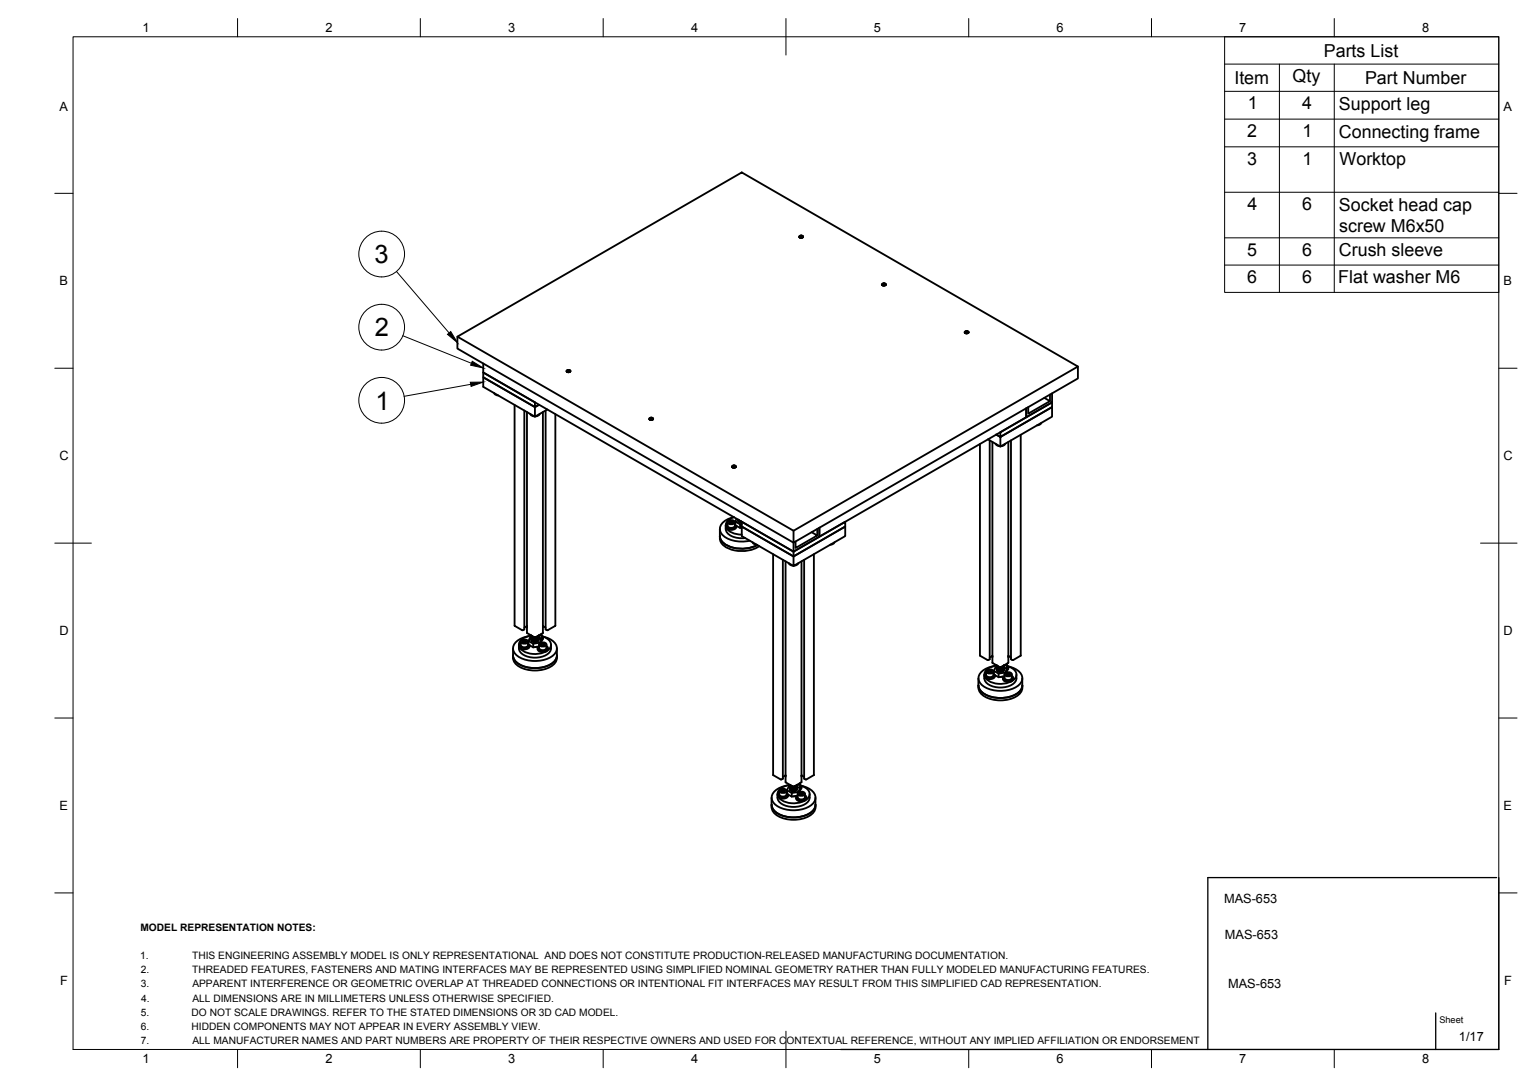
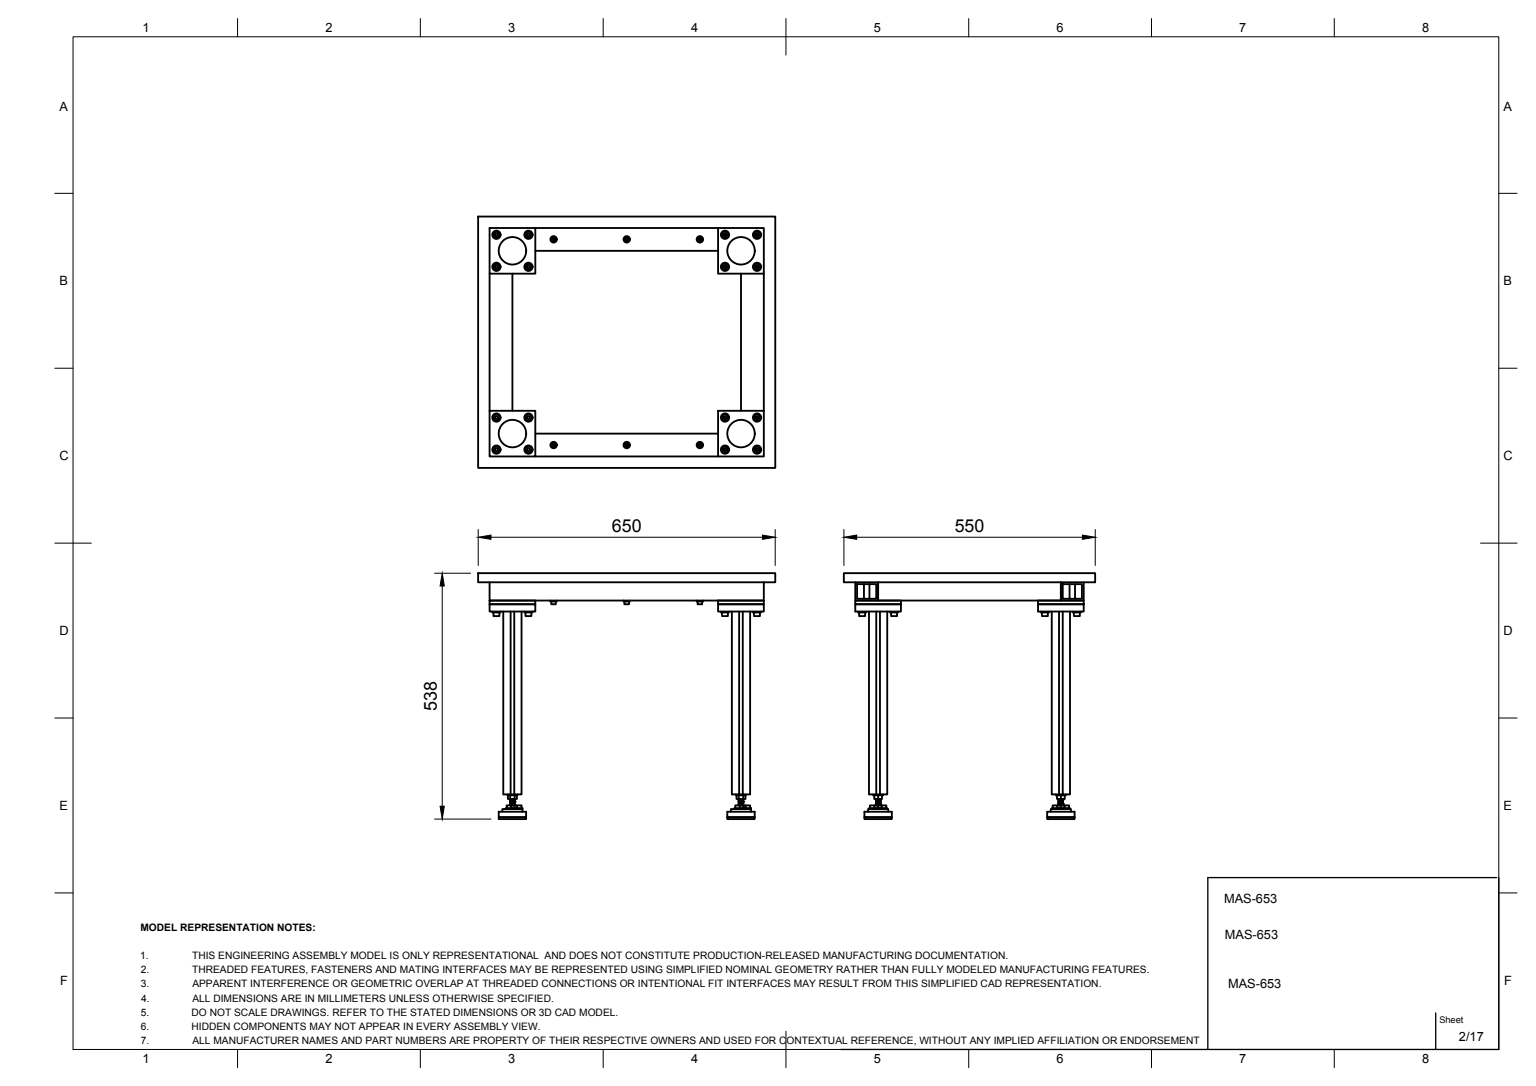
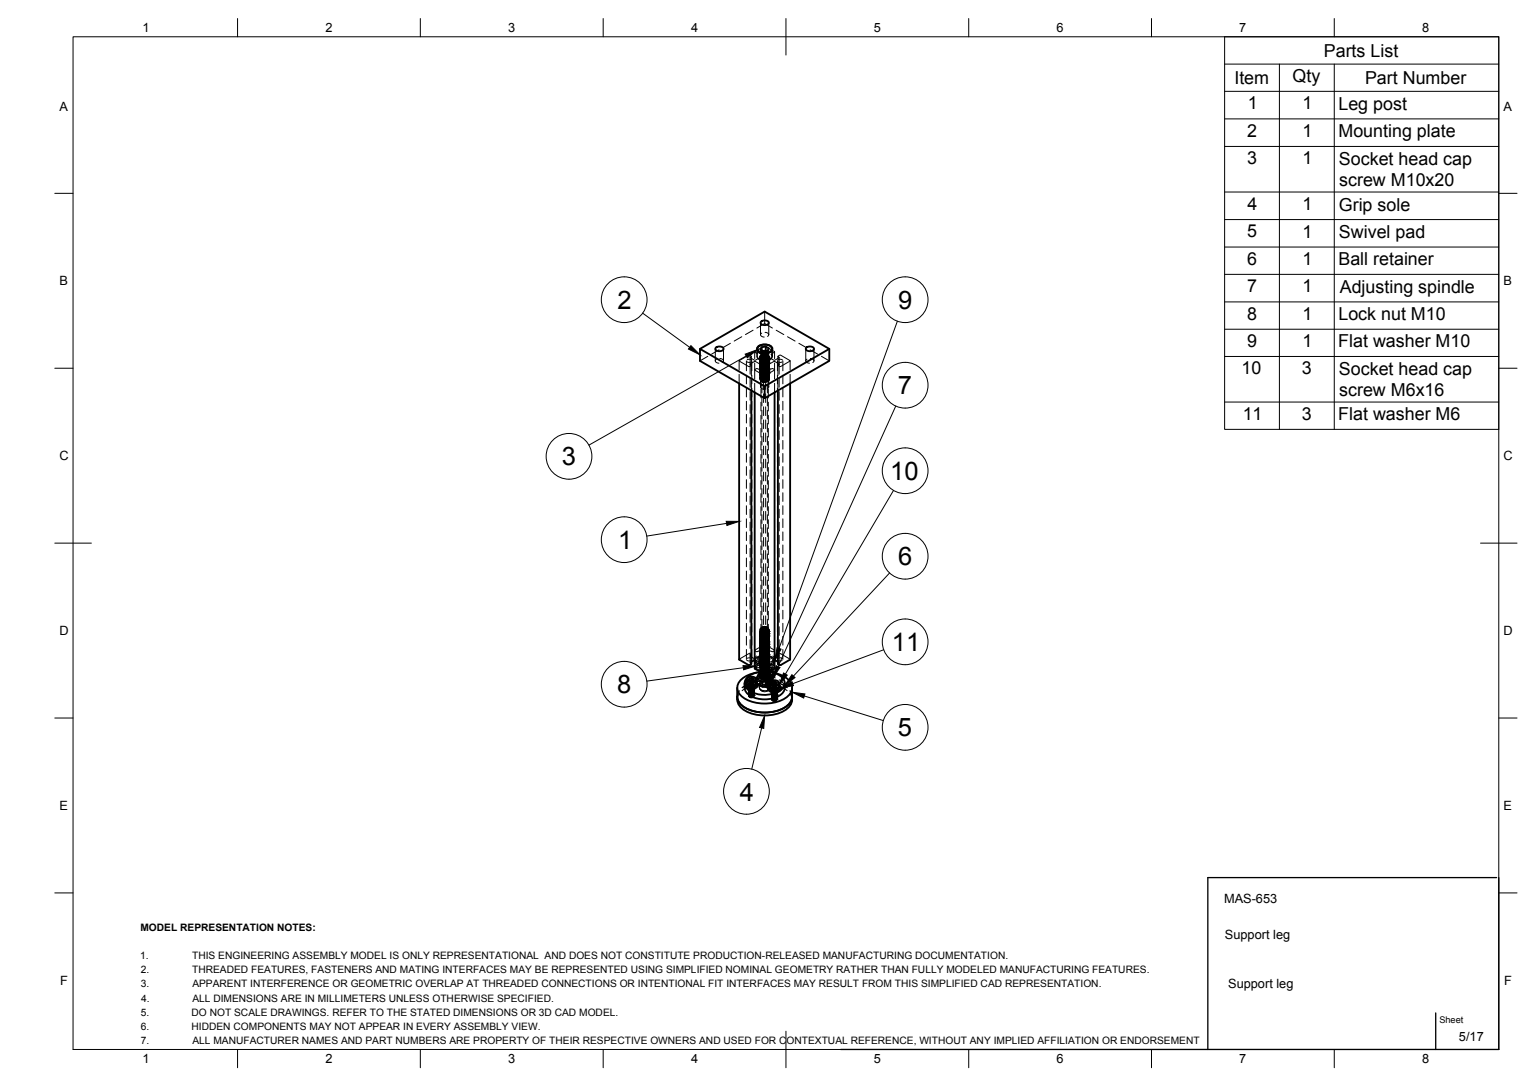
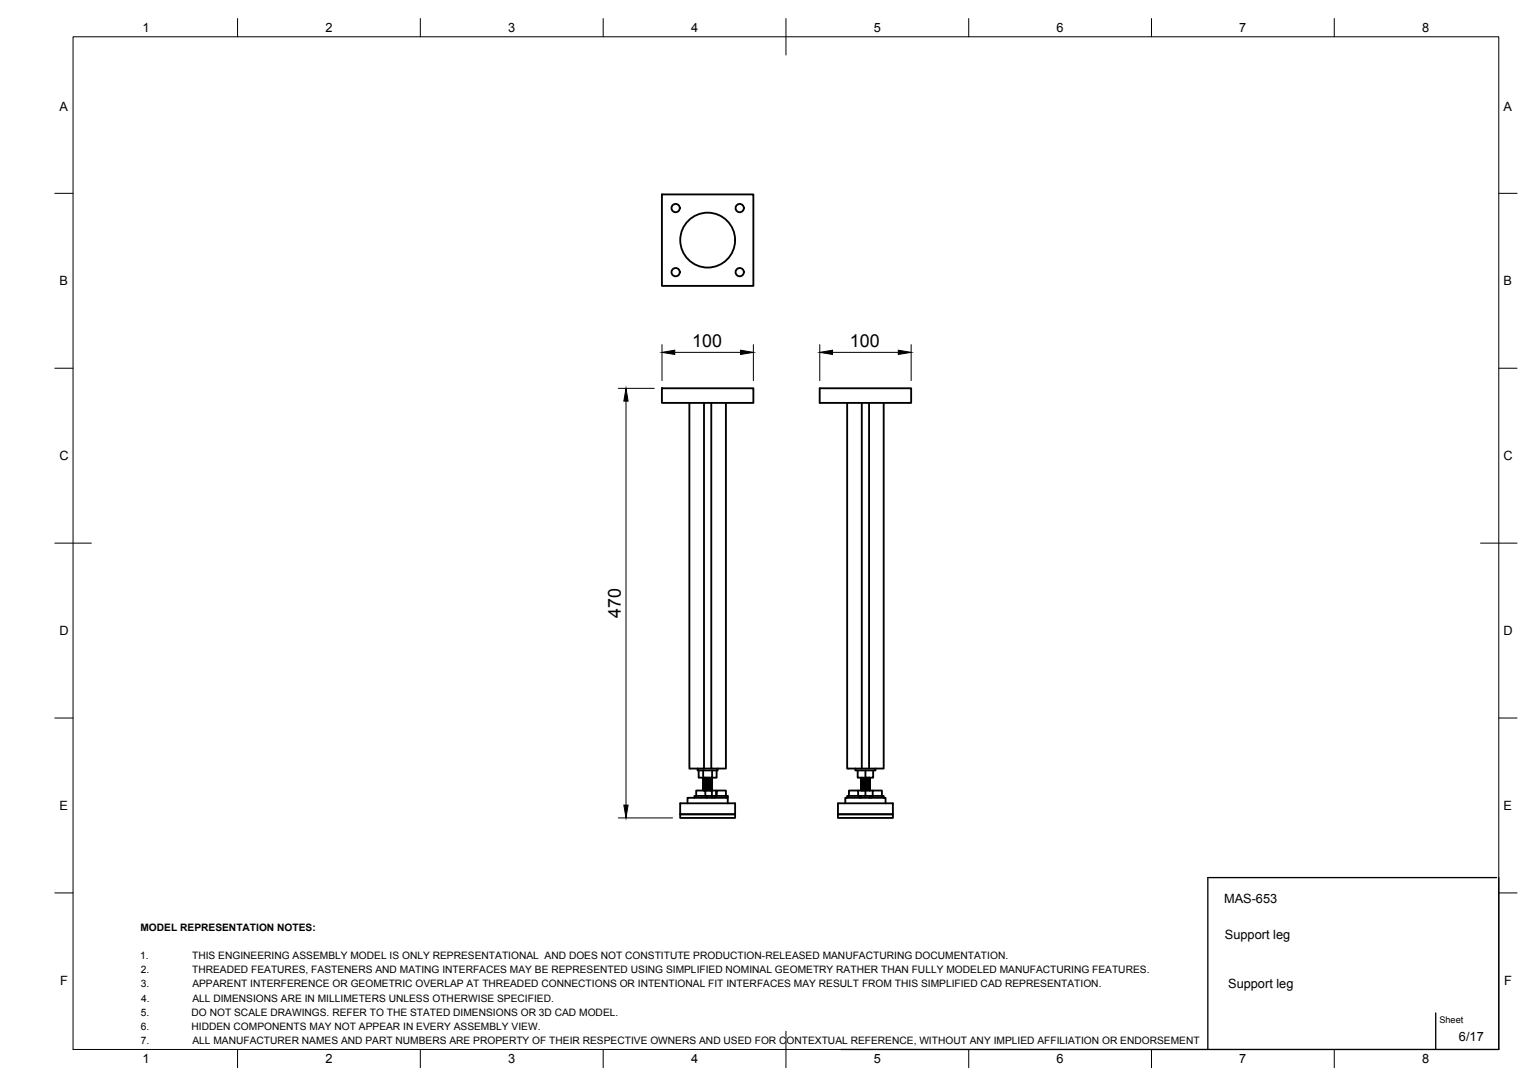
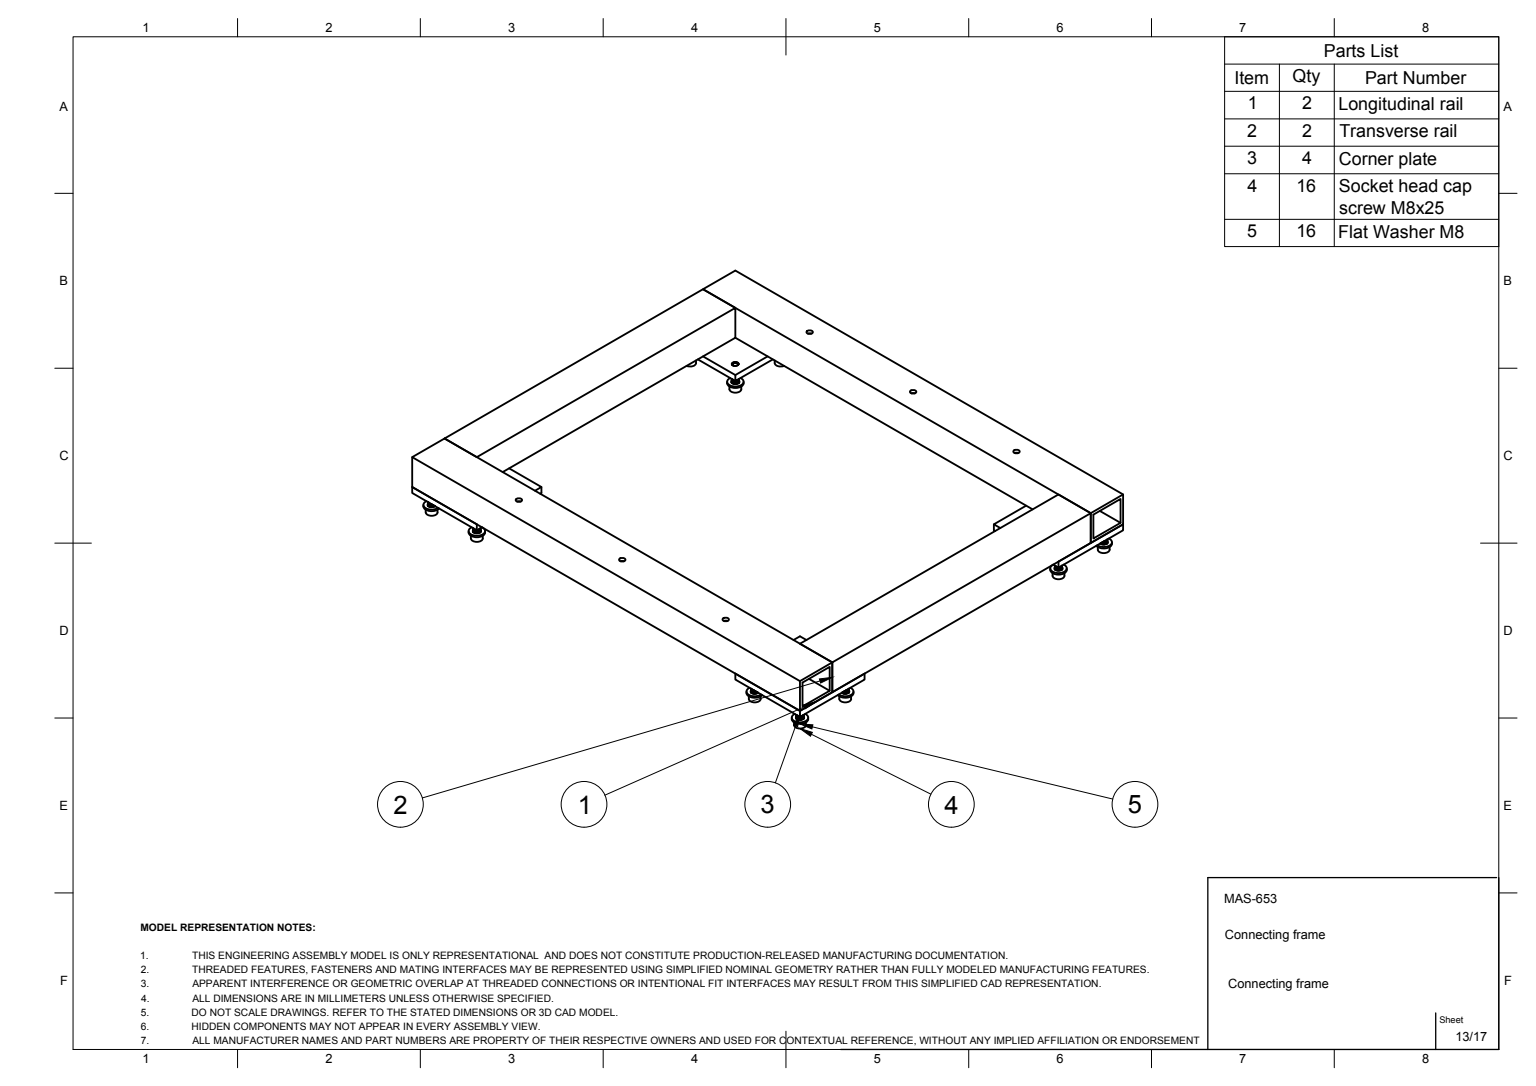
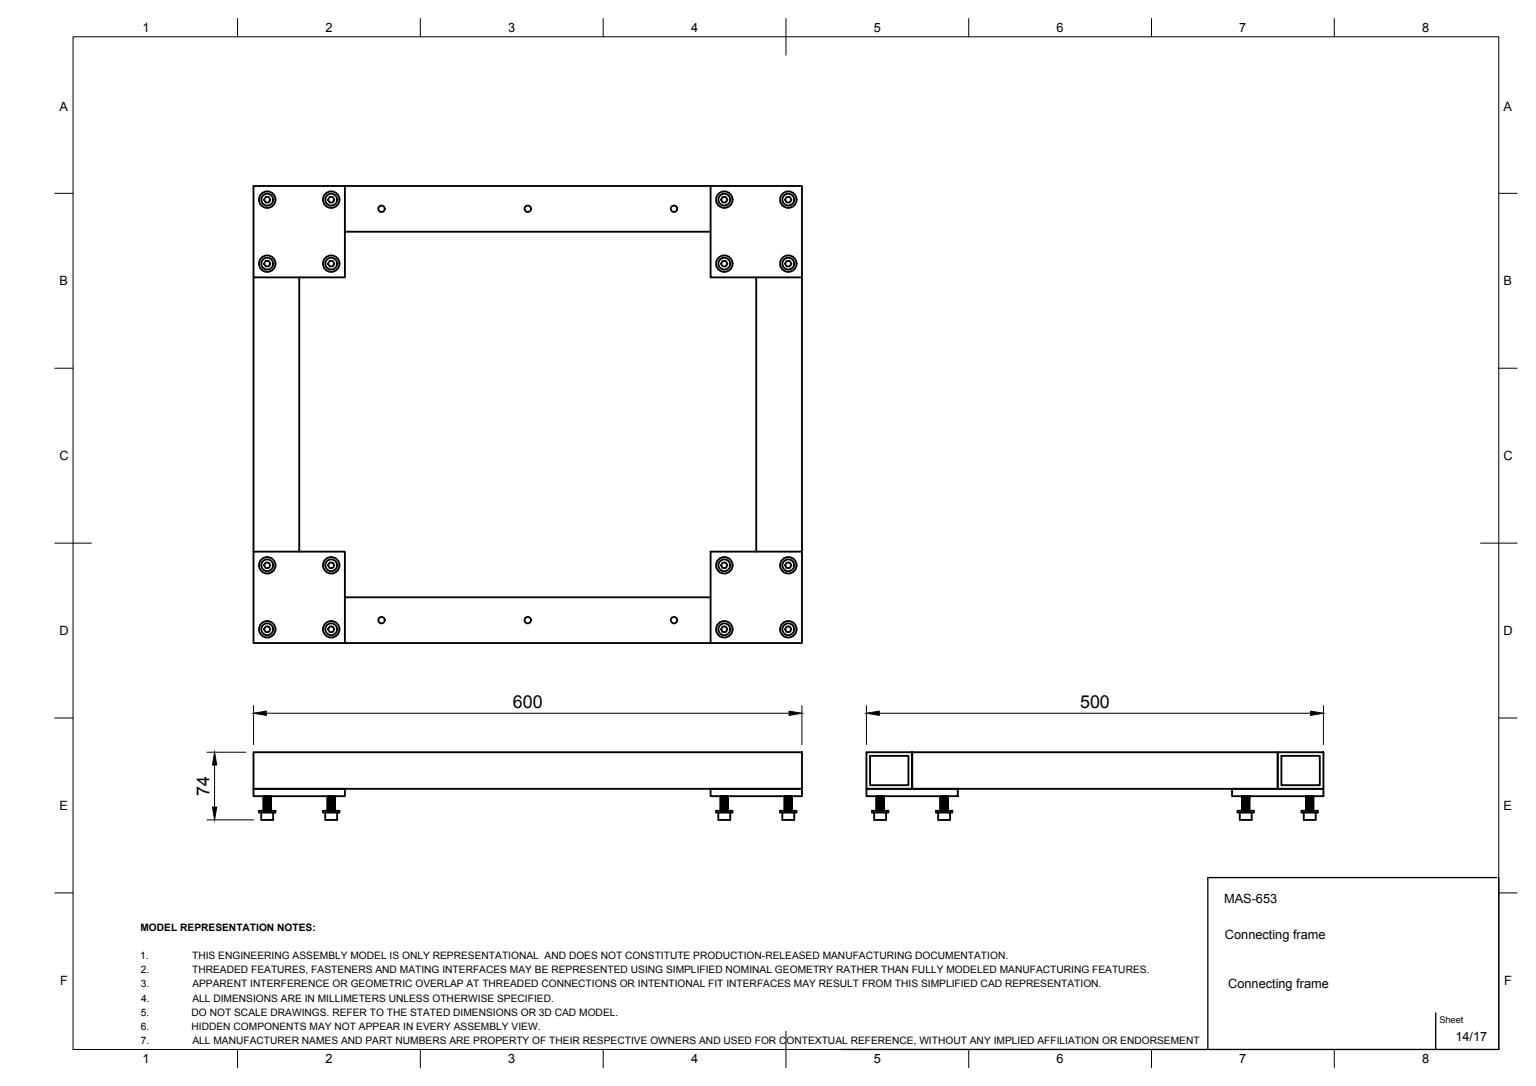
ISO-10303-21;
HEADER;
/* Generated by software containing ST-Developer
 * from STEP Tools, Inc. (www.steptools.com) 
 */

FILE_DESCRIPTION(
/* description */ ('Independent compact industrial fixture table, bolted aluminum worktop
 on connected adjustable support base. Whole-mm nominal dimensions. No
 load rating assigned.'),
/* implementation_level */ '2;1');

FILE_NAME(
/* name */ 'MAS-653.step',
/* time_stamp */ '2026-11-07T17:47:58-08:00',
/* author */ (''),
/* organization */ (''),
/* preprocessor_version */ 'ST-DEVELOPER v20.2',
/* originating_system */ 'Autodesk Translation Framework v15.17.0.0',
/* authorisation */ '');

FILE_SCHEMA (('AUTOMOTIVE_DESIGN { 1 0 10303 214 3 1 1 }'));
ENDSEC;

DATA;
#10=MECHANICAL_DESIGN_GEOMETRIC_PRESENTATION_REPRESENTATION('',(#2250,#2251,
#2252,#2253,#2254,#2255,#2256,#2257,#2258,#2259,#2260,#2261,#2262,#2263,
#2264,#2265,#2266,#2267,#2268),#97475);
#11=SPHERICAL_SURFACE('',#22780,6.);
#12=SPHERICAL_SURFACE('',#22798,6.);
#13=SPHERICAL_SURFACE('',#22948,6.);
#14=ITEM_DEFINED_TRANSFORMATION($,$,#22042,#22256);
#15=ITEM_DEFINED_TRANSFORMATION($,$,#22071,#22257);
#16=ITEM_DEFINED_TRANSFORMATION($,$,#22082,#22258);
#17=ITEM_DEFINED_TRANSFORMATION($,$,#22177,#22259);
#18=ITEM_DEFINED_TRANSFORMATION($,$,#22247,#22260);
#19=ITEM_DEFINED_TRANSFORMATION($,$,#22042,#22261);
#20=ITEM_DEFINED_TRANSFORMATION($,$,#22071,#22262);
#21=ITEM_DEFINED_TRANSFORMATION($,$,#22082,#22263);
#22=ITEM_DEFINED_TRANSFORMATION($,$,#22082,#22264);
#23=ITEM_DEFINED_TRANSFORMATION($,$,#22082,#22265);
#24=ITEM_DEFINED_TRANSFORMATION($,$,#22177,#22266);
#25=ITEM_DEFINED_TRANSFORMATION($,$,#22247,#22267);
#26=ITEM_DEFINED_TRANSFORMATION($,$,#22177,#22268);
#27=ITEM_DEFINED_TRANSFORMATION($,$,#22247,#22269);
#28=ITEM_DEFINED_TRANSFORMATION($,$,#22177,#22270);
#29=ITEM_DEFINED_TRANSFORMATION($,$,#22247,#22271);
#30=ITEM_DEFINED_TRANSFORMATION($,$,#22177,#22272);
#31=ITEM_DEFINED_TRANSFORMATION($,$,#22247,#22273);
#32=ITEM_DEFINED_TRANSFORMATION($,$,#22177,#22274);
#33=ITEM_DEFINED_TRANSFORMATION($,$,#22247,#22275);
#34=ITEM_DEFINED_TRANSFORMATION($,$,#22177,#22276);
#35=ITEM_DEFINED_TRANSFORMATION($,$,#22247,#22277);
#36=ITEM_DEFINED_TRANSFORMATION($,$,#22177,#22278);
#37=ITEM_DEFINED_TRANSFORMATION($,$,#22247,#22279);
#38=ITEM_DEFINED_TRANSFORMATION($,$,#22177,#22280);
#39=ITEM_DEFINED_TRANSFORMATION($,$,#22247,#22281);
#40=ITEM_DEFINED_TRANSFORMATION($,$,#22177,#22282);
#41=ITEM_DEFINED_TRANSFORMATION($,$,#22247,#22283);
#42=ITEM_DEFINED_TRANSFORMATION($,$,#22177,#22284);
#43=ITEM_DEFINED_TRANSFORMATION($,$,#22247,#22285);
#44=ITEM_DEFINED_TRANSFORMATION($,$,#22177,#22286);
#45=ITEM_DEFINED_TRANSFORMATION($,$,#22247,#22287);
#46=ITEM_DEFINED_TRANSFORMATION($,$,#22177,#22288);
#47=ITEM_DEFINED_TRANSFORMATION($,$,#22247,#22289);
#48=ITEM_DEFINED_TRANSFORMATION($,$,#22177,#22290);
#49=ITEM_DEFINED_TRANSFORMATION($,$,#22247,#22291);
#50=ITEM_DEFINED_TRANSFORMATION($,$,#22177,#22292);
#51=ITEM_DEFINED_TRANSFORMATION($,$,#22247,#22293);
#52=ITEM_DEFINED_TRANSFORMATION($,$,#22177,#22294);
#53=ITEM_DEFINED_TRANSFORMATION($,$,#22247,#22295);
#54=ITEM_DEFINED_TRANSFORMATION($,$,#22297,#23463);
#55=ITEM_DEFINED_TRANSFORMATION($,$,#22609,#23464);
#56=ITEM_DEFINED_TRANSFORMATION($,$,#22635,#23465);
#57=ITEM_DEFINED_TRANSFORMATION($,$,#22695,#23466);
#58=ITEM_DEFINED_TRANSFORMATION($,$,#22701,#23467);
#59=ITEM_DEFINED_TRANSFORMATION($,$,#22788,#23468);
#60=ITEM_DEFINED_TRANSFORMATION($,$,#22809,#23469);
#61=ITEM_DEFINED_TRANSFORMATION($,$,#22950,#23470);
#62=ITEM_DEFINED_TRANSFORMATION($,$,#22981,#23471);
#63=ITEM_DEFINED_TRANSFORMATION($,$,#22990,#23472);
#64=ITEM_DEFINED_TRANSFORMATION($,$,#23454,#23473);
#65=ITEM_DEFINED_TRANSFORMATION($,$,#22990,#23474);
#66=ITEM_DEFINED_TRANSFORMATION($,$,#23454,#23475);
#67=ITEM_DEFINED_TRANSFORMATION($,$,#22990,#23476);
#68=ITEM_DEFINED_TRANSFORMATION($,$,#23454,#23477);
#69=ITEM_DEFINED_TRANSFORMATION($,$,#22296,#23478);
#70=ITEM_DEFINED_TRANSFORMATION($,$,#22041,#23479);
#71=ITEM_DEFINED_TRANSFORMATION($,$,#22296,#23480);
#72=ITEM_DEFINED_TRANSFORMATION($,$,#22296,#23481);
#73=ITEM_DEFINED_TRANSFORMATION($,$,#22296,#23482);
#74=ITEM_DEFINED_TRANSFORMATION($,$,#23042,#23483);
#75=ITEM_DEFINED_TRANSFORMATION($,$,#23325,#23484);
#76=ITEM_DEFINED_TRANSFORMATION($,$,#23445,#23485);
#77=ITEM_DEFINED_TRANSFORMATION($,$,#23454,#23486);
#78=ITEM_DEFINED_TRANSFORMATION($,$,#23325,#23487);
#79=ITEM_DEFINED_TRANSFORMATION($,$,#23445,#23488);
#80=ITEM_DEFINED_TRANSFORMATION($,$,#23454,#23489);
#81=ITEM_DEFINED_TRANSFORMATION($,$,#23325,#23490);
#82=ITEM_DEFINED_TRANSFORMATION($,$,#23445,#23491);
#83=ITEM_DEFINED_TRANSFORMATION($,$,#23454,#23492);
#84=ITEM_DEFINED_TRANSFORMATION($,$,#23325,#23493);
#85=ITEM_DEFINED_TRANSFORMATION($,$,#23445,#23494);
#86=ITEM_DEFINED_TRANSFORMATION($,$,#23454,#23495);
#87=ITEM_DEFINED_TRANSFORMATION($,$,#23325,#23496);
#88=ITEM_DEFINED_TRANSFORMATION($,$,#23445,#23497);
#89=ITEM_DEFINED_TRANSFORMATION($,$,#23454,#23498);
#90=ITEM_DEFINED_TRANSFORMATION($,$,#23325,#23499);
#91=ITEM_DEFINED_TRANSFORMATION($,$,#23445,#23500);
#92=ITEM_DEFINED_TRANSFORMATION($,$,#23454,#23501);
#93=(
REPRESENTATION_RELATIONSHIP($,$,#97605,#97604)
REPRESENTATION_RELATIONSHIP_WITH_TRANSFORMATION(#14)
SHAPE_REPRESENTATION_RELATIONSHIP()
);
#94=(
REPRESENTATION_RELATIONSHIP($,$,#97606,#97604)
REPRESENTATION_RELATIONSHIP_WITH_TRANSFORMATION(#15)
SHAPE_REPRESENTATION_RELATIONSHIP()
);
#95=(
REPRESENTATION_RELATIONSHIP($,$,#97607,#97604)
REPRESENTATION_RELATIONSHIP_WITH_TRANSFORMATION(#16)
SHAPE_REPRESENTATION_RELATIONSHIP()
);
#96=(
REPRESENTATION_RELATIONSHIP($,$,#97608,#97604)
REPRESENTATION_RELATIONSHIP_WITH_TRANSFORMATION(#17)
SHAPE_REPRESENTATION_RELATIONSHIP()
);
#97=(
REPRESENTATION_RELATIONSHIP($,$,#97609,#97604)
REPRESENTATION_RELATIONSHIP_WITH_TRANSFORMATION(#18)
SHAPE_REPRESENTATION_RELATIONSHIP()
);
#98=(
REPRESENTATION_RELATIONSHIP($,$,#97605,#97604)
REPRESENTATION_RELATIONSHIP_WITH_TRANSFORMATION(#19)
SHAPE_REPRESENTATION_RELATIONSHIP()
);
#99=(
REPRESENTATION_RELATIONSHIP($,$,#97606,#97604)
REPRESENTATION_RELATIONSHIP_WITH_TRANSFORMATION(#20)
SHAPE_REPRESENTATION_RELATIONSHIP()
);
#100=(
REPRESENTATION_RELATIONSHIP($,$,#97607,#97604)
REPRESENTATION_RELATIONSHIP_WITH_TRANSFORMATION(#21)
SHAPE_REPRESENTATION_RELATIONSHIP()
);
#101=(
REPRESENTATION_RELATIONSHIP($,$,#97607,#97604)
REPRESENTATION_RELATIONSHIP_WITH_TRANSFORMATION(#22)
SHAPE_REPRESENTATION_RELATIONSHIP()
);
#102=(
REPRESENTATION_RELATIONSHIP($,$,#97607,#97604)
REPRESENTATION_RELATIONSHIP_WITH_TRANSFORMATION(#23)
SHAPE_REPRESENTATION_RELATIONSHIP()
);
#103=(
REPRESENTATION_RELATIONSHIP($,$,#97608,#97604)
REPRESENTATION_RELATIONSHIP_WITH_TRANSFORMATION(#24)
SHAPE_REPRESENTATION_RELATIONSHIP()
);
#104=(
REPRESENTATION_RELATIONSHIP($,$,#97609,#97604)
REPRESENTATION_RELATIONSHIP_WITH_TRANSFORMATION(#25)
SHAPE_REPRESENTATION_RELATIONSHIP()
);
#105=(
REPRESENTATION_RELATIONSHIP($,$,#97608,#97604)
REPRESENTATION_RELATIONSHIP_WITH_TRANSFORMATION(#26)
SHAPE_REPRESENTATION_RELATIONSHIP()
);
#106=(
REPRESENTATION_RELATIONSHIP($,$,#97609,#97604)
REPRESENTATION_RELATIONSHIP_WITH_TRANSFORMATION(#27)
SHAPE_REPRESENTATION_RELATIONSHIP()
);
#107=(
REPRESENTATION_RELATIONSHIP($,$,#97608,#97604)
REPRESENTATION_RELATIONSHIP_WITH_TRANSFORMATION(#28)
SHAPE_REPRESENTATION_RELATIONSHIP()
);
#108=(
REPRESENTATION_RELATIONSHIP($,$,#97609,#97604)
REPRESENTATION_RELATIONSHIP_WITH_TRANSFORMATION(#29)
SHAPE_REPRESENTATION_RELATIONSHIP()
);
#109=(
REPRESENTATION_RELATIONSHIP($,$,#97608,#97604)
REPRESENTATION_RELATIONSHIP_WITH_TRANSFORMATION(#30)
SHAPE_REPRESENTATION_RELATIONSHIP()
);
#110=(
REPRESENTATION_RELATIONSHIP($,$,#97609,#97604)
REPRESENTATION_RELATIONSHIP_WITH_TRANSFORMATION(#31)
SHAPE_REPRESENTATION_RELATIONSHIP()
);
#111=(
REPRESENTATION_RELATIONSHIP($,$,#97608,#97604)
REPRESENTATION_RELATIONSHIP_WITH_TRANSFORMATION(#32)
SHAPE_REPRESENTATION_RELATIONSHIP()
);
#112=(
REPRESENTATION_RELATIONSHIP($,$,#97609,#97604)
REPRESENTATION_RELATIONSHIP_WITH_TRANSFORMATION(#33)
SHAPE_REPRESENTATION_RELATIONSHIP()
);
#113=(
REPRESENTATION_RELATIONSHIP($,$,#97608,#97604)
REPRESENTATION_RELATIONSHIP_WITH_TRANSFORMATION(#34)
SHAPE_REPRESENTATION_RELATIONSHIP()
);
#114=(
REPRESENTATION_RELATIONSHIP($,$,#97609,#97604)
REPRESENTATION_RELATIONSHIP_WITH_TRANSFORMATION(#35)
SHAPE_REPRESENTATION_RELATIONSHIP()
);
#115=(
REPRESENTATION_RELATIONSHIP($,$,#97608,#97604)
REPRESENTATION_RELATIONSHIP_WITH_TRANSFORMATION(#36)
SHAPE_REPRESENTATION_RELATIONSHIP()
);
#116=(
REPRESENTATION_RELATIONSHIP($,$,#97609,#97604)
REPRESENTATION_RELATIONSHIP_WITH_TRANSFORMATION(#37)
SHAPE_REPRESENTATION_RELATIONSHIP()
);
#117=(
REPRESENTATION_RELATIONSHIP($,$,#97608,#97604)
REPRESENTATION_RELATIONSHIP_WITH_TRANSFORMATION(#38)
SHAPE_REPRESENTATION_RELATIONSHIP()
);
#118=(
REPRESENTATION_RELATIONSHIP($,$,#97609,#97604)
REPRESENTATION_RELATIONSHIP_WITH_TRANSFORMATION(#39)
SHAPE_REPRESENTATION_RELATIONSHIP()
);
#119=(
REPRESENTATION_RELATIONSHIP($,$,#97608,#97604)
REPRESENTATION_RELATIONSHIP_WITH_TRANSFORMATION(#40)
SHAPE_REPRESENTATION_RELATIONSHIP()
);
#120=(
REPRESENTATION_RELATIONSHIP($,$,#97609,#97604)
REPRESENTATION_RELATIONSHIP_WITH_TRANSFORMATION(#41)
SHAPE_REPRESENTATION_RELATIONSHIP()
);
#121=(
REPRESENTATION_RELATIONSHIP($,$,#97608,#97604)
REPRESENTATION_RELATIONSHIP_WITH_TRANSFORMATION(#42)
SHAPE_REPRESENTATION_RELATIONSHIP()
);
#122=(
REPRESENTATION_RELATIONSHIP($,$,#97609,#97604)
REPRESENTATION_RELATIONSHIP_WITH_TRANSFORMATION(#43)
SHAPE_REPRESENTATION_RELATIONSHIP()
);
#123=(
REPRESENTATION_RELATIONSHIP($,$,#97608,#97604)
REPRESENTATION_RELATIONSHIP_WITH_TRANSFORMATION(#44)
SHAPE_REPRESENTATION_RELATIONSHIP()
);
#124=(
REPRESENTATION_RELATIONSHIP($,$,#97609,#97604)
REPRESENTATION_RELATIONSHIP_WITH_TRANSFORMATION(#45)
SHAPE_REPRESENTATION_RELATIONSHIP()
);
#125=(
REPRESENTATION_RELATIONSHIP($,$,#97608,#97604)
REPRESENTATION_RELATIONSHIP_WITH_TRANSFORMATION(#46)
SHAPE_REPRESENTATION_RELATIONSHIP()
);
#126=(
REPRESENTATION_RELATIONSHIP($,$,#97609,#97604)
REPRESENTATION_RELATIONSHIP_WITH_TRANSFORMATION(#47)
SHAPE_REPRESENTATION_RELATIONSHIP()
);
#127=(
REPRESENTATION_RELATIONSHIP($,$,#97608,#97604)
REPRESENTATION_RELATIONSHIP_WITH_TRANSFORMATION(#48)
SHAPE_REPRESENTATION_RELATIONSHIP()
);
#128=(
REPRESENTATION_RELATIONSHIP($,$,#97609,#97604)
REPRESENTATION_RELATIONSHIP_WITH_TRANSFORMATION(#49)
SHAPE_REPRESENTATION_RELATIONSHIP()
);
#129=(
REPRESENTATION_RELATIONSHIP($,$,#97608,#97604)
REPRESENTATION_RELATIONSHIP_WITH_TRANSFORMATION(#50)
SHAPE_REPRESENTATION_RELATIONSHIP()
);
#130=(
REPRESENTATION_RELATIONSHIP($,$,#97609,#97604)
REPRESENTATION_RELATIONSHIP_WITH_TRANSFORMATION(#51)
SHAPE_REPRESENTATION_RELATIONSHIP()
);
#131=(
REPRESENTATION_RELATIONSHIP($,$,#97608,#97604)
REPRESENTATION_RELATIONSHIP_WITH_TRANSFORMATION(#52)
SHAPE_REPRESENTATION_RELATIONSHIP()
);
#132=(
REPRESENTATION_RELATIONSHIP($,$,#97609,#97604)
REPRESENTATION_RELATIONSHIP_WITH_TRANSFORMATION(#53)
SHAPE_REPRESENTATION_RELATIONSHIP()
);
#133=(
REPRESENTATION_RELATIONSHIP($,$,#97611,#97610)
REPRESENTATION_RELATIONSHIP_WITH_TRANSFORMATION(#54)
SHAPE_REPRESENTATION_RELATIONSHIP()
);
#134=(
REPRESENTATION_RELATIONSHIP($,$,#97612,#97610)
REPRESENTATION_RELATIONSHIP_WITH_TRANSFORMATION(#55)
SHAPE_REPRESENTATION_RELATIONSHIP()
);
#135=(
REPRESENTATION_RELATIONSHIP($,$,#97613,#97610)
REPRESENTATION_RELATIONSHIP_WITH_TRANSFORMATION(#56)
SHAPE_REPRESENTATION_RELATIONSHIP()
);
#136=(
REPRESENTATION_RELATIONSHIP($,$,#97614,#97610)
REPRESENTATION_RELATIONSHIP_WITH_TRANSFORMATION(#57)
SHAPE_REPRESENTATION_RELATIONSHIP()
);
#137=(
REPRESENTATION_RELATIONSHIP($,$,#97615,#97610)
REPRESENTATION_RELATIONSHIP_WITH_TRANSFORMATION(#58)
SHAPE_REPRESENTATION_RELATIONSHIP()
);
#138=(
REPRESENTATION_RELATIONSHIP($,$,#97616,#97610)
REPRESENTATION_RELATIONSHIP_WITH_TRANSFORMATION(#59)
SHAPE_REPRESENTATION_RELATIONSHIP()
);
#139=(
REPRESENTATION_RELATIONSHIP($,$,#97617,#97610)
REPRESENTATION_RELATIONSHIP_WITH_TRANSFORMATION(#60)
SHAPE_REPRESENTATION_RELATIONSHIP()
);
#140=(
REPRESENTATION_RELATIONSHIP($,$,#97618,#97610)
REPRESENTATION_RELATIONSHIP_WITH_TRANSFORMATION(#61)
SHAPE_REPRESENTATION_RELATIONSHIP()
);
#141=(
REPRESENTATION_RELATIONSHIP($,$,#97619,#97610)
REPRESENTATION_RELATIONSHIP_WITH_TRANSFORMATION(#62)
SHAPE_REPRESENTATION_RELATIONSHIP()
);
#142=(
REPRESENTATION_RELATIONSHIP($,$,#97620,#97610)
REPRESENTATION_RELATIONSHIP_WITH_TRANSFORMATION(#63)
SHAPE_REPRESENTATION_RELATIONSHIP()
);
#143=(
REPRESENTATION_RELATIONSHIP($,$,#97624,#97610)
REPRESENTATION_RELATIONSHIP_WITH_TRANSFORMATION(#64)
SHAPE_REPRESENTATION_RELATIONSHIP()
);
#144=(
REPRESENTATION_RELATIONSHIP($,$,#97620,#97610)
REPRESENTATION_RELATIONSHIP_WITH_TRANSFORMATION(#65)
SHAPE_REPRESENTATION_RELATIONSHIP()
);
#145=(
REPRESENTATION_RELATIONSHIP($,$,#97624,#97610)
REPRESENTATION_RELATIONSHIP_WITH_TRANSFORMATION(#66)
SHAPE_REPRESENTATION_RELATIONSHIP()
);
#146=(
REPRESENTATION_RELATIONSHIP($,$,#97620,#97610)
REPRESENTATION_RELATIONSHIP_WITH_TRANSFORMATION(#67)
SHAPE_REPRESENTATION_RELATIONSHIP()
);
#147=(
REPRESENTATION_RELATIONSHIP($,$,#97624,#97610)
REPRESENTATION_RELATIONSHIP_WITH_TRANSFORMATION(#68)
SHAPE_REPRESENTATION_RELATIONSHIP()
);
#148=(
REPRESENTATION_RELATIONSHIP($,$,#97610,#97603)
REPRESENTATION_RELATIONSHIP_WITH_TRANSFORMATION(#69)
SHAPE_REPRESENTATION_RELATIONSHIP()
);
#149=(
REPRESENTATION_RELATIONSHIP($,$,#97604,#97603)
REPRESENTATION_RELATIONSHIP_WITH_TRANSFORMATION(#70)
SHAPE_REPRESENTATION_RELATIONSHIP()
);
#150=(
REPRESENTATION_RELATIONSHIP($,$,#97610,#97603)
REPRESENTATION_RELATIONSHIP_WITH_TRANSFORMATION(#71)
SHAPE_REPRESENTATION_RELATIONSHIP()
);
#151=(
REPRESENTATION_RELATIONSHIP($,$,#97610,#97603)
REPRESENTATION_RELATIONSHIP_WITH_TRANSFORMATION(#72)
SHAPE_REPRESENTATION_RELATIONSHIP()
);
#152=(
REPRESENTATION_RELATIONSHIP($,$,#97610,#97603)
REPRESENTATION_RELATIONSHIP_WITH_TRANSFORMATION(#73)
SHAPE_REPRESENTATION_RELATIONSHIP()
);
#153=(
REPRESENTATION_RELATIONSHIP($,$,#97621,#97603)
REPRESENTATION_RELATIONSHIP_WITH_TRANSFORMATION(#74)
SHAPE_REPRESENTATION_RELATIONSHIP()
);
#154=(
REPRESENTATION_RELATIONSHIP($,$,#97622,#97603)
REPRESENTATION_RELATIONSHIP_WITH_TRANSFORMATION(#75)
SHAPE_REPRESENTATION_RELATIONSHIP()
);
#155=(
REPRESENTATION_RELATIONSHIP($,$,#97623,#97603)
REPRESENTATION_RELATIONSHIP_WITH_TRANSFORMATION(#76)
SHAPE_REPRESENTATION_RELATIONSHIP()
);
#156=(
REPRESENTATION_RELATIONSHIP($,$,#97624,#97603)
REPRESENTATION_RELATIONSHIP_WITH_TRANSFORMATION(#77)
SHAPE_REPRESENTATION_RELATIONSHIP()
);
#157=(
REPRESENTATION_RELATIONSHIP($,$,#97622,#97603)
REPRESENTATION_RELATIONSHIP_WITH_TRANSFORMATION(#78)
SHAPE_REPRESENTATION_RELATIONSHIP()
);
#158=(
REPRESENTATION_RELATIONSHIP($,$,#97623,#97603)
REPRESENTATION_RELATIONSHIP_WITH_TRANSFORMATION(#79)
SHAPE_REPRESENTATION_RELATIONSHIP()
);
#159=(
REPRESENTATION_RELATIONSHIP($,$,#97624,#97603)
REPRESENTATION_RELATIONSHIP_WITH_TRANSFORMATION(#80)
SHAPE_REPRESENTATION_RELATIONSHIP()
);
#160=(
REPRESENTATION_RELATIONSHIP($,$,#97622,#97603)
REPRESENTATION_RELATIONSHIP_WITH_TRANSFORMATION(#81)
SHAPE_REPRESENTATION_RELATIONSHIP()
);
#161=(
REPRESENTATION_RELATIONSHIP($,$,#97623,#97603)
REPRESENTATION_RELATIONSHIP_WITH_TRANSFORMATION(#82)
SHAPE_REPRESENTATION_RELATIONSHIP()
);
#162=(
REPRESENTATION_RELATIONSHIP($,$,#97624,#97603)
REPRESENTATION_RELATIONSHIP_WITH_TRANSFORMATION(#83)
SHAPE_REPRESENTATION_RELATIONSHIP()
);
#163=(
REPRESENTATION_RELATIONSHIP($,$,#97622,#97603)
REPRESENTATION_RELATIONSHIP_WITH_TRANSFORMATION(#84)
SHAPE_REPRESENTATION_RELATIONSHIP()
);
#164=(
REPRESENTATION_RELATIONSHIP($,$,#97623,#97603)
REPRESENTATION_RELATIONSHIP_WITH_TRANSFORMATION(#85)
SHAPE_REPRESENTATION_RELATIONSHIP()
);
#165=(
REPRESENTATION_RELATIONSHIP($,$,#97624,#97603)
REPRESENTATION_RELATIONSHIP_WITH_TRANSFORMATION(#86)
SHAPE_REPRESENTATION_RELATIONSHIP()
);
#166=(
REPRESENTATION_RELATIONSHIP($,$,#97622,#97603)
REPRESENTATION_RELATIONSHIP_WITH_TRANSFORMATION(#87)
SHAPE_REPRESENTATION_RELATIONSHIP()
);
#167=(
REPRESENTATION_RELATIONSHIP($,$,#97623,#97603)
REPRESENTATION_RELATIONSHIP_WITH_TRANSFORMATION(#88)
SHAPE_REPRESENTATION_RELATIONSHIP()
);
#168=(
REPRESENTATION_RELATIONSHIP($,$,#97624,#97603)
REPRESENTATION_RELATIONSHIP_WITH_TRANSFORMATION(#89)
SHAPE_REPRESENTATION_RELATIONSHIP()
);
#169=(
REPRESENTATION_RELATIONSHIP($,$,#97622,#97603)
REPRESENTATION_RELATIONSHIP_WITH_TRANSFORMATION(#90)
SHAPE_REPRESENTATION_RELATIONSHIP()
);
#170=(
REPRESENTATION_RELATIONSHIP($,$,#97623,#97603)
REPRESENTATION_RELATIONSHIP_WITH_TRANSFORMATION(#91)
SHAPE_REPRESENTATION_RELATIONSHIP()
);
#171=(
REPRESENTATION_RELATIONSHIP($,$,#97624,#97603)
REPRESENTATION_RELATIONSHIP_WITH_TRANSFORMATION(#92)
SHAPE_REPRESENTATION_RELATIONSHIP()
);
#172=CONTEXT_DEPENDENT_SHAPE_REPRESENTATION(#93,#97509);
#173=CONTEXT_DEPENDENT_SHAPE_REPRESENTATION(#94,#97510);
#174=CONTEXT_DEPENDENT_SHAPE_REPRESENTATION(#95,#97511);
#175=CONTEXT_DEPENDENT_SHAPE_REPRESENTATION(#96,#97512);
#176=CONTEXT_DEPENDENT_SHAPE_REPRESENTATION(#97,#97513);
#177=CONTEXT_DEPENDENT_SHAPE_REPRESENTATION(#98,#97514);
#178=CONTEXT_DEPENDENT_SHAPE_REPRESENTATION(#99,#97515);
#179=CONTEXT_DEPENDENT_SHAPE_REPRESENTATION(#100,#97516);
#180=CONTEXT_DEPENDENT_SHAPE_REPRESENTATION(#101,#97517);
#181=CONTEXT_DEPENDENT_SHAPE_REPRESENTATION(#102,#97518);
#182=CONTEXT_DEPENDENT_SHAPE_REPRESENTATION(#103,#97519);
#183=CONTEXT_DEPENDENT_SHAPE_REPRESENTATION(#104,#97520);
#184=CONTEXT_DEPENDENT_SHAPE_REPRESENTATION(#105,#97521);
#185=CONTEXT_DEPENDENT_SHAPE_REPRESENTATION(#106,#97522);
#186=CONTEXT_DEPENDENT_SHAPE_REPRESENTATION(#107,#97523);
#187=CONTEXT_DEPENDENT_SHAPE_REPRESENTATION(#108,#97524);
#188=CONTEXT_DEPENDENT_SHAPE_REPRESENTATION(#109,#97525);
#189=CONTEXT_DEPENDENT_SHAPE_REPRESENTATION(#110,#97526);
#190=CONTEXT_DEPENDENT_SHAPE_REPRESENTATION(#111,#97527);
#191=CONTEXT_DEPENDENT_SHAPE_REPRESENTATION(#112,#97528);
#192=CONTEXT_DEPENDENT_SHAPE_REPRESENTATION(#113,#97529);
#193=CONTEXT_DEPENDENT_SHAPE_REPRESENTATION(#114,#97530);
#194=CONTEXT_DEPENDENT_SHAPE_REPRESENTATION(#115,#97531);
#195=CONTEXT_DEPENDENT_SHAPE_REPRESENTATION(#116,#97532);
#196=CONTEXT_DEPENDENT_SHAPE_REPRESENTATION(#117,#97533);
#197=CONTEXT_DEPENDENT_SHAPE_REPRESENTATION(#118,#97534);
#198=CONTEXT_DEPENDENT_SHAPE_REPRESENTATION(#119,#97535);
#199=CONTEXT_DEPENDENT_SHAPE_REPRESENTATION(#120,#97536);
#200=CONTEXT_DEPENDENT_SHAPE_REPRESENTATION(#121,#97537);
#201=CONTEXT_DEPENDENT_SHAPE_REPRESENTATION(#122,#97538);
#202=CONTEXT_DEPENDENT_SHAPE_REPRESENTATION(#123,#97539);
#203=CONTEXT_DEPENDENT_SHAPE_REPRESENTATION(#124,#97540);
#204=CONTEXT_DEPENDENT_SHAPE_REPRESENTATION(#125,#97541);
#205=CONTEXT_DEPENDENT_SHAPE_REPRESENTATION(#126,#97542);
#206=CONTEXT_DEPENDENT_SHAPE_REPRESENTATION(#127,#97543);
#207=CONTEXT_DEPENDENT_SHAPE_REPRESENTATION(#128,#97544);
#208=CONTEXT_DEPENDENT_SHAPE_REPRESENTATION(#129,#97545);
#209=CONTEXT_DEPENDENT_SHAPE_REPRESENTATION(#130,#97546);
#210=CONTEXT_DEPENDENT_SHAPE_REPRESENTATION(#131,#97547);
#211=CONTEXT_DEPENDENT_SHAPE_REPRESENTATION(#132,#97548);
#212=CONTEXT_DEPENDENT_SHAPE_REPRESENTATION(#133,#97564);
#213=CONTEXT_DEPENDENT_SHAPE_REPRESENTATION(#134,#97565);
#214=CONTEXT_DEPENDENT_SHAPE_REPRESENTATION(#135,#97566);
#215=CONTEXT_DEPENDENT_SHAPE_REPRESENTATION(#136,#97567);
#216=CONTEXT_DEPENDENT_SHAPE_REPRESENTATION(#137,#97568);
#217=CONTEXT_DEPENDENT_SHAPE_REPRESENTATION(#138,#97569);
#218=CONTEXT_DEPENDENT_SHAPE_REPRESENTATION(#139,#97570);
#219=CONTEXT_DEPENDENT_SHAPE_REPRESENTATION(#140,#97571);
#220=CONTEXT_DEPENDENT_SHAPE_REPRESENTATION(#141,#97572);
#221=CONTEXT_DEPENDENT_SHAPE_REPRESENTATION(#142,#97573);
#222=CONTEXT_DEPENDENT_SHAPE_REPRESENTATION(#143,#97574);
#223=CONTEXT_DEPENDENT_SHAPE_REPRESENTATION(#144,#97575);
#224=CONTEXT_DEPENDENT_SHAPE_REPRESENTATION(#145,#97576);
#225=CONTEXT_DEPENDENT_SHAPE_REPRESENTATION(#146,#97577);
#226=CONTEXT_DEPENDENT_SHAPE_REPRESENTATION(#147,#97578);
#227=CONTEXT_DEPENDENT_SHAPE_REPRESENTATION(#148,#97579);
#228=CONTEXT_DEPENDENT_SHAPE_REPRESENTATION(#149,#97580);
#229=CONTEXT_DEPENDENT_SHAPE_REPRESENTATION(#150,#97581);
#230=CONTEXT_DEPENDENT_SHAPE_REPRESENTATION(#151,#97582);
#231=CONTEXT_DEPENDENT_SHAPE_REPRESENTATION(#152,#97583);
#232=CONTEXT_DEPENDENT_SHAPE_REPRESENTATION(#153,#97584);
#233=CONTEXT_DEPENDENT_SHAPE_REPRESENTATION(#154,#97585);
#234=CONTEXT_DEPENDENT_SHAPE_REPRESENTATION(#155,#97586);
#235=CONTEXT_DEPENDENT_SHAPE_REPRESENTATION(#156,#97587);
#236=CONTEXT_DEPENDENT_SHAPE_REPRESENTATION(#157,#97588);
#237=CONTEXT_DEPENDENT_SHAPE_REPRESENTATION(#158,#97589);
#238=CONTEXT_DEPENDENT_SHAPE_REPRESENTATION(#159,#97590);
#239=CONTEXT_DEPENDENT_SHAPE_REPRESENTATION(#160,#97591);
#240=CONTEXT_DEPENDENT_SHAPE_REPRESENTATION(#161,#97592);
#241=CONTEXT_DEPENDENT_SHAPE_REPRESENTATION(#162,#97593);
#242=CONTEXT_DEPENDENT_SHAPE_REPRESENTATION(#163,#97594);
#243=CONTEXT_DEPENDENT_SHAPE_REPRESENTATION(#164,#97595);
#244=CONTEXT_DEPENDENT_SHAPE_REPRESENTATION(#165,#97596);
#245=CONTEXT_DEPENDENT_SHAPE_REPRESENTATION(#166,#97597);
#246=CONTEXT_DEPENDENT_SHAPE_REPRESENTATION(#167,#97598);
#247=CONTEXT_DEPENDENT_SHAPE_REPRESENTATION(#168,#97599);
#248=CONTEXT_DEPENDENT_SHAPE_REPRESENTATION(#169,#97600);
#249=CONTEXT_DEPENDENT_SHAPE_REPRESENTATION(#170,#97601);
#250=CONTEXT_DEPENDENT_SHAPE_REPRESENTATION(#171,#97602);
#251=NEXT_ASSEMBLY_USAGE_OCCURRENCE('Longitudinal rail:1',
'Longitudinal rail:1','Longitudinal rail:1',#97627,#97628,
'Longitudinal rail:1');
#252=NEXT_ASSEMBLY_USAGE_OCCURRENCE('Transverse rail:1',
'Transverse rail:1','Transverse rail:1',#97627,#97629,
'Transverse rail:1');
#253=NEXT_ASSEMBLY_USAGE_OCCURRENCE('Corner plate:1','Corner plate:1',
'Corner plate:1',#97627,#97630,'Corner plate:1');
#254=NEXT_ASSEMBLY_USAGE_OCCURRENCE('Socket head cap screw M8x25:1',
'Socket head cap screw M8x25:1','Socket head cap screw M8x25:1',#97627,
#97631,'Socket head cap screw M8x25:1');
#255=NEXT_ASSEMBLY_USAGE_OCCURRENCE('Flat washer M8:1',
'Flat washer M8:1','Flat washer M8:1',#97627,#97632,'Flat washer M8:1');
#256=NEXT_ASSEMBLY_USAGE_OCCURRENCE('Longitudinal rail:2',
'Longitudinal rail:2','Longitudinal rail:2',#97627,#97628,
'Longitudinal rail:2');
#257=NEXT_ASSEMBLY_USAGE_OCCURRENCE('Transverse rail:2',
'Transverse rail:2','Transverse rail:2',#97627,#97629,
'Transverse rail:2');
#258=NEXT_ASSEMBLY_USAGE_OCCURRENCE('Corner plate:2','Corner plate:2',
'Corner plate:2',#97627,#97630,'Corner plate:2');
#259=NEXT_ASSEMBLY_USAGE_OCCURRENCE('Corner plate:3','Corner plate:3',
'Corner plate:3',#97627,#97630,'Corner plate:3');
#260=NEXT_ASSEMBLY_USAGE_OCCURRENCE('Corner plate:4','Corner plate:4',
'Corner plate:4',#97627,#97630,'Corner plate:4');
#261=NEXT_ASSEMBLY_USAGE_OCCURRENCE('Socket head cap screw M8x25:2',
'Socket head cap screw M8x25:2','Socket head cap screw M8x25:2',#97627,
#97631,'Socket head cap screw M8x25:2');
#262=NEXT_ASSEMBLY_USAGE_OCCURRENCE('Flat washer M8:2',
'Flat washer M8:2','Flat washer M8:2',#97627,#97632,'Flat washer M8:2');
#263=NEXT_ASSEMBLY_USAGE_OCCURRENCE('Socket head cap screw M8x25:3',
'Socket head cap screw M8x25:3','Socket head cap screw M8x25:3',#97627,
#97631,'Socket head cap screw M8x25:3');
#264=NEXT_ASSEMBLY_USAGE_OCCURRENCE('Flat washer M8:3',
'Flat washer M8:3','Flat washer M8:3',#97627,#97632,'Flat washer M8:3');
#265=NEXT_ASSEMBLY_USAGE_OCCURRENCE('Socket head cap screw M8x25:4',
'Socket head cap screw M8x25:4','Socket head cap screw M8x25:4',#97627,
#97631,'Socket head cap screw M8x25:4');
#266=NEXT_ASSEMBLY_USAGE_OCCURRENCE('Flat washer M8:4',
'Flat washer M8:4','Flat washer M8:4',#97627,#97632,'Flat washer M8:4');
#267=NEXT_ASSEMBLY_USAGE_OCCURRENCE('Socket head cap screw M8x25:5',
'Socket head cap screw M8x25:5','Socket head cap screw M8x25:5',#97627,
#97631,'Socket head cap screw M8x25:5');
#268=NEXT_ASSEMBLY_USAGE_OCCURRENCE('Flat washer M8:5',
'Flat washer M8:5','Flat washer M8:5',#97627,#97632,'Flat washer M8:5');
#269=NEXT_ASSEMBLY_USAGE_OCCURRENCE('Socket head cap screw M8x25:6',
'Socket head cap screw M8x25:6','Socket head cap screw M8x25:6',#97627,
#97631,'Socket head cap screw M8x25:6');
#270=NEXT_ASSEMBLY_USAGE_OCCURRENCE('Flat washer M8:6',
'Flat washer M8:6','Flat washer M8:6',#97627,#97632,'Flat washer M8:6');
#271=NEXT_ASSEMBLY_USAGE_OCCURRENCE('Socket head cap screw M8x25:7',
'Socket head cap screw M8x25:7','Socket head cap screw M8x25:7',#97627,
#97631,'Socket head cap screw M8x25:7');
#272=NEXT_ASSEMBLY_USAGE_OCCURRENCE('Flat washer M8:7',
'Flat washer M8:7','Flat washer M8:7',#97627,#97632,'Flat washer M8:7');
#273=NEXT_ASSEMBLY_USAGE_OCCURRENCE('Socket head cap screw M8x25:8',
'Socket head cap screw M8x25:8','Socket head cap screw M8x25:8',#97627,
#97631,'Socket head cap screw M8x25:8');
#274=NEXT_ASSEMBLY_USAGE_OCCURRENCE('Flat washer M8:8',
'Flat washer M8:8','Flat washer M8:8',#97627,#97632,'Flat washer M8:8');
#275=NEXT_ASSEMBLY_USAGE_OCCURRENCE('Socket head cap screw M8x25:9',
'Socket head cap screw M8x25:9','Socket head cap screw M8x25:9',#97627,
#97631,'Socket head cap screw M8x25:9');
#276=NEXT_ASSEMBLY_USAGE_OCCURRENCE('Flat washer M8:9',
'Flat washer M8:9','Flat washer M8:9',#97627,#97632,'Flat washer M8:9');
#277=NEXT_ASSEMBLY_USAGE_OCCURRENCE('Socket head cap screw M8x25:10',
'Socket head cap screw M8x25:10','Socket head cap screw M8x25:10',#97627,
#97631,'Socket head cap screw M8x25:10');
#278=NEXT_ASSEMBLY_USAGE_OCCURRENCE('Flat washer M8:10',
'Flat washer M8:10','Flat washer M8:10',#97627,#97632,
'Flat washer M8:10');
#279=NEXT_ASSEMBLY_USAGE_OCCURRENCE('Socket head cap screw M8x25:11',
'Socket head cap screw M8x25:11','Socket head cap screw M8x25:11',#97627,
#97631,'Socket head cap screw M8x25:11');
#280=NEXT_ASSEMBLY_USAGE_OCCURRENCE('Flat washer M8:11',
'Flat washer M8:11','Flat washer M8:11',#97627,#97632,
'Flat washer M8:11');
#281=NEXT_ASSEMBLY_USAGE_OCCURRENCE('Socket head cap screw M8x25:12',
'Socket head cap screw M8x25:12','Socket head cap screw M8x25:12',#97627,
#97631,'Socket head cap screw M8x25:12');
#282=NEXT_ASSEMBLY_USAGE_OCCURRENCE('Flat washer M8:12',
'Flat washer M8:12','Flat washer M8:12',#97627,#97632,
'Flat washer M8:12');
#283=NEXT_ASSEMBLY_USAGE_OCCURRENCE('Socket head cap screw M8x25:13',
'Socket head cap screw M8x25:13','Socket head cap screw M8x25:13',#97627,
#97631,'Socket head cap screw M8x25:13');
#284=NEXT_ASSEMBLY_USAGE_OCCURRENCE('Flat washer M8:13',
'Flat washer M8:13','Flat washer M8:13',#97627,#97632,
'Flat washer M8:13');
#285=NEXT_ASSEMBLY_USAGE_OCCURRENCE('Socket head cap screw M8x25:14',
'Socket head cap screw M8x25:14','Socket head cap screw M8x25:14',#97627,
#97631,'Socket head cap screw M8x25:14');
#286=NEXT_ASSEMBLY_USAGE_OCCURRENCE('Flat washer M8:14',
'Flat washer M8:14','Flat washer M8:14',#97627,#97632,
'Flat washer M8:14');
#287=NEXT_ASSEMBLY_USAGE_OCCURRENCE('Socket head cap screw M8x25:15',
'Socket head cap screw M8x25:15','Socket head cap screw M8x25:15',#97627,
#97631,'Socket head cap screw M8x25:15');
#288=NEXT_ASSEMBLY_USAGE_OCCURRENCE('Flat washer M8:15',
'Flat washer M8:15','Flat washer M8:15',#97627,#97632,
'Flat washer M8:15');
#289=NEXT_ASSEMBLY_USAGE_OCCURRENCE('Socket head cap screw M8x25:16',
'Socket head cap screw M8x25:16','Socket head cap screw M8x25:16',#97627,
#97631,'Socket head cap screw M8x25:16');
#290=NEXT_ASSEMBLY_USAGE_OCCURRENCE('Flat washer M8:16',
'Flat washer M8:16','Flat washer M8:16',#97627,#97632,
'Flat washer M8:16');
#291=NEXT_ASSEMBLY_USAGE_OCCURRENCE('Leg post:1','Leg post:1',
'Leg post:1',#97633,#97634,'Leg post:1');
#292=NEXT_ASSEMBLY_USAGE_OCCURRENCE('Mounting plate:1',
'Mounting plate:1','Mounting plate:1',#97633,#97635,'Mounting plate:1');
#293=NEXT_ASSEMBLY_USAGE_OCCURRENCE('Socket head cap screw M10x20:1',
'Socket head cap screw M10x20:1','Socket head cap screw M10x20:1',#97633,
#97636,'Socket head cap screw M10x20:1');
#294=NEXT_ASSEMBLY_USAGE_OCCURRENCE('Grip sole:1','Grip sole:1',
'Grip sole:1',#97633,#97637,'Grip sole:1');
#295=NEXT_ASSEMBLY_USAGE_OCCURRENCE('Swivel pad:1','Swivel pad:1',
'Swivel pad:1',#97633,#97638,'Swivel pad:1');
#296=NEXT_ASSEMBLY_USAGE_OCCURRENCE('Ball retainer:1','Ball retainer:1',
'Ball retainer:1',#97633,#97639,'Ball retainer:1');
#297=NEXT_ASSEMBLY_USAGE_OCCURRENCE('Adjusting spindle:1',
'Adjusting spindle:1','Adjusting spindle:1',#97633,#97640,
'Adjusting spindle:1');
#298=NEXT_ASSEMBLY_USAGE_OCCURRENCE('Lock nut M10:1','Lock nut M10:1',
'Lock nut M10:1',#97633,#97641,'Lock nut M10:1');
#299=NEXT_ASSEMBLY_USAGE_OCCURRENCE('Flat washer M10:1',
'Flat washer M10:1','Flat washer M10:1',#97633,#97642,
'Flat washer M10:1');
#300=NEXT_ASSEMBLY_USAGE_OCCURRENCE('Socket head cap screw M6x16:1',
'Socket head cap screw M6x16:1','Socket head cap screw M6x16:1',#97633,
#97643,'Socket head cap screw M6x16:1');
#301=NEXT_ASSEMBLY_USAGE_OCCURRENCE('Flat washer M6:1',
'Flat washer M6:1','Flat washer M6:1',#97633,#97647,'Flat washer M6:1');
#302=NEXT_ASSEMBLY_USAGE_OCCURRENCE('Socket head cap screw M6x16:2',
'Socket head cap screw M6x16:2','Socket head cap screw M6x16:2',#97633,
#97643,'Socket head cap screw M6x16:2');
#303=NEXT_ASSEMBLY_USAGE_OCCURRENCE('Flat washer M6:2',
'Flat washer M6:2','Flat washer M6:2',#97633,#97647,'Flat washer M6:2');
#304=NEXT_ASSEMBLY_USAGE_OCCURRENCE('Socket head cap screw M6x16:3',
'Socket head cap screw M6x16:3','Socket head cap screw M6x16:3',#97633,
#97643,'Socket head cap screw M6x16:3');
#305=NEXT_ASSEMBLY_USAGE_OCCURRENCE('Flat washer M6:3',
'Flat washer M6:3','Flat washer M6:3',#97633,#97647,'Flat washer M6:3');
#306=NEXT_ASSEMBLY_USAGE_OCCURRENCE('Support leg:1','Support leg:1',
'Support leg:1',#97626,#97633,'Support leg:1');
#307=NEXT_ASSEMBLY_USAGE_OCCURRENCE('Connecting frame:1',
'Connecting frame:1','Connecting frame:1',#97626,#97627,
'Connecting frame:1');
#308=NEXT_ASSEMBLY_USAGE_OCCURRENCE('Support leg:2','Support leg:2',
'Support leg:2',#97626,#97633,'Support leg:2');
#309=NEXT_ASSEMBLY_USAGE_OCCURRENCE('Support leg:3','Support leg:3',
'Support leg:3',#97626,#97633,'Support leg:3');
#310=NEXT_ASSEMBLY_USAGE_OCCURRENCE('Support leg:4','Support leg:4',
'Support leg:4',#97626,#97633,'Support leg:4');
#311=NEXT_ASSEMBLY_USAGE_OCCURRENCE('Worktop:1','Worktop:1','Worktop:1',
#97626,#97644,'Worktop:1');
#312=NEXT_ASSEMBLY_USAGE_OCCURRENCE('Socket head cap screw M6x50:1',
'Socket head cap screw M6x50:1','Socket head cap screw M6x50:1',#97626,
#97645,'Socket head cap screw M6x50:1');
#313=NEXT_ASSEMBLY_USAGE_OCCURRENCE('Crush sleeve:1','Crush sleeve:1',
'Crush sleeve:1',#97626,#97646,'Crush sleeve:1');
#314=NEXT_ASSEMBLY_USAGE_OCCURRENCE('Flat washer M6:4',
'Flat washer M6:4','Flat washer M6:4',#97626,#97647,'Flat washer M6:4');
#315=NEXT_ASSEMBLY_USAGE_OCCURRENCE('Socket head cap screw M6x50:2',
'Socket head cap screw M6x50:2','Socket head cap screw M6x50:2',#97626,
#97645,'Socket head cap screw M6x50:2');
#316=NEXT_ASSEMBLY_USAGE_OCCURRENCE('Crush sleeve:2','Crush sleeve:2',
'Crush sleeve:2',#97626,#97646,'Crush sleeve:2');
#317=NEXT_ASSEMBLY_USAGE_OCCURRENCE('Flat washer M6:5',
'Flat washer M6:5','Flat washer M6:5',#97626,#97647,'Flat washer M6:5');
#318=NEXT_ASSEMBLY_USAGE_OCCURRENCE('Socket head cap screw M6x50:3',
'Socket head cap screw M6x50:3','Socket head cap screw M6x50:3',#97626,
#97645,'Socket head cap screw M6x50:3');
#319=NEXT_ASSEMBLY_USAGE_OCCURRENCE('Crush sleeve:3','Crush sleeve:3',
'Crush sleeve:3',#97626,#97646,'Crush sleeve:3');
#320=NEXT_ASSEMBLY_USAGE_OCCURRENCE('Flat washer M6:6',
'Flat washer M6:6','Flat washer M6:6',#97626,#97647,'Flat washer M6:6');
#321=NEXT_ASSEMBLY_USAGE_OCCURRENCE('Socket head cap screw M6x50:4',
'Socket head cap screw M6x50:4','Socket head cap screw M6x50:4',#97626,
#97645,'Socket head cap screw M6x50:4');
#322=NEXT_ASSEMBLY_USAGE_OCCURRENCE('Crush sleeve:4','Crush sleeve:4',
'Crush sleeve:4',#97626,#97646,'Crush sleeve:4');
#323=NEXT_ASSEMBLY_USAGE_OCCURRENCE('Flat washer M6:7',
'Flat washer M6:7','Flat washer M6:7',#97626,#97647,'Flat washer M6:7');
#324=NEXT_ASSEMBLY_USAGE_OCCURRENCE('Socket head cap screw M6x50:5',
'Socket head cap screw M6x50:5','Socket head cap screw M6x50:5',#97626,
#97645,'Socket head cap screw M6x50:5');
#325=NEXT_ASSEMBLY_USAGE_OCCURRENCE('Crush sleeve:5','Crush sleeve:5',
'Crush sleeve:5',#97626,#97646,'Crush sleeve:5');
#326=NEXT_ASSEMBLY_USAGE_OCCURRENCE('Flat washer M6:8',
'Flat washer M6:8','Flat washer M6:8',#97626,#97647,'Flat washer M6:8');
#327=NEXT_ASSEMBLY_USAGE_OCCURRENCE('Socket head cap screw M6x50:6',
'Socket head cap screw M6x50:6','Socket head cap screw M6x50:6',#97626,
#97645,'Socket head cap screw M6x50:6');
#328=NEXT_ASSEMBLY_USAGE_OCCURRENCE('Crush sleeve:6','Crush sleeve:6',
'Crush sleeve:6',#97626,#97646,'Crush sleeve:6');
#329=NEXT_ASSEMBLY_USAGE_OCCURRENCE('Flat washer M6:9',
'Flat washer M6:9','Flat washer M6:9',#97626,#97647,'Flat washer M6:9');
#330=CONICAL_SURFACE('',#22228,3.5,0.785398163397448);
#331=CONICAL_SURFACE('',#22676,4.5,0.785398163397448);
#332=CONICAL_SURFACE('',#23023,2.5,0.785398163397448);
#333=CONICAL_SURFACE('',#23426,2.5,0.78539816339745);
#334=B_SPLINE_SURFACE_WITH_KNOTS('',3,3,((#29999,#30000,#30001,#30002,#30003,
#30004,#30005,#30006,#30007,#30008,#30009,#30010,#30011,#30012,#30013,#30014,
#30015,#30016,#30017,#30018,#30019,#30020,#30021,#30022,#30023,#30024,#30025,
#30026,#30027,#30028,#30029,#30030,#30031,#30032,#30033,#30034,#30035,#30036,
#30037,#30038,#30039,#30040,#30041,#30042,#30043,#30044,#30045,#30046,#30047,
#30048,#30049,#30050,#30051,#30052,#30053,#30054),(#30055,#30056,#30057,
#30058,#30059,#30060,#30061,#30062,#30063,#30064,#30065,#30066,#30067,#30068,
#30069,#30070,#30071,#30072,#30073,#30074,#30075,#30076,#30077,#30078,#30079,
#30080,#30081,#30082,#30083,#30084,#30085,#30086,#30087,#30088,#30089,#30090,
#30091,#30092,#30093,#30094,#30095,#30096,#30097,#30098,#30099,#30100,#30101,
#30102,#30103,#30104,#30105,#30106,#30107,#30108,#30109,#30110),(#30111,
#30112,#30113,#30114,#30115,#30116,#30117,#30118,#30119,#30120,#30121,#30122,
#30123,#30124,#30125,#30126,#30127,#30128,#30129,#30130,#30131,#30132,#30133,
#30134,#30135,#30136,#30137,#30138,#30139,#30140,#30141,#30142,#30143,#30144,
#30145,#30146,#30147,#30148,#30149,#30150,#30151,#30152,#30153,#30154,#30155,
#30156,#30157,#30158,#30159,#30160,#30161,#30162,#30163,#30164,#30165,#30166),
(#30167,#30168,#30169,#30170,#30171,#30172,#30173,#30174,#30175,#30176,
#30177,#30178,#30179,#30180,#30181,#30182,#30183,#30184,#30185,#30186,#30187,
#30188,#30189,#30190,#30191,#30192,#30193,#30194,#30195,#30196,#30197,#30198,
#30199,#30200,#30201,#30202,#30203,#30204,#30205,#30206,#30207,#30208,#30209,
#30210,#30211,#30212,#30213,#30214,#30215,#30216,#30217,#30218,#30219,#30220,
#30221,#30222)),.UNSPECIFIED.,.F.,.F.,.F.,(4,4),(4,1,1,1,1,1,1,1,1,1,1,
1,1,1,1,1,1,1,1,1,1,1,1,1,1,1,1,1,1,1,1,1,1,1,1,1,1,1,1,1,1,1,1,1,1,1,1,
1,1,1,1,1,1,4),(0.,0.0642013499338865),(11.8589888623078,12.8454497557128,
13.8319106491178,14.8183715425228,15.8048324359278,16.7912933293328,17.7777542227378,
18.7642151161428,19.7506760095478,20.7371369029528,21.7235977963578,22.7100586897628,
23.6965195831678,24.6829804765728,25.6694413699778,26.6559022633828,27.6423631567878,
28.6288240501928,29.6152849435978,30.6017458370028,31.5882067304078,32.5746676238129,
33.5611285172179,34.5475894106229,35.5340503040279,36.5205111974329,37.5069720908379,
38.4934329842429,39.4798938776479,40.4663547710529,41.4528156644579,42.4392765578629,
43.4257374512679,44.4121983446729,45.3986592380779,46.3851201314829,47.3715810248879,
48.3580419182929,49.3445028116979,50.3309637051029,51.3174245985079,52.3038854919129,
53.2903463853179,54.2768072787229,55.2632681721279,56.2497290655329,57.2361899589379,
58.2226508523429,59.2091117457479,60.1955726391529,61.1820335325579,62.1684944259629,
63.1549553193679,64.1414162127729),.UNSPECIFIED.);
#335=B_SPLINE_SURFACE_WITH_KNOTS('',3,3,((#30439,#30440,#30441,#30442,#30443,
#30444,#30445,#30446,#30447,#30448,#30449,#30450,#30451,#30452,#30453,#30454,
#30455,#30456,#30457,#30458,#30459,#30460,#30461,#30462,#30463,#30464,#30465,
#30466,#30467,#30468,#30469,#30470,#30471,#30472,#30473,#30474,#30475,#30476,
#30477,#30478,#30479,#30480,#30481,#30482,#30483,#30484,#30485,#30486,#30487,
#30488,#30489,#30490,#30491,#30492,#30493,#30494),(#30495,#30496,#30497,
#30498,#30499,#30500,#30501,#30502,#30503,#30504,#30505,#30506,#30507,#30508,
#30509,#30510,#30511,#30512,#30513,#30514,#30515,#30516,#30517,#30518,#30519,
#30520,#30521,#30522,#30523,#30524,#30525,#30526,#30527,#30528,#30529,#30530,
#30531,#30532,#30533,#30534,#30535,#30536,#30537,#30538,#30539,#30540,#30541,
#30542,#30543,#30544,#30545,#30546,#30547,#30548,#30549,#30550),(#30551,
#30552,#30553,#30554,#30555,#30556,#30557,#30558,#30559,#30560,#30561,#30562,
#30563,#30564,#30565,#30566,#30567,#30568,#30569,#30570,#30571,#30572,#30573,
#30574,#30575,#30576,#30577,#30578,#30579,#30580,#30581,#30582,#30583,#30584,
#30585,#30586,#30587,#30588,#30589,#30590,#30591,#30592,#30593,#30594,#30595,
#30596,#30597,#30598,#30599,#30600,#30601,#30602,#30603,#30604,#30605,#30606),
(#30607,#30608,#30609,#30610,#30611,#30612,#30613,#30614,#30615,#30616,
#30617,#30618,#30619,#30620,#30621,#30622,#30623,#30624,#30625,#30626,#30627,
#30628,#30629,#30630,#30631,#30632,#30633,#30634,#30635,#30636,#30637,#30638,
#30639,#30640,#30641,#30642,#30643,#30644,#30645,#30646,#30647,#30648,#30649,
#30650,#30651,#30652,#30653,#30654,#30655,#30656,#30657,#30658,#30659,#30660,
#30661,#30662)),.UNSPECIFIED.,.F.,.F.,.F.,(4,4),(4,1,1,1,1,1,1,1,1,1,1,
1,1,1,1,1,1,1,1,1,1,1,1,1,1,1,1,1,1,1,1,1,1,1,1,1,1,1,1,1,1,1,1,1,1,1,1,
1,1,1,1,1,1,4),(0.,0.0642013499338865),(14.3984001269718,15.3848610203768,
16.3713219137818,17.3577828071868,18.3442437005918,19.3307045939968,20.3171654874019,
21.3036263808069,22.2900872742119,23.2765481676169,24.2630090610219,25.2494699544269,
26.2359308478319,27.2223917412369,28.2088526346419,29.1953135280469,30.1817744214519,
31.1682353148569,32.1546962082619,33.1411571016669,34.1276179950719,35.1140788884769,
36.1005397818819,37.0870006752869,38.0734615686919,39.0599224620969,40.0463833555019,
41.0328442489069,42.0193051423119,43.0057660357169,43.9922269291219,44.9786878225269,
45.9651487159319,46.9516096093369,47.9380705027419,48.9245313961469,49.9109922895519,
50.8974531829569,51.8839140763619,52.8703749697669,53.856835863172,54.843296756577,
55.829757649982,56.816218543387,57.802679436792,58.789140330197,59.775601223602,
60.762062117007,61.748523010412,62.734983903817,63.721444797222,64.707905690627,
65.694366584032,66.680827477437),.UNSPECIFIED.);
#336=B_SPLINE_SURFACE_WITH_KNOTS('',3,3,((#31483,#31484,#31485,#31486,#31487,
#31488,#31489,#31490,#31491,#31492,#31493,#31494,#31495,#31496,#31497,#31498,
#31499,#31500,#31501,#31502,#31503,#31504,#31505,#31506,#31507,#31508,#31509,
#31510,#31511,#31512,#31513,#31514,#31515,#31516,#31517,#31518,#31519,#31520,
#31521,#31522,#31523,#31524,#31525,#31526,#31527,#31528,#31529,#31530,#31531,
#31532,#31533,#31534,#31535,#31536,#31537,#31538),(#31539,#31540,#31541,
#31542,#31543,#31544,#31545,#31546,#31547,#31548,#31549,#31550,#31551,#31552,
#31553,#31554,#31555,#31556,#31557,#31558,#31559,#31560,#31561,#31562,#31563,
#31564,#31565,#31566,#31567,#31568,#31569,#31570,#31571,#31572,#31573,#31574,
#31575,#31576,#31577,#31578,#31579,#31580,#31581,#31582,#31583,#31584,#31585,
#31586,#31587,#31588,#31589,#31590,#31591,#31592,#31593,#31594),(#31595,
#31596,#31597,#31598,#31599,#31600,#31601,#31602,#31603,#31604,#31605,#31606,
#31607,#31608,#31609,#31610,#31611,#31612,#31613,#31614,#31615,#31616,#31617,
#31618,#31619,#31620,#31621,#31622,#31623,#31624,#31625,#31626,#31627,#31628,
#31629,#31630,#31631,#31632,#31633,#31634,#31635,#31636,#31637,#31638,#31639,
#31640,#31641,#31642,#31643,#31644,#31645,#31646,#31647,#31648,#31649,#31650),
(#31651,#31652,#31653,#31654,#31655,#31656,#31657,#31658,#31659,#31660,
#31661,#31662,#31663,#31664,#31665,#31666,#31667,#31668,#31669,#31670,#31671,
#31672,#31673,#31674,#31675,#31676,#31677,#31678,#31679,#31680,#31681,#31682,
#31683,#31684,#31685,#31686,#31687,#31688,#31689,#31690,#31691,#31692,#31693,
#31694,#31695,#31696,#31697,#31698,#31699,#31700,#31701,#31702,#31703,#31704,
#31705,#31706)),.UNSPECIFIED.,.F.,.F.,.F.,(4,4),(4,1,1,1,1,1,1,1,1,1,1,
1,1,1,1,1,1,1,1,1,1,1,1,1,1,1,1,1,1,1,1,1,1,1,1,1,1,1,1,1,1,1,1,1,1,1,1,
1,1,1,1,1,1,4),(0.,0.0642013499338865),(11.8589888623078,12.8454497557128,
13.8319106491178,14.8183715425228,15.8048324359278,16.7912933293328,17.7777542227378,
18.7642151161428,19.7506760095478,20.7371369029528,21.7235977963578,22.7100586897628,
23.6965195831678,24.6829804765728,25.6694413699778,26.6559022633828,27.6423631567879,
28.6288240501929,29.6152849435979,30.6017458370029,31.5882067304079,32.5746676238129,
33.5611285172179,34.5475894106229,35.5340503040279,36.5205111974329,37.5069720908379,
38.4934329842429,39.4798938776479,40.4663547710529,41.4528156644579,42.4392765578629,
43.4257374512679,44.4121983446729,45.3986592380779,46.3851201314829,47.3715810248879,
48.3580419182929,49.3445028116979,50.3309637051029,51.3174245985079,52.3038854919129,
53.2903463853179,54.2768072787229,55.2632681721279,56.2497290655329,57.2361899589379,
58.2226508523429,59.2091117457479,60.1955726391529,61.1820335325579,62.1684944259629,
63.154955319368,64.141416212773),.UNSPECIFIED.);
#337=B_SPLINE_SURFACE_WITH_KNOTS('',3,3,((#31829,#31830,#31831,#31832,#31833,
#31834,#31835,#31836,#31837,#31838,#31839,#31840,#31841,#31842,#31843,#31844,
#31845,#31846,#31847,#31848,#31849,#31850,#31851,#31852,#31853,#31854,#31855,
#31856,#31857,#31858,#31859,#31860,#31861,#31862,#31863,#31864,#31865,#31866,
#31867,#31868,#31869,#31870,#31871,#31872,#31873,#31874,#31875,#31876,#31877,
#31878,#31879,#31880,#31881,#31882,#31883,#31884),(#31885,#31886,#31887,
#31888,#31889,#31890,#31891,#31892,#31893,#31894,#31895,#31896,#31897,#31898,
#31899,#31900,#31901,#31902,#31903,#31904,#31905,#31906,#31907,#31908,#31909,
#31910,#31911,#31912,#31913,#31914,#31915,#31916,#31917,#31918,#31919,#31920,
#31921,#31922,#31923,#31924,#31925,#31926,#31927,#31928,#31929,#31930,#31931,
#31932,#31933,#31934,#31935,#31936,#31937,#31938,#31939,#31940),(#31941,
#31942,#31943,#31944,#31945,#31946,#31947,#31948,#31949,#31950,#31951,#31952,
#31953,#31954,#31955,#31956,#31957,#31958,#31959,#31960,#31961,#31962,#31963,
#31964,#31965,#31966,#31967,#31968,#31969,#31970,#31971,#31972,#31973,#31974,
#31975,#31976,#31977,#31978,#31979,#31980,#31981,#31982,#31983,#31984,#31985,
#31986,#31987,#31988,#31989,#31990,#31991,#31992,#31993,#31994,#31995,#31996),
(#31997,#31998,#31999,#32000,#32001,#32002,#32003,#32004,#32005,#32006,
#32007,#32008,#32009,#32010,#32011,#32012,#32013,#32014,#32015,#32016,#32017,
#32018,#32019,#32020,#32021,#32022,#32023,#32024,#32025,#32026,#32027,#32028,
#32029,#32030,#32031,#32032,#32033,#32034,#32035,#32036,#32037,#32038,#32039,
#32040,#32041,#32042,#32043,#32044,#32045,#32046,#32047,#32048,#32049,#32050,
#32051,#32052)),.UNSPECIFIED.,.F.,.F.,.F.,(4,4),(4,1,1,1,1,1,1,1,1,1,1,
1,1,1,1,1,1,1,1,1,1,1,1,1,1,1,1,1,1,1,1,1,1,1,1,1,1,1,1,1,1,1,1,1,1,1,1,
1,1,1,1,1,1,4),(0.,0.0642013499338865),(14.3984001269718,15.3848610203768,
16.3713219137818,17.3577828071869,18.3442437005919,19.3307045939969,20.3171654874019,
21.3036263808069,22.2900872742119,23.2765481676169,24.2630090610219,25.2494699544269,
26.2359308478319,27.2223917412369,28.2088526346419,29.1953135280469,30.1817744214519,
31.1682353148569,32.1546962082619,33.1411571016669,34.1276179950719,35.1140788884769,
36.1005397818819,37.0870006752869,38.0734615686919,39.0599224620969,40.0463833555019,
41.0328442489069,42.0193051423119,43.0057660357169,43.9922269291219,44.9786878225269,
45.9651487159319,46.9516096093369,47.9380705027419,48.9245313961469,49.9109922895519,
50.8974531829569,51.8839140763619,52.8703749697669,53.856835863172,54.843296756577,
55.829757649982,56.816218543387,57.802679436792,58.789140330197,59.775601223602,
60.762062117007,61.748523010412,62.734983903817,63.721444797222,64.707905690627,
65.694366584032,66.680827477437),.UNSPECIFIED.);
#338=B_SPLINE_SURFACE_WITH_KNOTS('',3,3,((#32194,#32195,#32196,#32197,#32198,
#32199,#32200,#32201,#32202,#32203,#32204,#32205,#32206,#32207,#32208,#32209,
#32210,#32211,#32212,#32213,#32214,#32215,#32216,#32217,#32218,#32219,#32220,
#32221,#32222,#32223,#32224,#32225,#32226,#32227,#32228,#32229,#32230,#32231,
#32232,#32233,#32234,#32235,#32236,#32237,#32238,#32239,#32240,#32241,#32242,
#32243,#32244,#32245,#32246,#32247,#32248,#32249),(#32250,#32251,#32252,
#32253,#32254,#32255,#32256,#32257,#32258,#32259,#32260,#32261,#32262,#32263,
#32264,#32265,#32266,#32267,#32268,#32269,#32270,#32271,#32272,#32273,#32274,
#32275,#32276,#32277,#32278,#32279,#32280,#32281,#32282,#32283,#32284,#32285,
#32286,#32287,#32288,#32289,#32290,#32291,#32292,#32293,#32294,#32295,#32296,
#32297,#32298,#32299,#32300,#32301,#32302,#32303,#32304,#32305),(#32306,
#32307,#32308,#32309,#32310,#32311,#32312,#32313,#32314,#32315,#32316,#32317,
#32318,#32319,#32320,#32321,#32322,#32323,#32324,#32325,#32326,#32327,#32328,
#32329,#32330,#32331,#32332,#32333,#32334,#32335,#32336,#32337,#32338,#32339,
#32340,#32341,#32342,#32343,#32344,#32345,#32346,#32347,#32348,#32349,#32350,
#32351,#32352,#32353,#32354,#32355,#32356,#32357,#32358,#32359,#32360,#32361),
(#32362,#32363,#32364,#32365,#32366,#32367,#32368,#32369,#32370,#32371,
#32372,#32373,#32374,#32375,#32376,#32377,#32378,#32379,#32380,#32381,#32382,
#32383,#32384,#32385,#32386,#32387,#32388,#32389,#32390,#32391,#32392,#32393,
#32394,#32395,#32396,#32397,#32398,#32399,#32400,#32401,#32402,#32403,#32404,
#32405,#32406,#32407,#32408,#32409,#32410,#32411,#32412,#32413,#32414,#32415,
#32416,#32417)),.UNSPECIFIED.,.F.,.F.,.F.,(4,4),(4,1,1,1,1,1,1,1,1,1,1,
1,1,1,1,1,1,1,1,1,1,1,1,1,1,1,1,1,1,1,1,1,1,1,1,1,1,1,1,1,1,1,1,1,1,1,1,
1,1,1,1,1,1,4),(0.,0.0642013499338865),(11.8589888623078,12.8454497557128,
13.8319106491178,14.8183715425228,15.8048324359278,16.7912933293328,17.7777542227378,
18.7642151161428,19.7506760095478,20.7371369029528,21.7235977963578,22.7100586897628,
23.6965195831678,24.6829804765728,25.6694413699778,26.6559022633828,27.6423631567878,
28.6288240501928,29.6152849435978,30.6017458370028,31.5882067304078,32.5746676238129,
33.5611285172179,34.5475894106229,35.5340503040279,36.5205111974329,37.5069720908379,
38.4934329842429,39.4798938776479,40.4663547710529,41.4528156644579,42.4392765578629,
43.4257374512679,44.4121983446729,45.3986592380779,46.3851201314829,47.3715810248879,
48.3580419182929,49.3445028116979,50.3309637051029,51.3174245985079,52.3038854919129,
53.2903463853179,54.2768072787229,55.2632681721279,56.2497290655329,57.2361899589379,
58.2226508523429,59.2091117457479,60.1955726391529,61.1820335325579,62.1684944259629,
63.1549553193679,64.1414162127729),.UNSPECIFIED.);
#339=B_SPLINE_SURFACE_WITH_KNOTS('',3,3,((#32540,#32541,#32542,#32543,#32544,
#32545,#32546,#32547,#32548,#32549,#32550,#32551,#32552,#32553,#32554,#32555,
#32556,#32557,#32558,#32559,#32560,#32561,#32562,#32563,#32564,#32565,#32566,
#32567,#32568,#32569,#32570,#32571,#32572,#32573,#32574,#32575,#32576,#32577,
#32578,#32579,#32580,#32581,#32582,#32583,#32584,#32585,#32586,#32587,#32588,
#32589,#32590,#32591,#32592,#32593,#32594,#32595),(#32596,#32597,#32598,
#32599,#32600,#32601,#32602,#32603,#32604,#32605,#32606,#32607,#32608,#32609,
#32610,#32611,#32612,#32613,#32614,#32615,#32616,#32617,#32618,#32619,#32620,
#32621,#32622,#32623,#32624,#32625,#32626,#32627,#32628,#32629,#32630,#32631,
#32632,#32633,#32634,#32635,#32636,#32637,#32638,#32639,#32640,#32641,#32642,
#32643,#32644,#32645,#32646,#32647,#32648,#32649,#32650,#32651),(#32652,
#32653,#32654,#32655,#32656,#32657,#32658,#32659,#32660,#32661,#32662,#32663,
#32664,#32665,#32666,#32667,#32668,#32669,#32670,#32671,#32672,#32673,#32674,
#32675,#32676,#32677,#32678,#32679,#32680,#32681,#32682,#32683,#32684,#32685,
#32686,#32687,#32688,#32689,#32690,#32691,#32692,#32693,#32694,#32695,#32696,
#32697,#32698,#32699,#32700,#32701,#32702,#32703,#32704,#32705,#32706,#32707),
(#32708,#32709,#32710,#32711,#32712,#32713,#32714,#32715,#32716,#32717,
#32718,#32719,#32720,#32721,#32722,#32723,#32724,#32725,#32726,#32727,#32728,
#32729,#32730,#32731,#32732,#32733,#32734,#32735,#32736,#32737,#32738,#32739,
#32740,#32741,#32742,#32743,#32744,#32745,#32746,#32747,#32748,#32749,#32750,
#32751,#32752,#32753,#32754,#32755,#32756,#32757,#32758,#32759,#32760,#32761,
#32762,#32763)),.UNSPECIFIED.,.F.,.F.,.F.,(4,4),(4,1,1,1,1,1,1,1,1,1,1,
1,1,1,1,1,1,1,1,1,1,1,1,1,1,1,1,1,1,1,1,1,1,1,1,1,1,1,1,1,1,1,1,1,1,1,1,
1,1,1,1,1,1,4),(0.,0.0642013499338865),(14.3984001269718,15.3848610203768,
16.3713219137818,17.3577828071868,18.3442437005918,19.3307045939968,20.3171654874019,
21.3036263808069,22.2900872742119,23.2765481676169,24.2630090610219,25.2494699544269,
26.2359308478319,27.2223917412369,28.2088526346419,29.1953135280469,30.1817744214519,
31.1682353148569,32.1546962082619,33.1411571016669,34.1276179950719,35.1140788884769,
36.1005397818819,37.0870006752869,38.0734615686919,39.0599224620969,40.0463833555019,
41.0328442489069,42.0193051423119,43.0057660357169,43.9922269291219,44.9786878225269,
45.9651487159319,46.9516096093369,47.9380705027419,48.9245313961469,49.9109922895519,
50.8974531829569,51.8839140763619,52.8703749697669,53.856835863172,54.843296756577,
55.829757649982,56.816218543387,57.802679436792,58.789140330197,59.775601223602,
60.762062117007,61.748523010412,62.734983903817,63.721444797222,64.707905690627,
65.694366584032,66.680827477437),.UNSPECIFIED.);
#340=B_SPLINE_SURFACE_WITH_KNOTS('',3,3,((#32905,#32906,#32907,#32908,#32909,
#32910,#32911,#32912,#32913,#32914,#32915,#32916,#32917,#32918,#32919,#32920,
#32921,#32922,#32923,#32924,#32925,#32926,#32927,#32928,#32929,#32930,#32931,
#32932,#32933,#32934,#32935,#32936,#32937,#32938,#32939,#32940,#32941,#32942,
#32943,#32944,#32945,#32946,#32947,#32948,#32949,#32950,#32951,#32952,#32953,
#32954,#32955,#32956,#32957,#32958,#32959,#32960),(#32961,#32962,#32963,
#32964,#32965,#32966,#32967,#32968,#32969,#32970,#32971,#32972,#32973,#32974,
#32975,#32976,#32977,#32978,#32979,#32980,#32981,#32982,#32983,#32984,#32985,
#32986,#32987,#32988,#32989,#32990,#32991,#32992,#32993,#32994,#32995,#32996,
#32997,#32998,#32999,#33000,#33001,#33002,#33003,#33004,#33005,#33006,#33007,
#33008,#33009,#33010,#33011,#33012,#33013,#33014,#33015,#33016),(#33017,
#33018,#33019,#33020,#33021,#33022,#33023,#33024,#33025,#33026,#33027,#33028,
#33029,#33030,#33031,#33032,#33033,#33034,#33035,#33036,#33037,#33038,#33039,
#33040,#33041,#33042,#33043,#33044,#33045,#33046,#33047,#33048,#33049,#33050,
#33051,#33052,#33053,#33054,#33055,#33056,#33057,#33058,#33059,#33060,#33061,
#33062,#33063,#33064,#33065,#33066,#33067,#33068,#33069,#33070,#33071,#33072),
(#33073,#33074,#33075,#33076,#33077,#33078,#33079,#33080,#33081,#33082,
#33083,#33084,#33085,#33086,#33087,#33088,#33089,#33090,#33091,#33092,#33093,
#33094,#33095,#33096,#33097,#33098,#33099,#33100,#33101,#33102,#33103,#33104,
#33105,#33106,#33107,#33108,#33109,#33110,#33111,#33112,#33113,#33114,#33115,
#33116,#33117,#33118,#33119,#33120,#33121,#33122,#33123,#33124,#33125,#33126,
#33127,#33128)),.UNSPECIFIED.,.F.,.F.,.F.,(4,4),(4,1,1,1,1,1,1,1,1,1,1,
1,1,1,1,1,1,1,1,1,1,1,1,1,1,1,1,1,1,1,1,1,1,1,1,1,1,1,1,1,1,1,1,1,1,1,1,
1,1,1,1,1,1,4),(0.,0.0642013499338865),(11.8589888623078,12.8454497557128,
13.8319106491178,14.8183715425228,15.8048324359278,16.7912933293328,17.7777542227378,
18.7642151161428,19.7506760095478,20.7371369029528,21.7235977963578,22.7100586897628,
23.6965195831678,24.6829804765728,25.6694413699778,26.6559022633828,27.6423631567879,
28.6288240501929,29.6152849435979,30.6017458370029,31.5882067304079,32.5746676238129,
33.5611285172179,34.5475894106229,35.5340503040279,36.5205111974329,37.5069720908379,
38.4934329842429,39.4798938776479,40.4663547710529,41.4528156644579,42.4392765578629,
43.4257374512679,44.4121983446729,45.3986592380779,46.3851201314829,47.3715810248879,
48.3580419182929,49.3445028116979,50.3309637051029,51.3174245985079,52.3038854919129,
53.2903463853179,54.2768072787229,55.2632681721279,56.2497290655329,57.2361899589379,
58.2226508523429,59.2091117457479,60.1955726391529,61.1820335325579,62.1684944259629,
63.154955319368,64.141416212773),.UNSPECIFIED.);
#341=B_SPLINE_SURFACE_WITH_KNOTS('',3,3,((#33251,#33252,#33253,#33254,#33255,
#33256,#33257,#33258,#33259,#33260,#33261,#33262,#33263,#33264,#33265,#33266,
#33267,#33268,#33269,#33270,#33271,#33272,#33273,#33274,#33275,#33276,#33277,
#33278,#33279,#33280,#33281,#33282,#33283,#33284,#33285,#33286,#33287,#33288,
#33289,#33290,#33291,#33292,#33293,#33294,#33295,#33296,#33297,#33298,#33299,
#33300,#33301,#33302,#33303,#33304,#33305,#33306),(#33307,#33308,#33309,
#33310,#33311,#33312,#33313,#33314,#33315,#33316,#33317,#33318,#33319,#33320,
#33321,#33322,#33323,#33324,#33325,#33326,#33327,#33328,#33329,#33330,#33331,
#33332,#33333,#33334,#33335,#33336,#33337,#33338,#33339,#33340,#33341,#33342,
#33343,#33344,#33345,#33346,#33347,#33348,#33349,#33350,#33351,#33352,#33353,
#33354,#33355,#33356,#33357,#33358,#33359,#33360,#33361,#33362),(#33363,
#33364,#33365,#33366,#33367,#33368,#33369,#33370,#33371,#33372,#33373,#33374,
#33375,#33376,#33377,#33378,#33379,#33380,#33381,#33382,#33383,#33384,#33385,
#33386,#33387,#33388,#33389,#33390,#33391,#33392,#33393,#33394,#33395,#33396,
#33397,#33398,#33399,#33400,#33401,#33402,#33403,#33404,#33405,#33406,#33407,
#33408,#33409,#33410,#33411,#33412,#33413,#33414,#33415,#33416,#33417,#33418),
(#33419,#33420,#33421,#33422,#33423,#33424,#33425,#33426,#33427,#33428,
#33429,#33430,#33431,#33432,#33433,#33434,#33435,#33436,#33437,#33438,#33439,
#33440,#33441,#33442,#33443,#33444,#33445,#33446,#33447,#33448,#33449,#33450,
#33451,#33452,#33453,#33454,#33455,#33456,#33457,#33458,#33459,#33460,#33461,
#33462,#33463,#33464,#33465,#33466,#33467,#33468,#33469,#33470,#33471,#33472,
#33473,#33474)),.UNSPECIFIED.,.F.,.F.,.F.,(4,4),(4,1,1,1,1,1,1,1,1,1,1,
1,1,1,1,1,1,1,1,1,1,1,1,1,1,1,1,1,1,1,1,1,1,1,1,1,1,1,1,1,1,1,1,1,1,1,1,
1,1,1,1,1,1,4),(0.,0.0642013499338865),(14.3984001269718,15.3848610203768,
16.3713219137818,17.3577828071869,18.3442437005919,19.3307045939969,20.3171654874019,
21.3036263808069,22.2900872742119,23.2765481676169,24.2630090610219,25.2494699544269,
26.2359308478319,27.2223917412369,28.2088526346419,29.1953135280469,30.1817744214519,
31.1682353148569,32.1546962082619,33.1411571016669,34.1276179950719,35.1140788884769,
36.1005397818819,37.0870006752869,38.0734615686919,39.0599224620969,40.0463833555019,
41.0328442489069,42.0193051423119,43.0057660357169,43.9922269291219,44.9786878225269,
45.9651487159319,46.9516096093369,47.9380705027419,48.9245313961469,49.9109922895519,
50.8974531829569,51.8839140763619,52.8703749697669,53.856835863172,54.843296756577,
55.829757649982,56.816218543387,57.802679436792,58.789140330197,59.775601223602,
60.762062117007,61.748523010412,62.734983903817,63.721444797222,64.707905690627,
65.694366584032,66.680827477437),.UNSPECIFIED.);
#342=B_SPLINE_SURFACE_WITH_KNOTS('',3,3,((#35708,#35709,#35710,#35711,#35712,
#35713,#35714,#35715,#35716,#35717,#35718,#35719,#35720,#35721,#35722,#35723,
#35724,#35725,#35726,#35727,#35728,#35729,#35730,#35731,#35732,#35733,#35734,
#35735,#35736,#35737,#35738,#35739,#35740,#35741,#35742,#35743,#35744,#35745,
#35746,#35747,#35748,#35749,#35750,#35751,#35752,#35753,#35754,#35755,#35756,
#35757,#35758,#35759,#35760,#35761,#35762,#35763,#35764,#35765,#35766,#35767,
#35768,#35769,#35770,#35771,#35772,#35773,#35774,#35775,#35776,#35777,#35778,
#35779,#35780,#35781,#35782,#35783,#35784,#35785,#35786,#35787,#35788,#35789,
#35790,#35791,#35792,#35793,#35794,#35795,#35796,#35797,#35798,#35799,#35800,
#35801,#35802,#35803,#35804,#35805,#35806,#35807,#35808,#35809,#35810,#35811,
#35812,#35813,#35814,#35815,#35816,#35817,#35818,#35819,#35820,#35821,#35822,
#35823,#35824,#35825,#35826,#35827,#35828,#35829,#35830,#35831,#35832,#35833,
#35834,#35835,#35836,#35837,#35838,#35839,#35840,#35841,#35842,#35843,#35844,
#35845,#35846,#35847,#35848,#35849,#35850,#35851,#35852,#35853,#35854,#35855,
#35856,#35857,#35858,#35859,#35860,#35861,#35862,#35863,#35864,#35865),
(#35866,#35867,#35868,#35869,#35870,#35871,#35872,#35873,#35874,#35875,
#35876,#35877,#35878,#35879,#35880,#35881,#35882,#35883,#35884,#35885,#35886,
#35887,#35888,#35889,#35890,#35891,#35892,#35893,#35894,#35895,#35896,#35897,
#35898,#35899,#35900,#35901,#35902,#35903,#35904,#35905,#35906,#35907,#35908,
#35909,#35910,#35911,#35912,#35913,#35914,#35915,#35916,#35917,#35918,#35919,
#35920,#35921,#35922,#35923,#35924,#35925,#35926,#35927,#35928,#35929,#35930,
#35931,#35932,#35933,#35934,#35935,#35936,#35937,#35938,#35939,#35940,#35941,
#35942,#35943,#35944,#35945,#35946,#35947,#35948,#35949,#35950,#35951,#35952,
#35953,#35954,#35955,#35956,#35957,#35958,#35959,#35960,#35961,#35962,#35963,
#35964,#35965,#35966,#35967,#35968,#35969,#35970,#35971,#35972,#35973,#35974,
#35975,#35976,#35977,#35978,#35979,#35980,#35981,#35982,#35983,#35984,#35985,
#35986,#35987,#35988,#35989,#35990,#35991,#35992,#35993,#35994,#35995,#35996,
#35997,#35998,#35999,#36000,#36001,#36002,#36003,#36004,#36005,#36006,#36007,
#36008,#36009,#36010,#36011,#36012,#36013,#36014,#36015,#36016,#36017,#36018,
#36019,#36020,#36021,#36022,#36023),(#36024,#36025,#36026,#36027,#36028,
#36029,#36030,#36031,#36032,#36033,#36034,#36035,#36036,#36037,#36038,#36039,
#36040,#36041,#36042,#36043,#36044,#36045,#36046,#36047,#36048,#36049,#36050,
#36051,#36052,#36053,#36054,#36055,#36056,#36057,#36058,#36059,#36060,#36061,
#36062,#36063,#36064,#36065,#36066,#36067,#36068,#36069,#36070,#36071,#36072,
#36073,#36074,#36075,#36076,#36077,#36078,#36079,#36080,#36081,#36082,#36083,
#36084,#36085,#36086,#36087,#36088,#36089,#36090,#36091,#36092,#36093,#36094,
#36095,#36096,#36097,#36098,#36099,#36100,#36101,#36102,#36103,#36104,#36105,
#36106,#36107,#36108,#36109,#36110,#36111,#36112,#36113,#36114,#36115,#36116,
#36117,#36118,#36119,#36120,#36121,#36122,#36123,#36124,#36125,#36126,#36127,
#36128,#36129,#36130,#36131,#36132,#36133,#36134,#36135,#36136,#36137,#36138,
#36139,#36140,#36141,#36142,#36143,#36144,#36145,#36146,#36147,#36148,#36149,
#36150,#36151,#36152,#36153,#36154,#36155,#36156,#36157,#36158,#36159,#36160,
#36161,#36162,#36163,#36164,#36165,#36166,#36167,#36168,#36169,#36170,#36171,
#36172,#36173,#36174,#36175,#36176,#36177,#36178,#36179,#36180,#36181),
(#36182,#36183,#36184,#36185,#36186,#36187,#36188,#36189,#36190,#36191,
#36192,#36193,#36194,#36195,#36196,#36197,#36198,#36199,#36200,#36201,#36202,
#36203,#36204,#36205,#36206,#36207,#36208,#36209,#36210,#36211,#36212,#36213,
#36214,#36215,#36216,#36217,#36218,#36219,#36220,#36221,#36222,#36223,#36224,
#36225,#36226,#36227,#36228,#36229,#36230,#36231,#36232,#36233,#36234,#36235,
#36236,#36237,#36238,#36239,#36240,#36241,#36242,#36243,#36244,#36245,#36246,
#36247,#36248,#36249,#36250,#36251,#36252,#36253,#36254,#36255,#36256,#36257,
#36258,#36259,#36260,#36261,#36262,#36263,#36264,#36265,#36266,#36267,#36268,
#36269,#36270,#36271,#36272,#36273,#36274,#36275,#36276,#36277,#36278,#36279,
#36280,#36281,#36282,#36283,#36284,#36285,#36286,#36287,#36288,#36289,#36290,
#36291,#36292,#36293,#36294,#36295,#36296,#36297,#36298,#36299,#36300,#36301,
#36302,#36303,#36304,#36305,#36306,#36307,#36308,#36309,#36310,#36311,#36312,
#36313,#36314,#36315,#36316,#36317,#36318,#36319,#36320,#36321,#36322,#36323,
#36324,#36325,#36326,#36327,#36328,#36329,#36330,#36331,#36332,#36333,#36334,
#36335,#36336,#36337,#36338,#36339)),.UNSPECIFIED.,.F.,.F.,.F.,(4,4),(4,
1,1,1,1,1,1,1,1,1,1,1,1,1,1,1,1,1,1,1,1,1,1,1,1,1,1,1,1,1,1,1,1,1,1,1,1,
1,1,1,1,1,1,1,1,1,1,1,1,1,1,1,1,1,1,1,1,1,1,1,1,1,1,1,1,1,1,1,1,1,1,1,1,
1,1,1,1,1,1,1,1,1,1,1,1,1,1,1,1,1,1,1,1,1,1,1,1,1,1,1,1,1,1,1,1,1,1,1,1,
1,1,1,1,1,1,1,1,1,1,1,1,1,1,1,1,1,1,1,1,1,1,1,1,1,1,1,1,1,1,1,1,1,1,1,1,
1,1,1,1,1,1,1,1,1,1,4),(0.,0.0658467982010769),(11.6150328478184,12.61338032228,
13.6117277967416,14.6100752712031,15.6084227456647,16.6067702201263,17.6051176945879,
18.6034651690495,19.6018126435111,20.6001601179726,21.5985075924342,22.5968550668958,
23.5952025413574,24.593550015819,25.5918974902806,26.5902449647422,27.5885924392037,
28.5869399136653,29.5852873881269,30.5836348625885,31.5819823370501,32.5803298115117,
33.5786772859732,34.5770247604348,35.5753722348964,36.573719709358,37.5720671838196,
38.5704146582812,39.5687621327428,40.5671096072043,41.5654570816659,42.5638045561275,
43.5621520305891,44.5604995050507,45.5588469795123,46.5571944539738,47.5555419284354,
48.553889402897,49.5522368773586,50.5505843518202,51.5489318262818,52.5472793007434,
53.545626775205,54.5439742496665,55.5423217241281,56.5406691985897,57.5390166730513,
58.5373641475129,59.5357116219745,60.534059096436,61.5324065708976,62.5307540453592,
63.5291015198208,64.5274489942824,65.525796468744,66.5241439432056,67.5224914176671,
68.5208388921287,69.5191863665903,70.5175338410519,71.5158813155135,72.5142287899751,
73.5125762644366,74.5109237388982,75.5092712133598,76.5076186878214,77.505966162283,
78.5043136367446,79.5026611112062,80.5010085856677,81.4993560601293,82.4977035345909,
83.4960510090525,84.4943984835141,85.4927459579757,86.4910934324373,87.4894409068988,
88.4877883813604,89.486135855822,90.4844833302836,91.4828308047452,92.4811782792068,
93.4795257536684,94.4778732281299,95.4762207025915,96.4745681770531,97.4729156515147,
98.4712631259763,99.4696106004379,100.467958074899,101.466305549361,102.464653023823,
103.463000498284,104.461347972746,105.459695447207,106.458042921669,107.456390396131,
108.454737870592,109.453085345054,110.451432819515,111.449780293977,112.448127768438,
113.4464752429,114.444822717362,115.443170191823,116.441517666285,117.439865140746,
118.438212615208,119.43656008967,120.434907564131,121.433255038593,122.431602513054,
123.429949987516,124.428297461977,125.426644936439,126.424992410901,127.423339885362,
128.421687359824,129.420034834285,130.418382308747,131.416729783209,132.41507725767,
133.413424732132,134.411772206593,135.410119681055,136.408467155516,137.406814629978,
138.40516210444,139.403509578901,140.401857053363,141.400204527824,142.398552002286,
143.396899476748,144.395246951209,145.393594425671,146.391941900132,147.390289374594,
148.388636849056,149.386984323517,150.385331797979,151.38367927244,152.382026746902,
153.380374221363,154.378721695825,155.377069170287,156.375416644748,157.37376411921,
158.372111593671,159.370459068133,160.368806542595,161.367154017056,162.365501491518,
163.363848965979,164.362196440441,165.360543914902,166.358891389364),
 .UNSPECIFIED.);
#343=B_SPLINE_SURFACE_WITH_KNOTS('',3,3,((#36477,#36478,#36479,#36480,#36481,
#36482,#36483,#36484,#36485,#36486,#36487,#36488,#36489,#36490,#36491,#36492,
#36493,#36494,#36495,#36496,#36497,#36498,#36499,#36500,#36501,#36502,#36503,
#36504,#36505,#36506,#36507,#36508,#36509,#36510,#36511,#36512,#36513,#36514,
#36515,#36516,#36517,#36518,#36519,#36520,#36521,#36522,#36523,#36524,#36525,
#36526,#36527,#36528,#36529,#36530,#36531,#36532,#36533,#36534,#36535,#36536,
#36537,#36538,#36539,#36540,#36541,#36542,#36543,#36544,#36545,#36546,#36547,
#36548,#36549,#36550,#36551,#36552,#36553,#36554,#36555,#36556,#36557,#36558,
#36559,#36560,#36561,#36562,#36563,#36564,#36565,#36566,#36567,#36568,#36569,
#36570,#36571,#36572,#36573,#36574,#36575,#36576,#36577,#36578,#36579,#36580,
#36581,#36582,#36583,#36584,#36585,#36586,#36587,#36588,#36589,#36590,#36591,
#36592,#36593,#36594,#36595,#36596,#36597,#36598,#36599,#36600,#36601,#36602,
#36603,#36604,#36605,#36606,#36607,#36608,#36609,#36610,#36611,#36612,#36613,
#36614,#36615,#36616,#36617,#36618,#36619,#36620,#36621,#36622,#36623,#36624,
#36625,#36626,#36627,#36628,#36629,#36630,#36631,#36632,#36633,#36634,#36635,
#36636),(#36637,#36638,#36639,#36640,#36641,#36642,#36643,#36644,#36645,
#36646,#36647,#36648,#36649,#36650,#36651,#36652,#36653,#36654,#36655,#36656,
#36657,#36658,#36659,#36660,#36661,#36662,#36663,#36664,#36665,#36666,#36667,
#36668,#36669,#36670,#36671,#36672,#36673,#36674,#36675,#36676,#36677,#36678,
#36679,#36680,#36681,#36682,#36683,#36684,#36685,#36686,#36687,#36688,#36689,
#36690,#36691,#36692,#36693,#36694,#36695,#36696,#36697,#36698,#36699,#36700,
#36701,#36702,#36703,#36704,#36705,#36706,#36707,#36708,#36709,#36710,#36711,
#36712,#36713,#36714,#36715,#36716,#36717,#36718,#36719,#36720,#36721,#36722,
#36723,#36724,#36725,#36726,#36727,#36728,#36729,#36730,#36731,#36732,#36733,
#36734,#36735,#36736,#36737,#36738,#36739,#36740,#36741,#36742,#36743,#36744,
#36745,#36746,#36747,#36748,#36749,#36750,#36751,#36752,#36753,#36754,#36755,
#36756,#36757,#36758,#36759,#36760,#36761,#36762,#36763,#36764,#36765,#36766,
#36767,#36768,#36769,#36770,#36771,#36772,#36773,#36774,#36775,#36776,#36777,
#36778,#36779,#36780,#36781,#36782,#36783,#36784,#36785,#36786,#36787,#36788,
#36789,#36790,#36791,#36792,#36793,#36794,#36795,#36796),(#36797,#36798,
#36799,#36800,#36801,#36802,#36803,#36804,#36805,#36806,#36807,#36808,#36809,
#36810,#36811,#36812,#36813,#36814,#36815,#36816,#36817,#36818,#36819,#36820,
#36821,#36822,#36823,#36824,#36825,#36826,#36827,#36828,#36829,#36830,#36831,
#36832,#36833,#36834,#36835,#36836,#36837,#36838,#36839,#36840,#36841,#36842,
#36843,#36844,#36845,#36846,#36847,#36848,#36849,#36850,#36851,#36852,#36853,
#36854,#36855,#36856,#36857,#36858,#36859,#36860,#36861,#36862,#36863,#36864,
#36865,#36866,#36867,#36868,#36869,#36870,#36871,#36872,#36873,#36874,#36875,
#36876,#36877,#36878,#36879,#36880,#36881,#36882,#36883,#36884,#36885,#36886,
#36887,#36888,#36889,#36890,#36891,#36892,#36893,#36894,#36895,#36896,#36897,
#36898,#36899,#36900,#36901,#36902,#36903,#36904,#36905,#36906,#36907,#36908,
#36909,#36910,#36911,#36912,#36913,#36914,#36915,#36916,#36917,#36918,#36919,
#36920,#36921,#36922,#36923,#36924,#36925,#36926,#36927,#36928,#36929,#36930,
#36931,#36932,#36933,#36934,#36935,#36936,#36937,#36938,#36939,#36940,#36941,
#36942,#36943,#36944,#36945,#36946,#36947,#36948,#36949,#36950,#36951,#36952,
#36953,#36954,#36955,#36956),(#36957,#36958,#36959,#36960,#36961,#36962,
#36963,#36964,#36965,#36966,#36967,#36968,#36969,#36970,#36971,#36972,#36973,
#36974,#36975,#36976,#36977,#36978,#36979,#36980,#36981,#36982,#36983,#36984,
#36985,#36986,#36987,#36988,#36989,#36990,#36991,#36992,#36993,#36994,#36995,
#36996,#36997,#36998,#36999,#37000,#37001,#37002,#37003,#37004,#37005,#37006,
#37007,#37008,#37009,#37010,#37011,#37012,#37013,#37014,#37015,#37016,#37017,
#37018,#37019,#37020,#37021,#37022,#37023,#37024,#37025,#37026,#37027,#37028,
#37029,#37030,#37031,#37032,#37033,#37034,#37035,#37036,#37037,#37038,#37039,
#37040,#37041,#37042,#37043,#37044,#37045,#37046,#37047,#37048,#37049,#37050,
#37051,#37052,#37053,#37054,#37055,#37056,#37057,#37058,#37059,#37060,#37061,
#37062,#37063,#37064,#37065,#37066,#37067,#37068,#37069,#37070,#37071,#37072,
#37073,#37074,#37075,#37076,#37077,#37078,#37079,#37080,#37081,#37082,#37083,
#37084,#37085,#37086,#37087,#37088,#37089,#37090,#37091,#37092,#37093,#37094,
#37095,#37096,#37097,#37098,#37099,#37100,#37101,#37102,#37103,#37104,#37105,
#37106,#37107,#37108,#37109,#37110,#37111,#37112,#37113,#37114,#37115,#37116)),
 .UNSPECIFIED.,.F.,.F.,.F.,(4,4),(4,1,1,1,1,1,1,1,1,1,1,1,1,1,1,1,1,1,1,
1,1,1,1,1,1,1,1,1,1,1,1,1,1,1,1,1,1,1,1,1,1,1,1,1,1,1,1,1,1,1,1,1,1,1,1,
1,1,1,1,1,1,1,1,1,1,1,1,1,1,1,1,1,1,1,1,1,1,1,1,1,1,1,1,1,1,1,1,1,1,1,1,
1,1,1,1,1,1,1,1,1,1,1,1,1,1,1,1,1,1,1,1,1,1,1,1,1,1,1,1,1,1,1,1,1,1,1,1,
1,1,1,1,1,1,1,1,1,1,1,1,1,1,1,1,1,1,1,1,1,1,1,1,1,1,1,1,1,1,4),(0.,0.0658467982010769),
(8.30747755240114,9.30628326397092,10.3050889755407,11.3038946871105,12.3027003986802,
13.30150611025,14.3003118218198,15.2991175333896,16.2979232449593,17.2967289565291,
18.2955346680989,19.2943403796687,20.2931460912385,21.2919518028082,22.290757514378,
23.2895632259478,24.2883689375176,25.2871746490873,26.2859803606571,27.2847860722269,
28.2835917837967,29.2823974953664,30.2812032069362,31.280008918506,32.2788146300758,
33.2776203416455,34.2764260532153,35.2752317647851,36.2740374763549,37.2728431879246,
38.2716488994944,39.2704546110642,40.269260322634,41.2680660342037,42.2668717457735,
43.2656774573433,44.2644831689131,45.2632888804829,46.2620945920526,47.2609003036224,
48.2597060151922,49.258511726762,50.2573174383317,51.2561231499015,52.2549288614713,
53.2537345730411,54.2525402846108,55.2513459961806,56.2501517077504,57.2489574193202,
58.2477631308899,59.2465688424597,60.2453745540295,61.2441802655993,62.242985977169,
63.2417916887388,64.2405974003086,65.2394031118784,66.2382088234481,67.2370145350179,
68.2358202465877,69.2346259581575,70.2334316697272,71.232237381297,72.2310430928668,
73.2298488044366,74.2286545160063,75.2274602275761,76.2262659391459,77.2250716507157,
78.2238773622854,79.2226830738552,80.221488785425,81.2202944969948,82.2191002085646,
83.2179059201343,84.2167116317041,85.2155173432739,86.2143230548436,87.2131287664134,
88.2119344779832,89.210740189553,90.2095459011228,91.2083516126925,92.2071573242623,
93.2059630358321,94.2047687474019,95.2035744589716,96.2023801705414,97.2011858821112,
98.199991593681,99.1987973052507,100.197603016821,101.19640872839,102.19521443996,
103.19402015153,104.1928258631,105.191631574669,106.190437286239,107.189242997809,
108.188048709379,109.186854420948,110.185660132518,111.184465844088,112.183271555658,
113.182077267228,114.180882978797,115.179688690367,116.178494401937,117.177300113507,
118.176105825076,119.174911536646,120.173717248216,121.172522959786,122.171328671356,
123.170134382925,124.168940094495,125.167745806065,126.166551517635,127.165357229204,
128.164162940774,129.162968652344,130.161774363914,131.160580075484,132.159385787053,
133.158191498623,134.156997210193,135.155802921763,136.154608633332,137.153414344902,
138.152220056472,139.151025768042,140.149831479612,141.148637191181,142.147442902751,
143.146248614321,144.145054325891,145.14386003746,146.14266574903,147.1414714606,
148.14027717217,149.13908288374,150.137888595309,151.136694306879,152.135500018449,
153.134305730019,154.133111441588,155.131917153158,156.130722864728,157.129528576298,
158.128334287868,159.127139999437,160.125945711007,161.124751422577,162.123557134147,
163.122362845716,164.121168557286,165.119974268856),.UNSPECIFIED.);
#344=B_SPLINE_SURFACE_WITH_KNOTS('',3,3,((#45406,#45407,#45408,#45409,#45410,
#45411,#45412,#45413,#45414,#45415,#45416,#45417,#45418,#45419,#45420,#45421,
#45422,#45423,#45424,#45425,#45426,#45427,#45428,#45429,#45430,#45431,#45432,
#45433,#45434,#45435,#45436,#45437,#45438,#45439,#45440,#45441,#45442,#45443,
#45444,#45445,#45446,#45447,#45448,#45449,#45450,#45451,#45452,#45453,#45454,
#45455,#45456,#45457,#45458,#45459,#45460,#45461,#45462,#45463,#45464,#45465,
#45466,#45467,#45468,#45469,#45470,#45471,#45472,#45473,#45474,#45475,#45476,
#45477,#45478,#45479,#45480,#45481,#45482,#45483,#45484,#45485,#45486,#45487,
#45488,#45489,#45490,#45491,#45492,#45493,#45494,#45495,#45496,#45497,#45498,
#45499,#45500,#45501,#45502,#45503,#45504,#45505,#45506,#45507,#45508,#45509,
#45510,#45511,#45512,#45513,#45514,#45515,#45516,#45517,#45518,#45519,#45520,
#45521,#45522,#45523,#45524,#45525,#45526,#45527,#45528,#45529,#45530,#45531,
#45532,#45533,#45534,#45535,#45536,#45537,#45538,#45539,#45540,#45541,#45542,
#45543,#45544,#45545,#45546,#45547,#45548,#45549,#45550,#45551,#45552,#45553,
#45554,#45555,#45556,#45557,#45558,#45559,#45560,#45561,#45562,#45563,#45564,
#45565,#45566,#45567,#45568,#45569,#45570,#45571,#45572,#45573,#45574,#45575,
#45576,#45577,#45578,#45579,#45580,#45581,#45582,#45583,#45584,#45585,#45586,
#45587,#45588,#45589,#45590,#45591,#45592,#45593,#45594,#45595,#45596,#45597,
#45598,#45599,#45600,#45601,#45602,#45603,#45604,#45605,#45606,#45607,#45608,
#45609,#45610,#45611,#45612,#45613,#45614,#45615,#45616,#45617,#45618,#45619,
#45620,#45621,#45622,#45623,#45624,#45625,#45626,#45627,#45628,#45629,#45630,
#45631,#45632,#45633,#45634,#45635,#45636,#45637,#45638,#45639,#45640,#45641,
#45642,#45643,#45644,#45645,#45646,#45647,#45648,#45649,#45650,#45651,#45652,
#45653,#45654,#45655,#45656,#45657,#45658,#45659,#45660,#45661,#45662,#45663,
#45664,#45665,#45666,#45667,#45668,#45669,#45670,#45671,#45672,#45673,#45674,
#45675,#45676,#45677,#45678,#45679,#45680,#45681,#45682,#45683,#45684,#45685,
#45686,#45687,#45688,#45689,#45690,#45691,#45692,#45693,#45694,#45695,#45696,
#45697,#45698,#45699,#45700,#45701,#45702,#45703,#45704,#45705,#45706,#45707,
#45708,#45709,#45710,#45711,#45712,#45713,#45714,#45715,#45716,#45717,#45718,
#45719,#45720,#45721,#45722,#45723,#45724,#45725,#45726,#45727,#45728,#45729,
#45730,#45731,#45732,#45733,#45734,#45735,#45736,#45737,#45738,#45739,#45740,
#45741,#45742,#45743,#45744,#45745,#45746,#45747,#45748,#45749,#45750,#45751,
#45752,#45753,#45754,#45755,#45756,#45757,#45758,#45759,#45760,#45761,#45762,
#45763,#45764,#45765,#45766,#45767,#45768,#45769,#45770,#45771,#45772,#45773,
#45774,#45775,#45776,#45777,#45778,#45779,#45780,#45781,#45782,#45783,#45784,
#45785,#45786,#45787,#45788,#45789,#45790,#45791,#45792,#45793,#45794,#45795,
#45796,#45797,#45798,#45799,#45800,#45801,#45802,#45803,#45804,#45805,#45806,
#45807,#45808,#45809,#45810,#45811,#45812,#45813,#45814,#45815,#45816,#45817,
#45818,#45819,#45820,#45821,#45822,#45823,#45824,#45825,#45826,#45827,#45828,
#45829,#45830,#45831,#45832,#45833,#45834,#45835,#45836,#45837,#45838,#45839,
#45840,#45841,#45842,#45843,#45844,#45845,#45846,#45847,#45848,#45849,#45850,
#45851,#45852,#45853,#45854,#45855,#45856,#45857,#45858,#45859,#45860,#45861,
#45862,#45863,#45864,#45865,#45866,#45867,#45868,#45869,#45870,#45871,#45872,
#45873,#45874,#45875,#45876,#45877,#45878,#45879,#45880,#45881,#45882,#45883,
#45884,#45885,#45886,#45887,#45888,#45889,#45890,#45891,#45892,#45893,#45894,
#45895,#45896,#45897,#45898,#45899,#45900,#45901,#45902),(#45903,#45904,
#45905,#45906,#45907,#45908,#45909,#45910,#45911,#45912,#45913,#45914,#45915,
#45916,#45917,#45918,#45919,#45920,#45921,#45922,#45923,#45924,#45925,#45926,
#45927,#45928,#45929,#45930,#45931,#45932,#45933,#45934,#45935,#45936,#45937,
#45938,#45939,#45940,#45941,#45942,#45943,#45944,#45945,#45946,#45947,#45948,
#45949,#45950,#45951,#45952,#45953,#45954,#45955,#45956,#45957,#45958,#45959,
#45960,#45961,#45962,#45963,#45964,#45965,#45966,#45967,#45968,#45969,#45970,
#45971,#45972,#45973,#45974,#45975,#45976,#45977,#45978,#45979,#45980,#45981,
#45982,#45983,#45984,#45985,#45986,#45987,#45988,#45989,#45990,#45991,#45992,
#45993,#45994,#45995,#45996,#45997,#45998,#45999,#46000,#46001,#46002,#46003,
#46004,#46005,#46006,#46007,#46008,#46009,#46010,#46011,#46012,#46013,#46014,
#46015,#46016,#46017,#46018,#46019,#46020,#46021,#46022,#46023,#46024,#46025,
#46026,#46027,#46028,#46029,#46030,#46031,#46032,#46033,#46034,#46035,#46036,
#46037,#46038,#46039,#46040,#46041,#46042,#46043,#46044,#46045,#46046,#46047,
#46048,#46049,#46050,#46051,#46052,#46053,#46054,#46055,#46056,#46057,#46058,
#46059,#46060,#46061,#46062,#46063,#46064,#46065,#46066,#46067,#46068,#46069,
#46070,#46071,#46072,#46073,#46074,#46075,#46076,#46077,#46078,#46079,#46080,
#46081,#46082,#46083,#46084,#46085,#46086,#46087,#46088,#46089,#46090,#46091,
#46092,#46093,#46094,#46095,#46096,#46097,#46098,#46099,#46100,#46101,#46102,
#46103,#46104,#46105,#46106,#46107,#46108,#46109,#46110,#46111,#46112,#46113,
#46114,#46115,#46116,#46117,#46118,#46119,#46120,#46121,#46122,#46123,#46124,
#46125,#46126,#46127,#46128,#46129,#46130,#46131,#46132,#46133,#46134,#46135,
#46136,#46137,#46138,#46139,#46140,#46141,#46142,#46143,#46144,#46145,#46146,
#46147,#46148,#46149,#46150,#46151,#46152,#46153,#46154,#46155,#46156,#46157,
#46158,#46159,#46160,#46161,#46162,#46163,#46164,#46165,#46166,#46167,#46168,
#46169,#46170,#46171,#46172,#46173,#46174,#46175,#46176,#46177,#46178,#46179,
#46180,#46181,#46182,#46183,#46184,#46185,#46186,#46187,#46188,#46189,#46190,
#46191,#46192,#46193,#46194,#46195,#46196,#46197,#46198,#46199,#46200,#46201,
#46202,#46203,#46204,#46205,#46206,#46207,#46208,#46209,#46210,#46211,#46212,
#46213,#46214,#46215,#46216,#46217,#46218,#46219,#46220,#46221,#46222,#46223,
#46224,#46225,#46226,#46227,#46228,#46229,#46230,#46231,#46232,#46233,#46234,
#46235,#46236,#46237,#46238,#46239,#46240,#46241,#46242,#46243,#46244,#46245,
#46246,#46247,#46248,#46249,#46250,#46251,#46252,#46253,#46254,#46255,#46256,
#46257,#46258,#46259,#46260,#46261,#46262,#46263,#46264,#46265,#46266,#46267,
#46268,#46269,#46270,#46271,#46272,#46273,#46274,#46275,#46276,#46277,#46278,
#46279,#46280,#46281,#46282,#46283,#46284,#46285,#46286,#46287,#46288,#46289,
#46290,#46291,#46292,#46293,#46294,#46295,#46296,#46297,#46298,#46299,#46300,
#46301,#46302,#46303,#46304,#46305,#46306,#46307,#46308,#46309,#46310,#46311,
#46312,#46313,#46314,#46315,#46316,#46317,#46318,#46319,#46320,#46321,#46322,
#46323,#46324,#46325,#46326,#46327,#46328,#46329,#46330,#46331,#46332,#46333,
#46334,#46335,#46336,#46337,#46338,#46339,#46340,#46341,#46342,#46343,#46344,
#46345,#46346,#46347,#46348,#46349,#46350,#46351,#46352,#46353,#46354,#46355,
#46356,#46357,#46358,#46359,#46360,#46361,#46362,#46363,#46364,#46365,#46366,
#46367,#46368,#46369,#46370,#46371,#46372,#46373,#46374,#46375,#46376,#46377,
#46378,#46379,#46380,#46381,#46382,#46383,#46384,#46385,#46386,#46387,#46388,
#46389,#46390,#46391,#46392,#46393,#46394,#46395,#46396,#46397,#46398,#46399),
(#46400,#46401,#46402,#46403,#46404,#46405,#46406,#46407,#46408,#46409,
#46410,#46411,#46412,#46413,#46414,#46415,#46416,#46417,#46418,#46419,#46420,
#46421,#46422,#46423,#46424,#46425,#46426,#46427,#46428,#46429,#46430,#46431,
#46432,#46433,#46434,#46435,#46436,#46437,#46438,#46439,#46440,#46441,#46442,
#46443,#46444,#46445,#46446,#46447,#46448,#46449,#46450,#46451,#46452,#46453,
#46454,#46455,#46456,#46457,#46458,#46459,#46460,#46461,#46462,#46463,#46464,
#46465,#46466,#46467,#46468,#46469,#46470,#46471,#46472,#46473,#46474,#46475,
#46476,#46477,#46478,#46479,#46480,#46481,#46482,#46483,#46484,#46485,#46486,
#46487,#46488,#46489,#46490,#46491,#46492,#46493,#46494,#46495,#46496,#46497,
#46498,#46499,#46500,#46501,#46502,#46503,#46504,#46505,#46506,#46507,#46508,
#46509,#46510,#46511,#46512,#46513,#46514,#46515,#46516,#46517,#46518,#46519,
#46520,#46521,#46522,#46523,#46524,#46525,#46526,#46527,#46528,#46529,#46530,
#46531,#46532,#46533,#46534,#46535,#46536,#46537,#46538,#46539,#46540,#46541,
#46542,#46543,#46544,#46545,#46546,#46547,#46548,#46549,#46550,#46551,#46552,
#46553,#46554,#46555,#46556,#46557,#46558,#46559,#46560,#46561,#46562,#46563,
#46564,#46565,#46566,#46567,#46568,#46569,#46570,#46571,#46572,#46573,#46574,
#46575,#46576,#46577,#46578,#46579,#46580,#46581,#46582,#46583,#46584,#46585,
#46586,#46587,#46588,#46589,#46590,#46591,#46592,#46593,#46594,#46595,#46596,
#46597,#46598,#46599,#46600,#46601,#46602,#46603,#46604,#46605,#46606,#46607,
#46608,#46609,#46610,#46611,#46612,#46613,#46614,#46615,#46616,#46617,#46618,
#46619,#46620,#46621,#46622,#46623,#46624,#46625,#46626,#46627,#46628,#46629,
#46630,#46631,#46632,#46633,#46634,#46635,#46636,#46637,#46638,#46639,#46640,
#46641,#46642,#46643,#46644,#46645,#46646,#46647,#46648,#46649,#46650,#46651,
#46652,#46653,#46654,#46655,#46656,#46657,#46658,#46659,#46660,#46661,#46662,
#46663,#46664,#46665,#46666,#46667,#46668,#46669,#46670,#46671,#46672,#46673,
#46674,#46675,#46676,#46677,#46678,#46679,#46680,#46681,#46682,#46683,#46684,
#46685,#46686,#46687,#46688,#46689,#46690,#46691,#46692,#46693,#46694,#46695,
#46696,#46697,#46698,#46699,#46700,#46701,#46702,#46703,#46704,#46705,#46706,
#46707,#46708,#46709,#46710,#46711,#46712,#46713,#46714,#46715,#46716,#46717,
#46718,#46719,#46720,#46721,#46722,#46723,#46724,#46725,#46726,#46727,#46728,
#46729,#46730,#46731,#46732,#46733,#46734,#46735,#46736,#46737,#46738,#46739,
#46740,#46741,#46742,#46743,#46744,#46745,#46746,#46747,#46748,#46749,#46750,
#46751,#46752,#46753,#46754,#46755,#46756,#46757,#46758,#46759,#46760,#46761,
#46762,#46763,#46764,#46765,#46766,#46767,#46768,#46769,#46770,#46771,#46772,
#46773,#46774,#46775,#46776,#46777,#46778,#46779,#46780,#46781,#46782,#46783,
#46784,#46785,#46786,#46787,#46788,#46789,#46790,#46791,#46792,#46793,#46794,
#46795,#46796,#46797,#46798,#46799,#46800,#46801,#46802,#46803,#46804,#46805,
#46806,#46807,#46808,#46809,#46810,#46811,#46812,#46813,#46814,#46815,#46816,
#46817,#46818,#46819,#46820,#46821,#46822,#46823,#46824,#46825,#46826,#46827,
#46828,#46829,#46830,#46831,#46832,#46833,#46834,#46835,#46836,#46837,#46838,
#46839,#46840,#46841,#46842,#46843,#46844,#46845,#46846,#46847,#46848,#46849,
#46850,#46851,#46852,#46853,#46854,#46855,#46856,#46857,#46858,#46859,#46860,
#46861,#46862,#46863,#46864,#46865,#46866,#46867,#46868,#46869,#46870,#46871,
#46872,#46873,#46874,#46875,#46876,#46877,#46878,#46879,#46880,#46881,#46882,
#46883,#46884,#46885,#46886,#46887,#46888,#46889,#46890,#46891,#46892,#46893,
#46894,#46895,#46896),(#46897,#46898,#46899,#46900,#46901,#46902,#46903,
#46904,#46905,#46906,#46907,#46908,#46909,#46910,#46911,#46912,#46913,#46914,
#46915,#46916,#46917,#46918,#46919,#46920,#46921,#46922,#46923,#46924,#46925,
#46926,#46927,#46928,#46929,#46930,#46931,#46932,#46933,#46934,#46935,#46936,
#46937,#46938,#46939,#46940,#46941,#46942,#46943,#46944,#46945,#46946,#46947,
#46948,#46949,#46950,#46951,#46952,#46953,#46954,#46955,#46956,#46957,#46958,
#46959,#46960,#46961,#46962,#46963,#46964,#46965,#46966,#46967,#46968,#46969,
#46970,#46971,#46972,#46973,#46974,#46975,#46976,#46977,#46978,#46979,#46980,
#46981,#46982,#46983,#46984,#46985,#46986,#46987,#46988,#46989,#46990,#46991,
#46992,#46993,#46994,#46995,#46996,#46997,#46998,#46999,#47000,#47001,#47002,
#47003,#47004,#47005,#47006,#47007,#47008,#47009,#47010,#47011,#47012,#47013,
#47014,#47015,#47016,#47017,#47018,#47019,#47020,#47021,#47022,#47023,#47024,
#47025,#47026,#47027,#47028,#47029,#47030,#47031,#47032,#47033,#47034,#47035,
#47036,#47037,#47038,#47039,#47040,#47041,#47042,#47043,#47044,#47045,#47046,
#47047,#47048,#47049,#47050,#47051,#47052,#47053,#47054,#47055,#47056,#47057,
#47058,#47059,#47060,#47061,#47062,#47063,#47064,#47065,#47066,#47067,#47068,
#47069,#47070,#47071,#47072,#47073,#47074,#47075,#47076,#47077,#47078,#47079,
#47080,#47081,#47082,#47083,#47084,#47085,#47086,#47087,#47088,#47089,#47090,
#47091,#47092,#47093,#47094,#47095,#47096,#47097,#47098,#47099,#47100,#47101,
#47102,#47103,#47104,#47105,#47106,#47107,#47108,#47109,#47110,#47111,#47112,
#47113,#47114,#47115,#47116,#47117,#47118,#47119,#47120,#47121,#47122,#47123,
#47124,#47125,#47126,#47127,#47128,#47129,#47130,#47131,#47132,#47133,#47134,
#47135,#47136,#47137,#47138,#47139,#47140,#47141,#47142,#47143,#47144,#47145,
#47146,#47147,#47148,#47149,#47150,#47151,#47152,#47153,#47154,#47155,#47156,
#47157,#47158,#47159,#47160,#47161,#47162,#47163,#47164,#47165,#47166,#47167,
#47168,#47169,#47170,#47171,#47172,#47173,#47174,#47175,#47176,#47177,#47178,
#47179,#47180,#47181,#47182,#47183,#47184,#47185,#47186,#47187,#47188,#47189,
#47190,#47191,#47192,#47193,#47194,#47195,#47196,#47197,#47198,#47199,#47200,
#47201,#47202,#47203,#47204,#47205,#47206,#47207,#47208,#47209,#47210,#47211,
#47212,#47213,#47214,#47215,#47216,#47217,#47218,#47219,#47220,#47221,#47222,
#47223,#47224,#47225,#47226,#47227,#47228,#47229,#47230,#47231,#47232,#47233,
#47234,#47235,#47236,#47237,#47238,#47239,#47240,#47241,#47242,#47243,#47244,
#47245,#47246,#47247,#47248,#47249,#47250,#47251,#47252,#47253,#47254,#47255,
#47256,#47257,#47258,#47259,#47260,#47261,#47262,#47263,#47264,#47265,#47266,
#47267,#47268,#47269,#47270,#47271,#47272,#47273,#47274,#47275,#47276,#47277,
#47278,#47279,#47280,#47281,#47282,#47283,#47284,#47285,#47286,#47287,#47288,
#47289,#47290,#47291,#47292,#47293,#47294,#47295,#47296,#47297,#47298,#47299,
#47300,#47301,#47302,#47303,#47304,#47305,#47306,#47307,#47308,#47309,#47310,
#47311,#47312,#47313,#47314,#47315,#47316,#47317,#47318,#47319,#47320,#47321,
#47322,#47323,#47324,#47325,#47326,#47327,#47328,#47329,#47330,#47331,#47332,
#47333,#47334,#47335,#47336,#47337,#47338,#47339,#47340,#47341,#47342,#47343,
#47344,#47345,#47346,#47347,#47348,#47349,#47350,#47351,#47352,#47353,#47354,
#47355,#47356,#47357,#47358,#47359,#47360,#47361,#47362,#47363,#47364,#47365,
#47366,#47367,#47368,#47369,#47370,#47371,#47372,#47373,#47374,#47375,#47376,
#47377,#47378,#47379,#47380,#47381,#47382,#47383,#47384,#47385,#47386,#47387,
#47388,#47389,#47390,#47391,#47392,#47393)),.UNSPECIFIED.,.F.,.F.,.F.,(4,
4),(4,1,1,1,1,1,1,1,1,1,1,1,1,1,1,1,1,1,1,1,1,1,1,1,1,1,1,1,1,1,1,1,1,1,
1,1,1,1,1,1,1,1,1,1,1,1,1,1,1,1,1,1,1,1,1,1,1,1,1,1,1,1,1,1,1,1,1,1,1,1,
1,1,1,1,1,1,1,1,1,1,1,1,1,1,1,1,1,1,1,1,1,1,1,1,1,1,1,1,1,1,1,1,1,1,1,1,
1,1,1,1,1,1,1,1,1,1,1,1,1,1,1,1,1,1,1,1,1,1,1,1,1,1,1,1,1,1,1,1,1,1,1,1,
1,1,1,1,1,1,1,1,1,1,1,1,1,1,1,1,1,1,1,1,1,1,1,1,1,1,1,1,1,1,1,1,1,1,1,1,
1,1,1,1,1,1,1,1,1,1,1,1,1,1,1,1,1,1,1,1,1,1,1,1,1,1,1,1,1,1,1,1,1,1,1,1,
1,1,1,1,1,1,1,1,1,1,1,1,1,1,1,1,1,1,1,1,1,1,1,1,1,1,1,1,1,1,1,1,1,1,1,1,
1,1,1,1,1,1,1,1,1,1,1,1,1,1,1,1,1,1,1,1,1,1,1,1,1,1,1,1,1,1,1,1,1,1,1,1,
1,1,1,1,1,1,1,1,1,1,1,1,1,1,1,1,1,1,1,1,1,1,1,1,1,1,1,1,1,1,1,1,1,1,1,1,
1,1,1,1,1,1,1,1,1,1,1,1,1,1,1,1,1,1,1,1,1,1,1,1,1,1,1,1,1,1,1,1,1,1,1,1,
1,1,1,1,1,1,1,1,1,1,1,1,1,1,1,1,1,1,1,1,1,1,1,1,1,1,1,1,1,1,1,1,1,1,1,1,
1,1,1,1,1,1,1,1,1,1,1,1,1,1,1,1,1,1,1,1,1,1,1,1,1,1,1,1,1,1,1,1,1,1,1,1,
1,1,1,1,1,1,1,1,1,1,1,1,1,1,1,1,1,1,1,1,1,1,1,1,1,1,1,1,1,1,1,1,1,1,1,1,
1,1,1,1,1,1,1,1,1,1,1,1,1,1,1,1,1,1,1,1,1,1,1,1,1,1,1,1,4),(0.,0.0641840294258107),
(11.8589888623082,12.3576971556948,12.8564054490814,13.355113742468,13.8538220358547,
14.3525303292413,14.8512386226279,15.3499469160145,15.8486552094011,16.3473635027878,
16.8460717961744,17.344780089561,17.8434883829476,18.3421966763342,18.8409049697209,
19.3396132631075,19.8383215564941,20.3370298498807,20.8357381432673,21.334446436654,
21.8331547300406,22.3318630234272,22.8305713168138,23.3292796102004,23.8279879035871,
24.3266961969737,24.8254044903603,25.3241127837469,25.8228210771335,26.3215293705201,
26.8202376639068,27.3189459572934,27.81765425068,28.3163625440666,28.8150708374532,
29.3137791308399,29.8124874242265,30.3111957176131,30.8099040109997,31.3086123043863,
31.807320597773,32.3060288911596,32.8047371845462,33.3034454779328,33.8021537713194,
34.3008620647061,34.7995703580927,35.2982786514793,35.7969869448659,36.2956952382525,
36.7944035316392,37.2931118250258,37.7918201184124,38.290528411799,38.7892367051856,
39.2879449985723,39.7866532919589,40.2853615853455,40.7840698787321,41.2827781721187,
41.7814864655054,42.280194758892,42.7789030522786,43.2776113456652,43.7763196390518,
44.2750279324384,44.7737362258251,45.2724445192117,45.7711528125983,46.2698611059849,
46.7685693993716,47.2672776927582,47.7659859861448,48.2646942795314,48.763402572918,
49.2621108663046,49.7608191596913,50.2595274530779,50.7582357464645,51.2569440398511,
51.7556523332377,52.2543606266244,52.753068920011,53.2517772133976,53.7504855067842,
54.2491938001708,54.7479020935575,55.2466103869441,55.7453186803307,56.2440269737173,
56.7427352671039,57.2414435604906,57.7401518538772,58.2388601472638,58.7375684406504,
59.236276734037,59.7349850274237,60.2336933208103,60.7324016141969,61.2311099075835,
61.7298182009701,62.2285264943567,62.7272347877434,63.22594308113,63.7246513745166,
64.2233596679032,64.7220679612898,65.2207762546765,65.7194845480631,66.2181928414497,
66.7169011348363,67.2156094282229,67.7143177216096,68.2130260149962,68.7117343083828,
69.2104426017694,69.709150895156,70.2078591885427,70.7065674819293,71.2052757753159,
71.7039840687025,72.2026923620891,72.7014006554758,73.2001089488624,73.698817242249,
74.1975255356356,74.6962338290222,75.1949421224089,75.6936504157955,76.1923587091821,
76.6910670025687,77.1897752959553,77.6884835893419,78.1871918827286,78.6859001761152,
79.1846084695018,79.6833167628884,80.1820250562751,80.6807333496617,81.1794416430483,
81.6781499364349,82.1768582298215,82.6755665232081,83.1742748165948,83.6729831099814,
84.171691403368,84.6703996967546,85.1691079901412,85.6678162835279,86.1665245769145,
86.6652328703011,87.1639411636877,87.6626494570743,88.161357750461,88.6600660438476,
89.1587743372342,89.6574826306208,90.1561909240074,90.654899217394,91.1536075107807,
91.6523158041673,92.1510240975539,92.6497323909405,93.1484406843271,93.6471489777138,
94.1458572711004,94.644565564487,95.1432738578736,95.6419821512603,96.1406904446469,
96.6393987380335,97.1381070314201,97.6368153248067,98.1355236181933,98.63423191158,
99.1329402049666,99.6316484983532,100.13035679174,100.629065085126,101.127773378513,
101.6264816719,102.125189965286,102.623898258673,103.12260655206,103.621314845446,
104.120023138833,104.618731432219,105.117439725606,105.616148018993,106.114856312379,
106.613564605766,107.112272899152,107.610981192539,108.109689485926,108.608397779312,
109.107106072699,109.605814366086,110.104522659472,110.603230952859,111.101939246245,
111.600647539632,112.099355833019,112.598064126405,113.096772419792,113.595480713179,
114.094189006565,114.592897299952,115.091605593338,115.590313886725,116.089022180112,
116.587730473498,117.086438766885,117.585147060271,118.083855353658,118.582563647045,
119.081271940431,119.579980233818,120.078688527205,120.577396820591,121.076105113978,
121.574813407364,122.073521700751,122.572229994138,123.070938287524,123.569646580911,
124.068354874298,124.567063167684,125.065771461071,125.564479754457,126.063188047844,
126.561896341231,127.060604634617,127.559312928004,128.058021221391,128.556729514777,
129.055437808164,129.55414610155,130.052854394937,130.551562688324,131.05027098171,
131.548979275097,132.54639586187,133.543812448643,134.541229035417,135.53864562219,
136.536062208963,137.533478795736,138.53089538251,139.528311969283,140.525728556056,
141.523145142829,142.520561729602,143.517978316376,144.515394903149,145.512811489922,
146.011519783309,146.510228076695,147.008936370082,147.507644663469,148.006352956855,
148.505061250242,149.003769543629,149.502477837015,150.001186130402,150.499894423788,
150.998602717175,151.497311010562,151.996019303948,152.494727597335,152.993435890721,
153.492144184108,153.990852477495,154.489560770881,154.988269064268,155.486977357655,
155.985685651041,156.484393944428,156.983102237814,157.481810531201,157.980518824588,
158.479227117974,158.977935411361,159.476643704748,159.975351998134,160.474060291521,
160.972768584907,161.471476878294,161.970185171681,162.468893465067,162.967601758454,
163.466310051841,163.965018345227,164.463726638614,164.962434932,165.461143225387,
165.959851518774,166.45855981216,166.957268105547,167.455976398933,167.95468469232,
168.453392985707,168.952101279093,169.45080957248,169.949517865867,170.448226159253,
170.94693445264,171.445642746026,171.944351039413,172.4430593328,172.941767626186,
173.440475919573,173.93918421296,174.437892506346,174.936600799733,175.435309093119,
175.934017386506,176.432725679893,176.931433973279,177.430142266666,177.928850560052,
178.427558853439,178.926267146826,179.424975440212,179.923683733599,180.422392026986,
180.921100320372,181.419808613759,181.918516907145,182.417225200532,182.915933493919,
183.414641787305,183.913350080692,184.412058374079,184.910766667465,185.409474960852,
185.908183254238,186.406891547625,186.905599841012,187.404308134398,187.903016427785,
188.401724721171,188.900433014558,189.399141307945,189.897849601331,190.396557894718,
190.895266188105,191.393974481491,191.892682774878,192.391391068264,192.890099361651,
193.388807655038,193.887515948424,194.386224241811,194.884932535198,195.383640828584,
195.882349121971,196.381057415357,196.879765708744,197.378474002131,197.877182295517,
198.375890588904,198.87459888229,199.373307175677,199.872015469064,200.37072376245,
200.869432055837,201.368140349224,201.86684864261,202.365556935997,202.864265229383,
203.36297352277,203.861681816157,204.360390109543,204.85909840293,205.357806696317,
205.856514989703,206.35522328309,206.853931576476,207.352639869863,207.85134816325,
208.350056456636,208.848764750023,209.347473043409,209.846181336796,210.344889630183,
210.843597923569,211.342306216956,211.841014510343,212.339722803729,212.838431097116,
213.337139390502,213.835847683889,214.334555977276,214.833264270662,215.331972564049,
215.830680857436,216.329389150822,216.828097444209,217.326805737595,217.825514030982,
218.324222324369,218.822930617755,219.321638911142,219.820347204529,220.319055497915,
220.817763791302,221.316472084688,221.815180378075,222.313888671462,222.812596964848,
223.311305258235,223.810013551621,224.308721845008,224.807430138395,225.306138431781,
225.804846725168,226.303555018555,226.802263311941,227.300971605328,227.799679898714,
228.298388192101,228.797096485488,229.295804778874,229.794513072261,230.293221365647,
230.791929659034,231.290637952421,231.789346245807,232.288054539194,232.786762832581,
233.285471125967,233.784179419354,234.28288771274,234.781596006127,235.280304299514,
235.7790125929,236.277720886287,236.776429179674,237.27513747306,237.773845766447,
238.272554059833,238.77126235322,239.269970646607,239.768678939993,240.26738723338,
240.766095526767,241.264803820153,241.76351211354,242.262220406926,242.760928700313,
243.2596369937,243.758345287086,244.257053580473,244.755761873859,245.254470167246,
245.753178460633,246.251886754019,246.750595047406,247.249303340793,247.748011634179,
248.246719927566,248.745428220952,249.244136514339,249.742844807726,250.241553101112,
250.740261394499,251.238969687886,251.737677981272,252.236386274659,252.735094568045,
253.233802861432,253.732511154819,254.231219448205,254.729927741592,255.228636034978,
255.727344328365,256.226052621752,256.724760915138,257.223469208525,257.722177501912,
258.220885795298,258.719594088685,259.218302382071,259.717010675458,260.215718968845,
260.714427262231,261.213135555618,261.711843849004,262.210552142391,262.709260435778,
263.207968729164,263.706677022551,264.205385315938,264.704093609324,265.202801902711),
 .UNSPECIFIED.);
#345=B_SPLINE_SURFACE_WITH_KNOTS('',3,3,((#47543,#47544,#47545,#47546,#47547,
#47548,#47549,#47550,#47551,#47552,#47553,#47554,#47555,#47556,#47557,#47558,
#47559,#47560,#47561,#47562,#47563,#47564,#47565,#47566,#47567,#47568,#47569,
#47570,#47571,#47572,#47573,#47574,#47575,#47576,#47577,#47578,#47579,#47580,
#47581,#47582,#47583,#47584,#47585,#47586,#47587,#47588,#47589,#47590,#47591,
#47592,#47593,#47594,#47595,#47596,#47597,#47598,#47599,#47600,#47601,#47602,
#47603,#47604,#47605,#47606,#47607,#47608,#47609,#47610,#47611,#47612,#47613,
#47614,#47615,#47616,#47617,#47618,#47619,#47620,#47621,#47622,#47623,#47624,
#47625,#47626,#47627,#47628,#47629,#47630,#47631,#47632,#47633,#47634,#47635,
#47636,#47637,#47638,#47639,#47640,#47641,#47642,#47643,#47644,#47645,#47646,
#47647,#47648,#47649,#47650,#47651,#47652,#47653,#47654,#47655,#47656,#47657,
#47658,#47659,#47660,#47661,#47662,#47663,#47664,#47665,#47666,#47667,#47668,
#47669,#47670,#47671,#47672,#47673,#47674,#47675,#47676,#47677,#47678,#47679,
#47680,#47681,#47682,#47683,#47684,#47685,#47686,#47687,#47688,#47689,#47690,
#47691,#47692,#47693,#47694,#47695,#47696,#47697,#47698,#47699,#47700,#47701,
#47702,#47703,#47704,#47705,#47706,#47707,#47708,#47709,#47710,#47711,#47712,
#47713,#47714,#47715,#47716,#47717,#47718,#47719,#47720,#47721,#47722,#47723,
#47724,#47725,#47726,#47727,#47728,#47729,#47730,#47731,#47732,#47733,#47734,
#47735,#47736,#47737,#47738,#47739,#47740,#47741,#47742,#47743,#47744,#47745,
#47746,#47747,#47748,#47749,#47750,#47751,#47752,#47753,#47754,#47755,#47756,
#47757,#47758,#47759,#47760,#47761,#47762,#47763,#47764,#47765,#47766,#47767,
#47768,#47769,#47770,#47771,#47772,#47773,#47774,#47775,#47776,#47777,#47778,
#47779,#47780,#47781,#47782,#47783,#47784,#47785,#47786,#47787,#47788,#47789,
#47790,#47791,#47792,#47793,#47794,#47795,#47796,#47797,#47798,#47799,#47800,
#47801,#47802,#47803,#47804,#47805,#47806,#47807,#47808,#47809,#47810,#47811,
#47812,#47813,#47814,#47815,#47816,#47817,#47818,#47819,#47820,#47821,#47822,
#47823,#47824,#47825,#47826,#47827,#47828,#47829,#47830,#47831,#47832,#47833,
#47834,#47835,#47836,#47837,#47838,#47839,#47840,#47841,#47842,#47843,#47844,
#47845,#47846,#47847,#47848,#47849,#47850,#47851,#47852,#47853,#47854,#47855,
#47856,#47857,#47858,#47859,#47860,#47861,#47862,#47863,#47864,#47865,#47866,
#47867,#47868,#47869,#47870,#47871,#47872,#47873,#47874,#47875,#47876,#47877,
#47878,#47879,#47880,#47881,#47882,#47883,#47884,#47885,#47886,#47887,#47888,
#47889,#47890,#47891,#47892,#47893,#47894,#47895,#47896,#47897,#47898,#47899,
#47900,#47901,#47902,#47903,#47904,#47905,#47906,#47907,#47908,#47909,#47910,
#47911,#47912,#47913,#47914,#47915,#47916,#47917,#47918,#47919,#47920,#47921,
#47922,#47923,#47924,#47925,#47926,#47927,#47928,#47929,#47930,#47931,#47932,
#47933,#47934,#47935,#47936,#47937,#47938,#47939,#47940,#47941,#47942,#47943,
#47944,#47945,#47946,#47947,#47948,#47949,#47950,#47951,#47952,#47953,#47954,
#47955,#47956,#47957,#47958,#47959,#47960,#47961,#47962,#47963,#47964,#47965,
#47966,#47967,#47968,#47969,#47970,#47971,#47972,#47973,#47974,#47975,#47976,
#47977,#47978,#47979,#47980,#47981,#47982,#47983,#47984,#47985,#47986,#47987,
#47988,#47989,#47990,#47991,#47992,#47993,#47994,#47995,#47996,#47997,#47998,
#47999,#48000,#48001,#48002,#48003,#48004,#48005,#48006,#48007,#48008,#48009,
#48010,#48011,#48012,#48013,#48014,#48015,#48016,#48017,#48018,#48019,#48020,
#48021,#48022,#48023,#48024,#48025,#48026,#48027,#48028,#48029,#48030,#48031,
#48032,#48033,#48034,#48035,#48036,#48037,#48038,#48039),(#48040,#48041,
#48042,#48043,#48044,#48045,#48046,#48047,#48048,#48049,#48050,#48051,#48052,
#48053,#48054,#48055,#48056,#48057,#48058,#48059,#48060,#48061,#48062,#48063,
#48064,#48065,#48066,#48067,#48068,#48069,#48070,#48071,#48072,#48073,#48074,
#48075,#48076,#48077,#48078,#48079,#48080,#48081,#48082,#48083,#48084,#48085,
#48086,#48087,#48088,#48089,#48090,#48091,#48092,#48093,#48094,#48095,#48096,
#48097,#48098,#48099,#48100,#48101,#48102,#48103,#48104,#48105,#48106,#48107,
#48108,#48109,#48110,#48111,#48112,#48113,#48114,#48115,#48116,#48117,#48118,
#48119,#48120,#48121,#48122,#48123,#48124,#48125,#48126,#48127,#48128,#48129,
#48130,#48131,#48132,#48133,#48134,#48135,#48136,#48137,#48138,#48139,#48140,
#48141,#48142,#48143,#48144,#48145,#48146,#48147,#48148,#48149,#48150,#48151,
#48152,#48153,#48154,#48155,#48156,#48157,#48158,#48159,#48160,#48161,#48162,
#48163,#48164,#48165,#48166,#48167,#48168,#48169,#48170,#48171,#48172,#48173,
#48174,#48175,#48176,#48177,#48178,#48179,#48180,#48181,#48182,#48183,#48184,
#48185,#48186,#48187,#48188,#48189,#48190,#48191,#48192,#48193,#48194,#48195,
#48196,#48197,#48198,#48199,#48200,#48201,#48202,#48203,#48204,#48205,#48206,
#48207,#48208,#48209,#48210,#48211,#48212,#48213,#48214,#48215,#48216,#48217,
#48218,#48219,#48220,#48221,#48222,#48223,#48224,#48225,#48226,#48227,#48228,
#48229,#48230,#48231,#48232,#48233,#48234,#48235,#48236,#48237,#48238,#48239,
#48240,#48241,#48242,#48243,#48244,#48245,#48246,#48247,#48248,#48249,#48250,
#48251,#48252,#48253,#48254,#48255,#48256,#48257,#48258,#48259,#48260,#48261,
#48262,#48263,#48264,#48265,#48266,#48267,#48268,#48269,#48270,#48271,#48272,
#48273,#48274,#48275,#48276,#48277,#48278,#48279,#48280,#48281,#48282,#48283,
#48284,#48285,#48286,#48287,#48288,#48289,#48290,#48291,#48292,#48293,#48294,
#48295,#48296,#48297,#48298,#48299,#48300,#48301,#48302,#48303,#48304,#48305,
#48306,#48307,#48308,#48309,#48310,#48311,#48312,#48313,#48314,#48315,#48316,
#48317,#48318,#48319,#48320,#48321,#48322,#48323,#48324,#48325,#48326,#48327,
#48328,#48329,#48330,#48331,#48332,#48333,#48334,#48335,#48336,#48337,#48338,
#48339,#48340,#48341,#48342,#48343,#48344,#48345,#48346,#48347,#48348,#48349,
#48350,#48351,#48352,#48353,#48354,#48355,#48356,#48357,#48358,#48359,#48360,
#48361,#48362,#48363,#48364,#48365,#48366,#48367,#48368,#48369,#48370,#48371,
#48372,#48373,#48374,#48375,#48376,#48377,#48378,#48379,#48380,#48381,#48382,
#48383,#48384,#48385,#48386,#48387,#48388,#48389,#48390,#48391,#48392,#48393,
#48394,#48395,#48396,#48397,#48398,#48399,#48400,#48401,#48402,#48403,#48404,
#48405,#48406,#48407,#48408,#48409,#48410,#48411,#48412,#48413,#48414,#48415,
#48416,#48417,#48418,#48419,#48420,#48421,#48422,#48423,#48424,#48425,#48426,
#48427,#48428,#48429,#48430,#48431,#48432,#48433,#48434,#48435,#48436,#48437,
#48438,#48439,#48440,#48441,#48442,#48443,#48444,#48445,#48446,#48447,#48448,
#48449,#48450,#48451,#48452,#48453,#48454,#48455,#48456,#48457,#48458,#48459,
#48460,#48461,#48462,#48463,#48464,#48465,#48466,#48467,#48468,#48469,#48470,
#48471,#48472,#48473,#48474,#48475,#48476,#48477,#48478,#48479,#48480,#48481,
#48482,#48483,#48484,#48485,#48486,#48487,#48488,#48489,#48490,#48491,#48492,
#48493,#48494,#48495,#48496,#48497,#48498,#48499,#48500,#48501,#48502,#48503,
#48504,#48505,#48506,#48507,#48508,#48509,#48510,#48511,#48512,#48513,#48514,
#48515,#48516,#48517,#48518,#48519,#48520,#48521,#48522,#48523,#48524,#48525,
#48526,#48527,#48528,#48529,#48530,#48531,#48532,#48533,#48534,#48535,#48536),
(#48537,#48538,#48539,#48540,#48541,#48542,#48543,#48544,#48545,#48546,
#48547,#48548,#48549,#48550,#48551,#48552,#48553,#48554,#48555,#48556,#48557,
#48558,#48559,#48560,#48561,#48562,#48563,#48564,#48565,#48566,#48567,#48568,
#48569,#48570,#48571,#48572,#48573,#48574,#48575,#48576,#48577,#48578,#48579,
#48580,#48581,#48582,#48583,#48584,#48585,#48586,#48587,#48588,#48589,#48590,
#48591,#48592,#48593,#48594,#48595,#48596,#48597,#48598,#48599,#48600,#48601,
#48602,#48603,#48604,#48605,#48606,#48607,#48608,#48609,#48610,#48611,#48612,
#48613,#48614,#48615,#48616,#48617,#48618,#48619,#48620,#48621,#48622,#48623,
#48624,#48625,#48626,#48627,#48628,#48629,#48630,#48631,#48632,#48633,#48634,
#48635,#48636,#48637,#48638,#48639,#48640,#48641,#48642,#48643,#48644,#48645,
#48646,#48647,#48648,#48649,#48650,#48651,#48652,#48653,#48654,#48655,#48656,
#48657,#48658,#48659,#48660,#48661,#48662,#48663,#48664,#48665,#48666,#48667,
#48668,#48669,#48670,#48671,#48672,#48673,#48674,#48675,#48676,#48677,#48678,
#48679,#48680,#48681,#48682,#48683,#48684,#48685,#48686,#48687,#48688,#48689,
#48690,#48691,#48692,#48693,#48694,#48695,#48696,#48697,#48698,#48699,#48700,
#48701,#48702,#48703,#48704,#48705,#48706,#48707,#48708,#48709,#48710,#48711,
#48712,#48713,#48714,#48715,#48716,#48717,#48718,#48719,#48720,#48721,#48722,
#48723,#48724,#48725,#48726,#48727,#48728,#48729,#48730,#48731,#48732,#48733,
#48734,#48735,#48736,#48737,#48738,#48739,#48740,#48741,#48742,#48743,#48744,
#48745,#48746,#48747,#48748,#48749,#48750,#48751,#48752,#48753,#48754,#48755,
#48756,#48757,#48758,#48759,#48760,#48761,#48762,#48763,#48764,#48765,#48766,
#48767,#48768,#48769,#48770,#48771,#48772,#48773,#48774,#48775,#48776,#48777,
#48778,#48779,#48780,#48781,#48782,#48783,#48784,#48785,#48786,#48787,#48788,
#48789,#48790,#48791,#48792,#48793,#48794,#48795,#48796,#48797,#48798,#48799,
#48800,#48801,#48802,#48803,#48804,#48805,#48806,#48807,#48808,#48809,#48810,
#48811,#48812,#48813,#48814,#48815,#48816,#48817,#48818,#48819,#48820,#48821,
#48822,#48823,#48824,#48825,#48826,#48827,#48828,#48829,#48830,#48831,#48832,
#48833,#48834,#48835,#48836,#48837,#48838,#48839,#48840,#48841,#48842,#48843,
#48844,#48845,#48846,#48847,#48848,#48849,#48850,#48851,#48852,#48853,#48854,
#48855,#48856,#48857,#48858,#48859,#48860,#48861,#48862,#48863,#48864,#48865,
#48866,#48867,#48868,#48869,#48870,#48871,#48872,#48873,#48874,#48875,#48876,
#48877,#48878,#48879,#48880,#48881,#48882,#48883,#48884,#48885,#48886,#48887,
#48888,#48889,#48890,#48891,#48892,#48893,#48894,#48895,#48896,#48897,#48898,
#48899,#48900,#48901,#48902,#48903,#48904,#48905,#48906,#48907,#48908,#48909,
#48910,#48911,#48912,#48913,#48914,#48915,#48916,#48917,#48918,#48919,#48920,
#48921,#48922,#48923,#48924,#48925,#48926,#48927,#48928,#48929,#48930,#48931,
#48932,#48933,#48934,#48935,#48936,#48937,#48938,#48939,#48940,#48941,#48942,
#48943,#48944,#48945,#48946,#48947,#48948,#48949,#48950,#48951,#48952,#48953,
#48954,#48955,#48956,#48957,#48958,#48959,#48960,#48961,#48962,#48963,#48964,
#48965,#48966,#48967,#48968,#48969,#48970,#48971,#48972,#48973,#48974,#48975,
#48976,#48977,#48978,#48979,#48980,#48981,#48982,#48983,#48984,#48985,#48986,
#48987,#48988,#48989,#48990,#48991,#48992,#48993,#48994,#48995,#48996,#48997,
#48998,#48999,#49000,#49001,#49002,#49003,#49004,#49005,#49006,#49007,#49008,
#49009,#49010,#49011,#49012,#49013,#49014,#49015,#49016,#49017,#49018,#49019,
#49020,#49021,#49022,#49023,#49024,#49025,#49026,#49027,#49028,#49029,#49030,
#49031,#49032,#49033),(#49034,#49035,#49036,#49037,#49038,#49039,#49040,
#49041,#49042,#49043,#49044,#49045,#49046,#49047,#49048,#49049,#49050,#49051,
#49052,#49053,#49054,#49055,#49056,#49057,#49058,#49059,#49060,#49061,#49062,
#49063,#49064,#49065,#49066,#49067,#49068,#49069,#49070,#49071,#49072,#49073,
#49074,#49075,#49076,#49077,#49078,#49079,#49080,#49081,#49082,#49083,#49084,
#49085,#49086,#49087,#49088,#49089,#49090,#49091,#49092,#49093,#49094,#49095,
#49096,#49097,#49098,#49099,#49100,#49101,#49102,#49103,#49104,#49105,#49106,
#49107,#49108,#49109,#49110,#49111,#49112,#49113,#49114,#49115,#49116,#49117,
#49118,#49119,#49120,#49121,#49122,#49123,#49124,#49125,#49126,#49127,#49128,
#49129,#49130,#49131,#49132,#49133,#49134,#49135,#49136,#49137,#49138,#49139,
#49140,#49141,#49142,#49143,#49144,#49145,#49146,#49147,#49148,#49149,#49150,
#49151,#49152,#49153,#49154,#49155,#49156,#49157,#49158,#49159,#49160,#49161,
#49162,#49163,#49164,#49165,#49166,#49167,#49168,#49169,#49170,#49171,#49172,
#49173,#49174,#49175,#49176,#49177,#49178,#49179,#49180,#49181,#49182,#49183,
#49184,#49185,#49186,#49187,#49188,#49189,#49190,#49191,#49192,#49193,#49194,
#49195,#49196,#49197,#49198,#49199,#49200,#49201,#49202,#49203,#49204,#49205,
#49206,#49207,#49208,#49209,#49210,#49211,#49212,#49213,#49214,#49215,#49216,
#49217,#49218,#49219,#49220,#49221,#49222,#49223,#49224,#49225,#49226,#49227,
#49228,#49229,#49230,#49231,#49232,#49233,#49234,#49235,#49236,#49237,#49238,
#49239,#49240,#49241,#49242,#49243,#49244,#49245,#49246,#49247,#49248,#49249,
#49250,#49251,#49252,#49253,#49254,#49255,#49256,#49257,#49258,#49259,#49260,
#49261,#49262,#49263,#49264,#49265,#49266,#49267,#49268,#49269,#49270,#49271,
#49272,#49273,#49274,#49275,#49276,#49277,#49278,#49279,#49280,#49281,#49282,
#49283,#49284,#49285,#49286,#49287,#49288,#49289,#49290,#49291,#49292,#49293,
#49294,#49295,#49296,#49297,#49298,#49299,#49300,#49301,#49302,#49303,#49304,
#49305,#49306,#49307,#49308,#49309,#49310,#49311,#49312,#49313,#49314,#49315,
#49316,#49317,#49318,#49319,#49320,#49321,#49322,#49323,#49324,#49325,#49326,
#49327,#49328,#49329,#49330,#49331,#49332,#49333,#49334,#49335,#49336,#49337,
#49338,#49339,#49340,#49341,#49342,#49343,#49344,#49345,#49346,#49347,#49348,
#49349,#49350,#49351,#49352,#49353,#49354,#49355,#49356,#49357,#49358,#49359,
#49360,#49361,#49362,#49363,#49364,#49365,#49366,#49367,#49368,#49369,#49370,
#49371,#49372,#49373,#49374,#49375,#49376,#49377,#49378,#49379,#49380,#49381,
#49382,#49383,#49384,#49385,#49386,#49387,#49388,#49389,#49390,#49391,#49392,
#49393,#49394,#49395,#49396,#49397,#49398,#49399,#49400,#49401,#49402,#49403,
#49404,#49405,#49406,#49407,#49408,#49409,#49410,#49411,#49412,#49413,#49414,
#49415,#49416,#49417,#49418,#49419,#49420,#49421,#49422,#49423,#49424,#49425,
#49426,#49427,#49428,#49429,#49430,#49431,#49432,#49433,#49434,#49435,#49436,
#49437,#49438,#49439,#49440,#49441,#49442,#49443,#49444,#49445,#49446,#49447,
#49448,#49449,#49450,#49451,#49452,#49453,#49454,#49455,#49456,#49457,#49458,
#49459,#49460,#49461,#49462,#49463,#49464,#49465,#49466,#49467,#49468,#49469,
#49470,#49471,#49472,#49473,#49474,#49475,#49476,#49477,#49478,#49479,#49480,
#49481,#49482,#49483,#49484,#49485,#49486,#49487,#49488,#49489,#49490,#49491,
#49492,#49493,#49494,#49495,#49496,#49497,#49498,#49499,#49500,#49501,#49502,
#49503,#49504,#49505,#49506,#49507,#49508,#49509,#49510,#49511,#49512,#49513,
#49514,#49515,#49516,#49517,#49518,#49519,#49520,#49521,#49522,#49523,#49524,
#49525,#49526,#49527,#49528,#49529,#49530)),.UNSPECIFIED.,.F.,.F.,.F.,(4,
4),(4,1,1,1,1,1,1,1,1,1,1,1,1,1,1,1,1,1,1,1,1,1,1,1,1,1,1,1,1,1,1,1,1,1,
1,1,1,1,1,1,1,1,1,1,1,1,1,1,1,1,1,1,1,1,1,1,1,1,1,1,1,1,1,1,1,1,1,1,1,1,
1,1,1,1,1,1,1,1,1,1,1,1,1,1,1,1,1,1,1,1,1,1,1,1,1,1,1,1,1,1,1,1,1,1,1,1,
1,1,1,1,1,1,1,1,1,1,1,1,1,1,1,1,1,1,1,1,1,1,1,1,1,1,1,1,1,1,1,1,1,1,1,1,
1,1,1,1,1,1,1,1,1,1,1,1,1,1,1,1,1,1,1,1,1,1,1,1,1,1,1,1,1,1,1,1,1,1,1,1,
1,1,1,1,1,1,1,1,1,1,1,1,1,1,1,1,1,1,1,1,1,1,1,1,1,1,1,1,1,1,1,1,1,1,1,1,
1,1,1,1,1,1,1,1,1,1,1,1,1,1,1,1,1,1,1,1,1,1,1,1,1,1,1,1,1,1,1,1,1,1,1,1,
1,1,1,1,1,1,1,1,1,1,1,1,1,1,1,1,1,1,1,1,1,1,1,1,1,1,1,1,1,1,1,1,1,1,1,1,
1,1,1,1,1,1,1,1,1,1,1,1,1,1,1,1,1,1,1,1,1,1,1,1,1,1,1,1,1,1,1,1,1,1,1,1,
1,1,1,1,1,1,1,1,1,1,1,1,1,1,1,1,1,1,1,1,1,1,1,1,1,1,1,1,1,1,1,1,1,1,1,1,
1,1,1,1,1,1,1,1,1,1,1,1,1,1,1,1,1,1,1,1,1,1,1,1,1,1,1,1,1,1,1,1,1,1,1,1,
1,1,1,1,1,1,1,1,1,1,1,1,1,1,1,1,1,1,1,1,1,1,1,1,1,1,1,1,1,1,1,1,1,1,1,1,
1,1,1,1,1,1,1,1,1,1,1,1,1,1,1,1,1,1,1,1,1,1,1,1,1,1,1,1,1,1,1,1,1,1,1,1,
1,1,1,1,1,1,1,1,1,1,1,1,1,1,1,1,1,1,1,1,1,1,1,1,1,1,1,1,4),(0.,0.0641840294258107),
(14.3989442667815,14.8976525601681,15.3963608535547,15.8950691469414,16.393777440328,
16.8924857337146,17.3911940271012,17.8899023204878,18.3886106138744,18.8873189072611,
19.3860272006477,19.8847354940343,20.3834437874209,20.8821520808075,21.3808603741942,
21.8795686675808,22.3782769609674,22.876985254354,23.3756935477406,23.8744018411273,
24.3731101345139,24.8718184279005,25.3705267212871,25.8692350146737,26.3679433080604,
26.866651601447,27.3653598948336,27.8640681882202,28.3627764816068,28.8614847749935,
29.3601930683801,29.8589013617667,30.3576096551533,30.8563179485399,31.3550262419266,
31.8537345353132,32.3524428286998,32.8511511220864,33.349859415473,33.8485677088597,
34.3472760022463,34.8459842956329,35.3446925890195,35.8434008824061,36.3421091757927,
36.8408174691794,37.339525762566,37.8382340559526,38.3369423493392,38.8356506427259,
39.3343589361125,39.8330672294991,40.3317755228857,40.8304838162723,41.3291921096589,
41.8279004030456,42.3266086964322,42.8253169898188,43.3240252832054,43.822733576592,
44.3214418699787,44.8201501633653,45.3188584567519,45.8175667501385,46.3162750435251,
46.8149833369118,47.3136916302984,47.812399923685,48.3111082170716,48.8098165104582,
49.3085248038449,49.8072330972315,50.3059413906181,50.8046496840047,51.3033579773913,
51.802066270778,52.3007745641646,52.7994828575512,53.2981911509378,53.7968994443244,
54.2956077377111,54.7943160310977,55.2930243244843,55.7917326178709,56.2904409112575,
56.7891492046442,57.2878574980308,57.7865657914174,58.285274084804,58.7839823781906,
59.2826906715772,59.7813989649639,60.2801072583505,60.7788155517371,61.2775238451237,
61.7762321385104,62.274940431897,62.7736487252836,63.2723570186702,63.7710653120568,
64.2697736054434,64.7684818988301,65.2671901922167,65.7658984856033,66.2646067789899,
66.7633150723765,67.2620233657632,67.7607316591498,68.2594399525364,68.758148245923,
69.2568565393096,69.7555648326963,70.2542731260829,70.7529814194695,71.2516897128561,
71.7503980062427,72.2491062996294,72.747814593016,73.2465228864026,73.7452311797892,
74.2439394731758,74.7426477665625,75.2413560599491,75.7400643533357,76.2387726467223,
76.7374809401089,77.2361892334956,77.7348975268822,78.2336058202688,78.7323141136554,
79.231022407042,79.7297307004287,80.2284389938153,80.7271472872019,81.2258555805885,
81.7245638739751,82.2232721673618,82.7219804607484,83.220688754135,83.7193970475216,
84.2181053409082,84.7168136342949,85.2155219276815,85.7142302210681,86.2129385144547,
86.7116468078413,87.2103551012279,87.7090633946146,88.2077716880012,88.7064799813878,
89.2051882747744,89.703896568161,90.2026048615477,90.7013131549343,91.2000214483209,
91.6987297417075,92.1974380350942,92.6961463284808,93.1948546218674,93.693562915254,
94.1922712086406,94.6909795020272,95.1896877954139,95.6883960888005,96.1871043821871,
96.6858126755737,97.1845209689603,97.683229262347,98.1819375557336,98.6806458491202,
99.1793541425068,99.6780624358935,100.17677072928,100.675479022667,101.174187316053,
101.67289560944,102.171603902827,102.670312196213,103.1690204896,103.667728782986,
104.166437076373,104.66514536976,105.163853663146,105.662561956533,106.161270249919,
106.659978543306,107.158686836693,107.657395130079,108.156103423466,108.654811716853,
109.153520010239,109.652228303626,110.150936597012,110.649644890399,111.148353183786,
111.647061477172,112.145769770559,112.644478063946,113.143186357332,113.641894650719,
114.140602944105,114.639311237492,115.138019530879,115.636727824265,116.135436117652,
116.634144411039,117.132852704425,117.631560997812,118.130269291198,118.628977584585,
119.127685877972,119.626394171358,120.125102464745,120.623810758131,121.122519051518,
121.621227344905,122.119935638291,122.618643931678,123.117352225065,123.616060518451,
124.114768811838,124.613477105224,125.112185398611,125.610893691998,126.109601985384,
126.608310278771,127.107018572158,127.605726865544,128.104435158931,128.603143452317,
129.101851745704,129.600560039091,130.099268332477,130.597976625864,131.09668491925,
131.595393212637,132.094101506024,132.59280979941,133.091518092797,133.590226386184,
134.08893467957,135.086351266343,136.083767853117,137.08118443989,138.078601026663,
139.076017613436,140.07343420021,141.070850786983,142.068267373756,143.065683960529,
144.063100547303,145.060517134076,146.057933720849,147.055350307622,148.052766894396,
148.551475187782,149.050183481169,149.548891774555,150.047600067942,150.546308361329,
151.045016654715,151.543724948102,152.042433241488,152.541141534875,153.039849828262,
153.538558121648,154.037266415035,154.535974708422,155.034683001808,155.533391295195,
156.032099588581,156.530807881968,157.029516175355,157.528224468741,158.026932762128,
158.525641055515,159.024349348901,159.523057642288,160.021765935674,160.520474229061,
161.019182522448,161.517890815834,162.016599109221,162.515307402608,163.014015695994,
163.512723989381,164.011432282767,164.510140576154,165.008848869541,165.507557162927,
166.006265456314,166.5049737497,167.003682043087,167.502390336474,168.00109862986,
168.499806923247,168.998515216634,169.49722351002,169.995931803407,170.494640096793,
170.99334839018,171.492056683567,171.990764976953,172.48947327034,172.988181563726,
173.486889857113,173.9855981505,174.484306443886,174.983014737273,175.48172303066,
175.980431324046,176.479139617433,176.977847910819,177.476556204206,177.975264497593,
178.473972790979,178.972681084366,179.471389377753,179.970097671139,180.468805964526,
180.967514257912,181.466222551299,181.964930844686,182.463639138072,182.962347431459,
183.461055724845,183.959764018232,184.458472311619,184.957180605005,185.455888898392,
185.954597191779,186.453305485165,186.952013778552,187.450722071938,187.949430365325,
188.448138658712,188.946846952098,189.445555245485,189.944263538872,190.442971832258,
190.941680125645,191.440388419031,191.939096712418,192.437805005805,192.936513299191,
193.435221592578,193.933929885965,194.432638179351,194.931346472738,195.430054766124,
195.928763059511,196.427471352898,196.926179646284,197.424887939671,197.923596233057,
198.422304526444,198.921012819831,199.419721113217,199.918429406604,200.417137699991,
200.915845993377,201.414554286764,201.91326258015,202.411970873537,202.910679166924,
203.40938746031,203.908095753697,204.406804047084,204.90551234047,205.404220633857,
205.902928927243,206.40163722063,206.900345514017,207.399053807403,207.89776210079,
208.396470394177,208.895178687563,209.39388698095,209.892595274336,210.391303567723,
210.89001186111,211.388720154496,211.887428447883,212.386136741269,212.884845034656,
213.383553328043,213.882261621429,214.380969914816,214.879678208203,215.378386501589,
215.877094794976,216.375803088362,216.874511381749,217.373219675136,217.871927968522,
218.370636261909,218.869344555295,219.368052848682,219.866761142069,220.365469435455,
220.864177728842,221.362886022229,221.861594315615,222.360302609002,222.859010902388,
223.357719195775,223.856427489162,224.355135782548,224.853844075935,225.352552369322,
225.851260662708,226.349968956095,226.848677249481,227.347385542868,227.846093836255,
228.344802129641,228.843510423028,229.342218716414,229.840927009801,230.339635303188,
230.838343596574,231.337051889961,231.835760183348,232.334468476734,232.833176770121,
233.331885063507,233.830593356894,234.329301650281,234.828009943667,235.326718237054,
235.825426530441,236.324134823827,236.822843117214,237.3215514106,237.820259703987,
238.318967997374,238.81767629076,239.316384584147,239.815092877534,240.31380117092,
240.812509464307,241.311217757693,241.80992605108,242.308634344467,242.807342637853,
243.30605093124,243.804759224626,244.303467518013,244.8021758114,245.300884104786,
245.799592398173,246.29830069156,246.797008984946,247.295717278333,247.794425571719,
248.293133865106,248.791842158493,249.290550451879,249.789258745266,250.287967038653,
250.786675332039,251.285383625426,251.784091918812,252.282800212199,252.781508505586,
253.280216798972,253.778925092359,254.277633385745,254.776341679132,255.275049972519,
255.773758265905,256.272466559292,256.771174852679,257.269883146065,257.768591439452,
258.267299732838,258.766008026225,259.264716319612,259.763424612998,260.262132906385,
260.760841199772,261.259549493158,261.758257786545,262.256966079931,262.755674373318,
263.254382666705,263.753090960091,264.251799253478,264.750507546865,265.249215840251,
265.747924133638,266.246632427024,266.745340720411,267.244049013798,267.742757307184),
 .UNSPECIFIED.);
#346=B_SPLINE_SURFACE_WITH_KNOTS('',3,3,((#49923,#49924,#49925,#49926,#49927,
#49928,#49929,#49930,#49931,#49932,#49933,#49934,#49935,#49936,#49937,#49938,
#49939,#49940,#49941,#49942,#49943,#49944,#49945,#49946,#49947,#49948,#49949,
#49950,#49951,#49952,#49953,#49954,#49955,#49956,#49957,#49958,#49959,#49960,
#49961,#49962,#49963,#49964,#49965,#49966,#49967,#49968,#49969,#49970,#49971,
#49972,#49973,#49974,#49975,#49976,#49977,#49978,#49979,#49980,#49981,#49982,
#49983,#49984,#49985,#49986,#49987,#49988,#49989,#49990,#49991,#49992,#49993,
#49994,#49995,#49996,#49997,#49998,#49999,#50000,#50001,#50002,#50003,#50004,
#50005,#50006,#50007,#50008,#50009,#50010,#50011,#50012,#50013,#50014,#50015,
#50016,#50017,#50018,#50019,#50020,#50021,#50022,#50023,#50024,#50025,#50026,
#50027,#50028,#50029,#50030,#50031,#50032,#50033,#50034,#50035,#50036,#50037,
#50038,#50039,#50040,#50041,#50042,#50043,#50044,#50045,#50046,#50047,#50048,
#50049,#50050,#50051,#50052,#50053,#50054,#50055,#50056,#50057,#50058,#50059,
#50060,#50061,#50062,#50063,#50064,#50065,#50066,#50067,#50068,#50069,#50070,
#50071,#50072,#50073,#50074,#50075,#50076,#50077,#50078,#50079,#50080,#50081,
#50082,#50083,#50084,#50085,#50086,#50087,#50088,#50089,#50090,#50091,#50092,
#50093,#50094,#50095,#50096,#50097,#50098,#50099,#50100,#50101,#50102,#50103,
#50104,#50105,#50106,#50107,#50108,#50109,#50110,#50111,#50112,#50113,#50114,
#50115,#50116,#50117,#50118,#50119,#50120,#50121,#50122,#50123,#50124,#50125,
#50126,#50127,#50128,#50129,#50130,#50131,#50132,#50133,#50134,#50135,#50136,
#50137,#50138,#50139,#50140,#50141,#50142,#50143,#50144,#50145,#50146,#50147,
#50148,#50149,#50150,#50151,#50152,#50153,#50154,#50155,#50156,#50157,#50158,
#50159,#50160,#50161,#50162,#50163,#50164,#50165,#50166,#50167,#50168,#50169,
#50170,#50171,#50172,#50173,#50174,#50175,#50176,#50177,#50178,#50179,#50180,
#50181,#50182,#50183,#50184,#50185,#50186,#50187,#50188,#50189,#50190,#50191,
#50192,#50193,#50194,#50195,#50196,#50197,#50198,#50199,#50200,#50201,#50202,
#50203,#50204,#50205,#50206,#50207,#50208,#50209,#50210,#50211,#50212,#50213,
#50214,#50215,#50216,#50217,#50218,#50219,#50220,#50221,#50222,#50223,#50224,
#50225,#50226,#50227,#50228,#50229,#50230,#50231,#50232,#50233,#50234,#50235,
#50236,#50237,#50238,#50239,#50240,#50241,#50242,#50243,#50244,#50245),
(#50246,#50247,#50248,#50249,#50250,#50251,#50252,#50253,#50254,#50255,
#50256,#50257,#50258,#50259,#50260,#50261,#50262,#50263,#50264,#50265,#50266,
#50267,#50268,#50269,#50270,#50271,#50272,#50273,#50274,#50275,#50276,#50277,
#50278,#50279,#50280,#50281,#50282,#50283,#50284,#50285,#50286,#50287,#50288,
#50289,#50290,#50291,#50292,#50293,#50294,#50295,#50296,#50297,#50298,#50299,
#50300,#50301,#50302,#50303,#50304,#50305,#50306,#50307,#50308,#50309,#50310,
#50311,#50312,#50313,#50314,#50315,#50316,#50317,#50318,#50319,#50320,#50321,
#50322,#50323,#50324,#50325,#50326,#50327,#50328,#50329,#50330,#50331,#50332,
#50333,#50334,#50335,#50336,#50337,#50338,#50339,#50340,#50341,#50342,#50343,
#50344,#50345,#50346,#50347,#50348,#50349,#50350,#50351,#50352,#50353,#50354,
#50355,#50356,#50357,#50358,#50359,#50360,#50361,#50362,#50363,#50364,#50365,
#50366,#50367,#50368,#50369,#50370,#50371,#50372,#50373,#50374,#50375,#50376,
#50377,#50378,#50379,#50380,#50381,#50382,#50383,#50384,#50385,#50386,#50387,
#50388,#50389,#50390,#50391,#50392,#50393,#50394,#50395,#50396,#50397,#50398,
#50399,#50400,#50401,#50402,#50403,#50404,#50405,#50406,#50407,#50408,#50409,
#50410,#50411,#50412,#50413,#50414,#50415,#50416,#50417,#50418,#50419,#50420,
#50421,#50422,#50423,#50424,#50425,#50426,#50427,#50428,#50429,#50430,#50431,
#50432,#50433,#50434,#50435,#50436,#50437,#50438,#50439,#50440,#50441,#50442,
#50443,#50444,#50445,#50446,#50447,#50448,#50449,#50450,#50451,#50452,#50453,
#50454,#50455,#50456,#50457,#50458,#50459,#50460,#50461,#50462,#50463,#50464,
#50465,#50466,#50467,#50468,#50469,#50470,#50471,#50472,#50473,#50474,#50475,
#50476,#50477,#50478,#50479,#50480,#50481,#50482,#50483,#50484,#50485,#50486,
#50487,#50488,#50489,#50490,#50491,#50492,#50493,#50494,#50495,#50496,#50497,
#50498,#50499,#50500,#50501,#50502,#50503,#50504,#50505,#50506,#50507,#50508,
#50509,#50510,#50511,#50512,#50513,#50514,#50515,#50516,#50517,#50518,#50519,
#50520,#50521,#50522,#50523,#50524,#50525,#50526,#50527,#50528,#50529,#50530,
#50531,#50532,#50533,#50534,#50535,#50536,#50537,#50538,#50539,#50540,#50541,
#50542,#50543,#50544,#50545,#50546,#50547,#50548,#50549,#50550,#50551,#50552,
#50553,#50554,#50555,#50556,#50557,#50558,#50559,#50560,#50561,#50562,#50563,
#50564,#50565,#50566,#50567,#50568),(#50569,#50570,#50571,#50572,#50573,
#50574,#50575,#50576,#50577,#50578,#50579,#50580,#50581,#50582,#50583,#50584,
#50585,#50586,#50587,#50588,#50589,#50590,#50591,#50592,#50593,#50594,#50595,
#50596,#50597,#50598,#50599,#50600,#50601,#50602,#50603,#50604,#50605,#50606,
#50607,#50608,#50609,#50610,#50611,#50612,#50613,#50614,#50615,#50616,#50617,
#50618,#50619,#50620,#50621,#50622,#50623,#50624,#50625,#50626,#50627,#50628,
#50629,#50630,#50631,#50632,#50633,#50634,#50635,#50636,#50637,#50638,#50639,
#50640,#50641,#50642,#50643,#50644,#50645,#50646,#50647,#50648,#50649,#50650,
#50651,#50652,#50653,#50654,#50655,#50656,#50657,#50658,#50659,#50660,#50661,
#50662,#50663,#50664,#50665,#50666,#50667,#50668,#50669,#50670,#50671,#50672,
#50673,#50674,#50675,#50676,#50677,#50678,#50679,#50680,#50681,#50682,#50683,
#50684,#50685,#50686,#50687,#50688,#50689,#50690,#50691,#50692,#50693,#50694,
#50695,#50696,#50697,#50698,#50699,#50700,#50701,#50702,#50703,#50704,#50705,
#50706,#50707,#50708,#50709,#50710,#50711,#50712,#50713,#50714,#50715,#50716,
#50717,#50718,#50719,#50720,#50721,#50722,#50723,#50724,#50725,#50726,#50727,
#50728,#50729,#50730,#50731,#50732,#50733,#50734,#50735,#50736,#50737,#50738,
#50739,#50740,#50741,#50742,#50743,#50744,#50745,#50746,#50747,#50748,#50749,
#50750,#50751,#50752,#50753,#50754,#50755,#50756,#50757,#50758,#50759,#50760,
#50761,#50762,#50763,#50764,#50765,#50766,#50767,#50768,#50769,#50770,#50771,
#50772,#50773,#50774,#50775,#50776,#50777,#50778,#50779,#50780,#50781,#50782,
#50783,#50784,#50785,#50786,#50787,#50788,#50789,#50790,#50791,#50792,#50793,
#50794,#50795,#50796,#50797,#50798,#50799,#50800,#50801,#50802,#50803,#50804,
#50805,#50806,#50807,#50808,#50809,#50810,#50811,#50812,#50813,#50814,#50815,
#50816,#50817,#50818,#50819,#50820,#50821,#50822,#50823,#50824,#50825,#50826,
#50827,#50828,#50829,#50830,#50831,#50832,#50833,#50834,#50835,#50836,#50837,
#50838,#50839,#50840,#50841,#50842,#50843,#50844,#50845,#50846,#50847,#50848,
#50849,#50850,#50851,#50852,#50853,#50854,#50855,#50856,#50857,#50858,#50859,
#50860,#50861,#50862,#50863,#50864,#50865,#50866,#50867,#50868,#50869,#50870,
#50871,#50872,#50873,#50874,#50875,#50876,#50877,#50878,#50879,#50880,#50881,
#50882,#50883,#50884,#50885,#50886,#50887,#50888,#50889,#50890,#50891),
(#50892,#50893,#50894,#50895,#50896,#50897,#50898,#50899,#50900,#50901,
#50902,#50903,#50904,#50905,#50906,#50907,#50908,#50909,#50910,#50911,#50912,
#50913,#50914,#50915,#50916,#50917,#50918,#50919,#50920,#50921,#50922,#50923,
#50924,#50925,#50926,#50927,#50928,#50929,#50930,#50931,#50932,#50933,#50934,
#50935,#50936,#50937,#50938,#50939,#50940,#50941,#50942,#50943,#50944,#50945,
#50946,#50947,#50948,#50949,#50950,#50951,#50952,#50953,#50954,#50955,#50956,
#50957,#50958,#50959,#50960,#50961,#50962,#50963,#50964,#50965,#50966,#50967,
#50968,#50969,#50970,#50971,#50972,#50973,#50974,#50975,#50976,#50977,#50978,
#50979,#50980,#50981,#50982,#50983,#50984,#50985,#50986,#50987,#50988,#50989,
#50990,#50991,#50992,#50993,#50994,#50995,#50996,#50997,#50998,#50999,#51000,
#51001,#51002,#51003,#51004,#51005,#51006,#51007,#51008,#51009,#51010,#51011,
#51012,#51013,#51014,#51015,#51016,#51017,#51018,#51019,#51020,#51021,#51022,
#51023,#51024,#51025,#51026,#51027,#51028,#51029,#51030,#51031,#51032,#51033,
#51034,#51035,#51036,#51037,#51038,#51039,#51040,#51041,#51042,#51043,#51044,
#51045,#51046,#51047,#51048,#51049,#51050,#51051,#51052,#51053,#51054,#51055,
#51056,#51057,#51058,#51059,#51060,#51061,#51062,#51063,#51064,#51065,#51066,
#51067,#51068,#51069,#51070,#51071,#51072,#51073,#51074,#51075,#51076,#51077,
#51078,#51079,#51080,#51081,#51082,#51083,#51084,#51085,#51086,#51087,#51088,
#51089,#51090,#51091,#51092,#51093,#51094,#51095,#51096,#51097,#51098,#51099,
#51100,#51101,#51102,#51103,#51104,#51105,#51106,#51107,#51108,#51109,#51110,
#51111,#51112,#51113,#51114,#51115,#51116,#51117,#51118,#51119,#51120,#51121,
#51122,#51123,#51124,#51125,#51126,#51127,#51128,#51129,#51130,#51131,#51132,
#51133,#51134,#51135,#51136,#51137,#51138,#51139,#51140,#51141,#51142,#51143,
#51144,#51145,#51146,#51147,#51148,#51149,#51150,#51151,#51152,#51153,#51154,
#51155,#51156,#51157,#51158,#51159,#51160,#51161,#51162,#51163,#51164,#51165,
#51166,#51167,#51168,#51169,#51170,#51171,#51172,#51173,#51174,#51175,#51176,
#51177,#51178,#51179,#51180,#51181,#51182,#51183,#51184,#51185,#51186,#51187,
#51188,#51189,#51190,#51191,#51192,#51193,#51194,#51195,#51196,#51197,#51198,
#51199,#51200,#51201,#51202,#51203,#51204,#51205,#51206,#51207,#51208,#51209,
#51210,#51211,#51212,#51213,#51214)),.UNSPECIFIED.,.F.,.F.,.F.,(4,4),(4,
1,1,1,1,1,1,1,1,1,1,1,1,1,1,1,1,1,1,1,1,1,1,1,1,1,1,1,1,1,1,1,1,1,1,1,1,
1,1,1,1,1,1,1,1,1,1,1,1,1,1,1,1,1,1,1,1,1,1,1,1,1,1,1,1,1,1,1,1,1,1,1,1,
1,1,1,1,1,1,1,1,1,1,1,1,1,1,1,1,1,1,1,1,1,1,1,1,1,1,1,1,1,1,1,1,1,1,1,1,
1,1,1,1,1,1,1,1,1,1,1,1,1,1,1,1,1,1,1,1,1,1,1,1,1,1,1,1,1,1,1,1,1,1,1,1,
1,1,1,1,1,1,1,1,1,1,1,1,1,1,1,1,1,1,1,1,1,1,1,1,1,1,1,1,1,1,1,1,1,1,1,1,
1,1,1,1,1,1,1,1,1,1,1,1,1,1,1,1,1,1,1,1,1,1,1,1,1,1,1,1,1,1,1,1,1,1,1,1,
1,1,1,1,1,1,1,1,1,1,1,1,1,1,1,1,1,1,1,1,1,1,1,1,1,1,1,1,1,1,1,1,1,1,1,1,
1,1,1,1,1,1,1,1,1,1,1,1,1,1,1,1,1,1,1,1,1,1,1,1,1,1,1,1,1,1,1,1,1,1,1,1,
1,1,1,1,1,1,1,1,1,1,1,1,1,1,1,1,1,1,1,1,1,1,1,1,1,1,1,1,1,1,1,4),(0.,0.0641840294258124),
(11.8589888623079,12.3561639667852,12.8533390712624,13.3505141757396,13.8476892802168,
14.344864384694,14.8420394891712,15.3392145936484,15.8363896981257,16.3335648026029,
16.8307399070801,17.3279150115573,17.8250901160345,18.3222652205117,18.8194403249889,
19.3166154294662,19.8137905339434,20.3109656384206,20.8081407428978,21.305315847375,
21.8024909518522,22.2996660563294,22.7968411608067,23.2940162652839,23.7911913697611,
24.2883664742383,24.7855415787155,25.2827166831927,25.7798917876699,26.2770668921472,
26.7742419966244,27.2714171011016,27.7685922055788,28.265767310056,28.7629424145332,
29.2601175190104,29.7572926234877,30.2544677279649,30.7516428324421,31.2488179369193,
31.7459930413965,32.2431681458737,32.7403432503509,33.2375183548282,33.7346934593054,
34.2318685637826,34.7290436682598,35.226218772737,35.7233938772142,36.2205689816915,
36.7177440861687,37.2149191906459,37.7120942951231,38.2092693996003,38.7064445040775,
39.2036196085547,39.700794713032,40.1979698175092,40.6951449219864,41.1923200264636,
41.6894951309408,42.186670235418,42.6838453398952,43.1810204443725,43.6781955488497,
44.1753706533269,44.6725457578041,45.1697208622813,45.6668959667585,46.1640710712357,
46.661246175713,47.1584212801902,47.6555963846674,48.1527714891446,48.6499465936218,
49.147121698099,49.6442968025762,50.1414719070535,50.6386470115307,51.1358221160079,
51.6329972204851,52.1301723249623,52.6273474294395,53.1245225339167,53.621697638394,
54.1188727428712,54.6160478473484,55.1132229518256,55.6103980563028,56.10757316078,
56.6047482652572,57.1019233697345,57.5990984742117,58.0962735786889,58.5934486831661,
59.0906237876433,59.5877988921205,60.0849739965977,60.582149101075,61.0793242055522,
61.5764993100294,62.0736744145066,62.5708495189838,63.068024623461,63.5651997279382,
64.0623748324155,64.5595499368927,65.0567250413699,65.5539001458471,66.0510752503243,
66.5482503548015,67.0454254592788,67.542600563756,68.0397756682332,68.5369507727104,
69.0341258771876,69.5313009816648,70.028476086142,70.5256511906192,71.0228262950965,
71.5200013995737,72.0171765040509,72.5143516085281,73.0115267130053,73.5087018174825,
74.0058769219598,74.503052026437,75.0002271309142,75.4974022353914,75.9945773398686,
76.4917524443458,76.988927548823,77.4861026533003,77.9832777577775,78.4804528622547,
78.9776279667319,79.4748030712091,79.9719781756863,80.4691532801635,80.9663283846407,
81.463503489118,81.9606785935952,82.4578536980724,82.9550288025496,83.4522039070268,
83.949379011504,84.4465541159813,84.9437292204585,85.4409043249357,85.9380794294129,
86.4352545338901,86.9324296383673,87.4296047428445,87.9267798473217,88.423954951799,
88.9211300562762,89.4183051607534,89.9154802652306,90.4126553697078,90.909830474185,
91.4070055786623,91.9041806831395,92.4013557876167,92.8985308920939,93.3957059965711,
93.8928811010483,94.3900562055255,94.8872313100028,95.38440641448,95.8815815189572,
96.3787566234344,96.8759317279116,97.3731068323888,97.870281936866,98.3674570413433,
98.8646321458205,99.3618072502977,99.8589823547749,100.356157459252,100.853332563729,
101.350507668207,101.847682772684,102.344857877161,102.842032981638,103.339208086115,
103.836383190593,104.33355829507,104.830733399547,105.327908504024,105.825083608501,
106.322258712979,106.819433817456,107.316608921933,107.81378402641,108.310959130888,
108.808134235365,109.305309339842,109.802484444319,110.299659548796,110.796834653274,
111.294009757751,111.791184862228,112.288359966705,112.785535071182,113.28271017566,
113.779885280137,114.277060384614,114.774235489091,115.271410593569,115.768585698046,
116.265760802523,116.762935907,117.260111011477,117.757286115955,118.254461220432,
118.751636324909,119.248811429386,119.745986533863,120.243161638341,120.740336742818,
121.237511847295,121.734686951772,122.23186205625,122.729037160727,123.226212265204,
123.723387369681,124.220562474158,124.717737578636,125.214912683113,125.71208778759,
126.209262892067,126.706437996544,127.203613101022,127.700788205499,128.197963309976,
128.695138414453,129.192313518931,129.689488623408,130.186663727885,130.683838832362,
131.181013936839,131.678189041317,132.175364145794,132.672539250271,133.169714354748,
133.666889459226,134.164064563703,134.66123966818,135.158414772657,135.655589877134,
136.152764981612,136.649940086089,137.147115190566,137.644290295043,138.14146539952,
138.638640503998,139.135815608475,139.632990712952,140.130165817429,140.627340921906,
141.124516026384,141.621691130861,142.118866235338,142.616041339815,143.113216444293,
143.61039154877,144.107566653247,144.604741757724,145.101916862201,145.599091966679,
146.096267071156,146.593442175633,147.09061728011,147.587792384587,148.084967489065,
148.582142593542,149.079317698019,149.576492802496,150.073667906974,150.570843011451,
151.068018115928,151.565193220405,152.062368324882,152.55954342936,153.056718533837,
153.553893638314,154.051068742791,154.548243847269,155.045418951746,155.542594056223,
156.0397691607,156.536944265177,157.034119369655,157.531294474132,158.028469578609,
158.525644683086,159.022819787563,159.519994892041,160.017169996518,160.514345100995,
161.011520205472,161.508695309949,162.005870414427,162.503045518904,163.000220623381,
163.497395727858,163.994570832336,164.491745936813,164.98892104129,165.486096145767,
165.983271250244,166.480446354722,166.977621459199,167.474796563676,167.971971668153,
168.46914677263,168.966321877108,169.463496981585,169.960672086062,170.457847190539,
170.955022295017),.UNSPECIFIED.);
#347=B_SPLINE_SURFACE_WITH_KNOTS('',3,3,((#51364,#51365,#51366,#51367,#51368,
#51369,#51370,#51371,#51372,#51373,#51374,#51375,#51376,#51377,#51378,#51379,
#51380,#51381,#51382,#51383,#51384,#51385,#51386,#51387,#51388,#51389,#51390,
#51391,#51392,#51393,#51394,#51395,#51396,#51397,#51398,#51399,#51400,#51401,
#51402,#51403,#51404,#51405,#51406,#51407,#51408,#51409,#51410,#51411,#51412,
#51413,#51414,#51415,#51416,#51417,#51418,#51419,#51420,#51421,#51422,#51423,
#51424,#51425,#51426,#51427,#51428,#51429,#51430,#51431,#51432,#51433,#51434,
#51435,#51436,#51437,#51438,#51439,#51440,#51441,#51442,#51443,#51444,#51445,
#51446,#51447,#51448,#51449,#51450,#51451,#51452,#51453,#51454,#51455,#51456,
#51457,#51458,#51459,#51460,#51461,#51462,#51463,#51464,#51465,#51466,#51467,
#51468,#51469,#51470,#51471,#51472,#51473,#51474,#51475,#51476,#51477,#51478,
#51479,#51480,#51481,#51482,#51483,#51484,#51485,#51486,#51487,#51488,#51489,
#51490,#51491,#51492,#51493,#51494,#51495,#51496,#51497,#51498,#51499,#51500,
#51501,#51502,#51503,#51504,#51505,#51506,#51507,#51508,#51509,#51510,#51511,
#51512,#51513,#51514,#51515,#51516,#51517,#51518,#51519,#51520,#51521,#51522,
#51523,#51524,#51525,#51526,#51527,#51528,#51529,#51530,#51531,#51532,#51533,
#51534,#51535,#51536,#51537,#51538,#51539,#51540,#51541,#51542,#51543,#51544,
#51545,#51546,#51547,#51548,#51549,#51550,#51551,#51552,#51553,#51554,#51555,
#51556,#51557,#51558,#51559,#51560,#51561,#51562,#51563,#51564,#51565,#51566,
#51567,#51568,#51569,#51570,#51571,#51572,#51573,#51574,#51575,#51576,#51577,
#51578,#51579,#51580,#51581,#51582,#51583,#51584,#51585,#51586,#51587,#51588,
#51589,#51590,#51591,#51592,#51593,#51594,#51595,#51596,#51597,#51598,#51599,
#51600,#51601,#51602,#51603,#51604,#51605,#51606,#51607,#51608,#51609,#51610,
#51611,#51612,#51613,#51614,#51615,#51616,#51617,#51618,#51619,#51620,#51621,
#51622,#51623,#51624,#51625,#51626,#51627,#51628,#51629,#51630,#51631,#51632,
#51633,#51634,#51635,#51636,#51637,#51638,#51639,#51640,#51641,#51642,#51643,
#51644,#51645,#51646,#51647,#51648,#51649,#51650,#51651,#51652,#51653,#51654,
#51655,#51656,#51657,#51658,#51659,#51660,#51661,#51662,#51663,#51664,#51665,
#51666,#51667,#51668,#51669,#51670,#51671,#51672,#51673,#51674,#51675,#51676,
#51677,#51678,#51679,#51680,#51681,#51682,#51683,#51684,#51685,#51686),
(#51687,#51688,#51689,#51690,#51691,#51692,#51693,#51694,#51695,#51696,
#51697,#51698,#51699,#51700,#51701,#51702,#51703,#51704,#51705,#51706,#51707,
#51708,#51709,#51710,#51711,#51712,#51713,#51714,#51715,#51716,#51717,#51718,
#51719,#51720,#51721,#51722,#51723,#51724,#51725,#51726,#51727,#51728,#51729,
#51730,#51731,#51732,#51733,#51734,#51735,#51736,#51737,#51738,#51739,#51740,
#51741,#51742,#51743,#51744,#51745,#51746,#51747,#51748,#51749,#51750,#51751,
#51752,#51753,#51754,#51755,#51756,#51757,#51758,#51759,#51760,#51761,#51762,
#51763,#51764,#51765,#51766,#51767,#51768,#51769,#51770,#51771,#51772,#51773,
#51774,#51775,#51776,#51777,#51778,#51779,#51780,#51781,#51782,#51783,#51784,
#51785,#51786,#51787,#51788,#51789,#51790,#51791,#51792,#51793,#51794,#51795,
#51796,#51797,#51798,#51799,#51800,#51801,#51802,#51803,#51804,#51805,#51806,
#51807,#51808,#51809,#51810,#51811,#51812,#51813,#51814,#51815,#51816,#51817,
#51818,#51819,#51820,#51821,#51822,#51823,#51824,#51825,#51826,#51827,#51828,
#51829,#51830,#51831,#51832,#51833,#51834,#51835,#51836,#51837,#51838,#51839,
#51840,#51841,#51842,#51843,#51844,#51845,#51846,#51847,#51848,#51849,#51850,
#51851,#51852,#51853,#51854,#51855,#51856,#51857,#51858,#51859,#51860,#51861,
#51862,#51863,#51864,#51865,#51866,#51867,#51868,#51869,#51870,#51871,#51872,
#51873,#51874,#51875,#51876,#51877,#51878,#51879,#51880,#51881,#51882,#51883,
#51884,#51885,#51886,#51887,#51888,#51889,#51890,#51891,#51892,#51893,#51894,
#51895,#51896,#51897,#51898,#51899,#51900,#51901,#51902,#51903,#51904,#51905,
#51906,#51907,#51908,#51909,#51910,#51911,#51912,#51913,#51914,#51915,#51916,
#51917,#51918,#51919,#51920,#51921,#51922,#51923,#51924,#51925,#51926,#51927,
#51928,#51929,#51930,#51931,#51932,#51933,#51934,#51935,#51936,#51937,#51938,
#51939,#51940,#51941,#51942,#51943,#51944,#51945,#51946,#51947,#51948,#51949,
#51950,#51951,#51952,#51953,#51954,#51955,#51956,#51957,#51958,#51959,#51960,
#51961,#51962,#51963,#51964,#51965,#51966,#51967,#51968,#51969,#51970,#51971,
#51972,#51973,#51974,#51975,#51976,#51977,#51978,#51979,#51980,#51981,#51982,
#51983,#51984,#51985,#51986,#51987,#51988,#51989,#51990,#51991,#51992,#51993,
#51994,#51995,#51996,#51997,#51998,#51999,#52000,#52001,#52002,#52003,#52004,
#52005,#52006,#52007,#52008,#52009),(#52010,#52011,#52012,#52013,#52014,
#52015,#52016,#52017,#52018,#52019,#52020,#52021,#52022,#52023,#52024,#52025,
#52026,#52027,#52028,#52029,#52030,#52031,#52032,#52033,#52034,#52035,#52036,
#52037,#52038,#52039,#52040,#52041,#52042,#52043,#52044,#52045,#52046,#52047,
#52048,#52049,#52050,#52051,#52052,#52053,#52054,#52055,#52056,#52057,#52058,
#52059,#52060,#52061,#52062,#52063,#52064,#52065,#52066,#52067,#52068,#52069,
#52070,#52071,#52072,#52073,#52074,#52075,#52076,#52077,#52078,#52079,#52080,
#52081,#52082,#52083,#52084,#52085,#52086,#52087,#52088,#52089,#52090,#52091,
#52092,#52093,#52094,#52095,#52096,#52097,#52098,#52099,#52100,#52101,#52102,
#52103,#52104,#52105,#52106,#52107,#52108,#52109,#52110,#52111,#52112,#52113,
#52114,#52115,#52116,#52117,#52118,#52119,#52120,#52121,#52122,#52123,#52124,
#52125,#52126,#52127,#52128,#52129,#52130,#52131,#52132,#52133,#52134,#52135,
#52136,#52137,#52138,#52139,#52140,#52141,#52142,#52143,#52144,#52145,#52146,
#52147,#52148,#52149,#52150,#52151,#52152,#52153,#52154,#52155,#52156,#52157,
#52158,#52159,#52160,#52161,#52162,#52163,#52164,#52165,#52166,#52167,#52168,
#52169,#52170,#52171,#52172,#52173,#52174,#52175,#52176,#52177,#52178,#52179,
#52180,#52181,#52182,#52183,#52184,#52185,#52186,#52187,#52188,#52189,#52190,
#52191,#52192,#52193,#52194,#52195,#52196,#52197,#52198,#52199,#52200,#52201,
#52202,#52203,#52204,#52205,#52206,#52207,#52208,#52209,#52210,#52211,#52212,
#52213,#52214,#52215,#52216,#52217,#52218,#52219,#52220,#52221,#52222,#52223,
#52224,#52225,#52226,#52227,#52228,#52229,#52230,#52231,#52232,#52233,#52234,
#52235,#52236,#52237,#52238,#52239,#52240,#52241,#52242,#52243,#52244,#52245,
#52246,#52247,#52248,#52249,#52250,#52251,#52252,#52253,#52254,#52255,#52256,
#52257,#52258,#52259,#52260,#52261,#52262,#52263,#52264,#52265,#52266,#52267,
#52268,#52269,#52270,#52271,#52272,#52273,#52274,#52275,#52276,#52277,#52278,
#52279,#52280,#52281,#52282,#52283,#52284,#52285,#52286,#52287,#52288,#52289,
#52290,#52291,#52292,#52293,#52294,#52295,#52296,#52297,#52298,#52299,#52300,
#52301,#52302,#52303,#52304,#52305,#52306,#52307,#52308,#52309,#52310,#52311,
#52312,#52313,#52314,#52315,#52316,#52317,#52318,#52319,#52320,#52321,#52322,
#52323,#52324,#52325,#52326,#52327,#52328,#52329,#52330,#52331,#52332),
(#52333,#52334,#52335,#52336,#52337,#52338,#52339,#52340,#52341,#52342,
#52343,#52344,#52345,#52346,#52347,#52348,#52349,#52350,#52351,#52352,#52353,
#52354,#52355,#52356,#52357,#52358,#52359,#52360,#52361,#52362,#52363,#52364,
#52365,#52366,#52367,#52368,#52369,#52370,#52371,#52372,#52373,#52374,#52375,
#52376,#52377,#52378,#52379,#52380,#52381,#52382,#52383,#52384,#52385,#52386,
#52387,#52388,#52389,#52390,#52391,#52392,#52393,#52394,#52395,#52396,#52397,
#52398,#52399,#52400,#52401,#52402,#52403,#52404,#52405,#52406,#52407,#52408,
#52409,#52410,#52411,#52412,#52413,#52414,#52415,#52416,#52417,#52418,#52419,
#52420,#52421,#52422,#52423,#52424,#52425,#52426,#52427,#52428,#52429,#52430,
#52431,#52432,#52433,#52434,#52435,#52436,#52437,#52438,#52439,#52440,#52441,
#52442,#52443,#52444,#52445,#52446,#52447,#52448,#52449,#52450,#52451,#52452,
#52453,#52454,#52455,#52456,#52457,#52458,#52459,#52460,#52461,#52462,#52463,
#52464,#52465,#52466,#52467,#52468,#52469,#52470,#52471,#52472,#52473,#52474,
#52475,#52476,#52477,#52478,#52479,#52480,#52481,#52482,#52483,#52484,#52485,
#52486,#52487,#52488,#52489,#52490,#52491,#52492,#52493,#52494,#52495,#52496,
#52497,#52498,#52499,#52500,#52501,#52502,#52503,#52504,#52505,#52506,#52507,
#52508,#52509,#52510,#52511,#52512,#52513,#52514,#52515,#52516,#52517,#52518,
#52519,#52520,#52521,#52522,#52523,#52524,#52525,#52526,#52527,#52528,#52529,
#52530,#52531,#52532,#52533,#52534,#52535,#52536,#52537,#52538,#52539,#52540,
#52541,#52542,#52543,#52544,#52545,#52546,#52547,#52548,#52549,#52550,#52551,
#52552,#52553,#52554,#52555,#52556,#52557,#52558,#52559,#52560,#52561,#52562,
#52563,#52564,#52565,#52566,#52567,#52568,#52569,#52570,#52571,#52572,#52573,
#52574,#52575,#52576,#52577,#52578,#52579,#52580,#52581,#52582,#52583,#52584,
#52585,#52586,#52587,#52588,#52589,#52590,#52591,#52592,#52593,#52594,#52595,
#52596,#52597,#52598,#52599,#52600,#52601,#52602,#52603,#52604,#52605,#52606,
#52607,#52608,#52609,#52610,#52611,#52612,#52613,#52614,#52615,#52616,#52617,
#52618,#52619,#52620,#52621,#52622,#52623,#52624,#52625,#52626,#52627,#52628,
#52629,#52630,#52631,#52632,#52633,#52634,#52635,#52636,#52637,#52638,#52639,
#52640,#52641,#52642,#52643,#52644,#52645,#52646,#52647,#52648,#52649,#52650,
#52651,#52652,#52653,#52654,#52655)),.UNSPECIFIED.,.F.,.F.,.F.,(4,4),(4,
1,1,1,1,1,1,1,1,1,1,1,1,1,1,1,1,1,1,1,1,1,1,1,1,1,1,1,1,1,1,1,1,1,1,1,1,
1,1,1,1,1,1,1,1,1,1,1,1,1,1,1,1,1,1,1,1,1,1,1,1,1,1,1,1,1,1,1,1,1,1,1,1,
1,1,1,1,1,1,1,1,1,1,1,1,1,1,1,1,1,1,1,1,1,1,1,1,1,1,1,1,1,1,1,1,1,1,1,1,
1,1,1,1,1,1,1,1,1,1,1,1,1,1,1,1,1,1,1,1,1,1,1,1,1,1,1,1,1,1,1,1,1,1,1,1,
1,1,1,1,1,1,1,1,1,1,1,1,1,1,1,1,1,1,1,1,1,1,1,1,1,1,1,1,1,1,1,1,1,1,1,1,
1,1,1,1,1,1,1,1,1,1,1,1,1,1,1,1,1,1,1,1,1,1,1,1,1,1,1,1,1,1,1,1,1,1,1,1,
1,1,1,1,1,1,1,1,1,1,1,1,1,1,1,1,1,1,1,1,1,1,1,1,1,1,1,1,1,1,1,1,1,1,1,1,
1,1,1,1,1,1,1,1,1,1,1,1,1,1,1,1,1,1,1,1,1,1,1,1,1,1,1,1,1,1,1,1,1,1,1,1,
1,1,1,1,1,1,1,1,1,1,1,1,1,1,1,1,1,1,1,1,1,1,1,1,1,1,1,1,1,1,1,4),(0.,0.0641840294258124),
(14.398944266781,14.8961193712582,15.3932944757354,15.8904695802126,16.3876446846898,
16.884819789167,17.3819948936443,17.8791699981215,18.3763451025987,18.8735202070759,
19.3706953115531,19.8678704160303,20.3650455205075,20.8622206249848,21.359395729462,
21.8565708339392,22.3537459384164,22.8509210428936,23.3480961473708,23.845271251848,
24.3424463563253,24.8396214608025,25.3367965652797,25.8339716697569,26.3311467742341,
26.8283218787113,27.3254969831885,27.8226720876658,28.319847192143,28.8170222966202,
29.3141974010974,29.8113725055746,30.3085476100518,30.805722714529,31.3028978190063,
31.8000729234835,32.2972480279607,32.7944231324379,33.2915982369151,33.7887733413923,
34.2859484458695,34.7831235503468,35.280298654824,35.7774737593012,36.2746488637784,
36.7718239682556,37.2689990727328,37.76617417721,38.2633492816873,38.7605243861645,
39.2576994906417,39.7548745951189,40.2520496995961,40.7492248040733,41.2463999085505,
41.7435750130278,42.240750117505,42.7379252219822,43.2351003264594,43.7322754309366,
44.2294505354138,44.726625639891,45.2238007443683,45.7209758488455,46.2181509533227,
46.7153260577999,47.2125011622771,47.7096762667543,48.2068513712315,48.7040264757088,
49.201201580186,49.6983766846632,50.1955517891404,50.6927268936176,51.1899019980948,
51.687077102572,52.1842522070493,52.6814273115265,53.1786024160037,53.6757775204809,
54.1729526249581,54.6701277294353,55.1673028339125,55.6644779383898,56.161653042867,
56.6588281473442,57.1560032518214,57.6531783562986,58.1503534607758,58.647528565253,
59.1447036697303,59.6418787742075,60.1390538786847,60.6362289831619,61.1334040876391,
61.6305791921163,62.1277542965935,62.6249294010708,63.122104505548,63.6192796100252,
64.1164547145024,64.6136298189796,65.1108049234568,65.607980027934,66.1051551324113,
66.6023302368885,67.0995053413657,67.5966804458429,68.0938555503201,68.5910306547973,
69.0882057592745,69.5853808637518,70.082555968229,70.5797310727062,71.0769061771834,
71.5740812816606,72.0712563861378,72.568431490615,73.0656065950923,73.5627816995695,
74.0599568040467,74.5571319085239,75.0543070130011,75.5514821174783,76.0486572219556,
76.5458323264328,77.04300743091,77.5401825353872,78.0373576398644,78.5345327443416,
79.0317078488188,79.528882953296,80.0260580577733,80.5232331622505,81.0204082667277,
81.5175833712049,82.0147584756821,82.5119335801593,83.0091086846365,83.5062837891138,
84.003458893591,84.5006339980682,84.9978091025454,85.4949842070226,85.9921593114998,
86.4893344159771,86.9865095204543,87.4836846249315,87.9808597294087,88.4780348338859,
88.9752099383631,89.4723850428403,89.9695601473175,90.4667352517948,90.963910356272,
91.4610854607492,91.9582605652264,92.4554356697036,92.9526107741808,93.449785878658,
93.9469609831353,94.4441360876125,94.9413111920897,95.4384862965669,95.9356614010441,
96.4328365055213,96.9300116099986,97.4271867144758,97.924361818953,98.4215369234302,
98.9187120279074,99.4158871323846,99.9130622368618,100.410237341339,100.907412445816,
101.404587550293,101.901762654771,102.398937759248,102.896112863725,103.393287968202,
103.89046307268,104.387638177157,104.884813281634,105.381988386111,105.879163490588,
106.376338595066,106.873513699543,107.37068880402,107.867863908497,108.365039012974,
108.862214117452,109.359389221929,109.856564326406,110.353739430883,110.850914535361,
111.348089639838,111.845264744315,112.342439848792,112.839614953269,113.336790057747,
113.833965162224,114.331140266701,114.828315371178,115.325490475655,115.822665580133,
116.31984068461,116.817015789087,117.314190893564,117.811365998042,118.308541102519,
118.805716206996,119.302891311473,119.80006641595,120.297241520428,120.794416624905,
121.291591729382,121.788766833859,122.285941938336,122.783117042814,123.280292147291,
123.777467251768,124.274642356245,124.771817460723,125.2689925652,125.766167669677,
126.263342774154,126.760517878631,127.257692983109,127.754868087586,128.252043192063,
128.74921829654,129.246393401017,129.743568505495,130.240743609972,130.737918714449,
131.235093818926,131.732268923404,132.229444027881,132.726619132358,133.223794236835,
133.720969341312,134.21814444579,134.715319550267,135.212494654744,135.709669759221,
136.206844863698,136.704019968176,137.201195072653,137.69837017713,138.195545281607,
138.692720386085,139.189895490562,139.687070595039,140.184245699516,140.681420803993,
141.178595908471,141.675771012948,142.172946117425,142.670121221902,143.167296326379,
143.664471430857,144.161646535334,144.658821639811,145.155996744288,145.653171848766,
146.150346953243,146.64752205772,147.144697162197,147.641872266674,148.139047371152,
148.636222475629,149.133397580106,149.630572684583,150.12774778906,150.624922893538,
151.122097998015,151.619273102492,152.116448206969,152.613623311447,153.110798415924,
153.607973520401,154.105148624878,154.602323729355,155.099498833833,155.59667393831,
156.093849042787,156.591024147264,157.088199251742,157.585374356219,158.082549460696,
158.579724565173,159.07689966965,159.574074774128,160.071249878605,160.568424983082,
161.065600087559,161.562775192036,162.059950296514,162.557125400991,163.054300505468,
163.551475609945,164.048650714422,164.5458258189,165.043000923377,165.540176027854,
166.037351132331,166.534526236809,167.031701341286,167.528876445763,168.02605155024,
168.523226654717,169.020401759195,169.517576863672,170.014751968149,170.511927072626,
171.009102177104,171.506277281581,172.003452386058,172.500627490535,172.997802595012,
173.49497769949),.UNSPECIFIED.);
#348=B_SPLINE_SURFACE_WITH_KNOTS('',3,3,((#55084,#55085,#55086,#55087,#55088,
#55089,#55090,#55091,#55092,#55093,#55094,#55095,#55096,#55097,#55098,#55099,
#55100,#55101,#55102,#55103,#55104,#55105,#55106,#55107,#55108,#55109,#55110,
#55111,#55112,#55113,#55114,#55115,#55116,#55117,#55118,#55119,#55120,#55121,
#55122,#55123,#55124,#55125,#55126,#55127,#55128,#55129,#55130,#55131,#55132,
#55133,#55134,#55135,#55136,#55137,#55138,#55139,#55140,#55141,#55142,#55143,
#55144,#55145,#55146,#55147,#55148,#55149,#55150,#55151,#55152,#55153,#55154,
#55155,#55156,#55157,#55158,#55159,#55160,#55161,#55162,#55163,#55164,#55165,
#55166,#55167,#55168,#55169,#55170,#55171,#55172,#55173,#55174,#55175,#55176,
#55177,#55178,#55179,#55180,#55181,#55182,#55183,#55184,#55185,#55186,#55187,
#55188,#55189,#55190,#55191,#55192,#55193,#55194,#55195,#55196,#55197,#55198,
#55199,#55200,#55201,#55202,#55203,#55204,#55205,#55206,#55207,#55208,#55209,
#55210,#55211,#55212),(#55213,#55214,#55215,#55216,#55217,#55218,#55219,
#55220,#55221,#55222,#55223,#55224,#55225,#55226,#55227,#55228,#55229,#55230,
#55231,#55232,#55233,#55234,#55235,#55236,#55237,#55238,#55239,#55240,#55241,
#55242,#55243,#55244,#55245,#55246,#55247,#55248,#55249,#55250,#55251,#55252,
#55253,#55254,#55255,#55256,#55257,#55258,#55259,#55260,#55261,#55262,#55263,
#55264,#55265,#55266,#55267,#55268,#55269,#55270,#55271,#55272,#55273,#55274,
#55275,#55276,#55277,#55278,#55279,#55280,#55281,#55282,#55283,#55284,#55285,
#55286,#55287,#55288,#55289,#55290,#55291,#55292,#55293,#55294,#55295,#55296,
#55297,#55298,#55299,#55300,#55301,#55302,#55303,#55304,#55305,#55306,#55307,
#55308,#55309,#55310,#55311,#55312,#55313,#55314,#55315,#55316,#55317,#55318,
#55319,#55320,#55321,#55322,#55323,#55324,#55325,#55326,#55327,#55328,#55329,
#55330,#55331,#55332,#55333,#55334,#55335,#55336,#55337,#55338,#55339,#55340,
#55341),(#55342,#55343,#55344,#55345,#55346,#55347,#55348,#55349,#55350,
#55351,#55352,#55353,#55354,#55355,#55356,#55357,#55358,#55359,#55360,#55361,
#55362,#55363,#55364,#55365,#55366,#55367,#55368,#55369,#55370,#55371,#55372,
#55373,#55374,#55375,#55376,#55377,#55378,#55379,#55380,#55381,#55382,#55383,
#55384,#55385,#55386,#55387,#55388,#55389,#55390,#55391,#55392,#55393,#55394,
#55395,#55396,#55397,#55398,#55399,#55400,#55401,#55402,#55403,#55404,#55405,
#55406,#55407,#55408,#55409,#55410,#55411,#55412,#55413,#55414,#55415,#55416,
#55417,#55418,#55419,#55420,#55421,#55422,#55423,#55424,#55425,#55426,#55427,
#55428,#55429,#55430,#55431,#55432,#55433,#55434,#55435,#55436,#55437,#55438,
#55439,#55440,#55441,#55442,#55443,#55444,#55445,#55446,#55447,#55448,#55449,
#55450,#55451,#55452,#55453,#55454,#55455,#55456,#55457,#55458,#55459,#55460,
#55461,#55462,#55463,#55464,#55465,#55466,#55467,#55468,#55469,#55470),
(#55471,#55472,#55473,#55474,#55475,#55476,#55477,#55478,#55479,#55480,
#55481,#55482,#55483,#55484,#55485,#55486,#55487,#55488,#55489,#55490,#55491,
#55492,#55493,#55494,#55495,#55496,#55497,#55498,#55499,#55500,#55501,#55502,
#55503,#55504,#55505,#55506,#55507,#55508,#55509,#55510,#55511,#55512,#55513,
#55514,#55515,#55516,#55517,#55518,#55519,#55520,#55521,#55522,#55523,#55524,
#55525,#55526,#55527,#55528,#55529,#55530,#55531,#55532,#55533,#55534,#55535,
#55536,#55537,#55538,#55539,#55540,#55541,#55542,#55543,#55544,#55545,#55546,
#55547,#55548,#55549,#55550,#55551,#55552,#55553,#55554,#55555,#55556,#55557,
#55558,#55559,#55560,#55561,#55562,#55563,#55564,#55565,#55566,#55567,#55568,
#55569,#55570,#55571,#55572,#55573,#55574,#55575,#55576,#55577,#55578,#55579,
#55580,#55581,#55582,#55583,#55584,#55585,#55586,#55587,#55588,#55589,#55590,
#55591,#55592,#55593,#55594,#55595,#55596,#55597,#55598,#55599)),
 .UNSPECIFIED.,.F.,.F.,.F.,(4,4),(4,1,1,1,1,1,1,1,1,1,1,1,1,1,1,1,1,1,1,
1,1,1,1,1,1,1,1,1,1,1,1,1,1,1,1,1,1,1,1,1,1,1,1,1,1,1,1,1,1,1,1,1,1,1,1,
1,1,1,1,1,1,1,1,1,1,1,1,1,1,1,1,1,1,1,1,1,1,1,1,1,1,1,1,1,1,1,1,1,1,1,1,
1,1,1,1,1,1,1,1,1,1,1,1,1,1,1,1,1,1,1,1,1,1,1,1,1,1,1,1,1,1,1,1,1,1,1,4),
(0.,0.0658179306876173),(11.6150328478182,12.1123165623719,12.6096002769257,
13.6041677060331,14.5987351351405,15.5933025642479,16.5878699933554,17.5824374224628,
18.5770048515702,19.5715722806776,20.5661397097851,21.5607071388925,22.5552745679999,
23.5498419971074,24.5444094262148,25.5389768553222,26.5335442844296,27.5281117135371,
28.5226791426445,29.5172465717519,30.5118140008593,31.5063814299668,32.5009488590742,
33.4955162881816,34.490083717289,35.4846511463965,36.4792185755039,37.4737860046113,
38.4683534337187,39.4629208628262,40.4574882919336,41.452055721041,42.4466231501485,
43.4411905792559,44.4357580083633,45.4303254374707,46.4248928665782,47.4194602956856,
48.414027724793,49.4085951539004,50.4031625830079,51.3977300121153,52.3922974412227,
53.3868648703302,54.3814322994376,55.375999728545,56.3705671576524,57.3651345867599,
58.3597020158673,59.3542694449747,60.3488368740821,61.3434043031896,62.337971732297,
63.3325391614044,64.3271065905118,65.3216740196193,66.3162414487267,67.3108088778341,
68.3053763069416,69.299943736049,70.2945111651564,71.2890785942638,72.2836460233713,
73.2782134524787,74.2727808815861,75.2673483106935,76.261915739801,77.2564831689084,
78.2510505980158,79.2456180271232,80.2401854562307,81.2347528853381,82.2293203144455,
83.223887743553,84.2184551726604,85.2130226017678,86.2075900308752,87.2021574599827,
88.1967248890901,89.1912923181975,90.1858597473049,91.1804271764124,92.1749946055198,
93.1695620346272,94.1641294637347,95.1586968928421,96.1532643219495,97.1478317510569,
98.1423991801644,99.1369666092718,100.131534038379,101.126101467487,102.120668896594,
103.115236325701,104.109803754809,105.104371183916,106.098938613024,107.093506042131,
108.088073471239,109.082640900346,110.077208329453,111.071775758561,112.066343187668,
113.060910616776,114.055478045883,115.050045474991,116.044612904098,117.039180333205,
118.033747762313,119.02831519142,120.022882620528,121.017450049635,122.012017478743,
123.00658490785,124.001152336957,124.995719766065,125.990287195172,126.98485462428,
127.979422053387,128.973989482495,129.968556911602,130.963124340709,131.957691769817,
132.952259198924,133.946826628032,134.444110342585,134.941394057139),
 .UNSPECIFIED.);
#349=B_SPLINE_SURFACE_WITH_KNOTS('',3,3,((#55744,#55745,#55746,#55747,#55748,
#55749,#55750,#55751,#55752,#55753,#55754,#55755,#55756,#55757,#55758,#55759,
#55760,#55761,#55762,#55763,#55764,#55765,#55766,#55767,#55768,#55769,#55770,
#55771,#55772,#55773,#55774,#55775,#55776,#55777,#55778,#55779,#55780,#55781,
#55782,#55783,#55784,#55785,#55786,#55787,#55788,#55789,#55790,#55791,#55792,
#55793,#55794,#55795,#55796,#55797,#55798,#55799,#55800,#55801,#55802,#55803,
#55804,#55805,#55806,#55807,#55808,#55809,#55810,#55811,#55812,#55813,#55814,
#55815,#55816,#55817,#55818,#55819,#55820,#55821,#55822,#55823,#55824,#55825,
#55826,#55827,#55828,#55829,#55830,#55831,#55832,#55833,#55834,#55835,#55836,
#55837,#55838,#55839,#55840,#55841,#55842,#55843,#55844,#55845,#55846,#55847,
#55848,#55849,#55850,#55851,#55852,#55853,#55854,#55855,#55856,#55857,#55858,
#55859,#55860,#55861,#55862,#55863,#55864,#55865,#55866,#55867,#55868,#55869,
#55870,#55871,#55872,#55873,#55874),(#55875,#55876,#55877,#55878,#55879,
#55880,#55881,#55882,#55883,#55884,#55885,#55886,#55887,#55888,#55889,#55890,
#55891,#55892,#55893,#55894,#55895,#55896,#55897,#55898,#55899,#55900,#55901,
#55902,#55903,#55904,#55905,#55906,#55907,#55908,#55909,#55910,#55911,#55912,
#55913,#55914,#55915,#55916,#55917,#55918,#55919,#55920,#55921,#55922,#55923,
#55924,#55925,#55926,#55927,#55928,#55929,#55930,#55931,#55932,#55933,#55934,
#55935,#55936,#55937,#55938,#55939,#55940,#55941,#55942,#55943,#55944,#55945,
#55946,#55947,#55948,#55949,#55950,#55951,#55952,#55953,#55954,#55955,#55956,
#55957,#55958,#55959,#55960,#55961,#55962,#55963,#55964,#55965,#55966,#55967,
#55968,#55969,#55970,#55971,#55972,#55973,#55974,#55975,#55976,#55977,#55978,
#55979,#55980,#55981,#55982,#55983,#55984,#55985,#55986,#55987,#55988,#55989,
#55990,#55991,#55992,#55993,#55994,#55995,#55996,#55997,#55998,#55999,#56000,
#56001,#56002,#56003,#56004,#56005),(#56006,#56007,#56008,#56009,#56010,
#56011,#56012,#56013,#56014,#56015,#56016,#56017,#56018,#56019,#56020,#56021,
#56022,#56023,#56024,#56025,#56026,#56027,#56028,#56029,#56030,#56031,#56032,
#56033,#56034,#56035,#56036,#56037,#56038,#56039,#56040,#56041,#56042,#56043,
#56044,#56045,#56046,#56047,#56048,#56049,#56050,#56051,#56052,#56053,#56054,
#56055,#56056,#56057,#56058,#56059,#56060,#56061,#56062,#56063,#56064,#56065,
#56066,#56067,#56068,#56069,#56070,#56071,#56072,#56073,#56074,#56075,#56076,
#56077,#56078,#56079,#56080,#56081,#56082,#56083,#56084,#56085,#56086,#56087,
#56088,#56089,#56090,#56091,#56092,#56093,#56094,#56095,#56096,#56097,#56098,
#56099,#56100,#56101,#56102,#56103,#56104,#56105,#56106,#56107,#56108,#56109,
#56110,#56111,#56112,#56113,#56114,#56115,#56116,#56117,#56118,#56119,#56120,
#56121,#56122,#56123,#56124,#56125,#56126,#56127,#56128,#56129,#56130,#56131,
#56132,#56133,#56134,#56135,#56136),(#56137,#56138,#56139,#56140,#56141,
#56142,#56143,#56144,#56145,#56146,#56147,#56148,#56149,#56150,#56151,#56152,
#56153,#56154,#56155,#56156,#56157,#56158,#56159,#56160,#56161,#56162,#56163,
#56164,#56165,#56166,#56167,#56168,#56169,#56170,#56171,#56172,#56173,#56174,
#56175,#56176,#56177,#56178,#56179,#56180,#56181,#56182,#56183,#56184,#56185,
#56186,#56187,#56188,#56189,#56190,#56191,#56192,#56193,#56194,#56195,#56196,
#56197,#56198,#56199,#56200,#56201,#56202,#56203,#56204,#56205,#56206,#56207,
#56208,#56209,#56210,#56211,#56212,#56213,#56214,#56215,#56216,#56217,#56218,
#56219,#56220,#56221,#56222,#56223,#56224,#56225,#56226,#56227,#56228,#56229,
#56230,#56231,#56232,#56233,#56234,#56235,#56236,#56237,#56238,#56239,#56240,
#56241,#56242,#56243,#56244,#56245,#56246,#56247,#56248,#56249,#56250,#56251,
#56252,#56253,#56254,#56255,#56256,#56257,#56258,#56259,#56260,#56261,#56262,
#56263,#56264,#56265,#56266,#56267)),.UNSPECIFIED.,.F.,.F.,.F.,(4,4),(4,
1,1,1,1,1,1,1,1,1,1,1,1,1,1,1,1,1,1,1,1,1,1,1,1,1,1,1,1,1,1,1,1,1,1,1,1,
1,1,1,1,1,1,1,1,1,1,1,1,1,1,1,1,1,1,1,1,1,1,1,1,1,1,1,1,1,1,1,1,1,1,1,1,
1,1,1,1,1,1,1,1,1,1,1,1,1,1,1,1,1,1,1,1,1,1,1,1,1,1,1,1,1,1,1,1,1,1,1,1,
1,1,1,1,1,1,1,1,1,1,1,1,1,1,1,1,1,1,1,4),(0.,0.0658179306876173),(8.30838445208313,
8.80598005718054,9.30357566227795,10.2987668724728,11.2939580826676,12.2891492928624,
13.2843405030573,14.2795317132521,15.2747229234469,16.2699141336417,17.2651053438366,
18.2602965540314,19.2554877642262,20.250678974421,21.2458701846159,22.2410613948107,
23.2362526050055,24.2314438152003,25.2266350253952,26.22182623559,27.2170174457848,
28.2122086559796,29.2073998661744,30.2025910763693,31.1977822865641,32.1929734967589,
33.1881647069537,34.1833559171486,35.1785471273434,36.1737383375382,37.168929547733,
38.1641207579279,39.1593119681227,40.1545031783175,41.1496943885123,42.1448855987072,
43.140076808902,44.1352680190968,45.1304592292916,46.1256504394865,47.1208416496813,
48.1160328598761,49.1112240700709,50.1064152802658,51.1016064904606,52.0967977006554,
53.0919889108502,54.0871801210451,55.0823713312399,56.0775625414347,57.0727537516295,
58.0679449618244,59.0631361720192,60.058327382214,61.0535185924088,62.0487098026037,
63.0439010127985,64.0390922229933,65.0342834331881,66.029474643383,67.0246658535778,
68.0198570637726,69.0150482739674,70.0102394841623,71.0054306943571,72.0006219045519,
72.9958131147467,73.9910043249416,74.9861955351364,75.9813867453312,76.976577955526,
77.9717691657209,78.9669603759157,79.9621515861105,80.9573427963053,81.9525340065002,
82.947725216695,83.9429164268898,84.9381076370846,85.9332988472795,86.9284900574743,
87.9236812676691,88.9188724778639,89.9140636880588,90.9092548982536,91.9044461084484,
92.8996373186432,93.8948285288381,94.8900197390329,95.8852109492277,96.8804021594225,
97.8755933696174,98.8707845798122,99.865975790007,100.861167000202,101.856358210397,
102.851549420591,103.846740630786,104.841931840981,105.837123051176,106.832314261371,
107.827505471566,108.82269668176,109.817887891955,110.81307910215,111.808270312345,
112.80346152254,113.798652732735,114.793843942929,115.789035153124,116.784226363319,
117.779417573514,118.774608783709,119.769799993904,120.764991204098,121.760182414293,
122.755373624488,123.750564834683,124.745756044878,125.740947255072,126.736138465267,
127.731329675462,128.726520885657,129.721712095852,130.716903306047,131.712094516241,
132.707285726436,133.204881331534,133.702476936631),.UNSPECIFIED.);
#350=B_SPLINE_SURFACE_WITH_KNOTS('',3,3,((#58329,#58330,#58331,#58332,#58333,
#58334,#58335,#58336,#58337,#58338,#58339,#58340,#58341,#58342,#58343,#58344,
#58345,#58346,#58347,#58348,#58349,#58350,#58351,#58352,#58353,#58354,#58355,
#58356,#58357,#58358,#58359,#58360,#58361,#58362,#58363,#58364,#58365,#58366,
#58367,#58368,#58369,#58370,#58371,#58372,#58373,#58374,#58375,#58376,#58377,
#58378,#58379,#58380,#58381,#58382,#58383,#58384),(#58385,#58386,#58387,
#58388,#58389,#58390,#58391,#58392,#58393,#58394,#58395,#58396,#58397,#58398,
#58399,#58400,#58401,#58402,#58403,#58404,#58405,#58406,#58407,#58408,#58409,
#58410,#58411,#58412,#58413,#58414,#58415,#58416,#58417,#58418,#58419,#58420,
#58421,#58422,#58423,#58424,#58425,#58426,#58427,#58428,#58429,#58430,#58431,
#58432,#58433,#58434,#58435,#58436,#58437,#58438,#58439,#58440),(#58441,
#58442,#58443,#58444,#58445,#58446,#58447,#58448,#58449,#58450,#58451,#58452,
#58453,#58454,#58455,#58456,#58457,#58458,#58459,#58460,#58461,#58462,#58463,
#58464,#58465,#58466,#58467,#58468,#58469,#58470,#58471,#58472,#58473,#58474,
#58475,#58476,#58477,#58478,#58479,#58480,#58481,#58482,#58483,#58484,#58485,
#58486,#58487,#58488,#58489,#58490,#58491,#58492,#58493,#58494,#58495,#58496),
(#58497,#58498,#58499,#58500,#58501,#58502,#58503,#58504,#58505,#58506,
#58507,#58508,#58509,#58510,#58511,#58512,#58513,#58514,#58515,#58516,#58517,
#58518,#58519,#58520,#58521,#58522,#58523,#58524,#58525,#58526,#58527,#58528,
#58529,#58530,#58531,#58532,#58533,#58534,#58535,#58536,#58537,#58538,#58539,
#58540,#58541,#58542,#58543,#58544,#58545,#58546,#58547,#58548,#58549,#58550,
#58551,#58552)),.UNSPECIFIED.,.F.,.F.,.F.,(4,4),(4,1,1,1,1,1,1,1,1,1,1,
1,1,1,1,1,1,1,1,1,1,1,1,1,1,1,1,1,1,1,1,1,1,1,1,1,1,1,1,1,1,1,1,1,1,1,1,
1,1,1,1,1,1,4),(0.,0.0642013499338863),(11.8589888623078,12.8454497557128,
13.8319106491178,14.8183715425228,15.8048324359278,16.7912933293328,17.7777542227378,
18.7642151161429,19.7506760095479,20.7371369029529,21.7235977963579,22.7100586897629,
23.6965195831679,24.6829804765729,25.6694413699779,26.6559022633829,27.6423631567879,
28.6288240501929,29.6152849435979,30.6017458370029,31.5882067304079,32.5746676238129,
33.5611285172179,34.5475894106229,35.5340503040279,36.5205111974329,37.5069720908379,
38.4934329842429,39.4798938776479,40.4663547710529,41.4528156644579,42.4392765578629,
43.4257374512679,44.4121983446729,45.3986592380779,46.3851201314829,47.3715810248879,
48.3580419182929,49.3445028116979,50.3309637051029,51.3174245985079,52.3038854919129,
53.2903463853179,54.2768072787229,55.2632681721279,56.2497290655329,57.2361899589379,
58.222650852343,59.209111745748,60.195572639153,61.182033532558,62.168494425963,
63.154955319368,64.141416212773),.UNSPECIFIED.);
#351=B_SPLINE_SURFACE_WITH_KNOTS('',3,3,((#58669,#58670,#58671,#58672,#58673,
#58674,#58675,#58676,#58677,#58678,#58679,#58680,#58681,#58682,#58683,#58684,
#58685,#58686,#58687,#58688,#58689,#58690,#58691,#58692,#58693,#58694,#58695,
#58696,#58697,#58698,#58699,#58700,#58701,#58702,#58703,#58704,#58705,#58706,
#58707,#58708,#58709,#58710,#58711,#58712,#58713,#58714,#58715,#58716,#58717,
#58718,#58719,#58720,#58721,#58722,#58723,#58724),(#58725,#58726,#58727,
#58728,#58729,#58730,#58731,#58732,#58733,#58734,#58735,#58736,#58737,#58738,
#58739,#58740,#58741,#58742,#58743,#58744,#58745,#58746,#58747,#58748,#58749,
#58750,#58751,#58752,#58753,#58754,#58755,#58756,#58757,#58758,#58759,#58760,
#58761,#58762,#58763,#58764,#58765,#58766,#58767,#58768,#58769,#58770,#58771,
#58772,#58773,#58774,#58775,#58776,#58777,#58778,#58779,#58780),(#58781,
#58782,#58783,#58784,#58785,#58786,#58787,#58788,#58789,#58790,#58791,#58792,
#58793,#58794,#58795,#58796,#58797,#58798,#58799,#58800,#58801,#58802,#58803,
#58804,#58805,#58806,#58807,#58808,#58809,#58810,#58811,#58812,#58813,#58814,
#58815,#58816,#58817,#58818,#58819,#58820,#58821,#58822,#58823,#58824,#58825,
#58826,#58827,#58828,#58829,#58830,#58831,#58832,#58833,#58834,#58835,#58836),
(#58837,#58838,#58839,#58840,#58841,#58842,#58843,#58844,#58845,#58846,
#58847,#58848,#58849,#58850,#58851,#58852,#58853,#58854,#58855,#58856,#58857,
#58858,#58859,#58860,#58861,#58862,#58863,#58864,#58865,#58866,#58867,#58868,
#58869,#58870,#58871,#58872,#58873,#58874,#58875,#58876,#58877,#58878,#58879,
#58880,#58881,#58882,#58883,#58884,#58885,#58886,#58887,#58888,#58889,#58890,
#58891,#58892)),.UNSPECIFIED.,.F.,.F.,.F.,(4,4),(4,1,1,1,1,1,1,1,1,1,1,
1,1,1,1,1,1,1,1,1,1,1,1,1,1,1,1,1,1,1,1,1,1,1,1,1,1,1,1,1,1,1,1,1,1,1,1,
1,1,1,1,1,1,4),(0.,0.0642013499338863),(14.3984001269719,15.3848610203769,
16.3713219137819,17.3577828071869,18.3442437005919,19.3307045939969,20.3171654874019,
21.3036263808069,22.2900872742119,23.2765481676169,24.2630090610219,25.2494699544269,
26.2359308478319,27.2223917412369,28.2088526346419,29.1953135280469,30.1817744214519,
31.1682353148569,32.1546962082619,33.1411571016669,34.1276179950719,35.1140788884769,
36.1005397818819,37.0870006752869,38.0734615686919,39.0599224620969,40.0463833555019,
41.0328442489069,42.0193051423119,43.0057660357169,43.9922269291219,44.978687822527,
45.965148715932,46.951609609337,47.938070502742,48.924531396147,49.910992289552,
50.897453182957,51.883914076362,52.870374969767,53.856835863172,54.843296756577,
55.829757649982,56.816218543387,57.802679436792,58.789140330197,59.775601223602,
60.762062117007,61.748523010412,62.734983903817,63.721444797222,64.707905690627,
65.694366584032,66.680827477437),.UNSPECIFIED.);
#352=B_SPLINE_SURFACE_WITH_KNOTS('',3,3,((#59221,#59222,#59223,#59224,#59225,
#59226,#59227,#59228,#59229,#59230,#59231,#59232,#59233,#59234,#59235,#59236,
#59237,#59238,#59239,#59240,#59241,#59242,#59243,#59244,#59245,#59246,#59247,
#59248,#59249,#59250,#59251,#59252,#59253,#59254,#59255,#59256,#59257,#59258,
#59259,#59260,#59261,#59262,#59263,#59264,#59265,#59266,#59267,#59268,#59269,
#59270,#59271,#59272,#59273,#59274,#59275,#59276),(#59277,#59278,#59279,
#59280,#59281,#59282,#59283,#59284,#59285,#59286,#59287,#59288,#59289,#59290,
#59291,#59292,#59293,#59294,#59295,#59296,#59297,#59298,#59299,#59300,#59301,
#59302,#59303,#59304,#59305,#59306,#59307,#59308,#59309,#59310,#59311,#59312,
#59313,#59314,#59315,#59316,#59317,#59318,#59319,#59320,#59321,#59322,#59323,
#59324,#59325,#59326,#59327,#59328,#59329,#59330,#59331,#59332),(#59333,
#59334,#59335,#59336,#59337,#59338,#59339,#59340,#59341,#59342,#59343,#59344,
#59345,#59346,#59347,#59348,#59349,#59350,#59351,#59352,#59353,#59354,#59355,
#59356,#59357,#59358,#59359,#59360,#59361,#59362,#59363,#59364,#59365,#59366,
#59367,#59368,#59369,#59370,#59371,#59372,#59373,#59374,#59375,#59376,#59377,
#59378,#59379,#59380,#59381,#59382,#59383,#59384,#59385,#59386,#59387,#59388),
(#59389,#59390,#59391,#59392,#59393,#59394,#59395,#59396,#59397,#59398,
#59399,#59400,#59401,#59402,#59403,#59404,#59405,#59406,#59407,#59408,#59409,
#59410,#59411,#59412,#59413,#59414,#59415,#59416,#59417,#59418,#59419,#59420,
#59421,#59422,#59423,#59424,#59425,#59426,#59427,#59428,#59429,#59430,#59431,
#59432,#59433,#59434,#59435,#59436,#59437,#59438,#59439,#59440,#59441,#59442,
#59443,#59444)),.UNSPECIFIED.,.F.,.F.,.F.,(4,4),(4,1,1,1,1,1,1,1,1,1,1,
1,1,1,1,1,1,1,1,1,1,1,1,1,1,1,1,1,1,1,1,1,1,1,1,1,1,1,1,1,1,1,1,1,1,1,1,
1,1,1,1,1,1,4),(0.,0.0642013499338863),(11.8589888623078,12.8454497557128,
13.8319106491178,14.8183715425228,15.8048324359278,16.7912933293328,17.7777542227378,
18.7642151161428,19.7506760095478,20.7371369029528,21.7235977963578,22.7100586897628,
23.6965195831678,24.6829804765729,25.6694413699779,26.6559022633829,27.6423631567879,
28.6288240501929,29.6152849435979,30.6017458370029,31.5882067304079,32.5746676238129,
33.5611285172179,34.5475894106229,35.5340503040279,36.5205111974329,37.5069720908379,
38.4934329842429,39.4798938776479,40.4663547710529,41.4528156644579,42.4392765578629,
43.4257374512679,44.4121983446729,45.3986592380779,46.3851201314829,47.3715810248879,
48.3580419182929,49.3445028116979,50.3309637051029,51.3174245985079,52.3038854919129,
53.2903463853179,54.2768072787229,55.2632681721279,56.2497290655329,57.2361899589379,
58.2226508523429,59.2091117457479,60.1955726391529,61.1820335325579,62.1684944259629,
63.154955319368,64.141416212773),.UNSPECIFIED.);
#353=B_SPLINE_SURFACE_WITH_KNOTS('',3,3,((#59561,#59562,#59563,#59564,#59565,
#59566,#59567,#59568,#59569,#59570,#59571,#59572,#59573,#59574,#59575,#59576,
#59577,#59578,#59579,#59580,#59581,#59582,#59583,#59584,#59585,#59586,#59587,
#59588,#59589,#59590,#59591,#59592,#59593,#59594,#59595,#59596,#59597,#59598,
#59599,#59600,#59601,#59602,#59603,#59604,#59605,#59606,#59607,#59608,#59609,
#59610,#59611,#59612,#59613,#59614,#59615,#59616),(#59617,#59618,#59619,
#59620,#59621,#59622,#59623,#59624,#59625,#59626,#59627,#59628,#59629,#59630,
#59631,#59632,#59633,#59634,#59635,#59636,#59637,#59638,#59639,#59640,#59641,
#59642,#59643,#59644,#59645,#59646,#59647,#59648,#59649,#59650,#59651,#59652,
#59653,#59654,#59655,#59656,#59657,#59658,#59659,#59660,#59661,#59662,#59663,
#59664,#59665,#59666,#59667,#59668,#59669,#59670,#59671,#59672),(#59673,
#59674,#59675,#59676,#59677,#59678,#59679,#59680,#59681,#59682,#59683,#59684,
#59685,#59686,#59687,#59688,#59689,#59690,#59691,#59692,#59693,#59694,#59695,
#59696,#59697,#59698,#59699,#59700,#59701,#59702,#59703,#59704,#59705,#59706,
#59707,#59708,#59709,#59710,#59711,#59712,#59713,#59714,#59715,#59716,#59717,
#59718,#59719,#59720,#59721,#59722,#59723,#59724,#59725,#59726,#59727,#59728),
(#59729,#59730,#59731,#59732,#59733,#59734,#59735,#59736,#59737,#59738,
#59739,#59740,#59741,#59742,#59743,#59744,#59745,#59746,#59747,#59748,#59749,
#59750,#59751,#59752,#59753,#59754,#59755,#59756,#59757,#59758,#59759,#59760,
#59761,#59762,#59763,#59764,#59765,#59766,#59767,#59768,#59769,#59770,#59771,
#59772,#59773,#59774,#59775,#59776,#59777,#59778,#59779,#59780,#59781,#59782,
#59783,#59784)),.UNSPECIFIED.,.F.,.F.,.F.,(4,4),(4,1,1,1,1,1,1,1,1,1,1,
1,1,1,1,1,1,1,1,1,1,1,1,1,1,1,1,1,1,1,1,1,1,1,1,1,1,1,1,1,1,1,1,1,1,1,1,
1,1,1,1,1,1,4),(0.,0.0642013499338863),(14.3984001269719,15.3848610203769,
16.3713219137819,17.3577828071869,18.3442437005919,19.3307045939969,20.3171654874019,
21.3036263808069,22.2900872742119,23.2765481676169,24.2630090610219,25.2494699544269,
26.2359308478319,27.2223917412369,28.2088526346419,29.1953135280469,30.1817744214519,
31.1682353148569,32.1546962082619,33.1411571016669,34.1276179950719,35.1140788884769,
36.1005397818819,37.0870006752869,38.0734615686919,39.0599224620969,40.0463833555019,
41.0328442489069,42.0193051423119,43.0057660357169,43.9922269291219,44.9786878225269,
45.9651487159319,46.9516096093369,47.9380705027419,48.9245313961469,49.9109922895519,
50.897453182957,51.883914076362,52.870374969767,53.856835863172,54.843296756577,
55.829757649982,56.816218543387,57.802679436792,58.789140330197,59.775601223602,
60.762062117007,61.748523010412,62.734983903817,63.721444797222,64.707905690627,
65.694366584032,66.680827477437),.UNSPECIFIED.);
#354=B_SPLINE_SURFACE_WITH_KNOTS('',3,3,((#60113,#60114,#60115,#60116,#60117,
#60118,#60119,#60120,#60121,#60122,#60123,#60124,#60125,#60126,#60127,#60128,
#60129,#60130,#60131,#60132,#60133,#60134,#60135,#60136,#60137,#60138,#60139,
#60140,#60141,#60142,#60143,#60144,#60145,#60146,#60147,#60148,#60149,#60150,
#60151,#60152,#60153,#60154,#60155,#60156,#60157,#60158,#60159,#60160,#60161,
#60162,#60163,#60164,#60165,#60166,#60167,#60168),(#60169,#60170,#60171,
#60172,#60173,#60174,#60175,#60176,#60177,#60178,#60179,#60180,#60181,#60182,
#60183,#60184,#60185,#60186,#60187,#60188,#60189,#60190,#60191,#60192,#60193,
#60194,#60195,#60196,#60197,#60198,#60199,#60200,#60201,#60202,#60203,#60204,
#60205,#60206,#60207,#60208,#60209,#60210,#60211,#60212,#60213,#60214,#60215,
#60216,#60217,#60218,#60219,#60220,#60221,#60222,#60223,#60224),(#60225,
#60226,#60227,#60228,#60229,#60230,#60231,#60232,#60233,#60234,#60235,#60236,
#60237,#60238,#60239,#60240,#60241,#60242,#60243,#60244,#60245,#60246,#60247,
#60248,#60249,#60250,#60251,#60252,#60253,#60254,#60255,#60256,#60257,#60258,
#60259,#60260,#60261,#60262,#60263,#60264,#60265,#60266,#60267,#60268,#60269,
#60270,#60271,#60272,#60273,#60274,#60275,#60276,#60277,#60278,#60279,#60280),
(#60281,#60282,#60283,#60284,#60285,#60286,#60287,#60288,#60289,#60290,
#60291,#60292,#60293,#60294,#60295,#60296,#60297,#60298,#60299,#60300,#60301,
#60302,#60303,#60304,#60305,#60306,#60307,#60308,#60309,#60310,#60311,#60312,
#60313,#60314,#60315,#60316,#60317,#60318,#60319,#60320,#60321,#60322,#60323,
#60324,#60325,#60326,#60327,#60328,#60329,#60330,#60331,#60332,#60333,#60334,
#60335,#60336)),.UNSPECIFIED.,.F.,.F.,.F.,(4,4),(4,1,1,1,1,1,1,1,1,1,1,
1,1,1,1,1,1,1,1,1,1,1,1,1,1,1,1,1,1,1,1,1,1,1,1,1,1,1,1,1,1,1,1,1,1,1,1,
1,1,1,1,1,1,4),(0.,0.0642013499338865),(11.8589888623078,12.8454497557128,
13.8319106491178,14.8183715425228,15.8048324359278,16.7912933293328,17.7777542227378,
18.7642151161428,19.7506760095478,20.7371369029528,21.7235977963578,22.7100586897628,
23.6965195831678,24.6829804765729,25.6694413699779,26.6559022633829,27.6423631567879,
28.6288240501929,29.6152849435979,30.6017458370029,31.5882067304079,32.5746676238129,
33.5611285172179,34.5475894106229,35.5340503040279,36.5205111974329,37.5069720908379,
38.4934329842429,39.4798938776479,40.4663547710529,41.4528156644579,42.4392765578629,
43.4257374512679,44.4121983446729,45.3986592380779,46.3851201314829,47.3715810248879,
48.3580419182929,49.3445028116979,50.3309637051029,51.3174245985079,52.3038854919129,
53.2903463853179,54.2768072787229,55.2632681721279,56.2497290655329,57.2361899589379,
58.2226508523429,59.2091117457479,60.1955726391529,61.1820335325579,62.1684944259629,
63.154955319368,64.141416212773),.UNSPECIFIED.);
#355=B_SPLINE_SURFACE_WITH_KNOTS('',3,3,((#60453,#60454,#60455,#60456,#60457,
#60458,#60459,#60460,#60461,#60462,#60463,#60464,#60465,#60466,#60467,#60468,
#60469,#60470,#60471,#60472,#60473,#60474,#60475,#60476,#60477,#60478,#60479,
#60480,#60481,#60482,#60483,#60484,#60485,#60486,#60487,#60488,#60489,#60490,
#60491,#60492,#60493,#60494,#60495,#60496,#60497,#60498,#60499,#60500,#60501,
#60502,#60503,#60504,#60505,#60506,#60507,#60508),(#60509,#60510,#60511,
#60512,#60513,#60514,#60515,#60516,#60517,#60518,#60519,#60520,#60521,#60522,
#60523,#60524,#60525,#60526,#60527,#60528,#60529,#60530,#60531,#60532,#60533,
#60534,#60535,#60536,#60537,#60538,#60539,#60540,#60541,#60542,#60543,#60544,
#60545,#60546,#60547,#60548,#60549,#60550,#60551,#60552,#60553,#60554,#60555,
#60556,#60557,#60558,#60559,#60560,#60561,#60562,#60563,#60564),(#60565,
#60566,#60567,#60568,#60569,#60570,#60571,#60572,#60573,#60574,#60575,#60576,
#60577,#60578,#60579,#60580,#60581,#60582,#60583,#60584,#60585,#60586,#60587,
#60588,#60589,#60590,#60591,#60592,#60593,#60594,#60595,#60596,#60597,#60598,
#60599,#60600,#60601,#60602,#60603,#60604,#60605,#60606,#60607,#60608,#60609,
#60610,#60611,#60612,#60613,#60614,#60615,#60616,#60617,#60618,#60619,#60620),
(#60621,#60622,#60623,#60624,#60625,#60626,#60627,#60628,#60629,#60630,
#60631,#60632,#60633,#60634,#60635,#60636,#60637,#60638,#60639,#60640,#60641,
#60642,#60643,#60644,#60645,#60646,#60647,#60648,#60649,#60650,#60651,#60652,
#60653,#60654,#60655,#60656,#60657,#60658,#60659,#60660,#60661,#60662,#60663,
#60664,#60665,#60666,#60667,#60668,#60669,#60670,#60671,#60672,#60673,#60674,
#60675,#60676)),.UNSPECIFIED.,.F.,.F.,.F.,(4,4),(4,1,1,1,1,1,1,1,1,1,1,
1,1,1,1,1,1,1,1,1,1,1,1,1,1,1,1,1,1,1,1,1,1,1,1,1,1,1,1,1,1,1,1,1,1,1,1,
1,1,1,1,1,1,4),(0.,0.0642013499338865),(14.3984001269719,15.3848610203769,
16.3713219137819,17.3577828071869,18.3442437005919,19.3307045939969,20.3171654874019,
21.3036263808069,22.2900872742119,23.2765481676169,24.2630090610219,25.2494699544269,
26.2359308478319,27.2223917412369,28.2088526346419,29.1953135280469,30.1817744214519,
31.1682353148569,32.1546962082619,33.1411571016669,34.1276179950719,35.1140788884769,
36.1005397818819,37.0870006752869,38.0734615686919,39.0599224620969,40.0463833555019,
41.0328442489069,42.0193051423119,43.0057660357169,43.9922269291219,44.9786878225269,
45.9651487159319,46.9516096093369,47.9380705027419,48.9245313961469,49.9109922895519,
50.897453182957,51.883914076362,52.870374969767,53.856835863172,54.843296756577,
55.829757649982,56.816218543387,57.802679436792,58.789140330197,59.775601223602,
60.762062117007,61.748523010412,62.734983903817,63.721444797222,64.707905690627,
65.694366584032,66.680827477437),.UNSPECIFIED.);
#356=B_SPLINE_SURFACE_WITH_KNOTS('',3,3,((#65272,#65273,#65274,#65275,#65276,
#65277,#65278,#65279,#65280,#65281,#65282,#65283,#65284,#65285,#65286,#65287,
#65288,#65289,#65290,#65291,#65292,#65293,#65294,#65295,#65296,#65297,#65298,
#65299,#65300,#65301,#65302,#65303,#65304,#65305,#65306,#65307,#65308,#65309,
#65310,#65311,#65312,#65313,#65314,#65315,#65316,#65317,#65318,#65319,#65320,
#65321,#65322,#65323,#65324,#65325,#65326,#65327,#65328,#65329,#65330,#65331,
#65332,#65333,#65334,#65335,#65336,#65337,#65338,#65339,#65340,#65341,#65342,
#65343,#65344,#65345,#65346,#65347,#65348,#65349,#65350,#65351,#65352,#65353,
#65354,#65355,#65356,#65357,#65358,#65359,#65360,#65361,#65362,#65363,#65364,
#65365,#65366,#65367,#65368,#65369,#65370,#65371,#65372,#65373,#65374,#65375,
#65376,#65377,#65378,#65379,#65380,#65381,#65382,#65383,#65384,#65385,#65386,
#65387,#65388,#65389,#65390,#65391,#65392,#65393,#65394,#65395,#65396,#65397,
#65398,#65399,#65400,#65401,#65402,#65403,#65404,#65405,#65406,#65407,#65408,
#65409,#65410,#65411,#65412,#65413,#65414,#65415,#65416,#65417,#65418,#65419,
#65420,#65421,#65422,#65423,#65424,#65425,#65426,#65427,#65428,#65429,#65430,
#65431,#65432,#65433,#65434,#65435,#65436,#65437,#65438,#65439,#65440,#65441,
#65442,#65443,#65444,#65445,#65446,#65447,#65448,#65449,#65450,#65451,#65452,
#65453,#65454,#65455,#65456,#65457,#65458,#65459,#65460,#65461,#65462,#65463,
#65464,#65465,#65466,#65467,#65468,#65469,#65470,#65471,#65472,#65473,#65474,
#65475,#65476,#65477,#65478,#65479,#65480,#65481,#65482,#65483,#65484,#65485,
#65486,#65487,#65488,#65489,#65490,#65491,#65492,#65493,#65494,#65495,#65496,
#65497,#65498,#65499,#65500,#65501,#65502,#65503,#65504,#65505,#65506,#65507,
#65508,#65509,#65510,#65511,#65512,#65513,#65514,#65515,#65516,#65517,#65518,
#65519,#65520,#65521,#65522,#65523,#65524,#65525,#65526,#65527,#65528,#65529,
#65530,#65531,#65532,#65533,#65534,#65535,#65536,#65537,#65538,#65539,#65540,
#65541,#65542,#65543,#65544,#65545,#65546,#65547,#65548,#65549,#65550,#65551,
#65552,#65553,#65554,#65555,#65556,#65557,#65558,#65559,#65560,#65561,#65562,
#65563,#65564,#65565,#65566,#65567,#65568,#65569,#65570,#65571,#65572,#65573,
#65574,#65575,#65576,#65577,#65578,#65579,#65580,#65581,#65582,#65583,#65584,
#65585,#65586,#65587,#65588,#65589,#65590,#65591,#65592,#65593,#65594,#65595,
#65596,#65597,#65598,#65599,#65600,#65601,#65602,#65603,#65604,#65605,#65606,
#65607,#65608,#65609,#65610,#65611,#65612,#65613,#65614,#65615,#65616,#65617,
#65618,#65619,#65620,#65621,#65622,#65623,#65624,#65625,#65626,#65627,#65628,
#65629,#65630,#65631,#65632,#65633,#65634,#65635,#65636,#65637,#65638,#65639,
#65640,#65641,#65642,#65643,#65644,#65645,#65646,#65647,#65648,#65649,#65650,
#65651,#65652,#65653,#65654,#65655,#65656),(#65657,#65658,#65659,#65660,
#65661,#65662,#65663,#65664,#65665,#65666,#65667,#65668,#65669,#65670,#65671,
#65672,#65673,#65674,#65675,#65676,#65677,#65678,#65679,#65680,#65681,#65682,
#65683,#65684,#65685,#65686,#65687,#65688,#65689,#65690,#65691,#65692,#65693,
#65694,#65695,#65696,#65697,#65698,#65699,#65700,#65701,#65702,#65703,#65704,
#65705,#65706,#65707,#65708,#65709,#65710,#65711,#65712,#65713,#65714,#65715,
#65716,#65717,#65718,#65719,#65720,#65721,#65722,#65723,#65724,#65725,#65726,
#65727,#65728,#65729,#65730,#65731,#65732,#65733,#65734,#65735,#65736,#65737,
#65738,#65739,#65740,#65741,#65742,#65743,#65744,#65745,#65746,#65747,#65748,
#65749,#65750,#65751,#65752,#65753,#65754,#65755,#65756,#65757,#65758,#65759,
#65760,#65761,#65762,#65763,#65764,#65765,#65766,#65767,#65768,#65769,#65770,
#65771,#65772,#65773,#65774,#65775,#65776,#65777,#65778,#65779,#65780,#65781,
#65782,#65783,#65784,#65785,#65786,#65787,#65788,#65789,#65790,#65791,#65792,
#65793,#65794,#65795,#65796,#65797,#65798,#65799,#65800,#65801,#65802,#65803,
#65804,#65805,#65806,#65807,#65808,#65809,#65810,#65811,#65812,#65813,#65814,
#65815,#65816,#65817,#65818,#65819,#65820,#65821,#65822,#65823,#65824,#65825,
#65826,#65827,#65828,#65829,#65830,#65831,#65832,#65833,#65834,#65835,#65836,
#65837,#65838,#65839,#65840,#65841,#65842,#65843,#65844,#65845,#65846,#65847,
#65848,#65849,#65850,#65851,#65852,#65853,#65854,#65855,#65856,#65857,#65858,
#65859,#65860,#65861,#65862,#65863,#65864,#65865,#65866,#65867,#65868,#65869,
#65870,#65871,#65872,#65873,#65874,#65875,#65876,#65877,#65878,#65879,#65880,
#65881,#65882,#65883,#65884,#65885,#65886,#65887,#65888,#65889,#65890,#65891,
#65892,#65893,#65894,#65895,#65896,#65897,#65898,#65899,#65900,#65901,#65902,
#65903,#65904,#65905,#65906,#65907,#65908,#65909,#65910,#65911,#65912,#65913,
#65914,#65915,#65916,#65917,#65918,#65919,#65920,#65921,#65922,#65923,#65924,
#65925,#65926,#65927,#65928,#65929,#65930,#65931,#65932,#65933,#65934,#65935,
#65936,#65937,#65938,#65939,#65940,#65941,#65942,#65943,#65944,#65945,#65946,
#65947,#65948,#65949,#65950,#65951,#65952,#65953,#65954,#65955,#65956,#65957,
#65958,#65959,#65960,#65961,#65962,#65963,#65964,#65965,#65966,#65967,#65968,
#65969,#65970,#65971,#65972,#65973,#65974,#65975,#65976,#65977,#65978,#65979,
#65980,#65981,#65982,#65983,#65984,#65985,#65986,#65987,#65988,#65989,#65990,
#65991,#65992,#65993,#65994,#65995,#65996,#65997,#65998,#65999,#66000,#66001,
#66002,#66003,#66004,#66005,#66006,#66007,#66008,#66009,#66010,#66011,#66012,
#66013,#66014,#66015,#66016,#66017,#66018,#66019,#66020,#66021,#66022,#66023,
#66024,#66025,#66026,#66027,#66028,#66029,#66030,#66031,#66032,#66033,#66034,
#66035,#66036,#66037,#66038,#66039,#66040,#66041),(#66042,#66043,#66044,
#66045,#66046,#66047,#66048,#66049,#66050,#66051,#66052,#66053,#66054,#66055,
#66056,#66057,#66058,#66059,#66060,#66061,#66062,#66063,#66064,#66065,#66066,
#66067,#66068,#66069,#66070,#66071,#66072,#66073,#66074,#66075,#66076,#66077,
#66078,#66079,#66080,#66081,#66082,#66083,#66084,#66085,#66086,#66087,#66088,
#66089,#66090,#66091,#66092,#66093,#66094,#66095,#66096,#66097,#66098,#66099,
#66100,#66101,#66102,#66103,#66104,#66105,#66106,#66107,#66108,#66109,#66110,
#66111,#66112,#66113,#66114,#66115,#66116,#66117,#66118,#66119,#66120,#66121,
#66122,#66123,#66124,#66125,#66126,#66127,#66128,#66129,#66130,#66131,#66132,
#66133,#66134,#66135,#66136,#66137,#66138,#66139,#66140,#66141,#66142,#66143,
#66144,#66145,#66146,#66147,#66148,#66149,#66150,#66151,#66152,#66153,#66154,
#66155,#66156,#66157,#66158,#66159,#66160,#66161,#66162,#66163,#66164,#66165,
#66166,#66167,#66168,#66169,#66170,#66171,#66172,#66173,#66174,#66175,#66176,
#66177,#66178,#66179,#66180,#66181,#66182,#66183,#66184,#66185,#66186,#66187,
#66188,#66189,#66190,#66191,#66192,#66193,#66194,#66195,#66196,#66197,#66198,
#66199,#66200,#66201,#66202,#66203,#66204,#66205,#66206,#66207,#66208,#66209,
#66210,#66211,#66212,#66213,#66214,#66215,#66216,#66217,#66218,#66219,#66220,
#66221,#66222,#66223,#66224,#66225,#66226,#66227,#66228,#66229,#66230,#66231,
#66232,#66233,#66234,#66235,#66236,#66237,#66238,#66239,#66240,#66241,#66242,
#66243,#66244,#66245,#66246,#66247,#66248,#66249,#66250,#66251,#66252,#66253,
#66254,#66255,#66256,#66257,#66258,#66259,#66260,#66261,#66262,#66263,#66264,
#66265,#66266,#66267,#66268,#66269,#66270,#66271,#66272,#66273,#66274,#66275,
#66276,#66277,#66278,#66279,#66280,#66281,#66282,#66283,#66284,#66285,#66286,
#66287,#66288,#66289,#66290,#66291,#66292,#66293,#66294,#66295,#66296,#66297,
#66298,#66299,#66300,#66301,#66302,#66303,#66304,#66305,#66306,#66307,#66308,
#66309,#66310,#66311,#66312,#66313,#66314,#66315,#66316,#66317,#66318,#66319,
#66320,#66321,#66322,#66323,#66324,#66325,#66326,#66327,#66328,#66329,#66330,
#66331,#66332,#66333,#66334,#66335,#66336,#66337,#66338,#66339,#66340,#66341,
#66342,#66343,#66344,#66345,#66346,#66347,#66348,#66349,#66350,#66351,#66352,
#66353,#66354,#66355,#66356,#66357,#66358,#66359,#66360,#66361,#66362,#66363,
#66364,#66365,#66366,#66367,#66368,#66369,#66370,#66371,#66372,#66373,#66374,
#66375,#66376,#66377,#66378,#66379,#66380,#66381,#66382,#66383,#66384,#66385,
#66386,#66387,#66388,#66389,#66390,#66391,#66392,#66393,#66394,#66395,#66396,
#66397,#66398,#66399,#66400,#66401,#66402,#66403,#66404,#66405,#66406,#66407,
#66408,#66409,#66410,#66411,#66412,#66413,#66414,#66415,#66416,#66417,#66418,
#66419,#66420,#66421,#66422,#66423,#66424,#66425,#66426),(#66427,#66428,
#66429,#66430,#66431,#66432,#66433,#66434,#66435,#66436,#66437,#66438,#66439,
#66440,#66441,#66442,#66443,#66444,#66445,#66446,#66447,#66448,#66449,#66450,
#66451,#66452,#66453,#66454,#66455,#66456,#66457,#66458,#66459,#66460,#66461,
#66462,#66463,#66464,#66465,#66466,#66467,#66468,#66469,#66470,#66471,#66472,
#66473,#66474,#66475,#66476,#66477,#66478,#66479,#66480,#66481,#66482,#66483,
#66484,#66485,#66486,#66487,#66488,#66489,#66490,#66491,#66492,#66493,#66494,
#66495,#66496,#66497,#66498,#66499,#66500,#66501,#66502,#66503,#66504,#66505,
#66506,#66507,#66508,#66509,#66510,#66511,#66512,#66513,#66514,#66515,#66516,
#66517,#66518,#66519,#66520,#66521,#66522,#66523,#66524,#66525,#66526,#66527,
#66528,#66529,#66530,#66531,#66532,#66533,#66534,#66535,#66536,#66537,#66538,
#66539,#66540,#66541,#66542,#66543,#66544,#66545,#66546,#66547,#66548,#66549,
#66550,#66551,#66552,#66553,#66554,#66555,#66556,#66557,#66558,#66559,#66560,
#66561,#66562,#66563,#66564,#66565,#66566,#66567,#66568,#66569,#66570,#66571,
#66572,#66573,#66574,#66575,#66576,#66577,#66578,#66579,#66580,#66581,#66582,
#66583,#66584,#66585,#66586,#66587,#66588,#66589,#66590,#66591,#66592,#66593,
#66594,#66595,#66596,#66597,#66598,#66599,#66600,#66601,#66602,#66603,#66604,
#66605,#66606,#66607,#66608,#66609,#66610,#66611,#66612,#66613,#66614,#66615,
#66616,#66617,#66618,#66619,#66620,#66621,#66622,#66623,#66624,#66625,#66626,
#66627,#66628,#66629,#66630,#66631,#66632,#66633,#66634,#66635,#66636,#66637,
#66638,#66639,#66640,#66641,#66642,#66643,#66644,#66645,#66646,#66647,#66648,
#66649,#66650,#66651,#66652,#66653,#66654,#66655,#66656,#66657,#66658,#66659,
#66660,#66661,#66662,#66663,#66664,#66665,#66666,#66667,#66668,#66669,#66670,
#66671,#66672,#66673,#66674,#66675,#66676,#66677,#66678,#66679,#66680,#66681,
#66682,#66683,#66684,#66685,#66686,#66687,#66688,#66689,#66690,#66691,#66692,
#66693,#66694,#66695,#66696,#66697,#66698,#66699,#66700,#66701,#66702,#66703,
#66704,#66705,#66706,#66707,#66708,#66709,#66710,#66711,#66712,#66713,#66714,
#66715,#66716,#66717,#66718,#66719,#66720,#66721,#66722,#66723,#66724,#66725,
#66726,#66727,#66728,#66729,#66730,#66731,#66732,#66733,#66734,#66735,#66736,
#66737,#66738,#66739,#66740,#66741,#66742,#66743,#66744,#66745,#66746,#66747,
#66748,#66749,#66750,#66751,#66752,#66753,#66754,#66755,#66756,#66757,#66758,
#66759,#66760,#66761,#66762,#66763,#66764,#66765,#66766,#66767,#66768,#66769,
#66770,#66771,#66772,#66773,#66774,#66775,#66776,#66777,#66778,#66779,#66780,
#66781,#66782,#66783,#66784,#66785,#66786,#66787,#66788,#66789,#66790,#66791,
#66792,#66793,#66794,#66795,#66796,#66797,#66798,#66799,#66800,#66801,#66802,
#66803,#66804,#66805,#66806,#66807,#66808,#66809,#66810,#66811)),
 .UNSPECIFIED.,.F.,.F.,.F.,(4,4),(4,1,1,1,1,1,1,1,1,1,1,1,1,1,1,1,1,1,1,
1,1,1,1,1,1,1,1,1,1,1,1,1,1,1,1,1,1,1,1,1,1,1,1,1,1,1,1,1,1,1,1,1,1,1,1,
1,1,1,1,1,1,1,1,1,1,1,1,1,1,1,1,1,1,1,1,1,1,1,1,1,1,1,1,1,1,1,1,1,1,1,1,
1,1,1,1,1,1,1,1,1,1,1,1,1,1,1,1,1,1,1,1,1,1,1,1,1,1,1,1,1,1,1,1,1,1,1,1,
1,1,1,1,1,1,1,1,1,1,1,1,1,1,1,1,1,1,1,1,1,1,1,1,1,1,1,1,1,1,1,1,1,1,1,1,
1,1,1,1,1,1,1,1,1,1,1,1,1,1,1,1,1,1,1,1,1,1,1,1,1,1,1,1,1,1,1,1,1,1,1,1,
1,1,1,1,1,1,1,1,1,1,1,1,1,1,1,1,1,1,1,1,1,1,1,1,1,1,1,1,1,1,1,1,1,1,1,1,
1,1,1,1,1,1,1,1,1,1,1,1,1,1,1,1,1,1,1,1,1,1,1,1,1,1,1,1,1,1,1,1,1,1,1,1,
1,1,1,1,1,1,1,1,1,1,1,1,1,1,1,1,1,1,1,1,1,1,1,1,1,1,1,1,1,1,1,1,1,1,1,1,
1,1,1,1,1,1,1,1,1,1,1,1,1,1,1,1,1,1,1,1,1,1,1,1,1,1,1,1,1,1,1,1,1,1,1,1,
1,1,1,1,1,1,1,1,1,1,1,1,1,1,1,1,1,1,1,1,1,1,1,1,1,1,1,1,1,1,1,1,1,1,1,1,
1,1,1,4),(0.,0.0658179306876174),(8.30838445208392,8.80714609643392,9.30590774078392,
10.3034310294839,11.3009543181839,12.2984776068839,13.2960008955839,14.2935241842839,
15.291047472984,16.288570761684,17.286094050384,18.283617339084,19.281140627784,
20.278663916484,21.276187205184,22.273710493884,23.271233782584,24.268757071284,
25.266280359984,26.263803648684,27.261326937384,28.258850226084,29.256373514784,
30.253896803484,31.251420092184,32.2489433808841,33.2464666695841,34.2439899582841,
35.2415132469841,36.2390365356841,37.2365598243841,38.2340831130841,39.2316064017841,
40.2291296904841,41.2266529791841,42.2241762678841,43.2216995565841,44.2192228452841,
45.2167461339841,46.2142694226841,47.2117927113841,48.2093160000841,49.2068392887841,
50.2043625774841,51.2018858661842,52.1994091548842,53.1969324435842,54.1944557322842,
55.1919790209842,56.1895023096842,57.1870255983842,58.1845488870842,59.1820721757842,
60.1795954644842,61.1771187531842,62.1746420418842,63.1721653305842,64.1696886192842,
65.1672119079842,66.1647351966842,67.1622584853842,68.1597817740843,69.1573050627842,
70.1548283514843,71.1523516401843,72.1498749288843,73.1473982175843,74.1449215062843,
75.1424447949843,76.1399680836843,77.1374913723843,78.1350146610843,79.1325379497843,
80.1300612384843,81.1275845271843,82.1251078158843,83.1226311045843,84.1201543932843,
85.1176776819843,86.1152009706843,87.1127242593844,88.1102475480844,89.1077708367844,
90.1052941254844,91.1028174141844,92.1003407028844,93.0978639915844,94.0953872802844,
95.0929105689844,96.0904338576844,97.0879571463844,98.0854804350844,99.0830037237844,
100.080527012484,101.078050301184,102.075573589884,103.073096878584,104.070620167284,
105.068143455984,106.065666744684,107.063190033384,108.060713322084,109.058236610784,
110.055759899484,111.053283188184,112.050806476884,113.048329765584,114.045853054284,
115.043376342985,116.040899631685,117.038422920385,118.035946209085,119.033469497785,
120.030992786485,121.028516075185,122.026039363885,123.023562652585,124.021085941285,
125.018609229985,126.016132518685,127.013655807385,128.011179096085,129.008702384785,
130.006225673485,131.003748962185,132.001272250885,132.998795539585,133.996318828285,
134.993842116985,135.991365405685,136.988888694385,137.986411983085,138.983935271785,
139.981458560485,140.978981849185,141.976505137885,142.974028426585,143.971551715285,
144.969075003985,145.966598292685,146.964121581385,147.961644870085,148.959168158785,
149.956691447485,150.954214736185,151.951738024885,152.949261313585,153.946784602285,
154.944307890985,155.941831179685,156.939354468385,157.936877757085,158.934401045785,
159.931924334485,160.929447623185,161.926970911885,162.924494200585,163.922017489285,
164.919540777985,165.917064066685,166.914587355385,167.912110644085,168.909633932785,
169.907157221485,170.904680510185,171.902203798885,172.899727087585,173.897250376285,
174.894773664985,175.892296953685,176.889820242385,177.887343531085,178.884866819785,
179.882390108485,180.879913397185,181.877436685885,182.874959974585,183.872483263285,
184.870006551985,185.867529840685,186.865053129385,187.862576418085,188.860099706785,
189.857622995485,190.855146284185,191.852669572885,192.850192861585,193.847716150285,
194.845239438985,195.842762727685,196.840286016385,197.837809305085,198.835332593785,
199.832855882485,200.830379171185,201.827902459885,202.825425748585,203.822949037285,
204.820472325985,205.817995614685,206.815518903385,207.813042192085,208.810565480785,
209.808088769485,210.805612058185,211.803135346885,212.800658635585,213.798181924285,
214.795705212985,215.793228501685,216.790751790385,217.788275079085,218.785798367785,
219.783321656485,220.780844945185,221.778368233885,222.775891522585,223.773414811285,
224.770938099985,225.768461388685,226.765984677385,227.763507966085,228.761031254785,
229.758554543485,230.756077832185,231.753601120885,232.751124409585,233.748647698285,
234.746170986985,235.743694275685,236.741217564385,237.738740853085,238.736264141785,
239.733787430485,240.731310719185,241.728834007885,242.726357296585,243.723880585285,
244.721403873985,245.718927162685,246.716450451385,247.713973740085,248.711497028785,
249.709020317485,250.706543606185,251.704066894885,252.701590183585,253.699113472285,
254.696636760985,255.694160049685,256.691683338385,257.689206627085,258.686729915785,
259.684253204485,260.681776493185,261.679299781885,262.676823070585,263.674346359285,
264.671869647985,265.669392936685,266.666916225385,267.664439514085,268.661962802785,
269.659486091485,270.657009380185,271.654532668885,272.652055957585,273.649579246285,
274.647102534985,275.644625823685,276.642149112385,277.639672401085,278.637195689785,
279.634718978485,280.632242267185,281.629765555885,282.627288844585,283.624812133285,
284.622335421985,285.619858710685,286.617381999385,287.614905288085,288.612428576785,
289.609951865485,290.607475154186,291.604998442886,292.602521731586,293.600045020286,
294.597568308986,295.595091597686,296.592614886386,297.590138175086,298.587661463786,
299.585184752486,300.582708041186,301.580231329886,302.577754618586,303.575277907286,
304.572801195986,305.570324484686,306.567847773386,307.565371062086,308.562894350786,
309.560417639486,310.557940928186,311.555464216886,312.552987505586,313.550510794286,
314.548034082986,315.545557371686,316.543080660386,317.540603949086,318.538127237786,
319.535650526486,320.533173815186,321.530697103886,322.528220392586,323.525743681286,
324.523266969986,325.520790258686,326.518313547386,327.515836836086,328.513360124786,
329.510883413486,330.508406702186,331.505929990886,332.503453279586,333.500976568286,
334.498499856986,335.496023145686,336.493546434386,337.491069723086,338.488593011786,
339.486116300486,340.483639589186,341.481162877886,342.478686166586,343.476209455286,
344.473732743986,345.471256032686,346.468779321386,347.466302610086,348.463825898786,
349.461349187486,350.458872476186,351.456395764886,352.453919053586,353.451442342286,
354.448965630986,355.446488919686,356.444012208386,357.441535497086,358.439058785786,
359.436582074486,360.434105363186,361.431628651886,362.429151940586,363.426675229286,
364.424198517986,365.421721806686,366.419245095386,367.416768384086,368.414291672786,
369.411814961486,370.409338250186,371.406861538886,372.404384827586,373.401908116286,
374.399431404986,375.396954693686,376.394477982386,377.392001271086,378.389524559786,
379.387047848486,380.384571137186,381.382094425886,382.379617714586,383.377141003286,
384.374664291986,385.372187580686,386.369710869386,386.868472513736,387.367234158086),
 .UNSPECIFIED.);
#357=B_SPLINE_SURFACE_WITH_KNOTS('',3,3,((#67069,#67070,#67071,#67072,#67073,
#67074,#67075,#67076,#67077,#67078,#67079,#67080,#67081,#67082,#67083,#67084,
#67085,#67086,#67087,#67088,#67089,#67090,#67091,#67092,#67093,#67094,#67095,
#67096,#67097,#67098,#67099,#67100,#67101,#67102,#67103,#67104,#67105,#67106,
#67107,#67108,#67109,#67110,#67111,#67112,#67113,#67114,#67115,#67116,#67117,
#67118,#67119,#67120,#67121,#67122,#67123,#67124,#67125,#67126,#67127,#67128,
#67129,#67130,#67131,#67132,#67133,#67134,#67135,#67136,#67137,#67138,#67139,
#67140,#67141,#67142,#67143,#67144,#67145,#67146,#67147,#67148,#67149,#67150,
#67151,#67152,#67153,#67154,#67155,#67156,#67157,#67158,#67159,#67160,#67161,
#67162,#67163,#67164,#67165,#67166,#67167,#67168,#67169,#67170,#67171,#67172,
#67173,#67174,#67175,#67176,#67177,#67178,#67179,#67180,#67181,#67182,#67183,
#67184,#67185,#67186,#67187,#67188,#67189,#67190,#67191,#67192,#67193,#67194,
#67195,#67196,#67197,#67198,#67199,#67200,#67201,#67202,#67203,#67204,#67205,
#67206,#67207,#67208,#67209,#67210,#67211,#67212,#67213,#67214,#67215,#67216,
#67217,#67218,#67219,#67220,#67221,#67222,#67223,#67224,#67225,#67226,#67227,
#67228,#67229,#67230,#67231,#67232,#67233,#67234,#67235,#67236,#67237,#67238,
#67239,#67240,#67241,#67242,#67243,#67244,#67245,#67246,#67247,#67248,#67249,
#67250,#67251,#67252,#67253,#67254,#67255,#67256,#67257,#67258,#67259,#67260,
#67261,#67262,#67263,#67264,#67265,#67266,#67267,#67268,#67269,#67270,#67271,
#67272,#67273,#67274,#67275,#67276,#67277,#67278,#67279,#67280,#67281,#67282,
#67283,#67284,#67285,#67286,#67287,#67288,#67289,#67290,#67291,#67292,#67293,
#67294,#67295,#67296,#67297,#67298,#67299,#67300,#67301,#67302,#67303,#67304,
#67305,#67306,#67307,#67308,#67309,#67310,#67311,#67312,#67313,#67314,#67315,
#67316,#67317,#67318,#67319,#67320,#67321,#67322,#67323,#67324,#67325,#67326,
#67327,#67328,#67329,#67330,#67331,#67332,#67333,#67334,#67335,#67336,#67337,
#67338,#67339,#67340,#67341,#67342,#67343,#67344,#67345,#67346,#67347,#67348,
#67349,#67350,#67351,#67352,#67353,#67354,#67355,#67356,#67357,#67358,#67359,
#67360,#67361,#67362,#67363,#67364,#67365,#67366,#67367,#67368,#67369,#67370,
#67371,#67372,#67373,#67374,#67375,#67376,#67377,#67378,#67379,#67380,#67381,
#67382,#67383,#67384,#67385,#67386,#67387,#67388,#67389,#67390,#67391,#67392,
#67393,#67394,#67395,#67396,#67397,#67398,#67399,#67400,#67401,#67402,#67403,
#67404,#67405,#67406,#67407,#67408,#67409,#67410,#67411,#67412,#67413,#67414,
#67415,#67416,#67417,#67418,#67419,#67420,#67421,#67422,#67423,#67424,#67425,
#67426,#67427,#67428,#67429,#67430,#67431,#67432,#67433,#67434,#67435,#67436,
#67437,#67438,#67439,#67440,#67441,#67442,#67443,#67444,#67445,#67446,#67447,
#67448,#67449,#67450,#67451,#67452,#67453),(#67454,#67455,#67456,#67457,
#67458,#67459,#67460,#67461,#67462,#67463,#67464,#67465,#67466,#67467,#67468,
#67469,#67470,#67471,#67472,#67473,#67474,#67475,#67476,#67477,#67478,#67479,
#67480,#67481,#67482,#67483,#67484,#67485,#67486,#67487,#67488,#67489,#67490,
#67491,#67492,#67493,#67494,#67495,#67496,#67497,#67498,#67499,#67500,#67501,
#67502,#67503,#67504,#67505,#67506,#67507,#67508,#67509,#67510,#67511,#67512,
#67513,#67514,#67515,#67516,#67517,#67518,#67519,#67520,#67521,#67522,#67523,
#67524,#67525,#67526,#67527,#67528,#67529,#67530,#67531,#67532,#67533,#67534,
#67535,#67536,#67537,#67538,#67539,#67540,#67541,#67542,#67543,#67544,#67545,
#67546,#67547,#67548,#67549,#67550,#67551,#67552,#67553,#67554,#67555,#67556,
#67557,#67558,#67559,#67560,#67561,#67562,#67563,#67564,#67565,#67566,#67567,
#67568,#67569,#67570,#67571,#67572,#67573,#67574,#67575,#67576,#67577,#67578,
#67579,#67580,#67581,#67582,#67583,#67584,#67585,#67586,#67587,#67588,#67589,
#67590,#67591,#67592,#67593,#67594,#67595,#67596,#67597,#67598,#67599,#67600,
#67601,#67602,#67603,#67604,#67605,#67606,#67607,#67608,#67609,#67610,#67611,
#67612,#67613,#67614,#67615,#67616,#67617,#67618,#67619,#67620,#67621,#67622,
#67623,#67624,#67625,#67626,#67627,#67628,#67629,#67630,#67631,#67632,#67633,
#67634,#67635,#67636,#67637,#67638,#67639,#67640,#67641,#67642,#67643,#67644,
#67645,#67646,#67647,#67648,#67649,#67650,#67651,#67652,#67653,#67654,#67655,
#67656,#67657,#67658,#67659,#67660,#67661,#67662,#67663,#67664,#67665,#67666,
#67667,#67668,#67669,#67670,#67671,#67672,#67673,#67674,#67675,#67676,#67677,
#67678,#67679,#67680,#67681,#67682,#67683,#67684,#67685,#67686,#67687,#67688,
#67689,#67690,#67691,#67692,#67693,#67694,#67695,#67696,#67697,#67698,#67699,
#67700,#67701,#67702,#67703,#67704,#67705,#67706,#67707,#67708,#67709,#67710,
#67711,#67712,#67713,#67714,#67715,#67716,#67717,#67718,#67719,#67720,#67721,
#67722,#67723,#67724,#67725,#67726,#67727,#67728,#67729,#67730,#67731,#67732,
#67733,#67734,#67735,#67736,#67737,#67738,#67739,#67740,#67741,#67742,#67743,
#67744,#67745,#67746,#67747,#67748,#67749,#67750,#67751,#67752,#67753,#67754,
#67755,#67756,#67757,#67758,#67759,#67760,#67761,#67762,#67763,#67764,#67765,
#67766,#67767,#67768,#67769,#67770,#67771,#67772,#67773,#67774,#67775,#67776,
#67777,#67778,#67779,#67780,#67781,#67782,#67783,#67784,#67785,#67786,#67787,
#67788,#67789,#67790,#67791,#67792,#67793,#67794,#67795,#67796,#67797,#67798,
#67799,#67800,#67801,#67802,#67803,#67804,#67805,#67806,#67807,#67808,#67809,
#67810,#67811,#67812,#67813,#67814,#67815,#67816,#67817,#67818,#67819,#67820,
#67821,#67822,#67823,#67824,#67825,#67826,#67827,#67828,#67829,#67830,#67831,
#67832,#67833,#67834,#67835,#67836,#67837,#67838),(#67839,#67840,#67841,
#67842,#67843,#67844,#67845,#67846,#67847,#67848,#67849,#67850,#67851,#67852,
#67853,#67854,#67855,#67856,#67857,#67858,#67859,#67860,#67861,#67862,#67863,
#67864,#67865,#67866,#67867,#67868,#67869,#67870,#67871,#67872,#67873,#67874,
#67875,#67876,#67877,#67878,#67879,#67880,#67881,#67882,#67883,#67884,#67885,
#67886,#67887,#67888,#67889,#67890,#67891,#67892,#67893,#67894,#67895,#67896,
#67897,#67898,#67899,#67900,#67901,#67902,#67903,#67904,#67905,#67906,#67907,
#67908,#67909,#67910,#67911,#67912,#67913,#67914,#67915,#67916,#67917,#67918,
#67919,#67920,#67921,#67922,#67923,#67924,#67925,#67926,#67927,#67928,#67929,
#67930,#67931,#67932,#67933,#67934,#67935,#67936,#67937,#67938,#67939,#67940,
#67941,#67942,#67943,#67944,#67945,#67946,#67947,#67948,#67949,#67950,#67951,
#67952,#67953,#67954,#67955,#67956,#67957,#67958,#67959,#67960,#67961,#67962,
#67963,#67964,#67965,#67966,#67967,#67968,#67969,#67970,#67971,#67972,#67973,
#67974,#67975,#67976,#67977,#67978,#67979,#67980,#67981,#67982,#67983,#67984,
#67985,#67986,#67987,#67988,#67989,#67990,#67991,#67992,#67993,#67994,#67995,
#67996,#67997,#67998,#67999,#68000,#68001,#68002,#68003,#68004,#68005,#68006,
#68007,#68008,#68009,#68010,#68011,#68012,#68013,#68014,#68015,#68016,#68017,
#68018,#68019,#68020,#68021,#68022,#68023,#68024,#68025,#68026,#68027,#68028,
#68029,#68030,#68031,#68032,#68033,#68034,#68035,#68036,#68037,#68038,#68039,
#68040,#68041,#68042,#68043,#68044,#68045,#68046,#68047,#68048,#68049,#68050,
#68051,#68052,#68053,#68054,#68055,#68056,#68057,#68058,#68059,#68060,#68061,
#68062,#68063,#68064,#68065,#68066,#68067,#68068,#68069,#68070,#68071,#68072,
#68073,#68074,#68075,#68076,#68077,#68078,#68079,#68080,#68081,#68082,#68083,
#68084,#68085,#68086,#68087,#68088,#68089,#68090,#68091,#68092,#68093,#68094,
#68095,#68096,#68097,#68098,#68099,#68100,#68101,#68102,#68103,#68104,#68105,
#68106,#68107,#68108,#68109,#68110,#68111,#68112,#68113,#68114,#68115,#68116,
#68117,#68118,#68119,#68120,#68121,#68122,#68123,#68124,#68125,#68126,#68127,
#68128,#68129,#68130,#68131,#68132,#68133,#68134,#68135,#68136,#68137,#68138,
#68139,#68140,#68141,#68142,#68143,#68144,#68145,#68146,#68147,#68148,#68149,
#68150,#68151,#68152,#68153,#68154,#68155,#68156,#68157,#68158,#68159,#68160,
#68161,#68162,#68163,#68164,#68165,#68166,#68167,#68168,#68169,#68170,#68171,
#68172,#68173,#68174,#68175,#68176,#68177,#68178,#68179,#68180,#68181,#68182,
#68183,#68184,#68185,#68186,#68187,#68188,#68189,#68190,#68191,#68192,#68193,
#68194,#68195,#68196,#68197,#68198,#68199,#68200,#68201,#68202,#68203,#68204,
#68205,#68206,#68207,#68208,#68209,#68210,#68211,#68212,#68213,#68214,#68215,
#68216,#68217,#68218,#68219,#68220,#68221,#68222,#68223),(#68224,#68225,
#68226,#68227,#68228,#68229,#68230,#68231,#68232,#68233,#68234,#68235,#68236,
#68237,#68238,#68239,#68240,#68241,#68242,#68243,#68244,#68245,#68246,#68247,
#68248,#68249,#68250,#68251,#68252,#68253,#68254,#68255,#68256,#68257,#68258,
#68259,#68260,#68261,#68262,#68263,#68264,#68265,#68266,#68267,#68268,#68269,
#68270,#68271,#68272,#68273,#68274,#68275,#68276,#68277,#68278,#68279,#68280,
#68281,#68282,#68283,#68284,#68285,#68286,#68287,#68288,#68289,#68290,#68291,
#68292,#68293,#68294,#68295,#68296,#68297,#68298,#68299,#68300,#68301,#68302,
#68303,#68304,#68305,#68306,#68307,#68308,#68309,#68310,#68311,#68312,#68313,
#68314,#68315,#68316,#68317,#68318,#68319,#68320,#68321,#68322,#68323,#68324,
#68325,#68326,#68327,#68328,#68329,#68330,#68331,#68332,#68333,#68334,#68335,
#68336,#68337,#68338,#68339,#68340,#68341,#68342,#68343,#68344,#68345,#68346,
#68347,#68348,#68349,#68350,#68351,#68352,#68353,#68354,#68355,#68356,#68357,
#68358,#68359,#68360,#68361,#68362,#68363,#68364,#68365,#68366,#68367,#68368,
#68369,#68370,#68371,#68372,#68373,#68374,#68375,#68376,#68377,#68378,#68379,
#68380,#68381,#68382,#68383,#68384,#68385,#68386,#68387,#68388,#68389,#68390,
#68391,#68392,#68393,#68394,#68395,#68396,#68397,#68398,#68399,#68400,#68401,
#68402,#68403,#68404,#68405,#68406,#68407,#68408,#68409,#68410,#68411,#68412,
#68413,#68414,#68415,#68416,#68417,#68418,#68419,#68420,#68421,#68422,#68423,
#68424,#68425,#68426,#68427,#68428,#68429,#68430,#68431,#68432,#68433,#68434,
#68435,#68436,#68437,#68438,#68439,#68440,#68441,#68442,#68443,#68444,#68445,
#68446,#68447,#68448,#68449,#68450,#68451,#68452,#68453,#68454,#68455,#68456,
#68457,#68458,#68459,#68460,#68461,#68462,#68463,#68464,#68465,#68466,#68467,
#68468,#68469,#68470,#68471,#68472,#68473,#68474,#68475,#68476,#68477,#68478,
#68479,#68480,#68481,#68482,#68483,#68484,#68485,#68486,#68487,#68488,#68489,
#68490,#68491,#68492,#68493,#68494,#68495,#68496,#68497,#68498,#68499,#68500,
#68501,#68502,#68503,#68504,#68505,#68506,#68507,#68508,#68509,#68510,#68511,
#68512,#68513,#68514,#68515,#68516,#68517,#68518,#68519,#68520,#68521,#68522,
#68523,#68524,#68525,#68526,#68527,#68528,#68529,#68530,#68531,#68532,#68533,
#68534,#68535,#68536,#68537,#68538,#68539,#68540,#68541,#68542,#68543,#68544,
#68545,#68546,#68547,#68548,#68549,#68550,#68551,#68552,#68553,#68554,#68555,
#68556,#68557,#68558,#68559,#68560,#68561,#68562,#68563,#68564,#68565,#68566,
#68567,#68568,#68569,#68570,#68571,#68572,#68573,#68574,#68575,#68576,#68577,
#68578,#68579,#68580,#68581,#68582,#68583,#68584,#68585,#68586,#68587,#68588,
#68589,#68590,#68591,#68592,#68593,#68594,#68595,#68596,#68597,#68598,#68599,
#68600,#68601,#68602,#68603,#68604,#68605,#68606,#68607,#68608)),
 .UNSPECIFIED.,.F.,.F.,.F.,(4,4),(4,1,1,1,1,1,1,1,1,1,1,1,1,1,1,1,1,1,1,
1,1,1,1,1,1,1,1,1,1,1,1,1,1,1,1,1,1,1,1,1,1,1,1,1,1,1,1,1,1,1,1,1,1,1,1,
1,1,1,1,1,1,1,1,1,1,1,1,1,1,1,1,1,1,1,1,1,1,1,1,1,1,1,1,1,1,1,1,1,1,1,1,
1,1,1,1,1,1,1,1,1,1,1,1,1,1,1,1,1,1,1,1,1,1,1,1,1,1,1,1,1,1,1,1,1,1,1,1,
1,1,1,1,1,1,1,1,1,1,1,1,1,1,1,1,1,1,1,1,1,1,1,1,1,1,1,1,1,1,1,1,1,1,1,1,
1,1,1,1,1,1,1,1,1,1,1,1,1,1,1,1,1,1,1,1,1,1,1,1,1,1,1,1,1,1,1,1,1,1,1,1,
1,1,1,1,1,1,1,1,1,1,1,1,1,1,1,1,1,1,1,1,1,1,1,1,1,1,1,1,1,1,1,1,1,1,1,1,
1,1,1,1,1,1,1,1,1,1,1,1,1,1,1,1,1,1,1,1,1,1,1,1,1,1,1,1,1,1,1,1,1,1,1,1,
1,1,1,1,1,1,1,1,1,1,1,1,1,1,1,1,1,1,1,1,1,1,1,1,1,1,1,1,1,1,1,1,1,1,1,1,
1,1,1,1,1,1,1,1,1,1,1,1,1,1,1,1,1,1,1,1,1,1,1,1,1,1,1,1,1,1,1,1,1,1,1,1,
1,1,1,1,1,1,1,1,1,1,1,1,1,1,1,1,1,1,1,1,1,1,1,1,1,1,1,1,1,1,1,1,1,1,1,1,
1,1,1,4),(0.,0.0658179306876174),(11.6150328478191,12.1137944921691,12.6125561365191,
13.6100794252191,14.6076027139191,15.6051260026191,16.6026492913191,17.6001725800191,
18.5976958687191,19.5952191574192,20.5927424461192,21.5902657348192,22.5877890235192,
23.5853123122192,24.5828356009192,25.5803588896192,26.5778821783192,27.5754054670192,
28.5729287557192,29.5704520444192,30.5679753331192,31.5654986218192,32.5630219105192,
33.5605451992192,34.5580684879192,35.5555917766192,36.5531150653192,37.5506383540192,
38.5481616427193,39.5456849314193,40.5432082201193,41.5407315088193,42.5382547975193,
43.5357780862193,44.5333013749193,45.5308246636193,46.5283479523193,47.5258712410193,
48.5233945297193,49.5209178184193,50.5184411071193,51.5159643958193,52.5134876845193,
53.5110109732193,54.5085342619193,55.5060575506193,56.5035808393194,57.5011041280194,
58.4986274167194,59.4961507054194,60.4936739941194,61.4911972828194,62.4887205715194,
63.4862438602194,64.4837671489194,65.4812904376194,66.4788137263194,67.4763370150194,
68.4738603037194,69.4713835924194,70.4689068811194,71.4664301698194,72.4639534585194,
73.4614767472195,74.4590000359194,75.4565233246195,76.4540466133195,77.4515699020195,
78.4490931907195,79.4466164794195,80.4441397681195,81.4416630568195,82.4391863455195,
83.4367096342195,84.4342329229195,85.4317562116195,86.4292795003195,87.4268027890195,
88.4243260777195,89.4218493664195,90.4193726551195,91.4168959438195,92.4144192325195,
93.4119425212196,94.4094658099196,95.4069890986196,96.4045123873196,97.4020356760196,
98.3995589647196,99.3970822534196,100.39460554212,101.39212883082,102.38965211952,
103.38717540822,104.38469869692,105.38222198562,106.37974527432,107.37726856302,
108.37479185172,109.37231514042,110.36983842912,111.36736171782,112.36488500652,
113.36240829522,114.35993158392,115.35745487262,116.35497816132,117.35250145002,
118.35002473872,119.34754802742,120.34507131612,121.34259460482,122.34011789352,
123.33764118222,124.33516447092,125.33268775962,126.33021104832,127.32773433702,
128.32525762572,129.32278091442,130.32030420312,131.31782749182,132.31535078052,
133.31287406922,134.31039735792,135.30792064662,136.30544393532,137.30296722402,
138.30049051272,139.29801380142,140.29553709012,141.29306037882,142.29058366752,
143.28810695622,144.28563024492,145.28315353362,146.28067682232,147.27820011102,
148.27572339972,149.27324668842,150.27076997712,151.26829326582,152.26581655452,
153.26333984322,154.26086313192,155.25838642062,156.25590970932,157.25343299802,
158.25095628672,159.24847957542,160.24600286412,161.24352615282,162.24104944152,
163.23857273022,164.23609601892,165.23361930762,166.23114259632,167.22866588502,
168.22618917372,169.22371246242,170.22123575112,171.21875903982,172.21628232852,
173.21380561722,174.21132890592,175.20885219462,176.20637548332,177.20389877202,
178.20142206072,179.19894534942,180.19646863812,181.19399192682,182.19151521552,
183.18903850422,184.18656179292,185.18408508162,186.18160837032,187.17913165902,
188.17665494772,189.17417823642,190.17170152512,191.16922481382,192.16674810252,
193.16427139122,194.16179467992,195.15931796862,196.15684125732,197.15436454602,
198.15188783472,199.14941112342,200.14693441212,201.14445770082,202.14198098952,
203.13950427822,204.13702756692,205.13455085562,206.13207414432,207.12959743302,
208.12712072172,209.12464401042,210.12216729912,211.11969058782,212.11721387652,
213.11473716522,214.11226045392,215.10978374262,216.10730703132,217.10483032002,
218.10235360872,219.09987689742,220.09740018612,221.09492347482,222.09244676352,
223.08997005222,224.08749334092,225.08501662962,226.08253991832,227.08006320702,
228.07758649572,229.07510978442,230.07263307312,231.07015636182,232.06767965052,
233.06520293922,234.06272622792,235.06024951662,236.05777280532,237.05529609402,
238.05281938272,239.05034267142,240.04786596012,241.04538924882,242.04291253752,
243.04043582622,244.03795911492,245.03548240362,246.03300569232,247.03052898102,
248.02805226972,249.02557555842,250.02309884712,251.02062213582,252.01814542452,
253.01566871322,254.01319200192,255.01071529062,256.00823857932,257.00576186802,
258.00328515672,259.00080844542,259.99833173412,260.99585502282,261.99337831152,
262.99090160022,263.98842488892,264.98594817762,265.983471466321,266.980994755021,
267.97851804372,268.97604133242,269.973564621121,270.971087909821,271.968611198521,
272.966134487221,273.963657775921,274.961181064621,275.958704353321,276.956227642021,
277.953750930721,278.951274219421,279.948797508121,280.946320796821,281.943844085521,
282.941367374221,283.938890662921,284.936413951621,285.933937240321,286.931460529021,
287.928983817721,288.926507106421,289.924030395121,290.921553683821,291.919076972521,
292.916600261221,293.914123549921,294.911646838621,295.909170127321,296.906693416021,
297.904216704721,298.901739993421,299.899263282121,300.896786570821,301.894309859521,
302.891833148221,303.889356436921,304.886879725621,305.884403014321,306.881926303021,
307.879449591721,308.876972880421,309.874496169121,310.872019457821,311.869542746521,
312.867066035221,313.864589323921,314.862112612621,315.859635901321,316.857159190021,
317.854682478721,318.852205767421,319.849729056121,320.847252344821,321.844775633521,
322.842298922221,323.839822210921,324.837345499621,325.834868788321,326.832392077021,
327.829915365721,328.827438654421,329.824961943121,330.822485231821,331.820008520521,
332.817531809221,333.815055097921,334.812578386621,335.810101675321,336.807624964021,
337.805148252721,338.802671541421,339.800194830121,340.797718118821,341.795241407521,
342.792764696221,343.790287984921,344.787811273621,345.785334562321,346.782857851021,
347.780381139721,348.777904428421,349.775427717121,350.772951005821,351.770474294521,
352.767997583221,353.765520871921,354.763044160621,355.760567449321,356.758090738021,
357.755614026721,358.753137315421,359.750660604121,360.748183892821,361.745707181521,
362.743230470221,363.740753758921,364.738277047621,365.735800336321,366.733323625021,
367.730846913721,368.728370202421,369.725893491121,370.723416779821,371.720940068521,
372.718463357221,373.715986645921,374.713509934621,375.711033223321,376.708556512021,
377.706079800721,378.703603089421,379.701126378121,380.698649666821,381.696172955521,
382.693696244221,383.691219532921,384.688742821621,385.686266110321,386.683789399021,
387.681312687721,388.678835976421,389.676359265121,390.175120909471,390.673882553821),
 .UNSPECIFIED.);
#358=B_SPLINE_SURFACE_WITH_KNOTS('',3,3,((#69471,#69472,#69473,#69474,#69475,
#69476,#69477,#69478,#69479,#69480,#69481,#69482,#69483,#69484,#69485,#69486,
#69487,#69488,#69489,#69490,#69491,#69492,#69493,#69494,#69495,#69496,#69497,
#69498,#69499,#69500,#69501,#69502,#69503,#69504,#69505,#69506,#69507,#69508,
#69509,#69510,#69511,#69512,#69513,#69514,#69515,#69516,#69517,#69518,#69519,
#69520,#69521,#69522,#69523,#69524,#69525,#69526,#69527,#69528),(#69529,
#69530,#69531,#69532,#69533,#69534,#69535,#69536,#69537,#69538,#69539,#69540,
#69541,#69542,#69543,#69544,#69545,#69546,#69547,#69548,#69549,#69550,#69551,
#69552,#69553,#69554,#69555,#69556,#69557,#69558,#69559,#69560,#69561,#69562,
#69563,#69564,#69565,#69566,#69567,#69568,#69569,#69570,#69571,#69572,#69573,
#69574,#69575,#69576,#69577,#69578,#69579,#69580,#69581,#69582,#69583,#69584,
#69585,#69586),(#69587,#69588,#69589,#69590,#69591,#69592,#69593,#69594,
#69595,#69596,#69597,#69598,#69599,#69600,#69601,#69602,#69603,#69604,#69605,
#69606,#69607,#69608,#69609,#69610,#69611,#69612,#69613,#69614,#69615,#69616,
#69617,#69618,#69619,#69620,#69621,#69622,#69623,#69624,#69625,#69626,#69627,
#69628,#69629,#69630,#69631,#69632,#69633,#69634,#69635,#69636,#69637,#69638,
#69639,#69640,#69641,#69642,#69643,#69644),(#69645,#69646,#69647,#69648,
#69649,#69650,#69651,#69652,#69653,#69654,#69655,#69656,#69657,#69658,#69659,
#69660,#69661,#69662,#69663,#69664,#69665,#69666,#69667,#69668,#69669,#69670,
#69671,#69672,#69673,#69674,#69675,#69676,#69677,#69678,#69679,#69680,#69681,
#69682,#69683,#69684,#69685,#69686,#69687,#69688,#69689,#69690,#69691,#69692,
#69693,#69694,#69695,#69696,#69697,#69698,#69699,#69700,#69701,#69702)),
 .UNSPECIFIED.,.F.,.F.,.F.,(4,4),(4,1,1,1,1,1,1,1,1,1,1,1,1,1,1,1,1,1,1,
1,1,1,1,1,1,1,1,1,1,1,1,1,1,1,1,1,1,1,1,1,1,1,1,1,1,1,1,1,1,1,1,1,1,1,1,
4),(0.,0.0641840294258107),(11.8589888623078,12.3522141756159,12.8454394889239,
13.8318901155401,14.8183407421562,15.8047913687724,16.7912419953885,17.7776926220047,
18.7641432486208,19.750593875237,20.7370445018531,21.7234951284693,22.7099457550854,
23.6963963817016,24.6828470083177,25.6692976349339,26.65574826155,27.6421988881662,
28.6286495147823,29.6151001413985,30.6015507680146,31.5880013946308,32.5744520212469,
33.5609026478631,34.5473532744792,35.5338039010954,36.5202545277115,37.5067051543277,
38.4931557809438,39.47960640756,40.4660570341761,41.4525076607923,42.4389582874084,
43.4254089140245,44.4118595406407,45.3983101672568,46.384760793873,47.3712114204891,
48.3576620471053,49.3441126737214,50.3305633003376,51.3170139269537,52.3034645535699,
53.289915180186,54.2763658068022,55.2628164334183,56.2492670600345,57.2357176866506,
58.2221683132668,59.2086189398829,60.1950695664991,61.1815201931152,62.1679708197314,
63.1544214463475,63.6476467596556,64.1408720729637),.UNSPECIFIED.);
#359=B_SPLINE_SURFACE_WITH_KNOTS('',3,3,((#69937,#69938,#69939,#69940,#69941,
#69942,#69943,#69944,#69945,#69946,#69947,#69948,#69949,#69950,#69951,#69952,
#69953,#69954,#69955,#69956,#69957,#69958,#69959,#69960,#69961,#69962,#69963,
#69964,#69965,#69966,#69967,#69968,#69969,#69970,#69971,#69972,#69973,#69974,
#69975,#69976,#69977,#69978,#69979,#69980,#69981,#69982,#69983,#69984,#69985,
#69986,#69987,#69988,#69989,#69990,#69991,#69992,#69993,#69994),(#69995,
#69996,#69997,#69998,#69999,#70000,#70001,#70002,#70003,#70004,#70005,#70006,
#70007,#70008,#70009,#70010,#70011,#70012,#70013,#70014,#70015,#70016,#70017,
#70018,#70019,#70020,#70021,#70022,#70023,#70024,#70025,#70026,#70027,#70028,
#70029,#70030,#70031,#70032,#70033,#70034,#70035,#70036,#70037,#70038,#70039,
#70040,#70041,#70042,#70043,#70044,#70045,#70046,#70047,#70048,#70049,#70050,
#70051,#70052),(#70053,#70054,#70055,#70056,#70057,#70058,#70059,#70060,
#70061,#70062,#70063,#70064,#70065,#70066,#70067,#70068,#70069,#70070,#70071,
#70072,#70073,#70074,#70075,#70076,#70077,#70078,#70079,#70080,#70081,#70082,
#70083,#70084,#70085,#70086,#70087,#70088,#70089,#70090,#70091,#70092,#70093,
#70094,#70095,#70096,#70097,#70098,#70099,#70100,#70101,#70102,#70103,#70104,
#70105,#70106,#70107,#70108,#70109,#70110),(#70111,#70112,#70113,#70114,
#70115,#70116,#70117,#70118,#70119,#70120,#70121,#70122,#70123,#70124,#70125,
#70126,#70127,#70128,#70129,#70130,#70131,#70132,#70133,#70134,#70135,#70136,
#70137,#70138,#70139,#70140,#70141,#70142,#70143,#70144,#70145,#70146,#70147,
#70148,#70149,#70150,#70151,#70152,#70153,#70154,#70155,#70156,#70157,#70158,
#70159,#70160,#70161,#70162,#70163,#70164,#70165,#70166,#70167,#70168)),
 .UNSPECIFIED.,.F.,.F.,.F.,(4,4),(4,1,1,1,1,1,1,1,1,1,1,1,1,1,1,1,1,1,1,
1,1,1,1,1,1,1,1,1,1,1,1,1,1,1,1,1,1,1,1,1,1,1,1,1,1,1,1,1,1,1,1,1,1,1,1,
4),(0.,0.0641840294258107),(14.3989442667811,14.8921695800892,15.3853948933972,
16.3718455200134,17.3582961466295,18.3447467732457,19.3311973998618,20.317648026478,
21.3040986530941,22.2905492797103,23.2769999063264,24.2634505329426,25.2499011595587,
26.2363517861749,27.222802412791,28.2092530394072,29.1957036660233,30.1821542926395,
31.1686049192556,32.1550555458718,33.1415061724879,34.1279567991041,35.1144074257202,
36.1008580523364,37.0873086789525,38.0737593055687,39.0602099321848,40.046660558801,
41.0331111854171,42.0195618120333,43.0060124386494,43.9924630652656,44.9789136918817,
45.9653643184979,46.951814945114,47.9382655717301,48.9247161983463,49.9111668249625,
50.8976174515786,51.8840680781948,52.8705187048109,53.856969331427,54.8434199580432,
55.8298705846593,56.8163212112755,57.8027718378916,58.7892224645078,59.7756730911239,
60.7621237177401,61.7485743443562,62.7350249709724,63.7214755975885,64.7079262242047,
65.6943768508208,66.1876021641289,66.680827477437),.UNSPECIFIED.);
#360=B_SPLINE_SURFACE_WITH_KNOTS('',3,3,((#71871,#71872,#71873,#71874,#71875,
#71876,#71877,#71878,#71879,#71880,#71881,#71882,#71883,#71884,#71885,#71886,
#71887,#71888,#71889,#71890,#71891,#71892,#71893,#71894,#71895,#71896,#71897,
#71898,#71899,#71900,#71901,#71902,#71903,#71904,#71905,#71906,#71907,#71908,
#71909,#71910,#71911,#71912,#71913,#71914,#71915,#71916,#71917,#71918,#71919,
#71920,#71921,#71922,#71923,#71924,#71925,#71926,#71927,#71928,#71929,#71930,
#71931,#71932,#71933,#71934,#71935,#71936,#71937,#71938,#71939,#71940,#71941,
#71942,#71943,#71944,#71945,#71946,#71947,#71948,#71949,#71950,#71951,#71952,
#71953,#71954,#71955,#71956,#71957,#71958,#71959,#71960,#71961,#71962,#71963,
#71964,#71965,#71966,#71967,#71968,#71969,#71970,#71971,#71972),(#71973,
#71974,#71975,#71976,#71977,#71978,#71979,#71980,#71981,#71982,#71983,#71984,
#71985,#71986,#71987,#71988,#71989,#71990,#71991,#71992,#71993,#71994,#71995,
#71996,#71997,#71998,#71999,#72000,#72001,#72002,#72003,#72004,#72005,#72006,
#72007,#72008,#72009,#72010,#72011,#72012,#72013,#72014,#72015,#72016,#72017,
#72018,#72019,#72020,#72021,#72022,#72023,#72024,#72025,#72026,#72027,#72028,
#72029,#72030,#72031,#72032,#72033,#72034,#72035,#72036,#72037,#72038,#72039,
#72040,#72041,#72042,#72043,#72044,#72045,#72046,#72047,#72048,#72049,#72050,
#72051,#72052,#72053,#72054,#72055,#72056,#72057,#72058,#72059,#72060,#72061,
#72062,#72063,#72064,#72065,#72066,#72067,#72068,#72069,#72070,#72071,#72072,
#72073,#72074),(#72075,#72076,#72077,#72078,#72079,#72080,#72081,#72082,
#72083,#72084,#72085,#72086,#72087,#72088,#72089,#72090,#72091,#72092,#72093,
#72094,#72095,#72096,#72097,#72098,#72099,#72100,#72101,#72102,#72103,#72104,
#72105,#72106,#72107,#72108,#72109,#72110,#72111,#72112,#72113,#72114,#72115,
#72116,#72117,#72118,#72119,#72120,#72121,#72122,#72123,#72124,#72125,#72126,
#72127,#72128,#72129,#72130,#72131,#72132,#72133,#72134,#72135,#72136,#72137,
#72138,#72139,#72140,#72141,#72142,#72143,#72144,#72145,#72146,#72147,#72148,
#72149,#72150,#72151,#72152,#72153,#72154,#72155,#72156,#72157,#72158,#72159,
#72160,#72161,#72162,#72163,#72164,#72165,#72166,#72167,#72168,#72169,#72170,
#72171,#72172,#72173,#72174,#72175,#72176),(#72177,#72178,#72179,#72180,
#72181,#72182,#72183,#72184,#72185,#72186,#72187,#72188,#72189,#72190,#72191,
#72192,#72193,#72194,#72195,#72196,#72197,#72198,#72199,#72200,#72201,#72202,
#72203,#72204,#72205,#72206,#72207,#72208,#72209,#72210,#72211,#72212,#72213,
#72214,#72215,#72216,#72217,#72218,#72219,#72220,#72221,#72222,#72223,#72224,
#72225,#72226,#72227,#72228,#72229,#72230,#72231,#72232,#72233,#72234,#72235,
#72236,#72237,#72238,#72239,#72240,#72241,#72242,#72243,#72244,#72245,#72246,
#72247,#72248,#72249,#72250,#72251,#72252,#72253,#72254,#72255,#72256,#72257,
#72258,#72259,#72260,#72261,#72262,#72263,#72264,#72265,#72266,#72267,#72268,
#72269,#72270,#72271,#72272,#72273,#72274,#72275,#72276,#72277,#72278)),
 .UNSPECIFIED.,.F.,.F.,.F.,(4,4),(4,1,1,1,1,1,1,1,1,1,1,1,1,1,1,1,1,1,1,
1,1,1,1,1,1,1,1,1,1,1,1,1,1,1,1,1,1,1,1,1,1,1,1,1,1,1,1,1,1,1,1,1,1,1,1,
1,1,1,1,1,1,1,1,1,1,1,1,1,1,1,1,1,1,1,1,1,1,1,1,1,1,1,1,1,1,1,1,1,1,1,1,
1,1,1,1,1,1,1,1,4),(0.,0.0658467982010768),(11.6150328478182,12.6069034617266,
13.598774075635,14.5906446895433,15.5825153034517,16.5743859173601,17.5662565312685,
18.5581271451769,19.5499977590852,20.5418683729936,21.533738986902,22.5256096008104,
23.5174802147187,24.5093508286271,25.5012214425355,26.4930920564439,27.4849626703523,
28.4768332842606,29.468703898169,30.4605745120774,31.4524451259858,32.4443157398941,
33.4361863538025,34.4280569677109,35.4199275816193,36.4117981955277,37.403668809436,
38.3955394233444,39.3874100372528,40.3792806511612,41.3711512650695,42.3630218789779,
43.3548924928863,44.3467631067947,45.3386337207031,46.3305043346114,47.3223749485198,
48.3142455624282,49.3061161763366,50.2979867902449,51.2898574041533,52.2817280180617,
53.2735986319701,54.2654692458785,55.2573398597868,56.2492104736952,57.2410810876036,
58.232951701512,59.2248223154203,60.2166929293287,61.2085635432371,62.2004341571455,
63.1923047710539,64.1841753849622,65.1760459988706,66.167916612779,67.1597872266874,
68.1516578405957,69.1435284545041,70.1353990684125,71.1272696823209,72.1191402962293,
73.1110109101376,74.102881524046,75.0947521379544,76.0866227518628,77.0784933657711,
78.0703639796795,79.0622345935879,80.0541052074963,81.0459758214047,82.037846435313,
83.0297170492214,84.0215876631298,85.0134582770382,86.0053288909465,86.9971995048549,
87.9890701187633,88.9809407326717,89.9728113465801,90.9646819604884,91.9565525743968,
92.9484231883052,93.9402938022136,94.9321644161219,95.9240350300303,96.9159056439387,
97.9077762578471,98.8996468717555,99.8915174856638,100.883388099572,101.875258713481,
102.867129327389,103.858999941297,104.850870555206,105.842741169114,106.834611783022,
107.826482396931,108.818353010839,109.810223624748),.UNSPECIFIED.);
#361=B_SPLINE_SURFACE_WITH_KNOTS('',3,3,((#72407,#72408,#72409,#72410,#72411,
#72412,#72413,#72414,#72415,#72416,#72417,#72418,#72419,#72420,#72421,#72422,
#72423,#72424,#72425,#72426,#72427,#72428,#72429,#72430,#72431,#72432,#72433,
#72434,#72435,#72436,#72437,#72438,#72439,#72440,#72441,#72442,#72443,#72444,
#72445,#72446,#72447,#72448,#72449,#72450,#72451,#72452,#72453,#72454,#72455,
#72456,#72457,#72458,#72459,#72460,#72461,#72462,#72463,#72464,#72465,#72466,
#72467,#72468,#72469,#72470,#72471,#72472,#72473,#72474,#72475,#72476,#72477,
#72478,#72479,#72480,#72481,#72482,#72483,#72484,#72485,#72486,#72487,#72488,
#72489,#72490,#72491,#72492,#72493,#72494,#72495,#72496,#72497,#72498,#72499,
#72500,#72501,#72502,#72503,#72504,#72505,#72506,#72507,#72508,#72509,#72510),
(#72511,#72512,#72513,#72514,#72515,#72516,#72517,#72518,#72519,#72520,
#72521,#72522,#72523,#72524,#72525,#72526,#72527,#72528,#72529,#72530,#72531,
#72532,#72533,#72534,#72535,#72536,#72537,#72538,#72539,#72540,#72541,#72542,
#72543,#72544,#72545,#72546,#72547,#72548,#72549,#72550,#72551,#72552,#72553,
#72554,#72555,#72556,#72557,#72558,#72559,#72560,#72561,#72562,#72563,#72564,
#72565,#72566,#72567,#72568,#72569,#72570,#72571,#72572,#72573,#72574,#72575,
#72576,#72577,#72578,#72579,#72580,#72581,#72582,#72583,#72584,#72585,#72586,
#72587,#72588,#72589,#72590,#72591,#72592,#72593,#72594,#72595,#72596,#72597,
#72598,#72599,#72600,#72601,#72602,#72603,#72604,#72605,#72606,#72607,#72608,
#72609,#72610,#72611,#72612,#72613,#72614),(#72615,#72616,#72617,#72618,
#72619,#72620,#72621,#72622,#72623,#72624,#72625,#72626,#72627,#72628,#72629,
#72630,#72631,#72632,#72633,#72634,#72635,#72636,#72637,#72638,#72639,#72640,
#72641,#72642,#72643,#72644,#72645,#72646,#72647,#72648,#72649,#72650,#72651,
#72652,#72653,#72654,#72655,#72656,#72657,#72658,#72659,#72660,#72661,#72662,
#72663,#72664,#72665,#72666,#72667,#72668,#72669,#72670,#72671,#72672,#72673,
#72674,#72675,#72676,#72677,#72678,#72679,#72680,#72681,#72682,#72683,#72684,
#72685,#72686,#72687,#72688,#72689,#72690,#72691,#72692,#72693,#72694,#72695,
#72696,#72697,#72698,#72699,#72700,#72701,#72702,#72703,#72704,#72705,#72706,
#72707,#72708,#72709,#72710,#72711,#72712,#72713,#72714,#72715,#72716,#72717,
#72718),(#72719,#72720,#72721,#72722,#72723,#72724,#72725,#72726,#72727,
#72728,#72729,#72730,#72731,#72732,#72733,#72734,#72735,#72736,#72737,#72738,
#72739,#72740,#72741,#72742,#72743,#72744,#72745,#72746,#72747,#72748,#72749,
#72750,#72751,#72752,#72753,#72754,#72755,#72756,#72757,#72758,#72759,#72760,
#72761,#72762,#72763,#72764,#72765,#72766,#72767,#72768,#72769,#72770,#72771,
#72772,#72773,#72774,#72775,#72776,#72777,#72778,#72779,#72780,#72781,#72782,
#72783,#72784,#72785,#72786,#72787,#72788,#72789,#72790,#72791,#72792,#72793,
#72794,#72795,#72796,#72797,#72798,#72799,#72800,#72801,#72802,#72803,#72804,
#72805,#72806,#72807,#72808,#72809,#72810,#72811,#72812,#72813,#72814,#72815,
#72816,#72817,#72818,#72819,#72820,#72821,#72822)),.UNSPECIFIED.,.F.,.F.,
 .F.,(4,4),(4,1,1,1,1,1,1,1,1,1,1,1,1,1,1,1,1,1,1,1,1,1,1,1,1,1,1,1,1,1,
1,1,1,1,1,1,1,1,1,1,1,1,1,1,1,1,1,1,1,1,1,1,1,1,1,1,1,1,1,1,1,1,1,1,1,1,
1,1,1,1,1,1,1,1,1,1,1,1,1,1,1,1,1,1,1,1,1,1,1,1,1,1,1,1,1,1,1,1,1,1,1,4),
(0.,0.0658467982010768),(8.30747755240101,9.30018873014199,10.292899907883,
11.2856110856239,12.2783222633649,13.2710334411059,14.2637446188469,15.2564557965878,
16.2491669743288,17.2418781520698,18.2345893298108,19.2273005075518,20.2200116852927,
21.2127228630337,22.2054340407747,23.1981452185157,24.1908563962566,25.1835675739976,
26.1762787517386,27.1689899294796,28.1617011072206,29.1544122849615,30.1471234627025,
31.1398346404435,32.1325458181845,33.1252569959254,34.1179681736664,35.1106793514074,
36.1033905291484,37.0961017068893,38.0888128846303,39.0815240623713,40.0742352401123,
41.0669464178533,42.0596575955942,43.0523687733352,44.0450799510762,45.0377911288172,
46.0305023065581,47.0232134842991,48.0159246620401,49.0086358397811,50.001347017522,
50.994058195263,51.986769373004,52.979480550745,53.972191728486,54.9649029062269,
55.9576140839679,56.9503252617089,57.9430364394499,58.9357476171908,59.9284587949318,
60.9211699726728,61.9138811504138,62.9065923281547,63.8993035058957,64.8920146836367,
65.8847258613777,66.8774370391187,67.8701482168596,68.8628593946006,69.8555705723416,
70.8482817500825,71.8409929278235,72.8337041055645,73.8264152833055,74.8191264610465,
75.8118376387874,76.8045488165284,77.7972599942694,78.7899711720104,79.7826823497514,
80.7753935274923,81.7681047052333,82.7608158829743,83.7535270607153,84.7462382384562,
85.7389494161972,86.7316605939382,87.7243717716792,88.7170829494201,89.7097941271611,
90.7025053049021,91.6952164826431,92.687927660384,93.680638838125,94.673350015866,
95.666061193607,96.658772371348,97.6514835490889,98.6441947268299,99.6369059045709,
100.629617082312,101.622328260053,102.615039437794,103.607750615535,104.600461793276,
105.593172971017,106.585884148758,107.578595326499,108.57130650424),
 .UNSPECIFIED.);
#362=B_SPLINE_SURFACE_WITH_KNOTS('',3,3,((#81643,#81644,#81645,#81646,#81647,
#81648,#81649,#81650,#81651,#81652,#81653,#81654,#81655,#81656,#81657,#81658,
#81659,#81660,#81661,#81662,#81663,#81664,#81665,#81666,#81667,#81668,#81669,
#81670,#81671,#81672,#81673,#81674,#81675,#81676,#81677,#81678,#81679,#81680,
#81681,#81682,#81683,#81684,#81685,#81686,#81687,#81688,#81689,#81690,#81691,
#81692,#81693,#81694,#81695,#81696,#81697,#81698,#81699,#81700,#81701,#81702,
#81703,#81704,#81705,#81706,#81707,#81708,#81709,#81710,#81711,#81712,#81713,
#81714,#81715,#81716,#81717,#81718,#81719,#81720,#81721,#81722,#81723,#81724,
#81725,#81726,#81727,#81728,#81729,#81730,#81731,#81732,#81733,#81734,#81735,
#81736,#81737,#81738,#81739,#81740,#81741,#81742,#81743,#81744,#81745,#81746,
#81747,#81748,#81749,#81750,#81751,#81752,#81753,#81754,#81755,#81756,#81757,
#81758,#81759,#81760,#81761,#81762,#81763,#81764,#81765,#81766,#81767,#81768,
#81769,#81770,#81771,#81772,#81773),(#81774,#81775,#81776,#81777,#81778,
#81779,#81780,#81781,#81782,#81783,#81784,#81785,#81786,#81787,#81788,#81789,
#81790,#81791,#81792,#81793,#81794,#81795,#81796,#81797,#81798,#81799,#81800,
#81801,#81802,#81803,#81804,#81805,#81806,#81807,#81808,#81809,#81810,#81811,
#81812,#81813,#81814,#81815,#81816,#81817,#81818,#81819,#81820,#81821,#81822,
#81823,#81824,#81825,#81826,#81827,#81828,#81829,#81830,#81831,#81832,#81833,
#81834,#81835,#81836,#81837,#81838,#81839,#81840,#81841,#81842,#81843,#81844,
#81845,#81846,#81847,#81848,#81849,#81850,#81851,#81852,#81853,#81854,#81855,
#81856,#81857,#81858,#81859,#81860,#81861,#81862,#81863,#81864,#81865,#81866,
#81867,#81868,#81869,#81870,#81871,#81872,#81873,#81874,#81875,#81876,#81877,
#81878,#81879,#81880,#81881,#81882,#81883,#81884,#81885,#81886,#81887,#81888,
#81889,#81890,#81891,#81892,#81893,#81894,#81895,#81896,#81897,#81898,#81899,
#81900,#81901,#81902,#81903,#81904),(#81905,#81906,#81907,#81908,#81909,
#81910,#81911,#81912,#81913,#81914,#81915,#81916,#81917,#81918,#81919,#81920,
#81921,#81922,#81923,#81924,#81925,#81926,#81927,#81928,#81929,#81930,#81931,
#81932,#81933,#81934,#81935,#81936,#81937,#81938,#81939,#81940,#81941,#81942,
#81943,#81944,#81945,#81946,#81947,#81948,#81949,#81950,#81951,#81952,#81953,
#81954,#81955,#81956,#81957,#81958,#81959,#81960,#81961,#81962,#81963,#81964,
#81965,#81966,#81967,#81968,#81969,#81970,#81971,#81972,#81973,#81974,#81975,
#81976,#81977,#81978,#81979,#81980,#81981,#81982,#81983,#81984,#81985,#81986,
#81987,#81988,#81989,#81990,#81991,#81992,#81993,#81994,#81995,#81996,#81997,
#81998,#81999,#82000,#82001,#82002,#82003,#82004,#82005,#82006,#82007,#82008,
#82009,#82010,#82011,#82012,#82013,#82014,#82015,#82016,#82017,#82018,#82019,
#82020,#82021,#82022,#82023,#82024,#82025,#82026,#82027,#82028,#82029,#82030,
#82031,#82032,#82033,#82034,#82035),(#82036,#82037,#82038,#82039,#82040,
#82041,#82042,#82043,#82044,#82045,#82046,#82047,#82048,#82049,#82050,#82051,
#82052,#82053,#82054,#82055,#82056,#82057,#82058,#82059,#82060,#82061,#82062,
#82063,#82064,#82065,#82066,#82067,#82068,#82069,#82070,#82071,#82072,#82073,
#82074,#82075,#82076,#82077,#82078,#82079,#82080,#82081,#82082,#82083,#82084,
#82085,#82086,#82087,#82088,#82089,#82090,#82091,#82092,#82093,#82094,#82095,
#82096,#82097,#82098,#82099,#82100,#82101,#82102,#82103,#82104,#82105,#82106,
#82107,#82108,#82109,#82110,#82111,#82112,#82113,#82114,#82115,#82116,#82117,
#82118,#82119,#82120,#82121,#82122,#82123,#82124,#82125,#82126,#82127,#82128,
#82129,#82130,#82131,#82132,#82133,#82134,#82135,#82136,#82137,#82138,#82139,
#82140,#82141,#82142,#82143,#82144,#82145,#82146,#82147,#82148,#82149,#82150,
#82151,#82152,#82153,#82154,#82155,#82156,#82157,#82158,#82159,#82160,#82161,
#82162,#82163,#82164,#82165,#82166)),.UNSPECIFIED.,.F.,.F.,.F.,(4,4),(4,
1,1,1,1,1,1,1,1,1,1,1,1,1,1,1,1,1,1,1,1,1,1,1,1,1,1,1,1,1,1,1,1,1,1,1,1,
1,1,1,1,1,1,1,1,1,1,1,1,1,1,1,1,1,1,1,1,1,1,1,1,1,1,1,1,1,1,1,1,1,1,1,1,
1,1,1,1,1,1,1,1,1,1,1,1,1,1,1,1,1,1,1,1,1,1,1,1,1,1,1,1,1,1,1,1,1,1,1,1,
1,1,1,1,1,1,1,1,1,1,1,1,1,1,1,1,1,1,1,4),(0.,0.0642013499338863),(11.8589888623077,
12.8564939485313,13.8539990347549,14.8515041209785,15.8490092072021,16.8465142934257,
17.8440193796493,18.8415244658729,19.8390295520965,20.8365346383201,21.8340397245437,
22.8315448107673,23.8290498969909,24.8265549832145,25.8240600694381,26.8215651556617,
27.8190702418853,28.8165753281089,29.8140804143324,30.811585500556,31.8090905867796,
32.8065956730032,33.8041007592268,34.8016058454504,35.799110931674,36.7966160178976,
37.7941211041212,38.7916261903448,39.7891312765684,40.786636362792,41.7841414490156,
42.7816465352392,43.7791516214628,44.7766567076864,45.77416179391,46.7716668801336,
47.7691719663572,48.7666770525807,49.7641821388043,50.7616872250279,51.7591923112515,
52.7566973974751,53.7542024836987,54.7517075699223,55.7492126561459,56.7467177423695,
57.7442228285931,58.7417279148167,59.7392330010403,60.7367380872639,61.7342431734875,
62.7317482597111,63.7292533459347,64.7267584321583,65.7242635183819,66.7217686046055,
67.7192736908291,68.7167787770527,69.7142838632763,70.7117889494998,71.7092940357234,
72.706799121947,73.7043042081706,74.7018092943942,75.6993143806178,76.6968194668414,
77.694324553065,78.6918296392886,79.6893347255122,80.6868398117358,81.6843448979594,
82.681849984183,83.6793550704066,84.6768601566302,85.6743652428538,86.6718703290774,
87.669375415301,88.6668805015246,89.6643855877482,90.6618906739717,91.6593957601953,
92.6569008464189,93.6544059326425,94.6519110188661,95.6494161050897,96.6469211913133,
97.6444262775369,98.6419313637605,99.6394364499841,100.636941536208,101.634446622431,
102.631951708655,103.629456794878,104.626961881102,105.624466967326,106.621972053549,
107.619477139773,108.616982225996,109.61448731222,110.611992398444,111.609497484667,
112.607002570891,113.604507657114,114.602012743338,115.599517829562,116.597022915785,
117.594528002009,118.592033088232,119.589538174456,120.58704326068,121.584548346903,
122.582053433127,123.57955851935,124.577063605574,125.574568691798,126.572073778021,
127.569578864245,128.567083950468,129.564589036692,130.562094122916,131.559599209139,
132.557104295363,133.554609381586,134.55211446781,135.549619554034,136.547124640257,
137.544629726481,138.542134812704,139.539639898928),.UNSPECIFIED.);
#363=B_SPLINE_SURFACE_WITH_KNOTS('',3,3,((#82380,#82381,#82382,#82383,#82384,
#82385,#82386,#82387,#82388,#82389,#82390,#82391,#82392,#82393,#82394,#82395,
#82396,#82397,#82398,#82399,#82400,#82401,#82402,#82403,#82404,#82405,#82406,
#82407,#82408,#82409,#82410,#82411,#82412,#82413,#82414,#82415,#82416,#82417,
#82418,#82419,#82420,#82421,#82422,#82423,#82424,#82425,#82426,#82427,#82428,
#82429,#82430,#82431,#82432,#82433,#82434,#82435,#82436,#82437,#82438,#82439,
#82440,#82441,#82442,#82443,#82444,#82445,#82446,#82447,#82448,#82449,#82450,
#82451,#82452,#82453,#82454,#82455,#82456,#82457,#82458,#82459,#82460,#82461,
#82462,#82463,#82464,#82465,#82466,#82467,#82468,#82469,#82470,#82471,#82472,
#82473,#82474,#82475,#82476,#82477,#82478,#82479,#82480,#82481,#82482,#82483,
#82484,#82485,#82486,#82487,#82488,#82489,#82490,#82491,#82492,#82493,#82494,
#82495,#82496,#82497,#82498,#82499,#82500,#82501,#82502,#82503,#82504,#82505,
#82506,#82507,#82508,#82509,#82510),(#82511,#82512,#82513,#82514,#82515,
#82516,#82517,#82518,#82519,#82520,#82521,#82522,#82523,#82524,#82525,#82526,
#82527,#82528,#82529,#82530,#82531,#82532,#82533,#82534,#82535,#82536,#82537,
#82538,#82539,#82540,#82541,#82542,#82543,#82544,#82545,#82546,#82547,#82548,
#82549,#82550,#82551,#82552,#82553,#82554,#82555,#82556,#82557,#82558,#82559,
#82560,#82561,#82562,#82563,#82564,#82565,#82566,#82567,#82568,#82569,#82570,
#82571,#82572,#82573,#82574,#82575,#82576,#82577,#82578,#82579,#82580,#82581,
#82582,#82583,#82584,#82585,#82586,#82587,#82588,#82589,#82590,#82591,#82592,
#82593,#82594,#82595,#82596,#82597,#82598,#82599,#82600,#82601,#82602,#82603,
#82604,#82605,#82606,#82607,#82608,#82609,#82610,#82611,#82612,#82613,#82614,
#82615,#82616,#82617,#82618,#82619,#82620,#82621,#82622,#82623,#82624,#82625,
#82626,#82627,#82628,#82629,#82630,#82631,#82632,#82633,#82634,#82635,#82636,
#82637,#82638,#82639,#82640,#82641),(#82642,#82643,#82644,#82645,#82646,
#82647,#82648,#82649,#82650,#82651,#82652,#82653,#82654,#82655,#82656,#82657,
#82658,#82659,#82660,#82661,#82662,#82663,#82664,#82665,#82666,#82667,#82668,
#82669,#82670,#82671,#82672,#82673,#82674,#82675,#82676,#82677,#82678,#82679,
#82680,#82681,#82682,#82683,#82684,#82685,#82686,#82687,#82688,#82689,#82690,
#82691,#82692,#82693,#82694,#82695,#82696,#82697,#82698,#82699,#82700,#82701,
#82702,#82703,#82704,#82705,#82706,#82707,#82708,#82709,#82710,#82711,#82712,
#82713,#82714,#82715,#82716,#82717,#82718,#82719,#82720,#82721,#82722,#82723,
#82724,#82725,#82726,#82727,#82728,#82729,#82730,#82731,#82732,#82733,#82734,
#82735,#82736,#82737,#82738,#82739,#82740,#82741,#82742,#82743,#82744,#82745,
#82746,#82747,#82748,#82749,#82750,#82751,#82752,#82753,#82754,#82755,#82756,
#82757,#82758,#82759,#82760,#82761,#82762,#82763,#82764,#82765,#82766,#82767,
#82768,#82769,#82770,#82771,#82772),(#82773,#82774,#82775,#82776,#82777,
#82778,#82779,#82780,#82781,#82782,#82783,#82784,#82785,#82786,#82787,#82788,
#82789,#82790,#82791,#82792,#82793,#82794,#82795,#82796,#82797,#82798,#82799,
#82800,#82801,#82802,#82803,#82804,#82805,#82806,#82807,#82808,#82809,#82810,
#82811,#82812,#82813,#82814,#82815,#82816,#82817,#82818,#82819,#82820,#82821,
#82822,#82823,#82824,#82825,#82826,#82827,#82828,#82829,#82830,#82831,#82832,
#82833,#82834,#82835,#82836,#82837,#82838,#82839,#82840,#82841,#82842,#82843,
#82844,#82845,#82846,#82847,#82848,#82849,#82850,#82851,#82852,#82853,#82854,
#82855,#82856,#82857,#82858,#82859,#82860,#82861,#82862,#82863,#82864,#82865,
#82866,#82867,#82868,#82869,#82870,#82871,#82872,#82873,#82874,#82875,#82876,
#82877,#82878,#82879,#82880,#82881,#82882,#82883,#82884,#82885,#82886,#82887,
#82888,#82889,#82890,#82891,#82892,#82893,#82894,#82895,#82896,#82897,#82898,
#82899,#82900,#82901,#82902,#82903)),.UNSPECIFIED.,.F.,.F.,.F.,(4,4),(4,
1,1,1,1,1,1,1,1,1,1,1,1,1,1,1,1,1,1,1,1,1,1,1,1,1,1,1,1,1,1,1,1,1,1,1,1,
1,1,1,1,1,1,1,1,1,1,1,1,1,1,1,1,1,1,1,1,1,1,1,1,1,1,1,1,1,1,1,1,1,1,1,1,
1,1,1,1,1,1,1,1,1,1,1,1,1,1,1,1,1,1,1,1,1,1,1,1,1,1,1,1,1,1,1,1,1,1,1,1,
1,1,1,1,1,1,1,1,1,1,1,1,1,1,1,1,1,1,1,4),(0.,0.0642013499338863),(14.3984001269718,
15.3959052131954,16.393410299419,17.3909153856426,18.3884204718662,19.3859255580897,
20.3834306443133,21.3809357305369,22.3784408167605,23.3759459029841,24.3734509892077,
25.3709560754313,26.3684611616549,27.3659662478785,28.3634713341021,29.3609764203257,
30.3584815065493,31.3559865927729,32.3534916789965,33.3509967652201,34.3485018514437,
35.3460069376673,36.3435120238909,37.3410171101145,38.3385221963381,39.3360272825616,
40.3335323687852,41.3310374550088,42.3285425412324,43.326047627456,44.3235527136796,
45.3210577999032,46.3185628861268,47.3160679723504,48.313573058574,49.3110781447976,
50.3085832310212,51.3060883172448,52.3035934034684,53.301098489692,54.2986035759156,
55.2961086621392,56.2936137483628,57.2911188345864,58.28862392081,59.2861290070336,
60.2836340932571,61.2811391794807,62.2786442657043,63.2761493519279,64.2736544381515,
65.2711595243751,66.2686646105987,67.2661696968223,68.2636747830459,69.2611798692695,
70.2586849554931,71.2561900417167,72.2536951279403,73.2512002141639,74.2487053003875,
75.2462103866111,76.2437154728347,77.2412205590583,78.2387256452818,79.2362307315055,
80.233735817729,81.2312409039526,82.2287459901762,83.2262510763998,84.2237561626234,
85.221261248847,86.2187663350706,87.2162714212942,88.2137765075178,89.2112815937414,
90.208786679965,91.2062917661886,92.2037968524122,93.2013019386358,94.1988070248594,
95.196312111083,96.1938171973066,97.1913222835302,98.1888273697538,99.1863324559774,
100.183837542201,101.181342628425,102.178847714648,103.176352800872,104.173857887095,
105.171362973319,106.168868059543,107.166373145766,108.16387823199,109.161383318213,
110.158888404437,111.15639349066,112.153898576884,113.151403663108,114.148908749331,
115.146413835555,116.143918921778,117.141424008002,118.138929094226,119.136434180449,
120.133939266673,121.131444352896,122.12894943912,123.126454525344,124.123959611567,
125.121464697791,126.118969784014,127.116474870238,128.113979956462,129.111485042685,
130.108990128909,131.106495215132,132.104000301356,133.10150538758,134.099010473803,
135.096515560027,136.09402064625,137.091525732474,138.089030818698,139.086535904921,
140.084040991145,141.081546077368,142.079051163592),.UNSPECIFIED.);
#364=B_SPLINE_SURFACE_WITH_KNOTS('',3,3,((#84085,#84086,#84087,#84088,#84089,
#84090,#84091,#84092,#84093,#84094,#84095,#84096,#84097,#84098,#84099,#84100,
#84101,#84102,#84103,#84104,#84105,#84106,#84107,#84108,#84109,#84110,#84111,
#84112,#84113,#84114,#84115,#84116,#84117,#84118,#84119,#84120,#84121,#84122,
#84123,#84124,#84125,#84126,#84127,#84128,#84129,#84130,#84131,#84132,#84133,
#84134,#84135,#84136,#84137,#84138,#84139,#84140,#84141,#84142,#84143,#84144,
#84145,#84146,#84147,#84148,#84149,#84150,#84151,#84152,#84153,#84154,#84155,
#84156,#84157,#84158,#84159,#84160,#84161,#84162,#84163,#84164,#84165,#84166,
#84167,#84168,#84169,#84170,#84171,#84172,#84173,#84174,#84175,#84176,#84177,
#84178,#84179,#84180,#84181,#84182,#84183,#84184,#84185,#84186,#84187,#84188,
#84189,#84190,#84191,#84192,#84193,#84194,#84195,#84196,#84197,#84198,#84199,
#84200,#84201,#84202,#84203,#84204,#84205,#84206,#84207,#84208,#84209,#84210,
#84211,#84212,#84213,#84214,#84215),(#84216,#84217,#84218,#84219,#84220,
#84221,#84222,#84223,#84224,#84225,#84226,#84227,#84228,#84229,#84230,#84231,
#84232,#84233,#84234,#84235,#84236,#84237,#84238,#84239,#84240,#84241,#84242,
#84243,#84244,#84245,#84246,#84247,#84248,#84249,#84250,#84251,#84252,#84253,
#84254,#84255,#84256,#84257,#84258,#84259,#84260,#84261,#84262,#84263,#84264,
#84265,#84266,#84267,#84268,#84269,#84270,#84271,#84272,#84273,#84274,#84275,
#84276,#84277,#84278,#84279,#84280,#84281,#84282,#84283,#84284,#84285,#84286,
#84287,#84288,#84289,#84290,#84291,#84292,#84293,#84294,#84295,#84296,#84297,
#84298,#84299,#84300,#84301,#84302,#84303,#84304,#84305,#84306,#84307,#84308,
#84309,#84310,#84311,#84312,#84313,#84314,#84315,#84316,#84317,#84318,#84319,
#84320,#84321,#84322,#84323,#84324,#84325,#84326,#84327,#84328,#84329,#84330,
#84331,#84332,#84333,#84334,#84335,#84336,#84337,#84338,#84339,#84340,#84341,
#84342,#84343,#84344,#84345,#84346),(#84347,#84348,#84349,#84350,#84351,
#84352,#84353,#84354,#84355,#84356,#84357,#84358,#84359,#84360,#84361,#84362,
#84363,#84364,#84365,#84366,#84367,#84368,#84369,#84370,#84371,#84372,#84373,
#84374,#84375,#84376,#84377,#84378,#84379,#84380,#84381,#84382,#84383,#84384,
#84385,#84386,#84387,#84388,#84389,#84390,#84391,#84392,#84393,#84394,#84395,
#84396,#84397,#84398,#84399,#84400,#84401,#84402,#84403,#84404,#84405,#84406,
#84407,#84408,#84409,#84410,#84411,#84412,#84413,#84414,#84415,#84416,#84417,
#84418,#84419,#84420,#84421,#84422,#84423,#84424,#84425,#84426,#84427,#84428,
#84429,#84430,#84431,#84432,#84433,#84434,#84435,#84436,#84437,#84438,#84439,
#84440,#84441,#84442,#84443,#84444,#84445,#84446,#84447,#84448,#84449,#84450,
#84451,#84452,#84453,#84454,#84455,#84456,#84457,#84458,#84459,#84460,#84461,
#84462,#84463,#84464,#84465,#84466,#84467,#84468,#84469,#84470,#84471,#84472,
#84473,#84474,#84475,#84476,#84477),(#84478,#84479,#84480,#84481,#84482,
#84483,#84484,#84485,#84486,#84487,#84488,#84489,#84490,#84491,#84492,#84493,
#84494,#84495,#84496,#84497,#84498,#84499,#84500,#84501,#84502,#84503,#84504,
#84505,#84506,#84507,#84508,#84509,#84510,#84511,#84512,#84513,#84514,#84515,
#84516,#84517,#84518,#84519,#84520,#84521,#84522,#84523,#84524,#84525,#84526,
#84527,#84528,#84529,#84530,#84531,#84532,#84533,#84534,#84535,#84536,#84537,
#84538,#84539,#84540,#84541,#84542,#84543,#84544,#84545,#84546,#84547,#84548,
#84549,#84550,#84551,#84552,#84553,#84554,#84555,#84556,#84557,#84558,#84559,
#84560,#84561,#84562,#84563,#84564,#84565,#84566,#84567,#84568,#84569,#84570,
#84571,#84572,#84573,#84574,#84575,#84576,#84577,#84578,#84579,#84580,#84581,
#84582,#84583,#84584,#84585,#84586,#84587,#84588,#84589,#84590,#84591,#84592,
#84593,#84594,#84595,#84596,#84597,#84598,#84599,#84600,#84601,#84602,#84603,
#84604,#84605,#84606,#84607,#84608)),.UNSPECIFIED.,.F.,.F.,.F.,(4,4),(4,
1,1,1,1,1,1,1,1,1,1,1,1,1,1,1,1,1,1,1,1,1,1,1,1,1,1,1,1,1,1,1,1,1,1,1,1,
1,1,1,1,1,1,1,1,1,1,1,1,1,1,1,1,1,1,1,1,1,1,1,1,1,1,1,1,1,1,1,1,1,1,1,1,
1,1,1,1,1,1,1,1,1,1,1,1,1,1,1,1,1,1,1,1,1,1,1,1,1,1,1,1,1,1,1,1,1,1,1,1,
1,1,1,1,1,1,1,1,1,1,1,1,1,1,1,1,1,1,1,4),(0.,0.0642013499338864),(11.8589888623077,
12.8564939485313,13.8539990347549,14.8515041209785,15.8490092072021,16.8465142934257,
17.8440193796493,18.8415244658729,19.8390295520965,20.8365346383201,21.8340397245437,
22.8315448107673,23.8290498969909,24.8265549832144,25.824060069438,26.8215651556616,
27.8190702418852,28.8165753281088,29.8140804143324,30.811585500556,31.8090905867796,
32.8065956730032,33.8041007592268,34.8016058454504,35.799110931674,36.7966160178976,
37.7941211041212,38.7916261903448,39.7891312765684,40.786636362792,41.7841414490156,
42.7816465352392,43.7791516214628,44.7766567076863,45.7741617939099,46.7716668801335,
47.7691719663571,48.7666770525807,49.7641821388043,50.7616872250279,51.7591923112515,
52.7566973974751,53.7542024836987,54.7517075699223,55.7492126561459,56.7467177423695,
57.7442228285931,58.7417279148167,59.7392330010403,60.7367380872639,61.7342431734875,
62.7317482597111,63.7292533459347,64.7267584321582,65.7242635183818,66.7217686046054,
67.719273690829,68.7167787770526,69.7142838632762,70.7117889494998,71.7092940357234,
72.706799121947,73.7043042081706,74.7018092943942,75.6993143806178,76.6968194668414,
77.694324553065,78.6918296392886,79.6893347255122,80.6868398117358,81.6843448979594,
82.681849984183,83.6793550704066,84.6768601566301,85.6743652428537,86.6718703290773,
87.6693754153009,88.6668805015245,89.6643855877481,90.6618906739717,91.6593957601953,
92.6569008464189,93.6544059326425,94.6519110188661,95.6494161050897,96.6469211913133,
97.6444262775369,98.6419313637605,99.6394364499841,100.636941536208,101.634446622431,
102.631951708655,103.629456794878,104.626961881102,105.624466967326,106.621972053549,
107.619477139773,108.616982225996,109.61448731222,110.611992398444,111.609497484667,
112.607002570891,113.604507657114,114.602012743338,115.599517829562,116.597022915785,
117.594528002009,118.592033088232,119.589538174456,120.58704326068,121.584548346903,
122.582053433127,123.57955851935,124.577063605574,125.574568691798,126.572073778021,
127.569578864245,128.567083950468,129.564589036692,130.562094122916,131.559599209139,
132.557104295363,133.554609381586,134.55211446781,135.549619554033,136.547124640257,
137.544629726481,138.542134812704,139.539639898928),.UNSPECIFIED.);
#365=B_SPLINE_SURFACE_WITH_KNOTS('',3,3,((#84728,#84729,#84730,#84731,#84732,
#84733,#84734,#84735,#84736,#84737,#84738,#84739,#84740,#84741,#84742,#84743,
#84744,#84745,#84746,#84747,#84748,#84749,#84750,#84751,#84752,#84753,#84754,
#84755,#84756,#84757,#84758,#84759,#84760,#84761,#84762,#84763,#84764,#84765,
#84766,#84767,#84768,#84769,#84770,#84771,#84772,#84773,#84774,#84775,#84776,
#84777,#84778,#84779,#84780,#84781,#84782,#84783,#84784,#84785,#84786,#84787,
#84788,#84789,#84790,#84791,#84792,#84793,#84794,#84795,#84796,#84797,#84798,
#84799,#84800,#84801,#84802,#84803,#84804,#84805,#84806,#84807,#84808,#84809,
#84810,#84811,#84812,#84813,#84814,#84815,#84816,#84817,#84818,#84819,#84820,
#84821,#84822,#84823,#84824,#84825,#84826,#84827,#84828,#84829,#84830,#84831,
#84832,#84833,#84834,#84835,#84836,#84837,#84838,#84839,#84840,#84841,#84842,
#84843,#84844,#84845,#84846,#84847,#84848,#84849,#84850,#84851,#84852,#84853,
#84854,#84855,#84856,#84857,#84858),(#84859,#84860,#84861,#84862,#84863,
#84864,#84865,#84866,#84867,#84868,#84869,#84870,#84871,#84872,#84873,#84874,
#84875,#84876,#84877,#84878,#84879,#84880,#84881,#84882,#84883,#84884,#84885,
#84886,#84887,#84888,#84889,#84890,#84891,#84892,#84893,#84894,#84895,#84896,
#84897,#84898,#84899,#84900,#84901,#84902,#84903,#84904,#84905,#84906,#84907,
#84908,#84909,#84910,#84911,#84912,#84913,#84914,#84915,#84916,#84917,#84918,
#84919,#84920,#84921,#84922,#84923,#84924,#84925,#84926,#84927,#84928,#84929,
#84930,#84931,#84932,#84933,#84934,#84935,#84936,#84937,#84938,#84939,#84940,
#84941,#84942,#84943,#84944,#84945,#84946,#84947,#84948,#84949,#84950,#84951,
#84952,#84953,#84954,#84955,#84956,#84957,#84958,#84959,#84960,#84961,#84962,
#84963,#84964,#84965,#84966,#84967,#84968,#84969,#84970,#84971,#84972,#84973,
#84974,#84975,#84976,#84977,#84978,#84979,#84980,#84981,#84982,#84983,#84984,
#84985,#84986,#84987,#84988,#84989),(#84990,#84991,#84992,#84993,#84994,
#84995,#84996,#84997,#84998,#84999,#85000,#85001,#85002,#85003,#85004,#85005,
#85006,#85007,#85008,#85009,#85010,#85011,#85012,#85013,#85014,#85015,#85016,
#85017,#85018,#85019,#85020,#85021,#85022,#85023,#85024,#85025,#85026,#85027,
#85028,#85029,#85030,#85031,#85032,#85033,#85034,#85035,#85036,#85037,#85038,
#85039,#85040,#85041,#85042,#85043,#85044,#85045,#85046,#85047,#85048,#85049,
#85050,#85051,#85052,#85053,#85054,#85055,#85056,#85057,#85058,#85059,#85060,
#85061,#85062,#85063,#85064,#85065,#85066,#85067,#85068,#85069,#85070,#85071,
#85072,#85073,#85074,#85075,#85076,#85077,#85078,#85079,#85080,#85081,#85082,
#85083,#85084,#85085,#85086,#85087,#85088,#85089,#85090,#85091,#85092,#85093,
#85094,#85095,#85096,#85097,#85098,#85099,#85100,#85101,#85102,#85103,#85104,
#85105,#85106,#85107,#85108,#85109,#85110,#85111,#85112,#85113,#85114,#85115,
#85116,#85117,#85118,#85119,#85120),(#85121,#85122,#85123,#85124,#85125,
#85126,#85127,#85128,#85129,#85130,#85131,#85132,#85133,#85134,#85135,#85136,
#85137,#85138,#85139,#85140,#85141,#85142,#85143,#85144,#85145,#85146,#85147,
#85148,#85149,#85150,#85151,#85152,#85153,#85154,#85155,#85156,#85157,#85158,
#85159,#85160,#85161,#85162,#85163,#85164,#85165,#85166,#85167,#85168,#85169,
#85170,#85171,#85172,#85173,#85174,#85175,#85176,#85177,#85178,#85179,#85180,
#85181,#85182,#85183,#85184,#85185,#85186,#85187,#85188,#85189,#85190,#85191,
#85192,#85193,#85194,#85195,#85196,#85197,#85198,#85199,#85200,#85201,#85202,
#85203,#85204,#85205,#85206,#85207,#85208,#85209,#85210,#85211,#85212,#85213,
#85214,#85215,#85216,#85217,#85218,#85219,#85220,#85221,#85222,#85223,#85224,
#85225,#85226,#85227,#85228,#85229,#85230,#85231,#85232,#85233,#85234,#85235,
#85236,#85237,#85238,#85239,#85240,#85241,#85242,#85243,#85244,#85245,#85246,
#85247,#85248,#85249,#85250,#85251)),.UNSPECIFIED.,.F.,.F.,.F.,(4,4),(4,
1,1,1,1,1,1,1,1,1,1,1,1,1,1,1,1,1,1,1,1,1,1,1,1,1,1,1,1,1,1,1,1,1,1,1,1,
1,1,1,1,1,1,1,1,1,1,1,1,1,1,1,1,1,1,1,1,1,1,1,1,1,1,1,1,1,1,1,1,1,1,1,1,
1,1,1,1,1,1,1,1,1,1,1,1,1,1,1,1,1,1,1,1,1,1,1,1,1,1,1,1,1,1,1,1,1,1,1,1,
1,1,1,1,1,1,1,1,1,1,1,1,1,1,1,1,1,1,1,4),(0.,0.0642013499338864),(14.3984001269717,
15.3959052131953,16.3934102994189,17.3909153856425,18.3884204718661,19.3859255580897,
20.3834306443133,21.3809357305369,22.3784408167605,23.3759459029841,24.3734509892077,
25.3709560754313,26.3684611616549,27.3659662478785,28.3634713341021,29.3609764203257,
30.3584815065493,31.3559865927729,32.3534916789965,33.3509967652201,34.3485018514437,
35.3460069376672,36.3435120238908,37.3410171101144,38.338522196338,39.3360272825616,
40.3335323687852,41.3310374550088,42.3285425412324,43.326047627456,44.3235527136796,
45.3210577999032,46.3185628861268,47.3160679723504,48.313573058574,49.3110781447976,
50.3085832310212,51.3060883172448,52.3035934034684,53.301098489692,54.2986035759156,
55.2961086621392,56.2936137483628,57.2911188345863,58.2886239208099,59.2861290070335,
60.2836340932571,61.2811391794807,62.2786442657043,63.2761493519279,64.2736544381515,
65.2711595243751,66.2686646105987,67.2661696968223,68.2636747830459,69.2611798692695,
70.2586849554931,71.2561900417167,72.2536951279403,73.2512002141639,74.2487053003875,
75.2462103866111,76.2437154728347,77.2412205590582,78.2387256452818,79.2362307315054,
80.233735817729,81.2312409039526,82.2287459901762,83.2262510763998,84.2237561626234,
85.221261248847,86.2187663350706,87.2162714212942,88.2137765075178,89.2112815937414,
90.208786679965,91.2062917661886,92.2037968524122,93.2013019386358,94.1988070248594,
95.196312111083,96.1938171973066,97.1913222835302,98.1888273697538,99.1863324559773,
100.183837542201,101.181342628425,102.178847714648,103.176352800872,104.173857887095,
105.171362973319,106.168868059543,107.166373145766,108.16387823199,109.161383318213,
110.158888404437,111.15639349066,112.153898576884,113.151403663108,114.148908749331,
115.146413835555,116.143918921778,117.141424008002,118.138929094226,119.136434180449,
120.133939266673,121.131444352896,122.12894943912,123.126454525344,124.123959611567,
125.121464697791,126.118969784014,127.116474870238,128.113979956462,129.111485042685,
130.108990128909,131.106495215132,132.104000301356,133.10150538758,134.099010473803,
135.096515560027,136.09402064625,137.091525732474,138.089030818698,139.086535904921,
140.084040991145,141.081546077368,142.079051163592),.UNSPECIFIED.);
#366=B_SPLINE_SURFACE_WITH_KNOTS('',3,3,((#85390,#85391,#85392,#85393,#85394,
#85395,#85396,#85397,#85398,#85399,#85400,#85401,#85402,#85403,#85404,#85405,
#85406,#85407,#85408,#85409,#85410,#85411,#85412,#85413,#85414,#85415,#85416,
#85417,#85418,#85419,#85420,#85421,#85422,#85423,#85424,#85425,#85426,#85427,
#85428,#85429,#85430,#85431,#85432,#85433,#85434,#85435,#85436,#85437,#85438,
#85439,#85440,#85441,#85442,#85443,#85444,#85445,#85446,#85447,#85448,#85449,
#85450,#85451,#85452,#85453,#85454,#85455,#85456,#85457,#85458,#85459,#85460,
#85461,#85462,#85463,#85464,#85465,#85466,#85467,#85468,#85469,#85470,#85471,
#85472,#85473,#85474,#85475,#85476,#85477,#85478,#85479,#85480,#85481,#85482,
#85483,#85484,#85485,#85486,#85487,#85488,#85489,#85490,#85491,#85492,#85493,
#85494,#85495,#85496,#85497,#85498,#85499,#85500,#85501,#85502,#85503,#85504,
#85505,#85506,#85507,#85508,#85509,#85510,#85511,#85512,#85513,#85514,#85515,
#85516,#85517,#85518,#85519,#85520),(#85521,#85522,#85523,#85524,#85525,
#85526,#85527,#85528,#85529,#85530,#85531,#85532,#85533,#85534,#85535,#85536,
#85537,#85538,#85539,#85540,#85541,#85542,#85543,#85544,#85545,#85546,#85547,
#85548,#85549,#85550,#85551,#85552,#85553,#85554,#85555,#85556,#85557,#85558,
#85559,#85560,#85561,#85562,#85563,#85564,#85565,#85566,#85567,#85568,#85569,
#85570,#85571,#85572,#85573,#85574,#85575,#85576,#85577,#85578,#85579,#85580,
#85581,#85582,#85583,#85584,#85585,#85586,#85587,#85588,#85589,#85590,#85591,
#85592,#85593,#85594,#85595,#85596,#85597,#85598,#85599,#85600,#85601,#85602,
#85603,#85604,#85605,#85606,#85607,#85608,#85609,#85610,#85611,#85612,#85613,
#85614,#85615,#85616,#85617,#85618,#85619,#85620,#85621,#85622,#85623,#85624,
#85625,#85626,#85627,#85628,#85629,#85630,#85631,#85632,#85633,#85634,#85635,
#85636,#85637,#85638,#85639,#85640,#85641,#85642,#85643,#85644,#85645,#85646,
#85647,#85648,#85649,#85650,#85651),(#85652,#85653,#85654,#85655,#85656,
#85657,#85658,#85659,#85660,#85661,#85662,#85663,#85664,#85665,#85666,#85667,
#85668,#85669,#85670,#85671,#85672,#85673,#85674,#85675,#85676,#85677,#85678,
#85679,#85680,#85681,#85682,#85683,#85684,#85685,#85686,#85687,#85688,#85689,
#85690,#85691,#85692,#85693,#85694,#85695,#85696,#85697,#85698,#85699,#85700,
#85701,#85702,#85703,#85704,#85705,#85706,#85707,#85708,#85709,#85710,#85711,
#85712,#85713,#85714,#85715,#85716,#85717,#85718,#85719,#85720,#85721,#85722,
#85723,#85724,#85725,#85726,#85727,#85728,#85729,#85730,#85731,#85732,#85733,
#85734,#85735,#85736,#85737,#85738,#85739,#85740,#85741,#85742,#85743,#85744,
#85745,#85746,#85747,#85748,#85749,#85750,#85751,#85752,#85753,#85754,#85755,
#85756,#85757,#85758,#85759,#85760,#85761,#85762,#85763,#85764,#85765,#85766,
#85767,#85768,#85769,#85770,#85771,#85772,#85773,#85774,#85775,#85776,#85777,
#85778,#85779,#85780,#85781,#85782),(#85783,#85784,#85785,#85786,#85787,
#85788,#85789,#85790,#85791,#85792,#85793,#85794,#85795,#85796,#85797,#85798,
#85799,#85800,#85801,#85802,#85803,#85804,#85805,#85806,#85807,#85808,#85809,
#85810,#85811,#85812,#85813,#85814,#85815,#85816,#85817,#85818,#85819,#85820,
#85821,#85822,#85823,#85824,#85825,#85826,#85827,#85828,#85829,#85830,#85831,
#85832,#85833,#85834,#85835,#85836,#85837,#85838,#85839,#85840,#85841,#85842,
#85843,#85844,#85845,#85846,#85847,#85848,#85849,#85850,#85851,#85852,#85853,
#85854,#85855,#85856,#85857,#85858,#85859,#85860,#85861,#85862,#85863,#85864,
#85865,#85866,#85867,#85868,#85869,#85870,#85871,#85872,#85873,#85874,#85875,
#85876,#85877,#85878,#85879,#85880,#85881,#85882,#85883,#85884,#85885,#85886,
#85887,#85888,#85889,#85890,#85891,#85892,#85893,#85894,#85895,#85896,#85897,
#85898,#85899,#85900,#85901,#85902,#85903,#85904,#85905,#85906,#85907,#85908,
#85909,#85910,#85911,#85912,#85913)),.UNSPECIFIED.,.F.,.F.,.F.,(4,4),(4,
1,1,1,1,1,1,1,1,1,1,1,1,1,1,1,1,1,1,1,1,1,1,1,1,1,1,1,1,1,1,1,1,1,1,1,1,
1,1,1,1,1,1,1,1,1,1,1,1,1,1,1,1,1,1,1,1,1,1,1,1,1,1,1,1,1,1,1,1,1,1,1,1,
1,1,1,1,1,1,1,1,1,1,1,1,1,1,1,1,1,1,1,1,1,1,1,1,1,1,1,1,1,1,1,1,1,1,1,1,
1,1,1,1,1,1,1,1,1,1,1,1,1,1,1,1,1,1,1,4),(0.,0.0642013499338879),(11.8589888623077,
12.8564939485313,13.8539990347549,14.8515041209785,15.8490092072021,16.8465142934257,
17.8440193796493,18.8415244658729,19.8390295520965,20.8365346383201,21.8340397245437,
22.8315448107673,23.8290498969909,24.8265549832145,25.8240600694381,26.8215651556617,
27.8190702418853,28.8165753281089,29.8140804143324,30.811585500556,31.8090905867796,
32.8065956730032,33.8041007592268,34.8016058454504,35.799110931674,36.7966160178976,
37.7941211041212,38.7916261903448,39.7891312765684,40.786636362792,41.7841414490156,
42.7816465352392,43.7791516214628,44.7766567076864,45.77416179391,46.7716668801336,
47.7691719663572,48.7666770525808,49.7641821388044,50.7616872250279,51.7591923112515,
52.7566973974751,53.7542024836987,54.7517075699223,55.7492126561459,56.7467177423695,
57.7442228285931,58.7417279148167,59.7392330010403,60.7367380872639,61.7342431734875,
62.7317482597111,63.7292533459347,64.7267584321583,65.7242635183819,66.7217686046055,
67.7192736908291,68.7167787770527,69.7142838632763,70.7117889494998,71.7092940357234,
72.706799121947,73.7043042081706,74.7018092943942,75.6993143806178,76.6968194668414,
77.694324553065,78.6918296392886,79.6893347255122,80.6868398117358,81.6843448979594,
82.681849984183,83.6793550704066,84.6768601566302,85.6743652428538,86.6718703290774,
87.669375415301,88.6668805015246,89.6643855877482,90.6618906739718,91.6593957601954,
92.6569008464189,93.6544059326425,94.6519110188661,95.6494161050897,96.6469211913133,
97.6444262775369,98.6419313637605,99.6394364499841,100.636941536208,101.634446622431,
102.631951708655,103.629456794878,104.626961881102,105.624466967326,106.621972053549,
107.619477139773,108.616982225996,109.61448731222,110.611992398444,111.609497484667,
112.607002570891,113.604507657114,114.602012743338,115.599517829562,116.597022915785,
117.594528002009,118.592033088232,119.589538174456,120.58704326068,121.584548346903,
122.582053433127,123.57955851935,124.577063605574,125.574568691798,126.572073778021,
127.569578864245,128.567083950468,129.564589036692,130.562094122916,131.559599209139,
132.557104295363,133.554609381586,134.55211446781,135.549619554034,136.547124640257,
137.544629726481,138.542134812704,139.539639898928),.UNSPECIFIED.);
#367=B_SPLINE_SURFACE_WITH_KNOTS('',3,3,((#86033,#86034,#86035,#86036,#86037,
#86038,#86039,#86040,#86041,#86042,#86043,#86044,#86045,#86046,#86047,#86048,
#86049,#86050,#86051,#86052,#86053,#86054,#86055,#86056,#86057,#86058,#86059,
#86060,#86061,#86062,#86063,#86064,#86065,#86066,#86067,#86068,#86069,#86070,
#86071,#86072,#86073,#86074,#86075,#86076,#86077,#86078,#86079,#86080,#86081,
#86082,#86083,#86084,#86085,#86086,#86087,#86088,#86089,#86090,#86091,#86092,
#86093,#86094,#86095,#86096,#86097,#86098,#86099,#86100,#86101,#86102,#86103,
#86104,#86105,#86106,#86107,#86108,#86109,#86110,#86111,#86112,#86113,#86114,
#86115,#86116,#86117,#86118,#86119,#86120,#86121,#86122,#86123,#86124,#86125,
#86126,#86127,#86128,#86129,#86130,#86131,#86132,#86133,#86134,#86135,#86136,
#86137,#86138,#86139,#86140,#86141,#86142,#86143,#86144,#86145,#86146,#86147,
#86148,#86149,#86150,#86151,#86152,#86153,#86154,#86155,#86156,#86157,#86158,
#86159,#86160,#86161,#86162,#86163),(#86164,#86165,#86166,#86167,#86168,
#86169,#86170,#86171,#86172,#86173,#86174,#86175,#86176,#86177,#86178,#86179,
#86180,#86181,#86182,#86183,#86184,#86185,#86186,#86187,#86188,#86189,#86190,
#86191,#86192,#86193,#86194,#86195,#86196,#86197,#86198,#86199,#86200,#86201,
#86202,#86203,#86204,#86205,#86206,#86207,#86208,#86209,#86210,#86211,#86212,
#86213,#86214,#86215,#86216,#86217,#86218,#86219,#86220,#86221,#86222,#86223,
#86224,#86225,#86226,#86227,#86228,#86229,#86230,#86231,#86232,#86233,#86234,
#86235,#86236,#86237,#86238,#86239,#86240,#86241,#86242,#86243,#86244,#86245,
#86246,#86247,#86248,#86249,#86250,#86251,#86252,#86253,#86254,#86255,#86256,
#86257,#86258,#86259,#86260,#86261,#86262,#86263,#86264,#86265,#86266,#86267,
#86268,#86269,#86270,#86271,#86272,#86273,#86274,#86275,#86276,#86277,#86278,
#86279,#86280,#86281,#86282,#86283,#86284,#86285,#86286,#86287,#86288,#86289,
#86290,#86291,#86292,#86293,#86294),(#86295,#86296,#86297,#86298,#86299,
#86300,#86301,#86302,#86303,#86304,#86305,#86306,#86307,#86308,#86309,#86310,
#86311,#86312,#86313,#86314,#86315,#86316,#86317,#86318,#86319,#86320,#86321,
#86322,#86323,#86324,#86325,#86326,#86327,#86328,#86329,#86330,#86331,#86332,
#86333,#86334,#86335,#86336,#86337,#86338,#86339,#86340,#86341,#86342,#86343,
#86344,#86345,#86346,#86347,#86348,#86349,#86350,#86351,#86352,#86353,#86354,
#86355,#86356,#86357,#86358,#86359,#86360,#86361,#86362,#86363,#86364,#86365,
#86366,#86367,#86368,#86369,#86370,#86371,#86372,#86373,#86374,#86375,#86376,
#86377,#86378,#86379,#86380,#86381,#86382,#86383,#86384,#86385,#86386,#86387,
#86388,#86389,#86390,#86391,#86392,#86393,#86394,#86395,#86396,#86397,#86398,
#86399,#86400,#86401,#86402,#86403,#86404,#86405,#86406,#86407,#86408,#86409,
#86410,#86411,#86412,#86413,#86414,#86415,#86416,#86417,#86418,#86419,#86420,
#86421,#86422,#86423,#86424,#86425),(#86426,#86427,#86428,#86429,#86430,
#86431,#86432,#86433,#86434,#86435,#86436,#86437,#86438,#86439,#86440,#86441,
#86442,#86443,#86444,#86445,#86446,#86447,#86448,#86449,#86450,#86451,#86452,
#86453,#86454,#86455,#86456,#86457,#86458,#86459,#86460,#86461,#86462,#86463,
#86464,#86465,#86466,#86467,#86468,#86469,#86470,#86471,#86472,#86473,#86474,
#86475,#86476,#86477,#86478,#86479,#86480,#86481,#86482,#86483,#86484,#86485,
#86486,#86487,#86488,#86489,#86490,#86491,#86492,#86493,#86494,#86495,#86496,
#86497,#86498,#86499,#86500,#86501,#86502,#86503,#86504,#86505,#86506,#86507,
#86508,#86509,#86510,#86511,#86512,#86513,#86514,#86515,#86516,#86517,#86518,
#86519,#86520,#86521,#86522,#86523,#86524,#86525,#86526,#86527,#86528,#86529,
#86530,#86531,#86532,#86533,#86534,#86535,#86536,#86537,#86538,#86539,#86540,
#86541,#86542,#86543,#86544,#86545,#86546,#86547,#86548,#86549,#86550,#86551,
#86552,#86553,#86554,#86555,#86556)),.UNSPECIFIED.,.F.,.F.,.F.,(4,4),(4,
1,1,1,1,1,1,1,1,1,1,1,1,1,1,1,1,1,1,1,1,1,1,1,1,1,1,1,1,1,1,1,1,1,1,1,1,
1,1,1,1,1,1,1,1,1,1,1,1,1,1,1,1,1,1,1,1,1,1,1,1,1,1,1,1,1,1,1,1,1,1,1,1,
1,1,1,1,1,1,1,1,1,1,1,1,1,1,1,1,1,1,1,1,1,1,1,1,1,1,1,1,1,1,1,1,1,1,1,1,
1,1,1,1,1,1,1,1,1,1,1,1,1,1,1,1,1,1,1,4),(0.,0.0642013499338879),(14.3984001269718,
15.3959052131954,16.393410299419,17.3909153856426,18.3884204718662,19.3859255580897,
20.3834306443133,21.3809357305369,22.3784408167605,23.3759459029841,24.3734509892077,
25.3709560754313,26.3684611616549,27.3659662478785,28.3634713341021,29.3609764203257,
30.3584815065493,31.3559865927729,32.3534916789965,33.3509967652201,34.3485018514437,
35.3460069376673,36.3435120238909,37.3410171101145,38.3385221963381,39.3360272825617,
40.3335323687852,41.3310374550088,42.3285425412324,43.326047627456,44.3235527136796,
45.3210577999032,46.3185628861268,47.3160679723504,48.313573058574,49.3110781447976,
50.3085832310212,51.3060883172448,52.3035934034684,53.301098489692,54.2986035759156,
55.2961086621392,56.2936137483628,57.2911188345864,58.28862392081,59.2861290070336,
60.2836340932571,61.2811391794807,62.2786442657043,63.2761493519279,64.2736544381515,
65.2711595243751,66.2686646105987,67.2661696968223,68.2636747830459,69.2611798692695,
70.2586849554931,71.2561900417167,72.2536951279403,73.2512002141639,74.2487053003875,
75.2462103866111,76.2437154728347,77.2412205590583,78.2387256452819,79.2362307315055,
80.2337358177291,81.2312409039526,82.2287459901762,83.2262510763998,84.2237561626234,
85.221261248847,86.2187663350706,87.2162714212942,88.2137765075178,89.2112815937414,
90.208786679965,91.2062917661886,92.2037968524122,93.2013019386358,94.1988070248594,
95.196312111083,96.1938171973066,97.1913222835302,98.1888273697538,99.1863324559774,
100.183837542201,101.181342628425,102.178847714648,103.176352800872,104.173857887095,
105.171362973319,106.168868059543,107.166373145766,108.16387823199,109.161383318213,
110.158888404437,111.15639349066,112.153898576884,113.151403663108,114.148908749331,
115.146413835555,116.143918921778,117.141424008002,118.138929094226,119.136434180449,
120.133939266673,121.131444352896,122.12894943912,123.126454525344,124.123959611567,
125.121464697791,126.118969784014,127.116474870238,128.113979956462,129.111485042685,
130.108990128909,131.106495215132,132.104000301356,133.10150538758,134.099010473803,
135.096515560027,136.09402064625,137.091525732474,138.089030818698,139.086535904921,
140.084040991145,141.081546077368,142.079051163592),.UNSPECIFIED.);
#368=B_SPLINE_SURFACE_WITH_KNOTS('',3,3,((#86695,#86696,#86697,#86698,#86699,
#86700,#86701,#86702,#86703,#86704,#86705,#86706,#86707,#86708,#86709,#86710,
#86711,#86712,#86713,#86714,#86715,#86716,#86717,#86718,#86719,#86720,#86721,
#86722,#86723,#86724,#86725,#86726,#86727,#86728,#86729,#86730,#86731,#86732,
#86733,#86734,#86735,#86736,#86737,#86738,#86739,#86740,#86741,#86742,#86743,
#86744,#86745,#86746,#86747,#86748,#86749,#86750,#86751,#86752,#86753,#86754,
#86755,#86756,#86757,#86758,#86759,#86760,#86761,#86762,#86763,#86764,#86765,
#86766,#86767,#86768,#86769,#86770,#86771,#86772,#86773,#86774,#86775,#86776,
#86777,#86778,#86779,#86780,#86781,#86782,#86783,#86784,#86785,#86786,#86787,
#86788,#86789,#86790,#86791,#86792,#86793,#86794,#86795,#86796,#86797,#86798,
#86799,#86800,#86801,#86802,#86803,#86804,#86805,#86806,#86807,#86808,#86809,
#86810,#86811,#86812,#86813,#86814,#86815,#86816,#86817,#86818,#86819,#86820,
#86821,#86822,#86823,#86824,#86825),(#86826,#86827,#86828,#86829,#86830,
#86831,#86832,#86833,#86834,#86835,#86836,#86837,#86838,#86839,#86840,#86841,
#86842,#86843,#86844,#86845,#86846,#86847,#86848,#86849,#86850,#86851,#86852,
#86853,#86854,#86855,#86856,#86857,#86858,#86859,#86860,#86861,#86862,#86863,
#86864,#86865,#86866,#86867,#86868,#86869,#86870,#86871,#86872,#86873,#86874,
#86875,#86876,#86877,#86878,#86879,#86880,#86881,#86882,#86883,#86884,#86885,
#86886,#86887,#86888,#86889,#86890,#86891,#86892,#86893,#86894,#86895,#86896,
#86897,#86898,#86899,#86900,#86901,#86902,#86903,#86904,#86905,#86906,#86907,
#86908,#86909,#86910,#86911,#86912,#86913,#86914,#86915,#86916,#86917,#86918,
#86919,#86920,#86921,#86922,#86923,#86924,#86925,#86926,#86927,#86928,#86929,
#86930,#86931,#86932,#86933,#86934,#86935,#86936,#86937,#86938,#86939,#86940,
#86941,#86942,#86943,#86944,#86945,#86946,#86947,#86948,#86949,#86950,#86951,
#86952,#86953,#86954,#86955,#86956),(#86957,#86958,#86959,#86960,#86961,
#86962,#86963,#86964,#86965,#86966,#86967,#86968,#86969,#86970,#86971,#86972,
#86973,#86974,#86975,#86976,#86977,#86978,#86979,#86980,#86981,#86982,#86983,
#86984,#86985,#86986,#86987,#86988,#86989,#86990,#86991,#86992,#86993,#86994,
#86995,#86996,#86997,#86998,#86999,#87000,#87001,#87002,#87003,#87004,#87005,
#87006,#87007,#87008,#87009,#87010,#87011,#87012,#87013,#87014,#87015,#87016,
#87017,#87018,#87019,#87020,#87021,#87022,#87023,#87024,#87025,#87026,#87027,
#87028,#87029,#87030,#87031,#87032,#87033,#87034,#87035,#87036,#87037,#87038,
#87039,#87040,#87041,#87042,#87043,#87044,#87045,#87046,#87047,#87048,#87049,
#87050,#87051,#87052,#87053,#87054,#87055,#87056,#87057,#87058,#87059,#87060,
#87061,#87062,#87063,#87064,#87065,#87066,#87067,#87068,#87069,#87070,#87071,
#87072,#87073,#87074,#87075,#87076,#87077,#87078,#87079,#87080,#87081,#87082,
#87083,#87084,#87085,#87086,#87087),(#87088,#87089,#87090,#87091,#87092,
#87093,#87094,#87095,#87096,#87097,#87098,#87099,#87100,#87101,#87102,#87103,
#87104,#87105,#87106,#87107,#87108,#87109,#87110,#87111,#87112,#87113,#87114,
#87115,#87116,#87117,#87118,#87119,#87120,#87121,#87122,#87123,#87124,#87125,
#87126,#87127,#87128,#87129,#87130,#87131,#87132,#87133,#87134,#87135,#87136,
#87137,#87138,#87139,#87140,#87141,#87142,#87143,#87144,#87145,#87146,#87147,
#87148,#87149,#87150,#87151,#87152,#87153,#87154,#87155,#87156,#87157,#87158,
#87159,#87160,#87161,#87162,#87163,#87164,#87165,#87166,#87167,#87168,#87169,
#87170,#87171,#87172,#87173,#87174,#87175,#87176,#87177,#87178,#87179,#87180,
#87181,#87182,#87183,#87184,#87185,#87186,#87187,#87188,#87189,#87190,#87191,
#87192,#87193,#87194,#87195,#87196,#87197,#87198,#87199,#87200,#87201,#87202,
#87203,#87204,#87205,#87206,#87207,#87208,#87209,#87210,#87211,#87212,#87213,
#87214,#87215,#87216,#87217,#87218)),.UNSPECIFIED.,.F.,.F.,.F.,(4,4),(4,
1,1,1,1,1,1,1,1,1,1,1,1,1,1,1,1,1,1,1,1,1,1,1,1,1,1,1,1,1,1,1,1,1,1,1,1,
1,1,1,1,1,1,1,1,1,1,1,1,1,1,1,1,1,1,1,1,1,1,1,1,1,1,1,1,1,1,1,1,1,1,1,1,
1,1,1,1,1,1,1,1,1,1,1,1,1,1,1,1,1,1,1,1,1,1,1,1,1,1,1,1,1,1,1,1,1,1,1,1,
1,1,1,1,1,1,1,1,1,1,1,1,1,1,1,1,1,1,1,4),(0.,0.0642013499338879),(11.8589888623077,
12.8564939485313,13.8539990347549,14.8515041209785,15.8490092072021,16.8465142934257,
17.8440193796493,18.8415244658729,19.8390295520965,20.8365346383201,21.8340397245437,
22.8315448107673,23.8290498969909,24.8265549832145,25.8240600694381,26.8215651556617,
27.8190702418853,28.8165753281089,29.8140804143324,30.811585500556,31.8090905867796,
32.8065956730032,33.8041007592268,34.8016058454504,35.799110931674,36.7966160178976,
37.7941211041212,38.7916261903448,39.7891312765684,40.786636362792,41.7841414490156,
42.7816465352392,43.7791516214628,44.7766567076864,45.77416179391,46.7716668801336,
47.7691719663572,48.7666770525807,49.7641821388043,50.7616872250279,51.7591923112515,
52.7566973974751,53.7542024836987,54.7517075699223,55.7492126561459,56.7467177423695,
57.7442228285931,58.7417279148167,59.7392330010403,60.7367380872639,61.7342431734875,
62.7317482597111,63.7292533459347,64.7267584321583,65.7242635183819,66.7217686046055,
67.7192736908291,68.7167787770527,69.7142838632763,70.7117889494998,71.7092940357234,
72.706799121947,73.7043042081706,74.7018092943942,75.6993143806178,76.6968194668414,
77.694324553065,78.6918296392886,79.6893347255122,80.6868398117358,81.6843448979594,
82.681849984183,83.6793550704066,84.6768601566302,85.6743652428538,86.6718703290774,
87.669375415301,88.6668805015246,89.6643855877482,90.6618906739717,91.6593957601953,
92.6569008464189,93.6544059326425,94.6519110188661,95.6494161050897,96.6469211913133,
97.6444262775369,98.6419313637605,99.6394364499841,100.636941536208,101.634446622431,
102.631951708655,103.629456794878,104.626961881102,105.624466967326,106.621972053549,
107.619477139773,108.616982225996,109.61448731222,110.611992398444,111.609497484667,
112.607002570891,113.604507657114,114.602012743338,115.599517829562,116.597022915785,
117.594528002009,118.592033088232,119.589538174456,120.58704326068,121.584548346903,
122.582053433127,123.57955851935,124.577063605574,125.574568691798,126.572073778021,
127.569578864245,128.567083950468,129.564589036692,130.562094122916,131.559599209139,
132.557104295363,133.554609381586,134.55211446781,135.549619554034,136.547124640257,
137.544629726481,138.542134812704,139.539639898928),.UNSPECIFIED.);
#369=B_SPLINE_SURFACE_WITH_KNOTS('',3,3,((#87338,#87339,#87340,#87341,#87342,
#87343,#87344,#87345,#87346,#87347,#87348,#87349,#87350,#87351,#87352,#87353,
#87354,#87355,#87356,#87357,#87358,#87359,#87360,#87361,#87362,#87363,#87364,
#87365,#87366,#87367,#87368,#87369,#87370,#87371,#87372,#87373,#87374,#87375,
#87376,#87377,#87378,#87379,#87380,#87381,#87382,#87383,#87384,#87385,#87386,
#87387,#87388,#87389,#87390,#87391,#87392,#87393,#87394,#87395,#87396,#87397,
#87398,#87399,#87400,#87401,#87402,#87403,#87404,#87405,#87406,#87407,#87408,
#87409,#87410,#87411,#87412,#87413,#87414,#87415,#87416,#87417,#87418,#87419,
#87420,#87421,#87422,#87423,#87424,#87425,#87426,#87427,#87428,#87429,#87430,
#87431,#87432,#87433,#87434,#87435,#87436,#87437,#87438,#87439,#87440,#87441,
#87442,#87443,#87444,#87445,#87446,#87447,#87448,#87449,#87450,#87451,#87452,
#87453,#87454,#87455,#87456,#87457,#87458,#87459,#87460,#87461,#87462,#87463,
#87464,#87465,#87466,#87467,#87468),(#87469,#87470,#87471,#87472,#87473,
#87474,#87475,#87476,#87477,#87478,#87479,#87480,#87481,#87482,#87483,#87484,
#87485,#87486,#87487,#87488,#87489,#87490,#87491,#87492,#87493,#87494,#87495,
#87496,#87497,#87498,#87499,#87500,#87501,#87502,#87503,#87504,#87505,#87506,
#87507,#87508,#87509,#87510,#87511,#87512,#87513,#87514,#87515,#87516,#87517,
#87518,#87519,#87520,#87521,#87522,#87523,#87524,#87525,#87526,#87527,#87528,
#87529,#87530,#87531,#87532,#87533,#87534,#87535,#87536,#87537,#87538,#87539,
#87540,#87541,#87542,#87543,#87544,#87545,#87546,#87547,#87548,#87549,#87550,
#87551,#87552,#87553,#87554,#87555,#87556,#87557,#87558,#87559,#87560,#87561,
#87562,#87563,#87564,#87565,#87566,#87567,#87568,#87569,#87570,#87571,#87572,
#87573,#87574,#87575,#87576,#87577,#87578,#87579,#87580,#87581,#87582,#87583,
#87584,#87585,#87586,#87587,#87588,#87589,#87590,#87591,#87592,#87593,#87594,
#87595,#87596,#87597,#87598,#87599),(#87600,#87601,#87602,#87603,#87604,
#87605,#87606,#87607,#87608,#87609,#87610,#87611,#87612,#87613,#87614,#87615,
#87616,#87617,#87618,#87619,#87620,#87621,#87622,#87623,#87624,#87625,#87626,
#87627,#87628,#87629,#87630,#87631,#87632,#87633,#87634,#87635,#87636,#87637,
#87638,#87639,#87640,#87641,#87642,#87643,#87644,#87645,#87646,#87647,#87648,
#87649,#87650,#87651,#87652,#87653,#87654,#87655,#87656,#87657,#87658,#87659,
#87660,#87661,#87662,#87663,#87664,#87665,#87666,#87667,#87668,#87669,#87670,
#87671,#87672,#87673,#87674,#87675,#87676,#87677,#87678,#87679,#87680,#87681,
#87682,#87683,#87684,#87685,#87686,#87687,#87688,#87689,#87690,#87691,#87692,
#87693,#87694,#87695,#87696,#87697,#87698,#87699,#87700,#87701,#87702,#87703,
#87704,#87705,#87706,#87707,#87708,#87709,#87710,#87711,#87712,#87713,#87714,
#87715,#87716,#87717,#87718,#87719,#87720,#87721,#87722,#87723,#87724,#87725,
#87726,#87727,#87728,#87729,#87730),(#87731,#87732,#87733,#87734,#87735,
#87736,#87737,#87738,#87739,#87740,#87741,#87742,#87743,#87744,#87745,#87746,
#87747,#87748,#87749,#87750,#87751,#87752,#87753,#87754,#87755,#87756,#87757,
#87758,#87759,#87760,#87761,#87762,#87763,#87764,#87765,#87766,#87767,#87768,
#87769,#87770,#87771,#87772,#87773,#87774,#87775,#87776,#87777,#87778,#87779,
#87780,#87781,#87782,#87783,#87784,#87785,#87786,#87787,#87788,#87789,#87790,
#87791,#87792,#87793,#87794,#87795,#87796,#87797,#87798,#87799,#87800,#87801,
#87802,#87803,#87804,#87805,#87806,#87807,#87808,#87809,#87810,#87811,#87812,
#87813,#87814,#87815,#87816,#87817,#87818,#87819,#87820,#87821,#87822,#87823,
#87824,#87825,#87826,#87827,#87828,#87829,#87830,#87831,#87832,#87833,#87834,
#87835,#87836,#87837,#87838,#87839,#87840,#87841,#87842,#87843,#87844,#87845,
#87846,#87847,#87848,#87849,#87850,#87851,#87852,#87853,#87854,#87855,#87856,
#87857,#87858,#87859,#87860,#87861)),.UNSPECIFIED.,.F.,.F.,.F.,(4,4),(4,
1,1,1,1,1,1,1,1,1,1,1,1,1,1,1,1,1,1,1,1,1,1,1,1,1,1,1,1,1,1,1,1,1,1,1,1,
1,1,1,1,1,1,1,1,1,1,1,1,1,1,1,1,1,1,1,1,1,1,1,1,1,1,1,1,1,1,1,1,1,1,1,1,
1,1,1,1,1,1,1,1,1,1,1,1,1,1,1,1,1,1,1,1,1,1,1,1,1,1,1,1,1,1,1,1,1,1,1,1,
1,1,1,1,1,1,1,1,1,1,1,1,1,1,1,1,1,1,1,4),(0.,0.0642013499338879),(14.3984001269718,
15.3959052131954,16.393410299419,17.3909153856426,18.3884204718662,19.3859255580897,
20.3834306443133,21.3809357305369,22.3784408167605,23.3759459029841,24.3734509892077,
25.3709560754313,26.3684611616549,27.3659662478785,28.3634713341021,29.3609764203257,
30.3584815065493,31.3559865927729,32.3534916789965,33.3509967652201,34.3485018514437,
35.3460069376673,36.3435120238909,37.3410171101145,38.3385221963381,39.3360272825616,
40.3335323687852,41.3310374550088,42.3285425412324,43.326047627456,44.3235527136796,
45.3210577999032,46.3185628861268,47.3160679723504,48.313573058574,49.3110781447976,
50.3085832310212,51.3060883172448,52.3035934034684,53.301098489692,54.2986035759156,
55.2961086621392,56.2936137483628,57.2911188345864,58.28862392081,59.2861290070336,
60.2836340932571,61.2811391794807,62.2786442657043,63.2761493519279,64.2736544381515,
65.2711595243751,66.2686646105987,67.2661696968223,68.2636747830459,69.2611798692695,
70.2586849554931,71.2561900417167,72.2536951279403,73.2512002141639,74.2487053003875,
75.2462103866111,76.2437154728347,77.2412205590583,78.2387256452818,79.2362307315055,
80.233735817729,81.2312409039526,82.2287459901762,83.2262510763998,84.2237561626234,
85.221261248847,86.2187663350706,87.2162714212942,88.2137765075178,89.2112815937414,
90.208786679965,91.2062917661886,92.2037968524122,93.2013019386358,94.1988070248594,
95.196312111083,96.1938171973066,97.1913222835302,98.1888273697538,99.1863324559774,
100.183837542201,101.181342628425,102.178847714648,103.176352800872,104.173857887095,
105.171362973319,106.168868059543,107.166373145766,108.16387823199,109.161383318213,
110.158888404437,111.15639349066,112.153898576884,113.151403663108,114.148908749331,
115.146413835555,116.143918921778,117.141424008002,118.138929094226,119.136434180449,
120.133939266673,121.131444352896,122.12894943912,123.126454525344,124.123959611567,
125.121464697791,126.118969784014,127.116474870238,128.113979956462,129.111485042685,
130.108990128909,131.106495215132,132.104000301356,133.10150538758,134.099010473803,
135.096515560027,136.09402064625,137.091525732474,138.089030818698,139.086535904921,
140.084040991145,141.081546077368,142.079051163592),.UNSPECIFIED.);
#370=B_SPLINE_SURFACE_WITH_KNOTS('',3,3,((#88000,#88001,#88002,#88003,#88004,
#88005,#88006,#88007,#88008,#88009,#88010,#88011,#88012,#88013,#88014,#88015,
#88016,#88017,#88018,#88019,#88020,#88021,#88022,#88023,#88024,#88025,#88026,
#88027,#88028,#88029,#88030,#88031,#88032,#88033,#88034,#88035,#88036,#88037,
#88038,#88039,#88040,#88041,#88042,#88043,#88044,#88045,#88046,#88047,#88048,
#88049,#88050,#88051,#88052,#88053,#88054,#88055,#88056,#88057,#88058,#88059,
#88060,#88061,#88062,#88063,#88064,#88065,#88066,#88067,#88068,#88069,#88070,
#88071,#88072,#88073,#88074,#88075,#88076,#88077,#88078,#88079,#88080,#88081,
#88082,#88083,#88084,#88085,#88086,#88087,#88088,#88089,#88090,#88091,#88092,
#88093,#88094,#88095,#88096,#88097,#88098,#88099,#88100,#88101,#88102,#88103,
#88104,#88105,#88106,#88107,#88108,#88109,#88110,#88111,#88112,#88113,#88114,
#88115,#88116,#88117,#88118,#88119,#88120,#88121,#88122,#88123,#88124,#88125,
#88126,#88127,#88128,#88129,#88130),(#88131,#88132,#88133,#88134,#88135,
#88136,#88137,#88138,#88139,#88140,#88141,#88142,#88143,#88144,#88145,#88146,
#88147,#88148,#88149,#88150,#88151,#88152,#88153,#88154,#88155,#88156,#88157,
#88158,#88159,#88160,#88161,#88162,#88163,#88164,#88165,#88166,#88167,#88168,
#88169,#88170,#88171,#88172,#88173,#88174,#88175,#88176,#88177,#88178,#88179,
#88180,#88181,#88182,#88183,#88184,#88185,#88186,#88187,#88188,#88189,#88190,
#88191,#88192,#88193,#88194,#88195,#88196,#88197,#88198,#88199,#88200,#88201,
#88202,#88203,#88204,#88205,#88206,#88207,#88208,#88209,#88210,#88211,#88212,
#88213,#88214,#88215,#88216,#88217,#88218,#88219,#88220,#88221,#88222,#88223,
#88224,#88225,#88226,#88227,#88228,#88229,#88230,#88231,#88232,#88233,#88234,
#88235,#88236,#88237,#88238,#88239,#88240,#88241,#88242,#88243,#88244,#88245,
#88246,#88247,#88248,#88249,#88250,#88251,#88252,#88253,#88254,#88255,#88256,
#88257,#88258,#88259,#88260,#88261),(#88262,#88263,#88264,#88265,#88266,
#88267,#88268,#88269,#88270,#88271,#88272,#88273,#88274,#88275,#88276,#88277,
#88278,#88279,#88280,#88281,#88282,#88283,#88284,#88285,#88286,#88287,#88288,
#88289,#88290,#88291,#88292,#88293,#88294,#88295,#88296,#88297,#88298,#88299,
#88300,#88301,#88302,#88303,#88304,#88305,#88306,#88307,#88308,#88309,#88310,
#88311,#88312,#88313,#88314,#88315,#88316,#88317,#88318,#88319,#88320,#88321,
#88322,#88323,#88324,#88325,#88326,#88327,#88328,#88329,#88330,#88331,#88332,
#88333,#88334,#88335,#88336,#88337,#88338,#88339,#88340,#88341,#88342,#88343,
#88344,#88345,#88346,#88347,#88348,#88349,#88350,#88351,#88352,#88353,#88354,
#88355,#88356,#88357,#88358,#88359,#88360,#88361,#88362,#88363,#88364,#88365,
#88366,#88367,#88368,#88369,#88370,#88371,#88372,#88373,#88374,#88375,#88376,
#88377,#88378,#88379,#88380,#88381,#88382,#88383,#88384,#88385,#88386,#88387,
#88388,#88389,#88390,#88391,#88392),(#88393,#88394,#88395,#88396,#88397,
#88398,#88399,#88400,#88401,#88402,#88403,#88404,#88405,#88406,#88407,#88408,
#88409,#88410,#88411,#88412,#88413,#88414,#88415,#88416,#88417,#88418,#88419,
#88420,#88421,#88422,#88423,#88424,#88425,#88426,#88427,#88428,#88429,#88430,
#88431,#88432,#88433,#88434,#88435,#88436,#88437,#88438,#88439,#88440,#88441,
#88442,#88443,#88444,#88445,#88446,#88447,#88448,#88449,#88450,#88451,#88452,
#88453,#88454,#88455,#88456,#88457,#88458,#88459,#88460,#88461,#88462,#88463,
#88464,#88465,#88466,#88467,#88468,#88469,#88470,#88471,#88472,#88473,#88474,
#88475,#88476,#88477,#88478,#88479,#88480,#88481,#88482,#88483,#88484,#88485,
#88486,#88487,#88488,#88489,#88490,#88491,#88492,#88493,#88494,#88495,#88496,
#88497,#88498,#88499,#88500,#88501,#88502,#88503,#88504,#88505,#88506,#88507,
#88508,#88509,#88510,#88511,#88512,#88513,#88514,#88515,#88516,#88517,#88518,
#88519,#88520,#88521,#88522,#88523)),.UNSPECIFIED.,.F.,.F.,.F.,(4,4),(4,
1,1,1,1,1,1,1,1,1,1,1,1,1,1,1,1,1,1,1,1,1,1,1,1,1,1,1,1,1,1,1,1,1,1,1,1,
1,1,1,1,1,1,1,1,1,1,1,1,1,1,1,1,1,1,1,1,1,1,1,1,1,1,1,1,1,1,1,1,1,1,1,1,
1,1,1,1,1,1,1,1,1,1,1,1,1,1,1,1,1,1,1,1,1,1,1,1,1,1,1,1,1,1,1,1,1,1,1,1,
1,1,1,1,1,1,1,1,1,1,1,1,1,1,1,1,1,1,1,4),(0.,0.0642013499338864),(11.8589888623077,
12.8564939485313,13.8539990347549,14.8515041209785,15.8490092072021,16.8465142934256,
17.8440193796492,18.8415244658728,19.8390295520964,20.83653463832,21.8340397245436,
22.8315448107672,23.8290498969908,24.8265549832144,25.824060069438,26.8215651556616,
27.8190702418852,28.8165753281088,29.8140804143324,30.811585500556,31.8090905867796,
32.8065956730032,33.8041007592268,34.8016058454504,35.799110931674,36.7966160178976,
37.7941211041212,38.7916261903448,39.7891312765683,40.7866363627919,41.7841414490155,
42.7816465352391,43.7791516214627,44.7766567076863,45.7741617939099,46.7716668801335,
47.7691719663571,48.7666770525807,49.7641821388043,50.7616872250279,51.7591923112515,
52.7566973974751,53.7542024836987,54.7517075699223,55.7492126561459,56.7467177423695,
57.7442228285931,58.7417279148167,59.7392330010403,60.7367380872638,61.7342431734874,
62.731748259711,63.7292533459346,64.7267584321582,65.7242635183818,66.7217686046054,
67.719273690829,68.7167787770526,69.7142838632762,70.7117889494998,71.7092940357234,
72.706799121947,73.7043042081706,74.7018092943942,75.6993143806178,76.6968194668414,
77.694324553065,78.6918296392886,79.6893347255122,80.6868398117358,81.6843448979593,
82.6818499841829,83.6793550704065,84.6768601566301,85.6743652428537,86.6718703290773,
87.6693754153009,88.6668805015245,89.6643855877481,90.6618906739717,91.6593957601953,
92.6569008464189,93.6544059326425,94.6519110188661,95.6494161050897,96.6469211913133,
97.6444262775369,98.6419313637605,99.6394364499841,100.636941536208,101.634446622431,
102.631951708655,103.629456794878,104.626961881102,105.624466967326,106.621972053549,
107.619477139773,108.616982225996,109.61448731222,110.611992398444,111.609497484667,
112.607002570891,113.604507657114,114.602012743338,115.599517829562,116.597022915785,
117.594528002009,118.592033088232,119.589538174456,120.58704326068,121.584548346903,
122.582053433127,123.57955851935,124.577063605574,125.574568691798,126.572073778021,
127.569578864245,128.567083950468,129.564589036692,130.562094122916,131.559599209139,
132.557104295363,133.554609381586,134.55211446781,135.549619554034,136.547124640257,
137.544629726481,138.542134812704,139.539639898928),.UNSPECIFIED.);
#371=B_SPLINE_SURFACE_WITH_KNOTS('',3,3,((#88643,#88644,#88645,#88646,#88647,
#88648,#88649,#88650,#88651,#88652,#88653,#88654,#88655,#88656,#88657,#88658,
#88659,#88660,#88661,#88662,#88663,#88664,#88665,#88666,#88667,#88668,#88669,
#88670,#88671,#88672,#88673,#88674,#88675,#88676,#88677,#88678,#88679,#88680,
#88681,#88682,#88683,#88684,#88685,#88686,#88687,#88688,#88689,#88690,#88691,
#88692,#88693,#88694,#88695,#88696,#88697,#88698,#88699,#88700,#88701,#88702,
#88703,#88704,#88705,#88706,#88707,#88708,#88709,#88710,#88711,#88712,#88713,
#88714,#88715,#88716,#88717,#88718,#88719,#88720,#88721,#88722,#88723,#88724,
#88725,#88726,#88727,#88728,#88729,#88730,#88731,#88732,#88733,#88734,#88735,
#88736,#88737,#88738,#88739,#88740,#88741,#88742,#88743,#88744,#88745,#88746,
#88747,#88748,#88749,#88750,#88751,#88752,#88753,#88754,#88755,#88756,#88757,
#88758,#88759,#88760,#88761,#88762,#88763,#88764,#88765,#88766,#88767,#88768,
#88769,#88770,#88771,#88772,#88773),(#88774,#88775,#88776,#88777,#88778,
#88779,#88780,#88781,#88782,#88783,#88784,#88785,#88786,#88787,#88788,#88789,
#88790,#88791,#88792,#88793,#88794,#88795,#88796,#88797,#88798,#88799,#88800,
#88801,#88802,#88803,#88804,#88805,#88806,#88807,#88808,#88809,#88810,#88811,
#88812,#88813,#88814,#88815,#88816,#88817,#88818,#88819,#88820,#88821,#88822,
#88823,#88824,#88825,#88826,#88827,#88828,#88829,#88830,#88831,#88832,#88833,
#88834,#88835,#88836,#88837,#88838,#88839,#88840,#88841,#88842,#88843,#88844,
#88845,#88846,#88847,#88848,#88849,#88850,#88851,#88852,#88853,#88854,#88855,
#88856,#88857,#88858,#88859,#88860,#88861,#88862,#88863,#88864,#88865,#88866,
#88867,#88868,#88869,#88870,#88871,#88872,#88873,#88874,#88875,#88876,#88877,
#88878,#88879,#88880,#88881,#88882,#88883,#88884,#88885,#88886,#88887,#88888,
#88889,#88890,#88891,#88892,#88893,#88894,#88895,#88896,#88897,#88898,#88899,
#88900,#88901,#88902,#88903,#88904),(#88905,#88906,#88907,#88908,#88909,
#88910,#88911,#88912,#88913,#88914,#88915,#88916,#88917,#88918,#88919,#88920,
#88921,#88922,#88923,#88924,#88925,#88926,#88927,#88928,#88929,#88930,#88931,
#88932,#88933,#88934,#88935,#88936,#88937,#88938,#88939,#88940,#88941,#88942,
#88943,#88944,#88945,#88946,#88947,#88948,#88949,#88950,#88951,#88952,#88953,
#88954,#88955,#88956,#88957,#88958,#88959,#88960,#88961,#88962,#88963,#88964,
#88965,#88966,#88967,#88968,#88969,#88970,#88971,#88972,#88973,#88974,#88975,
#88976,#88977,#88978,#88979,#88980,#88981,#88982,#88983,#88984,#88985,#88986,
#88987,#88988,#88989,#88990,#88991,#88992,#88993,#88994,#88995,#88996,#88997,
#88998,#88999,#89000,#89001,#89002,#89003,#89004,#89005,#89006,#89007,#89008,
#89009,#89010,#89011,#89012,#89013,#89014,#89015,#89016,#89017,#89018,#89019,
#89020,#89021,#89022,#89023,#89024,#89025,#89026,#89027,#89028,#89029,#89030,
#89031,#89032,#89033,#89034,#89035),(#89036,#89037,#89038,#89039,#89040,
#89041,#89042,#89043,#89044,#89045,#89046,#89047,#89048,#89049,#89050,#89051,
#89052,#89053,#89054,#89055,#89056,#89057,#89058,#89059,#89060,#89061,#89062,
#89063,#89064,#89065,#89066,#89067,#89068,#89069,#89070,#89071,#89072,#89073,
#89074,#89075,#89076,#89077,#89078,#89079,#89080,#89081,#89082,#89083,#89084,
#89085,#89086,#89087,#89088,#89089,#89090,#89091,#89092,#89093,#89094,#89095,
#89096,#89097,#89098,#89099,#89100,#89101,#89102,#89103,#89104,#89105,#89106,
#89107,#89108,#89109,#89110,#89111,#89112,#89113,#89114,#89115,#89116,#89117,
#89118,#89119,#89120,#89121,#89122,#89123,#89124,#89125,#89126,#89127,#89128,
#89129,#89130,#89131,#89132,#89133,#89134,#89135,#89136,#89137,#89138,#89139,
#89140,#89141,#89142,#89143,#89144,#89145,#89146,#89147,#89148,#89149,#89150,
#89151,#89152,#89153,#89154,#89155,#89156,#89157,#89158,#89159,#89160,#89161,
#89162,#89163,#89164,#89165,#89166)),.UNSPECIFIED.,.F.,.F.,.F.,(4,4),(4,
1,1,1,1,1,1,1,1,1,1,1,1,1,1,1,1,1,1,1,1,1,1,1,1,1,1,1,1,1,1,1,1,1,1,1,1,
1,1,1,1,1,1,1,1,1,1,1,1,1,1,1,1,1,1,1,1,1,1,1,1,1,1,1,1,1,1,1,1,1,1,1,1,
1,1,1,1,1,1,1,1,1,1,1,1,1,1,1,1,1,1,1,1,1,1,1,1,1,1,1,1,1,1,1,1,1,1,1,1,
1,1,1,1,1,1,1,1,1,1,1,1,1,1,1,1,1,1,1,4),(0.,0.0642013499338864),(14.3984001269717,
15.3959052131953,16.3934102994189,17.3909153856425,18.3884204718661,19.3859255580897,
20.3834306443133,21.3809357305369,22.3784408167605,23.3759459029841,24.3734509892077,
25.3709560754313,26.3684611616549,27.3659662478785,28.363471334102,29.3609764203256,
30.3584815065492,31.3559865927728,32.3534916789964,33.35099676522,34.3485018514436,
35.3460069376672,36.3435120238908,37.3410171101144,38.338522196338,39.3360272825616,
40.3335323687852,41.3310374550088,42.3285425412324,43.326047627456,44.3235527136796,
45.3210577999032,46.3185628861268,47.3160679723504,48.3135730585739,49.3110781447975,
50.3085832310211,51.3060883172447,52.3035934034683,53.3010984896919,54.2986035759155,
55.2961086621391,56.2936137483627,57.2911188345863,58.2886239208099,59.2861290070335,
60.2836340932571,61.2811391794807,62.2786442657043,63.2761493519279,64.2736544381515,
65.2711595243751,66.2686646105986,67.2661696968223,68.2636747830458,69.2611798692694,
70.258684955493,71.2561900417166,72.2536951279402,73.2512002141638,74.2487053003874,
75.246210386611,76.2437154728346,77.2412205590582,78.2387256452818,79.2362307315054,
80.233735817729,81.2312409039526,82.2287459901762,83.2262510763998,84.2237561626234,
85.221261248847,86.2187663350706,87.2162714212942,88.2137765075177,89.2112815937413,
90.2087866799649,91.2062917661885,92.2037968524121,93.2013019386357,94.1988070248593,
95.1963121110829,96.1938171973065,97.1913222835301,98.1888273697537,99.1863324559773,
100.183837542201,101.181342628424,102.178847714648,103.176352800872,104.173857887095,
105.171362973319,106.168868059542,107.166373145766,108.16387823199,109.161383318213,
110.158888404437,111.15639349066,112.153898576884,113.151403663108,114.148908749331,
115.146413835555,116.143918921778,117.141424008002,118.138929094226,119.136434180449,
120.133939266673,121.131444352896,122.12894943912,123.126454525344,124.123959611567,
125.121464697791,126.118969784014,127.116474870238,128.113979956462,129.111485042685,
130.108990128909,131.106495215132,132.104000301356,133.10150538758,134.099010473803,
135.096515560027,136.09402064625,137.091525732474,138.089030818697,139.086535904921,
140.084040991145,141.081546077368,142.079051163592),.UNSPECIFIED.);
#372=B_SPLINE_SURFACE_WITH_KNOTS('',3,3,((#89305,#89306,#89307,#89308,#89309,
#89310,#89311,#89312,#89313,#89314,#89315,#89316,#89317,#89318,#89319,#89320,
#89321,#89322,#89323,#89324,#89325,#89326,#89327,#89328,#89329,#89330,#89331,
#89332,#89333,#89334,#89335,#89336,#89337,#89338,#89339,#89340,#89341,#89342,
#89343,#89344,#89345,#89346,#89347,#89348,#89349,#89350,#89351,#89352,#89353,
#89354,#89355,#89356,#89357,#89358,#89359,#89360,#89361,#89362,#89363,#89364,
#89365,#89366,#89367,#89368,#89369,#89370,#89371,#89372,#89373,#89374,#89375,
#89376,#89377,#89378,#89379,#89380,#89381,#89382,#89383,#89384,#89385,#89386,
#89387,#89388,#89389,#89390,#89391,#89392,#89393,#89394,#89395,#89396,#89397,
#89398,#89399,#89400,#89401,#89402,#89403,#89404,#89405,#89406,#89407,#89408,
#89409,#89410,#89411,#89412,#89413,#89414,#89415,#89416,#89417,#89418,#89419,
#89420,#89421,#89422,#89423,#89424,#89425,#89426,#89427,#89428,#89429,#89430,
#89431,#89432,#89433,#89434,#89435),(#89436,#89437,#89438,#89439,#89440,
#89441,#89442,#89443,#89444,#89445,#89446,#89447,#89448,#89449,#89450,#89451,
#89452,#89453,#89454,#89455,#89456,#89457,#89458,#89459,#89460,#89461,#89462,
#89463,#89464,#89465,#89466,#89467,#89468,#89469,#89470,#89471,#89472,#89473,
#89474,#89475,#89476,#89477,#89478,#89479,#89480,#89481,#89482,#89483,#89484,
#89485,#89486,#89487,#89488,#89489,#89490,#89491,#89492,#89493,#89494,#89495,
#89496,#89497,#89498,#89499,#89500,#89501,#89502,#89503,#89504,#89505,#89506,
#89507,#89508,#89509,#89510,#89511,#89512,#89513,#89514,#89515,#89516,#89517,
#89518,#89519,#89520,#89521,#89522,#89523,#89524,#89525,#89526,#89527,#89528,
#89529,#89530,#89531,#89532,#89533,#89534,#89535,#89536,#89537,#89538,#89539,
#89540,#89541,#89542,#89543,#89544,#89545,#89546,#89547,#89548,#89549,#89550,
#89551,#89552,#89553,#89554,#89555,#89556,#89557,#89558,#89559,#89560,#89561,
#89562,#89563,#89564,#89565,#89566),(#89567,#89568,#89569,#89570,#89571,
#89572,#89573,#89574,#89575,#89576,#89577,#89578,#89579,#89580,#89581,#89582,
#89583,#89584,#89585,#89586,#89587,#89588,#89589,#89590,#89591,#89592,#89593,
#89594,#89595,#89596,#89597,#89598,#89599,#89600,#89601,#89602,#89603,#89604,
#89605,#89606,#89607,#89608,#89609,#89610,#89611,#89612,#89613,#89614,#89615,
#89616,#89617,#89618,#89619,#89620,#89621,#89622,#89623,#89624,#89625,#89626,
#89627,#89628,#89629,#89630,#89631,#89632,#89633,#89634,#89635,#89636,#89637,
#89638,#89639,#89640,#89641,#89642,#89643,#89644,#89645,#89646,#89647,#89648,
#89649,#89650,#89651,#89652,#89653,#89654,#89655,#89656,#89657,#89658,#89659,
#89660,#89661,#89662,#89663,#89664,#89665,#89666,#89667,#89668,#89669,#89670,
#89671,#89672,#89673,#89674,#89675,#89676,#89677,#89678,#89679,#89680,#89681,
#89682,#89683,#89684,#89685,#89686,#89687,#89688,#89689,#89690,#89691,#89692,
#89693,#89694,#89695,#89696,#89697),(#89698,#89699,#89700,#89701,#89702,
#89703,#89704,#89705,#89706,#89707,#89708,#89709,#89710,#89711,#89712,#89713,
#89714,#89715,#89716,#89717,#89718,#89719,#89720,#89721,#89722,#89723,#89724,
#89725,#89726,#89727,#89728,#89729,#89730,#89731,#89732,#89733,#89734,#89735,
#89736,#89737,#89738,#89739,#89740,#89741,#89742,#89743,#89744,#89745,#89746,
#89747,#89748,#89749,#89750,#89751,#89752,#89753,#89754,#89755,#89756,#89757,
#89758,#89759,#89760,#89761,#89762,#89763,#89764,#89765,#89766,#89767,#89768,
#89769,#89770,#89771,#89772,#89773,#89774,#89775,#89776,#89777,#89778,#89779,
#89780,#89781,#89782,#89783,#89784,#89785,#89786,#89787,#89788,#89789,#89790,
#89791,#89792,#89793,#89794,#89795,#89796,#89797,#89798,#89799,#89800,#89801,
#89802,#89803,#89804,#89805,#89806,#89807,#89808,#89809,#89810,#89811,#89812,
#89813,#89814,#89815,#89816,#89817,#89818,#89819,#89820,#89821,#89822,#89823,
#89824,#89825,#89826,#89827,#89828)),.UNSPECIFIED.,.F.,.F.,.F.,(4,4),(4,
1,1,1,1,1,1,1,1,1,1,1,1,1,1,1,1,1,1,1,1,1,1,1,1,1,1,1,1,1,1,1,1,1,1,1,1,
1,1,1,1,1,1,1,1,1,1,1,1,1,1,1,1,1,1,1,1,1,1,1,1,1,1,1,1,1,1,1,1,1,1,1,1,
1,1,1,1,1,1,1,1,1,1,1,1,1,1,1,1,1,1,1,1,1,1,1,1,1,1,1,1,1,1,1,1,1,1,1,1,
1,1,1,1,1,1,1,1,1,1,1,1,1,1,1,1,1,1,1,4),(0.,0.0642013499338863),(11.8589888623077,
12.8564939485313,13.8539990347549,14.8515041209785,15.8490092072021,16.8465142934257,
17.8440193796493,18.8415244658729,19.8390295520965,20.8365346383201,21.8340397245437,
22.8315448107673,23.8290498969909,24.8265549832145,25.8240600694381,26.8215651556617,
27.8190702418853,28.8165753281089,29.8140804143324,30.811585500556,31.8090905867796,
32.8065956730032,33.8041007592268,34.8016058454504,35.799110931674,36.7966160178976,
37.7941211041212,38.7916261903448,39.7891312765684,40.786636362792,41.7841414490156,
42.7816465352392,43.7791516214628,44.7766567076864,45.77416179391,46.7716668801336,
47.7691719663572,48.7666770525807,49.7641821388043,50.7616872250279,51.7591923112515,
52.7566973974751,53.7542024836987,54.7517075699223,55.7492126561459,56.7467177423695,
57.7442228285931,58.7417279148167,59.7392330010403,60.7367380872639,61.7342431734875,
62.7317482597111,63.7292533459347,64.7267584321583,65.7242635183819,66.7217686046055,
67.7192736908291,68.7167787770527,69.7142838632763,70.7117889494998,71.7092940357234,
72.706799121947,73.7043042081706,74.7018092943942,75.6993143806178,76.6968194668414,
77.694324553065,78.6918296392886,79.6893347255122,80.6868398117358,81.6843448979594,
82.681849984183,83.6793550704066,84.6768601566302,85.6743652428538,86.6718703290774,
87.669375415301,88.6668805015246,89.6643855877482,90.6618906739717,91.6593957601953,
92.6569008464189,93.6544059326425,94.6519110188661,95.6494161050897,96.6469211913133,
97.6444262775369,98.6419313637605,99.6394364499841,100.636941536208,101.634446622431,
102.631951708655,103.629456794878,104.626961881102,105.624466967326,106.621972053549,
107.619477139773,108.616982225996,109.61448731222,110.611992398444,111.609497484667,
112.607002570891,113.604507657114,114.602012743338,115.599517829562,116.597022915785,
117.594528002009,118.592033088232,119.589538174456,120.58704326068,121.584548346903,
122.582053433127,123.57955851935,124.577063605574,125.574568691798,126.572073778021,
127.569578864245,128.567083950468,129.564589036692,130.562094122916,131.559599209139,
132.557104295363,133.554609381586,134.55211446781,135.549619554034,136.547124640257,
137.544629726481,138.542134812704,139.539639898928),.UNSPECIFIED.);
#373=B_SPLINE_SURFACE_WITH_KNOTS('',3,3,((#89948,#89949,#89950,#89951,#89952,
#89953,#89954,#89955,#89956,#89957,#89958,#89959,#89960,#89961,#89962,#89963,
#89964,#89965,#89966,#89967,#89968,#89969,#89970,#89971,#89972,#89973,#89974,
#89975,#89976,#89977,#89978,#89979,#89980,#89981,#89982,#89983,#89984,#89985,
#89986,#89987,#89988,#89989,#89990,#89991,#89992,#89993,#89994,#89995,#89996,
#89997,#89998,#89999,#90000,#90001,#90002,#90003,#90004,#90005,#90006,#90007,
#90008,#90009,#90010,#90011,#90012,#90013,#90014,#90015,#90016,#90017,#90018,
#90019,#90020,#90021,#90022,#90023,#90024,#90025,#90026,#90027,#90028,#90029,
#90030,#90031,#90032,#90033,#90034,#90035,#90036,#90037,#90038,#90039,#90040,
#90041,#90042,#90043,#90044,#90045,#90046,#90047,#90048,#90049,#90050,#90051,
#90052,#90053,#90054,#90055,#90056,#90057,#90058,#90059,#90060,#90061,#90062,
#90063,#90064,#90065,#90066,#90067,#90068,#90069,#90070,#90071,#90072,#90073,
#90074,#90075,#90076,#90077,#90078),(#90079,#90080,#90081,#90082,#90083,
#90084,#90085,#90086,#90087,#90088,#90089,#90090,#90091,#90092,#90093,#90094,
#90095,#90096,#90097,#90098,#90099,#90100,#90101,#90102,#90103,#90104,#90105,
#90106,#90107,#90108,#90109,#90110,#90111,#90112,#90113,#90114,#90115,#90116,
#90117,#90118,#90119,#90120,#90121,#90122,#90123,#90124,#90125,#90126,#90127,
#90128,#90129,#90130,#90131,#90132,#90133,#90134,#90135,#90136,#90137,#90138,
#90139,#90140,#90141,#90142,#90143,#90144,#90145,#90146,#90147,#90148,#90149,
#90150,#90151,#90152,#90153,#90154,#90155,#90156,#90157,#90158,#90159,#90160,
#90161,#90162,#90163,#90164,#90165,#90166,#90167,#90168,#90169,#90170,#90171,
#90172,#90173,#90174,#90175,#90176,#90177,#90178,#90179,#90180,#90181,#90182,
#90183,#90184,#90185,#90186,#90187,#90188,#90189,#90190,#90191,#90192,#90193,
#90194,#90195,#90196,#90197,#90198,#90199,#90200,#90201,#90202,#90203,#90204,
#90205,#90206,#90207,#90208,#90209),(#90210,#90211,#90212,#90213,#90214,
#90215,#90216,#90217,#90218,#90219,#90220,#90221,#90222,#90223,#90224,#90225,
#90226,#90227,#90228,#90229,#90230,#90231,#90232,#90233,#90234,#90235,#90236,
#90237,#90238,#90239,#90240,#90241,#90242,#90243,#90244,#90245,#90246,#90247,
#90248,#90249,#90250,#90251,#90252,#90253,#90254,#90255,#90256,#90257,#90258,
#90259,#90260,#90261,#90262,#90263,#90264,#90265,#90266,#90267,#90268,#90269,
#90270,#90271,#90272,#90273,#90274,#90275,#90276,#90277,#90278,#90279,#90280,
#90281,#90282,#90283,#90284,#90285,#90286,#90287,#90288,#90289,#90290,#90291,
#90292,#90293,#90294,#90295,#90296,#90297,#90298,#90299,#90300,#90301,#90302,
#90303,#90304,#90305,#90306,#90307,#90308,#90309,#90310,#90311,#90312,#90313,
#90314,#90315,#90316,#90317,#90318,#90319,#90320,#90321,#90322,#90323,#90324,
#90325,#90326,#90327,#90328,#90329,#90330,#90331,#90332,#90333,#90334,#90335,
#90336,#90337,#90338,#90339,#90340),(#90341,#90342,#90343,#90344,#90345,
#90346,#90347,#90348,#90349,#90350,#90351,#90352,#90353,#90354,#90355,#90356,
#90357,#90358,#90359,#90360,#90361,#90362,#90363,#90364,#90365,#90366,#90367,
#90368,#90369,#90370,#90371,#90372,#90373,#90374,#90375,#90376,#90377,#90378,
#90379,#90380,#90381,#90382,#90383,#90384,#90385,#90386,#90387,#90388,#90389,
#90390,#90391,#90392,#90393,#90394,#90395,#90396,#90397,#90398,#90399,#90400,
#90401,#90402,#90403,#90404,#90405,#90406,#90407,#90408,#90409,#90410,#90411,
#90412,#90413,#90414,#90415,#90416,#90417,#90418,#90419,#90420,#90421,#90422,
#90423,#90424,#90425,#90426,#90427,#90428,#90429,#90430,#90431,#90432,#90433,
#90434,#90435,#90436,#90437,#90438,#90439,#90440,#90441,#90442,#90443,#90444,
#90445,#90446,#90447,#90448,#90449,#90450,#90451,#90452,#90453,#90454,#90455,
#90456,#90457,#90458,#90459,#90460,#90461,#90462,#90463,#90464,#90465,#90466,
#90467,#90468,#90469,#90470,#90471)),.UNSPECIFIED.,.F.,.F.,.F.,(4,4),(4,
1,1,1,1,1,1,1,1,1,1,1,1,1,1,1,1,1,1,1,1,1,1,1,1,1,1,1,1,1,1,1,1,1,1,1,1,
1,1,1,1,1,1,1,1,1,1,1,1,1,1,1,1,1,1,1,1,1,1,1,1,1,1,1,1,1,1,1,1,1,1,1,1,
1,1,1,1,1,1,1,1,1,1,1,1,1,1,1,1,1,1,1,1,1,1,1,1,1,1,1,1,1,1,1,1,1,1,1,1,
1,1,1,1,1,1,1,1,1,1,1,1,1,1,1,1,1,1,1,4),(0.,0.0642013499338863),(14.3984001269718,
15.3959052131954,16.393410299419,17.3909153856426,18.3884204718662,19.3859255580897,
20.3834306443133,21.3809357305369,22.3784408167605,23.3759459029841,24.3734509892077,
25.3709560754313,26.3684611616549,27.3659662478785,28.3634713341021,29.3609764203257,
30.3584815065493,31.3559865927729,32.3534916789965,33.3509967652201,34.3485018514437,
35.3460069376673,36.3435120238909,37.3410171101145,38.3385221963381,39.3360272825617,
40.3335323687852,41.3310374550088,42.3285425412324,43.326047627456,44.3235527136796,
45.3210577999032,46.3185628861268,47.3160679723504,48.313573058574,49.3110781447976,
50.3085832310212,51.3060883172448,52.3035934034684,53.301098489692,54.2986035759156,
55.2961086621392,56.2936137483628,57.2911188345864,58.28862392081,59.2861290070336,
60.2836340932571,61.2811391794807,62.2786442657043,63.2761493519279,64.2736544381515,
65.2711595243751,66.2686646105987,67.2661696968223,68.2636747830459,69.2611798692695,
70.2586849554931,71.2561900417167,72.2536951279403,73.2512002141639,74.2487053003875,
75.2462103866111,76.2437154728347,77.2412205590583,78.2387256452819,79.2362307315055,
80.2337358177291,81.2312409039527,82.2287459901763,83.2262510763998,84.2237561626234,
85.221261248847,86.2187663350706,87.2162714212942,88.2137765075178,89.2112815937414,
90.208786679965,91.2062917661886,92.2037968524122,93.2013019386358,94.1988070248594,
95.196312111083,96.1938171973066,97.1913222835302,98.1888273697538,99.1863324559774,
100.183837542201,101.181342628425,102.178847714648,103.176352800872,104.173857887095,
105.171362973319,106.168868059543,107.166373145766,108.16387823199,109.161383318213,
110.158888404437,111.156393490661,112.153898576884,113.151403663108,114.148908749331,
115.146413835555,116.143918921778,117.141424008002,118.138929094226,119.136434180449,
120.133939266673,121.131444352896,122.12894943912,123.126454525344,124.123959611567,
125.121464697791,126.118969784014,127.116474870238,128.113979956462,129.111485042685,
130.108990128909,131.106495215132,132.104000301356,133.10150538758,134.099010473803,
135.096515560027,136.09402064625,137.091525732474,138.089030818698,139.086535904921,
140.084040991145,141.081546077368,142.079051163592),.UNSPECIFIED.);
#374=B_SPLINE_SURFACE_WITH_KNOTS('',3,3,((#94542,#94543,#94544,#94545,#94546,
#94547,#94548,#94549,#94550,#94551,#94552,#94553,#94554,#94555,#94556,#94557,
#94558,#94559,#94560,#94561,#94562,#94563,#94564,#94565,#94566,#94567,#94568,
#94569,#94570,#94571,#94572,#94573,#94574,#94575,#94576,#94577,#94578,#94579,
#94580,#94581,#94582,#94583,#94584,#94585,#94586,#94587,#94588,#94589,#94590,
#94591,#94592,#94593,#94594,#94595,#94596,#94597,#94598,#94599,#94600,#94601,
#94602,#94603,#94604,#94605,#94606,#94607,#94608,#94609,#94610,#94611,#94612,
#94613,#94614,#94615,#94616,#94617,#94618,#94619,#94620,#94621,#94622,#94623,
#94624,#94625,#94626,#94627,#94628,#94629,#94630,#94631,#94632,#94633,#94634,
#94635,#94636,#94637,#94638,#94639,#94640,#94641,#94642,#94643,#94644,#94645,
#94646,#94647,#94648,#94649,#94650,#94651,#94652,#94653,#94654,#94655,#94656,
#94657,#94658,#94659,#94660,#94661,#94662,#94663,#94664,#94665,#94666,#94667,
#94668,#94669,#94670,#94671,#94672,#94673,#94674,#94675,#94676,#94677,#94678,
#94679,#94680,#94681,#94682,#94683,#94684,#94685,#94686,#94687,#94688,#94689,
#94690,#94691,#94692,#94693,#94694,#94695,#94696,#94697,#94698,#94699,#94700,
#94701,#94702,#94703,#94704,#94705,#94706,#94707,#94708,#94709,#94710,#94711,
#94712,#94713,#94714,#94715,#94716,#94717,#94718,#94719,#94720,#94721,#94722,
#94723,#94724,#94725,#94726,#94727,#94728,#94729,#94730,#94731,#94732,#94733,
#94734,#94735,#94736,#94737,#94738,#94739,#94740,#94741,#94742,#94743,#94744,
#94745,#94746,#94747,#94748,#94749,#94750,#94751,#94752,#94753,#94754,#94755,
#94756,#94757,#94758,#94759,#94760,#94761,#94762,#94763,#94764,#94765,#94766,
#94767,#94768,#94769,#94770,#94771,#94772,#94773,#94774,#94775,#94776,#94777,
#94778,#94779,#94780,#94781,#94782,#94783,#94784,#94785,#94786,#94787,#94788,
#94789,#94790,#94791,#94792,#94793,#94794,#94795,#94796,#94797,#94798,#94799,
#94800,#94801,#94802,#94803,#94804,#94805,#94806,#94807,#94808,#94809,#94810,
#94811,#94812,#94813,#94814,#94815,#94816,#94817,#94818,#94819,#94820,#94821,
#94822,#94823,#94824,#94825,#94826,#94827,#94828,#94829,#94830,#94831,#94832,
#94833,#94834,#94835,#94836,#94837,#94838,#94839,#94840,#94841,#94842,#94843,
#94844,#94845,#94846,#94847,#94848,#94849,#94850,#94851,#94852,#94853,#94854,
#94855,#94856),(#94857,#94858,#94859,#94860,#94861,#94862,#94863,#94864,
#94865,#94866,#94867,#94868,#94869,#94870,#94871,#94872,#94873,#94874,#94875,
#94876,#94877,#94878,#94879,#94880,#94881,#94882,#94883,#94884,#94885,#94886,
#94887,#94888,#94889,#94890,#94891,#94892,#94893,#94894,#94895,#94896,#94897,
#94898,#94899,#94900,#94901,#94902,#94903,#94904,#94905,#94906,#94907,#94908,
#94909,#94910,#94911,#94912,#94913,#94914,#94915,#94916,#94917,#94918,#94919,
#94920,#94921,#94922,#94923,#94924,#94925,#94926,#94927,#94928,#94929,#94930,
#94931,#94932,#94933,#94934,#94935,#94936,#94937,#94938,#94939,#94940,#94941,
#94942,#94943,#94944,#94945,#94946,#94947,#94948,#94949,#94950,#94951,#94952,
#94953,#94954,#94955,#94956,#94957,#94958,#94959,#94960,#94961,#94962,#94963,
#94964,#94965,#94966,#94967,#94968,#94969,#94970,#94971,#94972,#94973,#94974,
#94975,#94976,#94977,#94978,#94979,#94980,#94981,#94982,#94983,#94984,#94985,
#94986,#94987,#94988,#94989,#94990,#94991,#94992,#94993,#94994,#94995,#94996,
#94997,#94998,#94999,#95000,#95001,#95002,#95003,#95004,#95005,#95006,#95007,
#95008,#95009,#95010,#95011,#95012,#95013,#95014,#95015,#95016,#95017,#95018,
#95019,#95020,#95021,#95022,#95023,#95024,#95025,#95026,#95027,#95028,#95029,
#95030,#95031,#95032,#95033,#95034,#95035,#95036,#95037,#95038,#95039,#95040,
#95041,#95042,#95043,#95044,#95045,#95046,#95047,#95048,#95049,#95050,#95051,
#95052,#95053,#95054,#95055,#95056,#95057,#95058,#95059,#95060,#95061,#95062,
#95063,#95064,#95065,#95066,#95067,#95068,#95069,#95070,#95071,#95072,#95073,
#95074,#95075,#95076,#95077,#95078,#95079,#95080,#95081,#95082,#95083,#95084,
#95085,#95086,#95087,#95088,#95089,#95090,#95091,#95092,#95093,#95094,#95095,
#95096,#95097,#95098,#95099,#95100,#95101,#95102,#95103,#95104,#95105,#95106,
#95107,#95108,#95109,#95110,#95111,#95112,#95113,#95114,#95115,#95116,#95117,
#95118,#95119,#95120,#95121,#95122,#95123,#95124,#95125,#95126,#95127,#95128,
#95129,#95130,#95131,#95132,#95133,#95134,#95135,#95136,#95137,#95138,#95139,
#95140,#95141,#95142,#95143,#95144,#95145,#95146,#95147,#95148,#95149,#95150,
#95151,#95152,#95153,#95154,#95155,#95156,#95157,#95158,#95159,#95160,#95161,
#95162,#95163,#95164,#95165,#95166,#95167,#95168,#95169,#95170,#95171),
(#95172,#95173,#95174,#95175,#95176,#95177,#95178,#95179,#95180,#95181,
#95182,#95183,#95184,#95185,#95186,#95187,#95188,#95189,#95190,#95191,#95192,
#95193,#95194,#95195,#95196,#95197,#95198,#95199,#95200,#95201,#95202,#95203,
#95204,#95205,#95206,#95207,#95208,#95209,#95210,#95211,#95212,#95213,#95214,
#95215,#95216,#95217,#95218,#95219,#95220,#95221,#95222,#95223,#95224,#95225,
#95226,#95227,#95228,#95229,#95230,#95231,#95232,#95233,#95234,#95235,#95236,
#95237,#95238,#95239,#95240,#95241,#95242,#95243,#95244,#95245,#95246,#95247,
#95248,#95249,#95250,#95251,#95252,#95253,#95254,#95255,#95256,#95257,#95258,
#95259,#95260,#95261,#95262,#95263,#95264,#95265,#95266,#95267,#95268,#95269,
#95270,#95271,#95272,#95273,#95274,#95275,#95276,#95277,#95278,#95279,#95280,
#95281,#95282,#95283,#95284,#95285,#95286,#95287,#95288,#95289,#95290,#95291,
#95292,#95293,#95294,#95295,#95296,#95297,#95298,#95299,#95300,#95301,#95302,
#95303,#95304,#95305,#95306,#95307,#95308,#95309,#95310,#95311,#95312,#95313,
#95314,#95315,#95316,#95317,#95318,#95319,#95320,#95321,#95322,#95323,#95324,
#95325,#95326,#95327,#95328,#95329,#95330,#95331,#95332,#95333,#95334,#95335,
#95336,#95337,#95338,#95339,#95340,#95341,#95342,#95343,#95344,#95345,#95346,
#95347,#95348,#95349,#95350,#95351,#95352,#95353,#95354,#95355,#95356,#95357,
#95358,#95359,#95360,#95361,#95362,#95363,#95364,#95365,#95366,#95367,#95368,
#95369,#95370,#95371,#95372,#95373,#95374,#95375,#95376,#95377,#95378,#95379,
#95380,#95381,#95382,#95383,#95384,#95385,#95386,#95387,#95388,#95389,#95390,
#95391,#95392,#95393,#95394,#95395,#95396,#95397,#95398,#95399,#95400,#95401,
#95402,#95403,#95404,#95405,#95406,#95407,#95408,#95409,#95410,#95411,#95412,
#95413,#95414,#95415,#95416,#95417,#95418,#95419,#95420,#95421,#95422,#95423,
#95424,#95425,#95426,#95427,#95428,#95429,#95430,#95431,#95432,#95433,#95434,
#95435,#95436,#95437,#95438,#95439,#95440,#95441,#95442,#95443,#95444,#95445,
#95446,#95447,#95448,#95449,#95450,#95451,#95452,#95453,#95454,#95455,#95456,
#95457,#95458,#95459,#95460,#95461,#95462,#95463,#95464,#95465,#95466,#95467,
#95468,#95469,#95470,#95471,#95472,#95473,#95474,#95475,#95476,#95477,#95478,
#95479,#95480,#95481,#95482,#95483,#95484,#95485,#95486),(#95487,#95488,
#95489,#95490,#95491,#95492,#95493,#95494,#95495,#95496,#95497,#95498,#95499,
#95500,#95501,#95502,#95503,#95504,#95505,#95506,#95507,#95508,#95509,#95510,
#95511,#95512,#95513,#95514,#95515,#95516,#95517,#95518,#95519,#95520,#95521,
#95522,#95523,#95524,#95525,#95526,#95527,#95528,#95529,#95530,#95531,#95532,
#95533,#95534,#95535,#95536,#95537,#95538,#95539,#95540,#95541,#95542,#95543,
#95544,#95545,#95546,#95547,#95548,#95549,#95550,#95551,#95552,#95553,#95554,
#95555,#95556,#95557,#95558,#95559,#95560,#95561,#95562,#95563,#95564,#95565,
#95566,#95567,#95568,#95569,#95570,#95571,#95572,#95573,#95574,#95575,#95576,
#95577,#95578,#95579,#95580,#95581,#95582,#95583,#95584,#95585,#95586,#95587,
#95588,#95589,#95590,#95591,#95592,#95593,#95594,#95595,#95596,#95597,#95598,
#95599,#95600,#95601,#95602,#95603,#95604,#95605,#95606,#95607,#95608,#95609,
#95610,#95611,#95612,#95613,#95614,#95615,#95616,#95617,#95618,#95619,#95620,
#95621,#95622,#95623,#95624,#95625,#95626,#95627,#95628,#95629,#95630,#95631,
#95632,#95633,#95634,#95635,#95636,#95637,#95638,#95639,#95640,#95641,#95642,
#95643,#95644,#95645,#95646,#95647,#95648,#95649,#95650,#95651,#95652,#95653,
#95654,#95655,#95656,#95657,#95658,#95659,#95660,#95661,#95662,#95663,#95664,
#95665,#95666,#95667,#95668,#95669,#95670,#95671,#95672,#95673,#95674,#95675,
#95676,#95677,#95678,#95679,#95680,#95681,#95682,#95683,#95684,#95685,#95686,
#95687,#95688,#95689,#95690,#95691,#95692,#95693,#95694,#95695,#95696,#95697,
#95698,#95699,#95700,#95701,#95702,#95703,#95704,#95705,#95706,#95707,#95708,
#95709,#95710,#95711,#95712,#95713,#95714,#95715,#95716,#95717,#95718,#95719,
#95720,#95721,#95722,#95723,#95724,#95725,#95726,#95727,#95728,#95729,#95730,
#95731,#95732,#95733,#95734,#95735,#95736,#95737,#95738,#95739,#95740,#95741,
#95742,#95743,#95744,#95745,#95746,#95747,#95748,#95749,#95750,#95751,#95752,
#95753,#95754,#95755,#95756,#95757,#95758,#95759,#95760,#95761,#95762,#95763,
#95764,#95765,#95766,#95767,#95768,#95769,#95770,#95771,#95772,#95773,#95774,
#95775,#95776,#95777,#95778,#95779,#95780,#95781,#95782,#95783,#95784,#95785,
#95786,#95787,#95788,#95789,#95790,#95791,#95792,#95793,#95794,#95795,#95796,
#95797,#95798,#95799,#95800,#95801)),.UNSPECIFIED.,.F.,.F.,.F.,(4,4),(4,
1,1,1,1,1,1,1,1,1,1,1,1,1,1,1,1,1,1,1,1,1,1,1,1,1,1,1,1,1,1,1,1,1,1,1,1,
1,1,1,1,1,1,1,1,1,1,1,1,1,1,1,1,1,1,1,1,1,1,1,1,1,1,1,1,1,1,1,1,1,1,1,1,
1,1,1,1,1,1,1,1,1,1,1,1,1,1,1,1,1,1,1,1,1,1,1,1,1,1,1,1,1,1,1,1,1,1,1,1,
1,1,1,1,1,1,1,1,1,1,1,1,1,1,1,1,1,1,1,1,1,1,1,1,1,1,1,1,1,1,1,1,1,1,1,1,
1,1,1,1,1,1,1,1,1,1,1,1,1,1,1,1,1,1,1,1,1,1,1,1,1,1,1,1,1,1,1,1,1,1,1,1,
1,1,1,1,1,1,1,1,1,1,1,1,1,1,1,1,1,1,1,1,1,1,1,1,1,1,1,1,1,1,1,1,1,1,1,1,
1,1,1,1,1,1,1,1,1,1,1,1,1,1,1,1,1,1,1,1,1,1,1,1,1,1,1,1,1,1,1,1,1,1,1,1,
1,1,1,1,1,1,1,1,1,1,1,1,1,1,1,1,1,1,1,1,1,1,1,1,1,1,1,1,1,1,1,1,1,1,1,1,
1,1,1,1,1,1,1,1,1,1,1,1,1,1,1,1,1,1,1,1,1,1,1,4),(0.,0.0658467982010768),
(11.6150328478189,12.614467114553,13.6139013812871,14.6133356480212,15.6127699147553,
16.6122041814894,17.6116384482234,18.6110727149575,19.6105069816916,20.6099412484257,
21.6093755151598,22.6088097818939,23.608244048628,24.6076783153621,25.6071125820962,
26.6065468488302,27.6059811155643,28.6054153822984,29.6048496490325,30.6042839157666,
31.6037181825007,32.6031524492348,33.6025867159689,34.6020209827029,35.601455249437,
36.6008895161711,37.6003237829052,38.5997580496393,39.5991923163734,40.5986265831075,
41.5980608498416,42.5974951165757,43.5969293833097,44.5963636500438,45.5957979167779,
46.595232183512,47.5946664502461,48.5941007169802,49.5935349837143,50.5929692504484,
51.5924035171824,52.5918377839165,53.5912720506506,54.5907063173847,55.5901405841188,
56.5895748508529,57.589009117587,58.5884433843211,59.5878776510552,60.5873119177892,
61.5867461845233,62.5861804512574,63.5856147179915,64.5850489847256,65.5844832514597,
66.5839175181938,67.5833517849279,68.582786051662,69.582220318396,70.5816545851301,
71.5810888518642,72.5805231185983,73.5799573853324,74.5793916520665,75.5788259188006,
76.5782601855347,77.5776944522688,78.5771287190028,79.5765629857369,80.575997252471,
81.5754315192051,82.5748657859392,83.5743000526733,84.5737343194074,85.5731685861415,
86.5726028528755,87.5720371196096,88.5714713863437,89.5709056530778,90.5703399198119,
91.569774186546,92.5692084532801,93.5686427200142,94.5680769867483,95.5675112534823,
96.5669455202164,97.5663797869505,98.5658140536846,99.5652483204187,100.564682587153,
101.564116853887,102.563551120621,103.562985387355,104.562419654089,105.561853920823,
106.561288187557,107.560722454291,108.560156721025,109.55959098776,110.559025254494,
111.558459521228,112.557893787962,113.557328054696,114.55676232143,115.556196588164,
116.555630854898,117.555065121632,118.554499388366,119.5539336551,120.553367921835,
121.552802188569,122.552236455303,123.551670722037,124.551104988771,125.550539255505,
126.549973522239,127.549407788973,128.548842055707,129.548276322441,130.547710589175,
131.54714485591,132.546579122644,133.546013389378,134.545447656112,135.544881922846,
136.54431618958,137.543750456314,138.543184723048,139.542618989782,140.542053256516,
141.54148752325,142.540921789984,143.540356056719,144.539790323453,145.539224590187,
146.538658856921,147.538093123655,148.537527390389,149.536961657123,150.536395923857,
151.535830190591,152.535264457325,153.534698724059,154.534132990794,155.533567257528,
156.533001524262,157.532435790996,158.53187005773,159.531304324464,160.530738591198,
161.530172857932,162.529607124666,163.5290413914,164.528475658134,165.527909924869,
166.527344191603,167.526778458337,168.526212725071,169.525646991805,170.525081258539,
171.524515525273,172.523949792007,173.523384058741,174.522818325475,175.522252592209,
176.521686858943,177.521121125678,178.520555392412,179.519989659146,180.51942392588,
181.518858192614,182.518292459348,183.517726726082,184.517160992816,185.51659525955,
186.516029526284,187.515463793018,188.514898059753,189.514332326487,190.513766593221,
191.513200859955,192.512635126689,193.512069393423,194.511503660157,195.510937926891,
196.510372193625,197.509806460359,198.509240727093,199.508674993828,200.508109260562,
201.507543527296,202.50697779403,203.506412060764,204.505846327498,205.505280594232,
206.504714860966,207.5041491277,208.503583394434,209.503017661168,210.502451927902,
211.501886194637,212.501320461371,213.500754728105,214.500188994839,215.499623261573,
216.499057528307,217.498491795041,218.497926061775,219.497360328509,220.496794595243,
221.496228861977,222.495663128712,223.495097395446,224.49453166218,225.493965928914,
226.493400195648,227.492834462382,228.492268729116,229.49170299585,230.491137262584,
231.490571529318,232.490005796052,233.489440062787,234.488874329521,235.488308596255,
236.487742862989,237.487177129723,238.486611396457,239.486045663191,240.485479929925,
241.484914196659,242.484348463393,243.483782730127,244.483216996862,245.482651263596,
246.48208553033,247.481519797064,248.480954063798,249.480388330532,250.479822597266,
251.479256864,252.478691130734,253.478125397468,254.477559664202,255.476993930936,
256.476428197671,257.475862464405,258.475296731139,259.474730997873,260.474165264607,
261.473599531341,262.473033798075,263.472468064809,264.471902331543,265.471336598277,
266.470770865011,267.470205131746,268.46963939848,269.469073665214,270.468507931948,
271.467942198682,272.467376465416,273.46681073215,274.466244998884,275.465679265618,
276.465113532352,277.464547799086,278.46398206582,279.463416332555,280.462850599289,
281.462284866023,282.461719132757,283.461153399491,284.460587666225,285.460021932959,
286.459456199693,287.458890466427,288.458324733161,289.457758999895,290.45719326663,
291.456627533364,292.456061800098,293.455496066832,294.454930333566,295.4543646003,
296.453798867034,297.453233133768,298.452667400502,299.452101667236,300.45153593397,
301.450970200704,302.450404467439,303.449838734173,304.449273000907,305.448707267641,
306.448141534375,307.447575801109,308.447010067843,309.446444334577,310.445878601311,
311.445312868045,312.444747134779,313.444181401514,314.443615668248,315.443049934982,
316.442484201716,317.44191846845,318.441352735184,319.440787001918,320.440221268652,
321.439655535386,322.43908980212,323.438524068854),.UNSPECIFIED.);
#375=B_SPLINE_SURFACE_WITH_KNOTS('',3,3,((#95936,#95937,#95938,#95939,#95940,
#95941,#95942,#95943,#95944,#95945,#95946,#95947,#95948,#95949,#95950,#95951,
#95952,#95953,#95954,#95955,#95956,#95957,#95958,#95959,#95960,#95961,#95962,
#95963,#95964,#95965,#95966,#95967,#95968,#95969,#95970,#95971,#95972,#95973,
#95974,#95975,#95976,#95977,#95978,#95979,#95980,#95981,#95982,#95983,#95984,
#95985,#95986,#95987,#95988,#95989,#95990,#95991,#95992,#95993,#95994,#95995,
#95996,#95997,#95998,#95999,#96000,#96001,#96002,#96003,#96004,#96005,#96006,
#96007,#96008,#96009,#96010,#96011,#96012,#96013,#96014,#96015,#96016,#96017,
#96018,#96019,#96020,#96021,#96022,#96023,#96024,#96025,#96026,#96027,#96028,
#96029,#96030,#96031,#96032,#96033,#96034,#96035,#96036,#96037,#96038,#96039,
#96040,#96041,#96042,#96043,#96044,#96045,#96046,#96047,#96048,#96049,#96050,
#96051,#96052,#96053,#96054,#96055,#96056,#96057,#96058,#96059,#96060,#96061,
#96062,#96063,#96064,#96065,#96066,#96067,#96068,#96069,#96070,#96071,#96072,
#96073,#96074,#96075,#96076,#96077,#96078,#96079,#96080,#96081,#96082,#96083,
#96084,#96085,#96086,#96087,#96088,#96089,#96090,#96091,#96092,#96093,#96094,
#96095,#96096,#96097,#96098,#96099,#96100,#96101,#96102,#96103,#96104,#96105,
#96106,#96107,#96108,#96109,#96110,#96111,#96112,#96113,#96114,#96115,#96116,
#96117,#96118,#96119,#96120,#96121,#96122,#96123,#96124,#96125,#96126,#96127,
#96128,#96129,#96130,#96131,#96132,#96133,#96134,#96135,#96136,#96137,#96138,
#96139,#96140,#96141,#96142,#96143,#96144,#96145,#96146,#96147,#96148,#96149,
#96150,#96151,#96152,#96153,#96154,#96155,#96156,#96157,#96158,#96159,#96160,
#96161,#96162,#96163,#96164,#96165,#96166,#96167,#96168,#96169,#96170,#96171,
#96172,#96173,#96174,#96175,#96176,#96177,#96178,#96179,#96180,#96181,#96182,
#96183,#96184,#96185,#96186,#96187,#96188,#96189,#96190,#96191,#96192,#96193,
#96194,#96195,#96196,#96197,#96198,#96199,#96200,#96201,#96202,#96203,#96204,
#96205,#96206,#96207,#96208,#96209,#96210,#96211,#96212,#96213,#96214,#96215,
#96216,#96217,#96218,#96219,#96220,#96221,#96222,#96223,#96224,#96225,#96226,
#96227,#96228,#96229,#96230,#96231,#96232,#96233,#96234,#96235,#96236,#96237,
#96238,#96239,#96240,#96241,#96242,#96243,#96244,#96245,#96246,#96247,#96248,
#96249,#96250,#96251,#96252),(#96253,#96254,#96255,#96256,#96257,#96258,
#96259,#96260,#96261,#96262,#96263,#96264,#96265,#96266,#96267,#96268,#96269,
#96270,#96271,#96272,#96273,#96274,#96275,#96276,#96277,#96278,#96279,#96280,
#96281,#96282,#96283,#96284,#96285,#96286,#96287,#96288,#96289,#96290,#96291,
#96292,#96293,#96294,#96295,#96296,#96297,#96298,#96299,#96300,#96301,#96302,
#96303,#96304,#96305,#96306,#96307,#96308,#96309,#96310,#96311,#96312,#96313,
#96314,#96315,#96316,#96317,#96318,#96319,#96320,#96321,#96322,#96323,#96324,
#96325,#96326,#96327,#96328,#96329,#96330,#96331,#96332,#96333,#96334,#96335,
#96336,#96337,#96338,#96339,#96340,#96341,#96342,#96343,#96344,#96345,#96346,
#96347,#96348,#96349,#96350,#96351,#96352,#96353,#96354,#96355,#96356,#96357,
#96358,#96359,#96360,#96361,#96362,#96363,#96364,#96365,#96366,#96367,#96368,
#96369,#96370,#96371,#96372,#96373,#96374,#96375,#96376,#96377,#96378,#96379,
#96380,#96381,#96382,#96383,#96384,#96385,#96386,#96387,#96388,#96389,#96390,
#96391,#96392,#96393,#96394,#96395,#96396,#96397,#96398,#96399,#96400,#96401,
#96402,#96403,#96404,#96405,#96406,#96407,#96408,#96409,#96410,#96411,#96412,
#96413,#96414,#96415,#96416,#96417,#96418,#96419,#96420,#96421,#96422,#96423,
#96424,#96425,#96426,#96427,#96428,#96429,#96430,#96431,#96432,#96433,#96434,
#96435,#96436,#96437,#96438,#96439,#96440,#96441,#96442,#96443,#96444,#96445,
#96446,#96447,#96448,#96449,#96450,#96451,#96452,#96453,#96454,#96455,#96456,
#96457,#96458,#96459,#96460,#96461,#96462,#96463,#96464,#96465,#96466,#96467,
#96468,#96469,#96470,#96471,#96472,#96473,#96474,#96475,#96476,#96477,#96478,
#96479,#96480,#96481,#96482,#96483,#96484,#96485,#96486,#96487,#96488,#96489,
#96490,#96491,#96492,#96493,#96494,#96495,#96496,#96497,#96498,#96499,#96500,
#96501,#96502,#96503,#96504,#96505,#96506,#96507,#96508,#96509,#96510,#96511,
#96512,#96513,#96514,#96515,#96516,#96517,#96518,#96519,#96520,#96521,#96522,
#96523,#96524,#96525,#96526,#96527,#96528,#96529,#96530,#96531,#96532,#96533,
#96534,#96535,#96536,#96537,#96538,#96539,#96540,#96541,#96542,#96543,#96544,
#96545,#96546,#96547,#96548,#96549,#96550,#96551,#96552,#96553,#96554,#96555,
#96556,#96557,#96558,#96559,#96560,#96561,#96562,#96563,#96564,#96565,#96566,
#96567,#96568,#96569),(#96570,#96571,#96572,#96573,#96574,#96575,#96576,
#96577,#96578,#96579,#96580,#96581,#96582,#96583,#96584,#96585,#96586,#96587,
#96588,#96589,#96590,#96591,#96592,#96593,#96594,#96595,#96596,#96597,#96598,
#96599,#96600,#96601,#96602,#96603,#96604,#96605,#96606,#96607,#96608,#96609,
#96610,#96611,#96612,#96613,#96614,#96615,#96616,#96617,#96618,#96619,#96620,
#96621,#96622,#96623,#96624,#96625,#96626,#96627,#96628,#96629,#96630,#96631,
#96632,#96633,#96634,#96635,#96636,#96637,#96638,#96639,#96640,#96641,#96642,
#96643,#96644,#96645,#96646,#96647,#96648,#96649,#96650,#96651,#96652,#96653,
#96654,#96655,#96656,#96657,#96658,#96659,#96660,#96661,#96662,#96663,#96664,
#96665,#96666,#96667,#96668,#96669,#96670,#96671,#96672,#96673,#96674,#96675,
#96676,#96677,#96678,#96679,#96680,#96681,#96682,#96683,#96684,#96685,#96686,
#96687,#96688,#96689,#96690,#96691,#96692,#96693,#96694,#96695,#96696,#96697,
#96698,#96699,#96700,#96701,#96702,#96703,#96704,#96705,#96706,#96707,#96708,
#96709,#96710,#96711,#96712,#96713,#96714,#96715,#96716,#96717,#96718,#96719,
#96720,#96721,#96722,#96723,#96724,#96725,#96726,#96727,#96728,#96729,#96730,
#96731,#96732,#96733,#96734,#96735,#96736,#96737,#96738,#96739,#96740,#96741,
#96742,#96743,#96744,#96745,#96746,#96747,#96748,#96749,#96750,#96751,#96752,
#96753,#96754,#96755,#96756,#96757,#96758,#96759,#96760,#96761,#96762,#96763,
#96764,#96765,#96766,#96767,#96768,#96769,#96770,#96771,#96772,#96773,#96774,
#96775,#96776,#96777,#96778,#96779,#96780,#96781,#96782,#96783,#96784,#96785,
#96786,#96787,#96788,#96789,#96790,#96791,#96792,#96793,#96794,#96795,#96796,
#96797,#96798,#96799,#96800,#96801,#96802,#96803,#96804,#96805,#96806,#96807,
#96808,#96809,#96810,#96811,#96812,#96813,#96814,#96815,#96816,#96817,#96818,
#96819,#96820,#96821,#96822,#96823,#96824,#96825,#96826,#96827,#96828,#96829,
#96830,#96831,#96832,#96833,#96834,#96835,#96836,#96837,#96838,#96839,#96840,
#96841,#96842,#96843,#96844,#96845,#96846,#96847,#96848,#96849,#96850,#96851,
#96852,#96853,#96854,#96855,#96856,#96857,#96858,#96859,#96860,#96861,#96862,
#96863,#96864,#96865,#96866,#96867,#96868,#96869,#96870,#96871,#96872,#96873,
#96874,#96875,#96876,#96877,#96878,#96879,#96880,#96881,#96882,#96883,#96884,
#96885,#96886),(#96887,#96888,#96889,#96890,#96891,#96892,#96893,#96894,
#96895,#96896,#96897,#96898,#96899,#96900,#96901,#96902,#96903,#96904,#96905,
#96906,#96907,#96908,#96909,#96910,#96911,#96912,#96913,#96914,#96915,#96916,
#96917,#96918,#96919,#96920,#96921,#96922,#96923,#96924,#96925,#96926,#96927,
#96928,#96929,#96930,#96931,#96932,#96933,#96934,#96935,#96936,#96937,#96938,
#96939,#96940,#96941,#96942,#96943,#96944,#96945,#96946,#96947,#96948,#96949,
#96950,#96951,#96952,#96953,#96954,#96955,#96956,#96957,#96958,#96959,#96960,
#96961,#96962,#96963,#96964,#96965,#96966,#96967,#96968,#96969,#96970,#96971,
#96972,#96973,#96974,#96975,#96976,#96977,#96978,#96979,#96980,#96981,#96982,
#96983,#96984,#96985,#96986,#96987,#96988,#96989,#96990,#96991,#96992,#96993,
#96994,#96995,#96996,#96997,#96998,#96999,#97000,#97001,#97002,#97003,#97004,
#97005,#97006,#97007,#97008,#97009,#97010,#97011,#97012,#97013,#97014,#97015,
#97016,#97017,#97018,#97019,#97020,#97021,#97022,#97023,#97024,#97025,#97026,
#97027,#97028,#97029,#97030,#97031,#97032,#97033,#97034,#97035,#97036,#97037,
#97038,#97039,#97040,#97041,#97042,#97043,#97044,#97045,#97046,#97047,#97048,
#97049,#97050,#97051,#97052,#97053,#97054,#97055,#97056,#97057,#97058,#97059,
#97060,#97061,#97062,#97063,#97064,#97065,#97066,#97067,#97068,#97069,#97070,
#97071,#97072,#97073,#97074,#97075,#97076,#97077,#97078,#97079,#97080,#97081,
#97082,#97083,#97084,#97085,#97086,#97087,#97088,#97089,#97090,#97091,#97092,
#97093,#97094,#97095,#97096,#97097,#97098,#97099,#97100,#97101,#97102,#97103,
#97104,#97105,#97106,#97107,#97108,#97109,#97110,#97111,#97112,#97113,#97114,
#97115,#97116,#97117,#97118,#97119,#97120,#97121,#97122,#97123,#97124,#97125,
#97126,#97127,#97128,#97129,#97130,#97131,#97132,#97133,#97134,#97135,#97136,
#97137,#97138,#97139,#97140,#97141,#97142,#97143,#97144,#97145,#97146,#97147,
#97148,#97149,#97150,#97151,#97152,#97153,#97154,#97155,#97156,#97157,#97158,
#97159,#97160,#97161,#97162,#97163,#97164,#97165,#97166,#97167,#97168,#97169,
#97170,#97171,#97172,#97173,#97174,#97175,#97176,#97177,#97178,#97179,#97180,
#97181,#97182,#97183,#97184,#97185,#97186,#97187,#97188,#97189,#97190,#97191,
#97192,#97193,#97194,#97195,#97196,#97197,#97198,#97199,#97200,#97201,#97202,
#97203)),.UNSPECIFIED.,.F.,.F.,.F.,(4,4),(4,1,1,1,1,1,1,1,1,1,1,1,1,1,1,
1,1,1,1,1,1,1,1,1,1,1,1,1,1,1,1,1,1,1,1,1,1,1,1,1,1,1,1,1,1,1,1,1,1,1,1,
1,1,1,1,1,1,1,1,1,1,1,1,1,1,1,1,1,1,1,1,1,1,1,1,1,1,1,1,1,1,1,1,1,1,1,1,
1,1,1,1,1,1,1,1,1,1,1,1,1,1,1,1,1,1,1,1,1,1,1,1,1,1,1,1,1,1,1,1,1,1,1,1,
1,1,1,1,1,1,1,1,1,1,1,1,1,1,1,1,1,1,1,1,1,1,1,1,1,1,1,1,1,1,1,1,1,1,1,1,
1,1,1,1,1,1,1,1,1,1,1,1,1,1,1,1,1,1,1,1,1,1,1,1,1,1,1,1,1,1,1,1,1,1,1,1,
1,1,1,1,1,1,1,1,1,1,1,1,1,1,1,1,1,1,1,1,1,1,1,1,1,1,1,1,1,1,1,1,1,1,1,1,
1,1,1,1,1,1,1,1,1,1,1,1,1,1,1,1,1,1,1,1,1,1,1,1,1,1,1,1,1,1,1,1,1,1,1,1,
1,1,1,1,1,1,1,1,1,1,1,1,1,1,1,1,1,1,1,1,1,1,1,1,1,1,1,1,1,1,1,1,1,1,1,1,
1,1,1,1,1,1,1,1,1,1,1,4),(0.,0.0658467982010768),(8.30747755240155,9.30713401544597,
10.3067904784904,11.3064469415348,12.3061034045792,13.3057598676236,14.305416330668,
15.3050727937124,16.3047292567569,17.3043857198013,18.3040421828457,19.3036986458901,
20.3033551089345,21.3030115719789,22.3026680350233,23.3023244980677,24.3019809611122,
25.3016374241566,26.301293887201,27.3009503502454,28.3006068132898,29.3002632763342,
30.2999197393786,31.299576202423,32.2992326654675,33.2988891285119,34.2985455915563,
35.2982020546007,36.2978585176451,37.2975149806895,38.2971714437339,39.2968279067783,
40.2964843698228,41.2961408328672,42.2957972959116,43.295453758956,44.2951102220004,
45.2947666850448,46.2944231480892,47.2940796111337,48.2937360741781,49.2933925372225,
50.2930490002669,51.2927054633113,52.2923619263557,53.2920183894001,54.2916748524445,
55.2913313154889,56.2909877785334,57.2906442415778,58.2903007046222,59.2899571676666,
60.289613630711,61.2892700937554,62.2889265567998,63.2885830198443,64.2882394828887,
65.2878959459331,66.2875524089775,67.2872088720219,68.2868653350663,69.2865217981107,
70.2861782611551,71.2858347241996,72.285491187244,73.2851476502884,74.2848041133328,
75.2844605763772,76.2841170394216,77.283773502466,78.2834299655104,79.2830864285549,
80.2827428915993,81.2823993546437,82.2820558176881,83.2817122807325,84.2813687437769,
85.2810252068213,86.2806816698657,87.2803381329102,88.2799945959546,89.279651058999,
90.2793075220434,91.2789639850878,92.2786204481322,93.2782769111766,94.277933374221,
95.2775898372655,96.2772463003099,97.2769027633543,98.2765592263987,99.2762156894431,
100.275872152488,101.275528615532,102.275185078576,103.274841541621,104.274498004665,
105.27415446771,106.273810930754,107.273467393798,108.273123856843,109.272780319887,
110.272436782932,111.272093245976,112.27174970902,113.271406172065,114.271062635109,
115.270719098154,116.270375561198,117.270032024243,118.269688487287,119.269344950331,
120.269001413376,121.26865787642,122.268314339465,123.267970802509,124.267627265553,
125.267283728598,126.266940191642,127.266596654687,128.266253117731,129.265909580775,
130.26556604382,131.265222506864,132.264878969909,133.264535432953,134.264191895998,
135.263848359042,136.263504822086,137.263161285131,138.262817748175,139.26247421122,
140.262130674264,141.261787137308,142.261443600353,143.261100063397,144.260756526442,
145.260412989486,146.260069452531,147.259725915575,148.259382378619,149.259038841664,
150.258695304708,151.258351767753,152.258008230797,153.257664693841,154.257321156886,
155.25697761993,156.256634082975,157.256290546019,158.255947009063,159.255603472108,
160.255259935152,161.254916398197,162.254572861241,163.254229324286,164.25388578733,
165.253542250374,166.253198713419,167.252855176463,168.252511639508,169.252168102552,
170.251824565596,171.251481028641,172.251137491685,173.25079395473,174.250450417774,
175.250106880818,176.249763343863,177.249419806907,178.249076269952,179.248732732996,
180.248389196041,181.248045659085,182.247702122129,183.247358585174,184.247015048218,
185.246671511263,186.246327974307,187.245984437351,188.245640900396,189.24529736344,
190.244953826485,191.244610289529,192.244266752574,193.243923215618,194.243579678662,
195.243236141707,196.242892604751,197.242549067796,198.24220553084,199.241861993884,
200.241518456929,201.241174919973,202.240831383018,203.240487846062,204.240144309106,
205.239800772151,206.239457235195,207.23911369824,208.238770161284,209.238426624329,
210.238083087373,211.237739550417,212.237396013462,213.237052476506,214.236708939551,
215.236365402595,216.236021865639,217.235678328684,218.235334791728,219.234991254773,
220.234647717817,221.234304180861,222.233960643906,223.23361710695,224.233273569995,
225.232930033039,226.232586496084,227.232242959128,228.231899422172,229.231555885217,
230.231212348261,231.230868811306,232.23052527435,233.230181737394,234.229838200439,
235.229494663483,236.229151126528,237.228807589572,238.228464052616,239.228120515661,
240.227776978705,241.22743344175,242.227089904794,243.226746367839,244.226402830883,
245.226059293927,246.225715756972,247.225372220016,248.225028683061,249.224685146105,
250.224341609149,251.223998072194,252.223654535238,253.223310998283,254.222967461327,
255.222623924372,256.222280387416,257.22193685046,258.221593313505,259.221249776549,
260.220906239594,261.220562702638,262.220219165682,263.219875628727,264.219532091771,
265.219188554816,266.21884501786,267.218501480904,268.218157943949,269.217814406993,
270.217470870038,271.217127333082,272.216783796126,273.216440259171,274.216096722215,
275.21575318526,276.215409648304,277.215066111349,278.214722574393,279.214379037437,
280.214035500482,281.213691963526,282.213348426571,283.213004889615,284.212661352659,
285.212317815704,286.211974278748,287.211630741793,288.211287204837,289.210943667882,
290.210600130926,291.21025659397,292.209913057015,293.209569520059,294.209225983104,
295.208882446148,296.208538909192,297.208195372237,298.207851835281,299.207508298326,
300.20716476137,301.206821224415,302.206477687459,303.206134150503,304.205790613548,
305.205447076592,306.205103539637,307.204760002681,308.204416465725,309.20407292877,
310.203729391814,311.203385854859,312.203042317903,313.202698780947,314.202355243992,
315.202011707036,316.201668170081,317.201324633125,318.200981096169,319.200637559214,
320.200294022258,321.199950485303,322.199606948347),.UNSPECIFIED.);
#376=B_SPLINE_CURVE_WITH_KNOTS('',3,(#27786,#27787,#27788,#27789),
 .UNSPECIFIED.,.F.,.F.,(4,4),(51.5750455984138,52.2824273504652),
 .UNSPECIFIED.);
#377=B_SPLINE_CURVE_WITH_KNOTS('',3,(#27792,#27793,#27794,#27795,#27796,
#27797,#27798,#27799,#27800,#27801),.UNSPECIFIED.,.F.,.F.,(4,3,3,4),(-50.2654824574367,
-49.3230446702501,-48.3365837768451,-47.8312715558983),.UNSPECIFIED.);
#378=B_SPLINE_CURVE_WITH_KNOTS('',3,(#27806,#27807,#27808,#27809,#27810,
#27811,#27812,#27813,#27814,#27815,#27816,#27817,#27818,#27819,#27820,#27821,
#27822,#27823,#27824,#27825,#27826,#27827,#27828,#27829,#27830),
 .UNSPECIFIED.,.F.,.F.,(4,3,3,3,3,3,3,3,4),(45.2918602912342,45.3772010966301,
46.3636619900351,47.3501228834401,48.3365837768452,49.3230446702501,50.3095055636552,
51.2959664570602,51.5750455984138),.UNSPECIFIED.);
#379=B_SPLINE_CURVE_WITH_KNOTS('',3,(#27831,#27832,#27833,#27834,#27835,
#27836,#27837,#27838,#27839,#27840,#27841,#27842,#27843,#27844,#27845,#27846,
#27847,#27848,#27849,#27850,#27851,#27852),.UNSPECIFIED.,.F.,.F.,(4,3,3,
3,3,3,3,4),(-47.8312715558983,-47.3501228834401,-46.3636619900351,-45.3772010966301,
-44.3907402032251,-43.4042793098201,-42.4178184164151,-41.5480862487187),
 .UNSPECIFIED.);
#380=B_SPLINE_CURVE_WITH_KNOTS('',3,(#27857,#27858,#27859,#27860,#27861,
#27862,#27863,#27864,#27865,#27866,#27867,#27868,#27869,#27870,#27871,#27872,
#27873,#27874,#27875,#27876,#27877,#27878),.UNSPECIFIED.,.F.,.F.,(4,3,3,
3,3,3,3,4),(39.0086749840546,39.4584357362001,40.4448966296051,41.4313575230101,
42.4178184164151,43.4042793098201,44.3907402032251,45.2918602912342),
 .UNSPECIFIED.);
#381=B_SPLINE_CURVE_WITH_KNOTS('',3,(#27879,#27880,#27881,#27882,#27883,
#27884,#27885,#27886,#27887,#27888,#27889,#27890,#27891,#27892,#27893,#27894,
#27895,#27896,#27897,#27898,#27899,#27900,#27901,#27902,#27903),
 .UNSPECIFIED.,.F.,.F.,(4,3,3,3,3,3,3,3,4),(-41.5480862487187,-41.4313575230101,
-40.4448966296051,-39.4584357362001,-38.4719748427951,-37.4855139493901,
-36.4990530559851,-35.5125921625801,-35.2649009415391),.UNSPECIFIED.);
#382=B_SPLINE_CURVE_WITH_KNOTS('',3,(#27908,#27909,#27910,#27911,#27912,
#27913,#27914,#27915,#27916,#27917,#27918,#27919,#27920,#27921,#27922,#27923,
#27924,#27925,#27926,#27927,#27928,#27929),.UNSPECIFIED.,.F.,.F.,(4,3,3,
3,3,3,3,4),(32.725489676875,33.5396703757701,34.5261312691751,35.5125921625801,
36.4990530559851,37.4855139493901,38.4719748427951,39.0086749840546),
 .UNSPECIFIED.);
#383=B_SPLINE_CURVE_WITH_KNOTS('',3,(#27930,#27931,#27932,#27933,#27934,
#27935,#27936,#27937,#27938,#27939,#27940,#27941,#27942,#27943,#27944,#27945,
#27946,#27947,#27948,#27949,#27950,#27951),.UNSPECIFIED.,.F.,.F.,(4,3,3,
3,3,3,3,4),(-35.2649009415391,-34.5261312691751,-33.5396703757701,-32.5532094823651,
-31.5667485889601,-30.5802876955551,-29.5938268021501,-28.9817156343595),
 .UNSPECIFIED.);
#384=B_SPLINE_CURVE_WITH_KNOTS('',3,(#27956,#27957,#27958,#27959,#27960,
#27961,#27962,#27963,#27964,#27965,#27966,#27967,#27968,#27969,#27970,#27971,
#27972,#27973,#27974,#27975,#27976,#27977,#27978,#27979,#27980),
 .UNSPECIFIED.,.F.,.F.,(4,3,3,3,3,3,3,3,4),(26.4423043696954,26.6344441219351,
27.6209050153401,28.6073659087451,29.5938268021501,30.5802876955551,31.5667485889601,
32.5532094823651,32.725489676875),.UNSPECIFIED.);
#385=B_SPLINE_CURVE_WITH_KNOTS('',3,(#27981,#27982,#27983,#27984,#27985,
#27986,#27987,#27988,#27989,#27990,#27991,#27992,#27993,#27994,#27995,#27996,
#27997,#27998,#27999,#28000,#28001,#28002),.UNSPECIFIED.,.F.,.F.,(4,3,3,
3,3,3,3,4),(-28.9817156343595,-28.6073659087451,-27.6209050153401,-26.6344441219351,
-25.6479832285301,-24.6615223351251,-23.6750614417201,-22.6985303271799),
 .UNSPECIFIED.);
#386=B_SPLINE_CURVE_WITH_KNOTS('',3,(#28007,#28008,#28009,#28010,#28011,
#28012,#28013,#28014,#28015,#28016,#28017,#28018,#28019,#28020,#28021,#28022,
#28023,#28024,#28025,#28026,#28027,#28028),.UNSPECIFIED.,.F.,.F.,(4,3,3,
3,3,3,3,4),(20.1591190625159,20.7156787615051,21.7021396549101,22.6886005483151,
23.6750614417201,24.6615223351251,25.6479832285301,26.4423043696954),
 .UNSPECIFIED.);
#387=B_SPLINE_CURVE_WITH_KNOTS('',3,(#28029,#28030,#28031,#28032,#28033,
#28034,#28035,#28036,#28037,#28038,#28039,#28040,#28041,#28042,#28043,#28044,
#28045,#28046,#28047,#28048,#28049,#28050,#28051,#28052,#28053),
 .UNSPECIFIED.,.F.,.F.,(4,3,3,3,3,3,3,3,4),(-22.6985303271799,-22.6886005483151,
-21.7021396549101,-20.7156787615051,-19.7292178681001,-18.7427569746951,
-17.7562960812901,-16.7698351878851,-16.4153450200003),.UNSPECIFIED.);
#388=B_SPLINE_CURVE_WITH_KNOTS('',3,(#28058,#28059,#28060,#28061,#28062,
#28063,#28064,#28065,#28066,#28067,#28068,#28069,#28070,#28071,#28072,#28073,
#28074,#28075,#28076,#28077,#28078,#28079),.UNSPECIFIED.,.F.,.F.,(4,3,3,
3,3,3,3,4),(13.8759337553363,14.7969134010751,15.78337429448,16.7698351878851,
17.75629608129,18.7427569746951,19.7292178681001,20.1591190625159),
 .UNSPECIFIED.);
#389=B_SPLINE_CURVE_WITH_KNOTS('',3,(#28080,#28081,#28082,#28083,#28084,
#28085,#28086,#28087,#28088,#28089,#28090,#28091,#28092,#28093,#28094,#28095,
#28096,#28097,#28098,#28099,#28100,#28101),.UNSPECIFIED.,.F.,.F.,(4,3,3,
3,3,3,3,4),(-16.4153450200003,-15.78337429448,-14.796913401075,-13.81045250767,
-12.823991614265,-11.83753072086,-10.851069827455,-10.1321597128207),
 .UNSPECIFIED.);
#390=B_SPLINE_CURVE_WITH_KNOTS('',3,(#28107,#28108,#28109,#28110,#28111,
#28112,#28113,#28114,#28115,#28116,#28117,#28118,#28119),.UNSPECIFIED.,
 .F.,.F.,(4,3,3,3,4),(-3.84897440564115,-2.95938268021501,-1.97292178681001,
-0.986460893405001,0.),.UNSPECIFIED.);
#391=B_SPLINE_CURVE_WITH_KNOTS('',3,(#28122,#28123,#28124,#28125,#28126,
#28127,#28128,#28129,#28130,#28131,#28132,#28133,#28134,#28135,#28136,#28137,
#28138,#28139,#28140),.UNSPECIFIED.,.F.,.F.,(4,3,3,3,3,3,4),(2.01694489302848,
2.95938268021501,3.94584357362001,4.93230446702502,5.91876536043002,6.90522625383502,
7.59274844815668),.UNSPECIFIED.);
#392=B_SPLINE_CURVE_WITH_KNOTS('',3,(#28146,#28147,#28148,#28149),
 .UNSPECIFIED.,.F.,.F.,(4,4),(51.5750455984138,52.2824273504652),
 .UNSPECIFIED.);
#393=B_SPLINE_CURVE_WITH_KNOTS('',3,(#28152,#28153,#28154,#28155,#28156,
#28157,#28158,#28159,#28160,#28161),.UNSPECIFIED.,.F.,.F.,(4,3,3,4),(-50.2654824574367,
-49.3230446702501,-48.3365837768451,-47.8312715558982),.UNSPECIFIED.);
#394=B_SPLINE_CURVE_WITH_KNOTS('',3,(#28166,#28167,#28168,#28169,#28170,
#28171,#28172,#28173,#28174,#28175,#28176,#28177,#28178,#28179,#28180,#28181,
#28182,#28183,#28184,#28185,#28186,#28187,#28188,#28189,#28190),
 .UNSPECIFIED.,.F.,.F.,(4,3,3,3,3,3,3,3,4),(45.2918602912342,45.3772010966301,
46.3636619900351,47.3501228834401,48.3365837768451,49.3230446702501,50.3095055636551,
51.2959664570602,51.5750455984138),.UNSPECIFIED.);
#395=B_SPLINE_CURVE_WITH_KNOTS('',3,(#28191,#28192,#28193,#28194,#28195,
#28196,#28197,#28198,#28199,#28200,#28201,#28202,#28203,#28204,#28205,#28206,
#28207,#28208,#28209,#28210,#28211,#28212),.UNSPECIFIED.,.F.,.F.,(4,3,3,
3,3,3,3,4),(-47.8312715558982,-47.3501228834401,-46.3636619900351,-45.3772010966301,
-44.3907402032251,-43.4042793098201,-42.4178184164151,-41.5480862487187),
 .UNSPECIFIED.);
#396=B_SPLINE_CURVE_WITH_KNOTS('',3,(#28217,#28218,#28219,#28220,#28221,
#28222,#28223,#28224,#28225,#28226,#28227,#28228,#28229,#28230,#28231,#28232,
#28233,#28234,#28235,#28236,#28237,#28238),.UNSPECIFIED.,.F.,.F.,(4,3,3,
3,3,3,3,4),(39.0086749840546,39.4584357362001,40.4448966296051,41.4313575230101,
42.4178184164151,43.4042793098201,44.3907402032251,45.2918602912342),
 .UNSPECIFIED.);
#397=B_SPLINE_CURVE_WITH_KNOTS('',3,(#28239,#28240,#28241,#28242,#28243,
#28244,#28245,#28246,#28247,#28248,#28249,#28250,#28251,#28252,#28253,#28254,
#28255,#28256,#28257,#28258,#28259,#28260,#28261,#28262,#28263),
 .UNSPECIFIED.,.F.,.F.,(4,3,3,3,3,3,3,3,4),(-41.5480862487187,-41.4313575230101,
-40.4448966296051,-39.4584357362001,-38.4719748427951,-37.4855139493901,
-36.4990530559851,-35.5125921625801,-35.2649009415391),.UNSPECIFIED.);
#398=B_SPLINE_CURVE_WITH_KNOTS('',3,(#28268,#28269,#28270,#28271,#28272,
#28273,#28274,#28275,#28276,#28277,#28278,#28279,#28280,#28281,#28282,#28283,
#28284,#28285,#28286,#28287,#28288,#28289),.UNSPECIFIED.,.F.,.F.,(4,3,3,
3,3,3,3,4),(32.725489676875,33.5396703757701,34.5261312691751,35.5125921625801,
36.4990530559851,37.4855139493901,38.4719748427951,39.0086749840546),
 .UNSPECIFIED.);
#399=B_SPLINE_CURVE_WITH_KNOTS('',3,(#28290,#28291,#28292,#28293,#28294,
#28295,#28296,#28297,#28298,#28299,#28300,#28301,#28302,#28303,#28304,#28305,
#28306,#28307,#28308,#28309,#28310,#28311),.UNSPECIFIED.,.F.,.F.,(4,3,3,
3,3,3,3,4),(-35.2649009415391,-34.5261312691751,-33.5396703757701,-32.5532094823651,
-31.5667485889601,-30.5802876955551,-29.5938268021501,-28.9817156343595),
 .UNSPECIFIED.);
#400=B_SPLINE_CURVE_WITH_KNOTS('',3,(#28316,#28317,#28318,#28319,#28320,
#28321,#28322,#28323,#28324,#28325,#28326,#28327,#28328,#28329,#28330,#28331,
#28332,#28333,#28334,#28335,#28336,#28337,#28338,#28339,#28340),
 .UNSPECIFIED.,.F.,.F.,(4,3,3,3,3,3,3,3,4),(26.4423043696954,26.6344441219351,
27.6209050153401,28.6073659087451,29.5938268021501,30.5802876955551,31.5667485889601,
32.5532094823651,32.725489676875),.UNSPECIFIED.);
#401=B_SPLINE_CURVE_WITH_KNOTS('',3,(#28341,#28342,#28343,#28344,#28345,
#28346,#28347,#28348,#28349,#28350,#28351,#28352,#28353,#28354,#28355,#28356,
#28357,#28358,#28359,#28360,#28361,#28362),.UNSPECIFIED.,.F.,.F.,(4,3,3,
3,3,3,3,4),(-28.9817156343595,-28.6073659087451,-27.6209050153401,-26.6344441219351,
-25.6479832285301,-24.6615223351251,-23.6750614417201,-22.6985303271799),
 .UNSPECIFIED.);
#402=B_SPLINE_CURVE_WITH_KNOTS('',3,(#28367,#28368,#28369,#28370,#28371,
#28372,#28373,#28374,#28375,#28376,#28377,#28378,#28379,#28380,#28381,#28382,
#28383,#28384,#28385,#28386,#28387,#28388),.UNSPECIFIED.,.F.,.F.,(4,3,3,
3,3,3,3,4),(20.1591190625158,20.7156787615051,21.7021396549101,22.6886005483151,
23.6750614417201,24.6615223351251,25.6479832285301,26.4423043696954),
 .UNSPECIFIED.);
#403=B_SPLINE_CURVE_WITH_KNOTS('',3,(#28389,#28390,#28391,#28392,#28393,
#28394,#28395,#28396,#28397,#28398,#28399,#28400,#28401,#28402,#28403,#28404,
#28405,#28406,#28407,#28408,#28409,#28410,#28411,#28412,#28413),
 .UNSPECIFIED.,.F.,.F.,(4,3,3,3,3,3,3,3,4),(-22.6985303271799,-22.6886005483151,
-21.7021396549101,-20.7156787615051,-19.7292178681001,-18.7427569746951,
-17.7562960812901,-16.7698351878851,-16.4153450200003),.UNSPECIFIED.);
#404=B_SPLINE_CURVE_WITH_KNOTS('',3,(#28418,#28419,#28420,#28421,#28422,
#28423,#28424,#28425,#28426,#28427,#28428,#28429,#28430,#28431,#28432,#28433,
#28434,#28435,#28436,#28437,#28438,#28439),.UNSPECIFIED.,.F.,.F.,(4,3,3,
3,3,3,3,4),(13.8759337553363,14.796913401075,15.78337429448,16.7698351878851,
17.7562960812901,18.7427569746951,19.7292178681001,20.1591190625158),
 .UNSPECIFIED.);
#405=B_SPLINE_CURVE_WITH_KNOTS('',3,(#28440,#28441,#28442,#28443,#28444,
#28445,#28446,#28447,#28448,#28449,#28450,#28451,#28452,#28453,#28454,#28455,
#28456,#28457,#28458,#28459,#28460,#28461),.UNSPECIFIED.,.F.,.F.,(4,3,3,
3,3,3,3,4),(-16.4153450200003,-15.7833742944801,-14.796913401075,-13.81045250767,
-12.823991614265,-11.83753072086,-10.851069827455,-10.1321597128207),
 .UNSPECIFIED.);
#406=B_SPLINE_CURVE_WITH_KNOTS('',3,(#28467,#28468,#28469,#28470,#28471,
#28472,#28473,#28474,#28475,#28476,#28477,#28478,#28479),.UNSPECIFIED.,
 .F.,.F.,(4,3,3,3,4),(-3.84897440564114,-2.95938268021501,-1.97292178681001,
-0.986460893405001,0.),.UNSPECIFIED.);
#407=B_SPLINE_CURVE_WITH_KNOTS('',3,(#28482,#28483,#28484,#28485,#28486,
#28487,#28488,#28489,#28490,#28491,#28492,#28493,#28494,#28495,#28496,#28497,
#28498,#28499,#28500),.UNSPECIFIED.,.F.,.F.,(4,3,3,3,3,3,4),(2.01694489302845,
2.95938268021501,3.94584357362001,4.93230446702501,5.91876536043001,6.90522625383501,
7.59274844815667),.UNSPECIFIED.);
#408=B_SPLINE_CURVE_WITH_KNOTS('',3,(#28506,#28507,#28508,#28509),
 .UNSPECIFIED.,.F.,.F.,(4,4),(51.5750455984138,52.2824273504652),
 .UNSPECIFIED.);
#409=B_SPLINE_CURVE_WITH_KNOTS('',3,(#28512,#28513,#28514,#28515,#28516,
#28517,#28518,#28519,#28520,#28521),.UNSPECIFIED.,.F.,.F.,(4,3,3,4),(-50.2654824574367,
-49.3230446702501,-48.3365837768451,-47.8312715558982),.UNSPECIFIED.);
#410=B_SPLINE_CURVE_WITH_KNOTS('',3,(#28526,#28527,#28528,#28529,#28530,
#28531,#28532,#28533,#28534,#28535,#28536,#28537,#28538,#28539,#28540,#28541,
#28542,#28543,#28544,#28545,#28546,#28547,#28548,#28549,#28550),
 .UNSPECIFIED.,.F.,.F.,(4,3,3,3,3,3,3,3,4),(45.2918602912342,45.3772010966301,
46.3636619900351,47.3501228834401,48.3365837768451,49.3230446702501,50.3095055636552,
51.2959664570602,51.5750455984138),.UNSPECIFIED.);
#411=B_SPLINE_CURVE_WITH_KNOTS('',3,(#28551,#28552,#28553,#28554,#28555,
#28556,#28557,#28558,#28559,#28560,#28561,#28562,#28563,#28564,#28565,#28566,
#28567,#28568,#28569,#28570,#28571,#28572),.UNSPECIFIED.,.F.,.F.,(4,3,3,
3,3,3,3,4),(-47.8312715558982,-47.3501228834401,-46.3636619900351,-45.3772010966301,
-44.3907402032251,-43.4042793098201,-42.4178184164151,-41.5480862487187),
 .UNSPECIFIED.);
#412=B_SPLINE_CURVE_WITH_KNOTS('',3,(#28577,#28578,#28579,#28580,#28581,
#28582,#28583,#28584,#28585,#28586,#28587,#28588,#28589,#28590,#28591,#28592,
#28593,#28594,#28595,#28596,#28597,#28598),.UNSPECIFIED.,.F.,.F.,(4,3,3,
3,3,3,3,4),(39.0086749840546,39.4584357362001,40.4448966296051,41.4313575230101,
42.4178184164151,43.4042793098201,44.3907402032251,45.2918602912342),
 .UNSPECIFIED.);
#413=B_SPLINE_CURVE_WITH_KNOTS('',3,(#28599,#28600,#28601,#28602,#28603,
#28604,#28605,#28606,#28607,#28608,#28609,#28610,#28611,#28612,#28613,#28614,
#28615,#28616,#28617,#28618,#28619,#28620,#28621,#28622,#28623),
 .UNSPECIFIED.,.F.,.F.,(4,3,3,3,3,3,3,3,4),(-41.5480862487187,-41.4313575230101,
-40.4448966296051,-39.4584357362001,-38.4719748427951,-37.4855139493901,
-36.4990530559851,-35.5125921625801,-35.2649009415391),.UNSPECIFIED.);
#414=B_SPLINE_CURVE_WITH_KNOTS('',3,(#28628,#28629,#28630,#28631,#28632,
#28633,#28634,#28635,#28636,#28637,#28638,#28639,#28640,#28641,#28642,#28643,
#28644,#28645,#28646,#28647,#28648,#28649),.UNSPECIFIED.,.F.,.F.,(4,3,3,
3,3,3,3,4),(32.725489676875,33.5396703757701,34.5261312691751,35.5125921625801,
36.4990530559851,37.4855139493901,38.4719748427951,39.0086749840546),
 .UNSPECIFIED.);
#415=B_SPLINE_CURVE_WITH_KNOTS('',3,(#28650,#28651,#28652,#28653,#28654,
#28655,#28656,#28657,#28658,#28659,#28660,#28661,#28662,#28663,#28664,#28665,
#28666,#28667,#28668,#28669,#28670,#28671),.UNSPECIFIED.,.F.,.F.,(4,3,3,
3,3,3,3,4),(-35.2649009415391,-34.5261312691751,-33.5396703757701,-32.5532094823651,
-31.5667485889601,-30.5802876955551,-29.5938268021501,-28.9817156343595),
 .UNSPECIFIED.);
#416=B_SPLINE_CURVE_WITH_KNOTS('',3,(#28676,#28677,#28678,#28679,#28680,
#28681,#28682,#28683,#28684,#28685,#28686,#28687,#28688,#28689,#28690,#28691,
#28692,#28693,#28694,#28695,#28696,#28697,#28698,#28699,#28700),
 .UNSPECIFIED.,.F.,.F.,(4,3,3,3,3,3,3,3,4),(26.4423043696954,26.6344441219351,
27.6209050153401,28.6073659087451,29.5938268021501,30.5802876955551,31.5667485889601,
32.5532094823651,32.725489676875),.UNSPECIFIED.);
#417=B_SPLINE_CURVE_WITH_KNOTS('',3,(#28701,#28702,#28703,#28704,#28705,
#28706,#28707,#28708,#28709,#28710,#28711,#28712,#28713,#28714,#28715,#28716,
#28717,#28718,#28719,#28720,#28721,#28722),.UNSPECIFIED.,.F.,.F.,(4,3,3,
3,3,3,3,4),(-28.9817156343595,-28.6073659087451,-27.6209050153401,-26.6344441219351,
-25.6479832285301,-24.6615223351251,-23.6750614417201,-22.6985303271799),
 .UNSPECIFIED.);
#418=B_SPLINE_CURVE_WITH_KNOTS('',3,(#28727,#28728,#28729,#28730,#28731,
#28732,#28733,#28734,#28735,#28736,#28737,#28738,#28739,#28740,#28741,#28742,
#28743,#28744,#28745,#28746,#28747,#28748),.UNSPECIFIED.,.F.,.F.,(4,3,3,
3,3,3,3,4),(20.1591190625158,20.7156787615051,21.7021396549101,22.6886005483151,
23.6750614417201,24.6615223351251,25.6479832285301,26.4423043696954),
 .UNSPECIFIED.);
#419=B_SPLINE_CURVE_WITH_KNOTS('',3,(#28749,#28750,#28751,#28752,#28753,
#28754,#28755,#28756,#28757,#28758,#28759,#28760,#28761,#28762,#28763,#28764,
#28765,#28766,#28767,#28768,#28769,#28770,#28771,#28772,#28773),
 .UNSPECIFIED.,.F.,.F.,(4,3,3,3,3,3,3,3,4),(-22.6985303271799,-22.6886005483151,
-21.7021396549101,-20.715678761505,-19.7292178681001,-18.742756974695,-17.75629608129,
-16.769835187885,-16.4153450200003),.UNSPECIFIED.);
#420=B_SPLINE_CURVE_WITH_KNOTS('',3,(#28778,#28779,#28780,#28781,#28782,
#28783,#28784,#28785,#28786,#28787,#28788,#28789,#28790,#28791,#28792,#28793,
#28794,#28795,#28796,#28797,#28798,#28799),.UNSPECIFIED.,.F.,.F.,(4,3,3,
3,3,3,3,4),(13.8759337553363,14.796913401075,15.78337429448,16.7698351878851,
17.7562960812901,18.7427569746951,19.7292178681001,20.1591190625158),
 .UNSPECIFIED.);
#421=B_SPLINE_CURVE_WITH_KNOTS('',3,(#28800,#28801,#28802,#28803,#28804,
#28805,#28806,#28807,#28808,#28809,#28810,#28811,#28812,#28813,#28814,#28815,
#28816,#28817,#28818,#28819,#28820,#28821),.UNSPECIFIED.,.F.,.F.,(4,3,3,
3,3,3,3,4),(-16.4153450200003,-15.78337429448,-14.796913401075,-13.81045250767,
-12.823991614265,-11.83753072086,-10.851069827455,-10.1321597128207),
 .UNSPECIFIED.);
#422=B_SPLINE_CURVE_WITH_KNOTS('',3,(#28827,#28828,#28829,#28830,#28831,
#28832,#28833,#28834,#28835,#28836,#28837,#28838,#28839),.UNSPECIFIED.,
 .F.,.F.,(4,3,3,3,4),(-3.84897440564114,-2.95938268021501,-1.97292178681001,
-0.986460893405004,0.),.UNSPECIFIED.);
#423=B_SPLINE_CURVE_WITH_KNOTS('',3,(#28842,#28843,#28844,#28845,#28846,
#28847,#28848,#28849,#28850,#28851,#28852,#28853,#28854,#28855,#28856,#28857,
#28858,#28859,#28860),.UNSPECIFIED.,.F.,.F.,(4,3,3,3,3,3,4),(2.01694489302844,
2.95938268021501,3.94584357362001,4.93230446702501,5.91876536043001,6.90522625383502,
7.59274844815667),.UNSPECIFIED.);
#424=B_SPLINE_CURVE_WITH_KNOTS('',3,(#28866,#28867,#28868,#28869),
 .UNSPECIFIED.,.F.,.F.,(4,4),(51.5750455984138,52.2824273504652),
 .UNSPECIFIED.);
#425=B_SPLINE_CURVE_WITH_KNOTS('',3,(#28872,#28873,#28874,#28875,#28876,
#28877,#28878,#28879,#28880,#28881),.UNSPECIFIED.,.F.,.F.,(4,3,3,4),(-50.2654824574367,
-49.3230446702501,-48.3365837768451,-47.8312715558983),.UNSPECIFIED.);
#426=B_SPLINE_CURVE_WITH_KNOTS('',3,(#28886,#28887,#28888,#28889,#28890,
#28891,#28892,#28893,#28894,#28895,#28896,#28897,#28898,#28899,#28900,#28901,
#28902,#28903,#28904,#28905,#28906,#28907,#28908,#28909,#28910),
 .UNSPECIFIED.,.F.,.F.,(4,3,3,3,3,3,3,3,4),(45.2918602912342,45.3772010966301,
46.3636619900351,47.3501228834401,48.3365837768452,49.3230446702501,50.3095055636552,
51.2959664570602,51.5750455984138),.UNSPECIFIED.);
#427=B_SPLINE_CURVE_WITH_KNOTS('',3,(#28911,#28912,#28913,#28914,#28915,
#28916,#28917,#28918,#28919,#28920,#28921,#28922,#28923,#28924,#28925,#28926,
#28927,#28928,#28929,#28930,#28931,#28932),.UNSPECIFIED.,.F.,.F.,(4,3,3,
3,3,3,3,4),(-47.8312715558983,-47.3501228834401,-46.3636619900351,-45.3772010966301,
-44.3907402032251,-43.4042793098201,-42.4178184164151,-41.5480862487187),
 .UNSPECIFIED.);
#428=B_SPLINE_CURVE_WITH_KNOTS('',3,(#28937,#28938,#28939,#28940,#28941,
#28942,#28943,#28944,#28945,#28946,#28947,#28948,#28949,#28950,#28951,#28952,
#28953,#28954,#28955,#28956,#28957,#28958),.UNSPECIFIED.,.F.,.F.,(4,3,3,
3,3,3,3,4),(39.0086749840546,39.4584357362001,40.4448966296051,41.4313575230101,
42.4178184164151,43.4042793098201,44.3907402032251,45.2918602912342),
 .UNSPECIFIED.);
#429=B_SPLINE_CURVE_WITH_KNOTS('',3,(#28959,#28960,#28961,#28962,#28963,
#28964,#28965,#28966,#28967,#28968,#28969,#28970,#28971,#28972,#28973,#28974,
#28975,#28976,#28977,#28978,#28979,#28980,#28981,#28982,#28983),
 .UNSPECIFIED.,.F.,.F.,(4,3,3,3,3,3,3,3,4),(-41.5480862487187,-41.4313575230101,
-40.4448966296051,-39.4584357362001,-38.4719748427951,-37.4855139493901,
-36.4990530559851,-35.5125921625801,-35.2649009415391),.UNSPECIFIED.);
#430=B_SPLINE_CURVE_WITH_KNOTS('',3,(#28988,#28989,#28990,#28991,#28992,
#28993,#28994,#28995,#28996,#28997,#28998,#28999,#29000,#29001,#29002,#29003,
#29004,#29005,#29006,#29007,#29008,#29009),.UNSPECIFIED.,.F.,.F.,(4,3,3,
3,3,3,3,4),(32.725489676875,33.5396703757701,34.5261312691751,35.5125921625801,
36.4990530559851,37.4855139493901,38.4719748427951,39.0086749840546),
 .UNSPECIFIED.);
#431=B_SPLINE_CURVE_WITH_KNOTS('',3,(#29010,#29011,#29012,#29013,#29014,
#29015,#29016,#29017,#29018,#29019,#29020,#29021,#29022,#29023,#29024,#29025,
#29026,#29027,#29028,#29029,#29030,#29031),.UNSPECIFIED.,.F.,.F.,(4,3,3,
3,3,3,3,4),(-35.2649009415391,-34.5261312691751,-33.5396703757701,-32.5532094823651,
-31.5667485889601,-30.5802876955551,-29.5938268021501,-28.9817156343595),
 .UNSPECIFIED.);
#432=B_SPLINE_CURVE_WITH_KNOTS('',3,(#29036,#29037,#29038,#29039,#29040,
#29041,#29042,#29043,#29044,#29045,#29046,#29047,#29048,#29049,#29050,#29051,
#29052,#29053,#29054,#29055,#29056,#29057,#29058,#29059,#29060),
 .UNSPECIFIED.,.F.,.F.,(4,3,3,3,3,3,3,3,4),(26.4423043696954,26.6344441219351,
27.6209050153401,28.6073659087451,29.5938268021501,30.5802876955551,31.5667485889601,
32.5532094823651,32.725489676875),.UNSPECIFIED.);
#433=B_SPLINE_CURVE_WITH_KNOTS('',3,(#29061,#29062,#29063,#29064,#29065,
#29066,#29067,#29068,#29069,#29070,#29071,#29072,#29073,#29074,#29075,#29076,
#29077,#29078,#29079,#29080,#29081,#29082),.UNSPECIFIED.,.F.,.F.,(4,3,3,
3,3,3,3,4),(-28.9817156343595,-28.6073659087451,-27.6209050153401,-26.6344441219351,
-25.6479832285301,-24.6615223351251,-23.6750614417201,-22.6985303271799),
 .UNSPECIFIED.);
#434=B_SPLINE_CURVE_WITH_KNOTS('',3,(#29087,#29088,#29089,#29090,#29091,
#29092,#29093,#29094,#29095,#29096,#29097,#29098,#29099,#29100,#29101,#29102,
#29103,#29104,#29105,#29106,#29107,#29108),.UNSPECIFIED.,.F.,.F.,(4,3,3,
3,3,3,3,4),(20.1591190625159,20.7156787615051,21.7021396549101,22.6886005483151,
23.6750614417201,24.6615223351251,25.6479832285301,26.4423043696954),
 .UNSPECIFIED.);
#435=B_SPLINE_CURVE_WITH_KNOTS('',3,(#29109,#29110,#29111,#29112,#29113,
#29114,#29115,#29116,#29117,#29118,#29119,#29120,#29121,#29122,#29123,#29124,
#29125,#29126,#29127,#29128,#29129,#29130,#29131,#29132,#29133),
 .UNSPECIFIED.,.F.,.F.,(4,3,3,3,3,3,3,3,4),(-22.6985303271799,-22.6886005483151,
-21.7021396549101,-20.7156787615051,-19.7292178681001,-18.7427569746951,
-17.7562960812901,-16.7698351878851,-16.4153450200003),.UNSPECIFIED.);
#436=B_SPLINE_CURVE_WITH_KNOTS('',3,(#29138,#29139,#29140,#29141,#29142,
#29143,#29144,#29145,#29146,#29147,#29148,#29149,#29150,#29151,#29152,#29153,
#29154,#29155,#29156,#29157,#29158,#29159),.UNSPECIFIED.,.F.,.F.,(4,3,3,
3,3,3,3,4),(13.8759337553363,14.7969134010751,15.78337429448,16.7698351878851,
17.75629608129,18.7427569746951,19.7292178681001,20.1591190625159),
 .UNSPECIFIED.);
#437=B_SPLINE_CURVE_WITH_KNOTS('',3,(#29160,#29161,#29162,#29163,#29164,
#29165,#29166,#29167,#29168,#29169,#29170,#29171,#29172,#29173,#29174,#29175,
#29176,#29177,#29178,#29179,#29180,#29181),.UNSPECIFIED.,.F.,.F.,(4,3,3,
3,3,3,3,4),(-16.4153450200003,-15.78337429448,-14.796913401075,-13.81045250767,
-12.823991614265,-11.83753072086,-10.851069827455,-10.1321597128207),
 .UNSPECIFIED.);
#438=B_SPLINE_CURVE_WITH_KNOTS('',3,(#29187,#29188,#29189,#29190,#29191,
#29192,#29193,#29194,#29195,#29196,#29197,#29198,#29199),.UNSPECIFIED.,
 .F.,.F.,(4,3,3,3,4),(-3.84897440564115,-2.95938268021501,-1.97292178681001,
-0.986460893405001,0.),.UNSPECIFIED.);
#439=B_SPLINE_CURVE_WITH_KNOTS('',3,(#29202,#29203,#29204,#29205,#29206,
#29207,#29208,#29209,#29210,#29211,#29212,#29213,#29214,#29215,#29216,#29217,
#29218,#29219,#29220),.UNSPECIFIED.,.F.,.F.,(4,3,3,3,3,3,4),(2.01694489302845,
2.95938268021501,3.94584357362001,4.93230446702501,5.91876536043001,6.90522625383502,
7.59274844815668),.UNSPECIFIED.);
#440=B_SPLINE_CURVE_WITH_KNOTS('',3,(#29226,#29227,#29228,#29229,#29230,
#29231,#29232,#29233),.UNSPECIFIED.,.F.,.F.,(4,1,1,1,1,4),(59.6902604182061,
60.1955726391529,61.1820335325579,62.1684944259629,63.154955319368,64.141416212773),
 .UNSPECIFIED.);
#441=B_SPLINE_CURVE_WITH_KNOTS('',3,(#29236,#29237,#29238,#29239,#29240,
#29241,#29242,#29243,#29244),.UNSPECIFIED.,.F.,.F.,(4,1,1,1,1,1,4),(59.6902604182061,
59.775601223602,60.762062117007,61.748523010412,62.734983903817,63.721444797222,
64.6638825844085),.UNSPECIFIED.);
#442=B_SPLINE_CURVE_WITH_KNOTS('',3,(#29249,#29250,#29251,#29252,#29253,
#29254,#29255,#29256,#29257,#29258),.UNSPECIFIED.,.F.,.F.,(4,1,1,1,1,1,
1,4),(53.4070751110265,54.2768072787229,55.2632681721279,56.2497290655329,
57.2361899589379,58.2226508523429,59.2091117457479,59.6902604182061),
 .UNSPECIFIED.);
#443=B_SPLINE_CURVE_WITH_KNOTS('',3,(#29259,#29260,#29261,#29262,#29263,
#29264,#29265,#29266,#29267,#29268),.UNSPECIFIED.,.F.,.F.,(4,1,1,1,1,1,
1,4),(53.4070751110265,53.856835863172,54.843296756577,55.829757649982,
56.816218543387,57.802679436792,58.789140330197,59.6902604182061),
 .UNSPECIFIED.);
#444=B_SPLINE_CURVE_WITH_KNOTS('',3,(#29273,#29274,#29275,#29276,#29277,
#29278,#29279,#29280,#29281,#29282,#29283),.UNSPECIFIED.,.F.,.F.,(4,1,1,
1,1,1,1,1,4),(47.1238898038469,47.3715810248879,48.3580419182929,49.3445028116979,
50.3309637051029,51.3174245985079,52.3038854919129,53.2903463853179,53.4070751110265),
 .UNSPECIFIED.);
#445=B_SPLINE_CURVE_WITH_KNOTS('',3,(#29284,#29285,#29286,#29287,#29288,
#29289,#29290,#29291,#29292,#29293),.UNSPECIFIED.,.F.,.F.,(4,1,1,1,1,1,
1,4),(47.1238898038469,47.9380705027419,48.9245313961469,49.9109922895519,
50.8974531829569,51.8839140763619,52.8703749697669,53.4070751110265),
 .UNSPECIFIED.);
#446=B_SPLINE_CURVE_WITH_KNOTS('',3,(#29298,#29299,#29300,#29301,#29302,
#29303,#29304,#29305,#29306,#29307),.UNSPECIFIED.,.F.,.F.,(4,1,1,1,1,1,
1,4),(40.8407044966673,41.4528156644579,42.4392765578629,43.4257374512679,
44.4121983446729,45.3986592380779,46.3851201314829,47.1238898038469),
 .UNSPECIFIED.);
#447=B_SPLINE_CURVE_WITH_KNOTS('',3,(#29308,#29309,#29310,#29311,#29312,
#29313,#29314,#29315,#29316,#29317,#29318),.UNSPECIFIED.,.F.,.F.,(4,1,1,
1,1,1,1,1,4),(40.8407044966673,41.0328442489069,42.0193051423119,43.0057660357169,
43.9922269291219,44.9786878225269,45.9651487159319,46.9516096093369,47.1238898038469),
 .UNSPECIFIED.);
#448=B_SPLINE_CURVE_WITH_KNOTS('',3,(#29323,#29324,#29325,#29326,#29327,
#29328,#29329,#29330,#29331,#29332),.UNSPECIFIED.,.F.,.F.,(4,1,1,1,1,1,
1,4),(34.5575191894877,35.5340503040279,36.5205111974329,37.5069720908379,
38.4934329842429,39.4798938776479,40.4663547710529,40.8407044966673),
 .UNSPECIFIED.);
#449=B_SPLINE_CURVE_WITH_KNOTS('',3,(#29333,#29334,#29335,#29336,#29337,
#29338,#29339,#29340,#29341,#29342),.UNSPECIFIED.,.F.,.F.,(4,1,1,1,1,1,
1,4),(34.5575191894877,35.1140788884769,36.1005397818819,37.0870006752869,
38.0734615686919,39.0599224620969,40.0463833555019,40.8407044966673),
 .UNSPECIFIED.);
#450=B_SPLINE_CURVE_WITH_KNOTS('',3,(#29347,#29348,#29349,#29350,#29351,
#29352,#29353,#29354,#29355,#29356,#29357),.UNSPECIFIED.,.F.,.F.,(4,1,1,
1,1,1,1,1,4),(28.2743338823081,28.6288240501929,29.6152849435979,30.6017458370029,
31.5882067304079,32.5746676238129,33.5611285172179,34.5475894106229,34.5575191894877),
 .UNSPECIFIED.);
#451=B_SPLINE_CURVE_WITH_KNOTS('',3,(#29358,#29359,#29360,#29361,#29362,
#29363,#29364,#29365,#29366,#29367),.UNSPECIFIED.,.F.,.F.,(4,1,1,1,1,1,
1,4),(28.2743338823081,29.1953135280469,30.1817744214519,31.1682353148569,
32.1546962082619,33.1411571016669,34.1276179950719,34.5575191894877),
 .UNSPECIFIED.);
#452=B_SPLINE_CURVE_WITH_KNOTS('',3,(#29372,#29373,#29374,#29375,#29376,
#29377,#29378,#29379,#29380,#29381),.UNSPECIFIED.,.F.,.F.,(4,1,1,1,1,1,
1,4),(21.9911485751285,22.7100586897628,23.6965195831678,24.6829804765728,
25.6694413699778,26.6559022633828,27.6423631567879,28.2743338823081),
 .UNSPECIFIED.);
#453=B_SPLINE_CURVE_WITH_KNOTS('',3,(#29382,#29383,#29384,#29385,#29386,
#29387,#29388,#29389,#29390,#29391,#29392),.UNSPECIFIED.,.F.,.F.,(4,1,1,
1,1,1,1,1,4),(21.9911485751285,22.2900872742119,23.2765481676169,24.2630090610219,
25.2494699544269,26.2359308478319,27.2223917412369,28.2088526346419,28.2743338823081),
 .UNSPECIFIED.);
#454=B_SPLINE_CURVE_WITH_KNOTS('',3,(#29398,#29399,#29400,#29401,#29402),
 .UNSPECIFIED.,.F.,.F.,(4,1,4),(14.3984001269718,15.3848610203768,15.7079632679489),
 .UNSPECIFIED.);
#455=B_SPLINE_CURVE_WITH_KNOTS('',3,(#29405,#29406,#29407,#29408,#29409),
 .UNSPECIFIED.,.F.,.F.,(4,1,4),(13.8759337553363,14.8183715425228,15.7079632679489),
 .UNSPECIFIED.);
#456=B_SPLINE_CURVE_WITH_KNOTS('',3,(#29415,#29416,#29417,#29418,#29419,
#29420,#29421,#29422),.UNSPECIFIED.,.F.,.F.,(4,1,1,1,1,4),(59.6902604182061,
60.1955726391529,61.1820335325579,62.1684944259629,63.1549553193679,64.1414162127729),
 .UNSPECIFIED.);
#457=B_SPLINE_CURVE_WITH_KNOTS('',3,(#29425,#29426,#29427,#29428,#29429,
#29430,#29431,#29432,#29433),.UNSPECIFIED.,.F.,.F.,(4,1,1,1,1,1,4),(59.6902604182061,
59.775601223602,60.762062117007,61.748523010412,62.734983903817,63.721444797222,
64.6638825844085),.UNSPECIFIED.);
#458=B_SPLINE_CURVE_WITH_KNOTS('',3,(#29438,#29439,#29440,#29441,#29442,
#29443,#29444,#29445,#29446,#29447),.UNSPECIFIED.,.F.,.F.,(4,1,1,1,1,1,
1,4),(53.4070751110265,54.2768072787229,55.2632681721279,56.2497290655329,
57.2361899589379,58.2226508523429,59.2091117457479,59.6902604182061),
 .UNSPECIFIED.);
#459=B_SPLINE_CURVE_WITH_KNOTS('',3,(#29448,#29449,#29450,#29451,#29452,
#29453,#29454,#29455,#29456,#29457),.UNSPECIFIED.,.F.,.F.,(4,1,1,1,1,1,
1,4),(53.4070751110265,53.856835863172,54.843296756577,55.829757649982,
56.816218543387,57.802679436792,58.789140330197,59.6902604182061),
 .UNSPECIFIED.);
#460=B_SPLINE_CURVE_WITH_KNOTS('',3,(#29462,#29463,#29464,#29465,#29466,
#29467,#29468,#29469,#29470,#29471,#29472),.UNSPECIFIED.,.F.,.F.,(4,1,1,
1,1,1,1,1,4),(47.1238898038469,47.3715810248879,48.3580419182929,49.3445028116979,
50.3309637051029,51.3174245985079,52.3038854919129,53.2903463853179,53.4070751110265),
 .UNSPECIFIED.);
#461=B_SPLINE_CURVE_WITH_KNOTS('',3,(#29473,#29474,#29475,#29476,#29477,
#29478,#29479,#29480,#29481,#29482),.UNSPECIFIED.,.F.,.F.,(4,1,1,1,1,1,
1,4),(47.1238898038469,47.9380705027419,48.9245313961469,49.9109922895519,
50.8974531829569,51.8839140763619,52.8703749697669,53.4070751110265),
 .UNSPECIFIED.);
#462=B_SPLINE_CURVE_WITH_KNOTS('',3,(#29487,#29488,#29489,#29490,#29491,
#29492,#29493,#29494,#29495,#29496),.UNSPECIFIED.,.F.,.F.,(4,1,1,1,1,1,
1,4),(40.8407044966673,41.4528156644579,42.4392765578629,43.4257374512679,
44.4121983446729,45.3986592380779,46.3851201314829,47.1238898038469),
 .UNSPECIFIED.);
#463=B_SPLINE_CURVE_WITH_KNOTS('',3,(#29497,#29498,#29499,#29500,#29501,
#29502,#29503,#29504,#29505,#29506,#29507),.UNSPECIFIED.,.F.,.F.,(4,1,1,
1,1,1,1,1,4),(40.8407044966673,41.0328442489069,42.0193051423119,43.0057660357169,
43.9922269291219,44.9786878225269,45.9651487159319,46.9516096093369,47.1238898038469),
 .UNSPECIFIED.);
#464=B_SPLINE_CURVE_WITH_KNOTS('',3,(#29512,#29513,#29514,#29515,#29516,
#29517,#29518,#29519,#29520,#29521),.UNSPECIFIED.,.F.,.F.,(4,1,1,1,1,1,
1,4),(34.5575191894877,35.5340503040279,36.5205111974329,37.5069720908379,
38.4934329842429,39.4798938776479,40.4663547710529,40.8407044966673),
 .UNSPECIFIED.);
#465=B_SPLINE_CURVE_WITH_KNOTS('',3,(#29522,#29523,#29524,#29525,#29526,
#29527,#29528,#29529,#29530,#29531),.UNSPECIFIED.,.F.,.F.,(4,1,1,1,1,1,
1,4),(34.5575191894877,35.1140788884769,36.1005397818819,37.0870006752869,
38.0734615686919,39.0599224620969,40.0463833555019,40.8407044966673),
 .UNSPECIFIED.);
#466=B_SPLINE_CURVE_WITH_KNOTS('',3,(#29536,#29537,#29538,#29539,#29540,
#29541,#29542,#29543,#29544,#29545,#29546),.UNSPECIFIED.,.F.,.F.,(4,1,1,
1,1,1,1,1,4),(28.2743338823081,28.6288240501928,29.6152849435978,30.6017458370028,
31.5882067304078,32.5746676238129,33.5611285172179,34.5475894106229,34.5575191894877),
 .UNSPECIFIED.);
#467=B_SPLINE_CURVE_WITH_KNOTS('',3,(#29547,#29548,#29549,#29550,#29551,
#29552,#29553,#29554,#29555,#29556),.UNSPECIFIED.,.F.,.F.,(4,1,1,1,1,1,
1,4),(28.2743338823081,29.1953135280469,30.1817744214519,31.1682353148569,
32.1546962082619,33.1411571016669,34.1276179950719,34.5575191894877),
 .UNSPECIFIED.);
#468=B_SPLINE_CURVE_WITH_KNOTS('',3,(#29561,#29562,#29563,#29564,#29565,
#29566,#29567,#29568,#29569,#29570),.UNSPECIFIED.,.F.,.F.,(4,1,1,1,1,1,
1,4),(21.9911485751285,22.7100586897628,23.6965195831678,24.6829804765728,
25.6694413699778,26.6559022633828,27.6423631567878,28.2743338823081),
 .UNSPECIFIED.);
#469=B_SPLINE_CURVE_WITH_KNOTS('',3,(#29571,#29572,#29573,#29574,#29575,
#29576,#29577,#29578,#29579,#29580,#29581),.UNSPECIFIED.,.F.,.F.,(4,1,1,
1,1,1,1,1,4),(21.9911485751285,22.2900872742119,23.2765481676169,24.2630090610219,
25.2494699544269,26.2359308478319,27.2223917412369,28.2088526346419,28.2743338823081),
 .UNSPECIFIED.);
#470=B_SPLINE_CURVE_WITH_KNOTS('',3,(#29587,#29588,#29589,#29590,#29591),
 .UNSPECIFIED.,.F.,.F.,(4,1,4),(14.3984001269718,15.3848610203768,15.7079632679489),
 .UNSPECIFIED.);
#471=B_SPLINE_CURVE_WITH_KNOTS('',3,(#29594,#29595,#29596,#29597,#29598),
 .UNSPECIFIED.,.F.,.F.,(4,1,4),(13.8759337553362,14.8183715425228,15.707963267949),
 .UNSPECIFIED.);
#472=B_SPLINE_CURVE_WITH_KNOTS('',3,(#29604,#29605,#29606,#29607,#29608,
#29609,#29610,#29611),.UNSPECIFIED.,.F.,.F.,(4,1,1,1,1,4),(59.6902604182061,
60.1955726391529,61.1820335325579,62.1684944259629,63.154955319368,64.141416212773),
 .UNSPECIFIED.);
#473=B_SPLINE_CURVE_WITH_KNOTS('',3,(#29614,#29615,#29616,#29617,#29618,
#29619,#29620,#29621,#29622),.UNSPECIFIED.,.F.,.F.,(4,1,1,1,1,1,4),(59.6902604182061,
59.775601223602,60.762062117007,61.748523010412,62.734983903817,63.721444797222,
64.6638825844085),.UNSPECIFIED.);
#474=B_SPLINE_CURVE_WITH_KNOTS('',3,(#29627,#29628,#29629,#29630,#29631,
#29632,#29633,#29634,#29635,#29636),.UNSPECIFIED.,.F.,.F.,(4,1,1,1,1,1,
1,4),(53.4070751110265,54.2768072787229,55.2632681721279,56.2497290655329,
57.2361899589379,58.2226508523429,59.2091117457479,59.6902604182061),
 .UNSPECIFIED.);
#475=B_SPLINE_CURVE_WITH_KNOTS('',3,(#29637,#29638,#29639,#29640,#29641,
#29642,#29643,#29644,#29645,#29646),.UNSPECIFIED.,.F.,.F.,(4,1,1,1,1,1,
1,4),(53.4070751110265,53.856835863172,54.843296756577,55.829757649982,
56.816218543387,57.802679436792,58.789140330197,59.6902604182061),
 .UNSPECIFIED.);
#476=B_SPLINE_CURVE_WITH_KNOTS('',3,(#29651,#29652,#29653,#29654,#29655,
#29656,#29657,#29658,#29659,#29660,#29661),.UNSPECIFIED.,.F.,.F.,(4,1,1,
1,1,1,1,1,4),(47.1238898038469,47.3715810248879,48.3580419182929,49.3445028116979,
50.3309637051029,51.3174245985079,52.3038854919129,53.2903463853179,53.4070751110265),
 .UNSPECIFIED.);
#477=B_SPLINE_CURVE_WITH_KNOTS('',3,(#29662,#29663,#29664,#29665,#29666,
#29667,#29668,#29669,#29670,#29671),.UNSPECIFIED.,.F.,.F.,(4,1,1,1,1,1,
1,4),(47.1238898038469,47.9380705027419,48.9245313961469,49.9109922895519,
50.8974531829569,51.8839140763619,52.8703749697669,53.4070751110265),
 .UNSPECIFIED.);
#478=B_SPLINE_CURVE_WITH_KNOTS('',3,(#29676,#29677,#29678,#29679,#29680,
#29681,#29682,#29683,#29684,#29685),.UNSPECIFIED.,.F.,.F.,(4,1,1,1,1,1,
1,4),(40.8407044966673,41.4528156644579,42.4392765578629,43.4257374512679,
44.4121983446729,45.3986592380779,46.3851201314829,47.1238898038469),
 .UNSPECIFIED.);
#479=B_SPLINE_CURVE_WITH_KNOTS('',3,(#29686,#29687,#29688,#29689,#29690,
#29691,#29692,#29693,#29694,#29695,#29696),.UNSPECIFIED.,.F.,.F.,(4,1,1,
1,1,1,1,1,4),(40.8407044966673,41.0328442489069,42.0193051423119,43.0057660357169,
43.9922269291219,44.9786878225269,45.9651487159319,46.9516096093369,47.1238898038469),
 .UNSPECIFIED.);
#480=B_SPLINE_CURVE_WITH_KNOTS('',3,(#29701,#29702,#29703,#29704,#29705,
#29706,#29707,#29708,#29709,#29710),.UNSPECIFIED.,.F.,.F.,(4,1,1,1,1,1,
1,4),(34.5575191894877,35.5340503040279,36.5205111974329,37.5069720908379,
38.4934329842429,39.4798938776479,40.4663547710529,40.8407044966673),
 .UNSPECIFIED.);
#481=B_SPLINE_CURVE_WITH_KNOTS('',3,(#29711,#29712,#29713,#29714,#29715,
#29716,#29717,#29718,#29719,#29720),.UNSPECIFIED.,.F.,.F.,(4,1,1,1,1,1,
1,4),(34.5575191894877,35.1140788884769,36.1005397818819,37.0870006752869,
38.0734615686919,39.0599224620969,40.0463833555019,40.8407044966673),
 .UNSPECIFIED.);
#482=B_SPLINE_CURVE_WITH_KNOTS('',3,(#29725,#29726,#29727,#29728,#29729,
#29730,#29731,#29732,#29733,#29734,#29735),.UNSPECIFIED.,.F.,.F.,(4,1,1,
1,1,1,1,1,4),(28.2743338823081,28.6288240501929,29.6152849435979,30.6017458370029,
31.5882067304079,32.5746676238129,33.5611285172179,34.5475894106229,34.5575191894877),
 .UNSPECIFIED.);
#483=B_SPLINE_CURVE_WITH_KNOTS('',3,(#29736,#29737,#29738,#29739,#29740,
#29741,#29742,#29743,#29744,#29745),.UNSPECIFIED.,.F.,.F.,(4,1,1,1,1,1,
1,4),(28.2743338823081,29.1953135280469,30.1817744214519,31.1682353148569,
32.1546962082619,33.1411571016669,34.1276179950719,34.5575191894877),
 .UNSPECIFIED.);
#484=B_SPLINE_CURVE_WITH_KNOTS('',3,(#29750,#29751,#29752,#29753,#29754,
#29755,#29756,#29757,#29758,#29759),.UNSPECIFIED.,.F.,.F.,(4,1,1,1,1,1,
1,4),(21.9911485751285,22.7100586897628,23.6965195831678,24.6829804765728,
25.6694413699778,26.6559022633828,27.6423631567879,28.2743338823081),
 .UNSPECIFIED.);
#485=B_SPLINE_CURVE_WITH_KNOTS('',3,(#29760,#29761,#29762,#29763,#29764,
#29765,#29766,#29767,#29768,#29769,#29770),.UNSPECIFIED.,.F.,.F.,(4,1,1,
1,1,1,1,1,4),(21.9911485751285,22.2900872742119,23.2765481676169,24.2630090610219,
25.2494699544269,26.2359308478319,27.2223917412369,28.2088526346419,28.2743338823081),
 .UNSPECIFIED.);
#486=B_SPLINE_CURVE_WITH_KNOTS('',3,(#29776,#29777,#29778,#29779,#29780),
 .UNSPECIFIED.,.F.,.F.,(4,1,4),(14.3984001269718,15.3848610203768,15.7079632679489),
 .UNSPECIFIED.);
#487=B_SPLINE_CURVE_WITH_KNOTS('',3,(#29783,#29784,#29785,#29786,#29787),
 .UNSPECIFIED.,.F.,.F.,(4,1,4),(13.8759337553363,14.8183715425228,15.707963267949),
 .UNSPECIFIED.);
#488=B_SPLINE_CURVE_WITH_KNOTS('',3,(#29793,#29794,#29795,#29796,#29797,
#29798,#29799,#29800),.UNSPECIFIED.,.F.,.F.,(4,1,1,1,1,4),(59.6902604182061,
60.1955726391529,61.1820335325579,62.1684944259629,63.1549553193679,64.1414162127729),
 .UNSPECIFIED.);
#489=B_SPLINE_CURVE_WITH_KNOTS('',3,(#29803,#29804,#29805,#29806,#29807,
#29808,#29809,#29810,#29811),.UNSPECIFIED.,.F.,.F.,(4,1,1,1,1,1,4),(59.6902604182061,
59.775601223602,60.762062117007,61.748523010412,62.734983903817,63.721444797222,
64.6638825844085),.UNSPECIFIED.);
#490=B_SPLINE_CURVE_WITH_KNOTS('',3,(#29816,#29817,#29818,#29819,#29820,
#29821,#29822,#29823,#29824,#29825),.UNSPECIFIED.,.F.,.F.,(4,1,1,1,1,1,
1,4),(53.4070751110265,54.2768072787229,55.2632681721279,56.2497290655329,
57.2361899589379,58.2226508523429,59.2091117457479,59.6902604182061),
 .UNSPECIFIED.);
#491=B_SPLINE_CURVE_WITH_KNOTS('',3,(#29826,#29827,#29828,#29829,#29830,
#29831,#29832,#29833,#29834,#29835),.UNSPECIFIED.,.F.,.F.,(4,1,1,1,1,1,
1,4),(53.4070751110265,53.856835863172,54.843296756577,55.829757649982,
56.816218543387,57.802679436792,58.789140330197,59.6902604182061),
 .UNSPECIFIED.);
#492=B_SPLINE_CURVE_WITH_KNOTS('',3,(#29840,#29841,#29842,#29843,#29844,
#29845,#29846,#29847,#29848,#29849,#29850),.UNSPECIFIED.,.F.,.F.,(4,1,1,
1,1,1,1,1,4),(47.1238898038469,47.3715810248879,48.3580419182929,49.3445028116979,
50.3309637051029,51.3174245985079,52.3038854919129,53.2903463853179,53.4070751110265),
 .UNSPECIFIED.);
#493=B_SPLINE_CURVE_WITH_KNOTS('',3,(#29851,#29852,#29853,#29854,#29855,
#29856,#29857,#29858,#29859,#29860),.UNSPECIFIED.,.F.,.F.,(4,1,1,1,1,1,
1,4),(47.1238898038469,47.9380705027419,48.9245313961469,49.9109922895519,
50.8974531829569,51.8839140763619,52.8703749697669,53.4070751110265),
 .UNSPECIFIED.);
#494=B_SPLINE_CURVE_WITH_KNOTS('',3,(#29865,#29866,#29867,#29868,#29869,
#29870,#29871,#29872,#29873,#29874),.UNSPECIFIED.,.F.,.F.,(4,1,1,1,1,1,
1,4),(40.8407044966673,41.4528156644579,42.4392765578629,43.4257374512679,
44.4121983446729,45.3986592380779,46.3851201314829,47.1238898038469),
 .UNSPECIFIED.);
#495=B_SPLINE_CURVE_WITH_KNOTS('',3,(#29875,#29876,#29877,#29878,#29879,
#29880,#29881,#29882,#29883,#29884,#29885),.UNSPECIFIED.,.F.,.F.,(4,1,1,
1,1,1,1,1,4),(40.8407044966673,41.0328442489069,42.0193051423119,43.0057660357169,
43.9922269291219,44.9786878225269,45.9651487159319,46.9516096093369,47.1238898038469),
 .UNSPECIFIED.);
#496=B_SPLINE_CURVE_WITH_KNOTS('',3,(#29890,#29891,#29892,#29893,#29894,
#29895,#29896,#29897,#29898,#29899),.UNSPECIFIED.,.F.,.F.,(4,1,1,1,1,1,
1,4),(34.5575191894877,35.5340503040279,36.5205111974329,37.5069720908379,
38.4934329842429,39.4798938776479,40.4663547710529,40.8407044966673),
 .UNSPECIFIED.);
#497=B_SPLINE_CURVE_WITH_KNOTS('',3,(#29900,#29901,#29902,#29903,#29904,
#29905,#29906,#29907,#29908,#29909),.UNSPECIFIED.,.F.,.F.,(4,1,1,1,1,1,
1,4),(34.5575191894877,35.1140788884769,36.1005397818819,37.0870006752869,
38.0734615686919,39.0599224620969,40.0463833555019,40.8407044966673),
 .UNSPECIFIED.);
#498=B_SPLINE_CURVE_WITH_KNOTS('',3,(#29914,#29915,#29916,#29917,#29918,
#29919,#29920,#29921,#29922,#29923,#29924),.UNSPECIFIED.,.F.,.F.,(4,1,1,
1,1,1,1,1,4),(28.2743338823081,28.6288240501928,29.6152849435978,30.6017458370028,
31.5882067304078,32.5746676238129,33.5611285172179,34.5475894106229,34.5575191894877),
 .UNSPECIFIED.);
#499=B_SPLINE_CURVE_WITH_KNOTS('',3,(#29925,#29926,#29927,#29928,#29929,
#29930,#29931,#29932,#29933,#29934),.UNSPECIFIED.,.F.,.F.,(4,1,1,1,1,1,
1,4),(28.2743338823081,29.1953135280469,30.1817744214519,31.1682353148569,
32.1546962082619,33.1411571016669,34.1276179950719,34.5575191894877),
 .UNSPECIFIED.);
#500=B_SPLINE_CURVE_WITH_KNOTS('',3,(#29939,#29940,#29941,#29942,#29943,
#29944,#29945,#29946,#29947,#29948),.UNSPECIFIED.,.F.,.F.,(4,1,1,1,1,1,
1,4),(21.9911485751285,22.7100586897628,23.6965195831678,24.6829804765728,
25.6694413699778,26.6559022633828,27.6423631567878,28.2743338823081),
 .UNSPECIFIED.);
#501=B_SPLINE_CURVE_WITH_KNOTS('',3,(#29949,#29950,#29951,#29952,#29953,
#29954,#29955,#29956,#29957,#29958,#29959),.UNSPECIFIED.,.F.,.F.,(4,1,1,
1,1,1,1,1,4),(21.9911485751285,22.2900872742119,23.2765481676169,24.2630090610219,
25.2494699544269,26.2359308478319,27.2223917412369,28.2088526346419,28.2743338823081),
 .UNSPECIFIED.);
#502=B_SPLINE_CURVE_WITH_KNOTS('',3,(#29965,#29966,#29967,#29968,#29969),
 .UNSPECIFIED.,.F.,.F.,(4,1,4),(14.3984001269718,15.3848610203768,15.7079632679489),
 .UNSPECIFIED.);
#503=B_SPLINE_CURVE_WITH_KNOTS('',3,(#29972,#29973,#29974,#29975,#29976),
 .UNSPECIFIED.,.F.,.F.,(4,1,4),(13.8759337553362,14.8183715425228,15.707963267949),
 .UNSPECIFIED.);
#504=B_SPLINE_CURVE_WITH_KNOTS('',3,(#29978,#29979,#29980,#29981,#29982,
#29983,#29984,#29985,#29986,#29987,#29988),.UNSPECIFIED.,.F.,.F.,(4,1,1,
1,1,1,1,1,4),(15.707963267949,15.8048324359278,16.7912933293328,17.7777542227378,
18.7642151161428,19.7506760095478,20.7371369029528,21.7235977963578,21.9911485751285),
 .UNSPECIFIED.);
#505=B_SPLINE_CURVE_WITH_KNOTS('',3,(#29989,#29990,#29991,#29992,#29993,
#29994,#29995,#29996,#29997,#29998),.UNSPECIFIED.,.F.,.F.,(4,1,1,1,1,1,
1,4),(15.7079632679489,16.3713219137818,17.3577828071868,18.3442437005918,
19.3307045939968,20.3171654874019,21.3036263808069,21.9911485751285),
 .UNSPECIFIED.);
#506=B_SPLINE_CURVE_WITH_KNOTS('',3,(#30223,#30224,#30225,#30226,#30227,
#30228,#30229,#30230,#30231,#30232,#30233,#30234,#30235,#30236,#30237,#30238,
#30239,#30240,#30241,#30242,#30243,#30244,#30245,#30246,#30247,#30248,#30249,
#30250,#30251,#30252,#30253,#30254,#30255,#30256,#30257,#30258,#30259,#30260,
#30261,#30262,#30263,#30264,#30265,#30266,#30267,#30268,#30269,#30270,#30271,
#30272,#30273,#30274,#30275,#30276,#30277,#30278,#30279,#30280,#30281,#30282,
#30283,#30284,#30285,#30286,#30287,#30288,#30289,#30290,#30291,#30292,#30293,
#30294,#30295,#30296,#30297,#30298,#30299,#30300,#30301,#30302,#30303,#30304,
#30305,#30306,#30307,#30308,#30309,#30310,#30311,#30312,#30313,#30314,#30315,
#30316,#30317,#30318,#30319),.UNSPECIFIED.,.F.,.F.,(4,3,3,3,3,3,3,3,3,3,
3,3,3,3,3,3,3,3,3,3,3,3,3,3,3,3,3,3,3,3,3,3,4),(0.,0.0368039558979425,0.074433304608195,
0.113993701727663,0.148609049207197,0.155428774052918,0.160415086629183,
0.19765208124705,0.234804500431717,0.271449068097489,0.301315921464101,
0.308903275242872,0.314301747825082,0.350380426672586,0.385744311753463,
0.390916481563936,0.427339708778546,0.447829010848363,0.457282933923372,
0.462717602197838,0.49927396966006,0.535072007005015,0.570520291726377,
0.593601322997532,0.601390754314479,0.606406537654944,0.641366377472567,
0.669816918578329,0.683592881655056,0.691680493901417,0.725189682307058,
0.755168541895614,0.770777738583641),.UNSPECIFIED.);
#507=B_SPLINE_CURVE_WITH_KNOTS('',3,(#30320,#30321,#30322,#30323,#30324,
#30325,#30326,#30327,#30328,#30329,#30330,#30331,#30332,#30333,#30334,#30335,
#30336,#30337,#30338,#30339,#30340,#30341,#30342,#30343,#30344,#30345,#30346,
#30347,#30348,#30349,#30350,#30351,#30352,#30353,#30354,#30355,#30356,#30357,
#30358,#30359,#30360,#30361,#30362,#30363,#30364,#30365,#30366,#30367,#30368,
#30369,#30370,#30371,#30372,#30373,#30374,#30375,#30376,#30377,#30378,#30379,
#30380,#30381,#30382,#30383,#30384,#30385,#30386,#30387,#30388,#30389,#30390,
#30391,#30392,#30393,#30394,#30395,#30396,#30397,#30398,#30399,#30400,#30401,
#30402,#30403,#30404,#30405,#30406,#30407,#30408,#30409,#30410,#30411,#30412,
#30413),.UNSPECIFIED.,.F.,.F.,(4,3,3,3,3,3,3,3,3,3,3,3,3,3,3,3,3,3,3,3,
3,3,3,3,3,3,3,3,3,3,3,4),(0.,0.0327224441775746,0.0662804107708102,0.100536831058394,
0.133256562666979,0.138568566128973,0.143645838996043,0.178633774293771,
0.214080648720454,0.251134157522108,0.278924289123348,0.285558989031475,
0.321777080052277,0.357762779229756,0.362294683927068,0.397656599693718,
0.419708620040541,0.427245869011975,0.432639317722629,0.468078758515067,
0.504737423019667,0.541741021670041,0.567834509616647,0.5794821004587,0.584482028048437,
0.622064205916635,0.6541703857482,0.668577115889702,0.678363311229139,0.716158211242659,
0.750488925242892,0.768398079192695),.UNSPECIFIED.);
#508=B_SPLINE_CURVE_WITH_KNOTS('',3,(#30414,#30415,#30416,#30417,#30418,
#30419,#30420,#30421,#30422,#30423,#30424,#30425,#30426,#30427,#30428,#30429,
#30430,#30431,#30432,#30433,#30434,#30435,#30436,#30437,#30438),
 .UNSPECIFIED.,.F.,.F.,(4,3,3,3,3,3,3,3,4),(-10.1321597128207,-9.86460893405003,
-8.87814804064502,-7.89168714724003,-6.90522625383502,-5.91876536043002,
-4.93230446702502,-3.94584357362001,-3.84897440564115),.UNSPECIFIED.);
#509=B_SPLINE_CURVE_WITH_KNOTS('',3,(#30663,#30664,#30665,#30666,#30667,
#30668,#30669,#30670,#30671,#30672,#30673,#30674,#30675,#30676,#30677,#30678,
#30679,#30680,#30681,#30682,#30683,#30684,#30685,#30686,#30687,#30688,#30689,
#30690,#30691,#30692,#30693,#30694,#30695,#30696,#30697,#30698,#30699,#30700,
#30701,#30702,#30703,#30704,#30705,#30706,#30707,#30708,#30709,#30710,#30711,
#30712,#30713,#30714,#30715,#30716,#30717,#30718,#30719,#30720,#30721,#30722,
#30723,#30724,#30725,#30726,#30727,#30728,#30729,#30730,#30731,#30732,#30733,
#30734,#30735,#30736,#30737,#30738,#30739,#30740,#30741,#30742,#30743,#30744,
#30745,#30746,#30747,#30748,#30749,#30750,#30751,#30752,#30753,#30754,#30755,
#30756),.UNSPECIFIED.,.F.,.F.,(4,3,3,3,3,3,3,3,3,3,3,3,3,3,3,3,3,3,3,3,
3,3,3,3,3,3,3,3,3,3,3,4),(0.,0.0327225492804934,0.0662806081929849,0.100537094180834,
0.133256792899112,0.138569651942616,0.143645965484312,0.178633966005382,
0.214080867277344,0.251134321439773,0.278924412061594,0.285558992744241,
0.321777089637378,0.35776275463403,0.362294683927058,0.397656555534726,
0.419708578641487,0.427246439006672,0.432639234997264,0.468078611004923,
0.504737248356826,0.541740841146129,0.567834351658225,0.579481449773753,
0.584481041781399,0.622063204762494,0.654169634882595,0.668576564062872,
0.678363413635591,0.716158311359956,0.750488925242897,0.768398079192707),
 .UNSPECIFIED.);
#510=B_SPLINE_CURVE_WITH_KNOTS('',3,(#30757,#30758,#30759,#30760,#30761,
#30762,#30763,#30764,#30765,#30766,#30767,#30768,#30769,#30770,#30771,#30772,
#30773,#30774,#30775,#30776,#30777,#30778,#30779,#30780,#30781),
 .UNSPECIFIED.,.F.,.F.,(4,3,3,3,3,3,3,3,4),(7.59274844815668,7.89168714724002,
8.87814804064503,9.86460893405003,10.851069827455,11.83753072086,12.823991614265,
13.81045250767,13.8759337553363),.UNSPECIFIED.);
#511=B_SPLINE_CURVE_WITH_KNOTS('',3,(#30782,#30783,#30784,#30785,#30786,
#30787,#30788,#30789,#30790,#30791,#30792,#30793,#30794,#30795,#30796,#30797,
#30798,#30799,#30800,#30801,#30802,#30803,#30804,#30805,#30806,#30807,#30808,
#30809,#30810,#30811,#30812,#30813,#30814,#30815,#30816,#30817,#30818,#30819,
#30820,#30821,#30822,#30823,#30824,#30825,#30826,#30827,#30828,#30829,#30830,
#30831,#30832,#30833,#30834,#30835,#30836,#30837,#30838,#30839,#30840,#30841,
#30842,#30843,#30844,#30845,#30846,#30847,#30848,#30849,#30850,#30851,#30852,
#30853,#30854,#30855,#30856,#30857,#30858,#30859,#30860,#30861,#30862,#30863,
#30864,#30865,#30866,#30867,#30868,#30869,#30870,#30871,#30872,#30873,#30874,
#30875,#30876,#30877,#30878),.UNSPECIFIED.,.F.,.F.,(4,3,3,3,3,3,3,3,3,3,
3,3,3,3,3,3,3,3,3,3,3,3,3,3,3,3,3,3,3,3,3,3,4),(0.,0.036804046830165,0.0744334499110545,
0.113993828867664,0.148609160454698,0.155429461366191,0.160415755364031,
0.197652761113477,0.234805154528782,0.271449678901402,0.301316379567035,
0.30890483519103,0.314302031357973,0.350380678677425,0.385744531292533,
0.390916481563933,0.427339707871941,0.447829009998422,0.457282914861488,
0.462717597114684,0.499273965212302,0.535072004716797,0.570520279377824,
0.59360131219255,0.601390713399489,0.606406454642536,0.641366288894707,
0.669816852144937,0.683592817141769,0.691680484574319,0.72518963603372,
0.75516854189563,0.77077773858366),.UNSPECIFIED.);
#512=B_SPLINE_CURVE_WITH_KNOTS('',3,(#30888,#30889,#30890,#30891,#30892,
#30893,#30894,#30895,#30896,#30897,#30898,#30899,#30900,#30901,#30902,#30903,
#30904,#30905,#30906,#30907,#30908,#30909,#30910,#30911,#30912,#30913,#30914,
#30915,#30916,#30917,#30918,#30919,#30920,#30921,#30922,#30923,#30924,#30925,
#30926,#30927,#30928,#30929,#30930,#30931,#30932,#30933,#30934,#30935,#30936,
#30937,#30938,#30939,#30940,#30941,#30942,#30943,#30944,#30945,#30946,#30947,
#30948,#30949,#30950,#30951,#30952,#30953,#30954,#30955,#30956,#30957,#30958,
#30959,#30960,#30961,#30962,#30963,#30964,#30965,#30966,#30967,#30968,#30969,
#30970,#30971,#30972,#30973,#30974,#30975,#30976,#30977,#30978,#30979,#30980,
#30981),.UNSPECIFIED.,.F.,.F.,(4,3,3,3,3,3,3,3,3,3,3,3,3,3,3,3,3,3,3,3,
3,3,3,3,3,3,3,3,3,3,3,4),(0.,0.032722467477059,0.0662804545367435,0.10053688939052,
0.133256613707586,0.138568806761047,0.143645866999149,0.178633816756561,
0.214080697136686,0.251134193834276,0.278924316357469,0.285558989874725,
0.321777082201843,0.35776277380543,0.362294683927046,0.397656589907163,
0.419708610865643,0.427245995316486,0.432639299360784,0.468078725795143,
0.504737384281388,0.54174098163239,0.567834474583697,0.579481956142016,
0.584481809181592,0.622063983748247,0.654170219121896,0.668576993434055,
0.678363333947687,0.716158233455664,0.750488925242844,0.768398079192646),
 .UNSPECIFIED.);
#513=B_SPLINE_CURVE_WITH_KNOTS('',3,(#30982,#30983,#30984,#30985,#30986,
#30987,#30988,#30989,#30990,#30991,#30992,#30993,#30994,#30995,#30996,#30997,
#30998,#30999,#31000,#31001,#31002,#31003,#31004,#31005,#31006,#31007,#31008,
#31009,#31010,#31011,#31012,#31013,#31014,#31015,#31016,#31017,#31018,#31019,
#31020,#31021,#31022,#31023,#31024,#31025,#31026,#31027,#31028,#31029,#31030,
#31031,#31032,#31033,#31034,#31035,#31036,#31037,#31038,#31039,#31040,#31041,
#31042,#31043,#31044,#31045,#31046,#31047,#31048,#31049,#31050,#31051,#31052,
#31053,#31054,#31055,#31056,#31057,#31058,#31059,#31060,#31061,#31062,#31063,
#31064,#31065,#31066,#31067,#31068,#31069,#31070,#31071,#31072,#31073,#31074,
#31075,#31076,#31077,#31078),.UNSPECIFIED.,.F.,.F.,(4,3,3,3,3,3,3,3,3,3,
3,3,3,3,3,3,3,3,3,3,3,3,3,3,3,3,3,3,3,3,3,3,4),(0.,0.0368040733914109,0.0744334923513577,
0.113993866002931,0.148609192948057,0.155429662167008,0.160415950914505,
0.197652959912295,0.23480534579311,0.271449857509325,0.301316513522979,
0.308905291482282,0.314302114409216,0.350380752512021,0.385744595636286,
0.390916481563942,0.427339707606562,0.447829009749629,0.457282909273663,
0.462717595625807,0.499273963909537,0.53507200404104,0.57052027575377,0.593601309021504,
0.60139070143526,0.60640643038342,0.641366263001721,0.669816832725203,0.683592798284754,
0.691680481858046,0.725189622506651,0.755168541895646,0.770777738583679),
 .UNSPECIFIED.);
#514=B_SPLINE_CURVE_WITH_KNOTS('',3,(#31079,#31080,#31081,#31082,#31083,
#31084,#31085,#31086,#31087,#31088,#31089,#31090,#31091,#31092,#31093,#31094,
#31095,#31096,#31097,#31098,#31099,#31100,#31101,#31102,#31103,#31104,#31105,
#31106,#31107,#31108,#31109,#31110,#31111,#31112,#31113,#31114,#31115,#31116,
#31117,#31118,#31119,#31120,#31121,#31122,#31123,#31124,#31125,#31126,#31127,
#31128,#31129,#31130,#31131,#31132,#31133,#31134,#31135,#31136,#31137,#31138,
#31139,#31140,#31141,#31142,#31143,#31144,#31145,#31146,#31147,#31148,#31149,
#31150,#31151,#31152,#31153,#31154,#31155,#31156,#31157,#31158,#31159,#31160,
#31161,#31162,#31163,#31164,#31165,#31166,#31167,#31168,#31169,#31170,#31171,
#31172),.UNSPECIFIED.,.F.,.F.,(4,3,3,3,3,3,3,3,3,3,3,3,3,3,3,3,3,3,3,3,
3,3,3,3,3,3,3,3,3,3,3,4),(0.,0.0327224959120641,0.0662805079475318,0.100536960576692,
0.133256675995489,0.138569100515552,0.143645901206212,0.1786338686101,0.214080756253453,
0.251134238171856,0.278924349610658,0.285558990870915,0.321777084786821,
0.35776276714434,0.362294683927063,0.39765657796237,0.419708599667403,0.427246149485785,
0.432639276975905,0.468078685886249,0.504737337027106,0.541740932792406,
0.567834431848717,0.579481780097231,0.584481542244862,0.622063712786212,
0.654170015900382,0.6685768440841,0.678363361689231,0.716158260579035,0.750488925242892,
0.768398079192696),.UNSPECIFIED.);
#515=B_SPLINE_CURVE_WITH_KNOTS('',3,(#31173,#31174,#31175,#31176,#31177,
#31178,#31179,#31180,#31181,#31182,#31183,#31184,#31185,#31186,#31187,#31188,
#31189,#31190,#31191,#31192,#31193,#31194,#31195,#31196,#31197,#31198,#31199,
#31200,#31201,#31202,#31203,#31204,#31205,#31206,#31207,#31208,#31209,#31210,
#31211,#31212,#31213,#31214,#31215,#31216,#31217,#31218,#31219,#31220,#31221,
#31222,#31223,#31224,#31225,#31226,#31227,#31228,#31229,#31230,#31231,#31232,
#31233,#31234,#31235,#31236,#31237,#31238,#31239,#31240,#31241,#31242,#31243,
#31244,#31245,#31246,#31247,#31248,#31249,#31250,#31251,#31252,#31253,#31254,
#31255,#31256,#31257,#31258,#31259,#31260,#31261,#31262,#31263,#31264,#31265,
#31266,#31267,#31268,#31269),.UNSPECIFIED.,.F.,.F.,(4,3,3,3,3,3,3,3,3,3,
3,3,3,3,3,3,3,3,3,3,3,3,3,3,3,3,3,3,3,3,3,3,4),(0.,0.0368039914157241,0.0744333613634087,
0.113993751388472,0.148609092660403,0.155429042492168,0.160415347695229,
0.197652346662473,0.234804755786334,0.271449306551343,0.301316100304487,
0.308903884150417,0.314301858425386,0.350380524963378,0.385744397367857,
0.390916481563918,0.427339708424226,0.447829010516186,0.457282926489124,
0.462717600214839,0.499273967924932,0.53507200611566,0.570520286913965,
0.593601318786667,0.601390738323114,0.606406505217338,0.64136634286951,
0.669816892626028,0.683592856456032,0.691680490247784,0.725189664234744,
0.75516854189558,0.770777738583609),.UNSPECIFIED.);
#516=B_SPLINE_CURVE_WITH_KNOTS('',3,(#31270,#31271,#31272,#31273,#31274,
#31275,#31276,#31277,#31278,#31279,#31280,#31281,#31282,#31283,#31284,#31285,
#31286,#31287,#31288,#31289,#31290,#31291,#31292,#31293,#31294,#31295,#31296,
#31297,#31298,#31299,#31300,#31301,#31302,#31303,#31304,#31305,#31306,#31307,
#31308,#31309,#31310,#31311,#31312,#31313,#31314,#31315,#31316,#31317,#31318,
#31319,#31320,#31321,#31322,#31323,#31324,#31325,#31326,#31327,#31328,#31329,
#31330,#31331,#31332,#31333,#31334,#31335,#31336,#31337,#31338,#31339,#31340,
#31341,#31342,#31343,#31344,#31345,#31346,#31347,#31348,#31349,#31350,#31351,
#31352,#31353,#31354,#31355,#31356,#31357,#31358,#31359,#31360,#31361,#31362,
#31363),.UNSPECIFIED.,.F.,.F.,(4,3,3,3,3,3,3,3,3,3,3,3,3,3,3,3,3,3,3,3,
3,3,3,3,3,3,3,3,3,3,3,4),(0.,0.0327225294770781,0.0662805709960721,0.100537044605592,
0.133256749520777,0.138569447222746,0.143645941610917,0.17863392984422,
0.214080826059521,0.251134290526409,0.278924388876575,0.285558992053491,
0.321777087844177,0.357762759284444,0.362294683927074,0.397656563857957,
0.419708586444518,0.427246331524387,0.432639250564409,0.468078638783316,
0.50473728125208,0.541740875145429,0.567834381407617,0.579481572313244,
0.584481227357561,0.622063393148413,0.654169776172043,0.668576667903374,
0.678363394448717,0.71615829260595,0.750488925242933,0.768398079192735),
 .UNSPECIFIED.);
#517=B_SPLINE_CURVE_WITH_KNOTS('',3,(#31364,#31365,#31366,#31367,#31368,
#31369,#31370,#31371,#31372,#31373,#31374,#31375,#31376,#31377,#31378,#31379,
#31380,#31381,#31382,#31383,#31384,#31385,#31386,#31387,#31388,#31389,#31390,
#31391,#31392,#31393,#31394,#31395,#31396,#31397,#31398,#31399,#31400,#31401,
#31402,#31403,#31404,#31405,#31406,#31407,#31408,#31409,#31410,#31411,#31412,
#31413,#31414,#31415,#31416,#31417,#31418,#31419,#31420,#31421,#31422,#31423,
#31424,#31425,#31426,#31427,#31428,#31429,#31430,#31431,#31432,#31433,#31434,
#31435,#31436,#31437,#31438,#31439,#31440,#31441,#31442,#31443,#31444,#31445,
#31446,#31447,#31448,#31449,#31450,#31451,#31452,#31453,#31454,#31455,#31456,
#31457,#31458,#31459,#31460),.UNSPECIFIED.,.F.,.F.,(4,3,3,3,3,3,3,3,3,3,
3,3,3,3,3,3,3,3,3,3,3,3,3,3,3,3,3,3,3,3,3,3,4),(0.,0.0368040169038835,0.0744334020924358,
0.11399378702637,0.148609123843563,0.155429235171562,0.160415535189551,
0.197652537277058,0.234804939176668,0.271449477805488,0.301316228745094,
0.308904321525207,0.31430193792665,0.350380595626898,0.385744458930709,
0.390916481563911,0.427339708170469,0.447829010278287,0.45728292112946,
0.462717598788197,0.499273966676618,0.535072005472898,0.570520283450759,
0.593601315756361,0.601390726866048,0.606406481970154,0.641366318060403,
0.669816874019195,0.683592838382448,0.691680487645043,0.725189651274617,
0.75516854189557,0.770777738583599),.UNSPECIFIED.);
#518=B_SPLINE_CURVE_WITH_KNOTS('',3,(#31462,#31463,#31464,#31465,#31466,
#31467,#31468,#31469,#31470,#31471,#31472),.UNSPECIFIED.,.F.,.F.,(4,1,1,
1,1,1,1,1,4),(15.707963267949,15.8048324359278,16.7912933293328,17.7777542227378,
18.7642151161428,19.7506760095478,20.7371369029528,21.7235977963578,21.9911485751285),
 .UNSPECIFIED.);
#519=B_SPLINE_CURVE_WITH_KNOTS('',3,(#31473,#31474,#31475,#31476,#31477,
#31478,#31479,#31480,#31481,#31482),.UNSPECIFIED.,.F.,.F.,(4,1,1,1,1,1,
1,4),(15.7079632679489,16.3713219137818,17.3577828071869,18.3442437005919,
19.3307045939969,20.3171654874019,21.3036263808069,21.9911485751285),
 .UNSPECIFIED.);
#520=B_SPLINE_CURVE_WITH_KNOTS('',3,(#31707,#31708,#31709,#31710,#31711,
#31712,#31713,#31714,#31715,#31716,#31717,#31718,#31719,#31720,#31721,#31722,
#31723,#31724,#31725,#31726,#31727,#31728,#31729,#31730,#31731,#31732,#31733,
#31734,#31735,#31736,#31737,#31738,#31739,#31740,#31741,#31742,#31743,#31744,
#31745,#31746,#31747,#31748,#31749,#31750,#31751,#31752,#31753,#31754,#31755,
#31756,#31757,#31758,#31759,#31760,#31761,#31762,#31763,#31764,#31765,#31766,
#31767,#31768,#31769,#31770,#31771,#31772,#31773,#31774,#31775,#31776,#31777,
#31778,#31779,#31780,#31781,#31782,#31783,#31784,#31785,#31786,#31787,#31788,
#31789,#31790,#31791,#31792,#31793,#31794,#31795,#31796,#31797,#31798,#31799,
#31800,#31801,#31802,#31803),.UNSPECIFIED.,.F.,.F.,(4,3,3,3,3,3,3,3,3,3,
3,3,3,3,3,3,3,3,3,3,3,3,3,3,3,3,3,3,3,3,3,3,4),(0.,0.0368040006584821,0.0744333761311954,
0.113993764310286,0.14860910396699,0.155429112383965,0.160415415803185,
0.19765241590165,0.234804822404722,0.27144936877189,0.301316146969897,0.308904043046986,
0.314301887301155,0.350380550636825,0.385744419741531,0.39091648156392,
0.427339708332513,0.447829010430206,0.45728292453119,0.462717599696291,
0.499273967471206,0.535072005882051,0.570520285658179,0.593601317687859,
0.601390734201157,0.60640649698701,0.641366334082055,0.669816886035445,
0.683592850009941,0.691680489272535,0.725189659504915,0.755168541895614,
0.770777738583643),.UNSPECIFIED.);
#521=B_SPLINE_CURVE_WITH_KNOTS('',3,(#31804,#31805,#31806,#31807,#31808,
#31809,#31810,#31811,#31812,#31813,#31814,#31815,#31816,#31817,#31818,#31819,
#31820,#31821,#31822,#31823,#31824,#31825,#31826,#31827,#31828),
 .UNSPECIFIED.,.F.,.F.,(4,3,3,3,3,3,3,3,4),(-10.1321597128207,-9.86460893405003,
-8.87814804064502,-7.89168714724002,-6.90522625383502,-5.91876536043002,
-4.93230446702501,-3.94584357362001,-3.84897440564114),.UNSPECIFIED.);
#522=B_SPLINE_CURVE_WITH_KNOTS('',3,(#32053,#32054,#32055,#32056,#32057,
#32058,#32059,#32060,#32061,#32062,#32063,#32064,#32065,#32066,#32067,#32068,
#32069,#32070,#32071,#32072,#32073,#32074,#32075,#32076,#32077,#32078,#32079,
#32080,#32081,#32082,#32083,#32084,#32085,#32086,#32087,#32088,#32089,#32090,
#32091,#32092,#32093,#32094,#32095,#32096,#32097,#32098,#32099,#32100,#32101,
#32102,#32103,#32104,#32105,#32106,#32107,#32108,#32109,#32110,#32111,#32112,
#32113,#32114,#32115,#32116,#32117,#32118,#32119,#32120,#32121,#32122,#32123,
#32124,#32125,#32126,#32127,#32128,#32129,#32130,#32131,#32132,#32133,#32134,
#32135,#32136,#32137,#32138,#32139,#32140,#32141,#32142,#32143,#32144,#32145,
#32146),.UNSPECIFIED.,.F.,.F.,(4,3,3,3,3,3,3,3,3,3,3,3,3,3,3,3,3,3,3,3,
3,3,3,3,3,3,3,3,3,3,3,4),(0.,0.0327224852298601,0.0662804878799529,0.100536933829056,
0.133256652591307,0.138568990289855,0.143645888367285,0.178633849142766,
0.214080734056413,0.251134221524075,0.278924337124821,0.285558990484342,
0.321777083808023,0.357762769641534,0.362294683927059,0.397656582449134,
0.419708603873742,0.427246091593913,0.432639285230977,0.468078700718258,
0.504737354615871,0.541740950976496,0.567834447759792,0.579481845655055,
0.584481641657808,0.62206381370368,0.654170091588477,0.668576899729838,
0.678363351333556,0.716158250454694,0.750488925242868,0.768398079192674),
 .UNSPECIFIED.);
#523=B_SPLINE_CURVE_WITH_KNOTS('',3,(#32147,#32148,#32149,#32150,#32151,
#32152,#32153,#32154,#32155,#32156,#32157,#32158,#32159,#32160,#32161,#32162,
#32163,#32164,#32165,#32166,#32167,#32168,#32169,#32170,#32171),
 .UNSPECIFIED.,.F.,.F.,(4,3,3,3,3,3,3,3,4),(7.59274844815667,7.89168714724002,
8.87814804064502,9.86460893405003,10.851069827455,11.83753072086,12.823991614265,
13.81045250767,13.8759337553363),.UNSPECIFIED.);
#524=B_SPLINE_CURVE_WITH_KNOTS('',3,(#32173,#32174,#32175,#32176,#32177,
#32178,#32179,#32180,#32181,#32182,#32183),.UNSPECIFIED.,.F.,.F.,(4,1,1,
1,1,1,1,1,4),(15.707963267949,15.8048324359278,16.7912933293328,17.7777542227378,
18.7642151161428,19.7506760095478,20.7371369029528,21.7235977963578,21.9911485751285),
 .UNSPECIFIED.);
#525=B_SPLINE_CURVE_WITH_KNOTS('',3,(#32184,#32185,#32186,#32187,#32188,
#32189,#32190,#32191,#32192,#32193),.UNSPECIFIED.,.F.,.F.,(4,1,1,1,1,1,
1,4),(15.7079632679489,16.3713219137818,17.3577828071868,18.3442437005918,
19.3307045939968,20.3171654874019,21.3036263808069,21.9911485751285),
 .UNSPECIFIED.);
#526=B_SPLINE_CURVE_WITH_KNOTS('',3,(#32418,#32419,#32420,#32421,#32422,
#32423,#32424,#32425,#32426,#32427,#32428,#32429,#32430,#32431,#32432,#32433,
#32434,#32435,#32436,#32437,#32438,#32439,#32440,#32441,#32442,#32443,#32444,
#32445,#32446,#32447,#32448,#32449,#32450,#32451,#32452,#32453,#32454,#32455,
#32456,#32457,#32458,#32459,#32460,#32461,#32462,#32463,#32464,#32465,#32466,
#32467,#32468,#32469,#32470,#32471,#32472,#32473,#32474,#32475,#32476,#32477,
#32478,#32479,#32480,#32481,#32482,#32483,#32484,#32485,#32486,#32487,#32488,
#32489,#32490,#32491,#32492,#32493,#32494,#32495,#32496,#32497,#32498,#32499,
#32500,#32501,#32502,#32503,#32504,#32505,#32506,#32507,#32508,#32509,#32510,
#32511,#32512,#32513,#32514),.UNSPECIFIED.,.F.,.F.,(4,3,3,3,3,3,3,3,3,3,
3,3,3,3,3,3,3,3,3,3,3,3,3,3,3,3,3,3,3,3,3,3,4),(0.,0.0368039760561726,0.0744333368184212,
0.113993729911609,0.148609073868149,0.155428926386467,0.160415234743925,
0.197652231831378,0.234804645306633,0.271449203389433,0.301316022933056,
0.308903620706599,0.314301810562592,0.350380482429235,0.385744360315095,
0.390916481563925,0.427339708572203,0.447829010654916,0.457282929707203,
0.462717601073039,0.49927396867586,0.535072006502099,0.570520288994985,
0.593601320607563,0.601390745293023,0.606406519246091,0.641366357839995,
0.669816903853899,0.683592867357584,0.691680491796103,0.725189672020684,
0.755168541895609,0.770777738583641),.UNSPECIFIED.);
#527=B_SPLINE_CURVE_WITH_KNOTS('',3,(#32515,#32516,#32517,#32518,#32519,
#32520,#32521,#32522,#32523,#32524,#32525,#32526,#32527,#32528,#32529,#32530,
#32531,#32532,#32533,#32534,#32535,#32536,#32537,#32538,#32539),
 .UNSPECIFIED.,.F.,.F.,(4,3,3,3,3,3,3,3,4),(-10.1321597128207,-9.86460893405003,
-8.87814804064502,-7.89168714724003,-6.90522625383502,-5.91876536043002,
-4.93230446702502,-3.94584357362001,-3.84897440564115),.UNSPECIFIED.);
#528=B_SPLINE_CURVE_WITH_KNOTS('',3,(#32764,#32765,#32766,#32767,#32768,
#32769,#32770,#32771,#32772,#32773,#32774,#32775,#32776,#32777,#32778,#32779,
#32780,#32781,#32782,#32783,#32784,#32785,#32786,#32787,#32788,#32789,#32790,
#32791,#32792,#32793,#32794,#32795,#32796,#32797,#32798,#32799,#32800,#32801,
#32802,#32803,#32804,#32805,#32806,#32807,#32808,#32809,#32810,#32811,#32812,
#32813,#32814,#32815,#32816,#32817,#32818,#32819,#32820,#32821,#32822,#32823,
#32824,#32825,#32826,#32827,#32828,#32829,#32830,#32831,#32832,#32833,#32834,
#32835,#32836,#32837,#32838,#32839,#32840,#32841,#32842,#32843,#32844,#32845,
#32846,#32847,#32848,#32849,#32850,#32851,#32852,#32853,#32854,#32855,#32856,
#32857),.UNSPECIFIED.,.F.,.F.,(4,3,3,3,3,3,3,3,3,3,3,3,3,3,3,3,3,3,3,3,
3,3,3,3,3,3,3,3,3,3,3,4),(0.,0.0327225799773267,0.0662806658545984,0.100537171029244,
0.133256860141472,0.138569969050608,0.143646002487887,0.178634022059388,
0.214080931165366,0.251134369355791,0.27892444799861,0.285558993885552,
0.321777092476967,0.357762747477908,0.362294683927068,0.397656542631737,
0.419708566544936,0.427246605750548,0.432639210952107,0.468078568034648,
0.504737197455354,0.541740788532467,0.567834305621274,0.579481260120421,
0.584480754431237,0.622062913075079,0.654169416117039,0.668576403279121,
0.678363443657298,0.716158340709877,0.750488925242921,0.768398079192729),
 .UNSPECIFIED.);
#529=B_SPLINE_CURVE_WITH_KNOTS('',3,(#32858,#32859,#32860,#32861,#32862,
#32863,#32864,#32865,#32866,#32867,#32868,#32869,#32870,#32871,#32872,#32873,
#32874,#32875,#32876,#32877,#32878,#32879,#32880,#32881,#32882),
 .UNSPECIFIED.,.F.,.F.,(4,3,3,3,3,3,3,3,4),(7.59274844815668,7.89168714724002,
8.87814804064503,9.86460893405003,10.851069827455,11.83753072086,12.823991614265,
13.81045250767,13.8759337553363),.UNSPECIFIED.);
#530=B_SPLINE_CURVE_WITH_KNOTS('',3,(#32884,#32885,#32886,#32887,#32888,
#32889,#32890,#32891,#32892,#32893,#32894),.UNSPECIFIED.,.F.,.F.,(4,1,1,
1,1,1,1,1,4),(15.7079632679489,15.8048324359278,16.7912933293328,17.7777542227378,
18.7642151161428,19.7506760095478,20.7371369029528,21.7235977963578,21.9911485751285),
 .UNSPECIFIED.);
#531=B_SPLINE_CURVE_WITH_KNOTS('',3,(#32895,#32896,#32897,#32898,#32899,
#32900,#32901,#32902,#32903,#32904),.UNSPECIFIED.,.F.,.F.,(4,1,1,1,1,1,
1,4),(15.7079632679489,16.3713219137818,17.3577828071869,18.3442437005919,
19.3307045939969,20.3171654874019,21.3036263808069,21.9911485751285),
 .UNSPECIFIED.);
#532=B_SPLINE_CURVE_WITH_KNOTS('',3,(#33129,#33130,#33131,#33132,#33133,
#33134,#33135,#33136,#33137,#33138,#33139,#33140,#33141,#33142,#33143,#33144,
#33145,#33146,#33147,#33148,#33149,#33150,#33151,#33152,#33153,#33154,#33155,
#33156,#33157,#33158,#33159,#33160,#33161,#33162,#33163,#33164,#33165,#33166,
#33167,#33168,#33169,#33170,#33171,#33172,#33173,#33174,#33175,#33176,#33177,
#33178,#33179,#33180,#33181,#33182,#33183,#33184,#33185,#33186,#33187,#33188,
#33189,#33190,#33191,#33192,#33193,#33194,#33195,#33196,#33197,#33198,#33199,
#33200,#33201,#33202,#33203,#33204,#33205,#33206,#33207,#33208,#33209,#33210,
#33211,#33212,#33213,#33214,#33215,#33216,#33217,#33218,#33219,#33220,#33221,
#33222,#33223,#33224,#33225),.UNSPECIFIED.,.F.,.F.,(4,3,3,3,3,3,3,3,3,3,
3,3,3,3,3,3,3,3,3,3,3,3,3,3,3,3,3,3,3,3,3,3,4),(0.,0.0368040296983295,0.0744334225357169,
0.113993804914242,0.148609139495452,0.155429331856321,0.160415629309949,
0.19765263296232,0.234805031233744,0.271449563770314,0.301316293218716,
0.308904541097941,0.314301977856807,0.350380631124549,0.385744489860858,
0.39091648156392,0.427339708037647,0.447829010153769,0.457282918385807,
0.462717598065727,0.499273966044462,0.535072005142963,0.570520281705417,
0.593601314229191,0.601390721049491,0.606406470197016,0.641366305496701,
0.669816864596427,0.6835928292529,0.691680486306265,0.725189644734797,0.755168541895606,
0.770777738583634),.UNSPECIFIED.);
#533=B_SPLINE_CURVE_WITH_KNOTS('',3,(#33226,#33227,#33228,#33229,#33230,
#33231,#33232,#33233,#33234,#33235,#33236,#33237,#33238,#33239,#33240,#33241,
#33242,#33243,#33244,#33245,#33246,#33247,#33248,#33249,#33250),
 .UNSPECIFIED.,.F.,.F.,(4,3,3,3,3,3,3,3,4),(-10.1321597128207,-9.86460893405003,
-8.87814804064502,-7.89168714724002,-6.90522625383502,-5.91876536043002,
-4.93230446702502,-3.94584357362001,-3.84897440564114),.UNSPECIFIED.);
#534=B_SPLINE_CURVE_WITH_KNOTS('',3,(#33475,#33476,#33477,#33478,#33479,
#33480,#33481,#33482,#33483,#33484,#33485,#33486,#33487,#33488,#33489,#33490,
#33491,#33492,#33493,#33494,#33495,#33496,#33497,#33498,#33499,#33500,#33501,
#33502,#33503,#33504,#33505,#33506,#33507,#33508,#33509,#33510,#33511,#33512,
#33513,#33514,#33515,#33516,#33517,#33518,#33519,#33520,#33521,#33522,#33523,
#33524,#33525,#33526,#33527,#33528,#33529,#33530,#33531,#33532,#33533,#33534,
#33535,#33536,#33537,#33538,#33539,#33540,#33541,#33542,#33543,#33544,#33545,
#33546,#33547,#33548,#33549,#33550,#33551,#33552,#33553,#33554,#33555,#33556,
#33557,#33558,#33559,#33560,#33561,#33562,#33563,#33564,#33565,#33566,#33567,
#33568),.UNSPECIFIED.,.F.,.F.,(4,3,3,3,3,3,3,3,3,3,3,3,3,3,3,3,3,3,3,3,
3,3,3,3,3,3,3,3,3,3,3,4),(0.,0.0327225146876364,0.0662805432171355,0.10053700758566,
0.133256717128334,0.138569294358745,0.143645923792125,0.178633902850418,
0.21408079528951,0.251134267448895,0.278924371568434,0.28555899152832,0.321777086502174,
0.357762762756158,0.36229468392705,0.397656570072467,0.419708592270616,
0.427246251204994,0.432639262274467,0.468078659615991,0.504737305906693,
0.541740900625277,0.567834403702473,0.579481664146009,0.584481366534682,
0.622063534445468,0.654169882144813,0.668576745773135,0.678363380045444,
0.716158278526066,0.750488925242846,0.768398079192654),.UNSPECIFIED.);
#535=B_SPLINE_CURVE_WITH_KNOTS('',3,(#33569,#33570,#33571,#33572,#33573,
#33574,#33575,#33576,#33577,#33578,#33579,#33580,#33581,#33582,#33583,#33584,
#33585,#33586,#33587,#33588,#33589,#33590,#33591,#33592,#33593),
 .UNSPECIFIED.,.F.,.F.,(4,3,3,3,3,3,3,3,4),(7.59274844815667,7.89168714724002,
8.87814804064502,9.86460893405002,10.851069827455,11.83753072086,12.823991614265,
13.81045250767,13.8759337553363),.UNSPECIFIED.);
#536=B_SPLINE_CURVE_WITH_KNOTS('',3,(#33621,#33622,#33623,#33624,#33625,
#33626,#33627,#33628,#33629,#33630),.UNSPECIFIED.,.F.,.F.,(4,3,3,4),(-4.09293042013064,
-3.99338989784634,-2.99504242338475,-2.06863817490912),.UNSPECIFIED.);
#537=B_SPLINE_CURVE_WITH_KNOTS('',3,(#33633,#33634,#33635,#33636,#33637,
#33638,#33639),.UNSPECIFIED.,.F.,.F.,(4,3,4),(0.,0.998805711569778,1.11730040836826),
 .UNSPECIFIED.);
#538=B_SPLINE_CURVE_WITH_KNOTS('',3,(#33644,#33645,#33646,#33647,#33648,
#33649,#33650,#33651,#33652,#33653,#33654,#33655,#33656,#33657,#33658,#33659,
#33660,#33661,#33662,#33663,#33664,#33665),.UNSPECIFIED.,.F.,.F.,(4,3,3,
3,3,3,3,4),(-10.3761157273102,-9.98347474461585,-8.98512727015427,-7.98677979569268,
-6.98843232123109,-5.99008484676951,-4.99173737230793,-4.09293042013064),
 .UNSPECIFIED.);
#539=B_SPLINE_CURVE_WITH_KNOTS('',3,(#33666,#33667,#33668,#33669,#33670,
#33671,#33672,#33673,#33674,#33675,#33676,#33677,#33678,#33679,#33680,#33681,
#33682,#33683,#33684,#33685,#33686,#33687),.UNSPECIFIED.,.F.,.F.,(4,3,3,
3,3,3,3,4),(1.11730040836826,1.99761142313956,2.99641713470934,3.99522284627912,
4.99402855784889,5.99283426941867,6.99163998098846,7.40048571554784),
 .UNSPECIFIED.);
#540=B_SPLINE_CURVE_WITH_KNOTS('',3,(#33692,#33693,#33694,#33695,#33696,
#33697,#33698,#33699,#33700,#33701,#33702,#33703,#33704,#33705,#33706,#33707,
#33708,#33709,#33710,#33711,#33712,#33713),.UNSPECIFIED.,.F.,.F.,(4,3,3,
3,3,3,3,4),(-16.6593010344898,-15.9735595913854,-14.9752121169238,-13.9768646424622,
-12.9785171680006,-11.980169693539,-10.9818222190774,-10.3761157273102),
 .UNSPECIFIED.);
#541=B_SPLINE_CURVE_WITH_KNOTS('',3,(#33714,#33715,#33716,#33717,#33718,
#33719,#33720,#33721,#33722,#33723,#33724,#33725,#33726,#33727,#33728,#33729,
#33730,#33731,#33732,#33733,#33734,#33735),.UNSPECIFIED.,.F.,.F.,(4,3,3,
3,3,3,3,4),(7.40048571554784,7.99044569255823,8.989251404128,9.98805711569777,
10.9868628272675,11.9856685388373,12.9844742504071,13.6836710227274),
 .UNSPECIFIED.);
#542=B_SPLINE_CURVE_WITH_KNOTS('',3,(#33740,#33741,#33742,#33743,#33744,
#33745,#33746,#33747,#33748,#33749,#33750,#33751,#33752,#33753,#33754,#33755,
#33756,#33757,#33758,#33759,#33760,#33761),.UNSPECIFIED.,.F.,.F.,(4,3,3,
3,3,3,3,4),(-22.9424863416694,-21.9636444381549,-20.9652969636933,-19.9669494892317,
-18.9686020147701,-17.9702545403085,-16.9719070658469,-16.6593010344898),
 .UNSPECIFIED.);
#543=B_SPLINE_CURVE_WITH_KNOTS('',3,(#33762,#33763,#33764,#33765,#33766,
#33767,#33768,#33769,#33770,#33771,#33772,#33773,#33774,#33775,#33776,#33777,
#33778,#33779,#33780,#33781,#33782,#33783),.UNSPECIFIED.,.F.,.F.,(4,3,3,
3,3,3,3,4),(13.6836710227274,13.9832799619769,14.9820856735466,15.9808913851164,
16.9796970966862,17.978502808256,18.9773085198257,19.966856329907),
 .UNSPECIFIED.);
#544=B_SPLINE_CURVE_WITH_KNOTS('',3,(#33788,#33789,#33790,#33791,#33792,
#33793,#33794,#33795,#33796,#33797,#33798,#33799,#33800,#33801,#33802,#33803,
#33804,#33805,#33806,#33807,#33808,#33809,#33810,#33811,#33812),
 .UNSPECIFIED.,.F.,.F.,(4,3,3,3,3,3,3,3,4),(-29.225671648849,-28.952076759386,
-27.9537292849244,-26.9553818104628,-25.9570343360012,-24.9586868615396,
-23.960339387078,-22.9619919126165,-22.9424863416694),.UNSPECIFIED.);
#545=B_SPLINE_CURVE_WITH_KNOTS('',3,(#33813,#33814,#33815,#33816,#33817,
#33818,#33819,#33820,#33821,#33822,#33823,#33824,#33825,#33826,#33827,#33828,
#33829,#33830,#33831,#33832,#33833,#33834,#33835,#33836,#33837),
 .UNSPECIFIED.,.F.,.F.,(4,3,3,3,3,3,3,3,4),(19.966856329907,19.9761142313955,
20.9749199429653,21.9737256545351,22.9725313661048,23.9713370776746,24.9701427892444,
25.9689485008142,26.2500416370866),.UNSPECIFIED.);
#546=B_SPLINE_CURVE_WITH_KNOTS('',3,(#33842,#33843,#33844,#33845,#33846,
#33847,#33848,#33849,#33850,#33851,#33852,#33853,#33854,#33855,#33856,#33857,
#33858,#33859,#33860,#33861,#33862,#33863),.UNSPECIFIED.,.F.,.F.,(4,3,3,
3,3,3,3,4),(-35.5088569560286,-34.9421616061555,-33.9438141316939,-32.9454666572323,
-31.9471191827707,-30.9487717083091,-29.9504242338475,-29.225671648849),
 .UNSPECIFIED.);
#547=B_SPLINE_CURVE_WITH_KNOTS('',3,(#33864,#33865,#33866,#33867,#33868,
#33869,#33870,#33871,#33872,#33873,#33874,#33875,#33876,#33877,#33878,#33879,
#33880,#33881,#33882,#33883,#33884,#33885),.UNSPECIFIED.,.F.,.F.,(4,3,3,
3,3,3,3,4),(26.2500416370866,26.9677542123839,27.9665599239537,28.9653656355235,
29.9641713470933,30.9629770586631,31.9617827702328,32.5332269442662),
 .UNSPECIFIED.);
#548=B_SPLINE_CURVE_WITH_KNOTS('',3,(#33890,#33891,#33892,#33893,#33894,
#33895,#33896,#33897,#33898,#33899,#33900,#33901,#33902,#33903,#33904,#33905,
#33906,#33907,#33908,#33909,#33910,#33911),.UNSPECIFIED.,.F.,.F.,(4,3,3,
3,3,3,3,4),(-41.7920422632082,-40.932246452925,-39.9338989784634,-38.9355515040018,
-37.9372040295402,-36.9388565550787,-35.9405090806171,-35.5088569560286),
 .UNSPECIFIED.);
#549=B_SPLINE_CURVE_WITH_KNOTS('',3,(#33912,#33913,#33914,#33915,#33916,
#33917,#33918,#33919,#33920,#33921,#33922,#33923,#33924,#33925,#33926,#33927,
#33928,#33929,#33930,#33931,#33932,#33933),.UNSPECIFIED.,.F.,.F.,(4,3,3,
3,3,3,3,4),(32.5332269442662,32.9605884818026,33.9593941933724,34.9581999049422,
35.9570056165119,36.9558113280817,37.9546170396515,38.8164122514458),
 .UNSPECIFIED.);
#550=B_SPLINE_CURVE_WITH_KNOTS('',3,(#33938,#33939,#33940,#33941,#33942,
#33943,#33944,#33945,#33946,#33947,#33948,#33949,#33950,#33951,#33952,#33953,
#33954,#33955,#33956,#33957,#33958,#33959,#33960,#33961,#33962),
 .UNSPECIFIED.,.F.,.F.,(4,3,3,3,3,3,3,3,4),(-48.0752275703878,-47.9206787741561,
-46.9223312996945,-45.9239838252329,-44.9256363507713,-43.9272888763097,
-42.9289414018482,-41.9305939273866,-41.7920422632082),.UNSPECIFIED.);
#551=B_SPLINE_CURVE_WITH_KNOTS('',3,(#33963,#33964,#33965,#33966,#33967,
#33968,#33969,#33970,#33971,#33972,#33973,#33974,#33975,#33976,#33977,#33978,
#33979,#33980,#33981,#33982,#33983,#33984,#33985,#33986,#33987),
 .UNSPECIFIED.,.F.,.F.,(4,3,3,3,3,3,3,3,4),(38.8164122514458,38.9534227512213,
39.952228462791,40.9510341743608,41.9498398859306,42.9486455975004,43.9474513090701,
44.9462570206399,45.0995975586254),.UNSPECIFIED.);
#552=B_SPLINE_CURVE_WITH_KNOTS('',3,(#33992,#33993,#33994,#33995,#33996,
#33997,#33998,#33999,#34000,#34001,#34002,#34003,#34004,#34005,#34006,#34007,
#34008,#34009,#34010,#34011,#34012,#34013),.UNSPECIFIED.,.F.,.F.,(4,3,3,
3,3,3,3,4),(-54.3584128775673,-53.9107636209256,-52.912416146464,-51.9140686720024,
-50.9157211975408,-49.9173737230793,-48.9190262486177,-48.0752275703878),
 .UNSPECIFIED.);
#553=B_SPLINE_CURVE_WITH_KNOTS('',3,(#34014,#34015,#34016,#34017,#34018,
#34019,#34020,#34021,#34022,#34023,#34024,#34025,#34026,#34027,#34028,#34029,
#34030,#34031,#34032,#34033,#34034,#34035),.UNSPECIFIED.,.F.,.F.,(4,3,3,
3,3,3,3,4),(45.0995975586254,45.9450627322097,46.9438684437795,47.9426741553493,
48.941479866919,49.9402855784888,50.9390912900586,51.382782865805),
 .UNSPECIFIED.);
#554=B_SPLINE_CURVE_WITH_KNOTS('',3,(#34040,#34041,#34042,#34043,#34044,
#34045,#34046,#34047,#34048,#34049,#34050,#34051,#34052,#34053,#34054,#34055,
#34056,#34057,#34058,#34059,#34060,#34061),.UNSPECIFIED.,.F.,.F.,(4,3,3,
3,3,3,3,4),(-60.6415981847469,-59.9008484676951,-58.9025009932335,-57.9041535187719,
-56.9058060443103,-55.9074585698488,-54.9091110953872,-54.3584128775673),
 .UNSPECIFIED.);
#555=B_SPLINE_CURVE_WITH_KNOTS('',3,(#34062,#34063,#34064,#34065,#34066,
#34067,#34068,#34069,#34070,#34071,#34072,#34073,#34074,#34075,#34076,#34077,
#34078,#34079,#34080,#34081,#34082,#34083),.UNSPECIFIED.,.F.,.F.,(4,3,3,
3,3,3,3,4),(51.382782865805,51.9378970016283,52.9367027131981,53.9355084247679,
54.9343141363377,55.9331198479074,56.9319255594772,57.6659681729846),
 .UNSPECIFIED.);
#556=B_SPLINE_CURVE_WITH_KNOTS('',3,(#34088,#34089,#34090,#34091,#34092,
#34093,#34094,#34095,#34096,#34097,#34098,#34099,#34100,#34101,#34102,#34103,
#34104,#34105,#34106,#34107,#34108,#34109,#34110,#34111,#34112),
 .UNSPECIFIED.,.F.,.F.,(4,3,3,3,3,3,3,3,4),(-66.9247834919265,-66.8892807889262,
-65.8909333144646,-64.892585840003,-63.8942383655414,-62.8958908910799,
-61.8975434166182,-60.8991959421567,-60.6415981847469),.UNSPECIFIED.);
#557=B_SPLINE_CURVE_WITH_KNOTS('',3,(#34113,#34114,#34115,#34116,#34117,
#34118,#34119,#34120,#34121,#34122,#34123,#34124,#34125,#34126,#34127,#34128,
#34129,#34130,#34131,#34132,#34133,#34134,#34135,#34136,#34137),
 .UNSPECIFIED.,.F.,.F.,(4,3,3,3,3,3,3,3,4),(57.6659681729846,57.930731271047,
58.9295369826168,59.9283426941866,60.9271484057563,61.9259541173261,62.9247598288959,
63.9235655404657,63.9491534801642),.UNSPECIFIED.);
#558=B_SPLINE_CURVE_WITH_KNOTS('',3,(#34142,#34143,#34144,#34145,#34146,
#34147,#34148,#34149,#34150,#34151,#34152,#34153,#34154,#34155,#34156,#34157,
#34158,#34159,#34160,#34161,#34162,#34163),.UNSPECIFIED.,.F.,.F.,(4,3,3,
3,3,3,3,4),(-73.2079687991061,-72.8793656356957,-71.8810181612341,-70.8826706867726,
-69.8843232123109,-68.8859757378494,-67.8876282633878,-66.9247834919265),
 .UNSPECIFIED.);
#559=B_SPLINE_CURVE_WITH_KNOTS('',3,(#34164,#34165,#34166,#34167,#34168,
#34169,#34170,#34171,#34172,#34173,#34174,#34175,#34176,#34177,#34178,#34179,
#34180,#34181,#34182,#34183,#34184,#34185),.UNSPECIFIED.,.F.,.F.,(4,3,3,
3,3,3,3,4),(63.9491534801642,64.9223712520354,65.9211769636052,66.919982675175,
67.9187883867447,68.9175940983145,69.9163998098843,70.2323387873437),
 .UNSPECIFIED.);
#560=B_SPLINE_CURVE_WITH_KNOTS('',3,(#34190,#34191,#34192,#34193,#34194,
#34195,#34196,#34197,#34198,#34199,#34200,#34201,#34202,#34203,#34204,#34205,
#34206,#34207,#34208,#34209,#34210,#34211),.UNSPECIFIED.,.F.,.F.,(4,3,3,
3,3,3,3,4),(-79.4911541062857,-78.8694504824652,-77.8711030080036,-76.8727555335421,
-75.8744080590805,-74.8760605846189,-73.8777131101573,-73.2079687991061),
 .UNSPECIFIED.);
#561=B_SPLINE_CURVE_WITH_KNOTS('',3,(#34212,#34213,#34214,#34215,#34216,
#34217,#34218,#34219,#34220,#34221,#34222,#34223,#34224,#34225,#34226,#34227,
#34228,#34229,#34230,#34231,#34232,#34233),.UNSPECIFIED.,.F.,.F.,(4,3,3,
3,3,3,3,4),(70.2323387873437,70.9152055214541,71.9140112330238,72.9128169445936,
73.9116226561634,74.9104283677332,75.909234079303,76.5155240945233),
 .UNSPECIFIED.);
#562=B_SPLINE_CURVE_WITH_KNOTS('',3,(#34238,#34239,#34240,#34241,#34242,
#34243,#34244,#34245,#34246,#34247,#34248,#34249,#34250,#34251,#34252,#34253,
#34254,#34255,#34256,#34257,#34258,#34259),.UNSPECIFIED.,.F.,.F.,(4,3,3,
3,3,3,3,4),(-85.7743394134653,-84.8595353292348,-83.8611878547731,-82.8628403803116,
-81.86449290585,-80.8661454313884,-79.8677979569268,-79.4911541062857),
 .UNSPECIFIED.);
#563=B_SPLINE_CURVE_WITH_KNOTS('',3,(#34260,#34261,#34262,#34263,#34264,
#34265,#34266,#34267,#34268,#34269,#34270,#34271,#34272,#34273,#34274,#34275,
#34276,#34277,#34278,#34279,#34280,#34281),.UNSPECIFIED.,.F.,.F.,(4,3,3,
3,3,3,3,4),(76.5155240945233,76.9080397908727,77.9068455024425,78.9056512140123,
79.9044569255821,80.9032626371518,81.9020683487216,82.7987094017029),
 .UNSPECIFIED.);
#564=B_SPLINE_CURVE_WITH_KNOTS('',3,(#34286,#34287,#34288,#34289,#34290,
#34291,#34292,#34293,#34294,#34295,#34296,#34297,#34298,#34299,#34300,#34301,
#34302,#34303,#34304,#34305,#34306,#34307,#34308,#34309,#34310),
 .UNSPECIFIED.,.F.,.F.,(4,3,3,3,3,3,3,3,4),(-92.0575247206449,-91.8479676504658,
-90.8496201760042,-89.8512727015427,-88.8529252270811,-87.8545777526195,
-86.8562302781579,-85.8578828036963,-85.7743394134653),.UNSPECIFIED.);
#565=B_SPLINE_CURVE_WITH_KNOTS('',3,(#34311,#34312,#34313,#34314,#34315,
#34316,#34317,#34318,#34319,#34320,#34321,#34322,#34323,#34324,#34325,#34326,
#34327,#34328,#34329,#34330,#34331,#34332,#34333,#34334,#34335),
 .UNSPECIFIED.,.F.,.F.,(4,3,3,3,3,3,3,3,4),(82.7987094017029,82.9008740602914,
83.8996797718612,84.8984854834309,85.8972911950007,86.8960969065705,87.8949026181403,
88.8937083297101,89.0818947088825),.UNSPECIFIED.);
#566=B_SPLINE_CURVE_WITH_KNOTS('',3,(#34340,#34341,#34342,#34343,#34344,
#34345,#34346,#34347,#34348,#34349,#34350,#34351,#34352,#34353,#34354,#34355,
#34356,#34357,#34358,#34359,#34360,#34361),.UNSPECIFIED.,.F.,.F.,(4,3,3,
3,3,3,3,4),(-98.3407100278245,-97.8380524972353,-96.8397050227737,-95.8413575483122,
-94.8430100738506,-93.844662599389,-92.8463151249274,-92.0575247206449),
 .UNSPECIFIED.);
#567=B_SPLINE_CURVE_WITH_KNOTS('',3,(#34362,#34363,#34364,#34365,#34366,
#34367,#34368,#34369,#34370,#34371,#34372,#34373,#34374,#34375,#34376,#34377,
#34378,#34379,#34380,#34381,#34382,#34383),.UNSPECIFIED.,.F.,.F.,(4,3,3,
3,3,3,3,4),(89.0818947088825,89.8925140412798,90.8913197528496,91.8901254644194,
92.8889311759891,93.8877368875589,94.8865425991287,95.3650800160621),
 .UNSPECIFIED.);
#568=B_SPLINE_CURVE_WITH_KNOTS('',3,(#34388,#34389,#34390,#34391,#34392,
#34393,#34394,#34395,#34396,#34397,#34398,#34399,#34400,#34401,#34402,#34403,
#34404,#34405,#34406,#34407,#34408,#34409),.UNSPECIFIED.,.F.,.F.,(4,3,3,
3,3,3,3,4),(-104.623895335004,-103.828137344005,-102.829789869543,-101.831442395082,
-100.83309492062,-99.8347474461585,-98.8363999716969,-98.3407100278245),
 .UNSPECIFIED.);
#569=B_SPLINE_CURVE_WITH_KNOTS('',3,(#34410,#34411,#34412,#34413,#34414,
#34415,#34416,#34417,#34418,#34419,#34420,#34421,#34422,#34423,#34424,#34425,
#34426,#34427,#34428,#34429,#34430,#34431),.UNSPECIFIED.,.F.,.F.,(4,3,3,
3,3,3,3,4),(95.3650800160621,95.8853483106984,96.8841540222682,97.882959733838,
98.8817654454078,99.8805711569776,100.879376868547,101.648265323242),
 .UNSPECIFIED.);
#570=B_SPLINE_CURVE_WITH_KNOTS('',3,(#34436,#34437,#34438,#34439,#34440,
#34441,#34442,#34443,#34444,#34445,#34446,#34447,#34448,#34449,#34450,#34451,
#34452,#34453,#34454,#34455,#34456,#34457,#34458,#34459,#34460),
 .UNSPECIFIED.,.F.,.F.,(4,3,3,3,3,3,3,3,4),(-110.907080642184,-110.816569665236,
-109.818222190774,-108.819874716313,-107.821527241851,-106.82317976739,
-105.824832292928,-104.826484818466,-104.623895335004),.UNSPECIFIED.);
#571=B_SPLINE_CURVE_WITH_KNOTS('',3,(#34461,#34462,#34463,#34464,#34465,
#34466,#34467,#34468,#34469,#34470,#34471,#34472,#34473,#34474,#34475,#34476,
#34477,#34478,#34479,#34480,#34481,#34482,#34483,#34484,#34485),
 .UNSPECIFIED.,.F.,.F.,(4,3,3,3,3,3,3,3,4),(101.648265323242,101.878182580117,
102.876988291687,103.875794003257,104.874599714826,105.873405426396,106.872211137966,
107.871016849536,107.931450630421),.UNSPECIFIED.);
#572=B_SPLINE_CURVE_WITH_KNOTS('',3,(#34490,#34491,#34492,#34493,#34494,
#34495,#34496,#34497,#34498,#34499,#34500,#34501,#34502,#34503,#34504,#34505,
#34506,#34507,#34508,#34509,#34510,#34511),.UNSPECIFIED.,.F.,.F.,(4,3,3,
3,3,3,3,4),(-117.190265949363,-116.806654512005,-115.808307037544,-114.809959563082,
-113.811612088621,-112.813264614159,-111.814917139698,-110.907080642184),
 .UNSPECIFIED.);
#573=B_SPLINE_CURVE_WITH_KNOTS('',3,(#34512,#34513,#34514,#34515,#34516,
#34517,#34518,#34519,#34520,#34521,#34522,#34523,#34524,#34525,#34526,#34527,
#34528,#34529,#34530,#34531,#34532,#34533),.UNSPECIFIED.,.F.,.F.,(4,3,3,
3,3,3,3,4),(107.931450630421,108.869822561106,109.868628272675,110.867433984245,
111.866239695815,112.865045407385,113.863851118954,114.214635937601),
 .UNSPECIFIED.);
#574=B_SPLINE_CURVE_WITH_KNOTS('',3,(#34538,#34539,#34540,#34541,#34542,
#34543,#34544,#34545,#34546,#34547,#34548,#34549,#34550,#34551,#34552,#34553,
#34554,#34555,#34556,#34557,#34558,#34559),.UNSPECIFIED.,.F.,.F.,(4,3,3,
3,3,3,3,4),(-123.473451256543,-122.796739358775,-121.798391884313,-120.800044409852,
-119.80169693539,-118.803349460929,-117.805001986467,-117.190265949363),
 .UNSPECIFIED.);
#575=B_SPLINE_CURVE_WITH_KNOTS('',3,(#34560,#34561,#34562,#34563,#34564,
#34565,#34566,#34567,#34568,#34569,#34570,#34571,#34572,#34573,#34574,#34575,
#34576,#34577,#34578,#34579,#34580,#34581),.UNSPECIFIED.,.F.,.F.,(4,3,3,
3,3,3,3,4),(114.214635937601,114.862656830524,115.861462542094,116.860268253664,
117.859073965234,118.857879676803,119.856685388373,120.49782124478),
 .UNSPECIFIED.);
#576=B_SPLINE_CURVE_WITH_KNOTS('',3,(#34586,#34587,#34588,#34589,#34590,
#34591,#34592,#34593,#34594,#34595,#34596,#34597,#34598,#34599,#34600,#34601,
#34602,#34603,#34604,#34605,#34606,#34607),.UNSPECIFIED.,.F.,.F.,(4,3,3,
3,3,3,3,4),(-129.756636563722,-128.786824205544,-127.788476731083,-126.790129256621,
-125.79178178216,-124.793434307698,-123.795086833237,-123.473451256543),
 .UNSPECIFIED.);
#577=B_SPLINE_CURVE_WITH_KNOTS('',3,(#34608,#34609,#34610,#34611,#34612,
#34613,#34614,#34615,#34616,#34617,#34618,#34619,#34620,#34621,#34622,#34623,
#34624,#34625,#34626,#34627,#34628,#34629),.UNSPECIFIED.,.F.,.F.,(4,3,3,
3,3,3,3,4),(120.49782124478,120.855491099943,121.854296811513,122.853102523082,
123.851908234652,124.850713946222,125.849519657792,126.78100655196),
 .UNSPECIFIED.);
#578=B_SPLINE_CURVE_WITH_KNOTS('',3,(#34634,#34635,#34636,#34637,#34638,
#34639,#34640,#34641,#34642,#34643,#34644,#34645,#34646,#34647,#34648,#34649,
#34650,#34651,#34652,#34653,#34654,#34655,#34656,#34657,#34658),
 .UNSPECIFIED.,.F.,.F.,(4,3,3,3,3,3,3,3,4),(-136.039821870902,-135.775256526776,
-134.776909052314,-133.778561577852,-132.780214103391,-131.781866628929,
-130.783519154468,-129.785171680006,-129.756636563722),.UNSPECIFIED.);
#579=B_SPLINE_CURVE_WITH_KNOTS('',3,(#34659,#34660,#34661,#34662,#34663,
#34664,#34665,#34666,#34667,#34668,#34669,#34670,#34671,#34672,#34673,#34674,
#34675,#34676,#34677,#34678,#34679,#34680,#34681,#34682,#34683),
 .UNSPECIFIED.,.F.,.F.,(4,3,3,3,3,3,3,3,4),(126.78100655196,126.848325369362,
127.847131080931,128.845936792501,129.844742504071,130.843548215641,131.84235392721,
132.84115963878,133.06419185914),.UNSPECIFIED.);
#580=B_SPLINE_CURVE_WITH_KNOTS('',3,(#34688,#34689,#34690,#34691,#34692,
#34693,#34694,#34695,#34696,#34697,#34698,#34699,#34700,#34701,#34702,#34703,
#34704,#34705,#34706,#34707,#34708,#34709),.UNSPECIFIED.,.F.,.F.,(4,3,3,
3,3,3,3,4),(-142.323007178082,-141.765341373545,-140.766993899083,-139.768646424622,
-138.77029895016,-137.771951475699,-136.773604001237,-136.039821870902),
 .UNSPECIFIED.);
#581=B_SPLINE_CURVE_WITH_KNOTS('',3,(#34710,#34711,#34712,#34713,#34714,
#34715,#34716,#34717,#34718,#34719,#34720,#34721,#34722,#34723,#34724,#34725,
#34726,#34727,#34728,#34729,#34730,#34731),.UNSPECIFIED.,.F.,.F.,(4,3,3,
3,3,3,3,4),(133.06419185914,133.83996535035,134.83877106192,135.83757677349,
136.836382485059,137.835188196629,138.833993908199,139.347377166319),
 .UNSPECIFIED.);
#582=B_SPLINE_CURVE_WITH_KNOTS('',3,(#34736,#34737,#34738,#34739,#34740,
#34741,#34742,#34743,#34744,#34745,#34746,#34747,#34748,#34749,#34750,#34751,
#34752,#34753,#34754,#34755,#34756,#34757),.UNSPECIFIED.,.F.,.F.,(4,3,3,
3,3,3,3,4),(-148.606192485261,-147.755426220315,-146.757078745853,-145.758731271391,
-144.76038379693,-143.762036322468,-142.763688848007,-142.323007178082),
 .UNSPECIFIED.);
#583=B_SPLINE_CURVE_WITH_KNOTS('',3,(#34758,#34759,#34760,#34761,#34762,
#34763,#34764,#34765,#34766,#34767,#34768,#34769,#34770,#34771,#34772,#34773,
#34774,#34775,#34776,#34777,#34778,#34779),.UNSPECIFIED.,.F.,.F.,(4,3,3,
3,3,3,3,4),(139.347377166319,139.832799619769,140.831605331338,141.830411042908,
142.829216754478,143.828022466048,144.826828177618,145.630562473499),
 .UNSPECIFIED.);
#584=B_SPLINE_CURVE_WITH_KNOTS('',3,(#34785,#34786,#34787,#34788,#34789,
#34790,#34791,#34792,#34793,#34794),.UNSPECIFIED.,.F.,.F.,(4,1,1,1,1,1,
1,4),(160.221225333079,160.368806542595,161.367154017056,162.365501491518,
163.363848965979,164.362196440441,165.360543914902,166.358891389364),
 .UNSPECIFIED.);
#585=B_SPLINE_CURVE_WITH_KNOTS('',3,(#34797,#34798,#34799,#34800,#34801,
#34802,#34803,#34804),.UNSPECIFIED.,.F.,.F.,(4,1,1,1,1,4),(160.221225333079,
161.124751422577,162.123557134147,163.122362845716,164.121168557286,165.119974268856),
 .UNSPECIFIED.);
#586=B_SPLINE_CURVE_WITH_KNOTS('',3,(#34809,#34810,#34811,#34812,#34813,
#34814,#34815,#34816,#34817,#34818),.UNSPECIFIED.,.F.,.F.,(4,1,1,1,1,1,
1,4),(153.9380400259,154.378721695825,155.377069170287,156.375416644748,
157.37376411921,158.372111593671,159.370459068133,160.221225333079),
 .UNSPECIFIED.);
#587=B_SPLINE_CURVE_WITH_KNOTS('',3,(#34819,#34820,#34821,#34822,#34823,
#34824,#34825,#34826,#34827,#34828,#34829),.UNSPECIFIED.,.F.,.F.,(4,1,1,
1,1,1,1,1,4),(153.9380400259,154.133111441588,155.131917153158,156.130722864728,
157.129528576298,158.128334287868,159.127139999437,160.125945711007,160.221225333079),
 .UNSPECIFIED.);
#588=B_SPLINE_CURVE_WITH_KNOTS('',3,(#34834,#34835,#34836,#34837,#34838,
#34839,#34840,#34841,#34842,#34843),.UNSPECIFIED.,.F.,.F.,(4,1,1,1,1,1,
1,4),(147.65485471872,148.388636849056,149.386984323517,150.385331797979,
151.38367927244,152.382026746902,153.380374221363,153.9380400259),
 .UNSPECIFIED.);
#589=B_SPLINE_CURVE_WITH_KNOTS('',3,(#34844,#34845,#34846,#34847,#34848,
#34849,#34850,#34851,#34852,#34853),.UNSPECIFIED.,.F.,.F.,(4,1,1,1,1,1,
1,4),(147.65485471872,148.14027717217,149.13908288374,150.137888595309,
151.136694306879,152.135500018449,153.134305730019,153.9380400259),
 .UNSPECIFIED.);
#590=B_SPLINE_CURVE_WITH_KNOTS('',3,(#34858,#34859,#34860,#34861,#34862,
#34863,#34864,#34865,#34866,#34867,#34868),.UNSPECIFIED.,.F.,.F.,(4,1,1,
1,1,1,1,1,4),(141.371669411541,141.400204527824,142.398552002286,143.396899476748,
144.395246951209,145.393594425671,146.391941900132,147.390289374594,147.65485471872),
 .UNSPECIFIED.);
#591=B_SPLINE_CURVE_WITH_KNOTS('',3,(#34869,#34870,#34871,#34872,#34873,
#34874,#34875,#34876,#34877,#34878),.UNSPECIFIED.,.F.,.F.,(4,1,1,1,1,1,
1,4),(141.371669411541,142.147442902751,143.146248614321,144.145054325891,
145.14386003746,146.14266574903,147.1414714606,147.65485471872),
 .UNSPECIFIED.);
#592=B_SPLINE_CURVE_WITH_KNOTS('',3,(#34883,#34884,#34885,#34886,#34887,
#34888,#34889,#34890,#34891,#34892),.UNSPECIFIED.,.F.,.F.,(4,1,1,1,1,1,
1,4),(135.088484104361,135.410119681055,136.408467155516,137.406814629978,
138.40516210444,139.403509578901,140.401857053363,141.371669411541),
 .UNSPECIFIED.);
#593=B_SPLINE_CURVE_WITH_KNOTS('',3,(#34893,#34894,#34895,#34896,#34897,
#34898,#34899,#34900,#34901,#34902,#34903),.UNSPECIFIED.,.F.,.F.,(4,1,1,
1,1,1,1,1,4),(135.088484104361,135.155802921763,136.154608633332,137.153414344902,
138.152220056472,139.151025768042,140.149831479612,141.148637191181,141.371669411541),
 .UNSPECIFIED.);
#594=B_SPLINE_CURVE_WITH_KNOTS('',3,(#34908,#34909,#34910,#34911,#34912,
#34913,#34914,#34915,#34916,#34917),.UNSPECIFIED.,.F.,.F.,(4,1,1,1,1,1,
1,4),(128.805298797182,129.420034834285,130.418382308747,131.416729783209,
132.41507725767,133.413424732132,134.411772206593,135.088484104361),
 .UNSPECIFIED.);
#595=B_SPLINE_CURVE_WITH_KNOTS('',3,(#34918,#34919,#34920,#34921,#34922,
#34923,#34924,#34925,#34926,#34927),.UNSPECIFIED.,.F.,.F.,(4,1,1,1,1,1,
1,4),(128.805298797182,129.162968652344,130.161774363914,131.160580075484,
132.159385787053,133.158191498623,134.156997210193,135.088484104361),
 .UNSPECIFIED.);
#596=B_SPLINE_CURVE_WITH_KNOTS('',3,(#34932,#34933,#34934,#34935,#34936,
#34937,#34938,#34939,#34940,#34941),.UNSPECIFIED.,.F.,.F.,(4,1,1,1,1,1,
1,4),(122.522113490002,123.429949987516,124.428297461977,125.426644936439,
126.424992410901,127.423339885362,128.421687359824,128.805298797182),
 .UNSPECIFIED.);
#597=B_SPLINE_CURVE_WITH_KNOTS('',3,(#34942,#34943,#34944,#34945,#34946,
#34947,#34948,#34949,#34950,#34951),.UNSPECIFIED.,.F.,.F.,(4,1,1,1,1,1,
1,4),(122.522113490002,123.170134382925,124.168940094495,125.167745806065,
126.166551517635,127.165357229204,128.164162940774,128.805298797182),
 .UNSPECIFIED.);
#598=B_SPLINE_CURVE_WITH_KNOTS('',3,(#34956,#34957,#34958,#34959,#34960,
#34961,#34962,#34963,#34964,#34965,#34966),.UNSPECIFIED.,.F.,.F.,(4,1,1,
1,1,1,1,1,4),(116.238928182822,116.441517666285,117.439865140746,118.438212615208,
119.43656008967,120.434907564131,121.433255038593,122.431602513054,122.522113490002),
 .UNSPECIFIED.);
#599=B_SPLINE_CURVE_WITH_KNOTS('',3,(#34967,#34968,#34969,#34970,#34971,
#34972,#34973,#34974,#34975,#34976),.UNSPECIFIED.,.F.,.F.,(4,1,1,1,1,1,
1,4),(116.238928182822,117.177300113507,118.176105825076,119.174911536646,
120.173717248216,121.172522959786,122.171328671356,122.522113490002),
 .UNSPECIFIED.);
#600=B_SPLINE_CURVE_WITH_KNOTS('',3,(#34981,#34982,#34983,#34984,#34985,
#34986,#34987,#34988,#34989,#34990),.UNSPECIFIED.,.F.,.F.,(4,1,1,1,1,1,
1,4),(109.955742875643,110.451432819515,111.449780293977,112.448127768438,
113.4464752429,114.444822717362,115.443170191823,116.238928182822),
 .UNSPECIFIED.);
#601=B_SPLINE_CURVE_WITH_KNOTS('',3,(#34991,#34992,#34993,#34994,#34995,
#34996,#34997,#34998,#34999,#35000,#35001),.UNSPECIFIED.,.F.,.F.,(4,1,1,
1,1,1,1,1,4),(109.955742875643,110.185660132518,111.184465844088,112.183271555658,
113.182077267228,114.180882978797,115.179688690367,116.178494401937,116.238928182822),
 .UNSPECIFIED.);
#602=B_SPLINE_CURVE_WITH_KNOTS('',3,(#35006,#35007,#35008,#35009,#35010,
#35011,#35012,#35013,#35014,#35015),.UNSPECIFIED.,.F.,.F.,(4,1,1,1,1,1,
1,4),(103.672557568463,104.461347972746,105.459695447207,106.458042921669,
107.456390396131,108.454737870592,109.453085345054,109.955742875643),
 .UNSPECIFIED.);
#603=B_SPLINE_CURVE_WITH_KNOTS('',3,(#35016,#35017,#35018,#35019,#35020,
#35021,#35022,#35023,#35024,#35025),.UNSPECIFIED.,.F.,.F.,(4,1,1,1,1,1,
1,4),(103.672557568463,104.1928258631,105.191631574669,106.190437286239,
107.189242997809,108.188048709379,109.186854420948,109.955742875643),
 .UNSPECIFIED.);
#604=B_SPLINE_CURVE_WITH_KNOTS('',3,(#35030,#35031,#35032,#35033,#35034,
#35035,#35036,#35037,#35038,#35039,#35040),.UNSPECIFIED.,.F.,.F.,(4,1,1,
1,1,1,1,1,4),(97.3893722612837,97.4729156515147,98.4712631259763,99.4696106004379,
100.467958074899,101.466305549361,102.464653023823,103.463000498284,103.672557568463),
 .UNSPECIFIED.);
#605=B_SPLINE_CURVE_WITH_KNOTS('',3,(#35041,#35042,#35043,#35044,#35045,
#35046,#35047,#35048,#35049,#35050),.UNSPECIFIED.,.F.,.F.,(4,1,1,1,1,1,
1,4),(97.3893722612837,98.199991593681,99.1987973052507,100.197603016821,
101.19640872839,102.19521443996,103.19402015153,103.672557568463),
 .UNSPECIFIED.);
#606=B_SPLINE_CURVE_WITH_KNOTS('',3,(#35055,#35056,#35057,#35058,#35059,
#35060,#35061,#35062,#35063,#35064),.UNSPECIFIED.,.F.,.F.,(4,1,1,1,1,1,
1,4),(91.1061869541041,91.4828308047452,92.4811782792068,93.4795257536684,
94.4778732281299,95.4762207025915,96.4745681770531,97.3893722612837),
 .UNSPECIFIED.);
#607=B_SPLINE_CURVE_WITH_KNOTS('',3,(#35065,#35066,#35067,#35068,#35069,
#35070,#35071,#35072,#35073,#35074,#35075),.UNSPECIFIED.,.F.,.F.,(4,1,1,
1,1,1,1,1,4),(91.1061869541041,91.2083516126925,92.2071573242623,93.2059630358321,
94.2047687474019,95.2035744589716,96.2023801705414,97.2011858821112,97.3893722612837),
 .UNSPECIFIED.);
#608=B_SPLINE_CURVE_WITH_KNOTS('',3,(#35080,#35081,#35082,#35083,#35084,
#35085,#35086,#35087,#35088,#35089),.UNSPECIFIED.,.F.,.F.,(4,1,1,1,1,1,
1,4),(84.8230016469245,85.4927459579757,86.4910934324373,87.4894409068988,
88.4877883813604,89.486135855822,90.4844833302836,91.1061869541041),
 .UNSPECIFIED.);
#609=B_SPLINE_CURVE_WITH_KNOTS('',3,(#35090,#35091,#35092,#35093,#35094,
#35095,#35096,#35097,#35098,#35099),.UNSPECIFIED.,.F.,.F.,(4,1,1,1,1,1,
1,4),(84.8230016469245,85.2155173432739,86.2143230548436,87.2131287664134,
88.2119344779832,89.210740189553,90.2095459011228,91.1061869541041),
 .UNSPECIFIED.);
#610=B_SPLINE_CURVE_WITH_KNOTS('',3,(#35104,#35105,#35106,#35107,#35108,
#35109,#35110,#35111,#35112,#35113),.UNSPECIFIED.,.F.,.F.,(4,1,1,1,1,1,
1,4),(78.5398163397449,79.5026611112062,80.5010085856677,81.4993560601293,
82.4977035345909,83.4960510090525,84.4943984835141,84.8230016469245),
 .UNSPECIFIED.);
#611=B_SPLINE_CURVE_WITH_KNOTS('',3,(#35114,#35115,#35116,#35117,#35118,
#35119,#35120,#35121,#35122,#35123),.UNSPECIFIED.,.F.,.F.,(4,1,1,1,1,1,
1,4),(78.5398163397449,79.2226830738552,80.221488785425,81.2202944969948,
82.2191002085646,83.2179059201343,84.2167116317041,84.8230016469245),
 .UNSPECIFIED.);
#612=B_SPLINE_CURVE_WITH_KNOTS('',3,(#35128,#35129,#35130,#35131,#35132,
#35133,#35134,#35135,#35136,#35137,#35138),.UNSPECIFIED.,.F.,.F.,(4,1,1,
1,1,1,1,1,4),(72.2566310325653,72.5142287899751,73.5125762644366,74.5109237388982,
75.5092712133598,76.5076186878214,77.505966162283,78.5043136367446,78.5398163397449),
 .UNSPECIFIED.);
#613=B_SPLINE_CURVE_WITH_KNOTS('',3,(#35139,#35140,#35141,#35142,#35143,
#35144,#35145,#35146,#35147,#35148),.UNSPECIFIED.,.F.,.F.,(4,1,1,1,1,1,
1,4),(72.2566310325653,73.2298488044366,74.2286545160063,75.2274602275761,
76.2262659391459,77.2250716507157,78.2238773622854,78.5398163397449),
 .UNSPECIFIED.);
#614=B_SPLINE_CURVE_WITH_KNOTS('',3,(#35153,#35154,#35155,#35156,#35157,
#35158,#35159,#35160,#35161,#35162),.UNSPECIFIED.,.F.,.F.,(4,1,1,1,1,1,
1,4),(65.9734457253857,66.5241439432056,67.5224914176671,68.5208388921287,
69.5191863665903,70.5175338410519,71.5158813155135,72.2566310325653),
 .UNSPECIFIED.);
#615=B_SPLINE_CURVE_WITH_KNOTS('',3,(#35163,#35164,#35165,#35166,#35167,
#35168,#35169,#35170,#35171,#35172,#35173),.UNSPECIFIED.,.F.,.F.,(4,1,1,
1,1,1,1,1,4),(65.9734457253857,66.2382088234481,67.2370145350179,68.2358202465877,
69.2346259581575,70.2334316697272,71.232237381297,72.2310430928668,72.2566310325653),
 .UNSPECIFIED.);
#616=B_SPLINE_CURVE_WITH_KNOTS('',3,(#35178,#35179,#35180,#35181,#35182,
#35183,#35184,#35185,#35186,#35187),.UNSPECIFIED.,.F.,.F.,(4,1,1,1,1,1,
1,4),(59.6902604182061,60.534059096436,61.5324065708976,62.5307540453592,
63.5291015198208,64.5274489942824,65.525796468744,65.9734457253857),
 .UNSPECIFIED.);
#617=B_SPLINE_CURVE_WITH_KNOTS('',3,(#35188,#35189,#35190,#35191,#35192,
#35193,#35194,#35195,#35196,#35197),.UNSPECIFIED.,.F.,.F.,(4,1,1,1,1,1,
1,4),(59.6902604182061,60.2453745540295,61.2441802655993,62.242985977169,
63.2417916887388,64.2405974003086,65.2394031118784,65.9734457253857),
 .UNSPECIFIED.);
#618=B_SPLINE_CURVE_WITH_KNOTS('',3,(#35202,#35203,#35204,#35205,#35206,
#35207,#35208,#35209,#35210,#35211,#35212),.UNSPECIFIED.,.F.,.F.,(4,1,1,
1,1,1,1,1,4),(53.4070751110265,53.545626775205,54.5439742496665,55.5423217241281,
56.5406691985897,57.5390166730513,58.5373641475129,59.5357116219745,59.6902604182061),
 .UNSPECIFIED.);
#619=B_SPLINE_CURVE_WITH_KNOTS('',3,(#35213,#35214,#35215,#35216,#35217,
#35218,#35219,#35220,#35221,#35222),.UNSPECIFIED.,.F.,.F.,(4,1,1,1,1,1,
1,4),(53.4070751110265,54.2525402846108,55.2513459961806,56.2501517077504,
57.2489574193202,58.2477631308899,59.2465688424597,59.6902604182061),
 .UNSPECIFIED.);
#620=B_SPLINE_CURVE_WITH_KNOTS('',3,(#35227,#35228,#35229,#35230,#35231,
#35232,#35233,#35234,#35235,#35236),.UNSPECIFIED.,.F.,.F.,(4,1,1,1,1,1,
1,4),(47.1238898038469,47.5555419284354,48.553889402897,49.5522368773586,
50.5505843518202,51.5489318262818,52.5472793007434,53.4070751110265),
 .UNSPECIFIED.);
#621=B_SPLINE_CURVE_WITH_KNOTS('',3,(#35237,#35238,#35239,#35240,#35241,
#35242,#35243,#35244,#35245,#35246,#35247),.UNSPECIFIED.,.F.,.F.,(4,1,1,
1,1,1,1,1,4),(47.1238898038469,47.2609003036224,48.2597060151922,49.258511726762,
50.2573174383317,51.2561231499015,52.2549288614713,53.2537345730411,53.4070751110265),
 .UNSPECIFIED.);
#622=B_SPLINE_CURVE_WITH_KNOTS('',3,(#35252,#35253,#35254,#35255,#35256,
#35257,#35258,#35259,#35260,#35261),.UNSPECIFIED.,.F.,.F.,(4,1,1,1,1,1,
1,4),(40.8407044966673,41.5654570816659,42.5638045561275,43.5621520305891,
44.5604995050507,45.5588469795123,46.5571944539738,47.1238898038469),
 .UNSPECIFIED.);
#623=B_SPLINE_CURVE_WITH_KNOTS('',3,(#35262,#35263,#35264,#35265,#35266,
#35267,#35268,#35269,#35270,#35271),.UNSPECIFIED.,.F.,.F.,(4,1,1,1,1,1,
1,4),(40.8407044966673,41.2680660342037,42.2668717457735,43.2656774573433,
44.2644831689131,45.2632888804829,46.2620945920526,47.1238898038469),
 .UNSPECIFIED.);
#624=B_SPLINE_CURVE_WITH_KNOTS('',3,(#35276,#35277,#35278,#35279,#35280,
#35281,#35282,#35283,#35284,#35285,#35286),.UNSPECIFIED.,.F.,.F.,(4,1,1,
1,1,1,1,1,4),(34.5575191894877,34.5770247604348,35.5753722348964,36.573719709358,
37.5720671838196,38.5704146582812,39.5687621327428,40.5671096072043,40.8407044966673),
 .UNSPECIFIED.);
#625=B_SPLINE_CURVE_WITH_KNOTS('',3,(#35287,#35288,#35289,#35290,#35291,
#35292,#35293,#35294,#35295,#35296),.UNSPECIFIED.,.F.,.F.,(4,1,1,1,1,1,
1,4),(34.5575191894877,35.2752317647851,36.2740374763549,37.2728431879246,
38.2716488994944,39.2704546110642,40.269260322634,40.8407044966673),
 .UNSPECIFIED.);
#626=B_SPLINE_CURVE_WITH_KNOTS('',3,(#35301,#35302,#35303,#35304,#35305,
#35306,#35307,#35308,#35309,#35310),.UNSPECIFIED.,.F.,.F.,(4,1,1,1,1,1,
1,4),(28.2743338823082,28.5869399136653,29.5852873881269,30.5836348625885,
31.5819823370501,32.5803298115117,33.5786772859732,34.5575191894877),
 .UNSPECIFIED.);
#627=B_SPLINE_CURVE_WITH_KNOTS('',3,(#35311,#35312,#35313,#35314,#35315,
#35316,#35317,#35318,#35319,#35320,#35321),.UNSPECIFIED.,.F.,.F.,(4,1,1,
1,1,1,1,1,4),(28.2743338823082,28.2835917837967,29.2823974953664,30.2812032069362,
31.280008918506,32.2788146300758,33.2776203416455,34.2764260532153,34.5575191894877),
 .UNSPECIFIED.);
#628=B_SPLINE_CURVE_WITH_KNOTS('',3,(#35326,#35327,#35328,#35329,#35330,
#35331,#35332,#35333,#35334,#35335),.UNSPECIFIED.,.F.,.F.,(4,1,1,1,1,1,
1,4),(21.9911485751286,22.5968550668958,23.5952025413574,24.593550015819,
25.5918974902806,26.5902449647422,27.5885924392037,28.2743338823082),
 .UNSPECIFIED.);
#629=B_SPLINE_CURVE_WITH_KNOTS('',3,(#35336,#35337,#35338,#35339,#35340,
#35341,#35342,#35343,#35344,#35345),.UNSPECIFIED.,.F.,.F.,(4,1,1,1,1,1,
1,4),(21.9911485751286,22.290757514378,23.2895632259478,24.2883689375176,
25.2871746490873,26.2859803606571,27.2847860722269,28.2743338823082),
 .UNSPECIFIED.);
#630=B_SPLINE_CURVE_WITH_KNOTS('',3,(#35350,#35351,#35352,#35353,#35354,
#35355,#35356,#35357,#35358,#35359),.UNSPECIFIED.,.F.,.F.,(4,1,1,1,1,1,
1,4),(15.707963267949,16.6067702201263,17.6051176945879,18.6034651690495,
19.6018126435111,20.6001601179726,21.5985075924342,21.9911485751286),
 .UNSPECIFIED.);
#631=B_SPLINE_CURVE_WITH_KNOTS('',3,(#35360,#35361,#35362,#35363,#35364,
#35365,#35366,#35367,#35368,#35369),.UNSPECIFIED.,.F.,.F.,(4,1,1,1,1,1,
1,4),(15.707963267949,16.2979232449593,17.2967289565291,18.2955346680989,
19.2943403796687,20.2931460912385,21.2919518028082,21.9911485751286),
 .UNSPECIFIED.);
#632=B_SPLINE_CURVE_WITH_KNOTS('',3,(#35372,#35373,#35374,#35375,#35376,
#35377,#35378,#35379,#35380,#35381,#35382,#35383,#35384,#35385,#35386,#35387,
#35388,#35389,#35390,#35391,#35392,#35393,#35394,#35395,#35396,#35397,#35398,
#35399,#35400,#35401,#35402,#35403,#35404,#35405,#35406,#35407,#35408,#35409,
#35410,#35411,#35412,#35413,#35414,#35415,#35416,#35417,#35418,#35419,#35420,
#35421,#35422,#35423,#35424,#35425,#35426,#35427,#35428,#35429,#35430,#35431,
#35432,#35433,#35434,#35435,#35436,#35437,#35438,#35439,#35440,#35441,#35442,
#35443,#35444,#35445,#35446,#35447,#35448,#35449,#35450,#35451,#35452,#35453,
#35454,#35455,#35456,#35457,#35458,#35459,#35460,#35461,#35462,#35463,#35464,
#35465,#35466,#35467,#35468,#35469,#35470,#35471,#35472,#35473,#35474,#35475,
#35476,#35477,#35478,#35479,#35480,#35481,#35482,#35483,#35484,#35485,#35486,
#35487,#35488,#35489,#35490,#35491,#35492,#35493,#35494,#35495,#35496,#35497,
#35498,#35499,#35500,#35501,#35502,#35503,#35504,#35505,#35506,#35507,#35508,
#35509,#35510,#35511,#35512,#35513,#35514,#35515,#35516,#35517,#35518,#35519,
#35520,#35521,#35522,#35523,#35524,#35525,#35526,#35527,#35528,#35529,#35530,
#35531,#35532,#35533,#35534,#35535,#35536,#35537,#35538,#35539,#35540,#35541,
#35542,#35543,#35544,#35545,#35546,#35547,#35548,#35549,#35550,#35551,#35552,
#35553,#35554,#35555,#35556,#35557,#35558,#35559,#35560,#35561,#35562,#35563,
#35564,#35565,#35566,#35567,#35568,#35569,#35570,#35571,#35572,#35573,#35574,
#35575,#35576,#35577,#35578,#35579,#35580,#35581,#35582,#35583,#35584,#35585,
#35586,#35587,#35588,#35589,#35590,#35591,#35592,#35593,#35594,#35595,#35596,
#35597,#35598,#35599,#35600,#35601,#35602,#35603),.UNSPECIFIED.,.F.,.F.,
(4,3,3,3,3,3,3,3,3,3,3,3,3,3,3,3,3,3,3,3,3,3,3,3,3,3,3,3,3,3,3,3,3,3,3,
3,3,3,3,3,3,3,3,3,3,3,3,3,3,3,3,3,3,3,3,3,3,3,3,3,3,3,3,3,3,3,3,3,3,3,3,
3,3,3,3,3,3,4),(-2.07787844821581,-2.04563640817454,-2.01260600406739,-1.99390262471517,
-1.97880815407869,-1.97343611688677,-1.93978265453417,-1.90587423526444,
-1.88438455677208,-1.87589993511254,-1.87071648916707,-1.83652656870669,
-1.80253536734925,-1.7682460873374,-1.75110144733148,-1.74333138277347,
-1.73705920337893,-1.73395680732556,-1.70122489773177,-1.66760788468754,
-1.63163034935991,-1.61589017765406,-1.60492981834386,-1.60020318232811,
-1.56577415958123,-1.53098947454713,-1.49635100238812,-1.4672101523077,
-1.46216466120046,-1.42716054566692,-1.39267814268788,-1.37978760206645,
-1.34531390132733,-1.33245646351828,-1.32592267957129,-1.32082668753048,
-1.28679878189102,-1.2516716099619,-1.21635641577775,-1.19129075085948,
-1.18499879133774,-1.18014246087519,-1.1446795062145,-1.10922024591651,
-1.07424600071327,-1.04503854857244,-1.03811338002803,-1.0158310964316,
-0.981392848951218,-0.946133107350497,-0.910369520876374,-0.899628872347486,
-0.89368994999567,-0.857962841308724,-0.82181130706931,-0.785718553763474,
-0.767732714465289,-0.754402261382112,-0.748013249342093,-0.711600160631613,
-0.675777877337977,-0.641831839377992,-0.620163722971144,-0.609175591942721,
-0.603763283335243,-0.56872451739821,-0.532416642828612,-0.495724942594248,
-0.470652071878519,-0.458093605572563,-0.451831603827856,-0.415093157349795,
-0.378123471546787,-0.341518871530435,-0.318330424199427,-0.308274893383926,
-0.301672805800084,-0.295141976868419),.UNSPECIFIED.);
#633=B_SPLINE_CURVE_WITH_KNOTS('',3,(#35605,#35606,#35607,#35608,#35609,
#35610,#35611,#35612,#35613,#35614,#35615,#35616,#35617,#35618,#35619,#35620,
#35621,#35622,#35623,#35624,#35625,#35626,#35627,#35628,#35629,#35630,#35631,
#35632,#35633,#35634,#35635,#35636,#35637,#35638,#35639,#35640,#35641,#35642,
#35643,#35644,#35645,#35646,#35647,#35648,#35649,#35650,#35651,#35652,#35653,
#35654,#35655,#35656,#35657,#35658,#35659,#35660,#35661,#35662,#35663,#35664,
#35665,#35666,#35667,#35668,#35669,#35670,#35671),.UNSPECIFIED.,.F.,.F.,
(4,3,3,3,3,3,3,3,3,3,3,3,3,3,3,3,3,3,3,3,3,3,4),(-0.560387248253829,-0.523489675423405,
-0.486909280826814,-0.451409765500931,-0.428581929912694,-0.422644096024468,
-0.417538776764712,-0.382486843658728,-0.360098423147984,-0.324342694600126,
-0.288456460870319,-0.277039646852259,-0.272658549855339,-0.23782854730266,
-0.202954723102529,-0.168490668078001,-0.147429334568251,-0.135539740506508,
-0.130645012249701,-0.0971180289394068,-0.0640503905793665,-0.0319885771286076,
0.),.UNSPECIFIED.);
#634=B_SPLINE_CURVE_WITH_KNOTS('',3,(#35674,#35675,#35676,#35677,#35678,
#35679,#35680,#35681,#35682,#35683,#35684,#35685,#35686,#35687,#35688,#35689,
#35690,#35691,#35692,#35693,#35694,#35695,#35696,#35697,#35698,#35699,#35700,
#35701,#35702,#35703,#35704),.UNSPECIFIED.,.F.,.F.,(4,3,3,3,3,3,3,3,3,3,
4),(-0.295141976868419,-0.258118008913044,-0.221832521729933,-0.184905796964689,
-0.161792572344103,-0.155196944416255,-0.149950158553442,-0.112462618915081,
-0.0749997768837546,-0.0374998884418773,0.),.UNSPECIFIED.);
#635=B_SPLINE_CURVE_WITH_KNOTS('',3,(#36341,#36342,#36343,#36344,#36345,
#36346,#36347,#36348),.UNSPECIFIED.,.F.,.F.,(4,1,1,1,1,4),(11.6150328478184,
12.61338032228,13.6117277967416,14.6100752712031,15.6084227456647,15.707963267949),
 .UNSPECIFIED.);
#636=B_SPLINE_CURVE_WITH_KNOTS('',3,(#36349,#36350,#36351,#36352,#36353,
#36354,#36355,#36356,#36357,#36358,#36359,#36360,#36361,#36362,#36363,#36364,
#36365,#36366,#36367,#36368,#36369,#36370,#36371,#36372,#36373,#36374,#36375,
#36376,#36377,#36378,#36379,#36380,#36381,#36382,#36383,#36384,#36385,#36386,
#36387,#36388,#36389,#36390,#36391,#36392,#36393,#36394,#36395,#36396,#36397,
#36398,#36399,#36400,#36401,#36402,#36403,#36404,#36405,#36406,#36407,#36408,
#36409,#36410,#36411,#36412,#36413,#36414,#36415,#36416,#36417,#36418,#36419,
#36420,#36421,#36422,#36423,#36424,#36425,#36426,#36427,#36428,#36429,#36430,
#36431,#36432,#36433,#36434,#36435,#36436,#36437,#36438,#36439,#36440,#36441,
#36442,#36443,#36444,#36445),.UNSPECIFIED.,.F.,.F.,(4,3,3,3,3,3,3,3,3,3,
3,3,3,3,3,3,3,3,3,3,3,3,3,3,3,3,3,3,3,3,3,3,4),(-0.75940314415766,-0.731099230044352,
-0.694405090916541,-0.673021753795954,-0.659792230351525,-0.653579099280099,
-0.615915673993481,-0.58296017686769,-0.568542146875157,-0.56016187063185,
-0.554528541316208,-0.518574457756444,-0.482794928028838,-0.44802285832865,
-0.424085067993276,-0.41225754927003,-0.407433722504049,-0.373002009397425,
-0.352271696987154,-0.317344582417244,-0.282174956583422,-0.274866834214802,
-0.269904808501567,-0.23562822660491,-0.201185303792214,-0.167047167238569,
-0.146166271333748,-0.135071182701311,-0.130169248221992,-0.0967451917617864,
-0.0637506042838665,-0.03178494031496,0.),.UNSPECIFIED.);
#637=B_SPLINE_CURVE_WITH_KNOTS('',3,(#36446,#36447,#36448,#36449,#36450,
#36451,#36452,#36453,#36454,#36455,#36456,#36457,#36458,#36459,#36460,#36461,
#36462,#36463,#36464),.UNSPECIFIED.,.F.,.F.,(4,3,3,3,3,3,4),(-153.229510295036,
-152.747163592623,-151.748816118161,-150.750468643699,-149.752121169238,
-148.753773694776,-148.606192485261),.UNSPECIFIED.);
#638=B_SPLINE_CURVE_WITH_KNOTS('',3,(#36467,#36468,#36469,#36470,#36471,
#36472,#36473,#36474,#36475),.UNSPECIFIED.,.F.,.F.,(4,1,1,1,1,1,4),(10.3761157273103,
11.3038946871105,12.3027003986802,13.30150611025,14.3003118218198,15.2991175333896,
15.707963267949),.UNSPECIFIED.);
#639=B_SPLINE_CURVE_WITH_KNOTS('',3,(#37117,#37118,#37119,#37120,#37121,
#37122,#37123,#37124,#37125,#37126,#37127,#37128,#37129,#37130,#37131,#37132,
#37133,#37134,#37135,#37136,#37137,#37138),.UNSPECIFIED.,.F.,.F.,(4,3,3,
3,3,3,3,4),(145.630562473499,145.825633889187,146.824439600757,147.823245312327,
148.822051023897,149.820856735466,150.819662447036,151.160872120127),
 .UNSPECIFIED.);
#640=B_SPLINE_CURVE_WITH_KNOTS('',3,(#37139,#37140,#37141,#37142,#37143,
#37144,#37145,#37146,#37147,#37148,#37149,#37150,#37151,#37152,#37153,#37154,
#37155,#37156,#37157,#37158,#37159,#37160,#37161,#37162,#37163,#37164,#37165,
#37166,#37167,#37168,#37169,#37170,#37171,#37172,#37173,#37174,#37175,#37176,
#37177,#37178,#37179,#37180,#37181,#37182,#37183,#37184,#37185,#37186,#37187,
#37188,#37189,#37190,#37191,#37192,#37193,#37194,#37195,#37196,#37197,#37198,
#37199,#37200,#37201,#37202,#37203,#37204,#37205,#37206,#37207,#37208,#37209,
#37210,#37211,#37212,#37213,#37214,#37215,#37216,#37217,#37218,#37219,#37220,
#37221,#37222,#37223,#37224,#37225,#37226,#37227,#37228,#37229,#37230,#37231,
#37232,#37233,#37234,#37235),.UNSPECIFIED.,.F.,.F.,(4,3,3,3,3,3,3,3,3,3,
3,3,3,3,3,3,3,3,3,3,3,3,3,3,3,3,3,3,3,3,3,3,4),(-0.761903739928579,-0.737714840814909,
-0.705408016786385,-0.685226614670373,-0.676627161339419,-0.668738660960247,
-0.635678094311993,-0.604031530389268,-0.590186158673076,-0.583843379993958,
-0.578312161070379,-0.543995147795815,-0.509206617715678,-0.474634013675463,
-0.451601905989146,-0.445054542245308,-0.439067220218037,-0.403526955466083,
-0.382505582930195,-0.348068670802762,-0.312989133154698,-0.301425205487243,
-0.296110141258073,-0.261171717718659,-0.225140081955213,-0.188826370911274,
-0.165223074547365,-0.15245028863213,-0.147771515823046,-0.110734161208511,
-0.0736990584503352,-0.0368495292251676,0.),.UNSPECIFIED.);
#641=B_SPLINE_CURVE_WITH_KNOTS('',3,(#37345,#37346,#37347,#37348,#37349,
#37350,#37351),.UNSPECIFIED.,.F.,.F.,(4,3,4),(158.388651680658,158.598858328231,
159.096033432709),.UNSPECIFIED.);
#642=B_SPLINE_CURVE_WITH_KNOTS('',3,(#37359,#37360,#37361,#37362,#37363,
#37364,#37365,#37366,#37367,#37368,#37369,#37370,#37371,#37372,#37373,#37374),
 .UNSPECIFIED.,.F.,.F.,(4,3,3,3,3,4),(-157.079632679489,-156.610157910323,
-156.112982805845,-155.615807701368,-155.118632596891,-154.645421777951),
 .UNSPECIFIED.);
#643=B_SPLINE_CURVE_WITH_KNOTS('',3,(#37379,#37380,#37381,#37382,#37383,
#37384,#37385,#37386,#37387,#37388,#37389,#37390,#37391,#37392,#37393,#37394,
#37395,#37396,#37397,#37398,#37399,#37400,#37401,#37402,#37403,#37404,#37405,
#37406,#37407,#37408,#37409,#37410,#37411,#37412,#37413,#37414,#37415,#37416,
#37417,#37418,#37419,#37420,#37421),.UNSPECIFIED.,.F.,.F.,(4,3,3,3,3,3,
3,3,3,3,3,3,3,3,4),(152.105466373478,152.135581970028,152.632757074505,
153.129932178982,153.627107283459,154.124282387936,154.621457492414,155.118632596891,
155.615807701368,156.112982805845,156.610157910323,157.1073330148,157.604508119277,
158.101683223754,158.388651680658),.UNSPECIFIED.);
#644=B_SPLINE_CURVE_WITH_KNOTS('',3,(#37422,#37423,#37424,#37425,#37426,
#37427,#37428,#37429,#37430,#37431,#37432,#37433,#37434,#37435,#37436,#37437,
#37438,#37439,#37440,#37441,#37442,#37443,#37444,#37445,#37446,#37447,#37448,
#37449,#37450,#37451,#37452,#37453,#37454,#37455,#37456,#37457,#37458,#37459,
#37460,#37461,#37462,#37463,#37464),.UNSPECIFIED.,.F.,.F.,(4,3,3,3,3,3,
3,3,3,3,3,3,3,3,4),(-154.645421777951,-154.621457492414,-154.124282387936,
-153.627107283459,-153.129932178982,-152.632757074505,-152.135581970028,
-151.63840686555,-151.141231761073,-150.644056656596,-150.146881552119,
-149.649706447642,-149.152531343164,-148.655356238687,-148.362236470772),
 .UNSPECIFIED.);
#645=B_SPLINE_CURVE_WITH_KNOTS('',3,(#37469,#37470,#37471,#37472,#37473,
#37474,#37475,#37476,#37477,#37478,#37479,#37480,#37481,#37482,#37483,#37484,
#37485,#37486,#37487,#37488,#37489,#37490,#37491,#37492,#37493,#37494,#37495,
#37496,#37497,#37498,#37499,#37500,#37501,#37502,#37503,#37504,#37505,#37506,
#37507,#37508),.UNSPECIFIED.,.F.,.F.,(4,3,3,3,3,3,3,3,3,3,3,3,3,4),(145.822281066299,
146.169480716301,146.666655820778,147.163830925255,147.661006029733,148.15818113421,
148.655356238687,149.152531343164,149.649706447642,150.146881552119,150.644056656596,
151.141231761073,151.63840686555,152.105466373478),.UNSPECIFIED.);
#646=B_SPLINE_CURVE_WITH_KNOTS('',3,(#37509,#37510,#37511,#37512,#37513,
#37514,#37515,#37516,#37517,#37518,#37519,#37520,#37521,#37522,#37523,#37524,
#37525,#37526,#37527,#37528,#37529,#37530,#37531,#37532,#37533,#37534,#37535,
#37536,#37537,#37538,#37539,#37540,#37541,#37542,#37543,#37544,#37545,#37546,
#37547,#37548,#37549,#37550,#37551),.UNSPECIFIED.,.F.,.F.,(4,3,3,3,3,3,
3,3,3,3,3,3,3,3,4),(-148.362236470772,-148.15818113421,-147.661006029733,
-147.163830925255,-146.666655820778,-146.169480716301,-145.672305611824,
-145.175130507347,-144.677955402869,-144.180780298392,-143.683605193915,
-143.186430089438,-142.689254984961,-142.192079880483,-142.079051163592),
 .UNSPECIFIED.);
#647=B_SPLINE_CURVE_WITH_KNOTS('',3,(#37556,#37557,#37558,#37559,#37560,
#37561,#37562,#37563,#37564,#37565,#37566,#37567,#37568,#37569,#37570,#37571,
#37572,#37573,#37574,#37575,#37576,#37577,#37578,#37579,#37580,#37581,#37582,
#37583,#37584,#37585,#37586,#37587,#37588,#37589,#37590,#37591,#37592,#37593,
#37594,#37595,#37596,#37597,#37598),.UNSPECIFIED.,.F.,.F.,(4,3,3,3,3,3,
3,3,3,3,3,3,3,3,4),(139.539095759119,139.706204358097,140.203379462574,
140.700554567052,141.197729671529,141.694904776006,142.192079880483,142.689254984961,
143.186430089438,143.683605193915,144.180780298392,144.677955402869,145.175130507347,
145.672305611824,145.822281066299),.UNSPECIFIED.);
#648=B_SPLINE_CURVE_WITH_KNOTS('',3,(#37599,#37600,#37601,#37602,#37603,
#37604,#37605,#37606,#37607,#37608,#37609,#37610,#37611,#37612,#37613,#37614,
#37615,#37616,#37617,#37618,#37619,#37620,#37621,#37622,#37623,#37624,#37625,
#37626,#37627,#37628,#37629,#37630,#37631,#37632,#37633,#37634,#37635,#37636,
#37637,#37638),.UNSPECIFIED.,.F.,.F.,(4,3,3,3,3,3,3,3,3,3,3,3,3,4),(-142.079051163592,
-141.694904776006,-141.197729671529,-140.700554567052,-140.203379462574,
-139.706204358097,-139.20902925362,-138.711854149143,-138.214679044666,
-137.717503940188,-137.220328835711,-136.723153731234,-136.225978626757,
-135.795865856412),.UNSPECIFIED.);
#649=B_SPLINE_CURVE_WITH_KNOTS('',3,(#37643,#37644,#37645,#37646,#37647,
#37648,#37649,#37650,#37651,#37652,#37653,#37654,#37655,#37656,#37657,#37658,
#37659,#37660,#37661,#37662,#37663,#37664,#37665,#37666,#37667,#37668,#37669,
#37670,#37671,#37672,#37673,#37674,#37675,#37676,#37677,#37678,#37679,#37680,
#37681,#37682),.UNSPECIFIED.,.F.,.F.,(4,3,3,3,3,3,3,3,3,3,3,3,3,4),(133.255910451939,
133.740103104371,134.237278208848,134.734453313325,135.231628417802,135.72880352228,
136.225978626757,136.723153731234,137.220328835711,137.717503940188,138.214679044666,
138.711854149143,139.20902925362,139.539095759119),.UNSPECIFIED.);
#650=B_SPLINE_CURVE_WITH_KNOTS('',3,(#37683,#37684,#37685,#37686,#37687,
#37688,#37689,#37690,#37691,#37692,#37693,#37694,#37695,#37696,#37697,#37698,
#37699,#37700,#37701,#37702,#37703,#37704,#37705,#37706,#37707,#37708,#37709,
#37710,#37711,#37712,#37713,#37714,#37715,#37716,#37717,#37718,#37719,#37720,
#37721,#37722,#37723,#37724,#37725),.UNSPECIFIED.,.F.,.F.,(4,3,3,3,3,3,
3,3,3,3,3,3,3,3,4),(-135.795865856412,-135.72880352228,-135.231628417802,
-134.734453313325,-134.237278208848,-133.740103104371,-133.242927999893,
-132.745752895416,-132.248577790939,-131.751402686462,-131.254227581985,
-130.757052477507,-130.25987737303,-129.762702268553,-129.512680549233),
 .UNSPECIFIED.);
#651=B_SPLINE_CURVE_WITH_KNOTS('',3,(#37730,#37731,#37732,#37733,#37734,
#37735,#37736,#37737,#37738,#37739,#37740,#37741,#37742,#37743,#37744,#37745,
#37746,#37747,#37748,#37749,#37750,#37751,#37752,#37753,#37754,#37755,#37756,
#37757,#37758,#37759,#37760,#37761,#37762,#37763,#37764,#37765,#37766,#37767,
#37768,#37769,#37770,#37771,#37772),.UNSPECIFIED.,.F.,.F.,(4,3,3,3,3,3,
3,3,3,3,3,3,3,3,4),(126.97272514476,127.276826746167,127.774001850644,128.271176955121,
128.768352059598,129.265527164076,129.762702268553,130.25987737303,130.757052477507,
131.254227581985,131.751402686462,132.248577790939,132.745752895416,133.242927999893,
133.255910451939),.UNSPECIFIED.);
#652=B_SPLINE_CURVE_WITH_KNOTS('',3,(#37773,#37774,#37775,#37776,#37777,
#37778,#37779,#37780,#37781,#37782,#37783,#37784,#37785,#37786,#37787,#37788,
#37789,#37790,#37791,#37792,#37793,#37794,#37795,#37796,#37797,#37798,#37799,
#37800,#37801,#37802,#37803,#37804,#37805,#37806,#37807,#37808,#37809,#37810,
#37811,#37812,#37813,#37814,#37815),.UNSPECIFIED.,.F.,.F.,(4,3,3,3,3,3,
3,3,3,3,3,3,3,3,4),(-129.512680549233,-129.265527164076,-128.768352059599,
-128.271176955121,-127.774001850644,-127.276826746167,-126.77965164169,
-126.282476537213,-125.785301432735,-125.288126328258,-124.790951223781,
-124.293776119304,-123.796601014826,-123.299425910349,-123.229495242054),
 .UNSPECIFIED.);
#653=B_SPLINE_CURVE_WITH_KNOTS('',3,(#37820,#37821,#37822,#37823,#37824,
#37825,#37826,#37827,#37828,#37829,#37830,#37831,#37832,#37833,#37834,#37835,
#37836,#37837,#37838,#37839,#37840,#37841,#37842,#37843,#37844,#37845,#37846,
#37847,#37848,#37849,#37850,#37851,#37852,#37853,#37854,#37855,#37856,#37857,
#37858,#37859,#37860,#37861,#37862),.UNSPECIFIED.,.F.,.F.,(4,3,3,3,3,3,
3,3,3,3,3,3,3,3,4),(120.68953983758,120.813550387963,121.31072549244,121.807900596918,
122.305075701395,122.802250805872,123.299425910349,123.796601014826,124.293776119304,
124.790951223781,125.288126328258,125.785301432735,126.282476537212,126.77965164169,
126.97272514476),.UNSPECIFIED.);
#654=B_SPLINE_CURVE_WITH_KNOTS('',3,(#37863,#37864,#37865,#37866,#37867,
#37868,#37869,#37870,#37871,#37872,#37873,#37874,#37875,#37876,#37877,#37878,
#37879,#37880,#37881,#37882,#37883,#37884,#37885,#37886,#37887,#37888,#37889,
#37890,#37891,#37892,#37893,#37894,#37895,#37896,#37897,#37898,#37899,#37900,
#37901,#37902),.UNSPECIFIED.,.F.,.F.,(4,3,3,3,3,3,3,3,3,3,3,3,3,4),(-123.229495242054,
-122.802250805872,-122.305075701395,-121.807900596918,-121.31072549244,
-120.813550387963,-120.316375283486,-119.819200179009,-119.322025074531,
-118.824849970054,-118.327674865577,-117.8304997611,-117.333324656623,-116.946309934874),
 .UNSPECIFIED.);
#655=B_SPLINE_CURVE_WITH_KNOTS('',3,(#37907,#37908,#37909,#37910,#37911,
#37912,#37913,#37914,#37915,#37916,#37917,#37918,#37919,#37920,#37921,#37922,
#37923,#37924,#37925,#37926,#37927,#37928,#37929,#37930,#37931,#37932,#37933,
#37934,#37935,#37936,#37937,#37938,#37939,#37940,#37941,#37942,#37943,#37944,
#37945,#37946),.UNSPECIFIED.,.F.,.F.,(4,3,3,3,3,3,3,3,3,3,3,3,3,4),(114.406354530401,
114.847449134237,115.344624238714,115.841799343191,116.338974447668,116.836149552145,
117.333324656623,117.8304997611,118.327674865577,118.824849970054,119.322025074531,
119.819200179009,120.316375283486,120.68953983758),.UNSPECIFIED.);
#656=B_SPLINE_CURVE_WITH_KNOTS('',3,(#37947,#37948,#37949,#37950,#37951,
#37952,#37953,#37954,#37955,#37956,#37957,#37958,#37959,#37960,#37961,#37962,
#37963,#37964,#37965,#37966,#37967,#37968,#37969,#37970,#37971,#37972,#37973,
#37974,#37975,#37976,#37977,#37978,#37979,#37980,#37981,#37982,#37983,#37984,
#37985,#37986,#37987,#37988,#37989),.UNSPECIFIED.,.F.,.F.,(4,3,3,3,3,3,
3,3,3,3,3,3,3,3,4),(-116.946309934874,-116.836149552145,-116.338974447668,
-115.841799343191,-115.344624238714,-114.847449134237,-114.350274029759,
-113.853098925282,-113.355923820805,-112.858748716328,-112.36157361185,
-111.864398507373,-111.367223402896,-110.870048298419,-110.663124627694),
 .UNSPECIFIED.);
#657=B_SPLINE_CURVE_WITH_KNOTS('',3,(#37994,#37995,#37996,#37997,#37998,
#37999,#38000,#38001,#38002,#38003,#38004,#38005,#38006,#38007,#38008,#38009,
#38010,#38011,#38012,#38013,#38014,#38015,#38016,#38017,#38018,#38019,#38020,
#38021,#38022,#38023,#38024,#38025,#38026,#38027,#38028,#38029,#38030,#38031,
#38032,#38033,#38034,#38035,#38036),.UNSPECIFIED.,.F.,.F.,(4,3,3,3,3,3,
3,3,3,3,3,3,3,3,4),(108.123169223221,108.384172776033,108.88134788051,109.378522984987,
109.875698089464,110.372873193942,110.870048298419,111.367223402896,111.864398507373,
112.36157361185,112.858748716328,113.355923820805,113.853098925282,114.350274029759,
114.406354530401),.UNSPECIFIED.);
#658=B_SPLINE_CURVE_WITH_KNOTS('',3,(#38037,#38038,#38039,#38040,#38041,
#38042,#38043,#38044,#38045,#38046,#38047,#38048,#38049,#38050,#38051,#38052,
#38053,#38054,#38055,#38056,#38057,#38058,#38059,#38060,#38061,#38062,#38063,
#38064,#38065,#38066,#38067,#38068,#38069,#38070,#38071,#38072,#38073,#38074,
#38075,#38076,#38077,#38078,#38079),.UNSPECIFIED.,.F.,.F.,(4,3,3,3,3,3,
3,3,3,3,3,3,3,3,4),(-110.663124627694,-110.372873193942,-109.875698089464,
-109.378522984987,-108.88134788051,-108.384172776033,-107.886997671556,
-107.389822567078,-106.892647462601,-106.395472358124,-105.898297253647,
-105.401122149169,-104.903947044692,-104.406771940215,-104.379939320514),
 .UNSPECIFIED.);
#659=B_SPLINE_CURVE_WITH_KNOTS('',3,(#38084,#38085,#38086,#38087,#38088,
#38089,#38090,#38091,#38092,#38093,#38094,#38095,#38096,#38097,#38098,#38099,
#38100,#38101,#38102,#38103,#38104,#38105,#38106,#38107,#38108,#38109,#38110,
#38111,#38112,#38113,#38114,#38115,#38116,#38117,#38118,#38119,#38120,#38121,
#38122,#38123,#38124,#38125,#38126),.UNSPECIFIED.,.F.,.F.,(4,3,3,3,3,3,
3,3,3,3,3,3,3,3,4),(101.839983916041,101.920896417829,102.418071522306,
102.915246626783,103.412421731261,103.909596835738,104.406771940215,104.903947044692,
105.401122149169,105.898297253647,106.395472358124,106.892647462601,107.389822567078,
107.886997671556,108.123169223221),.UNSPECIFIED.);
#660=B_SPLINE_CURVE_WITH_KNOTS('',3,(#38127,#38128,#38129,#38130,#38131,
#38132,#38133,#38134,#38135,#38136,#38137,#38138,#38139,#38140,#38141,#38142,
#38143,#38144,#38145,#38146,#38147,#38148,#38149,#38150,#38151,#38152,#38153,
#38154,#38155,#38156,#38157,#38158,#38159,#38160,#38161,#38162,#38163,#38164,
#38165,#38166),.UNSPECIFIED.,.F.,.F.,(4,3,3,3,3,3,3,3,3,3,3,3,3,4),(-104.379939320514,
-103.909596835738,-103.412421731261,-102.915246626783,-102.418071522306,
-101.920896417829,-101.423721313352,-100.926546208875,-100.429371104397,
-99.9321959999201,-99.4350208954429,-98.9378457909657,-98.4406706864885,
-98.0967540133348),.UNSPECIFIED.);
#661=B_SPLINE_CURVE_WITH_KNOTS('',3,(#38171,#38172,#38173,#38174,#38175,
#38176,#38177,#38178,#38179,#38180,#38181,#38182,#38183,#38184,#38185,#38186,
#38187,#38188,#38189,#38190,#38191,#38192,#38193,#38194,#38195,#38196,#38197,
#38198,#38199,#38200,#38201,#38202,#38203,#38204,#38205,#38206,#38207,#38208,
#38209,#38210),.UNSPECIFIED.,.F.,.F.,(4,3,3,3,3,3,3,3,3,3,3,3,3,4),(95.5567986088618,
95.9547951641024,96.4519702685796,96.9491453730568,97.446320477534,97.9434955820112,
98.4406706864884,98.9378457909657,99.4350208954429,99.9321959999201,100.429371104397,
100.926546208875,101.423721313352,101.839983916041),.UNSPECIFIED.);
#662=B_SPLINE_CURVE_WITH_KNOTS('',3,(#38211,#38212,#38213,#38214,#38215,
#38216,#38217,#38218,#38219,#38220,#38221,#38222,#38223,#38224,#38225,#38226,
#38227,#38228,#38229,#38230,#38231,#38232,#38233,#38234,#38235,#38236,#38237,
#38238,#38239,#38240,#38241,#38242,#38243,#38244,#38245,#38246,#38247,#38248,
#38249,#38250,#38251,#38252,#38253),.UNSPECIFIED.,.F.,.F.,(4,3,3,3,3,3,
3,3,3,3,3,3,3,3,4),(-98.0967540133348,-97.9434955820113,-97.446320477534,
-96.9491453730568,-96.4519702685796,-95.9547951641024,-95.4576200596252,
-94.960444955148,-94.4632698506707,-93.9660947461935,-93.4689196417163,
-92.9717445372391,-92.4745694327619,-91.9773943282847,-91.8135687061551),
 .UNSPECIFIED.);
#663=B_SPLINE_CURVE_WITH_KNOTS('',3,(#38258,#38259,#38260,#38261,#38262,
#38263,#38264,#38265,#38266,#38267,#38268,#38269,#38270,#38271,#38272,#38273,
#38274,#38275,#38276,#38277,#38278,#38279,#38280,#38281,#38282,#38283,#38284,
#38285,#38286,#38287,#38288,#38289,#38290,#38291,#38292,#38293,#38294,#38295,
#38296,#38297,#38298,#38299,#38300),.UNSPECIFIED.,.F.,.F.,(4,3,3,3,3,3,
3,3,3,3,3,3,3,3,4),(89.2736133016821,89.4915188058986,89.9886939103758,
90.485869014853,90.9830441193302,91.4802192238075,91.9773943282847,92.4745694327619,
92.9717445372391,93.4689196417163,93.9660947461935,94.4632698506707,94.9604449551479,
95.4576200596252,95.5567986088618),.UNSPECIFIED.);
#664=B_SPLINE_CURVE_WITH_KNOTS('',3,(#38301,#38302,#38303,#38304,#38305,
#38306,#38307,#38308,#38309,#38310,#38311,#38312,#38313,#38314,#38315,#38316,
#38317,#38318,#38319,#38320,#38321,#38322,#38323,#38324,#38325,#38326,#38327,
#38328,#38329,#38330,#38331,#38332,#38333,#38334,#38335,#38336,#38337,#38338,
#38339,#38340),.UNSPECIFIED.,.F.,.F.,(4,3,3,3,3,3,3,3,3,3,3,3,3,4),(-91.8135687061551,
-91.4802192238075,-90.9830441193302,-90.485869014853,-89.9886939103758,
-89.4915188058986,-88.9943437014214,-88.4971685969442,-87.9999934924669,
-87.5028183879897,-87.0056432835125,-86.5084681790353,-86.0112930745581,
-85.5303833989759),.UNSPECIFIED.);
#665=B_SPLINE_CURVE_WITH_KNOTS('',3,(#38345,#38346,#38347,#38348,#38349,
#38350,#38351,#38352,#38353,#38354,#38355,#38356,#38357,#38358,#38359,#38360,
#38361,#38362,#38363,#38364,#38365,#38366,#38367,#38368,#38369,#38370,#38371,
#38372,#38373,#38374,#38375,#38376,#38377,#38378,#38379,#38380,#38381,#38382,
#38383,#38384,#38385,#38386,#38387),.UNSPECIFIED.,.F.,.F.,(4,3,3,3,3,3,
3,3,3,3,3,3,3,3,4),(82.9904279945029,83.0282424476948,83.525417552172,84.0225926566493,
84.5197677611265,85.0169428656037,85.5141179700809,86.0112930745581,86.5084681790353,
87.0056432835125,87.5028183879897,87.9999934924669,88.4971685969441,88.9943437014214,
89.2736133016821),.UNSPECIFIED.);
#666=B_SPLINE_CURVE_WITH_KNOTS('',3,(#38388,#38389,#38390,#38391,#38392,
#38393,#38394,#38395,#38396,#38397,#38398,#38399,#38400,#38401,#38402,#38403,
#38404,#38405,#38406,#38407,#38408,#38409,#38410,#38411,#38412,#38413,#38414,
#38415,#38416,#38417,#38418,#38419,#38420,#38421,#38422,#38423,#38424,#38425,
#38426,#38427,#38428,#38429,#38430),.UNSPECIFIED.,.F.,.F.,(4,3,3,3,3,3,
3,3,3,3,3,3,3,3,4),(-85.5303833989759,-85.5141179700809,-85.0169428656037,
-84.5197677611264,-84.0225926566492,-83.525417552172,-83.0282424476948,
-82.5310673432176,-82.0338922387404,-81.5367171342632,-81.039542029786,
-80.5423669253087,-80.0451918208315,-79.5480167163543,-79.2471980917962),
 .UNSPECIFIED.);
#667=B_SPLINE_CURVE_WITH_KNOTS('',3,(#38435,#38436,#38437,#38438,#38439,
#38440,#38441,#38442,#38443,#38444,#38445,#38446,#38447,#38448,#38449,#38450,
#38451,#38452,#38453,#38454,#38455,#38456,#38457,#38458,#38459,#38460,#38461,
#38462,#38463,#38464,#38465,#38466,#38467,#38468,#38469,#38470,#38471,#38472,
#38473,#38474),.UNSPECIFIED.,.F.,.F.,(4,3,3,3,3,3,3,3,3,3,3,3,3,4),(76.7072426873232,
77.0621411939682,77.5593162984454,78.0564914029227,78.5536665073999,79.0508416118771,
79.5480167163543,80.0451918208315,80.5423669253087,81.0395420297859,81.5367171342632,
82.0338922387404,82.5310673432176,82.9904279945029),.UNSPECIFIED.);
#668=B_SPLINE_CURVE_WITH_KNOTS('',3,(#38475,#38476,#38477,#38478,#38479,
#38480,#38481,#38482,#38483,#38484,#38485,#38486,#38487,#38488,#38489,#38490,
#38491,#38492,#38493,#38494,#38495,#38496,#38497,#38498,#38499,#38500,#38501,
#38502,#38503,#38504,#38505,#38506,#38507,#38508,#38509,#38510,#38511,#38512,
#38513,#38514,#38515,#38516,#38517),.UNSPECIFIED.,.F.,.F.,(4,3,3,3,3,3,
3,3,3,3,3,3,3,3,4),(-79.2471980917962,-79.0508416118771,-78.5536665073999,
-78.0564914029227,-77.5593162984455,-77.0621411939683,-76.564966089491,
-76.0677909850138,-75.5706158805366,-75.0734407760594,-74.5762656715822,
-74.079090567105,-73.5819154626277,-73.0847403581505,-72.9640127846165),
 .UNSPECIFIED.);
#669=B_SPLINE_CURVE_WITH_KNOTS('',3,(#38522,#38523,#38524,#38525,#38526,
#38527,#38528,#38529,#38530,#38531,#38532,#38533,#38534,#38535,#38536,#38537,
#38538,#38539,#38540,#38541,#38542,#38543,#38544,#38545,#38546,#38547,#38548,
#38549,#38550,#38551,#38552,#38553,#38554,#38555,#38556,#38557,#38558,#38559,
#38560,#38561,#38562,#38563,#38564),.UNSPECIFIED.,.F.,.F.,(4,3,3,3,3,3,
3,3,3,3,3,3,3,3,4),(70.4240573801435,70.5988648357644,71.0960399402417,
71.5932150447189,72.0903901491961,72.5875652536733,73.0847403581505,73.5819154626277,
74.0790905671049,74.5762656715822,75.0734407760594,75.5706158805366,76.0677909850138,
76.564966089491,76.7072426873232),.UNSPECIFIED.);
#670=B_SPLINE_CURVE_WITH_KNOTS('',3,(#38565,#38566,#38567,#38568,#38569,
#38570,#38571,#38572,#38573,#38574,#38575,#38576,#38577,#38578,#38579,#38580,
#38581,#38582,#38583,#38584,#38585,#38586,#38587,#38588,#38589,#38590,#38591,
#38592,#38593,#38594,#38595,#38596,#38597,#38598,#38599,#38600,#38601,#38602,
#38603,#38604),.UNSPECIFIED.,.F.,.F.,(4,3,3,3,3,3,3,3,3,3,3,3,3,4),(-72.9640127846165,
-72.5875652536733,-72.0903901491961,-71.5932150447189,-71.0960399402417,
-70.5988648357645,-70.1016897312873,-69.60451462681,-69.1073395223328,-68.6101644178556,
-68.1129893133784,-67.6158142089012,-67.1186391044239,-66.6808274774369),
 .UNSPECIFIED.);
#671=B_SPLINE_CURVE_WITH_KNOTS('',3,(#38609,#38610,#38611,#38612,#38613,
#38614,#38615,#38616,#38617,#38618,#38619,#38620,#38621,#38622,#38623,#38624,
#38625,#38626,#38627,#38628,#38629,#38630,#38631,#38632,#38633,#38634,#38635,
#38636,#38637,#38638,#38639,#38640,#38641,#38642,#38643,#38644,#38645,#38646,
#38647,#38648),.UNSPECIFIED.,.F.,.F.,(4,3,3,3,3,3,3,3,3,3,3,3,3,4),(64.1408720729639,
64.6327635820379,65.1299386865151,65.6271137909923,66.1242888954695,66.6214639999467,
67.1186391044239,67.6158142089012,68.1129893133784,68.6101644178556,69.1073395223328,
69.60451462681,70.1016897312872,70.4240573801435),.UNSPECIFIED.);
#672=B_SPLINE_CURVE_WITH_KNOTS('',3,(#38649,#38650,#38651,#38652,#38653,
#38654,#38655,#38656,#38657,#38658,#38659,#38660,#38661,#38662,#38663,#38664,
#38665,#38666,#38667,#38668,#38669,#38670,#38671,#38672,#38673,#38674,#38675,
#38676,#38677,#38678,#38679,#38680,#38681,#38682,#38683,#38684,#38685,#38686,
#38687,#38688,#38689,#38690,#38691),.UNSPECIFIED.,.F.,.F.,(4,3,3,3,3,3,
3,3,3,3,3,3,3,3,4),(-66.6808274774369,-66.6214639999467,-66.1242888954695,
-65.6271137909923,-65.1299386865151,-64.6327635820379,-64.1355884775607,
-63.6384133730835,-63.1412382686062,-62.644063164129,-62.1468880596518,
-61.6497129551746,-61.1525378506974,-60.6553627462202,-60.3976421702572),
 .UNSPECIFIED.);
#673=B_SPLINE_CURVE_WITH_KNOTS('',3,(#38696,#38697,#38698,#38699,#38700,
#38701,#38702,#38703,#38704,#38705,#38706,#38707,#38708,#38709,#38710,#38711,
#38712,#38713,#38714,#38715,#38716,#38717,#38718,#38719,#38720,#38721,#38722,
#38723,#38724,#38725,#38726,#38727,#38728,#38729,#38730,#38731,#38732,#38733,
#38734,#38735,#38736,#38737,#38738),.UNSPECIFIED.,.F.,.F.,(4,3,3,3,3,3,
3,3,3,3,3,3,3,3,4),(57.8576867657842,58.1694872238341,58.6666623283113,
59.1638374327885,59.6610125372657,60.1581876417429,60.6553627462201,61.1525378506974,
61.6497129551746,62.1468880596518,62.644063164129,63.1412382686062,63.6384133730835,
64.1355884775607,64.1408720729639),.UNSPECIFIED.);
#674=B_SPLINE_CURVE_WITH_KNOTS('',3,(#38739,#38740,#38741,#38742,#38743,
#38744,#38745,#38746,#38747,#38748,#38749,#38750,#38751,#38752,#38753,#38754,
#38755,#38756,#38757,#38758,#38759,#38760,#38761,#38762,#38763,#38764,#38765,
#38766,#38767,#38768,#38769,#38770,#38771,#38772,#38773,#38774,#38775,#38776,
#38777,#38778,#38779,#38780,#38781),.UNSPECIFIED.,.F.,.F.,(4,3,3,3,3,3,
3,3,3,3,3,3,3,3,4),(-60.3976421702572,-60.158187641743,-59.6610125372657,
-59.1638374327885,-58.6666623283113,-58.1694872238341,-57.6723121193569,
-57.1751370148797,-56.6779619104025,-56.1807868059252,-55.683611701448,
-55.1864365969708,-54.6892614924936,-54.1920863880164,-54.114456863078),
 .UNSPECIFIED.);
#675=B_SPLINE_CURVE_WITH_KNOTS('',3,(#38786,#38787,#38788,#38789,#38790,
#38791,#38792,#38793,#38794,#38795,#38796,#38797,#38798,#38799,#38800,#38801,
#38802,#38803,#38804,#38805,#38806,#38807,#38808,#38809,#38810,#38811,#38812,
#38813,#38814,#38815,#38816,#38817,#38818,#38819,#38820,#38821,#38822,#38823,
#38824,#38825,#38826,#38827,#38828),.UNSPECIFIED.,.F.,.F.,(4,3,3,3,3,3,
3,3,3,3,3,3,3,3,4),(51.5745014586045,51.7062108656303,52.2033859701075,
52.7005610745847,53.1977361790619,53.6949112835391,54.1920863880164,54.6892614924936,
55.1864365969708,55.683611701448,56.1807868059252,56.6779619104024,57.1751370148797,
57.6723121193569,57.8576867657842),.UNSPECIFIED.);
#676=B_SPLINE_CURVE_WITH_KNOTS('',3,(#38829,#38830,#38831,#38832,#38833,
#38834,#38835,#38836,#38837,#38838,#38839,#38840,#38841,#38842,#38843,#38844,
#38845,#38846,#38847,#38848,#38849,#38850,#38851,#38852,#38853,#38854,#38855,
#38856,#38857,#38858,#38859,#38860,#38861,#38862,#38863,#38864,#38865,#38866,
#38867,#38868),.UNSPECIFIED.,.F.,.F.,(4,3,3,3,3,3,3,3,3,3,3,3,3,4),(-54.114456863078,
-53.6949112835392,-53.197736179062,-52.7005610745847,-52.2033859701075,
-51.7062108656303,-51.2090357611531,-50.7118606566759,-50.2146855521987,
-49.7175104477215,-49.2203353432442,-48.723160238767,-48.2259851342898,
-47.8312715558983),.UNSPECIFIED.);
#677=B_SPLINE_CURVE_WITH_KNOTS('',3,(#38873,#38874,#38875,#38876,#38877,
#38878,#38879,#38880,#38881,#38882,#38883,#38884,#38885,#38886,#38887,#38888,
#38889,#38890,#38891,#38892,#38893,#38894,#38895,#38896,#38897,#38898,#38899,
#38900,#38901,#38902,#38903,#38904,#38905,#38906,#38907,#38908,#38909,#38910,
#38911,#38912),.UNSPECIFIED.,.F.,.F.,(4,3,3,3,3,3,3,3,3,3,3,3,3,4),(45.2913161514253,
45.7401096119037,46.2372847163809,46.7344598208582,47.2316349253354,47.7288100298126,
48.2259851342898,48.723160238767,49.2203353432442,49.7175104477214,50.2146855521987,
50.7118606566759,51.2090357611531,51.5745014586045),.UNSPECIFIED.);
#678=B_SPLINE_CURVE_WITH_KNOTS('',3,(#38913,#38914,#38915,#38916,#38917,
#38918,#38919,#38920,#38921,#38922,#38923,#38924,#38925,#38926,#38927,#38928,
#38929,#38930,#38931,#38932,#38933,#38934,#38935,#38936,#38937,#38938,#38939,
#38940,#38941,#38942,#38943,#38944,#38945,#38946,#38947,#38948,#38949,#38950,
#38951,#38952,#38953,#38954,#38955),.UNSPECIFIED.,.F.,.F.,(4,3,3,3,3,3,
3,3,3,3,3,3,3,3,4),(-47.8312715558983,-47.7288100298126,-47.2316349253354,
-46.7344598208582,-46.2372847163809,-45.7401096119037,-45.2429345074265,
-44.7457594029493,-44.2485842984721,-43.7514091939949,-43.2542340895177,
-42.7570589850404,-42.2598838805632,-41.762708776086,-41.5480862487186),
 .UNSPECIFIED.);
#679=B_SPLINE_CURVE_WITH_KNOTS('',3,(#38960,#38961,#38962,#38963,#38964,
#38965,#38966,#38967,#38968,#38969,#38970,#38971,#38972,#38973,#38974,#38975,
#38976,#38977,#38978,#38979,#38980,#38981,#38982,#38983,#38984,#38985,#38986,
#38987,#38988,#38989,#38990,#38991,#38992,#38993,#38994,#38995,#38996,#38997,
#38998,#38999,#39000,#39001,#39002),.UNSPECIFIED.,.F.,.F.,(4,3,3,3,3,3,
3,3,3,3,3,3,3,3,4),(39.0081308442456,39.2768332536999,39.7740083581771,
40.2711834626544,40.7683585671316,41.2655336716088,41.762708776086,42.2598838805632,
42.7570589850404,43.2542340895177,43.7514091939949,44.2485842984721,44.7457594029493,
45.2429345074265,45.2913161514253),.UNSPECIFIED.);
#680=B_SPLINE_CURVE_WITH_KNOTS('',3,(#39003,#39004,#39005,#39006,#39007,
#39008,#39009,#39010,#39011,#39012,#39013,#39014,#39015,#39016,#39017,#39018,
#39019,#39020,#39021,#39022,#39023,#39024,#39025,#39026,#39027,#39028,#39029,
#39030,#39031,#39032,#39033,#39034,#39035,#39036,#39037,#39038,#39039,#39040,
#39041,#39042,#39043,#39044,#39045),.UNSPECIFIED.,.F.,.F.,(4,3,3,3,3,3,
3,3,3,3,3,3,3,3,4),(-41.5480862487186,-41.2655336716088,-40.7683585671316,
-40.2711834626544,-39.7740083581772,-39.2768332536999,-38.7796581492227,
-38.2824830447455,-37.7853079402683,-37.2881328357911,-36.7909577313139,
-36.2937826268367,-35.7966075223594,-35.2994324178822,-35.2649009415389),
 .UNSPECIFIED.);
#681=B_SPLINE_CURVE_WITH_KNOTS('',3,(#39050,#39051,#39052,#39053,#39054,
#39055,#39056,#39057,#39058,#39059,#39060,#39061,#39062,#39063,#39064,#39065,
#39066,#39067,#39068,#39069,#39070,#39071,#39072,#39073,#39074,#39075,#39076,
#39077,#39078,#39079,#39080,#39081,#39082,#39083,#39084,#39085,#39086,#39087,
#39088,#39089,#39090,#39091,#39092),.UNSPECIFIED.,.F.,.F.,(4,3,3,3,3,3,
3,3,3,3,3,3,3,3,4),(32.7249455370659,32.8135568954961,33.3107319999734,
33.8079071044506,34.3050822089278,34.802257313405,35.2994324178822,35.7966075223594,
36.2937826268367,36.7909577313139,37.2881328357911,37.7853079402683,38.2824830447455,
38.7796581492227,39.0081308442456),.UNSPECIFIED.);
#682=B_SPLINE_CURVE_WITH_KNOTS('',3,(#39093,#39094,#39095,#39096,#39097,
#39098,#39099,#39100,#39101,#39102,#39103,#39104,#39105,#39106,#39107,#39108,
#39109,#39110,#39111,#39112,#39113,#39114,#39115,#39116,#39117,#39118,#39119,
#39120,#39121,#39122,#39123,#39124,#39125,#39126,#39127,#39128,#39129,#39130,
#39131,#39132),.UNSPECIFIED.,.F.,.F.,(4,3,3,3,3,3,3,3,3,3,3,3,3,4),(-35.2649009415389,
-34.802257313405,-34.3050822089278,-33.8079071044506,-33.3107319999734,
-32.8135568954962,-32.3163817910189,-31.8192066865417,-31.3220315820645,
-30.8248564775873,-30.3276813731101,-29.8305062686329,-29.3333311641557,
-28.9817156343593),.UNSPECIFIED.);
#683=B_SPLINE_CURVE_WITH_KNOTS('',3,(#39137,#39138,#39139,#39140,#39141,
#39142,#39143,#39144,#39145,#39146,#39147,#39148,#39149,#39150,#39151,#39152,
#39153,#39154,#39155,#39156,#39157,#39158,#39159,#39160,#39161,#39162,#39163,
#39164,#39165,#39166,#39167,#39168,#39169,#39170,#39171,#39172,#39173,#39174,
#39175,#39176),.UNSPECIFIED.,.F.,.F.,(4,3,3,3,3,3,3,3,3,3,3,3,3,4),(26.4417602298863,
26.8474556417696,27.3446307462468,27.841805850724,28.3389809552012,28.8361560596784,
29.3333311641556,29.8305062686329,30.3276813731101,30.8248564775873,31.3220315820645,
31.8192066865417,32.3163817910189,32.7249455370659),.UNSPECIFIED.);
#684=B_SPLINE_CURVE_WITH_KNOTS('',3,(#39177,#39178,#39179,#39180,#39181,
#39182,#39183,#39184,#39185,#39186,#39187,#39188,#39189,#39190,#39191,#39192,
#39193,#39194,#39195,#39196,#39197,#39198,#39199,#39200,#39201,#39202,#39203,
#39204,#39205,#39206,#39207,#39208,#39209,#39210,#39211,#39212,#39213,#39214,
#39215,#39216,#39217,#39218,#39219),.UNSPECIFIED.,.F.,.F.,(4,3,3,3,3,3,
3,3,3,3,3,3,3,3,4),(-28.9817156343593,-28.8361560596784,-28.3389809552012,
-27.841805850724,-27.3446307462468,-26.8474556417696,-26.3502805372924,
-25.8531054328152,-25.3559303283379,-24.8587552238607,-24.3615801193835,
-23.8644050149063,-23.3672299104291,-22.8700548059519,-22.69853032718),
 .UNSPECIFIED.);
#685=B_SPLINE_CURVE_WITH_KNOTS('',3,(#39224,#39225,#39226,#39227,#39228,
#39229,#39230,#39231,#39232,#39233,#39234,#39235,#39236,#39237,#39238,#39239,
#39240,#39241,#39242,#39243,#39244,#39245,#39246,#39247,#39248,#39249,#39250,
#39251,#39252,#39253,#39254,#39255,#39256,#39257,#39258,#39259,#39260,#39261,
#39262,#39263,#39264,#39265,#39266),.UNSPECIFIED.,.F.,.F.,(4,3,3,3,3,3,
3,3,3,3,3,3,3,3,4),(20.1585749227066,20.3841792835658,20.881354388043,21.3785294925202,
21.8757045969974,22.3728797014746,22.8700548059519,23.3672299104291,23.8644050149063,
24.3615801193835,24.8587552238607,25.3559303283379,25.8531054328151,26.3502805372924,
26.4417602298863),.UNSPECIFIED.);
#686=B_SPLINE_CURVE_WITH_KNOTS('',3,(#39267,#39268,#39269,#39270,#39271,
#39272,#39273,#39274,#39275,#39276,#39277,#39278,#39279,#39280,#39281,#39282,
#39283,#39284,#39285,#39286,#39287,#39288,#39289,#39290,#39291,#39292,#39293,
#39294,#39295,#39296,#39297,#39298,#39299,#39300,#39301,#39302,#39303,#39304,
#39305,#39306),.UNSPECIFIED.,.F.,.F.,(4,3,3,3,3,3,3,3,3,3,3,3,3,4),(-22.69853032718,
-22.3728797014747,-21.8757045969974,-21.3785294925202,-20.881354388043,
-20.3841792835658,-19.8870041790886,-19.3898290746114,-18.8926539701342,
-18.3954788656569,-17.8983037611797,-17.4011286567025,-16.9039535522253,
-16.4153450200004),.UNSPECIFIED.);
#687=B_SPLINE_CURVE_WITH_KNOTS('',3,(#39311,#39312,#39313,#39314,#39315,
#39316,#39317,#39318,#39319,#39320,#39321,#39322,#39323,#39324,#39325,#39326,
#39327,#39328,#39329,#39330,#39331,#39332,#39333,#39334,#39335,#39336,#39337,
#39338,#39339,#39340,#39341,#39342,#39343,#39344,#39345,#39346,#39347,#39348,
#39349,#39350,#39351,#39352,#39353),.UNSPECIFIED.,.F.,.F.,(4,3,3,3,3,3,
3,3,3,3,3,3,3,3,4),(13.8753896155273,13.920902925362,14.4180780298392,14.9152531343164,
15.4124282387936,15.9096033432709,16.4067784477481,16.9039535522253,17.4011286567025,
17.8983037611797,18.3954788656569,18.8926539701341,19.3898290746114,19.8870041790886,
20.1585749227066),.UNSPECIFIED.);
#688=B_SPLINE_CURVE_WITH_KNOTS('',3,(#39354,#39355,#39356,#39357,#39358,
#39359,#39360,#39361,#39362,#39363,#39364,#39365,#39366,#39367,#39368,#39369,
#39370,#39371,#39372,#39373,#39374,#39375,#39376,#39377,#39378,#39379,#39380,
#39381,#39382,#39383,#39384,#39385,#39386,#39387,#39388,#39389,#39390,#39391,
#39392,#39393,#39394,#39395,#39396),.UNSPECIFIED.,.F.,.F.,(4,3,3,3,3,3,
3,3,3,3,3,3,3,3,4),(-16.4153450200004,-16.4067784477481,-15.9096033432709,
-15.4124282387936,-14.9152531343164,-14.4180780298392,-13.920902925362,
-13.4237278208848,-12.9265527164076,-12.4293776119304,-11.9322025074531,
-11.4350274029759,-10.9378522984987,-10.4406771940215,-10.1321597128207),
 .UNSPECIFIED.);
#689=B_SPLINE_CURVE_WITH_KNOTS('',3,(#39402,#39403,#39404,#39405,#39406,
#39407,#39408,#39409,#39410,#39411,#39412,#39413,#39414,#39415,#39416,#39417,
#39418,#39419,#39420,#39421,#39422,#39423,#39424,#39425,#39426),
 .UNSPECIFIED.,.F.,.F.,(4,3,3,3,3,3,3,3,4),(-3.848974405641,-3.4802257313405,
-2.98305062686329,-2.48587552238607,-1.98870041790886,-1.49152531343164,
-0.99435020895443,-0.497175104477215,0.),.UNSPECIFIED.);
#690=B_SPLINE_CURVE_WITH_KNOTS('',3,(#39429,#39430,#39431,#39432,#39433,
#39434,#39435,#39436,#39437,#39438,#39439,#39440,#39441,#39442,#39443,#39444,
#39445,#39446,#39447,#39448,#39449,#39450,#39451,#39452,#39453,#39454,#39455,
#39456,#39457,#39458,#39459,#39460,#39461,#39462,#39463,#39464,#39465),
 .UNSPECIFIED.,.F.,.F.,(4,3,3,3,3,3,3,3,3,3,3,3,4),(2.01640075321939,2.48587552238607,
2.98305062686328,3.4802257313405,3.97740083581771,4.47457594029493,4.97175104477214,
5.46892614924935,5.96610125372657,6.46327635820378,6.960451462681,7.45762656715821,
7.59220430834767),.UNSPECIFIED.);
#691=B_SPLINE_CURVE_WITH_KNOTS('',3,(#39471,#39472,#39473,#39474,#39475,
#39476,#39477,#39478,#39479,#39480,#39481,#39482),.UNSPECIFIED.,.F.,.F.,
(4,1,1,1,1,1,1,1,1,4),(166.504410640259,166.977621459199,167.474796563676,
167.971971668153,168.46914677263,168.966321877108,169.463496981585,169.960672086062,
170.457847190539,170.955022295017),.UNSPECIFIED.);
#692=B_SPLINE_CURVE_WITH_KNOTS('',3,(#39485,#39486,#39487,#39488,#39489,
#39490,#39491,#39492,#39493,#39494,#39495,#39496,#39497,#39498),
 .UNSPECIFIED.,.F.,.F.,(4,1,1,1,1,1,1,1,1,1,1,4),(166.504410640259,166.534526236809,
167.031701341286,167.528876445763,168.02605155024,168.523226654717,169.020401759195,
169.517576863672,170.014751968149,170.511927072626,171.009102177104,171.47857694627),
 .UNSPECIFIED.);
#693=B_SPLINE_CURVE_WITH_KNOTS('',3,(#39503,#39504,#39505,#39506,#39507,
#39508,#39509,#39510,#39511,#39512,#39513,#39514,#39515,#39516,#39517,#39518,
#39519),.UNSPECIFIED.,.F.,.F.,(4,1,1,1,1,1,1,1,1,1,1,1,1,1,4),(160.22122533308,
160.514345100995,161.011520205472,161.508695309949,162.005870414427,162.503045518904,
163.000220623381,163.497395727858,163.994570832336,164.491745936813,164.98892104129,
165.486096145767,165.983271250244,166.480446354722,166.504410640259),
 .UNSPECIFIED.);
#694=B_SPLINE_CURVE_WITH_KNOTS('',3,(#39520,#39521,#39522,#39523,#39524,
#39525,#39526,#39527,#39528,#39529,#39530,#39531,#39532,#39533,#39534,#39535),
 .UNSPECIFIED.,.F.,.F.,(4,1,1,1,1,1,1,1,1,1,1,1,1,4),(160.22122533308,160.568424983082,
161.065600087559,161.562775192036,162.059950296514,162.557125400991,163.054300505468,
163.551475609945,164.048650714422,164.5458258189,165.043000923377,165.540176027854,
166.037351132331,166.504410640259),.UNSPECIFIED.);
#695=B_SPLINE_CURVE_WITH_KNOTS('',3,(#39540,#39541,#39542,#39543,#39544,
#39545,#39546,#39547,#39548,#39549,#39550,#39551,#39552,#39553,#39554,#39555,
#39556),.UNSPECIFIED.,.F.,.F.,(4,1,1,1,1,1,1,1,1,1,1,1,1,1,4),(153.9380400259,
154.051068742791,154.548243847269,155.045418951746,155.542594056223,156.0397691607,
156.536944265177,157.034119369655,157.531294474132,158.028469578609,158.525644683086,
159.022819787563,159.519994892041,160.017169996518,160.22122533308),
 .UNSPECIFIED.);
#696=B_SPLINE_CURVE_WITH_KNOTS('',3,(#39557,#39558,#39559,#39560,#39561,
#39562,#39563,#39564,#39565,#39566,#39567,#39568,#39569,#39570,#39571,#39572,
#39573),.UNSPECIFIED.,.F.,.F.,(4,1,1,1,1,1,1,1,1,1,1,1,1,1,4),(153.9380400259,
154.105148624878,154.602323729355,155.099498833833,155.59667393831,156.093849042787,
156.591024147264,157.088199251742,157.585374356219,158.082549460696,158.579724565173,
159.07689966965,159.574074774128,160.071249878605,160.22122533308),
 .UNSPECIFIED.);
#697=B_SPLINE_CURVE_WITH_KNOTS('',3,(#39578,#39579,#39580,#39581,#39582,
#39583,#39584,#39585,#39586,#39587,#39588,#39589,#39590,#39591,#39592,#39593),
 .UNSPECIFIED.,.F.,.F.,(4,1,1,1,1,1,1,1,1,1,1,1,1,4),(147.65485471872,148.084967489065,
148.582142593542,149.079317698019,149.576492802496,150.073667906974,150.570843011451,
151.068018115928,151.565193220405,152.062368324882,152.55954342936,153.056718533837,
153.553893638314,153.9380400259),.UNSPECIFIED.);
#698=B_SPLINE_CURVE_WITH_KNOTS('',3,(#39594,#39595,#39596,#39597,#39598,
#39599,#39600,#39601,#39602,#39603,#39604,#39605,#39606,#39607,#39608,#39609),
 .UNSPECIFIED.,.F.,.F.,(4,1,1,1,1,1,1,1,1,1,1,1,1,4),(147.65485471872,148.139047371152,
148.636222475629,149.133397580106,149.630572684583,150.12774778906,150.624922893538,
151.122097998015,151.619273102492,152.116448206969,152.613623311447,153.110798415924,
153.607973520401,153.9380400259),.UNSPECIFIED.);
#699=B_SPLINE_CURVE_WITH_KNOTS('',3,(#39614,#39615,#39616,#39617,#39618,
#39619,#39620,#39621,#39622,#39623,#39624,#39625,#39626,#39627,#39628,#39629,
#39630),.UNSPECIFIED.,.F.,.F.,(4,1,1,1,1,1,1,1,1,1,1,1,1,1,4),(141.371669411541,
141.621691130861,142.118866235338,142.616041339815,143.113216444293,143.61039154877,
144.107566653247,144.604741757724,145.101916862201,145.599091966679,146.096267071156,
146.593442175633,147.09061728011,147.587792384587,147.65485471872),
 .UNSPECIFIED.);
#700=B_SPLINE_CURVE_WITH_KNOTS('',3,(#39631,#39632,#39633,#39634,#39635,
#39636,#39637,#39638,#39639,#39640,#39641,#39642,#39643,#39644,#39645,#39646,
#39647),.UNSPECIFIED.,.F.,.F.,(4,1,1,1,1,1,1,1,1,1,1,1,1,1,4),(141.371669411541,
141.675771012948,142.172946117425,142.670121221902,143.167296326379,143.664471430857,
144.161646535334,144.658821639811,145.155996744288,145.653171848766,146.150346953243,
146.64752205772,147.144697162197,147.641872266674,147.65485471872),
 .UNSPECIFIED.);
#701=B_SPLINE_CURVE_WITH_KNOTS('',3,(#39652,#39653,#39654,#39655,#39656,
#39657,#39658,#39659,#39660,#39661,#39662,#39663,#39664,#39665,#39666,#39667,
#39668),.UNSPECIFIED.,.F.,.F.,(4,1,1,1,1,1,1,1,1,1,1,1,1,1,4),(135.088484104361,
135.158414772657,135.655589877134,136.152764981612,136.649940086089,137.147115190566,
137.644290295043,138.14146539952,138.638640503998,139.135815608475,139.632990712952,
140.130165817429,140.627340921906,141.124516026384,141.371669411541),
 .UNSPECIFIED.);
#702=B_SPLINE_CURVE_WITH_KNOTS('',3,(#39669,#39670,#39671,#39672,#39673,
#39674,#39675,#39676,#39677,#39678,#39679,#39680,#39681,#39682,#39683,#39684,
#39685),.UNSPECIFIED.,.F.,.F.,(4,1,1,1,1,1,1,1,1,1,1,1,1,1,4),(135.088484104361,
135.212494654744,135.709669759221,136.206844863698,136.704019968176,137.201195072653,
137.69837017713,138.195545281607,138.692720386085,139.189895490562,139.687070595039,
140.184245699516,140.681420803993,141.178595908471,141.371669411541),
 .UNSPECIFIED.);
#703=B_SPLINE_CURVE_WITH_KNOTS('',3,(#39690,#39691,#39692,#39693,#39694,
#39695,#39696,#39697,#39698,#39699,#39700,#39701,#39702,#39703,#39704,#39705),
 .UNSPECIFIED.,.F.,.F.,(4,1,1,1,1,1,1,1,1,1,1,1,1,4),(128.805298797182,
129.192313518931,129.689488623408,130.186663727885,130.683838832362,131.181013936839,
131.678189041317,132.175364145794,132.672539250271,133.169714354748,133.666889459226,
134.164064563703,134.66123966818,135.088484104361),.UNSPECIFIED.);
#704=B_SPLINE_CURVE_WITH_KNOTS('',3,(#39706,#39707,#39708,#39709,#39710,
#39711,#39712,#39713,#39714,#39715,#39716,#39717,#39718,#39719,#39720,#39721),
 .UNSPECIFIED.,.F.,.F.,(4,1,1,1,1,1,1,1,1,1,1,1,1,4),(128.805298797182,
129.246393401017,129.743568505495,130.240743609972,130.737918714449,131.235093818926,
131.732268923404,132.229444027881,132.726619132358,133.223794236835,133.720969341312,
134.21814444579,134.715319550267,135.088484104361),.UNSPECIFIED.);
#705=B_SPLINE_CURVE_WITH_KNOTS('',3,(#39726,#39727,#39728,#39729,#39730,
#39731,#39732,#39733,#39734,#39735,#39736,#39737,#39738,#39739,#39740,#39741,
#39742),.UNSPECIFIED.,.F.,.F.,(4,1,1,1,1,1,1,1,1,1,1,1,1,1,4),(122.522113490002,
122.729037160727,123.226212265204,123.723387369681,124.220562474158,124.717737578636,
125.214912683113,125.71208778759,126.209262892067,126.706437996544,127.203613101022,
127.700788205499,128.197963309976,128.695138414453,128.805298797182),
 .UNSPECIFIED.);
#706=B_SPLINE_CURVE_WITH_KNOTS('',3,(#39743,#39744,#39745,#39746,#39747,
#39748,#39749,#39750,#39751,#39752,#39753,#39754,#39755,#39756,#39757,#39758,
#39759),.UNSPECIFIED.,.F.,.F.,(4,1,1,1,1,1,1,1,1,1,1,1,1,1,4),(122.522113490002,
122.783117042814,123.280292147291,123.777467251768,124.274642356245,124.771817460723,
125.2689925652,125.766167669677,126.263342774154,126.760517878631,127.257692983109,
127.754868087586,128.252043192063,128.74921829654,128.805298797182),
 .UNSPECIFIED.);
#707=B_SPLINE_CURVE_WITH_KNOTS('',3,(#39764,#39765,#39766,#39767,#39768,
#39769,#39770,#39771,#39772,#39773,#39774,#39775,#39776,#39777,#39778,#39779,
#39780),.UNSPECIFIED.,.F.,.F.,(4,1,1,1,1,1,1,1,1,1,1,1,1,1,4),(116.238928182822,
116.265760802523,116.762935907,117.260111011477,117.757286115955,118.254461220432,
118.751636324909,119.248811429386,119.745986533863,120.243161638341,120.740336742818,
121.237511847295,121.734686951772,122.23186205625,122.522113490002),
 .UNSPECIFIED.);
#708=B_SPLINE_CURVE_WITH_KNOTS('',3,(#39781,#39782,#39783,#39784,#39785,
#39786,#39787,#39788,#39789,#39790,#39791,#39792,#39793,#39794,#39795,#39796,
#39797),.UNSPECIFIED.,.F.,.F.,(4,1,1,1,1,1,1,1,1,1,1,1,1,1,4),(116.238928182822,
116.31984068461,116.817015789087,117.314190893564,117.811365998042,118.308541102519,
118.805716206996,119.302891311473,119.80006641595,120.297241520428,120.794416624905,
121.291591729382,121.788766833859,122.285941938336,122.522113490002),
 .UNSPECIFIED.);
#709=B_SPLINE_CURVE_WITH_KNOTS('',3,(#39802,#39803,#39804,#39805,#39806,
#39807,#39808,#39809,#39810,#39811,#39812,#39813,#39814,#39815,#39816,#39817),
 .UNSPECIFIED.,.F.,.F.,(4,1,1,1,1,1,1,1,1,1,1,1,1,4),(109.955742875643,
110.299659548796,110.796834653274,111.294009757751,111.791184862228,112.288359966705,
112.785535071182,113.28271017566,113.779885280137,114.277060384614,114.774235489091,
115.271410593569,115.768585698046,116.238928182822),.UNSPECIFIED.);
#710=B_SPLINE_CURVE_WITH_KNOTS('',3,(#39818,#39819,#39820,#39821,#39822,
#39823,#39824,#39825,#39826,#39827,#39828,#39829,#39830,#39831,#39832,#39833),
 .UNSPECIFIED.,.F.,.F.,(4,1,1,1,1,1,1,1,1,1,1,1,1,4),(109.955742875643,
110.353739430883,110.850914535361,111.348089639838,111.845264744315,112.342439848792,
112.839614953269,113.336790057747,113.833965162224,114.331140266701,114.828315371178,
115.325490475655,115.822665580133,116.238928182822),.UNSPECIFIED.);
#711=B_SPLINE_CURVE_WITH_KNOTS('',3,(#39838,#39839,#39840,#39841,#39842,
#39843,#39844,#39845,#39846,#39847,#39848,#39849,#39850,#39851,#39852,#39853,
#39854),.UNSPECIFIED.,.F.,.F.,(4,1,1,1,1,1,1,1,1,1,1,1,1,1,4),(103.672557568463,
103.836383190593,104.33355829507,104.830733399547,105.327908504024,105.825083608501,
106.322258712979,106.819433817456,107.316608921933,107.81378402641,108.310959130888,
108.808134235365,109.305309339842,109.802484444319,109.955742875643),
 .UNSPECIFIED.);
#712=B_SPLINE_CURVE_WITH_KNOTS('',3,(#39855,#39856,#39857,#39858,#39859,
#39860,#39861,#39862,#39863,#39864,#39865,#39866,#39867,#39868,#39869,#39870,
#39871),.UNSPECIFIED.,.F.,.F.,(4,1,1,1,1,1,1,1,1,1,1,1,1,1,4),(103.672557568463,
103.89046307268,104.387638177157,104.884813281634,105.381988386111,105.879163490588,
106.376338595066,106.873513699543,107.37068880402,107.867863908497,108.365039012974,
108.862214117452,109.359389221929,109.856564326406,109.955742875643),
 .UNSPECIFIED.);
#713=B_SPLINE_CURVE_WITH_KNOTS('',3,(#39876,#39877,#39878,#39879,#39880,
#39881,#39882,#39883,#39884,#39885,#39886,#39887,#39888,#39889,#39890,#39891),
 .UNSPECIFIED.,.F.,.F.,(4,1,1,1,1,1,1,1,1,1,1,1,1,4),(97.3893722612839,
97.870281936866,98.3674570413433,98.8646321458205,99.3618072502977,99.8589823547749,
100.356157459252,100.853332563729,101.350507668207,101.847682772684,102.344857877161,
102.842032981638,103.339208086115,103.672557568463),.UNSPECIFIED.);
#714=B_SPLINE_CURVE_WITH_KNOTS('',3,(#39892,#39893,#39894,#39895,#39896,
#39897,#39898,#39899,#39900,#39901,#39902,#39903,#39904,#39905,#39906,#39907,
#39908),.UNSPECIFIED.,.F.,.F.,(4,1,1,1,1,1,1,1,1,1,1,1,1,1,4),(97.3893722612839,
97.4271867144758,97.924361818953,98.4215369234302,98.9187120279074,99.4158871323846,
99.9130622368618,100.410237341339,100.907412445816,101.404587550293,101.901762654771,
102.398937759248,102.896112863725,103.393287968202,103.672557568463),
 .UNSPECIFIED.);
#715=B_SPLINE_CURVE_WITH_KNOTS('',3,(#39913,#39914,#39915,#39916,#39917,
#39918,#39919,#39920,#39921,#39922,#39923,#39924,#39925,#39926,#39927,#39928,
#39929),.UNSPECIFIED.,.F.,.F.,(4,1,1,1,1,1,1,1,1,1,1,1,1,1,4),(91.1061869541042,
91.4070055786623,91.9041806831395,92.4013557876167,92.8985308920939,93.3957059965711,
93.8928811010483,94.3900562055255,94.8872313100028,95.38440641448,95.8815815189572,
96.3787566234344,96.8759317279116,97.3731068323888,97.3893722612839),
 .UNSPECIFIED.);
#716=B_SPLINE_CURVE_WITH_KNOTS('',3,(#39930,#39931,#39932,#39933,#39934,
#39935,#39936,#39937,#39938,#39939,#39940,#39941,#39942,#39943,#39944,#39945),
 .UNSPECIFIED.,.F.,.F.,(4,1,1,1,1,1,1,1,1,1,1,1,1,4),(91.1061869541042,
91.4610854607492,91.9582605652264,92.4554356697036,92.9526107741808,93.449785878658,
93.9469609831353,94.4441360876125,94.9413111920897,95.4384862965669,95.9356614010441,
96.4328365055213,96.9300116099986,97.3893722612839),.UNSPECIFIED.);
#717=B_SPLINE_CURVE_WITH_KNOTS('',3,(#39950,#39951,#39952,#39953,#39954,
#39955,#39956,#39957,#39958,#39959,#39960,#39961,#39962,#39963,#39964,#39965,
#39966),.UNSPECIFIED.,.F.,.F.,(4,1,1,1,1,1,1,1,1,1,1,1,1,1,4),(84.8230016469245,
84.9437292204585,85.4409043249357,85.9380794294129,86.4352545338901,86.9324296383673,
87.4296047428445,87.9267798473217,88.423954951799,88.9211300562762,89.4183051607534,
89.9154802652306,90.4126553697078,90.909830474185,91.1061869541042),
 .UNSPECIFIED.);
#718=B_SPLINE_CURVE_WITH_KNOTS('',3,(#39967,#39968,#39969,#39970,#39971,
#39972,#39973,#39974,#39975,#39976,#39977,#39978,#39979,#39980,#39981,#39982,
#39983),.UNSPECIFIED.,.F.,.F.,(4,1,1,1,1,1,1,1,1,1,1,1,1,1,4),(84.8230016469245,
84.9978091025454,85.4949842070226,85.9921593114998,86.4893344159771,86.9865095204543,
87.4836846249315,87.9808597294087,88.4780348338859,88.9752099383631,89.4723850428403,
89.9695601473175,90.4667352517948,90.963910356272,91.1061869541042),
 .UNSPECIFIED.);
#719=B_SPLINE_CURVE_WITH_KNOTS('',3,(#39988,#39989,#39990,#39991,#39992,
#39993,#39994,#39995,#39996,#39997,#39998,#39999,#40000,#40001,#40002,#40003),
 .UNSPECIFIED.,.F.,.F.,(4,1,1,1,1,1,1,1,1,1,1,1,1,4),(78.5398163397448,
78.9776279667319,79.4748030712091,79.9719781756863,80.4691532801635,80.9663283846407,
81.463503489118,81.9606785935952,82.4578536980724,82.9550288025496,83.4522039070268,
83.949379011504,84.4465541159813,84.8230016469245),.UNSPECIFIED.);
#720=B_SPLINE_CURVE_WITH_KNOTS('',3,(#40004,#40005,#40006,#40007,#40008,
#40009,#40010,#40011,#40012,#40013,#40014,#40015,#40016,#40017,#40018,#40019),
 .UNSPECIFIED.,.F.,.F.,(4,1,1,1,1,1,1,1,1,1,1,1,1,4),(78.5398163397448,
79.0317078488188,79.528882953296,80.0260580577733,80.5232331622505,81.0204082667277,
81.5175833712049,82.0147584756821,82.5119335801593,83.0091086846365,83.5062837891138,
84.003458893591,84.5006339980682,84.8230016469245),.UNSPECIFIED.);
#721=B_SPLINE_CURVE_WITH_KNOTS('',3,(#40024,#40025,#40026,#40027,#40028,
#40029,#40030,#40031,#40032,#40033,#40034,#40035,#40036,#40037,#40038,#40039,
#40040),.UNSPECIFIED.,.F.,.F.,(4,1,1,1,1,1,1,1,1,1,1,1,1,1,4),(72.2566310325651,
72.5143516085281,73.0115267130053,73.5087018174825,74.0058769219598,74.503052026437,
75.0002271309142,75.4974022353914,75.9945773398686,76.4917524443458,76.988927548823,
77.4861026533003,77.9832777577775,78.4804528622547,78.5398163397448),
 .UNSPECIFIED.);
#722=B_SPLINE_CURVE_WITH_KNOTS('',3,(#40041,#40042,#40043,#40044,#40045,
#40046,#40047,#40048,#40049,#40050,#40051,#40052,#40053,#40054,#40055,#40056,
#40057),.UNSPECIFIED.,.F.,.F.,(4,1,1,1,1,1,1,1,1,1,1,1,1,1,4),(72.2566310325651,
72.568431490615,73.0656065950923,73.5627816995695,74.0599568040467,74.5571319085239,
75.0543070130011,75.5514821174783,76.0486572219556,76.5458323264328,77.04300743091,
77.5401825353872,78.0373576398644,78.5345327443416,78.5398163397448),
 .UNSPECIFIED.);
#723=B_SPLINE_CURVE_WITH_KNOTS('',3,(#40062,#40063,#40064,#40065,#40066,
#40067,#40068,#40069,#40070,#40071,#40072,#40073,#40074,#40075,#40076,#40077,
#40078),.UNSPECIFIED.,.F.,.F.,(4,1,1,1,1,1,1,1,1,1,1,1,1,1,4),(65.9734457253859,
66.0510752503243,66.5482503548015,67.0454254592788,67.542600563756,68.0397756682332,
68.5369507727104,69.0341258771876,69.5313009816648,70.028476086142,70.5256511906192,
71.0228262950965,71.5200013995737,72.0171765040509,72.2566310325651),
 .UNSPECIFIED.);
#724=B_SPLINE_CURVE_WITH_KNOTS('',3,(#40079,#40080,#40081,#40082,#40083,
#40084,#40085,#40086,#40087,#40088,#40089,#40090,#40091,#40092,#40093,#40094,
#40095),.UNSPECIFIED.,.F.,.F.,(4,1,1,1,1,1,1,1,1,1,1,1,1,1,4),(65.9734457253859,
66.1051551324113,66.6023302368885,67.0995053413657,67.5966804458429,68.0938555503201,
68.5910306547973,69.0882057592745,69.5853808637518,70.082555968229,70.5797310727062,
71.0769061771834,71.5740812816606,72.0712563861378,72.2566310325651),
 .UNSPECIFIED.);
#725=B_SPLINE_CURVE_WITH_KNOTS('',3,(#40100,#40101,#40102,#40103,#40104,
#40105,#40106,#40107,#40108,#40109,#40110,#40111,#40112,#40113,#40114,#40115),
 .UNSPECIFIED.,.F.,.F.,(4,1,1,1,1,1,1,1,1,1,1,1,1,4),(59.6902604182062,
60.0849739965977,60.582149101075,61.0793242055522,61.5764993100294,62.0736744145066,
62.5708495189838,63.068024623461,63.5651997279382,64.0623748324155,64.5595499368927,
65.0567250413699,65.5539001458471,65.9734457253859),.UNSPECIFIED.);
#726=B_SPLINE_CURVE_WITH_KNOTS('',3,(#40116,#40117,#40118,#40119,#40120,
#40121,#40122,#40123,#40124,#40125,#40126,#40127,#40128,#40129,#40130,#40131),
 .UNSPECIFIED.,.F.,.F.,(4,1,1,1,1,1,1,1,1,1,1,1,1,4),(59.6902604182062,
60.1390538786847,60.6362289831619,61.1334040876391,61.6305791921163,62.1277542965935,
62.6249294010708,63.122104505548,63.6192796100252,64.1164547145024,64.6136298189796,
65.1108049234568,65.607980027934,65.9734457253859),.UNSPECIFIED.);
#727=B_SPLINE_CURVE_WITH_KNOTS('',3,(#40136,#40137,#40138,#40139,#40140,
#40141,#40142,#40143,#40144,#40145,#40146,#40147,#40148,#40149,#40150,#40151,
#40152),.UNSPECIFIED.,.F.,.F.,(4,1,1,1,1,1,1,1,1,1,1,1,1,1,4),(53.4070751110266,
53.621697638394,54.1188727428712,54.6160478473484,55.1132229518256,55.6103980563028,
56.10757316078,56.6047482652572,57.1019233697345,57.5990984742117,58.0962735786889,
58.5934486831661,59.0906237876433,59.5877988921205,59.6902604182062),
 .UNSPECIFIED.);
#728=B_SPLINE_CURVE_WITH_KNOTS('',3,(#40153,#40154,#40155,#40156,#40157,
#40158,#40159,#40160,#40161,#40162,#40163,#40164,#40165,#40166,#40167,#40168,
#40169),.UNSPECIFIED.,.F.,.F.,(4,1,1,1,1,1,1,1,1,1,1,1,1,1,4),(53.4070751110266,
53.6757775204809,54.1729526249581,54.6701277294353,55.1673028339125,55.6644779383898,
56.161653042867,56.6588281473442,57.1560032518214,57.6531783562986,58.1503534607758,
58.647528565253,59.1447036697303,59.6418787742075,59.6902604182062),
 .UNSPECIFIED.);
#729=B_SPLINE_CURVE_WITH_KNOTS('',3,(#40174,#40175,#40176,#40177,#40178,
#40179,#40180,#40181,#40182,#40183,#40184,#40185,#40186,#40187,#40188,#40189,
#40190),.UNSPECIFIED.,.F.,.F.,(4,1,1,1,1,1,1,1,1,1,1,1,1,1,4),(47.1238898038469,
47.1584212801902,47.6555963846674,48.1527714891446,48.6499465936218,49.147121698099,
49.6442968025762,50.1414719070535,50.6386470115307,51.1358221160079,51.6329972204851,
52.1301723249623,52.6273474294395,53.1245225339167,53.4070751110266),
 .UNSPECIFIED.);
#730=B_SPLINE_CURVE_WITH_KNOTS('',3,(#40191,#40192,#40193,#40194,#40195,
#40196,#40197,#40198,#40199,#40200,#40201,#40202,#40203,#40204,#40205,#40206,
#40207),.UNSPECIFIED.,.F.,.F.,(4,1,1,1,1,1,1,1,1,1,1,1,1,1,4),(47.1238898038469,
47.2125011622771,47.7096762667543,48.2068513712315,48.7040264757088,49.201201580186,
49.6983766846632,50.1955517891404,50.6927268936176,51.1899019980948,51.687077102572,
52.1842522070493,52.6814273115265,53.1786024160037,53.4070751110266),
 .UNSPECIFIED.);
#731=B_SPLINE_CURVE_WITH_KNOTS('',3,(#40212,#40213,#40214,#40215,#40216,
#40217,#40218,#40219,#40220,#40221,#40222,#40223,#40224,#40225,#40226,#40227),
 .UNSPECIFIED.,.F.,.F.,(4,1,1,1,1,1,1,1,1,1,1,1,1,4),(40.8407044966672,
41.1923200264636,41.6894951309408,42.186670235418,42.6838453398952,43.1810204443725,
43.6781955488497,44.1753706533269,44.6725457578041,45.1697208622813,45.6668959667585,
46.1640710712357,46.661246175713,47.1238898038469),.UNSPECIFIED.);
#732=B_SPLINE_CURVE_WITH_KNOTS('',3,(#40228,#40229,#40230,#40231,#40232,
#40233,#40234,#40235,#40236,#40237,#40238,#40239,#40240,#40241,#40242,#40243),
 .UNSPECIFIED.,.F.,.F.,(4,1,1,1,1,1,1,1,1,1,1,1,1,4),(40.8407044966672,
41.2463999085505,41.7435750130278,42.240750117505,42.7379252219822,43.2351003264594,
43.7322754309366,44.2294505354138,44.726625639891,45.2238007443683,45.7209758488455,
46.2181509533227,46.7153260577999,47.1238898038469),.UNSPECIFIED.);
#733=B_SPLINE_CURVE_WITH_KNOTS('',3,(#40248,#40249,#40250,#40251,#40252,
#40253,#40254,#40255,#40256,#40257,#40258,#40259,#40260,#40261,#40262,#40263,
#40264),.UNSPECIFIED.,.F.,.F.,(4,1,1,1,1,1,1,1,1,1,1,1,1,1,4),(34.557519189488,
34.7290436682598,35.226218772737,35.7233938772142,36.2205689816915,36.7177440861687,
37.2149191906459,37.7120942951231,38.2092693996003,38.7064445040775,39.2036196085547,
39.700794713032,40.1979698175092,40.6951449219864,40.8407044966672),
 .UNSPECIFIED.);
#734=B_SPLINE_CURVE_WITH_KNOTS('',3,(#40265,#40266,#40267,#40268,#40269,
#40270,#40271,#40272,#40273,#40274,#40275,#40276,#40277,#40278,#40279,#40280,
#40281),.UNSPECIFIED.,.F.,.F.,(4,1,1,1,1,1,1,1,1,1,1,1,1,1,4),(34.557519189488,
34.7831235503468,35.280298654824,35.7774737593012,36.2746488637784,36.7718239682556,
37.2689990727328,37.76617417721,38.2633492816873,38.7605243861645,39.2576994906417,
39.7548745951189,40.2520496995961,40.7492248040733,40.8407044966672),
 .UNSPECIFIED.);
#735=B_SPLINE_CURVE_WITH_KNOTS('',3,(#40286,#40287,#40288,#40289,#40290,
#40291,#40292,#40293,#40294,#40295,#40296,#40297,#40298,#40299,#40300,#40301),
 .UNSPECIFIED.,.F.,.F.,(4,1,1,1,1,1,1,1,1,1,1,1,1,4),(28.2743338823083,
28.7629424145332,29.2601175190104,29.7572926234877,30.2544677279649,30.7516428324421,
31.2488179369193,31.7459930413965,32.2431681458737,32.7403432503509,33.2375183548282,
33.7346934593054,34.2318685637826,34.557519189488),.UNSPECIFIED.);
#736=B_SPLINE_CURVE_WITH_KNOTS('',3,(#40302,#40303,#40304,#40305,#40306,
#40307,#40308,#40309,#40310,#40311,#40312,#40313,#40314,#40315,#40316,#40317,
#40318),.UNSPECIFIED.,.F.,.F.,(4,1,1,1,1,1,1,1,1,1,1,1,1,1,4),(28.2743338823083,
28.319847192143,28.8170222966202,29.3141974010974,29.8113725055746,30.3085476100518,
30.805722714529,31.3028978190063,31.8000729234835,32.2972480279607,32.7944231324379,
33.2915982369151,33.7887733413923,34.2859484458695,34.557519189488),
 .UNSPECIFIED.);
#737=B_SPLINE_CURVE_WITH_KNOTS('',3,(#40323,#40324,#40325,#40326,#40327,
#40328,#40329,#40330,#40331,#40332,#40333,#40334,#40335,#40336,#40337,#40338,
#40339),.UNSPECIFIED.,.F.,.F.,(4,1,1,1,1,1,1,1,1,1,1,1,1,1,4),(21.9911485751286,
22.2996660563294,22.7968411608067,23.2940162652839,23.7911913697611,24.2883664742383,
24.7855415787155,25.2827166831927,25.7798917876699,26.2770668921472,26.7742419966244,
27.2714171011016,27.7685922055788,28.265767310056,28.2743338823083),
 .UNSPECIFIED.);
#738=B_SPLINE_CURVE_WITH_KNOTS('',3,(#40340,#40341,#40342,#40343,#40344,
#40345,#40346,#40347,#40348,#40349,#40350,#40351,#40352,#40353,#40354,#40355),
 .UNSPECIFIED.,.F.,.F.,(4,1,1,1,1,1,1,1,1,1,1,1,1,4),(21.9911485751286,
22.3537459384164,22.8509210428936,23.3480961473708,23.845271251848,24.3424463563253,
24.8396214608025,25.3367965652797,25.8339716697569,26.3311467742341,26.8283218787113,
27.3254969831885,27.8226720876658,28.2743338823083),.UNSPECIFIED.);
#739=B_SPLINE_CURVE_WITH_KNOTS('',3,(#40361,#40362,#40363,#40364,#40365,
#40366),.UNSPECIFIED.,.F.,.F.,(4,1,1,4),(14.398944266781,14.8961193712582,
15.3932944757354,15.707963267949),.UNSPECIFIED.);
#740=B_SPLINE_CURVE_WITH_KNOTS('',3,(#40369,#40370,#40371,#40372,#40373,
#40374,#40375),.UNSPECIFIED.,.F.,.F.,(4,1,1,1,4),(13.8753896155273,14.344864384694,
14.8420394891712,15.3392145936484,15.707963267949),.UNSPECIFIED.);
#741=B_SPLINE_CURVE_WITH_KNOTS('',3,(#40381,#40382,#40383,#40384,#40385,
#40386,#40387),.UNSPECIFIED.,.F.,.F.,(4,3,4),(252.636431288351,252.845104747016,
253.343813040403),.UNSPECIFIED.);
#742=B_SPLINE_CURVE_WITH_KNOTS('',3,(#40395,#40396,#40397,#40398,#40399,
#40400,#40401,#40402,#40403,#40404,#40405,#40406,#40407,#40408,#40409,#40410),
 .UNSPECIFIED.,.F.,.F.,(4,3,3,3,3,4),(-251.327412287183,-250.85027157347,
-250.351563280083,-249.852854986696,-249.35414669331,-248.893201385645),
 .UNSPECIFIED.);
#743=B_SPLINE_CURVE_WITH_KNOTS('',3,(#40415,#40416,#40417,#40418,#40419,
#40420,#40421,#40422,#40423,#40424,#40425,#40426,#40427,#40428,#40429,#40430,
#40431,#40432,#40433,#40434,#40435,#40436,#40437,#40438,#40439,#40440,#40441,
#40442,#40443,#40444,#40445,#40446,#40447,#40448,#40449,#40450,#40451,#40452,
#40453,#40454,#40455,#40456,#40457),.UNSPECIFIED.,.F.,.F.,(4,3,3,3,3,3,
3,3,3,3,3,3,3,3,4),(246.353245981172,246.36189693299,246.860605226377,247.359313519763,
247.85802181315,248.356730106537,248.855438399923,249.35414669331,249.852854986696,
250.351563280083,250.85027157347,251.348979866856,251.847688160243,252.346396453629,
252.636431288351),.UNSPECIFIED.);
#744=B_SPLINE_CURVE_WITH_KNOTS('',3,(#40458,#40459,#40460,#40461,#40462,
#40463,#40464,#40465,#40466,#40467,#40468,#40469,#40470,#40471,#40472,#40473,
#40474,#40475,#40476,#40477,#40478,#40479,#40480,#40481,#40482,#40483,#40484,
#40485,#40486,#40487,#40488,#40489,#40490,#40491,#40492,#40493,#40494,#40495,
#40496,#40497,#40498,#40499,#40500),.UNSPECIFIED.,.F.,.F.,(4,3,3,3,3,3,
3,3,3,3,3,3,3,3,4),(-248.893201385645,-248.855438399923,-248.356730106536,
-247.85802181315,-247.359313519763,-246.860605226377,-246.36189693299,-245.863188639603,
-245.364480346217,-244.86577205283,-244.367063759444,-243.868355466057,
-243.36964717267,-242.870938879284,-242.610016078465),.UNSPECIFIED.);
#745=B_SPLINE_CURVE_WITH_KNOTS('',3,(#40505,#40506,#40507,#40508,#40509,
#40510,#40511,#40512,#40513,#40514,#40515,#40516,#40517,#40518,#40519,#40520,
#40521,#40522,#40523,#40524,#40525,#40526,#40527,#40528,#40529,#40530,#40531,
#40532,#40533,#40534,#40535,#40536,#40537,#40538,#40539,#40540,#40541,#40542,
#40543,#40544),.UNSPECIFIED.,.F.,.F.,(4,3,3,3,3,3,3,3,3,3,3,3,3,4),(240.070060673992,
240.377397412351,240.876105705737,241.374813999124,241.873522292511,242.372230585897,
242.870938879284,243.36964717267,243.868355466057,244.367063759444,244.86577205283,
245.364480346217,245.863188639603,246.353245981172),.UNSPECIFIED.);
#746=B_SPLINE_CURVE_WITH_KNOTS('',3,(#40545,#40546,#40547,#40548,#40549,
#40550,#40551,#40552,#40553,#40554,#40555,#40556,#40557,#40558,#40559,#40560,
#40561,#40562,#40563,#40564,#40565,#40566,#40567,#40568,#40569,#40570,#40571,
#40572,#40573,#40574,#40575,#40576,#40577,#40578,#40579,#40580,#40581,#40582,
#40583,#40584,#40585,#40586,#40587),.UNSPECIFIED.,.F.,.F.,(4,3,3,3,3,3,
3,3,3,3,3,3,3,3,4),(-242.610016078465,-242.372230585897,-241.87352229251,
-241.374813999124,-240.876105705737,-240.377397412351,-239.878689118964,
-239.379980825577,-238.881272532191,-238.382564238804,-237.883855945417,
-237.385147652031,-236.886439358644,-236.387731065258,-236.326830771286),
 .UNSPECIFIED.);
#747=B_SPLINE_CURVE_WITH_KNOTS('',3,(#40592,#40593,#40594,#40595,#40596,
#40597,#40598,#40599,#40600,#40601,#40602,#40603,#40604,#40605,#40606,#40607,
#40608,#40609,#40610,#40611,#40612,#40613,#40614,#40615,#40616,#40617,#40618,
#40619,#40620,#40621,#40622,#40623,#40624,#40625,#40626,#40627,#40628,#40629,
#40630,#40631,#40632,#40633,#40634),.UNSPECIFIED.,.F.,.F.,(4,3,3,3,3,3,
3,3,3,3,3,3,3,3,4),(233.786875366813,233.894189598325,234.392897891711,
234.891606185098,235.390314478484,235.889022771871,236.387731065258,236.886439358644,
237.385147652031,237.883855945418,238.382564238804,238.881272532191,239.379980825577,
239.878689118964,240.070060673992),.UNSPECIFIED.);
#748=B_SPLINE_CURVE_WITH_KNOTS('',3,(#40635,#40636,#40637,#40638,#40639,
#40640,#40641,#40642,#40643,#40644,#40645,#40646,#40647,#40648,#40649,#40650,
#40651,#40652,#40653,#40654,#40655,#40656,#40657,#40658,#40659,#40660,#40661,
#40662,#40663,#40664,#40665,#40666,#40667,#40668,#40669,#40670,#40671,#40672,
#40673,#40674),.UNSPECIFIED.,.F.,.F.,(4,3,3,3,3,3,3,3,3,3,3,3,3,4),(-236.326830771286,
-235.889022771871,-235.390314478484,-234.891606185098,-234.392897891711,
-233.894189598325,-233.395481304938,-232.896773011551,-232.398064718165,
-231.899356424778,-231.400648131391,-230.901939838005,-230.403231544618,
-230.043645464106),.UNSPECIFIED.);
#749=B_SPLINE_CURVE_WITH_KNOTS('',3,(#40679,#40680,#40681,#40682,#40683,
#40684,#40685,#40686,#40687,#40688,#40689,#40690,#40691,#40692,#40693,#40694,
#40695,#40696,#40697,#40698,#40699,#40700,#40701,#40702,#40703,#40704,#40705,
#40706,#40707,#40708,#40709,#40710,#40711,#40712,#40713,#40714,#40715,#40716,
#40717,#40718),.UNSPECIFIED.,.F.,.F.,(4,3,3,3,3,3,3,3,3,3,3,3,3,4),(227.503690059633,
227.909690077685,228.408398371072,228.907106664458,229.405814957845,229.904523251232,
230.403231544618,230.901939838005,231.400648131391,231.899356424778,232.398064718165,
232.896773011551,233.395481304938,233.786875366813),.UNSPECIFIED.);
#750=B_SPLINE_CURVE_WITH_KNOTS('',3,(#40719,#40720,#40721,#40722,#40723,
#40724,#40725,#40726,#40727,#40728,#40729,#40730,#40731,#40732,#40733,#40734,
#40735,#40736,#40737,#40738,#40739,#40740,#40741,#40742,#40743,#40744,#40745,
#40746,#40747,#40748,#40749,#40750,#40751,#40752,#40753,#40754,#40755,#40756,
#40757,#40758,#40759,#40760,#40761),.UNSPECIFIED.,.F.,.F.,(4,3,3,3,3,3,
3,3,3,3,3,3,3,3,4),(-230.043645464106,-229.904523251232,-229.405814957845,
-228.907106664458,-228.408398371072,-227.909690077685,-227.410981784298,
-226.912273490912,-226.413565197525,-225.914856904139,-225.416148610752,
-224.917440317365,-224.418732023979,-223.920023730592,-223.760460156926),
 .UNSPECIFIED.);
#751=B_SPLINE_CURVE_WITH_KNOTS('',3,(#40766,#40767,#40768,#40769,#40770,
#40771,#40772,#40773,#40774,#40775,#40776,#40777,#40778,#40779,#40780,#40781,
#40782,#40783,#40784,#40785,#40786,#40787,#40788,#40789,#40790,#40791,#40792,
#40793,#40794,#40795,#40796,#40797,#40798,#40799,#40800,#40801,#40802,#40803,
#40804,#40805,#40806,#40807,#40808),.UNSPECIFIED.,.F.,.F.,(4,3,3,3,3,3,
3,3,3,3,3,3,3,3,4),(221.220504752453,221.426482263659,221.925190557046,
222.423898850432,222.922607143819,223.421315437206,223.920023730592,224.418732023979,
224.917440317365,225.416148610752,225.914856904139,226.413565197525,226.912273490912,
227.410981784299,227.503690059633),.UNSPECIFIED.);
#752=B_SPLINE_CURVE_WITH_KNOTS('',3,(#40809,#40810,#40811,#40812,#40813,
#40814,#40815,#40816,#40817,#40818,#40819,#40820,#40821,#40822,#40823,#40824,
#40825,#40826,#40827,#40828,#40829,#40830,#40831,#40832,#40833,#40834,#40835,
#40836,#40837,#40838,#40839,#40840,#40841,#40842,#40843,#40844,#40845,#40846,
#40847,#40848),.UNSPECIFIED.,.F.,.F.,(4,3,3,3,3,3,3,3,3,3,3,3,3,4),(-223.760460156926,
-223.421315437206,-222.922607143819,-222.423898850432,-221.925190557046,
-221.426482263659,-220.927773970272,-220.429065676886,-219.930357383499,
-219.431649090113,-218.932940796726,-218.434232503339,-217.935524209953,
-217.477274849747),.UNSPECIFIED.);
#753=B_SPLINE_CURVE_WITH_KNOTS('',3,(#40853,#40854,#40855,#40856,#40857,
#40858,#40859,#40860,#40861,#40862,#40863,#40864,#40865,#40866,#40867,#40868,
#40869,#40870,#40871,#40872,#40873,#40874,#40875,#40876,#40877,#40878,#40879,
#40880,#40881,#40882,#40883,#40884,#40885,#40886,#40887,#40888,#40889,#40890,
#40891,#40892,#40893,#40894,#40895),.UNSPECIFIED.,.F.,.F.,(4,3,3,3,3,3,
3,3,3,3,3,3,3,3,4),(214.937319445274,214.943274449633,215.44198274302,215.940691036406,
216.439399329793,216.93810762318,217.436815916566,217.935524209953,218.434232503339,
218.932940796726,219.431649090113,219.930357383499,220.429065676886,220.927773970272,
221.220504752453),.UNSPECIFIED.);
#754=B_SPLINE_CURVE_WITH_KNOTS('',3,(#40896,#40897,#40898,#40899,#40900,
#40901,#40902,#40903,#40904,#40905,#40906,#40907,#40908,#40909,#40910,#40911,
#40912,#40913,#40914,#40915,#40916,#40917,#40918,#40919,#40920,#40921,#40922,
#40923,#40924,#40925,#40926,#40927,#40928,#40929,#40930,#40931,#40932,#40933,
#40934,#40935,#40936,#40937,#40938),.UNSPECIFIED.,.F.,.F.,(4,3,3,3,3,3,
3,3,3,3,3,3,3,3,4),(-217.477274849747,-217.436815916566,-216.938107623179,
-216.439399329793,-215.940691036406,-215.44198274302,-214.943274449633,
-214.444566156246,-213.94585786286,-213.447149569473,-212.948441276087,
-212.4497329827,-211.951024689313,-211.452316395927,-211.194089542567),
 .UNSPECIFIED.);
#755=B_SPLINE_CURVE_WITH_KNOTS('',3,(#40943,#40944,#40945,#40946,#40947,
#40948,#40949,#40950,#40951,#40952,#40953,#40954,#40955,#40956,#40957,#40958,
#40959,#40960,#40961,#40962,#40963,#40964,#40965,#40966,#40967,#40968,#40969,
#40970,#40971,#40972,#40973,#40974,#40975,#40976,#40977,#40978,#40979,#40980,
#40981,#40982),.UNSPECIFIED.,.F.,.F.,(4,3,3,3,3,3,3,3,3,3,3,3,3,4),(208.654134138094,
208.958774928994,209.45748322238,209.956191515767,210.454899809153,210.95360810254,
211.452316395927,211.951024689313,212.4497329827,212.948441276087,213.447149569473,
213.94585786286,214.444566156246,214.937319445274),.UNSPECIFIED.);
#756=B_SPLINE_CURVE_WITH_KNOTS('',3,(#40983,#40984,#40985,#40986,#40987,
#40988,#40989,#40990,#40991,#40992,#40993,#40994,#40995,#40996,#40997,#40998,
#40999,#41000,#41001,#41002,#41003,#41004,#41005,#41006,#41007,#41008,#41009,
#41010,#41011,#41012,#41013,#41014,#41015,#41016,#41017,#41018,#41019,#41020,
#41021,#41022,#41023,#41024,#41025),.UNSPECIFIED.,.F.,.F.,(4,3,3,3,3,3,
3,3,3,3,3,3,3,3,4),(-211.194089542567,-210.95360810254,-210.454899809153,
-209.956191515767,-209.45748322238,-208.958774928994,-208.460066635607,
-207.96135834222,-207.462650048834,-206.963941755447,-206.46523346206,-205.966525168674,
-205.467816875287,-204.969108581901,-204.910904235388),.UNSPECIFIED.);
#757=B_SPLINE_CURVE_WITH_KNOTS('',3,(#41030,#41031,#41032,#41033,#41034,
#41035,#41036,#41037,#41038,#41039,#41040,#41041,#41042,#41043,#41044,#41045,
#41046,#41047,#41048,#41049,#41050,#41051,#41052,#41053,#41054,#41055,#41056,
#41057,#41058,#41059,#41060,#41061,#41062,#41063,#41064,#41065,#41066,#41067,
#41068,#41069,#41070,#41071,#41072),.UNSPECIFIED.,.F.,.F.,(4,3,3,3,3,3,
3,3,3,3,3,3,3,3,4),(202.370948830915,202.475567114968,202.974275408354,
203.472983701741,203.971691995127,204.470400288514,204.969108581901,205.467816875287,
205.966525168674,206.46523346206,206.963941755447,207.462650048834,207.96135834222,
208.460066635607,208.654134138094),.UNSPECIFIED.);
#758=B_SPLINE_CURVE_WITH_KNOTS('',3,(#41073,#41074,#41075,#41076,#41077,
#41078,#41079,#41080,#41081,#41082,#41083,#41084,#41085,#41086,#41087,#41088,
#41089,#41090,#41091,#41092,#41093,#41094,#41095,#41096,#41097,#41098,#41099,
#41100,#41101,#41102,#41103,#41104,#41105,#41106,#41107,#41108,#41109,#41110,
#41111,#41112),.UNSPECIFIED.,.F.,.F.,(4,3,3,3,3,3,3,3,3,3,3,3,3,4),(-204.910904235388,
-204.470400288514,-203.971691995127,-203.472983701741,-202.974275408354,
-202.475567114968,-201.976858821581,-201.478150528194,-200.979442234808,
-200.480733941421,-199.982025648034,-199.483317354648,-198.984609061261,
-198.627718928208),.UNSPECIFIED.);
#759=B_SPLINE_CURVE_WITH_KNOTS('',3,(#41117,#41118,#41119,#41120,#41121,
#41122,#41123,#41124,#41125,#41126,#41127,#41128,#41129,#41130,#41131,#41132,
#41133,#41134,#41135,#41136,#41137,#41138,#41139,#41140,#41141,#41142,#41143,
#41144,#41145,#41146,#41147,#41148,#41149,#41150,#41151,#41152,#41153,#41154,
#41155,#41156),.UNSPECIFIED.,.F.,.F.,(4,3,3,3,3,3,3,3,3,3,3,3,3,4),(196.087763523735,
196.491067594328,196.989775887715,197.488484181101,197.987192474488,198.485900767875,
198.984609061261,199.483317354648,199.982025648034,200.480733941421,200.979442234808,
201.478150528194,201.976858821581,202.370948830915),.UNSPECIFIED.);
#760=B_SPLINE_CURVE_WITH_KNOTS('',3,(#41157,#41158,#41159,#41160,#41161,
#41162,#41163,#41164,#41165,#41166,#41167,#41168,#41169,#41170,#41171,#41172,
#41173,#41174,#41175,#41176,#41177,#41178,#41179,#41180,#41181,#41182,#41183,
#41184,#41185,#41186,#41187,#41188,#41189,#41190,#41191,#41192,#41193,#41194,
#41195,#41196,#41197,#41198,#41199),.UNSPECIFIED.,.F.,.F.,(4,3,3,3,3,3,
3,3,3,3,3,3,3,3,4),(-198.627718928208,-198.485900767875,-197.987192474488,
-197.488484181101,-196.989775887715,-196.491067594328,-195.992359300941,
-195.493651007555,-194.994942714168,-194.496234420782,-193.997526127395,
-193.498817834008,-193.000109540622,-192.501401247235,-192.344533621029),
 .UNSPECIFIED.);
#761=B_SPLINE_CURVE_WITH_KNOTS('',3,(#41204,#41205,#41206,#41207,#41208,
#41209,#41210,#41211,#41212,#41213,#41214,#41215,#41216,#41217,#41218,#41219,
#41220,#41221,#41222,#41223,#41224,#41225,#41226,#41227,#41228,#41229,#41230,
#41231,#41232,#41233,#41234,#41235,#41236,#41237,#41238,#41239,#41240,#41241,
#41242,#41243,#41244,#41245,#41246),.UNSPECIFIED.,.F.,.F.,(4,3,3,3,3,3,
3,3,3,3,3,3,3,3,4),(189.804578216556,190.007859780302,190.506568073689,
191.005276367075,191.503984660462,192.002692953849,192.501401247235,193.000109540622,
193.498817834008,193.997526127395,194.496234420782,194.994942714168,195.493651007555,
195.992359300941,196.087763523735),.UNSPECIFIED.);
#762=B_SPLINE_CURVE_WITH_KNOTS('',3,(#41247,#41248,#41249,#41250,#41251,
#41252,#41253,#41254,#41255,#41256,#41257,#41258,#41259,#41260,#41261,#41262,
#41263,#41264,#41265,#41266,#41267,#41268,#41269,#41270,#41271,#41272,#41273,
#41274,#41275,#41276,#41277,#41278,#41279,#41280,#41281,#41282,#41283,#41284,
#41285,#41286),.UNSPECIFIED.,.F.,.F.,(4,3,3,3,3,3,3,3,3,3,3,3,3,4),(-192.344533621029,
-192.002692953848,-191.503984660462,-191.005276367075,-190.506568073689,
-190.007859780302,-189.509151486915,-189.010443193529,-188.511734900142,
-188.013026606756,-187.514318313369,-187.015610019982,-186.516901726596,
-186.061348313849),.UNSPECIFIED.);
#763=B_SPLINE_CURVE_WITH_KNOTS('',3,(#41291,#41292,#41293,#41294,#41295,
#41296,#41297,#41298,#41299,#41300,#41301,#41302,#41303,#41304,#41305,#41306,
#41307,#41308,#41309,#41310,#41311,#41312,#41313,#41314,#41315,#41316,#41317,
#41318,#41319,#41320,#41321,#41322,#41323,#41324,#41325,#41326,#41327,#41328,
#41329,#41330,#41331,#41332,#41333),.UNSPECIFIED.,.F.,.F.,(4,3,3,3,3,3,
3,3,3,3,3,3,3,3,4),(183.521392909376,183.524651966276,184.023360259663,
184.522068553049,185.020776846436,185.519485139823,186.018193433209,186.516901726596,
187.015610019982,187.514318313369,188.013026606756,188.511734900142,189.010443193529,
189.509151486915,189.804578216556),.UNSPECIFIED.);
#764=B_SPLINE_CURVE_WITH_KNOTS('',3,(#41334,#41335,#41336,#41337,#41338,
#41339,#41340,#41341,#41342,#41343,#41344,#41345,#41346,#41347,#41348,#41349,
#41350,#41351,#41352,#41353,#41354,#41355,#41356,#41357,#41358,#41359,#41360,
#41361,#41362,#41363,#41364,#41365,#41366,#41367,#41368,#41369,#41370,#41371,
#41372,#41373,#41374,#41375,#41376),.UNSPECIFIED.,.F.,.F.,(4,3,3,3,3,3,
3,3,3,3,3,3,3,3,4),(-186.061348313849,-186.018193433209,-185.519485139822,
-185.020776846436,-184.522068553049,-184.023360259663,-183.524651966276,
-183.025943672889,-182.527235379503,-182.028527086116,-181.529818792729,
-181.031110499343,-180.532402205956,-180.03369391257,-179.77816300667),
 .UNSPECIFIED.);
#765=B_SPLINE_CURVE_WITH_KNOTS('',3,(#41381,#41382,#41383,#41384,#41385,
#41386,#41387,#41388,#41389,#41390,#41391,#41392,#41393,#41394,#41395,#41396,
#41397,#41398,#41399,#41400,#41401,#41402,#41403,#41404,#41405,#41406,#41407,
#41408,#41409,#41410,#41411,#41412,#41413,#41414,#41415,#41416,#41417,#41418,
#41419,#41420),.UNSPECIFIED.,.F.,.F.,(4,3,3,3,3,3,3,3,3,3,3,3,3,4),(177.238207602196,
177.540152445637,178.038860739023,178.53756903241,179.036277325796,179.534985619183,
180.03369391257,180.532402205956,181.031110499343,181.52981879273,182.028527086116,
182.527235379503,183.025943672889,183.521392909376),.UNSPECIFIED.);
#766=B_SPLINE_CURVE_WITH_KNOTS('',3,(#41421,#41422,#41423,#41424,#41425,
#41426,#41427,#41428,#41429,#41430,#41431,#41432,#41433,#41434,#41435,#41436,
#41437,#41438,#41439,#41440,#41441,#41442,#41443,#41444,#41445,#41446,#41447,
#41448,#41449,#41450,#41451,#41452,#41453,#41454,#41455,#41456,#41457,#41458,
#41459,#41460,#41461,#41462,#41463),.UNSPECIFIED.,.F.,.F.,(4,3,3,3,3,3,
3,3,3,3,3,3,3,3,4),(-179.77816300667,-179.534985619183,-179.036277325796,
-178.53756903241,-178.038860739023,-177.540152445637,-177.04144415225,-176.542735858863,
-176.044027565477,-175.54531927209,-175.046610978703,-174.547902685317,
-174.04919439193,-173.550486098544,-173.49497769949),.UNSPECIFIED.);
#767=B_SPLINE_CURVE_WITH_KNOTS('',3,(#41468,#41469,#41470,#41471,#41472,
#41473,#41474,#41475,#41476,#41477,#41478,#41479,#41480,#41481,#41482,#41483,
#41484,#41485,#41486,#41487,#41488,#41489,#41490,#41491,#41492,#41493,#41494,
#41495,#41496,#41497,#41498,#41499,#41500,#41501,#41502,#41503,#41504,#41505,
#41506,#41507,#41508,#41509,#41510),.UNSPECIFIED.,.F.,.F.,(4,3,3,3,3,3,
3,3,3,3,3,3,3,3,4),(170.955022295017,171.056944631611,171.555652924997,
172.054361218384,172.55306951177,173.051777805157,173.550486098544,174.04919439193,
174.547902685317,175.046610978703,175.54531927209,176.044027565477,176.542735858863,
177.04144415225,177.238207602196),.UNSPECIFIED.);
#768=B_SPLINE_CURVE_WITH_KNOTS('',3,(#41511,#41512,#41513,#41514,#41515,
#41516,#41517,#41518,#41519,#41520,#41521,#41522,#41523,#41524,#41525,#41526,
#41527,#41528,#41529,#41530,#41531,#41532,#41533,#41534,#41535,#41536,#41537,
#41538,#41539,#41540,#41541,#41542,#41543,#41544,#41545,#41546,#41547,#41548,
#41549,#41550),.UNSPECIFIED.,.F.,.F.,(4,3,3,3,3,3,3,3,3,3,3,3,3,4),(-173.49497769949,
-173.051777805157,-172.55306951177,-172.054361218384,-171.555652924997,
-171.05694463161,-170.558236338224,-170.059528044837,-169.560819751451,
-169.062111458064,-168.563403164677,-168.064694871291,-167.565986577904,
-167.21179239231),.UNSPECIFIED.);
#769=B_SPLINE_CURVE_WITH_KNOTS('',3,(#41555,#41556,#41557,#41558,#41559,
#41560,#41561,#41562,#41563,#41564,#41565,#41566,#41567,#41568,#41569,#41570,
#41571,#41572,#41573,#41574,#41575,#41576,#41577,#41578,#41579,#41580,#41581,
#41582,#41583,#41584,#41585,#41586,#41587,#41588,#41589,#41590,#41591,#41592,
#41593,#41594),.UNSPECIFIED.,.F.,.F.,(4,3,3,3,3,3,3,3,3,3,3,3,3,4),(164.671836987837,
165.072445110971,165.571153404358,166.069861697744,166.568569991131,167.067278284518,
167.565986577904,168.064694871291,168.563403164677,169.062111458064,169.560819751451,
170.059528044837,170.558236338224,170.955022295017),.UNSPECIFIED.);
#770=B_SPLINE_CURVE_WITH_KNOTS('',3,(#41595,#41596,#41597,#41598,#41599,
#41600,#41601,#41602,#41603,#41604,#41605,#41606,#41607,#41608,#41609,#41610,
#41611,#41612,#41613,#41614,#41615,#41616,#41617,#41618,#41619,#41620,#41621,
#41622,#41623,#41624,#41625,#41626,#41627,#41628,#41629,#41630,#41631,#41632,
#41633,#41634,#41635,#41636,#41637),.UNSPECIFIED.,.F.,.F.,(4,3,3,3,3,3,
3,3,3,3,3,3,3,3,4),(-167.21179239231,-167.067278284517,-166.568569991131,
-166.069861697744,-165.571153404358,-165.072445110971,-164.573736817584,
-164.075028524198,-163.576320230811,-163.077611937425,-162.578903644038,
-162.080195350651,-161.581487057265,-161.082778763878,-160.928607085131),
 .UNSPECIFIED.);
#771=B_SPLINE_CURVE_WITH_KNOTS('',3,(#41642,#41643,#41644,#41645,#41646,
#41647,#41648,#41649,#41650,#41651,#41652,#41653,#41654,#41655,#41656,#41657,
#41658,#41659,#41660,#41661,#41662,#41663,#41664,#41665,#41666,#41667,#41668,
#41669,#41670,#41671,#41672,#41673,#41674,#41675,#41676,#41677,#41678,#41679,
#41680,#41681,#41682,#41683,#41684),.UNSPECIFIED.,.F.,.F.,(4,3,3,3,3,3,
3,3,3,3,3,3,3,3,4),(158.388651680658,158.589237296945,159.087945590332,
159.586653883718,160.085362177105,160.584070470491,161.082778763878,161.581487057265,
162.080195350651,162.578903644038,163.077611937425,163.576320230811,164.075028524198,
164.573736817584,164.671836987837),.UNSPECIFIED.);
#772=B_SPLINE_CURVE_WITH_KNOTS('',3,(#41685,#41686,#41687,#41688,#41689,
#41690,#41691,#41692,#41693,#41694,#41695,#41696,#41697,#41698,#41699,#41700,
#41701,#41702,#41703,#41704,#41705,#41706,#41707,#41708,#41709,#41710,#41711,
#41712,#41713,#41714,#41715,#41716,#41717,#41718,#41719,#41720,#41721,#41722,
#41723,#41724),.UNSPECIFIED.,.F.,.F.,(4,3,3,3,3,3,3,3,3,3,3,3,3,4),(-160.928607085131,
-160.584070470491,-160.085362177105,-159.586653883718,-159.087945590332,
-158.589237296945,-158.090529003558,-157.591820710172,-157.093112416785,
-156.594404123399,-156.095695830012,-155.596987536625,-155.098279243239,
-154.645421777951),.UNSPECIFIED.);
#773=B_SPLINE_CURVE_WITH_KNOTS('',3,(#41729,#41730,#41731,#41732,#41733,
#41734,#41735,#41736,#41737,#41738,#41739,#41740,#41741,#41742,#41743,#41744,
#41745,#41746,#41747,#41748,#41749,#41750,#41751,#41752,#41753,#41754,#41755,
#41756,#41757,#41758,#41759,#41760,#41761,#41762,#41763,#41764,#41765,#41766,
#41767,#41768),.UNSPECIFIED.,.F.,.F.,(4,3,3,3,3,3,3,3,3,3,3,3,3,4),(152.105466373478,
152.604737776306,153.103446069692,153.602154363079,154.100862656465,154.599570949852,
155.098279243239,155.596987536625,156.095695830012,156.594404123399,157.093112416785,
157.591820710172,158.090529003558,158.388651680658),.UNSPECIFIED.);
#774=B_SPLINE_CURVE_WITH_KNOTS('',3,(#41769,#41770,#41771,#41772,#41773,
#41774,#41775,#41776,#41777,#41778,#41779,#41780,#41781,#41782,#41783,#41784,
#41785,#41786,#41787,#41788,#41789,#41790,#41791,#41792,#41793,#41794,#41795,
#41796,#41797,#41798,#41799,#41800,#41801,#41802,#41803,#41804,#41805,#41806,
#41807,#41808,#41809,#41810,#41811),.UNSPECIFIED.,.F.,.F.,(4,3,3,3,3,3,
3,3,3,3,3,3,3,3,4),(-154.645421777951,-154.599570949852,-154.100862656465,
-153.602154363079,-153.103446069692,-152.604737776306,-152.106029482919,
-151.607321189532,-151.108612896146,-150.609904602759,-150.111196309372,
-149.612488015986,-149.113779722599,-148.615071429213,-148.362236470772),
 .UNSPECIFIED.);
#775=B_SPLINE_CURVE_WITH_KNOTS('',3,(#41816,#41817,#41818,#41819,#41820,
#41821,#41822,#41823,#41824,#41825,#41826,#41827,#41828,#41829,#41830,#41831,
#41832,#41833,#41834,#41835,#41836,#41837,#41838,#41839,#41840,#41841,#41842,
#41843,#41844,#41845,#41846,#41847,#41848,#41849,#41850,#41851,#41852,#41853,
#41854,#41855),.UNSPECIFIED.,.F.,.F.,(4,3,3,3,3,3,3,3,3,3,3,3,3,4),(145.822281066299,
146.121529962279,146.620238255666,147.118946549053,147.617654842439,148.116363135826,
148.615071429213,149.113779722599,149.612488015986,150.111196309372,150.609904602759,
151.108612896146,151.607321189532,152.105466373478),.UNSPECIFIED.);
#776=B_SPLINE_CURVE_WITH_KNOTS('',3,(#41856,#41857,#41858,#41859,#41860,
#41861,#41862,#41863,#41864,#41865,#41866,#41867,#41868,#41869,#41870,#41871,
#41872,#41873,#41874,#41875,#41876,#41877,#41878,#41879,#41880,#41881,#41882,
#41883,#41884,#41885,#41886,#41887,#41888,#41889,#41890,#41891,#41892,#41893,
#41894,#41895,#41896,#41897,#41898),.UNSPECIFIED.,.F.,.F.,(4,3,3,3,3,3,
3,3,3,3,3,3,3,3,4),(-148.362236470772,-148.116363135826,-147.617654842439,
-147.118946549053,-146.620238255666,-146.12152996228,-145.622821668893,
-145.124113375506,-144.62540508212,-144.126696788733,-143.627988495346,
-143.12928020196,-142.630571908573,-142.131863615187,-142.079051163592),
 .UNSPECIFIED.);
#777=B_SPLINE_CURVE_WITH_KNOTS('',3,(#41903,#41904,#41905,#41906,#41907,
#41908,#41909,#41910,#41911,#41912,#41913,#41914,#41915,#41916,#41917,#41918,
#41919,#41920,#41921,#41922,#41923,#41924,#41925,#41926,#41927,#41928,#41929,
#41930,#41931,#41932,#41933,#41934,#41935,#41936,#41937,#41938,#41939,#41940,
#41941,#41942,#41943,#41944,#41945),.UNSPECIFIED.,.F.,.F.,(4,3,3,3,3,3,
3,3,3,3,3,3,3,3,4),(139.539095759119,139.638322148253,140.13703044164,140.635738735027,
141.134447028413,141.6331553218,142.131863615187,142.630571908573,143.12928020196,
143.627988495346,144.126696788733,144.62540508212,145.124113375506,145.622821668893,
145.822281066299),.UNSPECIFIED.);
#778=B_SPLINE_CURVE_WITH_KNOTS('',3,(#41946,#41947,#41948,#41949,#41950,
#41951,#41952,#41953,#41954,#41955,#41956,#41957,#41958,#41959,#41960,#41961,
#41962,#41963,#41964,#41965,#41966,#41967,#41968,#41969,#41970,#41971,#41972,
#41973,#41974,#41975,#41976,#41977,#41978,#41979,#41980,#41981,#41982,#41983,
#41984,#41985),.UNSPECIFIED.,.F.,.F.,(4,3,3,3,3,3,3,3,3,3,3,3,3,4),(-142.079051163592,
-141.6331553218,-141.134447028413,-140.635738735027,-140.13703044164,-139.638322148253,
-139.139613854867,-138.64090556148,-138.142197268094,-137.643488974707,
-137.14478068132,-136.646072387934,-136.147364094547,-135.795865856413),
 .UNSPECIFIED.);
#779=B_SPLINE_CURVE_WITH_KNOTS('',3,(#41990,#41991,#41992,#41993,#41994,
#41995,#41996,#41997,#41998,#41999,#42000,#42001,#42002,#42003,#42004,#42005,
#42006,#42007,#42008,#42009,#42010,#42011,#42012,#42013,#42014,#42015,#42016,
#42017,#42018,#42019,#42020,#42021,#42022,#42023,#42024,#42025,#42026,#42027,
#42028,#42029),.UNSPECIFIED.,.F.,.F.,(4,3,3,3,3,3,3,3,3,3,3,3,3,4),(133.25591045194,
133.653822627614,134.152530921001,134.651239214387,135.149947507774,135.648655801161,
136.147364094547,136.646072387934,137.14478068132,137.643488974707,138.142197268094,
138.64090556148,139.139613854867,139.539095759119),.UNSPECIFIED.);
#780=B_SPLINE_CURVE_WITH_KNOTS('',3,(#42030,#42031,#42032,#42033,#42034,
#42035,#42036,#42037,#42038,#42039,#42040,#42041,#42042,#42043,#42044,#42045,
#42046,#42047,#42048,#42049,#42050,#42051,#42052,#42053,#42054,#42055,#42056,
#42057,#42058,#42059,#42060),.UNSPECIFIED.,.F.,.F.,(4,3,3,3,3,3,3,3,3,3,
4),(-135.795865856413,-135.648655801161,-135.149947507774,-134.651239214387,
-134.152530921001,-133.653822627614,-132.656406040841,-131.658989454068,
-130.661572867294,-129.664156280521,-129.512680549233),.UNSPECIFIED.);
#781=B_SPLINE_CURVE_WITH_KNOTS('',3,(#42065,#42066,#42067,#42068,#42069,
#42070,#42071,#42072,#42073,#42074,#42075,#42076,#42077,#42078,#42079,#42080,
#42081,#42082,#42083,#42084,#42085,#42086),.UNSPECIFIED.,.F.,.F.,(4,3,3,
3,3,3,3,4),(126.97272514476,127.669323106975,128.666739693748,129.664156280521,
130.661572867294,131.658989454068,132.656406040841,133.25591045194),
 .UNSPECIFIED.);
#782=B_SPLINE_CURVE_WITH_KNOTS('',3,(#42087,#42088,#42089,#42090,#42091,
#42092,#42093,#42094,#42095,#42096,#42097,#42098,#42099,#42100,#42101,#42102,
#42103,#42104,#42105,#42106,#42107,#42108),.UNSPECIFIED.,.F.,.F.,(4,3,3,
3,3,3,3,4),(-129.512680549233,-128.666739693748,-127.669323106975,-126.671906520201,
-125.674489933428,-124.677073346655,-123.679656759882,-123.229495242053),
 .UNSPECIFIED.);
#783=B_SPLINE_CURVE_WITH_KNOTS('',3,(#42113,#42114,#42115,#42116,#42117,
#42118,#42119,#42120,#42121,#42122,#42123,#42124,#42125,#42126,#42127,#42128,
#42129,#42130,#42131,#42132,#42133,#42134),.UNSPECIFIED.,.F.,.F.,(4,3,3,
3,3,3,3,4),(120.68953983758,121.684823586335,122.682240173108,123.679656759882,
124.677073346655,125.674489933428,126.671906520201,126.97272514476),
 .UNSPECIFIED.);
#784=B_SPLINE_CURVE_WITH_KNOTS('',3,(#42135,#42136,#42137,#42138,#42139,
#42140,#42141,#42142,#42143,#42144,#42145,#42146,#42147,#42148,#42149,#42150,
#42151,#42152,#42153,#42154,#42155,#42156,#42157,#42158,#42159,#42160,#42161,
#42162,#42163,#42164,#42165),.UNSPECIFIED.,.F.,.F.,(4,3,3,3,3,3,3,3,3,3,
4),(-123.229495242053,-122.682240173108,-121.684823586335,-120.687406999562,
-119.689990412789,-119.191282119402,-118.692573826015,-118.193865532629,
-117.695157239242,-117.196448945856,-116.946309934874),.UNSPECIFIED.);
#785=B_SPLINE_CURVE_WITH_KNOTS('',3,(#42170,#42171,#42172,#42173,#42174,
#42175,#42176,#42177,#42178,#42179,#42180,#42181,#42182,#42183,#42184,#42185,
#42186,#42187,#42188,#42189,#42190,#42191,#42192,#42193,#42194,#42195,#42196,
#42197,#42198,#42199,#42200,#42201,#42202,#42203,#42204,#42205,#42206,#42207,
#42208,#42209),.UNSPECIFIED.,.F.,.F.,(4,3,3,3,3,3,3,3,3,3,3,3,3,4),(114.406354530401,
114.702907478922,115.201615772309,115.700324065696,116.199032359082,116.697740652469,
117.196448945856,117.695157239242,118.193865532629,118.692573826015,119.191282119402,
119.689990412789,120.687406999562,120.68953983758),.UNSPECIFIED.);
#786=B_SPLINE_CURVE_WITH_KNOTS('',3,(#42210,#42211,#42212,#42213,#42214,
#42215,#42216,#42217,#42218,#42219,#42220,#42221,#42222,#42223,#42224,#42225,
#42226,#42227,#42228,#42229,#42230,#42231,#42232,#42233,#42234,#42235,#42236,
#42237,#42238,#42239,#42240,#42241,#42242,#42243,#42244,#42245,#42246,#42247,
#42248,#42249,#42250,#42251,#42252),.UNSPECIFIED.,.F.,.F.,(4,3,3,3,3,3,
3,3,3,3,3,3,3,3,4),(-116.946309934874,-116.697740652469,-116.199032359082,
-115.700324065696,-115.201615772309,-114.702907478922,-114.204199185536,
-113.705490892149,-113.206782598763,-112.708074305376,-112.209366011989,
-111.710657718603,-111.211949425216,-110.71324113183,-110.663124627694),
 .UNSPECIFIED.);
#787=B_SPLINE_CURVE_WITH_KNOTS('',3,(#42257,#42258,#42259,#42260,#42261,
#42262,#42263,#42264,#42265,#42266,#42267,#42268,#42269,#42270,#42271,#42272,
#42273,#42274,#42275,#42276,#42277,#42278,#42279,#42280,#42281,#42282,#42283,
#42284,#42285,#42286,#42287,#42288,#42289,#42290,#42291,#42292,#42293,#42294,
#42295,#42296,#42297,#42298,#42299),.UNSPECIFIED.,.F.,.F.,(4,3,3,3,3,3,
3,3,3,3,3,3,3,3,4),(108.123169223221,108.219699664896,108.718407958283,
109.21711625167,109.715824545056,110.214532838443,110.71324113183,111.211949425216,
111.710657718603,112.209366011989,112.708074305376,113.206782598763,113.705490892149,
114.204199185536,114.406354530401),.UNSPECIFIED.);
#788=B_SPLINE_CURVE_WITH_KNOTS('',3,(#42300,#42301,#42302,#42303,#42304,
#42305,#42306,#42307,#42308,#42309,#42310,#42311,#42312,#42313,#42314,#42315,
#42316,#42317,#42318,#42319,#42320,#42321,#42322,#42323,#42324,#42325,#42326,
#42327,#42328,#42329,#42330,#42331,#42332,#42333,#42334,#42335,#42336,#42337,
#42338,#42339),.UNSPECIFIED.,.F.,.F.,(4,3,3,3,3,3,3,3,3,3,3,3,3,4),(-110.663124627694,
-110.214532838443,-109.715824545056,-109.21711625167,-108.718407958283,
-108.219699664896,-107.72099137151,-107.222283078123,-106.723574784737,
-106.22486649135,-105.726158197963,-105.227449904577,-104.72874161119,-104.379939320515),
 .UNSPECIFIED.);
#789=B_SPLINE_CURVE_WITH_KNOTS('',3,(#42344,#42345,#42346,#42347,#42348,
#42349,#42350,#42351,#42352,#42353,#42354,#42355,#42356,#42357,#42358,#42359,
#42360,#42361,#42362,#42363,#42364,#42365,#42366,#42367,#42368,#42369,#42370,
#42371,#42372,#42373,#42374,#42375,#42376,#42377,#42378,#42379,#42380,#42381,
#42382,#42383),.UNSPECIFIED.,.F.,.F.,(4,3,3,3,3,3,3,3,3,3,3,3,3,4),(101.839983916042,
102.235200144257,102.733908437644,103.23261673103,103.731325024417,104.230033317804,
104.72874161119,105.227449904577,105.726158197963,106.22486649135,106.723574784737,
107.222283078123,107.72099137151,108.123169223221),.UNSPECIFIED.);
#790=B_SPLINE_CURVE_WITH_KNOTS('',3,(#42384,#42385,#42386,#42387,#42388,
#42389,#42390,#42391,#42392,#42393,#42394,#42395,#42396,#42397,#42398,#42399,
#42400,#42401,#42402,#42403,#42404,#42405,#42406,#42407,#42408,#42409,#42410,
#42411,#42412,#42413,#42414,#42415,#42416,#42417,#42418,#42419,#42420,#42421,
#42422,#42423,#42424,#42425,#42426),.UNSPECIFIED.,.F.,.F.,(4,3,3,3,3,3,
3,3,3,3,3,3,3,3,4),(-104.379939320515,-104.230033317803,-103.731325024417,
-103.23261673103,-102.733908437644,-102.235200144257,-101.73649185087,-101.237783557484,
-100.739075264097,-100.24036697071,-99.7416586773239,-99.2429503839373,
-98.7442420905506,-98.245533797164,-98.096754013335),.UNSPECIFIED.);
#791=B_SPLINE_CURVE_WITH_KNOTS('',3,(#42431,#42432,#42433,#42434,#42435,
#42436,#42437,#42438,#42439,#42440,#42441,#42442,#42443,#42444,#42445,#42446,
#42447,#42448,#42449,#42450,#42451,#42452,#42453,#42454,#42455,#42456,#42457,
#42458,#42459,#42460,#42461,#42462,#42463,#42464,#42465,#42466,#42467,#42468,
#42469,#42470,#42471,#42472,#42473),.UNSPECIFIED.,.F.,.F.,(4,3,3,3,3,3,
3,3,3,3,3,3,3,3,4),(95.556798608862,95.751992330231,96.2507006236176,96.7494089170042,
97.2481172103908,97.7468255037774,98.2455337971641,98.7442420905507,99.2429503839373,
99.7416586773239,100.240366970711,100.739075264097,101.237783557484,101.73649185087,
101.839983916042),.UNSPECIFIED.);
#792=B_SPLINE_CURVE_WITH_KNOTS('',3,(#42474,#42475,#42476,#42477,#42478,
#42479,#42480,#42481,#42482,#42483,#42484,#42485,#42486,#42487,#42488,#42489,
#42490,#42491,#42492,#42493,#42494,#42495,#42496,#42497,#42498,#42499,#42500,
#42501,#42502,#42503,#42504,#42505,#42506,#42507,#42508,#42509,#42510,#42511,
#42512,#42513),.UNSPECIFIED.,.F.,.F.,(4,3,3,3,3,3,3,3,3,3,3,3,3,4),(-98.096754013335,
-97.7468255037774,-97.2481172103908,-96.7494089170042,-96.2507006236176,
-95.7519923302309,-95.2532840368443,-94.7545757434577,-94.2558674500711,
-93.7571591566845,-93.2584508632978,-92.7597425699112,-92.2610342765246,
-91.8135687061554),.UNSPECIFIED.);
#793=B_SPLINE_CURVE_WITH_KNOTS('',3,(#42518,#42519,#42520,#42521,#42522,
#42523,#42524,#42525,#42526,#42527,#42528,#42529,#42530,#42531,#42532,#42533,
#42534,#42535,#42536,#42537,#42538,#42539,#42540,#42541,#42542,#42543,#42544,
#42545,#42546,#42547,#42548,#42549,#42550,#42551,#42552,#42553,#42554,#42555,
#42556,#42557),.UNSPECIFIED.,.F.,.F.,(4,3,3,3,3,3,3,3,3,3,3,3,3,4),(89.2736133016824,
89.7674928095915,90.2662011029781,90.7649093963648,91.2636176897514,91.762325983138,
92.2610342765246,92.7597425699113,93.2584508632979,93.7571591566845,94.2558674500711,
94.7545757434577,95.2532840368443,95.556798608862),.UNSPECIFIED.);
#794=B_SPLINE_CURVE_WITH_KNOTS('',3,(#42558,#42559,#42560,#42561,#42562,
#42563,#42564,#42565,#42566,#42567,#42568,#42569,#42570,#42571,#42572,#42573,
#42574,#42575,#42576,#42577,#42578,#42579,#42580,#42581,#42582,#42583,#42584,
#42585,#42586,#42587,#42588,#42589,#42590,#42591,#42592,#42593,#42594,#42595,
#42596,#42597,#42598,#42599,#42600),.UNSPECIFIED.,.F.,.F.,(4,3,3,3,3,3,
3,3,3,3,3,3,3,3,4),(-91.8135687061554,-91.762325983138,-91.2636176897513,
-90.7649093963647,-90.2662011029781,-89.7674928095915,-89.2687845162049,
-88.7700762228182,-88.2713679294316,-87.772659636045,-87.2739513426584,
-86.7752430492718,-86.2765347558852,-85.7778264624986,-85.5303833989758),
 .UNSPECIFIED.);
#795=B_SPLINE_CURVE_WITH_KNOTS('',3,(#42605,#42606,#42607,#42608,#42609,
#42610,#42611,#42612,#42613,#42614,#42615,#42616,#42617,#42618,#42619,#42620,
#42621,#42622,#42623,#42624,#42625,#42626,#42627,#42628,#42629,#42630,#42631,
#42632,#42633,#42634,#42635,#42636,#42637,#42638,#42639,#42640,#42641,#42642,
#42643,#42644,#42645,#42646,#42647),.UNSPECIFIED.,.F.,.F.,(4,3,3,3,3,3,
3,3,3,3,3,3,3,3,4),(82.9904279945028,83.2842849955655,83.7829932889521,
84.2817015823387,84.7804098757253,85.279118169112,85.7778264624986,86.2765347558852,
86.7752430492718,87.2739513426584,87.772659636045,88.2713679294317,88.7700762228183,
89.2687845162049,89.2736133016824),.UNSPECIFIED.);
#796=B_SPLINE_CURVE_WITH_KNOTS('',3,(#42648,#42649,#42650,#42651,#42652,
#42653,#42654,#42655,#42656,#42657,#42658,#42659,#42660,#42661,#42662,#42663,
#42664,#42665,#42666,#42667,#42668,#42669,#42670,#42671,#42672,#42673,#42674,
#42675,#42676,#42677,#42678,#42679,#42680,#42681,#42682,#42683,#42684,#42685,
#42686,#42687,#42688,#42689,#42690),.UNSPECIFIED.,.F.,.F.,(4,3,3,3,3,3,
3,3,3,3,3,3,3,3,4),(-85.5303833989758,-85.2791181691119,-84.7804098757253,
-84.2817015823387,-83.7829932889521,-83.2842849955654,-82.7855767021788,
-82.2868684087922,-81.7881601154056,-81.289451822019,-80.7907435286323,
-80.2920352352457,-79.7933269418591,-79.2946186484725,-79.2471980917962),
 .UNSPECIFIED.);
#797=B_SPLINE_CURVE_WITH_KNOTS('',3,(#42695,#42696,#42697,#42698,#42699,
#42700,#42701,#42702,#42703,#42704,#42705,#42706,#42707,#42708,#42709,#42710,
#42711,#42712,#42713,#42714,#42715,#42716,#42717,#42718,#42719,#42720,#42721,
#42722,#42723,#42724,#42725,#42726,#42727,#42728,#42729,#42730,#42731,#42732,
#42733,#42734,#42735,#42736,#42737),.UNSPECIFIED.,.F.,.F.,(4,3,3,3,3,3,
3,3,3,3,3,3,3,3,4),(76.7072426873232,76.8010771815394,77.299785474926,77.7984937683127,
78.2972020616993,78.7959103550859,79.2946186484725,79.7933269418591,80.2920352352457,
80.7907435286324,81.289451822019,81.7881601154056,82.2868684087922,82.7855767021789,
82.9904279945028),.UNSPECIFIED.);
#798=B_SPLINE_CURVE_WITH_KNOTS('',3,(#42738,#42739,#42740,#42741,#42742,
#42743,#42744,#42745,#42746,#42747,#42748,#42749,#42750,#42751,#42752,#42753,
#42754,#42755,#42756,#42757,#42758,#42759,#42760,#42761,#42762,#42763,#42764,
#42765,#42766,#42767,#42768,#42769,#42770,#42771,#42772,#42773,#42774,#42775,
#42776,#42777),.UNSPECIFIED.,.F.,.F.,(4,3,3,3,3,3,3,3,3,3,3,3,3,4),(-79.2471980917962,
-78.7959103550859,-78.2972020616993,-77.7984937683126,-77.299785474926,
-76.8010771815394,-76.3023688881528,-75.8036605947662,-75.3049523013795,
-74.8062440079929,-74.3075357146063,-73.8088274212197,-73.3101191278331,
-72.9640127846166),.UNSPECIFIED.);
#799=B_SPLINE_CURVE_WITH_KNOTS('',3,(#42782,#42783,#42784,#42785,#42786,
#42787,#42788,#42789,#42790,#42791,#42792,#42793,#42794,#42795,#42796,#42797,
#42798,#42799,#42800,#42801,#42802,#42803,#42804,#42805,#42806,#42807,#42808,
#42809,#42810,#42811,#42812,#42813,#42814,#42815,#42816,#42817,#42818,#42819,
#42820,#42821),.UNSPECIFIED.,.F.,.F.,(4,3,3,3,3,3,3,3,3,3,3,3,3,4),(70.4240573801436,
70.8165776609,71.3152859542866,71.8139942476732,72.3127025410598,72.8114108344465,
73.3101191278331,73.8088274212197,74.3075357146063,74.8062440079929,75.3049523013796,
75.8036605947662,76.3023688881528,76.7072426873232),.UNSPECIFIED.);
#800=B_SPLINE_CURVE_WITH_KNOTS('',3,(#42822,#42823,#42824,#42825,#42826,
#42827,#42828,#42829,#42830,#42831,#42832,#42833,#42834,#42835,#42836,#42837,
#42838,#42839,#42840,#42841,#42842,#42843,#42844,#42845,#42846,#42847,#42848,
#42849,#42850,#42851,#42852,#42853,#42854,#42855,#42856,#42857,#42858,#42859,
#42860,#42861,#42862,#42863,#42864),.UNSPECIFIED.,.F.,.F.,(4,3,3,3,3,3,
3,3,3,3,3,3,3,3,4),(-72.9640127846166,-72.8114108344464,-72.3127025410598,
-71.8139942476732,-71.3152859542866,-70.8165776609,-70.3178693675133,-69.8191610741267,
-69.3204527807401,-68.8217444873535,-68.3230361939669,-67.8243279005802,
-67.3256196071936,-66.826911313807,-66.680827477437),.UNSPECIFIED.);
#801=B_SPLINE_CURVE_WITH_KNOTS('',3,(#42869,#42870,#42871,#42872,#42873,
#42874,#42875,#42876,#42877,#42878,#42879,#42880,#42881,#42882,#42883,#42884,
#42885,#42886,#42887,#42888,#42889,#42890,#42891,#42892,#42893,#42894,#42895,
#42896,#42897,#42898,#42899,#42900,#42901,#42902,#42903,#42904,#42905,#42906,
#42907,#42908,#42909,#42910,#42911),.UNSPECIFIED.,.F.,.F.,(4,3,3,3,3,3,
3,3,3,3,3,3,3,3,4),(64.140872072964,64.3333698468739,64.8320781402605,65.3307864336472,
65.8294947270338,66.3282030204204,66.826911313807,67.3256196071937,67.8243279005803,
68.3230361939669,68.8217444873535,69.3204527807401,69.8191610741268,70.3178693675134,
70.4240573801436),.UNSPECIFIED.);
#802=B_SPLINE_CURVE_WITH_KNOTS('',3,(#42912,#42913,#42914,#42915,#42916,
#42917,#42918,#42919,#42920,#42921,#42922,#42923,#42924,#42925,#42926,#42927,
#42928,#42929,#42930,#42931,#42932,#42933,#42934,#42935,#42936,#42937,#42938,
#42939,#42940,#42941,#42942,#42943,#42944,#42945,#42946,#42947,#42948,#42949,
#42950,#42951),.UNSPECIFIED.,.F.,.F.,(4,3,3,3,3,3,3,3,3,3,3,3,3,4),(-66.680827477437,
-66.3282030204204,-65.8294947270337,-65.3307864336471,-64.8320781402605,
-64.3333698468739,-63.8346615534873,-63.3359532601007,-62.837244966714,
-62.3385366733274,-61.8398283799408,-61.3411200865542,-60.8424117931676,
-60.3976421702575),.UNSPECIFIED.);
#803=B_SPLINE_CURVE_WITH_KNOTS('',3,(#42956,#42957,#42958,#42959,#42960,
#42961,#42962,#42963,#42964,#42965,#42966,#42967,#42968,#42969,#42970,#42971,
#42972,#42973,#42974,#42975,#42976,#42977,#42978,#42979,#42980,#42981,#42982,
#42983,#42984,#42985,#42986,#42987,#42988,#42989,#42990,#42991,#42992,#42993,
#42994,#42995),.UNSPECIFIED.,.F.,.F.,(4,3,3,3,3,3,3,3,3,3,3,3,3,4),(57.8576867657844,
58.3488703262345,58.8475786196211,59.3462869130077,59.8449952063944,60.343703499781,
60.8424117931676,61.3411200865542,61.8398283799408,62.3385366733274,62.8372449667141,
63.3359532601007,63.8346615534873,64.140872072964),.UNSPECIFIED.);
#804=B_SPLINE_CURVE_WITH_KNOTS('',3,(#42996,#42997,#42998,#42999,#43000,
#43001,#43002,#43003,#43004,#43005,#43006,#43007,#43008,#43009,#43010,#43011,
#43012,#43013,#43014,#43015,#43016,#43017,#43018,#43019,#43020,#43021,#43022,
#43023,#43024,#43025,#43026,#43027,#43028,#43029,#43030,#43031,#43032,#43033,
#43034,#43035,#43036,#43037,#43038),.UNSPECIFIED.,.F.,.F.,(4,3,3,3,3,3,
3,3,3,3,3,3,3,3,4),(-60.3976421702575,-60.3437034997809,-59.8449952063943,
-59.3462869130077,-58.8475786196211,-58.3488703262345,-57.8501620328479,
-57.3514537394612,-56.8527454460746,-56.354037152688,-55.8553288593014,
-55.3566205659148,-54.8579122725281,-54.3592039791415,-54.1144568630779),
 .UNSPECIFIED.);
#805=B_SPLINE_CURVE_WITH_KNOTS('',3,(#43043,#43044,#43045,#43046,#43047,
#43048,#43049,#43050,#43051,#43052,#43053,#43054,#43055,#43056,#43057,#43058,
#43059,#43060,#43061,#43062,#43063,#43064,#43065,#43066,#43067,#43068,#43069,
#43070,#43071,#43072,#43073,#43074,#43075,#43076,#43077,#43078,#43079,#43080,
#43081,#43082,#43083,#43084,#43085),.UNSPECIFIED.,.F.,.F.,(4,3,3,3,3,3,
3,3,3,3,3,3,3,3,4),(51.5745014586048,51.8656625122084,52.3643708055951,
52.8630790989817,53.3617873923683,53.8604956857549,54.3592039791415,54.8579122725282,
55.3566205659148,55.8553288593014,56.354037152688,56.8527454460746,57.3514537394612,
57.8501620328479,57.8576867657844),.UNSPECIFIED.);
#806=B_SPLINE_CURVE_WITH_KNOTS('',3,(#43086,#43087,#43088,#43089,#43090,
#43091,#43092,#43093,#43094,#43095,#43096,#43097,#43098,#43099,#43100,#43101,
#43102,#43103,#43104,#43105,#43106,#43107,#43108,#43109,#43110,#43111,#43112,
#43113,#43114,#43115,#43116,#43117,#43118,#43119,#43120,#43121,#43122,#43123,
#43124,#43125,#43126,#43127,#43128),.UNSPECIFIED.,.F.,.F.,(4,3,3,3,3,3,
3,3,3,3,3,3,3,3,4),(-54.1144568630779,-53.8604956857549,-53.3617873923683,
-52.8630790989817,-52.3643708055951,-51.8656625122084,-51.3669542188218,
-50.8682459254352,-50.3695376320486,-49.8708293386619,-49.3721210452753,
-48.8734127518887,-48.3747044585021,-47.8759961651155,-47.8312715558983),
 .UNSPECIFIED.);
#807=B_SPLINE_CURVE_WITH_KNOTS('',3,(#43133,#43134,#43135,#43136,#43137,
#43138,#43139,#43140,#43141,#43142,#43143,#43144,#43145,#43146,#43147,#43148,
#43149,#43150,#43151,#43152,#43153,#43154,#43155,#43156,#43157,#43158,#43159,
#43160,#43161,#43162,#43163,#43164,#43165,#43166,#43167,#43168,#43169,#43170,
#43171,#43172,#43173,#43174,#43175),.UNSPECIFIED.,.F.,.F.,(4,3,3,3,3,3,
3,3,3,3,3,3,3,3,4),(45.2913161514252,45.3824546981824,45.881162991569,46.3798712849556,
46.8785795783422,47.3772878717289,47.8759961651155,48.3747044585021,48.8734127518887,
49.3721210452753,49.870829338662,50.3695376320486,50.8682459254352,51.3669542188218,
51.5745014586048),.UNSPECIFIED.);
#808=B_SPLINE_CURVE_WITH_KNOTS('',3,(#43176,#43177,#43178,#43179,#43180,
#43181,#43182,#43183,#43184,#43185,#43186,#43187,#43188,#43189,#43190,#43191,
#43192,#43193,#43194,#43195,#43196,#43197,#43198,#43199,#43200,#43201,#43202,
#43203,#43204,#43205,#43206,#43207,#43208,#43209,#43210,#43211,#43212,#43213,
#43214,#43215),.UNSPECIFIED.,.F.,.F.,(4,3,3,3,3,3,3,3,3,3,3,3,3,4),(-47.8312715558983,
-47.3772878717289,-46.8785795783422,-46.3798712849556,-45.881162991569,
-45.3824546981824,-44.8837464047958,-44.3850381114091,-43.8863298180225,
-43.3876215246359,-42.8889132312493,-42.3902049378627,-41.891496644476,
-41.5480862487187),.UNSPECIFIED.);
#809=B_SPLINE_CURVE_WITH_KNOTS('',3,(#43220,#43221,#43222,#43223,#43224,
#43225,#43226,#43227,#43228,#43229,#43230,#43231,#43232,#43233,#43234,#43235,
#43236,#43237,#43238,#43239,#43240,#43241,#43242,#43243,#43244,#43245,#43246,
#43247,#43248,#43249,#43250,#43251,#43252,#43253,#43254,#43255,#43256,#43257,
#43258,#43259),.UNSPECIFIED.,.F.,.F.,(4,3,3,3,3,3,3,3,3,3,3,3,3,4),(39.0081308442456,
39.3979551775429,39.8966634709296,40.3953717643162,40.8940800577028,41.3927883510894,
41.891496644476,42.3902049378627,42.8889132312493,43.3876215246359,43.8863298180225,
44.3850381114091,44.8837464047958,45.2913161514252),.UNSPECIFIED.);
#810=B_SPLINE_CURVE_WITH_KNOTS('',3,(#43260,#43261,#43262,#43263,#43264,
#43265,#43266,#43267,#43268,#43269,#43270,#43271,#43272,#43273,#43274,#43275,
#43276,#43277,#43278,#43279,#43280,#43281,#43282,#43283,#43284,#43285,#43286,
#43287,#43288,#43289,#43290,#43291,#43292,#43293,#43294,#43295,#43296,#43297,
#43298,#43299,#43300,#43301,#43302),.UNSPECIFIED.,.F.,.F.,(4,3,3,3,3,3,
3,3,3,3,3,3,3,3,4),(-41.5480862487187,-41.3927883510894,-40.8940800577028,
-40.3953717643162,-39.8966634709296,-39.3979551775429,-38.8992468841563,
-38.4005385907697,-37.9018302973831,-37.4031220039965,-36.9044137106098,
-36.4057054172232,-35.9069971238366,-35.40828883045,-35.2649009415391),
 .UNSPECIFIED.);
#811=B_SPLINE_CURVE_WITH_KNOTS('',3,(#43307,#43308,#43309,#43310,#43311,
#43312,#43313,#43314,#43315,#43316,#43317,#43318,#43319,#43320,#43321,#43322,
#43323,#43324,#43325,#43326,#43327,#43328,#43329,#43330,#43331,#43332,#43333,
#43334,#43335,#43336,#43337,#43338,#43339,#43340,#43341,#43342,#43343,#43344,
#43345,#43346,#43347,#43348,#43349),.UNSPECIFIED.,.F.,.F.,(4,3,3,3,3,3,
3,3,3,3,3,3,3,3,4),(32.7249455370661,32.9147473635169,33.4134556569035,
33.9121639502901,34.4108722436767,34.9095805370634,35.40828883045,35.9069971238366,
36.4057054172232,36.9044137106099,37.4031220039965,37.9018302973831,38.4005385907697,
38.8992468841563,39.0081308442456),.UNSPECIFIED.);
#812=B_SPLINE_CURVE_WITH_KNOTS('',3,(#43350,#43351,#43352,#43353,#43354,
#43355,#43356,#43357,#43358,#43359,#43360,#43361,#43362,#43363,#43364,#43365,
#43366,#43367,#43368,#43369,#43370,#43371,#43372,#43373,#43374,#43375,#43376,
#43377,#43378,#43379,#43380,#43381,#43382,#43383,#43384,#43385,#43386,#43387,
#43388,#43389),.UNSPECIFIED.,.F.,.F.,(4,3,3,3,3,3,3,3,3,3,3,3,3,4),(-35.2649009415391,
-34.9095805370634,-34.4108722436767,-33.9121639502901,-33.4134556569035,
-32.9147473635169,-32.4160390701303,-31.9173307767436,-31.418622483357,
-30.9199141899704,-30.4212058965838,-29.9224976031972,-29.4237893098105,
-28.9817156343595),.UNSPECIFIED.);
#813=B_SPLINE_CURVE_WITH_KNOTS('',3,(#43394,#43395,#43396,#43397,#43398,
#43399,#43400,#43401,#43402,#43403,#43404,#43405,#43406,#43407,#43408,#43409,
#43410,#43411,#43412,#43413,#43414,#43415,#43416,#43417,#43418,#43419,#43420,
#43421,#43422,#43423,#43424,#43425,#43426,#43427,#43428,#43429,#43430,#43431,
#43432,#43433),.UNSPECIFIED.,.F.,.F.,(4,3,3,3,3,3,3,3,3,3,3,3,3,4),(26.4417602298865,
26.9302478428775,27.4289561362641,27.9276644296507,28.4263727230373,28.9250810164239,
29.4237893098106,29.9224976031972,30.4212058965838,30.9199141899704,31.418622483357,
31.9173307767437,32.4160390701303,32.7249455370661),.UNSPECIFIED.);
#814=B_SPLINE_CURVE_WITH_KNOTS('',3,(#43434,#43435,#43436,#43437,#43438,
#43439,#43440,#43441,#43442,#43443,#43444,#43445,#43446,#43447,#43448,#43449,
#43450,#43451,#43452,#43453,#43454,#43455,#43456,#43457,#43458,#43459,#43460,
#43461,#43462,#43463,#43464,#43465,#43466,#43467,#43468,#43469,#43470,#43471,
#43472,#43473,#43474,#43475,#43476),.UNSPECIFIED.,.F.,.F.,(4,3,3,3,3,3,
3,3,3,3,3,3,3,3,4),(-28.9817156343595,-28.9250810164239,-28.4263727230373,
-27.9276644296507,-27.4289561362641,-26.9302478428774,-26.4315395494908,
-25.9328312561042,-25.4341229627176,-24.935414669331,-24.4367063759443,
-23.9379980825577,-23.4392897891711,-22.9405814957845,-22.6985303271799),
 .UNSPECIFIED.);
#815=B_SPLINE_CURVE_WITH_KNOTS('',3,(#43481,#43482,#43483,#43484,#43485,
#43486,#43487,#43488,#43489,#43490,#43491,#43492,#43493,#43494,#43495,#43496,
#43497,#43498,#43499,#43500,#43501,#43502,#43503,#43504,#43505,#43506,#43507,
#43508,#43509,#43510,#43511,#43512,#43513,#43514,#43515,#43516,#43517,#43518,
#43519,#43520,#43521,#43522,#43523),.UNSPECIFIED.,.F.,.F.,(4,3,3,3,3,3,
3,3,3,3,3,3,3,3,4),(20.1585749227069,20.4470400288514,20.945748322238,21.4444566156246,
21.9431649090113,22.4418732023979,22.9405814957845,23.4392897891711,23.9379980825577,
24.4367063759444,24.935414669331,25.4341229627176,25.9328312561042,26.4315395494908,
26.4417602298865),.UNSPECIFIED.);
#816=B_SPLINE_CURVE_WITH_KNOTS('',3,(#43524,#43525,#43526,#43527,#43528,
#43529,#43530,#43531,#43532,#43533,#43534,#43535,#43536,#43537,#43538,#43539,
#43540,#43541,#43542,#43543,#43544,#43545,#43546,#43547,#43548,#43549,#43550,
#43551,#43552,#43553,#43554,#43555,#43556,#43557,#43558,#43559,#43560,#43561,
#43562,#43563,#43564,#43565,#43566),.UNSPECIFIED.,.F.,.F.,(4,3,3,3,3,3,
3,3,3,3,3,3,3,3,4),(-22.6985303271799,-22.4418732023979,-21.9431649090112,
-21.4444566156246,-20.945748322238,-20.4470400288514,-19.9483317354648,
-19.4496234420782,-18.9509151486915,-18.4522068553049,-17.9534985619183,
-17.4547902685317,-16.9560819751451,-16.4573736817584,-16.4153450200003),
 .UNSPECIFIED.);
#817=B_SPLINE_CURVE_WITH_KNOTS('',3,(#43571,#43572,#43573,#43574,#43575,
#43576,#43577,#43578,#43579,#43580,#43581,#43582,#43583,#43584,#43585,#43586,
#43587,#43588,#43589,#43590,#43591,#43592,#43593,#43594,#43595,#43596,#43597,
#43598,#43599,#43600,#43601,#43602,#43603,#43604,#43605,#43606,#43607,#43608,
#43609,#43610,#43611,#43612,#43613),.UNSPECIFIED.,.F.,.F.,(4,3,3,3,3,3,
3,3,3,3,3,3,3,3,4),(13.8753896155273,13.9638322148253,14.462540508212,14.9612488015986,
15.4599570949852,15.9586653883718,16.4573736817584,16.9560819751451,17.4547902685317,
17.9534985619183,18.4522068553049,18.9509151486915,19.4496234420782,19.9483317354648,
20.1585749227069),.UNSPECIFIED.);
#818=B_SPLINE_CURVE_WITH_KNOTS('',3,(#43614,#43615,#43616,#43617,#43618,
#43619,#43620,#43621,#43622,#43623,#43624,#43625,#43626,#43627,#43628,#43629,
#43630,#43631,#43632,#43633,#43634,#43635,#43636,#43637,#43638,#43639,#43640,
#43641,#43642,#43643,#43644,#43645,#43646,#43647,#43648,#43649,#43650,#43651,
#43652,#43653),.UNSPECIFIED.,.F.,.F.,(4,3,3,3,3,3,3,3,3,3,3,3,3,4),(-16.4153450200003,
-15.9586653883718,-15.4599570949852,-14.9612488015986,-14.462540508212,
-13.9638322148253,-13.4651239214387,-12.9664156280521,-12.4677073346655,
-11.9689990412789,-11.4702907478922,-10.9715824545056,-10.472874161119,
-10.1321597128207),.UNSPECIFIED.);
#819=B_SPLINE_CURVE_WITH_KNOTS('',3,(#43659,#43660,#43661,#43662,#43663,
#43664,#43665,#43666,#43667,#43668,#43669,#43670,#43671,#43672,#43673,#43674,
#43675,#43676,#43677,#43678,#43679,#43680,#43681,#43682,#43683),
 .UNSPECIFIED.,.F.,.F.,(4,3,3,3,3,3,3,3,4),(-3.84897440564115,-3.49095805370634,
-2.99224976031972,-2.4935414669331,-1.99483317354648,-1.49612488015986,
-0.997416586773239,-0.49870829338662,0.),.UNSPECIFIED.);
#820=B_SPLINE_CURVE_WITH_KNOTS('',3,(#43686,#43687,#43688,#43689,#43690,
#43691,#43692,#43693,#43694,#43695,#43696,#43697,#43698,#43699,#43700,#43701,
#43702,#43703,#43704,#43705,#43706,#43707,#43708,#43709,#43710,#43711,#43712,
#43713,#43714,#43715,#43716,#43717,#43718,#43719,#43720,#43721,#43722),
 .UNSPECIFIED.,.F.,.F.,(4,3,3,3,3,3,3,3,3,3,3,3,4),(2.01640075321917,2.4935414669331,
2.99224976031972,3.49095805370634,3.98966634709296,4.48837464047958,4.9870829338662,
5.48579122725282,5.98449952063944,6.48320781402605,6.98191610741268,7.48062440079929,
7.59220430834772),.UNSPECIFIED.);
#821=B_SPLINE_CURVE_WITH_KNOTS('',3,(#43728,#43729,#43730,#43731,#43732,
#43733,#43734,#43735,#43736,#43737,#43738,#43739),.UNSPECIFIED.,.F.,.F.,
(4,1,1,1,1,1,1,1,1,4),(260.752190247953,261.213135555618,261.711843849004,
262.210552142391,262.709260435778,263.207968729164,263.706677022551,264.205385315938,
264.704093609324,265.202801902711),.UNSPECIFIED.);
#822=B_SPLINE_CURVE_WITH_KNOTS('',3,(#43742,#43743,#43744,#43745,#43746,
#43747,#43748,#43749,#43750,#43751,#43752,#43753,#43754,#43755),
 .UNSPECIFIED.,.F.,.F.,(4,1,1,1,1,1,1,1,1,1,1,4),(260.752190247953,260.760841199772,
261.259549493158,261.758257786545,262.256966079931,262.755674373318,263.254382666705,
263.753090960091,264.251799253478,264.750507546865,265.249215840251,265.726356553965),
 .UNSPECIFIED.);
#823=B_SPLINE_CURVE_WITH_KNOTS('',3,(#43760,#43761,#43762,#43763,#43764,
#43765,#43766,#43767,#43768,#43769,#43770,#43771,#43772,#43773,#43774,#43775,
#43776),.UNSPECIFIED.,.F.,.F.,(4,1,1,1,1,1,1,1,1,1,1,1,1,1,4),(254.469004940773,
254.729927741592,255.228636034978,255.727344328365,256.226052621752,256.724760915138,
257.223469208525,257.722177501912,258.220885795298,258.719594088685,259.218302382071,
259.717010675458,260.215718968845,260.714427262231,260.752190247953),
 .UNSPECIFIED.);
#824=B_SPLINE_CURVE_WITH_KNOTS('',3,(#43777,#43778,#43779,#43780,#43781,
#43782,#43783,#43784,#43785,#43786,#43787,#43788,#43789,#43790,#43791,#43792),
 .UNSPECIFIED.,.F.,.F.,(4,1,1,1,1,1,1,1,1,1,1,1,1,4),(254.469004940773,
254.776341679132,255.275049972519,255.773758265905,256.272466559292,256.771174852679,
257.269883146065,257.768591439452,258.267299732838,258.766008026225,259.264716319612,
259.763424612998,260.262132906385,260.752190247953),.UNSPECIFIED.);
#825=B_SPLINE_CURVE_WITH_KNOTS('',3,(#43797,#43798,#43799,#43800,#43801,
#43802,#43803,#43804,#43805,#43806,#43807,#43808,#43809,#43810,#43811,#43812,
#43813),.UNSPECIFIED.,.F.,.F.,(4,1,1,1,1,1,1,1,1,1,1,1,1,1,4),(248.185819633594,
248.246719927566,248.745428220952,249.244136514339,249.742844807726,250.241553101112,
250.740261394499,251.238969687886,251.737677981272,252.236386274659,252.735094568045,
253.233802861432,253.732511154819,254.231219448205,254.469004940773),
 .UNSPECIFIED.);
#826=B_SPLINE_CURVE_WITH_KNOTS('',3,(#43814,#43815,#43816,#43817,#43818,
#43819,#43820,#43821,#43822,#43823,#43824,#43825,#43826,#43827,#43828,#43829,
#43830),.UNSPECIFIED.,.F.,.F.,(4,1,1,1,1,1,1,1,1,1,1,1,1,1,4),(248.185819633594,
248.293133865106,248.791842158493,249.290550451879,249.789258745266,250.287967038653,
250.786675332039,251.285383625426,251.784091918812,252.282800212199,252.781508505586,
253.280216798972,253.778925092359,254.277633385745,254.469004940773),
 .UNSPECIFIED.);
#827=B_SPLINE_CURVE_WITH_KNOTS('',3,(#43835,#43836,#43837,#43838,#43839,
#43840,#43841,#43842,#43843,#43844,#43845,#43846,#43847,#43848,#43849,#43850),
 .UNSPECIFIED.,.F.,.F.,(4,1,1,1,1,1,1,1,1,1,1,1,1,4),(241.902634326414,
242.262220406926,242.760928700313,243.2596369937,243.758345287086,244.257053580473,
244.755761873859,245.254470167246,245.753178460633,246.251886754019,246.750595047406,
247.249303340793,247.748011634179,248.185819633594),.UNSPECIFIED.);
#828=B_SPLINE_CURVE_WITH_KNOTS('',3,(#43851,#43852,#43853,#43854,#43855,
#43856,#43857,#43858,#43859,#43860,#43861,#43862,#43863,#43864,#43865,#43866),
 .UNSPECIFIED.,.F.,.F.,(4,1,1,1,1,1,1,1,1,1,1,1,1,4),(241.902634326414,
242.308634344467,242.807342637853,243.30605093124,243.804759224626,244.303467518013,
244.8021758114,245.300884104786,245.799592398173,246.29830069156,246.797008984946,
247.295717278333,247.794425571719,248.185819633594),.UNSPECIFIED.);
#829=B_SPLINE_CURVE_WITH_KNOTS('',3,(#43871,#43872,#43873,#43874,#43875,
#43876,#43877,#43878,#43879,#43880,#43881,#43882,#43883,#43884,#43885,#43886,
#43887),.UNSPECIFIED.,.F.,.F.,(4,1,1,1,1,1,1,1,1,1,1,1,1,1,4),(235.619449019235,
235.7790125929,236.277720886287,236.776429179674,237.27513747306,237.773845766447,
238.272554059833,238.77126235322,239.269970646607,239.768678939993,240.26738723338,
240.766095526767,241.264803820153,241.76351211354,241.902634326414),
 .UNSPECIFIED.);
#830=B_SPLINE_CURVE_WITH_KNOTS('',3,(#43888,#43889,#43890,#43891,#43892,
#43893,#43894,#43895,#43896,#43897,#43898,#43899,#43900,#43901,#43902,#43903,
#43904),.UNSPECIFIED.,.F.,.F.,(4,1,1,1,1,1,1,1,1,1,1,1,1,1,4),(235.619449019235,
235.825426530441,236.324134823827,236.822843117214,237.3215514106,237.820259703987,
238.318967997374,238.81767629076,239.316384584147,239.815092877534,240.31380117092,
240.812509464307,241.311217757693,241.80992605108,241.902634326414),
 .UNSPECIFIED.);
#831=B_SPLINE_CURVE_WITH_KNOTS('',3,(#43909,#43910,#43911,#43912,#43913,
#43914,#43915,#43916,#43917,#43918,#43919,#43920,#43921,#43922,#43923,#43924),
 .UNSPECIFIED.,.F.,.F.,(4,1,1,1,1,1,1,1,1,1,1,1,1,4),(229.336263712055,
229.794513072261,230.293221365647,230.791929659034,231.290637952421,231.789346245807,
232.288054539194,232.786762832581,233.285471125967,233.784179419354,234.28288771274,
234.781596006127,235.280304299514,235.619449019235),.UNSPECIFIED.);
#832=B_SPLINE_CURVE_WITH_KNOTS('',3,(#43925,#43926,#43927,#43928,#43929,
#43930,#43931,#43932,#43933,#43934,#43935,#43936,#43937,#43938,#43939,#43940,
#43941),.UNSPECIFIED.,.F.,.F.,(4,1,1,1,1,1,1,1,1,1,1,1,1,1,4),(229.336263712055,
229.342218716414,229.840927009801,230.339635303188,230.838343596574,231.337051889961,
231.835760183348,232.334468476734,232.833176770121,233.331885063507,233.830593356894,
234.329301650281,234.828009943667,235.326718237054,235.619449019235),
 .UNSPECIFIED.);
#833=B_SPLINE_CURVE_WITH_KNOTS('',3,(#43946,#43947,#43948,#43949,#43950,
#43951,#43952,#43953,#43954,#43955,#43956,#43957,#43958,#43959,#43960,#43961,
#43962),.UNSPECIFIED.,.F.,.F.,(4,1,1,1,1,1,1,1,1,1,1,1,1,1,4),(223.053078404875,
223.311305258235,223.810013551621,224.308721845008,224.807430138395,225.306138431781,
225.804846725168,226.303555018555,226.802263311941,227.300971605328,227.799679898714,
228.298388192101,228.797096485488,229.295804778874,229.336263712055),
 .UNSPECIFIED.);
#834=B_SPLINE_CURVE_WITH_KNOTS('',3,(#43963,#43964,#43965,#43966,#43967,
#43968,#43969,#43970,#43971,#43972,#43973,#43974,#43975,#43976,#43977,#43978),
 .UNSPECIFIED.,.F.,.F.,(4,1,1,1,1,1,1,1,1,1,1,1,1,4),(223.053078404875,
223.357719195775,223.856427489162,224.355135782548,224.853844075935,225.352552369322,
225.851260662708,226.349968956095,226.848677249481,227.347385542868,227.846093836255,
228.344802129641,228.843510423028,229.336263712055),.UNSPECIFIED.);
#835=B_SPLINE_CURVE_WITH_KNOTS('',3,(#43983,#43984,#43985,#43986,#43987,
#43988,#43989,#43990,#43991,#43992,#43993,#43994,#43995,#43996,#43997,#43998,
#43999),.UNSPECIFIED.,.F.,.F.,(4,1,1,1,1,1,1,1,1,1,1,1,1,1,4),(216.769893097696,
216.828097444209,217.326805737595,217.825514030982,218.324222324369,218.822930617755,
219.321638911142,219.820347204529,220.319055497915,220.817763791302,221.316472084688,
221.815180378075,222.313888671462,222.812596964848,223.053078404875),
 .UNSPECIFIED.);
#836=B_SPLINE_CURVE_WITH_KNOTS('',3,(#44000,#44001,#44002,#44003,#44004,
#44005,#44006,#44007,#44008,#44009,#44010,#44011,#44012,#44013,#44014,#44015,
#44016),.UNSPECIFIED.,.F.,.F.,(4,1,1,1,1,1,1,1,1,1,1,1,1,1,4),(216.769893097696,
216.874511381749,217.373219675136,217.871927968522,218.370636261909,218.869344555295,
219.368052848682,219.866761142069,220.365469435455,220.864177728842,221.362886022229,
221.861594315615,222.360302609002,222.859010902388,223.053078404875),
 .UNSPECIFIED.);
#837=B_SPLINE_CURVE_WITH_KNOTS('',3,(#44021,#44022,#44023,#44024,#44025,
#44026,#44027,#44028,#44029,#44030,#44031,#44032,#44033,#44034,#44035,#44036),
 .UNSPECIFIED.,.F.,.F.,(4,1,1,1,1,1,1,1,1,1,1,1,1,4),(210.486707790516,
210.843597923569,211.342306216956,211.841014510343,212.339722803729,212.838431097116,
213.337139390502,213.835847683889,214.334555977276,214.833264270662,215.331972564049,
215.830680857436,216.329389150822,216.769893097696),.UNSPECIFIED.);
#838=B_SPLINE_CURVE_WITH_KNOTS('',3,(#44037,#44038,#44039,#44040,#44041,
#44042,#44043,#44044,#44045,#44046,#44047,#44048,#44049,#44050,#44051,#44052),
 .UNSPECIFIED.,.F.,.F.,(4,1,1,1,1,1,1,1,1,1,1,1,1,4),(210.486707790516,
210.89001186111,211.388720154496,211.887428447883,212.386136741269,212.884845034656,
213.383553328043,213.882261621429,214.380969914816,214.879678208203,215.378386501589,
215.877094794976,216.375803088362,216.769893097696),.UNSPECIFIED.);
#839=B_SPLINE_CURVE_WITH_KNOTS('',3,(#44057,#44058,#44059,#44060,#44061,
#44062,#44063,#44064,#44065,#44066,#44067,#44068,#44069,#44070,#44071,#44072,
#44073),.UNSPECIFIED.,.F.,.F.,(4,1,1,1,1,1,1,1,1,1,1,1,1,1,4),(204.203522483337,
204.360390109543,204.85909840293,205.357806696317,205.856514989703,206.35522328309,
206.853931576476,207.352639869863,207.85134816325,208.350056456636,208.848764750023,
209.347473043409,209.846181336796,210.344889630183,210.486707790516),
 .UNSPECIFIED.);
#840=B_SPLINE_CURVE_WITH_KNOTS('',3,(#44074,#44075,#44076,#44077,#44078,
#44079,#44080,#44081,#44082,#44083,#44084,#44085,#44086,#44087,#44088,#44089,
#44090),.UNSPECIFIED.,.F.,.F.,(4,1,1,1,1,1,1,1,1,1,1,1,1,1,4),(204.203522483337,
204.406804047084,204.90551234047,205.404220633857,205.902928927243,206.40163722063,
206.900345514017,207.399053807403,207.89776210079,208.396470394177,208.895178687563,
209.39388698095,209.892595274336,210.391303567723,210.486707790516),
 .UNSPECIFIED.);
#841=B_SPLINE_CURVE_WITH_KNOTS('',3,(#44095,#44096,#44097,#44098,#44099,
#44100,#44101,#44102,#44103,#44104,#44105,#44106,#44107,#44108,#44109,#44110),
 .UNSPECIFIED.,.F.,.F.,(4,1,1,1,1,1,1,1,1,1,1,1,1,4),(197.920337176157,
198.375890588904,198.87459888229,199.373307175677,199.872015469064,200.37072376245,
200.869432055837,201.368140349224,201.86684864261,202.365556935997,202.864265229383,
203.36297352277,203.861681816157,204.203522483337),.UNSPECIFIED.);
#842=B_SPLINE_CURVE_WITH_KNOTS('',3,(#44111,#44112,#44113,#44114,#44115,
#44116,#44117,#44118,#44119,#44120,#44121,#44122,#44123,#44124,#44125,#44126,
#44127),.UNSPECIFIED.,.F.,.F.,(4,1,1,1,1,1,1,1,1,1,1,1,1,1,4),(197.920337176157,
197.923596233057,198.422304526444,198.921012819831,199.419721113217,199.918429406604,
200.417137699991,200.915845993377,201.414554286764,201.91326258015,202.411970873537,
202.910679166924,203.40938746031,203.908095753697,204.203522483337),
 .UNSPECIFIED.);
#843=B_SPLINE_CURVE_WITH_KNOTS('',3,(#44132,#44133,#44134,#44135,#44136,
#44137,#44138,#44139,#44140,#44141,#44142,#44143,#44144,#44145,#44146,#44147,
#44148),.UNSPECIFIED.,.F.,.F.,(4,1,1,1,1,1,1,1,1,1,1,1,1,1,4),(191.637151868978,
191.892682774878,192.391391068264,192.890099361651,193.388807655038,193.887515948424,
194.386224241811,194.884932535198,195.383640828584,195.882349121971,196.381057415357,
196.879765708744,197.378474002131,197.877182295517,197.920337176157),
 .UNSPECIFIED.);
#844=B_SPLINE_CURVE_WITH_KNOTS('',3,(#44149,#44150,#44151,#44152,#44153,
#44154,#44155,#44156,#44157,#44158,#44159,#44160,#44161,#44162,#44163,#44164),
 .UNSPECIFIED.,.F.,.F.,(4,1,1,1,1,1,1,1,1,1,1,1,1,4),(191.637151868978,
191.939096712418,192.437805005805,192.936513299191,193.435221592578,193.933929885965,
194.432638179351,194.931346472738,195.430054766124,195.928763059511,196.427471352898,
196.926179646284,197.424887939671,197.920337176157),.UNSPECIFIED.);
#845=B_SPLINE_CURVE_WITH_KNOTS('',3,(#44169,#44170,#44171,#44172,#44173,
#44174,#44175,#44176,#44177,#44178,#44179,#44180,#44181,#44182,#44183,#44184,
#44185),.UNSPECIFIED.,.F.,.F.,(4,1,1,1,1,1,1,1,1,1,1,1,1,1,4),(185.353966561798,
185.409474960852,185.908183254238,186.406891547625,186.905599841012,187.404308134398,
187.903016427785,188.401724721171,188.900433014558,189.399141307945,189.897849601331,
190.396557894718,190.895266188105,191.393974481491,191.637151868978),
 .UNSPECIFIED.);
#846=B_SPLINE_CURVE_WITH_KNOTS('',3,(#44186,#44187,#44188,#44189,#44190,
#44191,#44192,#44193,#44194,#44195,#44196,#44197,#44198,#44199,#44200,#44201,
#44202),.UNSPECIFIED.,.F.,.F.,(4,1,1,1,1,1,1,1,1,1,1,1,1,1,4),(185.353966561798,
185.455888898392,185.954597191779,186.453305485165,186.952013778552,187.450722071938,
187.949430365325,188.448138658712,188.946846952098,189.445555245485,189.944263538872,
190.442971832258,190.941680125645,191.440388419031,191.637151868978),
 .UNSPECIFIED.);
#847=B_SPLINE_CURVE_WITH_KNOTS('',3,(#44207,#44208,#44209,#44210,#44211,
#44212,#44213,#44214,#44215,#44216,#44217,#44218,#44219,#44220,#44221,#44222),
 .UNSPECIFIED.,.F.,.F.,(4,1,1,1,1,1,1,1,1,1,1,1,1,4),(179.070781254618,
179.424975440212,179.923683733599,180.422392026986,180.921100320372,181.419808613759,
181.918516907145,182.417225200532,182.915933493919,183.414641787305,183.913350080692,
184.412058374079,184.910766667465,185.353966561798),.UNSPECIFIED.);
#848=B_SPLINE_CURVE_WITH_KNOTS('',3,(#44223,#44224,#44225,#44226,#44227,
#44228,#44229,#44230,#44231,#44232,#44233,#44234,#44235,#44236,#44237,#44238),
 .UNSPECIFIED.,.F.,.F.,(4,1,1,1,1,1,1,1,1,1,1,1,1,4),(179.070781254618,
179.471389377753,179.970097671139,180.468805964526,180.967514257912,181.466222551299,
181.964930844686,182.463639138072,182.962347431459,183.461055724845,183.959764018232,
184.458472311619,184.957180605005,185.353966561798),.UNSPECIFIED.);
#849=B_SPLINE_CURVE_WITH_KNOTS('',3,(#44243,#44244,#44245,#44246,#44247,
#44248,#44249,#44250,#44251,#44252,#44253,#44254,#44255,#44256,#44257,#44258,
#44259),.UNSPECIFIED.,.F.,.F.,(4,1,1,1,1,1,1,1,1,1,1,1,1,1,4),(172.787595947439,
172.941767626186,173.440475919573,173.93918421296,174.437892506346,174.936600799733,
175.435309093119,175.934017386506,176.432725679893,176.931433973279,177.430142266666,
177.928850560052,178.427558853439,178.926267146826,179.070781254618),
 .UNSPECIFIED.);
#850=B_SPLINE_CURVE_WITH_KNOTS('',3,(#44260,#44261,#44262,#44263,#44264,
#44265,#44266,#44267,#44268,#44269,#44270,#44271,#44272,#44273,#44274,#44275,
#44276),.UNSPECIFIED.,.F.,.F.,(4,1,1,1,1,1,1,1,1,1,1,1,1,1,4),(172.787595947439,
172.988181563726,173.486889857113,173.9855981505,174.484306443886,174.983014737273,
175.48172303066,175.980431324046,176.479139617433,176.977847910819,177.476556204206,
177.975264497593,178.473972790979,178.972681084366,179.070781254618),
 .UNSPECIFIED.);
#851=B_SPLINE_CURVE_WITH_KNOTS('',3,(#44281,#44282,#44283,#44284,#44285,
#44286,#44287,#44288,#44289,#44290,#44291,#44292,#44293,#44294,#44295,#44296),
 .UNSPECIFIED.,.F.,.F.,(4,1,1,1,1,1,1,1,1,1,1,1,1,4),(166.504410640259,
166.957268105547,167.455976398933,167.95468469232,168.453392985707,168.952101279093,
169.45080957248,169.949517865867,170.448226159253,170.94693445264,171.445642746026,
171.944351039413,172.4430593328,172.787595947439),.UNSPECIFIED.);
#852=B_SPLINE_CURVE_WITH_KNOTS('',3,(#44297,#44298,#44299,#44300,#44301,
#44302,#44303,#44304,#44305,#44306,#44307,#44308,#44309,#44310,#44311,#44312,
#44313),.UNSPECIFIED.,.F.,.F.,(4,1,1,1,1,1,1,1,1,1,1,1,1,1,4),(166.504410640259,
166.5049737497,167.003682043087,167.502390336474,168.00109862986,168.499806923247,
168.998515216634,169.49722351002,169.995931803407,170.494640096793,170.99334839018,
171.492056683567,171.990764976953,172.48947327034,172.787595947439),
 .UNSPECIFIED.);
#853=B_SPLINE_CURVE_WITH_KNOTS('',3,(#44318,#44319,#44320,#44321,#44322,
#44323,#44324,#44325,#44326,#44327,#44328,#44329,#44330,#44331,#44332,#44333,
#44334),.UNSPECIFIED.,.F.,.F.,(4,1,1,1,1,1,1,1,1,1,1,1,1,1,4),(160.22122533308,
160.474060291521,160.972768584907,161.471476878294,161.970185171681,162.468893465067,
162.967601758454,163.466310051841,163.965018345227,164.463726638614,164.962434932,
165.461143225387,165.959851518774,166.45855981216,166.504410640259),
 .UNSPECIFIED.);
#854=B_SPLINE_CURVE_WITH_KNOTS('',3,(#44335,#44336,#44337,#44338,#44339,
#44340,#44341,#44342,#44343,#44344,#44345,#44346,#44347,#44348,#44349,#44350),
 .UNSPECIFIED.,.F.,.F.,(4,1,1,1,1,1,1,1,1,1,1,1,1,4),(160.22122533308,160.520474229061,
161.019182522448,161.517890815834,162.016599109221,162.515307402608,163.014015695994,
163.512723989381,164.011432282767,164.510140576154,165.008848869541,165.507557162927,
166.006265456314,166.504410640259),.UNSPECIFIED.);
#855=B_SPLINE_CURVE_WITH_KNOTS('',3,(#44355,#44356,#44357,#44358,#44359,
#44360,#44361,#44362,#44363,#44364,#44365,#44366,#44367,#44368,#44369,#44370,
#44371),.UNSPECIFIED.,.F.,.F.,(4,1,1,1,1,1,1,1,1,1,1,1,1,1,4),(153.9380400259,
153.990852477495,154.489560770881,154.988269064268,155.486977357655,155.985685651041,
156.484393944428,156.983102237814,157.481810531201,157.980518824588,158.479227117974,
158.977935411361,159.476643704748,159.975351998134,160.22122533308),
 .UNSPECIFIED.);
#856=B_SPLINE_CURVE_WITH_KNOTS('',3,(#44372,#44373,#44374,#44375,#44376,
#44377,#44378,#44379,#44380,#44381,#44382,#44383,#44384,#44385,#44386,#44387,
#44388),.UNSPECIFIED.,.F.,.F.,(4,1,1,1,1,1,1,1,1,1,1,1,1,1,4),(153.9380400259,
154.037266415035,154.535974708422,155.034683001808,155.533391295195,156.032099588581,
156.530807881968,157.029516175355,157.528224468741,158.026932762128,158.525641055515,
159.024349348901,159.523057642288,160.021765935674,160.22122533308),
 .UNSPECIFIED.);
#857=B_SPLINE_CURVE_WITH_KNOTS('',3,(#44393,#44394,#44395,#44396,#44397,
#44398,#44399,#44400,#44401,#44402,#44403,#44404,#44405,#44406,#44407,#44408),
 .UNSPECIFIED.,.F.,.F.,(4,1,1,1,1,1,1,1,1,1,1,1,1,4),(147.654854718721,
148.006352956855,148.505061250242,149.003769543629,149.502477837015,150.001186130402,
150.499894423788,150.998602717175,151.497311010562,151.996019303948,152.494727597335,
152.993435890721,153.492144184108,153.9380400259),.UNSPECIFIED.);
#858=B_SPLINE_CURVE_WITH_KNOTS('',3,(#44409,#44410,#44411,#44412,#44413,
#44414,#44415,#44416,#44417,#44418,#44419,#44420,#44421,#44422,#44423,#44424),
 .UNSPECIFIED.,.F.,.F.,(4,1,1,1,1,1,1,1,1,1,1,1,1,4),(147.654854718721,
148.052766894396,148.551475187782,149.050183481169,149.548891774555,150.047600067942,
150.546308361329,151.045016654715,151.543724948102,152.042433241488,152.541141534875,
153.039849828262,153.538558121648,153.9380400259),.UNSPECIFIED.);
#859=B_SPLINE_CURVE_WITH_KNOTS('',3,(#44429,#44430,#44431,#44432,#44433,
#44434,#44435,#44436,#44437,#44438,#44439,#44440,#44441),.UNSPECIFIED.,
 .F.,.F.,(4,1,1,1,1,1,1,1,1,1,4),(141.371669411541,141.523145142829,142.520561729602,
143.517978316376,144.515394903149,145.512811489922,146.011519783309,146.510228076695,
147.008936370082,147.507644663469,147.654854718721),.UNSPECIFIED.);
#860=B_SPLINE_CURVE_WITH_KNOTS('',3,(#44442,#44443,#44444,#44445,#44446,
#44447,#44448,#44449,#44450,#44451),.UNSPECIFIED.,.F.,.F.,(4,1,1,1,1,1,
1,4),(141.371669411541,142.068267373756,143.065683960529,144.063100547303,
145.060517134076,146.057933720849,147.055350307622,147.654854718721),
 .UNSPECIFIED.);
#861=B_SPLINE_CURVE_WITH_KNOTS('',3,(#44456,#44457,#44458,#44459,#44460,
#44461,#44462,#44463,#44464,#44465),.UNSPECIFIED.,.F.,.F.,(4,1,1,1,1,1,
1,4),(135.088484104362,135.53864562219,136.536062208963,137.533478795736,
138.53089538251,139.528311969283,140.525728556056,141.371669411541),
 .UNSPECIFIED.);
#862=B_SPLINE_CURVE_WITH_KNOTS('',3,(#44466,#44467,#44468,#44469,#44470,
#44471,#44472,#44473,#44474,#44475),.UNSPECIFIED.,.F.,.F.,(4,1,1,1,1,1,
1,4),(135.088484104362,136.083767853117,137.08118443989,138.078601026663,
139.076017613436,140.07343420021,141.070850786983,141.371669411541),
 .UNSPECIFIED.);
#863=B_SPLINE_CURVE_WITH_KNOTS('',3,(#44480,#44481,#44482,#44483,#44484,
#44485,#44486,#44487,#44488,#44489,#44490,#44491,#44492),.UNSPECIFIED.,
 .F.,.F.,(4,1,1,1,1,1,1,1,1,1,4),(128.805298797182,129.055437808164,129.55414610155,
130.052854394937,130.551562688324,131.05027098171,131.548979275097,132.54639586187,
133.543812448643,134.541229035417,135.088484104362),.UNSPECIFIED.);
#864=B_SPLINE_CURVE_WITH_KNOTS('',3,(#44493,#44494,#44495,#44496,#44497,
#44498,#44499,#44500,#44501,#44502,#44503,#44504,#44505,#44506,#44507,#44508),
 .UNSPECIFIED.,.F.,.F.,(4,1,1,1,1,1,1,1,1,1,1,1,1,4),(128.805298797182,
129.101851745704,129.600560039091,130.099268332477,130.597976625864,131.09668491925,
131.595393212637,132.094101506024,132.59280979941,133.091518092797,133.590226386184,
134.08893467957,135.086351266343,135.088484104362),.UNSPECIFIED.);
#865=B_SPLINE_CURVE_WITH_KNOTS('',3,(#44513,#44514,#44515,#44516,#44517,
#44518,#44519,#44520,#44521,#44522,#44523,#44524,#44525,#44526,#44527,#44528,
#44529),.UNSPECIFIED.,.F.,.F.,(4,1,1,1,1,1,1,1,1,1,1,1,1,1,4),(122.522113490002,
122.572229994138,123.070938287524,123.569646580911,124.068354874298,124.567063167684,
125.065771461071,125.564479754457,126.063188047844,126.561896341231,127.060604634617,
127.559312928004,128.058021221391,128.556729514777,128.805298797182),
 .UNSPECIFIED.);
#866=B_SPLINE_CURVE_WITH_KNOTS('',3,(#44530,#44531,#44532,#44533,#44534,
#44535,#44536,#44537,#44538,#44539,#44540,#44541,#44542,#44543,#44544,#44545,
#44546),.UNSPECIFIED.,.F.,.F.,(4,1,1,1,1,1,1,1,1,1,1,1,1,1,4),(122.522113490002,
122.618643931678,123.117352225065,123.616060518451,124.114768811838,124.613477105224,
125.112185398611,125.610893691998,126.109601985384,126.608310278771,127.107018572158,
127.605726865544,128.104435158931,128.603143452317,128.805298797182),
 .UNSPECIFIED.);
#867=B_SPLINE_CURVE_WITH_KNOTS('',3,(#44551,#44552,#44553,#44554,#44555,
#44556,#44557,#44558,#44559,#44560,#44561,#44562,#44563,#44564,#44565,#44566),
 .UNSPECIFIED.,.F.,.F.,(4,1,1,1,1,1,1,1,1,1,1,1,1,4),(116.238928182823,
116.587730473498,117.086438766885,117.585147060271,118.083855353658,118.582563647045,
119.081271940431,119.579980233818,120.078688527205,120.577396820591,121.076105113978,
121.574813407364,122.073521700751,122.522113490002),.UNSPECIFIED.);
#868=B_SPLINE_CURVE_WITH_KNOTS('',3,(#44567,#44568,#44569,#44570,#44571,
#44572,#44573,#44574,#44575,#44576,#44577,#44578,#44579,#44580,#44581,#44582),
 .UNSPECIFIED.,.F.,.F.,(4,1,1,1,1,1,1,1,1,1,1,1,1,4),(116.238928182823,
116.634144411039,117.132852704425,117.631560997812,118.130269291198,118.628977584585,
119.127685877972,119.626394171358,120.125102464745,120.623810758131,121.122519051518,
121.621227344905,122.119935638291,122.522113490002),.UNSPECIFIED.);
#869=B_SPLINE_CURVE_WITH_KNOTS('',3,(#44587,#44588,#44589,#44590,#44591,
#44592,#44593,#44594,#44595,#44596,#44597,#44598,#44599,#44600,#44601,#44602,
#44603),.UNSPECIFIED.,.F.,.F.,(4,1,1,1,1,1,1,1,1,1,1,1,1,1,4),(109.955742875643,
110.104522659472,110.603230952859,111.101939246245,111.600647539632,112.099355833019,
112.598064126405,113.096772419792,113.595480713179,114.094189006565,114.592897299952,
115.091605593338,115.590313886725,116.089022180112,116.238928182823),
 .UNSPECIFIED.);
#870=B_SPLINE_CURVE_WITH_KNOTS('',3,(#44604,#44605,#44606,#44607,#44608,
#44609,#44610,#44611,#44612,#44613,#44614,#44615,#44616,#44617,#44618,#44619,
#44620),.UNSPECIFIED.,.F.,.F.,(4,1,1,1,1,1,1,1,1,1,1,1,1,1,4),(109.955742875643,
110.150936597012,110.649644890399,111.148353183786,111.647061477172,112.145769770559,
112.644478063946,113.143186357332,113.641894650719,114.140602944105,114.639311237492,
115.138019530879,115.636727824265,116.135436117652,116.238928182823),
 .UNSPECIFIED.);
#871=B_SPLINE_CURVE_WITH_KNOTS('',3,(#44625,#44626,#44627,#44628,#44629,
#44630,#44631,#44632,#44633,#44634,#44635,#44636,#44637,#44638,#44639,#44640),
 .UNSPECIFIED.,.F.,.F.,(4,1,1,1,1,1,1,1,1,1,1,1,1,4),(103.672557568464,
104.120023138833,104.618731432219,105.117439725606,105.616148018993,106.114856312379,
106.613564605766,107.112272899152,107.610981192539,108.109689485926,108.608397779312,
109.107106072699,109.605814366086,109.955742875643),.UNSPECIFIED.);
#872=B_SPLINE_CURVE_WITH_KNOTS('',3,(#44641,#44642,#44643,#44644,#44645,
#44646,#44647,#44648,#44649,#44650,#44651,#44652,#44653,#44654,#44655,#44656),
 .UNSPECIFIED.,.F.,.F.,(4,1,1,1,1,1,1,1,1,1,1,1,1,4),(103.672557568464,
104.166437076373,104.66514536976,105.163853663146,105.662561956533,106.161270249919,
106.659978543306,107.158686836693,107.657395130079,108.156103423466,108.654811716853,
109.153520010239,109.652228303626,109.955742875643),.UNSPECIFIED.);
#873=B_SPLINE_CURVE_WITH_KNOTS('',3,(#44661,#44662,#44663,#44664,#44665,
#44666,#44667,#44668,#44669,#44670,#44671,#44672,#44673,#44674,#44675,#44676,
#44677),.UNSPECIFIED.,.F.,.F.,(4,1,1,1,1,1,1,1,1,1,1,1,1,1,4),(97.389372261284,
97.6368153248067,98.1355236181933,98.63423191158,99.1329402049666,99.6316484983532,
100.13035679174,100.629065085126,101.127773378513,101.6264816719,102.125189965286,
102.623898258673,103.12260655206,103.621314845446,103.672557568464),
 .UNSPECIFIED.);
#874=B_SPLINE_CURVE_WITH_KNOTS('',3,(#44678,#44679,#44680,#44681,#44682,
#44683,#44684,#44685,#44686,#44687,#44688,#44689,#44690,#44691,#44692,#44693,
#44694),.UNSPECIFIED.,.F.,.F.,(4,1,1,1,1,1,1,1,1,1,1,1,1,1,4),(97.389372261284,
97.683229262347,98.1819375557336,98.6806458491202,99.1793541425068,99.6780624358935,
100.17677072928,100.675479022667,101.174187316053,101.67289560944,102.171603902827,
102.670312196213,103.1690204896,103.667728782986,103.672557568464),
 .UNSPECIFIED.);
#875=B_SPLINE_CURVE_WITH_KNOTS('',3,(#44699,#44700,#44701,#44702,#44703,
#44704,#44705,#44706,#44707,#44708,#44709,#44710,#44711,#44712,#44713,#44714,
#44715),.UNSPECIFIED.,.F.,.F.,(4,1,1,1,1,1,1,1,1,1,1,1,1,1,4),(91.1061869541044,
91.1536075107807,91.6523158041673,92.1510240975539,92.6497323909405,93.1484406843271,
93.6471489777138,94.1458572711004,94.644565564487,95.1432738578736,95.6419821512603,
96.1406904446469,96.6393987380335,97.1381070314201,97.389372261284),
 .UNSPECIFIED.);
#876=B_SPLINE_CURVE_WITH_KNOTS('',3,(#44716,#44717,#44718,#44719,#44720,
#44721,#44722,#44723,#44724,#44725,#44726,#44727,#44728,#44729,#44730,#44731,
#44732),.UNSPECIFIED.,.F.,.F.,(4,1,1,1,1,1,1,1,1,1,1,1,1,1,4),(91.1061869541044,
91.2000214483209,91.6987297417075,92.1974380350942,92.6961463284808,93.1948546218674,
93.693562915254,94.1922712086406,94.6909795020272,95.1896877954139,95.6883960888005,
96.1871043821871,96.6858126755737,97.1845209689603,97.389372261284),
 .UNSPECIFIED.);
#877=B_SPLINE_CURVE_WITH_KNOTS('',3,(#44737,#44738,#44739,#44740,#44741,
#44742,#44743,#44744,#44745,#44746,#44747,#44748,#44749,#44750,#44751,#44752),
 .UNSPECIFIED.,.F.,.F.,(4,1,1,1,1,1,1,1,1,1,1,1,1,4),(84.8230016469248,
85.1691079901412,85.6678162835279,86.1665245769145,86.6652328703011,87.1639411636877,
87.6626494570743,88.161357750461,88.6600660438476,89.1587743372342,89.6574826306208,
90.1561909240074,90.654899217394,91.1061869541044),.UNSPECIFIED.);
#878=B_SPLINE_CURVE_WITH_KNOTS('',3,(#44753,#44754,#44755,#44756,#44757,
#44758,#44759,#44760,#44761,#44762,#44763,#44764,#44765,#44766,#44767,#44768),
 .UNSPECIFIED.,.F.,.F.,(4,1,1,1,1,1,1,1,1,1,1,1,1,4),(84.8230016469248,
85.2155219276815,85.7142302210681,86.2129385144547,86.7116468078413,87.2103551012279,
87.7090633946146,88.2077716880012,88.7064799813878,89.2051882747744,89.703896568161,
90.2026048615477,90.7013131549343,91.1061869541044),.UNSPECIFIED.);
#879=B_SPLINE_CURVE_WITH_KNOTS('',3,(#44773,#44774,#44775,#44776,#44777,
#44778,#44779,#44780,#44781,#44782,#44783,#44784,#44785,#44786,#44787,#44788,
#44789),.UNSPECIFIED.,.F.,.F.,(4,1,1,1,1,1,1,1,1,1,1,1,1,1,4),(78.5398163397452,
78.6859001761152,79.1846084695018,79.6833167628884,80.1820250562751,80.6807333496617,
81.1794416430483,81.6781499364349,82.1768582298215,82.6755665232081,83.1742748165948,
83.6729831099814,84.171691403368,84.6703996967546,84.8230016469248),
 .UNSPECIFIED.);
#880=B_SPLINE_CURVE_WITH_KNOTS('',3,(#44790,#44791,#44792,#44793,#44794,
#44795,#44796,#44797,#44798,#44799,#44800,#44801,#44802,#44803,#44804,#44805,
#44806),.UNSPECIFIED.,.F.,.F.,(4,1,1,1,1,1,1,1,1,1,1,1,1,1,4),(78.5398163397452,
78.7323141136554,79.231022407042,79.7297307004287,80.2284389938153,80.7271472872019,
81.2258555805885,81.7245638739751,82.2232721673618,82.7219804607484,83.220688754135,
83.7193970475216,84.2181053409082,84.7168136342949,84.8230016469248),
 .UNSPECIFIED.);
#881=B_SPLINE_CURVE_WITH_KNOTS('',3,(#44811,#44812,#44813,#44814,#44815,
#44816,#44817,#44818,#44819,#44820,#44821,#44822,#44823,#44824,#44825,#44826),
 .UNSPECIFIED.,.F.,.F.,(4,1,1,1,1,1,1,1,1,1,1,1,1,4),(72.2566310325657,
72.7014006554758,73.2001089488624,73.698817242249,74.1975255356356,74.6962338290222,
75.1949421224089,75.6936504157955,76.1923587091821,76.6910670025687,77.1897752959553,
77.6884835893419,78.1871918827286,78.5398163397452),.UNSPECIFIED.);
#882=B_SPLINE_CURVE_WITH_KNOTS('',3,(#44827,#44828,#44829,#44830,#44831,
#44832,#44833,#44834,#44835,#44836,#44837,#44838,#44839,#44840,#44841,#44842),
 .UNSPECIFIED.,.F.,.F.,(4,1,1,1,1,1,1,1,1,1,1,1,1,4),(72.2566310325657,
72.747814593016,73.2465228864026,73.7452311797892,74.2439394731758,74.7426477665625,
75.2413560599491,75.7400643533357,76.2387726467223,76.7374809401089,77.2361892334956,
77.7348975268822,78.2336058202688,78.5398163397452),.UNSPECIFIED.);
#883=B_SPLINE_CURVE_WITH_KNOTS('',3,(#44847,#44848,#44849,#44850,#44851,
#44852,#44853,#44854,#44855,#44856,#44857,#44858,#44859,#44860,#44861,#44862,
#44863),.UNSPECIFIED.,.F.,.F.,(4,1,1,1,1,1,1,1,1,1,1,1,1,1,4),(65.973445725386,
66.2181928414497,66.7169011348363,67.2156094282229,67.7143177216096,68.2130260149962,
68.7117343083828,69.2104426017694,69.709150895156,70.2078591885427,70.7065674819293,
71.2052757753159,71.7039840687025,72.2026923620891,72.2566310325657),
 .UNSPECIFIED.);
#884=B_SPLINE_CURVE_WITH_KNOTS('',3,(#44864,#44865,#44866,#44867,#44868,
#44869,#44870,#44871,#44872,#44873,#44874,#44875,#44876,#44877,#44878,#44879,
#44880),.UNSPECIFIED.,.F.,.F.,(4,1,1,1,1,1,1,1,1,1,1,1,1,1,4),(65.973445725386,
66.2646067789899,66.7633150723765,67.2620233657632,67.7607316591498,68.2594399525364,
68.758148245923,69.2568565393096,69.7555648326963,70.2542731260829,70.7529814194695,
71.2516897128561,71.7503980062427,72.2491062996294,72.2566310325657),
 .UNSPECIFIED.);
#885=B_SPLINE_CURVE_WITH_KNOTS('',3,(#44885,#44886,#44887,#44888,#44889,
#44890,#44891,#44892,#44893,#44894,#44895,#44896,#44897,#44898,#44899,#44900,
#44901),.UNSPECIFIED.,.F.,.F.,(4,1,1,1,1,1,1,1,1,1,1,1,1,1,4),(59.6902604182065,
59.7349850274237,60.2336933208103,60.7324016141969,61.2311099075835,61.7298182009701,
62.2285264943567,62.7272347877434,63.22594308113,63.7246513745166,64.2233596679032,
64.7220679612898,65.2207762546765,65.7194845480631,65.973445725386),
 .UNSPECIFIED.);
#886=B_SPLINE_CURVE_WITH_KNOTS('',3,(#44902,#44903,#44904,#44905,#44906,
#44907,#44908,#44909,#44910,#44911,#44912,#44913,#44914,#44915,#44916,#44917,
#44918),.UNSPECIFIED.,.F.,.F.,(4,1,1,1,1,1,1,1,1,1,1,1,1,1,4),(59.6902604182065,
59.7813989649639,60.2801072583505,60.7788155517371,61.2775238451237,61.7762321385104,
62.274940431897,62.7736487252836,63.2723570186702,63.7710653120568,64.2697736054434,
64.7684818988301,65.2671901922167,65.7658984856033,65.973445725386),
 .UNSPECIFIED.);
#887=B_SPLINE_CURVE_WITH_KNOTS('',3,(#44923,#44924,#44925,#44926,#44927,
#44928,#44929,#44930,#44931,#44932,#44933,#44934,#44935,#44936,#44937,#44938),
 .UNSPECIFIED.,.F.,.F.,(4,1,1,1,1,1,1,1,1,1,1,1,1,4),(53.4070751110269,
53.7504855067842,54.2491938001708,54.7479020935575,55.2466103869441,55.7453186803307,
56.2440269737173,56.7427352671039,57.2414435604906,57.7401518538772,58.2388601472638,
58.7375684406504,59.236276734037,59.6902604182065),.UNSPECIFIED.);
#888=B_SPLINE_CURVE_WITH_KNOTS('',3,(#44939,#44940,#44941,#44942,#44943,
#44944,#44945,#44946,#44947,#44948,#44949,#44950,#44951,#44952,#44953,#44954),
 .UNSPECIFIED.,.F.,.F.,(4,1,1,1,1,1,1,1,1,1,1,1,1,4),(53.4070751110269,
53.7968994443244,54.2956077377111,54.7943160310977,55.2930243244843,55.7917326178709,
56.2904409112575,56.7891492046442,57.2878574980308,57.7865657914174,58.285274084804,
58.7839823781906,59.2826906715772,59.6902604182065),.UNSPECIFIED.);
#889=B_SPLINE_CURVE_WITH_KNOTS('',3,(#44959,#44960,#44961,#44962,#44963,
#44964,#44965,#44966,#44967,#44968,#44969,#44970,#44971,#44972,#44973,#44974,
#44975),.UNSPECIFIED.,.F.,.F.,(4,1,1,1,1,1,1,1,1,1,1,1,1,1,4),(47.1238898038473,
47.2672776927582,47.7659859861448,48.2646942795314,48.763402572918,49.2621108663046,
49.7608191596913,50.2595274530779,50.7582357464645,51.2569440398511,51.7556523332377,
52.2543606266244,52.753068920011,53.2517772133976,53.4070751110269),
 .UNSPECIFIED.);
#890=B_SPLINE_CURVE_WITH_KNOTS('',3,(#44976,#44977,#44978,#44979,#44980,
#44981,#44982,#44983,#44984,#44985,#44986,#44987,#44988,#44989,#44990,#44991,
#44992),.UNSPECIFIED.,.F.,.F.,(4,1,1,1,1,1,1,1,1,1,1,1,1,1,4),(47.1238898038473,
47.3136916302984,47.812399923685,48.3111082170716,48.8098165104582,49.3085248038449,
49.8072330972315,50.3059413906181,50.8046496840047,51.3033579773913,51.802066270778,
52.3007745641646,52.7994828575512,53.2981911509378,53.4070751110269),
 .UNSPECIFIED.);
#891=B_SPLINE_CURVE_WITH_KNOTS('',3,(#44997,#44998,#44999,#45000,#45001,
#45002,#45003,#45004,#45005,#45006,#45007,#45008,#45009,#45010,#45011,#45012),
 .UNSPECIFIED.,.F.,.F.,(4,1,1,1,1,1,1,1,1,1,1,1,1,4),(40.8407044966677,
41.2827781721187,41.7814864655054,42.280194758892,42.7789030522786,43.2776113456652,
43.7763196390518,44.2750279324384,44.7737362258251,45.2724445192117,45.7711528125983,
46.2698611059849,46.7685693993716,47.1238898038473),.UNSPECIFIED.);
#892=B_SPLINE_CURVE_WITH_KNOTS('',3,(#45013,#45014,#45015,#45016,#45017,
#45018,#45019,#45020,#45021,#45022,#45023,#45024,#45025,#45026,#45027,#45028),
 .UNSPECIFIED.,.F.,.F.,(4,1,1,1,1,1,1,1,1,1,1,1,1,4),(40.8407044966677,
41.3291921096589,41.8279004030456,42.3266086964322,42.8253169898188,43.3240252832054,
43.822733576592,44.3214418699787,44.8201501633653,45.3188584567519,45.8175667501385,
46.3162750435251,46.8149833369118,47.1238898038473),.UNSPECIFIED.);
#893=B_SPLINE_CURVE_WITH_KNOTS('',3,(#45033,#45034,#45035,#45036,#45037,
#45038,#45039,#45040,#45041,#45042,#45043,#45044,#45045,#45046,#45047,#45048,
#45049),.UNSPECIFIED.,.F.,.F.,(4,1,1,1,1,1,1,1,1,1,1,1,1,1,4),(34.5575191894881,
34.7995703580927,35.2982786514793,35.7969869448659,36.2956952382525,36.7944035316392,
37.2931118250258,37.7918201184124,38.290528411799,38.7892367051856,39.2879449985723,
39.7866532919589,40.2853615853455,40.7840698787321,40.8407044966677),
 .UNSPECIFIED.);
#894=B_SPLINE_CURVE_WITH_KNOTS('',3,(#45050,#45051,#45052,#45053,#45054,
#45055,#45056,#45057,#45058,#45059,#45060,#45061,#45062,#45063,#45064,#45065,
#45066),.UNSPECIFIED.,.F.,.F.,(4,1,1,1,1,1,1,1,1,1,1,1,1,1,4),(34.5575191894881,
34.8459842956329,35.3446925890195,35.8434008824061,36.3421091757927,36.8408174691794,
37.339525762566,37.8382340559526,38.3369423493392,38.8356506427259,39.3343589361125,
39.8330672294991,40.3317755228857,40.8304838162723,40.8407044966677),
 .UNSPECIFIED.);
#895=B_SPLINE_CURVE_WITH_KNOTS('',3,(#45071,#45072,#45073,#45074,#45075,
#45076,#45077,#45078,#45079,#45080,#45081,#45082,#45083,#45084,#45085,#45086,
#45087),.UNSPECIFIED.,.F.,.F.,(4,1,1,1,1,1,1,1,1,1,1,1,1,1,4),(28.2743338823085,
28.3163625440666,28.8150708374532,29.3137791308399,29.8124874242265,30.3111957176131,
30.8099040109997,31.3086123043863,31.807320597773,32.3060288911596,32.8047371845462,
33.3034454779328,33.8021537713194,34.3008620647061,34.5575191894881),
 .UNSPECIFIED.);
#896=B_SPLINE_CURVE_WITH_KNOTS('',3,(#45088,#45089,#45090,#45091,#45092,
#45093,#45094,#45095,#45096,#45097,#45098,#45099,#45100,#45101,#45102,#45103,
#45104),.UNSPECIFIED.,.F.,.F.,(4,1,1,1,1,1,1,1,1,1,1,1,1,1,4),(28.2743338823085,
28.3627764816068,28.8614847749935,29.3601930683801,29.8589013617667,30.3576096551533,
30.8563179485399,31.3550262419266,31.8537345353132,32.3524428286998,32.8511511220864,
33.349859415473,33.8485677088597,34.3472760022463,34.5575191894881),
 .UNSPECIFIED.);
#897=B_SPLINE_CURVE_WITH_KNOTS('',3,(#45109,#45110,#45111,#45112,#45113,
#45114,#45115,#45116,#45117,#45118,#45119,#45120,#45121,#45122,#45123,#45124),
 .UNSPECIFIED.,.F.,.F.,(4,1,1,1,1,1,1,1,1,1,1,1,1,4),(21.9911485751289,
22.3318630234272,22.8305713168138,23.3292796102004,23.8279879035871,24.3266961969737,
24.8254044903603,25.3241127837469,25.8228210771335,26.3215293705201,26.8202376639068,
27.3189459572934,27.81765425068,28.2743338823085),.UNSPECIFIED.);
#898=B_SPLINE_CURVE_WITH_KNOTS('',3,(#45125,#45126,#45127,#45128,#45129,
#45130,#45131,#45132,#45133,#45134,#45135,#45136,#45137,#45138,#45139,#45140),
 .UNSPECIFIED.,.F.,.F.,(4,1,1,1,1,1,1,1,1,1,1,1,1,4),(21.9911485751289,
22.3782769609674,22.876985254354,23.3756935477406,23.8744018411273,24.3731101345139,
24.8718184279005,25.3705267212871,25.8692350146737,26.3679433080604,26.866651601447,
27.3653598948336,27.8640681882202,28.2743338823085),.UNSPECIFIED.);
#899=B_SPLINE_CURVE_WITH_KNOTS('',3,(#45146,#45147,#45148,#45149,#45150,
#45151),.UNSPECIFIED.,.F.,.F.,(4,1,1,4),(14.3989442667815,14.8976525601681,
15.3963608535547,15.7079632679493),.UNSPECIFIED.);
#900=B_SPLINE_CURVE_WITH_KNOTS('',3,(#45154,#45155,#45156,#45157,#45158,
#45159,#45160),.UNSPECIFIED.,.F.,.F.,(4,1,1,1,4),(13.8753896155274,14.3525303292413,
14.8512386226279,15.3499469160145,15.7079632679493),.UNSPECIFIED.);
#901=B_SPLINE_CURVE_WITH_KNOTS('',3,(#45162,#45163,#45164,#45165,#45166,
#45167,#45168,#45169,#45170,#45171,#45172,#45173,#45174,#45175,#45176,#45177,
#45178,#45179,#45180,#45181,#45182,#45183,#45184,#45185,#45186,#45187,#45188,
#45189,#45190,#45191,#45192,#45193,#45194,#45195,#45196,#45197,#45198,#45199,
#45200,#45201,#45202,#45203,#45204,#45205,#45206,#45207,#45208,#45209,#45210,
#45211,#45212,#45213,#45214,#45215,#45216,#45217,#45218,#45219,#45220,#45221,
#45222,#45223,#45224,#45225,#45226,#45227,#45228,#45229,#45230,#45231,#45232,
#45233,#45234,#45235,#45236,#45237,#45238,#45239,#45240,#45241,#45242,#45243,
#45244,#45245,#45246,#45247,#45248,#45249,#45250,#45251,#45252,#45253,#45254,
#45255,#45256,#45257,#45258,#45259,#45260,#45261,#45262,#45263,#45264,#45265,
#45266,#45267),.UNSPECIFIED.,.F.,.F.,(4,3,3,3,3,3,3,3,3,3,3,3,3,3,3,3,3,
3,3,3,3,3,3,3,3,3,3,3,3,3,3,3,3,3,3,4),(-0.972375876542216,-0.931557379101648,
-0.890218542042487,-0.869392708916521,-0.861677237530619,-0.819813801882793,
-0.781167845425456,-0.769475619651221,-0.760546025724648,-0.754411794373795,
-0.74252188896812,-0.700976733031894,-0.65877791376378,-0.616292150528589,
-0.588572673703484,-0.579879678859757,-0.574332463387633,-0.531223905437004,
-0.505414243228169,-0.462559206201071,-0.419378313085458,-0.399643768345371,
-0.391565714980685,-0.383732909736738,-0.340135839018284,-0.296193649678293,
-0.261501955164762,-0.217668074296404,-0.204748702273309,-0.197210738162037,
-0.192140598791969,-0.1468449795757,-0.102253744983165,-0.0566059334550285,
-0.0109581219268922,0.),.UNSPECIFIED.);
#902=B_SPLINE_CURVE_WITH_KNOTS('',3,(#45268,#45269,#45270,#45271,#45272,
#45273,#45274,#45275,#45276,#45277,#45278,#45279,#45280,#45281,#45282,#45283,
#45284,#45285,#45286,#45287,#45288,#45289,#45290,#45291,#45292,#45293,#45294,
#45295,#45296,#45297,#45298,#45299,#45300,#45301,#45302,#45303,#45304,#45305,
#45306,#45307,#45308,#45309,#45310,#45311,#45312,#45313,#45314,#45315,#45316,
#45317,#45318,#45319,#45320,#45321,#45322,#45323,#45324,#45325,#45326,#45327,
#45328,#45329,#45330,#45331,#45332,#45333,#45334,#45335,#45336,#45337,#45338,
#45339,#45340,#45341,#45342,#45343,#45344,#45345,#45346,#45347,#45348,#45349,
#45350,#45351,#45352,#45353,#45354,#45355,#45356,#45357,#45358,#45359,#45360,
#45361,#45362,#45363,#45364,#45365,#45366,#45367,#45368,#45369,#45370),
 .UNSPECIFIED.,.F.,.F.,(4,3,3,3,3,3,3,3,3,3,3,3,3,3,3,3,3,3,3,3,3,3,3,3,
3,3,3,3,3,3,3,3,3,3,4),(-0.970006587573357,-0.925489021709122,-0.880831606117785,
-0.860106336836479,-0.852213503588024,-0.808023919462815,-0.764142093829507,
-0.741127929891385,-0.732995659095006,-0.720260268196198,-0.676886083169421,
-0.633189091074775,-0.58989356338977,-0.561603730397805,-0.548456029491321,
-0.542926374323804,-0.500045602531121,-0.476734231421911,-0.433752968122039,
-0.390893110149348,-0.372012672166435,-0.363955407652349,-0.356648068723258,
-0.314412819484753,-0.272458136815843,-0.239849606286048,-0.197688110523089,
-0.185715478561588,-0.179206252930902,-0.173732780061183,-0.132200928727762,
-0.0907046629355285,-0.0499294541163457,-0.00977294415302305,0.),
 .UNSPECIFIED.);
#903=B_SPLINE_CURVE_WITH_KNOTS('',3,(#45372,#45373,#45374,#45375,#45376,
#45377,#45378,#45379,#45380,#45381,#45382,#45383,#45384,#45385,#45386,#45387,
#45388),.UNSPECIFIED.,.F.,.F.,(4,1,1,1,1,1,1,1,1,1,1,1,1,1,4),(15.7079632679493,
15.8486552094011,16.3473635027878,16.8460717961744,17.344780089561,17.8434883829476,
18.3421966763342,18.8409049697209,19.3396132631075,19.8383215564941,20.3370298498807,
20.8357381432673,21.334446436654,21.8331547300406,21.9911485751289),
 .UNSPECIFIED.);
#904=B_SPLINE_CURVE_WITH_KNOTS('',3,(#45389,#45390,#45391,#45392,#45393,
#45394,#45395,#45396,#45397,#45398,#45399,#45400,#45401,#45402,#45403,#45404,
#45405),.UNSPECIFIED.,.F.,.F.,(4,1,1,1,1,1,1,1,1,1,1,1,1,1,4),(15.7079632679493,
15.8950691469414,16.393777440328,16.8924857337146,17.3911940271012,17.8899023204878,
18.3886106138744,18.8873189072611,19.3860272006477,19.8847354940343,20.3834437874209,
20.8821520808075,21.3808603741942,21.8795686675808,21.9911485751289),
 .UNSPECIFIED.);
#905=B_SPLINE_CURVE_WITH_KNOTS('',3,(#47394,#47395,#47396,#47397,#47398,
#47399,#47400,#47401,#47402,#47403,#47404,#47405,#47406,#47407,#47408,#47409,
#47410,#47411,#47412,#47413,#47414,#47415,#47416,#47417,#47418,#47419,#47420,
#47421,#47422,#47423,#47424,#47425,#47426,#47427,#47428,#47429,#47430,#47431,
#47432,#47433,#47434,#47435,#47436,#47437,#47438,#47439,#47440,#47441,#47442,
#47443,#47444,#47445,#47446,#47447,#47448,#47449,#47450,#47451,#47452,#47453,
#47454,#47455,#47456,#47457,#47458,#47459,#47460,#47461,#47462,#47463,#47464,
#47465,#47466,#47467,#47468,#47469,#47470,#47471,#47472,#47473,#47474,#47475,
#47476,#47477,#47478,#47479,#47480,#47481,#47482,#47483,#47484,#47485,#47486,
#47487,#47488,#47489,#47490,#47491,#47492,#47493,#47494,#47495,#47496,#47497,
#47498,#47499),.UNSPECIFIED.,.F.,.F.,(4,3,3,3,3,3,3,3,3,3,3,3,3,3,3,3,3,
3,3,3,3,3,3,3,3,3,3,3,3,3,3,3,3,3,3,4),(0.,0.040424976116911,0.081552621191953,
0.123116379418818,0.164484386952486,0.177258002125512,0.182429040513286,
0.224585211732574,0.229750939065668,0.271485437391992,0.313663426362065,
0.351832391899687,0.358992185792409,0.364434825962351,0.407093430609824,
0.45008484068709,0.466339288512555,0.509174339674324,0.534227886997736,
0.545013114142881,0.550666578456316,0.593964513128218,0.637614398405316,
0.68114810979745,0.709602718261623,0.725600523556765,0.736529828545389,
0.743509911151027,0.78723345430323,0.830193673824424,0.848440235266336,
0.858098500020291,0.902703209392534,0.947246712359152,0.959074332388006,
0.970006587573436),.UNSPECIFIED.);
#906=B_SPLINE_CURVE_WITH_KNOTS('',3,(#47500,#47501,#47502,#47503,#47504,
#47505,#47506,#47507,#47508,#47509,#47510,#47511,#47512,#47513,#47514,#47515,
#47516,#47517,#47518,#47519,#47520,#47521,#47522,#47523,#47524,#47525,#47526,
#47527,#47528,#47529,#47530,#47531,#47532,#47533,#47534,#47535,#47536,#47537,
#47538,#47539,#47540,#47541,#47542),.UNSPECIFIED.,.F.,.F.,(4,3,3,3,3,3,
3,3,3,3,3,3,3,3,4),(-10.1321597128207,-9.97416586773239,-9.47545757434577,
-8.97674928095915,-8.47804098757253,-7.97933269418591,-7.48062440079929,
-6.98191610741267,-6.48320781402605,-5.98449952063943,-5.48579122725281,
-4.98708293386619,-4.48837464047957,-3.98966634709295,-3.84897440564115),
 .UNSPECIFIED.);
#907=B_SPLINE_CURVE_WITH_KNOTS('',3,(#49531,#49532,#49533,#49534,#49535,
#49536,#49537,#49538,#49539,#49540,#49541,#49542,#49543,#49544,#49545,#49546,
#49547,#49548,#49549,#49550,#49551,#49552,#49553,#49554,#49555,#49556,#49557,
#49558,#49559,#49560,#49561,#49562,#49563,#49564,#49565,#49566,#49567,#49568,
#49569,#49570),.UNSPECIFIED.,.F.,.F.,(4,3,3,3,3,3,3,3,3,3,3,3,3,4),(7.59220430834772,
7.97933269418591,8.47804098757253,8.97674928095915,9.47545757434577,9.97416586773239,
10.472874161119,10.9715824545056,11.4702907478922,11.9689990412789,12.4677073346655,
12.9664156280521,13.4651239214387,13.8753896155273),.UNSPECIFIED.);
#908=B_SPLINE_CURVE_WITH_KNOTS('',3,(#49571,#49572,#49573,#49574,#49575,
#49576,#49577,#49578,#49579,#49580,#49581,#49582,#49583,#49584,#49585,#49586,
#49587,#49588,#49589,#49590,#49591,#49592,#49593,#49594,#49595,#49596,#49597,
#49598,#49599,#49600,#49601,#49602,#49603,#49604,#49605,#49606,#49607,#49608,
#49609,#49610,#49611,#49612,#49613,#49614,#49615,#49616,#49617,#49618,#49619,
#49620,#49621,#49622,#49623,#49624,#49625,#49626,#49627,#49628,#49629,#49630,
#49631,#49632,#49633,#49634,#49635,#49636,#49637,#49638,#49639,#49640,#49641,
#49642,#49643,#49644,#49645,#49646,#49647,#49648,#49649,#49650,#49651,#49652,
#49653,#49654,#49655,#49656,#49657,#49658,#49659,#49660,#49661,#49662,#49663,
#49664,#49665,#49666,#49667,#49668,#49669,#49670,#49671,#49672,#49673,#49674,
#49675,#49676),.UNSPECIFIED.,.F.,.F.,(4,3,3,3,3,3,3,3,3,3,3,3,3,3,3,3,3,
3,3,3,3,3,3,3,3,3,3,3,3,3,3,3,3,3,3,4),(0.,0.0441576970943254,0.088758491595093,
0.133154322886181,0.177017836347152,0.193697049021019,0.19965188566726,
0.243475277581627,0.250795014009384,0.294669452308725,0.338569619728244,
0.37767568962022,0.38721824859893,0.393275053464473,0.436458598855563,0.479377262352089,
0.494993899296151,0.538189921814499,0.562468636762688,0.572092716170009,
0.579226787127647,0.621711263641225,0.664154373258728,0.70594102510778,
0.732419641400012,0.748330061688134,0.757222465646011,0.763401818269173,
0.80529293424602,0.844615778238015,0.861173358979439,0.871344162504664,
0.912748133225373,0.953576775379504,0.962584310214001,0.972375876542313),
 .UNSPECIFIED.);
#909=B_SPLINE_CURVE_WITH_KNOTS('',3,(#49682,#49683,#49684,#49685,#49686,
#49687,#49688,#49689,#49690,#49691,#49692,#49693,#49694,#49695,#49696,#49697,
#49698,#49699,#49700,#49701,#49702,#49703,#49704,#49705,#49706,#49707,#49708,
#49709,#49710,#49711,#49712,#49713,#49714,#49715,#49716,#49717,#49718,#49719,
#49720,#49721,#49722,#49723,#49724,#49725,#49726,#49727,#49728,#49729,#49730,
#49731,#49732,#49733,#49734,#49735,#49736,#49737,#49738,#49739,#49740,#49741,
#49742,#49743,#49744,#49745,#49746,#49747,#49748,#49749,#49750,#49751,#49752,
#49753,#49754,#49755,#49756,#49757,#49758,#49759,#49760,#49761,#49762,#49763,
#49764,#49765,#49766,#49767,#49768,#49769,#49770,#49771,#49772,#49773,#49774,
#49775,#49776,#49777,#49778,#49779,#49780,#49781,#49782,#49783,#49784),
 .UNSPECIFIED.,.F.,.F.,(4,3,3,3,3,3,3,3,3,3,3,3,3,3,3,3,3,3,3,3,3,3,3,3,
3,3,3,3,3,3,3,3,3,3,4),(-0.972375876542414,-0.931565253728255,-0.890231005347033,
-0.869571408761885,-0.861266125665987,-0.819404433385386,-0.781321836236662,
-0.759040374121689,-0.752934683192443,-0.743239239087938,-0.701695078724687,
-0.659497058703992,-0.617009387497169,-0.589480672868744,-0.57644702705794,
-0.5714452780933,-0.528325351620324,-0.506894528983471,-0.464054318866617,
-0.420876860304666,-0.401240281040809,-0.388666227231065,-0.383537192824514,
-0.339939758883143,-0.295998103578765,-0.263784226193809,-0.219954566467475,
-0.204809517925579,-0.197308554950036,-0.192241015625869,-0.147699202975487,
-0.103111401264591,-0.0585925831444644,-0.0140737650243382,0.),
 .UNSPECIFIED.);
#910=B_SPLINE_CURVE_WITH_KNOTS('',3,(#49785,#49786,#49787,#49788,#49789,
#49790,#49791,#49792,#49793,#49794,#49795,#49796,#49797,#49798,#49799,#49800,
#49801,#49802,#49803,#49804,#49805,#49806,#49807,#49808,#49809,#49810,#49811,
#49812,#49813,#49814,#49815,#49816,#49817,#49818,#49819,#49820,#49821,#49822,
#49823,#49824,#49825,#49826,#49827,#49828,#49829,#49830,#49831,#49832,#49833,
#49834,#49835,#49836,#49837,#49838,#49839,#49840,#49841,#49842,#49843,#49844,
#49845,#49846,#49847,#49848,#49849,#49850,#49851,#49852,#49853,#49854,#49855,
#49856,#49857,#49858,#49859,#49860,#49861,#49862,#49863,#49864,#49865,#49866,
#49867,#49868,#49869,#49870,#49871,#49872,#49873,#49874,#49875,#49876,#49877,
#49878,#49879,#49880,#49881,#49882,#49883,#49884,#49885,#49886,#49887),
 .UNSPECIFIED.,.F.,.F.,(4,3,3,3,3,3,3,3,3,3,3,3,3,3,3,3,3,3,3,3,3,3,3,3,
3,3,3,3,3,3,3,3,3,3,4),(-0.97000658757332,-0.925493326456513,-0.880835987444213,
-0.86024842639854,-0.852333874766883,-0.808142692209155,-0.764580356539862,
-0.742334794451242,-0.733010188832428,-0.721018020870569,-0.677646574841948,
-0.633950360266973,-0.590648734368262,-0.562539792613221,-0.550153753024242,
-0.542978093928587,-0.50009796533363,-0.478212967348099,-0.435235450336473,
-0.392367497022972,-0.373572235159268,-0.361228651726056,-0.355614322341834,
-0.313378921971217,-0.271427075980555,-0.242005402113342,-0.199831951142943,
-0.186315085816715,-0.179649707786883,-0.174232916759018,-0.132703725702247,
-0.0912075908119877,-0.0504161836307489,-0.0125558726020182,0.),
 .UNSPECIFIED.);
#911=B_SPLINE_CURVE_WITH_KNOTS('',3,(#49889,#49890,#49891,#49892,#49893,
#49894,#49895,#49896,#49897,#49898,#49899,#49900,#49901,#49902,#49903,#49904,
#49905),.UNSPECIFIED.,.F.,.F.,(4,1,1,1,1,1,1,1,1,1,1,1,1,1,4),(15.707963267949,
15.8363896981257,16.3335648026029,16.8307399070801,17.3279150115573,17.8250901160345,
18.3222652205117,18.8194403249889,19.3166154294662,19.8137905339434,20.3109656384206,
20.8081407428978,21.305315847375,21.8024909518522,21.9911485751286),
 .UNSPECIFIED.);
#912=B_SPLINE_CURVE_WITH_KNOTS('',3,(#49906,#49907,#49908,#49909,#49910,
#49911,#49912,#49913,#49914,#49915,#49916,#49917,#49918,#49919,#49920,#49921,
#49922),.UNSPECIFIED.,.F.,.F.,(4,1,1,1,1,1,1,1,1,1,1,1,1,1,4),(15.707963267949,
15.8904695802126,16.3876446846898,16.884819789167,17.3819948936443,17.8791699981215,
18.3763451025987,18.8735202070759,19.3706953115531,19.8678704160303,20.3650455205075,
20.8622206249848,21.359395729462,21.8565708339392,21.9911485751286),
 .UNSPECIFIED.);
#913=B_SPLINE_CURVE_WITH_KNOTS('',3,(#51215,#51216,#51217,#51218,#51219,
#51220,#51221,#51222,#51223,#51224,#51225,#51226,#51227,#51228,#51229,#51230,
#51231,#51232,#51233,#51234,#51235,#51236,#51237,#51238,#51239,#51240,#51241,
#51242,#51243,#51244,#51245,#51246,#51247,#51248,#51249,#51250,#51251,#51252,
#51253,#51254,#51255,#51256,#51257,#51258,#51259,#51260,#51261,#51262,#51263,
#51264,#51265,#51266,#51267,#51268,#51269,#51270,#51271,#51272,#51273,#51274,
#51275,#51276,#51277,#51278,#51279,#51280,#51281,#51282,#51283,#51284,#51285,
#51286,#51287,#51288,#51289,#51290,#51291,#51292,#51293,#51294,#51295,#51296,
#51297,#51298,#51299,#51300,#51301,#51302,#51303,#51304,#51305,#51306,#51307,
#51308,#51309,#51310,#51311,#51312,#51313,#51314,#51315,#51316,#51317,#51318,
#51319,#51320),.UNSPECIFIED.,.F.,.F.,(4,3,3,3,3,3,3,3,3,3,3,3,3,3,3,3,3,
3,3,3,3,3,3,3,3,3,3,3,3,3,3,3,3,3,3,4),(0.,0.0404156030320338,0.0815364170314856,
0.123099442202208,0.164471164259153,0.177417333177223,0.182894508577368,
0.225046885757466,0.229033692090525,0.270767557602402,0.312945697761686,
0.350924838148176,0.357993918766748,0.363846074008531,0.406502560546029,
0.449493818503337,0.464862259307647,0.507689818261392,0.532644888553053,
0.54674918267878,0.552366866895522,0.595682545020243,0.639338821245014,
0.682868010841828,0.707330380594682,0.725816624679753,0.736955855775304,
0.74358314378864,0.787317407834192,0.829479796072424,0.846856648451819,
0.854114186312316,0.898699022066203,0.94326334774114,0.955966960787121,
0.97000658757331),.UNSPECIFIED.);
#914=B_SPLINE_CURVE_WITH_KNOTS('',3,(#51321,#51322,#51323,#51324,#51325,
#51326,#51327,#51328,#51329,#51330,#51331,#51332,#51333,#51334,#51335,#51336,
#51337,#51338,#51339,#51340,#51341,#51342,#51343,#51344,#51345,#51346,#51347,
#51348,#51349,#51350,#51351,#51352,#51353,#51354,#51355,#51356,#51357,#51358,
#51359,#51360,#51361,#51362,#51363),.UNSPECIFIED.,.F.,.F.,(4,3,3,3,3,3,
3,3,3,3,3,3,3,3,4),(-10.1321597128207,-9.94350208954429,-9.44632698506708,
-8.94915188058987,-8.45197677611265,-7.95480167163544,-7.45762656715822,
-6.96045146268101,-6.46327635820379,-5.96610125372657,-5.46892614924936,
-4.97175104477214,-4.47457594029493,-3.97740083581771,-3.848974405641),
 .UNSPECIFIED.);
#915=B_SPLINE_CURVE_WITH_KNOTS('',3,(#52656,#52657,#52658,#52659,#52660,
#52661,#52662,#52663,#52664,#52665,#52666,#52667,#52668,#52669,#52670,#52671,
#52672,#52673,#52674,#52675,#52676,#52677,#52678,#52679,#52680,#52681,#52682,
#52683,#52684,#52685,#52686,#52687,#52688,#52689,#52690,#52691,#52692,#52693,
#52694,#52695),.UNSPECIFIED.,.F.,.F.,(4,3,3,3,3,3,3,3,3,3,3,3,3,4),(7.59220430834767,
7.95480167163543,8.45197677611264,8.94915188058986,9.44632698506707,9.94350208954429,
10.4406771940215,10.9378522984987,11.4350274029759,11.9322025074531,12.4293776119304,
12.9265527164076,13.4237278208848,13.8753896155273),.UNSPECIFIED.);
#916=B_SPLINE_CURVE_WITH_KNOTS('',3,(#52696,#52697,#52698,#52699,#52700,
#52701,#52702,#52703,#52704,#52705,#52706,#52707,#52708,#52709,#52710,#52711,
#52712,#52713,#52714,#52715,#52716,#52717,#52718,#52719,#52720,#52721,#52722,
#52723,#52724,#52725,#52726,#52727,#52728,#52729,#52730,#52731,#52732,#52733,
#52734,#52735,#52736,#52737,#52738,#52739,#52740,#52741,#52742,#52743,#52744,
#52745,#52746,#52747,#52748,#52749,#52750,#52751,#52752,#52753,#52754,#52755,
#52756,#52757,#52758,#52759,#52760,#52761,#52762,#52763,#52764,#52765,#52766,
#52767,#52768,#52769,#52770,#52771,#52772,#52773,#52774,#52775,#52776,#52777,
#52778,#52779,#52780,#52781,#52782,#52783,#52784,#52785,#52786,#52787,#52788,
#52789,#52790,#52791,#52792,#52793,#52794,#52795,#52796,#52797,#52798,#52799,
#52800,#52801),.UNSPECIFIED.,.F.,.F.,(4,3,3,3,3,3,3,3,3,3,3,3,3,3,3,3,3,
3,3,3,3,3,3,3,3,3,3,3,3,3,3,3,3,3,3,4),(0.,0.044150773052086,0.0887487507111273,
0.133148741969068,0.177019043965151,0.193023436662248,0.199907412815446,
0.24373234733986,0.250033573379215,0.293906609053928,0.337808296166161,
0.376734021006827,0.385567082155686,0.391401994113249,0.434581851246655,
0.477513379513922,0.493511195528826,0.53671130462677,0.560905212030567,
0.574207000071321,0.579201605029167,0.62168463125547,0.664125603281933,
0.705919109414855,0.730262563857148,0.748325604460628,0.757394747707568,
0.762943677116111,0.804834492856293,0.843575066915537,0.859283154994003,
0.866889043776386,0.908311110283104,0.949189929713081,0.959796789093269,
0.972375876542504),.UNSPECIFIED.);
#917=B_SPLINE_CURVE_WITH_KNOTS('',3,(#53336,#53337,#53338,#53339,#53340,
#53341,#53342,#53343,#53344,#53345),.UNSPECIFIED.,.F.,.F.,(4,3,3,4),(-4.09293042013065,
-3.97826971642971,-2.98370228732228,-2.06773127522702),.UNSPECIFIED.);
#918=B_SPLINE_CURVE_WITH_KNOTS('',3,(#53348,#53349,#53350,#53351,#53352,
#53353,#53354,#53355,#53356,#53357),.UNSPECIFIED.,.F.,.F.,(4,3,3,4),(0.,
0.49759560509741,0.995191210194833,1.11639350868605),.UNSPECIFIED.);
#919=B_SPLINE_CURVE_WITH_KNOTS('',3,(#53362,#53363,#53364,#53365,#53366,
#53367,#53368,#53369,#53370,#53371,#53372,#53373,#53374,#53375,#53376,#53377,
#53378,#53379,#53380,#53381,#53382,#53383),.UNSPECIFIED.,.F.,.F.,(4,3,3,
3,3,3,3,4),(-10.3761157273102,-9.94567429107427,-8.95110686196684,-7.95653943285942,
-6.96197200375199,-5.96740457464456,-4.97283714553713,-4.09293042013065),
 .UNSPECIFIED.);
#920=B_SPLINE_CURVE_WITH_KNOTS('',3,(#53384,#53385,#53386,#53387,#53388,
#53389,#53390,#53391,#53392,#53393,#53394,#53395,#53396,#53397,#53398,#53399,
#53400,#53401,#53402,#53403,#53404,#53405),.UNSPECIFIED.,.F.,.F.,(4,3,3,
3,3,3,3,4),(1.11639350868605,1.99038242038966,2.98557363058448,3.9807648407793,
4.97595605097413,5.97114726116895,6.96633847136377,7.39957881586564),
 .UNSPECIFIED.);
#921=B_SPLINE_CURVE_WITH_KNOTS('',3,(#53410,#53411,#53412,#53413,#53414,
#53415,#53416,#53417,#53418,#53419,#53420,#53421,#53422,#53423,#53424,#53425,
#53426,#53427,#53428,#53429,#53430,#53431),.UNSPECIFIED.,.F.,.F.,(4,3,3,
3,3,3,3,4),(-16.6593010344898,-15.9130788657188,-14.9185114366114,-13.923944007504,
-12.9293765783965,-11.9348091492891,-10.9402417201817,-10.3761157273102),
 .UNSPECIFIED.);
#922=B_SPLINE_CURVE_WITH_KNOTS('',3,(#53432,#53433,#53434,#53435,#53436,
#53437,#53438,#53439,#53440,#53441,#53442,#53443,#53444,#53445,#53446,#53447,
#53448,#53449,#53450,#53451,#53452,#53453),.UNSPECIFIED.,.F.,.F.,(4,3,3,
3,3,3,3,4),(7.39957881586564,7.9615296815586,8.95672089175343,9.95191210194825,
10.9471033121431,11.9422945223379,12.9374857325327,13.6827641230452),
 .UNSPECIFIED.);
#923=B_SPLINE_CURVE_WITH_KNOTS('',3,(#53458,#53459,#53460,#53461,#53462,
#53463,#53464,#53465,#53466,#53467,#53468,#53469,#53470,#53471,#53472,#53473,
#53474,#53475,#53476,#53477,#53478,#53479,#53480,#53481,#53482),
 .UNSPECIFIED.,.F.,.F.,(4,3,3,3,3,3,3,3,4),(-22.9424863416694,-22.8750508694708,
-21.8804834403634,-20.885916011256,-19.8913485821485,-18.8967811530411,
-17.9022137239337,-16.9076462948263,-16.6593010344898),.UNSPECIFIED.);
#924=B_SPLINE_CURVE_WITH_KNOTS('',3,(#53483,#53484,#53485,#53486,#53487,
#53488,#53489,#53490,#53491,#53492,#53493,#53494,#53495,#53496,#53497,#53498,
#53499,#53500,#53501,#53502,#53503,#53504,#53505,#53506,#53507),
 .UNSPECIFIED.,.F.,.F.,(4,3,3,3,3,3,3,3,4),(13.6827641230452,13.9326769427276,
14.9278681529224,15.9230593631172,16.918250573312,17.9134417835069,18.9086329937017,
19.9038242038965,19.9659494302248),.UNSPECIFIED.);
#925=B_SPLINE_CURVE_WITH_KNOTS('',3,(#53512,#53513,#53514,#53515,#53516,
#53517,#53518,#53519,#53520,#53521,#53522,#53523,#53524,#53525,#53526,#53527,
#53528,#53529,#53530,#53531,#53532,#53533),.UNSPECIFIED.,.F.,.F.,(4,3,3,
3,3,3,3,4),(-29.225671648849,-28.8424554441154,-27.847888015008,-26.8533205859005,
-25.8587531567931,-24.8641857276857,-23.8696182985782,-22.9424863416694),
 .UNSPECIFIED.);
#926=B_SPLINE_CURVE_WITH_KNOTS('',3,(#53534,#53535,#53536,#53537,#53538,
#53539,#53540,#53541,#53542,#53543,#53544,#53545,#53546,#53547,#53548,#53549,
#53550,#53551,#53552,#53553,#53554,#53555),.UNSPECIFIED.,.F.,.F.,(4,3,3,
3,3,3,3,4),(19.9659494302248,20.8990154140913,21.8942066242861,22.889397834481,
23.8845890446758,24.8797802548706,25.8749714650654,26.2491347374044),
 .UNSPECIFIED.);
#927=B_SPLINE_CURVE_WITH_KNOTS('',3,(#53560,#53561,#53562,#53563,#53564,
#53565,#53566,#53567,#53568,#53569,#53570,#53571,#53572,#53573,#53574,#53575,
#53576,#53577,#53578,#53579,#53580,#53581),.UNSPECIFIED.,.F.,.F.,(4,3,3,
3,3,3,3,4),(-35.5088569560286,-34.8098600187599,-33.8152925896525,-32.8207251605451,
-31.8261577314377,-30.8315903023302,-29.8370228732228,-29.225671648849),
 .UNSPECIFIED.);
#928=B_SPLINE_CURVE_WITH_KNOTS('',3,(#53582,#53583,#53584,#53585,#53586,
#53587,#53588,#53589,#53590,#53591,#53592,#53593,#53594,#53595,#53596,#53597,
#53598,#53599,#53600,#53601,#53602,#53603),.UNSPECIFIED.,.F.,.F.,(4,3,3,
3,3,3,3,4),(26.2491347374044,26.8701626752603,27.8653538854551,28.8605450956499,
29.8557363058448,30.8509275160396,31.8461187262344,32.532320044584),
 .UNSPECIFIED.);
#929=B_SPLINE_CURVE_WITH_KNOTS('',3,(#53608,#53609,#53610,#53611,#53612,
#53613,#53614,#53615,#53616,#53617,#53618,#53619,#53620,#53621,#53622,#53623,
#53624,#53625,#53626,#53627,#53628,#53629,#53630,#53631,#53632),
 .UNSPECIFIED.,.F.,.F.,(4,3,3,3,3,3,3,3,4),(-41.7920422632082,-41.7718320225119,
-40.7772645934045,-39.7826971642971,-38.7881297351896,-37.7935623060822,
-36.7989948769748,-35.8044274478674,-35.5088569560286),.UNSPECIFIED.);
#930=B_SPLINE_CURVE_WITH_KNOTS('',3,(#53633,#53634,#53635,#53636,#53637,
#53638,#53639,#53640,#53641,#53642,#53643,#53644,#53645,#53646,#53647,#53648,
#53649,#53650,#53651,#53652,#53653,#53654,#53655,#53656,#53657),
 .UNSPECIFIED.,.F.,.F.,(4,3,3,3,3,3,3,3,4),(32.532320044584,32.8413099364292,
33.8365011466241,34.8316923568189,35.8268835670137,36.8220747772085,37.8172659874034,
38.8124571975982,38.8155053517636),.UNSPECIFIED.);
#931=B_SPLINE_CURVE_WITH_KNOTS('',3,(#53662,#53663,#53664,#53665,#53666,
#53667,#53668,#53669,#53670,#53671,#53672,#53673,#53674,#53675,#53676,#53677,
#53678,#53679,#53680,#53681,#53682,#53683),.UNSPECIFIED.,.F.,.F.,(4,3,3,
3,3,3,3,4),(-48.0752275703878,-47.7392365971565,-46.7446691680491,-45.7501017389416,
-44.7555343098342,-43.7609668807268,-42.7663994516193,-41.7920422632082),
 .UNSPECIFIED.);
#932=B_SPLINE_CURVE_WITH_KNOTS('',3,(#53684,#53685,#53686,#53687,#53688,
#53689,#53690,#53691,#53692,#53693,#53694,#53695,#53696,#53697,#53698,#53699,
#53700,#53701,#53702,#53703,#53704,#53705),.UNSPECIFIED.,.F.,.F.,(4,3,3,
3,3,3,3,4),(38.8155053517636,39.807648407793,40.8028396179878,41.7980308281826,
42.7932220383775,43.7884132485723,44.7836044587671,45.0986906589432),
 .UNSPECIFIED.);
#933=B_SPLINE_CURVE_WITH_KNOTS('',3,(#53710,#53711,#53712,#53713,#53714,
#53715,#53716,#53717,#53718,#53719,#53720,#53721,#53722,#53723,#53724,#53725,
#53726,#53727,#53728,#53729,#53730,#53731),.UNSPECIFIED.,.F.,.F.,(4,3,3,
3,3,3,3,4),(-54.3584128775674,-53.7066411718011,-52.7120737426936,-51.7175063135862,
-50.7229388844788,-49.7283714553713,-48.7338040262639,-48.0752275703878),
 .UNSPECIFIED.);
#934=B_SPLINE_CURVE_WITH_KNOTS('',3,(#53732,#53733,#53734,#53735,#53736,
#53737,#53738,#53739,#53740,#53741,#53742,#53743,#53744,#53745,#53746,#53747,
#53748,#53749,#53750,#53751,#53752,#53753),.UNSPECIFIED.,.F.,.F.,(4,3,3,
3,3,3,3,4),(45.0986906589432,45.7787956689619,46.7739868791568,47.7691780893516,
48.7643692995464,49.7595605097412,50.7547517199361,51.3818759661228),
 .UNSPECIFIED.);
#935=B_SPLINE_CURVE_WITH_KNOTS('',3,(#53758,#53759,#53760,#53761,#53762,
#53763,#53764,#53765,#53766,#53767,#53768,#53769,#53770,#53771,#53772,#53773,
#53774,#53775,#53776,#53777,#53778,#53779),.UNSPECIFIED.,.F.,.F.,(4,3,3,
3,3,3,3,4),(-60.641598184747,-59.6740457464456,-58.6794783173382,-57.6849108882308,
-56.6903434591233,-55.6957760300159,-54.7012086009085,-54.3584128775674),
 .UNSPECIFIED.);
#936=B_SPLINE_CURVE_WITH_KNOTS('',3,(#53780,#53781,#53782,#53783,#53784,
#53785,#53786,#53787,#53788,#53789,#53790,#53791,#53792,#53793,#53794,#53795,
#53796,#53797,#53798,#53799,#53800,#53801),.UNSPECIFIED.,.F.,.F.,(4,3,3,
3,3,3,3,4),(51.3818759661228,51.7499429301309,52.7451341403257,53.7403253505205,
54.7355165607154,55.7307077709102,56.725898981105,57.6650612733024),
 .UNSPECIFIED.);
#937=B_SPLINE_CURVE_WITH_KNOTS('',3,(#53806,#53807,#53808,#53809,#53810,
#53811,#53812,#53813,#53814,#53815,#53816,#53817,#53818,#53819,#53820,#53821,
#53822,#53823,#53824,#53825,#53826,#53827,#53828,#53829,#53830),
 .UNSPECIFIED.,.F.,.F.,(4,3,3,3,3,3,3,3,4),(-66.9247834919265,-66.6360177501976,
-65.6414503210902,-64.6468828919827,-63.6523154628753,-62.6577480337679,
-61.6631806046605,-60.668613175553,-60.641598184747),.UNSPECIFIED.);
#938=B_SPLINE_CURVE_WITH_KNOTS('',3,(#53831,#53832,#53833,#53834,#53835,
#53836,#53837,#53838,#53839,#53840,#53841,#53842,#53843,#53844,#53845,#53846,
#53847,#53848,#53849,#53850,#53851,#53852,#53853,#53854,#53855),
 .UNSPECIFIED.,.F.,.F.,(4,3,3,3,3,3,3,3,4),(57.6650612733024,57.7210901912998,
58.7162814014946,59.7114726116895,60.7066638218843,61.7018550320791,62.697046242274,
63.6922374524688,63.9482465804819),.UNSPECIFIED.);
#939=B_SPLINE_CURVE_WITH_KNOTS('',3,(#53860,#53861,#53862,#53863,#53864,
#53865,#53866,#53867,#53868,#53869,#53870,#53871,#53872,#53873,#53874,#53875,
#53876,#53877,#53878,#53879,#53880,#53881),.UNSPECIFIED.,.F.,.F.,(4,3,3,
3,3,3,3,4),(-73.2079687991061,-72.6034223248422,-71.6088548957347,-70.6142874666273,
-69.6197200375199,-68.6251526084124,-67.630585179305,-66.9247834919265),
 .UNSPECIFIED.);
#940=B_SPLINE_CURVE_WITH_KNOTS('',3,(#53882,#53883,#53884,#53885,#53886,
#53887,#53888,#53889,#53890,#53891,#53892,#53893,#53894,#53895,#53896,#53897,
#53898,#53899,#53900,#53901,#53902,#53903),.UNSPECIFIED.,.F.,.F.,(4,3,3,
3,3,3,3,4),(63.9482465804819,64.6874286626636,65.6826198728584,66.6778110830533,
67.6730022932481,68.6681935034429,69.6633847136378,70.2314318876615),
 .UNSPECIFIED.);
#941=B_SPLINE_CURVE_WITH_KNOTS('',3,(#53908,#53909,#53910,#53911,#53912,
#53913,#53914,#53915,#53916,#53917,#53918,#53919,#53920,#53921,#53922,#53923,
#53924,#53925,#53926,#53927,#53928,#53929),.UNSPECIFIED.,.F.,.F.,(4,3,3,
3,3,3,3,4),(-79.4911541062857,-78.5708268994867,-77.5762594703793,-76.5816920412719,
-75.5871246121644,-74.592557183057,-73.5979897539496,-73.2079687991061),
 .UNSPECIFIED.);
#942=B_SPLINE_CURVE_WITH_KNOTS('',3,(#53930,#53931,#53932,#53933,#53934,
#53935,#53936,#53937,#53938,#53939,#53940,#53941,#53942,#53943,#53944,#53945,
#53946,#53947,#53948,#53949,#53950,#53951),.UNSPECIFIED.,.F.,.F.,(4,3,3,
3,3,3,3,4),(70.2314318876615,70.6585759238326,71.6537671340274,72.6489583442222,
73.644149554417,74.6393407646119,75.6345319748067,76.5146171948411),
 .UNSPECIFIED.);
#943=B_SPLINE_CURVE_WITH_KNOTS('',3,(#53956,#53957,#53958,#53959,#53960,
#53961,#53962,#53963,#53964,#53965,#53966,#53967,#53968,#53969,#53970,#53971,
#53972,#53973,#53974,#53975,#53976,#53977,#53978,#53979,#53980),
 .UNSPECIFIED.,.F.,.F.,(4,3,3,3,3,3,3,3,4),(-85.7743394134653,-85.5327989032387,
-84.5382314741313,-83.5436640450238,-82.5490966159164,-81.554529186809,
-80.5599617577016,-79.5653943285942,-79.4911541062857),.UNSPECIFIED.);
#944=B_SPLINE_CURVE_WITH_KNOTS('',3,(#53981,#53982,#53983,#53984,#53985,
#53986,#53987,#53988,#53989,#53990,#53991,#53992,#53993,#53994,#53995,#53996,
#53997,#53998,#53999,#54000,#54001,#54002,#54003,#54004,#54005),
 .UNSPECIFIED.,.F.,.F.,(4,3,3,3,3,3,3,3,4),(76.5146171948411,76.6297231850015,
77.6249143951963,78.6201056053912,79.615296815586,80.6104880257808,81.6056792359756,
82.6008704461705,82.7978025020207),.UNSPECIFIED.);
#945=B_SPLINE_CURVE_WITH_KNOTS('',3,(#54010,#54011,#54012,#54013,#54014,
#54015,#54016,#54017,#54018,#54019,#54020,#54021,#54022,#54023,#54024,#54025,
#54026,#54027,#54028,#54029,#54030,#54031),.UNSPECIFIED.,.F.,.F.,(4,3,3,
3,3,3,3,4),(-92.0575247206449,-91.5002034778833,-90.5056360487758,-89.5110686196684,
-88.516501190561,-87.5219337614536,-86.5273663323461,-85.7743394134653),
 .UNSPECIFIED.);
#946=B_SPLINE_CURVE_WITH_KNOTS('',3,(#54032,#54033,#54034,#54035,#54036,
#54037,#54038,#54039,#54040,#54041,#54042,#54043,#54044,#54045,#54046,#54047,
#54048,#54049,#54050,#54051,#54052,#54053),.UNSPECIFIED.,.F.,.F.,(4,3,3,
3,3,3,3,4),(82.7978025020207,83.5960616563653,84.5912528665601,85.5864440767549,
86.5816352869498,87.5768264971446,88.5720177073394,89.0809878092003),
 .UNSPECIFIED.);
#947=B_SPLINE_CURVE_WITH_KNOTS('',3,(#54058,#54059,#54060,#54061,#54062,
#54063,#54064,#54065,#54066,#54067,#54068,#54069,#54070,#54071,#54072,#54073,
#54074,#54075,#54076,#54077,#54078,#54079),.UNSPECIFIED.,.F.,.F.,(4,3,3,
3,3,3,3,4),(-98.3407100278245,-97.4676080525278,-96.4730406234204,-95.478473194313,
-94.4839057652055,-93.4893383360981,-92.4947709069907,-92.0575247206449),
 .UNSPECIFIED.);
#948=B_SPLINE_CURVE_WITH_KNOTS('',3,(#54080,#54081,#54082,#54083,#54084,
#54085,#54086,#54087,#54088,#54089,#54090,#54091,#54092,#54093,#54094,#54095,
#54096,#54097,#54098,#54099,#54100,#54101),.UNSPECIFIED.,.F.,.F.,(4,3,3,
3,3,3,3,4),(89.0809878092003,89.5672089175342,90.5624001277291,91.5575913379239,
92.5527825481187,93.5479737583135,94.5431649685084,95.3641731163799),
 .UNSPECIFIED.);
#949=B_SPLINE_CURVE_WITH_KNOTS('',3,(#54106,#54107,#54108,#54109,#54110,
#54111,#54112,#54113,#54114,#54115,#54116,#54117,#54118,#54119,#54120,#54121,
#54122,#54123,#54124,#54125,#54126,#54127,#54128,#54129,#54130),
 .UNSPECIFIED.,.F.,.F.,(4,3,3,3,3,3,3,3,4),(-104.623895335004,-104.42958005628,
-103.435012627172,-102.440445198065,-101.445877768958,-100.45131033985,
-99.4567429107427,-98.4621754816353,-98.3407100278245),.UNSPECIFIED.);
#950=B_SPLINE_CURVE_WITH_KNOTS('',3,(#54131,#54132,#54133,#54134,#54135,
#54136,#54137,#54138,#54139,#54140,#54141,#54142,#54143,#54144,#54145,#54146,
#54147,#54148,#54149,#54150,#54151,#54152,#54153,#54154,#54155),
 .UNSPECIFIED.,.F.,.F.,(4,3,3,3,3,3,3,3,4),(95.3641731163799,95.5383561787032,
96.533547388898,97.5287385990929,98.5239298092877,99.5191210194825,100.514312229677,
101.509503439872,101.64735842356),.UNSPECIFIED.);
#951=B_SPLINE_CURVE_WITH_KNOTS('',3,(#54160,#54161,#54162,#54163,#54164,
#54165,#54166,#54167,#54168,#54169,#54170,#54171,#54172,#54173,#54174,#54175,
#54176,#54177,#54178,#54179,#54180,#54181),.UNSPECIFIED.,.F.,.F.,(4,3,3,
3,3,3,3,4),(-110.907080642184,-110.396984630924,-109.402417201817,-108.40784977271,
-107.413282343602,-106.418714914495,-105.424147485387,-104.623895335004),
 .UNSPECIFIED.);
#952=B_SPLINE_CURVE_WITH_KNOTS('',3,(#54182,#54183,#54184,#54185,#54186,
#54187,#54188,#54189,#54190,#54191,#54192,#54193,#54194,#54195,#54196,#54197,
#54198,#54199,#54200,#54201,#54202,#54203),.UNSPECIFIED.,.F.,.F.,(4,3,3,
3,3,3,3,4),(101.64735842356,102.504694650067,103.499885860262,104.495077070457,
105.490268280651,106.485459490846,107.480650701041,107.930543730739),
 .UNSPECIFIED.);
#953=B_SPLINE_CURVE_WITH_KNOTS('',3,(#54208,#54209,#54210,#54211,#54212,
#54213,#54214,#54215,#54216,#54217,#54218,#54219,#54220,#54221,#54222,#54223,
#54224,#54225,#54226,#54227,#54228,#54229),.UNSPECIFIED.,.F.,.F.,(4,3,3,
3,3,3,3,4),(-117.190265949363,-116.364389205569,-115.369821776462,-114.375254347354,
-113.380686918247,-112.386119489139,-111.391552060032,-110.907080642184),
 .UNSPECIFIED.);
#954=B_SPLINE_CURVE_WITH_KNOTS('',3,(#54230,#54231,#54232,#54233,#54234,
#54235,#54236,#54237,#54238,#54239,#54240,#54241,#54242,#54243,#54244,#54245,
#54246,#54247,#54248,#54249,#54250,#54251),.UNSPECIFIED.,.F.,.F.,(4,3,3,
3,3,3,3,4),(107.930543730739,108.475841911236,109.471033121431,110.466224331626,
111.46141554182,112.456606752015,113.45179796221,114.213729037919),
 .UNSPECIFIED.);
#955=B_SPLINE_CURVE_WITH_KNOTS('',3,(#54257,#54258,#54259,#54260,#54261,
#54262,#54263,#54264,#54265,#54266,#54267),.UNSPECIFIED.,.F.,.F.,(4,1,1,
1,1,1,1,1,4),(128.805298797182,128.973989482495,129.968556911602,130.963124340709,
131.957691769817,132.952259198924,133.946826628032,134.444110342585,134.941394057139),
 .UNSPECIFIED.);
#956=B_SPLINE_CURVE_WITH_KNOTS('',3,(#54270,#54271,#54272,#54273,#54274,
#54275,#54276,#54277,#54278),.UNSPECIFIED.,.F.,.F.,(4,1,1,1,1,1,4),(128.805298797182,
129.721712095852,130.716903306047,131.712094516241,132.707285726436,133.204881331534,
133.702476936631),.UNSPECIFIED.);
#957=B_SPLINE_CURVE_WITH_KNOTS('',3,(#54283,#54284,#54285,#54286,#54287,
#54288,#54289,#54290,#54291,#54292),.UNSPECIFIED.,.F.,.F.,(4,1,1,1,1,1,
1,4),(122.522113490002,123.00658490785,124.001152336957,124.995719766065,
125.990287195172,126.98485462428,127.979422053387,128.805298797182),
 .UNSPECIFIED.);
#958=B_SPLINE_CURVE_WITH_KNOTS('',3,(#54293,#54294,#54295,#54296,#54297,
#54298,#54299,#54300,#54301,#54302,#54303),.UNSPECIFIED.,.F.,.F.,(4,1,1,
1,1,1,1,1,4),(122.522113490002,122.755373624488,123.750564834683,124.745756044878,
125.740947255072,126.736138465267,127.731329675462,128.726520885657,128.805298797182),
 .UNSPECIFIED.);
#959=B_SPLINE_CURVE_WITH_KNOTS('',3,(#54308,#54309,#54310,#54311,#54312,
#54313,#54314,#54315,#54316,#54317),.UNSPECIFIED.,.F.,.F.,(4,1,1,1,1,1,
1,4),(116.238928182822,117.039180333205,118.033747762313,119.02831519142,
120.022882620528,121.017450049635,122.012017478743,122.522113490002),
 .UNSPECIFIED.);
#960=B_SPLINE_CURVE_WITH_KNOTS('',3,(#54318,#54319,#54320,#54321,#54322,
#54323,#54324,#54325,#54326,#54327),.UNSPECIFIED.,.F.,.F.,(4,1,1,1,1,1,
1,4),(116.238928182822,116.784226363319,117.779417573514,118.774608783709,
119.769799993904,120.764991204098,121.760182414293,122.522113490002),
 .UNSPECIFIED.);
#961=B_SPLINE_CURVE_WITH_KNOTS('',3,(#54332,#54333,#54334,#54335,#54336,
#54337,#54338,#54339,#54340,#54341,#54342),.UNSPECIFIED.,.F.,.F.,(4,1,1,
1,1,1,1,1,4),(109.955742875643,110.077208329453,111.071775758561,112.066343187668,
113.060910616776,114.055478045883,115.050045474991,116.044612904098,116.238928182822),
 .UNSPECIFIED.);
#962=B_SPLINE_CURVE_WITH_KNOTS('',3,(#54343,#54344,#54345,#54346,#54347,
#54348,#54349,#54350,#54351,#54352),.UNSPECIFIED.,.F.,.F.,(4,1,1,1,1,1,
1,4),(109.955742875643,110.81307910215,111.808270312345,112.80346152254,
113.798652732735,114.793843942929,115.789035153124,116.238928182822),
 .UNSPECIFIED.);
#963=B_SPLINE_CURVE_WITH_KNOTS('',3,(#54357,#54358,#54359,#54360,#54361,
#54362,#54363,#54364,#54365,#54366),.UNSPECIFIED.,.F.,.F.,(4,1,1,1,1,1,
1,4),(103.672557568463,104.109803754809,105.104371183916,106.098938613024,
107.093506042131,108.088073471239,109.082640900346,109.955742875643),
 .UNSPECIFIED.);
#964=B_SPLINE_CURVE_WITH_KNOTS('',3,(#54367,#54368,#54369,#54370,#54371,
#54372,#54373,#54374,#54375,#54376,#54377),.UNSPECIFIED.,.F.,.F.,(4,1,1,
1,1,1,1,1,4),(103.672557568463,103.846740630786,104.841931840981,105.837123051176,
106.832314261371,107.827505471566,108.82269668176,109.817887891955,109.955742875643),
 .UNSPECIFIED.);
#965=B_SPLINE_CURVE_WITH_KNOTS('',3,(#54382,#54383,#54384,#54385,#54386,
#54387,#54388,#54389,#54390,#54391),.UNSPECIFIED.,.F.,.F.,(4,1,1,1,1,1,
1,4),(97.3893722612836,98.1423991801644,99.1369666092718,100.131534038379,
101.126101467487,102.120668896594,103.115236325701,103.672557568463),
 .UNSPECIFIED.);
#966=B_SPLINE_CURVE_WITH_KNOTS('',3,(#54392,#54393,#54394,#54395,#54396,
#54397,#54398,#54399,#54400,#54401),.UNSPECIFIED.,.F.,.F.,(4,1,1,1,1,1,
1,4),(97.3893722612835,97.8755933696174,98.8707845798122,99.865975790007,
100.861167000202,101.856358210397,102.851549420591,103.672557568463),
 .UNSPECIFIED.);
#967=B_SPLINE_CURVE_WITH_KNOTS('',3,(#54406,#54407,#54408,#54409,#54410,
#54411,#54412,#54413,#54414,#54415,#54416),.UNSPECIFIED.,.F.,.F.,(4,1,1,
1,1,1,1,1,4),(91.106186954104,91.1804271764124,92.1749946055198,93.1695620346272,
94.1641294637347,95.1586968928421,96.1532643219495,97.1478317510569,97.3893722612836),
 .UNSPECIFIED.);
#968=B_SPLINE_CURVE_WITH_KNOTS('',3,(#54417,#54418,#54419,#54420,#54421,
#54422,#54423,#54424,#54425,#54426),.UNSPECIFIED.,.F.,.F.,(4,1,1,1,1,1,
1,4),(91.106186954104,91.9044461084484,92.8996373186432,93.8948285288381,
94.8900197390329,95.8852109492277,96.8804021594225,97.3893722612835),
 .UNSPECIFIED.);
#969=B_SPLINE_CURVE_WITH_KNOTS('',3,(#54431,#54432,#54433,#54434,#54435,
#54436,#54437,#54438,#54439,#54440),.UNSPECIFIED.,.F.,.F.,(4,1,1,1,1,1,
1,4),(84.8230016469244,85.2130226017678,86.2075900308752,87.2021574599827,
88.1967248890901,89.1912923181975,90.1858597473049,91.106186954104),
 .UNSPECIFIED.);
#970=B_SPLINE_CURVE_WITH_KNOTS('',3,(#54441,#54442,#54443,#54444,#54445,
#54446,#54447,#54448,#54449,#54450,#54451),.UNSPECIFIED.,.F.,.F.,(4,1,1,
1,1,1,1,1,4),(84.8230016469244,84.9381076370846,85.9332988472795,86.9284900574743,
87.9236812676691,88.9188724778639,89.9140636880588,90.9092548982536,91.106186954104),
 .UNSPECIFIED.);
#971=B_SPLINE_CURVE_WITH_KNOTS('',3,(#54456,#54457,#54458,#54459,#54460,
#54461,#54462,#54463,#54464,#54465),.UNSPECIFIED.,.F.,.F.,(4,1,1,1,1,1,
1,4),(78.5398163397448,79.2456180271232,80.2401854562307,81.2347528853381,
82.2293203144455,83.223887743553,84.2184551726604,84.8230016469244),
 .UNSPECIFIED.);
#972=B_SPLINE_CURVE_WITH_KNOTS('',3,(#54466,#54467,#54468,#54469,#54470,
#54471,#54472,#54473,#54474,#54475),.UNSPECIFIED.,.F.,.F.,(4,1,1,1,1,1,
1,4),(78.5398163397448,78.9669603759157,79.9621515861105,80.9573427963053,
81.9525340065002,82.947725216695,83.9429164268898,84.8230016469244),
 .UNSPECIFIED.);
#973=B_SPLINE_CURVE_WITH_KNOTS('',3,(#54480,#54481,#54482,#54483,#54484,
#54485,#54486,#54487,#54488,#54489,#54490),.UNSPECIFIED.,.F.,.F.,(4,1,1,
1,1,1,1,1,4),(72.2566310325652,72.2836460233713,73.2782134524787,74.2727808815861,
75.2673483106935,76.261915739801,77.2564831689084,78.2510505980158,78.5398163397448),
 .UNSPECIFIED.);
#974=B_SPLINE_CURVE_WITH_KNOTS('',3,(#54491,#54492,#54493,#54494,#54495,
#54496,#54497,#54498,#54499,#54500),.UNSPECIFIED.,.F.,.F.,(4,1,1,1,1,1,
1,4),(72.2566310325652,72.9958131147467,73.9910043249416,74.9861955351364,
75.9813867453312,76.976577955526,77.9717691657209,78.5398163397448),
 .UNSPECIFIED.);
#975=B_SPLINE_CURVE_WITH_KNOTS('',3,(#54505,#54506,#54507,#54508,#54509,
#54510,#54511,#54512,#54513,#54514),.UNSPECIFIED.,.F.,.F.,(4,1,1,1,1,1,
1,4),(65.9734457253856,66.3162414487267,67.3108088778341,68.3053763069416,
69.299943736049,70.2945111651564,71.2890785942638,72.2566310325652),
 .UNSPECIFIED.);
#976=B_SPLINE_CURVE_WITH_KNOTS('',3,(#54515,#54516,#54517,#54518,#54519,
#54520,#54521,#54522,#54523,#54524,#54525),.UNSPECIFIED.,.F.,.F.,(4,1,1,
1,1,1,1,1,4),(65.9734457253856,66.029474643383,67.0246658535778,68.0198570637726,
69.0150482739674,70.0102394841623,71.0054306943571,72.0006219045519,72.2566310325652),
 .UNSPECIFIED.);
#977=B_SPLINE_CURVE_WITH_KNOTS('',3,(#54530,#54531,#54532,#54533,#54534,
#54535,#54536,#54537,#54538,#54539),.UNSPECIFIED.,.F.,.F.,(4,1,1,1,1,1,
1,4),(59.690260418206,60.3488368740821,61.3434043031896,62.337971732297,
63.3325391614044,64.3271065905118,65.3216740196193,65.9734457253856),
 .UNSPECIFIED.);
#978=B_SPLINE_CURVE_WITH_KNOTS('',3,(#54540,#54541,#54542,#54543,#54544,
#54545,#54546,#54547,#54548,#54549),.UNSPECIFIED.,.F.,.F.,(4,1,1,1,1,1,
1,4),(59.690260418206,60.058327382214,61.0535185924088,62.0487098026037,
63.0439010127985,64.0390922229933,65.0342834331881,65.9734457253856),
 .UNSPECIFIED.);
#979=B_SPLINE_CURVE_WITH_KNOTS('',3,(#54554,#54555,#54556,#54557,#54558,
#54559,#54560,#54561,#54562,#54563),.UNSPECIFIED.,.F.,.F.,(4,1,1,1,1,1,
1,4),(53.4070751110264,54.3814322994376,55.375999728545,56.3705671576524,
57.3651345867599,58.3597020158673,59.3542694449747,59.690260418206),
 .UNSPECIFIED.);
#980=B_SPLINE_CURVE_WITH_KNOTS('',3,(#54564,#54565,#54566,#54567,#54568,
#54569,#54570,#54571,#54572,#54573),.UNSPECIFIED.,.F.,.F.,(4,1,1,1,1,1,
1,4),(53.4070751110264,54.0871801210451,55.0823713312399,56.0775625414347,
57.0727537516295,58.0679449618244,59.0631361720192,59.690260418206),
 .UNSPECIFIED.);
#981=B_SPLINE_CURVE_WITH_KNOTS('',3,(#54578,#54579,#54580,#54581,#54582,
#54583,#54584,#54585,#54586,#54587,#54588),.UNSPECIFIED.,.F.,.F.,(4,1,1,
1,1,1,1,1,4),(47.1238898038468,47.4194602956856,48.414027724793,49.4085951539004,
50.4031625830079,51.3977300121153,52.3922974412227,53.3868648703302,53.4070751110264),
 .UNSPECIFIED.);
#982=B_SPLINE_CURVE_WITH_KNOTS('',3,(#54589,#54590,#54591,#54592,#54593,
#54594,#54595,#54596,#54597,#54598),.UNSPECIFIED.,.F.,.F.,(4,1,1,1,1,1,
1,4),(47.1238898038468,48.1160328598761,49.1112240700709,50.1064152802658,
51.1016064904606,52.0967977006554,53.0919889108502,53.4070751110264),
 .UNSPECIFIED.);
#983=B_SPLINE_CURVE_WITH_KNOTS('',3,(#54603,#54604,#54605,#54606,#54607,
#54608,#54609,#54610,#54611,#54612),.UNSPECIFIED.,.F.,.F.,(4,1,1,1,1,1,
1,4),(40.8407044966672,41.452055721041,42.4466231501485,43.4411905792559,
44.4357580083633,45.4303254374707,46.4248928665782,47.1238898038468),
 .UNSPECIFIED.);
#984=B_SPLINE_CURVE_WITH_KNOTS('',3,(#54613,#54614,#54615,#54616,#54617,
#54618,#54619,#54620,#54621,#54622,#54623),.UNSPECIFIED.,.F.,.F.,(4,1,1,
1,1,1,1,1,4),(40.8407044966672,41.1496943885123,42.1448855987072,43.140076808902,
44.1352680190968,45.1304592292916,46.1256504394865,47.1208416496813,47.1238898038468),
 .UNSPECIFIED.);
#985=B_SPLINE_CURVE_WITH_KNOTS('',3,(#54628,#54629,#54630,#54631,#54632,
#54633,#54634,#54635,#54636,#54637),.UNSPECIFIED.,.F.,.F.,(4,1,1,1,1,1,
1,4),(34.5575191894876,35.4846511463965,36.4792185755039,37.4737860046113,
38.4683534337187,39.4629208628262,40.4574882919336,40.8407044966672),
 .UNSPECIFIED.);
#986=B_SPLINE_CURVE_WITH_KNOTS('',3,(#54638,#54639,#54640,#54641,#54642,
#54643,#54644,#54645,#54646,#54647),.UNSPECIFIED.,.F.,.F.,(4,1,1,1,1,1,
1,4),(34.5575191894876,35.1785471273434,36.1737383375382,37.168929547733,
38.1641207579279,39.1593119681227,40.1545031783175,40.8407044966672),
 .UNSPECIFIED.);
#987=B_SPLINE_CURVE_WITH_KNOTS('',3,(#54652,#54653,#54654,#54655,#54656,
#54657,#54658,#54659,#54660,#54661,#54662),.UNSPECIFIED.,.F.,.F.,(4,1,1,
1,1,1,1,1,4),(28.274333882308,28.5226791426445,29.5172465717519,30.5118140008593,
31.5063814299668,32.5009488590742,33.4955162881816,34.490083717289,34.5575191894876),
 .UNSPECIFIED.);
#988=B_SPLINE_CURVE_WITH_KNOTS('',3,(#54663,#54664,#54665,#54666,#54667,
#54668,#54669,#54670,#54671,#54672),.UNSPECIFIED.,.F.,.F.,(4,1,1,1,1,1,
1,4),(28.274333882308,29.2073998661744,30.2025910763693,31.1977822865641,
32.1929734967589,33.1881647069537,34.1833559171486,34.5575191894876),
 .UNSPECIFIED.);
#989=B_SPLINE_CURVE_WITH_KNOTS('',3,(#54677,#54678,#54679,#54680,#54681,
#54682,#54683,#54684,#54685,#54686),.UNSPECIFIED.,.F.,.F.,(4,1,1,1,1,1,
1,4),(21.9911485751285,22.5552745679999,23.5498419971074,24.5444094262148,
25.5389768553222,26.5335442844296,27.5281117135371,28.274333882308),
 .UNSPECIFIED.);
#990=B_SPLINE_CURVE_WITH_KNOTS('',3,(#54687,#54688,#54689,#54690,#54691,
#54692,#54693,#54694,#54695,#54696,#54697),.UNSPECIFIED.,.F.,.F.,(4,1,1,
1,1,1,1,1,4),(21.9911485751285,22.2410613948107,23.2362526050055,24.2314438152003,
25.2266350253952,26.22182623559,27.2170174457848,28.2122086559796,28.274333882308),
 .UNSPECIFIED.);
#991=B_SPLINE_CURVE_WITH_KNOTS('',3,(#54702,#54703,#54704,#54705,#54706,
#54707,#54708,#54709,#54710,#54711),.UNSPECIFIED.,.F.,.F.,(4,1,1,1,1,1,
1,4),(15.7079632679489,16.5878699933554,17.5824374224628,18.5770048515702,
19.5715722806776,20.5661397097851,21.5607071388925,21.9911485751285),
 .UNSPECIFIED.);
#992=B_SPLINE_CURVE_WITH_KNOTS('',3,(#54712,#54713,#54714,#54715,#54716,
#54717,#54718,#54719,#54720,#54721),.UNSPECIFIED.,.F.,.F.,(4,1,1,1,1,1,
1,4),(15.7079632679489,16.2699141336417,17.2651053438366,18.2602965540314,
19.2554877642262,20.250678974421,21.2458701846159,21.9911485751285),
 .UNSPECIFIED.);
#993=B_SPLINE_CURVE_WITH_KNOTS('',3,(#54724,#54725,#54726,#54727,#54728,
#54729,#54730,#54731,#54732,#54733,#54734,#54735,#54736,#54737,#54738,#54739,
#54740,#54741,#54742,#54743,#54744,#54745,#54746,#54747,#54748,#54749,#54750,
#54751,#54752,#54753,#54754,#54755,#54756,#54757,#54758,#54759,#54760,#54761,
#54762,#54763,#54764,#54765,#54766,#54767,#54768,#54769,#54770,#54771,#54772,
#54773,#54774,#54775,#54776,#54777,#54778,#54779,#54780,#54781,#54782,#54783,
#54784,#54785,#54786,#54787,#54788,#54789,#54790,#54791,#54792,#54793,#54794,
#54795,#54796,#54797,#54798,#54799,#54800,#54801,#54802,#54803,#54804,#54805,
#54806,#54807,#54808,#54809,#54810,#54811,#54812,#54813,#54814,#54815,#54816,
#54817,#54818,#54819,#54820,#54821,#54822,#54823,#54824,#54825,#54826,#54827,
#54828,#54829,#54830,#54831,#54832,#54833,#54834,#54835,#54836,#54837,#54838,
#54839,#54840,#54841,#54842,#54843,#54844,#54845,#54846,#54847,#54848,#54849,
#54850,#54851,#54852,#54853,#54854,#54855,#54856,#54857,#54858,#54859,#54860,
#54861,#54862,#54863,#54864,#54865,#54866,#54867,#54868,#54869,#54870,#54871,
#54872,#54873,#54874,#54875,#54876,#54877,#54878,#54879,#54880,#54881,#54882,
#54883,#54884,#54885,#54886,#54887,#54888,#54889,#54890,#54891,#54892,#54893,
#54894,#54895,#54896,#54897,#54898,#54899,#54900,#54901,#54902,#54903,#54904,
#54905,#54906,#54907,#54908,#54909,#54910,#54911,#54912,#54913,#54914,#54915,
#54916,#54917,#54918,#54919,#54920,#54921,#54922,#54923,#54924,#54925,#54926,
#54927,#54928,#54929,#54930,#54931,#54932,#54933,#54934,#54935,#54936,#54937,
#54938,#54939,#54940,#54941,#54942,#54943,#54944,#54945,#54946,#54947,#54948,
#54949,#54950,#54951,#54952,#54953,#54954,#54955,#54956,#54957,#54958,#54959,
#54960,#54961,#54962,#54963,#54964,#54965,#54966,#54967),.UNSPECIFIED.,
 .F.,.F.,(4,3,3,3,3,3,3,3,3,3,3,3,3,3,3,3,3,3,3,3,3,3,3,3,3,3,3,3,3,3,3,
3,3,3,3,3,3,3,3,3,3,3,3,3,3,3,3,3,3,3,3,3,3,3,3,3,3,3,3,3,3,3,3,3,3,3,3,
3,3,3,3,3,3,3,3,3,3,3,3,3,3,4),(-2.64334436896556,-2.60354403016607,-2.56319357704322,
-2.52826625024512,-2.51459318907079,-2.50781535649548,-2.46564981317316,
-2.42348426985084,-2.39566963603287,-2.38341570939638,-2.37761610684016,
-2.336849738158,-2.29583153162079,-2.25519438983726,-2.22808079457215,-2.2136427889914,
-2.20824896814423,-2.20096719930704,-2.16123852890373,-2.12054358173304,
-2.07915011465577,-2.03779648847865,-2.03243166702702,-1.99089005776529,
-1.94895701700167,-1.90713874879756,-1.86743433790788,-1.85926764668736,
-1.85203534200324,-1.80992713326301,-1.76842432689819,-1.74832110523882,
-1.70676763322338,-1.68046855645703,-1.67322668686903,-1.63229330306282,
-1.58900444080018,-1.54654889761395,-1.51397808603242,-1.5045713939363,
-1.49689579776549,-1.49148547399684,-1.44889513044297,-1.40637477884859,
-1.36441427917375,-1.32519834206773,-1.31745702219618,-1.31155026142285,
-1.28598240496172,-1.24479777214057,-1.20266268120784,-1.15989915790716,
-1.13825803467134,-1.13225377395059,-1.12622665290763,-1.08347961800304,
-1.04027268262164,-0.997123369249094,-0.954546729607404,-0.947141190072399,
-0.941377976925763,-0.897944447185484,-0.855190214624572,-0.813641186133967,
-0.785925562678236,-0.769826109785476,-0.761910560472749,-0.75632393840638,
-0.714342458530382,-0.67097419230323,-0.627232222714931,-0.595102096230848,
-0.581045165894062,-0.572765453161588,-0.566918945151293,-0.523130330920948,
-0.47917700856887,-0.435659870904986,-0.402925540873628,-0.383690774196495,
-0.377633521738216,-0.37019121084227),.UNSPECIFIED.);
#994=B_SPLINE_CURVE_WITH_KNOTS('',3,(#54969,#54970,#54971,#54972,#54973,
#54974,#54975,#54976,#54977,#54978,#54979,#54980,#54981,#54982,#54983,#54984,
#54985,#54986,#54987,#54988,#54989,#54990,#54991,#54992,#54993,#54994,#54995,
#54996,#54997,#54998,#54999,#55000,#55001,#55002,#55003,#55004,#55005,#55006,
#55007,#55008,#55009,#55010,#55011,#55012,#55013,#55014,#55015,#55016,#55017,
#55018,#55019,#55020,#55021,#55022,#55023,#55024,#55025,#55026,#55027,#55028,
#55029,#55030,#55031,#55032,#55033,#55034,#55035,#55036,#55037,#55038,#55039,
#55040,#55041),.UNSPECIFIED.,.F.,.F.,(4,3,3,3,3,3,3,3,3,3,3,3,3,3,3,3,3,
3,3,3,3,3,3,3,4),(-0.710745924398683,-0.666804013499017,-0.623090002091155,
-0.580490043399667,-0.549769720878275,-0.540030794848239,-0.533787755766615,
-0.491609440904295,-0.4576087533141,-0.414988201685294,-0.372400295436586,
-0.356121723662545,-0.350309819512417,-0.308708315030754,-0.266458526938774,
-0.224208738846794,-0.196182646490945,-0.183254318429312,-0.17525918271343,
-0.169900496948286,-0.127425372711214,-0.0868708094010787,-0.0467252344004481,
-0.00739903503843566,0.),.UNSPECIFIED.);
#995=B_SPLINE_CURVE_WITH_KNOTS('',3,(#55044,#55045,#55046,#55047,#55048,
#55049,#55050,#55051,#55052,#55053,#55054,#55055,#55056,#55057,#55058,#55059,
#55060,#55061,#55062,#55063,#55064,#55065,#55066,#55067,#55068,#55069,#55070,
#55071,#55072,#55073,#55074,#55075,#55076,#55077,#55078,#55079,#55080),
 .UNSPECIFIED.,.F.,.F.,(4,3,3,3,3,3,3,3,3,3,3,3,4),(-0.37019121084227,-0.331697325929431,
-0.288622232780515,-0.244797719637212,-0.21419800468256,-0.2008106293899,
-0.194172952745162,-0.188472403894731,-0.144967619206762,-0.100508059630889,
-0.0559598465844598,-0.0119678329618413,0.),.UNSPECIFIED.);
#996=B_SPLINE_CURVE_WITH_KNOTS('',3,(#55601,#55602,#55603,#55604,#55605,
#55606,#55607,#55608,#55609),.UNSPECIFIED.,.F.,.F.,(4,1,1,1,1,1,4),(11.6150328478182,
12.1123165623719,12.6096002769257,13.6041677060331,14.5987351351405,15.5933025642479,
15.7079632679489),.UNSPECIFIED.);
#997=B_SPLINE_CURVE_WITH_KNOTS('',3,(#55610,#55611,#55612,#55613,#55614,
#55615,#55616,#55617,#55618,#55619,#55620,#55621,#55622,#55623,#55624,#55625,
#55626,#55627,#55628,#55629,#55630,#55631,#55632,#55633,#55634,#55635,#55636,
#55637,#55638,#55639,#55640,#55641,#55642,#55643,#55644,#55645,#55646,#55647,
#55648,#55649,#55650,#55651,#55652,#55653,#55654,#55655,#55656,#55657,#55658,
#55659,#55660,#55661,#55662,#55663,#55664,#55665,#55666,#55667,#55668,#55669,
#55670,#55671,#55672,#55673,#55674,#55675,#55676,#55677,#55678,#55679,#55680,
#55681,#55682,#55683,#55684,#55685,#55686,#55687,#55688,#55689,#55690,#55691,
#55692,#55693,#55694,#55695,#55696,#55697,#55698,#55699,#55700,#55701,#55702,
#55703,#55704,#55705,#55706,#55707,#55708,#55709,#55710,#55711,#55712),
 .UNSPECIFIED.,.F.,.F.,(4,3,3,3,3,3,3,3,3,3,3,3,3,3,3,3,3,3,3,3,3,3,3,3,
3,3,3,3,3,3,3,3,3,3,4),(-0.965990216419481,-0.9272199902169,-0.883653696268922,
-0.856578499606751,-0.840281614965736,-0.83272424860471,-0.78942649842623,
-0.747054504832225,-0.728516757634848,-0.714850133126621,-0.708733859333935,
-0.665685633827477,-0.622719517527392,-0.579652275564091,-0.547351844091615,
-0.533932274491217,-0.525881927440116,-0.484249432147785,-0.450450549674188,
-0.408562082241703,-0.366597621077022,-0.351118396676314,-0.345479700399037,
-0.304353213451827,-0.263090931261655,-0.221828649071483,-0.194100067937547,
-0.181335497105944,-0.172973757166477,-0.167228677968348,-0.125421508476261,
-0.0849791978641806,-0.0449278087924871,-0.005690172937603,0.),
 .UNSPECIFIED.);
#998=B_SPLINE_CURVE_WITH_KNOTS('',3,(#55713,#55714,#55715,#55716,#55717,
#55718,#55719,#55720,#55721,#55722,#55723,#55724,#55725,#55726,#55727,#55728,
#55729,#55730,#55731),.UNSPECIFIED.,.F.,.F.,(4,3,3,3,3,3,4),(-121.812676859456,
-121.337226351106,-120.342658921999,-119.348091492891,-118.353524063784,
-117.358956634676,-117.190265949363),.UNSPECIFIED.);
#999=B_SPLINE_CURVE_WITH_KNOTS('',3,(#55734,#55735,#55736,#55737,#55738,
#55739,#55740,#55741,#55742),.UNSPECIFIED.,.F.,.F.,(4,1,1,1,1,1,4),(10.3761157273101,
11.2939580826676,12.2891492928624,13.2843405030573,14.2795317132521,15.2747229234469,
15.7079632679489),.UNSPECIFIED.);
#1000=B_SPLINE_CURVE_WITH_KNOTS('',3,(#56268,#56269,#56270,#56271,#56272,
#56273,#56274,#56275,#56276,#56277,#56278,#56279,#56280,#56281,#56282,#56283,
#56284,#56285,#56286,#56287,#56288,#56289),.UNSPECIFIED.,.F.,.F.,(4,3,3,
3,3,3,3,4),(114.213729037919,114.446989172405,115.4421803826,116.437371592795,
117.432562802989,118.427754013184,119.422945223379,119.744945584229),
 .UNSPECIFIED.);
#1001=B_SPLINE_CURVE_WITH_KNOTS('',3,(#56290,#56291,#56292,#56293,#56294,
#56295,#56296,#56297,#56298,#56299,#56300,#56301,#56302,#56303,#56304,#56305,
#56306,#56307,#56308,#56309,#56310,#56311,#56312,#56313,#56314,#56315,#56316,
#56317,#56318,#56319,#56320,#56321,#56322,#56323,#56324,#56325,#56326,#56327,
#56328,#56329,#56330,#56331,#56332,#56333,#56334,#56335,#56336,#56337,#56338,
#56339,#56340,#56341,#56342,#56343,#56344,#56345,#56346,#56347,#56348,#56349,
#56350,#56351,#56352,#56353,#56354,#56355,#56356,#56357,#56358,#56359,#56360,
#56361,#56362,#56363,#56364,#56365,#56366,#56367,#56368,#56369,#56370,#56371,
#56372,#56373,#56374,#56375,#56376,#56377,#56378,#56379,#56380,#56381,#56382,
#56383,#56384,#56385,#56386,#56387,#56388,#56389,#56390,#56391,#56392,#56393,
#56394,#56395),.UNSPECIFIED.,.F.,.F.,(4,3,3,3,3,3,3,3,3,3,3,3,3,3,3,3,3,
3,3,3,3,3,3,3,3,3,3,3,3,3,3,3,3,3,3,4),(-0.968477696161952,-0.934401878411372,
-0.894940908856935,-0.869057110968003,-0.857761995024893,-0.84957581141373,
-0.809420536841839,-0.768342987565862,-0.750371559757621,-0.741288256886726,
-0.734041921366352,-0.692568544969978,-0.650621991967233,-0.60816652963393,
-0.576324932883953,-0.562465720811907,-0.556565387998925,-0.513962262185476,
-0.480800142634022,-0.43927778705218,-0.397173024145668,-0.382659788254531,
-0.376822993230344,-0.334735665268914,-0.292008067784669,-0.248907378913767,
-0.243684959408641,-0.213224339482561,-0.199897818264901,-0.191569349313896,
-0.186008989480452,-0.142614739306227,-0.0987671132040068,-0.0550446346348842,
-0.0119839009752852,0.),.UNSPECIFIED.);
#1002=B_SPLINE_CURVE_WITH_KNOTS('',3,(#56458,#56459,#56460,#56461),
 .UNSPECIFIED.,.F.,.F.,(4,4),(51.5750455984138,52.2824273504651),
 .UNSPECIFIED.);
#1003=B_SPLINE_CURVE_WITH_KNOTS('',3,(#56469,#56470,#56471,#56472,#56473,
#56474,#56475,#56476,#56477,#56478),.UNSPECIFIED.,.F.,.F.,(4,3,3,4),(-50.2654824574367,
-49.3230446702501,-48.3365837768451,-47.8312715558982),.UNSPECIFIED.);
#1004=B_SPLINE_CURVE_WITH_KNOTS('',3,(#56483,#56484,#56485,#56486,#56487,
#56488,#56489,#56490,#56491,#56492,#56493,#56494,#56495,#56496,#56497,#56498,
#56499,#56500,#56501,#56502,#56503,#56504,#56505,#56506,#56507),
 .UNSPECIFIED.,.F.,.F.,(4,3,3,3,3,3,3,3,4),(45.2918602912342,45.3772010966301,
46.3636619900351,47.3501228834401,48.3365837768451,49.3230446702501,50.3095055636551,
51.2959664570601,51.5750455984138),.UNSPECIFIED.);
#1005=B_SPLINE_CURVE_WITH_KNOTS('',3,(#56508,#56509,#56510,#56511,#56512,
#56513,#56514,#56515,#56516,#56517,#56518,#56519,#56520,#56521,#56522,#56523,
#56524,#56525,#56526,#56527,#56528,#56529),.UNSPECIFIED.,.F.,.F.,(4,3,3,
3,3,3,3,4),(-47.8312715558982,-47.3501228834401,-46.3636619900351,-45.3772010966301,
-44.3907402032251,-43.4042793098201,-42.4178184164151,-41.5480862487186),
 .UNSPECIFIED.);
#1006=B_SPLINE_CURVE_WITH_KNOTS('',3,(#56534,#56535,#56536,#56537,#56538,
#56539,#56540,#56541,#56542,#56543,#56544,#56545,#56546,#56547,#56548,#56549,
#56550,#56551,#56552,#56553,#56554,#56555),.UNSPECIFIED.,.F.,.F.,(4,3,3,
3,3,3,3,4),(39.0086749840546,39.4584357362001,40.4448966296051,41.4313575230101,
42.4178184164151,43.4042793098201,44.3907402032251,45.2918602912342),
 .UNSPECIFIED.);
#1007=B_SPLINE_CURVE_WITH_KNOTS('',3,(#56556,#56557,#56558,#56559,#56560,
#56561,#56562,#56563,#56564,#56565,#56566,#56567,#56568,#56569,#56570,#56571,
#56572,#56573,#56574,#56575,#56576,#56577,#56578,#56579,#56580),
 .UNSPECIFIED.,.F.,.F.,(4,3,3,3,3,3,3,3,4),(-41.5480862487186,-41.4313575230101,
-40.4448966296051,-39.4584357362001,-38.4719748427951,-37.4855139493901,
-36.4990530559851,-35.5125921625801,-35.2649009415391),.UNSPECIFIED.);
#1008=B_SPLINE_CURVE_WITH_KNOTS('',3,(#56585,#56586,#56587,#56588,#56589,
#56590,#56591,#56592,#56593,#56594,#56595,#56596,#56597,#56598,#56599,#56600,
#56601,#56602,#56603,#56604,#56605,#56606),.UNSPECIFIED.,.F.,.F.,(4,3,3,
3,3,3,3,4),(32.725489676875,33.5396703757701,34.5261312691751,35.5125921625801,
36.4990530559851,37.4855139493901,38.4719748427951,39.0086749840546),
 .UNSPECIFIED.);
#1009=B_SPLINE_CURVE_WITH_KNOTS('',3,(#56607,#56608,#56609,#56610,#56611,
#56612,#56613,#56614,#56615,#56616,#56617,#56618,#56619,#56620,#56621,#56622,
#56623,#56624,#56625,#56626,#56627,#56628),.UNSPECIFIED.,.F.,.F.,(4,3,3,
3,3,3,3,4),(-35.2649009415391,-34.5261312691751,-33.5396703757701,-32.5532094823651,
-31.5667485889601,-30.5802876955551,-29.5938268021501,-28.9817156343595),
 .UNSPECIFIED.);
#1010=B_SPLINE_CURVE_WITH_KNOTS('',3,(#56633,#56634,#56635,#56636,#56637,
#56638,#56639,#56640,#56641,#56642,#56643,#56644,#56645,#56646,#56647,#56648,
#56649,#56650,#56651,#56652,#56653,#56654,#56655,#56656,#56657),
 .UNSPECIFIED.,.F.,.F.,(4,3,3,3,3,3,3,3,4),(26.4423043696954,26.6344441219351,
27.6209050153401,28.6073659087451,29.5938268021501,30.5802876955551,31.5667485889601,
32.5532094823651,32.725489676875),.UNSPECIFIED.);
#1011=B_SPLINE_CURVE_WITH_KNOTS('',3,(#56658,#56659,#56660,#56661,#56662,
#56663,#56664,#56665,#56666,#56667,#56668,#56669,#56670,#56671,#56672,#56673,
#56674,#56675,#56676,#56677,#56678,#56679),.UNSPECIFIED.,.F.,.F.,(4,3,3,
3,3,3,3,4),(-28.9817156343595,-28.6073659087451,-27.6209050153401,-26.6344441219351,
-25.6479832285301,-24.6615223351251,-23.6750614417201,-22.6985303271799),
 .UNSPECIFIED.);
#1012=B_SPLINE_CURVE_WITH_KNOTS('',3,(#56684,#56685,#56686,#56687,#56688,
#56689,#56690,#56691,#56692,#56693,#56694,#56695,#56696,#56697,#56698,#56699,
#56700,#56701,#56702,#56703,#56704,#56705),.UNSPECIFIED.,.F.,.F.,(4,3,3,
3,3,3,3,4),(20.1591190625158,20.7156787615051,21.7021396549101,22.6886005483151,
23.6750614417201,24.6615223351251,25.6479832285301,26.4423043696954),
 .UNSPECIFIED.);
#1013=B_SPLINE_CURVE_WITH_KNOTS('',3,(#56706,#56707,#56708,#56709,#56710,
#56711,#56712,#56713,#56714,#56715,#56716,#56717,#56718,#56719,#56720,#56721,
#56722,#56723,#56724,#56725,#56726,#56727,#56728,#56729,#56730),
 .UNSPECIFIED.,.F.,.F.,(4,3,3,3,3,3,3,3,4),(-22.6985303271799,-22.6886005483151,
-21.7021396549101,-20.7156787615051,-19.7292178681001,-18.742756974695,
-17.75629608129,-16.769835187885,-16.4153450200003),.UNSPECIFIED.);
#1014=B_SPLINE_CURVE_WITH_KNOTS('',3,(#56735,#56736,#56737,#56738,#56739,
#56740,#56741,#56742,#56743,#56744,#56745,#56746,#56747,#56748,#56749,#56750,
#56751,#56752,#56753,#56754,#56755,#56756),.UNSPECIFIED.,.F.,.F.,(4,3,3,
3,3,3,3,4),(13.8759337553362,14.796913401075,15.78337429448,16.769835187885,
17.75629608129,18.7427569746951,19.7292178681001,20.1591190625158),
 .UNSPECIFIED.);
#1015=B_SPLINE_CURVE_WITH_KNOTS('',3,(#56757,#56758,#56759,#56760,#56761,
#56762,#56763,#56764,#56765,#56766,#56767,#56768,#56769,#56770,#56771,#56772,
#56773,#56774,#56775,#56776,#56777,#56778),.UNSPECIFIED.,.F.,.F.,(4,3,3,
3,3,3,3,4),(-16.4153450200003,-15.78337429448,-14.796913401075,-13.81045250767,
-12.823991614265,-11.83753072086,-10.851069827455,-10.1321597128207),
 .UNSPECIFIED.);
#1016=B_SPLINE_CURVE_WITH_KNOTS('',3,(#56784,#56785,#56786,#56787,#56788,
#56789,#56790,#56791,#56792,#56793,#56794,#56795,#56796),.UNSPECIFIED.,
 .F.,.F.,(4,3,3,3,4),(-3.84897440564113,-2.95938268021501,-1.97292178681001,
-0.986460893405003,0.),.UNSPECIFIED.);
#1017=B_SPLINE_CURVE_WITH_KNOTS('',3,(#56799,#56800,#56801,#56802,#56803,
#56804,#56805,#56806,#56807,#56808,#56809,#56810,#56811,#56812,#56813,#56814,
#56815,#56816,#56817),.UNSPECIFIED.,.F.,.F.,(4,3,3,3,3,3,4),(2.01694489302845,
2.95938268021501,3.94584357362001,4.93230446702502,5.91876536043002,6.90522625383502,
7.59274844815666),.UNSPECIFIED.);
#1018=B_SPLINE_CURVE_WITH_KNOTS('',3,(#56823,#56824,#56825,#56826,#56827,
#56828,#56829,#56830),.UNSPECIFIED.,.F.,.F.,(4,1,1,1,1,4),(59.6902604182061,
60.1955726391529,61.1820335325579,62.1684944259629,63.154955319368,64.141416212773),
 .UNSPECIFIED.);
#1019=B_SPLINE_CURVE_WITH_KNOTS('',3,(#56833,#56834,#56835,#56836,#56837,
#56838,#56839,#56840,#56841),.UNSPECIFIED.,.F.,.F.,(4,1,1,1,1,1,4),(59.6902604182061,
59.775601223602,60.762062117007,61.748523010412,62.734983903817,63.721444797222,
64.6638825844085),.UNSPECIFIED.);
#1020=B_SPLINE_CURVE_WITH_KNOTS('',3,(#56846,#56847,#56848,#56849,#56850,
#56851,#56852,#56853,#56854,#56855),.UNSPECIFIED.,.F.,.F.,(4,1,1,1,1,1,
1,4),(53.4070751110265,54.2768072787229,55.2632681721279,56.2497290655329,
57.2361899589379,58.2226508523429,59.2091117457479,59.6902604182061),
 .UNSPECIFIED.);
#1021=B_SPLINE_CURVE_WITH_KNOTS('',3,(#56856,#56857,#56858,#56859,#56860,
#56861,#56862,#56863,#56864,#56865),.UNSPECIFIED.,.F.,.F.,(4,1,1,1,1,1,
1,4),(53.4070751110265,53.856835863172,54.843296756577,55.829757649982,
56.816218543387,57.802679436792,58.789140330197,59.6902604182061),
 .UNSPECIFIED.);
#1022=B_SPLINE_CURVE_WITH_KNOTS('',3,(#56870,#56871,#56872,#56873,#56874,
#56875,#56876,#56877,#56878,#56879,#56880),.UNSPECIFIED.,.F.,.F.,(4,1,1,
1,1,1,1,1,4),(47.1238898038469,47.3715810248879,48.3580419182929,49.3445028116979,
50.3309637051029,51.3174245985079,52.3038854919129,53.2903463853179,53.4070751110265),
 .UNSPECIFIED.);
#1023=B_SPLINE_CURVE_WITH_KNOTS('',3,(#56881,#56882,#56883,#56884,#56885,
#56886,#56887,#56888,#56889,#56890),.UNSPECIFIED.,.F.,.F.,(4,1,1,1,1,1,
1,4),(47.1238898038469,47.9380705027419,48.9245313961469,49.9109922895519,
50.897453182957,51.883914076362,52.870374969767,53.4070751110265),
 .UNSPECIFIED.);
#1024=B_SPLINE_CURVE_WITH_KNOTS('',3,(#56895,#56896,#56897,#56898,#56899,
#56900,#56901,#56902,#56903,#56904),.UNSPECIFIED.,.F.,.F.,(4,1,1,1,1,1,
1,4),(40.8407044966673,41.4528156644579,42.4392765578629,43.4257374512679,
44.4121983446729,45.3986592380779,46.3851201314829,47.1238898038469),
 .UNSPECIFIED.);
#1025=B_SPLINE_CURVE_WITH_KNOTS('',3,(#56905,#56906,#56907,#56908,#56909,
#56910,#56911,#56912,#56913,#56914,#56915),.UNSPECIFIED.,.F.,.F.,(4,1,1,
1,1,1,1,1,4),(40.8407044966673,41.0328442489069,42.0193051423119,43.0057660357169,
43.9922269291219,44.9786878225269,45.9651487159319,46.9516096093369,47.1238898038469),
 .UNSPECIFIED.);
#1026=B_SPLINE_CURVE_WITH_KNOTS('',3,(#56920,#56921,#56922,#56923,#56924,
#56925,#56926,#56927,#56928,#56929),.UNSPECIFIED.,.F.,.F.,(4,1,1,1,1,1,
1,4),(34.5575191894877,35.5340503040279,36.5205111974329,37.5069720908379,
38.4934329842429,39.4798938776479,40.4663547710529,40.8407044966673),
 .UNSPECIFIED.);
#1027=B_SPLINE_CURVE_WITH_KNOTS('',3,(#56930,#56931,#56932,#56933,#56934,
#56935,#56936,#56937,#56938,#56939),.UNSPECIFIED.,.F.,.F.,(4,1,1,1,1,1,
1,4),(34.5575191894877,35.1140788884769,36.1005397818819,37.0870006752869,
38.0734615686919,39.0599224620969,40.0463833555019,40.8407044966673),
 .UNSPECIFIED.);
#1028=B_SPLINE_CURVE_WITH_KNOTS('',3,(#56944,#56945,#56946,#56947,#56948,
#56949,#56950,#56951,#56952,#56953,#56954),.UNSPECIFIED.,.F.,.F.,(4,1,1,
1,1,1,1,1,4),(28.2743338823081,28.6288240501929,29.6152849435979,30.6017458370029,
31.5882067304079,32.5746676238129,33.5611285172179,34.5475894106229,34.5575191894877),
 .UNSPECIFIED.);
#1029=B_SPLINE_CURVE_WITH_KNOTS('',3,(#56955,#56956,#56957,#56958,#56959,
#56960,#56961,#56962,#56963,#56964),.UNSPECIFIED.,.F.,.F.,(4,1,1,1,1,1,
1,4),(28.2743338823081,29.1953135280469,30.1817744214519,31.1682353148569,
32.1546962082619,33.1411571016669,34.1276179950719,34.5575191894877),
 .UNSPECIFIED.);
#1030=B_SPLINE_CURVE_WITH_KNOTS('',3,(#56969,#56970,#56971,#56972,#56973,
#56974,#56975,#56976,#56977,#56978),.UNSPECIFIED.,.F.,.F.,(4,1,1,1,1,1,
1,4),(21.9911485751285,22.7100586897628,23.6965195831678,24.6829804765729,
25.6694413699779,26.6559022633829,27.6423631567879,28.2743338823081),
 .UNSPECIFIED.);
#1031=B_SPLINE_CURVE_WITH_KNOTS('',3,(#56979,#56980,#56981,#56982,#56983,
#56984,#56985,#56986,#56987,#56988,#56989),.UNSPECIFIED.,.F.,.F.,(4,1,1,
1,1,1,1,1,4),(21.9911485751285,22.2900872742119,23.2765481676169,24.2630090610219,
25.2494699544269,26.2359308478319,27.2223917412369,28.2088526346419,28.2743338823081),
 .UNSPECIFIED.);
#1032=B_SPLINE_CURVE_WITH_KNOTS('',3,(#56995,#56996,#56997,#56998,#56999),
 .UNSPECIFIED.,.F.,.F.,(4,1,4),(14.3984001269719,15.3848610203769,15.7079632679489),
 .UNSPECIFIED.);
#1033=B_SPLINE_CURVE_WITH_KNOTS('',3,(#57002,#57003,#57004,#57005,#57006),
 .UNSPECIFIED.,.F.,.F.,(4,1,4),(13.8759337553363,14.8183715425228,15.7079632679489),
 .UNSPECIFIED.);
#1034=B_SPLINE_CURVE_WITH_KNOTS('',3,(#57012,#57013,#57014,#57015),
 .UNSPECIFIED.,.F.,.F.,(4,4),(51.5750455984138,52.2824273504651),
 .UNSPECIFIED.);
#1035=B_SPLINE_CURVE_WITH_KNOTS('',3,(#57023,#57024,#57025,#57026,#57027,
#57028,#57029,#57030,#57031,#57032),.UNSPECIFIED.,.F.,.F.,(4,3,3,4),(-50.2654824574367,
-49.3230446702501,-48.3365837768451,-47.8312715558982),.UNSPECIFIED.);
#1036=B_SPLINE_CURVE_WITH_KNOTS('',3,(#57037,#57038,#57039,#57040,#57041,
#57042,#57043,#57044,#57045,#57046,#57047,#57048,#57049,#57050,#57051,#57052,
#57053,#57054,#57055,#57056,#57057,#57058,#57059,#57060,#57061),
 .UNSPECIFIED.,.F.,.F.,(4,3,3,3,3,3,3,3,4),(45.2918602912342,45.3772010966301,
46.3636619900351,47.3501228834401,48.3365837768451,49.3230446702501,50.3095055636551,
51.2959664570601,51.5750455984138),.UNSPECIFIED.);
#1037=B_SPLINE_CURVE_WITH_KNOTS('',3,(#57062,#57063,#57064,#57065,#57066,
#57067,#57068,#57069,#57070,#57071,#57072,#57073,#57074,#57075,#57076,#57077,
#57078,#57079,#57080,#57081,#57082,#57083),.UNSPECIFIED.,.F.,.F.,(4,3,3,
3,3,3,3,4),(-47.8312715558982,-47.3501228834401,-46.3636619900351,-45.3772010966301,
-44.3907402032251,-43.4042793098201,-42.4178184164151,-41.5480862487186),
 .UNSPECIFIED.);
#1038=B_SPLINE_CURVE_WITH_KNOTS('',3,(#57088,#57089,#57090,#57091,#57092,
#57093,#57094,#57095,#57096,#57097,#57098,#57099,#57100,#57101,#57102,#57103,
#57104,#57105,#57106,#57107,#57108,#57109),.UNSPECIFIED.,.F.,.F.,(4,3,3,
3,3,3,3,4),(39.0086749840546,39.4584357362001,40.4448966296051,41.4313575230101,
42.4178184164151,43.4042793098201,44.3907402032251,45.2918602912342),
 .UNSPECIFIED.);
#1039=B_SPLINE_CURVE_WITH_KNOTS('',3,(#57110,#57111,#57112,#57113,#57114,
#57115,#57116,#57117,#57118,#57119,#57120,#57121,#57122,#57123,#57124,#57125,
#57126,#57127,#57128,#57129,#57130,#57131,#57132,#57133,#57134),
 .UNSPECIFIED.,.F.,.F.,(4,3,3,3,3,3,3,3,4),(-41.5480862487186,-41.4313575230101,
-40.4448966296051,-39.4584357362001,-38.4719748427951,-37.4855139493901,
-36.4990530559851,-35.5125921625801,-35.2649009415391),.UNSPECIFIED.);
#1040=B_SPLINE_CURVE_WITH_KNOTS('',3,(#57139,#57140,#57141,#57142,#57143,
#57144,#57145,#57146,#57147,#57148,#57149,#57150,#57151,#57152,#57153,#57154,
#57155,#57156,#57157,#57158,#57159,#57160),.UNSPECIFIED.,.F.,.F.,(4,3,3,
3,3,3,3,4),(32.725489676875,33.5396703757701,34.5261312691751,35.5125921625801,
36.4990530559851,37.4855139493901,38.4719748427951,39.0086749840546),
 .UNSPECIFIED.);
#1041=B_SPLINE_CURVE_WITH_KNOTS('',3,(#57161,#57162,#57163,#57164,#57165,
#57166,#57167,#57168,#57169,#57170,#57171,#57172,#57173,#57174,#57175,#57176,
#57177,#57178,#57179,#57180,#57181,#57182),.UNSPECIFIED.,.F.,.F.,(4,3,3,
3,3,3,3,4),(-35.2649009415391,-34.5261312691751,-33.5396703757701,-32.5532094823651,
-31.5667485889601,-30.5802876955551,-29.5938268021501,-28.9817156343595),
 .UNSPECIFIED.);
#1042=B_SPLINE_CURVE_WITH_KNOTS('',3,(#57187,#57188,#57189,#57190,#57191,
#57192,#57193,#57194,#57195,#57196,#57197,#57198,#57199,#57200,#57201,#57202,
#57203,#57204,#57205,#57206,#57207,#57208,#57209,#57210,#57211),
 .UNSPECIFIED.,.F.,.F.,(4,3,3,3,3,3,3,3,4),(26.4423043696954,26.6344441219351,
27.6209050153401,28.6073659087451,29.5938268021501,30.5802876955551,31.5667485889601,
32.5532094823651,32.725489676875),.UNSPECIFIED.);
#1043=B_SPLINE_CURVE_WITH_KNOTS('',3,(#57212,#57213,#57214,#57215,#57216,
#57217,#57218,#57219,#57220,#57221,#57222,#57223,#57224,#57225,#57226,#57227,
#57228,#57229,#57230,#57231,#57232,#57233),.UNSPECIFIED.,.F.,.F.,(4,3,3,
3,3,3,3,4),(-28.9817156343595,-28.6073659087451,-27.6209050153401,-26.6344441219351,
-25.6479832285301,-24.6615223351251,-23.6750614417201,-22.6985303271799),
 .UNSPECIFIED.);
#1044=B_SPLINE_CURVE_WITH_KNOTS('',3,(#57238,#57239,#57240,#57241,#57242,
#57243,#57244,#57245,#57246,#57247,#57248,#57249,#57250,#57251,#57252,#57253,
#57254,#57255,#57256,#57257,#57258,#57259),.UNSPECIFIED.,.F.,.F.,(4,3,3,
3,3,3,3,4),(20.1591190625158,20.7156787615051,21.7021396549101,22.6886005483151,
23.6750614417201,24.6615223351251,25.6479832285301,26.4423043696954),
 .UNSPECIFIED.);
#1045=B_SPLINE_CURVE_WITH_KNOTS('',3,(#57260,#57261,#57262,#57263,#57264,
#57265,#57266,#57267,#57268,#57269,#57270,#57271,#57272,#57273,#57274,#57275,
#57276,#57277,#57278,#57279,#57280,#57281,#57282,#57283,#57284),
 .UNSPECIFIED.,.F.,.F.,(4,3,3,3,3,3,3,3,4),(-22.6985303271799,-22.6886005483151,
-21.70213965491,-20.715678761505,-19.7292178681,-18.742756974695,-17.75629608129,
-16.769835187885,-16.4153450200003),.UNSPECIFIED.);
#1046=B_SPLINE_CURVE_WITH_KNOTS('',3,(#57289,#57290,#57291,#57292,#57293,
#57294,#57295,#57296,#57297,#57298,#57299,#57300,#57301,#57302,#57303,#57304,
#57305,#57306,#57307,#57308,#57309,#57310),.UNSPECIFIED.,.F.,.F.,(4,3,3,
3,3,3,3,4),(13.8759337553362,14.796913401075,15.78337429448,16.769835187885,
17.7562960812901,18.7427569746951,19.7292178681001,20.1591190625158),
 .UNSPECIFIED.);
#1047=B_SPLINE_CURVE_WITH_KNOTS('',3,(#57311,#57312,#57313,#57314,#57315,
#57316,#57317,#57318,#57319,#57320,#57321,#57322,#57323,#57324,#57325,#57326,
#57327,#57328,#57329,#57330,#57331,#57332),.UNSPECIFIED.,.F.,.F.,(4,3,3,
3,3,3,3,4),(-16.4153450200003,-15.78337429448,-14.796913401075,-13.81045250767,
-12.823991614265,-11.83753072086,-10.851069827455,-10.1321597128207),
 .UNSPECIFIED.);
#1048=B_SPLINE_CURVE_WITH_KNOTS('',3,(#57338,#57339,#57340,#57341,#57342,
#57343,#57344,#57345,#57346,#57347,#57348,#57349,#57350),.UNSPECIFIED.,
 .F.,.F.,(4,3,3,3,4),(-3.84897440564113,-2.95938268021501,-1.97292178681,
-0.986460893405001,0.),.UNSPECIFIED.);
#1049=B_SPLINE_CURVE_WITH_KNOTS('',3,(#57353,#57354,#57355,#57356,#57357,
#57358,#57359,#57360,#57361,#57362,#57363,#57364,#57365,#57366,#57367,#57368,
#57369,#57370,#57371),.UNSPECIFIED.,.F.,.F.,(4,3,3,3,3,3,4),(2.01694489302845,
2.95938268021501,3.94584357362001,4.93230446702501,5.91876536043002,6.90522625383501,
7.59274844815666),.UNSPECIFIED.);
#1050=B_SPLINE_CURVE_WITH_KNOTS('',3,(#57377,#57378,#57379,#57380,#57381,
#57382,#57383,#57384),.UNSPECIFIED.,.F.,.F.,(4,1,1,1,1,4),(59.6902604182061,
60.1955726391529,61.1820335325579,62.1684944259629,63.154955319368,64.141416212773),
 .UNSPECIFIED.);
#1051=B_SPLINE_CURVE_WITH_KNOTS('',3,(#57387,#57388,#57389,#57390,#57391,
#57392,#57393,#57394,#57395),.UNSPECIFIED.,.F.,.F.,(4,1,1,1,1,1,4),(59.6902604182061,
59.775601223602,60.762062117007,61.748523010412,62.734983903817,63.721444797222,
64.6638825844085),.UNSPECIFIED.);
#1052=B_SPLINE_CURVE_WITH_KNOTS('',3,(#57400,#57401,#57402,#57403,#57404,
#57405,#57406,#57407,#57408,#57409),.UNSPECIFIED.,.F.,.F.,(4,1,1,1,1,1,
1,4),(53.4070751110265,54.2768072787229,55.2632681721279,56.2497290655329,
57.2361899589379,58.2226508523429,59.2091117457479,59.6902604182061),
 .UNSPECIFIED.);
#1053=B_SPLINE_CURVE_WITH_KNOTS('',3,(#57410,#57411,#57412,#57413,#57414,
#57415,#57416,#57417,#57418,#57419),.UNSPECIFIED.,.F.,.F.,(4,1,1,1,1,1,
1,4),(53.4070751110265,53.856835863172,54.843296756577,55.829757649982,
56.816218543387,57.802679436792,58.789140330197,59.6902604182061),
 .UNSPECIFIED.);
#1054=B_SPLINE_CURVE_WITH_KNOTS('',3,(#57424,#57425,#57426,#57427,#57428,
#57429,#57430,#57431,#57432,#57433,#57434),.UNSPECIFIED.,.F.,.F.,(4,1,1,
1,1,1,1,1,4),(47.1238898038469,47.3715810248879,48.3580419182929,49.3445028116979,
50.3309637051029,51.3174245985079,52.3038854919129,53.2903463853179,53.4070751110265),
 .UNSPECIFIED.);
#1055=B_SPLINE_CURVE_WITH_KNOTS('',3,(#57435,#57436,#57437,#57438,#57439,
#57440,#57441,#57442,#57443,#57444),.UNSPECIFIED.,.F.,.F.,(4,1,1,1,1,1,
1,4),(47.1238898038469,47.9380705027419,48.9245313961469,49.9109922895519,
50.897453182957,51.883914076362,52.870374969767,53.4070751110265),
 .UNSPECIFIED.);
#1056=B_SPLINE_CURVE_WITH_KNOTS('',3,(#57449,#57450,#57451,#57452,#57453,
#57454,#57455,#57456,#57457,#57458),.UNSPECIFIED.,.F.,.F.,(4,1,1,1,1,1,
1,4),(40.8407044966673,41.4528156644579,42.4392765578629,43.4257374512679,
44.4121983446729,45.3986592380779,46.3851201314829,47.1238898038469),
 .UNSPECIFIED.);
#1057=B_SPLINE_CURVE_WITH_KNOTS('',3,(#57459,#57460,#57461,#57462,#57463,
#57464,#57465,#57466,#57467,#57468,#57469),.UNSPECIFIED.,.F.,.F.,(4,1,1,
1,1,1,1,1,4),(40.8407044966673,41.0328442489069,42.0193051423119,43.0057660357169,
43.9922269291219,44.9786878225269,45.9651487159319,46.9516096093369,47.1238898038469),
 .UNSPECIFIED.);
#1058=B_SPLINE_CURVE_WITH_KNOTS('',3,(#57474,#57475,#57476,#57477,#57478,
#57479,#57480,#57481,#57482,#57483),.UNSPECIFIED.,.F.,.F.,(4,1,1,1,1,1,
1,4),(34.5575191894877,35.5340503040279,36.5205111974329,37.5069720908379,
38.4934329842429,39.4798938776479,40.4663547710529,40.8407044966673),
 .UNSPECIFIED.);
#1059=B_SPLINE_CURVE_WITH_KNOTS('',3,(#57484,#57485,#57486,#57487,#57488,
#57489,#57490,#57491,#57492,#57493),.UNSPECIFIED.,.F.,.F.,(4,1,1,1,1,1,
1,4),(34.5575191894877,35.1140788884769,36.1005397818819,37.0870006752869,
38.0734615686919,39.0599224620969,40.0463833555019,40.8407044966673),
 .UNSPECIFIED.);
#1060=B_SPLINE_CURVE_WITH_KNOTS('',3,(#57498,#57499,#57500,#57501,#57502,
#57503,#57504,#57505,#57506,#57507,#57508),.UNSPECIFIED.,.F.,.F.,(4,1,1,
1,1,1,1,1,4),(28.2743338823081,28.6288240501929,29.6152849435979,30.6017458370029,
31.5882067304079,32.5746676238129,33.5611285172179,34.5475894106229,34.5575191894877),
 .UNSPECIFIED.);
#1061=B_SPLINE_CURVE_WITH_KNOTS('',3,(#57509,#57510,#57511,#57512,#57513,
#57514,#57515,#57516,#57517,#57518),.UNSPECIFIED.,.F.,.F.,(4,1,1,1,1,1,
1,4),(28.2743338823081,29.1953135280469,30.1817744214519,31.1682353148569,
32.1546962082619,33.1411571016669,34.1276179950719,34.5575191894877),
 .UNSPECIFIED.);
#1062=B_SPLINE_CURVE_WITH_KNOTS('',3,(#57523,#57524,#57525,#57526,#57527,
#57528,#57529,#57530,#57531,#57532),.UNSPECIFIED.,.F.,.F.,(4,1,1,1,1,1,
1,4),(21.9911485751285,22.7100586897628,23.6965195831678,24.6829804765729,
25.6694413699779,26.6559022633829,27.6423631567879,28.2743338823081),
 .UNSPECIFIED.);
#1063=B_SPLINE_CURVE_WITH_KNOTS('',3,(#57533,#57534,#57535,#57536,#57537,
#57538,#57539,#57540,#57541,#57542,#57543),.UNSPECIFIED.,.F.,.F.,(4,1,1,
1,1,1,1,1,4),(21.9911485751285,22.2900872742119,23.2765481676169,24.2630090610219,
25.2494699544269,26.2359308478319,27.2223917412369,28.2088526346419,28.2743338823081),
 .UNSPECIFIED.);
#1064=B_SPLINE_CURVE_WITH_KNOTS('',3,(#57549,#57550,#57551,#57552,#57553),
 .UNSPECIFIED.,.F.,.F.,(4,1,4),(14.3984001269719,15.3848610203769,15.7079632679489),
 .UNSPECIFIED.);
#1065=B_SPLINE_CURVE_WITH_KNOTS('',3,(#57556,#57557,#57558,#57559,#57560),
 .UNSPECIFIED.,.F.,.F.,(4,1,4),(13.8759337553363,14.8183715425228,15.7079632679489),
 .UNSPECIFIED.);
#1066=B_SPLINE_CURVE_WITH_KNOTS('',3,(#57566,#57567,#57568,#57569),
 .UNSPECIFIED.,.F.,.F.,(4,4),(51.5750455984138,52.2824273504651),
 .UNSPECIFIED.);
#1067=B_SPLINE_CURVE_WITH_KNOTS('',3,(#57577,#57578,#57579,#57580,#57581,
#57582,#57583,#57584,#57585,#57586),.UNSPECIFIED.,.F.,.F.,(4,3,3,4),(-50.2654824574367,
-49.3230446702501,-48.3365837768451,-47.8312715558982),.UNSPECIFIED.);
#1068=B_SPLINE_CURVE_WITH_KNOTS('',3,(#57591,#57592,#57593,#57594,#57595,
#57596,#57597,#57598,#57599,#57600,#57601,#57602,#57603,#57604,#57605,#57606,
#57607,#57608,#57609,#57610,#57611,#57612,#57613,#57614,#57615),
 .UNSPECIFIED.,.F.,.F.,(4,3,3,3,3,3,3,3,4),(45.2918602912342,45.3772010966301,
46.3636619900351,47.3501228834401,48.3365837768451,49.3230446702501,50.3095055636551,
51.2959664570601,51.5750455984138),.UNSPECIFIED.);
#1069=B_SPLINE_CURVE_WITH_KNOTS('',3,(#57616,#57617,#57618,#57619,#57620,
#57621,#57622,#57623,#57624,#57625,#57626,#57627,#57628,#57629,#57630,#57631,
#57632,#57633,#57634,#57635,#57636,#57637),.UNSPECIFIED.,.F.,.F.,(4,3,3,
3,3,3,3,4),(-47.8312715558982,-47.3501228834401,-46.3636619900351,-45.3772010966301,
-44.3907402032251,-43.4042793098201,-42.4178184164151,-41.5480862487186),
 .UNSPECIFIED.);
#1070=B_SPLINE_CURVE_WITH_KNOTS('',3,(#57642,#57643,#57644,#57645,#57646,
#57647,#57648,#57649,#57650,#57651,#57652,#57653,#57654,#57655,#57656,#57657,
#57658,#57659,#57660,#57661,#57662,#57663),.UNSPECIFIED.,.F.,.F.,(4,3,3,
3,3,3,3,4),(39.0086749840546,39.4584357362001,40.4448966296051,41.4313575230101,
42.4178184164151,43.4042793098201,44.3907402032251,45.2918602912342),
 .UNSPECIFIED.);
#1071=B_SPLINE_CURVE_WITH_KNOTS('',3,(#57664,#57665,#57666,#57667,#57668,
#57669,#57670,#57671,#57672,#57673,#57674,#57675,#57676,#57677,#57678,#57679,
#57680,#57681,#57682,#57683,#57684,#57685,#57686,#57687,#57688),
 .UNSPECIFIED.,.F.,.F.,(4,3,3,3,3,3,3,3,4),(-41.5480862487186,-41.4313575230101,
-40.4448966296051,-39.4584357362001,-38.4719748427951,-37.4855139493901,
-36.4990530559851,-35.5125921625801,-35.264900941539),.UNSPECIFIED.);
#1072=B_SPLINE_CURVE_WITH_KNOTS('',3,(#57693,#57694,#57695,#57696,#57697,
#57698,#57699,#57700,#57701,#57702,#57703,#57704,#57705,#57706,#57707,#57708,
#57709,#57710,#57711,#57712,#57713,#57714),.UNSPECIFIED.,.F.,.F.,(4,3,3,
3,3,3,3,4),(32.725489676875,33.5396703757701,34.5261312691751,35.5125921625801,
36.4990530559851,37.4855139493901,38.4719748427951,39.0086749840546),
 .UNSPECIFIED.);
#1073=B_SPLINE_CURVE_WITH_KNOTS('',3,(#57715,#57716,#57717,#57718,#57719,
#57720,#57721,#57722,#57723,#57724,#57725,#57726,#57727,#57728,#57729,#57730,
#57731,#57732,#57733,#57734,#57735,#57736),.UNSPECIFIED.,.F.,.F.,(4,3,3,
3,3,3,3,4),(-35.264900941539,-34.5261312691751,-33.5396703757701,-32.5532094823651,
-31.5667485889601,-30.5802876955551,-29.5938268021501,-28.9817156343595),
 .UNSPECIFIED.);
#1074=B_SPLINE_CURVE_WITH_KNOTS('',3,(#57741,#57742,#57743,#57744,#57745,
#57746,#57747,#57748,#57749,#57750,#57751,#57752,#57753,#57754,#57755,#57756,
#57757,#57758,#57759,#57760,#57761,#57762,#57763,#57764,#57765),
 .UNSPECIFIED.,.F.,.F.,(4,3,3,3,3,3,3,3,4),(26.4423043696954,26.6344441219351,
27.6209050153401,28.6073659087451,29.5938268021501,30.5802876955551,31.5667485889601,
32.5532094823651,32.725489676875),.UNSPECIFIED.);
#1075=B_SPLINE_CURVE_WITH_KNOTS('',3,(#57766,#57767,#57768,#57769,#57770,
#57771,#57772,#57773,#57774,#57775,#57776,#57777,#57778,#57779,#57780,#57781,
#57782,#57783,#57784,#57785,#57786,#57787),.UNSPECIFIED.,.F.,.F.,(4,3,3,
3,3,3,3,4),(-28.9817156343595,-28.6073659087451,-27.6209050153401,-26.6344441219351,
-25.6479832285301,-24.6615223351251,-23.6750614417201,-22.6985303271799),
 .UNSPECIFIED.);
#1076=B_SPLINE_CURVE_WITH_KNOTS('',3,(#57792,#57793,#57794,#57795,#57796,
#57797,#57798,#57799,#57800,#57801,#57802,#57803,#57804,#57805,#57806,#57807,
#57808,#57809,#57810,#57811,#57812,#57813),.UNSPECIFIED.,.F.,.F.,(4,3,3,
3,3,3,3,4),(20.1591190625158,20.7156787615051,21.7021396549101,22.6886005483151,
23.6750614417201,24.6615223351251,25.6479832285301,26.4423043696954),
 .UNSPECIFIED.);
#1077=B_SPLINE_CURVE_WITH_KNOTS('',3,(#57814,#57815,#57816,#57817,#57818,
#57819,#57820,#57821,#57822,#57823,#57824,#57825,#57826,#57827,#57828,#57829,
#57830,#57831,#57832,#57833,#57834,#57835,#57836,#57837,#57838),
 .UNSPECIFIED.,.F.,.F.,(4,3,3,3,3,3,3,3,4),(-22.6985303271799,-22.6886005483151,
-21.7021396549101,-20.7156787615051,-19.7292178681001,-18.7427569746951,
-17.75629608129,-16.769835187885,-16.4153450200003),.UNSPECIFIED.);
#1078=B_SPLINE_CURVE_WITH_KNOTS('',3,(#57843,#57844,#57845,#57846,#57847,
#57848,#57849,#57850,#57851,#57852,#57853,#57854,#57855,#57856,#57857,#57858,
#57859,#57860,#57861,#57862,#57863,#57864),.UNSPECIFIED.,.F.,.F.,(4,3,3,
3,3,3,3,4),(13.8759337553362,14.796913401075,15.78337429448,16.769835187885,
17.75629608129,18.7427569746951,19.7292178681001,20.1591190625158),
 .UNSPECIFIED.);
#1079=B_SPLINE_CURVE_WITH_KNOTS('',3,(#57865,#57866,#57867,#57868,#57869,
#57870,#57871,#57872,#57873,#57874,#57875,#57876,#57877,#57878,#57879,#57880,
#57881,#57882,#57883,#57884,#57885,#57886),.UNSPECIFIED.,.F.,.F.,(4,3,3,
3,3,3,3,4),(-16.4153450200003,-15.78337429448,-14.796913401075,-13.81045250767,
-12.823991614265,-11.83753072086,-10.851069827455,-10.1321597128207),
 .UNSPECIFIED.);
#1080=B_SPLINE_CURVE_WITH_KNOTS('',3,(#57892,#57893,#57894,#57895,#57896,
#57897,#57898,#57899,#57900,#57901,#57902,#57903,#57904),.UNSPECIFIED.,
 .F.,.F.,(4,3,3,3,4),(-3.84897440564112,-2.95938268021501,-1.97292178681001,
-0.986460893405003,0.),.UNSPECIFIED.);
#1081=B_SPLINE_CURVE_WITH_KNOTS('',3,(#57907,#57908,#57909,#57910,#57911,
#57912,#57913,#57914,#57915,#57916,#57917,#57918,#57919,#57920,#57921,#57922,
#57923,#57924,#57925),.UNSPECIFIED.,.F.,.F.,(4,3,3,3,3,3,4),(2.01694489302844,
2.95938268021501,3.94584357362001,4.93230446702501,5.91876536043001,6.90522625383502,
7.59274844815664),.UNSPECIFIED.);
#1082=B_SPLINE_CURVE_WITH_KNOTS('',3,(#57931,#57932,#57933,#57934,#57935,
#57936,#57937,#57938),.UNSPECIFIED.,.F.,.F.,(4,1,1,1,1,4),(59.6902604182061,
60.195572639153,61.182033532558,62.168494425963,63.154955319368,64.141416212773),
 .UNSPECIFIED.);
#1083=B_SPLINE_CURVE_WITH_KNOTS('',3,(#57941,#57942,#57943,#57944,#57945,
#57946,#57947,#57948,#57949),.UNSPECIFIED.,.F.,.F.,(4,1,1,1,1,1,4),(59.6902604182061,
59.775601223602,60.762062117007,61.748523010412,62.734983903817,63.721444797222,
64.6638825844085),.UNSPECIFIED.);
#1084=B_SPLINE_CURVE_WITH_KNOTS('',3,(#57954,#57955,#57956,#57957,#57958,
#57959,#57960,#57961,#57962,#57963),.UNSPECIFIED.,.F.,.F.,(4,1,1,1,1,1,
1,4),(53.4070751110265,54.2768072787229,55.2632681721279,56.2497290655329,
57.2361899589379,58.222650852343,59.209111745748,59.6902604182061),
 .UNSPECIFIED.);
#1085=B_SPLINE_CURVE_WITH_KNOTS('',3,(#57964,#57965,#57966,#57967,#57968,
#57969,#57970,#57971,#57972,#57973),.UNSPECIFIED.,.F.,.F.,(4,1,1,1,1,1,
1,4),(53.4070751110265,53.856835863172,54.843296756577,55.829757649982,
56.816218543387,57.802679436792,58.789140330197,59.6902604182061),
 .UNSPECIFIED.);
#1086=B_SPLINE_CURVE_WITH_KNOTS('',3,(#57978,#57979,#57980,#57981,#57982,
#57983,#57984,#57985,#57986,#57987,#57988),.UNSPECIFIED.,.F.,.F.,(4,1,1,
1,1,1,1,1,4),(47.1238898038469,47.3715810248879,48.3580419182929,49.3445028116979,
50.3309637051029,51.3174245985079,52.3038854919129,53.2903463853179,53.4070751110265),
 .UNSPECIFIED.);
#1087=B_SPLINE_CURVE_WITH_KNOTS('',3,(#57989,#57990,#57991,#57992,#57993,
#57994,#57995,#57996,#57997,#57998),.UNSPECIFIED.,.F.,.F.,(4,1,1,1,1,1,
1,4),(47.1238898038469,47.938070502742,48.924531396147,49.910992289552,
50.897453182957,51.883914076362,52.870374969767,53.4070751110265),
 .UNSPECIFIED.);
#1088=B_SPLINE_CURVE_WITH_KNOTS('',3,(#58003,#58004,#58005,#58006,#58007,
#58008,#58009,#58010,#58011,#58012),.UNSPECIFIED.,.F.,.F.,(4,1,1,1,1,1,
1,4),(40.8407044966673,41.4528156644579,42.4392765578629,43.4257374512679,
44.4121983446729,45.3986592380779,46.3851201314829,47.1238898038469),
 .UNSPECIFIED.);
#1089=B_SPLINE_CURVE_WITH_KNOTS('',3,(#58013,#58014,#58015,#58016,#58017,
#58018,#58019,#58020,#58021,#58022,#58023),.UNSPECIFIED.,.F.,.F.,(4,1,1,
1,1,1,1,1,4),(40.8407044966673,41.0328442489069,42.0193051423119,43.0057660357169,
43.9922269291219,44.978687822527,45.965148715932,46.951609609337,47.1238898038469),
 .UNSPECIFIED.);
#1090=B_SPLINE_CURVE_WITH_KNOTS('',3,(#58028,#58029,#58030,#58031,#58032,
#58033,#58034,#58035,#58036,#58037),.UNSPECIFIED.,.F.,.F.,(4,1,1,1,1,1,
1,4),(34.5575191894877,35.5340503040279,36.5205111974329,37.5069720908379,
38.4934329842429,39.4798938776479,40.4663547710529,40.8407044966673),
 .UNSPECIFIED.);
#1091=B_SPLINE_CURVE_WITH_KNOTS('',3,(#58038,#58039,#58040,#58041,#58042,
#58043,#58044,#58045,#58046,#58047),.UNSPECIFIED.,.F.,.F.,(4,1,1,1,1,1,
1,4),(34.5575191894877,35.1140788884769,36.1005397818819,37.0870006752869,
38.0734615686919,39.0599224620969,40.0463833555019,40.8407044966673),
 .UNSPECIFIED.);
#1092=B_SPLINE_CURVE_WITH_KNOTS('',3,(#58052,#58053,#58054,#58055,#58056,
#58057,#58058,#58059,#58060,#58061,#58062),.UNSPECIFIED.,.F.,.F.,(4,1,1,
1,1,1,1,1,4),(28.2743338823081,28.6288240501929,29.6152849435979,30.6017458370029,
31.5882067304079,32.5746676238129,33.5611285172179,34.5475894106229,34.5575191894877),
 .UNSPECIFIED.);
#1093=B_SPLINE_CURVE_WITH_KNOTS('',3,(#58063,#58064,#58065,#58066,#58067,
#58068,#58069,#58070,#58071,#58072),.UNSPECIFIED.,.F.,.F.,(4,1,1,1,1,1,
1,4),(28.2743338823081,29.1953135280469,30.1817744214519,31.1682353148569,
32.1546962082619,33.1411571016669,34.1276179950719,34.5575191894877),
 .UNSPECIFIED.);
#1094=B_SPLINE_CURVE_WITH_KNOTS('',3,(#58077,#58078,#58079,#58080,#58081,
#58082,#58083,#58084,#58085,#58086),.UNSPECIFIED.,.F.,.F.,(4,1,1,1,1,1,
1,4),(21.9911485751285,22.7100586897629,23.6965195831679,24.6829804765729,
25.6694413699779,26.6559022633829,27.6423631567879,28.2743338823081),
 .UNSPECIFIED.);
#1095=B_SPLINE_CURVE_WITH_KNOTS('',3,(#58087,#58088,#58089,#58090,#58091,
#58092,#58093,#58094,#58095,#58096,#58097),.UNSPECIFIED.,.F.,.F.,(4,1,1,
1,1,1,1,1,4),(21.9911485751285,22.2900872742119,23.2765481676169,24.2630090610219,
25.2494699544269,26.2359308478319,27.2223917412369,28.2088526346419,28.2743338823081),
 .UNSPECIFIED.);
#1096=B_SPLINE_CURVE_WITH_KNOTS('',3,(#58103,#58104,#58105,#58106,#58107),
 .UNSPECIFIED.,.F.,.F.,(4,1,4),(14.3984001269719,15.3848610203769,15.7079632679489),
 .UNSPECIFIED.);
#1097=B_SPLINE_CURVE_WITH_KNOTS('',3,(#58110,#58111,#58112,#58113,#58114),
 .UNSPECIFIED.,.F.,.F.,(4,1,4),(13.8759337553363,14.8183715425228,15.7079632679489),
 .UNSPECIFIED.);
#1098=B_SPLINE_CURVE_WITH_KNOTS('',3,(#58116,#58117,#58118,#58119,#58120,
#58121,#58122,#58123,#58124,#58125,#58126,#58127,#58128,#58129,#58130,#58131,
#58132,#58133,#58134,#58135,#58136,#58137,#58138,#58139,#58140,#58141,#58142,
#58143,#58144,#58145,#58146,#58147,#58148,#58149,#58150,#58151,#58152,#58153,
#58154,#58155,#58156,#58157,#58158,#58159,#58160,#58161,#58162,#58163,#58164,
#58165,#58166,#58167,#58168,#58169,#58170,#58171,#58172,#58173,#58174,#58175,
#58176,#58177,#58178,#58179,#58180,#58181,#58182,#58183,#58184,#58185,#58186,
#58187,#58188,#58189,#58190,#58191,#58192,#58193,#58194,#58195,#58196,#58197,
#58198,#58199,#58200,#58201,#58202,#58203,#58204,#58205,#58206,#58207,#58208,
#58209),.UNSPECIFIED.,.F.,.F.,(4,3,3,3,3,3,3,3,3,3,3,3,3,3,3,3,3,3,3,3,
3,3,3,3,3,3,3,3,3,3,3,4),(-0.569248610399439,-0.54356321026788,-0.51725177755219,
-0.510354554433286,-0.504796969238609,-0.477731405971173,-0.456105549235436,
-0.448989007169752,-0.44252634525638,-0.41479354371395,-0.386635764628684,
-0.358697147124577,-0.345203998364752,-0.340863871144016,-0.336326749475397,
-0.307401033120815,-0.304724552085278,-0.27693747898326,-0.248513803621531,
-0.232656005969356,-0.228221175977861,-0.199230005786307,-0.169667310992576,
-0.139872005633123,-0.124084622535551,-0.117720237608985,-0.113355273030534,
-0.0828138353231538,-0.052246421283799,-0.0222710285652406,-0.0135729408525455,
0.),.UNSPECIFIED.);
#1099=B_SPLINE_CURVE_WITH_KNOTS('',3,(#58210,#58211,#58212,#58213,#58214,
#58215,#58216,#58217,#58218,#58219,#58220,#58221,#58222,#58223,#58224,#58225,
#58226,#58227,#58228,#58229,#58230,#58231,#58232,#58233,#58234,#58235,#58236,
#58237,#58238,#58239,#58240,#58241,#58242,#58243,#58244,#58245,#58246,#58247,
#58248,#58249,#58250,#58251,#58252,#58253,#58254,#58255,#58256,#58257,#58258,
#58259,#58260,#58261,#58262,#58263,#58264,#58265,#58266,#58267,#58268,#58269,
#58270,#58271,#58272,#58273,#58274,#58275,#58276,#58277,#58278,#58279,#58280,
#58281,#58282,#58283,#58284,#58285,#58286,#58287,#58288,#58289,#58290,#58291,
#58292,#58293,#58294,#58295,#58296,#58297,#58298,#58299,#58300,#58301,#58302,
#58303,#58304,#58305,#58306),.UNSPECIFIED.,.F.,.F.,(4,3,3,3,3,3,3,3,3,3,
3,3,3,3,3,3,3,3,3,3,3,3,3,3,3,3,3,3,3,3,3,3,4),(-0.566847306048084,-0.536659061903649,
-0.506054167513983,-0.49735931415594,-0.490469774907708,-0.46032717525434,
-0.437299554635119,-0.425273742105126,-0.42037664994689,-0.390957260822939,
-0.362078927205336,-0.333750616169337,-0.319339514702147,-0.312267662800037,
-0.308232039095118,-0.280241121737425,-0.276106210300576,-0.247648675773662,
-0.218090819684273,-0.209492296602851,-0.204738459070877,-0.200614645085577,
-0.172781389578512,-0.145026433045361,-0.117750656382618,-0.10443005271711,
-0.100025234036307,-0.0958388284225397,-0.0691738510173895,-0.0429555684736812,
-0.0175134533592336,-0.0111858270585534,0.),.UNSPECIFIED.);
#1100=B_SPLINE_CURVE_WITH_KNOTS('',3,(#58308,#58309,#58310,#58311,#58312,
#58313,#58314,#58315,#58316,#58317,#58318),.UNSPECIFIED.,.F.,.F.,(4,1,1,
1,1,1,1,1,4),(15.7079632679489,15.8048324359278,16.7912933293328,17.7777542227378,
18.7642151161429,19.7506760095479,20.7371369029529,21.7235977963579,21.9911485751285),
 .UNSPECIFIED.);
#1101=B_SPLINE_CURVE_WITH_KNOTS('',3,(#58319,#58320,#58321,#58322,#58323,
#58324,#58325,#58326,#58327,#58328),.UNSPECIFIED.,.F.,.F.,(4,1,1,1,1,1,
1,4),(15.7079632679489,16.3713219137819,17.3577828071869,18.3442437005919,
19.3307045939969,20.3171654874019,21.3036263808069,21.9911485751285),
 .UNSPECIFIED.);
#1102=B_SPLINE_CURVE_WITH_KNOTS('',3,(#58553,#58554,#58555,#58556,#58557,
#58558,#58559,#58560,#58561,#58562,#58563,#58564,#58565,#58566,#58567,#58568,
#58569,#58570,#58571,#58572,#58573,#58574,#58575,#58576,#58577,#58578,#58579,
#58580,#58581,#58582,#58583,#58584,#58585,#58586,#58587,#58588,#58589,#58590,
#58591,#58592,#58593,#58594,#58595,#58596,#58597,#58598,#58599,#58600,#58601,
#58602,#58603,#58604,#58605,#58606,#58607,#58608,#58609,#58610,#58611,#58612,
#58613,#58614,#58615,#58616,#58617,#58618,#58619,#58620,#58621,#58622,#58623,
#58624,#58625,#58626,#58627,#58628,#58629,#58630,#58631,#58632,#58633,#58634,
#58635,#58636,#58637,#58638,#58639,#58640,#58641,#58642,#58643),
 .UNSPECIFIED.,.F.,.F.,(4,3,3,3,3,3,3,3,3,3,3,3,3,3,3,3,3,3,3,3,3,3,3,3,
3,3,3,3,3,3,4),(0.,0.0253749761808373,0.0514202453857712,0.0779566483534038,
0.0899762183904566,0.0968038784409555,0.102648429733812,0.129953030321501,
0.157704740391969,0.184206422575685,0.195897654370316,0.20134852299372,
0.206600979641336,0.235231099301492,0.263711469126832,0.291580654157613,
0.307940063613124,0.312151264914525,0.340175958120619,0.369258857874792,
0.398694885878799,0.418024425824675,0.423205607838508,0.428149011920458,
0.459444560301794,0.482916221587795,0.491343691753009,0.498388187388185,
0.528903379110968,0.553331205445801,0.566847306048077),.UNSPECIFIED.);
#1103=B_SPLINE_CURVE_WITH_KNOTS('',3,(#58644,#58645,#58646,#58647,#58648,
#58649,#58650,#58651,#58652,#58653,#58654,#58655,#58656,#58657,#58658,#58659,
#58660,#58661,#58662,#58663,#58664,#58665,#58666,#58667,#58668),
 .UNSPECIFIED.,.F.,.F.,(4,3,3,3,3,3,3,3,4),(-10.1321597128207,-9.86460893405003,
-8.87814804064503,-7.89168714724002,-6.90522625383502,-5.91876536043002,
-4.93230446702501,-3.94584357362001,-3.84897440564112),.UNSPECIFIED.);
#1104=B_SPLINE_CURVE_WITH_KNOTS('',3,(#58893,#58894,#58895,#58896,#58897,
#58898,#58899,#58900,#58901,#58902,#58903,#58904,#58905,#58906,#58907,#58908,
#58909,#58910,#58911,#58912,#58913,#58914,#58915,#58916,#58917),
 .UNSPECIFIED.,.F.,.F.,(4,3,3,3,3,3,3,3,4),(7.59274844815664,7.89168714724002,
8.87814804064502,9.86460893405003,10.851069827455,11.83753072086,12.823991614265,
13.81045250767,13.8759337553362),.UNSPECIFIED.);
#1105=B_SPLINE_CURVE_WITH_KNOTS('',3,(#58918,#58919,#58920,#58921,#58922,
#58923,#58924,#58925,#58926,#58927,#58928,#58929,#58930,#58931,#58932,#58933,
#58934,#58935,#58936,#58937,#58938,#58939,#58940,#58941,#58942,#58943,#58944,
#58945,#58946,#58947,#58948,#58949,#58950,#58951,#58952,#58953,#58954,#58955,
#58956,#58957,#58958,#58959,#58960,#58961,#58962,#58963,#58964,#58965,#58966,
#58967,#58968,#58969,#58970,#58971,#58972,#58973,#58974,#58975,#58976,#58977,
#58978,#58979,#58980,#58981,#58982,#58983,#58984,#58985,#58986,#58987,#58988,
#58989,#58990,#58991,#58992,#58993,#58994,#58995,#58996,#58997,#58998,#58999,
#59000,#59001,#59002,#59003,#59004,#59005),.UNSPECIFIED.,.F.,.F.,(4,3,3,
3,3,3,3,3,3,3,3,3,3,3,3,3,3,3,3,3,3,3,3,3,3,3,3,3,3,4),(0.,0.0297343552567438,
0.0601207256243431,0.0891402780188099,0.114532386363968,0.120626668225237,
0.150381699187288,0.179970351010139,0.208047049452624,0.230390915983779,
0.234467415790057,0.263372280285067,0.292277144780078,0.321216399233671,
0.336017014192979,0.340284510578769,0.344592048040137,0.372696731227283,
0.400818676768978,0.428516493390579,0.439577089903316,0.445404908685826,
0.450327814198675,0.477288785913009,0.497473149080406,0.505236433644848,
0.511959475796908,0.537908351627998,0.558026238582596,0.569248610399449),
 .UNSPECIFIED.);
#1106=B_SPLINE_CURVE_WITH_KNOTS('',3,(#59008,#59009,#59010,#59011,#59012,
#59013,#59014,#59015,#59016,#59017,#59018,#59019,#59020,#59021,#59022,#59023,
#59024,#59025,#59026,#59027,#59028,#59029,#59030,#59031,#59032,#59033,#59034,
#59035,#59036,#59037,#59038,#59039,#59040,#59041,#59042,#59043,#59044,#59045,
#59046,#59047,#59048,#59049,#59050,#59051,#59052,#59053,#59054,#59055,#59056,
#59057,#59058,#59059,#59060,#59061,#59062,#59063,#59064,#59065,#59066,#59067,
#59068,#59069,#59070,#59071,#59072,#59073,#59074,#59075,#59076,#59077,#59078,
#59079,#59080,#59081,#59082,#59083,#59084,#59085,#59086,#59087,#59088,#59089,
#59090,#59091,#59092,#59093,#59094,#59095,#59096,#59097,#59098,#59099,#59100,
#59101),.UNSPECIFIED.,.F.,.F.,(4,3,3,3,3,3,3,3,3,3,3,3,3,3,3,3,3,3,3,3,
3,3,3,3,3,3,3,3,3,3,3,4),(-0.569248610399449,-0.543563182261633,-0.517251726319563,
-0.510354426439678,-0.50479695498386,-0.477731372271303,-0.456105519748053,
-0.448988869091777,-0.442526350881559,-0.414793531524841,-0.386635753667763,
-0.358697146614525,-0.34520399798222,-0.340863870845798,-0.33632674866549,
-0.307401034118885,-0.304724552085303,-0.276937498904782,-0.248513836066906,
-0.232656079580101,-0.228221193819419,-0.199230039362694,-0.1696673522492,
-0.139872047864531,-0.124084659488033,-0.117720027272243,-0.113355233265148,
-0.0828137979174933,-0.0522463837565239,-0.0222709947806455,-0.0135729408525504,
0.),.UNSPECIFIED.);
#1107=B_SPLINE_CURVE_WITH_KNOTS('',3,(#59102,#59103,#59104,#59105,#59106,
#59107,#59108,#59109,#59110,#59111,#59112,#59113,#59114,#59115,#59116,#59117,
#59118,#59119,#59120,#59121,#59122,#59123,#59124,#59125,#59126,#59127,#59128,
#59129,#59130,#59131,#59132,#59133,#59134,#59135,#59136,#59137,#59138,#59139,
#59140,#59141,#59142,#59143,#59144,#59145,#59146,#59147,#59148,#59149,#59150,
#59151,#59152,#59153,#59154,#59155,#59156,#59157,#59158,#59159,#59160,#59161,
#59162,#59163,#59164,#59165,#59166,#59167,#59168,#59169,#59170,#59171,#59172,
#59173,#59174,#59175,#59176,#59177,#59178,#59179,#59180,#59181,#59182,#59183,
#59184,#59185,#59186,#59187,#59188,#59189,#59190,#59191,#59192,#59193,#59194,
#59195,#59196,#59197,#59198),.UNSPECIFIED.,.F.,.F.,(4,3,3,3,3,3,3,3,3,3,
3,3,3,3,3,3,3,3,3,3,3,3,3,3,3,3,3,3,3,3,3,3,4),(-0.566847306048093,-0.536659041927388,
-0.506054142756331,-0.497359284644658,-0.490469768799004,-0.460327170439997,
-0.43729955042257,-0.425273732599625,-0.420376646332479,-0.390957260247852,
-0.362078935948881,-0.333750632250775,-0.319339526763226,-0.312267682102884,
-0.308232073167884,-0.280241164390834,-0.276106210300581,-0.247648676940529,
-0.218090820705282,-0.209492305755956,-0.204738428044034,-0.200614618605046,
-0.172781361973988,-0.145026407762726,-0.11775064123255,-0.1044300394608,
-0.100025210256123,-0.0958388268874492,-0.0691738559200647,-0.0429555864020897,
-0.0175134923892686,-0.011185827058555,0.),.UNSPECIFIED.);
#1108=B_SPLINE_CURVE_WITH_KNOTS('',3,(#59200,#59201,#59202,#59203,#59204,
#59205,#59206,#59207,#59208,#59209,#59210),.UNSPECIFIED.,.F.,.F.,(4,1,1,
1,1,1,1,1,4),(15.7079632679489,15.8048324359278,16.7912933293328,17.7777542227378,
18.7642151161428,19.7506760095478,20.7371369029528,21.7235977963578,21.9911485751285),
 .UNSPECIFIED.);
#1109=B_SPLINE_CURVE_WITH_KNOTS('',3,(#59211,#59212,#59213,#59214,#59215,
#59216,#59217,#59218,#59219,#59220),.UNSPECIFIED.,.F.,.F.,(4,1,1,1,1,1,
1,4),(15.7079632679489,16.3713219137819,17.3577828071869,18.3442437005919,
19.3307045939969,20.3171654874019,21.3036263808069,21.9911485751285),
 .UNSPECIFIED.);
#1110=B_SPLINE_CURVE_WITH_KNOTS('',3,(#59445,#59446,#59447,#59448,#59449,
#59450,#59451,#59452,#59453,#59454,#59455,#59456,#59457,#59458,#59459,#59460,
#59461,#59462,#59463,#59464,#59465,#59466,#59467,#59468,#59469,#59470,#59471,
#59472,#59473,#59474,#59475,#59476,#59477,#59478,#59479,#59480,#59481,#59482,
#59483,#59484,#59485,#59486,#59487,#59488,#59489,#59490,#59491,#59492,#59493,
#59494,#59495,#59496,#59497,#59498,#59499,#59500,#59501,#59502,#59503,#59504,
#59505,#59506,#59507,#59508,#59509,#59510,#59511,#59512,#59513,#59514,#59515,
#59516,#59517,#59518,#59519,#59520,#59521,#59522,#59523,#59524,#59525,#59526,
#59527,#59528,#59529,#59530,#59531,#59532,#59533,#59534,#59535),
 .UNSPECIFIED.,.F.,.F.,(4,3,3,3,3,3,3,3,3,3,3,3,3,3,3,3,3,3,3,3,3,3,3,3,
3,3,3,3,3,3,4),(0.,0.0253750087516075,0.0514203072172438,0.0779567024559424,
0.0899762332180016,0.0968038780381036,0.10264843024679,0.129953053284425,
0.157704773943122,0.18420644773905,0.195897666391424,0.201348497446843,
0.206600974226724,0.235231090538335,0.263711469126833,0.291580637154729,
0.307940047672921,0.312151253621455,0.340175922185425,0.369258810210864,
0.398694834915773,0.418024381232026,0.42320553295956,0.428148997028943,
0.459444549133158,0.482916213211318,0.491343671374895,0.498388182075807,
0.528903373982295,0.5533312054458,0.566847306048075),.UNSPECIFIED.);
#1111=B_SPLINE_CURVE_WITH_KNOTS('',3,(#59536,#59537,#59538,#59539,#59540,
#59541,#59542,#59543,#59544,#59545,#59546,#59547,#59548,#59549,#59550,#59551,
#59552,#59553,#59554,#59555,#59556,#59557,#59558,#59559,#59560),
 .UNSPECIFIED.,.F.,.F.,(4,3,3,3,3,3,3,3,4),(-10.1321597128207,-9.86460893405002,
-8.87814804064502,-7.89168714724002,-6.90522625383502,-5.91876536043002,
-4.93230446702501,-3.94584357362001,-3.84897440564113),.UNSPECIFIED.);
#1112=B_SPLINE_CURVE_WITH_KNOTS('',3,(#59785,#59786,#59787,#59788,#59789,
#59790,#59791,#59792,#59793,#59794,#59795,#59796,#59797,#59798,#59799,#59800,
#59801,#59802,#59803,#59804,#59805,#59806,#59807,#59808,#59809),
 .UNSPECIFIED.,.F.,.F.,(4,3,3,3,3,3,3,3,4),(7.59274844815666,7.89168714724002,
8.87814804064502,9.86460893405003,10.851069827455,11.83753072086,12.823991614265,
13.81045250767,13.8759337553362),.UNSPECIFIED.);
#1113=B_SPLINE_CURVE_WITH_KNOTS('',3,(#59810,#59811,#59812,#59813,#59814,
#59815,#59816,#59817,#59818,#59819,#59820,#59821,#59822,#59823,#59824,#59825,
#59826,#59827,#59828,#59829,#59830,#59831,#59832,#59833,#59834,#59835,#59836,
#59837,#59838,#59839,#59840,#59841,#59842,#59843,#59844,#59845,#59846,#59847,
#59848,#59849,#59850,#59851,#59852,#59853,#59854,#59855,#59856,#59857,#59858,
#59859,#59860,#59861,#59862,#59863,#59864,#59865,#59866,#59867,#59868,#59869,
#59870,#59871,#59872,#59873,#59874,#59875,#59876,#59877,#59878,#59879,#59880,
#59881,#59882,#59883,#59884,#59885,#59886,#59887,#59888,#59889,#59890,#59891,
#59892,#59893,#59894,#59895,#59896,#59897),.UNSPECIFIED.,.F.,.F.,(4,3,3,
3,3,3,3,3,3,3,3,3,3,3,3,3,3,3,3,3,3,3,3,3,3,3,3,3,3,4),(0.,0.0297343797035864,
0.060120761877283,0.0891403097401323,0.114532414120125,0.120626668186271,
0.150381698992516,0.17997034368319,0.208047043957412,0.230390900373193,
0.234467387186734,0.263372265983406,0.292277144780078,0.32121640004702,
0.336017014955494,0.340284508571086,0.34459204647613,0.372696730262498,
0.400818675119593,0.428516484798209,0.439577058767134,0.445404835481582,
0.450327801888399,0.477288765031749,0.497473133419461,0.505236404100872,
0.511959471749983,0.53790833305976,0.558026238582597,0.56924861039945),
 .UNSPECIFIED.);
#1114=B_SPLINE_CURVE_WITH_KNOTS('',3,(#59900,#59901,#59902,#59903,#59904,
#59905,#59906,#59907,#59908,#59909,#59910,#59911,#59912,#59913,#59914,#59915,
#59916,#59917,#59918,#59919,#59920,#59921,#59922,#59923,#59924,#59925,#59926,
#59927,#59928,#59929,#59930,#59931,#59932,#59933,#59934,#59935,#59936,#59937,
#59938,#59939,#59940,#59941,#59942,#59943,#59944,#59945,#59946,#59947,#59948,
#59949,#59950,#59951,#59952,#59953,#59954,#59955,#59956,#59957,#59958,#59959,
#59960,#59961,#59962,#59963,#59964,#59965,#59966,#59967,#59968,#59969,#59970,
#59971,#59972,#59973,#59974,#59975,#59976,#59977,#59978,#59979,#59980,#59981,
#59982,#59983,#59984,#59985,#59986,#59987,#59988,#59989,#59990,#59991,#59992,
#59993),.UNSPECIFIED.,.F.,.F.,(4,3,3,3,3,3,3,3,3,3,3,3,3,3,3,3,3,3,3,3,
3,3,3,3,3,3,3,3,3,3,3,4),(-0.569248610399453,-0.543562558043411,-0.517250584660783,
-0.510351573265488,-0.504796629765234,-0.477730613871864,-0.456104856148543,
-0.448985761186696,-0.442526474182097,-0.414793258161359,-0.386635508597981,
-0.358697135593994,-0.34520398971682,-0.340863862860947,-0.336326730527656,
-0.307401056922635,-0.304724552085299,-0.276937944371136,-0.248514561286397,
-0.23265772508323,-0.228221590562879,-0.199230787763733,-0.169668272024871,
-0.139872989252767,-0.12408548320274,-0.117715318700335,-0.113354339820942,
-0.0828129568830819,-0.0522455401301121,-0.022270235741096,-0.0135729408525504,
0.),.UNSPECIFIED.);
#1115=B_SPLINE_CURVE_WITH_KNOTS('',3,(#59994,#59995,#59996,#59997,#59998,
#59999,#60000,#60001,#60002,#60003,#60004,#60005,#60006,#60007,#60008,#60009,
#60010,#60011,#60012,#60013,#60014,#60015,#60016,#60017,#60018,#60019,#60020,
#60021,#60022,#60023,#60024,#60025,#60026,#60027,#60028,#60029,#60030,#60031,
#60032,#60033,#60034,#60035,#60036,#60037,#60038,#60039,#60040,#60041,#60042,
#60043,#60044,#60045,#60046,#60047,#60048,#60049,#60050,#60051,#60052,#60053,
#60054,#60055,#60056,#60057,#60058,#60059,#60060,#60061,#60062,#60063,#60064,
#60065,#60066,#60067,#60068,#60069,#60070,#60071,#60072,#60073,#60074,#60075,
#60076,#60077,#60078,#60079,#60080,#60081,#60082,#60083,#60084,#60085,#60086,
#60087,#60088,#60089,#60090),.UNSPECIFIED.,.F.,.F.,(4,3,3,3,3,3,3,3,3,3,
3,3,3,3,3,3,3,3,3,3,3,3,3,3,3,3,3,3,3,3,3,3,4),(-0.566847306048093,-0.536658716403432,
-0.50605373953314,-0.497358803993733,-0.490469668716376,-0.460327091817824,
-0.43729948162817,-0.425273577512184,-0.420376587364543,-0.390957251202536,
-0.362079079161669,-0.333750895422636,-0.319339724142124,-0.312267998605923,
-0.308232630749578,-0.280241862158672,-0.276106210300586,-0.247648696044962,
-0.218090837421661,-0.209492455589693,-0.204737921056362,-0.200614185310069,
-0.172780910553805,-0.145025994944757,-0.117750394973387,-0.104429823984033,
-0.100024823328952,-0.0958388020470428,-0.0691739371857627,-0.0429558817167698,
-0.017514133983365,-0.0111858270585532,0.),.UNSPECIFIED.);
#1116=B_SPLINE_CURVE_WITH_KNOTS('',3,(#60092,#60093,#60094,#60095,#60096,
#60097,#60098,#60099,#60100,#60101,#60102),.UNSPECIFIED.,.F.,.F.,(4,1,1,
1,1,1,1,1,4),(15.7079632679489,15.8048324359278,16.7912933293328,17.7777542227378,
18.7642151161428,19.7506760095478,20.7371369029528,21.7235977963578,21.9911485751285),
 .UNSPECIFIED.);
#1117=B_SPLINE_CURVE_WITH_KNOTS('',3,(#60103,#60104,#60105,#60106,#60107,
#60108,#60109,#60110,#60111,#60112),.UNSPECIFIED.,.F.,.F.,(4,1,1,1,1,1,
1,4),(15.7079632679489,16.3713219137819,17.3577828071869,18.3442437005919,
19.3307045939969,20.3171654874019,21.3036263808069,21.9911485751285),
 .UNSPECIFIED.);
#1118=B_SPLINE_CURVE_WITH_KNOTS('',3,(#60337,#60338,#60339,#60340,#60341,
#60342,#60343,#60344,#60345,#60346,#60347,#60348,#60349,#60350,#60351,#60352,
#60353,#60354,#60355,#60356,#60357,#60358,#60359,#60360,#60361,#60362,#60363,
#60364,#60365,#60366,#60367,#60368,#60369,#60370,#60371,#60372,#60373,#60374,
#60375,#60376,#60377,#60378,#60379,#60380,#60381,#60382,#60383,#60384,#60385,
#60386,#60387,#60388,#60389,#60390,#60391,#60392,#60393,#60394,#60395,#60396,
#60397,#60398,#60399,#60400,#60401,#60402,#60403,#60404,#60405,#60406,#60407,
#60408,#60409,#60410,#60411,#60412,#60413,#60414,#60415,#60416,#60417,#60418,
#60419,#60420,#60421,#60422,#60423,#60424,#60425,#60426,#60427),
 .UNSPECIFIED.,.F.,.F.,(4,3,3,3,3,3,3,3,3,3,3,3,3,3,3,3,3,3,3,3,3,3,3,3,
3,3,3,3,3,3,4),(0.,0.0253755398454445,0.0514213153132464,0.077957584539944,
0.0899764747654525,0.096803871475702,0.102648438541228,0.129953427359202,
0.157705320199216,0.184206857431119,0.195897861719558,0.201348082731475,
0.206600886453667,0.235230947526492,0.263711469126827,0.291580359310597,
0.307939787194046,0.312151069047901,0.340175334720984,0.369258031218753,
0.398694002185391,0.41802365259294,0.423204309536776,0.428148753834381,
0.459444366737233,0.482916076414372,0.491343338637999,0.498388095452059,
0.528903290158942,0.553331205445788,0.566847306048063),.UNSPECIFIED.);
#1119=B_SPLINE_CURVE_WITH_KNOTS('',3,(#60428,#60429,#60430,#60431,#60432,
#60433,#60434,#60435,#60436,#60437,#60438,#60439,#60440,#60441,#60442,#60443,
#60444,#60445,#60446,#60447,#60448,#60449,#60450,#60451,#60452),
 .UNSPECIFIED.,.F.,.F.,(4,3,3,3,3,3,3,3,4),(-10.1321597128207,-9.86460893405002,
-8.87814804064502,-7.89168714724002,-6.90522625383502,-5.91876536043002,
-4.93230446702501,-3.94584357362001,-3.84897440564113),.UNSPECIFIED.);
#1120=B_SPLINE_CURVE_WITH_KNOTS('',3,(#60677,#60678,#60679,#60680,#60681,
#60682,#60683,#60684,#60685,#60686,#60687,#60688,#60689,#60690,#60691,#60692,
#60693,#60694,#60695,#60696,#60697,#60698,#60699,#60700,#60701),
 .UNSPECIFIED.,.F.,.F.,(4,3,3,3,3,3,3,3,4),(7.59274844815666,7.89168714724002,
8.87814804064503,9.86460893405003,10.851069827455,11.83753072086,12.823991614265,
13.81045250767,13.8759337553362),.UNSPECIFIED.);
#1121=B_SPLINE_CURVE_WITH_KNOTS('',3,(#60702,#60703,#60704,#60705,#60706,
#60707,#60708,#60709,#60710,#60711,#60712,#60713,#60714,#60715,#60716,#60717,
#60718,#60719,#60720,#60721,#60722,#60723,#60724,#60725,#60726,#60727,#60728,
#60729,#60730,#60731,#60732,#60733,#60734,#60735,#60736,#60737,#60738,#60739,
#60740,#60741,#60742,#60743,#60744,#60745,#60746,#60747,#60748,#60749,#60750,
#60751,#60752,#60753,#60754,#60755,#60756,#60757,#60758,#60759,#60760,#60761,
#60762,#60763,#60764,#60765,#60766,#60767,#60768,#60769,#60770,#60771,#60772,
#60773,#60774,#60775,#60776,#60777,#60778,#60779,#60780,#60781,#60782,#60783,
#60784,#60785,#60786,#60787,#60788,#60789),.UNSPECIFIED.,.F.,.F.,(4,3,3,
3,3,3,3,3,3,3,3,3,3,3,3,3,3,3,3,3,3,3,3,3,3,3,3,3,3,4),(0.,0.0297349244535721,
0.060121569348429,0.0891410162773849,0.114533032340221,0.120626667476319,
0.15038169425931,0.17997017941563,0.208046920756741,0.230390549968388,0.234466744960236,
0.263371944870156,0.292277144780076,0.321216417936983,0.336017031727334,
0.340284462229876,0.344592011030409,0.372696707961539,0.400818636707195,
0.428516289762568,0.439576354164994,0.44540318305,0.450327524863458,0.477288294894219,
0.497472780816313,0.505235740104314,0.511959381000542,0.537907915849272,
0.558026238582596,0.569248610399449),.UNSPECIFIED.);
#1122=B_SPLINE_CURVE_WITH_KNOTS('',3,(#60850,#60851,#60852,#60853,#60854,
#60855,#60856,#60857,#60858,#60859),.UNSPECIFIED.,.F.,.F.,(4,3,3,4),(-4.09293042013064,
-3.99009315480002,-2.99256986610002,-2.06773127522702),.UNSPECIFIED.);
#1123=B_SPLINE_CURVE_WITH_KNOTS('',3,(#60862,#60863,#60864,#60865,#60866,
#60867,#60868,#60869,#60870,#60871),.UNSPECIFIED.,.F.,.F.,(4,3,3,4),(0.,
0.49876164434999,0.997523288699981,1.11639350868703),.UNSPECIFIED.);
#1124=B_SPLINE_CURVE_WITH_KNOTS('',3,(#60876,#60877,#60878,#60879,#60880,
#60881,#60882,#60883,#60884,#60885,#60886,#60887,#60888,#60889,#60890,#60891,
#60892,#60893,#60894,#60895,#60896,#60897),.UNSPECIFIED.,.F.,.F.,(4,3,3,
3,3,3,3,4),(-10.3761157273102,-9.97523288700005,-8.97770959830005,-7.98018630960004,
-6.98266302090004,-5.98513973220003,-4.98761644350003,-4.09293042013064),
 .UNSPECIFIED.);
#1125=B_SPLINE_CURVE_WITH_KNOTS('',3,(#60898,#60899,#60900,#60901,#60902,
#60903,#60904,#60905,#60906,#60907,#60908,#60909,#60910,#60911,#60912,#60913,
#60914,#60915,#60916,#60917,#60918,#60919),.UNSPECIFIED.,.F.,.F.,(4,3,3,
3,3,3,3,4),(1.11639350868703,1.99504657739999,2.9925698661,3.9900931548,
4.98761644350001,5.98513973220002,6.98266302090003,7.39957881586659),
 .UNSPECIFIED.);
#1126=B_SPLINE_CURVE_WITH_KNOTS('',3,(#60924,#60925,#60926,#60927,#60928,
#60929,#60930,#60931,#60932,#60933,#60934,#60935,#60936,#60937,#60938,#60939,
#60940,#60941,#60942,#60943,#60944,#60945),.UNSPECIFIED.,.F.,.F.,(4,3,3,
3,3,3,3,4),(-16.6593010344898,-15.9603726192001,-14.9628493305001,-13.9653260418001,
-12.9678027531001,-11.9702794644001,-10.9727561757001,-10.3761157273102),
 .UNSPECIFIED.);
#1127=B_SPLINE_CURVE_WITH_KNOTS('',3,(#60946,#60947,#60948,#60949,#60950,
#60951,#60952,#60953,#60954,#60955,#60956,#60957,#60958,#60959,#60960,#60961,
#60962,#60963,#60964,#60965,#60966,#60967),.UNSPECIFIED.,.F.,.F.,(4,3,3,
3,3,3,3,4),(7.39957881586659,7.98018630960004,8.97770959830006,9.97523288700007,
10.9727561757001,11.9702794644001,12.9678027531001,13.6827641230462),
 .UNSPECIFIED.);
#1128=B_SPLINE_CURVE_WITH_KNOTS('',3,(#60972,#60973,#60974,#60975,#60976,
#60977,#60978,#60979,#60980,#60981,#60982,#60983,#60984,#60985,#60986,#60987,
#60988,#60989,#60990,#60991,#60992,#60993),.UNSPECIFIED.,.F.,.F.,(4,3,3,
3,3,3,3,4),(-22.9424863416694,-21.9455123514001,-20.9479890627001,-19.9504657740001,
-18.9529424853001,-17.9554191966001,-16.9578959079001,-16.6593010344898),
 .UNSPECIFIED.);
#1129=B_SPLINE_CURVE_WITH_KNOTS('',3,(#60994,#60995,#60996,#60997,#60998,
#60999,#61000,#61001,#61002,#61003,#61004,#61005,#61006,#61007,#61008,#61009,
#61010,#61011,#61012,#61013,#61014,#61015,#61016,#61017,#61018),
 .UNSPECIFIED.,.F.,.F.,(4,3,3,3,3,3,3,3,4),(13.6827641230462,13.9653260418001,
14.9628493305001,15.9603726192001,16.9578959079001,17.9554191966001,18.9529424853001,
19.9504657740001,19.9659494302258),.UNSPECIFIED.);
#1130=B_SPLINE_CURVE_WITH_KNOTS('',3,(#61023,#61024,#61025,#61026,#61027,
#61028,#61029,#61030,#61031,#61032,#61033,#61034,#61035,#61036,#61037,#61038,
#61039,#61040,#61041,#61042,#61043,#61044),.UNSPECIFIED.,.F.,.F.,(4,3,3,
3,3,3,3,4),(-29.225671648849,-28.9281753723002,-27.9306520836002,-26.9331287949001,
-25.9356055062001,-24.9380822175001,-23.9405589288001,-22.9424863416694),
 .UNSPECIFIED.);
#1131=B_SPLINE_CURVE_WITH_KNOTS('',3,(#61045,#61046,#61047,#61048,#61049,
#61050,#61051,#61052,#61053,#61054,#61055,#61056,#61057,#61058,#61059,#61060,
#61061,#61062,#61063,#61064,#61065,#61066),.UNSPECIFIED.,.F.,.F.,(4,3,3,
3,3,3,3,4),(19.9659494302258,20.9479890627001,21.9455123514001,22.9430356401001,
23.9405589288002,24.9380822175002,25.9356055062002,26.2491347374054),
 .UNSPECIFIED.);
#1132=B_SPLINE_CURVE_WITH_KNOTS('',3,(#61071,#61072,#61073,#61074,#61075,
#61076,#61077,#61078,#61079,#61080,#61081,#61082,#61083,#61084,#61085,#61086,
#61087,#61088,#61089,#61090,#61091,#61092),.UNSPECIFIED.,.F.,.F.,(4,3,3,
3,3,3,3,4),(-35.5088569560286,-34.9133151045002,-33.9157918158002,-32.9182685271002,
-31.9207452384002,-30.9232219497002,-29.9256986610002,-29.225671648849),
 .UNSPECIFIED.);
#1133=B_SPLINE_CURVE_WITH_KNOTS('',3,(#61093,#61094,#61095,#61096,#61097,
#61098,#61099,#61100,#61101,#61102,#61103,#61104,#61105,#61106,#61107,#61108,
#61109,#61110,#61111,#61112,#61113,#61114),.UNSPECIFIED.,.F.,.F.,(4,3,3,
3,3,3,3,4),(26.2491347374054,26.9331287949002,27.9306520836002,28.9281753723002,
29.9256986610002,30.9232219497002,31.9207452384002,32.532320044585),
 .UNSPECIFIED.);
#1134=B_SPLINE_CURVE_WITH_KNOTS('',3,(#61119,#61120,#61121,#61122,#61123,
#61124,#61125,#61126,#61127,#61128,#61129,#61130,#61131,#61132,#61133,#61134,
#61135,#61136,#61137,#61138,#61139,#61140),.UNSPECIFIED.,.F.,.F.,(4,3,3,
3,3,3,3,4),(-41.7920422632082,-40.8984548367002,-39.9009315480002,-38.9034082593002,
-37.9058849706002,-36.9083616819002,-35.9108383932002,-35.5088569560286),
 .UNSPECIFIED.);
#1135=B_SPLINE_CURVE_WITH_KNOTS('',3,(#61141,#61142,#61143,#61144,#61145,
#61146,#61147,#61148,#61149,#61150,#61151,#61152,#61153,#61154,#61155,#61156,
#61157,#61158,#61159,#61160,#61161,#61162),.UNSPECIFIED.,.F.,.F.,(4,3,3,
3,3,3,3,4),(32.532320044585,32.9182685271002,33.9157918158002,34.9133151045002,
35.9108383932002,36.9083616819002,37.9058849706002,38.8155053517645),
 .UNSPECIFIED.);
#1136=B_SPLINE_CURVE_WITH_KNOTS('',3,(#61167,#61168,#61169,#61170,#61171,
#61172,#61173,#61174,#61175,#61176,#61177,#61178,#61179,#61180,#61181,#61182,
#61183,#61184,#61185,#61186,#61187,#61188,#61189,#61190,#61191),
 .UNSPECIFIED.,.F.,.F.,(4,3,3,3,3,3,3,3,4),(-48.0752275703878,-47.8811178576003,
-46.8835945689003,-45.8860712802002,-44.8885479915002,-43.8910247028002,
-42.8935014141002,-41.8959781254002,-41.7920422632082),.UNSPECIFIED.);
#1137=B_SPLINE_CURVE_WITH_KNOTS('',3,(#61192,#61193,#61194,#61195,#61196,
#61197,#61198,#61199,#61200,#61201,#61202,#61203,#61204,#61205,#61206,#61207,
#61208,#61209,#61210,#61211,#61212,#61213,#61214,#61215,#61216),
 .UNSPECIFIED.,.F.,.F.,(4,3,3,3,3,3,3,3,4),(38.8155053517645,38.9034082593002,
39.9009315480002,40.8984548367002,41.8959781254002,42.8935014141002,43.8910247028003,
44.8885479915003,45.0986906589441),.UNSPECIFIED.);
#1138=B_SPLINE_CURVE_WITH_KNOTS('',3,(#61221,#61222,#61223,#61224,#61225,
#61226,#61227,#61228,#61229,#61230,#61231,#61232,#61233,#61234,#61235,#61236,
#61237,#61238,#61239,#61240,#61241,#61242),.UNSPECIFIED.,.F.,.F.,(4,3,3,
3,3,3,3,4),(-54.3584128775673,-53.8662575898003,-52.8687343011003,-51.8712110124003,
-50.8736877237003,-49.8761644350003,-48.8786411463003,-48.0752275703878),
 .UNSPECIFIED.);
#1139=B_SPLINE_CURVE_WITH_KNOTS('',3,(#61243,#61244,#61245,#61246,#61247,
#61248,#61249,#61250,#61251,#61252,#61253,#61254,#61255,#61256,#61257,#61258,
#61259,#61260,#61261,#61262,#61263,#61264),.UNSPECIFIED.,.F.,.F.,(4,3,3,
3,3,3,3,4),(45.0986906589441,45.8860712802003,46.8835945689003,47.8811178576003,
48.8786411463002,49.8761644350002,50.8736877237002,51.3818759661237),
 .UNSPECIFIED.);
#1140=B_SPLINE_CURVE_WITH_KNOTS('',3,(#61269,#61270,#61271,#61272,#61273,
#61274,#61275,#61276,#61277,#61278,#61279,#61280,#61281,#61282,#61283,#61284,
#61285,#61286,#61287,#61288,#61289,#61290),.UNSPECIFIED.,.F.,.F.,(4,3,3,
3,3,3,3,4),(-60.6415981847469,-59.8513973220003,-58.8538740333003,-57.8563507446003,
-56.8588274559003,-55.8613041672003,-54.8637808785003,-54.3584128775673),
 .UNSPECIFIED.);
#1141=B_SPLINE_CURVE_WITH_KNOTS('',3,(#61291,#61292,#61293,#61294,#61295,
#61296,#61297,#61298,#61299,#61300,#61301,#61302,#61303,#61304,#61305,#61306,
#61307,#61308,#61309,#61310,#61311,#61312),.UNSPECIFIED.,.F.,.F.,(4,3,3,
3,3,3,3,4),(51.3818759661237,51.8712110124002,52.8687343011003,53.8662575898003,
54.8637808785003,55.8613041672003,56.8588274559003,57.6650612733033),
 .UNSPECIFIED.);
#1142=B_SPLINE_CURVE_WITH_KNOTS('',3,(#61317,#61318,#61319,#61320,#61321,
#61322,#61323,#61324,#61325,#61326,#61327,#61328,#61329,#61330,#61331,#61332,
#61333,#61334,#61335,#61336,#61337,#61338,#61339,#61340,#61341),
 .UNSPECIFIED.,.F.,.F.,(4,3,3,3,3,3,3,3,4),(-66.9247834919265,-66.8340603429004,
-65.8365370542004,-64.8390137655004,-63.8414904768003,-62.8439671881003,
-61.8464438994003,-60.8489206107003,-60.6415981847469),.UNSPECIFIED.);
#1143=B_SPLINE_CURVE_WITH_KNOTS('',3,(#61342,#61343,#61344,#61345,#61346,
#61347,#61348,#61349,#61350,#61351,#61352,#61353,#61354,#61355,#61356,#61357,
#61358,#61359,#61360,#61361,#61362,#61363,#61364,#61365,#61366),
 .UNSPECIFIED.,.F.,.F.,(4,3,3,3,3,3,3,3,4),(57.6650612733033,57.8563507446003,
58.8538740333003,59.8513973220003,60.8489206107003,61.8464438994003,62.8439671881003,
63.8414904768003,63.9482465804829),.UNSPECIFIED.);
#1144=B_SPLINE_CURVE_WITH_KNOTS('',3,(#61371,#61372,#61373,#61374,#61375,
#61376,#61377,#61378,#61379,#61380,#61381,#61382,#61383,#61384,#61385,#61386,
#61387,#61388,#61389,#61390,#61391,#61392),.UNSPECIFIED.,.F.,.F.,(4,3,3,
3,3,3,3,4),(-73.2079687991061,-72.8192000751004,-71.8216767864004,-70.8241534977004,
-69.8266302090004,-68.8291069203004,-67.8315836316004,-66.9247834919265),
 .UNSPECIFIED.);
#1145=B_SPLINE_CURVE_WITH_KNOTS('',3,(#61393,#61394,#61395,#61396,#61397,
#61398,#61399,#61400,#61401,#61402,#61403,#61404,#61405,#61406,#61407,#61408,
#61409,#61410,#61411,#61412,#61413,#61414),.UNSPECIFIED.,.F.,.F.,(4,3,3,
3,3,3,3,4),(63.9482465804829,64.8390137655003,65.8365370542003,66.8340603429004,
67.8315836316004,68.8291069203004,69.8266302090004,70.2314318876625),
 .UNSPECIFIED.);
#1146=B_SPLINE_CURVE_WITH_KNOTS('',3,(#61419,#61420,#61421,#61422,#61423,
#61424,#61425,#61426,#61427,#61428,#61429,#61430,#61431,#61432,#61433,#61434,
#61435,#61436,#61437,#61438,#61439,#61440),.UNSPECIFIED.,.F.,.F.,(4,3,3,
3,3,3,3,4),(-79.4911541062857,-78.8043398073004,-77.8068165186004,-76.8092932299004,
-75.8117699412004,-74.8142466525004,-73.8167233638004,-73.2079687991061),
 .UNSPECIFIED.);
#1147=B_SPLINE_CURVE_WITH_KNOTS('',3,(#61441,#61442,#61443,#61444,#61445,
#61446,#61447,#61448,#61449,#61450,#61451,#61452,#61453,#61454,#61455,#61456,
#61457,#61458,#61459,#61460,#61461,#61462),.UNSPECIFIED.,.F.,.F.,(4,3,3,
3,3,3,3,4),(70.2314318876625,70.8241534977004,71.8216767864004,72.8192000751004,
73.8167233638004,74.8142466525004,75.8117699412004,76.5146171948421),
 .UNSPECIFIED.);
#1148=B_SPLINE_CURVE_WITH_KNOTS('',3,(#61467,#61468,#61469,#61470,#61471,
#61472,#61473,#61474,#61475,#61476,#61477,#61478,#61479,#61480,#61481,#61482,
#61483,#61484,#61485,#61486,#61487,#61488),.UNSPECIFIED.,.F.,.F.,(4,3,3,
3,3,3,3,4),(-85.7743394134653,-84.7894795395005,-83.7919562508005,-82.7944329621005,
-81.7969096734005,-80.7993863847005,-79.8018630960004,-79.4911541062857),
 .UNSPECIFIED.);
#1149=B_SPLINE_CURVE_WITH_KNOTS('',3,(#61489,#61490,#61491,#61492,#61493,
#61494,#61495,#61496,#61497,#61498,#61499,#61500,#61501,#61502,#61503,#61504,
#61505,#61506,#61507,#61508,#61509,#61510,#61511,#61512,#61513),
 .UNSPECIFIED.,.F.,.F.,(4,3,3,3,3,3,3,3,4),(76.5146171948421,76.8092932299004,
77.8068165186004,78.8043398073004,79.8018630960004,80.7993863847004,81.7969096734004,
82.7944329621005,82.7978025020217),.UNSPECIFIED.);
#1150=B_SPLINE_CURVE_WITH_KNOTS('',3,(#61518,#61519,#61520,#61521,#61522,
#61523,#61524,#61525,#61526,#61527,#61528,#61529,#61530,#61531,#61532,#61533,
#61534,#61535,#61536,#61537,#61538,#61539,#61540,#61541,#61542),
 .UNSPECIFIED.,.F.,.F.,(4,3,3,3,3,3,3,3,4),(-92.0575247206449,-91.7721425604005,
-90.7746192717005,-89.7770959830005,-88.7795726943005,-87.7820494056005,
-86.7845261169005,-85.7870028282005,-85.7743394134653),.UNSPECIFIED.);
#1151=B_SPLINE_CURVE_WITH_KNOTS('',3,(#61543,#61544,#61545,#61546,#61547,
#61548,#61549,#61550,#61551,#61552,#61553,#61554,#61555,#61556,#61557,#61558,
#61559,#61560,#61561,#61562,#61563,#61564),.UNSPECIFIED.,.F.,.F.,(4,3,3,
3,3,3,3,4),(82.7978025020217,83.7919562508005,84.7894795395004,85.7870028282005,
86.7845261169005,87.7820494056005,88.7795726943005,89.0809878092013),
 .UNSPECIFIED.);
#1152=B_SPLINE_CURVE_WITH_KNOTS('',3,(#61569,#61570,#61571,#61572,#61573,
#61574,#61575,#61576,#61577,#61578,#61579,#61580,#61581,#61582,#61583,#61584,
#61585,#61586,#61587,#61588,#61589,#61590),.UNSPECIFIED.,.F.,.F.,(4,3,3,
3,3,3,3,4),(-98.3407100278245,-97.7572822926005,-96.7597590039005,-95.7622357152005,
-94.7647124265005,-93.7671891378005,-92.7696658491005,-92.0575247206449),
 .UNSPECIFIED.);
#1153=B_SPLINE_CURVE_WITH_KNOTS('',3,(#61591,#61592,#61593,#61594,#61595,
#61596,#61597,#61598,#61599,#61600,#61601,#61602,#61603,#61604,#61605,#61606,
#61607,#61608,#61609,#61610,#61611,#61612),.UNSPECIFIED.,.F.,.F.,(4,3,3,
3,3,3,3,4),(89.0809878092013,89.7770959830005,90.7746192717005,91.7721425604005,
92.7696658491005,93.7671891378005,94.7647124265005,95.3641731163809),
 .UNSPECIFIED.);
#1154=B_SPLINE_CURVE_WITH_KNOTS('',3,(#61617,#61618,#61619,#61620,#61621,
#61622,#61623,#61624,#61625,#61626,#61627,#61628,#61629,#61630,#61631,#61632,
#61633,#61634,#61635,#61636,#61637,#61638),.UNSPECIFIED.,.F.,.F.,(4,3,3,
3,3,3,3,4),(-104.623895335004,-103.742422024801,-102.744898736101,-101.747375447401,
-100.749852158701,-99.7523288700005,-98.7548055813005,-98.3407100278245),
 .UNSPECIFIED.);
#1155=B_SPLINE_CURVE_WITH_KNOTS('',3,(#61639,#61640,#61641,#61642,#61643,
#61644,#61645,#61646,#61647,#61648,#61649,#61650,#61651,#61652,#61653,#61654,
#61655,#61656,#61657,#61658,#61659,#61660),.UNSPECIFIED.,.F.,.F.,(4,3,3,
3,3,3,3,4),(95.3641731163809,95.7622357152005,96.7597590039006,97.7572822926005,
98.7548055813005,99.7523288700006,100.749852158701,101.647358423561),
 .UNSPECIFIED.);
#1156=B_SPLINE_CURVE_WITH_KNOTS('',3,(#61665,#61666,#61667,#61668,#61669,
#61670,#61671,#61672,#61673,#61674,#61675,#61676,#61677,#61678,#61679,#61680,
#61681,#61682,#61683,#61684,#61685,#61686,#61687,#61688,#61689),
 .UNSPECIFIED.,.F.,.F.,(4,3,3,3,3,3,3,3,4),(-110.907080642184,-110.725085045701,
-109.727561757001,-108.730038468301,-107.732515179601,-106.734991890901,
-105.737468602201,-104.739945313501,-104.623895335004),.UNSPECIFIED.);
#1157=B_SPLINE_CURVE_WITH_KNOTS('',3,(#61690,#61691,#61692,#61693,#61694,
#61695,#61696,#61697,#61698,#61699,#61700,#61701,#61702,#61703,#61704,#61705,
#61706,#61707,#61708,#61709,#61710,#61711,#61712,#61713,#61714),
 .UNSPECIFIED.,.F.,.F.,(4,3,3,3,3,3,3,3,4),(101.647358423561,101.747375447401,
102.744898736101,103.742422024801,104.739945313501,105.737468602201,106.734991890901,
107.732515179601,107.93054373074),.UNSPECIFIED.);
#1158=B_SPLINE_CURVE_WITH_KNOTS('',3,(#61719,#61720,#61721,#61722,#61723,
#61724,#61725,#61726,#61727,#61728,#61729,#61730,#61731,#61732,#61733,#61734,
#61735,#61736,#61737,#61738,#61739,#61740),.UNSPECIFIED.,.F.,.F.,(4,3,3,
3,3,3,3,4),(-117.190265949363,-116.710224777901,-115.712701489201,-114.715178200501,
-113.717654911801,-112.720131623101,-111.722608334401,-110.907080642184),
 .UNSPECIFIED.);
#1159=B_SPLINE_CURVE_WITH_KNOTS('',3,(#61741,#61742,#61743,#61744,#61745,
#61746,#61747,#61748,#61749,#61750,#61751,#61752,#61753,#61754,#61755,#61756,
#61757,#61758,#61759,#61760,#61761,#61762),.UNSPECIFIED.,.F.,.F.,(4,3,3,
3,3,3,3,4),(107.93054373074,108.730038468301,109.727561757001,110.725085045701,
111.722608334401,112.720131623101,113.717654911801,114.21372903792),
 .UNSPECIFIED.);
#1160=B_SPLINE_CURVE_WITH_KNOTS('',3,(#61767,#61768,#61769,#61770,#61771,
#61772,#61773,#61774,#61775,#61776,#61777,#61778,#61779,#61780,#61781,#61782,
#61783,#61784,#61785,#61786,#61787,#61788),.UNSPECIFIED.,.F.,.F.,(4,3,3,
3,3,3,3,4),(-123.473451256543,-122.695364510101,-121.697841221401,-120.700317932701,
-119.702794644001,-118.705271355301,-117.707748066601,-117.190265949363),
 .UNSPECIFIED.);
#1161=B_SPLINE_CURVE_WITH_KNOTS('',3,(#61789,#61790,#61791,#61792,#61793,
#61794,#61795,#61796,#61797,#61798,#61799,#61800,#61801,#61802,#61803,#61804,
#61805,#61806,#61807,#61808,#61809,#61810),.UNSPECIFIED.,.F.,.F.,(4,3,3,
3,3,3,3,4),(114.21372903792,114.715178200501,115.712701489201,116.710224777901,
117.707748066601,118.705271355301,119.702794644001,120.496914345099),
 .UNSPECIFIED.);
#1162=B_SPLINE_CURVE_WITH_KNOTS('',3,(#61815,#61816,#61817,#61818,#61819,
#61820,#61821,#61822,#61823,#61824,#61825,#61826,#61827,#61828,#61829,#61830,
#61831,#61832,#61833,#61834,#61835,#61836,#61837,#61838,#61839),
 .UNSPECIFIED.,.F.,.F.,(4,3,3,3,3,3,3,3,4),(-129.756636563722,-129.678027531001,
-128.680504242301,-127.682980953601,-126.685457664901,-125.687934376201,
-124.690411087501,-123.692887798801,-123.473451256543),.UNSPECIFIED.);
#1163=B_SPLINE_CURVE_WITH_KNOTS('',3,(#61840,#61841,#61842,#61843,#61844,
#61845,#61846,#61847,#61848,#61849,#61850,#61851,#61852,#61853,#61854,#61855,
#61856,#61857,#61858,#61859,#61860,#61861,#61862,#61863,#61864),
 .UNSPECIFIED.,.F.,.F.,(4,3,3,3,3,3,3,3,4),(120.496914345099,120.700317932701,
121.697841221401,122.695364510101,123.692887798801,124.690411087501,125.687934376201,
126.685457664901,126.780099652279),.UNSPECIFIED.);
#1164=B_SPLINE_CURVE_WITH_KNOTS('',3,(#61869,#61870,#61871,#61872,#61873,
#61874,#61875,#61876,#61877,#61878,#61879,#61880,#61881,#61882,#61883,#61884,
#61885,#61886,#61887,#61888,#61889,#61890),.UNSPECIFIED.,.F.,.F.,(4,3,3,
3,3,3,3,4),(-136.039821870902,-135.663167263201,-134.665643974501,-133.668120685801,
-132.670597397101,-131.673074108401,-130.675550819701,-129.756636563722),
 .UNSPECIFIED.);
#1165=B_SPLINE_CURVE_WITH_KNOTS('',3,(#61891,#61892,#61893,#61894,#61895,
#61896,#61897,#61898,#61899,#61900,#61901,#61902,#61903,#61904,#61905,#61906,
#61907,#61908,#61909,#61910,#61911,#61912),.UNSPECIFIED.,.F.,.F.,(4,3,3,
3,3,3,3,4),(126.780099652279,127.682980953601,128.680504242301,129.678027531001,
130.675550819701,131.673074108401,132.670597397101,133.063284959458),
 .UNSPECIFIED.);
#1166=B_SPLINE_CURVE_WITH_KNOTS('',3,(#61917,#61918,#61919,#61920,#61921,
#61922,#61923,#61924,#61925,#61926,#61927,#61928,#61929,#61930,#61931,#61932,
#61933,#61934,#61935,#61936,#61937,#61938),.UNSPECIFIED.,.F.,.F.,(4,3,3,
3,3,3,3,4),(-142.323007178082,-141.648306995401,-140.650783706701,-139.653260418001,
-138.655737129301,-137.658213840601,-136.660690551901,-136.039821870902),
 .UNSPECIFIED.);
#1167=B_SPLINE_CURVE_WITH_KNOTS('',3,(#61939,#61940,#61941,#61942,#61943,
#61944,#61945,#61946,#61947,#61948,#61949,#61950,#61951,#61952,#61953,#61954,
#61955,#61956,#61957,#61958,#61959,#61960),.UNSPECIFIED.,.F.,.F.,(4,3,3,
3,3,3,3,4),(133.063284959458,133.668120685801,134.665643974501,135.663167263201,
136.660690551901,137.658213840601,138.655737129301,139.346470266638),
 .UNSPECIFIED.);
#1168=B_SPLINE_CURVE_WITH_KNOTS('',3,(#61965,#61966,#61967,#61968,#61969,
#61970,#61971,#61972,#61973,#61974,#61975,#61976,#61977,#61978,#61979,#61980,
#61981,#61982,#61983,#61984,#61985,#61986),.UNSPECIFIED.,.F.,.F.,(4,3,3,
3,3,3,3,4),(-148.606192485261,-147.633446727601,-146.635923438901,-145.638400150201,
-144.640876861501,-143.643353572801,-142.645830284101,-142.323007178082),
 .UNSPECIFIED.);
#1169=B_SPLINE_CURVE_WITH_KNOTS('',3,(#61987,#61988,#61989,#61990,#61991,
#61992,#61993,#61994,#61995,#61996,#61997,#61998,#61999,#62000,#62001,#62002,
#62003,#62004,#62005,#62006,#62007,#62008),.UNSPECIFIED.,.F.,.F.,(4,3,3,
3,3,3,3,4),(139.346470266638,139.653260418001,140.650783706701,141.648306995401,
142.645830284101,143.643353572801,144.640876861501,145.629655573818),
 .UNSPECIFIED.);
#1170=B_SPLINE_CURVE_WITH_KNOTS('',3,(#62013,#62014,#62015,#62016,#62017,
#62018,#62019,#62020,#62021,#62022,#62023,#62024,#62025,#62026,#62027,#62028,
#62029,#62030,#62031,#62032,#62033,#62034,#62035,#62036,#62037),
 .UNSPECIFIED.,.F.,.F.,(4,3,3,3,3,3,3,3,4),(-154.889377792441,-154.616109748501,
-153.618586459801,-152.621063171101,-151.623539882401,-150.626016593701,
-149.628493305001,-148.630970016301,-148.606192485261),.UNSPECIFIED.);
#1171=B_SPLINE_CURVE_WITH_KNOTS('',3,(#62038,#62039,#62040,#62041,#62042,
#62043,#62044,#62045,#62046,#62047,#62048,#62049,#62050,#62051,#62052,#62053,
#62054,#62055,#62056,#62057,#62058,#62059,#62060,#62061,#62062),
 .UNSPECIFIED.,.F.,.F.,(4,3,3,3,3,3,3,3,4),(145.629655573818,145.638400150201,
146.635923438901,147.633446727601,148.630970016301,149.628493305001,150.626016593701,
151.623539882401,151.912840880997),.UNSPECIFIED.);
#1172=B_SPLINE_CURVE_WITH_KNOTS('',3,(#62067,#62068,#62069,#62070,#62071,
#62072,#62073,#62074,#62075,#62076,#62077,#62078,#62079,#62080,#62081,#62082,
#62083,#62084,#62085,#62086,#62087,#62088),.UNSPECIFIED.,.F.,.F.,(4,3,3,
3,3,3,3,4),(-161.17256309962,-160.601249480701,-159.603726192001,-158.606202903301,
-157.608679614601,-156.611156325901,-155.613633037201,-154.889377792441),
 .UNSPECIFIED.);
#1173=B_SPLINE_CURVE_WITH_KNOTS('',3,(#62089,#62090,#62091,#62092,#62093,
#62094,#62095,#62096,#62097,#62098,#62099,#62100,#62101,#62102,#62103,#62104,
#62105,#62106,#62107,#62108,#62109,#62110),.UNSPECIFIED.,.F.,.F.,(4,3,3,
3,3,3,3,4),(151.912840880997,152.621063171101,153.618586459801,154.616109748501,
155.613633037201,156.611156325901,157.608679614601,158.196026188177),
 .UNSPECIFIED.);
#1174=B_SPLINE_CURVE_WITH_KNOTS('',3,(#62115,#62116,#62117,#62118,#62119,
#62120,#62121,#62122,#62123,#62124,#62125,#62126,#62127,#62128,#62129,#62130,
#62131,#62132,#62133,#62134,#62135,#62136),.UNSPECIFIED.,.F.,.F.,(4,3,3,
3,3,3,3,4),(-167.4557484068,-166.586389212901,-165.588865924201,-164.591342635501,
-163.593819346801,-162.596296058101,-161.598772769401,-161.17256309962),
 .UNSPECIFIED.);
#1175=B_SPLINE_CURVE_WITH_KNOTS('',3,(#62137,#62138,#62139,#62140,#62141,
#62142,#62143,#62144,#62145,#62146,#62147,#62148,#62149,#62150,#62151,#62152,
#62153,#62154,#62155,#62156,#62157,#62158),.UNSPECIFIED.,.F.,.F.,(4,3,3,
3,3,3,3,4),(158.196026188177,158.606202903301,159.603726192001,160.601249480701,
161.598772769401,162.596296058101,163.593819346801,164.479211495356),
 .UNSPECIFIED.);
#1176=B_SPLINE_CURVE_WITH_KNOTS('',3,(#62163,#62164,#62165,#62166,#62167,
#62168,#62169,#62170,#62171,#62172,#62173,#62174,#62175,#62176,#62177,#62178,
#62179,#62180,#62181,#62182,#62183,#62184,#62185,#62186,#62187),
 .UNSPECIFIED.,.F.,.F.,(4,3,3,3,3,3,3,3,4),(-173.738933713979,-173.569052233801,
-172.571528945101,-171.574005656401,-170.576482367701,-169.578959079001,
-168.581435790301,-167.583912501601,-167.4557484068),.UNSPECIFIED.);
#1177=B_SPLINE_CURVE_WITH_KNOTS('',3,(#62188,#62189,#62190,#62191,#62192,
#62193,#62194,#62195,#62196,#62197,#62198,#62199,#62200,#62201,#62202,#62203,
#62204,#62205,#62206,#62207,#62208,#62209,#62210,#62211,#62212),
 .UNSPECIFIED.,.F.,.F.,(4,3,3,3,3,3,3,3,4),(164.479211495356,164.591342635501,
165.588865924201,166.586389212901,167.583912501601,168.581435790301,169.578959079001,
170.576482367701,170.762396802536),.UNSPECIFIED.);
#1178=B_SPLINE_CURVE_WITH_KNOTS('',3,(#62217,#62218,#62219,#62220,#62221,
#62222,#62223,#62224,#62225,#62226,#62227,#62228,#62229,#62230,#62231,#62232,
#62233,#62234,#62235,#62236,#62237,#62238),.UNSPECIFIED.,.F.,.F.,(4,3,3,
3,3,3,3,4),(-180.022119021159,-179.554191966001,-178.556668677301,-177.559145388601,
-176.561622099901,-175.564098811201,-174.566575522501,-173.738933713979),
 .UNSPECIFIED.);
#1179=B_SPLINE_CURVE_WITH_KNOTS('',3,(#62239,#62240,#62241,#62242,#62243,
#62244,#62245,#62246,#62247,#62248,#62249,#62250,#62251,#62252,#62253,#62254,
#62255,#62256,#62257,#62258,#62259,#62260),.UNSPECIFIED.,.F.,.F.,(4,3,3,
3,3,3,3,4),(170.762396802536,171.574005656401,172.571528945101,173.569052233801,
174.566575522501,175.564098811201,176.561622099901,177.045582109715),
 .UNSPECIFIED.);
#1180=B_SPLINE_CURVE_WITH_KNOTS('',3,(#62265,#62266,#62267,#62268,#62269,
#62270,#62271,#62272,#62273,#62274,#62275,#62276,#62277,#62278,#62279,#62280,
#62281,#62282,#62283,#62284,#62285,#62286),.UNSPECIFIED.,.F.,.F.,(4,3,3,
3,3,3,3,4),(-186.305304328338,-185.539331698201,-184.541808409501,-183.544285120801,
-182.546761832101,-181.549238543401,-180.551715254701,-180.022119021159),
 .UNSPECIFIED.);
#1181=B_SPLINE_CURVE_WITH_KNOTS('',3,(#62287,#62288,#62289,#62290,#62291,
#62292,#62293,#62294,#62295,#62296,#62297,#62298,#62299,#62300,#62301,#62302,
#62303,#62304,#62305,#62306,#62307,#62308),.UNSPECIFIED.,.F.,.F.,(4,3,3,
3,3,3,3,4),(177.045582109715,177.559145388601,178.556668677301,179.554191966001,
180.551715254701,181.549238543401,182.546761832101,183.328767416895),
 .UNSPECIFIED.);
#1182=B_SPLINE_CURVE_WITH_KNOTS('',3,(#62313,#62314,#62315,#62316,#62317,
#62318,#62319,#62320,#62321,#62322,#62323,#62324,#62325,#62326,#62327,#62328,
#62329,#62330,#62331,#62332,#62333,#62334,#62335,#62336,#62337),
 .UNSPECIFIED.,.F.,.F.,(4,3,3,3,3,3,3,3,4),(-192.588489635518,-192.521994719101,
-191.524471430401,-190.526948141701,-189.529424853001,-188.531901564301,
-187.534378275601,-186.536854986901,-186.305304328338),.UNSPECIFIED.);
#1183=B_SPLINE_CURVE_WITH_KNOTS('',3,(#62338,#62339,#62340,#62341,#62342,
#62343,#62344,#62345,#62346,#62347,#62348,#62349,#62350,#62351,#62352,#62353,
#62354,#62355,#62356,#62357,#62358,#62359,#62360,#62361,#62362),
 .UNSPECIFIED.,.F.,.F.,(4,3,3,3,3,3,3,3,4),(183.328767416895,183.544285120801,
184.541808409501,185.539331698201,186.536854986901,187.534378275601,188.531901564301,
189.529424853001,189.611952724075),.UNSPECIFIED.);
#1184=B_SPLINE_CURVE_WITH_KNOTS('',3,(#62367,#62368,#62369,#62370,#62371,
#62372,#62373,#62374,#62375,#62376,#62377,#62378,#62379,#62380,#62381,#62382,
#62383,#62384,#62385,#62386,#62387,#62388),.UNSPECIFIED.,.F.,.F.,(4,3,3,
3,3,3,3,4),(-198.871674942698,-198.507134451301,-197.509611162601,-196.512087873901,
-195.514564585201,-194.517041296501,-193.519518007801,-192.588489635518),
 .UNSPECIFIED.);
#1185=B_SPLINE_CURVE_WITH_KNOTS('',3,(#62389,#62390,#62391,#62392,#62393,
#62394,#62395,#62396,#62397,#62398,#62399,#62400,#62401,#62402,#62403,#62404,
#62405,#62406,#62407,#62408,#62409,#62410),.UNSPECIFIED.,.F.,.F.,(4,3,3,
3,3,3,3,4),(189.611952724075,190.526948141701,191.524471430401,192.521994719101,
193.519518007801,194.517041296501,195.514564585201,195.895138031254),
 .UNSPECIFIED.);
#1186=B_SPLINE_CURVE_WITH_KNOTS('',3,(#62415,#62416,#62417,#62418,#62419,
#62420,#62421,#62422,#62423,#62424,#62425,#62426,#62427,#62428,#62429,#62430,
#62431,#62432,#62433,#62434,#62435,#62436),.UNSPECIFIED.,.F.,.F.,(4,3,3,
3,3,3,3,4),(-205.154860249877,-204.492274183501,-203.494750894801,-202.497227606101,
-201.499704317401,-200.502181028701,-199.504657740001,-198.871674942698),
 .UNSPECIFIED.);
#1187=B_SPLINE_CURVE_WITH_KNOTS('',3,(#62437,#62438,#62439,#62440,#62441,
#62442,#62443,#62444,#62445,#62446,#62447,#62448,#62449,#62450,#62451,#62452,
#62453,#62454,#62455,#62456,#62457,#62458),.UNSPECIFIED.,.F.,.F.,(4,3,3,
3,3,3,3,4),(195.895138031254,196.512087873901,197.509611162601,198.507134451301,
199.504657740001,200.502181028701,201.499704317401,202.178323338434),
 .UNSPECIFIED.);
#1188=B_SPLINE_CURVE_WITH_KNOTS('',3,(#62463,#62464,#62465,#62466,#62467,
#62468,#62469,#62470,#62471,#62472,#62473,#62474,#62475,#62476,#62477,#62478,
#62479,#62480,#62481,#62482,#62483,#62484),.UNSPECIFIED.,.F.,.F.,(4,3,3,
3,3,3,3,4),(-211.438045557057,-210.477413915701,-209.479890627001,-208.482367338301,
-207.484844049601,-206.487320760901,-205.489797472201,-205.154860249877),
 .UNSPECIFIED.);
#1189=B_SPLINE_CURVE_WITH_KNOTS('',3,(#62485,#62486,#62487,#62488,#62489,
#62490,#62491,#62492,#62493,#62494,#62495,#62496,#62497,#62498,#62499,#62500,
#62501,#62502,#62503,#62504,#62505,#62506),.UNSPECIFIED.,.F.,.F.,(4,3,3,
3,3,3,3,4),(202.178323338434,202.497227606101,203.494750894801,204.492274183501,
205.489797472201,206.487320760901,207.484844049601,208.461508645613),
 .UNSPECIFIED.);
#1190=B_SPLINE_CURVE_WITH_KNOTS('',3,(#62511,#62512,#62513,#62514,#62515,
#62516,#62517,#62518,#62519,#62520,#62521,#62522,#62523,#62524,#62525,#62526,
#62527,#62528,#62529,#62530,#62531,#62532,#62533,#62534,#62535),
 .UNSPECIFIED.,.F.,.F.,(4,3,3,3,3,3,3,3,4),(-217.721230864236,-217.460076936601,
-216.462553647901,-215.465030359201,-214.467507070501,-213.469983781801,
-212.472460493101,-211.474937204401,-211.438045557057),.UNSPECIFIED.);
#1191=B_SPLINE_CURVE_WITH_KNOTS('',3,(#62536,#62537,#62538,#62539,#62540,
#62541,#62542,#62543,#62544,#62545,#62546,#62547,#62548,#62549,#62550,#62551,
#62552,#62553,#62554,#62555,#62556,#62557,#62558,#62559,#62560),
 .UNSPECIFIED.,.F.,.F.,(4,3,3,3,3,3,3,3,4),(208.461508645613,208.482367338301,
209.479890627001,210.477413915701,211.474937204401,212.472460493101,213.469983781801,
214.467507070501,214.744693952793),.UNSPECIFIED.);
#1192=B_SPLINE_CURVE_WITH_KNOTS('',3,(#62565,#62566,#62567,#62568,#62569,
#62570,#62571,#62572,#62573,#62574,#62575,#62576,#62577,#62578,#62579,#62580,
#62581,#62582,#62583,#62584,#62585,#62586),.UNSPECIFIED.,.F.,.F.,(4,3,3,
3,3,3,3,4),(-224.004416171416,-223.445216668801,-222.447693380101,-221.450170091401,
-220.452646802701,-219.455123514001,-218.457600225301,-217.721230864236),
 .UNSPECIFIED.);
#1193=B_SPLINE_CURVE_WITH_KNOTS('',3,(#62587,#62588,#62589,#62590,#62591,
#62592,#62593,#62594,#62595,#62596,#62597,#62598,#62599,#62600,#62601,#62602,
#62603,#62604,#62605,#62606,#62607,#62608),.UNSPECIFIED.,.F.,.F.,(4,3,3,
3,3,3,3,4),(214.744693952793,215.465030359201,216.462553647901,217.460076936601,
218.457600225301,219.455123514001,220.452646802701,221.027879259972),
 .UNSPECIFIED.);
#1194=B_SPLINE_CURVE_WITH_KNOTS('',3,(#62613,#62614,#62615,#62616,#62617,
#62618,#62619,#62620,#62621,#62622,#62623,#62624,#62625,#62626,#62627,#62628,
#62629,#62630,#62631,#62632,#62633,#62634),.UNSPECIFIED.,.F.,.F.,(4,3,3,
3,3,3,3,4),(-230.287601478595,-229.430356401001,-228.432833112301,-227.435309823601,
-226.437786534901,-225.440263246201,-224.442739957501,-224.004416171416),
 .UNSPECIFIED.);
#1195=B_SPLINE_CURVE_WITH_KNOTS('',3,(#62635,#62636,#62637,#62638,#62639,
#62640,#62641,#62642,#62643,#62644,#62645,#62646,#62647,#62648,#62649,#62650,
#62651,#62652,#62653,#62654,#62655,#62656),.UNSPECIFIED.,.F.,.F.,(4,3,3,
3,3,3,3,4),(221.027879259972,221.450170091401,222.447693380101,223.445216668801,
224.442739957501,225.440263246201,226.437786534901,227.311064567152),
 .UNSPECIFIED.);
#1196=B_SPLINE_CURVE_WITH_KNOTS('',3,(#62661,#62662,#62663,#62664,#62665,
#62666,#62667,#62668,#62669,#62670,#62671,#62672,#62673,#62674,#62675,#62676,
#62677,#62678,#62679,#62680,#62681,#62682,#62683,#62684,#62685),
 .UNSPECIFIED.,.F.,.F.,(4,3,3,3,3,3,3,3,4),(-236.570786785775,-236.413019421901,
-235.415496133201,-234.417972844501,-233.420449555801,-232.422926267101,
-231.425402978401,-230.427879689701,-230.287601478595),.UNSPECIFIED.);
#1197=B_SPLINE_CURVE_WITH_KNOTS('',3,(#62686,#62687,#62688,#62689,#62690,
#62691,#62692,#62693,#62694,#62695,#62696,#62697,#62698,#62699,#62700,#62701,
#62702,#62703,#62704,#62705,#62706,#62707,#62708,#62709,#62710),
 .UNSPECIFIED.,.F.,.F.,(4,3,3,3,3,3,3,3,4),(227.311064567152,227.435309823601,
228.432833112301,229.430356401001,230.427879689701,231.425402978401,232.422926267101,
233.420449555801,233.594249874331),.UNSPECIFIED.);
#1198=B_SPLINE_CURVE_WITH_KNOTS('',3,(#62715,#62716,#62717,#62718,#62719,
#62720,#62721,#62722,#62723,#62724,#62725,#62726,#62727,#62728,#62729,#62730,
#62731,#62732,#62733,#62734,#62735,#62736),.UNSPECIFIED.,.F.,.F.,(4,3,3,
3,3,3,3,4),(-242.853972092955,-242.398159154101,-241.400635865401,-240.403112576701,
-239.405589288001,-238.408065999301,-237.410542710601,-236.570786785775),
 .UNSPECIFIED.);
#1199=B_SPLINE_CURVE_WITH_KNOTS('',3,(#62737,#62738,#62739,#62740,#62741,
#62742,#62743,#62744,#62745,#62746,#62747,#62748,#62749,#62750,#62751,#62752,
#62753,#62754,#62755,#62756,#62757,#62758),.UNSPECIFIED.,.F.,.F.,(4,3,3,
3,3,3,3,4),(233.594249874331,234.417972844501,235.415496133201,236.413019421901,
237.410542710601,238.408065999301,239.405589288001,239.877435181511),
 .UNSPECIFIED.);
#1200=B_SPLINE_CURVE_WITH_KNOTS('',3,(#62763,#62764,#62765,#62766,#62767,
#62768,#62769,#62770,#62771,#62772,#62773,#62774,#62775,#62776,#62777,#62778,
#62779,#62780,#62781,#62782,#62783,#62784),.UNSPECIFIED.,.F.,.F.,(4,3,3,
3,3,3,3,4),(-249.137157400134,-248.383298886301,-247.385775597601,-246.388252308901,
-245.390729020201,-244.393205731501,-243.395682442801,-242.853972092955),
 .UNSPECIFIED.);
#1201=B_SPLINE_CURVE_WITH_KNOTS('',3,(#62785,#62786,#62787,#62788,#62789,
#62790,#62791,#62792,#62793,#62794,#62795,#62796,#62797,#62798,#62799,#62800,
#62801,#62802,#62803,#62804,#62805,#62806),.UNSPECIFIED.,.F.,.F.,(4,3,3,
3,3,3,3,4),(239.877435181511,240.403112576701,241.400635865401,242.398159154101,
243.395682442801,244.393205731501,245.390729020201,246.160620488691),
 .UNSPECIFIED.);
#1202=B_SPLINE_CURVE_WITH_KNOTS('',3,(#62811,#62812,#62813,#62814,#62815,
#62816,#62817,#62818,#62819,#62820,#62821,#62822,#62823,#62824,#62825,#62826,
#62827,#62828,#62829,#62830,#62831,#62832,#62833,#62834,#62835),
 .UNSPECIFIED.,.F.,.F.,(4,3,3,3,3,3,3,3,4),(-255.420342707314,-255.365961907201,
-254.368438618501,-253.370915329801,-252.373392041101,-251.375868752401,
-250.378345463701,-249.380822175001,-249.137157400134),.UNSPECIFIED.);
#1203=B_SPLINE_CURVE_WITH_KNOTS('',3,(#62836,#62837,#62838,#62839,#62840,
#62841,#62842,#62843,#62844,#62845,#62846,#62847,#62848,#62849,#62850,#62851,
#62852,#62853,#62854,#62855,#62856,#62857,#62858,#62859,#62860),
 .UNSPECIFIED.,.F.,.F.,(4,3,3,3,3,3,3,3,4),(246.160620488691,246.388252308901,
247.385775597601,248.383298886301,249.380822175001,250.378345463701,251.375868752401,
252.373392041101,252.44380579587),.UNSPECIFIED.);
#1204=B_SPLINE_CURVE_WITH_KNOTS('',3,(#62865,#62866,#62867,#62868,#62869,
#62870,#62871,#62872,#62873,#62874,#62875,#62876,#62877,#62878,#62879,#62880,
#62881,#62882,#62883,#62884,#62885,#62886),.UNSPECIFIED.,.F.,.F.,(4,3,3,
3,3,3,3,4),(-261.703528014493,-261.351101639401,-260.353578350701,-259.356055062001,
-258.358531773301,-257.361008484601,-256.363485195901,-255.420342707314),
 .UNSPECIFIED.);
#1205=B_SPLINE_CURVE_WITH_KNOTS('',3,(#62887,#62888,#62889,#62890,#62891,
#62892,#62893,#62894,#62895,#62896,#62897,#62898,#62899,#62900,#62901,#62902,
#62903,#62904,#62905,#62906,#62907,#62908),.UNSPECIFIED.,.F.,.F.,(4,3,3,
3,3,3,3,4),(252.44380579587,253.370915329801,254.368438618501,255.365961907201,
256.363485195901,257.361008484601,258.358531773301,258.72699110305),
 .UNSPECIFIED.);
#1206=B_SPLINE_CURVE_WITH_KNOTS('',3,(#62913,#62914,#62915,#62916,#62917,
#62918,#62919,#62920,#62921,#62922,#62923,#62924,#62925,#62926,#62927,#62928,
#62929,#62930,#62931,#62932,#62933,#62934),.UNSPECIFIED.,.F.,.F.,(4,3,3,
3,3,3,3,4),(-267.986713321673,-267.336241371601,-266.338718082901,-265.341194794201,
-264.343671505501,-263.346148216802,-262.348624928101,-261.703528014493),
 .UNSPECIFIED.);
#1207=B_SPLINE_CURVE_WITH_KNOTS('',3,(#62935,#62936,#62937,#62938,#62939,
#62940,#62941,#62942,#62943,#62944,#62945,#62946,#62947,#62948,#62949,#62950,
#62951,#62952,#62953,#62954,#62955,#62956),.UNSPECIFIED.,.F.,.F.,(4,3,3,
3,3,3,3,4),(258.72699110305,259.356055062001,260.353578350701,261.351101639402,
262.348624928102,263.346148216802,264.343671505502,265.010176410229),
 .UNSPECIFIED.);
#1208=B_SPLINE_CURVE_WITH_KNOTS('',3,(#62961,#62962,#62963,#62964,#62965,
#62966,#62967,#62968,#62969,#62970,#62971,#62972,#62973,#62974,#62975,#62976,
#62977,#62978,#62979,#62980,#62981,#62982),.UNSPECIFIED.,.F.,.F.,(4,3,3,
3,3,3,3,4),(-274.269898628852,-273.321381103802,-272.323857815102,-271.326334526402,
-270.328811237701,-269.331287949001,-268.333764660301,-267.986713321673),
 .UNSPECIFIED.);
#1209=B_SPLINE_CURVE_WITH_KNOTS('',3,(#62983,#62984,#62985,#62986,#62987,
#62988,#62989,#62990,#62991,#62992,#62993,#62994,#62995,#62996,#62997,#62998,
#62999,#63000,#63001,#63002,#63003,#63004),.UNSPECIFIED.,.F.,.F.,(4,3,3,
3,3,3,3,4),(265.010176410229,265.341194794201,266.338718082902,267.336241371602,
268.333764660302,269.331287949002,270.328811237702,271.293361717409),
 .UNSPECIFIED.);
#1210=B_SPLINE_CURVE_WITH_KNOTS('',3,(#63009,#63010,#63011,#63012,#63013,
#63014,#63015,#63016,#63017,#63018,#63019,#63020,#63021,#63022,#63023,#63024,
#63025,#63026,#63027,#63028,#63029,#63030,#63031,#63032,#63033),
 .UNSPECIFIED.,.F.,.F.,(4,3,3,3,3,3,3,3,4),(-280.553083936032,-280.304044124702,
-279.306520836001,-278.308997547301,-277.311474258601,-276.313950969901,
-275.316427681202,-274.318904392502,-274.269898628852),.UNSPECIFIED.);
#1211=B_SPLINE_CURVE_WITH_KNOTS('',3,(#63034,#63035,#63036,#63037,#63038,
#63039,#63040,#63041,#63042,#63043,#63044,#63045,#63046,#63047,#63048,#63049,
#63050,#63051,#63052,#63053,#63054,#63055,#63056,#63057,#63058),
 .UNSPECIFIED.,.F.,.F.,(4,3,3,3,3,3,3,3,4),(271.293361717409,271.326334526402,
272.323857815102,273.321381103802,274.318904392502,275.316427681202,276.313950969902,
277.311474258602,277.576547024588),.UNSPECIFIED.);
#1212=B_SPLINE_CURVE_WITH_KNOTS('',3,(#63063,#63064,#63065,#63066,#63067,
#63068,#63069,#63070,#63071,#63072,#63073,#63074,#63075,#63076,#63077,#63078,
#63079,#63080,#63081,#63082,#63083,#63084),.UNSPECIFIED.,.F.,.F.,(4,3,3,
3,3,3,3,4),(-286.836269243212,-286.289183856902,-285.291660568202,-284.294137279502,
-283.296613990802,-282.299090702102,-281.301567413402,-280.553083936032),
 .UNSPECIFIED.);
#1213=B_SPLINE_CURVE_WITH_KNOTS('',3,(#63085,#63086,#63087,#63088,#63089,
#63090,#63091,#63092,#63093,#63094,#63095,#63096,#63097,#63098,#63099,#63100,
#63101,#63102,#63103,#63104,#63105,#63106),.UNSPECIFIED.,.F.,.F.,(4,3,3,
3,3,3,3,4),(277.576547024588,278.308997547302,279.306520836002,280.304044124702,
281.301567413402,282.299090702102,283.296613990802,283.859732331768),
 .UNSPECIFIED.);
#1214=B_SPLINE_CURVE_WITH_KNOTS('',3,(#63111,#63112,#63113,#63114,#63115,
#63116,#63117,#63118,#63119,#63120,#63121,#63122,#63123,#63124,#63125,#63126,
#63127,#63128,#63129,#63130,#63131,#63132),.UNSPECIFIED.,.F.,.F.,(4,3,3,
3,3,3,3,4),(-293.119454550391,-292.274323589102,-291.276800300402,-290.279277011702,
-289.281753723002,-288.284230434302,-287.286707145602,-286.836269243212),
 .UNSPECIFIED.);
#1215=B_SPLINE_CURVE_WITH_KNOTS('',3,(#63133,#63134,#63135,#63136,#63137,
#63138,#63139,#63140,#63141,#63142,#63143,#63144,#63145,#63146,#63147,#63148,
#63149,#63150,#63151,#63152,#63153,#63154),.UNSPECIFIED.,.F.,.F.,(4,3,3,
3,3,3,3,4),(283.859732331768,284.294137279502,285.291660568202,286.289183856902,
287.286707145602,288.284230434302,289.281753723002,290.142917638947),
 .UNSPECIFIED.);
#1216=B_SPLINE_CURVE_WITH_KNOTS('',3,(#63159,#63160,#63161,#63162,#63163,
#63164,#63165,#63166,#63167,#63168,#63169,#63170,#63171,#63172,#63173,#63174,
#63175,#63176,#63177,#63178,#63179,#63180,#63181,#63182,#63183),
 .UNSPECIFIED.,.F.,.F.,(4,3,3,3,3,3,3,3,4),(-299.402639857571,-299.256986610002,
-298.259463321302,-297.261940032602,-296.264416743902,-295.266893455202,
-294.269370166502,-293.271846877802,-293.119454550391),.UNSPECIFIED.);
#1217=B_SPLINE_CURVE_WITH_KNOTS('',3,(#63184,#63185,#63186,#63187,#63188,
#63189,#63190,#63191,#63192,#63193,#63194,#63195,#63196,#63197,#63198,#63199,
#63200,#63201,#63202,#63203,#63204,#63205,#63206,#63207,#63208),
 .UNSPECIFIED.,.F.,.F.,(4,3,3,3,3,3,3,3,4),(290.142917638947,290.279277011702,
291.276800300402,292.274323589102,293.271846877802,294.269370166502,295.266893455202,
296.264416743902,296.426102946127),.UNSPECIFIED.);
#1218=B_SPLINE_CURVE_WITH_KNOTS('',3,(#63213,#63214,#63215,#63216,#63217,
#63218,#63219,#63220,#63221,#63222,#63223,#63224,#63225,#63226,#63227,#63228,
#63229,#63230,#63231,#63232,#63233,#63234),.UNSPECIFIED.,.F.,.F.,(4,3,3,
3,3,3,3,4),(-305.68582516475,-305.242126342202,-304.244603053502,-303.247079764802,
-302.249556476102,-301.252033187402,-300.254509898702,-299.402639857571),
 .UNSPECIFIED.);
#1219=B_SPLINE_CURVE_WITH_KNOTS('',3,(#63235,#63236,#63237,#63238,#63239,
#63240,#63241,#63242,#63243,#63244,#63245,#63246,#63247,#63248,#63249,#63250,
#63251,#63252,#63253,#63254,#63255,#63256),.UNSPECIFIED.,.F.,.F.,(4,3,3,
3,3,3,3,4),(296.426102946127,297.261940032602,298.259463321302,299.256986610002,
300.254509898702,301.252033187402,302.249556476102,302.709288253307),
 .UNSPECIFIED.);
#1220=B_SPLINE_CURVE_WITH_KNOTS('',3,(#63261,#63262,#63263,#63264,#63265,
#63266,#63267,#63268,#63269,#63270,#63271,#63272,#63273,#63274,#63275,#63276,
#63277,#63278,#63279,#63280,#63281,#63282),.UNSPECIFIED.,.F.,.F.,(4,3,3,
3,3,3,3,4),(-311.96901047193,-311.227266074402,-310.229742785702,-309.232219497002,
-308.234696208302,-307.237172919602,-306.239649630902,-305.68582516475),
 .UNSPECIFIED.);
#1221=B_SPLINE_CURVE_WITH_KNOTS('',3,(#63283,#63284,#63285,#63286,#63287,
#63288,#63289,#63290,#63291,#63292,#63293,#63294,#63295,#63296,#63297,#63298,
#63299,#63300,#63301,#63302,#63303,#63304),.UNSPECIFIED.,.F.,.F.,(4,3,3,
3,3,3,3,4),(302.709288253307,303.247079764802,304.244603053502,305.242126342202,
306.239649630902,307.237172919602,308.234696208302,308.992473560486),
 .UNSPECIFIED.);
#1222=B_SPLINE_CURVE_WITH_KNOTS('',3,(#63309,#63310,#63311,#63312,#63313,
#63314,#63315,#63316,#63317,#63318,#63319,#63320,#63321,#63322,#63323,#63324,
#63325,#63326,#63327,#63328,#63329,#63330,#63331,#63332,#63333),
 .UNSPECIFIED.,.F.,.F.,(4,3,3,3,3,3,3,3,4),(-318.252195779109,-318.209929095302,
-317.212405806602,-316.214882517902,-315.217359229202,-314.219835940502,
-313.222312651802,-312.224789363102,-311.96901047193),.UNSPECIFIED.);
#1223=B_SPLINE_CURVE_WITH_KNOTS('',3,(#63334,#63335,#63336,#63337,#63338,
#63339,#63340,#63341,#63342,#63343,#63344,#63345,#63346,#63347,#63348,#63349,
#63350,#63351,#63352,#63353,#63354,#63355,#63356,#63357,#63358),
 .UNSPECIFIED.,.F.,.F.,(4,3,3,3,3,3,3,3,4),(308.992473560486,309.232219497002,
310.229742785702,311.227266074402,312.224789363102,313.222312651802,314.219835940502,
315.217359229202,315.275658867666),.UNSPECIFIED.);
#1224=B_SPLINE_CURVE_WITH_KNOTS('',3,(#63363,#63364,#63365,#63366,#63367,
#63368,#63369,#63370,#63371,#63372,#63373,#63374,#63375,#63376,#63377,#63378,
#63379,#63380,#63381,#63382,#63383,#63384),.UNSPECIFIED.,.F.,.F.,(4,3,3,
3,3,3,3,4),(-324.535381086289,-324.195068827502,-323.197545538802,-322.200022250102,
-321.202498961402,-320.204975672702,-319.207452384002,-318.252195779109),
 .UNSPECIFIED.);
#1225=B_SPLINE_CURVE_WITH_KNOTS('',3,(#63385,#63386,#63387,#63388,#63389,
#63390,#63391,#63392,#63393,#63394,#63395,#63396,#63397,#63398,#63399,#63400,
#63401,#63402,#63403,#63404,#63405,#63406),.UNSPECIFIED.,.F.,.F.,(4,3,3,
3,3,3,3,4),(315.275658867666,316.214882517902,317.212405806602,318.209929095302,
319.207452384002,320.204975672702,321.202498961402,321.558844174845),
 .UNSPECIFIED.);
#1226=B_SPLINE_CURVE_WITH_KNOTS('',3,(#63411,#63412,#63413,#63414,#63415,
#63416,#63417,#63418,#63419,#63420,#63421,#63422,#63423,#63424,#63425,#63426,
#63427,#63428,#63429,#63430,#63431,#63432),.UNSPECIFIED.,.F.,.F.,(4,3,3,
3,3,3,3,4),(-330.818566393468,-330.180208559702,-329.182685271002,-328.185161982302,
-327.187638693602,-326.190115404902,-325.192592116202,-324.535381086289),
 .UNSPECIFIED.);
#1227=B_SPLINE_CURVE_WITH_KNOTS('',3,(#63433,#63434,#63435,#63436,#63437,
#63438,#63439,#63440,#63441,#63442,#63443,#63444,#63445,#63446,#63447,#63448,
#63449,#63450,#63451,#63452,#63453,#63454),.UNSPECIFIED.,.F.,.F.,(4,3,3,
3,3,3,3,4),(321.558844174845,322.200022250102,323.197545538802,324.195068827502,
325.192592116202,326.190115404902,327.187638693602,327.842029482025),
 .UNSPECIFIED.);
#1228=B_SPLINE_CURVE_WITH_KNOTS('',3,(#63459,#63460,#63461,#63462,#63463,
#63464,#63465,#63466,#63467,#63468,#63469,#63470,#63471,#63472,#63473,#63474,
#63475,#63476,#63477,#63478,#63479,#63480),.UNSPECIFIED.,.F.,.F.,(4,3,3,
3,3,3,3,4),(-337.101751700648,-336.165348291902,-335.167825003202,-334.170301714502,
-333.172778425802,-332.175255137102,-331.177731848402,-330.818566393468),
 .UNSPECIFIED.);
#1229=B_SPLINE_CURVE_WITH_KNOTS('',3,(#63481,#63482,#63483,#63484,#63485,
#63486,#63487,#63488,#63489,#63490,#63491,#63492,#63493,#63494,#63495,#63496,
#63497,#63498,#63499,#63500,#63501,#63502),.UNSPECIFIED.,.F.,.F.,(4,3,3,
3,3,3,3,4),(327.842029482025,328.185161982302,329.182685271002,330.180208559702,
331.177731848402,332.175255137102,333.172778425802,334.125214789205),
 .UNSPECIFIED.);
#1230=B_SPLINE_CURVE_WITH_KNOTS('',3,(#63507,#63508,#63509,#63510,#63511,
#63512,#63513,#63514,#63515,#63516,#63517,#63518,#63519,#63520,#63521,#63522,
#63523,#63524,#63525,#63526,#63527,#63528,#63529,#63530,#63531),
 .UNSPECIFIED.,.F.,.F.,(4,3,3,3,3,3,3,3,4),(-343.384937007828,-343.148011312802,
-342.150488024102,-341.152964735402,-340.155441446702,-339.157918158002,
-338.160394869302,-337.162871580602,-337.101751700648),.UNSPECIFIED.);
#1231=B_SPLINE_CURVE_WITH_KNOTS('',3,(#63532,#63533,#63534,#63535,#63536,
#63537,#63538,#63539,#63540,#63541,#63542,#63543,#63544,#63545,#63546,#63547,
#63548,#63549,#63550,#63551,#63552,#63553,#63554,#63555,#63556),
 .UNSPECIFIED.,.F.,.F.,(4,3,3,3,3,3,3,3,4),(334.125214789205,334.170301714502,
335.167825003202,336.165348291902,337.162871580602,338.160394869302,339.157918158002,
340.155441446702,340.408400096384),.UNSPECIFIED.);
#1232=B_SPLINE_CURVE_WITH_KNOTS('',3,(#63561,#63562,#63563,#63564,#63565,
#63566,#63567,#63568,#63569,#63570,#63571,#63572,#63573,#63574,#63575,#63576,
#63577,#63578,#63579,#63580,#63581,#63582),.UNSPECIFIED.,.F.,.F.,(4,3,3,
3,3,3,3,4),(-349.668122315007,-349.133151045002,-348.135627756302,-347.138104467602,
-346.140581178902,-345.143057890202,-344.145534601502,-343.384937007828),
 .UNSPECIFIED.);
#1233=B_SPLINE_CURVE_WITH_KNOTS('',3,(#63583,#63584,#63585,#63586,#63587,
#63588,#63589,#63590,#63591,#63592,#63593,#63594,#63595,#63596,#63597,#63598,
#63599,#63600,#63601,#63602,#63603,#63604),.UNSPECIFIED.,.F.,.F.,(4,3,3,
3,3,3,3,4),(340.408400096384,341.152964735402,342.150488024102,343.148011312802,
344.145534601502,345.143057890202,346.140581178902,346.691585403564),
 .UNSPECIFIED.);
#1234=B_SPLINE_CURVE_WITH_KNOTS('',3,(#63609,#63610,#63611,#63612,#63613,
#63614,#63615,#63616,#63617,#63618,#63619,#63620,#63621,#63622,#63623,#63624,
#63625,#63626,#63627,#63628,#63629,#63630),.UNSPECIFIED.,.F.,.F.,(4,3,3,
3,3,3,3,4),(-355.951307622187,-355.118290777202,-354.120767488502,-353.123244199802,
-352.125720911102,-351.128197622402,-350.130674333702,-349.668122315007),
 .UNSPECIFIED.);
#1235=B_SPLINE_CURVE_WITH_KNOTS('',3,(#63631,#63632,#63633,#63634,#63635,
#63636,#63637,#63638,#63639,#63640,#63641,#63642,#63643,#63644,#63645,#63646,
#63647,#63648,#63649,#63650,#63651,#63652),.UNSPECIFIED.,.F.,.F.,(4,3,3,
3,3,3,3,4),(346.691585403564,347.138104467602,348.135627756302,349.133151045002,
350.130674333702,351.128197622402,352.125720911102,352.974770710743),
 .UNSPECIFIED.);
#1236=B_SPLINE_CURVE_WITH_KNOTS('',3,(#63657,#63658,#63659,#63660,#63661,
#63662,#63663,#63664,#63665,#63666,#63667,#63668,#63669,#63670,#63671,#63672,
#63673,#63674,#63675,#63676,#63677,#63678,#63679,#63680,#63681),
 .UNSPECIFIED.,.F.,.F.,(4,3,3,3,3,3,3,3,4),(-362.234492929366,-362.100953798102,
-361.103430509402,-360.105907220702,-359.108383932002,-358.110860643302,
-357.113337354602,-356.115814065902,-355.951307622187),.UNSPECIFIED.);
#1237=B_SPLINE_CURVE_WITH_KNOTS('',3,(#63682,#63683,#63684,#63685,#63686,
#63687,#63688,#63689,#63690,#63691,#63692,#63693,#63694,#63695,#63696,#63697,
#63698,#63699,#63700,#63701,#63702,#63703,#63704,#63705,#63706),
 .UNSPECIFIED.,.F.,.F.,(4,3,3,3,3,3,3,3,4),(352.974770710743,353.123244199802,
354.120767488502,355.118290777202,356.115814065902,357.113337354602,358.110860643302,
359.108383932002,359.257956017923),.UNSPECIFIED.);
#1238=B_SPLINE_CURVE_WITH_KNOTS('',3,(#63711,#63712,#63713,#63714,#63715,
#63716,#63717,#63718,#63719,#63720,#63721,#63722,#63723,#63724,#63725,#63726,
#63727,#63728,#63729,#63730,#63731,#63732),.UNSPECIFIED.,.F.,.F.,(4,3,3,
3,3,3,3,4),(-368.517678236546,-368.086093530302,-367.088570241602,-366.091046952902,
-365.093523664202,-364.096000375502,-363.098477086802,-362.234492929366),
 .UNSPECIFIED.);
#1239=B_SPLINE_CURVE_WITH_KNOTS('',3,(#63733,#63734,#63735,#63736,#63737,
#63738,#63739,#63740,#63741,#63742,#63743,#63744,#63745,#63746,#63747,#63748,
#63749,#63750,#63751,#63752,#63753,#63754),.UNSPECIFIED.,.F.,.F.,(4,3,3,
3,3,3,3,4),(359.257956017923,360.105907220702,361.103430509402,362.100953798102,
363.098477086802,364.096000375502,365.093523664202,365.541141325102),
 .UNSPECIFIED.);
#1240=B_SPLINE_CURVE_WITH_KNOTS('',3,(#63759,#63760,#63761,#63762,#63763,
#63764,#63765,#63766,#63767,#63768,#63769,#63770,#63771,#63772,#63773,#63774,
#63775,#63776,#63777,#63778,#63779,#63780),.UNSPECIFIED.,.F.,.F.,(4,3,3,
3,3,3,3,4),(-374.800863543725,-374.071233262502,-373.073709973802,-372.076186685102,
-371.078663396402,-370.081140107702,-369.083616819002,-368.517678236546),
 .UNSPECIFIED.);
#1241=B_SPLINE_CURVE_WITH_KNOTS('',3,(#63781,#63782,#63783,#63784,#63785,
#63786,#63787,#63788,#63789,#63790,#63791,#63792,#63793,#63794,#63795,#63796,
#63797,#63798,#63799,#63800,#63801,#63802),.UNSPECIFIED.,.F.,.F.,(4,3,3,
3,3,3,3,4),(365.541141325102,366.091046952902,367.088570241602,368.086093530302,
369.083616819002,370.081140107702,371.078663396402,371.824326632282),
 .UNSPECIFIED.);
#1242=B_SPLINE_CURVE_WITH_KNOTS('',3,(#63808,#63809,#63810,#63811,#63812,
#63813),.UNSPECIFIED.,.F.,.F.,(4,1,1,4),(386.415896391544,386.683789399021,
387.681312687721,388.606151278594),.UNSPECIFIED.);
#1243=B_SPLINE_CURVE_WITH_KNOTS('',3,(#63816,#63817,#63818,#63819,#63820),
 .UNSPECIFIED.,.F.,.F.,(4,1,4),(386.415896391544,386.868472513736,387.367234158086),
 .UNSPECIFIED.);
#1244=B_SPLINE_CURVE_WITH_KNOTS('',3,(#63825,#63826,#63827,#63828,#63829,
#63830,#63831,#63832,#63833,#63834),.UNSPECIFIED.,.F.,.F.,(4,1,1,1,1,1,
1,4),(380.132711084365,380.698649666821,381.696172955521,382.693696244221,
383.691219532921,384.688742821621,385.686266110321,386.415896391544),
 .UNSPECIFIED.);
#1245=B_SPLINE_CURVE_WITH_KNOTS('',3,(#63835,#63836,#63837,#63838,#63839,
#63840,#63841,#63842,#63843,#63844,#63845),.UNSPECIFIED.,.F.,.F.,(4,1,1,
1,1,1,1,1,4),(380.132711084365,380.384571137186,381.382094425886,382.379617714586,
383.377141003286,384.374664291986,385.372187580686,386.369710869386,386.415896391544),
 .UNSPECIFIED.);
#1246=B_SPLINE_CURVE_WITH_KNOTS('',3,(#63850,#63851,#63852,#63853,#63854,
#63855,#63856,#63857,#63858,#63859),.UNSPECIFIED.,.F.,.F.,(4,1,1,1,1,1,
1,4),(373.849525777185,374.713509934621,375.711033223321,376.708556512021,
377.706079800721,378.703603089421,379.701126378121,380.132711084365),
 .UNSPECIFIED.);
#1247=B_SPLINE_CURVE_WITH_KNOTS('',3,(#63860,#63861,#63862,#63863,#63864,
#63865,#63866,#63867,#63868,#63869),.UNSPECIFIED.,.F.,.F.,(4,1,1,1,1,1,
1,4),(373.849525777185,374.399431404986,375.396954693686,376.394477982386,
377.392001271086,378.389524559786,379.387047848486,380.132711084365),
 .UNSPECIFIED.);
#1248=B_SPLINE_CURVE_WITH_KNOTS('',3,(#63874,#63875,#63876,#63877,#63878,
#63879,#63880,#63881,#63882,#63883,#63884),.UNSPECIFIED.,.F.,.F.,(4,1,1,
1,1,1,1,1,4),(367.566340470006,367.730846913721,368.728370202421,369.725893491121,
370.723416779821,371.720940068521,372.718463357221,373.715986645921,373.849525777185),
 .UNSPECIFIED.);
#1249=B_SPLINE_CURVE_WITH_KNOTS('',3,(#63885,#63886,#63887,#63888,#63889,
#63890,#63891,#63892,#63893,#63894),.UNSPECIFIED.,.F.,.F.,(4,1,1,1,1,1,
1,4),(367.566340470006,368.414291672786,369.411814961486,370.409338250186,
371.406861538886,372.404384827586,373.401908116286,373.849525777185),
 .UNSPECIFIED.);
#1250=B_SPLINE_CURVE_WITH_KNOTS('',3,(#63899,#63900,#63901,#63902,#63903,
#63904,#63905,#63906,#63907,#63908),.UNSPECIFIED.,.F.,.F.,(4,1,1,1,1,1,
1,4),(361.283155162826,361.745707181521,362.743230470221,363.740753758921,
364.738277047621,365.735800336321,366.733323625021,367.566340470006),
 .UNSPECIFIED.);
#1251=B_SPLINE_CURVE_WITH_KNOTS('',3,(#63909,#63910,#63911,#63912,#63913,
#63914,#63915,#63916,#63917,#63918,#63919),.UNSPECIFIED.,.F.,.F.,(4,1,1,
1,1,1,1,1,4),(361.283155162826,361.431628651886,362.429151940586,363.426675229286,
364.424198517986,365.421721806686,366.419245095386,367.416768384086,367.566340470006),
 .UNSPECIFIED.);
#1252=B_SPLINE_CURVE_WITH_KNOTS('',3,(#63924,#63925,#63926,#63927,#63928,
#63929,#63930,#63931,#63932,#63933),.UNSPECIFIED.,.F.,.F.,(4,1,1,1,1,1,
1,4),(354.999969855647,355.760567449321,356.758090738021,357.755614026721,
358.753137315421,359.750660604121,360.748183892821,361.283155162826),
 .UNSPECIFIED.);
#1253=B_SPLINE_CURVE_WITH_KNOTS('',3,(#63934,#63935,#63936,#63937,#63938,
#63939,#63940,#63941,#63942,#63943),.UNSPECIFIED.,.F.,.F.,(4,1,1,1,1,1,
1,4),(354.999969855647,355.446488919686,356.444012208386,357.441535497086,
358.439058785786,359.436582074486,360.434105363186,361.283155162826),
 .UNSPECIFIED.);
#1254=B_SPLINE_CURVE_WITH_KNOTS('',3,(#63948,#63949,#63950,#63951,#63952,
#63953,#63954,#63955,#63956,#63957,#63958),.UNSPECIFIED.,.F.,.F.,(4,1,1,
1,1,1,1,1,4),(348.716784548467,348.777904428421,349.775427717121,350.772951005821,
351.770474294521,352.767997583221,353.765520871921,354.763044160621,354.999969855647),
 .UNSPECIFIED.);
#1255=B_SPLINE_CURVE_WITH_KNOTS('',3,(#63959,#63960,#63961,#63962,#63963,
#63964,#63965,#63966,#63967,#63968),.UNSPECIFIED.,.F.,.F.,(4,1,1,1,1,1,
1,4),(348.716784548467,349.461349187486,350.458872476186,351.456395764886,
352.453919053586,353.451442342286,354.448965630986,354.999969855647),
 .UNSPECIFIED.);
#1256=B_SPLINE_CURVE_WITH_KNOTS('',3,(#63973,#63974,#63975,#63976,#63977,
#63978,#63979,#63980,#63981,#63982),.UNSPECIFIED.,.F.,.F.,(4,1,1,1,1,1,
1,4),(342.433599241287,342.792764696221,343.790287984921,344.787811273621,
345.785334562321,346.782857851021,347.780381139721,348.716784548467),
 .UNSPECIFIED.);
#1257=B_SPLINE_CURVE_WITH_KNOTS('',3,(#63983,#63984,#63985,#63986,#63987,
#63988,#63989,#63990,#63991,#63992,#63993),.UNSPECIFIED.,.F.,.F.,(4,1,1,
1,1,1,1,1,4),(342.433599241287,342.478686166586,343.476209455286,344.473732743986,
345.471256032686,346.468779321386,347.466302610086,348.463825898786,348.716784548467),
 .UNSPECIFIED.);
#1258=B_SPLINE_CURVE_WITH_KNOTS('',3,(#63998,#63999,#64000,#64001,#64002,
#64003,#64004,#64005,#64006,#64007),.UNSPECIFIED.,.F.,.F.,(4,1,1,1,1,1,
1,4),(336.150413934108,336.807624964021,337.805148252721,338.802671541421,
339.800194830121,340.797718118821,341.795241407521,342.433599241287),
 .UNSPECIFIED.);
#1259=B_SPLINE_CURVE_WITH_KNOTS('',3,(#64008,#64009,#64010,#64011,#64012,
#64013,#64014,#64015,#64016,#64017),.UNSPECIFIED.,.F.,.F.,(4,1,1,1,1,1,
1,4),(336.150413934108,336.493546434386,337.491069723086,338.488593011786,
339.486116300486,340.483639589186,341.481162877886,342.433599241287),
 .UNSPECIFIED.);
#1260=B_SPLINE_CURVE_WITH_KNOTS('',3,(#64022,#64023,#64024,#64025,#64026,
#64027,#64028,#64029,#64030,#64031),.UNSPECIFIED.,.F.,.F.,(4,1,1,1,1,1,
1,4),(329.867228626928,330.822485231821,331.820008520521,332.817531809221,
333.815055097921,334.812578386621,335.810101675321,336.150413934108),
 .UNSPECIFIED.);
#1261=B_SPLINE_CURVE_WITH_KNOTS('',3,(#64032,#64033,#64034,#64035,#64036,
#64037,#64038,#64039,#64040,#64041),.UNSPECIFIED.,.F.,.F.,(4,1,1,1,1,1,
1,4),(329.867228626928,330.508406702186,331.505929990886,332.503453279586,
333.500976568286,334.498499856986,335.496023145686,336.150413934108),
 .UNSPECIFIED.);
#1262=B_SPLINE_CURVE_WITH_KNOTS('',3,(#64046,#64047,#64048,#64049,#64050,
#64051,#64052,#64053,#64054,#64055,#64056),.UNSPECIFIED.,.F.,.F.,(4,1,1,
1,1,1,1,1,4),(323.584043319749,323.839822210921,324.837345499621,325.834868788321,
326.832392077021,327.829915365721,328.827438654421,329.824961943121,329.867228626928),
 .UNSPECIFIED.);
#1263=B_SPLINE_CURVE_WITH_KNOTS('',3,(#64057,#64058,#64059,#64060,#64061,
#64062,#64063,#64064,#64065,#64066),.UNSPECIFIED.,.F.,.F.,(4,1,1,1,1,1,
1,4),(323.584043319749,324.523266969986,325.520790258686,326.518313547386,
327.515836836086,328.513360124786,329.510883413486,329.867228626928),
 .UNSPECIFIED.);
#1264=B_SPLINE_CURVE_WITH_KNOTS('',3,(#64071,#64072,#64073,#64074,#64075,
#64076,#64077,#64078,#64079,#64080),.UNSPECIFIED.,.F.,.F.,(4,1,1,1,1,1,
1,4),(317.300858012569,317.854682478721,318.852205767421,319.849729056121,
320.847252344821,321.844775633521,322.842298922221,323.584043319749),
 .UNSPECIFIED.);
#1265=B_SPLINE_CURVE_WITH_KNOTS('',3,(#64081,#64082,#64083,#64084,#64085,
#64086,#64087,#64088,#64089,#64090,#64091),.UNSPECIFIED.,.F.,.F.,(4,1,1,
1,1,1,1,1,4),(317.300858012569,317.540603949086,318.538127237786,319.535650526486,
320.533173815186,321.530697103886,322.528220392586,323.525743681286,323.584043319749),
 .UNSPECIFIED.);
#1266=B_SPLINE_CURVE_WITH_KNOTS('',3,(#64096,#64097,#64098,#64099,#64100,
#64101,#64102,#64103,#64104,#64105),.UNSPECIFIED.,.F.,.F.,(4,1,1,1,1,1,
1,4),(311.01767270539,311.869542746521,312.867066035221,313.864589323921,
314.862112612621,315.859635901321,316.857159190021,317.300858012569),
 .UNSPECIFIED.);
#1267=B_SPLINE_CURVE_WITH_KNOTS('',3,(#64106,#64107,#64108,#64109,#64110,
#64111,#64112,#64113,#64114,#64115),.UNSPECIFIED.,.F.,.F.,(4,1,1,1,1,1,
1,4),(311.01767270539,311.555464216886,312.552987505586,313.550510794286,
314.548034082986,315.545557371686,316.543080660386,317.300858012569),
 .UNSPECIFIED.);
#1268=B_SPLINE_CURVE_WITH_KNOTS('',3,(#64120,#64121,#64122,#64123,#64124,
#64125,#64126,#64127,#64128,#64129,#64130),.UNSPECIFIED.,.F.,.F.,(4,1,1,
1,1,1,1,1,4),(304.73448739821,304.886879725621,305.884403014321,306.881926303021,
307.879449591721,308.876972880421,309.874496169121,310.872019457821,311.01767270539),
 .UNSPECIFIED.);
#1269=B_SPLINE_CURVE_WITH_KNOTS('',3,(#64131,#64132,#64133,#64134,#64135,
#64136,#64137,#64138,#64139,#64140),.UNSPECIFIED.,.F.,.F.,(4,1,1,1,1,1,
1,4),(304.73448739821,305.570324484686,306.567847773386,307.565371062086,
308.562894350786,309.560417639486,310.557940928186,311.01767270539),
 .UNSPECIFIED.);
#1270=B_SPLINE_CURVE_WITH_KNOTS('',3,(#64145,#64146,#64147,#64148,#64149,
#64150,#64151,#64152,#64153,#64154),.UNSPECIFIED.,.F.,.F.,(4,1,1,1,1,1,
1,4),(298.451302091031,298.901739993421,299.899263282121,300.896786570821,
301.894309859521,302.891833148221,303.889356436921,304.73448739821),
 .UNSPECIFIED.);
#1271=B_SPLINE_CURVE_WITH_KNOTS('',3,(#64155,#64156,#64157,#64158,#64159,
#64160,#64161,#64162,#64163,#64164,#64165),.UNSPECIFIED.,.F.,.F.,(4,1,1,
1,1,1,1,1,4),(298.451302091031,298.587661463786,299.585184752486,300.582708041186,
301.580231329886,302.577754618586,303.575277907286,304.572801195986,304.73448739821),
 .UNSPECIFIED.);
#1272=B_SPLINE_CURVE_WITH_KNOTS('',3,(#64170,#64171,#64172,#64173,#64174,
#64175,#64176,#64177,#64178,#64179),.UNSPECIFIED.,.F.,.F.,(4,1,1,1,1,1,
1,4),(292.168116783851,292.916600261221,293.914123549921,294.911646838621,
295.909170127321,296.906693416021,297.904216704721,298.451302091031),
 .UNSPECIFIED.);
#1273=B_SPLINE_CURVE_WITH_KNOTS('',3,(#64180,#64181,#64182,#64183,#64184,
#64185,#64186,#64187,#64188,#64189),.UNSPECIFIED.,.F.,.F.,(4,1,1,1,1,1,
1,4),(292.168116783851,292.602521731586,293.600045020286,294.597568308986,
295.595091597686,296.592614886386,297.590138175086,298.451302091031),
 .UNSPECIFIED.);
#1274=B_SPLINE_CURVE_WITH_KNOTS('',3,(#64194,#64195,#64196,#64197,#64198,
#64199,#64200,#64201,#64202,#64203,#64204),.UNSPECIFIED.,.F.,.F.,(4,1,1,
1,1,1,1,1,4),(285.884931476671,285.933937240321,286.931460529021,287.928983817721,
288.926507106421,289.924030395121,290.921553683821,291.919076972521,292.168116783851),
 .UNSPECIFIED.);
#1275=B_SPLINE_CURVE_WITH_KNOTS('',3,(#64205,#64206,#64207,#64208,#64209,
#64210,#64211,#64212,#64213,#64214),.UNSPECIFIED.,.F.,.F.,(4,1,1,1,1,1,
1,4),(285.884931476671,286.617381999385,287.614905288085,288.612428576785,
289.609951865485,290.607475154186,291.604998442886,292.168116783851),
 .UNSPECIFIED.);
#1276=B_SPLINE_CURVE_WITH_KNOTS('',3,(#64219,#64220,#64221,#64222,#64223,
#64224,#64225,#64226,#64227,#64228),.UNSPECIFIED.,.F.,.F.,(4,1,1,1,1,1,
1,4),(279.601746169492,279.948797508121,280.946320796821,281.943844085521,
282.941367374221,283.938890662921,284.936413951621,285.884931476671),
 .UNSPECIFIED.);
#1277=B_SPLINE_CURVE_WITH_KNOTS('',3,(#64229,#64230,#64231,#64232,#64233,
#64234,#64235,#64236,#64237,#64238,#64239),.UNSPECIFIED.,.F.,.F.,(4,1,1,
1,1,1,1,1,4),(279.601746169492,279.634718978485,280.632242267185,281.629765555885,
282.627288844585,283.624812133285,284.622335421985,285.619858710685,285.884931476671),
 .UNSPECIFIED.);
#1278=B_SPLINE_CURVE_WITH_KNOTS('',3,(#64244,#64245,#64246,#64247,#64248,
#64249,#64250,#64251,#64252,#64253),.UNSPECIFIED.,.F.,.F.,(4,1,1,1,1,1,
1,4),(273.318560862312,273.963657775921,274.961181064621,275.958704353321,
276.956227642021,277.953750930721,278.951274219421,279.601746169492),
 .UNSPECIFIED.);
#1279=B_SPLINE_CURVE_WITH_KNOTS('',3,(#64254,#64255,#64256,#64257,#64258,
#64259,#64260,#64261,#64262,#64263),.UNSPECIFIED.,.F.,.F.,(4,1,1,1,1,1,
1,4),(273.318560862312,273.649579246285,274.647102534985,275.644625823685,
276.642149112385,277.639672401085,278.637195689785,279.601746169492),
 .UNSPECIFIED.);
#1280=B_SPLINE_CURVE_WITH_KNOTS('',3,(#64268,#64269,#64270,#64271,#64272,
#64273,#64274,#64275,#64276,#64277),.UNSPECIFIED.,.F.,.F.,(4,1,1,1,1,1,
1,4),(267.035375555133,267.97851804372,268.97604133242,269.973564621121,
270.971087909821,271.968611198521,272.966134487221,273.318560862312),
 .UNSPECIFIED.);
#1281=B_SPLINE_CURVE_WITH_KNOTS('',3,(#64278,#64279,#64280,#64281,#64282,
#64283,#64284,#64285,#64286,#64287),.UNSPECIFIED.,.F.,.F.,(4,1,1,1,1,1,
1,4),(267.035375555133,267.664439514085,268.661962802785,269.659486091485,
270.657009380185,271.654532668885,272.652055957585,273.318560862312),
 .UNSPECIFIED.);
#1282=B_SPLINE_CURVE_WITH_KNOTS('',3,(#64292,#64293,#64294,#64295,#64296,
#64297,#64298,#64299,#64300,#64301,#64302),.UNSPECIFIED.,.F.,.F.,(4,1,1,
1,1,1,1,1,4),(260.752190247953,260.99585502282,261.99337831152,262.99090160022,
263.98842488892,264.98594817762,265.983471466321,266.980994755021,267.035375555133),
 .UNSPECIFIED.);
#1283=B_SPLINE_CURVE_WITH_KNOTS('',3,(#64303,#64304,#64305,#64306,#64307,
#64308,#64309,#64310,#64311,#64312),.UNSPECIFIED.,.F.,.F.,(4,1,1,1,1,1,
1,4),(260.752190247953,261.679299781885,262.676823070585,263.674346359285,
264.671869647985,265.669392936685,266.666916225385,267.035375555133),
 .UNSPECIFIED.);
#1284=B_SPLINE_CURVE_WITH_KNOTS('',3,(#64317,#64318,#64319,#64320,#64321,
#64322,#64323,#64324,#64325,#64326),.UNSPECIFIED.,.F.,.F.,(4,1,1,1,1,1,
1,4),(254.469004940774,255.01071529062,256.00823857932,257.00576186802,
258.00328515672,259.00080844542,259.99833173412,260.752190247953),
 .UNSPECIFIED.);
#1285=B_SPLINE_CURVE_WITH_KNOTS('',3,(#64327,#64328,#64329,#64330,#64331,
#64332,#64333,#64334,#64335,#64336,#64337),.UNSPECIFIED.,.F.,.F.,(4,1,1,
1,1,1,1,1,4),(254.469004940774,254.696636760985,255.694160049685,256.691683338385,
257.689206627085,258.686729915785,259.684253204485,260.681776493185,260.752190247953),
 .UNSPECIFIED.);
#1286=B_SPLINE_CURVE_WITH_KNOTS('',3,(#64342,#64343,#64344,#64345,#64346,
#64347,#64348,#64349,#64350,#64351),.UNSPECIFIED.,.F.,.F.,(4,1,1,1,1,1,
1,4),(248.185819633594,249.02557555842,250.02309884712,251.02062213582,
252.01814542452,253.01566871322,254.01319200192,254.469004940774),
 .UNSPECIFIED.);
#1287=B_SPLINE_CURVE_WITH_KNOTS('',3,(#64352,#64353,#64354,#64355,#64356,
#64357,#64358,#64359,#64360,#64361),.UNSPECIFIED.,.F.,.F.,(4,1,1,1,1,1,
1,4),(248.185819633594,248.711497028785,249.709020317485,250.706543606185,
251.704066894885,252.701590183585,253.699113472285,254.469004940774),
 .UNSPECIFIED.);
#1288=B_SPLINE_CURVE_WITH_KNOTS('',3,(#64366,#64367,#64368,#64369,#64370,
#64371,#64372,#64373,#64374,#64375,#64376),.UNSPECIFIED.,.F.,.F.,(4,1,1,
1,1,1,1,1,4),(241.902634326414,242.04291253752,243.04043582622,244.03795911492,
245.03548240362,246.03300569232,247.03052898102,248.02805226972,248.185819633594),
 .UNSPECIFIED.);
#1289=B_SPLINE_CURVE_WITH_KNOTS('',3,(#64377,#64378,#64379,#64380,#64381,
#64382,#64383,#64384,#64385,#64386),.UNSPECIFIED.,.F.,.F.,(4,1,1,1,1,1,
1,4),(241.902634326414,242.726357296585,243.723880585285,244.721403873985,
245.718927162685,246.716450451385,247.713973740085,248.185819633594),
 .UNSPECIFIED.);
#1290=B_SPLINE_CURVE_WITH_KNOTS('',3,(#64391,#64392,#64393,#64394,#64395,
#64396,#64397,#64398,#64399,#64400),.UNSPECIFIED.,.F.,.F.,(4,1,1,1,1,1,
1,4),(235.619449019235,236.05777280532,237.05529609402,238.05281938272,
239.05034267142,240.04786596012,241.04538924882,241.902634326414),
 .UNSPECIFIED.);
#1291=B_SPLINE_CURVE_WITH_KNOTS('',3,(#64401,#64402,#64403,#64404,#64405,
#64406,#64407,#64408,#64409,#64410,#64411),.UNSPECIFIED.,.F.,.F.,(4,1,1,
1,1,1,1,1,4),(235.619449019235,235.743694275685,236.741217564385,237.738740853085,
238.736264141785,239.733787430485,240.731310719185,241.728834007885,241.902634326414),
 .UNSPECIFIED.);
#1292=B_SPLINE_CURVE_WITH_KNOTS('',3,(#64416,#64417,#64418,#64419,#64420,
#64421,#64422,#64423,#64424,#64425),.UNSPECIFIED.,.F.,.F.,(4,1,1,1,1,1,
1,4),(229.336263712055,230.07263307312,231.07015636182,232.06767965052,
233.06520293922,234.06272622792,235.06024951662,235.619449019235),
 .UNSPECIFIED.);
#1293=B_SPLINE_CURVE_WITH_KNOTS('',3,(#64426,#64427,#64428,#64429,#64430,
#64431,#64432,#64433,#64434,#64435),.UNSPECIFIED.,.F.,.F.,(4,1,1,1,1,1,
1,4),(229.336263712055,229.758554543485,230.756077832185,231.753601120885,
232.751124409585,233.748647698285,234.746170986985,235.619449019235),
 .UNSPECIFIED.);
#1294=B_SPLINE_CURVE_WITH_KNOTS('',3,(#64440,#64441,#64442,#64443,#64444,
#64445,#64446,#64447,#64448,#64449,#64450),.UNSPECIFIED.,.F.,.F.,(4,1,1,
1,1,1,1,1,4),(223.053078404876,223.08997005222,224.08749334092,225.08501662962,
226.08253991832,227.08006320702,228.07758649572,229.07510978442,229.336263712055),
 .UNSPECIFIED.);
#1295=B_SPLINE_CURVE_WITH_KNOTS('',3,(#64451,#64452,#64453,#64454,#64455,
#64456,#64457,#64458,#64459,#64460),.UNSPECIFIED.,.F.,.F.,(4,1,1,1,1,1,
1,4),(223.053078404876,223.773414811285,224.770938099985,225.768461388685,
226.765984677385,227.763507966085,228.761031254785,229.336263712055),
 .UNSPECIFIED.);
#1296=B_SPLINE_CURVE_WITH_KNOTS('',3,(#64465,#64466,#64467,#64468,#64469,
#64470,#64471,#64472,#64473,#64474),.UNSPECIFIED.,.F.,.F.,(4,1,1,1,1,1,
1,4),(216.769893097696,217.10483032002,218.10235360872,219.09987689742,
220.09740018612,221.09492347482,222.09244676352,223.053078404876),
 .UNSPECIFIED.);
#1297=B_SPLINE_CURVE_WITH_KNOTS('',3,(#64475,#64476,#64477,#64478,#64479,
#64480,#64481,#64482,#64483,#64484,#64485),.UNSPECIFIED.,.F.,.F.,(4,1,1,
1,1,1,1,1,4),(216.769893097696,216.790751790385,217.788275079085,218.785798367785,
219.783321656485,220.780844945185,221.778368233885,222.775891522585,223.053078404876),
 .UNSPECIFIED.);
#1298=B_SPLINE_CURVE_WITH_KNOTS('',3,(#64490,#64491,#64492,#64493,#64494,
#64495,#64496,#64497,#64498,#64499),.UNSPECIFIED.,.F.,.F.,(4,1,1,1,1,1,
1,4),(210.486707790517,211.11969058782,212.11721387652,213.11473716522,
214.11226045392,215.10978374262,216.10730703132,216.769893097696),
 .UNSPECIFIED.);
#1299=B_SPLINE_CURVE_WITH_KNOTS('',3,(#64500,#64501,#64502,#64503,#64504,
#64505,#64506,#64507,#64508,#64509),.UNSPECIFIED.,.F.,.F.,(4,1,1,1,1,1,
1,4),(210.486707790517,210.805612058185,211.803135346885,212.800658635585,
213.798181924285,214.795705212985,215.793228501685,216.769893097696),
 .UNSPECIFIED.);
#1300=B_SPLINE_CURVE_WITH_KNOTS('',3,(#64514,#64515,#64516,#64517,#64518,
#64519,#64520,#64521,#64522,#64523),.UNSPECIFIED.,.F.,.F.,(4,1,1,1,1,1,
1,4),(204.203522483337,205.13455085562,206.13207414432,207.12959743302,
208.12712072172,209.12464401042,210.12216729912,210.486707790517),
 .UNSPECIFIED.);
#1301=B_SPLINE_CURVE_WITH_KNOTS('',3,(#64524,#64525,#64526,#64527,#64528,
#64529,#64530,#64531,#64532,#64533),.UNSPECIFIED.,.F.,.F.,(4,1,1,1,1,1,
1,4),(204.203522483337,204.820472325985,205.817995614685,206.815518903385,
207.813042192085,208.810565480785,209.808088769485,210.486707790517),
 .UNSPECIFIED.);
#1302=B_SPLINE_CURVE_WITH_KNOTS('',3,(#64538,#64539,#64540,#64541,#64542,
#64543,#64544,#64545,#64546,#64547,#64548),.UNSPECIFIED.,.F.,.F.,(4,1,1,
1,1,1,1,1,4),(197.920337176158,198.15188783472,199.14941112342,200.14693441212,
201.14445770082,202.14198098952,203.13950427822,204.13702756692,204.203522483337),
 .UNSPECIFIED.);
#1303=B_SPLINE_CURVE_WITH_KNOTS('',3,(#64549,#64550,#64551,#64552,#64553,
#64554,#64555,#64556,#64557,#64558),.UNSPECIFIED.,.F.,.F.,(4,1,1,1,1,1,
1,4),(197.920337176158,198.835332593785,199.832855882485,200.830379171185,
201.827902459885,202.825425748585,203.822949037285,204.203522483337),
 .UNSPECIFIED.);
#1304=B_SPLINE_CURVE_WITH_KNOTS('',3,(#64563,#64564,#64565,#64566,#64567,
#64568,#64569,#64570,#64571,#64572),.UNSPECIFIED.,.F.,.F.,(4,1,1,1,1,1,
1,4),(191.637151868978,192.16674810252,193.16427139122,194.16179467992,
195.15931796862,196.15684125732,197.15436454602,197.920337176158),
 .UNSPECIFIED.);
#1305=B_SPLINE_CURVE_WITH_KNOTS('',3,(#64573,#64574,#64575,#64576,#64577,
#64578,#64579,#64580,#64581,#64582,#64583),.UNSPECIFIED.,.F.,.F.,(4,1,1,
1,1,1,1,1,4),(191.637151868978,191.852669572885,192.850192861585,193.847716150285,
194.845239438985,195.842762727685,196.840286016385,197.837809305085,197.920337176158),
 .UNSPECIFIED.);
#1306=B_SPLINE_CURVE_WITH_KNOTS('',3,(#64588,#64589,#64590,#64591,#64592,
#64593,#64594,#64595,#64596,#64597),.UNSPECIFIED.,.F.,.F.,(4,1,1,1,1,1,
1,4),(185.353966561798,186.18160837032,187.17913165902,188.17665494772,
189.17417823642,190.17170152512,191.16922481382,191.637151868978),
 .UNSPECIFIED.);
#1307=B_SPLINE_CURVE_WITH_KNOTS('',3,(#64598,#64599,#64600,#64601,#64602,
#64603,#64604,#64605,#64606,#64607),.UNSPECIFIED.,.F.,.F.,(4,1,1,1,1,1,
1,4),(185.353966561798,185.867529840685,186.865053129385,187.862576418085,
188.860099706785,189.857622995485,190.855146284185,191.637151868978),
 .UNSPECIFIED.);
#1308=B_SPLINE_CURVE_WITH_KNOTS('',3,(#64612,#64613,#64614,#64615,#64616,
#64617,#64618,#64619,#64620,#64621,#64622),.UNSPECIFIED.,.F.,.F.,(4,1,1,
1,1,1,1,1,4),(179.070781254619,179.19894534942,180.19646863812,181.19399192682,
182.19151521552,183.18903850422,184.18656179292,185.18408508162,185.353966561798),
 .UNSPECIFIED.);
#1309=B_SPLINE_CURVE_WITH_KNOTS('',3,(#64623,#64624,#64625,#64626,#64627,
#64628,#64629,#64630,#64631,#64632),.UNSPECIFIED.,.F.,.F.,(4,1,1,1,1,1,
1,4),(179.070781254619,179.882390108485,180.879913397185,181.877436685885,
182.874959974585,183.872483263285,184.870006551985,185.353966561798),
 .UNSPECIFIED.);
#1310=B_SPLINE_CURVE_WITH_KNOTS('',3,(#64637,#64638,#64639,#64640,#64641,
#64642,#64643,#64644,#64645,#64646),.UNSPECIFIED.,.F.,.F.,(4,1,1,1,1,1,
1,4),(172.787595947439,173.21380561722,174.21132890592,175.20885219462,
176.20637548332,177.20389877202,178.20142206072,179.070781254619),
 .UNSPECIFIED.);
#1311=B_SPLINE_CURVE_WITH_KNOTS('',3,(#64647,#64648,#64649,#64650,#64651,
#64652,#64653,#64654,#64655,#64656,#64657),.UNSPECIFIED.,.F.,.F.,(4,1,1,
1,1,1,1,1,4),(172.787595947439,172.899727087585,173.897250376285,174.894773664985,
175.892296953685,176.889820242385,177.887343531085,178.884866819785,179.070781254619),
 .UNSPECIFIED.);
#1312=B_SPLINE_CURVE_WITH_KNOTS('',3,(#64662,#64663,#64664,#64665,#64666,
#64667,#64668,#64669,#64670,#64671),.UNSPECIFIED.,.F.,.F.,(4,1,1,1,1,1,
1,4),(166.50441064026,167.22866588502,168.22618917372,169.22371246242,170.22123575112,
171.21875903982,172.21628232852,172.787595947439),.UNSPECIFIED.);
#1313=B_SPLINE_CURVE_WITH_KNOTS('',3,(#64672,#64673,#64674,#64675,#64676,
#64677,#64678,#64679,#64680,#64681),.UNSPECIFIED.,.F.,.F.,(4,1,1,1,1,1,
1,4),(166.50441064026,166.914587355385,167.912110644085,168.909633932785,
169.907157221485,170.904680510185,171.902203798885,172.787595947439),
 .UNSPECIFIED.);
#1314=B_SPLINE_CURVE_WITH_KNOTS('',3,(#64686,#64687,#64688,#64689,#64690,
#64691,#64692,#64693,#64694,#64695,#64696),.UNSPECIFIED.,.F.,.F.,(4,1,1,
1,1,1,1,1,4),(160.22122533308,160.24600286412,161.24352615282,162.24104944152,
163.23857273022,164.23609601892,165.23361930762,166.23114259632,166.50441064026),
 .UNSPECIFIED.);
#1315=B_SPLINE_CURVE_WITH_KNOTS('',3,(#64697,#64698,#64699,#64700,#64701,
#64702,#64703,#64704,#64705,#64706),.UNSPECIFIED.,.F.,.F.,(4,1,1,1,1,1,
1,4),(160.22122533308,160.929447623185,161.926970911885,162.924494200585,
163.922017489285,164.919540777985,165.917064066685,166.50441064026),
 .UNSPECIFIED.);
#1316=B_SPLINE_CURVE_WITH_KNOTS('',3,(#64711,#64712,#64713,#64714,#64715,
#64716,#64717,#64718,#64719,#64720),.UNSPECIFIED.,.F.,.F.,(4,1,1,1,1,1,
1,4),(153.938040025901,154.26086313192,155.25838642062,156.25590970932,
157.25343299802,158.25095628672,159.24847957542,160.22122533308),
 .UNSPECIFIED.);
#1317=B_SPLINE_CURVE_WITH_KNOTS('',3,(#64721,#64722,#64723,#64724,#64725,
#64726,#64727,#64728,#64729,#64730,#64731),.UNSPECIFIED.,.F.,.F.,(4,1,1,
1,1,1,1,1,4),(153.938040025901,153.946784602285,154.944307890985,155.941831179685,
156.939354468385,157.936877757085,158.934401045785,159.931924334485,160.22122533308),
 .UNSPECIFIED.);
#1318=B_SPLINE_CURVE_WITH_KNOTS('',3,(#64736,#64737,#64738,#64739,#64740,
#64741,#64742,#64743,#64744,#64745),.UNSPECIFIED.,.F.,.F.,(4,1,1,1,1,1,
1,4),(147.654854718721,148.27572339972,149.27324668842,150.27076997712,
151.26829326582,152.26581655452,153.26333984322,153.938040025901),
 .UNSPECIFIED.);
#1319=B_SPLINE_CURVE_WITH_KNOTS('',3,(#64746,#64747,#64748,#64749,#64750,
#64751,#64752,#64753,#64754,#64755),.UNSPECIFIED.,.F.,.F.,(4,1,1,1,1,1,
1,4),(147.654854718721,147.961644870085,148.959168158785,149.956691447485,
150.954214736185,151.951738024885,152.949261313585,153.938040025901),
 .UNSPECIFIED.);
#1320=B_SPLINE_CURVE_WITH_KNOTS('',3,(#64760,#64761,#64762,#64763,#64764,
#64765,#64766,#64767,#64768,#64769),.UNSPECIFIED.,.F.,.F.,(4,1,1,1,1,1,
1,4),(141.371669411541,142.29058366752,143.28810695622,144.28563024492,
145.28315353362,146.28067682232,147.27820011102,147.654854718721),
 .UNSPECIFIED.);
#1321=B_SPLINE_CURVE_WITH_KNOTS('',3,(#64770,#64771,#64772,#64773,#64774,
#64775,#64776,#64777,#64778,#64779),.UNSPECIFIED.,.F.,.F.,(4,1,1,1,1,1,
1,4),(141.371669411541,141.976505137885,142.974028426585,143.971551715285,
144.969075003985,145.966598292685,146.964121581385,147.654854718721),
 .UNSPECIFIED.);
#1322=B_SPLINE_CURVE_WITH_KNOTS('',3,(#64784,#64785,#64786,#64787,#64788,
#64789,#64790,#64791,#64792,#64793,#64794),.UNSPECIFIED.,.F.,.F.,(4,1,1,
1,1,1,1,1,4),(135.088484104362,135.30792064662,136.30544393532,137.30296722402,
138.30049051272,139.29801380142,140.29553709012,141.29306037882,141.371669411541),
 .UNSPECIFIED.);
#1323=B_SPLINE_CURVE_WITH_KNOTS('',3,(#64795,#64796,#64797,#64798,#64799,
#64800,#64801,#64802,#64803,#64804),.UNSPECIFIED.,.F.,.F.,(4,1,1,1,1,1,
1,4),(135.088484104362,135.991365405685,136.988888694385,137.986411983085,
138.983935271785,139.981458560485,140.978981849185,141.371669411541),
 .UNSPECIFIED.);
#1324=B_SPLINE_CURVE_WITH_KNOTS('',3,(#64809,#64810,#64811,#64812,#64813,
#64814,#64815,#64816,#64817,#64818),.UNSPECIFIED.,.F.,.F.,(4,1,1,1,1,1,
1,4),(128.805298797182,129.32278091442,130.32030420312,131.31782749182,
132.31535078052,133.31287406922,134.31039735792,135.088484104362),
 .UNSPECIFIED.);
#1325=B_SPLINE_CURVE_WITH_KNOTS('',3,(#64819,#64820,#64821,#64822,#64823,
#64824,#64825,#64826,#64827,#64828,#64829),.UNSPECIFIED.,.F.,.F.,(4,1,1,
1,1,1,1,1,4),(128.805298797182,129.008702384785,130.006225673485,131.003748962185,
132.001272250885,132.998795539585,133.996318828285,134.993842116985,135.088484104362),
 .UNSPECIFIED.);
#1326=B_SPLINE_CURVE_WITH_KNOTS('',3,(#64834,#64835,#64836,#64837,#64838,
#64839,#64840,#64841,#64842,#64843),.UNSPECIFIED.,.F.,.F.,(4,1,1,1,1,1,
1,4),(122.522113490003,123.33764118222,124.33516447092,125.33268775962,
126.33021104832,127.32773433702,128.32525762572,128.805298797182),
 .UNSPECIFIED.);
#1327=B_SPLINE_CURVE_WITH_KNOTS('',3,(#64844,#64845,#64846,#64847,#64848,
#64849,#64850,#64851,#64852,#64853),.UNSPECIFIED.,.F.,.F.,(4,1,1,1,1,1,
1,4),(122.522113490003,123.023562652585,124.021085941285,125.018609229985,
126.016132518685,127.013655807385,128.011179096085,128.805298797182),
 .UNSPECIFIED.);
#1328=B_SPLINE_CURVE_WITH_KNOTS('',3,(#64858,#64859,#64860,#64861,#64862,
#64863,#64864,#64865,#64866,#64867,#64868),.UNSPECIFIED.,.F.,.F.,(4,1,1,
1,1,1,1,1,4),(116.238928182823,116.35497816132,117.35250145002,118.35002473872,
119.34754802742,120.34507131612,121.34259460482,122.34011789352,122.522113490003),
 .UNSPECIFIED.);
#1329=B_SPLINE_CURVE_WITH_KNOTS('',3,(#64869,#64870,#64871,#64872,#64873,
#64874,#64875,#64876,#64877,#64878),.UNSPECIFIED.,.F.,.F.,(4,1,1,1,1,1,
1,4),(116.238928182823,117.038422920385,118.035946209085,119.033469497785,
120.030992786485,121.028516075185,122.026039363885,122.522113490003),
 .UNSPECIFIED.);
#1330=B_SPLINE_CURVE_WITH_KNOTS('',3,(#64883,#64884,#64885,#64886,#64887,
#64888,#64889,#64890,#64891,#64892),.UNSPECIFIED.,.F.,.F.,(4,1,1,1,1,1,
1,4),(109.955742875644,110.36983842912,111.36736171782,112.36488500652,
113.36240829522,114.35993158392,115.35745487262,116.238928182823),
 .UNSPECIFIED.);
#1331=B_SPLINE_CURVE_WITH_KNOTS('',3,(#64893,#64894,#64895,#64896,#64897,
#64898,#64899,#64900,#64901,#64902,#64903),.UNSPECIFIED.,.F.,.F.,(4,1,1,
1,1,1,1,1,4),(109.955742875644,110.055759899484,111.053283188184,112.050806476884,
113.048329765584,114.045853054284,115.043376342985,116.040899631685,116.238928182823),
 .UNSPECIFIED.);
#1332=B_SPLINE_CURVE_WITH_KNOTS('',3,(#64908,#64909,#64910,#64911,#64912,
#64913,#64914,#64915,#64916,#64917),.UNSPECIFIED.,.F.,.F.,(4,1,1,1,1,1,
1,4),(103.672557568464,104.38469869692,105.38222198562,106.37974527432,
107.37726856302,108.37479185172,109.37231514042,109.955742875644),
 .UNSPECIFIED.);
#1333=B_SPLINE_CURVE_WITH_KNOTS('',3,(#64918,#64919,#64920,#64921,#64922,
#64923,#64924,#64925,#64926,#64927),.UNSPECIFIED.,.F.,.F.,(4,1,1,1,1,1,
1,4),(103.672557568464,104.070620167284,105.068143455984,106.065666744684,
107.063190033384,108.060713322084,109.058236610784,109.955742875644),
 .UNSPECIFIED.);
#1334=B_SPLINE_CURVE_WITH_KNOTS('',3,(#64932,#64933,#64934,#64935,#64936,
#64937,#64938,#64939,#64940,#64941,#64942),.UNSPECIFIED.,.F.,.F.,(4,1,1,
1,1,1,1,1,4),(97.3893722612843,97.4020356760196,98.3995589647196,99.3970822534196,
100.39460554212,101.39212883082,102.38965211952,103.38717540822,103.672557568464),
 .UNSPECIFIED.);
#1335=B_SPLINE_CURVE_WITH_KNOTS('',3,(#64943,#64944,#64945,#64946,#64947,
#64948,#64949,#64950,#64951,#64952),.UNSPECIFIED.,.F.,.F.,(4,1,1,1,1,1,
1,4),(97.3893722612844,98.0854804350844,99.0830037237844,100.080527012484,
101.078050301184,102.075573589884,103.073096878584,103.672557568464),
 .UNSPECIFIED.);
#1336=B_SPLINE_CURVE_WITH_KNOTS('',3,(#64957,#64958,#64959,#64960,#64961,
#64962,#64963,#64964,#64965,#64966),.UNSPECIFIED.,.F.,.F.,(4,1,1,1,1,1,
1,4),(91.1061869541047,91.4168959438195,92.4144192325195,93.4119425212196,
94.4094658099196,95.4069890986196,96.4045123873196,97.3893722612843),
 .UNSPECIFIED.);
#1337=B_SPLINE_CURVE_WITH_KNOTS('',3,(#64967,#64968,#64969,#64970,#64971,
#64972,#64973,#64974,#64975,#64976),.UNSPECIFIED.,.F.,.F.,(4,1,1,1,1,1,
1,4),(91.1061869541048,92.1003407028844,93.0978639915844,94.0953872802844,
95.0929105689844,96.0904338576844,97.0879571463844,97.3893722612844),
 .UNSPECIFIED.);
#1338=B_SPLINE_CURVE_WITH_KNOTS('',3,(#64981,#64982,#64983,#64984,#64985,
#64986,#64987,#64988,#64989,#64990),.UNSPECIFIED.,.F.,.F.,(4,1,1,1,1,1,
1,4),(84.8230016469251,85.4317562116195,86.4292795003195,87.4268027890195,
88.4243260777195,89.4218493664195,90.4193726551195,91.1061869541047),
 .UNSPECIFIED.);
#1339=B_SPLINE_CURVE_WITH_KNOTS('',3,(#64991,#64992,#64993,#64994,#64995,
#64996,#64997,#64998,#64999,#65000,#65001),.UNSPECIFIED.,.F.,.F.,(4,1,1,
1,1,1,1,1,4),(84.8230016469252,85.1176776819843,86.1152009706843,87.1127242593844,
88.1102475480844,89.1077708367844,90.1052941254844,91.1028174141844,91.1061869541048),
 .UNSPECIFIED.);
#1340=B_SPLINE_CURVE_WITH_KNOTS('',3,(#65006,#65007,#65008,#65009,#65010,
#65011,#65012,#65013,#65014,#65015),.UNSPECIFIED.,.F.,.F.,(4,1,1,1,1,1,
1,4),(78.5398163397455,79.4466164794195,80.4441397681195,81.4416630568195,
82.4391863455195,83.4367096342195,84.4342329229195,84.8230016469251),
 .UNSPECIFIED.);
#1341=B_SPLINE_CURVE_WITH_KNOTS('',3,(#65016,#65017,#65018,#65019,#65020,
#65021,#65022,#65023,#65024,#65025),.UNSPECIFIED.,.F.,.F.,(4,1,1,1,1,1,
1,4),(78.5398163397456,79.1325379497843,80.1300612384843,81.1275845271843,
82.1251078158843,83.1226311045843,84.1201543932843,84.8230016469252),
 .UNSPECIFIED.);
#1342=B_SPLINE_CURVE_WITH_KNOTS('',3,(#65030,#65031,#65032,#65033,#65034,
#65035,#65036,#65037,#65038,#65039,#65040),.UNSPECIFIED.,.F.,.F.,(4,1,1,
1,1,1,1,1,4),(72.2566310325659,72.4639534585194,73.4614767472195,74.4590000359194,
75.4565233246195,76.4540466133195,77.4515699020195,78.4490931907195,78.5398163397455),
 .UNSPECIFIED.);
#1343=B_SPLINE_CURVE_WITH_KNOTS('',3,(#65041,#65042,#65043,#65044,#65045,
#65046,#65047,#65048,#65049,#65050),.UNSPECIFIED.,.F.,.F.,(4,1,1,1,1,1,
1,4),(72.256631032566,73.1473982175843,74.1449215062843,75.1424447949843,
76.1399680836843,77.1374913723843,78.1350146610843,78.5398163397456),
 .UNSPECIFIED.);
#1344=B_SPLINE_CURVE_WITH_KNOTS('',3,(#65055,#65056,#65057,#65058,#65059,
#65060,#65061,#65062,#65063,#65064),.UNSPECIFIED.,.F.,.F.,(4,1,1,1,1,1,
1,4),(65.9734457253863,66.4788137263194,67.4763370150194,68.4738603037194,
69.4713835924194,70.4689068811194,71.4664301698194,72.2566310325659),
 .UNSPECIFIED.);
#1345=B_SPLINE_CURVE_WITH_KNOTS('',3,(#65065,#65066,#65067,#65068,#65069,
#65070,#65071,#65072,#65073,#65074,#65075),.UNSPECIFIED.,.F.,.F.,(4,1,1,
1,1,1,1,1,4),(65.9734457253864,66.1647351966842,67.1622584853842,68.1597817740843,
69.1573050627842,70.1548283514843,71.1523516401843,72.1498749288843,72.256631032566),
 .UNSPECIFIED.);
#1346=B_SPLINE_CURVE_WITH_KNOTS('',3,(#65080,#65081,#65082,#65083,#65084,
#65085,#65086,#65087,#65088,#65089),.UNSPECIFIED.,.F.,.F.,(4,1,1,1,1,1,
1,4),(59.6902604182067,60.4936739941194,61.4911972828194,62.4887205715194,
63.4862438602194,64.4837671489194,65.4812904376194,65.9734457253863),
 .UNSPECIFIED.);
#1347=B_SPLINE_CURVE_WITH_KNOTS('',3,(#65090,#65091,#65092,#65093,#65094,
#65095,#65096,#65097,#65098,#65099),.UNSPECIFIED.,.F.,.F.,(4,1,1,1,1,1,
1,4),(59.6902604182069,60.1795954644842,61.1771187531842,62.1746420418842,
63.1721653305842,64.1696886192842,65.1672119079842,65.9734457253864),
 .UNSPECIFIED.);
#1348=B_SPLINE_CURVE_WITH_KNOTS('',3,(#65104,#65105,#65106,#65107,#65108,
#65109,#65110,#65111,#65112,#65113,#65114),.UNSPECIFIED.,.F.,.F.,(4,1,1,
1,1,1,1,1,4),(53.4070751110272,53.5110109732193,54.5085342619193,55.5060575506193,
56.5035808393194,57.5011041280194,58.4986274167194,59.4961507054194,59.6902604182067),
 .UNSPECIFIED.);
#1349=B_SPLINE_CURVE_WITH_KNOTS('',3,(#65115,#65116,#65117,#65118,#65119,
#65120,#65121,#65122,#65123,#65124),.UNSPECIFIED.,.F.,.F.,(4,1,1,1,1,1,
1,4),(53.4070751110273,54.1944557322842,55.1919790209842,56.1895023096842,
57.1870255983842,58.1845488870842,59.1820721757842,59.6902604182069),
 .UNSPECIFIED.);
#1350=B_SPLINE_CURVE_WITH_KNOTS('',3,(#65129,#65130,#65131,#65132,#65133,
#65134,#65135,#65136,#65137,#65138),.UNSPECIFIED.,.F.,.F.,(4,1,1,1,1,1,
1,4),(47.1238898038476,47.5258712410193,48.5233945297193,49.5209178184193,
50.5184411071193,51.5159643958193,52.5134876845193,53.4070751110272),
 .UNSPECIFIED.);
#1351=B_SPLINE_CURVE_WITH_KNOTS('',3,(#65139,#65140,#65141,#65142,#65143,
#65144,#65145,#65146,#65147,#65148,#65149),.UNSPECIFIED.,.F.,.F.,(4,1,1,
1,1,1,1,1,4),(47.1238898038477,47.2117927113841,48.2093160000841,49.2068392887841,
50.2043625774841,51.2018858661842,52.1994091548842,53.1969324435842,53.4070751110273),
 .UNSPECIFIED.);
#1352=B_SPLINE_CURVE_WITH_KNOTS('',3,(#65154,#65155,#65156,#65157,#65158,
#65159,#65160,#65161,#65162,#65163),.UNSPECIFIED.,.F.,.F.,(4,1,1,1,1,1,
1,4),(40.840704496668,41.5407315088193,42.5382547975193,43.5357780862193,
44.5333013749193,45.5308246636193,46.5283479523193,47.1238898038476),
 .UNSPECIFIED.);
#1353=B_SPLINE_CURVE_WITH_KNOTS('',3,(#65164,#65165,#65166,#65167,#65168,
#65169,#65170,#65171,#65172,#65173),.UNSPECIFIED.,.F.,.F.,(4,1,1,1,1,1,
1,4),(40.8407044966681,41.2266529791841,42.2241762678841,43.2216995565841,
44.2192228452841,45.2167461339841,46.2142694226841,47.1238898038477),
 .UNSPECIFIED.);
#1354=B_SPLINE_CURVE_WITH_KNOTS('',3,(#65178,#65179,#65180,#65181,#65182,
#65183,#65184,#65185,#65186,#65187,#65188),.UNSPECIFIED.,.F.,.F.,(4,1,1,
1,1,1,1,1,4),(34.5575191894884,34.5580684879192,35.5555917766192,36.5531150653192,
37.5506383540192,38.5481616427193,39.5456849314193,40.5432082201193,40.840704496668),
 .UNSPECIFIED.);
#1355=B_SPLINE_CURVE_WITH_KNOTS('',3,(#65189,#65190,#65191,#65192,#65193,
#65194,#65195,#65196,#65197,#65198),.UNSPECIFIED.,.F.,.F.,(4,1,1,1,1,1,
1,4),(34.5575191894885,35.2415132469841,36.2390365356841,37.2365598243841,
38.2340831130841,39.2316064017841,40.2291296904841,40.8407044966681),
 .UNSPECIFIED.);
#1356=B_SPLINE_CURVE_WITH_KNOTS('',3,(#65203,#65204,#65205,#65206,#65207,
#65208,#65209,#65210,#65211,#65212),.UNSPECIFIED.,.F.,.F.,(4,1,1,1,1,1,
1,4),(28.2743338823088,28.5729287557192,29.5704520444192,30.5679753331192,
31.5654986218192,32.5630219105192,33.5605451992192,34.5575191894884),
 .UNSPECIFIED.);
#1357=B_SPLINE_CURVE_WITH_KNOTS('',3,(#65213,#65214,#65215,#65216,#65217,
#65218,#65219,#65220,#65221,#65222),.UNSPECIFIED.,.F.,.F.,(4,1,1,1,1,1,
1,4),(28.2743338823089,29.256373514784,30.253896803484,31.251420092184,
32.2489433808841,33.2464666695841,34.2439899582841,34.5575191894885),
 .UNSPECIFIED.);
#1358=B_SPLINE_CURVE_WITH_KNOTS('',3,(#65227,#65228,#65229,#65230,#65231,
#65232,#65233,#65234,#65235,#65236),.UNSPECIFIED.,.F.,.F.,(4,1,1,1,1,1,
1,4),(21.9911485751292,22.5877890235192,23.5853123122192,24.5828356009192,
25.5803588896192,26.5778821783192,27.5754054670192,28.2743338823088),
 .UNSPECIFIED.);
#1359=B_SPLINE_CURVE_WITH_KNOTS('',3,(#65237,#65238,#65239,#65240,#65241,
#65242,#65243,#65244,#65245,#65246,#65247),.UNSPECIFIED.,.F.,.F.,(4,1,1,
1,1,1,1,1,4),(21.9911485751293,22.273710493884,23.271233782584,24.268757071284,
25.266280359984,26.263803648684,27.261326937384,28.258850226084,28.2743338823089),
 .UNSPECIFIED.);
#1360=B_SPLINE_CURVE_WITH_KNOTS('',3,(#65252,#65253,#65254,#65255,#65256,
#65257,#65258,#65259,#65260,#65261),.UNSPECIFIED.,.F.,.F.,(4,1,1,1,1,1,
1,4),(15.7079632679496,16.6026492913191,17.6001725800191,18.5976958687191,
19.5952191574192,20.5927424461192,21.5902657348192,21.9911485751292),
 .UNSPECIFIED.);
#1361=B_SPLINE_CURVE_WITH_KNOTS('',3,(#65262,#65263,#65264,#65265,#65266,
#65267,#65268,#65269,#65270,#65271),.UNSPECIFIED.,.F.,.F.,(4,1,1,1,1,1,
1,4),(15.7079632679497,16.288570761684,17.286094050384,18.283617339084,
19.281140627784,20.278663916484,21.276187205184,21.9911485751293),
 .UNSPECIFIED.);
#1362=B_SPLINE_CURVE_WITH_KNOTS('',3,(#66813,#66814,#66815,#66816,#66817,
#66818,#66819,#66820,#66821,#66822,#66823,#66824,#66825,#66826,#66827,#66828,
#66829,#66830,#66831,#66832,#66833,#66834,#66835,#66836,#66837,#66838,#66839,
#66840,#66841,#66842,#66843,#66844,#66845,#66846,#66847,#66848,#66849,#66850,
#66851,#66852,#66853,#66854,#66855,#66856,#66857,#66858,#66859,#66860,#66861,
#66862,#66863,#66864,#66865,#66866,#66867,#66868,#66869,#66870,#66871,#66872,
#66873,#66874,#66875,#66876,#66877,#66878,#66879,#66880,#66881,#66882,#66883,
#66884,#66885,#66886,#66887,#66888,#66889,#66890,#66891,#66892,#66893,#66894,
#66895,#66896,#66897,#66898,#66899,#66900,#66901,#66902,#66903,#66904,#66905,
#66906,#66907,#66908,#66909,#66910,#66911,#66912,#66913,#66914,#66915,#66916,
#66917,#66918,#66919,#66920,#66921),.UNSPECIFIED.,.F.,.F.,(4,3,3,3,3,3,
3,3,3,3,3,3,3,3,3,3,3,3,3,3,3,3,3,3,3,3,3,3,3,3,3,3,3,3,3,3,4),(0.,0.0359628151845056,
0.0790640675124802,0.122944974172411,0.167078080679047,0.180430545026742,
0.19037773183983,0.196180338284082,0.239492682886256,0.282925566791464,
0.325969530232972,0.368238370501489,0.375078460706215,0.381042467863404,
0.42346125387141,0.465393907031249,0.506323913773678,0.51599109870151,0.544714566753401,
0.554178082246963,0.559723896450525,0.565364051500323,0.606359797650403,
0.648015429264718,0.689524423166306,0.717651633141474,0.732581126571207,
0.739096451862393,0.745778843116641,0.786822056096576,0.827804944486442,
0.845389038445888,0.853674880949773,0.860823772315063,0.901249933519242,
0.94103892518765,0.96847769616201),.UNSPECIFIED.);
#1363=B_SPLINE_CURVE_WITH_KNOTS('',3,(#66922,#66923,#66924,#66925,#66926,
#66927,#66928,#66929,#66930,#66931,#66932,#66933,#66934,#66935,#66936,#66937,
#66938,#66939,#66940),.UNSPECIFIED.,.F.,.F.,(4,3,3,3,3,3,4),(371.824326632282,
372.076186685102,373.073709973802,374.071233262502,375.068756551202,376.066279839902,
376.991118430775),.UNSPECIFIED.);
#1364=B_SPLINE_CURVE_WITH_KNOTS('',3,(#66942,#66943,#66944,#66945,#66946,
#66947,#66948,#66949,#66950,#66951,#66952,#66953,#66954,#66955,#66956,#66957,
#66958,#66959,#66960,#66961,#66962,#66963,#66964,#66965,#66966,#66967,#66968,
#66969,#66970,#66971,#66972,#66973,#66974,#66975,#66976,#66977,#66978,#66979,
#66980,#66981,#66982,#66983,#66984,#66985,#66986,#66987,#66988,#66989,#66990,
#66991,#66992,#66993,#66994,#66995,#66996,#66997,#66998,#66999,#67000,#67001,
#67002,#67003,#67004,#67005,#67006,#67007,#67008,#67009,#67010,#67011,#67012,
#67013,#67014,#67015,#67016,#67017,#67018,#67019,#67020,#67021,#67022,#67023,
#67024,#67025,#67026,#67027,#67028,#67029,#67030,#67031,#67032,#67033,#67034,
#67035,#67036,#67037,#67038,#67039,#67040,#67041,#67042,#67043,#67044,#67045,
#67046,#67047),.UNSPECIFIED.,.F.,.F.,(4,3,3,3,3,3,3,3,3,3,3,3,3,3,3,3,3,
3,3,3,3,3,3,3,3,3,3,3,3,3,3,3,3,3,3,4),(-0.968477696161913,-0.936462781732006,
-0.897034237282827,-0.871088158002514,-0.855755616551603,-0.849836345176422,
-0.809673382933614,-0.76870133116664,-0.750776058518589,-0.741856737530979,
-0.7341371378361,-0.692655598295136,-0.650704137993651,-0.608502345694694,
-0.576851001470477,-0.56347054188062,-0.556078670388381,-0.513475355214464,
-0.481896968797825,-0.440388916382611,-0.398291621794682,-0.386095361159993,
-0.379050278062876,-0.373539380612515,-0.331389873213074,-0.287819274607371,
-0.244248676001668,-0.213717591501459,-0.200360242032618,-0.19269654176718,
-0.1869673316623,-0.143586522253231,-0.0997397595963603,-0.0560111116848197,
-0.0129407155146067,0.),.UNSPECIFIED.);
#1365=B_SPLINE_CURVE_WITH_KNOTS('',3,(#67048,#67049,#67050,#67051,#67052,
#67053,#67054,#67055,#67056),.UNSPECIFIED.,.F.,.F.,(4,1,1,1,1,1,4),(10.3761157273111,
11.3009543181839,12.2984776068839,13.2960008955839,14.2935241842839,15.291047472984,
15.7079632679497),.UNSPECIFIED.);
#1366=B_SPLINE_CURVE_WITH_KNOTS('',3,(#67060,#67061,#67062,#67063,#67064,
#67065,#67066,#67067,#67068),.UNSPECIFIED.,.F.,.F.,(4,1,1,1,1,1,4),(11.6150328478191,
12.1137944921691,12.6125561365191,13.6100794252191,14.6076027139191,15.6051260026191,
15.7079632679496),.UNSPECIFIED.);
#1367=B_SPLINE_CURVE_WITH_KNOTS('',3,(#68610,#68611,#68612,#68613,#68614,
#68615,#68616,#68617,#68618,#68619,#68620,#68621,#68622,#68623,#68624,#68625,
#68626,#68627,#68628,#68629,#68630,#68631,#68632,#68633,#68634,#68635,#68636,
#68637,#68638,#68639,#68640,#68641,#68642,#68643,#68644,#68645,#68646,#68647,
#68648,#68649,#68650,#68651,#68652,#68653,#68654,#68655,#68656,#68657,#68658,
#68659,#68660,#68661,#68662,#68663,#68664,#68665,#68666,#68667,#68668,#68669,
#68670,#68671,#68672,#68673,#68674,#68675,#68676,#68677,#68678,#68679,#68680,
#68681,#68682,#68683,#68684,#68685,#68686,#68687,#68688,#68689,#68690,#68691,
#68692,#68693,#68694,#68695,#68696,#68697,#68698,#68699,#68700,#68701,#68702,
#68703,#68704,#68705,#68706,#68707,#68708,#68709,#68710,#68711,#68712,#68713,
#68714,#68715,#68716,#68717,#68718),.UNSPECIFIED.,.F.,.F.,(4,3,3,3,3,3,
3,3,3,3,3,3,3,3,3,3,3,3,3,3,3,3,3,3,3,3,3,3,3,3,3,3,3,3,3,3,4),(0.,0.0319610084124964,
0.0709970802367925,0.110918019903594,0.151489267836741,0.166268550959158,
0.172136820332691,0.17773227169752,0.218621519728627,0.260105203172031,
0.301749535598996,0.343042584632714,0.348577800050639,0.354310610465885,
0.396643769367683,0.438881645932778,0.480394489143215,0.485838103022159,
0.515447494563868,0.527322668925359,0.533096841618444,0.574119197999633,
0.616402831080215,0.659075854182062,0.69089454476895,0.706803890062393,
0.714443723340302,0.720575125052056,0.722713235355837,0.765747942600601,
0.80908641486819,0.828699390062085,0.838036583520388,0.844245630783005,
0.888067982944121,0.931632292905962,0.965990216419354),.UNSPECIFIED.);
#1368=B_SPLINE_CURVE_WITH_KNOTS('',3,(#68719,#68720,#68721,#68722,#68723,
#68724,#68725,#68726,#68727,#68728,#68729,#68730,#68731,#68732,#68733,#68734,
#68735,#68736,#68737,#68738,#68739,#68740,#68741,#68742,#68743,#68744,#68745,
#68746,#68747,#68748,#68749,#68750,#68751,#68752,#68753,#68754,#68755,#68756,
#68757,#68758,#68759,#68760,#68761,#68762,#68763,#68764,#68765,#68766,#68767,
#68768,#68769,#68770,#68771,#68772,#68773,#68774,#68775,#68776,#68777,#68778,
#68779,#68780,#68781,#68782,#68783,#68784,#68785,#68786,#68787,#68788,#68789,
#68790,#68791,#68792,#68793,#68794,#68795,#68796,#68797,#68798,#68799,#68800,
#68801,#68802,#68803,#68804,#68805,#68806,#68807,#68808,#68809,#68810,#68811,
#68812,#68813,#68814,#68815,#68816,#68817,#68818,#68819,#68820,#68821),
 .UNSPECIFIED.,.F.,.F.,(4,3,3,3,3,3,3,3,3,3,3,3,3,3,3,3,3,3,3,3,3,3,3,3,
3,3,3,3,3,3,3,3,3,3,4),(-0.965990216419533,-0.930132396483882,-0.886600314752691,
-0.859427241407658,-0.844575649172136,-0.83450269382505,-0.791217440053876,
-0.748794152701163,-0.730233964484351,-0.71490535117285,-0.708744621568391,
-0.665691199232105,-0.622727628938354,-0.580003507011809,-0.5479604155669,
-0.535021607402038,-0.529041072836267,-0.487381790675506,-0.451831141232172,
-0.409951411560376,-0.367982065107459,-0.353448430125576,-0.345247061313217,
-0.304116472475951,-0.262917042414806,-0.222498465588061,-0.194686157389553,
-0.181409937644946,-0.17316340151046,-0.167260443835079,-0.125445332876309,
-0.0850027204681986,-0.0449509623998064,-0.00571310113625183,0.),
 .UNSPECIFIED.);
#1369=B_SPLINE_CURVE_WITH_KNOTS('',3,(#68822,#68823,#68824,#68825,#68826,
#68827,#68828,#68829,#68830,#68831,#68832,#68833,#68834,#68835,#68836,#68837,
#68838,#68839,#68840),.UNSPECIFIED.,.F.,.F.,(4,3,3,3,3,3,4),(-379.058849706002,
-378.560088061652,-378.061326417302,-377.063803128602,-376.066279839902,
-375.068756551202,-374.800863543725),.UNSPECIFIED.);
#1370=B_SPLINE_CURVE_WITH_KNOTS('',3,(#68897,#68898,#68899,#68900,#68901,
#68902,#68903),.UNSPECIFIED.,.F.,.F.,(4,3,4),(51.5745014586045,51.7886578973478,
52.2818832106559),.UNSPECIFIED.);
#1371=B_SPLINE_CURVE_WITH_KNOTS('',3,(#68906,#68907,#68908,#68909,#68910,
#68911,#68912,#68913,#68914,#68915),.UNSPECIFIED.,.F.,.F.,(4,3,3,4),(-50.2654824574367,
-49.3225313308074,-48.3360807041913,-47.8312715558983),.UNSPECIFIED.);
#1372=B_SPLINE_CURVE_WITH_KNOTS('',3,(#68920,#68921,#68922,#68923,#68924,
#68925,#68926,#68927,#68928,#68929,#68930,#68931,#68932,#68933,#68934,#68935,
#68936,#68937,#68938,#68939,#68940,#68941,#68942,#68943,#68944),
 .UNSPECIFIED.,.F.,.F.,(4,3,3,3,3,3,3,3,4),(45.291316151425,45.3767288243428,
46.363179450959,47.3496300775751,48.3360807041913,49.3225313308074,50.3089819574236,
51.2954325840397,51.5745014586045),.UNSPECIFIED.);
#1373=B_SPLINE_CURVE_WITH_KNOTS('',3,(#68945,#68946,#68947,#68948,#68949,
#68950,#68951,#68952,#68953,#68954,#68955,#68956,#68957,#68958,#68959,#68960,
#68961,#68962,#68963,#68964,#68965,#68966),.UNSPECIFIED.,.F.,.F.,(4,3,3,
3,3,3,3,4),(-47.8312715558983,-47.3496300775751,-46.363179450959,-45.3767288243428,
-44.3902781977267,-43.4038275711106,-42.4173769444944,-41.5480862487187),
 .UNSPECIFIED.);
#1374=B_SPLINE_CURVE_WITH_KNOTS('',3,(#68971,#68972,#68973,#68974,#68975,
#68976,#68977,#68978,#68979,#68980,#68981,#68982,#68983,#68984,#68985,#68986,
#68987,#68988,#68989,#68990,#68991,#68992),.UNSPECIFIED.,.F.,.F.,(4,3,3,
3,3,3,3,4),(39.0081308442454,39.458025064646,40.4444756912621,41.4309263178782,
42.4173769444944,43.4038275711105,44.3902781977267,45.291316151425),
 .UNSPECIFIED.);
#1375=B_SPLINE_CURVE_WITH_KNOTS('',3,(#68993,#68994,#68995,#68996,#68997,
#68998,#68999,#69000,#69001,#69002,#69003,#69004,#69005,#69006,#69007,#69008,
#69009,#69010,#69011,#69012,#69013,#69014,#69015,#69016,#69017),
 .UNSPECIFIED.,.F.,.F.,(4,3,3,3,3,3,3,3,4),(-41.5480862487187,-41.4309263178783,
-40.4444756912621,-39.458025064646,-38.4715744380298,-37.4851238114137,
-36.4986731847975,-35.5122225581814,-35.2649009415391),.UNSPECIFIED.);
#1376=B_SPLINE_CURVE_WITH_KNOTS('',3,(#69022,#69023,#69024,#69025,#69026,
#69027,#69028,#69029,#69030,#69031,#69032,#69033,#69034,#69035,#69036,#69037,
#69038,#69039,#69040,#69041,#69042,#69043),.UNSPECIFIED.,.F.,.F.,(4,3,3,
3,3,3,3,4),(32.7249455370658,33.5393213049491,34.5257719315652,35.5122225581814,
36.4986731847975,37.4851238114137,38.4715744380298,39.0081308442454),
 .UNSPECIFIED.);
#1377=B_SPLINE_CURVE_WITH_KNOTS('',3,(#69044,#69045,#69046,#69047,#69048,
#69049,#69050,#69051,#69052,#69053,#69054,#69055,#69056,#69057,#69058,#69059,
#69060,#69061,#69062,#69063,#69064,#69065),.UNSPECIFIED.,.F.,.F.,(4,3,3,
3,3,3,3,4),(-35.2649009415391,-34.5257719315652,-33.5393213049491,-32.5528706783329,
-31.5664200517168,-30.5799694251006,-29.5935187984845,-28.9817156343595),
 .UNSPECIFIED.);
#1378=B_SPLINE_CURVE_WITH_KNOTS('',3,(#69070,#69071,#69072,#69073,#69074,
#69075,#69076,#69077,#69078,#69079,#69080,#69081,#69082,#69083,#69084,#69085,
#69086,#69087,#69088,#69089,#69090,#69091,#69092,#69093,#69094),
 .UNSPECIFIED.,.F.,.F.,(4,3,3,3,3,3,3,3,4),(26.4417602298862,26.634166918636,
27.6206175452522,28.6070681718683,29.5935187984845,30.5799694251006,31.5664200517168,
32.5528706783329,32.7249455370658),.UNSPECIFIED.);
#1379=B_SPLINE_CURVE_WITH_KNOTS('',3,(#69095,#69096,#69097,#69098,#69099,
#69100,#69101,#69102,#69103,#69104,#69105,#69106,#69107,#69108,#69109,#69110,
#69111,#69112,#69113,#69114,#69115,#69116),.UNSPECIFIED.,.F.,.F.,(4,3,3,
3,3,3,3,4),(-28.9817156343595,-28.6070681718683,-27.6206175452522,-26.634166918636,
-25.6477162920199,-24.6612656654037,-23.6748150387876,-22.6985303271799),
 .UNSPECIFIED.);
#1380=B_SPLINE_CURVE_WITH_KNOTS('',3,(#69121,#69122,#69123,#69124,#69125,
#69126,#69127,#69128,#69129,#69130,#69131,#69132,#69133,#69134,#69135,#69136,
#69137,#69138,#69139,#69140,#69141,#69142),.UNSPECIFIED.,.F.,.F.,(4,3,3,
3,3,3,3,4),(20.1585749227066,20.7154631589391,21.7019137855553,22.6883644121714,
23.6748150387876,24.6612656654037,25.6477162920199,26.4417602298862),
 .UNSPECIFIED.);
#1381=B_SPLINE_CURVE_WITH_KNOTS('',3,(#69143,#69144,#69145,#69146,#69147,
#69148,#69149,#69150,#69151,#69152,#69153,#69154,#69155,#69156,#69157,#69158,
#69159,#69160,#69161,#69162,#69163,#69164,#69165,#69166,#69167),
 .UNSPECIFIED.,.F.,.F.,(4,3,3,3,3,3,3,3,4),(-22.6985303271799,-22.6883644121714,
-21.7019137855553,-20.7154631589391,-19.729012532323,-18.7425619057068,
-17.7561112790907,-16.7696606524745,-16.4153450200003),.UNSPECIFIED.);
#1382=B_SPLINE_CURVE_WITH_KNOTS('',3,(#69172,#69173,#69174,#69175,#69176,
#69177,#69178,#69179,#69180,#69181,#69182,#69183,#69184,#69185,#69186,#69187,
#69188,#69189,#69190,#69191,#69192,#69193),.UNSPECIFIED.,.F.,.F.,(4,3,3,
3,3,3,3,4),(13.875389615527,14.7967593992422,15.7832100258584,16.7696606524745,
17.7561112790907,18.7425619057068,19.729012532323,20.1585749227066),
 .UNSPECIFIED.);
#1383=B_SPLINE_CURVE_WITH_KNOTS('',3,(#69194,#69195,#69196,#69197,#69198,
#69199,#69200,#69201,#69202,#69203,#69204,#69205,#69206,#69207,#69208,#69209,
#69210,#69211,#69212,#69213,#69214,#69215),.UNSPECIFIED.,.F.,.F.,(4,3,3,
3,3,3,3,4),(-16.4153450200003,-15.7832100258584,-14.7967593992422,-13.8103087726261,
-12.8238581460099,-11.8374075193938,-10.8509568927776,-10.1321597128207),
 .UNSPECIFIED.);
#1384=B_SPLINE_CURVE_WITH_KNOTS('',3,(#69221,#69222,#69223,#69224,#69225,
#69226,#69227,#69228,#69229,#69230,#69231,#69232,#69233,#69234,#69235,#69236),
 .UNSPECIFIED.,.F.,.F.,(4,3,3,3,3,4),(-3.84897440564117,-2.95935187984845,
-1.9729012532323,-0.986450626616147,-0.493225313308074,0.),
 .UNSPECIFIED.);
#1385=B_SPLINE_CURVE_WITH_KNOTS('',3,(#69239,#69240,#69241,#69242,#69243,
#69244,#69245,#69246,#69247,#69248,#69249,#69250,#69251,#69252,#69253,#69254,
#69255,#69256,#69257),.UNSPECIFIED.,.F.,.F.,(4,3,3,3,3,3,4),(2.01640075321919,
2.95935187984845,3.9458025064646,4.93225313308074,5.9187037596969,6.90515438631305,
7.59220430834742),.UNSPECIFIED.);
#1386=B_SPLINE_CURVE_WITH_KNOTS('',3,(#69263,#69264,#69265,#69266,#69267,
#69268,#69269,#69270,#69271),.UNSPECIFIED.,.F.,.F.,(4,1,1,1,1,1,4),(59.6902604182061,
60.1950695664991,61.1815201931152,62.1679708197314,63.1544214463475,63.6476467596556,
64.1408720729637),.UNSPECIFIED.);
#1387=B_SPLINE_CURVE_WITH_KNOTS('',3,(#69274,#69275,#69276,#69277,#69278,
#69279,#69280,#69281,#69282),.UNSPECIFIED.,.F.,.F.,(4,1,1,1,1,1,4),(59.6902604182061,
59.7756730911239,60.7621237177401,61.7485743443562,62.7350249709724,63.7214755975885,
64.6644267242178),.UNSPECIFIED.);
#1388=B_SPLINE_CURVE_WITH_KNOTS('',3,(#69287,#69288,#69289,#69290,#69291,
#69292,#69293,#69294,#69295,#69296),.UNSPECIFIED.,.F.,.F.,(4,1,1,1,1,1,
1,4),(53.4070751110265,54.2763658068022,55.2628164334183,56.2492670600345,
57.2357176866506,58.2221683132668,59.2086189398829,59.6902604182061),
 .UNSPECIFIED.);
#1389=B_SPLINE_CURVE_WITH_KNOTS('',3,(#69297,#69298,#69299,#69300,#69301,
#69302,#69303,#69304,#69305,#69306),.UNSPECIFIED.,.F.,.F.,(4,1,1,1,1,1,
1,4),(53.4070751110265,53.856969331427,54.8434199580432,55.8298705846593,
56.8163212112755,57.8027718378916,58.7892224645078,59.6902604182061),
 .UNSPECIFIED.);
#1390=B_SPLINE_CURVE_WITH_KNOTS('',3,(#69311,#69312,#69313,#69314,#69315,
#69316,#69317,#69318,#69319,#69320,#69321),.UNSPECIFIED.,.F.,.F.,(4,1,1,
1,1,1,1,1,4),(47.1238898038469,47.3712114204891,48.3576620471053,49.3441126737214,
50.3305633003376,51.3170139269537,52.3034645535699,53.289915180186,53.4070751110265),
 .UNSPECIFIED.);
#1391=B_SPLINE_CURVE_WITH_KNOTS('',3,(#69322,#69323,#69324,#69325,#69326,
#69327,#69328,#69329,#69330,#69331),.UNSPECIFIED.,.F.,.F.,(4,1,1,1,1,1,
1,4),(47.1238898038469,47.9382655717301,48.9247161983463,49.9111668249625,
50.8976174515786,51.8840680781948,52.8705187048109,53.4070751110265),
 .UNSPECIFIED.);
#1392=B_SPLINE_CURVE_WITH_KNOTS('',3,(#69336,#69337,#69338,#69339,#69340,
#69341,#69342,#69343,#69344,#69345),.UNSPECIFIED.,.F.,.F.,(4,1,1,1,1,1,
1,4),(40.8407044966673,41.4525076607923,42.4389582874084,43.4254089140245,
44.4118595406407,45.3983101672568,46.384760793873,47.1238898038469),
 .UNSPECIFIED.);
#1393=B_SPLINE_CURVE_WITH_KNOTS('',3,(#69346,#69347,#69348,#69349,#69350,
#69351,#69352,#69353,#69354,#69355,#69356),.UNSPECIFIED.,.F.,.F.,(4,1,1,
1,1,1,1,1,4),(40.8407044966673,41.0331111854171,42.0195618120333,43.0060124386494,
43.9924630652656,44.9789136918817,45.9653643184979,46.951814945114,47.1238898038469),
 .UNSPECIFIED.);
#1394=B_SPLINE_CURVE_WITH_KNOTS('',3,(#69361,#69362,#69363,#69364,#69365,
#69366,#69367,#69368,#69369,#69370),.UNSPECIFIED.,.F.,.F.,(4,1,1,1,1,1,
1,4),(34.5575191894877,35.5338039010954,36.5202545277115,37.5067051543277,
38.4931557809438,39.47960640756,40.4660570341761,40.8407044966673),
 .UNSPECIFIED.);
#1395=B_SPLINE_CURVE_WITH_KNOTS('',3,(#69371,#69372,#69373,#69374,#69375,
#69376,#69377,#69378,#69379,#69380),.UNSPECIFIED.,.F.,.F.,(4,1,1,1,1,1,
1,4),(34.5575191894877,35.1144074257202,36.1008580523364,37.0873086789525,
38.0737593055687,39.0602099321848,40.046660558801,40.8407044966673),
 .UNSPECIFIED.);
#1396=B_SPLINE_CURVE_WITH_KNOTS('',3,(#69385,#69386,#69387,#69388,#69389,
#69390,#69391,#69392,#69393,#69394,#69395),.UNSPECIFIED.,.F.,.F.,(4,1,1,
1,1,1,1,1,4),(28.2743338823081,28.6286495147823,29.6151001413985,30.6015507680146,
31.5880013946308,32.5744520212469,33.5609026478631,34.5473532744792,34.5575191894877),
 .UNSPECIFIED.);
#1397=B_SPLINE_CURVE_WITH_KNOTS('',3,(#69396,#69397,#69398,#69399,#69400,
#69401,#69402,#69403,#69404,#69405),.UNSPECIFIED.,.F.,.F.,(4,1,1,1,1,1,
1,4),(28.2743338823081,29.1957036660233,30.1821542926395,31.1686049192556,
32.1550555458718,33.1415061724879,34.1279567991041,34.5575191894877),
 .UNSPECIFIED.);
#1398=B_SPLINE_CURVE_WITH_KNOTS('',3,(#69410,#69411,#69412,#69413,#69414,
#69415,#69416,#69417,#69418,#69419),.UNSPECIFIED.,.F.,.F.,(4,1,1,1,1,1,
1,4),(21.9911485751285,22.7099457550854,23.6963963817016,24.6828470083177,
25.6692976349339,26.65574826155,27.6421988881662,28.2743338823081),
 .UNSPECIFIED.);
#1399=B_SPLINE_CURVE_WITH_KNOTS('',3,(#69420,#69421,#69422,#69423,#69424,
#69425,#69426,#69427,#69428,#69429,#69430),.UNSPECIFIED.,.F.,.F.,(4,1,1,
1,1,1,1,1,4),(21.9911485751285,22.2905492797103,23.2769999063264,24.2634505329426,
25.2499011595587,26.2363517861749,27.222802412791,28.2092530394072,28.2743338823081),
 .UNSPECIFIED.);
#1400=B_SPLINE_CURVE_WITH_KNOTS('',3,(#69436,#69437,#69438,#69439,#69440,
#69441),.UNSPECIFIED.,.F.,.F.,(4,1,1,4),(14.3989442667811,14.8921695800892,
15.3853948933972,15.7079632679489),.UNSPECIFIED.);
#1401=B_SPLINE_CURVE_WITH_KNOTS('',3,(#69444,#69445,#69446,#69447,#69448),
 .UNSPECIFIED.,.F.,.F.,(4,1,4),(13.875389615527,14.8183407421562,15.7079632679489),
 .UNSPECIFIED.);
#1402=B_SPLINE_CURVE_WITH_KNOTS('',3,(#69450,#69451,#69452,#69453,#69454,
#69455,#69456,#69457,#69458,#69459,#69460),.UNSPECIFIED.,.F.,.F.,(4,1,1,
1,1,1,1,1,4),(15.7079632679489,15.8047913687724,16.7912419953885,17.7776926220047,
18.7641432486208,19.750593875237,20.7370445018531,21.7234951284693,21.9911485751285),
 .UNSPECIFIED.);
#1403=B_SPLINE_CURVE_WITH_KNOTS('',3,(#69461,#69462,#69463,#69464,#69465,
#69466,#69467,#69468,#69469,#69470),.UNSPECIFIED.,.F.,.F.,(4,1,1,1,1,1,
1,4),(15.7079632679489,16.3718455200134,17.3582961466295,18.3447467732457,
19.3311973998618,20.317648026478,21.3040986530941,21.9911485751285),
 .UNSPECIFIED.);
#1404=B_SPLINE_CURVE_WITH_KNOTS('',3,(#69703,#69704,#69705,#69706,#69707,
#69708,#69709,#69710,#69711,#69712,#69713,#69714,#69715,#69716,#69717,#69718,
#69719,#69720,#69721,#69722,#69723,#69724,#69725,#69726,#69727,#69728,#69729,
#69730,#69731,#69732,#69733,#69734,#69735,#69736,#69737,#69738,#69739,#69740,
#69741,#69742,#69743,#69744,#69745,#69746,#69747,#69748,#69749,#69750,#69751,
#69752,#69753,#69754,#69755,#69756,#69757,#69758,#69759,#69760,#69761,#69762,
#69763,#69764,#69765,#69766,#69767,#69768,#69769,#69770,#69771,#69772,#69773,
#69774,#69775,#69776,#69777,#69778,#69779,#69780,#69781,#69782,#69783,#69784,
#69785,#69786,#69787,#69788,#69789,#69790,#69791,#69792,#69793,#69794,#69795,
#69796,#69797,#69798,#69799,#69800,#69801,#69802,#69803,#69804,#69805,#69806,
#69807,#69808),.UNSPECIFIED.,.F.,.F.,(4,3,3,3,3,3,3,3,3,3,3,3,3,3,3,3,3,
3,3,3,3,3,3,3,3,3,3,3,3,3,3,3,3,3,3,4),(0.,0.0439873495596682,0.088535234885729,
0.133203648537345,0.177539443303643,0.193269018030229,0.199971189808446,
0.243934275067846,0.248071778815114,0.292055723719706,0.335717872507241,
0.374210944067843,0.384315712222397,0.391619070879034,0.434698852730331,
0.47712046629841,0.48969015874965,0.533088907914198,0.559308924386188,0.574291000021554,
0.57984588764462,0.62205897872085,0.66496509314549,0.707636118884185,0.738257750456918,
0.752576412624451,0.758605909671541,0.765028679465915,0.807111218921827,
0.843485707057882,0.85917048475052,0.866049641644265,0.873236607794053,
0.913787166992983,0.952609171466047,0.972375876542335),.UNSPECIFIED.);
#1405=B_SPLINE_CURVE_WITH_KNOTS('',3,(#69809,#69810,#69811,#69812,#69813,
#69814,#69815,#69816,#69817,#69818,#69819,#69820,#69821,#69822,#69823,#69824,
#69825,#69826,#69827,#69828,#69829,#69830,#69831,#69832,#69833,#69834,#69835,
#69836,#69837,#69838,#69839,#69840,#69841,#69842,#69843,#69844,#69845,#69846,
#69847,#69848,#69849,#69850,#69851,#69852,#69853,#69854,#69855,#69856,#69857,
#69858,#69859,#69860,#69861,#69862,#69863,#69864,#69865,#69866,#69867,#69868,
#69869,#69870,#69871,#69872,#69873,#69874,#69875,#69876,#69877,#69878,#69879,
#69880,#69881,#69882,#69883,#69884,#69885,#69886,#69887,#69888,#69889,#69890,
#69891,#69892,#69893,#69894,#69895,#69896,#69897,#69898,#69899,#69900,#69901,
#69902,#69903,#69904,#69905,#69906,#69907,#69908,#69909,#69910,#69911),
 .UNSPECIFIED.,.F.,.F.,(4,3,3,3,3,3,3,3,3,3,3,3,3,3,3,3,3,3,3,3,3,3,3,3,
3,3,3,3,3,3,3,3,3,3,4),(0.,0.0403422905180338,0.0813682734786595,0.122949980351713,
0.16449095941097,0.178014361827899,0.183409369411602,0.227186329885339,
0.269229509469957,0.311535350955759,0.348916065443153,0.357705618004978,
0.364415764229672,0.407315005273426,0.450191512111689,0.461058208905336,
0.503507289353387,0.531285871131442,0.541027225498738,0.546474827271459,
0.552442453195144,0.594916660917874,0.639047653028424,0.683117962531696,
0.716223791940519,0.731747366121405,0.738184546707727,0.782779716156374,
0.824075936567849,0.84301368069624,0.852796512264844,0.860145827789084,
0.904729831180339,0.947964597802275,0.97000658757344),.UNSPECIFIED.);
#1406=B_SPLINE_CURVE_WITH_KNOTS('',3,(#69912,#69913,#69914,#69915,#69916,
#69917,#69918,#69919,#69920,#69921,#69922,#69923,#69924,#69925,#69926,#69927,
#69928,#69929,#69930,#69931,#69932,#69933,#69934,#69935,#69936),
 .UNSPECIFIED.,.F.,.F.,(4,3,3,3,3,3,3,3,4),(-10.1321597128207,-9.86450626616149,
-8.87805563954534,-7.89160501292919,-6.90515438631305,-5.91870375969689,
-4.93225313308075,-3.94580250646459,-3.84897440564117),.UNSPECIFIED.);
#1407=B_SPLINE_CURVE_WITH_KNOTS('',3,(#70169,#70170,#70171,#70172,#70173,
#70174,#70175,#70176,#70177,#70178,#70179,#70180,#70181,#70182,#70183,#70184,
#70185,#70186,#70187,#70188,#70189,#70190,#70191,#70192,#70193,#70194,#70195,
#70196,#70197,#70198,#70199,#70200,#70201,#70202,#70203,#70204,#70205,#70206,
#70207,#70208,#70209,#70210,#70211,#70212,#70213,#70214,#70215,#70216,#70217,
#70218,#70219,#70220,#70221,#70222,#70223,#70224,#70225,#70226,#70227,#70228,
#70229,#70230,#70231,#70232,#70233,#70234,#70235,#70236,#70237,#70238,#70239,
#70240,#70241,#70242,#70243,#70244,#70245,#70246,#70247,#70248,#70249,#70250,
#70251,#70252,#70253,#70254,#70255,#70256,#70257,#70258,#70259,#70260,#70261,
#70262,#70263,#70264,#70265,#70266,#70267,#70268,#70269,#70270,#70271),
 .UNSPECIFIED.,.F.,.F.,(4,3,3,3,3,3,3,3,3,3,3,3,3,3,3,3,3,3,3,3,3,3,3,3,
3,3,3,3,3,3,3,3,3,3,4),(0.,0.0403420728543006,0.0813678367855401,0.122949539928715,
0.164490759249614,0.178014431809021,0.183409385478703,0.227186329885338,
0.269229949539637,0.311536068831159,0.348916603849705,0.357706091108837,
0.364415856383174,0.407315466341614,0.450192046682075,0.461058208905346,
0.5035070595844,0.531285655723017,0.541026743529684,0.54647402973548,0.552442268108838,
0.59491621056702,0.639047258971427,0.683117463220518,0.716223355043237,
0.731746708435023,0.738183753475272,0.782778798969233,0.824075248677492,
0.843013807341498,0.852796973522259,0.860145921094186,0.904729940902664,
0.947964597802271,0.970006587573432),.UNSPECIFIED.);
#1408=B_SPLINE_CURVE_WITH_KNOTS('',3,(#70272,#70273,#70274,#70275,#70276,
#70277,#70278,#70279,#70280,#70281,#70282,#70283,#70284,#70285,#70286,#70287,
#70288,#70289,#70290,#70291,#70292,#70293,#70294,#70295,#70296),
 .UNSPECIFIED.,.F.,.F.,(4,3,3,3,3,3,3,3,4),(7.59220430834742,7.89160501292919,
8.87805563954534,9.86450626616149,10.8509568927776,11.8374075193938,12.8238581460099,
13.8103087726261,13.875389615527),.UNSPECIFIED.);
#1409=B_SPLINE_CURVE_WITH_KNOTS('',3,(#70297,#70298,#70299,#70300,#70301,
#70302,#70303,#70304,#70305,#70306,#70307,#70308,#70309,#70310,#70311,#70312,
#70313,#70314,#70315,#70316,#70317,#70318,#70319,#70320,#70321,#70322,#70323,
#70324,#70325,#70326,#70327,#70328,#70329,#70330,#70331,#70332,#70333,#70334,
#70335,#70336,#70337,#70338,#70339,#70340,#70341,#70342,#70343,#70344,#70345,
#70346,#70347,#70348,#70349,#70350,#70351,#70352,#70353,#70354,#70355,#70356,
#70357,#70358,#70359,#70360,#70361,#70362,#70363,#70364,#70365,#70366,#70367,
#70368,#70369,#70370,#70371,#70372,#70373,#70374,#70375,#70376,#70377,#70378,
#70379,#70380,#70381,#70382,#70383,#70384,#70385,#70386,#70387,#70388,#70389,
#70390,#70391,#70392,#70393,#70394,#70395,#70396,#70397,#70398,#70399,#70400,
#70401,#70402),.UNSPECIFIED.,.F.,.F.,(4,3,3,3,3,3,3,3,3,3,3,3,3,3,3,3,3,
3,3,3,3,3,3,3,3,3,3,3,3,3,3,3,3,3,3,4),(0.,0.0439870213484189,0.0885347768590274,
0.133203573182163,0.177540067473735,0.193271868519026,0.199972102087808,
0.24393536506854,0.248071778815114,0.29205601261511,0.335718137618304,0.374211142901135,
0.3843154671772,0.391619008898289,0.434698890696845,0.477120259746675,0.489690158749629,
0.533088750991939,0.55930877727157,0.574290713387234,0.579845401630218,
0.622058272372198,0.664964305291723,0.707635330968564,0.738257061030748,
0.752575428668685,0.758604644157454,0.765028377494937,0.80711091192384,
0.843485476809388,0.85917031769407,0.86604942682694,0.87323655891021,0.913787164180478,
0.95260917146603,0.972375876542318),.UNSPECIFIED.);
#1410=B_SPLINE_CURVE_WITH_KNOTS('',3,(#70463,#70464,#70465,#70466,#70467,
#70468,#70469,#70470,#70471,#70472),.UNSPECIFIED.,.F.,.F.,(4,3,3,4),(-4.09293042013066,
-3.96748245563351,-2.97561184172513,-2.06863817490915),.UNSPECIFIED.);
#1411=B_SPLINE_CURVE_WITH_KNOTS('',3,(#70475,#70476,#70477,#70478,#70479,
#70480,#70481),.UNSPECIFIED.,.F.,.F.,(4,3,4),(0.,0.992711177740983,1.1173004083682),
 .UNSPECIFIED.);
#1412=B_SPLINE_CURVE_WITH_KNOTS('',3,(#70486,#70487,#70488,#70489,#70490,
#70491,#70492,#70493,#70494,#70495,#70496,#70497,#70498,#70499,#70500,#70501,
#70502,#70503,#70504,#70505,#70506,#70507),.UNSPECIFIED.,.F.,.F.,(4,3,3,
3,3,3,3,4),(-10.3761157273102,-9.91870613908378,-8.9268355251754,-7.93496491126702,
-6.94309429735864,-5.95122368345026,-4.95935306954189,-4.09293042013066),
 .UNSPECIFIED.);
#1413=B_SPLINE_CURVE_WITH_KNOTS('',3,(#70508,#70509,#70510,#70511,#70512,
#70513,#70514,#70515,#70516,#70517,#70518,#70519,#70520,#70521,#70522,#70523,
#70524,#70525,#70526,#70527,#70528,#70529),.UNSPECIFIED.,.F.,.F.,(4,3,3,
3,3,3,3,4),(1.1173004083682,1.98542235548196,2.97813353322293,3.97084471096391,
4.96355588870488,5.95626706644586,6.94897824418683,7.40048571554779),
 .UNSPECIFIED.);
#1414=B_SPLINE_CURVE_WITH_KNOTS('',3,(#70534,#70535,#70536,#70537,#70538,
#70539,#70540,#70541,#70542,#70543,#70544,#70545,#70546,#70547,#70548,#70549,
#70550,#70551,#70552,#70553,#70554,#70555),.UNSPECIFIED.,.F.,.F.,(4,3,3,
3,3,3,3,4),(-16.6593010344898,-15.869929822534,-14.8780592086257,-13.8861885947173,
-12.8943179808089,-11.9024473669005,-10.9105767529922,-10.3761157273102),
 .UNSPECIFIED.);
#1415=B_SPLINE_CURVE_WITH_KNOTS('',3,(#70556,#70557,#70558,#70559,#70560,
#70561,#70562,#70563,#70564,#70565,#70566,#70567,#70568,#70569,#70570,#70571,
#70572,#70573,#70574,#70575,#70576,#70577),.UNSPECIFIED.,.F.,.F.,(4,3,3,
3,3,3,3,4),(7.40048571554779,7.94168942192781,8.93440059966879,9.92711177740977,
10.9198229551507,11.9125341328917,12.9052453106327,13.6836710227274),
 .UNSPECIFIED.);
#1416=B_SPLINE_CURVE_WITH_KNOTS('',3,(#70582,#70583,#70584,#70585,#70586,
#70587,#70588,#70589,#70590,#70591,#70592,#70593,#70594,#70595,#70596,#70597,
#70598,#70599,#70600,#70601,#70602,#70603,#70604,#70605,#70606),
 .UNSPECIFIED.,.F.,.F.,(4,3,3,3,3,3,3,3,4),(-22.9424863416694,-22.8130241198927,
-21.8211535059843,-20.8292828920759,-19.8374122781676,-18.8455416642592,
-17.8536710503508,-16.8618004364424,-16.6593010344898),.UNSPECIFIED.);
#1417=B_SPLINE_CURVE_WITH_KNOTS('',3,(#70607,#70608,#70609,#70610,#70611,
#70612,#70613,#70614,#70615,#70616,#70617,#70618,#70619,#70620,#70621,#70622,
#70623,#70624,#70625,#70626,#70627,#70628,#70629,#70630,#70631),
 .UNSPECIFIED.,.F.,.F.,(4,3,3,3,3,3,3,3,4),(13.6836710227274,13.8979564883737,
14.8906676661147,15.8833788438556,16.8760900215966,17.8688011993376,18.8615123770786,
19.8542235548195,19.966856329907),.UNSPECIFIED.);
#1418=B_SPLINE_CURVE_WITH_KNOTS('',3,(#70636,#70637,#70638,#70639,#70640,
#70641,#70642,#70643,#70644,#70645,#70646,#70647,#70648,#70649,#70650,#70651,
#70652,#70653,#70654,#70655,#70656,#70657),.UNSPECIFIED.,.F.,.F.,(4,3,3,
3,3,3,3,4),(-29.225671648849,-28.764247803343,-27.7723771894346,-26.7805065755262,
-25.7886359616178,-24.7967653477094,-23.8048947338011,-22.9424863416694),
 .UNSPECIFIED.);
#1419=B_SPLINE_CURVE_WITH_KNOTS('',3,(#70658,#70659,#70660,#70661,#70662,
#70663,#70664,#70665,#70666,#70667,#70668,#70669,#70670,#70671,#70672,#70673,
#70674,#70675,#70676,#70677,#70678,#70679),.UNSPECIFIED.,.F.,.F.,(4,3,3,
3,3,3,3,4),(19.966856329907,20.8469347325605,21.8396459103015,22.8323570880425,
23.8250682657834,24.8177794435244,25.8104906212654,26.2500416370865),
 .UNSPECIFIED.);
#1420=B_SPLINE_CURVE_WITH_KNOTS('',3,(#70684,#70685,#70686,#70687,#70688,
#70689,#70690,#70691,#70692,#70693,#70694,#70695,#70696,#70697,#70698,#70699,
#70700,#70701,#70702,#70703,#70704,#70705),.UNSPECIFIED.,.F.,.F.,(4,3,3,
3,3,3,3,4),(-35.5088569560286,-34.7154714867932,-33.7236008728848,-32.7317302589765,
-31.7398596450681,-30.7479890311597,-29.7561184172513,-29.225671648849),
 .UNSPECIFIED.);
#1421=B_SPLINE_CURVE_WITH_KNOTS('',3,(#70706,#70707,#70708,#70709,#70710,
#70711,#70712,#70713,#70714,#70715,#70716,#70717,#70718,#70719,#70720,#70721,
#70722,#70723,#70724,#70725,#70726,#70727),.UNSPECIFIED.,.F.,.F.,(4,3,3,
3,3,3,3,4),(26.2500416370865,26.8032017990064,27.7959129767474,28.7886241544883,
29.7813353322293,30.7740465099703,31.7667576877113,32.5332269442661),
 .UNSPECIFIED.);
#1422=B_SPLINE_CURVE_WITH_KNOTS('',3,(#70732,#70733,#70734,#70735,#70736,
#70737,#70738,#70739,#70740,#70741,#70742,#70743,#70744,#70745,#70746,#70747,
#70748,#70749,#70750,#70751,#70752,#70753,#70754,#70755,#70756),
 .UNSPECIFIED.,.F.,.F.,(4,3,3,3,3,3,3,3,4),(-41.7920422632082,-41.6585657841519,
-40.6666951702435,-39.6748245563351,-38.6829539424267,-37.6910833285184,
-36.69921271461,-35.7073421007016,-35.5088569560286),.UNSPECIFIED.);
#1423=B_SPLINE_CURVE_WITH_KNOTS('',3,(#70757,#70758,#70759,#70760,#70761,
#70762,#70763,#70764,#70765,#70766,#70767,#70768,#70769,#70770,#70771,#70772,
#70773,#70774,#70775,#70776,#70777,#70778,#70779,#70780,#70781),
 .UNSPECIFIED.,.F.,.F.,(4,3,3,3,3,3,3,3,4),(32.5332269442661,32.7594688654522,
33.7521800431932,34.7448912209342,35.7376023986752,36.7303135764161,37.7230247541571,
38.7157359318981,38.8164122514457),.UNSPECIFIED.);
#1424=B_SPLINE_CURVE_WITH_KNOTS('',3,(#70786,#70787,#70788,#70789,#70790,
#70791,#70792,#70793,#70794,#70795,#70796,#70797,#70798,#70799,#70800,#70801,
#70802,#70803,#70804,#70805,#70806,#70807),.UNSPECIFIED.,.F.,.F.,(4,3,3,
3,3,3,3,4),(-48.0752275703878,-47.6097894676021,-46.6179188536938,-45.6260482397854,
-44.634177625877,-43.6423070119686,-42.6504363980602,-41.7920422632082),
 .UNSPECIFIED.);
#1425=B_SPLINE_CURVE_WITH_KNOTS('',3,(#70808,#70809,#70810,#70811,#70812,
#70813,#70814,#70815,#70816,#70817,#70818,#70819,#70820,#70821,#70822,#70823,
#70824,#70825,#70826,#70827,#70828,#70829),.UNSPECIFIED.,.F.,.F.,(4,3,3,
3,3,3,3,4),(38.8164122514457,39.7084471096391,40.7011582873801,41.693869465121,
42.686580642862,43.679291820603,44.672002998344,45.0995975586253),
 .UNSPECIFIED.);
#1426=B_SPLINE_CURVE_WITH_KNOTS('',3,(#70834,#70835,#70836,#70837,#70838,
#70839,#70840,#70841,#70842,#70843,#70844,#70845,#70846,#70847,#70848,#70849,
#70850,#70851,#70852,#70853,#70854,#70855),.UNSPECIFIED.,.F.,.F.,(4,3,3,
3,3,3,3,4),(-54.3584128775674,-53.5610131510524,-52.569142537144,-51.5772719232356,
-50.5854013093273,-49.5935306954189,-48.6016600815105,-48.0752275703878),
 .UNSPECIFIED.);
#1427=B_SPLINE_CURVE_WITH_KNOTS('',3,(#70856,#70857,#70858,#70859,#70860,
#70861,#70862,#70863,#70864,#70865,#70866,#70867,#70868,#70869,#70870,#70871,
#70872,#70873,#70874,#70875,#70876,#70877),.UNSPECIFIED.,.F.,.F.,(4,3,3,
3,3,3,3,4),(45.0995975586253,45.6647141760849,46.6574253538259,47.6501365315669,
48.6428477093079,49.6355588870488,50.6282700647898,51.3827828658049),
 .UNSPECIFIED.);
#1428=B_SPLINE_CURVE_WITH_KNOTS('',3,(#70882,#70883,#70884,#70885,#70886,
#70887,#70888,#70889,#70890,#70891,#70892,#70893,#70894,#70895,#70896,#70897,
#70898,#70899,#70900,#70901,#70902,#70903,#70904,#70905,#70906),
 .UNSPECIFIED.,.F.,.F.,(4,3,3,3,3,3,3,3,4),(-60.641598184747,-60.5041074484111,
-59.5122368345027,-58.5203662205943,-57.5284956066859,-56.5366249927775,
-55.5447543788692,-54.5528837649608,-54.3584128775674),.UNSPECIFIED.);
#1429=B_SPLINE_CURVE_WITH_KNOTS('',3,(#70907,#70908,#70909,#70910,#70911,
#70912,#70913,#70914,#70915,#70916,#70917,#70918,#70919,#70920,#70921,#70922,
#70923,#70924,#70925,#70926,#70927,#70928,#70929,#70930,#70931),
 .UNSPECIFIED.,.F.,.F.,(4,3,3,3,3,3,3,3,4),(51.3827828658049,51.6209812425308,
52.6136924202718,53.6064035980127,54.5991147757537,55.5918259534947,56.5845371312357,
57.5772483089767,57.6659681729845),.UNSPECIFIED.);
#1430=B_SPLINE_CURVE_WITH_KNOTS('',3,(#70936,#70937,#70938,#70939,#70940,
#70941,#70942,#70943,#70944,#70945,#70946,#70947,#70948,#70949,#70950,#70951,
#70952,#70953,#70954,#70955,#70956,#70957),.UNSPECIFIED.,.F.,.F.,(4,3,3,
3,3,3,3,4),(-66.9247834919266,-66.4553311318613,-65.4634605179529,-64.4715899040445,
-63.4797192901362,-62.4878486762278,-61.4959780623194,-60.641598184747),
 .UNSPECIFIED.);
#1431=B_SPLINE_CURVE_WITH_KNOTS('',3,(#70958,#70959,#70960,#70961,#70962,
#70963,#70964,#70965,#70966,#70967,#70968,#70969,#70970,#70971,#70972,#70973,
#70974,#70975,#70976,#70977,#70978,#70979),.UNSPECIFIED.,.F.,.F.,(4,3,3,
3,3,3,3,4),(57.6659681729845,58.5699594867177,59.5626706644586,60.5553818421996,
61.5480930199406,62.5408041976816,63.5335153754225,63.9491534801641),
 .UNSPECIFIED.);
#1432=B_SPLINE_CURVE_WITH_KNOTS('',3,(#70984,#70985,#70986,#70987,#70988,
#70989,#70990,#70991,#70992,#70993,#70994,#70995,#70996,#70997,#70998,#70999,
#71000,#71001,#71002,#71003,#71004,#71005),.UNSPECIFIED.,.F.,.F.,(4,3,3,
3,3,3,3,4),(-73.2079687991062,-72.4065548153116,-71.4146842014032,-70.4228135874948,
-69.4309429735864,-68.4390723596781,-67.4472017457697,-66.9247834919266),
 .UNSPECIFIED.);
#1433=B_SPLINE_CURVE_WITH_KNOTS('',3,(#71006,#71007,#71008,#71009,#71010,
#71011,#71012,#71013,#71014,#71015,#71016,#71017,#71018,#71019,#71020,#71021,
#71022,#71023,#71024,#71025,#71026,#71027),.UNSPECIFIED.,.F.,.F.,(4,3,3,
3,3,3,3,4),(63.9491534801641,64.5262265531635,65.5189377309045,66.5116489086455,
67.5043600863864,68.4970712641274,69.4897824418684,70.2323387873437),
 .UNSPECIFIED.);
#1434=B_SPLINE_CURVE_WITH_KNOTS('',3,(#71032,#71033,#71034,#71035,#71036,
#71037,#71038,#71039,#71040,#71041,#71042,#71043,#71044,#71045,#71046,#71047,
#71048,#71049,#71050,#71051,#71052,#71053,#71054,#71055,#71056),
 .UNSPECIFIED.,.F.,.F.,(4,3,3,3,3,3,3,3,4),(-79.4911541062857,-79.3496491126702,
-78.3577784987618,-77.3659078848535,-76.3740372709451,-75.3821666570367,
-74.3902960431283,-73.3984254292199,-73.2079687991062),.UNSPECIFIED.);
#1435=B_SPLINE_CURVE_WITH_KNOTS('',3,(#71057,#71058,#71059,#71060,#71061,
#71062,#71063,#71064,#71065,#71066,#71067,#71068,#71069,#71070,#71071,#71072,
#71073,#71074,#71075,#71076,#71077,#71078,#71079,#71080,#71081),
 .UNSPECIFIED.,.F.,.F.,(4,3,3,3,3,3,3,3,4),(70.2323387873437,70.4824936196094,
71.4752047973503,72.4679159750913,73.4606271528323,74.4533383305733,75.4460495083142,
76.4387606860552,76.5155240945233),.UNSPECIFIED.);
#1436=B_SPLINE_CURVE_WITH_KNOTS('',3,(#71086,#71087,#71088,#71089,#71090,
#71091,#71092,#71093,#71094,#71095,#71096,#71097,#71098,#71099,#71100,#71101,
#71102,#71103,#71104,#71105,#71106,#71107),.UNSPECIFIED.,.F.,.F.,(4,3,3,
3,3,3,3,4),(-85.7743394134653,-85.3008727961205,-84.3090021822121,-83.3171315683037,
-82.3252609543953,-81.333390340487,-80.3415197265786,-79.4911541062857),
 .UNSPECIFIED.);
#1437=B_SPLINE_CURVE_WITH_KNOTS('',3,(#71108,#71109,#71110,#71111,#71112,
#71113,#71114,#71115,#71116,#71117,#71118,#71119,#71120,#71121,#71122,#71123,
#71124,#71125,#71126,#71127,#71128,#71129),.UNSPECIFIED.,.F.,.F.,(4,3,3,
3,3,3,3,4),(76.5155240945233,77.4314718637962,78.4241830415372,79.4168942192782,
80.4096053970191,81.4023165747601,82.3950277525011,82.7987094017029),
 .UNSPECIFIED.);
#1438=B_SPLINE_CURVE_WITH_KNOTS('',3,(#71134,#71135,#71136,#71137,#71138,
#71139,#71140,#71141,#71142,#71143,#71144,#71145,#71146,#71147,#71148,#71149,
#71150,#71151,#71152,#71153,#71154,#71155),.UNSPECIFIED.,.F.,.F.,(4,3,3,
3,3,3,3,4),(-92.0575247206449,-91.2520964795708,-90.2602258656624,-89.268355251754,
-88.2764846378456,-87.2846140239373,-86.2927434100289,-85.7743394134653),
 .UNSPECIFIED.);
#1439=B_SPLINE_CURVE_WITH_KNOTS('',3,(#71156,#71157,#71158,#71159,#71160,
#71161,#71162,#71163,#71164,#71165,#71166,#71167,#71168,#71169,#71170,#71171,
#71172,#71173,#71174,#71175,#71176,#71177),.UNSPECIFIED.,.F.,.F.,(4,3,3,
3,3,3,3,4),(82.7987094017029,83.3877389302421,84.380450107983,85.373161285724,
86.365872463465,87.358583641206,88.351294818947,89.0818947088825),
 .UNSPECIFIED.);
#1440=B_SPLINE_CURVE_WITH_KNOTS('',3,(#71183,#71184,#71185,#71186,#71187,
#71188,#71189,#71190,#71191,#71192),.UNSPECIFIED.,.F.,.F.,(4,1,1,1,1,1,
1,4),(103.672557568463,103.858999941297,104.850870555206,105.842741169114,
106.834611783022,107.826482396931,108.818353010839,109.810223624748),
 .UNSPECIFIED.);
#1441=B_SPLINE_CURVE_WITH_KNOTS('',3,(#71195,#71196,#71197,#71198,#71199,
#71200,#71201,#71202),.UNSPECIFIED.,.F.,.F.,(4,1,1,1,1,4),(103.672557568463,
104.600461793276,105.593172971017,106.585884148758,107.578595326499,108.57130650424),
 .UNSPECIFIED.);
#1442=B_SPLINE_CURVE_WITH_KNOTS('',3,(#71207,#71208,#71209,#71210,#71211,
#71212,#71213,#71214,#71215,#71216),.UNSPECIFIED.,.F.,.F.,(4,1,1,1,1,1,
1,4),(97.3893722612836,97.9077762578471,98.8996468717555,99.8915174856638,
100.883388099572,101.875258713481,102.867129327389,103.672557568463),
 .UNSPECIFIED.);
#1443=B_SPLINE_CURVE_WITH_KNOTS('',3,(#71217,#71218,#71219,#71220,#71221,
#71222,#71223,#71224,#71225,#71226,#71227),.UNSPECIFIED.,.F.,.F.,(4,1,1,
1,1,1,1,1,4),(97.3893722612836,97.6514835490889,98.6441947268299,99.6369059045709,
100.629617082312,101.622328260053,102.615039437794,103.607750615535,103.672557568463),
 .UNSPECIFIED.);
#1444=B_SPLINE_CURVE_WITH_KNOTS('',3,(#71232,#71233,#71234,#71235,#71236,
#71237,#71238,#71239,#71240,#71241),.UNSPECIFIED.,.F.,.F.,(4,1,1,1,1,1,
1,4),(91.106186954104,91.9565525743968,92.9484231883052,93.9402938022136,
94.9321644161219,95.9240350300303,96.9159056439387,97.3893722612836),
 .UNSPECIFIED.);
#1445=B_SPLINE_CURVE_WITH_KNOTS('',3,(#71242,#71243,#71244,#71245,#71246,
#71247,#71248,#71249,#71250,#71251),.UNSPECIFIED.,.F.,.F.,(4,1,1,1,1,1,
1,4),(91.106186954104,91.6952164826431,92.687927660384,93.680638838125,
94.673350015866,95.666061193607,96.658772371348,97.3893722612836),
 .UNSPECIFIED.);
#1446=B_SPLINE_CURVE_WITH_KNOTS('',3,(#71256,#71257,#71258,#71259,#71260,
#71261,#71262,#71263,#71264,#71265,#71266),.UNSPECIFIED.,.F.,.F.,(4,1,1,
1,1,1,1,1,4),(84.8230016469244,85.0134582770382,86.0053288909465,86.9971995048549,
87.9890701187633,88.9809407326717,89.9728113465801,90.9646819604884,91.106186954104),
 .UNSPECIFIED.);
#1447=B_SPLINE_CURVE_WITH_KNOTS('',3,(#71267,#71268,#71269,#71270,#71271,
#71272,#71273,#71274,#71275,#71276),.UNSPECIFIED.,.F.,.F.,(4,1,1,1,1,1,
1,4),(84.8230016469244,85.7389494161972,86.7316605939382,87.7243717716792,
88.7170829494201,89.7097941271611,90.7025053049021,91.106186954104),
 .UNSPECIFIED.);
#1448=B_SPLINE_CURVE_WITH_KNOTS('',3,(#71281,#71282,#71283,#71284,#71285,
#71286,#71287,#71288,#71289,#71290),.UNSPECIFIED.,.F.,.F.,(4,1,1,1,1,1,
1,4),(78.5398163397448,79.0622345935879,80.0541052074963,81.0459758214047,
82.037846435313,83.0297170492214,84.0215876631298,84.8230016469244),
 .UNSPECIFIED.);
#1449=B_SPLINE_CURVE_WITH_KNOTS('',3,(#71291,#71292,#71293,#71294,#71295,
#71296,#71297,#71298,#71299,#71300,#71301),.UNSPECIFIED.,.F.,.F.,(4,1,1,
1,1,1,1,1,4),(78.5398163397448,78.7899711720104,79.7826823497514,80.7753935274923,
81.7681047052333,82.7608158829743,83.7535270607153,84.7462382384562,84.8230016469244),
 .UNSPECIFIED.);
#1450=B_SPLINE_CURVE_WITH_KNOTS('',3,(#71306,#71307,#71308,#71309,#71310,
#71311,#71312,#71313,#71314,#71315),.UNSPECIFIED.,.F.,.F.,(4,1,1,1,1,1,
1,4),(72.2566310325652,73.1110109101376,74.102881524046,75.0947521379544,
76.0866227518628,77.0784933657711,78.0703639796795,78.5398163397448),
 .UNSPECIFIED.);
#1451=B_SPLINE_CURVE_WITH_KNOTS('',3,(#71316,#71317,#71318,#71319,#71320,
#71321,#71322,#71323,#71324,#71325),.UNSPECIFIED.,.F.,.F.,(4,1,1,1,1,1,
1,4),(72.2566310325652,72.8337041055645,73.8264152833055,74.8191264610465,
75.8118376387874,76.8045488165284,77.7972599942694,78.5398163397448),
 .UNSPECIFIED.);
#1452=B_SPLINE_CURVE_WITH_KNOTS('',3,(#71330,#71331,#71332,#71333,#71334,
#71335,#71336,#71337,#71338,#71339,#71340),.UNSPECIFIED.,.F.,.F.,(4,1,1,
1,1,1,1,1,4),(65.9734457253856,66.167916612779,67.1597872266874,68.1516578405957,
69.1435284545041,70.1353990684125,71.1272696823209,72.1191402962293,72.2566310325652),
 .UNSPECIFIED.);
#1453=B_SPLINE_CURVE_WITH_KNOTS('',3,(#71341,#71342,#71343,#71344,#71345,
#71346,#71347,#71348,#71349,#71350),.UNSPECIFIED.,.F.,.F.,(4,1,1,1,1,1,
1,4),(65.9734457253856,66.8774370391187,67.8701482168596,68.8628593946006,
69.8555705723416,70.8482817500825,71.8409929278235,72.2566310325652),
 .UNSPECIFIED.);
#1454=B_SPLINE_CURVE_WITH_KNOTS('',3,(#71355,#71356,#71357,#71358,#71359,
#71360,#71361,#71362,#71363,#71364),.UNSPECIFIED.,.F.,.F.,(4,1,1,1,1,1,
1,4),(59.6902604182061,60.2166929293287,61.2085635432371,62.2004341571455,
63.1923047710539,64.1841753849622,65.1760459988706,65.9734457253856),
 .UNSPECIFIED.);
#1455=B_SPLINE_CURVE_WITH_KNOTS('',3,(#71365,#71366,#71367,#71368,#71369,
#71370,#71371,#71372,#71373,#71374,#71375),.UNSPECIFIED.,.F.,.F.,(4,1,1,
1,1,1,1,1,4),(59.690260418206,59.9284587949318,60.9211699726728,61.9138811504138,
62.9065923281547,63.8993035058957,64.8920146836367,65.8847258613777,65.9734457253856),
 .UNSPECIFIED.);
#1456=B_SPLINE_CURVE_WITH_KNOTS('',3,(#71380,#71381,#71382,#71383,#71384,
#71385,#71386,#71387,#71388,#71389),.UNSPECIFIED.,.F.,.F.,(4,1,1,1,1,1,
1,4),(53.4070751110265,54.2654692458785,55.2573398597868,56.2492104736952,
57.2410810876036,58.232951701512,59.2248223154203,59.6902604182061),
 .UNSPECIFIED.);
#1457=B_SPLINE_CURVE_WITH_KNOTS('',3,(#71390,#71391,#71392,#71393,#71394,
#71395,#71396,#71397,#71398,#71399),.UNSPECIFIED.,.F.,.F.,(4,1,1,1,1,1,
1,4),(53.4070751110264,53.972191728486,54.9649029062269,55.9576140839679,
56.9503252617089,57.9430364394499,58.9357476171908,59.690260418206),
 .UNSPECIFIED.);
#1458=B_SPLINE_CURVE_WITH_KNOTS('',3,(#71404,#71405,#71406,#71407,#71408,
#71409,#71410,#71411,#71412,#71413,#71414),.UNSPECIFIED.,.F.,.F.,(4,1,1,
1,1,1,1,1,4),(47.1238898038469,47.3223749485198,48.3142455624282,49.3061161763366,
50.2979867902449,51.2898574041533,52.2817280180617,53.2735986319701,53.4070751110265),
 .UNSPECIFIED.);
#1459=B_SPLINE_CURVE_WITH_KNOTS('',3,(#71415,#71416,#71417,#71418,#71419,
#71420,#71421,#71422,#71423,#71424),.UNSPECIFIED.,.F.,.F.,(4,1,1,1,1,1,
1,4),(47.1238898038468,48.0159246620401,49.0086358397811,50.001347017522,
50.994058195263,51.986769373004,52.979480550745,53.4070751110264),
 .UNSPECIFIED.);
#1460=B_SPLINE_CURVE_WITH_KNOTS('',3,(#71429,#71430,#71431,#71432,#71433,
#71434,#71435,#71436,#71437,#71438),.UNSPECIFIED.,.F.,.F.,(4,1,1,1,1,1,
1,4),(40.8407044966673,41.3711512650695,42.3630218789779,43.3548924928863,
44.3467631067947,45.3386337207031,46.3305043346114,47.1238898038469),
 .UNSPECIFIED.);
#1461=B_SPLINE_CURVE_WITH_KNOTS('',3,(#71439,#71440,#71441,#71442,#71443,
#71444,#71445,#71446,#71447,#71448,#71449),.UNSPECIFIED.,.F.,.F.,(4,1,1,
1,1,1,1,1,4),(40.8407044966672,41.0669464178533,42.0596575955942,43.0523687733352,
44.0450799510762,45.0377911288172,46.0305023065581,47.0232134842991,47.1238898038468),
 .UNSPECIFIED.);
#1462=B_SPLINE_CURVE_WITH_KNOTS('',3,(#71454,#71455,#71456,#71457,#71458,
#71459,#71460,#71461,#71462,#71463),.UNSPECIFIED.,.F.,.F.,(4,1,1,1,1,1,
1,4),(34.5575191894877,35.4199275816193,36.4117981955277,37.403668809436,
38.3955394233444,39.3874100372528,40.3792806511612,40.8407044966673),
 .UNSPECIFIED.);
#1463=B_SPLINE_CURVE_WITH_KNOTS('',3,(#71464,#71465,#71466,#71467,#71468,
#71469,#71470,#71471,#71472,#71473),.UNSPECIFIED.,.F.,.F.,(4,1,1,1,1,1,
1,4),(34.5575191894876,35.1106793514074,36.1033905291484,37.0961017068893,
38.0888128846303,39.0815240623713,40.0742352401123,40.8407044966672),
 .UNSPECIFIED.);
#1464=B_SPLINE_CURVE_WITH_KNOTS('',3,(#71478,#71479,#71480,#71481,#71482,
#71483,#71484,#71485,#71486,#71487,#71488),.UNSPECIFIED.,.F.,.F.,(4,1,1,
1,1,1,1,1,4),(28.2743338823081,28.4768332842606,29.468703898169,30.4605745120774,
31.4524451259858,32.4443157398941,33.4361863538025,34.4280569677109,34.5575191894877),
 .UNSPECIFIED.);
#1465=B_SPLINE_CURVE_WITH_KNOTS('',3,(#71489,#71490,#71491,#71492,#71493,
#71494,#71495,#71496,#71497,#71498),.UNSPECIFIED.,.F.,.F.,(4,1,1,1,1,1,
1,4),(28.2743338823081,29.1544122849615,30.1471234627025,31.1398346404435,
32.1325458181845,33.1252569959254,34.1179681736664,34.5575191894876),
 .UNSPECIFIED.);
#1466=B_SPLINE_CURVE_WITH_KNOTS('',3,(#71503,#71504,#71505,#71506,#71507,
#71508,#71509,#71510,#71511,#71512),.UNSPECIFIED.,.F.,.F.,(4,1,1,1,1,1,
1,4),(21.9911485751285,22.5256096008104,23.5174802147187,24.5093508286271,
25.5012214425355,26.4930920564439,27.4849626703523,28.2743338823081),
 .UNSPECIFIED.);
#1467=B_SPLINE_CURVE_WITH_KNOTS('',3,(#71513,#71514,#71515,#71516,#71517,
#71518,#71519,#71520,#71521,#71522,#71523),.UNSPECIFIED.,.F.,.F.,(4,1,1,
1,1,1,1,1,4),(21.9911485751285,22.2054340407747,23.1981452185157,24.1908563962566,
25.1835675739976,26.1762787517386,27.1689899294796,28.1617011072206,28.2743338823081),
 .UNSPECIFIED.);
#1468=B_SPLINE_CURVE_WITH_KNOTS('',3,(#71528,#71529,#71530,#71531,#71532,
#71533,#71534,#71535,#71536,#71537),.UNSPECIFIED.,.F.,.F.,(4,1,1,1,1,1,
1,4),(15.7079632679489,16.5743859173601,17.5662565312685,18.5581271451769,
19.5499977590852,20.5418683729936,21.533738986902,21.9911485751285),
 .UNSPECIFIED.);
#1469=B_SPLINE_CURVE_WITH_KNOTS('',3,(#71538,#71539,#71540,#71541,#71542,
#71543,#71544,#71545,#71546,#71547),.UNSPECIFIED.,.F.,.F.,(4,1,1,1,1,1,
1,4),(15.7079632679489,16.2491669743288,17.2418781520698,18.2345893298108,
19.2273005075518,20.2200116852927,21.2127228630337,21.9911485751285),
 .UNSPECIFIED.);
#1470=B_SPLINE_CURVE_WITH_KNOTS('',3,(#71550,#71551,#71552,#71553,#71554,
#71555,#71556,#71557,#71558,#71559,#71560,#71561,#71562,#71563,#71564,#71565,
#71566,#71567,#71568,#71569,#71570,#71571,#71572,#71573,#71574,#71575,#71576,
#71577,#71578,#71579,#71580,#71581,#71582,#71583,#71584,#71585,#71586,#71587,
#71588,#71589,#71590,#71591,#71592,#71593,#71594,#71595,#71596,#71597,#71598,
#71599,#71600,#71601,#71602,#71603,#71604,#71605,#71606,#71607,#71608,#71609,
#71610,#71611,#71612,#71613,#71614,#71615,#71616,#71617,#71618,#71619,#71620,
#71621,#71622,#71623,#71624,#71625,#71626,#71627,#71628,#71629,#71630,#71631,
#71632,#71633,#71634,#71635,#71636,#71637,#71638,#71639,#71640,#71641,#71642,
#71643,#71644,#71645,#71646,#71647,#71648,#71649,#71650,#71651,#71652,#71653,
#71654,#71655,#71656,#71657,#71658,#71659,#71660,#71661,#71662,#71663,#71664,
#71665,#71666,#71667,#71668,#71669,#71670,#71671,#71672,#71673,#71674,#71675,
#71676,#71677,#71678,#71679,#71680,#71681,#71682,#71683,#71684,#71685,#71686,
#71687,#71688,#71689,#71690,#71691,#71692,#71693,#71694,#71695,#71696,#71697,
#71698,#71699,#71700,#71701,#71702,#71703,#71704,#71705,#71706,#71707,#71708,
#71709,#71710,#71711,#71712,#71713,#71714,#71715,#71716,#71717,#71718,#71719,
#71720,#71721,#71722,#71723,#71724,#71725,#71726,#71727,#71728,#71729,#71730,
#71731,#71732,#71733,#71734,#71735,#71736,#71737,#71738,#71739,#71740,#71741,
#71742,#71743,#71744,#71745,#71746,#71747,#71748,#71749,#71750,#71751,#71752,
#71753,#71754,#71755,#71756,#71757,#71758,#71759,#71760,#71761,#71762,#71763,
#71764,#71765,#71766,#71767,#71768,#71769),.UNSPECIFIED.,.F.,.F.,(4,3,3,
3,3,3,3,3,3,3,3,3,3,3,3,3,3,3,3,3,3,3,3,3,3,3,3,3,3,3,3,3,3,3,3,3,3,3,3,
3,3,3,3,3,3,3,3,3,3,3,3,3,3,3,3,3,3,3,3,3,3,3,3,3,3,3,3,3,3,3,3,3,3,4),
(-1.5115530493723,-1.48679433039677,-1.46137997144481,-1.44936627203976,
-1.44203978844916,-1.43723948275662,-1.41130482704604,-1.3851425648951,
-1.36907979899106,-1.36528335260342,-1.33883417182409,-1.31251413265359,
-1.29083745680875,-1.27999911888633,-1.27252822943752,-1.26916078096391,
-1.2438409010096,-1.21777622976252,-1.19264806966918,-1.18165449962834,
-1.17500808302858,-1.17140113753098,-1.14461626345551,-1.11752388424601,
-1.09233065043846,-1.08197947093734,-1.07663416157974,-1.07221334700158,
-1.04448214800868,-1.01675094901579,-0.989899829038698,-0.980534050538336,
-0.975142748268706,-0.971473262423844,-0.944367339171939,-0.916829945945447,
-0.889160172398661,-0.878253059899969,-0.87283587922991,-0.869128423226553,
-0.840502786522066,-0.812629809126308,-0.785184824902654,-0.776260550181423,
-0.769615191493828,-0.76539079696697,-0.754625876408607,-0.727617533495154,
-0.699889836956671,-0.672733437279935,-0.663027286995113,-0.658922109894078,
-0.630659562625353,-0.602060824740566,-0.57220527844112,-0.560770556686858,
-0.556383058918736,-0.552005977862112,-0.523133364911618,-0.494697204184849,
-0.482638639542781,-0.454174910522506,-0.448377858002803,-0.443883394073885,
-0.415482165359649,-0.386508614853008,-0.357316612716015,-0.340170191390177,
-0.335377465438287,-0.305918315871394,-0.27645436453335,-0.247645675491356,
-0.226999958751525,-0.219677966288016),.UNSPECIFIED.);
#1471=B_SPLINE_CURVE_WITH_KNOTS('',3,(#71771,#71772,#71773,#71774,#71775,
#71776,#71777,#71778,#71779,#71780,#71781,#71782,#71783,#71784,#71785,#71786,
#71787,#71788,#71789,#71790,#71791,#71792,#71793,#71794,#71795,#71796,#71797,
#71798,#71799,#71800,#71801,#71802,#71803,#71804,#71805,#71806,#71807,#71808,
#71809,#71810,#71811,#71812,#71813,#71814,#71815,#71816,#71817,#71818,#71819,
#71820,#71821,#71822,#71823,#71824,#71825,#71826,#71827,#71828,#71829,#71830,
#71831,#71832,#71833,#71834),.UNSPECIFIED.,.F.,.F.,(4,3,3,3,3,3,3,3,3,3,
3,3,3,3,3,3,3,3,3,3,3,4),(-0.410648750433038,-0.381296088292737,-0.350882391849445,
-0.328072119516976,-0.310964415267624,-0.305842993500878,-0.301661871504881,
-0.274116258800685,-0.259641302519569,-0.231392457082299,-0.202468399947011,
-0.198019208917011,-0.170841895434807,-0.143725312403613,-0.117042212888725,
-0.102411936277635,-0.097195049751494,-0.0935363835720784,-0.0677899334604712,
-0.0424347820407558,-0.0178142542830924,0.),.UNSPECIFIED.);
#1472=B_SPLINE_CURVE_WITH_KNOTS('',3,(#71837,#71838,#71839,#71840,#71841,
#71842,#71843,#71844,#71845,#71846,#71847,#71848,#71849,#71850,#71851,#71852,
#71853,#71854,#71855,#71856,#71857,#71858,#71859,#71860,#71861,#71862,#71863,
#71864,#71865,#71866,#71867),.UNSPECIFIED.,.F.,.F.,(4,3,3,3,3,3,3,3,3,3,
4),(-0.219677966288016,-0.201006229477425,-0.172158028090248,-0.142713390739092,
-0.124874216896705,-0.114789665948937,-0.110082687886506,-0.0803547102951982,
-0.0502957032480209,-0.0203907630638487,0.),.UNSPECIFIED.);
#1473=B_SPLINE_CURVE_WITH_KNOTS('',3,(#72280,#72281,#72282,#72283,#72284,
#72285,#72286,#72287),.UNSPECIFIED.,.F.,.F.,(4,1,1,1,1,4),(11.6150328478182,
12.6069034617266,13.598774075635,14.5906446895433,15.5825153034517,15.7079632679489),
 .UNSPECIFIED.);
#1474=B_SPLINE_CURVE_WITH_KNOTS('',3,(#72288,#72289,#72290,#72291,#72292,
#72293,#72294,#72295,#72296,#72297,#72298,#72299,#72300,#72301,#72302,#72303,
#72304,#72305,#72306,#72307,#72308,#72309,#72310,#72311,#72312,#72313,#72314,
#72315,#72316,#72317,#72318,#72319,#72320,#72321,#72322,#72323,#72324,#72325,
#72326,#72327,#72328,#72329,#72330,#72331,#72332,#72333,#72334,#72335,#72336,
#72337,#72338,#72339,#72340,#72341,#72342,#72343,#72344,#72345,#72346,#72347,
#72348,#72349,#72350,#72351,#72352,#72353,#72354,#72355,#72356,#72357,#72358,
#72359,#72360,#72361,#72362,#72363,#72364,#72365,#72366,#72367,#72368,#72369,
#72370,#72371,#72372,#72373,#72374,#72375),.UNSPECIFIED.,.F.,.F.,(4,3,3,
3,3,3,3,3,3,3,3,3,3,3,3,3,3,3,3,3,3,3,3,3,3,3,3,3,3,4),(-0.552745378375041,
-0.527830263536694,-0.498419933292456,-0.482944277728704,-0.477004703287069,
-0.471889411648522,-0.442842142020847,-0.418838054802294,-0.408336266644177,
-0.40199148464016,-0.397446251891128,-0.369139848009071,-0.341087780585202,
-0.313931322984348,-0.298150853306366,-0.293754274173184,-0.266922432864957,
-0.250809444272419,-0.223433348051691,-0.19550417954523,-0.19139998392206,
-0.164790719651446,-0.138164593558308,-0.11192170155777,-0.0979314888630491,
-0.0936568444848153,-0.0680692021908508,-0.0428602319276656,-0.0184469101431373,
0.),.UNSPECIFIED.);
#1475=B_SPLINE_CURVE_WITH_KNOTS('',3,(#72376,#72377,#72378,#72379,#72380,
#72381,#72382,#72383,#72384,#72385,#72386,#72387,#72388,#72389,#72390,#72391,
#72392,#72393,#72394),.UNSPECIFIED.,.F.,.F.,(4,3,3,3,3,3,4),(-96.6808425304193,
-96.2114495491126,-95.2195789352043,-94.2277083212959,-93.2358377073875,
-92.2439670934791,-92.0575247206449),.UNSPECIFIED.);
#1476=B_SPLINE_CURVE_WITH_KNOTS('',3,(#72397,#72398,#72399,#72400,#72401,
#72402,#72403,#72404,#72405),.UNSPECIFIED.,.F.,.F.,(4,1,1,1,1,1,4),(10.3761157273101,
11.2856110856239,12.2783222633649,13.2710334411059,14.2637446188469,15.2564557965878,
15.7079632679489),.UNSPECIFIED.);
#1477=B_SPLINE_CURVE_WITH_KNOTS('',3,(#72823,#72824,#72825,#72826,#72827,
#72828,#72829,#72830,#72831,#72832,#72833,#72834,#72835,#72836,#72837,#72838,
#72839,#72840,#72841,#72842,#72843,#72844),.UNSPECIFIED.,.F.,.F.,(4,3,3,
3,3,3,3,4),(89.0818947088825,89.3440059966879,90.3367171744289,91.3294283521699,
92.3221395299109,93.3148507076518,94.3075618853928,94.6122043555102),
 .UNSPECIFIED.);
#1478=B_SPLINE_CURVE_WITH_KNOTS('',3,(#72845,#72846,#72847,#72848,#72849,
#72850,#72851,#72852,#72853,#72854,#72855,#72856,#72857,#72858,#72859,#72860,
#72861,#72862,#72863,#72864,#72865,#72866,#72867,#72868,#72869,#72870,#72871,
#72872,#72873,#72874,#72875,#72876,#72877,#72878,#72879,#72880,#72881,#72882,
#72883,#72884,#72885,#72886,#72887,#72888,#72889,#72890,#72891,#72892,#72893,
#72894,#72895,#72896,#72897,#72898,#72899,#72900,#72901,#72902,#72903,#72904,
#72905,#72906,#72907,#72908,#72909,#72910,#72911,#72912,#72913,#72914,#72915,
#72916,#72917,#72918,#72919,#72920,#72921,#72922,#72923,#72924,#72925,#72926,
#72927,#72928,#72929,#72930,#72931,#72932),.UNSPECIFIED.,.F.,.F.,(4,3,3,
3,3,3,3,3,3,3,3,3,3,3,3,3,3,3,3,3,3,3,3,3,3,3,3,3,3,4),(-0.555272788399392,
-0.535208229286056,-0.51046000550438,-0.495927663091087,-0.490771565699598,
-0.464551573131573,-0.44160907963455,-0.431518091480653,-0.425427657470475,
-0.420791193383041,-0.394188077983384,-0.365893964776387,-0.344673379871139,
-0.328757941192203,-0.324434111993057,-0.296521822210165,-0.281011625155395,
-0.254049889550291,-0.226554106924644,-0.220947145848259,-0.216688100237889,
-0.188737539857684,-0.160250957640402,-0.131525362881473,-0.114279480489655,
-0.109581292141837,-0.0801117384511396,-0.0505679692714886,-0.0215915474943119,
0.),.UNSPECIFIED.);
#1479=B_SPLINE_CURVE_WITH_KNOTS('',3,(#72986,#72987,#72988,#72989),
 .UNSPECIFIED.,.F.,.F.,(4,4),(126.973269284569,127.68065103662),
 .UNSPECIFIED.);
#1480=B_SPLINE_CURVE_WITH_KNOTS('',3,(#72992,#72993,#72994,#72995,#72996,
#72997,#72998,#72999,#73000,#73001),.UNSPECIFIED.,.F.,.F.,(4,3,3,4),(-125.663706143592,
-124.688135777949,-123.690630691726,-123.229495242053),.UNSPECIFIED.);
#1481=B_SPLINE_CURVE_WITH_KNOTS('',3,(#73006,#73007,#73008,#73009,#73010,
#73011,#73012,#73013,#73014,#73015,#73016,#73017,#73018,#73019,#73020,#73021,
#73022,#73023,#73024,#73025,#73026,#73027,#73028,#73029,#73030),
 .UNSPECIFIED.,.F.,.F.,(4,3,3,3,3,3,3,3,4),(120.690083977389,120.698115433055,
121.695620519279,122.693125605502,123.690630691726,124.688135777949,125.685640864173,
126.683145950397,126.973269284569),.UNSPECIFIED.);
#1482=B_SPLINE_CURVE_WITH_KNOTS('',3,(#73031,#73032,#73033,#73034,#73035,
#73036,#73037,#73038,#73039,#73040,#73041,#73042,#73043,#73044,#73045,#73046,
#73047,#73048,#73049,#73050,#73051,#73052),.UNSPECIFIED.,.F.,.F.,(4,3,3,
3,3,3,3,4),(-123.229495242053,-122.693125605502,-121.695620519279,-120.698115433055,
-119.700610346831,-118.703105260608,-117.705600174384,-116.946309934874),
 .UNSPECIFIED.);
#1483=B_SPLINE_CURVE_WITH_KNOTS('',3,(#73057,#73058,#73059,#73060,#73061,
#73062,#73063,#73064,#73065,#73066,#73067,#73068,#73069,#73070,#73071,#73072,
#73073,#73074,#73075,#73076,#73077,#73078),.UNSPECIFIED.,.F.,.F.,(4,3,3,
3,3,3,3,4),(114.40689867021,114.713084915713,115.710590001937,116.708095088161,
117.705600174384,118.703105260608,119.700610346831,120.690083977389),
 .UNSPECIFIED.);
#1484=B_SPLINE_CURVE_WITH_KNOTS('',3,(#73079,#73080,#73081,#73082,#73083,
#73084,#73085,#73086,#73087,#73088,#73089,#73090,#73091,#73092,#73093,#73094,
#73095,#73096,#73097,#73098,#73099,#73100,#73101,#73102,#73103),
 .UNSPECIFIED.,.F.,.F.,(4,3,3,3,3,3,3,3,4),(-116.946309934874,-116.708095088161,
-115.710590001937,-114.713084915713,-113.71557982949,-112.718074743266,
-111.720569657043,-110.723064570819,-110.663124627694),.UNSPECIFIED.);
#1485=B_SPLINE_CURVE_WITH_KNOTS('',3,(#73108,#73109,#73110,#73111,#73112,
#73113,#73114,#73115,#73116,#73117,#73118,#73119,#73120,#73121,#73122,#73123,
#73124,#73125,#73126,#73127,#73128,#73129),.UNSPECIFIED.,.F.,.F.,(4,3,3,
3,3,3,3,4),(108.12371336303,108.728054398372,109.725559484595,110.723064570819,
111.720569657043,112.718074743266,113.71557982949,114.40689867021),
 .UNSPECIFIED.);
#1486=B_SPLINE_CURVE_WITH_KNOTS('',3,(#73130,#73131,#73132,#73133,#73134,
#73135,#73136,#73137,#73138,#73139,#73140,#73141,#73142,#73143,#73144,#73145,
#73146,#73147,#73148,#73149,#73150,#73151),.UNSPECIFIED.,.F.,.F.,(4,3,3,
3,3,3,3,4),(-110.663124627694,-109.725559484595,-108.728054398372,-107.730549312148,
-106.733044225925,-105.735539139701,-104.738034053478,-104.379939320515),
 .UNSPECIFIED.);
#1487=B_SPLINE_CURVE_WITH_KNOTS('',3,(#73156,#73157,#73158,#73159,#73160,
#73161,#73162,#73163,#73164,#73165,#73166,#73167,#73168,#73169,#73170,#73171,
#73172,#73173,#73174,#73175,#73176,#73177),.UNSPECIFIED.,.F.,.F.,(4,3,3,
3,3,3,3,4),(101.840528055851,102.74302388103,103.740528967254,104.738034053477,
105.735539139701,106.733044225925,107.730549312148,108.12371336303),
 .UNSPECIFIED.);
#1488=B_SPLINE_CURVE_WITH_KNOTS('',3,(#73178,#73179,#73180,#73181,#73182,
#73183,#73184,#73185,#73186,#73187,#73188,#73189,#73190,#73191,#73192,#73193,
#73194,#73195,#73196,#73197,#73198,#73199),.UNSPECIFIED.,.F.,.F.,(4,3,3,
3,3,3,3,4),(-104.379939320515,-103.740528967254,-102.74302388103,-101.745518794807,
-100.748013708583,-99.7505086223595,-98.7530035361359,-98.0967540133351),
 .UNSPECIFIED.);
#1489=B_SPLINE_CURVE_WITH_KNOTS('',3,(#73204,#73205,#73206,#73207,#73208,
#73209,#73210,#73211,#73212,#73213,#73214,#73215,#73216,#73217,#73218,#73219,
#73220,#73221,#73222,#73223,#73224,#73225,#73226,#73227,#73228),
 .UNSPECIFIED.,.F.,.F.,(4,3,3,3,3,3,3,3,4),(95.5573427486709,95.7604882774651,
96.7579933636887,97.7554984499123,98.7530035361359,99.7505086223595,100.748013708583,
101.745518794807,101.840528055851),.UNSPECIFIED.);
#1490=B_SPLINE_CURVE_WITH_KNOTS('',3,(#73229,#73230,#73231,#73232,#73233,
#73234,#73235,#73236,#73237,#73238,#73239,#73240,#73241,#73242,#73243,#73244,
#73245,#73246,#73247,#73248,#73249,#73250),.UNSPECIFIED.,.F.,.F.,(4,3,3,
3,3,3,3,4),(-98.0967540133351,-97.7554984499123,-96.7579933636887,-95.7604882774651,
-94.7629831912415,-93.7654781050179,-92.7679730187944,-91.8135687061555),
 .UNSPECIFIED.);
#1491=B_SPLINE_CURVE_WITH_KNOTS('',3,(#73255,#73256,#73257,#73258,#73259,
#73260,#73261,#73262,#73263,#73264,#73265,#73266,#73267,#73268,#73269,#73270,
#73271,#73272,#73273,#73274,#73275,#73276),.UNSPECIFIED.,.F.,.F.,(4,3,3,
3,3,3,3,4),(89.2741574414913,89.7754577601236,90.7729628463471,91.7704679325708,
92.7679730187943,93.7654781050179,94.7629831912415,95.5573427486709),
 .UNSPECIFIED.);
#1492=B_SPLINE_CURVE_WITH_KNOTS('',3,(#73277,#73278,#73279,#73280,#73281,
#73282,#73283,#73284,#73285,#73286,#73287,#73288,#73289,#73290,#73291,#73292,
#73293,#73294,#73295,#73296,#73297,#73298,#73299,#73300,#73301),
 .UNSPECIFIED.,.F.,.F.,(4,3,3,3,3,3,3,3,4),(-91.8135687061555,-91.7704679325708,
-90.7729628463472,-89.7754577601236,-88.7779526739,-87.7804475876764,-86.7829425014528,
-85.7854374152292,-85.5303833989759),.UNSPECIFIED.);
#1493=B_SPLINE_CURVE_WITH_KNOTS('',3,(#73306,#73307,#73308,#73309,#73310,
#73311,#73312,#73313,#73314,#73315,#73316,#73317,#73318,#73319,#73320,#73321,
#73322,#73323,#73324,#73325,#73326,#73327),.UNSPECIFIED.,.F.,.F.,(4,3,3,
3,3,3,3,4),(82.9909721343117,83.790427242782,84.7879323290056,85.7854374152292,
86.7829425014528,87.7804475876764,88.7779526739,89.2741574414913),
 .UNSPECIFIED.);
#1494=B_SPLINE_CURVE_WITH_KNOTS('',3,(#73328,#73329,#73330,#73331,#73332,
#73333,#73334,#73335,#73336,#73337,#73338,#73339,#73340,#73341,#73342,#73343,
#73344,#73345,#73346,#73347,#73348,#73349),.UNSPECIFIED.,.F.,.F.,(4,3,3,
3,3,3,3,4),(-85.5303833989759,-84.7879323290056,-83.790427242782,-82.7929221565584,
-81.7954170703348,-80.7979119841112,-79.8004068978876,-79.2471980917963),
 .UNSPECIFIED.);
#1495=B_SPLINE_CURVE_WITH_KNOTS('',3,(#73354,#73355,#73356,#73357,#73358,
#73359,#73360,#73361,#73362,#73363,#73364,#73365,#73366,#73367,#73368,#73369,
#73370,#73371,#73372,#73373,#73374,#73375,#73376,#73377,#73378),
 .UNSPECIFIED.,.F.,.F.,(4,3,3,3,3,3,3,3,4),(76.7077868271321,76.8078916392168,
77.8053967254404,78.802901811664,79.8004068978876,80.7979119841112,81.7954170703348,
82.7929221565584,82.9909721343117),.UNSPECIFIED.);
#1496=B_SPLINE_CURVE_WITH_KNOTS('',3,(#73379,#73380,#73381,#73382,#73383,
#73384,#73385,#73386,#73387,#73388,#73389,#73390,#73391,#73392,#73393,#73394,
#73395,#73396,#73397,#73398,#73399,#73400),.UNSPECIFIED.,.F.,.F.,(4,3,3,
3,3,3,3,4),(-79.2471980917963,-78.802901811664,-77.8053967254404,-76.8078916392168,
-75.8103865529932,-74.8128814667696,-73.815376380546,-72.9640127846167),
 .UNSPECIFIED.);
#1497=B_SPLINE_CURVE_WITH_KNOTS('',3,(#73405,#73406,#73407,#73408,#73409,
#73410,#73411,#73412,#73413,#73414,#73415,#73416,#73417,#73418,#73419,#73420,
#73421,#73422,#73423,#73424,#73425,#73426),.UNSPECIFIED.,.F.,.F.,(4,3,3,
3,3,3,3,4),(70.4246015199526,70.8228611218752,71.8203662080989,72.8178712943224,
73.815376380546,74.8128814667696,75.8103865529932,76.7077868271321),
 .UNSPECIFIED.);
#1498=B_SPLINE_CURVE_WITH_KNOTS('',3,(#73427,#73428,#73429,#73430,#73431,
#73432,#73433,#73434,#73435,#73436,#73437,#73438,#73439,#73440,#73441,#73442,
#73443,#73444,#73445,#73446,#73447,#73448,#73449,#73450,#73451),
 .UNSPECIFIED.,.F.,.F.,(4,3,3,3,3,3,3,3,4),(-72.9640127846167,-72.8178712943224,
-71.8203662080988,-70.8228611218752,-69.8253560356517,-68.8278509494281,
-67.8303458632045,-66.8328407769809,-66.6808274774371),.UNSPECIFIED.);
#1499=B_SPLINE_CURVE_WITH_KNOTS('',3,(#73456,#73457,#73458,#73459,#73460,
#73461,#73462,#73463,#73464,#73465,#73466,#73467,#73468,#73469,#73470,#73471,
#73472,#73473,#73474,#73475,#73476,#73477),.UNSPECIFIED.,.F.,.F.,(4,3,3,
3,3,3,3,4),(64.141416212773,64.8378306045337,65.8353356907573,66.8328407769809,
67.8303458632045,68.8278509494281,69.8253560356517,70.4246015199526),
 .UNSPECIFIED.);
#1500=B_SPLINE_CURVE_WITH_KNOTS('',3,(#73478,#73479,#73480,#73481,#73482,
#73483,#73484,#73485,#73486,#73487,#73488,#73489,#73490,#73491,#73492,#73493,
#73494,#73495,#73496,#73497,#73498,#73499),.UNSPECIFIED.,.F.,.F.,(4,3,3,
3,3,3,3,4),(-66.6808274774371,-65.8353356907573,-64.8378306045337,-63.8403255183101,
-62.8428204320865,-61.8453153458629,-60.8478102596393,-60.3976421702575),
 .UNSPECIFIED.);
#1501=B_SPLINE_CURVE_WITH_KNOTS('',3,(#73504,#73505,#73506,#73507,#73508,
#73509,#73510,#73511,#73512,#73513,#73514,#73515,#73516,#73517,#73518,#73519,
#73520,#73521,#73522,#73523,#73524,#73525),.UNSPECIFIED.,.F.,.F.,(4,3,3,
3,3,3,3,4),(57.8582309055934,58.8528000871921,59.8503051734157,60.8478102596393,
61.8453153458629,62.8428204320865,63.8403255183101,64.141416212773),
 .UNSPECIFIED.);
#1502=B_SPLINE_CURVE_WITH_KNOTS('',3,(#73526,#73527,#73528,#73529,#73530,
#73531,#73532,#73533,#73534,#73535,#73536,#73537,#73538,#73539,#73540,#73541,
#73542,#73543,#73544,#73545,#73546,#73547),.UNSPECIFIED.,.F.,.F.,(4,3,3,
3,3,3,3,4),(-60.3976421702575,-59.8503051734157,-58.8528000871921,-57.8552950009685,
-56.8577899147449,-55.8602848285214,-54.8627797422977,-54.1144568630779),
 .UNSPECIFIED.);
#1503=B_SPLINE_CURVE_WITH_KNOTS('',3,(#73552,#73553,#73554,#73555,#73556,
#73557,#73558,#73559,#73560,#73561,#73562,#73563,#73564,#73565,#73566,#73567,
#73568,#73569,#73570,#73571,#73572,#73573,#73574,#73575,#73576),
 .UNSPECIFIED.,.F.,.F.,(4,3,3,3,3,3,3,3,4),(51.5750455984138,51.8702644836269,
52.8677695698506,53.8652746560741,54.8627797422977,55.8602848285213,56.8577899147449,
57.8552950009686,57.8582309055934),.UNSPECIFIED.);
#1504=B_SPLINE_CURVE_WITH_KNOTS('',3,(#73577,#73578,#73579,#73580,#73581,
#73582,#73583,#73584,#73585,#73586,#73587,#73588,#73589,#73590,#73591,#73592,
#73593,#73594,#73595,#73596,#73597,#73598,#73599,#73600,#73601),
 .UNSPECIFIED.,.F.,.F.,(4,3,3,3,3,3,3,3,4),(-54.1144568630779,-53.8652746560741,
-52.8677695698505,-51.870264483627,-50.8727593974034,-49.8752543111798,
-48.8777492249562,-47.8802441387326,-47.8312715558983),.UNSPECIFIED.);
#1505=B_SPLINE_CURVE_WITH_KNOTS('',3,(#73606,#73607,#73608,#73609,#73610,
#73611,#73612,#73613,#73614,#73615,#73616,#73617,#73618,#73619,#73620,#73621,
#73622,#73623,#73624,#73625,#73626,#73627),.UNSPECIFIED.,.F.,.F.,(4,3,3,
3,3,3,3,4),(45.2918602912342,45.8852339662854,46.882739052509,47.8802441387326,
48.8777492249562,49.8752543111798,50.8727593974034,51.5750455984138),
 .UNSPECIFIED.);
#1506=B_SPLINE_CURVE_WITH_KNOTS('',3,(#73628,#73629,#73630,#73631,#73632,
#73633,#73634,#73635,#73636,#73637,#73638,#73639,#73640,#73641,#73642,#73643,
#73644,#73645,#73646,#73647,#73648,#73649),.UNSPECIFIED.,.F.,.F.,(4,3,3,
3,3,3,3,4),(-47.8312715558983,-46.882739052509,-45.8852339662854,-44.8877288800618,
-43.8902237938382,-42.8927187076146,-41.895213621391,-41.5480862487187),
 .UNSPECIFIED.);
#1507=B_SPLINE_CURVE_WITH_KNOTS('',3,(#73654,#73655,#73656,#73657,#73658,
#73659,#73660,#73661,#73662,#73663,#73664,#73665,#73666,#73667,#73668,#73669,
#73670,#73671,#73672,#73673,#73674,#73675),.UNSPECIFIED.,.F.,.F.,(4,3,3,
3,3,3,3,4),(39.0086749840546,39.9002034489438,40.8977085351674,41.895213621391,
42.8927187076146,43.8902237938382,44.8877288800618,45.2918602912342),
 .UNSPECIFIED.);
#1508=B_SPLINE_CURVE_WITH_KNOTS('',3,(#73676,#73677,#73678,#73679,#73680,
#73681,#73682,#73683,#73684,#73685,#73686,#73687,#73688,#73689,#73690,#73691,
#73692,#73693,#73694,#73695,#73696,#73697),.UNSPECIFIED.,.F.,.F.,(4,3,3,
3,3,3,3,4),(-41.5480862487187,-40.8977085351674,-39.9002034489438,-38.9026983627202,
-37.9051932764966,-36.907688190273,-35.9101831040494,-35.2649009415391),
 .UNSPECIFIED.);
#1509=B_SPLINE_CURVE_WITH_KNOTS('',3,(#73702,#73703,#73704,#73705,#73706,
#73707,#73708,#73709,#73710,#73711,#73712,#73713,#73714,#73715,#73716,#73717,
#73718,#73719,#73720,#73721,#73722,#73723,#73724,#73725,#73726),
 .UNSPECIFIED.,.F.,.F.,(4,3,3,3,3,3,3,3,4),(32.725489676875,32.9176678453786,
33.9151729316022,34.9126780178258,35.9101831040494,36.907688190273,37.9051932764966,
38.9026983627202,39.0086749840546),.UNSPECIFIED.);
#1510=B_SPLINE_CURVE_WITH_KNOTS('',3,(#73727,#73728,#73729,#73730,#73731,
#73732,#73733,#73734,#73735,#73736,#73737,#73738,#73739,#73740,#73741,#73742,
#73743,#73744,#73745,#73746,#73747,#73748),.UNSPECIFIED.,.F.,.F.,(4,3,3,
3,3,3,3,4),(-35.2649009415391,-34.9126780178258,-33.9151729316022,-32.9176678453786,
-31.920162759155,-30.9226576729315,-29.9251525867079,-28.9817156343596),
 .UNSPECIFIED.);
#1511=B_SPLINE_CURVE_WITH_KNOTS('',3,(#73753,#73754,#73755,#73756,#73757,
#73758,#73759,#73760,#73761,#73762,#73763,#73764,#73765,#73766,#73767,#73768,
#73769,#73770,#73771,#73772,#73773,#73774),.UNSPECIFIED.,.F.,.F.,(4,3,3,
3,3,3,3,4),(26.4423043696954,26.9326373280371,27.9301424142607,28.9276475004843,
29.9251525867079,30.9226576729315,31.920162759155,32.725489676875),
 .UNSPECIFIED.);
#1512=B_SPLINE_CURVE_WITH_KNOTS('',3,(#73775,#73776,#73777,#73778,#73779,
#73780,#73781,#73782,#73783,#73784,#73785,#73786,#73787,#73788,#73789,#73790,
#73791,#73792,#73793,#73794,#73795,#73796,#73797,#73798,#73799),
 .UNSPECIFIED.,.F.,.F.,(4,3,3,3,3,3,3,3,4),(-28.9817156343596,-28.9276475004843,
-27.9301424142607,-26.9326373280371,-25.9351322418135,-24.9376271555899,
-23.9401220693663,-22.9426169831427,-22.69853032718),.UNSPECIFIED.);
#1513=B_SPLINE_CURVE_WITH_KNOTS('',3,(#73804,#73805,#73806,#73807,#73808,
#73809,#73810,#73811,#73812,#73813,#73814,#73815,#73816,#73817,#73818,#73819,
#73820,#73821,#73822,#73823,#73824,#73825),.UNSPECIFIED.,.F.,.F.,(4,3,3,
3,3,3,3,4),(20.1591190625158,20.9476068106955,21.9451118969191,22.9426169831427,
23.9401220693663,24.9376271555899,25.9351322418135,26.4423043696954),
 .UNSPECIFIED.);
#1514=B_SPLINE_CURVE_WITH_KNOTS('',3,(#73826,#73827,#73828,#73829,#73830,
#73831,#73832,#73833,#73834,#73835,#73836,#73837,#73838,#73839,#73840,#73841,
#73842,#73843,#73844,#73845,#73846,#73847),.UNSPECIFIED.,.F.,.F.,(4,3,3,
3,3,3,3,4),(-22.69853032718,-21.9451118969191,-20.9476068106955,-19.9501017244719,
-18.9525966382483,-17.9550915520247,-16.9575864658011,-16.4153450200004),
 .UNSPECIFIED.);
#1515=B_SPLINE_CURVE_WITH_KNOTS('',3,(#73852,#73853,#73854,#73855,#73856,
#73857,#73858,#73859,#73860,#73861,#73862,#73863,#73864,#73865,#73866,#73867,
#73868,#73869,#73870,#73871,#73872,#73873,#73874,#73875,#73876),
 .UNSPECIFIED.,.F.,.F.,(4,3,3,3,3,3,3,3,4),(13.8759337553362,13.9650712071303,
14.9625762933539,15.9600813795775,16.9575864658011,17.9550915520247,18.9525966382483,
19.9501017244719,20.1591190625158),.UNSPECIFIED.);
#1516=B_SPLINE_CURVE_WITH_KNOTS('',3,(#73877,#73878,#73879,#73880,#73881,
#73882,#73883,#73884,#73885,#73886,#73887,#73888,#73889,#73890,#73891,#73892,
#73893,#73894,#73895,#73896,#73897,#73898),.UNSPECIFIED.,.F.,.F.,(4,3,3,
3,3,3,3,4),(-16.4153450200004,-15.9600813795775,-14.9625762933539,-13.9650712071303,
-12.9675661209067,-11.9700610346831,-10.9725559484595,-10.1321597128208),
 .UNSPECIFIED.);
#1517=B_SPLINE_CURVE_WITH_KNOTS('',3,(#73904,#73905,#73906,#73907,#73908,
#73909,#73910,#73911,#73912,#73913,#73914,#73915,#73916),.UNSPECIFIED.,
 .F.,.F.,(4,3,3,3,4),(-3.8489744056412,-2.99251525867078,-1.99501017244719,
-0.997505086223591,0.),.UNSPECIFIED.);
#1518=B_SPLINE_CURVE_WITH_KNOTS('',3,(#73919,#73920,#73921,#73922,#73923,
#73924,#73925,#73926,#73927,#73928,#73929,#73930,#73931,#73932,#73933,#73934,
#73935,#73936,#73937),.UNSPECIFIED.,.F.,.F.,(4,3,3,3,3,3,4),(2.01694489302841,
2.99251525867078,3.99002034489438,4.98752543111797,5.98503051734157,6.98253560356516,
7.59274844815666),.UNSPECIFIED.);
#1519=B_SPLINE_CURVE_WITH_KNOTS('',3,(#73943,#73944,#73945,#73946),
 .UNSPECIFIED.,.F.,.F.,(4,4),(126.973269284569,127.68065103662),
 .UNSPECIFIED.);
#1520=B_SPLINE_CURVE_WITH_KNOTS('',3,(#73949,#73950,#73951,#73952,#73953,
#73954,#73955,#73956,#73957,#73958),.UNSPECIFIED.,.F.,.F.,(4,3,3,4),(-125.663706143592,
-124.688135777949,-123.690630691726,-123.229495242053),.UNSPECIFIED.);
#1521=B_SPLINE_CURVE_WITH_KNOTS('',3,(#73963,#73964,#73965,#73966,#73967,
#73968,#73969,#73970,#73971,#73972,#73973,#73974,#73975,#73976,#73977,#73978,
#73979,#73980,#73981,#73982,#73983,#73984,#73985,#73986,#73987),
 .UNSPECIFIED.,.F.,.F.,(4,3,3,3,3,3,3,3,4),(120.690083977389,120.698115433055,
121.695620519279,122.693125605502,123.690630691726,124.688135777949,125.685640864173,
126.683145950397,126.973269284569),.UNSPECIFIED.);
#1522=B_SPLINE_CURVE_WITH_KNOTS('',3,(#73988,#73989,#73990,#73991,#73992,
#73993,#73994,#73995,#73996,#73997,#73998,#73999,#74000,#74001,#74002,#74003,
#74004,#74005,#74006,#74007,#74008,#74009),.UNSPECIFIED.,.F.,.F.,(4,3,3,
3,3,3,3,4),(-123.229495242053,-122.693125605502,-121.695620519279,-120.698115433055,
-119.700610346831,-118.703105260608,-117.705600174384,-116.946309934874),
 .UNSPECIFIED.);
#1523=B_SPLINE_CURVE_WITH_KNOTS('',3,(#74014,#74015,#74016,#74017,#74018,
#74019,#74020,#74021,#74022,#74023,#74024,#74025,#74026,#74027,#74028,#74029,
#74030,#74031,#74032,#74033,#74034,#74035),.UNSPECIFIED.,.F.,.F.,(4,3,3,
3,3,3,3,4),(114.40689867021,114.713084915713,115.710590001937,116.708095088161,
117.705600174384,118.703105260608,119.700610346831,120.690083977389),
 .UNSPECIFIED.);
#1524=B_SPLINE_CURVE_WITH_KNOTS('',3,(#74036,#74037,#74038,#74039,#74040,
#74041,#74042,#74043,#74044,#74045,#74046,#74047,#74048,#74049,#74050,#74051,
#74052,#74053,#74054,#74055,#74056,#74057,#74058,#74059,#74060),
 .UNSPECIFIED.,.F.,.F.,(4,3,3,3,3,3,3,3,4),(-116.946309934874,-116.708095088161,
-115.710590001937,-114.713084915713,-113.71557982949,-112.718074743266,
-111.720569657043,-110.723064570819,-110.663124627694),.UNSPECIFIED.);
#1525=B_SPLINE_CURVE_WITH_KNOTS('',3,(#74065,#74066,#74067,#74068,#74069,
#74070,#74071,#74072,#74073,#74074,#74075,#74076,#74077,#74078,#74079,#74080,
#74081,#74082,#74083,#74084,#74085,#74086),.UNSPECIFIED.,.F.,.F.,(4,3,3,
3,3,3,3,4),(108.12371336303,108.728054398372,109.725559484595,110.723064570819,
111.720569657043,112.718074743266,113.71557982949,114.40689867021),
 .UNSPECIFIED.);
#1526=B_SPLINE_CURVE_WITH_KNOTS('',3,(#74087,#74088,#74089,#74090,#74091,
#74092,#74093,#74094,#74095,#74096,#74097,#74098,#74099,#74100,#74101,#74102,
#74103,#74104,#74105,#74106,#74107,#74108),.UNSPECIFIED.,.F.,.F.,(4,3,3,
3,3,3,3,4),(-110.663124627694,-109.725559484595,-108.728054398372,-107.730549312148,
-106.733044225925,-105.735539139701,-104.738034053477,-104.379939320515),
 .UNSPECIFIED.);
#1527=B_SPLINE_CURVE_WITH_KNOTS('',3,(#74113,#74114,#74115,#74116,#74117,
#74118,#74119,#74120,#74121,#74122,#74123,#74124,#74125,#74126,#74127,#74128,
#74129,#74130,#74131,#74132,#74133,#74134),.UNSPECIFIED.,.F.,.F.,(4,3,3,
3,3,3,3,4),(101.84052805585,102.74302388103,103.740528967254,104.738034053477,
105.735539139701,106.733044225925,107.730549312148,108.12371336303),
 .UNSPECIFIED.);
#1528=B_SPLINE_CURVE_WITH_KNOTS('',3,(#74135,#74136,#74137,#74138,#74139,
#74140,#74141,#74142,#74143,#74144,#74145,#74146,#74147,#74148,#74149,#74150,
#74151,#74152,#74153,#74154,#74155,#74156),.UNSPECIFIED.,.F.,.F.,(4,3,3,
3,3,3,3,4),(-104.379939320515,-103.740528967254,-102.74302388103,-101.745518794807,
-100.748013708583,-99.7505086223595,-98.7530035361359,-98.096754013335),
 .UNSPECIFIED.);
#1529=B_SPLINE_CURVE_WITH_KNOTS('',3,(#74161,#74162,#74163,#74164,#74165,
#74166,#74167,#74168,#74169,#74170,#74171,#74172,#74173,#74174,#74175,#74176,
#74177,#74178,#74179,#74180,#74181,#74182,#74183,#74184,#74185),
 .UNSPECIFIED.,.F.,.F.,(4,3,3,3,3,3,3,3,4),(95.5573427486709,95.7604882774651,
96.7579933636887,97.7554984499123,98.7530035361359,99.7505086223595,100.748013708583,
101.745518794807,101.84052805585),.UNSPECIFIED.);
#1530=B_SPLINE_CURVE_WITH_KNOTS('',3,(#74186,#74187,#74188,#74189,#74190,
#74191,#74192,#74193,#74194,#74195,#74196,#74197,#74198,#74199,#74200,#74201,
#74202,#74203,#74204,#74205,#74206,#74207),.UNSPECIFIED.,.F.,.F.,(4,3,3,
3,3,3,3,4),(-98.096754013335,-97.7554984499123,-96.7579933636887,-95.7604882774651,
-94.7629831912415,-93.7654781050179,-92.7679730187943,-91.8135687061554),
 .UNSPECIFIED.);
#1531=B_SPLINE_CURVE_WITH_KNOTS('',3,(#74212,#74213,#74214,#74215,#74216,
#74217,#74218,#74219,#74220,#74221,#74222,#74223,#74224,#74225,#74226,#74227,
#74228,#74229,#74230,#74231,#74232,#74233),.UNSPECIFIED.,.F.,.F.,(4,3,3,
3,3,3,3,4),(89.2741574414913,89.7754577601235,90.7729628463471,91.7704679325707,
92.7679730187943,93.7654781050179,94.7629831912415,95.5573427486709),
 .UNSPECIFIED.);
#1532=B_SPLINE_CURVE_WITH_KNOTS('',3,(#74234,#74235,#74236,#74237,#74238,
#74239,#74240,#74241,#74242,#74243,#74244,#74245,#74246,#74247,#74248,#74249,
#74250,#74251,#74252,#74253,#74254,#74255,#74256,#74257,#74258),
 .UNSPECIFIED.,.F.,.F.,(4,3,3,3,3,3,3,3,4),(-91.8135687061554,-91.7704679325708,
-90.7729628463471,-89.7754577601236,-88.7779526739,-87.7804475876764,-86.7829425014528,
-85.7854374152292,-85.5303833989758),.UNSPECIFIED.);
#1533=B_SPLINE_CURVE_WITH_KNOTS('',3,(#74263,#74264,#74265,#74266,#74267,
#74268,#74269,#74270,#74271,#74272,#74273,#74274,#74275,#74276,#74277,#74278,
#74279,#74280,#74281,#74282,#74283,#74284),.UNSPECIFIED.,.F.,.F.,(4,3,3,
3,3,3,3,4),(82.9909721343117,83.790427242782,84.7879323290056,85.7854374152292,
86.7829425014528,87.7804475876763,88.7779526739,89.2741574414913),
 .UNSPECIFIED.);
#1534=B_SPLINE_CURVE_WITH_KNOTS('',3,(#74285,#74286,#74287,#74288,#74289,
#74290,#74291,#74292,#74293,#74294,#74295,#74296,#74297,#74298,#74299,#74300,
#74301,#74302,#74303,#74304,#74305,#74306),.UNSPECIFIED.,.F.,.F.,(4,3,3,
3,3,3,3,4),(-85.5303833989758,-84.7879323290056,-83.790427242782,-82.7929221565584,
-81.7954170703348,-80.7979119841112,-79.8004068978876,-79.2471980917962),
 .UNSPECIFIED.);
#1535=B_SPLINE_CURVE_WITH_KNOTS('',3,(#74311,#74312,#74313,#74314,#74315,
#74316,#74317,#74318,#74319,#74320,#74321,#74322,#74323,#74324,#74325,#74326,
#74327,#74328,#74329,#74330,#74331,#74332,#74333,#74334,#74335),
 .UNSPECIFIED.,.F.,.F.,(4,3,3,3,3,3,3,3,4),(76.7077868271321,76.8078916392168,
77.8053967254404,78.802901811664,79.8004068978876,80.7979119841112,81.7954170703348,
82.7929221565584,82.9909721343117),.UNSPECIFIED.);
#1536=B_SPLINE_CURVE_WITH_KNOTS('',3,(#74336,#74337,#74338,#74339,#74340,
#74341,#74342,#74343,#74344,#74345,#74346,#74347,#74348,#74349,#74350,#74351,
#74352,#74353,#74354,#74355,#74356,#74357),.UNSPECIFIED.,.F.,.F.,(4,3,3,
3,3,3,3,4),(-79.2471980917962,-78.802901811664,-77.8053967254404,-76.8078916392168,
-75.8103865529932,-74.8128814667696,-73.815376380546,-72.9640127846167),
 .UNSPECIFIED.);
#1537=B_SPLINE_CURVE_WITH_KNOTS('',3,(#74362,#74363,#74364,#74365,#74366,
#74367,#74368,#74369,#74370,#74371,#74372,#74373,#74374,#74375,#74376,#74377,
#74378,#74379,#74380,#74381,#74382,#74383),.UNSPECIFIED.,.F.,.F.,(4,3,3,
3,3,3,3,4),(70.4246015199525,70.8228611218752,71.8203662080988,72.8178712943224,
73.815376380546,74.8128814667696,75.8103865529932,76.7077868271321),
 .UNSPECIFIED.);
#1538=B_SPLINE_CURVE_WITH_KNOTS('',3,(#74384,#74385,#74386,#74387,#74388,
#74389,#74390,#74391,#74392,#74393,#74394,#74395,#74396,#74397,#74398,#74399,
#74400,#74401,#74402,#74403,#74404,#74405,#74406,#74407,#74408),
 .UNSPECIFIED.,.F.,.F.,(4,3,3,3,3,3,3,3,4),(-72.9640127846167,-72.8178712943224,
-71.8203662080988,-70.8228611218752,-69.8253560356517,-68.827850949428,
-67.8303458632045,-66.8328407769809,-66.680827477437),.UNSPECIFIED.);
#1539=B_SPLINE_CURVE_WITH_KNOTS('',3,(#74413,#74414,#74415,#74416,#74417,
#74418,#74419,#74420,#74421,#74422,#74423,#74424,#74425,#74426,#74427,#74428,
#74429,#74430,#74431,#74432,#74433,#74434),.UNSPECIFIED.,.F.,.F.,(4,3,3,
3,3,3,3,4),(64.1414162127729,64.8378306045337,65.8353356907573,66.8328407769808,
67.8303458632045,68.827850949428,69.8253560356517,70.4246015199525),
 .UNSPECIFIED.);
#1540=B_SPLINE_CURVE_WITH_KNOTS('',3,(#74435,#74436,#74437,#74438,#74439,
#74440,#74441,#74442,#74443,#74444,#74445,#74446,#74447,#74448,#74449,#74450,
#74451,#74452,#74453,#74454,#74455,#74456),.UNSPECIFIED.,.F.,.F.,(4,3,3,
3,3,3,3,4),(-66.680827477437,-65.8353356907573,-64.8378306045337,-63.8403255183101,
-62.8428204320865,-61.8453153458629,-60.8478102596393,-60.3976421702575),
 .UNSPECIFIED.);
#1541=B_SPLINE_CURVE_WITH_KNOTS('',3,(#74461,#74462,#74463,#74464,#74465,
#74466,#74467,#74468,#74469,#74470,#74471,#74472,#74473,#74474,#74475,#74476,
#74477,#74478,#74479,#74480,#74481,#74482),.UNSPECIFIED.,.F.,.F.,(4,3,3,
3,3,3,3,4),(57.8582309055933,58.8528000871921,59.8503051734157,60.8478102596393,
61.8453153458629,62.8428204320865,63.8403255183101,64.1414162127729),
 .UNSPECIFIED.);
#1542=B_SPLINE_CURVE_WITH_KNOTS('',3,(#74483,#74484,#74485,#74486,#74487,
#74488,#74489,#74490,#74491,#74492,#74493,#74494,#74495,#74496,#74497,#74498,
#74499,#74500,#74501,#74502,#74503,#74504),.UNSPECIFIED.,.F.,.F.,(4,3,3,
3,3,3,3,4),(-60.3976421702575,-59.8503051734157,-58.8528000871921,-57.8552950009685,
-56.8577899147449,-55.8602848285213,-54.8627797422977,-54.1144568630779),
 .UNSPECIFIED.);
#1543=B_SPLINE_CURVE_WITH_KNOTS('',3,(#74509,#74510,#74511,#74512,#74513,
#74514,#74515,#74516,#74517,#74518,#74519,#74520,#74521,#74522,#74523,#74524,
#74525,#74526,#74527,#74528,#74529,#74530,#74531,#74532,#74533),
 .UNSPECIFIED.,.F.,.F.,(4,3,3,3,3,3,3,3,4),(51.5750455984137,51.8702644836269,
52.8677695698505,53.8652746560741,54.8627797422977,55.8602848285213,56.8577899147449,
57.8552950009685,57.8582309055933),.UNSPECIFIED.);
#1544=B_SPLINE_CURVE_WITH_KNOTS('',3,(#74534,#74535,#74536,#74537,#74538,
#74539,#74540,#74541,#74542,#74543,#74544,#74545,#74546,#74547,#74548,#74549,
#74550,#74551,#74552,#74553,#74554,#74555,#74556,#74557,#74558),
 .UNSPECIFIED.,.F.,.F.,(4,3,3,3,3,3,3,3,4),(-54.1144568630779,-53.8652746560741,
-52.8677695698505,-51.8702644836269,-50.8727593974033,-49.8752543111797,
-48.8777492249561,-47.8802441387326,-47.8312715558983),.UNSPECIFIED.);
#1545=B_SPLINE_CURVE_WITH_KNOTS('',3,(#74563,#74564,#74565,#74566,#74567,
#74568,#74569,#74570,#74571,#74572,#74573,#74574,#74575,#74576,#74577,#74578,
#74579,#74580,#74581,#74582,#74583,#74584),.UNSPECIFIED.,.F.,.F.,(4,3,3,
3,3,3,3,4),(45.2918602912341,45.8852339662854,46.882739052509,47.8802441387326,
48.8777492249562,49.8752543111798,50.8727593974033,51.5750455984137),
 .UNSPECIFIED.);
#1546=B_SPLINE_CURVE_WITH_KNOTS('',3,(#74585,#74586,#74587,#74588,#74589,
#74590,#74591,#74592,#74593,#74594,#74595,#74596,#74597,#74598,#74599,#74600,
#74601,#74602,#74603,#74604,#74605,#74606),.UNSPECIFIED.,.F.,.F.,(4,3,3,
3,3,3,3,4),(-47.8312715558983,-46.882739052509,-45.8852339662854,-44.8877288800618,
-43.8902237938382,-42.8927187076146,-41.895213621391,-41.5480862487187),
 .UNSPECIFIED.);
#1547=B_SPLINE_CURVE_WITH_KNOTS('',3,(#74611,#74612,#74613,#74614,#74615,
#74616,#74617,#74618,#74619,#74620,#74621,#74622,#74623,#74624,#74625,#74626,
#74627,#74628,#74629,#74630,#74631,#74632),.UNSPECIFIED.,.F.,.F.,(4,3,3,
3,3,3,3,4),(39.0086749840545,39.9002034489438,40.8977085351674,41.895213621391,
42.8927187076146,43.8902237938382,44.8877288800618,45.2918602912341),
 .UNSPECIFIED.);
#1548=B_SPLINE_CURVE_WITH_KNOTS('',3,(#74633,#74634,#74635,#74636,#74637,
#74638,#74639,#74640,#74641,#74642,#74643,#74644,#74645,#74646,#74647,#74648,
#74649,#74650,#74651,#74652,#74653,#74654),.UNSPECIFIED.,.F.,.F.,(4,3,3,
3,3,3,3,4),(-41.5480862487187,-40.8977085351674,-39.9002034489438,-38.9026983627202,
-37.9051932764966,-36.907688190273,-35.9101831040494,-35.2649009415391),
 .UNSPECIFIED.);
#1549=B_SPLINE_CURVE_WITH_KNOTS('',3,(#74659,#74660,#74661,#74662,#74663,
#74664,#74665,#74666,#74667,#74668,#74669,#74670,#74671,#74672,#74673,#74674,
#74675,#74676,#74677,#74678,#74679,#74680,#74681,#74682,#74683),
 .UNSPECIFIED.,.F.,.F.,(4,3,3,3,3,3,3,3,4),(32.725489676875,32.9176678453786,
33.9151729316022,34.9126780178258,35.9101831040494,36.907688190273,37.9051932764966,
38.9026983627202,39.0086749840545),.UNSPECIFIED.);
#1550=B_SPLINE_CURVE_WITH_KNOTS('',3,(#74684,#74685,#74686,#74687,#74688,
#74689,#74690,#74691,#74692,#74693,#74694,#74695,#74696,#74697,#74698,#74699,
#74700,#74701,#74702,#74703,#74704,#74705),.UNSPECIFIED.,.F.,.F.,(4,3,3,
3,3,3,3,4),(-35.2649009415391,-34.9126780178258,-33.9151729316022,-32.9176678453786,
-31.920162759155,-30.9226576729314,-29.9251525867078,-28.9817156343595),
 .UNSPECIFIED.);
#1551=B_SPLINE_CURVE_WITH_KNOTS('',3,(#74710,#74711,#74712,#74713,#74714,
#74715,#74716,#74717,#74718,#74719,#74720,#74721,#74722,#74723,#74724,#74725,
#74726,#74727,#74728,#74729,#74730,#74731),.UNSPECIFIED.,.F.,.F.,(4,3,3,
3,3,3,3,4),(26.4423043696954,26.9326373280371,27.9301424142607,28.9276475004843,
29.9251525867078,30.9226576729314,31.920162759155,32.725489676875),
 .UNSPECIFIED.);
#1552=B_SPLINE_CURVE_WITH_KNOTS('',3,(#74732,#74733,#74734,#74735,#74736,
#74737,#74738,#74739,#74740,#74741,#74742,#74743,#74744,#74745,#74746,#74747,
#74748,#74749,#74750,#74751,#74752,#74753,#74754,#74755,#74756),
 .UNSPECIFIED.,.F.,.F.,(4,3,3,3,3,3,3,3,4),(-28.9817156343595,-28.9276475004842,
-27.9301424142607,-26.9326373280371,-25.9351322418135,-24.9376271555899,
-23.9401220693663,-22.9426169831427,-22.6985303271799),.UNSPECIFIED.);
#1553=B_SPLINE_CURVE_WITH_KNOTS('',3,(#74761,#74762,#74763,#74764,#74765,
#74766,#74767,#74768,#74769,#74770,#74771,#74772,#74773,#74774,#74775,#74776,
#74777,#74778,#74779,#74780,#74781,#74782),.UNSPECIFIED.,.F.,.F.,(4,3,3,
3,3,3,3,4),(20.1591190625158,20.9476068106955,21.9451118969191,22.9426169831427,
23.9401220693663,24.9376271555899,25.9351322418135,26.4423043696954),
 .UNSPECIFIED.);
#1554=B_SPLINE_CURVE_WITH_KNOTS('',3,(#74783,#74784,#74785,#74786,#74787,
#74788,#74789,#74790,#74791,#74792,#74793,#74794,#74795,#74796,#74797,#74798,
#74799,#74800,#74801,#74802,#74803,#74804),.UNSPECIFIED.,.F.,.F.,(4,3,3,
3,3,3,3,4),(-22.6985303271799,-21.9451118969191,-20.9476068106955,-19.9501017244719,
-18.9525966382483,-17.9550915520247,-16.9575864658011,-16.4153450200003),
 .UNSPECIFIED.);
#1555=B_SPLINE_CURVE_WITH_KNOTS('',3,(#74809,#74810,#74811,#74812,#74813,
#74814,#74815,#74816,#74817,#74818,#74819,#74820,#74821,#74822,#74823,#74824,
#74825,#74826,#74827,#74828,#74829,#74830,#74831,#74832,#74833),
 .UNSPECIFIED.,.F.,.F.,(4,3,3,3,3,3,3,3,4),(13.8759337553362,13.9650712071303,
14.9625762933539,15.9600813795775,16.9575864658011,17.9550915520247,18.9525966382483,
19.9501017244719,20.1591190625158),.UNSPECIFIED.);
#1556=B_SPLINE_CURVE_WITH_KNOTS('',3,(#74834,#74835,#74836,#74837,#74838,
#74839,#74840,#74841,#74842,#74843,#74844,#74845,#74846,#74847,#74848,#74849,
#74850,#74851,#74852,#74853,#74854,#74855),.UNSPECIFIED.,.F.,.F.,(4,3,3,
3,3,3,3,4),(-16.4153450200003,-15.9600813795775,-14.9625762933539,-13.9650712071303,
-12.9675661209067,-11.9700610346831,-10.9725559484595,-10.1321597128207),
 .UNSPECIFIED.);
#1557=B_SPLINE_CURVE_WITH_KNOTS('',3,(#74861,#74862,#74863,#74864,#74865,
#74866,#74867,#74868,#74869,#74870,#74871,#74872,#74873),.UNSPECIFIED.,
 .F.,.F.,(4,3,3,3,4),(-3.84897440564117,-2.99251525867078,-1.99501017244719,
-0.997505086223592,0.),.UNSPECIFIED.);
#1558=B_SPLINE_CURVE_WITH_KNOTS('',3,(#74876,#74877,#74878,#74879,#74880,
#74881,#74882,#74883,#74884,#74885,#74886,#74887,#74888,#74889,#74890,#74891,
#74892,#74893,#74894),.UNSPECIFIED.,.F.,.F.,(4,3,3,3,3,3,4),(2.01694489302822,
2.99251525867079,3.99002034489439,4.98752543111798,5.98503051734158,6.98253560356517,
7.59274844815661),.UNSPECIFIED.);
#1559=B_SPLINE_CURVE_WITH_KNOTS('',3,(#74900,#74901,#74902,#74903),
 .UNSPECIFIED.,.F.,.F.,(4,4),(126.973269284569,127.68065103662),
 .UNSPECIFIED.);
#1560=B_SPLINE_CURVE_WITH_KNOTS('',3,(#74906,#74907,#74908,#74909,#74910,
#74911,#74912,#74913,#74914,#74915),.UNSPECIFIED.,.F.,.F.,(4,3,3,4),(-125.663706143592,
-124.688135777949,-123.690630691726,-123.229495242053),.UNSPECIFIED.);
#1561=B_SPLINE_CURVE_WITH_KNOTS('',3,(#74920,#74921,#74922,#74923,#74924,
#74925,#74926,#74927,#74928,#74929,#74930,#74931,#74932,#74933,#74934,#74935,
#74936,#74937,#74938,#74939,#74940,#74941,#74942,#74943,#74944),
 .UNSPECIFIED.,.F.,.F.,(4,3,3,3,3,3,3,3,4),(120.690083977389,120.698115433055,
121.695620519279,122.693125605502,123.690630691726,124.688135777949,125.685640864173,
126.683145950397,126.973269284569),.UNSPECIFIED.);
#1562=B_SPLINE_CURVE_WITH_KNOTS('',3,(#74945,#74946,#74947,#74948,#74949,
#74950,#74951,#74952,#74953,#74954,#74955,#74956,#74957,#74958,#74959,#74960,
#74961,#74962,#74963,#74964,#74965,#74966),.UNSPECIFIED.,.F.,.F.,(4,3,3,
3,3,3,3,4),(-123.229495242053,-122.693125605502,-121.695620519279,-120.698115433055,
-119.700610346831,-118.703105260608,-117.705600174384,-116.946309934874),
 .UNSPECIFIED.);
#1563=B_SPLINE_CURVE_WITH_KNOTS('',3,(#74971,#74972,#74973,#74974,#74975,
#74976,#74977,#74978,#74979,#74980,#74981,#74982,#74983,#74984,#74985,#74986,
#74987,#74988,#74989,#74990,#74991,#74992),.UNSPECIFIED.,.F.,.F.,(4,3,3,
3,3,3,3,4),(114.40689867021,114.713084915713,115.710590001937,116.708095088161,
117.705600174384,118.703105260608,119.700610346831,120.690083977389),
 .UNSPECIFIED.);
#1564=B_SPLINE_CURVE_WITH_KNOTS('',3,(#74993,#74994,#74995,#74996,#74997,
#74998,#74999,#75000,#75001,#75002,#75003,#75004,#75005,#75006,#75007,#75008,
#75009,#75010,#75011,#75012,#75013,#75014,#75015,#75016,#75017),
 .UNSPECIFIED.,.F.,.F.,(4,3,3,3,3,3,3,3,4),(-116.946309934874,-116.708095088161,
-115.710590001937,-114.713084915713,-113.71557982949,-112.718074743266,
-111.720569657043,-110.723064570819,-110.663124627694),.UNSPECIFIED.);
#1565=B_SPLINE_CURVE_WITH_KNOTS('',3,(#75022,#75023,#75024,#75025,#75026,
#75027,#75028,#75029,#75030,#75031,#75032,#75033,#75034,#75035,#75036,#75037,
#75038,#75039,#75040,#75041,#75042,#75043),.UNSPECIFIED.,.F.,.F.,(4,3,3,
3,3,3,3,4),(108.12371336303,108.728054398372,109.725559484595,110.723064570819,
111.720569657043,112.718074743266,113.71557982949,114.40689867021),
 .UNSPECIFIED.);
#1566=B_SPLINE_CURVE_WITH_KNOTS('',3,(#75044,#75045,#75046,#75047,#75048,
#75049,#75050,#75051,#75052,#75053,#75054,#75055,#75056,#75057,#75058,#75059,
#75060,#75061,#75062,#75063,#75064,#75065),.UNSPECIFIED.,.F.,.F.,(4,3,3,
3,3,3,3,4),(-110.663124627694,-109.725559484595,-108.728054398372,-107.730549312148,
-106.733044225925,-105.735539139701,-104.738034053477,-104.379939320515),
 .UNSPECIFIED.);
#1567=B_SPLINE_CURVE_WITH_KNOTS('',3,(#75070,#75071,#75072,#75073,#75074,
#75075,#75076,#75077,#75078,#75079,#75080,#75081,#75082,#75083,#75084,#75085,
#75086,#75087,#75088,#75089,#75090,#75091),.UNSPECIFIED.,.F.,.F.,(4,3,3,
3,3,3,3,4),(101.84052805585,102.74302388103,103.740528967254,104.738034053477,
105.735539139701,106.733044225925,107.730549312148,108.12371336303),
 .UNSPECIFIED.);
#1568=B_SPLINE_CURVE_WITH_KNOTS('',3,(#75092,#75093,#75094,#75095,#75096,
#75097,#75098,#75099,#75100,#75101,#75102,#75103,#75104,#75105,#75106,#75107,
#75108,#75109,#75110,#75111,#75112,#75113),.UNSPECIFIED.,.F.,.F.,(4,3,3,
3,3,3,3,4),(-104.379939320515,-103.740528967254,-102.74302388103,-101.745518794807,
-100.748013708583,-99.7505086223595,-98.7530035361359,-98.096754013335),
 .UNSPECIFIED.);
#1569=B_SPLINE_CURVE_WITH_KNOTS('',3,(#75118,#75119,#75120,#75121,#75122,
#75123,#75124,#75125,#75126,#75127,#75128,#75129,#75130,#75131,#75132,#75133,
#75134,#75135,#75136,#75137,#75138,#75139,#75140,#75141,#75142),
 .UNSPECIFIED.,.F.,.F.,(4,3,3,3,3,3,3,3,4),(95.5573427486709,95.7604882774651,
96.7579933636887,97.7554984499123,98.7530035361359,99.7505086223595,100.748013708583,
101.745518794807,101.84052805585),.UNSPECIFIED.);
#1570=B_SPLINE_CURVE_WITH_KNOTS('',3,(#75143,#75144,#75145,#75146,#75147,
#75148,#75149,#75150,#75151,#75152,#75153,#75154,#75155,#75156,#75157,#75158,
#75159,#75160,#75161,#75162,#75163,#75164),.UNSPECIFIED.,.F.,.F.,(4,3,3,
3,3,3,3,4),(-98.096754013335,-97.7554984499123,-96.7579933636887,-95.7604882774651,
-94.7629831912415,-93.7654781050179,-92.7679730187943,-91.8135687061554),
 .UNSPECIFIED.);
#1571=B_SPLINE_CURVE_WITH_KNOTS('',3,(#75169,#75170,#75171,#75172,#75173,
#75174,#75175,#75176,#75177,#75178,#75179,#75180,#75181,#75182,#75183,#75184,
#75185,#75186,#75187,#75188,#75189,#75190),.UNSPECIFIED.,.F.,.F.,(4,3,3,
3,3,3,3,4),(89.2741574414913,89.7754577601236,90.7729628463471,91.7704679325707,
92.7679730187943,93.7654781050179,94.7629831912415,95.5573427486709),
 .UNSPECIFIED.);
#1572=B_SPLINE_CURVE_WITH_KNOTS('',3,(#75191,#75192,#75193,#75194,#75195,
#75196,#75197,#75198,#75199,#75200,#75201,#75202,#75203,#75204,#75205,#75206,
#75207,#75208,#75209,#75210,#75211,#75212,#75213,#75214,#75215),
 .UNSPECIFIED.,.F.,.F.,(4,3,3,3,3,3,3,3,4),(-91.8135687061554,-91.7704679325708,
-90.7729628463472,-89.7754577601236,-88.7779526739,-87.7804475876764,-86.7829425014528,
-85.7854374152292,-85.5303833989758),.UNSPECIFIED.);
#1573=B_SPLINE_CURVE_WITH_KNOTS('',3,(#75220,#75221,#75222,#75223,#75224,
#75225,#75226,#75227,#75228,#75229,#75230,#75231,#75232,#75233,#75234,#75235,
#75236,#75237,#75238,#75239,#75240,#75241),.UNSPECIFIED.,.F.,.F.,(4,3,3,
3,3,3,3,4),(82.9909721343117,83.790427242782,84.7879323290056,85.7854374152292,
86.7829425014528,87.7804475876764,88.7779526739,89.2741574414913),
 .UNSPECIFIED.);
#1574=B_SPLINE_CURVE_WITH_KNOTS('',3,(#75242,#75243,#75244,#75245,#75246,
#75247,#75248,#75249,#75250,#75251,#75252,#75253,#75254,#75255,#75256,#75257,
#75258,#75259,#75260,#75261,#75262,#75263),.UNSPECIFIED.,.F.,.F.,(4,3,3,
3,3,3,3,4),(-85.5303833989758,-84.7879323290056,-83.790427242782,-82.7929221565584,
-81.7954170703348,-80.7979119841112,-79.8004068978876,-79.2471980917962),
 .UNSPECIFIED.);
#1575=B_SPLINE_CURVE_WITH_KNOTS('',3,(#75268,#75269,#75270,#75271,#75272,
#75273,#75274,#75275,#75276,#75277,#75278,#75279,#75280,#75281,#75282,#75283,
#75284,#75285,#75286,#75287,#75288,#75289,#75290,#75291,#75292),
 .UNSPECIFIED.,.F.,.F.,(4,3,3,3,3,3,3,3,4),(76.7077868271321,76.8078916392168,
77.8053967254404,78.802901811664,79.8004068978876,80.7979119841112,81.7954170703348,
82.7929221565584,82.9909721343117),.UNSPECIFIED.);
#1576=B_SPLINE_CURVE_WITH_KNOTS('',3,(#75293,#75294,#75295,#75296,#75297,
#75298,#75299,#75300,#75301,#75302,#75303,#75304,#75305,#75306,#75307,#75308,
#75309,#75310,#75311,#75312,#75313,#75314),.UNSPECIFIED.,.F.,.F.,(4,3,3,
3,3,3,3,4),(-79.2471980917962,-78.802901811664,-77.8053967254404,-76.8078916392168,
-75.8103865529932,-74.8128814667696,-73.815376380546,-72.9640127846166),
 .UNSPECIFIED.);
#1577=B_SPLINE_CURVE_WITH_KNOTS('',3,(#75319,#75320,#75321,#75322,#75323,
#75324,#75325,#75326,#75327,#75328,#75329,#75330,#75331,#75332,#75333,#75334,
#75335,#75336,#75337,#75338,#75339,#75340),.UNSPECIFIED.,.F.,.F.,(4,3,3,
3,3,3,3,4),(70.4246015199525,70.8228611218752,71.8203662080988,72.8178712943224,
73.815376380546,74.8128814667696,75.8103865529932,76.7077868271321),
 .UNSPECIFIED.);
#1578=B_SPLINE_CURVE_WITH_KNOTS('',3,(#75341,#75342,#75343,#75344,#75345,
#75346,#75347,#75348,#75349,#75350,#75351,#75352,#75353,#75354,#75355,#75356,
#75357,#75358,#75359,#75360,#75361,#75362,#75363,#75364,#75365),
 .UNSPECIFIED.,.F.,.F.,(4,3,3,3,3,3,3,3,4),(-72.9640127846166,-72.8178712943224,
-71.8203662080988,-70.8228611218752,-69.8253560356517,-68.827850949428,
-67.8303458632045,-66.8328407769809,-66.680827477437),.UNSPECIFIED.);
#1579=B_SPLINE_CURVE_WITH_KNOTS('',3,(#75370,#75371,#75372,#75373,#75374,
#75375,#75376,#75377,#75378,#75379,#75380,#75381,#75382,#75383,#75384,#75385,
#75386,#75387,#75388,#75389,#75390,#75391),.UNSPECIFIED.,.F.,.F.,(4,3,3,
3,3,3,3,4),(64.1414162127729,64.8378306045337,65.8353356907573,66.8328407769809,
67.8303458632045,68.827850949428,69.8253560356517,70.4246015199525),
 .UNSPECIFIED.);
#1580=B_SPLINE_CURVE_WITH_KNOTS('',3,(#75392,#75393,#75394,#75395,#75396,
#75397,#75398,#75399,#75400,#75401,#75402,#75403,#75404,#75405,#75406,#75407,
#75408,#75409,#75410,#75411,#75412,#75413),.UNSPECIFIED.,.F.,.F.,(4,3,3,
3,3,3,3,4),(-66.680827477437,-65.8353356907573,-64.8378306045337,-63.8403255183101,
-62.8428204320865,-61.8453153458629,-60.8478102596393,-60.3976421702574),
 .UNSPECIFIED.);
#1581=B_SPLINE_CURVE_WITH_KNOTS('',3,(#75418,#75419,#75420,#75421,#75422,
#75423,#75424,#75425,#75426,#75427,#75428,#75429,#75430,#75431,#75432,#75433,
#75434,#75435,#75436,#75437,#75438,#75439),.UNSPECIFIED.,.F.,.F.,(4,3,3,
3,3,3,3,4),(57.8582309055933,58.8528000871921,59.8503051734157,60.8478102596393,
61.8453153458629,62.8428204320865,63.8403255183101,64.1414162127729),
 .UNSPECIFIED.);
#1582=B_SPLINE_CURVE_WITH_KNOTS('',3,(#75440,#75441,#75442,#75443,#75444,
#75445,#75446,#75447,#75448,#75449,#75450,#75451,#75452,#75453,#75454,#75455,
#75456,#75457,#75458,#75459,#75460,#75461),.UNSPECIFIED.,.F.,.F.,(4,3,3,
3,3,3,3,4),(-60.3976421702574,-59.8503051734157,-58.8528000871921,-57.8552950009685,
-56.8577899147449,-55.8602848285213,-54.8627797422977,-54.1144568630778),
 .UNSPECIFIED.);
#1583=B_SPLINE_CURVE_WITH_KNOTS('',3,(#75466,#75467,#75468,#75469,#75470,
#75471,#75472,#75473,#75474,#75475,#75476,#75477,#75478,#75479,#75480,#75481,
#75482,#75483,#75484,#75485,#75486,#75487,#75488,#75489,#75490),
 .UNSPECIFIED.,.F.,.F.,(4,3,3,3,3,3,3,3,4),(51.5750455984137,51.8702644836269,
52.8677695698506,53.8652746560741,54.8627797422977,55.8602848285213,56.8577899147449,
57.8552950009685,57.8582309055933),.UNSPECIFIED.);
#1584=B_SPLINE_CURVE_WITH_KNOTS('',3,(#75491,#75492,#75493,#75494,#75495,
#75496,#75497,#75498,#75499,#75500,#75501,#75502,#75503,#75504,#75505,#75506,
#75507,#75508,#75509,#75510,#75511,#75512,#75513,#75514,#75515),
 .UNSPECIFIED.,.F.,.F.,(4,3,3,3,3,3,3,3,4),(-54.1144568630778,-53.8652746560741,
-52.8677695698505,-51.8702644836269,-50.8727593974033,-49.8752543111797,
-48.8777492249561,-47.8802441387326,-47.8312715558983),.UNSPECIFIED.);
#1585=B_SPLINE_CURVE_WITH_KNOTS('',3,(#75520,#75521,#75522,#75523,#75524,
#75525,#75526,#75527,#75528,#75529,#75530,#75531,#75532,#75533,#75534,#75535,
#75536,#75537,#75538,#75539,#75540,#75541),.UNSPECIFIED.,.F.,.F.,(4,3,3,
3,3,3,3,4),(45.2918602912341,45.8852339662854,46.882739052509,47.8802441387326,
48.8777492249562,49.8752543111798,50.8727593974034,51.5750455984137),
 .UNSPECIFIED.);
#1586=B_SPLINE_CURVE_WITH_KNOTS('',3,(#75542,#75543,#75544,#75545,#75546,
#75547,#75548,#75549,#75550,#75551,#75552,#75553,#75554,#75555,#75556,#75557,
#75558,#75559,#75560,#75561,#75562,#75563),.UNSPECIFIED.,.F.,.F.,(4,3,3,
3,3,3,3,4),(-47.8312715558983,-46.882739052509,-45.8852339662854,-44.8877288800618,
-43.8902237938382,-42.8927187076146,-41.895213621391,-41.5480862487187),
 .UNSPECIFIED.);
#1587=B_SPLINE_CURVE_WITH_KNOTS('',3,(#75568,#75569,#75570,#75571,#75572,
#75573,#75574,#75575,#75576,#75577,#75578,#75579,#75580,#75581,#75582,#75583,
#75584,#75585,#75586,#75587,#75588,#75589),.UNSPECIFIED.,.F.,.F.,(4,3,3,
3,3,3,3,4),(39.0086749840545,39.9002034489438,40.8977085351674,41.895213621391,
42.8927187076146,43.8902237938382,44.8877288800618,45.2918602912341),
 .UNSPECIFIED.);
#1588=B_SPLINE_CURVE_WITH_KNOTS('',3,(#75590,#75591,#75592,#75593,#75594,
#75595,#75596,#75597,#75598,#75599,#75600,#75601,#75602,#75603,#75604,#75605,
#75606,#75607,#75608,#75609,#75610,#75611),.UNSPECIFIED.,.F.,.F.,(4,3,3,
3,3,3,3,4),(-41.5480862487187,-40.8977085351674,-39.9002034489438,-38.9026983627202,
-37.9051932764966,-36.907688190273,-35.9101831040494,-35.2649009415391),
 .UNSPECIFIED.);
#1589=B_SPLINE_CURVE_WITH_KNOTS('',3,(#75616,#75617,#75618,#75619,#75620,
#75621,#75622,#75623,#75624,#75625,#75626,#75627,#75628,#75629,#75630,#75631,
#75632,#75633,#75634,#75635,#75636,#75637,#75638,#75639,#75640),
 .UNSPECIFIED.,.F.,.F.,(4,3,3,3,3,3,3,3,4),(32.7254896768749,32.9176678453786,
33.9151729316022,34.9126780178258,35.9101831040494,36.907688190273,37.9051932764966,
38.9026983627202,39.0086749840545),.UNSPECIFIED.);
#1590=B_SPLINE_CURVE_WITH_KNOTS('',3,(#75641,#75642,#75643,#75644,#75645,
#75646,#75647,#75648,#75649,#75650,#75651,#75652,#75653,#75654,#75655,#75656,
#75657,#75658,#75659,#75660,#75661,#75662),.UNSPECIFIED.,.F.,.F.,(4,3,3,
3,3,3,3,4),(-35.2649009415391,-34.9126780178258,-33.9151729316022,-32.9176678453786,
-31.920162759155,-30.9226576729314,-29.9251525867078,-28.9817156343595),
 .UNSPECIFIED.);
#1591=B_SPLINE_CURVE_WITH_KNOTS('',3,(#75667,#75668,#75669,#75670,#75671,
#75672,#75673,#75674,#75675,#75676,#75677,#75678,#75679,#75680,#75681,#75682,
#75683,#75684,#75685,#75686,#75687,#75688),.UNSPECIFIED.,.F.,.F.,(4,3,3,
3,3,3,3,4),(26.4423043696953,26.9326373280371,27.9301424142607,28.9276475004843,
29.9251525867078,30.9226576729314,31.920162759155,32.7254896768749),
 .UNSPECIFIED.);
#1592=B_SPLINE_CURVE_WITH_KNOTS('',3,(#75689,#75690,#75691,#75692,#75693,
#75694,#75695,#75696,#75697,#75698,#75699,#75700,#75701,#75702,#75703,#75704,
#75705,#75706,#75707,#75708,#75709,#75710,#75711,#75712,#75713),
 .UNSPECIFIED.,.F.,.F.,(4,3,3,3,3,3,3,3,4),(-28.9817156343595,-28.9276475004843,
-27.9301424142607,-26.9326373280371,-25.9351322418135,-24.9376271555899,
-23.9401220693663,-22.9426169831427,-22.6985303271799),.UNSPECIFIED.);
#1593=B_SPLINE_CURVE_WITH_KNOTS('',3,(#75718,#75719,#75720,#75721,#75722,
#75723,#75724,#75725,#75726,#75727,#75728,#75729,#75730,#75731,#75732,#75733,
#75734,#75735,#75736,#75737,#75738,#75739),.UNSPECIFIED.,.F.,.F.,(4,3,3,
3,3,3,3,4),(20.1591190625158,20.9476068106955,21.9451118969191,22.9426169831427,
23.9401220693663,24.9376271555899,25.9351322418135,26.4423043696953),
 .UNSPECIFIED.);
#1594=B_SPLINE_CURVE_WITH_KNOTS('',3,(#75740,#75741,#75742,#75743,#75744,
#75745,#75746,#75747,#75748,#75749,#75750,#75751,#75752,#75753,#75754,#75755,
#75756,#75757,#75758,#75759,#75760,#75761),.UNSPECIFIED.,.F.,.F.,(4,3,3,
3,3,3,3,4),(-22.6985303271799,-21.9451118969191,-20.9476068106955,-19.9501017244719,
-18.9525966382483,-17.9550915520247,-16.9575864658011,-16.4153450200003),
 .UNSPECIFIED.);
#1595=B_SPLINE_CURVE_WITH_KNOTS('',3,(#75766,#75767,#75768,#75769,#75770,
#75771,#75772,#75773,#75774,#75775,#75776,#75777,#75778,#75779,#75780,#75781,
#75782,#75783,#75784,#75785,#75786,#75787,#75788,#75789,#75790),
 .UNSPECIFIED.,.F.,.F.,(4,3,3,3,3,3,3,3,4),(13.8759337553362,13.9650712071303,
14.9625762933539,15.9600813795775,16.9575864658011,17.9550915520247,18.9525966382483,
19.9501017244719,20.1591190625158),.UNSPECIFIED.);
#1596=B_SPLINE_CURVE_WITH_KNOTS('',3,(#75791,#75792,#75793,#75794,#75795,
#75796,#75797,#75798,#75799,#75800,#75801,#75802,#75803,#75804,#75805,#75806,
#75807,#75808,#75809,#75810,#75811,#75812),.UNSPECIFIED.,.F.,.F.,(4,3,3,
3,3,3,3,4),(-16.4153450200003,-15.9600813795775,-14.9625762933539,-13.9650712071303,
-12.9675661209067,-11.9700610346831,-10.9725559484596,-10.1321597128207),
 .UNSPECIFIED.);
#1597=B_SPLINE_CURVE_WITH_KNOTS('',3,(#75818,#75819,#75820,#75821,#75822,
#75823,#75824,#75825,#75826,#75827,#75828,#75829,#75830),.UNSPECIFIED.,
 .F.,.F.,(4,3,3,3,4),(-3.84897440564113,-2.99251525867078,-1.99501017244719,
-0.997505086223595,0.),.UNSPECIFIED.);
#1598=B_SPLINE_CURVE_WITH_KNOTS('',3,(#75833,#75834,#75835,#75836,#75837,
#75838,#75839,#75840,#75841,#75842,#75843,#75844,#75845,#75846,#75847,#75848,
#75849,#75850,#75851),.UNSPECIFIED.,.F.,.F.,(4,3,3,3,3,3,4),(2.01694489302847,
2.99251525867078,3.99002034489437,4.98752543111797,5.98503051734157,6.98253560356516,
7.59274844815659),.UNSPECIFIED.);
#1599=B_SPLINE_CURVE_WITH_KNOTS('',3,(#75857,#75858,#75859,#75860),
 .UNSPECIFIED.,.F.,.F.,(4,4),(126.973269284569,127.68065103662),
 .UNSPECIFIED.);
#1600=B_SPLINE_CURVE_WITH_KNOTS('',3,(#75863,#75864,#75865,#75866,#75867,
#75868,#75869,#75870,#75871,#75872),.UNSPECIFIED.,.F.,.F.,(4,3,3,4),(-125.663706143592,
-124.688135777949,-123.690630691726,-123.229495242053),.UNSPECIFIED.);
#1601=B_SPLINE_CURVE_WITH_KNOTS('',3,(#75877,#75878,#75879,#75880,#75881,
#75882,#75883,#75884,#75885,#75886,#75887,#75888,#75889,#75890,#75891,#75892,
#75893,#75894,#75895,#75896,#75897,#75898,#75899,#75900,#75901),
 .UNSPECIFIED.,.F.,.F.,(4,3,3,3,3,3,3,3,4),(120.690083977389,120.698115433055,
121.695620519279,122.693125605502,123.690630691726,124.688135777949,125.685640864173,
126.683145950397,126.973269284569),.UNSPECIFIED.);
#1602=B_SPLINE_CURVE_WITH_KNOTS('',3,(#75902,#75903,#75904,#75905,#75906,
#75907,#75908,#75909,#75910,#75911,#75912,#75913,#75914,#75915,#75916,#75917,
#75918,#75919,#75920,#75921,#75922,#75923),.UNSPECIFIED.,.F.,.F.,(4,3,3,
3,3,3,3,4),(-123.229495242053,-122.693125605502,-121.695620519279,-120.698115433055,
-119.700610346831,-118.703105260608,-117.705600174384,-116.946309934874),
 .UNSPECIFIED.);
#1603=B_SPLINE_CURVE_WITH_KNOTS('',3,(#75928,#75929,#75930,#75931,#75932,
#75933,#75934,#75935,#75936,#75937,#75938,#75939,#75940,#75941,#75942,#75943,
#75944,#75945,#75946,#75947,#75948,#75949),.UNSPECIFIED.,.F.,.F.,(4,3,3,
3,3,3,3,4),(114.40689867021,114.713084915713,115.710590001937,116.708095088161,
117.705600174384,118.703105260608,119.700610346831,120.690083977389),
 .UNSPECIFIED.);
#1604=B_SPLINE_CURVE_WITH_KNOTS('',3,(#75950,#75951,#75952,#75953,#75954,
#75955,#75956,#75957,#75958,#75959,#75960,#75961,#75962,#75963,#75964,#75965,
#75966,#75967,#75968,#75969,#75970,#75971,#75972,#75973,#75974),
 .UNSPECIFIED.,.F.,.F.,(4,3,3,3,3,3,3,3,4),(-116.946309934874,-116.708095088161,
-115.710590001937,-114.713084915713,-113.71557982949,-112.718074743266,
-111.720569657043,-110.723064570819,-110.663124627694),.UNSPECIFIED.);
#1605=B_SPLINE_CURVE_WITH_KNOTS('',3,(#75979,#75980,#75981,#75982,#75983,
#75984,#75985,#75986,#75987,#75988,#75989,#75990,#75991,#75992,#75993,#75994,
#75995,#75996,#75997,#75998,#75999,#76000),.UNSPECIFIED.,.F.,.F.,(4,3,3,
3,3,3,3,4),(108.12371336303,108.728054398372,109.725559484595,110.723064570819,
111.720569657043,112.718074743266,113.71557982949,114.40689867021),
 .UNSPECIFIED.);
#1606=B_SPLINE_CURVE_WITH_KNOTS('',3,(#76001,#76002,#76003,#76004,#76005,
#76006,#76007,#76008,#76009,#76010,#76011,#76012,#76013,#76014,#76015,#76016,
#76017,#76018,#76019,#76020,#76021,#76022),.UNSPECIFIED.,.F.,.F.,(4,3,3,
3,3,3,3,4),(-110.663124627694,-109.725559484596,-108.728054398372,-107.730549312148,
-106.733044225925,-105.735539139701,-104.738034053478,-104.379939320515),
 .UNSPECIFIED.);
#1607=B_SPLINE_CURVE_WITH_KNOTS('',3,(#76027,#76028,#76029,#76030,#76031,
#76032,#76033,#76034,#76035,#76036,#76037,#76038,#76039,#76040,#76041,#76042,
#76043,#76044,#76045,#76046,#76047,#76048),.UNSPECIFIED.,.F.,.F.,(4,3,3,
3,3,3,3,4),(101.84052805585,102.74302388103,103.740528967254,104.738034053478,
105.735539139701,106.733044225925,107.730549312148,108.12371336303),
 .UNSPECIFIED.);
#1608=B_SPLINE_CURVE_WITH_KNOTS('',3,(#76049,#76050,#76051,#76052,#76053,
#76054,#76055,#76056,#76057,#76058,#76059,#76060,#76061,#76062,#76063,#76064,
#76065,#76066,#76067,#76068,#76069,#76070),.UNSPECIFIED.,.F.,.F.,(4,3,3,
3,3,3,3,4),(-104.379939320515,-103.740528967254,-102.74302388103,-101.745518794807,
-100.748013708583,-99.7505086223595,-98.7530035361359,-98.096754013335),
 .UNSPECIFIED.);
#1609=B_SPLINE_CURVE_WITH_KNOTS('',3,(#76075,#76076,#76077,#76078,#76079,
#76080,#76081,#76082,#76083,#76084,#76085,#76086,#76087,#76088,#76089,#76090,
#76091,#76092,#76093,#76094,#76095,#76096,#76097,#76098,#76099),
 .UNSPECIFIED.,.F.,.F.,(4,3,3,3,3,3,3,3,4),(95.5573427486709,95.7604882774652,
96.7579933636887,97.7554984499123,98.7530035361359,99.7505086223595,100.748013708583,
101.745518794807,101.84052805585),.UNSPECIFIED.);
#1610=B_SPLINE_CURVE_WITH_KNOTS('',3,(#76100,#76101,#76102,#76103,#76104,
#76105,#76106,#76107,#76108,#76109,#76110,#76111,#76112,#76113,#76114,#76115,
#76116,#76117,#76118,#76119,#76120,#76121),.UNSPECIFIED.,.F.,.F.,(4,3,3,
3,3,3,3,4),(-98.096754013335,-97.7554984499123,-96.7579933636887,-95.7604882774651,
-94.7629831912416,-93.7654781050179,-92.7679730187944,-91.8135687061554),
 .UNSPECIFIED.);
#1611=B_SPLINE_CURVE_WITH_KNOTS('',3,(#76126,#76127,#76128,#76129,#76130,
#76131,#76132,#76133,#76134,#76135,#76136,#76137,#76138,#76139,#76140,#76141,
#76142,#76143,#76144,#76145,#76146,#76147),.UNSPECIFIED.,.F.,.F.,(4,3,3,
3,3,3,3,4),(89.2741574414913,89.7754577601236,90.7729628463472,91.7704679325708,
92.7679730187944,93.765478105018,94.7629831912415,95.5573427486709),
 .UNSPECIFIED.);
#1612=B_SPLINE_CURVE_WITH_KNOTS('',3,(#76148,#76149,#76150,#76151,#76152,
#76153,#76154,#76155,#76156,#76157,#76158,#76159,#76160,#76161,#76162,#76163,
#76164,#76165,#76166,#76167,#76168,#76169,#76170,#76171,#76172),
 .UNSPECIFIED.,.F.,.F.,(4,3,3,3,3,3,3,3,4),(-91.8135687061554,-91.7704679325708,
-90.7729628463472,-89.7754577601236,-88.7779526739,-87.7804475876764,-86.7829425014528,
-85.7854374152292,-85.5303833989758),.UNSPECIFIED.);
#1613=B_SPLINE_CURVE_WITH_KNOTS('',3,(#76177,#76178,#76179,#76180,#76181,
#76182,#76183,#76184,#76185,#76186,#76187,#76188,#76189,#76190,#76191,#76192,
#76193,#76194,#76195,#76196,#76197,#76198),.UNSPECIFIED.,.F.,.F.,(4,3,3,
3,3,3,3,4),(82.9909721343117,83.790427242782,84.7879323290056,85.7854374152292,
86.7829425014528,87.7804475876764,88.7779526739,89.2741574414913),
 .UNSPECIFIED.);
#1614=B_SPLINE_CURVE_WITH_KNOTS('',3,(#76199,#76200,#76201,#76202,#76203,
#76204,#76205,#76206,#76207,#76208,#76209,#76210,#76211,#76212,#76213,#76214,
#76215,#76216,#76217,#76218,#76219,#76220),.UNSPECIFIED.,.F.,.F.,(4,3,3,
3,3,3,3,4),(-85.5303833989758,-84.7879323290056,-83.790427242782,-82.7929221565584,
-81.7954170703348,-80.7979119841112,-79.8004068978876,-79.2471980917962),
 .UNSPECIFIED.);
#1615=B_SPLINE_CURVE_WITH_KNOTS('',3,(#76225,#76226,#76227,#76228,#76229,
#76230,#76231,#76232,#76233,#76234,#76235,#76236,#76237,#76238,#76239,#76240,
#76241,#76242,#76243,#76244,#76245,#76246,#76247,#76248,#76249),
 .UNSPECIFIED.,.F.,.F.,(4,3,3,3,3,3,3,3,4),(76.7077868271321,76.8078916392168,
77.8053967254404,78.802901811664,79.8004068978876,80.7979119841112,81.7954170703348,
82.7929221565584,82.9909721343117),.UNSPECIFIED.);
#1616=B_SPLINE_CURVE_WITH_KNOTS('',3,(#76250,#76251,#76252,#76253,#76254,
#76255,#76256,#76257,#76258,#76259,#76260,#76261,#76262,#76263,#76264,#76265,
#76266,#76267,#76268,#76269,#76270,#76271),.UNSPECIFIED.,.F.,.F.,(4,3,3,
3,3,3,3,4),(-79.2471980917962,-78.802901811664,-77.8053967254404,-76.8078916392168,
-75.8103865529932,-74.8128814667696,-73.815376380546,-72.9640127846166),
 .UNSPECIFIED.);
#1617=B_SPLINE_CURVE_WITH_KNOTS('',3,(#76276,#76277,#76278,#76279,#76280,
#76281,#76282,#76283,#76284,#76285,#76286,#76287,#76288,#76289,#76290,#76291,
#76292,#76293,#76294,#76295,#76296,#76297),.UNSPECIFIED.,.F.,.F.,(4,3,3,
3,3,3,3,4),(70.4246015199525,70.8228611218753,71.8203662080989,72.8178712943224,
73.815376380546,74.8128814667696,75.8103865529932,76.7077868271321),
 .UNSPECIFIED.);
#1618=B_SPLINE_CURVE_WITH_KNOTS('',3,(#76298,#76299,#76300,#76301,#76302,
#76303,#76304,#76305,#76306,#76307,#76308,#76309,#76310,#76311,#76312,#76313,
#76314,#76315,#76316,#76317,#76318,#76319,#76320,#76321,#76322),
 .UNSPECIFIED.,.F.,.F.,(4,3,3,3,3,3,3,3,4),(-72.9640127846166,-72.8178712943224,
-71.8203662080988,-70.8228611218752,-69.8253560356517,-68.8278509494281,
-67.8303458632045,-66.8328407769809,-66.680827477437),.UNSPECIFIED.);
#1619=B_SPLINE_CURVE_WITH_KNOTS('',3,(#76327,#76328,#76329,#76330,#76331,
#76332,#76333,#76334,#76335,#76336,#76337,#76338,#76339,#76340,#76341,#76342,
#76343,#76344,#76345,#76346,#76347,#76348),.UNSPECIFIED.,.F.,.F.,(4,3,3,
3,3,3,3,4),(64.1414162127729,64.8378306045337,65.8353356907573,66.8328407769809,
67.8303458632045,68.8278509494281,69.8253560356517,70.4246015199525),
 .UNSPECIFIED.);
#1620=B_SPLINE_CURVE_WITH_KNOTS('',3,(#76349,#76350,#76351,#76352,#76353,
#76354,#76355,#76356,#76357,#76358,#76359,#76360,#76361,#76362,#76363,#76364,
#76365,#76366,#76367,#76368,#76369,#76370),.UNSPECIFIED.,.F.,.F.,(4,3,3,
3,3,3,3,4),(-66.680827477437,-65.8353356907573,-64.8378306045337,-63.8403255183101,
-62.8428204320865,-61.8453153458629,-60.8478102596393,-60.3976421702575),
 .UNSPECIFIED.);
#1621=B_SPLINE_CURVE_WITH_KNOTS('',3,(#76375,#76376,#76377,#76378,#76379,
#76380,#76381,#76382,#76383,#76384,#76385,#76386,#76387,#76388,#76389,#76390,
#76391,#76392,#76393,#76394,#76395,#76396),.UNSPECIFIED.,.F.,.F.,(4,3,3,
3,3,3,3,4),(57.8582309055933,58.8528000871921,59.8503051734157,60.8478102596393,
61.8453153458629,62.8428204320865,63.8403255183101,64.1414162127729),
 .UNSPECIFIED.);
#1622=B_SPLINE_CURVE_WITH_KNOTS('',3,(#76397,#76398,#76399,#76400,#76401,
#76402,#76403,#76404,#76405,#76406,#76407,#76408,#76409,#76410,#76411,#76412,
#76413,#76414,#76415,#76416,#76417,#76418),.UNSPECIFIED.,.F.,.F.,(4,3,3,
3,3,3,3,4),(-60.3976421702575,-59.8503051734157,-58.8528000871921,-57.8552950009685,
-56.8577899147449,-55.8602848285213,-54.8627797422977,-54.1144568630778),
 .UNSPECIFIED.);
#1623=B_SPLINE_CURVE_WITH_KNOTS('',3,(#76423,#76424,#76425,#76426,#76427,
#76428,#76429,#76430,#76431,#76432,#76433,#76434,#76435,#76436,#76437,#76438,
#76439,#76440,#76441,#76442,#76443,#76444,#76445,#76446,#76447),
 .UNSPECIFIED.,.F.,.F.,(4,3,3,3,3,3,3,3,4),(51.5750455984137,51.870264483627,
52.8677695698506,53.8652746560741,54.8627797422977,55.8602848285213,56.8577899147449,
57.8552950009685,57.8582309055933),.UNSPECIFIED.);
#1624=B_SPLINE_CURVE_WITH_KNOTS('',3,(#76448,#76449,#76450,#76451,#76452,
#76453,#76454,#76455,#76456,#76457,#76458,#76459,#76460,#76461,#76462,#76463,
#76464,#76465,#76466,#76467,#76468,#76469,#76470,#76471,#76472),
 .UNSPECIFIED.,.F.,.F.,(4,3,3,3,3,3,3,3,4),(-54.1144568630778,-53.8652746560741,
-52.8677695698505,-51.870264483627,-50.8727593974034,-49.8752543111798,
-48.8777492249562,-47.8802441387326,-47.8312715558983),.UNSPECIFIED.);
#1625=B_SPLINE_CURVE_WITH_KNOTS('',3,(#76477,#76478,#76479,#76480,#76481,
#76482,#76483,#76484,#76485,#76486,#76487,#76488,#76489,#76490,#76491,#76492,
#76493,#76494,#76495,#76496,#76497,#76498),.UNSPECIFIED.,.F.,.F.,(4,3,3,
3,3,3,3,4),(45.2918602912341,45.8852339662854,46.882739052509,47.8802441387326,
48.8777492249562,49.8752543111798,50.8727593974034,51.5750455984137),
 .UNSPECIFIED.);
#1626=B_SPLINE_CURVE_WITH_KNOTS('',3,(#76499,#76500,#76501,#76502,#76503,
#76504,#76505,#76506,#76507,#76508,#76509,#76510,#76511,#76512,#76513,#76514,
#76515,#76516,#76517,#76518,#76519,#76520),.UNSPECIFIED.,.F.,.F.,(4,3,3,
3,3,3,3,4),(-47.8312715558983,-46.882739052509,-45.8852339662854,-44.8877288800618,
-43.8902237938382,-42.8927187076146,-41.895213621391,-41.5480862487187),
 .UNSPECIFIED.);
#1627=B_SPLINE_CURVE_WITH_KNOTS('',3,(#76525,#76526,#76527,#76528,#76529,
#76530,#76531,#76532,#76533,#76534,#76535,#76536,#76537,#76538,#76539,#76540,
#76541,#76542,#76543,#76544,#76545,#76546),.UNSPECIFIED.,.F.,.F.,(4,3,3,
3,3,3,3,4),(39.0086749840545,39.9002034489438,40.8977085351674,41.895213621391,
42.8927187076146,43.8902237938382,44.8877288800618,45.2918602912341),
 .UNSPECIFIED.);
#1628=B_SPLINE_CURVE_WITH_KNOTS('',3,(#76547,#76548,#76549,#76550,#76551,
#76552,#76553,#76554,#76555,#76556,#76557,#76558,#76559,#76560,#76561,#76562,
#76563,#76564,#76565,#76566,#76567,#76568),.UNSPECIFIED.,.F.,.F.,(4,3,3,
3,3,3,3,4),(-41.5480862487187,-40.8977085351674,-39.9002034489438,-38.9026983627202,
-37.9051932764966,-36.907688190273,-35.9101831040494,-35.2649009415391),
 .UNSPECIFIED.);
#1629=B_SPLINE_CURVE_WITH_KNOTS('',3,(#76573,#76574,#76575,#76576,#76577,
#76578,#76579,#76580,#76581,#76582,#76583,#76584,#76585,#76586,#76587,#76588,
#76589,#76590,#76591,#76592,#76593,#76594,#76595,#76596,#76597),
 .UNSPECIFIED.,.F.,.F.,(4,3,3,3,3,3,3,3,4),(32.725489676875,32.9176678453786,
33.9151729316022,34.9126780178258,35.9101831040494,36.907688190273,37.9051932764966,
38.9026983627202,39.0086749840545),.UNSPECIFIED.);
#1630=B_SPLINE_CURVE_WITH_KNOTS('',3,(#76598,#76599,#76600,#76601,#76602,
#76603,#76604,#76605,#76606,#76607,#76608,#76609,#76610,#76611,#76612,#76613,
#76614,#76615,#76616,#76617,#76618,#76619),.UNSPECIFIED.,.F.,.F.,(4,3,3,
3,3,3,3,4),(-35.2649009415391,-34.9126780178258,-33.9151729316022,-32.9176678453786,
-31.920162759155,-30.9226576729315,-29.9251525867079,-28.9817156343595),
 .UNSPECIFIED.);
#1631=B_SPLINE_CURVE_WITH_KNOTS('',3,(#76624,#76625,#76626,#76627,#76628,
#76629,#76630,#76631,#76632,#76633,#76634,#76635,#76636,#76637,#76638,#76639,
#76640,#76641,#76642,#76643,#76644,#76645),.UNSPECIFIED.,.F.,.F.,(4,3,3,
3,3,3,3,4),(26.4423043696954,26.9326373280371,27.9301424142607,28.9276475004843,
29.9251525867079,30.9226576729315,31.920162759155,32.725489676875),
 .UNSPECIFIED.);
#1632=B_SPLINE_CURVE_WITH_KNOTS('',3,(#76646,#76647,#76648,#76649,#76650,
#76651,#76652,#76653,#76654,#76655,#76656,#76657,#76658,#76659,#76660,#76661,
#76662,#76663,#76664,#76665,#76666,#76667,#76668,#76669,#76670),
 .UNSPECIFIED.,.F.,.F.,(4,3,3,3,3,3,3,3,4),(-28.9817156343595,-28.9276475004843,
-27.9301424142607,-26.9326373280371,-25.9351322418135,-24.9376271555899,
-23.9401220693663,-22.9426169831427,-22.6985303271799),.UNSPECIFIED.);
#1633=B_SPLINE_CURVE_WITH_KNOTS('',3,(#76675,#76676,#76677,#76678,#76679,
#76680,#76681,#76682,#76683,#76684,#76685,#76686,#76687,#76688,#76689,#76690,
#76691,#76692,#76693,#76694,#76695,#76696),.UNSPECIFIED.,.F.,.F.,(4,3,3,
3,3,3,3,4),(20.1591190625158,20.9476068106955,21.9451118969191,22.9426169831427,
23.9401220693663,24.9376271555899,25.9351322418135,26.4423043696954),
 .UNSPECIFIED.);
#1634=B_SPLINE_CURVE_WITH_KNOTS('',3,(#76697,#76698,#76699,#76700,#76701,
#76702,#76703,#76704,#76705,#76706,#76707,#76708,#76709,#76710,#76711,#76712,
#76713,#76714,#76715,#76716,#76717,#76718),.UNSPECIFIED.,.F.,.F.,(4,3,3,
3,3,3,3,4),(-22.6985303271799,-21.9451118969191,-20.9476068106955,-19.9501017244719,
-18.9525966382483,-17.9550915520247,-16.9575864658011,-16.4153450200003),
 .UNSPECIFIED.);
#1635=B_SPLINE_CURVE_WITH_KNOTS('',3,(#76723,#76724,#76725,#76726,#76727,
#76728,#76729,#76730,#76731,#76732,#76733,#76734,#76735,#76736,#76737,#76738,
#76739,#76740,#76741,#76742,#76743,#76744,#76745,#76746,#76747),
 .UNSPECIFIED.,.F.,.F.,(4,3,3,3,3,3,3,3,4),(13.8759337553362,13.9650712071303,
14.9625762933539,15.9600813795775,16.9575864658011,17.9550915520247,18.9525966382483,
19.9501017244719,20.1591190625158),.UNSPECIFIED.);
#1636=B_SPLINE_CURVE_WITH_KNOTS('',3,(#76748,#76749,#76750,#76751,#76752,
#76753,#76754,#76755,#76756,#76757,#76758,#76759,#76760,#76761,#76762,#76763,
#76764,#76765,#76766,#76767,#76768,#76769),.UNSPECIFIED.,.F.,.F.,(4,3,3,
3,3,3,3,4),(-16.4153450200003,-15.9600813795775,-14.9625762933539,-13.9650712071303,
-12.9675661209067,-11.9700610346831,-10.9725559484596,-10.1321597128207),
 .UNSPECIFIED.);
#1637=B_SPLINE_CURVE_WITH_KNOTS('',3,(#76775,#76776,#76777,#76778,#76779,
#76780,#76781,#76782,#76783,#76784,#76785,#76786,#76787),.UNSPECIFIED.,
 .F.,.F.,(4,3,3,3,4),(-3.84897440564114,-2.99251525867078,-1.99501017244719,
-0.997505086223593,0.),.UNSPECIFIED.);
#1638=B_SPLINE_CURVE_WITH_KNOTS('',3,(#76790,#76791,#76792,#76793,#76794,
#76795,#76796,#76797,#76798,#76799,#76800,#76801,#76802,#76803,#76804,#76805,
#76806,#76807,#76808),.UNSPECIFIED.,.F.,.F.,(4,3,3,3,3,3,4),(2.01694489302824,
2.99251525867079,3.99002034489439,4.98752543111799,5.98503051734158,6.98253560356518,
7.5927484481566),.UNSPECIFIED.);
#1639=B_SPLINE_CURVE_WITH_KNOTS('',3,(#76814,#76815,#76816,#76817),
 .UNSPECIFIED.,.F.,.F.,(4,4),(126.973269284569,127.68065103662),
 .UNSPECIFIED.);
#1640=B_SPLINE_CURVE_WITH_KNOTS('',3,(#76820,#76821,#76822,#76823,#76824,
#76825,#76826,#76827,#76828,#76829),.UNSPECIFIED.,.F.,.F.,(4,3,3,4),(-125.663706143592,
-124.688135777949,-123.690630691726,-123.229495242053),.UNSPECIFIED.);
#1641=B_SPLINE_CURVE_WITH_KNOTS('',3,(#76834,#76835,#76836,#76837,#76838,
#76839,#76840,#76841,#76842,#76843,#76844,#76845,#76846,#76847,#76848,#76849,
#76850,#76851,#76852,#76853,#76854,#76855,#76856,#76857,#76858),
 .UNSPECIFIED.,.F.,.F.,(4,3,3,3,3,3,3,3,4),(120.690083977389,120.698115433055,
121.695620519279,122.693125605502,123.690630691726,124.688135777949,125.685640864173,
126.683145950397,126.973269284569),.UNSPECIFIED.);
#1642=B_SPLINE_CURVE_WITH_KNOTS('',3,(#76859,#76860,#76861,#76862,#76863,
#76864,#76865,#76866,#76867,#76868,#76869,#76870,#76871,#76872,#76873,#76874,
#76875,#76876,#76877,#76878,#76879,#76880),.UNSPECIFIED.,.F.,.F.,(4,3,3,
3,3,3,3,4),(-123.229495242053,-122.693125605502,-121.695620519279,-120.698115433055,
-119.700610346831,-118.703105260608,-117.705600174384,-116.946309934874),
 .UNSPECIFIED.);
#1643=B_SPLINE_CURVE_WITH_KNOTS('',3,(#76885,#76886,#76887,#76888,#76889,
#76890,#76891,#76892,#76893,#76894,#76895,#76896,#76897,#76898,#76899,#76900,
#76901,#76902,#76903,#76904,#76905,#76906),.UNSPECIFIED.,.F.,.F.,(4,3,3,
3,3,3,3,4),(114.40689867021,114.713084915713,115.710590001937,116.708095088161,
117.705600174384,118.703105260608,119.700610346831,120.690083977389),
 .UNSPECIFIED.);
#1644=B_SPLINE_CURVE_WITH_KNOTS('',3,(#76907,#76908,#76909,#76910,#76911,
#76912,#76913,#76914,#76915,#76916,#76917,#76918,#76919,#76920,#76921,#76922,
#76923,#76924,#76925,#76926,#76927,#76928,#76929,#76930,#76931),
 .UNSPECIFIED.,.F.,.F.,(4,3,3,3,3,3,3,3,4),(-116.946309934874,-116.708095088161,
-115.710590001937,-114.713084915713,-113.71557982949,-112.718074743266,
-111.720569657043,-110.723064570819,-110.663124627694),.UNSPECIFIED.);
#1645=B_SPLINE_CURVE_WITH_KNOTS('',3,(#76936,#76937,#76938,#76939,#76940,
#76941,#76942,#76943,#76944,#76945,#76946,#76947,#76948,#76949,#76950,#76951,
#76952,#76953,#76954,#76955,#76956,#76957),.UNSPECIFIED.,.F.,.F.,(4,3,3,
3,3,3,3,4),(108.12371336303,108.728054398372,109.725559484595,110.723064570819,
111.720569657043,112.718074743266,113.71557982949,114.40689867021),
 .UNSPECIFIED.);
#1646=B_SPLINE_CURVE_WITH_KNOTS('',3,(#76958,#76959,#76960,#76961,#76962,
#76963,#76964,#76965,#76966,#76967,#76968,#76969,#76970,#76971,#76972,#76973,
#76974,#76975,#76976,#76977,#76978,#76979),.UNSPECIFIED.,.F.,.F.,(4,3,3,
3,3,3,3,4),(-110.663124627694,-109.725559484595,-108.728054398372,-107.730549312148,
-106.733044225925,-105.735539139701,-104.738034053477,-104.379939320515),
 .UNSPECIFIED.);
#1647=B_SPLINE_CURVE_WITH_KNOTS('',3,(#76984,#76985,#76986,#76987,#76988,
#76989,#76990,#76991,#76992,#76993,#76994,#76995,#76996,#76997,#76998,#76999,
#77000,#77001,#77002,#77003,#77004,#77005),.UNSPECIFIED.,.F.,.F.,(4,3,3,
3,3,3,3,4),(101.84052805585,102.74302388103,103.740528967254,104.738034053478,
105.735539139701,106.733044225925,107.730549312148,108.12371336303),
 .UNSPECIFIED.);
#1648=B_SPLINE_CURVE_WITH_KNOTS('',3,(#77006,#77007,#77008,#77009,#77010,
#77011,#77012,#77013,#77014,#77015,#77016,#77017,#77018,#77019,#77020,#77021,
#77022,#77023,#77024,#77025,#77026,#77027),.UNSPECIFIED.,.F.,.F.,(4,3,3,
3,3,3,3,4),(-104.379939320515,-103.740528967254,-102.74302388103,-101.745518794807,
-100.748013708583,-99.7505086223595,-98.7530035361359,-98.096754013335),
 .UNSPECIFIED.);
#1649=B_SPLINE_CURVE_WITH_KNOTS('',3,(#77032,#77033,#77034,#77035,#77036,
#77037,#77038,#77039,#77040,#77041,#77042,#77043,#77044,#77045,#77046,#77047,
#77048,#77049,#77050,#77051,#77052,#77053,#77054,#77055,#77056),
 .UNSPECIFIED.,.F.,.F.,(4,3,3,3,3,3,3,3,4),(95.5573427486709,95.7604882774652,
96.7579933636888,97.7554984499123,98.7530035361359,99.7505086223595,100.748013708583,
101.745518794807,101.84052805585),.UNSPECIFIED.);
#1650=B_SPLINE_CURVE_WITH_KNOTS('',3,(#77057,#77058,#77059,#77060,#77061,
#77062,#77063,#77064,#77065,#77066,#77067,#77068,#77069,#77070,#77071,#77072,
#77073,#77074,#77075,#77076,#77077,#77078),.UNSPECIFIED.,.F.,.F.,(4,3,3,
3,3,3,3,4),(-98.096754013335,-97.7554984499123,-96.7579933636887,-95.7604882774651,
-94.7629831912415,-93.7654781050179,-92.7679730187943,-91.8135687061554),
 .UNSPECIFIED.);
#1651=B_SPLINE_CURVE_WITH_KNOTS('',3,(#77083,#77084,#77085,#77086,#77087,
#77088,#77089,#77090,#77091,#77092,#77093,#77094,#77095,#77096,#77097,#77098,
#77099,#77100,#77101,#77102,#77103,#77104),.UNSPECIFIED.,.F.,.F.,(4,3,3,
3,3,3,3,4),(89.2741574414913,89.7754577601236,90.7729628463472,91.7704679325708,
92.7679730187944,93.765478105018,94.7629831912416,95.5573427486709),
 .UNSPECIFIED.);
#1652=B_SPLINE_CURVE_WITH_KNOTS('',3,(#77105,#77106,#77107,#77108,#77109,
#77110,#77111,#77112,#77113,#77114,#77115,#77116,#77117,#77118,#77119,#77120,
#77121,#77122,#77123,#77124,#77125,#77126,#77127,#77128,#77129),
 .UNSPECIFIED.,.F.,.F.,(4,3,3,3,3,3,3,3,4),(-91.8135687061554,-91.7704679325707,
-90.7729628463472,-89.7754577601236,-88.7779526739,-87.7804475876764,-86.7829425014528,
-85.7854374152292,-85.5303833989758),.UNSPECIFIED.);
#1653=B_SPLINE_CURVE_WITH_KNOTS('',3,(#77134,#77135,#77136,#77137,#77138,
#77139,#77140,#77141,#77142,#77143,#77144,#77145,#77146,#77147,#77148,#77149,
#77150,#77151,#77152,#77153,#77154,#77155),.UNSPECIFIED.,.F.,.F.,(4,3,3,
3,3,3,3,4),(82.9909721343117,83.790427242782,84.7879323290056,85.7854374152292,
86.7829425014528,87.7804475876764,88.7779526739,89.2741574414913),
 .UNSPECIFIED.);
#1654=B_SPLINE_CURVE_WITH_KNOTS('',3,(#77156,#77157,#77158,#77159,#77160,
#77161,#77162,#77163,#77164,#77165,#77166,#77167,#77168,#77169,#77170,#77171,
#77172,#77173,#77174,#77175,#77176,#77177),.UNSPECIFIED.,.F.,.F.,(4,3,3,
3,3,3,3,4),(-85.5303833989758,-84.7879323290056,-83.790427242782,-82.7929221565584,
-81.7954170703348,-80.7979119841112,-79.8004068978876,-79.2471980917962),
 .UNSPECIFIED.);
#1655=B_SPLINE_CURVE_WITH_KNOTS('',3,(#77182,#77183,#77184,#77185,#77186,
#77187,#77188,#77189,#77190,#77191,#77192,#77193,#77194,#77195,#77196,#77197,
#77198,#77199,#77200,#77201,#77202,#77203,#77204,#77205,#77206),
 .UNSPECIFIED.,.F.,.F.,(4,3,3,3,3,3,3,3,4),(76.7077868271321,76.8078916392168,
77.8053967254404,78.802901811664,79.8004068978876,80.7979119841112,81.7954170703348,
82.7929221565584,82.9909721343117),.UNSPECIFIED.);
#1656=B_SPLINE_CURVE_WITH_KNOTS('',3,(#77207,#77208,#77209,#77210,#77211,
#77212,#77213,#77214,#77215,#77216,#77217,#77218,#77219,#77220,#77221,#77222,
#77223,#77224,#77225,#77226,#77227,#77228),.UNSPECIFIED.,.F.,.F.,(4,3,3,
3,3,3,3,4),(-79.2471980917962,-78.802901811664,-77.8053967254404,-76.8078916392168,
-75.8103865529932,-74.8128814667696,-73.815376380546,-72.9640127846166),
 .UNSPECIFIED.);
#1657=B_SPLINE_CURVE_WITH_KNOTS('',3,(#77233,#77234,#77235,#77236,#77237,
#77238,#77239,#77240,#77241,#77242,#77243,#77244,#77245,#77246,#77247,#77248,
#77249,#77250,#77251,#77252,#77253,#77254),.UNSPECIFIED.,.F.,.F.,(4,3,3,
3,3,3,3,4),(70.4246015199525,70.8228611218753,71.8203662080989,72.8178712943225,
73.8153763805461,74.8128814667697,75.8103865529933,76.7077868271321),
 .UNSPECIFIED.);
#1658=B_SPLINE_CURVE_WITH_KNOTS('',3,(#77255,#77256,#77257,#77258,#77259,
#77260,#77261,#77262,#77263,#77264,#77265,#77266,#77267,#77268,#77269,#77270,
#77271,#77272,#77273,#77274,#77275,#77276,#77277,#77278,#77279),
 .UNSPECIFIED.,.F.,.F.,(4,3,3,3,3,3,3,3,4),(-72.9640127846166,-72.8178712943224,
-71.8203662080988,-70.8228611218753,-69.8253560356517,-68.8278509494281,
-67.8303458632045,-66.8328407769809,-66.680827477437),.UNSPECIFIED.);
#1659=B_SPLINE_CURVE_WITH_KNOTS('',3,(#77284,#77285,#77286,#77287,#77288,
#77289,#77290,#77291,#77292,#77293,#77294,#77295,#77296,#77297,#77298,#77299,
#77300,#77301,#77302,#77303,#77304,#77305),.UNSPECIFIED.,.F.,.F.,(4,3,3,
3,3,3,3,4),(64.1414162127729,64.8378306045337,65.8353356907573,66.8328407769809,
67.8303458632045,68.8278509494281,69.8253560356517,70.4246015199525),
 .UNSPECIFIED.);
#1660=B_SPLINE_CURVE_WITH_KNOTS('',3,(#77306,#77307,#77308,#77309,#77310,
#77311,#77312,#77313,#77314,#77315,#77316,#77317,#77318,#77319,#77320,#77321,
#77322,#77323,#77324,#77325,#77326,#77327),.UNSPECIFIED.,.F.,.F.,(4,3,3,
3,3,3,3,4),(-66.680827477437,-65.8353356907573,-64.8378306045337,-63.8403255183101,
-62.8428204320865,-61.8453153458629,-60.8478102596393,-60.3976421702575),
 .UNSPECIFIED.);
#1661=B_SPLINE_CURVE_WITH_KNOTS('',3,(#77332,#77333,#77334,#77335,#77336,
#77337,#77338,#77339,#77340,#77341,#77342,#77343,#77344,#77345,#77346,#77347,
#77348,#77349,#77350,#77351,#77352,#77353),.UNSPECIFIED.,.F.,.F.,(4,3,3,
3,3,3,3,4),(57.8582309055933,58.8528000871921,59.8503051734157,60.8478102596393,
61.8453153458629,62.8428204320865,63.8403255183101,64.1414162127729),
 .UNSPECIFIED.);
#1662=B_SPLINE_CURVE_WITH_KNOTS('',3,(#77354,#77355,#77356,#77357,#77358,
#77359,#77360,#77361,#77362,#77363,#77364,#77365,#77366,#77367,#77368,#77369,
#77370,#77371,#77372,#77373,#77374,#77375),.UNSPECIFIED.,.F.,.F.,(4,3,3,
3,3,3,3,4),(-60.3976421702575,-59.8503051734157,-58.8528000871921,-57.8552950009685,
-56.8577899147449,-55.8602848285213,-54.8627797422977,-54.1144568630778),
 .UNSPECIFIED.);
#1663=B_SPLINE_CURVE_WITH_KNOTS('',3,(#77380,#77381,#77382,#77383,#77384,
#77385,#77386,#77387,#77388,#77389,#77390,#77391,#77392,#77393,#77394,#77395,
#77396,#77397,#77398,#77399,#77400,#77401,#77402,#77403,#77404),
 .UNSPECIFIED.,.F.,.F.,(4,3,3,3,3,3,3,3,4),(51.5750455984137,51.870264483627,
52.8677695698506,53.8652746560742,54.8627797422978,55.8602848285214,56.857789914745,
57.8552950009686,57.8582309055933),.UNSPECIFIED.);
#1664=B_SPLINE_CURVE_WITH_KNOTS('',3,(#77405,#77406,#77407,#77408,#77409,
#77410,#77411,#77412,#77413,#77414,#77415,#77416,#77417,#77418,#77419,#77420,
#77421,#77422,#77423,#77424,#77425,#77426,#77427,#77428,#77429),
 .UNSPECIFIED.,.F.,.F.,(4,3,3,3,3,3,3,3,4),(-54.1144568630778,-53.8652746560741,
-52.8677695698505,-51.8702644836269,-50.8727593974033,-49.8752543111798,
-48.8777492249562,-47.8802441387326,-47.8312715558983),.UNSPECIFIED.);
#1665=B_SPLINE_CURVE_WITH_KNOTS('',3,(#77434,#77435,#77436,#77437,#77438,
#77439,#77440,#77441,#77442,#77443,#77444,#77445,#77446,#77447,#77448,#77449,
#77450,#77451,#77452,#77453,#77454,#77455),.UNSPECIFIED.,.F.,.F.,(4,3,3,
3,3,3,3,4),(45.2918602912341,45.8852339662854,46.882739052509,47.8802441387326,
48.8777492249562,49.8752543111798,50.8727593974034,51.5750455984137),
 .UNSPECIFIED.);
#1666=B_SPLINE_CURVE_WITH_KNOTS('',3,(#77456,#77457,#77458,#77459,#77460,
#77461,#77462,#77463,#77464,#77465,#77466,#77467,#77468,#77469,#77470,#77471,
#77472,#77473,#77474,#77475,#77476,#77477),.UNSPECIFIED.,.F.,.F.,(4,3,3,
3,3,3,3,4),(-47.8312715558983,-46.882739052509,-45.8852339662854,-44.8877288800618,
-43.8902237938382,-42.8927187076146,-41.895213621391,-41.5480862487187),
 .UNSPECIFIED.);
#1667=B_SPLINE_CURVE_WITH_KNOTS('',3,(#77482,#77483,#77484,#77485,#77486,
#77487,#77488,#77489,#77490,#77491,#77492,#77493,#77494,#77495,#77496,#77497,
#77498,#77499,#77500,#77501,#77502,#77503),.UNSPECIFIED.,.F.,.F.,(4,3,3,
3,3,3,3,4),(39.0086749840545,39.9002034489438,40.8977085351674,41.895213621391,
42.8927187076146,43.8902237938382,44.8877288800618,45.2918602912341),
 .UNSPECIFIED.);
#1668=B_SPLINE_CURVE_WITH_KNOTS('',3,(#77504,#77505,#77506,#77507,#77508,
#77509,#77510,#77511,#77512,#77513,#77514,#77515,#77516,#77517,#77518,#77519,
#77520,#77521,#77522,#77523,#77524,#77525),.UNSPECIFIED.,.F.,.F.,(4,3,3,
3,3,3,3,4),(-41.5480862487187,-40.8977085351674,-39.9002034489438,-38.9026983627202,
-37.9051932764966,-36.907688190273,-35.9101831040494,-35.2649009415391),
 .UNSPECIFIED.);
#1669=B_SPLINE_CURVE_WITH_KNOTS('',3,(#77530,#77531,#77532,#77533,#77534,
#77535,#77536,#77537,#77538,#77539,#77540,#77541,#77542,#77543,#77544,#77545,
#77546,#77547,#77548,#77549,#77550,#77551,#77552,#77553,#77554),
 .UNSPECIFIED.,.F.,.F.,(4,3,3,3,3,3,3,3,4),(32.725489676875,32.9176678453786,
33.9151729316022,34.9126780178258,35.9101831040494,36.907688190273,37.9051932764966,
38.9026983627202,39.0086749840545),.UNSPECIFIED.);
#1670=B_SPLINE_CURVE_WITH_KNOTS('',3,(#77555,#77556,#77557,#77558,#77559,
#77560,#77561,#77562,#77563,#77564,#77565,#77566,#77567,#77568,#77569,#77570,
#77571,#77572,#77573,#77574,#77575,#77576),.UNSPECIFIED.,.F.,.F.,(4,3,3,
3,3,3,3,4),(-35.2649009415391,-34.9126780178258,-33.9151729316022,-32.9176678453786,
-31.920162759155,-30.9226576729314,-29.9251525867079,-28.9817156343595),
 .UNSPECIFIED.);
#1671=B_SPLINE_CURVE_WITH_KNOTS('',3,(#77581,#77582,#77583,#77584,#77585,
#77586,#77587,#77588,#77589,#77590,#77591,#77592,#77593,#77594,#77595,#77596,
#77597,#77598,#77599,#77600,#77601,#77602),.UNSPECIFIED.,.F.,.F.,(4,3,3,
3,3,3,3,4),(26.4423043696954,26.9326373280371,27.9301424142607,28.9276475004843,
29.9251525867079,30.9226576729315,31.920162759155,32.725489676875),
 .UNSPECIFIED.);
#1672=B_SPLINE_CURVE_WITH_KNOTS('',3,(#77603,#77604,#77605,#77606,#77607,
#77608,#77609,#77610,#77611,#77612,#77613,#77614,#77615,#77616,#77617,#77618,
#77619,#77620,#77621,#77622,#77623,#77624,#77625,#77626,#77627),
 .UNSPECIFIED.,.F.,.F.,(4,3,3,3,3,3,3,3,4),(-28.9817156343595,-28.9276475004843,
-27.9301424142607,-26.9326373280371,-25.9351322418135,-24.9376271555899,
-23.9401220693663,-22.9426169831427,-22.6985303271799),.UNSPECIFIED.);
#1673=B_SPLINE_CURVE_WITH_KNOTS('',3,(#77632,#77633,#77634,#77635,#77636,
#77637,#77638,#77639,#77640,#77641,#77642,#77643,#77644,#77645,#77646,#77647,
#77648,#77649,#77650,#77651,#77652,#77653),.UNSPECIFIED.,.F.,.F.,(4,3,3,
3,3,3,3,4),(20.1591190625158,20.9476068106955,21.9451118969191,22.9426169831427,
23.9401220693663,24.9376271555899,25.9351322418135,26.4423043696954),
 .UNSPECIFIED.);
#1674=B_SPLINE_CURVE_WITH_KNOTS('',3,(#77654,#77655,#77656,#77657,#77658,
#77659,#77660,#77661,#77662,#77663,#77664,#77665,#77666,#77667,#77668,#77669,
#77670,#77671,#77672,#77673,#77674,#77675),.UNSPECIFIED.,.F.,.F.,(4,3,3,
3,3,3,3,4),(-22.6985303271799,-21.9451118969191,-20.9476068106955,-19.9501017244719,
-18.9525966382483,-17.9550915520247,-16.9575864658011,-16.4153450200003),
 .UNSPECIFIED.);
#1675=B_SPLINE_CURVE_WITH_KNOTS('',3,(#77680,#77681,#77682,#77683,#77684,
#77685,#77686,#77687,#77688,#77689,#77690,#77691,#77692,#77693,#77694,#77695,
#77696,#77697,#77698,#77699,#77700,#77701,#77702,#77703,#77704),
 .UNSPECIFIED.,.F.,.F.,(4,3,3,3,3,3,3,3,4),(13.8759337553362,13.9650712071303,
14.9625762933539,15.9600813795775,16.9575864658011,17.9550915520247,18.9525966382483,
19.9501017244719,20.1591190625158),.UNSPECIFIED.);
#1676=B_SPLINE_CURVE_WITH_KNOTS('',3,(#77705,#77706,#77707,#77708,#77709,
#77710,#77711,#77712,#77713,#77714,#77715,#77716,#77717,#77718,#77719,#77720,
#77721,#77722,#77723,#77724,#77725,#77726),.UNSPECIFIED.,.F.,.F.,(4,3,3,
3,3,3,3,4),(-16.4153450200003,-15.9600813795775,-14.9625762933539,-13.9650712071303,
-12.9675661209067,-11.9700610346831,-10.9725559484595,-10.1321597128207),
 .UNSPECIFIED.);
#1677=B_SPLINE_CURVE_WITH_KNOTS('',3,(#77732,#77733,#77734,#77735,#77736,
#77737,#77738,#77739,#77740,#77741,#77742,#77743,#77744),.UNSPECIFIED.,
 .F.,.F.,(4,3,3,3,4),(-3.84897440564114,-2.99251525867079,-1.99501017244719,
-0.997505086223596,0.),.UNSPECIFIED.);
#1678=B_SPLINE_CURVE_WITH_KNOTS('',3,(#77747,#77748,#77749,#77750,#77751,
#77752,#77753,#77754,#77755,#77756,#77757,#77758,#77759,#77760,#77761,#77762,
#77763,#77764,#77765),.UNSPECIFIED.,.F.,.F.,(4,3,3,3,3,3,4),(2.01694489302841,
2.99251525867079,3.99002034489439,4.98752543111798,5.98503051734158,6.98253560356517,
7.5927484481566),.UNSPECIFIED.);
#1679=B_SPLINE_CURVE_WITH_KNOTS('',3,(#77771,#77772,#77773,#77774),
 .UNSPECIFIED.,.F.,.F.,(4,4),(126.973269284569,127.68065103662),
 .UNSPECIFIED.);
#1680=B_SPLINE_CURVE_WITH_KNOTS('',3,(#77777,#77778,#77779,#77780,#77781,
#77782,#77783,#77784,#77785,#77786),.UNSPECIFIED.,.F.,.F.,(4,3,3,4),(-125.663706143592,
-124.688135777949,-123.690630691726,-123.229495242053),.UNSPECIFIED.);
#1681=B_SPLINE_CURVE_WITH_KNOTS('',3,(#77791,#77792,#77793,#77794,#77795,
#77796,#77797,#77798,#77799,#77800,#77801,#77802,#77803,#77804,#77805,#77806,
#77807,#77808,#77809,#77810,#77811,#77812,#77813,#77814,#77815),
 .UNSPECIFIED.,.F.,.F.,(4,3,3,3,3,3,3,3,4),(120.690083977389,120.698115433055,
121.695620519279,122.693125605502,123.690630691726,124.688135777949,125.685640864173,
126.683145950397,126.973269284569),.UNSPECIFIED.);
#1682=B_SPLINE_CURVE_WITH_KNOTS('',3,(#77816,#77817,#77818,#77819,#77820,
#77821,#77822,#77823,#77824,#77825,#77826,#77827,#77828,#77829,#77830,#77831,
#77832,#77833,#77834,#77835,#77836,#77837),.UNSPECIFIED.,.F.,.F.,(4,3,3,
3,3,3,3,4),(-123.229495242053,-122.693125605502,-121.695620519279,-120.698115433055,
-119.700610346831,-118.703105260608,-117.705600174384,-116.946309934874),
 .UNSPECIFIED.);
#1683=B_SPLINE_CURVE_WITH_KNOTS('',3,(#77842,#77843,#77844,#77845,#77846,
#77847,#77848,#77849,#77850,#77851,#77852,#77853,#77854,#77855,#77856,#77857,
#77858,#77859,#77860,#77861,#77862,#77863),.UNSPECIFIED.,.F.,.F.,(4,3,3,
3,3,3,3,4),(114.40689867021,114.713084915713,115.710590001937,116.708095088161,
117.705600174384,118.703105260608,119.700610346831,120.690083977389),
 .UNSPECIFIED.);
#1684=B_SPLINE_CURVE_WITH_KNOTS('',3,(#77864,#77865,#77866,#77867,#77868,
#77869,#77870,#77871,#77872,#77873,#77874,#77875,#77876,#77877,#77878,#77879,
#77880,#77881,#77882,#77883,#77884,#77885,#77886,#77887,#77888),
 .UNSPECIFIED.,.F.,.F.,(4,3,3,3,3,3,3,3,4),(-116.946309934874,-116.708095088161,
-115.710590001937,-114.713084915713,-113.71557982949,-112.718074743266,
-111.720569657043,-110.723064570819,-110.663124627694),.UNSPECIFIED.);
#1685=B_SPLINE_CURVE_WITH_KNOTS('',3,(#77893,#77894,#77895,#77896,#77897,
#77898,#77899,#77900,#77901,#77902,#77903,#77904,#77905,#77906,#77907,#77908,
#77909,#77910,#77911,#77912,#77913,#77914),.UNSPECIFIED.,.F.,.F.,(4,3,3,
3,3,3,3,4),(108.12371336303,108.728054398372,109.725559484595,110.723064570819,
111.720569657043,112.718074743266,113.71557982949,114.40689867021),
 .UNSPECIFIED.);
#1686=B_SPLINE_CURVE_WITH_KNOTS('',3,(#77915,#77916,#77917,#77918,#77919,
#77920,#77921,#77922,#77923,#77924,#77925,#77926,#77927,#77928,#77929,#77930,
#77931,#77932,#77933,#77934,#77935,#77936),.UNSPECIFIED.,.F.,.F.,(4,3,3,
3,3,3,3,4),(-110.663124627694,-109.725559484595,-108.728054398372,-107.730549312148,
-106.733044225925,-105.735539139701,-104.738034053477,-104.379939320515),
 .UNSPECIFIED.);
#1687=B_SPLINE_CURVE_WITH_KNOTS('',3,(#77941,#77942,#77943,#77944,#77945,
#77946,#77947,#77948,#77949,#77950,#77951,#77952,#77953,#77954,#77955,#77956,
#77957,#77958,#77959,#77960,#77961,#77962),.UNSPECIFIED.,.F.,.F.,(4,3,3,
3,3,3,3,4),(101.84052805585,102.74302388103,103.740528967254,104.738034053478,
105.735539139701,106.733044225925,107.730549312148,108.12371336303),
 .UNSPECIFIED.);
#1688=B_SPLINE_CURVE_WITH_KNOTS('',3,(#77963,#77964,#77965,#77966,#77967,
#77968,#77969,#77970,#77971,#77972,#77973,#77974,#77975,#77976,#77977,#77978,
#77979,#77980,#77981,#77982,#77983,#77984),.UNSPECIFIED.,.F.,.F.,(4,3,3,
3,3,3,3,4),(-104.379939320515,-103.740528967254,-102.74302388103,-101.745518794807,
-100.748013708583,-99.7505086223595,-98.7530035361359,-98.096754013335),
 .UNSPECIFIED.);
#1689=B_SPLINE_CURVE_WITH_KNOTS('',3,(#77989,#77990,#77991,#77992,#77993,
#77994,#77995,#77996,#77997,#77998,#77999,#78000,#78001,#78002,#78003,#78004,
#78005,#78006,#78007,#78008,#78009,#78010,#78011,#78012,#78013),
 .UNSPECIFIED.,.F.,.F.,(4,3,3,3,3,3,3,3,4),(95.5573427486709,95.7604882774652,
96.7579933636888,97.7554984499123,98.7530035361359,99.7505086223595,100.748013708583,
101.745518794807,101.84052805585),.UNSPECIFIED.);
#1690=B_SPLINE_CURVE_WITH_KNOTS('',3,(#78014,#78015,#78016,#78017,#78018,
#78019,#78020,#78021,#78022,#78023,#78024,#78025,#78026,#78027,#78028,#78029,
#78030,#78031,#78032,#78033,#78034,#78035),.UNSPECIFIED.,.F.,.F.,(4,3,3,
3,3,3,3,4),(-98.096754013335,-97.7554984499123,-96.7579933636887,-95.7604882774651,
-94.7629831912415,-93.7654781050179,-92.7679730187943,-91.8135687061554),
 .UNSPECIFIED.);
#1691=B_SPLINE_CURVE_WITH_KNOTS('',3,(#78040,#78041,#78042,#78043,#78044,
#78045,#78046,#78047,#78048,#78049,#78050,#78051,#78052,#78053,#78054,#78055,
#78056,#78057,#78058,#78059,#78060,#78061),.UNSPECIFIED.,.F.,.F.,(4,3,3,
3,3,3,3,4),(89.2741574414913,89.7754577601236,90.7729628463472,91.7704679325708,
92.7679730187944,93.765478105018,94.7629831912416,95.5573427486709),
 .UNSPECIFIED.);
#1692=B_SPLINE_CURVE_WITH_KNOTS('',3,(#78062,#78063,#78064,#78065,#78066,
#78067,#78068,#78069,#78070,#78071,#78072,#78073,#78074,#78075,#78076,#78077,
#78078,#78079,#78080,#78081,#78082,#78083,#78084,#78085,#78086),
 .UNSPECIFIED.,.F.,.F.,(4,3,3,3,3,3,3,3,4),(-91.8135687061554,-91.7704679325708,
-90.7729628463472,-89.7754577601236,-88.7779526739,-87.7804475876764,-86.7829425014528,
-85.7854374152292,-85.5303833989758),.UNSPECIFIED.);
#1693=B_SPLINE_CURVE_WITH_KNOTS('',3,(#78091,#78092,#78093,#78094,#78095,
#78096,#78097,#78098,#78099,#78100,#78101,#78102,#78103,#78104,#78105,#78106,
#78107,#78108,#78109,#78110,#78111,#78112),.UNSPECIFIED.,.F.,.F.,(4,3,3,
3,3,3,3,4),(82.9909721343117,83.790427242782,84.7879323290056,85.7854374152292,
86.7829425014528,87.7804475876764,88.7779526739,89.2741574414913),
 .UNSPECIFIED.);
#1694=B_SPLINE_CURVE_WITH_KNOTS('',3,(#78113,#78114,#78115,#78116,#78117,
#78118,#78119,#78120,#78121,#78122,#78123,#78124,#78125,#78126,#78127,#78128,
#78129,#78130,#78131,#78132,#78133,#78134),.UNSPECIFIED.,.F.,.F.,(4,3,3,
3,3,3,3,4),(-85.5303833989758,-84.7879323290056,-83.790427242782,-82.7929221565584,
-81.7954170703348,-80.7979119841112,-79.8004068978876,-79.2471980917962),
 .UNSPECIFIED.);
#1695=B_SPLINE_CURVE_WITH_KNOTS('',3,(#78139,#78140,#78141,#78142,#78143,
#78144,#78145,#78146,#78147,#78148,#78149,#78150,#78151,#78152,#78153,#78154,
#78155,#78156,#78157,#78158,#78159,#78160,#78161,#78162,#78163),
 .UNSPECIFIED.,.F.,.F.,(4,3,3,3,3,3,3,3,4),(76.7077868271321,76.8078916392168,
77.8053967254404,78.802901811664,79.8004068978876,80.7979119841112,81.7954170703348,
82.7929221565584,82.9909721343117),.UNSPECIFIED.);
#1696=B_SPLINE_CURVE_WITH_KNOTS('',3,(#78164,#78165,#78166,#78167,#78168,
#78169,#78170,#78171,#78172,#78173,#78174,#78175,#78176,#78177,#78178,#78179,
#78180,#78181,#78182,#78183,#78184,#78185),.UNSPECIFIED.,.F.,.F.,(4,3,3,
3,3,3,3,4),(-79.2471980917962,-78.802901811664,-77.8053967254404,-76.8078916392168,
-75.8103865529932,-74.8128814667696,-73.815376380546,-72.9640127846166),
 .UNSPECIFIED.);
#1697=B_SPLINE_CURVE_WITH_KNOTS('',3,(#78190,#78191,#78192,#78193,#78194,
#78195,#78196,#78197,#78198,#78199,#78200,#78201,#78202,#78203,#78204,#78205,
#78206,#78207,#78208,#78209,#78210,#78211),.UNSPECIFIED.,.F.,.F.,(4,3,3,
3,3,3,3,4),(70.4246015199525,70.8228611218753,71.8203662080989,72.8178712943224,
73.8153763805461,74.8128814667696,75.8103865529933,76.7077868271321),
 .UNSPECIFIED.);
#1698=B_SPLINE_CURVE_WITH_KNOTS('',3,(#78212,#78213,#78214,#78215,#78216,
#78217,#78218,#78219,#78220,#78221,#78222,#78223,#78224,#78225,#78226,#78227,
#78228,#78229,#78230,#78231,#78232,#78233,#78234,#78235,#78236),
 .UNSPECIFIED.,.F.,.F.,(4,3,3,3,3,3,3,3,4),(-72.9640127846166,-72.8178712943224,
-71.8203662080988,-70.8228611218752,-69.8253560356517,-68.827850949428,
-67.8303458632045,-66.8328407769809,-66.680827477437),.UNSPECIFIED.);
#1699=B_SPLINE_CURVE_WITH_KNOTS('',3,(#78241,#78242,#78243,#78244,#78245,
#78246,#78247,#78248,#78249,#78250,#78251,#78252,#78253,#78254,#78255,#78256,
#78257,#78258,#78259,#78260,#78261,#78262),.UNSPECIFIED.,.F.,.F.,(4,3,3,
3,3,3,3,4),(64.1414162127729,64.8378306045337,65.8353356907573,66.8328407769809,
67.8303458632045,68.8278509494281,69.8253560356517,70.4246015199525),
 .UNSPECIFIED.);
#1700=B_SPLINE_CURVE_WITH_KNOTS('',3,(#78263,#78264,#78265,#78266,#78267,
#78268,#78269,#78270,#78271,#78272,#78273,#78274,#78275,#78276,#78277,#78278,
#78279,#78280,#78281,#78282,#78283,#78284),.UNSPECIFIED.,.F.,.F.,(4,3,3,
3,3,3,3,4),(-66.680827477437,-65.8353356907573,-64.8378306045337,-63.8403255183101,
-62.8428204320865,-61.8453153458629,-60.8478102596393,-60.3976421702574),
 .UNSPECIFIED.);
#1701=B_SPLINE_CURVE_WITH_KNOTS('',3,(#78289,#78290,#78291,#78292,#78293,
#78294,#78295,#78296,#78297,#78298,#78299,#78300,#78301,#78302,#78303,#78304,
#78305,#78306,#78307,#78308,#78309,#78310),.UNSPECIFIED.,.F.,.F.,(4,3,3,
3,3,3,3,4),(57.8582309055933,58.8528000871921,59.8503051734157,60.8478102596393,
61.8453153458629,62.8428204320865,63.8403255183101,64.1414162127729),
 .UNSPECIFIED.);
#1702=B_SPLINE_CURVE_WITH_KNOTS('',3,(#78311,#78312,#78313,#78314,#78315,
#78316,#78317,#78318,#78319,#78320,#78321,#78322,#78323,#78324,#78325,#78326,
#78327,#78328,#78329,#78330,#78331,#78332),.UNSPECIFIED.,.F.,.F.,(4,3,3,
3,3,3,3,4),(-60.3976421702574,-59.8503051734157,-58.8528000871921,-57.8552950009685,
-56.8577899147449,-55.8602848285213,-54.8627797422977,-54.1144568630778),
 .UNSPECIFIED.);
#1703=B_SPLINE_CURVE_WITH_KNOTS('',3,(#78337,#78338,#78339,#78340,#78341,
#78342,#78343,#78344,#78345,#78346,#78347,#78348,#78349,#78350,#78351,#78352,
#78353,#78354,#78355,#78356,#78357,#78358,#78359,#78360,#78361),
 .UNSPECIFIED.,.F.,.F.,(4,3,3,3,3,3,3,3,4),(51.5750455984137,51.870264483627,
52.8677695698506,53.8652746560742,54.8627797422977,55.8602848285214,56.8577899147449,
57.8552950009685,57.8582309055933),.UNSPECIFIED.);
#1704=B_SPLINE_CURVE_WITH_KNOTS('',3,(#78362,#78363,#78364,#78365,#78366,
#78367,#78368,#78369,#78370,#78371,#78372,#78373,#78374,#78375,#78376,#78377,
#78378,#78379,#78380,#78381,#78382,#78383,#78384,#78385,#78386),
 .UNSPECIFIED.,.F.,.F.,(4,3,3,3,3,3,3,3,4),(-54.1144568630778,-53.8652746560741,
-52.8677695698505,-51.8702644836269,-50.8727593974033,-49.8752543111797,
-48.8777492249561,-47.8802441387326,-47.8312715558983),.UNSPECIFIED.);
#1705=B_SPLINE_CURVE_WITH_KNOTS('',3,(#78391,#78392,#78393,#78394,#78395,
#78396,#78397,#78398,#78399,#78400,#78401,#78402,#78403,#78404,#78405,#78406,
#78407,#78408,#78409,#78410,#78411,#78412),.UNSPECIFIED.,.F.,.F.,(4,3,3,
3,3,3,3,4),(45.2918602912341,45.8852339662854,46.882739052509,47.8802441387326,
48.8777492249562,49.8752543111798,50.8727593974034,51.5750455984137),
 .UNSPECIFIED.);
#1706=B_SPLINE_CURVE_WITH_KNOTS('',3,(#78413,#78414,#78415,#78416,#78417,
#78418,#78419,#78420,#78421,#78422,#78423,#78424,#78425,#78426,#78427,#78428,
#78429,#78430,#78431,#78432,#78433,#78434),.UNSPECIFIED.,.F.,.F.,(4,3,3,
3,3,3,3,4),(-47.8312715558983,-46.882739052509,-45.8852339662854,-44.8877288800618,
-43.8902237938382,-42.8927187076146,-41.895213621391,-41.5480862487187),
 .UNSPECIFIED.);
#1707=B_SPLINE_CURVE_WITH_KNOTS('',3,(#78439,#78440,#78441,#78442,#78443,
#78444,#78445,#78446,#78447,#78448,#78449,#78450,#78451,#78452,#78453,#78454,
#78455,#78456,#78457,#78458,#78459,#78460),.UNSPECIFIED.,.F.,.F.,(4,3,3,
3,3,3,3,4),(39.0086749840545,39.9002034489438,40.8977085351674,41.895213621391,
42.8927187076146,43.8902237938382,44.8877288800618,45.2918602912341),
 .UNSPECIFIED.);
#1708=B_SPLINE_CURVE_WITH_KNOTS('',3,(#78461,#78462,#78463,#78464,#78465,
#78466,#78467,#78468,#78469,#78470,#78471,#78472,#78473,#78474,#78475,#78476,
#78477,#78478,#78479,#78480,#78481,#78482),.UNSPECIFIED.,.F.,.F.,(4,3,3,
3,3,3,3,4),(-41.5480862487187,-40.8977085351674,-39.9002034489438,-38.9026983627202,
-37.9051932764966,-36.907688190273,-35.9101831040494,-35.2649009415391),
 .UNSPECIFIED.);
#1709=B_SPLINE_CURVE_WITH_KNOTS('',3,(#78487,#78488,#78489,#78490,#78491,
#78492,#78493,#78494,#78495,#78496,#78497,#78498,#78499,#78500,#78501,#78502,
#78503,#78504,#78505,#78506,#78507,#78508,#78509,#78510,#78511),
 .UNSPECIFIED.,.F.,.F.,(4,3,3,3,3,3,3,3,4),(32.7254896768749,32.9176678453786,
33.9151729316022,34.9126780178258,35.9101831040494,36.907688190273,37.9051932764966,
38.9026983627202,39.0086749840545),.UNSPECIFIED.);
#1710=B_SPLINE_CURVE_WITH_KNOTS('',3,(#78512,#78513,#78514,#78515,#78516,
#78517,#78518,#78519,#78520,#78521,#78522,#78523,#78524,#78525,#78526,#78527,
#78528,#78529,#78530,#78531,#78532,#78533),.UNSPECIFIED.,.F.,.F.,(4,3,3,
3,3,3,3,4),(-35.2649009415391,-34.9126780178258,-33.9151729316022,-32.9176678453786,
-31.920162759155,-30.9226576729314,-29.9251525867078,-28.9817156343595),
 .UNSPECIFIED.);
#1711=B_SPLINE_CURVE_WITH_KNOTS('',3,(#78538,#78539,#78540,#78541,#78542,
#78543,#78544,#78545,#78546,#78547,#78548,#78549,#78550,#78551,#78552,#78553,
#78554,#78555,#78556,#78557,#78558,#78559),.UNSPECIFIED.,.F.,.F.,(4,3,3,
3,3,3,3,4),(26.4423043696953,26.9326373280371,27.9301424142607,28.9276475004843,
29.9251525867079,30.9226576729315,31.920162759155,32.7254896768749),
 .UNSPECIFIED.);
#1712=B_SPLINE_CURVE_WITH_KNOTS('',3,(#78560,#78561,#78562,#78563,#78564,
#78565,#78566,#78567,#78568,#78569,#78570,#78571,#78572,#78573,#78574,#78575,
#78576,#78577,#78578,#78579,#78580,#78581,#78582,#78583,#78584),
 .UNSPECIFIED.,.F.,.F.,(4,3,3,3,3,3,3,3,4),(-28.9817156343595,-28.9276475004843,
-27.9301424142607,-26.9326373280371,-25.9351322418135,-24.9376271555899,
-23.9401220693663,-22.9426169831427,-22.6985303271799),.UNSPECIFIED.);
#1713=B_SPLINE_CURVE_WITH_KNOTS('',3,(#78589,#78590,#78591,#78592,#78593,
#78594,#78595,#78596,#78597,#78598,#78599,#78600,#78601,#78602,#78603,#78604,
#78605,#78606,#78607,#78608,#78609,#78610),.UNSPECIFIED.,.F.,.F.,(4,3,3,
3,3,3,3,4),(20.1591190625158,20.9476068106955,21.9451118969191,22.9426169831427,
23.9401220693663,24.9376271555899,25.9351322418135,26.4423043696953),
 .UNSPECIFIED.);
#1714=B_SPLINE_CURVE_WITH_KNOTS('',3,(#78611,#78612,#78613,#78614,#78615,
#78616,#78617,#78618,#78619,#78620,#78621,#78622,#78623,#78624,#78625,#78626,
#78627,#78628,#78629,#78630,#78631,#78632),.UNSPECIFIED.,.F.,.F.,(4,3,3,
3,3,3,3,4),(-22.6985303271799,-21.9451118969191,-20.9476068106955,-19.9501017244719,
-18.9525966382483,-17.9550915520247,-16.9575864658011,-16.4153450200003),
 .UNSPECIFIED.);
#1715=B_SPLINE_CURVE_WITH_KNOTS('',3,(#78637,#78638,#78639,#78640,#78641,
#78642,#78643,#78644,#78645,#78646,#78647,#78648,#78649,#78650,#78651,#78652,
#78653,#78654,#78655,#78656,#78657,#78658,#78659,#78660,#78661),
 .UNSPECIFIED.,.F.,.F.,(4,3,3,3,3,3,3,3,4),(13.8759337553362,13.9650712071303,
14.9625762933539,15.9600813795775,16.9575864658011,17.9550915520247,18.9525966382483,
19.9501017244719,20.1591190625158),.UNSPECIFIED.);
#1716=B_SPLINE_CURVE_WITH_KNOTS('',3,(#78662,#78663,#78664,#78665,#78666,
#78667,#78668,#78669,#78670,#78671,#78672,#78673,#78674,#78675,#78676,#78677,
#78678,#78679,#78680,#78681,#78682,#78683),.UNSPECIFIED.,.F.,.F.,(4,3,3,
3,3,3,3,4),(-16.4153450200003,-15.9600813795775,-14.9625762933539,-13.9650712071303,
-12.9675661209067,-11.9700610346831,-10.9725559484596,-10.1321597128207),
 .UNSPECIFIED.);
#1717=B_SPLINE_CURVE_WITH_KNOTS('',3,(#78689,#78690,#78691,#78692,#78693,
#78694,#78695,#78696,#78697,#78698,#78699,#78700,#78701),.UNSPECIFIED.,
 .F.,.F.,(4,3,3,3,4),(-3.84897440564113,-2.99251525867078,-1.99501017244719,
-0.997505086223595,0.),.UNSPECIFIED.);
#1718=B_SPLINE_CURVE_WITH_KNOTS('',3,(#78704,#78705,#78706,#78707,#78708,
#78709,#78710,#78711,#78712,#78713,#78714,#78715,#78716,#78717,#78718,#78719,
#78720,#78721,#78722),.UNSPECIFIED.,.F.,.F.,(4,3,3,3,3,3,4),(2.01694489302833,
2.99251525867079,3.99002034489438,4.98752543111798,5.98503051734158,6.98253560356517,
7.59274844815659),.UNSPECIFIED.);
#1719=B_SPLINE_CURVE_WITH_KNOTS('',3,(#78728,#78729,#78730,#78731,#78732,
#78733,#78734,#78735),.UNSPECIFIED.,.F.,.F.,(4,1,1,1,1,4),(135.088484104361,
135.549619554034,136.547124640257,137.544629726481,138.542134812704,139.539639898928),
 .UNSPECIFIED.);
#1720=B_SPLINE_CURVE_WITH_KNOTS('',3,(#78738,#78739,#78740,#78741,#78742,
#78743,#78744,#78745,#78746),.UNSPECIFIED.,.F.,.F.,(4,1,1,1,1,1,4),(135.088484104361,
135.096515560027,136.09402064625,137.091525732474,138.089030818698,139.086535904921,
140.062106270563),.UNSPECIFIED.);
#1721=B_SPLINE_CURVE_WITH_KNOTS('',3,(#78751,#78752,#78753,#78754,#78755,
#78756,#78757,#78758,#78759,#78760),.UNSPECIFIED.,.F.,.F.,(4,1,1,1,1,1,
1,4),(128.805298797182,129.564589036692,130.562094122916,131.559599209139,
132.557104295363,133.554609381586,134.55211446781,135.088484104361),
 .UNSPECIFIED.);
#1722=B_SPLINE_CURVE_WITH_KNOTS('',3,(#78761,#78762,#78763,#78764,#78765,
#78766,#78767,#78768,#78769,#78770),.UNSPECIFIED.,.F.,.F.,(4,1,1,1,1,1,
1,4),(128.805298797182,129.111485042685,130.108990128909,131.106495215132,
132.104000301356,133.10150538758,134.099010473803,135.088484104361),
 .UNSPECIFIED.);
#1723=B_SPLINE_CURVE_WITH_KNOTS('',3,(#78775,#78776,#78777,#78778,#78779,
#78780,#78781,#78782,#78783,#78784,#78785),.UNSPECIFIED.,.F.,.F.,(4,1,1,
1,1,1,1,1,4),(122.522113490002,122.582053433127,123.57955851935,124.577063605574,
125.574568691798,126.572073778021,127.569578864245,128.567083950468,128.805298797182),
 .UNSPECIFIED.);
#1724=B_SPLINE_CURVE_WITH_KNOTS('',3,(#78786,#78787,#78788,#78789,#78790,
#78791,#78792,#78793,#78794,#78795),.UNSPECIFIED.,.F.,.F.,(4,1,1,1,1,1,
1,4),(122.522113490002,123.126454525344,124.123959611567,125.121464697791,
126.118969784014,127.116474870238,128.113979956462,128.805298797182),
 .UNSPECIFIED.);
#1725=B_SPLINE_CURVE_WITH_KNOTS('',3,(#78800,#78801,#78802,#78803,#78804,
#78805,#78806,#78807,#78808,#78809),.UNSPECIFIED.,.F.,.F.,(4,1,1,1,1,1,
1,4),(116.238928182822,116.597022915785,117.594528002009,118.592033088232,
119.589538174456,120.58704326068,121.584548346903,122.522113490002),
 .UNSPECIFIED.);
#1726=B_SPLINE_CURVE_WITH_KNOTS('',3,(#78810,#78811,#78812,#78813,#78814,
#78815,#78816,#78817,#78818,#78819),.UNSPECIFIED.,.F.,.F.,(4,1,1,1,1,1,
1,4),(116.238928182822,117.141424008002,118.138929094226,119.136434180449,
120.133939266673,121.131444352896,122.12894943912,122.522113490002),
 .UNSPECIFIED.);
#1727=B_SPLINE_CURVE_WITH_KNOTS('',3,(#78824,#78825,#78826,#78827,#78828,
#78829,#78830,#78831,#78832,#78833),.UNSPECIFIED.,.F.,.F.,(4,1,1,1,1,1,
1,4),(109.955742875643,110.611992398444,111.609497484667,112.607002570891,
113.604507657114,114.602012743338,115.599517829562,116.238928182822),
 .UNSPECIFIED.);
#1728=B_SPLINE_CURVE_WITH_KNOTS('',3,(#78834,#78835,#78836,#78837,#78838,
#78839,#78840,#78841,#78842,#78843,#78844),.UNSPECIFIED.,.F.,.F.,(4,1,1,
1,1,1,1,1,4),(109.955742875643,110.158888404437,111.156393490661,112.153898576884,
113.151403663108,114.148908749331,115.146413835555,116.143918921778,116.238928182822),
 .UNSPECIFIED.);
#1729=B_SPLINE_CURVE_WITH_KNOTS('',3,(#78849,#78850,#78851,#78852,#78853,
#78854,#78855,#78856,#78857,#78858),.UNSPECIFIED.,.F.,.F.,(4,1,1,1,1,1,
1,4),(103.672557568463,104.626961881102,105.624466967326,106.621972053549,
107.619477139773,108.616982225996,109.61448731222,109.955742875643),
 .UNSPECIFIED.);
#1730=B_SPLINE_CURVE_WITH_KNOTS('',3,(#78859,#78860,#78861,#78862,#78863,
#78864,#78865,#78866,#78867,#78868),.UNSPECIFIED.,.F.,.F.,(4,1,1,1,1,1,
1,4),(103.672557568463,104.173857887095,105.171362973319,106.168868059543,
107.166373145766,108.16387823199,109.161383318213,109.955742875643),
 .UNSPECIFIED.);
#1731=B_SPLINE_CURVE_WITH_KNOTS('',3,(#78873,#78874,#78875,#78876,#78877,
#78878,#78879,#78880,#78881,#78882,#78883),.UNSPECIFIED.,.F.,.F.,(4,1,1,
1,1,1,1,1,4),(97.3893722612835,97.6444262775369,98.6419313637605,99.6394364499841,
100.636941536208,101.634446622431,102.631951708655,103.629456794878,103.672557568463),
 .UNSPECIFIED.);
#1732=B_SPLINE_CURVE_WITH_KNOTS('',3,(#78884,#78885,#78886,#78887,#78888,
#78889,#78890,#78891,#78892,#78893),.UNSPECIFIED.,.F.,.F.,(4,1,1,1,1,1,
1,4),(97.3893722612836,98.1888273697538,99.1863324559774,100.183837542201,
101.181342628425,102.178847714648,103.176352800872,103.672557568463),
 .UNSPECIFIED.);
#1733=B_SPLINE_CURVE_WITH_KNOTS('',3,(#78898,#78899,#78900,#78901,#78902,
#78903,#78904,#78905,#78906,#78907),.UNSPECIFIED.,.F.,.F.,(4,1,1,1,1,1,
1,4),(91.106186954104,91.6593957601953,92.6569008464189,93.6544059326425,
94.6519110188661,95.6494161050897,96.6469211913133,97.3893722612835),
 .UNSPECIFIED.);
#1734=B_SPLINE_CURVE_WITH_KNOTS('',3,(#78908,#78909,#78910,#78911,#78912,
#78913,#78914,#78915,#78916,#78917,#78918),.UNSPECIFIED.,.F.,.F.,(4,1,1,
1,1,1,1,1,4),(91.106186954104,91.2062917661886,92.2037968524122,93.2013019386358,
94.1988070248594,95.196312111083,96.1938171973066,97.1913222835302,97.3893722612836),
 .UNSPECIFIED.);
#1735=B_SPLINE_CURVE_WITH_KNOTS('',3,(#78923,#78924,#78925,#78926,#78927,
#78928,#78929,#78930,#78931,#78932),.UNSPECIFIED.,.F.,.F.,(4,1,1,1,1,1,
1,4),(84.8230016469244,85.6743652428538,86.6718703290774,87.669375415301,
88.6668805015246,89.6643855877482,90.6618906739717,91.106186954104),
 .UNSPECIFIED.);
#1736=B_SPLINE_CURVE_WITH_KNOTS('',3,(#78933,#78934,#78935,#78936,#78937,
#78938,#78939,#78940,#78941,#78942),.UNSPECIFIED.,.F.,.F.,(4,1,1,1,1,1,
1,4),(84.8230016469244,85.221261248847,86.2187663350706,87.2162714212942,
88.2137765075178,89.2112815937414,90.208786679965,91.106186954104),
 .UNSPECIFIED.);
#1737=B_SPLINE_CURVE_WITH_KNOTS('',3,(#78947,#78948,#78949,#78950,#78951,
#78952,#78953,#78954,#78955,#78956,#78957),.UNSPECIFIED.,.F.,.F.,(4,1,1,
1,1,1,1,1,4),(78.5398163397448,78.6918296392886,79.6893347255122,80.6868398117358,
81.6843448979594,82.681849984183,83.6793550704066,84.6768601566302,84.8230016469244),
 .UNSPECIFIED.);
#1738=B_SPLINE_CURVE_WITH_KNOTS('',3,(#78958,#78959,#78960,#78961,#78962,
#78963,#78964,#78965,#78966,#78967),.UNSPECIFIED.,.F.,.F.,(4,1,1,1,1,1,
1,4),(78.5398163397448,79.2362307315055,80.2337358177291,81.2312409039527,
82.2287459901763,83.2262510763998,84.2237561626234,84.8230016469244),
 .UNSPECIFIED.);
#1739=B_SPLINE_CURVE_WITH_KNOTS('',3,(#78972,#78973,#78974,#78975,#78976,
#78977,#78978,#78979,#78980,#78981),.UNSPECIFIED.,.F.,.F.,(4,1,1,1,1,1,
1,4),(72.2566310325652,72.706799121947,73.7043042081706,74.7018092943942,
75.6993143806178,76.6968194668414,77.694324553065,78.5398163397448),
 .UNSPECIFIED.);
#1740=B_SPLINE_CURVE_WITH_KNOTS('',3,(#78982,#78983,#78984,#78985,#78986,
#78987,#78988,#78989,#78990,#78991),.UNSPECIFIED.,.F.,.F.,(4,1,1,1,1,1,
1,4),(72.2566310325652,73.2512002141639,74.2487053003875,75.2462103866111,
76.2437154728347,77.2412205590583,78.2387256452819,78.5398163397448),
 .UNSPECIFIED.);
#1741=B_SPLINE_CURVE_WITH_KNOTS('',3,(#78996,#78997,#78998,#78999,#79000,
#79001,#79002,#79003,#79004,#79005),.UNSPECIFIED.,.F.,.F.,(4,1,1,1,1,1,
1,4),(65.9734457253856,66.7217686046055,67.7192736908291,68.7167787770527,
69.7142838632763,70.7117889494998,71.7092940357234,72.2566310325652),
 .UNSPECIFIED.);
#1742=B_SPLINE_CURVE_WITH_KNOTS('',3,(#79006,#79007,#79008,#79009,#79010,
#79011,#79012,#79013,#79014,#79015,#79016),.UNSPECIFIED.,.F.,.F.,(4,1,1,
1,1,1,1,1,4),(65.9734457253856,66.2686646105987,67.2661696968223,68.2636747830459,
69.2611798692695,70.2586849554931,71.2561900417167,72.2536951279403,72.2566310325652),
 .UNSPECIFIED.);
#1743=B_SPLINE_CURVE_WITH_KNOTS('',3,(#79021,#79022,#79023,#79024,#79025,
#79026,#79027,#79028,#79029,#79030,#79031),.UNSPECIFIED.,.F.,.F.,(4,1,1,
1,1,1,1,1,4),(59.690260418206,59.7392330010403,60.7367380872639,61.7342431734875,
62.7317482597111,63.7292533459347,64.7267584321583,65.7242635183819,65.9734457253856),
 .UNSPECIFIED.);
#1744=B_SPLINE_CURVE_WITH_KNOTS('',3,(#79032,#79033,#79034,#79035,#79036,
#79037,#79038,#79039,#79040,#79041),.UNSPECIFIED.,.F.,.F.,(4,1,1,1,1,1,
1,4),(59.690260418206,60.2836340932571,61.2811391794807,62.2786442657043,
63.2761493519279,64.2736544381515,65.2711595243751,65.9734457253856),
 .UNSPECIFIED.);
#1745=B_SPLINE_CURVE_WITH_KNOTS('',3,(#79046,#79047,#79048,#79049,#79050,
#79051,#79052,#79053,#79054,#79055),.UNSPECIFIED.,.F.,.F.,(4,1,1,1,1,1,
1,4),(53.4070751110264,53.7542024836987,54.7517075699223,55.7492126561459,
56.7467177423695,57.7442228285931,58.7417279148167,59.690260418206),
 .UNSPECIFIED.);
#1746=B_SPLINE_CURVE_WITH_KNOTS('',3,(#79056,#79057,#79058,#79059,#79060,
#79061,#79062,#79063,#79064,#79065),.UNSPECIFIED.,.F.,.F.,(4,1,1,1,1,1,
1,4),(53.4070751110264,54.2986035759156,55.2961086621392,56.2936137483628,
57.2911188345864,58.28862392081,59.2861290070336,59.690260418206),
 .UNSPECIFIED.);
#1747=B_SPLINE_CURVE_WITH_KNOTS('',3,(#79070,#79071,#79072,#79073,#79074,
#79075,#79076,#79077,#79078,#79079),.UNSPECIFIED.,.F.,.F.,(4,1,1,1,1,1,
1,4),(47.1238898038468,47.7691719663572,48.7666770525807,49.7641821388043,
50.7616872250279,51.7591923112515,52.7566973974751,53.4070751110264),
 .UNSPECIFIED.);
#1748=B_SPLINE_CURVE_WITH_KNOTS('',3,(#79080,#79081,#79082,#79083,#79084,
#79085,#79086,#79087,#79088,#79089,#79090),.UNSPECIFIED.,.F.,.F.,(4,1,1,
1,1,1,1,1,4),(47.1238898038468,47.3160679723504,48.313573058574,49.3110781447976,
50.3085832310212,51.3060883172448,52.3035934034684,53.301098489692,53.4070751110264),
 .UNSPECIFIED.);
#1749=B_SPLINE_CURVE_WITH_KNOTS('',3,(#79095,#79096,#79097,#79098,#79099,
#79100,#79101,#79102,#79103,#79104),.UNSPECIFIED.,.F.,.F.,(4,1,1,1,1,1,
1,4),(40.8407044966672,41.7841414490156,42.7816465352392,43.7791516214628,
44.7766567076864,45.77416179391,46.7716668801336,47.1238898038468),
 .UNSPECIFIED.);
#1750=B_SPLINE_CURVE_WITH_KNOTS('',3,(#79105,#79106,#79107,#79108,#79109,
#79110,#79111,#79112,#79113,#79114),.UNSPECIFIED.,.F.,.F.,(4,1,1,1,1,1,
1,4),(40.8407044966673,41.3310374550088,42.3285425412324,43.326047627456,
44.3235527136796,45.3210577999032,46.3185628861268,47.1238898038468),
 .UNSPECIFIED.);
#1751=B_SPLINE_CURVE_WITH_KNOTS('',3,(#79119,#79120,#79121,#79122,#79123,
#79124,#79125,#79126,#79127,#79128,#79129),.UNSPECIFIED.,.F.,.F.,(4,1,1,
1,1,1,1,1,4),(34.5575191894876,34.8016058454504,35.799110931674,36.7966160178976,
37.7941211041212,38.7916261903448,39.7891312765684,40.786636362792,40.8407044966672),
 .UNSPECIFIED.);
#1752=B_SPLINE_CURVE_WITH_KNOTS('',3,(#79130,#79131,#79132,#79133,#79134,
#79135,#79136,#79137,#79138,#79139),.UNSPECIFIED.,.F.,.F.,(4,1,1,1,1,1,
1,4),(34.5575191894877,35.3460069376673,36.3435120238909,37.3410171101145,
38.3385221963381,39.3360272825617,40.3335323687852,40.8407044966673),
 .UNSPECIFIED.);
#1753=B_SPLINE_CURVE_WITH_KNOTS('',3,(#79144,#79145,#79146,#79147,#79148,
#79149,#79150,#79151,#79152,#79153),.UNSPECIFIED.,.F.,.F.,(4,1,1,1,1,1,
1,4),(28.274333882308,28.8165753281089,29.8140804143324,30.811585500556,
31.8090905867796,32.8065956730032,33.8041007592268,34.5575191894876),
 .UNSPECIFIED.);
#1754=B_SPLINE_CURVE_WITH_KNOTS('',3,(#79154,#79155,#79156,#79157,#79158,
#79159,#79160,#79161,#79162,#79163,#79164),.UNSPECIFIED.,.F.,.F.,(4,1,1,
1,1,1,1,1,4),(28.2743338823081,28.3634713341021,29.3609764203257,30.3584815065493,
31.3559865927729,32.3534916789965,33.3509967652201,34.3485018514437,34.5575191894877),
 .UNSPECIFIED.);
#1755=B_SPLINE_CURVE_WITH_KNOTS('',3,(#79169,#79170,#79171,#79172,#79173,
#79174,#79175,#79176,#79177,#79178),.UNSPECIFIED.,.F.,.F.,(4,1,1,1,1,1,
1,4),(21.9911485751285,22.8315448107673,23.8290498969909,24.8265549832145,
25.8240600694381,26.8215651556617,27.8190702418853,28.274333882308),
 .UNSPECIFIED.);
#1756=B_SPLINE_CURVE_WITH_KNOTS('',3,(#79179,#79180,#79181,#79182,#79183,
#79184,#79185,#79186,#79187,#79188),.UNSPECIFIED.,.F.,.F.,(4,1,1,1,1,1,
1,4),(21.9911485751285,22.3784408167605,23.3759459029841,24.3734509892077,
25.3709560754313,26.3684611616549,27.3659662478785,28.2743338823081),
 .UNSPECIFIED.);
#1757=B_SPLINE_CURVE_WITH_KNOTS('',3,(#79194,#79195,#79196,#79197,#79198),
 .UNSPECIFIED.,.F.,.F.,(4,1,4),(14.3984001269718,15.3959052131954,15.7079632679489),
 .UNSPECIFIED.);
#1758=B_SPLINE_CURVE_WITH_KNOTS('',3,(#79201,#79202,#79203,#79204,#79205),
 .UNSPECIFIED.,.F.,.F.,(4,1,4),(13.8759337553362,14.8515041209785,15.7079632679489),
 .UNSPECIFIED.);
#1759=B_SPLINE_CURVE_WITH_KNOTS('',3,(#79211,#79212,#79213,#79214,#79215,
#79216,#79217,#79218),.UNSPECIFIED.,.F.,.F.,(4,1,1,1,1,4),(135.088484104361,
135.549619554034,136.547124640257,137.544629726481,138.542134812704,139.539639898928),
 .UNSPECIFIED.);
#1760=B_SPLINE_CURVE_WITH_KNOTS('',3,(#79221,#79222,#79223,#79224,#79225,
#79226,#79227,#79228,#79229),.UNSPECIFIED.,.F.,.F.,(4,1,1,1,1,1,4),(135.088484104361,
135.096515560027,136.09402064625,137.091525732474,138.089030818697,139.086535904921,
140.062106270563),.UNSPECIFIED.);
#1761=B_SPLINE_CURVE_WITH_KNOTS('',3,(#79234,#79235,#79236,#79237,#79238,
#79239,#79240,#79241,#79242,#79243),.UNSPECIFIED.,.F.,.F.,(4,1,1,1,1,1,
1,4),(128.805298797182,129.564589036692,130.562094122916,131.559599209139,
132.557104295363,133.554609381586,134.55211446781,135.088484104361),
 .UNSPECIFIED.);
#1762=B_SPLINE_CURVE_WITH_KNOTS('',3,(#79244,#79245,#79246,#79247,#79248,
#79249,#79250,#79251,#79252,#79253),.UNSPECIFIED.,.F.,.F.,(4,1,1,1,1,1,
1,4),(128.805298797182,129.111485042685,130.108990128909,131.106495215132,
132.104000301356,133.10150538758,134.099010473803,135.088484104361),
 .UNSPECIFIED.);
#1763=B_SPLINE_CURVE_WITH_KNOTS('',3,(#79258,#79259,#79260,#79261,#79262,
#79263,#79264,#79265,#79266,#79267,#79268),.UNSPECIFIED.,.F.,.F.,(4,1,1,
1,1,1,1,1,4),(122.522113490002,122.582053433127,123.57955851935,124.577063605574,
125.574568691798,126.572073778021,127.569578864245,128.567083950468,128.805298797182),
 .UNSPECIFIED.);
#1764=B_SPLINE_CURVE_WITH_KNOTS('',3,(#79269,#79270,#79271,#79272,#79273,
#79274,#79275,#79276,#79277,#79278),.UNSPECIFIED.,.F.,.F.,(4,1,1,1,1,1,
1,4),(122.522113490002,123.126454525344,124.123959611567,125.121464697791,
126.118969784014,127.116474870238,128.113979956462,128.805298797182),
 .UNSPECIFIED.);
#1765=B_SPLINE_CURVE_WITH_KNOTS('',3,(#79283,#79284,#79285,#79286,#79287,
#79288,#79289,#79290,#79291,#79292),.UNSPECIFIED.,.F.,.F.,(4,1,1,1,1,1,
1,4),(116.238928182822,116.597022915785,117.594528002009,118.592033088232,
119.589538174456,120.58704326068,121.584548346903,122.522113490002),
 .UNSPECIFIED.);
#1766=B_SPLINE_CURVE_WITH_KNOTS('',3,(#79293,#79294,#79295,#79296,#79297,
#79298,#79299,#79300,#79301,#79302),.UNSPECIFIED.,.F.,.F.,(4,1,1,1,1,1,
1,4),(116.238928182822,117.141424008002,118.138929094226,119.136434180449,
120.133939266673,121.131444352896,122.12894943912,122.522113490002),
 .UNSPECIFIED.);
#1767=B_SPLINE_CURVE_WITH_KNOTS('',3,(#79307,#79308,#79309,#79310,#79311,
#79312,#79313,#79314,#79315,#79316),.UNSPECIFIED.,.F.,.F.,(4,1,1,1,1,1,
1,4),(109.955742875643,110.611992398444,111.609497484667,112.607002570891,
113.604507657114,114.602012743338,115.599517829562,116.238928182822),
 .UNSPECIFIED.);
#1768=B_SPLINE_CURVE_WITH_KNOTS('',3,(#79317,#79318,#79319,#79320,#79321,
#79322,#79323,#79324,#79325,#79326,#79327),.UNSPECIFIED.,.F.,.F.,(4,1,1,
1,1,1,1,1,4),(109.955742875643,110.158888404437,111.15639349066,112.153898576884,
113.151403663108,114.148908749331,115.146413835555,116.143918921778,116.238928182822),
 .UNSPECIFIED.);
#1769=B_SPLINE_CURVE_WITH_KNOTS('',3,(#79332,#79333,#79334,#79335,#79336,
#79337,#79338,#79339,#79340,#79341),.UNSPECIFIED.,.F.,.F.,(4,1,1,1,1,1,
1,4),(103.672557568463,104.626961881102,105.624466967326,106.621972053549,
107.619477139773,108.616982225996,109.61448731222,109.955742875643),
 .UNSPECIFIED.);
#1770=B_SPLINE_CURVE_WITH_KNOTS('',3,(#79342,#79343,#79344,#79345,#79346,
#79347,#79348,#79349,#79350,#79351),.UNSPECIFIED.,.F.,.F.,(4,1,1,1,1,1,
1,4),(103.672557568463,104.173857887095,105.171362973319,106.168868059542,
107.166373145766,108.16387823199,109.161383318213,109.955742875643),
 .UNSPECIFIED.);
#1771=B_SPLINE_CURVE_WITH_KNOTS('',3,(#79356,#79357,#79358,#79359,#79360,
#79361,#79362,#79363,#79364,#79365,#79366),.UNSPECIFIED.,.F.,.F.,(4,1,1,
1,1,1,1,1,4),(97.3893722612835,97.6444262775369,98.6419313637605,99.6394364499841,
100.636941536208,101.634446622431,102.631951708655,103.629456794878,103.672557568463),
 .UNSPECIFIED.);
#1772=B_SPLINE_CURVE_WITH_KNOTS('',3,(#79367,#79368,#79369,#79370,#79371,
#79372,#79373,#79374,#79375,#79376),.UNSPECIFIED.,.F.,.F.,(4,1,1,1,1,1,
1,4),(97.3893722612836,98.1888273697537,99.1863324559773,100.183837542201,
101.181342628424,102.178847714648,103.176352800872,103.672557568463),
 .UNSPECIFIED.);
#1773=B_SPLINE_CURVE_WITH_KNOTS('',3,(#79381,#79382,#79383,#79384,#79385,
#79386,#79387,#79388,#79389,#79390),.UNSPECIFIED.,.F.,.F.,(4,1,1,1,1,1,
1,4),(91.106186954104,91.6593957601953,92.6569008464189,93.6544059326425,
94.6519110188661,95.6494161050897,96.6469211913133,97.3893722612835),
 .UNSPECIFIED.);
#1774=B_SPLINE_CURVE_WITH_KNOTS('',3,(#79391,#79392,#79393,#79394,#79395,
#79396,#79397,#79398,#79399,#79400,#79401),.UNSPECIFIED.,.F.,.F.,(4,1,1,
1,1,1,1,1,4),(91.106186954104,91.2062917661885,92.2037968524121,93.2013019386357,
94.1988070248593,95.1963121110829,96.1938171973065,97.1913222835301,97.3893722612836),
 .UNSPECIFIED.);
#1775=B_SPLINE_CURVE_WITH_KNOTS('',3,(#79406,#79407,#79408,#79409,#79410,
#79411,#79412,#79413,#79414,#79415),.UNSPECIFIED.,.F.,.F.,(4,1,1,1,1,1,
1,4),(84.8230016469244,85.6743652428537,86.6718703290773,87.6693754153009,
88.6668805015245,89.6643855877481,90.6618906739717,91.106186954104),
 .UNSPECIFIED.);
#1776=B_SPLINE_CURVE_WITH_KNOTS('',3,(#79416,#79417,#79418,#79419,#79420,
#79421,#79422,#79423,#79424,#79425),.UNSPECIFIED.,.F.,.F.,(4,1,1,1,1,1,
1,4),(84.8230016469244,85.221261248847,86.2187663350706,87.2162714212942,
88.2137765075177,89.2112815937413,90.2087866799649,91.106186954104),
 .UNSPECIFIED.);
#1777=B_SPLINE_CURVE_WITH_KNOTS('',3,(#79430,#79431,#79432,#79433,#79434,
#79435,#79436,#79437,#79438,#79439,#79440),.UNSPECIFIED.,.F.,.F.,(4,1,1,
1,1,1,1,1,4),(78.5398163397448,78.6918296392886,79.6893347255122,80.6868398117358,
81.6843448979593,82.6818499841829,83.6793550704065,84.6768601566301,84.8230016469244),
 .UNSPECIFIED.);
#1778=B_SPLINE_CURVE_WITH_KNOTS('',3,(#79441,#79442,#79443,#79444,#79445,
#79446,#79447,#79448,#79449,#79450),.UNSPECIFIED.,.F.,.F.,(4,1,1,1,1,1,
1,4),(78.5398163397448,79.2362307315054,80.233735817729,81.2312409039526,
82.2287459901762,83.2262510763998,84.2237561626234,84.8230016469244),
 .UNSPECIFIED.);
#1779=B_SPLINE_CURVE_WITH_KNOTS('',3,(#79455,#79456,#79457,#79458,#79459,
#79460,#79461,#79462,#79463,#79464),.UNSPECIFIED.,.F.,.F.,(4,1,1,1,1,1,
1,4),(72.2566310325652,72.706799121947,73.7043042081706,74.7018092943942,
75.6993143806178,76.6968194668414,77.694324553065,78.5398163397448),
 .UNSPECIFIED.);
#1780=B_SPLINE_CURVE_WITH_KNOTS('',3,(#79465,#79466,#79467,#79468,#79469,
#79470,#79471,#79472,#79473,#79474),.UNSPECIFIED.,.F.,.F.,(4,1,1,1,1,1,
1,4),(72.2566310325652,73.2512002141638,74.2487053003874,75.246210386611,
76.2437154728346,77.2412205590582,78.2387256452818,78.5398163397448),
 .UNSPECIFIED.);
#1781=B_SPLINE_CURVE_WITH_KNOTS('',3,(#79479,#79480,#79481,#79482,#79483,
#79484,#79485,#79486,#79487,#79488),.UNSPECIFIED.,.F.,.F.,(4,1,1,1,1,1,
1,4),(65.9734457253856,66.7217686046054,67.719273690829,68.7167787770526,
69.7142838632762,70.7117889494998,71.7092940357234,72.2566310325652),
 .UNSPECIFIED.);
#1782=B_SPLINE_CURVE_WITH_KNOTS('',3,(#79489,#79490,#79491,#79492,#79493,
#79494,#79495,#79496,#79497,#79498,#79499),.UNSPECIFIED.,.F.,.F.,(4,1,1,
1,1,1,1,1,4),(65.9734457253856,66.2686646105986,67.2661696968223,68.2636747830458,
69.2611798692694,70.258684955493,71.2561900417166,72.2536951279402,72.2566310325652),
 .UNSPECIFIED.);
#1783=B_SPLINE_CURVE_WITH_KNOTS('',3,(#79504,#79505,#79506,#79507,#79508,
#79509,#79510,#79511,#79512,#79513,#79514),.UNSPECIFIED.,.F.,.F.,(4,1,1,
1,1,1,1,1,4),(59.690260418206,59.7392330010403,60.7367380872638,61.7342431734874,
62.731748259711,63.7292533459346,64.7267584321582,65.7242635183818,65.9734457253856),
 .UNSPECIFIED.);
#1784=B_SPLINE_CURVE_WITH_KNOTS('',3,(#79515,#79516,#79517,#79518,#79519,
#79520,#79521,#79522,#79523,#79524),.UNSPECIFIED.,.F.,.F.,(4,1,1,1,1,1,
1,4),(59.690260418206,60.2836340932571,61.2811391794807,62.2786442657043,
63.2761493519279,64.2736544381515,65.2711595243751,65.9734457253856),
 .UNSPECIFIED.);
#1785=B_SPLINE_CURVE_WITH_KNOTS('',3,(#79529,#79530,#79531,#79532,#79533,
#79534,#79535,#79536,#79537,#79538),.UNSPECIFIED.,.F.,.F.,(4,1,1,1,1,1,
1,4),(53.4070751110264,53.7542024836987,54.7517075699223,55.7492126561459,
56.7467177423695,57.7442228285931,58.7417279148167,59.690260418206),
 .UNSPECIFIED.);
#1786=B_SPLINE_CURVE_WITH_KNOTS('',3,(#79539,#79540,#79541,#79542,#79543,
#79544,#79545,#79546,#79547,#79548),.UNSPECIFIED.,.F.,.F.,(4,1,1,1,1,1,
1,4),(53.4070751110264,54.2986035759155,55.2961086621391,56.2936137483627,
57.2911188345863,58.2886239208099,59.2861290070335,59.690260418206),
 .UNSPECIFIED.);
#1787=B_SPLINE_CURVE_WITH_KNOTS('',3,(#79553,#79554,#79555,#79556,#79557,
#79558,#79559,#79560,#79561,#79562),.UNSPECIFIED.,.F.,.F.,(4,1,1,1,1,1,
1,4),(47.1238898038468,47.7691719663571,48.7666770525807,49.7641821388043,
50.7616872250279,51.7591923112515,52.7566973974751,53.4070751110264),
 .UNSPECIFIED.);
#1788=B_SPLINE_CURVE_WITH_KNOTS('',3,(#79563,#79564,#79565,#79566,#79567,
#79568,#79569,#79570,#79571,#79572,#79573),.UNSPECIFIED.,.F.,.F.,(4,1,1,
1,1,1,1,1,4),(47.1238898038468,47.3160679723504,48.3135730585739,49.3110781447975,
50.3085832310211,51.3060883172447,52.3035934034683,53.3010984896919,53.4070751110264),
 .UNSPECIFIED.);
#1789=B_SPLINE_CURVE_WITH_KNOTS('',3,(#79578,#79579,#79580,#79581,#79582,
#79583,#79584,#79585,#79586,#79587),.UNSPECIFIED.,.F.,.F.,(4,1,1,1,1,1,
1,4),(40.8407044966672,41.7841414490155,42.7816465352391,43.7791516214627,
44.7766567076863,45.7741617939099,46.7716668801335,47.1238898038468),
 .UNSPECIFIED.);
#1790=B_SPLINE_CURVE_WITH_KNOTS('',3,(#79588,#79589,#79590,#79591,#79592,
#79593,#79594,#79595,#79596,#79597),.UNSPECIFIED.,.F.,.F.,(4,1,1,1,1,1,
1,4),(40.8407044966673,41.3310374550088,42.3285425412324,43.326047627456,
44.3235527136796,45.3210577999032,46.3185628861268,47.1238898038468),
 .UNSPECIFIED.);
#1791=B_SPLINE_CURVE_WITH_KNOTS('',3,(#79602,#79603,#79604,#79605,#79606,
#79607,#79608,#79609,#79610,#79611,#79612),.UNSPECIFIED.,.F.,.F.,(4,1,1,
1,1,1,1,1,4),(34.5575191894876,34.8016058454504,35.799110931674,36.7966160178976,
37.7941211041212,38.7916261903448,39.7891312765683,40.7866363627919,40.8407044966672),
 .UNSPECIFIED.);
#1792=B_SPLINE_CURVE_WITH_KNOTS('',3,(#79613,#79614,#79615,#79616,#79617,
#79618,#79619,#79620,#79621,#79622),.UNSPECIFIED.,.F.,.F.,(4,1,1,1,1,1,
1,4),(34.5575191894877,35.3460069376672,36.3435120238908,37.3410171101144,
38.338522196338,39.3360272825616,40.3335323687852,40.8407044966673),
 .UNSPECIFIED.);
#1793=B_SPLINE_CURVE_WITH_KNOTS('',3,(#79627,#79628,#79629,#79630,#79631,
#79632,#79633,#79634,#79635,#79636),.UNSPECIFIED.,.F.,.F.,(4,1,1,1,1,1,
1,4),(28.2743338823081,28.8165753281088,29.8140804143324,30.811585500556,
31.8090905867796,32.8065956730032,33.8041007592268,34.5575191894876),
 .UNSPECIFIED.);
#1794=B_SPLINE_CURVE_WITH_KNOTS('',3,(#79637,#79638,#79639,#79640,#79641,
#79642,#79643,#79644,#79645,#79646,#79647),.UNSPECIFIED.,.F.,.F.,(4,1,1,
1,1,1,1,1,4),(28.2743338823081,28.363471334102,29.3609764203256,30.3584815065492,
31.3559865927728,32.3534916789964,33.35099676522,34.3485018514436,34.5575191894877),
 .UNSPECIFIED.);
#1795=B_SPLINE_CURVE_WITH_KNOTS('',3,(#79652,#79653,#79654,#79655,#79656,
#79657,#79658,#79659,#79660,#79661),.UNSPECIFIED.,.F.,.F.,(4,1,1,1,1,1,
1,4),(21.9911485751285,22.8315448107672,23.8290498969908,24.8265549832144,
25.824060069438,26.8215651556616,27.8190702418852,28.2743338823081),
 .UNSPECIFIED.);
#1796=B_SPLINE_CURVE_WITH_KNOTS('',3,(#79662,#79663,#79664,#79665,#79666,
#79667,#79668,#79669,#79670,#79671),.UNSPECIFIED.,.F.,.F.,(4,1,1,1,1,1,
1,4),(21.9911485751285,22.3784408167605,23.3759459029841,24.3734509892077,
25.3709560754313,26.3684611616549,27.3659662478785,28.2743338823081),
 .UNSPECIFIED.);
#1797=B_SPLINE_CURVE_WITH_KNOTS('',3,(#79677,#79678,#79679,#79680,#79681),
 .UNSPECIFIED.,.F.,.F.,(4,1,4),(14.3984001269717,15.3959052131953,15.7079632679489),
 .UNSPECIFIED.);
#1798=B_SPLINE_CURVE_WITH_KNOTS('',3,(#79684,#79685,#79686,#79687,#79688),
 .UNSPECIFIED.,.F.,.F.,(4,1,4),(13.8759337553361,14.8515041209785,15.7079632679489),
 .UNSPECIFIED.);
#1799=B_SPLINE_CURVE_WITH_KNOTS('',3,(#79694,#79695,#79696,#79697,#79698,
#79699,#79700,#79701),.UNSPECIFIED.,.F.,.F.,(4,1,1,1,1,4),(135.088484104361,
135.549619554034,136.547124640257,137.544629726481,138.542134812704,139.539639898928),
 .UNSPECIFIED.);
#1800=B_SPLINE_CURVE_WITH_KNOTS('',3,(#79704,#79705,#79706,#79707,#79708,
#79709,#79710,#79711,#79712),.UNSPECIFIED.,.F.,.F.,(4,1,1,1,1,1,4),(135.088484104361,
135.096515560027,136.09402064625,137.091525732474,138.089030818698,139.086535904921,
140.062106270563),.UNSPECIFIED.);
#1801=B_SPLINE_CURVE_WITH_KNOTS('',3,(#79717,#79718,#79719,#79720,#79721,
#79722,#79723,#79724,#79725,#79726),.UNSPECIFIED.,.F.,.F.,(4,1,1,1,1,1,
1,4),(128.805298797182,129.564589036692,130.562094122916,131.559599209139,
132.557104295363,133.554609381586,134.55211446781,135.088484104361),
 .UNSPECIFIED.);
#1802=B_SPLINE_CURVE_WITH_KNOTS('',3,(#79727,#79728,#79729,#79730,#79731,
#79732,#79733,#79734,#79735,#79736),.UNSPECIFIED.,.F.,.F.,(4,1,1,1,1,1,
1,4),(128.805298797182,129.111485042685,130.108990128909,131.106495215132,
132.104000301356,133.10150538758,134.099010473803,135.088484104361),
 .UNSPECIFIED.);
#1803=B_SPLINE_CURVE_WITH_KNOTS('',3,(#79741,#79742,#79743,#79744,#79745,
#79746,#79747,#79748,#79749,#79750,#79751),.UNSPECIFIED.,.F.,.F.,(4,1,1,
1,1,1,1,1,4),(122.522113490002,122.582053433127,123.57955851935,124.577063605574,
125.574568691798,126.572073778021,127.569578864245,128.567083950468,128.805298797182),
 .UNSPECIFIED.);
#1804=B_SPLINE_CURVE_WITH_KNOTS('',3,(#79752,#79753,#79754,#79755,#79756,
#79757,#79758,#79759,#79760,#79761),.UNSPECIFIED.,.F.,.F.,(4,1,1,1,1,1,
1,4),(122.522113490002,123.126454525344,124.123959611567,125.121464697791,
126.118969784014,127.116474870238,128.113979956462,128.805298797182),
 .UNSPECIFIED.);
#1805=B_SPLINE_CURVE_WITH_KNOTS('',3,(#79766,#79767,#79768,#79769,#79770,
#79771,#79772,#79773,#79774,#79775),.UNSPECIFIED.,.F.,.F.,(4,1,1,1,1,1,
1,4),(116.238928182822,116.597022915785,117.594528002009,118.592033088232,
119.589538174456,120.58704326068,121.584548346903,122.522113490002),
 .UNSPECIFIED.);
#1806=B_SPLINE_CURVE_WITH_KNOTS('',3,(#79776,#79777,#79778,#79779,#79780,
#79781,#79782,#79783,#79784,#79785),.UNSPECIFIED.,.F.,.F.,(4,1,1,1,1,1,
1,4),(116.238928182822,117.141424008002,118.138929094226,119.136434180449,
120.133939266673,121.131444352896,122.12894943912,122.522113490002),
 .UNSPECIFIED.);
#1807=B_SPLINE_CURVE_WITH_KNOTS('',3,(#79790,#79791,#79792,#79793,#79794,
#79795,#79796,#79797,#79798,#79799),.UNSPECIFIED.,.F.,.F.,(4,1,1,1,1,1,
1,4),(109.955742875643,110.611992398444,111.609497484667,112.607002570891,
113.604507657114,114.602012743338,115.599517829562,116.238928182822),
 .UNSPECIFIED.);
#1808=B_SPLINE_CURVE_WITH_KNOTS('',3,(#79800,#79801,#79802,#79803,#79804,
#79805,#79806,#79807,#79808,#79809,#79810),.UNSPECIFIED.,.F.,.F.,(4,1,1,
1,1,1,1,1,4),(109.955742875643,110.158888404437,111.15639349066,112.153898576884,
113.151403663108,114.148908749331,115.146413835555,116.143918921778,116.238928182822),
 .UNSPECIFIED.);
#1809=B_SPLINE_CURVE_WITH_KNOTS('',3,(#79815,#79816,#79817,#79818,#79819,
#79820,#79821,#79822,#79823,#79824),.UNSPECIFIED.,.F.,.F.,(4,1,1,1,1,1,
1,4),(103.672557568463,104.626961881102,105.624466967326,106.621972053549,
107.619477139773,108.616982225996,109.61448731222,109.955742875643),
 .UNSPECIFIED.);
#1810=B_SPLINE_CURVE_WITH_KNOTS('',3,(#79825,#79826,#79827,#79828,#79829,
#79830,#79831,#79832,#79833,#79834),.UNSPECIFIED.,.F.,.F.,(4,1,1,1,1,1,
1,4),(103.672557568463,104.173857887095,105.171362973319,106.168868059543,
107.166373145766,108.16387823199,109.161383318213,109.955742875643),
 .UNSPECIFIED.);
#1811=B_SPLINE_CURVE_WITH_KNOTS('',3,(#79839,#79840,#79841,#79842,#79843,
#79844,#79845,#79846,#79847,#79848,#79849),.UNSPECIFIED.,.F.,.F.,(4,1,1,
1,1,1,1,1,4),(97.3893722612836,97.6444262775369,98.6419313637605,99.6394364499841,
100.636941536208,101.634446622431,102.631951708655,103.629456794878,103.672557568463),
 .UNSPECIFIED.);
#1812=B_SPLINE_CURVE_WITH_KNOTS('',3,(#79850,#79851,#79852,#79853,#79854,
#79855,#79856,#79857,#79858,#79859),.UNSPECIFIED.,.F.,.F.,(4,1,1,1,1,1,
1,4),(97.3893722612836,98.1888273697538,99.1863324559774,100.183837542201,
101.181342628425,102.178847714648,103.176352800872,103.672557568463),
 .UNSPECIFIED.);
#1813=B_SPLINE_CURVE_WITH_KNOTS('',3,(#79864,#79865,#79866,#79867,#79868,
#79869,#79870,#79871,#79872,#79873),.UNSPECIFIED.,.F.,.F.,(4,1,1,1,1,1,
1,4),(91.106186954104,91.6593957601953,92.6569008464189,93.6544059326425,
94.6519110188661,95.6494161050897,96.6469211913133,97.3893722612836),
 .UNSPECIFIED.);
#1814=B_SPLINE_CURVE_WITH_KNOTS('',3,(#79874,#79875,#79876,#79877,#79878,
#79879,#79880,#79881,#79882,#79883,#79884),.UNSPECIFIED.,.F.,.F.,(4,1,1,
1,1,1,1,1,4),(91.106186954104,91.2062917661886,92.2037968524122,93.2013019386358,
94.1988070248594,95.196312111083,96.1938171973066,97.1913222835302,97.3893722612836),
 .UNSPECIFIED.);
#1815=B_SPLINE_CURVE_WITH_KNOTS('',3,(#79889,#79890,#79891,#79892,#79893,
#79894,#79895,#79896,#79897,#79898),.UNSPECIFIED.,.F.,.F.,(4,1,1,1,1,1,
1,4),(84.8230016469244,85.6743652428538,86.6718703290774,87.669375415301,
88.6668805015246,89.6643855877482,90.6618906739717,91.106186954104),
 .UNSPECIFIED.);
#1816=B_SPLINE_CURVE_WITH_KNOTS('',3,(#79899,#79900,#79901,#79902,#79903,
#79904,#79905,#79906,#79907,#79908),.UNSPECIFIED.,.F.,.F.,(4,1,1,1,1,1,
1,4),(84.8230016469244,85.221261248847,86.2187663350706,87.2162714212942,
88.2137765075178,89.2112815937414,90.208786679965,91.106186954104),
 .UNSPECIFIED.);
#1817=B_SPLINE_CURVE_WITH_KNOTS('',3,(#79913,#79914,#79915,#79916,#79917,
#79918,#79919,#79920,#79921,#79922,#79923),.UNSPECIFIED.,.F.,.F.,(4,1,1,
1,1,1,1,1,4),(78.5398163397448,78.6918296392886,79.6893347255122,80.6868398117358,
81.6843448979594,82.681849984183,83.6793550704066,84.6768601566302,84.8230016469244),
 .UNSPECIFIED.);
#1818=B_SPLINE_CURVE_WITH_KNOTS('',3,(#79924,#79925,#79926,#79927,#79928,
#79929,#79930,#79931,#79932,#79933),.UNSPECIFIED.,.F.,.F.,(4,1,1,1,1,1,
1,4),(78.5398163397448,79.2362307315055,80.233735817729,81.2312409039526,
82.2287459901762,83.2262510763998,84.2237561626234,84.8230016469244),
 .UNSPECIFIED.);
#1819=B_SPLINE_CURVE_WITH_KNOTS('',3,(#79938,#79939,#79940,#79941,#79942,
#79943,#79944,#79945,#79946,#79947),.UNSPECIFIED.,.F.,.F.,(4,1,1,1,1,1,
1,4),(72.2566310325652,72.706799121947,73.7043042081706,74.7018092943942,
75.6993143806178,76.6968194668414,77.694324553065,78.5398163397448),
 .UNSPECIFIED.);
#1820=B_SPLINE_CURVE_WITH_KNOTS('',3,(#79948,#79949,#79950,#79951,#79952,
#79953,#79954,#79955,#79956,#79957),.UNSPECIFIED.,.F.,.F.,(4,1,1,1,1,1,
1,4),(72.2566310325652,73.2512002141639,74.2487053003875,75.2462103866111,
76.2437154728347,77.2412205590583,78.2387256452818,78.5398163397448),
 .UNSPECIFIED.);
#1821=B_SPLINE_CURVE_WITH_KNOTS('',3,(#79962,#79963,#79964,#79965,#79966,
#79967,#79968,#79969,#79970,#79971),.UNSPECIFIED.,.F.,.F.,(4,1,1,1,1,1,
1,4),(65.9734457253856,66.7217686046055,67.7192736908291,68.7167787770527,
69.7142838632763,70.7117889494998,71.7092940357234,72.2566310325652),
 .UNSPECIFIED.);
#1822=B_SPLINE_CURVE_WITH_KNOTS('',3,(#79972,#79973,#79974,#79975,#79976,
#79977,#79978,#79979,#79980,#79981,#79982),.UNSPECIFIED.,.F.,.F.,(4,1,1,
1,1,1,1,1,4),(65.9734457253856,66.2686646105987,67.2661696968223,68.2636747830459,
69.2611798692695,70.2586849554931,71.2561900417167,72.2536951279403,72.2566310325652),
 .UNSPECIFIED.);
#1823=B_SPLINE_CURVE_WITH_KNOTS('',3,(#79987,#79988,#79989,#79990,#79991,
#79992,#79993,#79994,#79995,#79996,#79997),.UNSPECIFIED.,.F.,.F.,(4,1,1,
1,1,1,1,1,4),(59.690260418206,59.7392330010403,60.7367380872639,61.7342431734875,
62.7317482597111,63.7292533459347,64.7267584321583,65.7242635183819,65.9734457253856),
 .UNSPECIFIED.);
#1824=B_SPLINE_CURVE_WITH_KNOTS('',3,(#79998,#79999,#80000,#80001,#80002,
#80003,#80004,#80005,#80006,#80007),.UNSPECIFIED.,.F.,.F.,(4,1,1,1,1,1,
1,4),(59.690260418206,60.2836340932571,61.2811391794807,62.2786442657043,
63.2761493519279,64.2736544381515,65.2711595243751,65.9734457253856),
 .UNSPECIFIED.);
#1825=B_SPLINE_CURVE_WITH_KNOTS('',3,(#80012,#80013,#80014,#80015,#80016,
#80017,#80018,#80019,#80020,#80021),.UNSPECIFIED.,.F.,.F.,(4,1,1,1,1,1,
1,4),(53.4070751110264,53.7542024836987,54.7517075699223,55.7492126561459,
56.7467177423695,57.7442228285931,58.7417279148167,59.690260418206),
 .UNSPECIFIED.);
#1826=B_SPLINE_CURVE_WITH_KNOTS('',3,(#80022,#80023,#80024,#80025,#80026,
#80027,#80028,#80029,#80030,#80031),.UNSPECIFIED.,.F.,.F.,(4,1,1,1,1,1,
1,4),(53.4070751110264,54.2986035759156,55.2961086621392,56.2936137483628,
57.2911188345864,58.28862392081,59.2861290070336,59.690260418206),
 .UNSPECIFIED.);
#1827=B_SPLINE_CURVE_WITH_KNOTS('',3,(#80036,#80037,#80038,#80039,#80040,
#80041,#80042,#80043,#80044,#80045),.UNSPECIFIED.,.F.,.F.,(4,1,1,1,1,1,
1,4),(47.1238898038468,47.7691719663572,48.7666770525807,49.7641821388043,
50.7616872250279,51.7591923112515,52.7566973974751,53.4070751110264),
 .UNSPECIFIED.);
#1828=B_SPLINE_CURVE_WITH_KNOTS('',3,(#80046,#80047,#80048,#80049,#80050,
#80051,#80052,#80053,#80054,#80055,#80056),.UNSPECIFIED.,.F.,.F.,(4,1,1,
1,1,1,1,1,4),(47.1238898038468,47.3160679723504,48.313573058574,49.3110781447976,
50.3085832310212,51.3060883172448,52.3035934034684,53.301098489692,53.4070751110264),
 .UNSPECIFIED.);
#1829=B_SPLINE_CURVE_WITH_KNOTS('',3,(#80061,#80062,#80063,#80064,#80065,
#80066,#80067,#80068,#80069,#80070),.UNSPECIFIED.,.F.,.F.,(4,1,1,1,1,1,
1,4),(40.8407044966673,41.7841414490156,42.7816465352392,43.7791516214628,
44.7766567076864,45.77416179391,46.7716668801336,47.1238898038468),
 .UNSPECIFIED.);
#1830=B_SPLINE_CURVE_WITH_KNOTS('',3,(#80071,#80072,#80073,#80074,#80075,
#80076,#80077,#80078,#80079,#80080),.UNSPECIFIED.,.F.,.F.,(4,1,1,1,1,1,
1,4),(40.8407044966673,41.3310374550088,42.3285425412324,43.326047627456,
44.3235527136796,45.3210577999032,46.3185628861268,47.1238898038468),
 .UNSPECIFIED.);
#1831=B_SPLINE_CURVE_WITH_KNOTS('',3,(#80085,#80086,#80087,#80088,#80089,
#80090,#80091,#80092,#80093,#80094,#80095),.UNSPECIFIED.,.F.,.F.,(4,1,1,
1,1,1,1,1,4),(34.5575191894877,34.8016058454504,35.799110931674,36.7966160178976,
37.7941211041212,38.7916261903448,39.7891312765684,40.786636362792,40.8407044966673),
 .UNSPECIFIED.);
#1832=B_SPLINE_CURVE_WITH_KNOTS('',3,(#80096,#80097,#80098,#80099,#80100,
#80101,#80102,#80103,#80104,#80105),.UNSPECIFIED.,.F.,.F.,(4,1,1,1,1,1,
1,4),(34.5575191894877,35.3460069376673,36.3435120238909,37.3410171101145,
38.3385221963381,39.3360272825616,40.3335323687852,40.8407044966673),
 .UNSPECIFIED.);
#1833=B_SPLINE_CURVE_WITH_KNOTS('',3,(#80110,#80111,#80112,#80113,#80114,
#80115,#80116,#80117,#80118,#80119),.UNSPECIFIED.,.F.,.F.,(4,1,1,1,1,1,
1,4),(28.2743338823081,28.8165753281089,29.8140804143324,30.811585500556,
31.8090905867796,32.8065956730032,33.8041007592268,34.5575191894877),
 .UNSPECIFIED.);
#1834=B_SPLINE_CURVE_WITH_KNOTS('',3,(#80120,#80121,#80122,#80123,#80124,
#80125,#80126,#80127,#80128,#80129,#80130),.UNSPECIFIED.,.F.,.F.,(4,1,1,
1,1,1,1,1,4),(28.2743338823081,28.3634713341021,29.3609764203257,30.3584815065493,
31.3559865927729,32.3534916789965,33.3509967652201,34.3485018514437,34.5575191894877),
 .UNSPECIFIED.);
#1835=B_SPLINE_CURVE_WITH_KNOTS('',3,(#80135,#80136,#80137,#80138,#80139,
#80140,#80141,#80142,#80143,#80144),.UNSPECIFIED.,.F.,.F.,(4,1,1,1,1,1,
1,4),(21.9911485751285,22.8315448107673,23.8290498969909,24.8265549832145,
25.8240600694381,26.8215651556617,27.8190702418853,28.2743338823081),
 .UNSPECIFIED.);
#1836=B_SPLINE_CURVE_WITH_KNOTS('',3,(#80145,#80146,#80147,#80148,#80149,
#80150,#80151,#80152,#80153,#80154),.UNSPECIFIED.,.F.,.F.,(4,1,1,1,1,1,
1,4),(21.9911485751285,22.3784408167605,23.3759459029841,24.3734509892077,
25.3709560754313,26.3684611616549,27.3659662478785,28.2743338823081),
 .UNSPECIFIED.);
#1837=B_SPLINE_CURVE_WITH_KNOTS('',3,(#80160,#80161,#80162,#80163,#80164),
 .UNSPECIFIED.,.F.,.F.,(4,1,4),(14.3984001269718,15.3959052131954,15.7079632679489),
 .UNSPECIFIED.);
#1838=B_SPLINE_CURVE_WITH_KNOTS('',3,(#80167,#80168,#80169,#80170,#80171),
 .UNSPECIFIED.,.F.,.F.,(4,1,4),(13.8759337553362,14.8515041209785,15.7079632679489),
 .UNSPECIFIED.);
#1839=B_SPLINE_CURVE_WITH_KNOTS('',3,(#80177,#80178,#80179,#80180,#80181,
#80182,#80183,#80184),.UNSPECIFIED.,.F.,.F.,(4,1,1,1,1,4),(135.088484104361,
135.549619554034,136.547124640257,137.544629726481,138.542134812704,139.539639898928),
 .UNSPECIFIED.);
#1840=B_SPLINE_CURVE_WITH_KNOTS('',3,(#80187,#80188,#80189,#80190,#80191,
#80192,#80193,#80194,#80195),.UNSPECIFIED.,.F.,.F.,(4,1,1,1,1,1,4),(135.088484104361,
135.096515560027,136.09402064625,137.091525732474,138.089030818698,139.086535904921,
140.062106270563),.UNSPECIFIED.);
#1841=B_SPLINE_CURVE_WITH_KNOTS('',3,(#80200,#80201,#80202,#80203,#80204,
#80205,#80206,#80207,#80208,#80209),.UNSPECIFIED.,.F.,.F.,(4,1,1,1,1,1,
1,4),(128.805298797182,129.564589036692,130.562094122916,131.559599209139,
132.557104295363,133.554609381586,134.55211446781,135.088484104361),
 .UNSPECIFIED.);
#1842=B_SPLINE_CURVE_WITH_KNOTS('',3,(#80210,#80211,#80212,#80213,#80214,
#80215,#80216,#80217,#80218,#80219),.UNSPECIFIED.,.F.,.F.,(4,1,1,1,1,1,
1,4),(128.805298797182,129.111485042685,130.108990128909,131.106495215132,
132.104000301356,133.10150538758,134.099010473803,135.088484104361),
 .UNSPECIFIED.);
#1843=B_SPLINE_CURVE_WITH_KNOTS('',3,(#80224,#80225,#80226,#80227,#80228,
#80229,#80230,#80231,#80232,#80233,#80234),.UNSPECIFIED.,.F.,.F.,(4,1,1,
1,1,1,1,1,4),(122.522113490002,122.582053433127,123.57955851935,124.577063605574,
125.574568691798,126.572073778021,127.569578864245,128.567083950468,128.805298797182),
 .UNSPECIFIED.);
#1844=B_SPLINE_CURVE_WITH_KNOTS('',3,(#80235,#80236,#80237,#80238,#80239,
#80240,#80241,#80242,#80243,#80244),.UNSPECIFIED.,.F.,.F.,(4,1,1,1,1,1,
1,4),(122.522113490002,123.126454525344,124.123959611567,125.121464697791,
126.118969784014,127.116474870238,128.113979956462,128.805298797182),
 .UNSPECIFIED.);
#1845=B_SPLINE_CURVE_WITH_KNOTS('',3,(#80249,#80250,#80251,#80252,#80253,
#80254,#80255,#80256,#80257,#80258),.UNSPECIFIED.,.F.,.F.,(4,1,1,1,1,1,
1,4),(116.238928182822,116.597022915785,117.594528002009,118.592033088232,
119.589538174456,120.58704326068,121.584548346903,122.522113490002),
 .UNSPECIFIED.);
#1846=B_SPLINE_CURVE_WITH_KNOTS('',3,(#80259,#80260,#80261,#80262,#80263,
#80264,#80265,#80266,#80267,#80268),.UNSPECIFIED.,.F.,.F.,(4,1,1,1,1,1,
1,4),(116.238928182822,117.141424008002,118.138929094226,119.136434180449,
120.133939266673,121.131444352896,122.12894943912,122.522113490002),
 .UNSPECIFIED.);
#1847=B_SPLINE_CURVE_WITH_KNOTS('',3,(#80273,#80274,#80275,#80276,#80277,
#80278,#80279,#80280,#80281,#80282),.UNSPECIFIED.,.F.,.F.,(4,1,1,1,1,1,
1,4),(109.955742875643,110.611992398444,111.609497484667,112.607002570891,
113.604507657114,114.602012743338,115.599517829562,116.238928182822),
 .UNSPECIFIED.);
#1848=B_SPLINE_CURVE_WITH_KNOTS('',3,(#80283,#80284,#80285,#80286,#80287,
#80288,#80289,#80290,#80291,#80292,#80293),.UNSPECIFIED.,.F.,.F.,(4,1,1,
1,1,1,1,1,4),(109.955742875643,110.158888404437,111.15639349066,112.153898576884,
113.151403663108,114.148908749331,115.146413835555,116.143918921778,116.238928182822),
 .UNSPECIFIED.);
#1849=B_SPLINE_CURVE_WITH_KNOTS('',3,(#80298,#80299,#80300,#80301,#80302,
#80303,#80304,#80305,#80306,#80307),.UNSPECIFIED.,.F.,.F.,(4,1,1,1,1,1,
1,4),(103.672557568463,104.626961881102,105.624466967326,106.621972053549,
107.619477139773,108.616982225996,109.61448731222,109.955742875643),
 .UNSPECIFIED.);
#1850=B_SPLINE_CURVE_WITH_KNOTS('',3,(#80308,#80309,#80310,#80311,#80312,
#80313,#80314,#80315,#80316,#80317),.UNSPECIFIED.,.F.,.F.,(4,1,1,1,1,1,
1,4),(103.672557568463,104.173857887095,105.171362973319,106.168868059543,
107.166373145766,108.16387823199,109.161383318213,109.955742875643),
 .UNSPECIFIED.);
#1851=B_SPLINE_CURVE_WITH_KNOTS('',3,(#80322,#80323,#80324,#80325,#80326,
#80327,#80328,#80329,#80330,#80331,#80332),.UNSPECIFIED.,.F.,.F.,(4,1,1,
1,1,1,1,1,4),(97.3893722612835,97.6444262775369,98.6419313637605,99.6394364499841,
100.636941536208,101.634446622431,102.631951708655,103.629456794878,103.672557568463),
 .UNSPECIFIED.);
#1852=B_SPLINE_CURVE_WITH_KNOTS('',3,(#80333,#80334,#80335,#80336,#80337,
#80338,#80339,#80340,#80341,#80342),.UNSPECIFIED.,.F.,.F.,(4,1,1,1,1,1,
1,4),(97.3893722612836,98.1888273697538,99.1863324559774,100.183837542201,
101.181342628425,102.178847714648,103.176352800872,103.672557568463),
 .UNSPECIFIED.);
#1853=B_SPLINE_CURVE_WITH_KNOTS('',3,(#80347,#80348,#80349,#80350,#80351,
#80352,#80353,#80354,#80355,#80356),.UNSPECIFIED.,.F.,.F.,(4,1,1,1,1,1,
1,4),(91.106186954104,91.6593957601954,92.6569008464189,93.6544059326425,
94.6519110188661,95.6494161050897,96.6469211913133,97.3893722612835),
 .UNSPECIFIED.);
#1854=B_SPLINE_CURVE_WITH_KNOTS('',3,(#80357,#80358,#80359,#80360,#80361,
#80362,#80363,#80364,#80365,#80366,#80367),.UNSPECIFIED.,.F.,.F.,(4,1,1,
1,1,1,1,1,4),(91.106186954104,91.2062917661886,92.2037968524122,93.2013019386358,
94.1988070248594,95.196312111083,96.1938171973066,97.1913222835302,97.3893722612836),
 .UNSPECIFIED.);
#1855=B_SPLINE_CURVE_WITH_KNOTS('',3,(#80372,#80373,#80374,#80375,#80376,
#80377,#80378,#80379,#80380,#80381),.UNSPECIFIED.,.F.,.F.,(4,1,1,1,1,1,
1,4),(84.8230016469244,85.6743652428538,86.6718703290774,87.669375415301,
88.6668805015246,89.6643855877482,90.6618906739718,91.106186954104),
 .UNSPECIFIED.);
#1856=B_SPLINE_CURVE_WITH_KNOTS('',3,(#80382,#80383,#80384,#80385,#80386,
#80387,#80388,#80389,#80390,#80391),.UNSPECIFIED.,.F.,.F.,(4,1,1,1,1,1,
1,4),(84.8230016469244,85.221261248847,86.2187663350706,87.2162714212942,
88.2137765075178,89.2112815937414,90.208786679965,91.106186954104),
 .UNSPECIFIED.);
#1857=B_SPLINE_CURVE_WITH_KNOTS('',3,(#80396,#80397,#80398,#80399,#80400,
#80401,#80402,#80403,#80404,#80405,#80406),.UNSPECIFIED.,.F.,.F.,(4,1,1,
1,1,1,1,1,4),(78.5398163397448,78.6918296392886,79.6893347255122,80.6868398117358,
81.6843448979594,82.681849984183,83.6793550704066,84.6768601566302,84.8230016469244),
 .UNSPECIFIED.);
#1858=B_SPLINE_CURVE_WITH_KNOTS('',3,(#80407,#80408,#80409,#80410,#80411,
#80412,#80413,#80414,#80415,#80416),.UNSPECIFIED.,.F.,.F.,(4,1,1,1,1,1,
1,4),(78.5398163397448,79.2362307315055,80.2337358177291,81.2312409039526,
82.2287459901762,83.2262510763998,84.2237561626234,84.8230016469244),
 .UNSPECIFIED.);
#1859=B_SPLINE_CURVE_WITH_KNOTS('',3,(#80421,#80422,#80423,#80424,#80425,
#80426,#80427,#80428,#80429,#80430),.UNSPECIFIED.,.F.,.F.,(4,1,1,1,1,1,
1,4),(72.2566310325652,72.706799121947,73.7043042081706,74.7018092943942,
75.6993143806178,76.6968194668414,77.694324553065,78.5398163397448),
 .UNSPECIFIED.);
#1860=B_SPLINE_CURVE_WITH_KNOTS('',3,(#80431,#80432,#80433,#80434,#80435,
#80436,#80437,#80438,#80439,#80440),.UNSPECIFIED.,.F.,.F.,(4,1,1,1,1,1,
1,4),(72.2566310325652,73.2512002141639,74.2487053003875,75.2462103866111,
76.2437154728347,77.2412205590583,78.2387256452819,78.5398163397448),
 .UNSPECIFIED.);
#1861=B_SPLINE_CURVE_WITH_KNOTS('',3,(#80445,#80446,#80447,#80448,#80449,
#80450,#80451,#80452,#80453,#80454),.UNSPECIFIED.,.F.,.F.,(4,1,1,1,1,1,
1,4),(65.9734457253856,66.7217686046055,67.7192736908291,68.7167787770527,
69.7142838632763,70.7117889494998,71.7092940357234,72.2566310325652),
 .UNSPECIFIED.);
#1862=B_SPLINE_CURVE_WITH_KNOTS('',3,(#80455,#80456,#80457,#80458,#80459,
#80460,#80461,#80462,#80463,#80464,#80465),.UNSPECIFIED.,.F.,.F.,(4,1,1,
1,1,1,1,1,4),(65.9734457253856,66.2686646105987,67.2661696968223,68.2636747830459,
69.2611798692695,70.2586849554931,71.2561900417167,72.2536951279403,72.2566310325652),
 .UNSPECIFIED.);
#1863=B_SPLINE_CURVE_WITH_KNOTS('',3,(#80470,#80471,#80472,#80473,#80474,
#80475,#80476,#80477,#80478,#80479,#80480),.UNSPECIFIED.,.F.,.F.,(4,1,1,
1,1,1,1,1,4),(59.690260418206,59.7392330010403,60.7367380872639,61.7342431734875,
62.7317482597111,63.7292533459347,64.7267584321583,65.7242635183819,65.9734457253856),
 .UNSPECIFIED.);
#1864=B_SPLINE_CURVE_WITH_KNOTS('',3,(#80481,#80482,#80483,#80484,#80485,
#80486,#80487,#80488,#80489,#80490),.UNSPECIFIED.,.F.,.F.,(4,1,1,1,1,1,
1,4),(59.690260418206,60.2836340932571,61.2811391794807,62.2786442657043,
63.2761493519279,64.2736544381515,65.2711595243751,65.9734457253856),
 .UNSPECIFIED.);
#1865=B_SPLINE_CURVE_WITH_KNOTS('',3,(#80495,#80496,#80497,#80498,#80499,
#80500,#80501,#80502,#80503,#80504),.UNSPECIFIED.,.F.,.F.,(4,1,1,1,1,1,
1,4),(53.4070751110264,53.7542024836987,54.7517075699223,55.7492126561459,
56.7467177423695,57.7442228285931,58.7417279148167,59.690260418206),
 .UNSPECIFIED.);
#1866=B_SPLINE_CURVE_WITH_KNOTS('',3,(#80505,#80506,#80507,#80508,#80509,
#80510,#80511,#80512,#80513,#80514),.UNSPECIFIED.,.F.,.F.,(4,1,1,1,1,1,
1,4),(53.4070751110264,54.2986035759156,55.2961086621392,56.2936137483628,
57.2911188345864,58.28862392081,59.2861290070336,59.690260418206),
 .UNSPECIFIED.);
#1867=B_SPLINE_CURVE_WITH_KNOTS('',3,(#80519,#80520,#80521,#80522,#80523,
#80524,#80525,#80526,#80527,#80528),.UNSPECIFIED.,.F.,.F.,(4,1,1,1,1,1,
1,4),(47.1238898038468,47.7691719663572,48.7666770525808,49.7641821388044,
50.7616872250279,51.7591923112515,52.7566973974751,53.4070751110264),
 .UNSPECIFIED.);
#1868=B_SPLINE_CURVE_WITH_KNOTS('',3,(#80529,#80530,#80531,#80532,#80533,
#80534,#80535,#80536,#80537,#80538,#80539),.UNSPECIFIED.,.F.,.F.,(4,1,1,
1,1,1,1,1,4),(47.1238898038468,47.3160679723504,48.313573058574,49.3110781447976,
50.3085832310212,51.3060883172448,52.3035934034684,53.301098489692,53.4070751110264),
 .UNSPECIFIED.);
#1869=B_SPLINE_CURVE_WITH_KNOTS('',3,(#80544,#80545,#80546,#80547,#80548,
#80549,#80550,#80551,#80552,#80553),.UNSPECIFIED.,.F.,.F.,(4,1,1,1,1,1,
1,4),(40.8407044966672,41.7841414490156,42.7816465352392,43.7791516214628,
44.7766567076864,45.77416179391,46.7716668801336,47.1238898038468),
 .UNSPECIFIED.);
#1870=B_SPLINE_CURVE_WITH_KNOTS('',3,(#80554,#80555,#80556,#80557,#80558,
#80559,#80560,#80561,#80562,#80563),.UNSPECIFIED.,.F.,.F.,(4,1,1,1,1,1,
1,4),(40.8407044966673,41.3310374550088,42.3285425412324,43.326047627456,
44.3235527136796,45.3210577999032,46.3185628861268,47.1238898038468),
 .UNSPECIFIED.);
#1871=B_SPLINE_CURVE_WITH_KNOTS('',3,(#80568,#80569,#80570,#80571,#80572,
#80573,#80574,#80575,#80576,#80577,#80578),.UNSPECIFIED.,.F.,.F.,(4,1,1,
1,1,1,1,1,4),(34.5575191894876,34.8016058454504,35.799110931674,36.7966160178976,
37.7941211041212,38.7916261903448,39.7891312765684,40.786636362792,40.8407044966672),
 .UNSPECIFIED.);
#1872=B_SPLINE_CURVE_WITH_KNOTS('',3,(#80579,#80580,#80581,#80582,#80583,
#80584,#80585,#80586,#80587,#80588),.UNSPECIFIED.,.F.,.F.,(4,1,1,1,1,1,
1,4),(34.5575191894877,35.3460069376673,36.3435120238909,37.3410171101145,
38.3385221963381,39.3360272825617,40.3335323687852,40.8407044966673),
 .UNSPECIFIED.);
#1873=B_SPLINE_CURVE_WITH_KNOTS('',3,(#80593,#80594,#80595,#80596,#80597,
#80598,#80599,#80600,#80601,#80602),.UNSPECIFIED.,.F.,.F.,(4,1,1,1,1,1,
1,4),(28.2743338823081,28.8165753281089,29.8140804143324,30.811585500556,
31.8090905867796,32.8065956730032,33.8041007592268,34.5575191894876),
 .UNSPECIFIED.);
#1874=B_SPLINE_CURVE_WITH_KNOTS('',3,(#80603,#80604,#80605,#80606,#80607,
#80608,#80609,#80610,#80611,#80612,#80613),.UNSPECIFIED.,.F.,.F.,(4,1,1,
1,1,1,1,1,4),(28.2743338823081,28.3634713341021,29.3609764203257,30.3584815065493,
31.3559865927729,32.3534916789965,33.3509967652201,34.3485018514437,34.5575191894877),
 .UNSPECIFIED.);
#1875=B_SPLINE_CURVE_WITH_KNOTS('',3,(#80618,#80619,#80620,#80621,#80622,
#80623,#80624,#80625,#80626,#80627),.UNSPECIFIED.,.F.,.F.,(4,1,1,1,1,1,
1,4),(21.9911485751285,22.8315448107673,23.8290498969909,24.8265549832145,
25.8240600694381,26.8215651556617,27.8190702418853,28.2743338823081),
 .UNSPECIFIED.);
#1876=B_SPLINE_CURVE_WITH_KNOTS('',3,(#80628,#80629,#80630,#80631,#80632,
#80633,#80634,#80635,#80636,#80637),.UNSPECIFIED.,.F.,.F.,(4,1,1,1,1,1,
1,4),(21.9911485751285,22.3784408167605,23.3759459029841,24.3734509892077,
25.3709560754313,26.3684611616549,27.3659662478785,28.2743338823081),
 .UNSPECIFIED.);
#1877=B_SPLINE_CURVE_WITH_KNOTS('',3,(#80643,#80644,#80645,#80646,#80647),
 .UNSPECIFIED.,.F.,.F.,(4,1,4),(14.3984001269718,15.3959052131954,15.7079632679489),
 .UNSPECIFIED.);
#1878=B_SPLINE_CURVE_WITH_KNOTS('',3,(#80650,#80651,#80652,#80653,#80654),
 .UNSPECIFIED.,.F.,.F.,(4,1,4),(13.8759337553362,14.8515041209785,15.7079632679489),
 .UNSPECIFIED.);
#1879=B_SPLINE_CURVE_WITH_KNOTS('',3,(#80660,#80661,#80662,#80663,#80664,
#80665,#80666,#80667),.UNSPECIFIED.,.F.,.F.,(4,1,1,1,1,4),(135.088484104361,
135.549619554033,136.547124640257,137.544629726481,138.542134812704,139.539639898928),
 .UNSPECIFIED.);
#1880=B_SPLINE_CURVE_WITH_KNOTS('',3,(#80670,#80671,#80672,#80673,#80674,
#80675,#80676,#80677,#80678),.UNSPECIFIED.,.F.,.F.,(4,1,1,1,1,1,4),(135.088484104361,
135.096515560027,136.09402064625,137.091525732474,138.089030818698,139.086535904921,
140.062106270563),.UNSPECIFIED.);
#1881=B_SPLINE_CURVE_WITH_KNOTS('',3,(#80683,#80684,#80685,#80686,#80687,
#80688,#80689,#80690,#80691,#80692),.UNSPECIFIED.,.F.,.F.,(4,1,1,1,1,1,
1,4),(128.805298797182,129.564589036692,130.562094122916,131.559599209139,
132.557104295363,133.554609381586,134.55211446781,135.088484104361),
 .UNSPECIFIED.);
#1882=B_SPLINE_CURVE_WITH_KNOTS('',3,(#80693,#80694,#80695,#80696,#80697,
#80698,#80699,#80700,#80701,#80702),.UNSPECIFIED.,.F.,.F.,(4,1,1,1,1,1,
1,4),(128.805298797182,129.111485042685,130.108990128909,131.106495215132,
132.104000301356,133.10150538758,134.099010473803,135.088484104361),
 .UNSPECIFIED.);
#1883=B_SPLINE_CURVE_WITH_KNOTS('',3,(#80707,#80708,#80709,#80710,#80711,
#80712,#80713,#80714,#80715,#80716,#80717),.UNSPECIFIED.,.F.,.F.,(4,1,1,
1,1,1,1,1,4),(122.522113490002,122.582053433127,123.57955851935,124.577063605574,
125.574568691798,126.572073778021,127.569578864245,128.567083950468,128.805298797182),
 .UNSPECIFIED.);
#1884=B_SPLINE_CURVE_WITH_KNOTS('',3,(#80718,#80719,#80720,#80721,#80722,
#80723,#80724,#80725,#80726,#80727),.UNSPECIFIED.,.F.,.F.,(4,1,1,1,1,1,
1,4),(122.522113490002,123.126454525344,124.123959611567,125.121464697791,
126.118969784014,127.116474870238,128.113979956462,128.805298797182),
 .UNSPECIFIED.);
#1885=B_SPLINE_CURVE_WITH_KNOTS('',3,(#80732,#80733,#80734,#80735,#80736,
#80737,#80738,#80739,#80740,#80741),.UNSPECIFIED.,.F.,.F.,(4,1,1,1,1,1,
1,4),(116.238928182822,116.597022915785,117.594528002009,118.592033088232,
119.589538174456,120.58704326068,121.584548346903,122.522113490002),
 .UNSPECIFIED.);
#1886=B_SPLINE_CURVE_WITH_KNOTS('',3,(#80742,#80743,#80744,#80745,#80746,
#80747,#80748,#80749,#80750,#80751),.UNSPECIFIED.,.F.,.F.,(4,1,1,1,1,1,
1,4),(116.238928182822,117.141424008002,118.138929094226,119.136434180449,
120.133939266673,121.131444352896,122.12894943912,122.522113490002),
 .UNSPECIFIED.);
#1887=B_SPLINE_CURVE_WITH_KNOTS('',3,(#80756,#80757,#80758,#80759,#80760,
#80761,#80762,#80763,#80764,#80765),.UNSPECIFIED.,.F.,.F.,(4,1,1,1,1,1,
1,4),(109.955742875643,110.611992398444,111.609497484667,112.607002570891,
113.604507657114,114.602012743338,115.599517829562,116.238928182822),
 .UNSPECIFIED.);
#1888=B_SPLINE_CURVE_WITH_KNOTS('',3,(#80766,#80767,#80768,#80769,#80770,
#80771,#80772,#80773,#80774,#80775,#80776),.UNSPECIFIED.,.F.,.F.,(4,1,1,
1,1,1,1,1,4),(109.955742875643,110.158888404437,111.15639349066,112.153898576884,
113.151403663108,114.148908749331,115.146413835555,116.143918921778,116.238928182822),
 .UNSPECIFIED.);
#1889=B_SPLINE_CURVE_WITH_KNOTS('',3,(#80781,#80782,#80783,#80784,#80785,
#80786,#80787,#80788,#80789,#80790),.UNSPECIFIED.,.F.,.F.,(4,1,1,1,1,1,
1,4),(103.672557568463,104.626961881102,105.624466967326,106.621972053549,
107.619477139773,108.616982225996,109.61448731222,109.955742875643),
 .UNSPECIFIED.);
#1890=B_SPLINE_CURVE_WITH_KNOTS('',3,(#80791,#80792,#80793,#80794,#80795,
#80796,#80797,#80798,#80799,#80800),.UNSPECIFIED.,.F.,.F.,(4,1,1,1,1,1,
1,4),(103.672557568463,104.173857887095,105.171362973319,106.168868059543,
107.166373145766,108.16387823199,109.161383318213,109.955742875643),
 .UNSPECIFIED.);
#1891=B_SPLINE_CURVE_WITH_KNOTS('',3,(#80805,#80806,#80807,#80808,#80809,
#80810,#80811,#80812,#80813,#80814,#80815),.UNSPECIFIED.,.F.,.F.,(4,1,1,
1,1,1,1,1,4),(97.3893722612835,97.6444262775369,98.6419313637605,99.6394364499841,
100.636941536208,101.634446622431,102.631951708655,103.629456794878,103.672557568463),
 .UNSPECIFIED.);
#1892=B_SPLINE_CURVE_WITH_KNOTS('',3,(#80816,#80817,#80818,#80819,#80820,
#80821,#80822,#80823,#80824,#80825),.UNSPECIFIED.,.F.,.F.,(4,1,1,1,1,1,
1,4),(97.3893722612836,98.1888273697538,99.1863324559773,100.183837542201,
101.181342628425,102.178847714648,103.176352800872,103.672557568463),
 .UNSPECIFIED.);
#1893=B_SPLINE_CURVE_WITH_KNOTS('',3,(#80830,#80831,#80832,#80833,#80834,
#80835,#80836,#80837,#80838,#80839),.UNSPECIFIED.,.F.,.F.,(4,1,1,1,1,1,
1,4),(91.106186954104,91.6593957601953,92.6569008464189,93.6544059326425,
94.6519110188661,95.6494161050897,96.6469211913133,97.3893722612835),
 .UNSPECIFIED.);
#1894=B_SPLINE_CURVE_WITH_KNOTS('',3,(#80840,#80841,#80842,#80843,#80844,
#80845,#80846,#80847,#80848,#80849,#80850),.UNSPECIFIED.,.F.,.F.,(4,1,1,
1,1,1,1,1,4),(91.106186954104,91.2062917661886,92.2037968524122,93.2013019386358,
94.1988070248594,95.196312111083,96.1938171973066,97.1913222835302,97.3893722612836),
 .UNSPECIFIED.);
#1895=B_SPLINE_CURVE_WITH_KNOTS('',3,(#80855,#80856,#80857,#80858,#80859,
#80860,#80861,#80862,#80863,#80864),.UNSPECIFIED.,.F.,.F.,(4,1,1,1,1,1,
1,4),(84.8230016469244,85.6743652428537,86.6718703290773,87.6693754153009,
88.6668805015245,89.6643855877481,90.6618906739717,91.106186954104),
 .UNSPECIFIED.);
#1896=B_SPLINE_CURVE_WITH_KNOTS('',3,(#80865,#80866,#80867,#80868,#80869,
#80870,#80871,#80872,#80873,#80874),.UNSPECIFIED.,.F.,.F.,(4,1,1,1,1,1,
1,4),(84.8230016469244,85.221261248847,86.2187663350706,87.2162714212942,
88.2137765075178,89.2112815937414,90.208786679965,91.106186954104),
 .UNSPECIFIED.);
#1897=B_SPLINE_CURVE_WITH_KNOTS('',3,(#80879,#80880,#80881,#80882,#80883,
#80884,#80885,#80886,#80887,#80888,#80889),.UNSPECIFIED.,.F.,.F.,(4,1,1,
1,1,1,1,1,4),(78.5398163397448,78.6918296392886,79.6893347255122,80.6868398117358,
81.6843448979594,82.681849984183,83.6793550704066,84.6768601566301,84.8230016469244),
 .UNSPECIFIED.);
#1898=B_SPLINE_CURVE_WITH_KNOTS('',3,(#80890,#80891,#80892,#80893,#80894,
#80895,#80896,#80897,#80898,#80899),.UNSPECIFIED.,.F.,.F.,(4,1,1,1,1,1,
1,4),(78.5398163397448,79.2362307315054,80.233735817729,81.2312409039526,
82.2287459901762,83.2262510763998,84.2237561626234,84.8230016469244),
 .UNSPECIFIED.);
#1899=B_SPLINE_CURVE_WITH_KNOTS('',3,(#80904,#80905,#80906,#80907,#80908,
#80909,#80910,#80911,#80912,#80913),.UNSPECIFIED.,.F.,.F.,(4,1,1,1,1,1,
1,4),(72.2566310325652,72.706799121947,73.7043042081706,74.7018092943942,
75.6993143806178,76.6968194668414,77.694324553065,78.5398163397448),
 .UNSPECIFIED.);
#1900=B_SPLINE_CURVE_WITH_KNOTS('',3,(#80914,#80915,#80916,#80917,#80918,
#80919,#80920,#80921,#80922,#80923),.UNSPECIFIED.,.F.,.F.,(4,1,1,1,1,1,
1,4),(72.2566310325652,73.2512002141639,74.2487053003875,75.2462103866111,
76.2437154728347,77.2412205590582,78.2387256452818,78.5398163397448),
 .UNSPECIFIED.);
#1901=B_SPLINE_CURVE_WITH_KNOTS('',3,(#80928,#80929,#80930,#80931,#80932,
#80933,#80934,#80935,#80936,#80937),.UNSPECIFIED.,.F.,.F.,(4,1,1,1,1,1,
1,4),(65.9734457253856,66.7217686046054,67.719273690829,68.7167787770526,
69.7142838632762,70.7117889494998,71.7092940357234,72.2566310325652),
 .UNSPECIFIED.);
#1902=B_SPLINE_CURVE_WITH_KNOTS('',3,(#80938,#80939,#80940,#80941,#80942,
#80943,#80944,#80945,#80946,#80947,#80948),.UNSPECIFIED.,.F.,.F.,(4,1,1,
1,1,1,1,1,4),(65.9734457253856,66.2686646105987,67.2661696968223,68.2636747830459,
69.2611798692695,70.2586849554931,71.2561900417167,72.2536951279403,72.2566310325652),
 .UNSPECIFIED.);
#1903=B_SPLINE_CURVE_WITH_KNOTS('',3,(#80953,#80954,#80955,#80956,#80957,
#80958,#80959,#80960,#80961,#80962,#80963),.UNSPECIFIED.,.F.,.F.,(4,1,1,
1,1,1,1,1,4),(59.690260418206,59.7392330010403,60.7367380872639,61.7342431734875,
62.7317482597111,63.7292533459347,64.7267584321582,65.7242635183818,65.9734457253856),
 .UNSPECIFIED.);
#1904=B_SPLINE_CURVE_WITH_KNOTS('',3,(#80964,#80965,#80966,#80967,#80968,
#80969,#80970,#80971,#80972,#80973),.UNSPECIFIED.,.F.,.F.,(4,1,1,1,1,1,
1,4),(59.690260418206,60.2836340932571,61.2811391794807,62.2786442657043,
63.2761493519279,64.2736544381515,65.2711595243751,65.9734457253856),
 .UNSPECIFIED.);
#1905=B_SPLINE_CURVE_WITH_KNOTS('',3,(#80978,#80979,#80980,#80981,#80982,
#80983,#80984,#80985,#80986,#80987),.UNSPECIFIED.,.F.,.F.,(4,1,1,1,1,1,
1,4),(53.4070751110264,53.7542024836987,54.7517075699223,55.7492126561459,
56.7467177423695,57.7442228285931,58.7417279148167,59.690260418206),
 .UNSPECIFIED.);
#1906=B_SPLINE_CURVE_WITH_KNOTS('',3,(#80988,#80989,#80990,#80991,#80992,
#80993,#80994,#80995,#80996,#80997),.UNSPECIFIED.,.F.,.F.,(4,1,1,1,1,1,
1,4),(53.4070751110264,54.2986035759156,55.2961086621392,56.2936137483628,
57.2911188345863,58.2886239208099,59.2861290070335,59.690260418206),
 .UNSPECIFIED.);
#1907=B_SPLINE_CURVE_WITH_KNOTS('',3,(#81002,#81003,#81004,#81005,#81006,
#81007,#81008,#81009,#81010,#81011),.UNSPECIFIED.,.F.,.F.,(4,1,1,1,1,1,
1,4),(47.1238898038468,47.7691719663571,48.7666770525807,49.7641821388043,
50.7616872250279,51.7591923112515,52.7566973974751,53.4070751110264),
 .UNSPECIFIED.);
#1908=B_SPLINE_CURVE_WITH_KNOTS('',3,(#81012,#81013,#81014,#81015,#81016,
#81017,#81018,#81019,#81020,#81021,#81022),.UNSPECIFIED.,.F.,.F.,(4,1,1,
1,1,1,1,1,4),(47.1238898038468,47.3160679723504,48.313573058574,49.3110781447976,
50.3085832310212,51.3060883172448,52.3035934034684,53.301098489692,53.4070751110264),
 .UNSPECIFIED.);
#1909=B_SPLINE_CURVE_WITH_KNOTS('',3,(#81027,#81028,#81029,#81030,#81031,
#81032,#81033,#81034,#81035,#81036),.UNSPECIFIED.,.F.,.F.,(4,1,1,1,1,1,
1,4),(40.8407044966672,41.7841414490156,42.7816465352392,43.7791516214628,
44.7766567076863,45.7741617939099,46.7716668801335,47.1238898038468),
 .UNSPECIFIED.);
#1910=B_SPLINE_CURVE_WITH_KNOTS('',3,(#81037,#81038,#81039,#81040,#81041,
#81042,#81043,#81044,#81045,#81046),.UNSPECIFIED.,.F.,.F.,(4,1,1,1,1,1,
1,4),(40.8407044966673,41.3310374550088,42.3285425412324,43.326047627456,
44.3235527136796,45.3210577999032,46.3185628861268,47.1238898038468),
 .UNSPECIFIED.);
#1911=B_SPLINE_CURVE_WITH_KNOTS('',3,(#81051,#81052,#81053,#81054,#81055,
#81056,#81057,#81058,#81059,#81060,#81061),.UNSPECIFIED.,.F.,.F.,(4,1,1,
1,1,1,1,1,4),(34.5575191894876,34.8016058454504,35.799110931674,36.7966160178976,
37.7941211041212,38.7916261903448,39.7891312765684,40.786636362792,40.8407044966672),
 .UNSPECIFIED.);
#1912=B_SPLINE_CURVE_WITH_KNOTS('',3,(#81062,#81063,#81064,#81065,#81066,
#81067,#81068,#81069,#81070,#81071),.UNSPECIFIED.,.F.,.F.,(4,1,1,1,1,1,
1,4),(34.5575191894877,35.3460069376672,36.3435120238908,37.3410171101144,
38.338522196338,39.3360272825616,40.3335323687852,40.8407044966673),
 .UNSPECIFIED.);
#1913=B_SPLINE_CURVE_WITH_KNOTS('',3,(#81076,#81077,#81078,#81079,#81080,
#81081,#81082,#81083,#81084,#81085),.UNSPECIFIED.,.F.,.F.,(4,1,1,1,1,1,
1,4),(28.2743338823081,28.8165753281088,29.8140804143324,30.811585500556,
31.8090905867796,32.8065956730032,33.8041007592268,34.5575191894876),
 .UNSPECIFIED.);
#1914=B_SPLINE_CURVE_WITH_KNOTS('',3,(#81086,#81087,#81088,#81089,#81090,
#81091,#81092,#81093,#81094,#81095,#81096),.UNSPECIFIED.,.F.,.F.,(4,1,1,
1,1,1,1,1,4),(28.2743338823081,28.3634713341021,29.3609764203257,30.3584815065493,
31.3559865927729,32.3534916789965,33.3509967652201,34.3485018514437,34.5575191894877),
 .UNSPECIFIED.);
#1915=B_SPLINE_CURVE_WITH_KNOTS('',3,(#81101,#81102,#81103,#81104,#81105,
#81106,#81107,#81108,#81109,#81110),.UNSPECIFIED.,.F.,.F.,(4,1,1,1,1,1,
1,4),(21.9911485751285,22.8315448107673,23.8290498969909,24.8265549832144,
25.824060069438,26.8215651556616,27.8190702418852,28.2743338823081),
 .UNSPECIFIED.);
#1916=B_SPLINE_CURVE_WITH_KNOTS('',3,(#81111,#81112,#81113,#81114,#81115,
#81116,#81117,#81118,#81119,#81120),.UNSPECIFIED.,.F.,.F.,(4,1,1,1,1,1,
1,4),(21.9911485751285,22.3784408167605,23.3759459029841,24.3734509892077,
25.3709560754313,26.3684611616549,27.3659662478785,28.2743338823081),
 .UNSPECIFIED.);
#1917=B_SPLINE_CURVE_WITH_KNOTS('',3,(#81126,#81127,#81128,#81129,#81130),
 .UNSPECIFIED.,.F.,.F.,(4,1,4),(14.3984001269717,15.3959052131953,15.7079632679489),
 .UNSPECIFIED.);
#1918=B_SPLINE_CURVE_WITH_KNOTS('',3,(#81133,#81134,#81135,#81136,#81137),
 .UNSPECIFIED.,.F.,.F.,(4,1,4),(13.8759337553361,14.8515041209785,15.7079632679489),
 .UNSPECIFIED.);
#1919=B_SPLINE_CURVE_WITH_KNOTS('',3,(#81143,#81144,#81145,#81146,#81147,
#81148,#81149,#81150),.UNSPECIFIED.,.F.,.F.,(4,1,1,1,1,4),(135.088484104361,
135.549619554034,136.547124640257,137.544629726481,138.542134812704,139.539639898928),
 .UNSPECIFIED.);
#1920=B_SPLINE_CURVE_WITH_KNOTS('',3,(#81153,#81154,#81155,#81156,#81157,
#81158,#81159,#81160,#81161),.UNSPECIFIED.,.F.,.F.,(4,1,1,1,1,1,4),(135.088484104361,
135.096515560027,136.09402064625,137.091525732474,138.089030818698,139.086535904921,
140.062106270563),.UNSPECIFIED.);
#1921=B_SPLINE_CURVE_WITH_KNOTS('',3,(#81166,#81167,#81168,#81169,#81170,
#81171,#81172,#81173,#81174,#81175),.UNSPECIFIED.,.F.,.F.,(4,1,1,1,1,1,
1,4),(128.805298797182,129.564589036692,130.562094122916,131.559599209139,
132.557104295363,133.554609381586,134.55211446781,135.088484104361),
 .UNSPECIFIED.);
#1922=B_SPLINE_CURVE_WITH_KNOTS('',3,(#81176,#81177,#81178,#81179,#81180,
#81181,#81182,#81183,#81184,#81185),.UNSPECIFIED.,.F.,.F.,(4,1,1,1,1,1,
1,4),(128.805298797182,129.111485042685,130.108990128909,131.106495215132,
132.104000301356,133.10150538758,134.099010473803,135.088484104361),
 .UNSPECIFIED.);
#1923=B_SPLINE_CURVE_WITH_KNOTS('',3,(#81190,#81191,#81192,#81193,#81194,
#81195,#81196,#81197,#81198,#81199,#81200),.UNSPECIFIED.,.F.,.F.,(4,1,1,
1,1,1,1,1,4),(122.522113490002,122.582053433127,123.57955851935,124.577063605574,
125.574568691798,126.572073778021,127.569578864245,128.567083950468,128.805298797182),
 .UNSPECIFIED.);
#1924=B_SPLINE_CURVE_WITH_KNOTS('',3,(#81201,#81202,#81203,#81204,#81205,
#81206,#81207,#81208,#81209,#81210),.UNSPECIFIED.,.F.,.F.,(4,1,1,1,1,1,
1,4),(122.522113490002,123.126454525344,124.123959611567,125.121464697791,
126.118969784014,127.116474870238,128.113979956462,128.805298797182),
 .UNSPECIFIED.);
#1925=B_SPLINE_CURVE_WITH_KNOTS('',3,(#81215,#81216,#81217,#81218,#81219,
#81220,#81221,#81222,#81223,#81224),.UNSPECIFIED.,.F.,.F.,(4,1,1,1,1,1,
1,4),(116.238928182822,116.597022915785,117.594528002009,118.592033088232,
119.589538174456,120.58704326068,121.584548346903,122.522113490002),
 .UNSPECIFIED.);
#1926=B_SPLINE_CURVE_WITH_KNOTS('',3,(#81225,#81226,#81227,#81228,#81229,
#81230,#81231,#81232,#81233,#81234),.UNSPECIFIED.,.F.,.F.,(4,1,1,1,1,1,
1,4),(116.238928182822,117.141424008002,118.138929094226,119.136434180449,
120.133939266673,121.131444352896,122.12894943912,122.522113490002),
 .UNSPECIFIED.);
#1927=B_SPLINE_CURVE_WITH_KNOTS('',3,(#81239,#81240,#81241,#81242,#81243,
#81244,#81245,#81246,#81247,#81248),.UNSPECIFIED.,.F.,.F.,(4,1,1,1,1,1,
1,4),(109.955742875643,110.611992398444,111.609497484667,112.607002570891,
113.604507657114,114.602012743338,115.599517829562,116.238928182822),
 .UNSPECIFIED.);
#1928=B_SPLINE_CURVE_WITH_KNOTS('',3,(#81249,#81250,#81251,#81252,#81253,
#81254,#81255,#81256,#81257,#81258,#81259),.UNSPECIFIED.,.F.,.F.,(4,1,1,
1,1,1,1,1,4),(109.955742875643,110.158888404437,111.15639349066,112.153898576884,
113.151403663108,114.148908749331,115.146413835555,116.143918921778,116.238928182822),
 .UNSPECIFIED.);
#1929=B_SPLINE_CURVE_WITH_KNOTS('',3,(#81264,#81265,#81266,#81267,#81268,
#81269,#81270,#81271,#81272,#81273),.UNSPECIFIED.,.F.,.F.,(4,1,1,1,1,1,
1,4),(103.672557568463,104.626961881102,105.624466967326,106.621972053549,
107.619477139773,108.616982225996,109.61448731222,109.955742875643),
 .UNSPECIFIED.);
#1930=B_SPLINE_CURVE_WITH_KNOTS('',3,(#81274,#81275,#81276,#81277,#81278,
#81279,#81280,#81281,#81282,#81283),.UNSPECIFIED.,.F.,.F.,(4,1,1,1,1,1,
1,4),(103.672557568463,104.173857887095,105.171362973319,106.168868059543,
107.166373145766,108.16387823199,109.161383318213,109.955742875643),
 .UNSPECIFIED.);
#1931=B_SPLINE_CURVE_WITH_KNOTS('',3,(#81288,#81289,#81290,#81291,#81292,
#81293,#81294,#81295,#81296,#81297,#81298),.UNSPECIFIED.,.F.,.F.,(4,1,1,
1,1,1,1,1,4),(97.3893722612835,97.6444262775369,98.6419313637605,99.6394364499841,
100.636941536208,101.634446622431,102.631951708655,103.629456794878,103.672557568463),
 .UNSPECIFIED.);
#1932=B_SPLINE_CURVE_WITH_KNOTS('',3,(#81299,#81300,#81301,#81302,#81303,
#81304,#81305,#81306,#81307,#81308),.UNSPECIFIED.,.F.,.F.,(4,1,1,1,1,1,
1,4),(97.3893722612836,98.1888273697538,99.1863324559774,100.183837542201,
101.181342628425,102.178847714648,103.176352800872,103.672557568463),
 .UNSPECIFIED.);
#1933=B_SPLINE_CURVE_WITH_KNOTS('',3,(#81313,#81314,#81315,#81316,#81317,
#81318,#81319,#81320,#81321,#81322),.UNSPECIFIED.,.F.,.F.,(4,1,1,1,1,1,
1,4),(91.106186954104,91.6593957601953,92.6569008464189,93.6544059326425,
94.6519110188661,95.6494161050897,96.6469211913133,97.3893722612835),
 .UNSPECIFIED.);
#1934=B_SPLINE_CURVE_WITH_KNOTS('',3,(#81323,#81324,#81325,#81326,#81327,
#81328,#81329,#81330,#81331,#81332,#81333),.UNSPECIFIED.,.F.,.F.,(4,1,1,
1,1,1,1,1,4),(91.106186954104,91.2062917661886,92.2037968524122,93.2013019386358,
94.1988070248594,95.196312111083,96.1938171973066,97.1913222835302,97.3893722612836),
 .UNSPECIFIED.);
#1935=B_SPLINE_CURVE_WITH_KNOTS('',3,(#81338,#81339,#81340,#81341,#81342,
#81343,#81344,#81345,#81346,#81347),.UNSPECIFIED.,.F.,.F.,(4,1,1,1,1,1,
1,4),(84.8230016469244,85.6743652428538,86.6718703290774,87.669375415301,
88.6668805015246,89.6643855877482,90.6618906739717,91.106186954104),
 .UNSPECIFIED.);
#1936=B_SPLINE_CURVE_WITH_KNOTS('',3,(#81348,#81349,#81350,#81351,#81352,
#81353,#81354,#81355,#81356,#81357),.UNSPECIFIED.,.F.,.F.,(4,1,1,1,1,1,
1,4),(84.8230016469244,85.221261248847,86.2187663350706,87.2162714212942,
88.2137765075178,89.2112815937414,90.208786679965,91.106186954104),
 .UNSPECIFIED.);
#1937=B_SPLINE_CURVE_WITH_KNOTS('',3,(#81362,#81363,#81364,#81365,#81366,
#81367,#81368,#81369,#81370,#81371,#81372),.UNSPECIFIED.,.F.,.F.,(4,1,1,
1,1,1,1,1,4),(78.5398163397448,78.6918296392886,79.6893347255122,80.6868398117358,
81.6843448979594,82.681849984183,83.6793550704066,84.6768601566302,84.8230016469244),
 .UNSPECIFIED.);
#1938=B_SPLINE_CURVE_WITH_KNOTS('',3,(#81373,#81374,#81375,#81376,#81377,
#81378,#81379,#81380,#81381,#81382),.UNSPECIFIED.,.F.,.F.,(4,1,1,1,1,1,
1,4),(78.5398163397448,79.2362307315055,80.233735817729,81.2312409039526,
82.2287459901762,83.2262510763998,84.2237561626234,84.8230016469244),
 .UNSPECIFIED.);
#1939=B_SPLINE_CURVE_WITH_KNOTS('',3,(#81387,#81388,#81389,#81390,#81391,
#81392,#81393,#81394,#81395,#81396),.UNSPECIFIED.,.F.,.F.,(4,1,1,1,1,1,
1,4),(72.2566310325652,72.706799121947,73.7043042081706,74.7018092943942,
75.6993143806178,76.6968194668414,77.694324553065,78.5398163397448),
 .UNSPECIFIED.);
#1940=B_SPLINE_CURVE_WITH_KNOTS('',3,(#81397,#81398,#81399,#81400,#81401,
#81402,#81403,#81404,#81405,#81406),.UNSPECIFIED.,.F.,.F.,(4,1,1,1,1,1,
1,4),(72.2566310325652,73.2512002141639,74.2487053003875,75.2462103866111,
76.2437154728347,77.2412205590583,78.2387256452818,78.5398163397448),
 .UNSPECIFIED.);
#1941=B_SPLINE_CURVE_WITH_KNOTS('',3,(#81411,#81412,#81413,#81414,#81415,
#81416,#81417,#81418,#81419,#81420),.UNSPECIFIED.,.F.,.F.,(4,1,1,1,1,1,
1,4),(65.9734457253856,66.7217686046055,67.7192736908291,68.7167787770527,
69.7142838632763,70.7117889494998,71.7092940357234,72.2566310325652),
 .UNSPECIFIED.);
#1942=B_SPLINE_CURVE_WITH_KNOTS('',3,(#81421,#81422,#81423,#81424,#81425,
#81426,#81427,#81428,#81429,#81430,#81431),.UNSPECIFIED.,.F.,.F.,(4,1,1,
1,1,1,1,1,4),(65.9734457253856,66.2686646105987,67.2661696968223,68.2636747830459,
69.2611798692695,70.2586849554931,71.2561900417167,72.2536951279403,72.2566310325652),
 .UNSPECIFIED.);
#1943=B_SPLINE_CURVE_WITH_KNOTS('',3,(#81436,#81437,#81438,#81439,#81440,
#81441,#81442,#81443,#81444,#81445,#81446),.UNSPECIFIED.,.F.,.F.,(4,1,1,
1,1,1,1,1,4),(59.690260418206,59.7392330010403,60.7367380872639,61.7342431734875,
62.7317482597111,63.7292533459347,64.7267584321583,65.7242635183819,65.9734457253856),
 .UNSPECIFIED.);
#1944=B_SPLINE_CURVE_WITH_KNOTS('',3,(#81447,#81448,#81449,#81450,#81451,
#81452,#81453,#81454,#81455,#81456),.UNSPECIFIED.,.F.,.F.,(4,1,1,1,1,1,
1,4),(59.690260418206,60.2836340932571,61.2811391794807,62.2786442657043,
63.2761493519279,64.2736544381515,65.2711595243751,65.9734457253856),
 .UNSPECIFIED.);
#1945=B_SPLINE_CURVE_WITH_KNOTS('',3,(#81461,#81462,#81463,#81464,#81465,
#81466,#81467,#81468,#81469,#81470),.UNSPECIFIED.,.F.,.F.,(4,1,1,1,1,1,
1,4),(53.4070751110264,53.7542024836987,54.7517075699223,55.7492126561459,
56.7467177423695,57.7442228285931,58.7417279148167,59.690260418206),
 .UNSPECIFIED.);
#1946=B_SPLINE_CURVE_WITH_KNOTS('',3,(#81471,#81472,#81473,#81474,#81475,
#81476,#81477,#81478,#81479,#81480),.UNSPECIFIED.,.F.,.F.,(4,1,1,1,1,1,
1,4),(53.4070751110264,54.2986035759156,55.2961086621392,56.2936137483628,
57.2911188345864,58.28862392081,59.2861290070336,59.690260418206),
 .UNSPECIFIED.);
#1947=B_SPLINE_CURVE_WITH_KNOTS('',3,(#81485,#81486,#81487,#81488,#81489,
#81490,#81491,#81492,#81493,#81494),.UNSPECIFIED.,.F.,.F.,(4,1,1,1,1,1,
1,4),(47.1238898038468,47.7691719663572,48.7666770525807,49.7641821388043,
50.7616872250279,51.7591923112515,52.7566973974751,53.4070751110264),
 .UNSPECIFIED.);
#1948=B_SPLINE_CURVE_WITH_KNOTS('',3,(#81495,#81496,#81497,#81498,#81499,
#81500,#81501,#81502,#81503,#81504,#81505),.UNSPECIFIED.,.F.,.F.,(4,1,1,
1,1,1,1,1,4),(47.1238898038468,47.3160679723504,48.313573058574,49.3110781447976,
50.3085832310212,51.3060883172448,52.3035934034684,53.301098489692,53.4070751110264),
 .UNSPECIFIED.);
#1949=B_SPLINE_CURVE_WITH_KNOTS('',3,(#81510,#81511,#81512,#81513,#81514,
#81515,#81516,#81517,#81518,#81519),.UNSPECIFIED.,.F.,.F.,(4,1,1,1,1,1,
1,4),(40.8407044966672,41.7841414490156,42.7816465352392,43.7791516214628,
44.7766567076864,45.77416179391,46.7716668801336,47.1238898038468),
 .UNSPECIFIED.);
#1950=B_SPLINE_CURVE_WITH_KNOTS('',3,(#81520,#81521,#81522,#81523,#81524,
#81525,#81526,#81527,#81528,#81529),.UNSPECIFIED.,.F.,.F.,(4,1,1,1,1,1,
1,4),(40.8407044966673,41.3310374550088,42.3285425412324,43.326047627456,
44.3235527136796,45.3210577999032,46.3185628861268,47.1238898038468),
 .UNSPECIFIED.);
#1951=B_SPLINE_CURVE_WITH_KNOTS('',3,(#81534,#81535,#81536,#81537,#81538,
#81539,#81540,#81541,#81542,#81543,#81544),.UNSPECIFIED.,.F.,.F.,(4,1,1,
1,1,1,1,1,4),(34.5575191894876,34.8016058454504,35.799110931674,36.7966160178976,
37.7941211041212,38.7916261903448,39.7891312765684,40.786636362792,40.8407044966672),
 .UNSPECIFIED.);
#1952=B_SPLINE_CURVE_WITH_KNOTS('',3,(#81545,#81546,#81547,#81548,#81549,
#81550,#81551,#81552,#81553,#81554),.UNSPECIFIED.,.F.,.F.,(4,1,1,1,1,1,
1,4),(34.5575191894877,35.3460069376673,36.3435120238909,37.3410171101145,
38.3385221963381,39.3360272825616,40.3335323687852,40.8407044966673),
 .UNSPECIFIED.);
#1953=B_SPLINE_CURVE_WITH_KNOTS('',3,(#81559,#81560,#81561,#81562,#81563,
#81564,#81565,#81566,#81567,#81568),.UNSPECIFIED.,.F.,.F.,(4,1,1,1,1,1,
1,4),(28.274333882308,28.8165753281089,29.8140804143324,30.811585500556,
31.8090905867796,32.8065956730032,33.8041007592268,34.5575191894876),
 .UNSPECIFIED.);
#1954=B_SPLINE_CURVE_WITH_KNOTS('',3,(#81569,#81570,#81571,#81572,#81573,
#81574,#81575,#81576,#81577,#81578,#81579),.UNSPECIFIED.,.F.,.F.,(4,1,1,
1,1,1,1,1,4),(28.2743338823081,28.3634713341021,29.3609764203257,30.3584815065493,
31.3559865927729,32.3534916789965,33.3509967652201,34.3485018514437,34.5575191894877),
 .UNSPECIFIED.);
#1955=B_SPLINE_CURVE_WITH_KNOTS('',3,(#81584,#81585,#81586,#81587,#81588,
#81589,#81590,#81591,#81592,#81593),.UNSPECIFIED.,.F.,.F.,(4,1,1,1,1,1,
1,4),(21.9911485751285,22.8315448107673,23.8290498969909,24.8265549832145,
25.8240600694381,26.8215651556617,27.8190702418853,28.274333882308),
 .UNSPECIFIED.);
#1956=B_SPLINE_CURVE_WITH_KNOTS('',3,(#81594,#81595,#81596,#81597,#81598,
#81599,#81600,#81601,#81602,#81603),.UNSPECIFIED.,.F.,.F.,(4,1,1,1,1,1,
1,4),(21.9911485751285,22.3784408167605,23.3759459029841,24.3734509892077,
25.3709560754313,26.3684611616549,27.3659662478785,28.2743338823081),
 .UNSPECIFIED.);
#1957=B_SPLINE_CURVE_WITH_KNOTS('',3,(#81609,#81610,#81611,#81612,#81613),
 .UNSPECIFIED.,.F.,.F.,(4,1,4),(14.3984001269718,15.3959052131954,15.7079632679489),
 .UNSPECIFIED.);
#1958=B_SPLINE_CURVE_WITH_KNOTS('',3,(#81616,#81617,#81618,#81619,#81620),
 .UNSPECIFIED.,.F.,.F.,(4,1,4),(13.8759337553362,14.8515041209785,15.7079632679489),
 .UNSPECIFIED.);
#1959=B_SPLINE_CURVE_WITH_KNOTS('',3,(#81622,#81623,#81624,#81625,#81626,
#81627,#81628,#81629,#81630,#81631,#81632),.UNSPECIFIED.,.F.,.F.,(4,1,1,
1,1,1,1,1,4),(15.7079632679489,15.8490092072021,16.8465142934257,17.8440193796493,
18.8415244658729,19.8390295520965,20.8365346383201,21.8340397245437,21.9911485751285),
 .UNSPECIFIED.);
#1960=B_SPLINE_CURVE_WITH_KNOTS('',3,(#81633,#81634,#81635,#81636,#81637,
#81638,#81639,#81640,#81641,#81642),.UNSPECIFIED.,.F.,.F.,(4,1,1,1,1,1,
1,4),(15.7079632679489,16.393410299419,17.3909153856426,18.3884204718662,
19.3859255580897,20.3834306443133,21.3809357305369,21.9911485751285),
 .UNSPECIFIED.);
#1961=B_SPLINE_CURVE_WITH_KNOTS('',3,(#82167,#82168,#82169,#82170,#82171,
#82172,#82173,#82174,#82175,#82176,#82177,#82178,#82179,#82180,#82181,#82182,
#82183,#82184,#82185,#82186,#82187,#82188,#82189,#82190,#82191,#82192,#82193,
#82194,#82195,#82196,#82197,#82198,#82199,#82200,#82201,#82202,#82203,#82204,
#82205,#82206,#82207,#82208,#82209,#82210,#82211,#82212,#82213,#82214,#82215,
#82216,#82217,#82218,#82219,#82220,#82221,#82222,#82223,#82224,#82225,#82226,
#82227,#82228,#82229,#82230,#82231,#82232,#82233,#82234,#82235,#82236,#82237,
#82238,#82239,#82240,#82241,#82242,#82243,#82244,#82245,#82246,#82247,#82248,
#82249,#82250,#82251,#82252,#82253,#82254,#82255,#82256,#82257,#82258,#82259,
#82260),.UNSPECIFIED.,.F.,.F.,(4,3,3,3,3,3,3,3,3,3,3,3,3,3,3,3,3,3,3,3,
3,3,3,3,3,3,3,3,3,3,3,4),(0.,0.0297230920696365,0.060107320285424,0.0895195747239277,
0.115255297357618,0.120660678709402,0.150423453169379,0.180022111707072,
0.208867922728668,0.221306013693075,0.229868731119957,0.234141593208093,
0.262685293208723,0.290598240531792,0.295405355793454,0.324357010294601,
0.334002571891444,0.339561520558749,0.343329583411178,0.371420199829295,
0.399566425708994,0.427315118725961,0.438104957742258,0.444429055894153,
0.449092671597708,0.477735779253812,0.499218109995891,0.505823880640041,
0.512084154674993,0.538002247703493,0.563665102222126,0.569248610399162),
 .UNSPECIFIED.);
#1962=B_SPLINE_CURVE_WITH_KNOTS('',3,(#82261,#82262,#82263,#82264,#82265,
#82266,#82267,#82268,#82269,#82270,#82271,#82272,#82273,#82274,#82275,#82276,
#82277,#82278,#82279,#82280,#82281,#82282,#82283,#82284,#82285,#82286,#82287,
#82288,#82289,#82290,#82291,#82292,#82293,#82294,#82295,#82296,#82297,#82298,
#82299,#82300,#82301,#82302,#82303,#82304,#82305,#82306,#82307,#82308,#82309,
#82310,#82311,#82312,#82313,#82314,#82315,#82316,#82317,#82318,#82319,#82320,
#82321,#82322,#82323,#82324,#82325,#82326,#82327,#82328,#82329,#82330,#82331,
#82332,#82333,#82334,#82335,#82336,#82337,#82338,#82339,#82340,#82341,#82342,
#82343,#82344,#82345,#82346,#82347,#82348,#82349,#82350,#82351,#82352,#82353,
#82354),.UNSPECIFIED.,.F.,.F.,(4,3,3,3,3,3,3,3,3,3,3,3,3,3,3,3,3,3,3,3,
3,3,3,3,3,3,3,3,3,3,3,4),(0.,0.0253621307813173,0.0513960159531074,0.0783235863046206,
0.0901043983334076,0.0965513395257098,0.102699668506175,0.130003032742825,
0.157757927018835,0.185022589955429,0.195825015771935,0.202226748487186,
0.206464577520137,0.235066962137,0.263572732749935,0.266816578765213,0.29472472571341,
0.305720896315937,0.310511082927085,0.314321197018662,0.342377239119157,
0.371487374222168,0.40093453850437,0.42163088746293,0.426693903714044,0.456743080020748,
0.482584342224751,0.492084926665187,0.49816865914989,0.529138393993325,
0.560108128836759,0.566847306048098),.UNSPECIFIED.);
#1963=B_SPLINE_CURVE_WITH_KNOTS('',3,(#82355,#82356,#82357,#82358,#82359,
#82360,#82361,#82362,#82363,#82364,#82365,#82366,#82367,#82368,#82369,#82370,
#82371,#82372,#82373,#82374,#82375,#82376,#82377,#82378,#82379),
 .UNSPECIFIED.,.F.,.F.,(4,3,3,3,3,3,3,3,4),(-10.1321597128207,-9.97505086223596,
-8.97754577601236,-7.98004068978877,-6.98253560356517,-5.98503051734157,
-4.98752543111798,-3.99002034489438,-3.84897440564113),.UNSPECIFIED.);
#1964=B_SPLINE_CURVE_WITH_KNOTS('',3,(#82904,#82905,#82906,#82907,#82908,
#82909,#82910,#82911,#82912,#82913,#82914,#82915,#82916,#82917,#82918,#82919,
#82920,#82921,#82922,#82923,#82924,#82925,#82926,#82927,#82928,#82929,#82930,
#82931,#82932,#82933,#82934,#82935,#82936,#82937,#82938,#82939,#82940,#82941,
#82942,#82943,#82944,#82945,#82946,#82947,#82948,#82949,#82950,#82951,#82952,
#82953,#82954,#82955,#82956,#82957,#82958,#82959,#82960,#82961,#82962,#82963,
#82964,#82965,#82966,#82967,#82968,#82969,#82970,#82971,#82972,#82973,#82974,
#82975,#82976,#82977,#82978,#82979,#82980,#82981,#82982,#82983,#82984,#82985,
#82986,#82987,#82988,#82989,#82990,#82991,#82992,#82993,#82994,#82995,#82996,
#82997),.UNSPECIFIED.,.F.,.F.,(4,3,3,3,3,3,3,3,3,3,3,3,3,3,3,3,3,3,3,3,
3,3,3,3,3,3,3,3,3,3,3,4),(0.,0.0253621358123242,0.0513960255360089,0.0783235946896633,
0.0901044061943871,0.096551342870137,0.102699667472934,0.130003035212993,
0.157757931226256,0.185022593111003,0.195825016620202,0.202226749482005,
0.206464578172652,0.23506696366167,0.263572732773266,0.266816578765244,
0.294724723356824,0.305720891161005,0.310511051384319,0.314321165540805,
0.342377203317934,0.371487336243674,0.400934499931709,0.421630800975239,
0.426693905360061,0.456743080929668,0.482584342906447,0.492084927719568,
0.498168658941421,0.529138393889102,0.560108128836783,0.56684730604811),
 .UNSPECIFIED.);
#1965=B_SPLINE_CURVE_WITH_KNOTS('',3,(#82998,#82999,#83000,#83001,#83002,
#83003,#83004,#83005,#83006,#83007,#83008,#83009,#83010,#83011,#83012,#83013,
#83014,#83015,#83016,#83017,#83018,#83019),.UNSPECIFIED.,.F.,.F.,(4,3,3,
3,3,3,3,4),(7.59274844815659,7.98004068978876,8.97754577601235,9.97505086223595,
10.9725559484595,11.9700610346831,12.9675661209067,13.8759337553362),
 .UNSPECIFIED.);
#1966=B_SPLINE_CURVE_WITH_KNOTS('',3,(#83020,#83021,#83022,#83023,#83024,
#83025,#83026,#83027,#83028,#83029,#83030,#83031,#83032,#83033,#83034,#83035,
#83036,#83037,#83038,#83039,#83040,#83041,#83042,#83043,#83044,#83045,#83046,
#83047,#83048,#83049,#83050,#83051,#83052,#83053,#83054,#83055,#83056,#83057,
#83058,#83059,#83060,#83061,#83062,#83063,#83064,#83065,#83066,#83067,#83068,
#83069,#83070,#83071,#83072,#83073,#83074,#83075,#83076,#83077,#83078,#83079,
#83080,#83081,#83082,#83083,#83084,#83085,#83086,#83087,#83088,#83089,#83090,
#83091,#83092,#83093,#83094,#83095,#83096,#83097,#83098,#83099,#83100,#83101,
#83102,#83103,#83104,#83105,#83106,#83107,#83108,#83109,#83110,#83111,#83112,
#83113),.UNSPECIFIED.,.F.,.F.,(4,3,3,3,3,3,3,3,3,3,3,3,3,3,3,3,3,3,3,3,
3,3,3,3,3,3,3,3,3,3,3,4),(0.,0.0297230962841146,0.0601073265980457,0.0895195802474777,
0.115255302190731,0.120660679792265,0.150423454314909,0.180022111713584,
0.208867922733564,0.221306013172714,0.229868724984429,0.234141588316278,
0.262685287083846,0.290598233431208,0.295405355793502,0.324357010515701,
0.334002571531716,0.339561519177542,0.343329581677685,0.371420198215134,
0.399566424158773,0.427315116346681,0.438104952273844,0.444429615489231,
0.449093069854903,0.477736077946735,0.499218334015609,0.505825295727651,
0.512084636520009,0.538002720680382,0.56366510222223,0.569248610399263),
 .UNSPECIFIED.);
#1967=B_SPLINE_CURVE_WITH_KNOTS('',3,(#83123,#83124,#83125,#83126,#83127,
#83128,#83129,#83130,#83131,#83132,#83133,#83134,#83135,#83136,#83137,#83138,
#83139,#83140,#83141,#83142,#83143,#83144,#83145,#83146,#83147,#83148,#83149,
#83150,#83151,#83152,#83153,#83154,#83155,#83156,#83157,#83158,#83159,#83160,
#83161,#83162,#83163,#83164,#83165,#83166,#83167,#83168,#83169,#83170,#83171,
#83172,#83173,#83174,#83175,#83176,#83177,#83178,#83179,#83180,#83181,#83182,
#83183,#83184,#83185,#83186,#83187,#83188,#83189,#83190,#83191,#83192,#83193,
#83194,#83195,#83196,#83197,#83198,#83199,#83200,#83201,#83202,#83203,#83204,
#83205,#83206,#83207,#83208,#83209,#83210,#83211,#83212,#83213,#83214,#83215,
#83216),.UNSPECIFIED.,.F.,.F.,(4,3,3,3,3,3,3,3,3,3,3,3,3,3,3,3,3,3,3,3,
3,3,3,3,3,3,3,3,3,3,3,4),(0.,0.0253579125993778,0.0513879730614739,0.078316548774439,
0.0900978006488612,0.096548549645776,0.10270053274012,0.130000942709176,
0.157754349497768,0.185019906814624,0.195824290931949,0.202225875665695,
0.206464010191211,0.235065614019142,0.263572590767915,0.266816578765194,
0.294726657909301,0.305725121816185,0.310537053618177,0.314348115889946,
0.342407723431573,0.37151966691571,0.400967327702673,0.42170458042185,0.426696514650315,
0.456746347586265,0.48258679289888,0.492091395740311,0.498168674804682,
0.529138401820704,0.560108128836725,0.566847306048067),.UNSPECIFIED.);
#1968=B_SPLINE_CURVE_WITH_KNOTS('',3,(#83217,#83218,#83219,#83220,#83221,
#83222,#83223,#83224,#83225,#83226,#83227,#83228,#83229,#83230,#83231,#83232,
#83233,#83234,#83235,#83236,#83237,#83238,#83239,#83240,#83241,#83242,#83243,
#83244,#83245,#83246,#83247,#83248,#83249,#83250,#83251,#83252,#83253,#83254,
#83255,#83256,#83257,#83258,#83259,#83260,#83261,#83262,#83263,#83264,#83265,
#83266,#83267,#83268,#83269,#83270,#83271,#83272,#83273,#83274,#83275,#83276,
#83277,#83278,#83279,#83280,#83281,#83282,#83283,#83284,#83285,#83286,#83287,
#83288,#83289,#83290,#83291,#83292,#83293,#83294,#83295,#83296,#83297,#83298,
#83299,#83300,#83301,#83302,#83303,#83304,#83305,#83306,#83307,#83308,#83309,
#83310),.UNSPECIFIED.,.F.,.F.,(4,3,3,3,3,3,3,3,3,3,3,3,3,3,3,3,3,3,3,3,
3,3,3,3,3,3,3,3,3,3,3,4),(0.,0.0297195669091192,0.0601020231284386,0.0895149397115918,
0.115251241721851,0.120659860690465,0.150422557383199,0.180022130955462,
0.208867937165012,0.221306452872675,0.229873833252823,0.234145682630168,
0.262690377679548,0.290604115247869,0.295405355793664,0.324356811547779,
0.334002824582243,0.339562575308007,0.343331007503921,0.371421512409186,
0.399567651381716,0.427316966374198,0.438109225720769,0.444058097014762,
0.44893104271735,0.47761455759364,0.499127193750858,0.50770469889405,0.513577910280885,
0.539477043608626,0.56366510222251,0.569248610399544),.UNSPECIFIED.);
#1969=B_SPLINE_CURVE_WITH_KNOTS('',3,(#83311,#83312,#83313,#83314,#83315,
#83316,#83317,#83318,#83319,#83320,#83321,#83322,#83323,#83324,#83325,#83326,
#83327,#83328,#83329,#83330,#83331,#83332,#83333,#83334,#83335,#83336,#83337,
#83338,#83339,#83340,#83341,#83342,#83343,#83344,#83345,#83346,#83347,#83348,
#83349,#83350,#83351,#83352,#83353,#83354,#83355,#83356,#83357,#83358,#83359,
#83360,#83361,#83362,#83363,#83364,#83365,#83366,#83367,#83368,#83369,#83370,
#83371,#83372,#83373,#83374,#83375,#83376,#83377,#83378,#83379,#83380,#83381,
#83382,#83383,#83384,#83385,#83386,#83387,#83388,#83389,#83390,#83391,#83392,
#83393,#83394,#83395,#83396,#83397,#83398,#83399,#83400,#83401,#83402,#83403,
#83404),.UNSPECIFIED.,.F.,.F.,(4,3,3,3,3,3,3,3,3,3,3,3,3,3,3,3,3,3,3,3,
3,3,3,3,3,3,3,3,3,3,3,4),(0.,0.0253579295510885,0.0513880054150265,0.0783165770837972,
0.0900978271888843,0.0965485607956795,0.102700529268948,0.13000095118214,
0.157754364082486,0.185019917753162,0.195824293899418,0.202225879318517,
0.206464012585979,0.235065619713782,0.263572591829656,0.266816578765192,
0.294726650343867,0.305725105274476,0.31053695159628,0.314348006525504,
0.342407600038078,0.371519536354756,0.400967195164478,0.421704281841331,
0.426696487776643,0.45674631791978,0.482586770649004,0.492091339583941,
0.498168675460501,0.529138402148588,0.560108128836676,0.566847306048011),
 .UNSPECIFIED.);
#1970=B_SPLINE_CURVE_WITH_KNOTS('',3,(#83405,#83406,#83407,#83408,#83409,
#83410,#83411,#83412,#83413,#83414,#83415,#83416,#83417,#83418,#83419,#83420,
#83421,#83422,#83423,#83424,#83425,#83426,#83427,#83428,#83429,#83430,#83431,
#83432,#83433,#83434,#83435,#83436,#83437,#83438,#83439,#83440,#83441,#83442,
#83443,#83444,#83445,#83446,#83447,#83448,#83449,#83450,#83451,#83452,#83453,
#83454,#83455,#83456,#83457,#83458,#83459,#83460,#83461,#83462,#83463,#83464,
#83465,#83466,#83467,#83468,#83469,#83470,#83471,#83472,#83473,#83474,#83475,
#83476,#83477,#83478,#83479,#83480,#83481,#83482,#83483,#83484,#83485,#83486,
#83487,#83488,#83489,#83490,#83491,#83492,#83493,#83494,#83495,#83496,#83497,
#83498),.UNSPECIFIED.,.F.,.F.,(4,3,3,3,3,3,3,3,3,3,3,3,3,3,3,3,3,3,3,3,
3,3,3,3,3,3,3,3,3,3,3,4),(0.,0.0297195615165264,0.0601020150014339,0.0895149326004449,
0.115251235499579,0.120659859449144,0.150422555982469,0.180022130905293,
0.20886793712735,0.221306453444634,0.229873839859354,0.2341456879374,0.26269038447235,
0.290604123217553,0.295405355793521,0.324356811216375,0.334002824878165,
0.339562576600837,0.343331009278728,0.371421513989523,0.399567652778866,
0.427316968616493,0.43810923101463,0.444057706366695,0.448930977598555,
0.47761450875452,0.499127157121493,0.507704470575279,0.513577860048999,
0.53947699656382,0.563665102222413,0.569248610399444),.UNSPECIFIED.);
#1971=B_SPLINE_CURVE_WITH_KNOTS('',3,(#83499,#83500,#83501,#83502,#83503,
#83504,#83505,#83506,#83507,#83508,#83509,#83510,#83511,#83512,#83513,#83514,
#83515,#83516,#83517,#83518,#83519,#83520,#83521,#83522,#83523,#83524,#83525,
#83526,#83527,#83528,#83529,#83530,#83531,#83532,#83533,#83534,#83535,#83536,
#83537,#83538,#83539,#83540,#83541,#83542,#83543,#83544,#83545,#83546,#83547,
#83548,#83549,#83550,#83551,#83552,#83553,#83554,#83555,#83556,#83557,#83558,
#83559,#83560,#83561,#83562,#83563,#83564,#83565,#83566,#83567,#83568,#83569,
#83570,#83571,#83572,#83573,#83574,#83575,#83576,#83577,#83578,#83579,#83580,
#83581,#83582,#83583,#83584,#83585,#83586,#83587,#83588,#83589,#83590,#83591,
#83592),.UNSPECIFIED.,.F.,.F.,(4,3,3,3,3,3,3,3,3,3,3,3,3,3,3,3,3,3,3,3,
3,3,3,3,3,3,3,3,3,3,3,4),(0.,0.0253579233504778,0.0513879935816182,0.078316566729565,
0.0900978174817918,0.0965485567174404,0.102700530547917,0.130000948093196,
0.157754358758536,0.1850199137602,0.195824292816032,0.202225877982008,0.206464011702015,
0.235065617622659,0.263572591433621,0.266816578765193,0.294726653110754,
0.305725111324118,0.310536988839073,0.314348046434504,0.342407645075261,
0.371519584011882,0.400967243544213,0.421704390831952,0.426696497574283,
0.456746328737469,0.482586778762282,0.492091360063141,0.498168675247584,
0.529138402042152,0.560108128836719,0.56684730604806),.UNSPECIFIED.);
#1972=B_SPLINE_CURVE_WITH_KNOTS('',3,(#83593,#83594,#83595,#83596,#83597,
#83598,#83599,#83600,#83601,#83602,#83603,#83604,#83605,#83606,#83607,#83608,
#83609,#83610,#83611,#83612,#83613,#83614,#83615,#83616,#83617,#83618,#83619,
#83620,#83621,#83622,#83623,#83624,#83625,#83626,#83627,#83628,#83629,#83630,
#83631,#83632,#83633,#83634,#83635,#83636,#83637,#83638,#83639,#83640,#83641,
#83642,#83643,#83644,#83645,#83646,#83647,#83648,#83649,#83650,#83651,#83652,
#83653,#83654,#83655,#83656,#83657,#83658,#83659,#83660,#83661,#83662,#83663,
#83664,#83665,#83666,#83667,#83668,#83669,#83670,#83671,#83672,#83673,#83674,
#83675,#83676,#83677,#83678,#83679,#83680,#83681,#83682,#83683,#83684,#83685,
#83686),.UNSPECIFIED.,.F.,.F.,(4,3,3,3,3,3,3,3,3,3,3,3,3,3,3,3,3,3,3,3,
3,3,3,3,3,3,3,3,3,3,3,4),(0.,0.02971955658432,0.0601020075682883,0.0895149260964493,
0.11525122980859,0.120659858309036,0.150422554696353,0.180022130854125,
0.208867937088988,0.221306453963038,0.229873845849775,0.234145692673294,
0.262690390567024,0.290604130388979,0.295405355793577,0.324356810915373,
0.334002825153036,0.339562577828411,0.343331010981896,0.371421515515497,
0.39956765413632,0.427316970744013,0.438109236017469,0.444057339059148,
0.448930916434902,0.47761446288177,0.49912712271692,0.507704256104763,0.513577812862897,
0.53947695230609,0.563665102222372,0.569248610399409),.UNSPECIFIED.);
#1973=B_SPLINE_CURVE_WITH_KNOTS('',3,(#83687,#83688,#83689,#83690,#83691,
#83692,#83693,#83694,#83695,#83696,#83697,#83698,#83699,#83700,#83701,#83702,
#83703,#83704,#83705,#83706,#83707,#83708,#83709,#83710,#83711,#83712,#83713,
#83714,#83715,#83716,#83717,#83718,#83719,#83720,#83721,#83722,#83723,#83724,
#83725,#83726,#83727,#83728,#83729,#83730,#83731,#83732,#83733,#83734,#83735,
#83736,#83737,#83738,#83739,#83740,#83741,#83742,#83743,#83744,#83745,#83746,
#83747,#83748,#83749,#83750,#83751,#83752,#83753,#83754,#83755,#83756,#83757,
#83758,#83759,#83760,#83761,#83762,#83763,#83764,#83765,#83766,#83767,#83768,
#83769,#83770,#83771,#83772,#83773,#83774,#83775,#83776,#83777,#83778,#83779,
#83780),.UNSPECIFIED.,.F.,.F.,(4,3,3,3,3,3,3,3,3,3,3,3,3,3,3,3,3,3,3,3,
3,3,3,3,3,3,3,3,3,3,3,4),(0.,0.0253579177000947,0.0513879827971935,0.0783165572931898,
0.0900978086351882,0.096548553000782,0.10270053169639,0.130000945260459,
0.15775435388846,0.185019910107636,0.195824291825238,0.202225876764932,
0.206464010941052,0.235065615761965,0.263572591116789,0.266816578765164,
0.294726655632965,0.305725116839123,0.310537022942245,0.314348082986944,
0.342407686307513,0.371519627634975,0.400967287826622,0.421704490588119,
0.42669650652894,0.456746338622913,0.482586786176388,0.492091378775912,
0.49816867504133,0.529138401939073,0.560108128836816,0.566847306048155),
 .UNSPECIFIED.);
#1974=B_SPLINE_CURVE_WITH_KNOTS('',3,(#83781,#83782,#83783,#83784,#83785,
#83786,#83787,#83788,#83789,#83790,#83791,#83792,#83793,#83794,#83795,#83796,
#83797,#83798,#83799,#83800,#83801,#83802,#83803,#83804,#83805,#83806,#83807,
#83808,#83809,#83810,#83811,#83812,#83813,#83814,#83815,#83816,#83817,#83818,
#83819,#83820,#83821,#83822,#83823,#83824,#83825,#83826,#83827,#83828,#83829,
#83830,#83831,#83832,#83833,#83834,#83835,#83836,#83837,#83838,#83839,#83840,
#83841,#83842,#83843,#83844,#83845,#83846,#83847,#83848,#83849,#83850,#83851,
#83852,#83853,#83854,#83855,#83856,#83857,#83858,#83859,#83860,#83861,#83862,
#83863,#83864,#83865,#83866,#83867,#83868,#83869,#83870,#83871,#83872,#83873,
#83874),.UNSPECIFIED.,.F.,.F.,(4,3,3,3,3,3,3,3,3,3,3,3,3,3,3,3,3,3,3,3,
3,3,3,3,3,3,3,3,3,3,3,4),(0.,0.0297195727594163,0.0601020319440672,0.0895149474252613,
0.115251248471306,0.120659862032104,0.150422558897904,0.180022131005185,
0.208867937202294,0.221306452247928,0.229873826038458,0.234145676897509,
0.262690370335612,0.290604106627827,0.29540535579362,0.32435681190214,0.334002824250451,
0.339562573810048,0.343331005503615,0.371421510618914,0.399567649790246,
0.427316963867809,0.43810921982249,0.444058531569151,0.448931115602164,
0.477614612257223,0.499127234748518,0.507704954507689,0.513577966546108,
0.539477096392581,0.563665102222402,0.569248610399436),.UNSPECIFIED.);
#1975=B_SPLINE_CURVE_WITH_KNOTS('',3,(#83875,#83876,#83877,#83878,#83879,
#83880,#83881,#83882,#83883,#83884,#83885,#83886,#83887,#83888,#83889,#83890,
#83891,#83892,#83893,#83894,#83895,#83896,#83897,#83898,#83899,#83900,#83901,
#83902,#83903,#83904,#83905,#83906,#83907,#83908,#83909,#83910,#83911,#83912,
#83913,#83914,#83915,#83916,#83917,#83918,#83919,#83920,#83921,#83922,#83923,
#83924,#83925,#83926,#83927,#83928,#83929,#83930,#83931,#83932,#83933,#83934,
#83935,#83936,#83937,#83938,#83939,#83940,#83941,#83942,#83943,#83944,#83945,
#83946,#83947,#83948,#83949,#83950,#83951,#83952,#83953,#83954,#83955,#83956,
#83957,#83958,#83959,#83960,#83961,#83962,#83963,#83964,#83965,#83966,#83967,
#83968),.UNSPECIFIED.,.F.,.F.,(4,3,3,3,3,3,3,3,3,3,3,3,3,3,3,3,3,3,3,3,
3,3,3,3,3,3,3,3,3,3,3,4),(0.,0.0253621238738449,0.051396002794732,0.078323574791042,
0.0901043875394277,0.0965513349313581,0.102699669924291,0.130003029352741,
0.157757921246207,0.185022585625959,0.195825014607035,0.202226747115019,
0.206464576640171,0.235066960042815,0.263572732714624,0.266816578765213,
0.294724728954443,0.305720903404729,0.310511126288789,0.314321240463125,
0.34237728851459,0.371487426613087,0.400934591712638,0.421631006765666,
0.426693901339546,0.456743078656559,0.482584341201609,0.492084925019561,
0.498168659606258,0.529138394221508,0.560108128836759,0.566847306048098),
 .UNSPECIFIED.);
#1976=B_SPLINE_CURVE_WITH_KNOTS('',3,(#83969,#83970,#83971,#83972,#83973,
#83974,#83975,#83976,#83977,#83978,#83979,#83980,#83981,#83982,#83983,#83984,
#83985,#83986,#83987,#83988,#83989,#83990,#83991,#83992,#83993,#83994,#83995,
#83996,#83997,#83998,#83999,#84000,#84001,#84002,#84003,#84004,#84005,#84006,
#84007,#84008,#84009,#84010,#84011,#84012,#84013,#84014,#84015,#84016,#84017,
#84018,#84019,#84020,#84021,#84022,#84023,#84024,#84025,#84026,#84027,#84028,
#84029,#84030,#84031,#84032,#84033,#84034,#84035,#84036,#84037,#84038,#84039,
#84040,#84041,#84042,#84043,#84044,#84045,#84046,#84047,#84048,#84049,#84050,
#84051,#84052,#84053,#84054,#84055,#84056,#84057,#84058,#84059,#84060,#84061,
#84062),.UNSPECIFIED.,.F.,.F.,(4,3,3,3,3,3,3,3,3,3,3,3,3,3,3,3,3,3,3,3,
3,3,3,3,3,3,3,3,3,3,3,4),(0.,0.0297231029452647,0.0601073365800704,0.0895195889817508,
0.115255309833221,0.120660681336277,0.15042345595793,0.18002211156947,0.208867922625481,
0.221306012212383,0.22986871379436,0.23414157933724,0.262685276183272,0.290598221000729,
0.295405355793514,0.324357010860702,0.334002570950606,0.339561516830048,
0.34332957848535,0.371420195205431,0.399566421251306,0.427315112131658,
0.438104942680454,0.444430605284565,0.449093775635353,0.477736607282077,
0.49921873101712,0.505827805964956,0.512085493792728,0.538003562612052,
0.56366510222225,0.569248610399281),.UNSPECIFIED.);
#1977=B_SPLINE_CURVE_WITH_KNOTS('',3,(#84064,#84065,#84066,#84067,#84068,
#84069,#84070,#84071,#84072,#84073,#84074),.UNSPECIFIED.,.F.,.F.,(4,1,1,
1,1,1,1,1,4),(15.7079632679489,15.8490092072021,16.8465142934257,17.8440193796493,
18.8415244658729,19.8390295520965,20.8365346383201,21.8340397245437,21.9911485751285),
 .UNSPECIFIED.);
#1978=B_SPLINE_CURVE_WITH_KNOTS('',3,(#84075,#84076,#84077,#84078,#84079,
#84080,#84081,#84082,#84083,#84084),.UNSPECIFIED.,.F.,.F.,(4,1,1,1,1,1,
1,4),(15.7079632679489,16.3934102994189,17.3909153856425,18.3884204718661,
19.3859255580897,20.3834306443133,21.3809357305369,21.9911485751285),
 .UNSPECIFIED.);
#1979=B_SPLINE_CURVE_WITH_KNOTS('',3,(#84609,#84610,#84611,#84612,#84613,
#84614,#84615,#84616,#84617,#84618,#84619,#84620,#84621,#84622,#84623,#84624,
#84625,#84626,#84627,#84628,#84629,#84630,#84631,#84632,#84633,#84634,#84635,
#84636,#84637,#84638,#84639,#84640,#84641,#84642,#84643,#84644,#84645,#84646,
#84647,#84648,#84649,#84650,#84651,#84652,#84653,#84654,#84655,#84656,#84657,
#84658,#84659,#84660,#84661,#84662,#84663,#84664,#84665,#84666,#84667,#84668,
#84669,#84670,#84671,#84672,#84673,#84674,#84675,#84676,#84677,#84678,#84679,
#84680,#84681,#84682,#84683,#84684,#84685,#84686,#84687,#84688,#84689,#84690,
#84691,#84692,#84693,#84694,#84695,#84696,#84697,#84698,#84699,#84700,#84701,
#84702),.UNSPECIFIED.,.F.,.F.,(4,3,3,3,3,3,3,3,3,3,3,3,3,3,3,3,3,3,3,3,
3,3,3,3,3,3,3,3,3,3,3,4),(0.,0.029719553462866,0.0601020028625436,0.0895149219789189,
0.115251226205747,0.120659857597101,0.150422553890565,0.180022130829953,
0.208867937070851,0.221306454298592,0.229873849718833,0.234145695936532,
0.262690394687643,0.290604135187481,0.295405355793546,0.324356810724873,
0.334002825327806,0.339562578752343,0.343331012311981,0.37142151673717,
0.39956765525167,0.427316972340056,0.438109239708711,0.44405706477218,0.448930870596609,
0.477614428503011,0.499127096932812,0.507704095272053,0.513577777440086,
0.539476918814607,0.563665102222215,0.569248610399244),.UNSPECIFIED.);
#1980=B_SPLINE_CURVE_WITH_KNOTS('',3,(#84703,#84704,#84705,#84706,#84707,
#84708,#84709,#84710,#84711,#84712,#84713,#84714,#84715,#84716,#84717,#84718,
#84719,#84720,#84721,#84722,#84723,#84724,#84725,#84726,#84727),
 .UNSPECIFIED.,.F.,.F.,(4,3,3,3,3,3,3,3,4),(-10.1321597128207,-9.97505086223594,
-8.97754577601236,-7.98004068978876,-6.98253560356516,-5.98503051734157,
-4.98752543111798,-3.99002034489438,-3.84897440564114),.UNSPECIFIED.);
#1981=B_SPLINE_CURVE_WITH_KNOTS('',3,(#85252,#85253,#85254,#85255,#85256,
#85257,#85258,#85259,#85260,#85261,#85262,#85263,#85264,#85265,#85266,#85267,
#85268,#85269,#85270,#85271,#85272,#85273,#85274,#85275,#85276,#85277,#85278,
#85279,#85280,#85281,#85282,#85283,#85284,#85285,#85286,#85287,#85288,#85289,
#85290,#85291,#85292,#85293,#85294,#85295,#85296,#85297,#85298,#85299,#85300,
#85301,#85302,#85303,#85304,#85305,#85306,#85307,#85308,#85309,#85310,#85311,
#85312,#85313,#85314,#85315,#85316,#85317,#85318,#85319,#85320,#85321,#85322,
#85323,#85324,#85325,#85326,#85327,#85328,#85329,#85330,#85331,#85332,#85333,
#85334,#85335,#85336,#85337,#85338,#85339,#85340,#85341,#85342,#85343,#85344,
#85345),.UNSPECIFIED.,.F.,.F.,(4,3,3,3,3,3,3,3,3,3,3,3,3,3,3,3,3,3,3,3,
3,3,3,3,3,3,3,3,3,3,3,4),(0.,0.0253579406450752,0.0513880265848102,0.0783165956073515,
0.0900978445547133,0.0965485680929113,0.102700527035756,0.130000956771981,
0.157754373672949,0.185019924945997,0.19582429585153,0.202225881705843,
0.206464013995299,0.235065623259909,0.26357259234097,0.26681657876514,0.294726645398039,
0.305725094458983,0.31053688482791,0.314347935050642,0.342407519392621,
0.371519451018736,0.400967108531887,0.42170408668503,0.426696470332184,
0.456746298642485,0.48258675619102,0.492091303088876,0.498168676068964,
0.529138402452796,0.560108128836627,0.566847306047961),.UNSPECIFIED.);
#1982=B_SPLINE_CURVE_WITH_KNOTS('',3,(#85346,#85347,#85348,#85349,#85350,
#85351,#85352,#85353,#85354,#85355,#85356,#85357,#85358,#85359,#85360,#85361,
#85362,#85363,#85364,#85365,#85366,#85367),.UNSPECIFIED.,.F.,.F.,(4,3,3,
3,3,3,3,4),(7.5927484481566,7.98004068978877,8.97754577601236,9.97505086223596,
10.9725559484596,11.9700610346831,12.9675661209067,13.8759337553362),
 .UNSPECIFIED.);
#1983=B_SPLINE_CURVE_WITH_KNOTS('',3,(#85369,#85370,#85371,#85372,#85373,
#85374,#85375,#85376,#85377,#85378,#85379),.UNSPECIFIED.,.F.,.F.,(4,1,1,
1,1,1,1,1,4),(15.7079632679489,15.8490092072021,16.8465142934257,17.8440193796493,
18.8415244658729,19.8390295520965,20.8365346383201,21.8340397245437,21.9911485751285),
 .UNSPECIFIED.);
#1984=B_SPLINE_CURVE_WITH_KNOTS('',3,(#85380,#85381,#85382,#85383,#85384,
#85385,#85386,#85387,#85388,#85389),.UNSPECIFIED.,.F.,.F.,(4,1,1,1,1,1,
1,4),(15.7079632679489,16.393410299419,17.3909153856426,18.3884204718662,
19.3859255580897,20.3834306443133,21.3809357305369,21.9911485751285),
 .UNSPECIFIED.);
#1985=B_SPLINE_CURVE_WITH_KNOTS('',3,(#85914,#85915,#85916,#85917,#85918,
#85919,#85920,#85921,#85922,#85923,#85924,#85925,#85926,#85927,#85928,#85929,
#85930,#85931,#85932,#85933,#85934,#85935,#85936,#85937,#85938,#85939,#85940,
#85941,#85942,#85943,#85944,#85945,#85946,#85947,#85948,#85949,#85950,#85951,
#85952,#85953,#85954,#85955,#85956,#85957,#85958,#85959,#85960,#85961,#85962,
#85963,#85964,#85965,#85966,#85967,#85968,#85969,#85970,#85971,#85972,#85973,
#85974,#85975,#85976,#85977,#85978,#85979,#85980,#85981,#85982,#85983,#85984,
#85985,#85986,#85987,#85988,#85989,#85990,#85991,#85992,#85993,#85994,#85995,
#85996,#85997,#85998,#85999,#86000,#86001,#86002,#86003,#86004,#86005,#86006,
#86007),.UNSPECIFIED.,.F.,.F.,(4,3,3,3,3,3,3,3,3,3,3,3,3,3,3,3,3,3,3,3,
3,3,3,3,3,3,3,3,3,3,3,4),(0.,0.0297195582152991,0.0601020100219757,0.0895149282434353,
0.115251231687213,0.120659858671462,0.150422555105996,0.180022130855786,
0.208867937090253,0.221306453778133,0.229873843701529,0.234145691059075,
0.262690388500622,0.290604127966643,0.295405355793653,0.324356811014206,
0.334002825060996,0.33956257734427,0.343331010204372,0.371421514794185,
0.399567653472246,0.427316969833453,0.43810923392799,0.444057492748723,
0.448930941962885,0.477614482027788,0.499127137076466,0.50770434571683,
0.51357783260646,0.539476971024577,0.563665102222498,0.569248610399526),
 .UNSPECIFIED.);
#1986=B_SPLINE_CURVE_WITH_KNOTS('',3,(#86008,#86009,#86010,#86011,#86012,
#86013,#86014,#86015,#86016,#86017,#86018,#86019,#86020,#86021,#86022,#86023,
#86024,#86025,#86026,#86027,#86028,#86029,#86030,#86031,#86032),
 .UNSPECIFIED.,.F.,.F.,(4,3,3,3,3,3,3,3,4),(-10.1321597128207,-9.97505086223596,
-8.97754577601236,-7.98004068978876,-6.98253560356516,-5.98503051734157,
-4.98752543111797,-3.99002034489438,-3.84897440564114),.UNSPECIFIED.);
#1987=B_SPLINE_CURVE_WITH_KNOTS('',3,(#86557,#86558,#86559,#86560,#86561,
#86562,#86563,#86564,#86565,#86566,#86567,#86568,#86569,#86570,#86571,#86572,
#86573,#86574,#86575,#86576,#86577,#86578,#86579,#86580,#86581,#86582,#86583,
#86584,#86585,#86586,#86587,#86588,#86589,#86590,#86591,#86592,#86593,#86594,
#86595,#86596,#86597,#86598,#86599,#86600,#86601,#86602,#86603,#86604,#86605,
#86606,#86607,#86608,#86609,#86610,#86611,#86612,#86613,#86614,#86615,#86616,
#86617,#86618,#86619,#86620,#86621,#86622,#86623,#86624,#86625,#86626,#86627,
#86628,#86629,#86630,#86631,#86632,#86633,#86634,#86635,#86636,#86637,#86638,
#86639,#86640,#86641,#86642,#86643,#86644,#86645,#86646,#86647,#86648,#86649,
#86650),.UNSPECIFIED.,.F.,.F.,(4,3,3,3,3,3,3,3,3,3,3,3,3,3,3,3,3,3,3,3,
3,3,3,3,3,3,3,3,3,3,3,4),(0.,0.0253579214134435,0.0513879898823703,0.0783165634927302,
0.0900978144472627,0.0965485554423931,0.10270053085291,0.130000947031645,
0.157754356995756,0.18501991243813,0.19582429245781,0.202225877564684,0.206464011401675,
0.235065616933209,0.263572591275628,0.26681657876525,0.294726653975806,
0.305725113216564,0.310537000090899,0.314348058459022,0.342407658669726,
0.371519598417381,0.400967258172793,0.421704423796584,0.42669650037878,
0.456746331848251,0.482586781095382,0.492091365967282,0.498168675056121,
0.529138401946449,0.560108128836777,0.56684730604809),.UNSPECIFIED.);
#1988=B_SPLINE_CURVE_WITH_KNOTS('',3,(#86651,#86652,#86653,#86654,#86655,
#86656,#86657,#86658,#86659,#86660,#86661,#86662,#86663,#86664,#86665,#86666,
#86667,#86668,#86669,#86670,#86671,#86672),.UNSPECIFIED.,.F.,.F.,(4,3,3,
3,3,3,3,4),(7.5927484481566,7.98004068978878,8.97754577601237,9.97505086223597,
10.9725559484596,11.9700610346831,12.9675661209067,13.8759337553362),
 .UNSPECIFIED.);
#1989=B_SPLINE_CURVE_WITH_KNOTS('',3,(#86674,#86675,#86676,#86677,#86678,
#86679,#86680,#86681,#86682,#86683,#86684),.UNSPECIFIED.,.F.,.F.,(4,1,1,
1,1,1,1,1,4),(15.7079632679489,15.8490092072021,16.8465142934257,17.8440193796493,
18.8415244658729,19.8390295520965,20.8365346383201,21.8340397245437,21.9911485751285),
 .UNSPECIFIED.);
#1990=B_SPLINE_CURVE_WITH_KNOTS('',3,(#86685,#86686,#86687,#86688,#86689,
#86690,#86691,#86692,#86693,#86694),.UNSPECIFIED.,.F.,.F.,(4,1,1,1,1,1,
1,4),(15.7079632679489,16.393410299419,17.3909153856426,18.3884204718662,
19.3859255580897,20.3834306443133,21.3809357305369,21.9911485751285),
 .UNSPECIFIED.);
#1991=B_SPLINE_CURVE_WITH_KNOTS('',3,(#87219,#87220,#87221,#87222,#87223,
#87224,#87225,#87226,#87227,#87228,#87229,#87230,#87231,#87232,#87233,#87234,
#87235,#87236,#87237,#87238,#87239,#87240,#87241,#87242,#87243,#87244,#87245,
#87246,#87247,#87248,#87249,#87250,#87251,#87252,#87253,#87254,#87255,#87256,
#87257,#87258,#87259,#87260,#87261,#87262,#87263,#87264,#87265,#87266,#87267,
#87268,#87269,#87270,#87271,#87272,#87273,#87274,#87275,#87276,#87277,#87278,
#87279,#87280,#87281,#87282,#87283,#87284,#87285,#87286,#87287,#87288,#87289,
#87290,#87291,#87292,#87293,#87294,#87295,#87296,#87297,#87298,#87299,#87300,
#87301,#87302,#87303,#87304,#87305,#87306,#87307,#87308,#87309,#87310,#87311,
#87312),.UNSPECIFIED.,.F.,.F.,(4,3,3,3,3,3,3,3,3,3,3,3,3,3,3,3,3,3,3,3,
3,3,3,3,3,3,3,3,3,3,3,4),(0.,0.0297195634297971,0.0601020178864358,0.089514935124822,
0.11525123770841,0.120659859971453,0.150422556566061,0.180022131006724,
0.208867937203424,0.221306453316953,0.229873838332913,0.234145686845126,
0.262690382844274,0.290604121164851,0.295405355793526,0.324356811328018,
0.334002824758734,0.33956257605137,0.343331008699606,0.371421513479927,
0.399567652332435,0.427316967866253,0.438109229229592,0.444057835021416,
0.448930999083887,0.477614524868509,0.499127169206975,0.507704545860101,
0.513577876601892,0.539477012001364,0.563665102222374,0.569248610399403),
 .UNSPECIFIED.);
#1992=B_SPLINE_CURVE_WITH_KNOTS('',3,(#87313,#87314,#87315,#87316,#87317,
#87318,#87319,#87320,#87321,#87322,#87323,#87324,#87325,#87326,#87327,#87328,
#87329,#87330,#87331,#87332,#87333,#87334,#87335,#87336,#87337),
 .UNSPECIFIED.,.F.,.F.,(4,3,3,3,3,3,3,3,4),(-10.1321597128207,-9.97505086223594,
-8.97754577601235,-7.98004068978876,-6.98253560356516,-5.98503051734157,
-4.98752543111797,-3.99002034489438,-3.84897440564117),.UNSPECIFIED.);
#1993=B_SPLINE_CURVE_WITH_KNOTS('',3,(#87862,#87863,#87864,#87865,#87866,
#87867,#87868,#87869,#87870,#87871,#87872,#87873,#87874,#87875,#87876,#87877,
#87878,#87879,#87880,#87881,#87882,#87883,#87884,#87885,#87886,#87887,#87888,
#87889,#87890,#87891,#87892,#87893,#87894,#87895,#87896,#87897,#87898,#87899,
#87900,#87901,#87902,#87903,#87904,#87905,#87906,#87907,#87908,#87909,#87910,
#87911,#87912,#87913,#87914,#87915,#87916,#87917,#87918,#87919,#87920,#87921,
#87922,#87923,#87924,#87925,#87926,#87927,#87928,#87929,#87930,#87931,#87932,
#87933,#87934,#87935,#87936,#87937,#87938,#87939,#87940,#87941,#87942,#87943,
#87944,#87945,#87946,#87947,#87948,#87949,#87950,#87951,#87952,#87953,#87954,
#87955),.UNSPECIFIED.,.F.,.F.,(4,3,3,3,3,3,3,3,3,3,3,3,3,3,3,3,3,3,3,3,
3,3,3,3,3,3,3,3,3,3,3,4),(0.,0.025357927272923,0.0513880010661254,0.0783165732785213,
0.0900978236214444,0.0965485592962299,0.10270052975136,0.130000950059032,
0.157754362139206,0.185019916295728,0.195824293504795,0.202225878835774,
0.206464012200268,0.235065618877475,0.263572591616992,0.266816578765292,
0.294726651357313,0.305725107490194,0.310536965130431,0.31434802098446,
0.342407616366947,0.371519553641245,0.400967212719098,0.421704321387406,
0.426696491317579,0.456746321829517,0.482586773581365,0.492091346987436,
0.498168675113734,0.52913840197532,0.560108128836907,0.566847306048237),
 .UNSPECIFIED.);
#1994=B_SPLINE_CURVE_WITH_KNOTS('',3,(#87956,#87957,#87958,#87959,#87960,
#87961,#87962,#87963,#87964,#87965,#87966,#87967,#87968,#87969,#87970,#87971,
#87972,#87973,#87974,#87975,#87976,#87977),.UNSPECIFIED.,.F.,.F.,(4,3,3,
3,3,3,3,4),(7.59274844815661,7.98004068978877,8.97754577601236,9.97505086223595,
10.9725559484595,11.9700610346831,12.9675661209067,13.8759337553362),
 .UNSPECIFIED.);
#1995=B_SPLINE_CURVE_WITH_KNOTS('',3,(#87979,#87980,#87981,#87982,#87983,
#87984,#87985,#87986,#87987,#87988,#87989),.UNSPECIFIED.,.F.,.F.,(4,1,1,
1,1,1,1,1,4),(15.7079632679489,15.8490092072021,16.8465142934256,17.8440193796492,
18.8415244658728,19.8390295520964,20.83653463832,21.8340397245436,21.9911485751285),
 .UNSPECIFIED.);
#1996=B_SPLINE_CURVE_WITH_KNOTS('',3,(#87990,#87991,#87992,#87993,#87994,
#87995,#87996,#87997,#87998,#87999),.UNSPECIFIED.,.F.,.F.,(4,1,1,1,1,1,
1,4),(15.7079632679489,16.3934102994189,17.3909153856425,18.3884204718661,
19.3859255580897,20.3834306443133,21.3809357305369,21.9911485751285),
 .UNSPECIFIED.);
#1997=B_SPLINE_CURVE_WITH_KNOTS('',3,(#88524,#88525,#88526,#88527,#88528,
#88529,#88530,#88531,#88532,#88533,#88534,#88535,#88536,#88537,#88538,#88539,
#88540,#88541,#88542,#88543,#88544,#88545,#88546,#88547,#88548,#88549,#88550,
#88551,#88552,#88553,#88554,#88555,#88556,#88557,#88558,#88559,#88560,#88561,
#88562,#88563,#88564,#88565,#88566,#88567,#88568,#88569,#88570,#88571,#88572,
#88573,#88574,#88575,#88576,#88577,#88578,#88579,#88580,#88581,#88582,#88583,
#88584,#88585,#88586,#88587,#88588,#88589,#88590,#88591,#88592,#88593,#88594,
#88595,#88596,#88597,#88598,#88599,#88600,#88601,#88602,#88603,#88604,#88605,
#88606,#88607,#88608,#88609,#88610,#88611,#88612,#88613,#88614,#88615,#88616,
#88617),.UNSPECIFIED.,.F.,.F.,(4,3,3,3,3,3,3,3,3,3,3,3,3,3,3,3,3,3,3,3,
3,3,3,3,3,3,3,3,3,3,3,4),(0.,0.0297195491700754,0.0601019963903511,0.0895149163157588,
0.11525122125049,0.120659856525908,0.150422552697531,0.180022130709648,
0.208867936980639,0.221306454680905,0.229873854178296,0.234145699383138,
0.262690399330253,0.290604140778558,0.295405355793612,0.324356810461168,
0.334002825560677,0.339562579599788,0.343331013402581,0.371421517667901,
0.399567656038419,0.427316973809471,0.438109243258802,0.444056806999033,
0.448930828212018,0.477614396714627,0.499127073091584,0.507703946830402,
0.513577744863538,0.539476888668399,0.563665102222456,0.569248610399499),
 .UNSPECIFIED.);
#1998=B_SPLINE_CURVE_WITH_KNOTS('',3,(#88618,#88619,#88620,#88621,#88622,
#88623,#88624,#88625,#88626,#88627,#88628,#88629,#88630,#88631,#88632,#88633,
#88634,#88635,#88636,#88637,#88638,#88639,#88640,#88641,#88642),
 .UNSPECIFIED.,.F.,.F.,(4,3,3,3,3,3,3,3,4),(-10.1321597128208,-9.97505086223595,
-8.97754577601236,-7.98004068978876,-6.98253560356516,-5.98503051734157,
-4.98752543111797,-3.99002034489437,-3.8489744056412),.UNSPECIFIED.);
#1999=B_SPLINE_CURVE_WITH_KNOTS('',3,(#89167,#89168,#89169,#89170,#89171,
#89172,#89173,#89174,#89175,#89176,#89177,#89178,#89179,#89180,#89181,#89182,
#89183,#89184,#89185,#89186,#89187,#89188,#89189,#89190,#89191,#89192,#89193,
#89194,#89195,#89196,#89197,#89198,#89199,#89200,#89201,#89202,#89203,#89204,
#89205,#89206,#89207,#89208,#89209,#89210,#89211,#89212,#89213,#89214,#89215,
#89216,#89217,#89218,#89219,#89220,#89221,#89222,#89223,#89224,#89225,#89226,
#89227,#89228,#89229,#89230,#89231,#89232,#89233,#89234,#89235,#89236,#89237,
#89238,#89239,#89240,#89241,#89242,#89243,#89244,#89245,#89246,#89247,#89248,
#89249,#89250,#89251,#89252,#89253,#89254,#89255,#89256,#89257,#89258,#89259,
#89260),.UNSPECIFIED.,.F.,.F.,(4,3,3,3,3,3,3,3,3,3,3,3,3,3,3,3,3,3,3,3,
3,3,3,3,3,3,3,3,3,3,3,4),(0.,0.0253579336883674,0.0513880133105813,0.0783165839924162,
0.0900978336657191,0.0965485635161028,0.102700528459906,0.130000953296085,
0.157754367684311,0.185019920454548,0.195824294631711,0.202225880214181,
0.206464013245021,0.235065621182224,0.263572592161767,0.266816578765261,
0.294726648497761,0.305725101238404,0.310536926466407,0.314347979466994,
0.342407569538569,0.371519504099032,0.400967162424359,0.421704208089393,
0.426696481095096,0.456746310536251,0.482586765111401,0.492091325612755,
0.498168675511062,0.529138402173956,0.56010812883685,0.566847306048169),
 .UNSPECIFIED.);
#2000=B_SPLINE_CURVE_WITH_KNOTS('',3,(#89261,#89262,#89263,#89264,#89265,
#89266,#89267,#89268,#89269,#89270,#89271,#89272,#89273,#89274,#89275,#89276,
#89277,#89278,#89279,#89280,#89281,#89282),.UNSPECIFIED.,.F.,.F.,(4,3,3,
3,3,3,3,4),(7.59274844815666,7.98004068978876,8.97754577601236,9.97505086223596,
10.9725559484595,11.9700610346831,12.9675661209067,13.8759337553362),
 .UNSPECIFIED.);
#2001=B_SPLINE_CURVE_WITH_KNOTS('',3,(#89284,#89285,#89286,#89287,#89288,
#89289,#89290,#89291,#89292,#89293,#89294),.UNSPECIFIED.,.F.,.F.,(4,1,1,
1,1,1,1,1,4),(15.7079632679489,15.8490092072021,16.8465142934257,17.8440193796493,
18.8415244658729,19.8390295520965,20.8365346383201,21.8340397245437,21.9911485751285),
 .UNSPECIFIED.);
#2002=B_SPLINE_CURVE_WITH_KNOTS('',3,(#89295,#89296,#89297,#89298,#89299,
#89300,#89301,#89302,#89303,#89304),.UNSPECIFIED.,.F.,.F.,(4,1,1,1,1,1,
1,4),(15.7079632679489,16.393410299419,17.3909153856426,18.3884204718662,
19.3859255580897,20.3834306443133,21.3809357305369,21.9911485751285),
 .UNSPECIFIED.);
#2003=B_SPLINE_CURVE_WITH_KNOTS('',3,(#89829,#89830,#89831,#89832,#89833,
#89834,#89835,#89836,#89837,#89838,#89839,#89840,#89841,#89842,#89843,#89844,
#89845,#89846,#89847,#89848,#89849,#89850,#89851,#89852,#89853,#89854,#89855,
#89856,#89857,#89858,#89859,#89860,#89861,#89862,#89863,#89864,#89865,#89866,
#89867,#89868,#89869,#89870,#89871,#89872,#89873,#89874,#89875,#89876,#89877,
#89878,#89879,#89880,#89881,#89882,#89883,#89884,#89885,#89886,#89887,#89888,
#89889,#89890,#89891,#89892,#89893,#89894,#89895,#89896,#89897,#89898,#89899,
#89900,#89901,#89902,#89903,#89904,#89905,#89906,#89907,#89908,#89909,#89910,
#89911,#89912,#89913,#89914,#89915,#89916,#89917,#89918,#89919,#89920,#89921,
#89922),.UNSPECIFIED.,.F.,.F.,(4,3,3,3,3,3,3,3,3,3,3,3,3,3,3,3,3,3,3,3,
3,3,3,3,3,3,3,3,3,3,3,4),(0.,0.0297230862766818,0.0601073115992879,0.0895195671235586,
0.115255290707296,0.120660677481967,0.150423451858438,0.180022111936673,
0.208867922900868,0.22130601462086,0.229868741866763,0.23414160178478,0.262685303441991,
0.290598252086167,0.295405355793454,0.324357009993761,0.334002572396988,
0.339561522550512,0.343329586354325,0.371420202614893,0.399566428404089,
0.42731512255639,0.438104966431693,0.444428160156713,0.4490920349478,0.477735301766382,
0.499217751880318,0.505821620193661,0.512083386782307,0.538001493461072,
0.563665102222126,0.569248610399162),.UNSPECIFIED.);
#2004=B_SPLINE_CURVE_WITH_KNOTS('',3,(#89923,#89924,#89925,#89926,#89927,
#89928,#89929,#89930,#89931,#89932,#89933,#89934,#89935,#89936,#89937,#89938,
#89939,#89940,#89941,#89942,#89943,#89944,#89945,#89946,#89947),
 .UNSPECIFIED.,.F.,.F.,(4,3,3,3,3,3,3,3,4),(-10.1321597128207,-9.97505086223596,
-8.97754577601236,-7.98004068978877,-6.98253560356517,-5.98503051734157,
-4.98752543111798,-3.99002034489438,-3.84897440564113),.UNSPECIFIED.);
#2005=B_SPLINE_CURVE_WITH_KNOTS('',3,(#90472,#90473,#90474,#90475,#90476,
#90477,#90478,#90479,#90480,#90481,#90482,#90483,#90484,#90485,#90486,#90487,
#90488,#90489,#90490,#90491,#90492,#90493,#90494,#90495,#90496,#90497,#90498,
#90499,#90500,#90501,#90502,#90503,#90504,#90505,#90506,#90507,#90508,#90509,
#90510,#90511,#90512,#90513,#90514,#90515,#90516,#90517,#90518,#90519,#90520,
#90521,#90522,#90523,#90524,#90525,#90526,#90527,#90528,#90529,#90530,#90531,
#90532,#90533,#90534,#90535,#90536,#90537,#90538,#90539,#90540,#90541,#90542,
#90543,#90544,#90545,#90546,#90547,#90548,#90549,#90550,#90551,#90552,#90553,
#90554,#90555,#90556,#90557,#90558,#90559,#90560,#90561,#90562,#90563,#90564,
#90565),.UNSPECIFIED.,.F.,.F.,(4,3,3,3,3,3,3,3,3,3,3,3,3,3,3,3,3,3,3,3,
3,3,3,3,3,3,3,3,3,3,3,4),(0.,0.0253621437511135,0.051396040655139,0.0783236079188992,
0.0901044185967943,0.096551348149287,0.102699665837524,0.130003039099533,
0.157757937849826,0.185022598078675,0.195825017956751,0.202226751064942,
0.206464579201341,0.235066966115335,0.263572732855357,0.266816578765221,
0.294724719624713,0.30572088299975,0.310511001289213,0.31432111535445,0.342377146267348,
0.371487275744893,0.400934438497277,0.421630663231168,0.426693908186306,
0.45674308258997,0.482584344151671,0.492084929769549,0.498168658059089,
0.529138393447932,0.560108128836774,0.566847306048129),.UNSPECIFIED.);
#2006=B_SPLINE_CURVE_WITH_KNOTS('',3,(#90566,#90567,#90568,#90569,#90570,
#90571,#90572,#90573,#90574,#90575,#90576,#90577,#90578,#90579,#90580,#90581,
#90582,#90583,#90584,#90585,#90586,#90587),.UNSPECIFIED.,.F.,.F.,(4,3,3,
3,3,3,3,4),(7.59274844815659,7.98004068978877,8.97754577601236,9.97505086223596,
10.9725559484595,11.9700610346831,12.9675661209067,13.8759337553362),
 .UNSPECIFIED.);
#2007=B_SPLINE_CURVE_WITH_KNOTS('',3,(#90617,#90618,#90619,#90620,#90621,
#90622,#90623,#90624,#90625,#90626),.UNSPECIFIED.,.F.,.F.,(4,3,3,4),(-4.09293042013064,
-3.99773706693635,-2.99830280020227,-2.06863817490912),.UNSPECIFIED.);
#2008=B_SPLINE_CURVE_WITH_KNOTS('',3,(#90629,#90630,#90631,#90632,#90633,
#90634,#90635),.UNSPECIFIED.,.F.,.F.,(4,3,4),(0.,0.999656463044431,1.11730040836905),
 .UNSPECIFIED.);
#2009=B_SPLINE_CURVE_WITH_KNOTS('',3,(#90640,#90641,#90642,#90643,#90644,
#90645,#90646,#90647,#90648,#90649,#90650,#90651,#90652,#90653,#90654,#90655,
#90656,#90657,#90658,#90659,#90660,#90661),.UNSPECIFIED.,.F.,.F.,(4,3,3,
3,3,3,3,4),(-10.3761157273102,-9.99434266734088,-8.99490840060679,-7.99547413387271,
-6.99603986713862,-5.99660560040453,-4.99717133367044,-4.09293042013064),
 .UNSPECIFIED.);
#2010=B_SPLINE_CURVE_WITH_KNOTS('',3,(#90662,#90663,#90664,#90665,#90666,
#90667,#90668,#90669,#90670,#90671,#90672,#90673,#90674,#90675,#90676,#90677,
#90678,#90679,#90680,#90681,#90682,#90683),.UNSPECIFIED.,.F.,.F.,(4,3,3,
3,3,3,3,4),(1.11730040836905,1.99931292608883,2.99896938913324,3.99862585217764,
4.99828231522204,5.99793877826645,6.99759524131085,7.40048571554864),
 .UNSPECIFIED.);
#2011=B_SPLINE_CURVE_WITH_KNOTS('',3,(#90688,#90689,#90690,#90691,#90692,
#90693,#90694,#90695,#90696,#90697,#90698,#90699,#90700,#90701,#90702,#90703,
#90704,#90705,#90706,#90707,#90708,#90709),.UNSPECIFIED.,.F.,.F.,(4,3,3,
3,3,3,3,4),(-16.6593010344898,-15.9909482677454,-14.9915140010113,-13.9920797342772,
-12.9926454675431,-11.9932112008091,-10.993776934075,-10.3761157273102),
 .UNSPECIFIED.);
#2012=B_SPLINE_CURVE_WITH_KNOTS('',3,(#90710,#90711,#90712,#90713,#90714,
#90715,#90716,#90717,#90718,#90719,#90720,#90721,#90722,#90723,#90724,#90725,
#90726,#90727,#90728,#90729,#90730,#90731),.UNSPECIFIED.,.F.,.F.,(4,3,3,
3,3,3,3,4),(7.40048571554864,7.99725170435527,8.99690816739968,9.99656463044411,
10.9962210934885,11.9958775565329,12.9955340195774,13.6836710227282),
 .UNSPECIFIED.);
#2013=B_SPLINE_CURVE_WITH_KNOTS('',3,(#90736,#90737,#90738,#90739,#90740,
#90741,#90742,#90743,#90744,#90745,#90746,#90747,#90748,#90749,#90750,#90751,
#90752,#90753,#90754,#90755,#90756,#90757),.UNSPECIFIED.,.F.,.F.,(4,3,3,
3,3,3,3,4),(-22.9424863416694,-21.9875538681499,-20.9881196014159,-19.9886853346818,
-18.9892510679477,-17.9898168012136,-16.9903825344795,-16.6593010344898),
 .UNSPECIFIED.);
#2014=B_SPLINE_CURVE_WITH_KNOTS('',3,(#90758,#90759,#90760,#90761,#90762,
#90763,#90764,#90765,#90766,#90767,#90768,#90769,#90770,#90771,#90772,#90773,
#90774,#90775,#90776,#90777,#90778,#90779),.UNSPECIFIED.,.F.,.F.,(4,3,3,
3,3,3,3,4),(13.6836710227282,13.9951904826218,14.9948469456662,15.9945034087106,
16.994159871755,17.9938163347994,18.9934727978439,19.9668563299078),
 .UNSPECIFIED.);
#2015=B_SPLINE_CURVE_WITH_KNOTS('',3,(#90784,#90785,#90786,#90787,#90788,
#90789,#90790,#90791,#90792,#90793,#90794,#90795,#90796,#90797,#90798,#90799,
#90800,#90801,#90802,#90803,#90804,#90805,#90806,#90807,#90808),
 .UNSPECIFIED.,.F.,.F.,(4,3,3,3,3,3,3,3,4),(-29.225671648849,-28.9835937352886,
-27.9841594685545,-26.9847252018204,-25.9852909350863,-24.9858566683522,
-23.9864224016181,-22.986988134884,-22.9424863416694),.UNSPECIFIED.);
#2016=B_SPLINE_CURVE_WITH_KNOTS('',3,(#90809,#90810,#90811,#90812,#90813,
#90814,#90815,#90816,#90817,#90818,#90819,#90820,#90821,#90822,#90823,#90824,
#90825,#90826,#90827,#90828,#90829,#90830,#90831,#90832,#90833),
 .UNSPECIFIED.,.F.,.F.,(4,3,3,3,3,3,3,3,4),(19.9668563299078,19.9931292608883,
20.9927857239327,21.9924421869771,22.9920986500215,23.9917551130659,24.9914115761103,
25.9910680391547,26.2500416370874),.UNSPECIFIED.);
#2017=B_SPLINE_CURVE_WITH_KNOTS('',3,(#90838,#90839,#90840,#90841,#90842,
#90843,#90844,#90845,#90846,#90847,#90848,#90849,#90850,#90851,#90852,#90853,
#90854,#90855,#90856,#90857,#90858,#90859),.UNSPECIFIED.,.F.,.F.,(4,3,3,
3,3,3,3,4),(-35.5088569560286,-34.9801993356931,-33.980765068959,-32.9813308022249,
-31.9818965354908,-30.9824622687567,-29.9830280020227,-29.225671648849),
 .UNSPECIFIED.);
#2018=B_SPLINE_CURVE_WITH_KNOTS('',3,(#90860,#90861,#90862,#90863,#90864,
#90865,#90866,#90867,#90868,#90869,#90870,#90871,#90872,#90873,#90874,#90875,
#90876,#90877,#90878,#90879,#90880,#90881),.UNSPECIFIED.,.F.,.F.,(4,3,3,
3,3,3,3,4),(26.2500416370874,26.9907245021991,27.9903809652435,28.990037428288,
29.9896938913324,30.9893503543768,31.9890068174212,32.533226944267),
 .UNSPECIFIED.);
#2019=B_SPLINE_CURVE_WITH_KNOTS('',3,(#90886,#90887,#90888,#90889,#90890,
#90891,#90892,#90893,#90894,#90895,#90896,#90897,#90898,#90899,#90900,#90901,
#90902,#90903,#90904,#90905,#90906,#90907),.UNSPECIFIED.,.F.,.F.,(4,3,3,
3,3,3,3,4),(-41.7920422632082,-40.9768049360976,-39.9773706693635,-38.9779364026294,
-37.9785021358954,-36.9790678691613,-35.9796336024272,-35.5088569560286),
 .UNSPECIFIED.);
#2020=B_SPLINE_CURVE_WITH_KNOTS('',3,(#90908,#90909,#90910,#90911,#90912,
#90913,#90914,#90915,#90916,#90917,#90918,#90919,#90920,#90921,#90922,#90923,
#90924,#90925,#90926,#90927,#90928,#90929),.UNSPECIFIED.,.F.,.F.,(4,3,3,
3,3,3,3,4),(32.533226944267,32.9886632804656,33.98831974351,34.9879762065544,
35.9876326695989,36.9872891326432,37.9869455956877,38.8164122514466),
 .UNSPECIFIED.);
#2021=B_SPLINE_CURVE_WITH_KNOTS('',3,(#90934,#90935,#90936,#90937,#90938,
#90939,#90940,#90941,#90942,#90943,#90944,#90945,#90946,#90947,#90948,#90949,
#90950,#90951,#90952,#90953,#90954,#90955,#90956,#90957,#90958),
 .UNSPECIFIED.,.F.,.F.,(4,3,3,3,3,3,3,3,4),(-48.0752275703878,-47.9728448032362,
-46.9734105365022,-45.9739762697681,-44.974542003034,-43.9751077362999,
-42.9756734695658,-41.9762392028317,-41.7920422632082),.UNSPECIFIED.);
#2022=B_SPLINE_CURVE_WITH_KNOTS('',3,(#90959,#90960,#90961,#90962,#90963,
#90964,#90965,#90966,#90967,#90968,#90969,#90970,#90971,#90972,#90973,#90974,
#90975,#90976,#90977,#90978,#90979,#90980,#90981,#90982,#90983),
 .UNSPECIFIED.,.F.,.F.,(4,3,3,3,3,3,3,3,4),(38.8164122514466,38.9866020587321,
39.9862585217765,40.9859149848209,41.9855714478653,42.9852279109097,43.9848843739542,
44.9845408369986,45.0995975586262),.UNSPECIFIED.);
#2023=B_SPLINE_CURVE_WITH_KNOTS('',3,(#90988,#90989,#90990,#90991,#90992,
#90993,#90994,#90995,#90996,#90997,#90998,#90999,#91000,#91001,#91002,#91003,
#91004,#91005,#91006,#91007,#91008,#91009),.UNSPECIFIED.,.F.,.F.,(4,3,3,
3,3,3,3,4),(-54.3584128775674,-53.9694504036408,-52.9700161369067,-51.9705818701726,
-50.9711476034385,-49.9717133367044,-48.9722790699703,-48.0752275703878),
 .UNSPECIFIED.);
#2024=B_SPLINE_CURVE_WITH_KNOTS('',3,(#91010,#91011,#91012,#91013,#91014,
#91015,#91016,#91017,#91018,#91019,#91020,#91021,#91022,#91023,#91024,#91025,
#91026,#91027,#91028,#91029,#91030,#91031),.UNSPECIFIED.,.F.,.F.,(4,3,3,
3,3,3,3,4),(45.0995975586262,45.984197300043,46.9838537630874,47.9835102261318,
48.9831666891762,49.9828231522206,50.982479615265,51.3827828658058),
 .UNSPECIFIED.);
#2025=B_SPLINE_CURVE_WITH_KNOTS('',3,(#91036,#91037,#91038,#91039,#91040,
#91041,#91042,#91043,#91044,#91045,#91046,#91047,#91048,#91049,#91050,#91051,
#91052,#91053,#91054,#91055,#91056,#91057),.UNSPECIFIED.,.F.,.F.,(4,3,3,
3,3,3,3,4),(-60.641598184747,-59.9660560040453,-58.9666217373112,-57.9671874705771,
-56.967753203843,-55.968318937109,-54.9688846703749,-54.3584128775674),
 .UNSPECIFIED.);
#2026=B_SPLINE_CURVE_WITH_KNOTS('',3,(#91058,#91059,#91060,#91061,#91062,
#91063,#91064,#91065,#91066,#91067,#91068,#91069,#91070,#91071,#91072,#91073,
#91074,#91075,#91076,#91077,#91078,#91079),.UNSPECIFIED.,.F.,.F.,(4,3,3,
3,3,3,3,4),(51.3827828658058,51.9821360783094,52.9817925413539,53.9814490043983,
54.9811054674427,55.9807619304871,56.9804183935315,57.6659681729854),
 .UNSPECIFIED.);
#2027=B_SPLINE_CURVE_WITH_KNOTS('',3,(#91084,#91085,#91086,#91087,#91088,
#91089,#91090,#91091,#91092,#91093,#91094,#91095,#91096,#91097,#91098,#91099,
#91100,#91101,#91102,#91103,#91104,#91105),.UNSPECIFIED.,.F.,.F.,(4,3,3,
3,3,3,3,4),(-66.9247834919265,-65.9626616044498,-64.9632273377157,-63.9637930709817,
-62.9643588042476,-61.9649245375135,-60.9654902707794,-60.641598184747),
 .UNSPECIFIED.);
#2028=B_SPLINE_CURVE_WITH_KNOTS('',3,(#91106,#91107,#91108,#91109,#91110,
#91111,#91112,#91113,#91114,#91115,#91116,#91117,#91118,#91119,#91120,#91121,
#91122,#91123,#91124,#91125,#91126,#91127),.UNSPECIFIED.,.F.,.F.,(4,3,3,
3,3,3,3,4),(57.6659681729854,57.980074856576,58.9797313196204,59.9793877826648,
60.9790442457092,61.9787007087536,62.978357171798,63.949153480165),
 .UNSPECIFIED.);
#2029=B_SPLINE_CURVE_WITH_KNOTS('',3,(#91132,#91133,#91134,#91135,#91136,
#91137,#91138,#91139,#91140,#91141,#91142,#91143,#91144,#91145,#91146,#91147,
#91148,#91149,#91150,#91151,#91152,#91153,#91154,#91155,#91156),
 .UNSPECIFIED.,.F.,.F.,(4,3,3,3,3,3,3,3,4),(-73.2079687991061,-72.9587014715884,
-71.9592672048544,-70.9598329381203,-69.9603986713862,-68.9609644046521,
-67.961530137918,-66.9620958711839,-66.9247834919265),.UNSPECIFIED.);
#2030=B_SPLINE_CURVE_WITH_KNOTS('',3,(#91157,#91158,#91159,#91160,#91161,
#91162,#91163,#91164,#91165,#91166,#91167,#91168,#91169,#91170,#91171,#91172,
#91173,#91174,#91175,#91176,#91177,#91178,#91179,#91180,#91181),
 .UNSPECIFIED.,.F.,.F.,(4,3,3,3,3,3,3,3,4),(63.949153480165,63.9780136348424,
64.9776700978868,65.9773265609312,66.9769830239756,67.9766394870201,68.9762959500645,
69.9759524131089,70.2323387873446),.UNSPECIFIED.);
#2031=B_SPLINE_CURVE_WITH_KNOTS('',3,(#91186,#91187,#91188,#91189,#91190,
#91191,#91192,#91193,#91194,#91195,#91196,#91197,#91198,#91199,#91200,#91201,
#91202,#91203,#91204,#91205,#91206,#91207),.UNSPECIFIED.,.F.,.F.,(4,3,3,
3,3,3,3,4),(-79.4911541062857,-78.955307071993,-77.9558728052589,-76.9564385385248,
-75.9570042717907,-74.9575700050566,-73.9581357383226,-73.2079687991061),
 .UNSPECIFIED.);
#2032=B_SPLINE_CURVE_WITH_KNOTS('',3,(#91208,#91209,#91210,#91211,#91212,
#91213,#91214,#91215,#91216,#91217,#91218,#91219,#91220,#91221,#91222,#91223,
#91224,#91225,#91226,#91227,#91228,#91229),.UNSPECIFIED.,.F.,.F.,(4,3,3,
3,3,3,3,4),(70.2323387873446,70.9756088761533,71.9752653391977,72.9749218022421,
73.9745782652865,74.9742347283309,75.9738911913753,76.5155240945241),
 .UNSPECIFIED.);
#2033=B_SPLINE_CURVE_WITH_KNOTS('',3,(#91234,#91235,#91236,#91237,#91238,
#91239,#91240,#91241,#91242,#91243,#91244,#91245,#91246,#91247,#91248,#91249,
#91250,#91251,#91252,#91253,#91254,#91255),.UNSPECIFIED.,.F.,.F.,(4,3,3,
3,3,3,3,4),(-85.7743394134653,-84.9519126723975,-83.9524784056634,-82.9530441389293,
-81.9536098721953,-80.9541756054612,-79.9547413387271,-79.4911541062857),
 .UNSPECIFIED.);
#2034=B_SPLINE_CURVE_WITH_KNOTS('',3,(#91256,#91257,#91258,#91259,#91260,
#91261,#91262,#91263,#91264,#91265,#91266,#91267,#91268,#91269,#91270,#91271,
#91272,#91273,#91274,#91275,#91276,#91277),.UNSPECIFIED.,.F.,.F.,(4,3,3,
3,3,3,3,4),(76.5155240945241,76.9735476544198,77.9732041174642,78.9728605805086,
79.972517043553,80.9721735065974,81.9718299696419,82.7987094017037),
 .UNSPECIFIED.);
#2035=B_SPLINE_CURVE_WITH_KNOTS('',3,(#91282,#91283,#91284,#91285,#91286,
#91287,#91288,#91289,#91290,#91291,#91292,#91293,#91294,#91295,#91296,#91297,
#91298,#91299,#91300,#91301,#91302,#91303,#91304,#91305,#91306),
 .UNSPECIFIED.,.F.,.F.,(4,3,3,3,3,3,3,3,4),(-92.0575247206449,-91.9479525395361,
-90.948518272802,-89.9490840060679,-88.9496497393339,-87.9502154725998,
-86.9507812058657,-85.9513469391316,-85.7743394134653),.UNSPECIFIED.);
#2036=B_SPLINE_CURVE_WITH_KNOTS('',3,(#91307,#91308,#91309,#91310,#91311,
#91312,#91313,#91314,#91315,#91316,#91317,#91318,#91319,#91320,#91321,#91322,
#91323,#91324,#91325,#91326,#91327,#91328,#91329,#91330,#91331),
 .UNSPECIFIED.,.F.,.F.,(4,3,3,3,3,3,3,3,4),(82.7987094017037,82.9714864326863,
83.9711428957307,84.9707993587751,85.9704558218195,86.9701122848639,87.9697687479083,
88.9694252109527,89.0818947088833),.UNSPECIFIED.);
#2037=B_SPLINE_CURVE_WITH_KNOTS('',3,(#91336,#91337,#91338,#91339,#91340,
#91341,#91342,#91343,#91344,#91345,#91346,#91347,#91348,#91349,#91350,#91351,
#91352,#91353,#91354,#91355,#91356,#91357),.UNSPECIFIED.,.F.,.F.,(4,3,3,
3,3,3,3,4),(-98.3407100278245,-97.9445581399407,-96.9451238732066,-95.9456896064725,
-94.9462553397384,-93.9468210730043,-92.9473868062702,-92.0575247206449),
 .UNSPECIFIED.);
#2038=B_SPLINE_CURVE_WITH_KNOTS('',3,(#91358,#91359,#91360,#91361,#91362,
#91363,#91364,#91365,#91366,#91367,#91368,#91369,#91370,#91371,#91372,#91373,
#91374,#91375,#91376,#91377,#91378,#91379),.UNSPECIFIED.,.F.,.F.,(4,3,3,
3,3,3,3,4),(89.0818947088833,89.9690816739971,90.9687381370416,91.968394600086,
92.9680510631304,93.9677075261748,94.9673639892192,95.3650800160629),
 .UNSPECIFIED.);
#2039=B_SPLINE_CURVE_WITH_KNOTS('',3,(#91384,#91385,#91386,#91387,#91388,
#91389,#91390,#91391,#91392,#91393,#91394,#91395,#91396,#91397,#91398,#91399,
#91400,#91401,#91402,#91403,#91404,#91405),.UNSPECIFIED.,.F.,.F.,(4,3,3,
3,3,3,3,4),(-104.623895335004,-103.941163740345,-102.941729473611,-101.942295206877,
-100.942860940143,-99.9434266734089,-98.9439924066748,-98.3407100278245),
 .UNSPECIFIED.);
#2040=B_SPLINE_CURVE_WITH_KNOTS('',3,(#91406,#91407,#91408,#91409,#91410,
#91411,#91412,#91413,#91414,#91415,#91416,#91417,#91418,#91419,#91420,#91421,
#91422,#91423,#91424,#91425,#91426,#91427),.UNSPECIFIED.,.F.,.F.,(4,3,3,
3,3,3,3,4),(95.3650800160629,95.9670204522636,96.966676915308,97.9663333783524,
98.9659898413969,99.9656463044413,100.965302767486,101.648265323242),
 .UNSPECIFIED.);
#2041=B_SPLINE_CURVE_WITH_KNOTS('',3,(#91432,#91433,#91434,#91435,#91436,
#91437,#91438,#91439,#91440,#91441,#91442,#91443,#91444,#91445,#91446,#91447,
#91448,#91449,#91450,#91451,#91452,#91453),.UNSPECIFIED.,.F.,.F.,(4,3,3,
3,3,3,3,4),(-110.907080642184,-109.93776934075,-108.938335074016,-107.938900807282,
-106.939466540547,-105.940032273813,-104.940598007079,-104.623895335004),
 .UNSPECIFIED.);
#2042=B_SPLINE_CURVE_WITH_KNOTS('',3,(#91454,#91455,#91456,#91457,#91458,
#91459,#91460,#91461,#91462,#91463,#91464,#91465,#91466,#91467,#91468,#91469,
#91470,#91471,#91472,#91473,#91474,#91475),.UNSPECIFIED.,.F.,.F.,(4,3,3,
3,3,3,3,4),(101.648265323242,101.96495923053,102.964615693575,103.964272156619,
104.963928619663,105.963585082708,106.963241545752,107.931450630422),
 .UNSPECIFIED.);
#2043=B_SPLINE_CURVE_WITH_KNOTS('',3,(#91480,#91481,#91482,#91483,#91484,
#91485,#91486,#91487,#91488,#91489,#91490,#91491,#91492,#91493,#91494,#91495,
#91496,#91497,#91498,#91499,#91500,#91501,#91502,#91503,#91504),
 .UNSPECIFIED.,.F.,.F.,(4,3,3,3,3,3,3,3,4),(-117.190265949363,-116.933809207888,
-115.934374941154,-114.93494067442,-113.935506407686,-112.936072140952,
-111.936637874218,-110.937203607484,-110.907080642184),.UNSPECIFIED.);
#2044=B_SPLINE_CURVE_WITH_KNOTS('',3,(#91505,#91506,#91507,#91508,#91509,
#91510,#91511,#91512,#91513,#91514,#91515,#91516,#91517,#91518,#91519,#91520,
#91521,#91522,#91523,#91524,#91525,#91526,#91527,#91528,#91529),
 .UNSPECIFIED.,.F.,.F.,(4,3,3,3,3,3,3,3,4),(107.931450630422,107.962898008797,
108.962554471841,109.962210934885,110.96186739793,111.961523860974,112.961180324019,
113.960836787063,114.214635937602),.UNSPECIFIED.);
#2045=B_SPLINE_CURVE_WITH_KNOTS('',3,(#91534,#91535,#91536,#91537,#91538,
#91539,#91540,#91541,#91542,#91543,#91544,#91545,#91546,#91547,#91548,#91549,
#91550,#91551,#91552,#91553,#91554,#91555),.UNSPECIFIED.,.F.,.F.,(4,3,3,
3,3,3,3,4),(-123.473451256543,-122.930414808293,-121.930980541559,-120.931546274825,
-119.932112008091,-118.932677741357,-117.933243474622,-117.190265949363),
 .UNSPECIFIED.);
#2046=B_SPLINE_CURVE_WITH_KNOTS('',3,(#91556,#91557,#91558,#91559,#91560,
#91561,#91562,#91563,#91564,#91565,#91566,#91567,#91568,#91569,#91570,#91571,
#91572,#91573,#91574,#91575,#91576,#91577),.UNSPECIFIED.,.F.,.F.,(4,3,3,
3,3,3,3,4),(114.214635937602,114.960493250107,115.960149713152,116.959806176196,
117.959462639241,118.959119102285,119.95877556533,120.497821244781),
 .UNSPECIFIED.);
#2047=B_SPLINE_CURVE_WITH_KNOTS('',3,(#91582,#91583,#91584,#91585,#91586,
#91587,#91588,#91589,#91590,#91591,#91592,#91593,#91594,#91595,#91596,#91597,
#91598,#91599,#91600,#91601,#91602,#91603),.UNSPECIFIED.,.F.,.F.,(4,3,3,
3,3,3,3,4),(-129.756636563722,-128.927020408697,-127.927586141963,-126.928151875229,
-125.928717608495,-124.929283341761,-123.929849075027,-123.473451256543),
 .UNSPECIFIED.);
#2048=B_SPLINE_CURVE_WITH_KNOTS('',3,(#91604,#91605,#91606,#91607,#91608,
#91609,#91610,#91611,#91612,#91613,#91614,#91615,#91616,#91617,#91618,#91619,
#91620,#91621,#91622,#91623,#91624,#91625),.UNSPECIFIED.,.F.,.F.,(4,3,3,
3,3,3,3,4),(120.497821244781,120.958432028374,121.958088491418,122.957744954463,
123.957401417507,124.957057880552,125.956714343596,126.781006551961),
 .UNSPECIFIED.);
#2049=B_SPLINE_CURVE_WITH_KNOTS('',3,(#91630,#91631,#91632,#91633,#91634,
#91635,#91636,#91637,#91638,#91639,#91640,#91641,#91642,#91643,#91644,#91645,
#91646,#91647,#91648,#91649,#91650,#91651,#91652,#91653,#91654),
 .UNSPECIFIED.,.F.,.F.,(4,3,3,3,3,3,3,3,4),(-136.039821870902,-135.923060275836,
-134.923626009102,-133.924191742368,-132.924757475634,-131.9253232089,-130.925888942166,
-129.926454675432,-129.756636563722),.UNSPECIFIED.);
#2050=B_SPLINE_CURVE_WITH_KNOTS('',3,(#91655,#91656,#91657,#91658,#91659,
#91660,#91661,#91662,#91663,#91664,#91665,#91666,#91667,#91668,#91669,#91670,
#91671,#91672,#91673,#91674,#91675,#91676,#91677,#91678,#91679),
 .UNSPECIFIED.,.F.,.F.,(4,3,3,3,3,3,3,3,4),(126.781006551961,126.95637080664,
127.956027269685,128.955683732729,129.955340195774,130.954996658818,131.954653121862,
132.954309584907,133.06419185914),.UNSPECIFIED.);
#2051=B_SPLINE_CURVE_WITH_KNOTS('',3,(#91684,#91685,#91686,#91687,#91688,
#91689,#91690,#91691,#91692,#91693,#91694,#91695,#91696,#91697,#91698,#91699,
#91700,#91701,#91702,#91703,#91704,#91705),.UNSPECIFIED.,.F.,.F.,(4,3,3,
3,3,3,3,4),(-142.323007178082,-141.919665876241,-140.920231609506,-139.920797342772,
-138.921363076038,-137.921928809304,-136.92249454257,-136.039821870902),
 .UNSPECIFIED.);
#2052=B_SPLINE_CURVE_WITH_KNOTS('',3,(#91706,#91707,#91708,#91709,#91710,
#91711,#91712,#91713,#91714,#91715,#91716,#91717,#91718,#91719,#91720,#91721,
#91722,#91723,#91724,#91725,#91726,#91727),.UNSPECIFIED.,.F.,.F.,(4,3,3,
3,3,3,3,4),(133.06419185914,133.953966047951,134.953622510996,135.95327897404,
136.952935437085,137.952591900129,138.952248363173,139.34737716632),
 .UNSPECIFIED.);
#2053=B_SPLINE_CURVE_WITH_KNOTS('',3,(#91732,#91733,#91734,#91735,#91736,
#91737,#91738,#91739,#91740,#91741,#91742,#91743,#91744,#91745,#91746,#91747,
#91748,#91749,#91750,#91751,#91752,#91753),.UNSPECIFIED.,.F.,.F.,(4,3,3,
3,3,3,3,4),(-148.606192485261,-147.916271476645,-146.916837209911,-145.917402943177,
-144.917968676443,-143.918534409709,-142.919100142975,-142.323007178082),
 .UNSPECIFIED.);
#2054=B_SPLINE_CURVE_WITH_KNOTS('',3,(#91754,#91755,#91756,#91757,#91758,
#91759,#91760,#91761,#91762,#91763,#91764,#91765,#91766,#91767,#91768,#91769,
#91770,#91771,#91772,#91773,#91774,#91775),.UNSPECIFIED.,.F.,.F.,(4,3,3,
3,3,3,3,4),(139.34737716632,139.951904826218,140.951561289262,141.951217752307,
142.950874215351,143.950530678395,144.95018714144,145.6305624735),
 .UNSPECIFIED.);
#2055=B_SPLINE_CURVE_WITH_KNOTS('',3,(#91780,#91781,#91782,#91783,#91784,
#91785,#91786,#91787,#91788,#91789,#91790,#91791,#91792,#91793,#91794,#91795,
#91796,#91797,#91798,#91799,#91800,#91801),.UNSPECIFIED.,.F.,.F.,(4,3,3,
3,3,3,3,4),(-154.889377792441,-153.91287707705,-152.913442810316,-151.914008543581,
-150.914574276847,-149.915140010113,-148.915705743379,-148.606192485261),
 .UNSPECIFIED.);
#2056=B_SPLINE_CURVE_WITH_KNOTS('',3,(#91802,#91803,#91804,#91805,#91806,
#91807,#91808,#91809,#91810,#91811,#91812,#91813,#91814,#91815,#91816,#91817,
#91818,#91819,#91820,#91821,#91822,#91823),.UNSPECIFIED.,.F.,.F.,(4,3,3,
3,3,3,3,4),(145.6305624735,145.949843604484,146.949500067529,147.949156530573,
148.948812993617,149.948469456662,150.948125919706,151.913747780679),
 .UNSPECIFIED.);
#2057=B_SPLINE_CURVE_WITH_KNOTS('',3,(#91828,#91829,#91830,#91831,#91832,
#91833,#91834,#91835,#91836,#91837,#91838,#91839,#91840,#91841,#91842,#91843,
#91844,#91845,#91846,#91847,#91848,#91849,#91850,#91851,#91852),
 .UNSPECIFIED.,.F.,.F.,(4,3,3,3,3,3,3,3,4),(-161.17256309962,-160.908916944188,
-159.909482677454,-158.91004841072,-157.910614143986,-156.911179877252,
-155.911745610518,-154.912311343784,-154.889377792441),.UNSPECIFIED.);
#2058=B_SPLINE_CURVE_WITH_KNOTS('',3,(#91853,#91854,#91855,#91856,#91857,
#91858,#91859,#91860,#91861,#91862,#91863,#91864,#91865,#91866,#91867,#91868,
#91869,#91870,#91871,#91872,#91873,#91874,#91875,#91876,#91877),
 .UNSPECIFIED.,.F.,.F.,(4,3,3,3,3,3,3,3,4),(151.913747780679,151.947782382751,
152.947438845795,153.94709530884,154.946751771884,155.946408234928,156.946064697973,
157.945721161017,158.196933087859),.UNSPECIFIED.);
#2059=B_SPLINE_CURVE_WITH_KNOTS('',3,(#91882,#91883,#91884,#91885,#91886,
#91887,#91888,#91889,#91890,#91891,#91892,#91893,#91894,#91895,#91896,#91897,
#91898,#91899,#91900,#91901,#91902,#91903),.UNSPECIFIED.,.F.,.F.,(4,3,3,
3,3,3,3,4),(-167.4557484068,-166.905522544593,-165.906088277859,-164.906654011125,
-163.90721974439,-162.907785477656,-161.908351210922,-161.17256309962),
 .UNSPECIFIED.);
#2060=B_SPLINE_CURVE_WITH_KNOTS('',3,(#91904,#91905,#91906,#91907,#91908,
#91909,#91910,#91911,#91912,#91913,#91914,#91915,#91916,#91917,#91918,#91919,
#91920,#91921,#91922,#91923,#91924,#91925),.UNSPECIFIED.,.F.,.F.,(4,3,3,
3,3,3,3,4),(158.196933087859,158.945377624062,159.945034087106,160.944690550151,
161.944347013195,162.944003476239,163.943659939284,164.480118395038),
 .UNSPECIFIED.);
#2061=B_SPLINE_CURVE_WITH_KNOTS('',3,(#91930,#91931,#91932,#91933,#91934,
#91935,#91936,#91937,#91938,#91939,#91940,#91941,#91942,#91943,#91944,#91945,
#91946,#91947,#91948,#91949,#91950,#91951),.UNSPECIFIED.,.F.,.F.,(4,3,3,
3,3,3,3,4),(-173.738933713979,-172.902128144997,-171.902693878263,-170.903259611529,
-169.903825344795,-168.904391078061,-167.904956811327,-167.4557484068),
 .UNSPECIFIED.);
#2062=B_SPLINE_CURVE_WITH_KNOTS('',3,(#91952,#91953,#91954,#91955,#91956,
#91957,#91958,#91959,#91960,#91961,#91962,#91963,#91964,#91965,#91966,#91967,
#91968,#91969,#91970,#91971,#91972,#91973),.UNSPECIFIED.,.F.,.F.,(4,3,3,
3,3,3,3,4),(164.480118395038,164.943316402328,165.942972865373,166.942629328417,
167.942285791461,168.941942254506,169.94159871755,170.763303702218),
 .UNSPECIFIED.);
#2063=B_SPLINE_CURVE_WITH_KNOTS('',3,(#91978,#91979,#91980,#91981,#91982,
#91983,#91984,#91985,#91986,#91987,#91988,#91989,#91990,#91991,#91992,#91993,
#91994,#91995,#91996,#91997,#91998,#91999,#92000,#92001,#92002),
 .UNSPECIFIED.,.F.,.F.,(4,3,3,3,3,3,3,3,4),(-180.022119021159,-179.898168012136,
-178.898733745402,-177.899299478668,-176.899865211934,-175.9004309452,-174.900996678466,
-173.901562411731,-173.738933713979),.UNSPECIFIED.);
#2064=B_SPLINE_CURVE_WITH_KNOTS('',3,(#92003,#92004,#92005,#92006,#92007,
#92008,#92009,#92010,#92011,#92012,#92013,#92014,#92015,#92016,#92017,#92018,
#92019,#92020,#92021,#92022,#92023,#92024,#92025,#92026,#92027),
 .UNSPECIFIED.,.F.,.F.,(4,3,3,3,3,3,3,3,4),(170.763303702218,170.941255180595,
171.940911643639,172.940568106683,173.940224569728,174.939881032772,175.939537495817,
176.939193958861,177.046489009397),.UNSPECIFIED.);
#2065=B_SPLINE_CURVE_WITH_KNOTS('',3,(#92032,#92033,#92034,#92035,#92036,
#92037,#92038,#92039,#92040,#92041,#92042,#92043,#92044,#92045,#92046,#92047,
#92048,#92049,#92050,#92051,#92052,#92053),.UNSPECIFIED.,.F.,.F.,(4,3,3,
3,3,3,3,4),(-186.305304328339,-185.89477361254,-184.895339345806,-183.895905079072,
-182.896470812338,-181.897036545604,-180.89760227887,-180.022119021159),
 .UNSPECIFIED.);
#2066=B_SPLINE_CURVE_WITH_KNOTS('',3,(#92054,#92055,#92056,#92057,#92058,
#92059,#92060,#92061,#92062,#92063,#92064,#92065,#92066,#92067,#92068,#92069,
#92070,#92071,#92072,#92073,#92074,#92075),.UNSPECIFIED.,.F.,.F.,(4,3,3,
3,3,3,3,4),(177.046489009397,177.938850421905,178.93850688495,179.938163347994,
180.937819811039,181.937476274083,182.937132737128,183.329674316577),
 .UNSPECIFIED.);
#2067=B_SPLINE_CURVE_WITH_KNOTS('',3,(#92080,#92081,#92082,#92083,#92084,
#92085,#92086,#92087,#92088,#92089,#92090,#92091,#92092,#92093,#92094,#92095,
#92096,#92097,#92098,#92099,#92100,#92101),.UNSPECIFIED.,.F.,.F.,(4,3,3,
3,3,3,3,4),(-192.588489635518,-191.891379212945,-190.891944946211,-189.892510679477,
-188.893076412743,-187.893642146009,-186.894207879275,-186.305304328339),
 .UNSPECIFIED.);
#2068=B_SPLINE_CURVE_WITH_KNOTS('',3,(#92102,#92103,#92104,#92105,#92106,
#92107,#92108,#92109,#92110,#92111,#92112,#92113,#92114,#92115,#92116,#92117,
#92118,#92119,#92120,#92121,#92122,#92123),.UNSPECIFIED.,.F.,.F.,(4,3,3,
3,3,3,3,4),(183.329674316577,183.936789200172,184.936445663216,185.936102126261,
186.935758589305,187.93541505235,188.935071515394,189.612859623757),
 .UNSPECIFIED.);
#2069=B_SPLINE_CURVE_WITH_KNOTS('',3,(#92128,#92129,#92130,#92131,#92132,
#92133,#92134,#92135,#92136,#92137,#92138,#92139,#92140,#92141,#92142,#92143,
#92144,#92145,#92146,#92147,#92148,#92149),.UNSPECIFIED.,.F.,.F.,(4,3,3,
3,3,3,3,4),(-198.871674942698,-197.887984813349,-196.888550546615,-195.889116279881,
-194.889682013147,-193.890247746413,-192.890813479679,-192.588489635518),
 .UNSPECIFIED.);
#2070=B_SPLINE_CURVE_WITH_KNOTS('',3,(#92150,#92151,#92152,#92153,#92154,
#92155,#92156,#92157,#92158,#92159,#92160,#92161,#92162,#92163,#92164,#92165,
#92166,#92167,#92168,#92169,#92170,#92171),.UNSPECIFIED.,.F.,.F.,(4,3,3,
3,3,3,3,4),(189.612859623757,189.934727978438,190.934384441483,191.934040904527,
192.933697367572,193.933353830616,194.93301029366,195.896044930936),
 .UNSPECIFIED.);
#2071=B_SPLINE_CURVE_WITH_KNOTS('',3,(#92176,#92177,#92178,#92179,#92180,
#92181,#92182,#92183,#92184,#92185,#92186,#92187,#92188,#92189,#92190,#92191,
#92192,#92193,#92194,#92195,#92196,#92197,#92198,#92199,#92200),
 .UNSPECIFIED.,.F.,.F.,(4,3,3,3,3,3,3,3,4),(-205.154860249877,-204.884024680488,
-203.884590413754,-202.88515614702,-201.885721880286,-200.886287613552,
-199.886853346818,-198.887419080084,-198.871674942698),.UNSPECIFIED.);
#2072=B_SPLINE_CURVE_WITH_KNOTS('',3,(#92201,#92202,#92203,#92204,#92205,
#92206,#92207,#92208,#92209,#92210,#92211,#92212,#92213,#92214,#92215,#92216,
#92217,#92218,#92219,#92220,#92221,#92222,#92223,#92224,#92225),
 .UNSPECIFIED.,.F.,.F.,(4,3,3,3,3,3,3,3,4),(195.896044930936,195.932666756705,
196.932323219749,197.931979682794,198.931636145838,199.931292608883,200.930949071927,
201.930605534971,202.179230238116),.UNSPECIFIED.);
#2073=B_SPLINE_CURVE_WITH_KNOTS('',3,(#92230,#92231,#92232,#92233,#92234,
#92235,#92236,#92237,#92238,#92239,#92240,#92241,#92242,#92243,#92244,#92245,
#92246,#92247,#92248,#92249,#92250,#92251),.UNSPECIFIED.,.F.,.F.,(4,3,3,
3,3,3,3,4),(-211.438045557057,-210.880630280893,-209.881196014159,-208.881761747424,
-207.88232748069,-206.882893213956,-205.883458947222,-205.154860249877),
 .UNSPECIFIED.);
#2074=B_SPLINE_CURVE_WITH_KNOTS('',3,(#92252,#92253,#92254,#92255,#92256,
#92257,#92258,#92259,#92260,#92261,#92262,#92263,#92264,#92265,#92266,#92267,
#92268,#92269,#92270,#92271,#92272,#92273),.UNSPECIFIED.,.F.,.F.,(4,3,3,
3,3,3,3,4),(202.179230238116,202.930261998016,203.92991846106,204.929574924105,
205.929231387149,206.928887850193,207.928544313238,208.462415545295),
 .UNSPECIFIED.);
#2075=B_SPLINE_CURVE_WITH_KNOTS('',3,(#92278,#92279,#92280,#92281,#92282,
#92283,#92284,#92285,#92286,#92287,#92288,#92289,#92290,#92291,#92292,#92293,
#92294,#92295,#92296,#92297,#92298,#92299),.UNSPECIFIED.,.F.,.F.,(4,3,3,
3,3,3,3,4),(-217.721230864236,-216.877235881297,-215.877801614563,-214.878367347829,
-213.878933081095,-212.879498814361,-211.880064547627,-211.438045557057),
 .UNSPECIFIED.);
#2076=B_SPLINE_CURVE_WITH_KNOTS('',3,(#92300,#92301,#92302,#92303,#92304,
#92305,#92306,#92307,#92308,#92309,#92310,#92311,#92312,#92313,#92314,#92315,
#92316,#92317,#92318,#92319,#92320,#92321),.UNSPECIFIED.,.F.,.F.,(4,3,3,
3,3,3,3,4),(208.462415545295,208.928200776282,209.927857239327,210.927513702371,
211.927170165416,212.92682662846,213.926483091504,214.745600852475),
 .UNSPECIFIED.);
#2077=B_SPLINE_CURVE_WITH_KNOTS('',3,(#92326,#92327,#92328,#92329,#92330,
#92331,#92332,#92333,#92334,#92335,#92336,#92337,#92338,#92339,#92340,#92341,
#92342,#92343,#92344,#92345,#92346,#92347,#92348,#92349,#92350),
 .UNSPECIFIED.,.F.,.F.,(4,3,3,3,3,3,3,3,4),(-224.004416171416,-223.873275748436,
-222.873841481702,-221.874407214968,-220.874972948234,-219.875538681499,
-218.876104414765,-217.876670148031,-217.721230864236),.UNSPECIFIED.);
#2078=B_SPLINE_CURVE_WITH_KNOTS('',3,(#92351,#92352,#92353,#92354,#92355,
#92356,#92357,#92358,#92359,#92360,#92361,#92362,#92363,#92364,#92365,#92366,
#92367,#92368,#92369,#92370,#92371,#92372,#92373,#92374,#92375),
 .UNSPECIFIED.,.F.,.F.,(4,3,3,3,3,3,3,3,4),(214.745600852475,214.926139554549,
215.925796017593,216.925452480638,217.925108943682,218.924765406726,219.924421869771,
220.924078332815,221.028786159654),.UNSPECIFIED.);
#2079=B_SPLINE_CURVE_WITH_KNOTS('',3,(#92380,#92381,#92382,#92383,#92384,
#92385,#92386,#92387,#92388,#92389,#92390,#92391,#92392,#92393,#92394,#92395,
#92396,#92397,#92398,#92399,#92400,#92401),.UNSPECIFIED.,.F.,.F.,(4,3,3,
3,3,3,3,4),(-230.287601478596,-229.86988134884,-228.870447082106,-227.871012815372,
-226.871578548638,-225.872144281904,-224.87271001517,-224.004416171416),
 .UNSPECIFIED.);
#2080=B_SPLINE_CURVE_WITH_KNOTS('',3,(#92402,#92403,#92404,#92405,#92406,
#92407,#92408,#92409,#92410,#92411,#92412,#92413,#92414,#92415,#92416,#92417,
#92418,#92419,#92420,#92421,#92422,#92423),.UNSPECIFIED.,.F.,.F.,(4,3,3,
3,3,3,3,4),(221.028786159654,221.92373479586,222.923391258904,223.923047721948,
224.922704184993,225.922360648037,226.922017111082,227.311971466834),
 .UNSPECIFIED.);
#2081=B_SPLINE_CURVE_WITH_KNOTS('',3,(#92428,#92429,#92430,#92431,#92432,
#92433,#92434,#92435,#92436,#92437,#92438,#92439,#92440,#92441,#92442,#92443,
#92444,#92445,#92446,#92447,#92448,#92449),.UNSPECIFIED.,.F.,.F.,(4,3,3,
3,3,3,3,4),(-236.570786785775,-235.866486949245,-234.867052682511,-233.867618415777,
-232.868184149043,-231.868749882309,-230.869315615574,-230.287601478596),
 .UNSPECIFIED.);
#2082=B_SPLINE_CURVE_WITH_KNOTS('',3,(#92450,#92451,#92452,#92453,#92454,
#92455,#92456,#92457,#92458,#92459,#92460,#92461,#92462,#92463,#92464,#92465,
#92466,#92467,#92468,#92469,#92470,#92471),.UNSPECIFIED.,.F.,.F.,(4,3,3,
3,3,3,3,4),(227.311971466834,227.921673574126,228.921330037171,229.920986500215,
230.920642963259,231.920299426304,232.919955889348,233.595156774013),
 .UNSPECIFIED.);
#2083=B_SPLINE_CURVE_WITH_KNOTS('',3,(#92476,#92477,#92478,#92479,#92480,
#92481,#92482,#92483,#92484,#92485,#92486,#92487,#92488,#92489,#92490,#92491,
#92492,#92493,#92494,#92495,#92496,#92497),.UNSPECIFIED.,.F.,.F.,(4,3,3,
3,3,3,3,4),(-242.853972092955,-241.863092549649,-240.863658282915,-239.864224016181,
-238.864789749447,-237.865355482713,-236.865921215979,-236.570786785775),
 .UNSPECIFIED.);
#2084=B_SPLINE_CURVE_WITH_KNOTS('',3,(#92498,#92499,#92500,#92501,#92502,
#92503,#92504,#92505,#92506,#92507,#92508,#92509,#92510,#92511,#92512,#92513,
#92514,#92515,#92516,#92517,#92518,#92519),.UNSPECIFIED.,.F.,.F.,(4,3,3,
3,3,3,3,4),(233.595156774013,233.919612352393,234.919268815437,235.918925278481,
236.918581741526,237.91823820457,238.917894667615,239.878342081193),
 .UNSPECIFIED.);
#2085=B_SPLINE_CURVE_WITH_KNOTS('',3,(#92524,#92525,#92526,#92527,#92528,
#92529,#92530,#92531,#92532,#92533,#92534,#92535,#92536,#92537,#92538,#92539,
#92540,#92541,#92542,#92543,#92544,#92545,#92546,#92547,#92548),
 .UNSPECIFIED.,.F.,.F.,(4,3,3,3,3,3,3,3,4),(-249.137157400134,-248.859132416788,
-247.859698150054,-246.86026388332,-245.860829616586,-244.861395349852,
-243.861961083118,-242.862526816383,-242.853972092955),.UNSPECIFIED.);
#2086=B_SPLINE_CURVE_WITH_KNOTS('',3,(#92549,#92550,#92551,#92552,#92553,
#92554,#92555,#92556,#92557,#92558,#92559,#92560,#92561,#92562,#92563,#92564,
#92565,#92566,#92567,#92568,#92569,#92570,#92571,#92572,#92573),
 .UNSPECIFIED.,.F.,.F.,(4,3,3,3,3,3,3,3,4),(239.878342081193,239.917551130659,
240.917207593703,241.916864056748,242.916520519792,243.916176982837,244.915833445881,
245.915489908926,246.161527388373),.UNSPECIFIED.);
#2087=B_SPLINE_CURVE_WITH_KNOTS('',3,(#92578,#92579,#92580,#92581,#92582,
#92583,#92584,#92585,#92586,#92587,#92588,#92589,#92590,#92591,#92592,#92593,
#92594,#92595,#92596,#92597,#92598,#92599),.UNSPECIFIED.,.F.,.F.,(4,3,3,
3,3,3,3,4),(-255.420342707314,-254.855738017193,-253.856303750458,-252.856869483724,
-251.85743521699,-250.858000950256,-249.858566683522,-249.137157400134),
 .UNSPECIFIED.);
#2088=B_SPLINE_CURVE_WITH_KNOTS('',3,(#92600,#92601,#92602,#92603,#92604,
#92605,#92606,#92607,#92608,#92609,#92610,#92611,#92612,#92613,#92614,#92615,
#92616,#92617,#92618,#92619,#92620,#92621),.UNSPECIFIED.,.F.,.F.,(4,3,3,
3,3,3,3,4),(246.161527388373,246.91514637197,247.914802835014,248.914459298059,
249.914115761103,250.913772224148,251.913428687192,252.444712695552),
 .UNSPECIFIED.);
#2089=B_SPLINE_CURVE_WITH_KNOTS('',3,(#92626,#92627,#92628,#92629,#92630,
#92631,#92632,#92633,#92634,#92635,#92636,#92637,#92638,#92639,#92640,#92641,
#92642,#92643,#92644,#92645,#92646,#92647),.UNSPECIFIED.,.F.,.F.,(4,3,3,
3,3,3,3,4),(-261.703528014493,-260.852343617597,-259.852909350863,-258.853475084129,
-257.854040817395,-256.854606550661,-255.855172283927,-255.420342707314),
 .UNSPECIFIED.);
#2090=B_SPLINE_CURVE_WITH_KNOTS('',3,(#92648,#92649,#92650,#92651,#92652,
#92653,#92654,#92655,#92656,#92657,#92658,#92659,#92660,#92661,#92662,#92663,
#92664,#92665,#92666,#92667,#92668,#92669),.UNSPECIFIED.,.F.,.F.,(4,3,3,
3,3,3,3,4),(252.444712695552,252.913085150236,253.912741613281,254.912398076325,
255.91205453937,256.911711002414,257.911367465458,258.727898002732),
 .UNSPECIFIED.);
#2091=B_SPLINE_CURVE_WITH_KNOTS('',3,(#92674,#92675,#92676,#92677,#92678,
#92679,#92680,#92681,#92682,#92683,#92684,#92685,#92686,#92687,#92688,#92689,
#92690,#92691,#92692,#92693,#92694,#92695,#92696,#92697,#92698),
 .UNSPECIFIED.,.F.,.F.,(4,3,3,3,3,3,3,3,4),(-267.986713321673,-267.848383484736,
-266.848949218002,-265.849514951268,-264.850080684533,-263.850646417799,
-262.851212151065,-261.851777884331,-261.703528014493),.UNSPECIFIED.);
#2092=B_SPLINE_CURVE_WITH_KNOTS('',3,(#92699,#92700,#92701,#92702,#92703,
#92704,#92705,#92706,#92707,#92708,#92709,#92710,#92711,#92712,#92713,#92714,
#92715,#92716,#92717,#92718,#92719,#92720,#92721,#92722,#92723),
 .UNSPECIFIED.,.F.,.F.,(4,3,3,3,3,3,3,3,4),(258.727898002732,258.911023928503,
259.910680391547,260.910336854592,261.909993317636,262.909649780681,263.909306243725,
264.908962706769,265.011083309911),.UNSPECIFIED.);
#2093=B_SPLINE_CURVE_WITH_KNOTS('',3,(#92728,#92729,#92730,#92731,#92732,
#92733,#92734,#92735,#92736,#92737,#92738,#92739,#92740,#92741,#92742,#92743,
#92744,#92745,#92746,#92747,#92748,#92749),.UNSPECIFIED.,.F.,.F.,(4,3,3,
3,3,3,3,4),(-274.269898628852,-273.84498908514,-272.845554818406,-271.846120551672,
-270.846686284938,-269.847252018204,-268.84781775147,-267.986713321673),
 .UNSPECIFIED.);
#2094=B_SPLINE_CURVE_WITH_KNOTS('',3,(#92750,#92751,#92752,#92753,#92754,
#92755,#92756,#92757,#92758,#92759,#92760,#92761,#92762,#92763,#92764,#92765,
#92766,#92767,#92768,#92769,#92770,#92771),.UNSPECIFIED.,.F.,.F.,(4,3,3,
3,3,3,3,4),(265.011083309911,265.908619169814,266.908275632858,267.907932095903,
268.907588558947,269.907245021991,270.906901485036,271.294268617091),
 .UNSPECIFIED.);
#2095=B_SPLINE_CURVE_WITH_KNOTS('',3,(#92776,#92777,#92778,#92779,#92780,
#92781,#92782,#92783,#92784,#92785,#92786,#92787,#92788,#92789,#92790,#92791,
#92792,#92793,#92794,#92795,#92796,#92797),.UNSPECIFIED.,.F.,.F.,(4,3,3,
3,3,3,3,4),(-280.553083936032,-279.841594685545,-278.842160418811,-277.842726152076,
-276.843291885342,-275.843857618608,-274.844423351874,-274.269898628852),
 .UNSPECIFIED.);
#2096=B_SPLINE_CURVE_WITH_KNOTS('',3,(#92798,#92799,#92800,#92801,#92802,
#92803,#92804,#92805,#92806,#92807,#92808,#92809,#92810,#92811,#92812,#92813,
#92814,#92815,#92816,#92817,#92818,#92819),.UNSPECIFIED.,.F.,.F.,(4,3,3,
3,3,3,3,4),(271.294268617091,271.90655794808,272.906214411125,273.905870874169,
274.905527337214,275.905183800258,276.904840263302,277.57745392427),
 .UNSPECIFIED.);
#2097=B_SPLINE_CURVE_WITH_KNOTS('',3,(#92824,#92825,#92826,#92827,#92828,
#92829,#92830,#92831,#92832,#92833,#92834,#92835,#92836,#92837,#92838,#92839,
#92840,#92841,#92842,#92843,#92844,#92845),.UNSPECIFIED.,.F.,.F.,(4,3,3,
3,3,3,3,4),(-286.836269243212,-285.838200285949,-284.838766019215,-283.839331752481,
-282.839897485747,-281.840463219013,-280.841028952279,-280.553083936032),
 .UNSPECIFIED.);
#2098=B_SPLINE_CURVE_WITH_KNOTS('',3,(#92846,#92847,#92848,#92849,#92850,
#92851,#92852,#92853,#92854,#92855,#92856,#92857,#92858,#92859,#92860,#92861,
#92862,#92863,#92864,#92865,#92866,#92867),.UNSPECIFIED.,.F.,.F.,(4,3,3,
3,3,3,3,4),(277.57745392427,277.904496726347,278.904153189391,279.903809652436,
280.90346611548,281.903122578524,282.902779041569,283.86063923145),
 .UNSPECIFIED.);
#2099=B_SPLINE_CURVE_WITH_KNOTS('',3,(#92872,#92873,#92874,#92875,#92876,
#92877,#92878,#92879,#92880,#92881,#92882,#92883,#92884,#92885,#92886,#92887,
#92888,#92889,#92890,#92891,#92892,#92893),.UNSPECIFIED.,.F.,.F.,(4,3,3,
3,3,3,3,4),(-293.119454550391,-292.834240153088,-291.834805886354,-290.83537161962,
-289.835937352886,-288.836503086152,-287.837068819417,-286.836269243212),
 .UNSPECIFIED.);
#2100=B_SPLINE_CURVE_WITH_KNOTS('',3,(#92894,#92895,#92896,#92897,#92898,
#92899,#92900,#92901,#92902,#92903,#92904,#92905,#92906,#92907,#92908,#92909,
#92910,#92911,#92912,#92913,#92914,#92915,#92916,#92917,#92918),
 .UNSPECIFIED.,.F.,.F.,(4,3,3,3,3,3,3,3,4),(283.86063923145,283.902435504613,
284.902091967658,285.901748430702,286.901404893746,287.901061356791,288.900717819835,
289.90037428288,290.14382453863),.UNSPECIFIED.);
#2101=B_SPLINE_CURVE_WITH_KNOTS('',3,(#92923,#92924,#92925,#92926,#92927,
#92928,#92929,#92930,#92931,#92932,#92933,#92934,#92935,#92936,#92937,#92938,
#92939,#92940,#92941,#92942,#92943,#92944),.UNSPECIFIED.,.F.,.F.,(4,3,3,
3,3,3,3,4),(-299.402639857571,-298.830845753492,-297.831411486758,-296.831977220024,
-295.83254295329,-294.833108686556,-293.833674419822,-293.119454550391),
 .UNSPECIFIED.);
#2102=B_SPLINE_CURVE_WITH_KNOTS('',3,(#92945,#92946,#92947,#92948,#92949,
#92950,#92951,#92952,#92953,#92954,#92955,#92956,#92957,#92958,#92959,#92960,
#92961,#92962,#92963,#92964,#92965,#92966),.UNSPECIFIED.,.F.,.F.,(4,3,3,
3,3,3,3,4),(290.14382453863,290.900030745924,291.899687208968,292.899343672013,
293.899000135057,294.898656598102,295.898313061146,296.427009845809),
 .UNSPECIFIED.);
#2103=B_SPLINE_CURVE_WITH_KNOTS('',3,(#92971,#92972,#92973,#92974,#92975,
#92976,#92977,#92978,#92979,#92980,#92981,#92982,#92983,#92984,#92985,#92986,
#92987,#92988,#92989,#92990,#92991,#92992),.UNSPECIFIED.,.F.,.F.,(4,3,3,
3,3,3,3,4),(-305.68582516475,-304.827451353897,-303.828017087163,-302.828582820429,
-301.829148553695,-300.829714286961,-299.830280020226,-299.402639857571),
 .UNSPECIFIED.);
#2104=B_SPLINE_CURVE_WITH_KNOTS('',3,(#92993,#92994,#92995,#92996,#92997,
#92998,#92999,#93000,#93001,#93002,#93003,#93004,#93005,#93006,#93007,#93008,
#93009,#93010,#93011,#93012,#93013,#93014),.UNSPECIFIED.,.F.,.F.,(4,3,3,
3,3,3,3,4),(296.427009845809,296.897969524191,297.897625987235,298.897282450279,
299.896938913324,300.896595376368,301.896251839413,302.710195152989),
 .UNSPECIFIED.);
#2105=B_SPLINE_CURVE_WITH_KNOTS('',3,(#93020,#93021,#93022,#93023,#93024,
#93025,#93026,#93027,#93028,#93029),.UNSPECIFIED.,.F.,.F.,(4,1,1,1,1,1,
1,4),(317.300858012569,317.44191846845,318.441352735184,319.440787001918,
320.440221268652,321.439655535386,322.43908980212,323.438524068854),
 .UNSPECIFIED.);
#2106=B_SPLINE_CURVE_WITH_KNOTS('',3,(#93032,#93033,#93034,#93035,#93036,
#93037,#93038,#93039),.UNSPECIFIED.,.F.,.F.,(4,1,1,1,1,4),(317.300858012569,
318.200981096169,319.200637559214,320.200294022258,321.199950485303,322.199606948347),
 .UNSPECIFIED.);
#2107=B_SPLINE_CURVE_WITH_KNOTS('',3,(#93044,#93045,#93046,#93047,#93048,
#93049,#93050,#93051,#93052,#93053),.UNSPECIFIED.,.F.,.F.,(4,1,1,1,1,1,
1,4),(311.017672705389,311.445312868045,312.444747134779,313.444181401514,
314.443615668248,315.443049934982,316.442484201716,317.300858012569),
 .UNSPECIFIED.);
#2108=B_SPLINE_CURVE_WITH_KNOTS('',3,(#93054,#93055,#93056,#93057,#93058,
#93059,#93060,#93061,#93062,#93063,#93064),.UNSPECIFIED.,.F.,.F.,(4,1,1,
1,1,1,1,1,4),(311.017672705389,311.203385854859,312.203042317903,313.202698780947,
314.202355243992,315.202011707036,316.201668170081,317.201324633125,317.300858012569),
 .UNSPECIFIED.);
#2109=B_SPLINE_CURVE_WITH_KNOTS('',3,(#93069,#93070,#93071,#93072,#93073,
#93074,#93075,#93076,#93077,#93078),.UNSPECIFIED.,.F.,.F.,(4,1,1,1,1,1,
1,4),(304.73448739821,305.448707267641,306.448141534375,307.447575801109,
308.447010067843,309.446444334577,310.445878601311,311.017672705389),
 .UNSPECIFIED.);
#2110=B_SPLINE_CURVE_WITH_KNOTS('',3,(#93079,#93080,#93081,#93082,#93083,
#93084,#93085,#93086,#93087,#93088),.UNSPECIFIED.,.F.,.F.,(4,1,1,1,1,1,
1,4),(304.73448739821,305.205447076592,306.205103539637,307.204760002681,
308.204416465725,309.20407292877,310.203729391814,311.017672705389),
 .UNSPECIFIED.);
#2111=B_SPLINE_CURVE_WITH_KNOTS('',3,(#93093,#93094,#93095,#93096,#93097,
#93098,#93099,#93100,#93101,#93102,#93103),.UNSPECIFIED.,.F.,.F.,(4,1,1,
1,1,1,1,1,4),(298.45130209103,298.452667400502,299.452101667236,300.45153593397,
301.450970200704,302.450404467439,303.449838734173,304.449273000907,304.73448739821),
 .UNSPECIFIED.);
#2112=B_SPLINE_CURVE_WITH_KNOTS('',3,(#93104,#93105,#93106,#93107,#93108,
#93109,#93110,#93111,#93112,#93113),.UNSPECIFIED.,.F.,.F.,(4,1,1,1,1,1,
1,4),(298.45130209103,299.207508298326,300.20716476137,301.206821224415,
302.206477687459,303.206134150503,304.205790613548,304.73448739821),
 .UNSPECIFIED.);
#2113=B_SPLINE_CURVE_WITH_KNOTS('',3,(#93118,#93119,#93120,#93121,#93122,
#93123,#93124,#93125,#93126,#93127),.UNSPECIFIED.,.F.,.F.,(4,1,1,1,1,1,
1,4),(292.168116783851,292.456061800098,293.455496066832,294.454930333566,
295.4543646003,296.453798867034,297.453233133768,298.45130209103),
 .UNSPECIFIED.);
#2114=B_SPLINE_CURVE_WITH_KNOTS('',3,(#93128,#93129,#93130,#93131,#93132,
#93133,#93134,#93135,#93136,#93137,#93138),.UNSPECIFIED.,.F.,.F.,(4,1,1,
1,1,1,1,1,4),(292.168116783851,292.209913057015,293.209569520059,294.209225983104,
295.208882446148,296.208538909192,297.208195372237,298.207851835281,298.45130209103),
 .UNSPECIFIED.);
#2115=B_SPLINE_CURVE_WITH_KNOTS('',3,(#93143,#93144,#93145,#93146,#93147,
#93148,#93149,#93150,#93151,#93152),.UNSPECIFIED.,.F.,.F.,(4,1,1,1,1,1,
1,4),(285.884931476671,286.459456199693,287.458890466427,288.458324733161,
289.457758999895,290.45719326663,291.456627533364,292.168116783851),
 .UNSPECIFIED.);
#2116=B_SPLINE_CURVE_WITH_KNOTS('',3,(#93153,#93154,#93155,#93156,#93157,
#93158,#93159,#93160,#93161,#93162),.UNSPECIFIED.,.F.,.F.,(4,1,1,1,1,1,
1,4),(285.884931476671,286.211974278748,287.211630741793,288.211287204837,
289.210943667882,290.210600130926,291.21025659397,292.168116783851),
 .UNSPECIFIED.);
#2117=B_SPLINE_CURVE_WITH_KNOTS('',3,(#93167,#93168,#93169,#93170,#93171,
#93172,#93173,#93174,#93175,#93176),.UNSPECIFIED.,.F.,.F.,(4,1,1,1,1,1,
1,4),(279.601746169491,280.462850599289,281.462284866023,282.461719132757,
283.461153399491,284.460587666225,285.460021932959,285.884931476671),
 .UNSPECIFIED.);
#2118=B_SPLINE_CURVE_WITH_KNOTS('',3,(#93177,#93178,#93179,#93180,#93181,
#93182,#93183,#93184,#93185,#93186),.UNSPECIFIED.,.F.,.F.,(4,1,1,1,1,1,
1,4),(279.601746169492,280.214035500482,281.213691963526,282.213348426571,
283.213004889615,284.212661352659,285.212317815704,285.884931476671),
 .UNSPECIFIED.);
#2119=B_SPLINE_CURVE_WITH_KNOTS('',3,(#93191,#93192,#93193,#93194,#93195,
#93196,#93197,#93198,#93199,#93200,#93201),.UNSPECIFIED.,.F.,.F.,(4,1,1,
1,1,1,1,1,4),(273.318560862312,273.46681073215,274.466244998884,275.465679265618,
276.465113532352,277.464547799086,278.46398206582,279.463416332555,279.601746169491),
 .UNSPECIFIED.);
#2120=B_SPLINE_CURVE_WITH_KNOTS('',3,(#93202,#93203,#93204,#93205,#93206,
#93207,#93208,#93209,#93210,#93211),.UNSPECIFIED.,.F.,.F.,(4,1,1,1,1,1,
1,4),(273.318560862312,274.216096722215,275.21575318526,276.215409648304,
277.215066111349,278.214722574393,279.214379037437,279.601746169492),
 .UNSPECIFIED.);
#2121=B_SPLINE_CURVE_WITH_KNOTS('',3,(#93216,#93217,#93218,#93219,#93220,
#93221,#93222,#93223,#93224,#93225),.UNSPECIFIED.,.F.,.F.,(4,1,1,1,1,1,
1,4),(267.035375555132,267.470205131746,268.46963939848,269.469073665214,
270.468507931948,271.467942198682,272.467376465416,273.318560862312),
 .UNSPECIFIED.);
#2122=B_SPLINE_CURVE_WITH_KNOTS('',3,(#93226,#93227,#93228,#93229,#93230,
#93231,#93232,#93233,#93234,#93235,#93236),.UNSPECIFIED.,.F.,.F.,(4,1,1,
1,1,1,1,1,4),(267.035375555133,267.218501480904,268.218157943949,269.217814406993,
270.217470870038,271.217127333082,272.216783796126,273.216440259171,273.318560862312),
 .UNSPECIFIED.);
#2123=B_SPLINE_CURVE_WITH_KNOTS('',3,(#93241,#93242,#93243,#93244,#93245,
#93246,#93247,#93248,#93249,#93250),.UNSPECIFIED.,.F.,.F.,(4,1,1,1,1,1,
1,4),(260.752190247953,261.473599531341,262.473033798075,263.472468064809,
264.471902331543,265.471336598277,266.470770865011,267.035375555132),
 .UNSPECIFIED.);
#2124=B_SPLINE_CURVE_WITH_KNOTS('',3,(#93251,#93252,#93253,#93254,#93255,
#93256,#93257,#93258,#93259,#93260),.UNSPECIFIED.,.F.,.F.,(4,1,1,1,1,1,
1,4),(260.752190247953,261.220562702638,262.220219165682,263.219875628727,
264.219532091771,265.219188554816,266.21884501786,267.035375555133),
 .UNSPECIFIED.);
#2125=B_SPLINE_CURVE_WITH_KNOTS('',3,(#93265,#93266,#93267,#93268,#93269,
#93270,#93271,#93272,#93273,#93274,#93275),.UNSPECIFIED.,.F.,.F.,(4,1,1,
1,1,1,1,1,4),(254.469004940773,254.477559664202,255.476993930936,256.476428197671,
257.475862464405,258.475296731139,259.474730997873,260.474165264607,260.752190247953),
 .UNSPECIFIED.);
#2126=B_SPLINE_CURVE_WITH_KNOTS('',3,(#93276,#93277,#93278,#93279,#93280,
#93281,#93282,#93283,#93284,#93285),.UNSPECIFIED.,.F.,.F.,(4,1,1,1,1,1,
1,4),(254.469004940773,255.222623924372,256.222280387416,257.22193685046,
258.221593313505,259.221249776549,260.220906239594,260.752190247953),
 .UNSPECIFIED.);
#2127=B_SPLINE_CURVE_WITH_KNOTS('',3,(#93290,#93291,#93292,#93293,#93294,
#93295,#93296,#93297,#93298,#93299),.UNSPECIFIED.,.F.,.F.,(4,1,1,1,1,1,
1,4),(248.185819633594,248.480954063798,249.480388330532,250.479822597266,
251.479256864,252.478691130734,253.478125397468,254.469004940773),
 .UNSPECIFIED.);
#2128=B_SPLINE_CURVE_WITH_KNOTS('',3,(#93300,#93301,#93302,#93303,#93304,
#93305,#93306,#93307,#93308,#93309,#93310),.UNSPECIFIED.,.F.,.F.,(4,1,1,
1,1,1,1,1,4),(248.185819633594,248.225028683061,249.224685146105,250.224341609149,
251.223998072194,252.223654535238,253.223310998283,254.222967461327,254.469004940773),
 .UNSPECIFIED.);
#2129=B_SPLINE_CURVE_WITH_KNOTS('',3,(#93315,#93316,#93317,#93318,#93319,
#93320,#93321,#93322,#93323,#93324),.UNSPECIFIED.,.F.,.F.,(4,1,1,1,1,1,
1,4),(241.902634326414,242.484348463393,243.483782730127,244.483216996862,
245.482651263596,246.48208553033,247.481519797064,248.185819633594),
 .UNSPECIFIED.);
#2130=B_SPLINE_CURVE_WITH_KNOTS('',3,(#93325,#93326,#93327,#93328,#93329,
#93330,#93331,#93332,#93333,#93334),.UNSPECIFIED.,.F.,.F.,(4,1,1,1,1,1,
1,4),(241.902634326414,242.227089904794,243.226746367839,244.226402830883,
245.226059293927,246.225715756972,247.225372220016,248.185819633594),
 .UNSPECIFIED.);
#2131=B_SPLINE_CURVE_WITH_KNOTS('',3,(#93339,#93340,#93341,#93342,#93343,
#93344,#93345,#93346,#93347,#93348),.UNSPECIFIED.,.F.,.F.,(4,1,1,1,1,1,
1,4),(235.619449019235,236.487742862989,237.487177129723,238.486611396457,
239.486045663191,240.485479929925,241.484914196659,241.902634326414),
 .UNSPECIFIED.);
#2132=B_SPLINE_CURVE_WITH_KNOTS('',3,(#93349,#93350,#93351,#93352,#93353,
#93354,#93355,#93356,#93357,#93358),.UNSPECIFIED.,.F.,.F.,(4,1,1,1,1,1,
1,4),(235.619449019235,236.229151126528,237.228807589572,238.228464052616,
239.228120515661,240.227776978705,241.22743344175,241.902634326414),
 .UNSPECIFIED.);
#2133=B_SPLINE_CURVE_WITH_KNOTS('',3,(#93363,#93364,#93365,#93366,#93367,
#93368,#93369,#93370,#93371,#93372,#93373),.UNSPECIFIED.,.F.,.F.,(4,1,1,
1,1,1,1,1,4),(229.336263712055,229.49170299585,230.491137262584,231.490571529318,
232.490005796052,233.489440062787,234.488874329521,235.488308596255,235.619449019235),
 .UNSPECIFIED.);
#2134=B_SPLINE_CURVE_WITH_KNOTS('',3,(#93374,#93375,#93376,#93377,#93378,
#93379,#93380,#93381,#93382,#93383),.UNSPECIFIED.,.F.,.F.,(4,1,1,1,1,1,
1,4),(229.336263712055,230.231212348261,231.230868811306,232.23052527435,
233.230181737394,234.229838200439,235.229494663483,235.619449019235),
 .UNSPECIFIED.);
#2135=B_SPLINE_CURVE_WITH_KNOTS('',3,(#93388,#93389,#93390,#93391,#93392,
#93393,#93394,#93395,#93396,#93397),.UNSPECIFIED.,.F.,.F.,(4,1,1,1,1,1,
1,4),(223.053078404875,223.495097395446,224.49453166218,225.493965928914,
226.493400195648,227.492834462382,228.492268729116,229.336263712055),
 .UNSPECIFIED.);
#2136=B_SPLINE_CURVE_WITH_KNOTS('',3,(#93398,#93399,#93400,#93401,#93402,
#93403,#93404,#93405,#93406,#93407,#93408),.UNSPECIFIED.,.F.,.F.,(4,1,1,
1,1,1,1,1,4),(223.053078404876,223.23361710695,224.233273569995,225.232930033039,
226.232586496084,227.232242959128,228.231899422172,229.231555885217,229.336263712055),
 .UNSPECIFIED.);
#2137=B_SPLINE_CURVE_WITH_KNOTS('',3,(#93413,#93414,#93415,#93416,#93417,
#93418,#93419,#93420,#93421,#93422),.UNSPECIFIED.,.F.,.F.,(4,1,1,1,1,1,
1,4),(216.769893097696,217.498491795041,218.497926061775,219.497360328509,
220.496794595243,221.496228861977,222.495663128712,223.053078404875),
 .UNSPECIFIED.);
#2138=B_SPLINE_CURVE_WITH_KNOTS('',3,(#93423,#93424,#93425,#93426,#93427,
#93428,#93429,#93430,#93431,#93432),.UNSPECIFIED.,.F.,.F.,(4,1,1,1,1,1,
1,4),(216.769893097696,217.235678328684,218.235334791728,219.234991254773,
220.234647717817,221.234304180861,222.233960643906,223.053078404876),
 .UNSPECIFIED.);
#2139=B_SPLINE_CURVE_WITH_KNOTS('',3,(#93437,#93438,#93439,#93440,#93441,
#93442,#93443,#93444,#93445,#93446,#93447),.UNSPECIFIED.,.F.,.F.,(4,1,1,
1,1,1,1,1,4),(210.486707790516,210.502451927902,211.501886194637,212.501320461371,
213.500754728105,214.500188994839,215.499623261573,216.499057528307,216.769893097696),
 .UNSPECIFIED.);
#2140=B_SPLINE_CURVE_WITH_KNOTS('',3,(#93448,#93449,#93450,#93451,#93452,
#93453,#93454,#93455,#93456,#93457),.UNSPECIFIED.,.F.,.F.,(4,1,1,1,1,1,
1,4),(210.486707790517,211.237739550417,212.237396013462,213.237052476506,
214.236708939551,215.236365402595,216.236021865639,216.769893097696),
 .UNSPECIFIED.);
#2141=B_SPLINE_CURVE_WITH_KNOTS('',3,(#93462,#93463,#93464,#93465,#93466,
#93467,#93468,#93469,#93470,#93471),.UNSPECIFIED.,.F.,.F.,(4,1,1,1,1,1,
1,4),(204.203522483337,204.505846327498,205.505280594232,206.504714860966,
207.5041491277,208.503583394434,209.503017661168,210.486707790516),
 .UNSPECIFIED.);
#2142=B_SPLINE_CURVE_WITH_KNOTS('',3,(#93472,#93473,#93474,#93475,#93476,
#93477,#93478,#93479,#93480,#93481,#93482),.UNSPECIFIED.,.F.,.F.,(4,1,1,
1,1,1,1,1,4),(204.203522483337,204.240144309106,205.239800772151,206.239457235195,
207.23911369824,208.238770161284,209.238426624329,210.238083087373,210.486707790517),
 .UNSPECIFIED.);
#2143=B_SPLINE_CURVE_WITH_KNOTS('',3,(#93487,#93488,#93489,#93490,#93491,
#93492,#93493,#93494,#93495,#93496),.UNSPECIFIED.,.F.,.F.,(4,1,1,1,1,1,
1,4),(197.920337176157,198.509240727093,199.508674993828,200.508109260562,
201.507543527296,202.50697779403,203.506412060764,204.203522483337),
 .UNSPECIFIED.);
#2144=B_SPLINE_CURVE_WITH_KNOTS('',3,(#93497,#93498,#93499,#93500,#93501,
#93502,#93503,#93504,#93505,#93506),.UNSPECIFIED.,.F.,.F.,(4,1,1,1,1,1,
1,4),(197.920337176157,198.24220553084,199.241861993884,200.241518456929,
201.241174919973,202.240831383018,203.240487846062,204.203522483337),
 .UNSPECIFIED.);
#2145=B_SPLINE_CURVE_WITH_KNOTS('',3,(#93511,#93512,#93513,#93514,#93515,
#93516,#93517,#93518,#93519,#93520),.UNSPECIFIED.,.F.,.F.,(4,1,1,1,1,1,
1,4),(191.637151868978,192.512635126689,193.512069393423,194.511503660157,
195.510937926891,196.510372193625,197.509806460359,197.920337176157),
 .UNSPECIFIED.);
#2146=B_SPLINE_CURVE_WITH_KNOTS('',3,(#93521,#93522,#93523,#93524,#93525,
#93526,#93527,#93528,#93529,#93530),.UNSPECIFIED.,.F.,.F.,(4,1,1,1,1,1,
1,4),(191.637151868978,192.244266752574,193.243923215618,194.243579678662,
195.243236141707,196.242892604751,197.242549067796,197.920337176157),
 .UNSPECIFIED.);
#2147=B_SPLINE_CURVE_WITH_KNOTS('',3,(#93535,#93536,#93537,#93538,#93539,
#93540,#93541,#93542,#93543,#93544,#93545),.UNSPECIFIED.,.F.,.F.,(4,1,1,
1,1,1,1,1,4),(185.353966561798,185.51659525955,186.516029526284,187.515463793018,
188.514898059753,189.514332326487,190.513766593221,191.513200859955,191.637151868978),
 .UNSPECIFIED.);
#2148=B_SPLINE_CURVE_WITH_KNOTS('',3,(#93546,#93547,#93548,#93549,#93550,
#93551,#93552,#93553,#93554,#93555),.UNSPECIFIED.,.F.,.F.,(4,1,1,1,1,1,
1,4),(185.353966561798,186.246327974307,187.245984437351,188.245640900396,
189.24529736344,190.244953826485,191.244610289529,191.637151868978),
 .UNSPECIFIED.);
#2149=B_SPLINE_CURVE_WITH_KNOTS('',3,(#93560,#93561,#93562,#93563,#93564,
#93565,#93566,#93567,#93568,#93569),.UNSPECIFIED.,.F.,.F.,(4,1,1,1,1,1,
1,4),(179.070781254618,179.519989659146,180.51942392588,181.518858192614,
182.518292459348,183.517726726082,184.517160992816,185.353966561798),
 .UNSPECIFIED.);
#2150=B_SPLINE_CURVE_WITH_KNOTS('',3,(#93570,#93571,#93572,#93573,#93574,
#93575,#93576,#93577,#93578,#93579,#93580),.UNSPECIFIED.,.F.,.F.,(4,1,1,
1,1,1,1,1,4),(179.070781254619,179.248732732996,180.248389196041,181.248045659085,
182.247702122129,183.247358585174,184.247015048218,185.246671511263,185.353966561798),
 .UNSPECIFIED.);
#2151=B_SPLINE_CURVE_WITH_KNOTS('',3,(#93585,#93586,#93587,#93588,#93589,
#93590,#93591,#93592,#93593,#93594),.UNSPECIFIED.,.F.,.F.,(4,1,1,1,1,1,
1,4),(172.787595947439,173.523384058741,174.522818325475,175.522252592209,
176.521686858943,177.521121125678,178.520555392412,179.070781254618),
 .UNSPECIFIED.);
#2152=B_SPLINE_CURVE_WITH_KNOTS('',3,(#93595,#93596,#93597,#93598,#93599,
#93600,#93601,#93602,#93603,#93604),.UNSPECIFIED.,.F.,.F.,(4,1,1,1,1,1,
1,4),(172.787595947439,173.25079395473,174.250450417774,175.250106880818,
176.249763343863,177.249419806907,178.249076269952,179.070781254619),
 .UNSPECIFIED.);
#2153=B_SPLINE_CURVE_WITH_KNOTS('',3,(#93609,#93610,#93611,#93612,#93613,
#93614,#93615,#93616,#93617,#93618,#93619),.UNSPECIFIED.,.F.,.F.,(4,1,1,
1,1,1,1,1,4),(166.504410640259,166.527344191603,167.526778458337,168.526212725071,
169.525646991805,170.525081258539,171.524515525273,172.523949792007,172.787595947439),
 .UNSPECIFIED.);
#2154=B_SPLINE_CURVE_WITH_KNOTS('',3,(#93620,#93621,#93622,#93623,#93624,
#93625,#93626,#93627,#93628,#93629),.UNSPECIFIED.,.F.,.F.,(4,1,1,1,1,1,
1,4),(166.50441064026,167.252855176463,168.252511639508,169.252168102552,
170.251824565596,171.251481028641,172.251137491685,172.787595947439),
 .UNSPECIFIED.);
#2155=B_SPLINE_CURVE_WITH_KNOTS('',3,(#93634,#93635,#93636,#93637,#93638,
#93639,#93640,#93641,#93642,#93643),.UNSPECIFIED.,.F.,.F.,(4,1,1,1,1,1,
1,4),(160.22122533308,160.530738591198,161.530172857932,162.529607124666,
163.5290413914,164.528475658134,165.527909924869,166.504410640259),
 .UNSPECIFIED.);
#2156=B_SPLINE_CURVE_WITH_KNOTS('',3,(#93644,#93645,#93646,#93647,#93648,
#93649,#93650,#93651,#93652,#93653,#93654),.UNSPECIFIED.,.F.,.F.,(4,1,1,
1,1,1,1,1,4),(160.22122533308,160.255259935152,161.254916398197,162.254572861241,
163.254229324286,164.25388578733,165.253542250374,166.253198713419,166.50441064026),
 .UNSPECIFIED.);
#2157=B_SPLINE_CURVE_WITH_KNOTS('',3,(#93659,#93660,#93661,#93662,#93663,
#93664,#93665,#93666,#93667,#93668),.UNSPECIFIED.,.F.,.F.,(4,1,1,1,1,1,
1,4),(153.9380400259,154.534132990794,155.533567257528,156.533001524262,
157.532435790996,158.53187005773,159.531304324464,160.22122533308),
 .UNSPECIFIED.);
#2158=B_SPLINE_CURVE_WITH_KNOTS('',3,(#93669,#93670,#93671,#93672,#93673,
#93674,#93675,#93676,#93677,#93678),.UNSPECIFIED.,.F.,.F.,(4,1,1,1,1,1,
1,4),(153.9380400259,154.257321156886,155.25697761993,156.256634082975,
157.256290546019,158.255947009063,159.255603472108,160.22122533308),
 .UNSPECIFIED.);
#2159=B_SPLINE_CURVE_WITH_KNOTS('',3,(#93683,#93684,#93685,#93686,#93687,
#93688,#93689,#93690,#93691,#93692),.UNSPECIFIED.,.F.,.F.,(4,1,1,1,1,1,
1,4),(147.654854718721,148.537527390389,149.536961657123,150.536395923857,
151.535830190591,152.535264457325,153.534698724059,153.9380400259),
 .UNSPECIFIED.);
#2160=B_SPLINE_CURVE_WITH_KNOTS('',3,(#93693,#93694,#93695,#93696,#93697,
#93698,#93699,#93700,#93701,#93702),.UNSPECIFIED.,.F.,.F.,(4,1,1,1,1,1,
1,4),(147.654854718721,148.259382378619,149.259038841664,150.258695304708,
151.258351767753,152.258008230797,153.257664693841,153.9380400259),
 .UNSPECIFIED.);
#2161=B_SPLINE_CURVE_WITH_KNOTS('',3,(#93707,#93708,#93709,#93710,#93711,
#93712,#93713,#93714,#93715,#93716,#93717),.UNSPECIFIED.,.F.,.F.,(4,1,1,
1,1,1,1,1,4),(141.371669411541,141.54148752325,142.540921789984,143.540356056719,
144.539790323453,145.539224590187,146.538658856921,147.538093123655,147.654854718721),
 .UNSPECIFIED.);
#2162=B_SPLINE_CURVE_WITH_KNOTS('',3,(#93718,#93719,#93720,#93721,#93722,
#93723,#93724,#93725,#93726,#93727),.UNSPECIFIED.,.F.,.F.,(4,1,1,1,1,1,
1,4),(141.371669411541,142.261443600353,143.261100063397,144.260756526442,
145.260412989486,146.260069452531,147.259725915575,147.654854718721),
 .UNSPECIFIED.);
#2163=B_SPLINE_CURVE_WITH_KNOTS('',3,(#93732,#93733,#93734,#93735,#93736,
#93737,#93738,#93739,#93740,#93741),.UNSPECIFIED.,.F.,.F.,(4,1,1,1,1,1,
1,4),(135.088484104362,135.544881922846,136.54431618958,137.543750456314,
138.543184723048,139.542618989782,140.542053256516,141.371669411541),
 .UNSPECIFIED.);
#2164=B_SPLINE_CURVE_WITH_KNOTS('',3,(#93742,#93743,#93744,#93745,#93746,
#93747,#93748,#93749,#93750,#93751,#93752),.UNSPECIFIED.,.F.,.F.,(4,1,1,
1,1,1,1,1,4),(135.088484104362,135.263848359042,136.263504822086,137.263161285131,
138.262817748175,139.26247421122,140.262130674264,141.261787137308,141.371669411541),
 .UNSPECIFIED.);
#2165=B_SPLINE_CURVE_WITH_KNOTS('',3,(#93757,#93758,#93759,#93760,#93761,
#93762,#93763,#93764,#93765,#93766),.UNSPECIFIED.,.F.,.F.,(4,1,1,1,1,1,
1,4),(128.805298797182,129.548276322441,130.547710589175,131.54714485591,
132.546579122644,133.546013389378,134.545447656112,135.088484104362),
 .UNSPECIFIED.);
#2166=B_SPLINE_CURVE_WITH_KNOTS('',3,(#93767,#93768,#93769,#93770,#93771,
#93772,#93773,#93774,#93775,#93776),.UNSPECIFIED.,.F.,.F.,(4,1,1,1,1,1,
1,4),(128.805298797182,129.265909580775,130.26556604382,131.265222506864,
132.264878969909,133.264535432953,134.264191895998,135.088484104362),
 .UNSPECIFIED.);
#2167=B_SPLINE_CURVE_WITH_KNOTS('',3,(#93781,#93782,#93783,#93784,#93785,
#93786,#93787,#93788,#93789,#93790,#93791),.UNSPECIFIED.,.F.,.F.,(4,1,1,
1,1,1,1,1,4),(122.522113490002,122.552236455303,123.551670722037,124.551104988771,
125.550539255505,126.549973522239,127.549407788973,128.548842055707,128.805298797182),
 .UNSPECIFIED.);
#2168=B_SPLINE_CURVE_WITH_KNOTS('',3,(#93792,#93793,#93794,#93795,#93796,
#93797,#93798,#93799,#93800,#93801),.UNSPECIFIED.,.F.,.F.,(4,1,1,1,1,1,
1,4),(122.522113490003,123.267970802509,124.267627265553,125.267283728598,
126.266940191642,127.266596654687,128.266253117731,128.805298797182),
 .UNSPECIFIED.);
#2169=B_SPLINE_CURVE_WITH_KNOTS('',3,(#93806,#93807,#93808,#93809,#93810,
#93811,#93812,#93813,#93814,#93815),.UNSPECIFIED.,.F.,.F.,(4,1,1,1,1,1,
1,4),(116.238928182823,116.555630854898,117.555065121632,118.554499388366,
119.5539336551,120.553367921835,121.552802188569,122.522113490002),
 .UNSPECIFIED.);
#2170=B_SPLINE_CURVE_WITH_KNOTS('',3,(#93816,#93817,#93818,#93819,#93820,
#93821,#93822,#93823,#93824,#93825,#93826),.UNSPECIFIED.,.F.,.F.,(4,1,1,
1,1,1,1,1,4),(116.238928182823,116.270375561198,117.270032024243,118.269688487287,
119.269344950331,120.269001413376,121.26865787642,122.268314339465,122.522113490003),
 .UNSPECIFIED.);
#2171=B_SPLINE_CURVE_WITH_KNOTS('',3,(#93831,#93832,#93833,#93834,#93835,
#93836,#93837,#93838,#93839,#93840),.UNSPECIFIED.,.F.,.F.,(4,1,1,1,1,1,
1,4),(109.955742875643,110.559025254494,111.558459521228,112.557893787962,
113.557328054696,114.55676232143,115.556196588164,116.238928182823),
 .UNSPECIFIED.);
#2172=B_SPLINE_CURVE_WITH_KNOTS('',3,(#93841,#93842,#93843,#93844,#93845,
#93846,#93847,#93848,#93849,#93850),.UNSPECIFIED.,.F.,.F.,(4,1,1,1,1,1,
1,4),(109.955742875643,110.272436782932,111.272093245976,112.27174970902,
113.271406172065,114.271062635109,115.270719098154,116.238928182823),
 .UNSPECIFIED.);
#2173=B_SPLINE_CURVE_WITH_KNOTS('',3,(#93855,#93856,#93857,#93858,#93859,
#93860,#93861,#93862,#93863,#93864),.UNSPECIFIED.,.F.,.F.,(4,1,1,1,1,1,
1,4),(103.672557568464,104.562419654089,105.561853920823,106.561288187557,
107.560722454291,108.560156721025,109.55959098776,109.955742875643),
 .UNSPECIFIED.);
#2174=B_SPLINE_CURVE_WITH_KNOTS('',3,(#93865,#93866,#93867,#93868,#93869,
#93870,#93871,#93872,#93873,#93874),.UNSPECIFIED.,.F.,.F.,(4,1,1,1,1,1,
1,4),(103.672557568464,104.274498004665,105.27415446771,106.273810930754,
107.273467393798,108.273123856843,109.272780319887,109.955742875643),
 .UNSPECIFIED.);
#2175=B_SPLINE_CURVE_WITH_KNOTS('',3,(#93879,#93880,#93881,#93882,#93883,
#93884,#93885,#93886,#93887,#93888,#93889),.UNSPECIFIED.,.F.,.F.,(4,1,1,
1,1,1,1,1,4),(97.389372261284,97.5663797869505,98.5658140536846,99.5652483204187,
100.564682587153,101.564116853887,102.563551120621,103.562985387355,103.672557568464),
 .UNSPECIFIED.);
#2176=B_SPLINE_CURVE_WITH_KNOTS('',3,(#93890,#93891,#93892,#93893,#93894,
#93895,#93896,#93897,#93898,#93899),.UNSPECIFIED.,.F.,.F.,(4,1,1,1,1,1,
1,4),(97.3893722612842,98.2765592263987,99.2762156894431,100.275872152488,
101.275528615532,102.275185078576,103.274841541621,103.672557568464),
 .UNSPECIFIED.);
#2177=B_SPLINE_CURVE_WITH_KNOTS('',3,(#93904,#93905,#93906,#93907,#93908,
#93909,#93910,#93911,#93912,#93913),.UNSPECIFIED.,.F.,.F.,(4,1,1,1,1,1,
1,4),(91.1061869541044,91.569774186546,92.5692084532801,93.5686427200142,
94.5680769867483,95.5675112534823,96.5669455202164,97.389372261284),
 .UNSPECIFIED.);
#2178=B_SPLINE_CURVE_WITH_KNOTS('',3,(#93914,#93915,#93916,#93917,#93918,
#93919,#93920,#93921,#93922,#93923,#93924),.UNSPECIFIED.,.F.,.F.,(4,1,1,
1,1,1,1,1,4),(91.1061869541046,91.2789639850878,92.2786204481322,93.2782769111766,
94.277933374221,95.2775898372655,96.2772463003099,97.2769027633543,97.3893722612842),
 .UNSPECIFIED.);
#2179=B_SPLINE_CURVE_WITH_KNOTS('',3,(#93929,#93930,#93931,#93932,#93933,
#93934,#93935,#93936,#93937,#93938),.UNSPECIFIED.,.F.,.F.,(4,1,1,1,1,1,
1,4),(84.8230016469248,85.5731685861415,86.5726028528755,87.5720371196096,
88.5714713863437,89.5709056530778,90.5703399198119,91.1061869541044),
 .UNSPECIFIED.);
#2180=B_SPLINE_CURVE_WITH_KNOTS('',3,(#93939,#93940,#93941,#93942,#93943,
#93944,#93945,#93946,#93947,#93948),.UNSPECIFIED.,.F.,.F.,(4,1,1,1,1,1,
1,4),(84.823001646925,85.2810252068213,86.2806816698657,87.2803381329102,
88.2799945959546,89.279651058999,90.2793075220434,91.1061869541046),
 .UNSPECIFIED.);
#2181=B_SPLINE_CURVE_WITH_KNOTS('',3,(#93953,#93954,#93955,#93956,#93957,
#93958,#93959,#93960,#93961,#93962,#93963),.UNSPECIFIED.,.F.,.F.,(4,1,1,
1,1,1,1,1,4),(78.5398163397452,78.5771287190028,79.5765629857369,80.575997252471,
81.5754315192051,82.5748657859392,83.5743000526733,84.5737343194074,84.8230016469248),
 .UNSPECIFIED.);
#2182=B_SPLINE_CURVE_WITH_KNOTS('',3,(#93964,#93965,#93966,#93967,#93968,
#93969,#93970,#93971,#93972,#93973),.UNSPECIFIED.,.F.,.F.,(4,1,1,1,1,1,
1,4),(78.5398163397454,79.2830864285549,80.2827428915993,81.2823993546437,
82.2820558176881,83.2817122807325,84.2813687437769,84.823001646925),
 .UNSPECIFIED.);
#2183=B_SPLINE_CURVE_WITH_KNOTS('',3,(#93978,#93979,#93980,#93981,#93982,
#93983,#93984,#93985,#93986,#93987),.UNSPECIFIED.,.F.,.F.,(4,1,1,1,1,1,
1,4),(72.2566310325657,72.5805231185983,73.5799573853324,74.5793916520665,
75.5788259188006,76.5782601855347,77.5776944522688,78.5398163397452),
 .UNSPECIFIED.);
#2184=B_SPLINE_CURVE_WITH_KNOTS('',3,(#93988,#93989,#93990,#93991,#93992,
#93993,#93994,#93995,#93996,#93997,#93998),.UNSPECIFIED.,.F.,.F.,(4,1,1,
1,1,1,1,1,4),(72.2566310325658,72.285491187244,73.2851476502884,74.2848041133328,
75.2844605763772,76.2841170394216,77.283773502466,78.2834299655104,78.5398163397454),
 .UNSPECIFIED.);
#2185=B_SPLINE_CURVE_WITH_KNOTS('',3,(#94003,#94004,#94005,#94006,#94007,
#94008,#94009,#94010,#94011,#94012),.UNSPECIFIED.,.F.,.F.,(4,1,1,1,1,1,
1,4),(65.973445725386,66.5839175181938,67.5833517849279,68.582786051662,
69.582220318396,70.5816545851301,71.5810888518642,72.2566310325657),
 .UNSPECIFIED.);
#2186=B_SPLINE_CURVE_WITH_KNOTS('',3,(#94013,#94014,#94015,#94016,#94017,
#94018,#94019,#94020,#94021,#94022),.UNSPECIFIED.,.F.,.F.,(4,1,1,1,1,1,
1,4),(65.9734457253862,66.2875524089775,67.2872088720219,68.2868653350663,
69.2865217981107,70.2861782611551,71.2858347241996,72.2566310325658),
 .UNSPECIFIED.);
#2187=B_SPLINE_CURVE_WITH_KNOTS('',3,(#94027,#94028,#94029,#94030,#94031,
#94032,#94033,#94034,#94035,#94036),.UNSPECIFIED.,.F.,.F.,(4,1,1,1,1,1,
1,4),(59.6902604182065,60.5873119177892,61.5867461845233,62.5861804512574,
63.5856147179915,64.5850489847256,65.5844832514597,65.973445725386),
 .UNSPECIFIED.);
#2188=B_SPLINE_CURVE_WITH_KNOTS('',3,(#94037,#94038,#94039,#94040,#94041,
#94042,#94043,#94044,#94045,#94046),.UNSPECIFIED.,.F.,.F.,(4,1,1,1,1,1,
1,4),(59.6902604182066,60.289613630711,61.2892700937554,62.2889265567998,
63.2885830198443,64.2882394828887,65.2878959459331,65.9734457253862),
 .UNSPECIFIED.);
#2189=B_SPLINE_CURVE_WITH_KNOTS('',3,(#94051,#94052,#94053,#94054,#94055,
#94056,#94057,#94058,#94059,#94060,#94061),.UNSPECIFIED.,.F.,.F.,(4,1,1,
1,1,1,1,1,4),(53.4070751110269,53.5912720506506,54.5907063173847,55.5901405841188,
56.5895748508529,57.589009117587,58.5884433843211,59.5878776510552,59.6902604182065),
 .UNSPECIFIED.);
#2190=B_SPLINE_CURVE_WITH_KNOTS('',3,(#94062,#94063,#94064,#94065,#94066,
#94067,#94068,#94069,#94070,#94071),.UNSPECIFIED.,.F.,.F.,(4,1,1,1,1,1,
1,4),(53.407075111027,54.2916748524445,55.2913313154889,56.2909877785334,
57.2906442415778,58.2903007046222,59.2899571676666,59.6902604182066),
 .UNSPECIFIED.);
#2191=B_SPLINE_CURVE_WITH_KNOTS('',3,(#94076,#94077,#94078,#94079,#94080,
#94081,#94082,#94083,#94084,#94085),.UNSPECIFIED.,.F.,.F.,(4,1,1,1,1,1,
1,4),(47.1238898038473,47.5946664502461,48.5941007169802,49.5935349837143,
50.5929692504484,51.5924035171824,52.5918377839165,53.4070751110269),
 .UNSPECIFIED.);
#2192=B_SPLINE_CURVE_WITH_KNOTS('',3,(#94086,#94087,#94088,#94089,#94090,
#94091,#94092,#94093,#94094,#94095,#94096),.UNSPECIFIED.,.F.,.F.,(4,1,1,
1,1,1,1,1,4),(47.1238898038474,47.2940796111337,48.2937360741781,49.2933925372225,
50.2930490002669,51.2927054633113,52.2923619263557,53.2920183894001,53.407075111027),
 .UNSPECIFIED.);
#2193=B_SPLINE_CURVE_WITH_KNOTS('',3,(#94101,#94102,#94103,#94104,#94105,
#94106,#94107,#94108,#94109,#94110),.UNSPECIFIED.,.F.,.F.,(4,1,1,1,1,1,
1,4),(40.8407044966677,41.5980608498416,42.5974951165757,43.5969293833097,
44.5963636500438,45.5957979167779,46.595232183512,47.1238898038473),
 .UNSPECIFIED.);
#2194=B_SPLINE_CURVE_WITH_KNOTS('',3,(#94111,#94112,#94113,#94114,#94115,
#94116,#94117,#94118,#94119,#94120),.UNSPECIFIED.,.F.,.F.,(4,1,1,1,1,1,
1,4),(40.8407044966679,41.2961408328672,42.2957972959116,43.295453758956,
44.2951102220004,45.2947666850448,46.2944231480892,47.1238898038474),
 .UNSPECIFIED.);
#2195=B_SPLINE_CURVE_WITH_KNOTS('',3,(#94125,#94126,#94127,#94128,#94129,
#94130,#94131,#94132,#94133,#94134,#94135),.UNSPECIFIED.,.F.,.F.,(4,1,1,
1,1,1,1,1,4),(34.5575191894881,34.6020209827029,35.601455249437,36.6008895161711,
37.6003237829052,38.5997580496393,39.5991923163734,40.5986265831075,40.8407044966677),
 .UNSPECIFIED.);
#2196=B_SPLINE_CURVE_WITH_KNOTS('',3,(#94136,#94137,#94138,#94139,#94140,
#94141,#94142,#94143,#94144,#94145),.UNSPECIFIED.,.F.,.F.,(4,1,1,1,1,1,
1,4),(34.5575191894883,35.2982020546007,36.2978585176451,37.2975149806895,
38.2971714437339,39.2968279067783,40.2964843698228,40.8407044966679),
 .UNSPECIFIED.);
#2197=B_SPLINE_CURVE_WITH_KNOTS('',3,(#94150,#94151,#94152,#94153,#94154,
#94155,#94156,#94157,#94158,#94159),.UNSPECIFIED.,.F.,.F.,(4,1,1,1,1,1,
1,4),(28.2743338823085,28.6054153822984,29.6048496490325,30.6042839157666,
31.6037181825007,32.6031524492348,33.6025867159689,34.5575191894881),
 .UNSPECIFIED.);
#2198=B_SPLINE_CURVE_WITH_KNOTS('',3,(#94160,#94161,#94162,#94163,#94164,
#94165,#94166,#94167,#94168,#94169,#94170),.UNSPECIFIED.,.F.,.F.,(4,1,1,
1,1,1,1,1,4),(28.2743338823087,28.3006068132898,29.3002632763342,30.2999197393786,
31.299576202423,32.2992326654675,33.2988891285119,34.2985455915563,34.5575191894883),
 .UNSPECIFIED.);
#2199=B_SPLINE_CURVE_WITH_KNOTS('',3,(#94175,#94176,#94177,#94178,#94179,
#94180,#94181,#94182,#94183,#94184),.UNSPECIFIED.,.F.,.F.,(4,1,1,1,1,1,
1,4),(21.9911485751289,22.6088097818939,23.608244048628,24.6076783153621,
25.6071125820962,26.6065468488302,27.6059811155643,28.2743338823085),
 .UNSPECIFIED.);
#2200=B_SPLINE_CURVE_WITH_KNOTS('',3,(#94185,#94186,#94187,#94188,#94189,
#94190,#94191,#94192,#94193,#94194),.UNSPECIFIED.,.F.,.F.,(4,1,1,1,1,1,
1,4),(21.9911485751291,22.3026680350233,23.3023244980677,24.3019809611122,
25.3016374241566,26.301293887201,27.3009503502454,28.2743338823087),
 .UNSPECIFIED.);
#2201=B_SPLINE_CURVE_WITH_KNOTS('',3,(#94199,#94200,#94201,#94202,#94203,
#94204,#94205,#94206,#94207,#94208),.UNSPECIFIED.,.F.,.F.,(4,1,1,1,1,1,
1,4),(15.7079632679493,16.6122041814894,17.6116384482234,18.6110727149575,
19.6105069816916,20.6099412484257,21.6093755151598,21.9911485751289),
 .UNSPECIFIED.);
#2202=B_SPLINE_CURVE_WITH_KNOTS('',3,(#94209,#94210,#94211,#94212,#94213,
#94214,#94215,#94216,#94217,#94218),.UNSPECIFIED.,.F.,.F.,(4,1,1,1,1,1,
1,4),(15.7079632679495,16.3047292567569,17.3043857198013,18.3040421828457,
19.3036986458901,20.3033551089345,21.3030115719789,21.9911485751291),
 .UNSPECIFIED.);
#2203=B_SPLINE_CURVE_WITH_KNOTS('',3,(#94221,#94222,#94223,#94224,#94225,
#94226,#94227,#94228,#94229,#94230,#94231,#94232,#94233,#94234,#94235,#94236,
#94237,#94238,#94239,#94240,#94241,#94242,#94243,#94244,#94245,#94246,#94247,
#94248,#94249,#94250,#94251,#94252,#94253,#94254,#94255,#94256,#94257,#94258,
#94259,#94260,#94261,#94262,#94263,#94264,#94265,#94266,#94267,#94268,#94269,
#94270,#94271,#94272,#94273,#94274,#94275,#94276,#94277,#94278,#94279,#94280,
#94281,#94282,#94283,#94284,#94285,#94286,#94287,#94288,#94289,#94290,#94291,
#94292,#94293,#94294,#94295,#94296,#94297,#94298,#94299,#94300,#94301,#94302,
#94303,#94304,#94305,#94306,#94307,#94308,#94309,#94310,#94311,#94312,#94313,
#94314,#94315,#94316,#94317,#94318,#94319,#94320,#94321,#94322,#94323,#94324,
#94325,#94326,#94327,#94328,#94329,#94330,#94331,#94332,#94333,#94334,#94335,
#94336,#94337,#94338,#94339,#94340,#94341,#94342,#94343,#94344,#94345,#94346,
#94347,#94348,#94349,#94350,#94351,#94352,#94353,#94354,#94355,#94356,#94357,
#94358,#94359,#94360,#94361,#94362,#94363,#94364,#94365,#94366,#94367,#94368,
#94369,#94370,#94371,#94372,#94373,#94374,#94375,#94376,#94377,#94378,#94379,
#94380,#94381,#94382,#94383,#94384,#94385,#94386,#94387,#94388,#94389,#94390,
#94391,#94392,#94393,#94394,#94395,#94396,#94397,#94398,#94399,#94400,#94401,
#94402,#94403,#94404,#94405,#94406,#94407,#94408,#94409,#94410,#94411,#94412,
#94413,#94414,#94415,#94416,#94417,#94418,#94419,#94420,#94421,#94422,#94423,
#94424,#94425,#94426,#94427,#94428,#94429,#94430,#94431,#94432,#94433,#94434,
#94435,#94436,#94437,#94438,#94439,#94440),.UNSPECIFIED.,.F.,.F.,(4,3,3,
3,3,3,3,3,3,3,3,3,3,3,3,3,3,3,3,3,3,3,3,3,3,3,3,3,3,3,3,3,3,3,3,3,3,3,3,
3,3,3,3,3,3,3,3,3,3,3,3,3,3,3,3,3,3,3,3,3,3,3,3,3,3,3,3,3,3,3,3,3,3,4),
(-1.51155304937021,-1.4867986341959,-1.46138663739248,-1.44926455530148,
-1.44198566695448,-1.43723139879395,-1.41129478811863,-1.38512863143085,
-1.36856346812421,-1.36399889752397,-1.33754355936836,-1.3112352326583,
-1.28933427829745,-1.27838380111703,-1.27269882676012,-1.26908809076141,
-1.2674333239366,-1.24208236385033,-1.21599084244255,-1.19063509328497,
-1.17954195302853,-1.17503012203446,-1.17142816095389,-1.1446505933564,
-1.11755538034957,-1.09145274755766,-1.08166426026069,-1.07535319071695,
-1.07096221841427,-1.04359919185664,-1.0166438108283,-1.01314484918191,
-0.98625222361255,-0.977200099492379,-0.971299394604424,-0.943514789093585,
-0.91597930726476,-0.888306650336328,-0.877800787937313,-0.872097086036976,
-0.867897812831546,-0.840032330792451,-0.812153981120299,-0.784705375823936,
-0.774482071494278,-0.768979249185249,-0.764756614985413,-0.749022550517709,
-0.721911653675323,-0.694106265473056,-0.66670330991581,-0.66275818307286,
-0.63460112991406,-0.606031897351057,-0.577483417867562,-0.564658318261003,
-0.558122567947299,-0.553679410026387,-0.524793660942482,-0.496363213790454,
-0.474882621015088,-0.459389954623598,-0.450074377816351,-0.44490829563357,
-0.416625100495465,-0.387728608299678,-0.358542858111977,-0.342099995691886,
-0.337681523304568,-0.308264569892219,-0.278761910588203,-0.24982670716456,
-0.226999958751254,-0.219677966287731),.UNSPECIFIED.);
#2204=B_SPLINE_CURVE_WITH_KNOTS('',3,(#94442,#94443,#94444,#94445,#94446,
#94447,#94448,#94449,#94450,#94451,#94452,#94453,#94454,#94455,#94456,#94457,
#94458,#94459,#94460,#94461,#94462,#94463,#94464,#94465,#94466,#94467,#94468,
#94469,#94470,#94471,#94472,#94473,#94474,#94475,#94476,#94477,#94478,#94479,
#94480,#94481,#94482,#94483,#94484,#94485,#94486,#94487,#94488,#94489,#94490,
#94491,#94492,#94493,#94494,#94495,#94496,#94497,#94498,#94499,#94500,#94501,
#94502,#94503,#94504,#94505),.UNSPECIFIED.,.F.,.F.,(4,3,3,3,3,3,3,3,3,3,
3,3,3,3,3,3,3,3,3,3,3,4),(-0.410648750431908,-0.381299054024905,-0.351414515897952,
-0.323345095993572,-0.314306783515406,-0.307608364286677,-0.302981488408948,
-0.275425436471569,-0.261760901517091,-0.233519805708424,-0.204329829994871,
-0.19862199232604,-0.194416727168087,-0.167215385011146,-0.140139152408172,
-0.113537500932685,-0.0982440424338316,-0.093782918547421,-0.0680367361001279,
-0.0426830224365629,-0.0180658198696843,0.),.UNSPECIFIED.);
#2205=B_SPLINE_CURVE_WITH_KNOTS('',3,(#94508,#94509,#94510,#94511,#94512,
#94513,#94514,#94515,#94516,#94517,#94518,#94519,#94520,#94521,#94522,#94523,
#94524,#94525,#94526,#94527,#94528,#94529,#94530,#94531,#94532,#94533,#94534,
#94535,#94536,#94537,#94538),.UNSPECIFIED.,.F.,.F.,(4,3,3,3,3,3,3,3,3,3,
4),(-0.219677966287731,-0.190969587719715,-0.161999262949595,-0.132480874583944,
-0.12283591709848,-0.116345167945464,-0.111098549044977,-0.0814759057122038,
-0.0514613231781522,-0.0214845368738984,0.),.UNSPECIFIED.);
#2206=B_SPLINE_CURVE_WITH_KNOTS('',3,(#95803,#95804,#95805,#95806,#95807,
#95808,#95809,#95810),.UNSPECIFIED.,.F.,.F.,(4,1,1,1,1,4),(11.6150328478189,
12.614467114553,13.6139013812871,14.6133356480212,15.6127699147553,15.7079632679493),
 .UNSPECIFIED.);
#2207=B_SPLINE_CURVE_WITH_KNOTS('',3,(#95811,#95812,#95813,#95814,#95815,
#95816,#95817,#95818,#95819,#95820,#95821,#95822,#95823,#95824,#95825,#95826,
#95827,#95828,#95829,#95830,#95831,#95832,#95833,#95834,#95835,#95836,#95837,
#95838,#95839,#95840,#95841,#95842,#95843,#95844,#95845,#95846,#95847,#95848,
#95849,#95850,#95851,#95852,#95853,#95854,#95855,#95856,#95857,#95858,#95859,
#95860,#95861,#95862,#95863,#95864,#95865,#95866,#95867,#95868,#95869,#95870,
#95871,#95872,#95873,#95874,#95875,#95876,#95877,#95878,#95879,#95880,#95881,
#95882,#95883,#95884,#95885,#95886,#95887,#95888,#95889,#95890,#95891,#95892,
#95893,#95894,#95895,#95896,#95897,#95898,#95899,#95900,#95901,#95902,#95903,
#95904),.UNSPECIFIED.,.F.,.F.,(4,3,3,3,3,3,3,3,3,3,3,3,3,3,3,3,3,3,3,3,
3,3,3,3,3,3,3,3,3,3,3,4),(-0.552745378375083,-0.532258650239557,-0.502894553245675,
-0.487265296433606,-0.479829702030211,-0.472037404847164,-0.442982148603388,
-0.419212685559536,-0.408392313611654,-0.401996182412567,-0.397451439969464,
-0.369143868093339,-0.340064512133147,-0.312946502615706,-0.297653419419827,
-0.291369319786409,-0.264567360030501,-0.252826444252568,-0.225465117340262,
-0.197281977672729,-0.192689798637887,-0.188527732452548,-0.16188748095911,
-0.135285222784929,-0.109106515899472,-0.100476530872862,-0.0940367162764452,
-0.0901450819999103,-0.0646019269342215,-0.0394615527910846,-0.015105273416719,
0.),.UNSPECIFIED.);
#2208=B_SPLINE_CURVE_WITH_KNOTS('',3,(#95905,#95906,#95907,#95908,#95909,
#95910,#95911,#95912,#95913,#95914,#95915,#95916,#95917,#95918,#95919,#95920,
#95921,#95922,#95923),.UNSPECIFIED.,.F.,.F.,(4,3,3,3,3,3,4),(-310.309142974525,
-309.824622687567,-308.825188420833,-307.825754154099,-306.826319887365,
-305.826885620631,-305.68582516475),.UNSPECIFIED.);
#2209=B_SPLINE_CURVE_WITH_KNOTS('',3,(#95926,#95927,#95928,#95929,#95930,
#95931,#95932,#95933,#95934),.UNSPECIFIED.,.F.,.F.,(4,1,1,1,1,1,4),(10.3761157273108,
11.3064469415348,12.3061034045792,13.3057598676236,14.305416330668,15.3050727937124,
15.7079632679495),.UNSPECIFIED.);
#2210=B_SPLINE_CURVE_WITH_KNOTS('',3,(#97204,#97205,#97206,#97207,#97208,
#97209,#97210,#97211,#97212,#97213,#97214,#97215,#97216,#97217,#97218,#97219,
#97220,#97221,#97222,#97223,#97224,#97225),.UNSPECIFIED.,.F.,.F.,(4,3,3,
3,3,3,3,4),(302.710195152989,302.895908302457,303.895564765501,304.895221228546,
305.89487769159,306.894534154635,307.894190617679,308.240504799617),
 .UNSPECIFIED.);
#2211=B_SPLINE_CURVE_WITH_KNOTS('',3,(#97226,#97227,#97228,#97229,#97230,
#97231,#97232,#97233,#97234,#97235,#97236,#97237,#97238,#97239,#97240,#97241,
#97242,#97243,#97244,#97245,#97246,#97247,#97248,#97249,#97250,#97251,#97252,
#97253,#97254,#97255,#97256,#97257,#97258,#97259,#97260,#97261,#97262,#97263,
#97264,#97265,#97266,#97267,#97268,#97269,#97270,#97271,#97272,#97273,#97274,
#97275,#97276,#97277,#97278,#97279,#97280,#97281,#97282,#97283,#97284,#97285,
#97286,#97287,#97288,#97289,#97290,#97291,#97292,#97293,#97294,#97295,#97296,
#97297,#97298,#97299,#97300,#97301,#97302,#97303,#97304,#97305,#97306,#97307,
#97308,#97309,#97310,#97311,#97312,#97313),.UNSPECIFIED.,.F.,.F.,(4,3,3,
3,3,3,3,3,3,3,3,3,3,3,3,3,3,3,3,3,3,3,3,3,3,3,3,3,3,4),(-0.555272788399347,
-0.538572946039236,-0.513888794201686,-0.499451161420365,-0.49303522077673,
-0.487943566425205,-0.462157372443835,-0.439748534600925,-0.429096047695605,
-0.424937757521379,-0.398410712364184,-0.371397275485531,-0.34441519227878,
-0.329033061634225,-0.324656870658717,-0.296742049498124,-0.282886669700559,
-0.255957572647936,-0.228482562489743,-0.22261183304744,-0.217969609570416,
-0.190037432453959,-0.161560762906833,-0.132831919803823,-0.116227929828345,
-0.111827184570658,-0.082369349120359,-0.0528160418819264,-0.0238157996808501,
0.),.UNSPECIFIED.);
#2212=SHAPE_REPRESENTATION_RELATIONSHIP('SRR','None',#97605,#2231);
#2213=SHAPE_REPRESENTATION_RELATIONSHIP('SRR','None',#97606,#2232);
#2214=SHAPE_REPRESENTATION_RELATIONSHIP('SRR','None',#97607,#2233);
#2215=SHAPE_REPRESENTATION_RELATIONSHIP('SRR','None',#97608,#2234);
#2216=SHAPE_REPRESENTATION_RELATIONSHIP('SRR','None',#97609,#2235);
#2217=SHAPE_REPRESENTATION_RELATIONSHIP('SRR','None',#97611,#2236);
#2218=SHAPE_REPRESENTATION_RELATIONSHIP('SRR','None',#97612,#2237);
#2219=SHAPE_REPRESENTATION_RELATIONSHIP('SRR','None',#97613,#2238);
#2220=SHAPE_REPRESENTATION_RELATIONSHIP('SRR','None',#97614,#2239);
#2221=SHAPE_REPRESENTATION_RELATIONSHIP('SRR','None',#97615,#2240);
#2222=SHAPE_REPRESENTATION_RELATIONSHIP('SRR','None',#97616,#2241);
#2223=SHAPE_REPRESENTATION_RELATIONSHIP('SRR','None',#97617,#2242);
#2224=SHAPE_REPRESENTATION_RELATIONSHIP('SRR','None',#97618,#2243);
#2225=SHAPE_REPRESENTATION_RELATIONSHIP('SRR','None',#97619,#2244);
#2226=SHAPE_REPRESENTATION_RELATIONSHIP('SRR','None',#97620,#2245);
#2227=SHAPE_REPRESENTATION_RELATIONSHIP('SRR','None',#97621,#2246);
#2228=SHAPE_REPRESENTATION_RELATIONSHIP('SRR','None',#97622,#2247);
#2229=SHAPE_REPRESENTATION_RELATIONSHIP('SRR','None',#97623,#2248);
#2230=SHAPE_REPRESENTATION_RELATIONSHIP('SRR','None',#97624,#2249);
#2231=ADVANCED_BREP_SHAPE_REPRESENTATION('',(#2269),#97455);
#2232=ADVANCED_BREP_SHAPE_REPRESENTATION('',(#2270),#97456);
#2233=ADVANCED_BREP_SHAPE_REPRESENTATION('',(#2271),#97457);
#2234=ADVANCED_BREP_SHAPE_REPRESENTATION('',(#2272),#97458);
#2235=ADVANCED_BREP_SHAPE_REPRESENTATION('',(#2273),#97459);
#2236=ADVANCED_BREP_SHAPE_REPRESENTATION('',(#2274),#97461);
#2237=ADVANCED_BREP_SHAPE_REPRESENTATION('',(#2275),#97462);
#2238=ADVANCED_BREP_SHAPE_REPRESENTATION('',(#2276),#97463);
#2239=ADVANCED_BREP_SHAPE_REPRESENTATION('',(#2277),#97464);
#2240=ADVANCED_BREP_SHAPE_REPRESENTATION('',(#2278),#97465);
#2241=ADVANCED_BREP_SHAPE_REPRESENTATION('',(#2279),#97466);
#2242=ADVANCED_BREP_SHAPE_REPRESENTATION('',(#2280),#97467);
#2243=ADVANCED_BREP_SHAPE_REPRESENTATION('',(#2281),#97468);
#2244=ADVANCED_BREP_SHAPE_REPRESENTATION('',(#2282),#97469);
#2245=ADVANCED_BREP_SHAPE_REPRESENTATION('',(#2283),#97470);
#2246=ADVANCED_BREP_SHAPE_REPRESENTATION('',(#2284),#97471);
#2247=ADVANCED_BREP_SHAPE_REPRESENTATION('',(#2285),#97472);
#2248=ADVANCED_BREP_SHAPE_REPRESENTATION('',(#2286),#97473);
#2249=ADVANCED_BREP_SHAPE_REPRESENTATION('',(#2287),#97474);
#2250=STYLED_ITEM('',(#97718),#2269);
#2251=STYLED_ITEM('',(#97718),#2270);
#2252=STYLED_ITEM('',(#97719),#2271);
#2253=STYLED_ITEM('',(#97720),#2272);
#2254=STYLED_ITEM('',(#97721),#2273);
#2255=STYLED_ITEM('',(#97718),#2274);
#2256=STYLED_ITEM('',(#97722),#2275);
#2257=STYLED_ITEM('',(#97720),#2276);
#2258=STYLED_ITEM('',(#97720),#2277);
#2259=STYLED_ITEM('',(#97722),#2278);
#2260=STYLED_ITEM('',(#97719),#2279);
#2261=STYLED_ITEM('',(#97723),#2280);
#2262=STYLED_ITEM('',(#97722),#2281);
#2263=STYLED_ITEM('',(#97721),#2282);
#2264=STYLED_ITEM('',(#97720),#2283);
#2265=STYLED_ITEM('',(#97721),#2284);
#2266=STYLED_ITEM('',(#97720),#2285);
#2267=STYLED_ITEM('',(#97722),#2286);
#2268=STYLED_ITEM('',(#97721),#2287);
#2269=MANIFOLD_SOLID_BREP('Body1',#21811);
#2270=MANIFOLD_SOLID_BREP('Body1',#21812);
#2271=MANIFOLD_SOLID_BREP('Body1',#21813);
#2272=MANIFOLD_SOLID_BREP('Body1',#21814);
#2273=MANIFOLD_SOLID_BREP('Body1',#21815);
#2274=MANIFOLD_SOLID_BREP('Aluminum slotted profile',#21816);
#2275=MANIFOLD_SOLID_BREP('Body1',#21817);
#2276=MANIFOLD_SOLID_BREP('Body1',#21818);
#2277=MANIFOLD_SOLID_BREP('Body1',#21819);
#2278=MANIFOLD_SOLID_BREP('Body1',#21820);
#2279=MANIFOLD_SOLID_BREP('Body1',#21821);
#2280=MANIFOLD_SOLID_BREP('Body1',#21822);
#2281=MANIFOLD_SOLID_BREP('Body1',#21823);
#2282=MANIFOLD_SOLID_BREP('Body1',#21824);
#2283=MANIFOLD_SOLID_BREP('Body1',#21825);
#2284=MANIFOLD_SOLID_BREP('Body1',#21826);
#2285=MANIFOLD_SOLID_BREP('Body1',#21827);
#2286=MANIFOLD_SOLID_BREP('Body1',#21828);
#2287=MANIFOLD_SOLID_BREP('Body1',#21829);
#2288=FACE_BOUND('',#3699,.T.);
#2289=FACE_BOUND('',#3700,.T.);
#2290=FACE_BOUND('',#3701,.T.);
#2291=FACE_BOUND('',#3704,.T.);
#2292=FACE_BOUND('',#3705,.T.);
#2293=FACE_BOUND('',#3706,.T.);
#2294=FACE_BOUND('',#3709,.T.);
#2295=FACE_BOUND('',#3710,.T.);
#2296=FACE_BOUND('',#3711,.T.);
#2297=FACE_BOUND('',#3714,.T.);
#2298=FACE_BOUND('',#3715,.T.);
#2299=FACE_BOUND('',#3716,.T.);
#2300=FACE_BOUND('',#3718,.T.);
#2301=FACE_BOUND('',#3720,.T.);
#2302=FACE_BOUND('',#3730,.T.);
#2303=FACE_BOUND('',#3732,.T.);
#2304=FACE_BOUND('',#3801,.T.);
#2305=FACE_BOUND('',#3802,.T.);
#2306=FACE_BOUND('',#3803,.T.);
#2307=FACE_BOUND('',#3804,.T.);
#2308=FACE_BOUND('',#3823,.T.);
#2309=FACE_BOUND('',#3824,.T.);
#2310=FACE_BOUND('',#3825,.T.);
#2311=FACE_BOUND('',#3826,.T.);
#2312=FACE_BOUND('',#3888,.T.);
#2313=FACE_BOUND('',#3891,.T.);
#2314=FACE_BOUND('',#3896,.T.);
#2315=FACE_BOUND('',#3898,.T.);
#2316=FACE_BOUND('',#4035,.T.);
#2317=FACE_BOUND('',#4042,.T.);
#2318=FACE_BOUND('',#4046,.T.);
#2319=FACE_BOUND('',#4047,.T.);
#2320=FACE_BOUND('',#4048,.T.);
#2321=FACE_BOUND('',#4049,.T.);
#2322=FACE_BOUND('',#4050,.T.);
#2323=FACE_BOUND('',#4127,.T.);
#2324=FACE_BOUND('',#4128,.T.);
#2325=FACE_BOUND('',#4129,.T.);
#2326=FACE_BOUND('',#4130,.T.);
#2327=FACE_BOUND('',#4131,.T.);
#2328=FACE_BOUND('',#4133,.T.);
#2329=FACE_BOUND('',#4145,.T.);
#2330=FACE_BOUND('',#4146,.T.);
#2331=FACE_BOUND('',#4147,.T.);
#2332=FACE_BOUND('',#4148,.T.);
#2333=FACE_BOUND('',#4149,.T.);
#2334=FACE_BOUND('',#4151,.T.);
#2335=FACE_BOUND('',#4152,.T.);
#2336=FACE_BOUND('',#4153,.T.);
#2337=FACE_BOUND('',#4154,.T.);
#2338=FACE_BOUND('',#4155,.T.);
#2339=FACE_BOUND('',#4207,.T.);
#2340=FACE_BOUND('',#4210,.T.);
#2341=FACE_BOUND('',#4284,.T.);
#2342=FACE_BOUND('',#4285,.T.);
#2343=FACE_BOUND('',#4286,.T.);
#2344=FACE_BOUND('',#4287,.T.);
#2345=FACE_BOUND('',#4296,.T.);
#2346=FACE_BOUND('',#4297,.T.);
#2347=FACE_BOUND('',#4298,.T.);
#2348=FACE_BOUND('',#4299,.T.);
#2349=FACE_BOUND('',#4301,.T.);
#2350=FACE_BOUND('',#4302,.T.);
#2351=FACE_BOUND('',#4303,.T.);
#2352=FACE_BOUND('',#4304,.T.);
#2353=FACE_BOUND('',#4430,.T.);
#2354=FACE_BOUND('',#4432,.T.);
#2355=FACE_BOUND('',#4462,.T.);
#2356=FACE_BOUND('',#4471,.T.);
#2357=FACE_BOUND('',#4475,.T.);
#2358=FACE_BOUND('',#4477,.T.);
#2359=FACE_BOUND('',#4521,.T.);
#2360=FACE_BOUND('',#4524,.T.);
#2361=FACE_BOUND('',#4770,.T.);
#2362=FACE_BOUND('',#4771,.T.);
#2363=FACE_BOUND('',#4772,.T.);
#2364=FACE_BOUND('',#4773,.T.);
#2365=FACE_BOUND('',#4774,.T.);
#2366=FACE_BOUND('',#4775,.T.);
#2367=FACE_BOUND('',#4802,.T.);
#2368=FACE_BOUND('',#4803,.T.);
#2369=FACE_BOUND('',#4804,.T.);
#2370=FACE_BOUND('',#4805,.T.);
#2371=FACE_BOUND('',#4806,.T.);
#2372=FACE_BOUND('',#4807,.T.);
#2373=FACE_BOUND('',#4919,.T.);
#2374=FACE_BOUND('',#4922,.T.);
#2375=FACE_BOUND('',#4927,.T.);
#2376=FACE_BOUND('',#4929,.T.);
#2377=FACE_BOUND('',#4933,.T.);
#2378=FACE_BOUND('',#4935,.T.);
#2379=PLANE('',#22061);
#2380=PLANE('',#22062);
#2381=PLANE('',#22063);
#2382=PLANE('',#22064);
#2383=PLANE('',#22065);
#2384=PLANE('',#22066);
#2385=PLANE('',#22067);
#2386=PLANE('',#22068);
#2387=PLANE('',#22069);
#2388=PLANE('',#22070);
#2389=PLANE('',#22072);
#2390=PLANE('',#22073);
#2391=PLANE('',#22074);
#2392=PLANE('',#22075);
#2393=PLANE('',#22076);
#2394=PLANE('',#22077);
#2395=PLANE('',#22078);
#2396=PLANE('',#22079);
#2397=PLANE('',#22080);
#2398=PLANE('',#22081);
#2399=PLANE('',#22164);
#2400=PLANE('',#22172);
#2401=PLANE('',#22173);
#2402=PLANE('',#22174);
#2403=PLANE('',#22175);
#2404=PLANE('',#22176);
#2405=PLANE('',#22234);
#2406=PLANE('',#22235);
#2407=PLANE('',#22236);
#2408=PLANE('',#22237);
#2409=PLANE('',#22238);
#2410=PLANE('',#22239);
#2411=PLANE('',#22240);
#2412=PLANE('',#22241);
#2413=PLANE('',#22245);
#2414=PLANE('',#22246);
#2415=PLANE('',#22254);
#2416=PLANE('',#22255);
#2417=PLANE('',#22440);
#2418=PLANE('',#22443);
#2419=PLANE('',#22445);
#2420=PLANE('',#22448);
#2421=PLANE('',#22453);
#2422=PLANE('',#22454);
#2423=PLANE('',#22496);
#2424=PLANE('',#22499);
#2425=PLANE('',#22502);
#2426=PLANE('',#22505);
#2427=PLANE('',#22510);
#2428=PLANE('',#22515);
#2429=PLANE('',#22520);
#2430=PLANE('',#22523);
#2431=PLANE('',#22526);
#2432=PLANE('',#22529);
#2433=PLANE('',#22534);
#2434=PLANE('',#22539);
#2435=PLANE('',#22544);
#2436=PLANE('',#22547);
#2437=PLANE('',#22550);
#2438=PLANE('',#22553);
#2439=PLANE('',#22558);
#2440=PLANE('',#22563);
#2441=PLANE('',#22568);
#2442=PLANE('',#22571);
#2443=PLANE('',#22574);
#2444=PLANE('',#22577);
#2445=PLANE('',#22582);
#2446=PLANE('',#22596);
#2447=PLANE('',#22597);
#2448=PLANE('',#22598);
#2449=PLANE('',#22599);
#2450=PLANE('',#22600);
#2451=PLANE('',#22601);
#2452=PLANE('',#22602);
#2453=PLANE('',#22603);
#2454=PLANE('',#22604);
#2455=PLANE('',#22605);
#2456=PLANE('',#22606);
#2457=PLANE('',#22607);
#2458=PLANE('',#22608);
#2459=PLANE('',#22610);
#2460=PLANE('',#22629);
#2461=PLANE('',#22630);
#2462=PLANE('',#22631);
#2463=PLANE('',#22632);
#2464=PLANE('',#22633);
#2465=PLANE('',#22634);
#2466=PLANE('',#22682);
#2467=PLANE('',#22683);
#2468=PLANE('',#22684);
#2469=PLANE('',#22685);
#2470=PLANE('',#22686);
#2471=PLANE('',#22687);
#2472=PLANE('',#22688);
#2473=PLANE('',#22689);
#2474=PLANE('',#22693);
#2475=PLANE('',#22694);
#2476=PLANE('',#22699);
#2477=PLANE('',#22700);
#2478=PLANE('',#22768);
#2479=PLANE('',#22771);
#2480=PLANE('',#22774);
#2481=PLANE('',#22777);
#2482=PLANE('',#22778);
#2483=PLANE('',#22779);
#2484=PLANE('',#22786);
#2485=PLANE('',#22787);
#2486=PLANE('',#22807);
#2487=PLANE('',#22808);
#2488=PLANE('',#22936);
#2489=PLANE('',#22937);
#2490=PLANE('',#22939);
#2491=PLANE('',#22940);
#2492=PLANE('',#22941);
#2493=PLANE('',#22942);
#2494=PLANE('',#22943);
#2495=PLANE('',#22944);
#2496=PLANE('',#22947);
#2497=PLANE('',#22972);
#2498=PLANE('',#22974);
#2499=PLANE('',#22975);
#2500=PLANE('',#22976);
#2501=PLANE('',#22977);
#2502=PLANE('',#22978);
#2503=PLANE('',#22979);
#2504=PLANE('',#22980);
#2505=PLANE('',#22988);
#2506=PLANE('',#22989);
#2507=PLANE('',#23029);
#2508=PLANE('',#23030);
#2509=PLANE('',#23031);
#2510=PLANE('',#23032);
#2511=PLANE('',#23033);
#2512=PLANE('',#23034);
#2513=PLANE('',#23035);
#2514=PLANE('',#23036);
#2515=PLANE('',#23040);
#2516=PLANE('',#23041);
#2517=PLANE('',#23308);
#2518=PLANE('',#23320);
#2519=PLANE('',#23321);
#2520=PLANE('',#23322);
#2521=PLANE('',#23323);
#2522=PLANE('',#23324);
#2523=PLANE('',#23432);
#2524=PLANE('',#23433);
#2525=PLANE('',#23434);
#2526=PLANE('',#23435);
#2527=PLANE('',#23436);
#2528=PLANE('',#23437);
#2529=PLANE('',#23438);
#2530=PLANE('',#23439);
#2531=PLANE('',#23443);
#2532=PLANE('',#23444);
#2533=PLANE('',#23452);
#2534=PLANE('',#23453);
#2535=PLANE('',#23461);
#2536=PLANE('',#23462);
#2537=FACE_OUTER_BOUND('',#3691,.T.);
#2538=FACE_OUTER_BOUND('',#3692,.T.);
#2539=FACE_OUTER_BOUND('',#3693,.T.);
#2540=FACE_OUTER_BOUND('',#3694,.T.);
#2541=FACE_OUTER_BOUND('',#3695,.T.);
#2542=FACE_OUTER_BOUND('',#3696,.T.);
#2543=FACE_OUTER_BOUND('',#3697,.T.);
#2544=FACE_OUTER_BOUND('',#3698,.T.);
#2545=FACE_OUTER_BOUND('',#3702,.T.);
#2546=FACE_OUTER_BOUND('',#3703,.T.);
#2547=FACE_OUTER_BOUND('',#3707,.T.);
#2548=FACE_OUTER_BOUND('',#3708,.T.);
#2549=FACE_OUTER_BOUND('',#3712,.T.);
#2550=FACE_OUTER_BOUND('',#3713,.T.);
#2551=FACE_OUTER_BOUND('',#3717,.T.);
#2552=FACE_OUTER_BOUND('',#3719,.T.);
#2553=FACE_OUTER_BOUND('',#3721,.T.);
#2554=FACE_OUTER_BOUND('',#3722,.T.);
#2555=FACE_OUTER_BOUND('',#3723,.T.);
#2556=FACE_OUTER_BOUND('',#3724,.T.);
#2557=FACE_OUTER_BOUND('',#3725,.T.);
#2558=FACE_OUTER_BOUND('',#3726,.T.);
#2559=FACE_OUTER_BOUND('',#3727,.T.);
#2560=FACE_OUTER_BOUND('',#3728,.T.);
#2561=FACE_OUTER_BOUND('',#3729,.T.);
#2562=FACE_OUTER_BOUND('',#3731,.T.);
#2563=FACE_OUTER_BOUND('',#3733,.T.);
#2564=FACE_OUTER_BOUND('',#3734,.T.);
#2565=FACE_OUTER_BOUND('',#3735,.T.);
#2566=FACE_OUTER_BOUND('',#3736,.T.);
#2567=FACE_OUTER_BOUND('',#3737,.T.);
#2568=FACE_OUTER_BOUND('',#3738,.T.);
#2569=FACE_OUTER_BOUND('',#3739,.T.);
#2570=FACE_OUTER_BOUND('',#3740,.T.);
#2571=FACE_OUTER_BOUND('',#3741,.T.);
#2572=FACE_OUTER_BOUND('',#3742,.T.);
#2573=FACE_OUTER_BOUND('',#3743,.T.);
#2574=FACE_OUTER_BOUND('',#3744,.T.);
#2575=FACE_OUTER_BOUND('',#3745,.T.);
#2576=FACE_OUTER_BOUND('',#3746,.T.);
#2577=FACE_OUTER_BOUND('',#3747,.T.);
#2578=FACE_OUTER_BOUND('',#3748,.T.);
#2579=FACE_OUTER_BOUND('',#3749,.T.);
#2580=FACE_OUTER_BOUND('',#3750,.T.);
#2581=FACE_OUTER_BOUND('',#3751,.T.);
#2582=FACE_OUTER_BOUND('',#3752,.T.);
#2583=FACE_OUTER_BOUND('',#3753,.T.);
#2584=FACE_OUTER_BOUND('',#3754,.T.);
#2585=FACE_OUTER_BOUND('',#3755,.T.);
#2586=FACE_OUTER_BOUND('',#3756,.T.);
#2587=FACE_OUTER_BOUND('',#3757,.T.);
#2588=FACE_OUTER_BOUND('',#3758,.T.);
#2589=FACE_OUTER_BOUND('',#3759,.T.);
#2590=FACE_OUTER_BOUND('',#3760,.T.);
#2591=FACE_OUTER_BOUND('',#3761,.T.);
#2592=FACE_OUTER_BOUND('',#3762,.T.);
#2593=FACE_OUTER_BOUND('',#3763,.T.);
#2594=FACE_OUTER_BOUND('',#3764,.T.);
#2595=FACE_OUTER_BOUND('',#3765,.T.);
#2596=FACE_OUTER_BOUND('',#3766,.T.);
#2597=FACE_OUTER_BOUND('',#3767,.T.);
#2598=FACE_OUTER_BOUND('',#3768,.T.);
#2599=FACE_OUTER_BOUND('',#3769,.T.);
#2600=FACE_OUTER_BOUND('',#3770,.T.);
#2601=FACE_OUTER_BOUND('',#3771,.T.);
#2602=FACE_OUTER_BOUND('',#3772,.T.);
#2603=FACE_OUTER_BOUND('',#3773,.T.);
#2604=FACE_OUTER_BOUND('',#3774,.T.);
#2605=FACE_OUTER_BOUND('',#3775,.T.);
#2606=FACE_OUTER_BOUND('',#3776,.T.);
#2607=FACE_OUTER_BOUND('',#3777,.T.);
#2608=FACE_OUTER_BOUND('',#3778,.T.);
#2609=FACE_OUTER_BOUND('',#3779,.T.);
#2610=FACE_OUTER_BOUND('',#3780,.T.);
#2611=FACE_OUTER_BOUND('',#3781,.T.);
#2612=FACE_OUTER_BOUND('',#3782,.T.);
#2613=FACE_OUTER_BOUND('',#3783,.T.);
#2614=FACE_OUTER_BOUND('',#3784,.T.);
#2615=FACE_OUTER_BOUND('',#3785,.T.);
#2616=FACE_OUTER_BOUND('',#3786,.T.);
#2617=FACE_OUTER_BOUND('',#3787,.T.);
#2618=FACE_OUTER_BOUND('',#3788,.T.);
#2619=FACE_OUTER_BOUND('',#3789,.T.);
#2620=FACE_OUTER_BOUND('',#3790,.T.);
#2621=FACE_OUTER_BOUND('',#3791,.T.);
#2622=FACE_OUTER_BOUND('',#3792,.T.);
#2623=FACE_OUTER_BOUND('',#3793,.T.);
#2624=FACE_OUTER_BOUND('',#3794,.T.);
#2625=FACE_OUTER_BOUND('',#3795,.T.);
#2626=FACE_OUTER_BOUND('',#3796,.T.);
#2627=FACE_OUTER_BOUND('',#3797,.T.);
#2628=FACE_OUTER_BOUND('',#3798,.T.);
#2629=FACE_OUTER_BOUND('',#3799,.T.);
#2630=FACE_OUTER_BOUND('',#3800,.T.);
#2631=FACE_OUTER_BOUND('',#3805,.T.);
#2632=FACE_OUTER_BOUND('',#3806,.T.);
#2633=FACE_OUTER_BOUND('',#3807,.T.);
#2634=FACE_OUTER_BOUND('',#3808,.T.);
#2635=FACE_OUTER_BOUND('',#3809,.T.);
#2636=FACE_OUTER_BOUND('',#3810,.T.);
#2637=FACE_OUTER_BOUND('',#3811,.T.);
#2638=FACE_OUTER_BOUND('',#3812,.T.);
#2639=FACE_OUTER_BOUND('',#3813,.T.);
#2640=FACE_OUTER_BOUND('',#3814,.T.);
#2641=FACE_OUTER_BOUND('',#3815,.T.);
#2642=FACE_OUTER_BOUND('',#3816,.T.);
#2643=FACE_OUTER_BOUND('',#3817,.T.);
#2644=FACE_OUTER_BOUND('',#3818,.T.);
#2645=FACE_OUTER_BOUND('',#3819,.T.);
#2646=FACE_OUTER_BOUND('',#3820,.T.);
#2647=FACE_OUTER_BOUND('',#3821,.T.);
#2648=FACE_OUTER_BOUND('',#3822,.T.);
#2649=FACE_OUTER_BOUND('',#3827,.T.);
#2650=FACE_OUTER_BOUND('',#3828,.T.);
#2651=FACE_OUTER_BOUND('',#3829,.T.);
#2652=FACE_OUTER_BOUND('',#3830,.T.);
#2653=FACE_OUTER_BOUND('',#3831,.T.);
#2654=FACE_OUTER_BOUND('',#3832,.T.);
#2655=FACE_OUTER_BOUND('',#3833,.T.);
#2656=FACE_OUTER_BOUND('',#3834,.T.);
#2657=FACE_OUTER_BOUND('',#3835,.T.);
#2658=FACE_OUTER_BOUND('',#3836,.T.);
#2659=FACE_OUTER_BOUND('',#3837,.T.);
#2660=FACE_OUTER_BOUND('',#3838,.T.);
#2661=FACE_OUTER_BOUND('',#3839,.T.);
#2662=FACE_OUTER_BOUND('',#3840,.T.);
#2663=FACE_OUTER_BOUND('',#3841,.T.);
#2664=FACE_OUTER_BOUND('',#3842,.T.);
#2665=FACE_OUTER_BOUND('',#3843,.T.);
#2666=FACE_OUTER_BOUND('',#3844,.T.);
#2667=FACE_OUTER_BOUND('',#3845,.T.);
#2668=FACE_OUTER_BOUND('',#3846,.T.);
#2669=FACE_OUTER_BOUND('',#3847,.T.);
#2670=FACE_OUTER_BOUND('',#3848,.T.);
#2671=FACE_OUTER_BOUND('',#3849,.T.);
#2672=FACE_OUTER_BOUND('',#3850,.T.);
#2673=FACE_OUTER_BOUND('',#3851,.T.);
#2674=FACE_OUTER_BOUND('',#3852,.T.);
#2675=FACE_OUTER_BOUND('',#3853,.T.);
#2676=FACE_OUTER_BOUND('',#3854,.T.);
#2677=FACE_OUTER_BOUND('',#3855,.T.);
#2678=FACE_OUTER_BOUND('',#3856,.T.);
#2679=FACE_OUTER_BOUND('',#3857,.T.);
#2680=FACE_OUTER_BOUND('',#3858,.T.);
#2681=FACE_OUTER_BOUND('',#3859,.T.);
#2682=FACE_OUTER_BOUND('',#3860,.T.);
#2683=FACE_OUTER_BOUND('',#3861,.T.);
#2684=FACE_OUTER_BOUND('',#3862,.T.);
#2685=FACE_OUTER_BOUND('',#3863,.T.);
#2686=FACE_OUTER_BOUND('',#3864,.T.);
#2687=FACE_OUTER_BOUND('',#3865,.T.);
#2688=FACE_OUTER_BOUND('',#3866,.T.);
#2689=FACE_OUTER_BOUND('',#3867,.T.);
#2690=FACE_OUTER_BOUND('',#3868,.T.);
#2691=FACE_OUTER_BOUND('',#3869,.T.);
#2692=FACE_OUTER_BOUND('',#3870,.T.);
#2693=FACE_OUTER_BOUND('',#3871,.T.);
#2694=FACE_OUTER_BOUND('',#3872,.T.);
#2695=FACE_OUTER_BOUND('',#3873,.T.);
#2696=FACE_OUTER_BOUND('',#3874,.T.);
#2697=FACE_OUTER_BOUND('',#3875,.T.);
#2698=FACE_OUTER_BOUND('',#3876,.T.);
#2699=FACE_OUTER_BOUND('',#3877,.T.);
#2700=FACE_OUTER_BOUND('',#3878,.T.);
#2701=FACE_OUTER_BOUND('',#3879,.T.);
#2702=FACE_OUTER_BOUND('',#3880,.T.);
#2703=FACE_OUTER_BOUND('',#3881,.T.);
#2704=FACE_OUTER_BOUND('',#3882,.T.);
#2705=FACE_OUTER_BOUND('',#3883,.T.);
#2706=FACE_OUTER_BOUND('',#3884,.T.);
#2707=FACE_OUTER_BOUND('',#3885,.T.);
#2708=FACE_OUTER_BOUND('',#3886,.T.);
#2709=FACE_OUTER_BOUND('',#3887,.T.);
#2710=FACE_OUTER_BOUND('',#3889,.T.);
#2711=FACE_OUTER_BOUND('',#3890,.T.);
#2712=FACE_OUTER_BOUND('',#3892,.T.);
#2713=FACE_OUTER_BOUND('',#3893,.T.);
#2714=FACE_OUTER_BOUND('',#3894,.T.);
#2715=FACE_OUTER_BOUND('',#3895,.T.);
#2716=FACE_OUTER_BOUND('',#3897,.T.);
#2717=FACE_OUTER_BOUND('',#3899,.T.);
#2718=FACE_OUTER_BOUND('',#3900,.T.);
#2719=FACE_OUTER_BOUND('',#3901,.T.);
#2720=FACE_OUTER_BOUND('',#3902,.T.);
#2721=FACE_OUTER_BOUND('',#3903,.T.);
#2722=FACE_OUTER_BOUND('',#3904,.T.);
#2723=FACE_OUTER_BOUND('',#3905,.T.);
#2724=FACE_OUTER_BOUND('',#3906,.T.);
#2725=FACE_OUTER_BOUND('',#3907,.T.);
#2726=FACE_OUTER_BOUND('',#3908,.T.);
#2727=FACE_OUTER_BOUND('',#3909,.T.);
#2728=FACE_OUTER_BOUND('',#3910,.T.);
#2729=FACE_OUTER_BOUND('',#3911,.T.);
#2730=FACE_OUTER_BOUND('',#3912,.T.);
#2731=FACE_OUTER_BOUND('',#3913,.T.);
#2732=FACE_OUTER_BOUND('',#3914,.T.);
#2733=FACE_OUTER_BOUND('',#3915,.T.);
#2734=FACE_OUTER_BOUND('',#3916,.T.);
#2735=FACE_OUTER_BOUND('',#3917,.T.);
#2736=FACE_OUTER_BOUND('',#3918,.T.);
#2737=FACE_OUTER_BOUND('',#3919,.T.);
#2738=FACE_OUTER_BOUND('',#3920,.T.);
#2739=FACE_OUTER_BOUND('',#3921,.T.);
#2740=FACE_OUTER_BOUND('',#3922,.T.);
#2741=FACE_OUTER_BOUND('',#3923,.T.);
#2742=FACE_OUTER_BOUND('',#3924,.T.);
#2743=FACE_OUTER_BOUND('',#3925,.T.);
#2744=FACE_OUTER_BOUND('',#3926,.T.);
#2745=FACE_OUTER_BOUND('',#3927,.T.);
#2746=FACE_OUTER_BOUND('',#3928,.T.);
#2747=FACE_OUTER_BOUND('',#3929,.T.);
#2748=FACE_OUTER_BOUND('',#3930,.T.);
#2749=FACE_OUTER_BOUND('',#3931,.T.);
#2750=FACE_OUTER_BOUND('',#3932,.T.);
#2751=FACE_OUTER_BOUND('',#3933,.T.);
#2752=FACE_OUTER_BOUND('',#3934,.T.);
#2753=FACE_OUTER_BOUND('',#3935,.T.);
#2754=FACE_OUTER_BOUND('',#3936,.T.);
#2755=FACE_OUTER_BOUND('',#3937,.T.);
#2756=FACE_OUTER_BOUND('',#3938,.T.);
#2757=FACE_OUTER_BOUND('',#3939,.T.);
#2758=FACE_OUTER_BOUND('',#3940,.T.);
#2759=FACE_OUTER_BOUND('',#3941,.T.);
#2760=FACE_OUTER_BOUND('',#3942,.T.);
#2761=FACE_OUTER_BOUND('',#3943,.T.);
#2762=FACE_OUTER_BOUND('',#3944,.T.);
#2763=FACE_OUTER_BOUND('',#3945,.T.);
#2764=FACE_OUTER_BOUND('',#3946,.T.);
#2765=FACE_OUTER_BOUND('',#3947,.T.);
#2766=FACE_OUTER_BOUND('',#3948,.T.);
#2767=FACE_OUTER_BOUND('',#3949,.T.);
#2768=FACE_OUTER_BOUND('',#3950,.T.);
#2769=FACE_OUTER_BOUND('',#3951,.T.);
#2770=FACE_OUTER_BOUND('',#3952,.T.);
#2771=FACE_OUTER_BOUND('',#3953,.T.);
#2772=FACE_OUTER_BOUND('',#3954,.T.);
#2773=FACE_OUTER_BOUND('',#3955,.T.);
#2774=FACE_OUTER_BOUND('',#3956,.T.);
#2775=FACE_OUTER_BOUND('',#3957,.T.);
#2776=FACE_OUTER_BOUND('',#3958,.T.);
#2777=FACE_OUTER_BOUND('',#3959,.T.);
#2778=FACE_OUTER_BOUND('',#3960,.T.);
#2779=FACE_OUTER_BOUND('',#3961,.T.);
#2780=FACE_OUTER_BOUND('',#3962,.T.);
#2781=FACE_OUTER_BOUND('',#3963,.T.);
#2782=FACE_OUTER_BOUND('',#3964,.T.);
#2783=FACE_OUTER_BOUND('',#3965,.T.);
#2784=FACE_OUTER_BOUND('',#3966,.T.);
#2785=FACE_OUTER_BOUND('',#3967,.T.);
#2786=FACE_OUTER_BOUND('',#3968,.T.);
#2787=FACE_OUTER_BOUND('',#3969,.T.);
#2788=FACE_OUTER_BOUND('',#3970,.T.);
#2789=FACE_OUTER_BOUND('',#3971,.T.);
#2790=FACE_OUTER_BOUND('',#3972,.T.);
#2791=FACE_OUTER_BOUND('',#3973,.T.);
#2792=FACE_OUTER_BOUND('',#3974,.T.);
#2793=FACE_OUTER_BOUND('',#3975,.T.);
#2794=FACE_OUTER_BOUND('',#3976,.T.);
#2795=FACE_OUTER_BOUND('',#3977,.T.);
#2796=FACE_OUTER_BOUND('',#3978,.T.);
#2797=FACE_OUTER_BOUND('',#3979,.T.);
#2798=FACE_OUTER_BOUND('',#3980,.T.);
#2799=FACE_OUTER_BOUND('',#3981,.T.);
#2800=FACE_OUTER_BOUND('',#3982,.T.);
#2801=FACE_OUTER_BOUND('',#3983,.T.);
#2802=FACE_OUTER_BOUND('',#3984,.T.);
#2803=FACE_OUTER_BOUND('',#3985,.T.);
#2804=FACE_OUTER_BOUND('',#3986,.T.);
#2805=FACE_OUTER_BOUND('',#3987,.T.);
#2806=FACE_OUTER_BOUND('',#3988,.T.);
#2807=FACE_OUTER_BOUND('',#3989,.T.);
#2808=FACE_OUTER_BOUND('',#3990,.T.);
#2809=FACE_OUTER_BOUND('',#3991,.T.);
#2810=FACE_OUTER_BOUND('',#3992,.T.);
#2811=FACE_OUTER_BOUND('',#3993,.T.);
#2812=FACE_OUTER_BOUND('',#3994,.T.);
#2813=FACE_OUTER_BOUND('',#3995,.T.);
#2814=FACE_OUTER_BOUND('',#3996,.T.);
#2815=FACE_OUTER_BOUND('',#3997,.T.);
#2816=FACE_OUTER_BOUND('',#3998,.T.);
#2817=FACE_OUTER_BOUND('',#3999,.T.);
#2818=FACE_OUTER_BOUND('',#4000,.T.);
#2819=FACE_OUTER_BOUND('',#4001,.T.);
#2820=FACE_OUTER_BOUND('',#4002,.T.);
#2821=FACE_OUTER_BOUND('',#4003,.T.);
#2822=FACE_OUTER_BOUND('',#4004,.T.);
#2823=FACE_OUTER_BOUND('',#4005,.T.);
#2824=FACE_OUTER_BOUND('',#4006,.T.);
#2825=FACE_OUTER_BOUND('',#4007,.T.);
#2826=FACE_OUTER_BOUND('',#4008,.T.);
#2827=FACE_OUTER_BOUND('',#4009,.T.);
#2828=FACE_OUTER_BOUND('',#4010,.T.);
#2829=FACE_OUTER_BOUND('',#4011,.T.);
#2830=FACE_OUTER_BOUND('',#4012,.T.);
#2831=FACE_OUTER_BOUND('',#4013,.T.);
#2832=FACE_OUTER_BOUND('',#4014,.T.);
#2833=FACE_OUTER_BOUND('',#4015,.T.);
#2834=FACE_OUTER_BOUND('',#4016,.T.);
#2835=FACE_OUTER_BOUND('',#4017,.T.);
#2836=FACE_OUTER_BOUND('',#4018,.T.);
#2837=FACE_OUTER_BOUND('',#4019,.T.);
#2838=FACE_OUTER_BOUND('',#4020,.T.);
#2839=FACE_OUTER_BOUND('',#4021,.T.);
#2840=FACE_OUTER_BOUND('',#4022,.T.);
#2841=FACE_OUTER_BOUND('',#4023,.T.);
#2842=FACE_OUTER_BOUND('',#4024,.T.);
#2843=FACE_OUTER_BOUND('',#4025,.T.);
#2844=FACE_OUTER_BOUND('',#4026,.T.);
#2845=FACE_OUTER_BOUND('',#4027,.T.);
#2846=FACE_OUTER_BOUND('',#4028,.T.);
#2847=FACE_OUTER_BOUND('',#4029,.T.);
#2848=FACE_OUTER_BOUND('',#4030,.T.);
#2849=FACE_OUTER_BOUND('',#4031,.T.);
#2850=FACE_OUTER_BOUND('',#4032,.T.);
#2851=FACE_OUTER_BOUND('',#4033,.T.);
#2852=FACE_OUTER_BOUND('',#4034,.T.);
#2853=FACE_OUTER_BOUND('',#4036,.T.);
#2854=FACE_OUTER_BOUND('',#4037,.T.);
#2855=FACE_OUTER_BOUND('',#4038,.T.);
#2856=FACE_OUTER_BOUND('',#4039,.T.);
#2857=FACE_OUTER_BOUND('',#4040,.T.);
#2858=FACE_OUTER_BOUND('',#4041,.T.);
#2859=FACE_OUTER_BOUND('',#4043,.T.);
#2860=FACE_OUTER_BOUND('',#4044,.T.);
#2861=FACE_OUTER_BOUND('',#4045,.T.);
#2862=FACE_OUTER_BOUND('',#4051,.T.);
#2863=FACE_OUTER_BOUND('',#4052,.T.);
#2864=FACE_OUTER_BOUND('',#4053,.T.);
#2865=FACE_OUTER_BOUND('',#4054,.T.);
#2866=FACE_OUTER_BOUND('',#4055,.T.);
#2867=FACE_OUTER_BOUND('',#4056,.T.);
#2868=FACE_OUTER_BOUND('',#4057,.T.);
#2869=FACE_OUTER_BOUND('',#4058,.T.);
#2870=FACE_OUTER_BOUND('',#4059,.T.);
#2871=FACE_OUTER_BOUND('',#4060,.T.);
#2872=FACE_OUTER_BOUND('',#4061,.T.);
#2873=FACE_OUTER_BOUND('',#4062,.T.);
#2874=FACE_OUTER_BOUND('',#4063,.T.);
#2875=FACE_OUTER_BOUND('',#4064,.T.);
#2876=FACE_OUTER_BOUND('',#4065,.T.);
#2877=FACE_OUTER_BOUND('',#4066,.T.);
#2878=FACE_OUTER_BOUND('',#4067,.T.);
#2879=FACE_OUTER_BOUND('',#4068,.T.);
#2880=FACE_OUTER_BOUND('',#4069,.T.);
#2881=FACE_OUTER_BOUND('',#4070,.T.);
#2882=FACE_OUTER_BOUND('',#4071,.T.);
#2883=FACE_OUTER_BOUND('',#4072,.T.);
#2884=FACE_OUTER_BOUND('',#4073,.T.);
#2885=FACE_OUTER_BOUND('',#4074,.T.);
#2886=FACE_OUTER_BOUND('',#4075,.T.);
#2887=FACE_OUTER_BOUND('',#4076,.T.);
#2888=FACE_OUTER_BOUND('',#4077,.T.);
#2889=FACE_OUTER_BOUND('',#4078,.T.);
#2890=FACE_OUTER_BOUND('',#4079,.T.);
#2891=FACE_OUTER_BOUND('',#4080,.T.);
#2892=FACE_OUTER_BOUND('',#4081,.T.);
#2893=FACE_OUTER_BOUND('',#4082,.T.);
#2894=FACE_OUTER_BOUND('',#4083,.T.);
#2895=FACE_OUTER_BOUND('',#4084,.T.);
#2896=FACE_OUTER_BOUND('',#4085,.T.);
#2897=FACE_OUTER_BOUND('',#4086,.T.);
#2898=FACE_OUTER_BOUND('',#4087,.T.);
#2899=FACE_OUTER_BOUND('',#4088,.T.);
#2900=FACE_OUTER_BOUND('',#4089,.T.);
#2901=FACE_OUTER_BOUND('',#4090,.T.);
#2902=FACE_OUTER_BOUND('',#4091,.T.);
#2903=FACE_OUTER_BOUND('',#4092,.T.);
#2904=FACE_OUTER_BOUND('',#4093,.T.);
#2905=FACE_OUTER_BOUND('',#4094,.T.);
#2906=FACE_OUTER_BOUND('',#4095,.T.);
#2907=FACE_OUTER_BOUND('',#4096,.T.);
#2908=FACE_OUTER_BOUND('',#4097,.T.);
#2909=FACE_OUTER_BOUND('',#4098,.T.);
#2910=FACE_OUTER_BOUND('',#4099,.T.);
#2911=FACE_OUTER_BOUND('',#4100,.T.);
#2912=FACE_OUTER_BOUND('',#4101,.T.);
#2913=FACE_OUTER_BOUND('',#4102,.T.);
#2914=FACE_OUTER_BOUND('',#4103,.T.);
#2915=FACE_OUTER_BOUND('',#4104,.T.);
#2916=FACE_OUTER_BOUND('',#4105,.T.);
#2917=FACE_OUTER_BOUND('',#4106,.T.);
#2918=FACE_OUTER_BOUND('',#4107,.T.);
#2919=FACE_OUTER_BOUND('',#4108,.T.);
#2920=FACE_OUTER_BOUND('',#4109,.T.);
#2921=FACE_OUTER_BOUND('',#4110,.T.);
#2922=FACE_OUTER_BOUND('',#4111,.T.);
#2923=FACE_OUTER_BOUND('',#4112,.T.);
#2924=FACE_OUTER_BOUND('',#4113,.T.);
#2925=FACE_OUTER_BOUND('',#4114,.T.);
#2926=FACE_OUTER_BOUND('',#4115,.T.);
#2927=FACE_OUTER_BOUND('',#4116,.T.);
#2928=FACE_OUTER_BOUND('',#4117,.T.);
#2929=FACE_OUTER_BOUND('',#4118,.T.);
#2930=FACE_OUTER_BOUND('',#4119,.T.);
#2931=FACE_OUTER_BOUND('',#4120,.T.);
#2932=FACE_OUTER_BOUND('',#4121,.T.);
#2933=FACE_OUTER_BOUND('',#4122,.T.);
#2934=FACE_OUTER_BOUND('',#4123,.T.);
#2935=FACE_OUTER_BOUND('',#4124,.T.);
#2936=FACE_OUTER_BOUND('',#4125,.T.);
#2937=FACE_OUTER_BOUND('',#4126,.T.);
#2938=FACE_OUTER_BOUND('',#4132,.T.);
#2939=FACE_OUTER_BOUND('',#4134,.T.);
#2940=FACE_OUTER_BOUND('',#4135,.T.);
#2941=FACE_OUTER_BOUND('',#4136,.T.);
#2942=FACE_OUTER_BOUND('',#4137,.T.);
#2943=FACE_OUTER_BOUND('',#4138,.T.);
#2944=FACE_OUTER_BOUND('',#4139,.T.);
#2945=FACE_OUTER_BOUND('',#4140,.T.);
#2946=FACE_OUTER_BOUND('',#4141,.T.);
#2947=FACE_OUTER_BOUND('',#4142,.T.);
#2948=FACE_OUTER_BOUND('',#4143,.T.);
#2949=FACE_OUTER_BOUND('',#4144,.T.);
#2950=FACE_OUTER_BOUND('',#4150,.T.);
#2951=FACE_OUTER_BOUND('',#4156,.T.);
#2952=FACE_OUTER_BOUND('',#4157,.T.);
#2953=FACE_OUTER_BOUND('',#4158,.T.);
#2954=FACE_OUTER_BOUND('',#4159,.T.);
#2955=FACE_OUTER_BOUND('',#4160,.T.);
#2956=FACE_OUTER_BOUND('',#4161,.T.);
#2957=FACE_OUTER_BOUND('',#4162,.T.);
#2958=FACE_OUTER_BOUND('',#4163,.T.);
#2959=FACE_OUTER_BOUND('',#4164,.T.);
#2960=FACE_OUTER_BOUND('',#4165,.T.);
#2961=FACE_OUTER_BOUND('',#4166,.T.);
#2962=FACE_OUTER_BOUND('',#4167,.T.);
#2963=FACE_OUTER_BOUND('',#4168,.T.);
#2964=FACE_OUTER_BOUND('',#4169,.T.);
#2965=FACE_OUTER_BOUND('',#4170,.T.);
#2966=FACE_OUTER_BOUND('',#4171,.T.);
#2967=FACE_OUTER_BOUND('',#4172,.T.);
#2968=FACE_OUTER_BOUND('',#4173,.T.);
#2969=FACE_OUTER_BOUND('',#4174,.T.);
#2970=FACE_OUTER_BOUND('',#4175,.T.);
#2971=FACE_OUTER_BOUND('',#4176,.T.);
#2972=FACE_OUTER_BOUND('',#4177,.T.);
#2973=FACE_OUTER_BOUND('',#4178,.T.);
#2974=FACE_OUTER_BOUND('',#4179,.T.);
#2975=FACE_OUTER_BOUND('',#4180,.T.);
#2976=FACE_OUTER_BOUND('',#4181,.T.);
#2977=FACE_OUTER_BOUND('',#4182,.T.);
#2978=FACE_OUTER_BOUND('',#4183,.T.);
#2979=FACE_OUTER_BOUND('',#4184,.T.);
#2980=FACE_OUTER_BOUND('',#4185,.T.);
#2981=FACE_OUTER_BOUND('',#4186,.T.);
#2982=FACE_OUTER_BOUND('',#4187,.T.);
#2983=FACE_OUTER_BOUND('',#4188,.T.);
#2984=FACE_OUTER_BOUND('',#4189,.T.);
#2985=FACE_OUTER_BOUND('',#4190,.T.);
#2986=FACE_OUTER_BOUND('',#4191,.T.);
#2987=FACE_OUTER_BOUND('',#4192,.T.);
#2988=FACE_OUTER_BOUND('',#4193,.T.);
#2989=FACE_OUTER_BOUND('',#4194,.T.);
#2990=FACE_OUTER_BOUND('',#4195,.T.);
#2991=FACE_OUTER_BOUND('',#4196,.T.);
#2992=FACE_OUTER_BOUND('',#4197,.T.);
#2993=FACE_OUTER_BOUND('',#4198,.T.);
#2994=FACE_OUTER_BOUND('',#4199,.T.);
#2995=FACE_OUTER_BOUND('',#4200,.T.);
#2996=FACE_OUTER_BOUND('',#4201,.T.);
#2997=FACE_OUTER_BOUND('',#4202,.T.);
#2998=FACE_OUTER_BOUND('',#4203,.T.);
#2999=FACE_OUTER_BOUND('',#4204,.T.);
#3000=FACE_OUTER_BOUND('',#4205,.T.);
#3001=FACE_OUTER_BOUND('',#4206,.T.);
#3002=FACE_OUTER_BOUND('',#4208,.T.);
#3003=FACE_OUTER_BOUND('',#4209,.T.);
#3004=FACE_OUTER_BOUND('',#4211,.T.);
#3005=FACE_OUTER_BOUND('',#4212,.T.);
#3006=FACE_OUTER_BOUND('',#4213,.T.);
#3007=FACE_OUTER_BOUND('',#4214,.T.);
#3008=FACE_OUTER_BOUND('',#4215,.T.);
#3009=FACE_OUTER_BOUND('',#4216,.T.);
#3010=FACE_OUTER_BOUND('',#4217,.T.);
#3011=FACE_OUTER_BOUND('',#4218,.T.);
#3012=FACE_OUTER_BOUND('',#4219,.T.);
#3013=FACE_OUTER_BOUND('',#4220,.T.);
#3014=FACE_OUTER_BOUND('',#4221,.T.);
#3015=FACE_OUTER_BOUND('',#4222,.T.);
#3016=FACE_OUTER_BOUND('',#4223,.T.);
#3017=FACE_OUTER_BOUND('',#4224,.T.);
#3018=FACE_OUTER_BOUND('',#4225,.T.);
#3019=FACE_OUTER_BOUND('',#4226,.T.);
#3020=FACE_OUTER_BOUND('',#4227,.T.);
#3021=FACE_OUTER_BOUND('',#4228,.T.);
#3022=FACE_OUTER_BOUND('',#4229,.T.);
#3023=FACE_OUTER_BOUND('',#4230,.T.);
#3024=FACE_OUTER_BOUND('',#4231,.T.);
#3025=FACE_OUTER_BOUND('',#4232,.T.);
#3026=FACE_OUTER_BOUND('',#4233,.T.);
#3027=FACE_OUTER_BOUND('',#4234,.T.);
#3028=FACE_OUTER_BOUND('',#4235,.T.);
#3029=FACE_OUTER_BOUND('',#4236,.T.);
#3030=FACE_OUTER_BOUND('',#4237,.T.);
#3031=FACE_OUTER_BOUND('',#4238,.T.);
#3032=FACE_OUTER_BOUND('',#4239,.T.);
#3033=FACE_OUTER_BOUND('',#4240,.T.);
#3034=FACE_OUTER_BOUND('',#4241,.T.);
#3035=FACE_OUTER_BOUND('',#4242,.T.);
#3036=FACE_OUTER_BOUND('',#4243,.T.);
#3037=FACE_OUTER_BOUND('',#4244,.T.);
#3038=FACE_OUTER_BOUND('',#4245,.T.);
#3039=FACE_OUTER_BOUND('',#4246,.T.);
#3040=FACE_OUTER_BOUND('',#4247,.T.);
#3041=FACE_OUTER_BOUND('',#4248,.T.);
#3042=FACE_OUTER_BOUND('',#4249,.T.);
#3043=FACE_OUTER_BOUND('',#4250,.T.);
#3044=FACE_OUTER_BOUND('',#4251,.T.);
#3045=FACE_OUTER_BOUND('',#4252,.T.);
#3046=FACE_OUTER_BOUND('',#4253,.T.);
#3047=FACE_OUTER_BOUND('',#4254,.T.);
#3048=FACE_OUTER_BOUND('',#4255,.T.);
#3049=FACE_OUTER_BOUND('',#4256,.T.);
#3050=FACE_OUTER_BOUND('',#4257,.T.);
#3051=FACE_OUTER_BOUND('',#4258,.T.);
#3052=FACE_OUTER_BOUND('',#4259,.T.);
#3053=FACE_OUTER_BOUND('',#4260,.T.);
#3054=FACE_OUTER_BOUND('',#4261,.T.);
#3055=FACE_OUTER_BOUND('',#4262,.T.);
#3056=FACE_OUTER_BOUND('',#4263,.T.);
#3057=FACE_OUTER_BOUND('',#4264,.T.);
#3058=FACE_OUTER_BOUND('',#4265,.T.);
#3059=FACE_OUTER_BOUND('',#4266,.T.);
#3060=FACE_OUTER_BOUND('',#4267,.T.);
#3061=FACE_OUTER_BOUND('',#4268,.T.);
#3062=FACE_OUTER_BOUND('',#4269,.T.);
#3063=FACE_OUTER_BOUND('',#4270,.T.);
#3064=FACE_OUTER_BOUND('',#4271,.T.);
#3065=FACE_OUTER_BOUND('',#4272,.T.);
#3066=FACE_OUTER_BOUND('',#4273,.T.);
#3067=FACE_OUTER_BOUND('',#4274,.T.);
#3068=FACE_OUTER_BOUND('',#4275,.T.);
#3069=FACE_OUTER_BOUND('',#4276,.T.);
#3070=FACE_OUTER_BOUND('',#4277,.T.);
#3071=FACE_OUTER_BOUND('',#4278,.T.);
#3072=FACE_OUTER_BOUND('',#4279,.T.);
#3073=FACE_OUTER_BOUND('',#4280,.T.);
#3074=FACE_OUTER_BOUND('',#4281,.T.);
#3075=FACE_OUTER_BOUND('',#4282,.T.);
#3076=FACE_OUTER_BOUND('',#4283,.T.);
#3077=FACE_OUTER_BOUND('',#4288,.T.);
#3078=FACE_OUTER_BOUND('',#4289,.T.);
#3079=FACE_OUTER_BOUND('',#4290,.T.);
#3080=FACE_OUTER_BOUND('',#4291,.T.);
#3081=FACE_OUTER_BOUND('',#4292,.T.);
#3082=FACE_OUTER_BOUND('',#4293,.T.);
#3083=FACE_OUTER_BOUND('',#4294,.T.);
#3084=FACE_OUTER_BOUND('',#4295,.T.);
#3085=FACE_OUTER_BOUND('',#4300,.T.);
#3086=FACE_OUTER_BOUND('',#4305,.T.);
#3087=FACE_OUTER_BOUND('',#4306,.T.);
#3088=FACE_OUTER_BOUND('',#4307,.T.);
#3089=FACE_OUTER_BOUND('',#4308,.T.);
#3090=FACE_OUTER_BOUND('',#4309,.T.);
#3091=FACE_OUTER_BOUND('',#4310,.T.);
#3092=FACE_OUTER_BOUND('',#4311,.T.);
#3093=FACE_OUTER_BOUND('',#4312,.T.);
#3094=FACE_OUTER_BOUND('',#4313,.T.);
#3095=FACE_OUTER_BOUND('',#4314,.T.);
#3096=FACE_OUTER_BOUND('',#4315,.T.);
#3097=FACE_OUTER_BOUND('',#4316,.T.);
#3098=FACE_OUTER_BOUND('',#4317,.T.);
#3099=FACE_OUTER_BOUND('',#4318,.T.);
#3100=FACE_OUTER_BOUND('',#4319,.T.);
#3101=FACE_OUTER_BOUND('',#4320,.T.);
#3102=FACE_OUTER_BOUND('',#4321,.T.);
#3103=FACE_OUTER_BOUND('',#4322,.T.);
#3104=FACE_OUTER_BOUND('',#4323,.T.);
#3105=FACE_OUTER_BOUND('',#4324,.T.);
#3106=FACE_OUTER_BOUND('',#4325,.T.);
#3107=FACE_OUTER_BOUND('',#4326,.T.);
#3108=FACE_OUTER_BOUND('',#4327,.T.);
#3109=FACE_OUTER_BOUND('',#4328,.T.);
#3110=FACE_OUTER_BOUND('',#4329,.T.);
#3111=FACE_OUTER_BOUND('',#4330,.T.);
#3112=FACE_OUTER_BOUND('',#4331,.T.);
#3113=FACE_OUTER_BOUND('',#4332,.T.);
#3114=FACE_OUTER_BOUND('',#4333,.T.);
#3115=FACE_OUTER_BOUND('',#4334,.T.);
#3116=FACE_OUTER_BOUND('',#4335,.T.);
#3117=FACE_OUTER_BOUND('',#4336,.T.);
#3118=FACE_OUTER_BOUND('',#4337,.T.);
#3119=FACE_OUTER_BOUND('',#4338,.T.);
#3120=FACE_OUTER_BOUND('',#4339,.T.);
#3121=FACE_OUTER_BOUND('',#4340,.T.);
#3122=FACE_OUTER_BOUND('',#4341,.T.);
#3123=FACE_OUTER_BOUND('',#4342,.T.);
#3124=FACE_OUTER_BOUND('',#4343,.T.);
#3125=FACE_OUTER_BOUND('',#4344,.T.);
#3126=FACE_OUTER_BOUND('',#4345,.T.);
#3127=FACE_OUTER_BOUND('',#4346,.T.);
#3128=FACE_OUTER_BOUND('',#4347,.T.);
#3129=FACE_OUTER_BOUND('',#4348,.T.);
#3130=FACE_OUTER_BOUND('',#4349,.T.);
#3131=FACE_OUTER_BOUND('',#4350,.T.);
#3132=FACE_OUTER_BOUND('',#4351,.T.);
#3133=FACE_OUTER_BOUND('',#4352,.T.);
#3134=FACE_OUTER_BOUND('',#4353,.T.);
#3135=FACE_OUTER_BOUND('',#4354,.T.);
#3136=FACE_OUTER_BOUND('',#4355,.T.);
#3137=FACE_OUTER_BOUND('',#4356,.T.);
#3138=FACE_OUTER_BOUND('',#4357,.T.);
#3139=FACE_OUTER_BOUND('',#4358,.T.);
#3140=FACE_OUTER_BOUND('',#4359,.T.);
#3141=FACE_OUTER_BOUND('',#4360,.T.);
#3142=FACE_OUTER_BOUND('',#4361,.T.);
#3143=FACE_OUTER_BOUND('',#4362,.T.);
#3144=FACE_OUTER_BOUND('',#4363,.T.);
#3145=FACE_OUTER_BOUND('',#4364,.T.);
#3146=FACE_OUTER_BOUND('',#4365,.T.);
#3147=FACE_OUTER_BOUND('',#4366,.T.);
#3148=FACE_OUTER_BOUND('',#4367,.T.);
#3149=FACE_OUTER_BOUND('',#4368,.T.);
#3150=FACE_OUTER_BOUND('',#4369,.T.);
#3151=FACE_OUTER_BOUND('',#4370,.T.);
#3152=FACE_OUTER_BOUND('',#4371,.T.);
#3153=FACE_OUTER_BOUND('',#4372,.T.);
#3154=FACE_OUTER_BOUND('',#4373,.T.);
#3155=FACE_OUTER_BOUND('',#4374,.T.);
#3156=FACE_OUTER_BOUND('',#4375,.T.);
#3157=FACE_OUTER_BOUND('',#4376,.T.);
#3158=FACE_OUTER_BOUND('',#4377,.T.);
#3159=FACE_OUTER_BOUND('',#4378,.T.);
#3160=FACE_OUTER_BOUND('',#4379,.T.);
#3161=FACE_OUTER_BOUND('',#4380,.T.);
#3162=FACE_OUTER_BOUND('',#4381,.T.);
#3163=FACE_OUTER_BOUND('',#4382,.T.);
#3164=FACE_OUTER_BOUND('',#4383,.T.);
#3165=FACE_OUTER_BOUND('',#4384,.T.);
#3166=FACE_OUTER_BOUND('',#4385,.T.);
#3167=FACE_OUTER_BOUND('',#4386,.T.);
#3168=FACE_OUTER_BOUND('',#4387,.T.);
#3169=FACE_OUTER_BOUND('',#4388,.T.);
#3170=FACE_OUTER_BOUND('',#4389,.T.);
#3171=FACE_OUTER_BOUND('',#4390,.T.);
#3172=FACE_OUTER_BOUND('',#4391,.T.);
#3173=FACE_OUTER_BOUND('',#4392,.T.);
#3174=FACE_OUTER_BOUND('',#4393,.T.);
#3175=FACE_OUTER_BOUND('',#4394,.T.);
#3176=FACE_OUTER_BOUND('',#4395,.T.);
#3177=FACE_OUTER_BOUND('',#4396,.T.);
#3178=FACE_OUTER_BOUND('',#4397,.T.);
#3179=FACE_OUTER_BOUND('',#4398,.T.);
#3180=FACE_OUTER_BOUND('',#4399,.T.);
#3181=FACE_OUTER_BOUND('',#4400,.T.);
#3182=FACE_OUTER_BOUND('',#4401,.T.);
#3183=FACE_OUTER_BOUND('',#4402,.T.);
#3184=FACE_OUTER_BOUND('',#4403,.T.);
#3185=FACE_OUTER_BOUND('',#4404,.T.);
#3186=FACE_OUTER_BOUND('',#4405,.T.);
#3187=FACE_OUTER_BOUND('',#4406,.T.);
#3188=FACE_OUTER_BOUND('',#4407,.T.);
#3189=FACE_OUTER_BOUND('',#4408,.T.);
#3190=FACE_OUTER_BOUND('',#4409,.T.);
#3191=FACE_OUTER_BOUND('',#4410,.T.);
#3192=FACE_OUTER_BOUND('',#4411,.T.);
#3193=FACE_OUTER_BOUND('',#4412,.T.);
#3194=FACE_OUTER_BOUND('',#4413,.T.);
#3195=FACE_OUTER_BOUND('',#4414,.T.);
#3196=FACE_OUTER_BOUND('',#4415,.T.);
#3197=FACE_OUTER_BOUND('',#4416,.T.);
#3198=FACE_OUTER_BOUND('',#4417,.T.);
#3199=FACE_OUTER_BOUND('',#4418,.T.);
#3200=FACE_OUTER_BOUND('',#4419,.T.);
#3201=FACE_OUTER_BOUND('',#4420,.T.);
#3202=FACE_OUTER_BOUND('',#4421,.T.);
#3203=FACE_OUTER_BOUND('',#4422,.T.);
#3204=FACE_OUTER_BOUND('',#4423,.T.);
#3205=FACE_OUTER_BOUND('',#4424,.T.);
#3206=FACE_OUTER_BOUND('',#4425,.T.);
#3207=FACE_OUTER_BOUND('',#4426,.T.);
#3208=FACE_OUTER_BOUND('',#4427,.T.);
#3209=FACE_OUTER_BOUND('',#4428,.T.);
#3210=FACE_OUTER_BOUND('',#4429,.T.);
#3211=FACE_OUTER_BOUND('',#4431,.T.);
#3212=FACE_OUTER_BOUND('',#4433,.T.);
#3213=FACE_OUTER_BOUND('',#4434,.T.);
#3214=FACE_OUTER_BOUND('',#4435,.T.);
#3215=FACE_OUTER_BOUND('',#4436,.T.);
#3216=FACE_OUTER_BOUND('',#4437,.T.);
#3217=FACE_OUTER_BOUND('',#4438,.T.);
#3218=FACE_OUTER_BOUND('',#4439,.T.);
#3219=FACE_OUTER_BOUND('',#4440,.T.);
#3220=FACE_OUTER_BOUND('',#4441,.T.);
#3221=FACE_OUTER_BOUND('',#4442,.T.);
#3222=FACE_OUTER_BOUND('',#4443,.T.);
#3223=FACE_OUTER_BOUND('',#4444,.T.);
#3224=FACE_OUTER_BOUND('',#4445,.T.);
#3225=FACE_OUTER_BOUND('',#4446,.T.);
#3226=FACE_OUTER_BOUND('',#4447,.T.);
#3227=FACE_OUTER_BOUND('',#4448,.T.);
#3228=FACE_OUTER_BOUND('',#4449,.T.);
#3229=FACE_OUTER_BOUND('',#4450,.T.);
#3230=FACE_OUTER_BOUND('',#4451,.T.);
#3231=FACE_OUTER_BOUND('',#4452,.T.);
#3232=FACE_OUTER_BOUND('',#4453,.T.);
#3233=FACE_OUTER_BOUND('',#4454,.T.);
#3234=FACE_OUTER_BOUND('',#4455,.T.);
#3235=FACE_OUTER_BOUND('',#4456,.T.);
#3236=FACE_OUTER_BOUND('',#4457,.T.);
#3237=FACE_OUTER_BOUND('',#4458,.T.);
#3238=FACE_OUTER_BOUND('',#4459,.T.);
#3239=FACE_OUTER_BOUND('',#4460,.T.);
#3240=FACE_OUTER_BOUND('',#4461,.T.);
#3241=FACE_OUTER_BOUND('',#4463,.T.);
#3242=FACE_OUTER_BOUND('',#4464,.T.);
#3243=FACE_OUTER_BOUND('',#4465,.T.);
#3244=FACE_OUTER_BOUND('',#4466,.T.);
#3245=FACE_OUTER_BOUND('',#4467,.T.);
#3246=FACE_OUTER_BOUND('',#4468,.T.);
#3247=FACE_OUTER_BOUND('',#4469,.T.);
#3248=FACE_OUTER_BOUND('',#4470,.T.);
#3249=FACE_OUTER_BOUND('',#4472,.T.);
#3250=FACE_OUTER_BOUND('',#4473,.T.);
#3251=FACE_OUTER_BOUND('',#4474,.T.);
#3252=FACE_OUTER_BOUND('',#4476,.T.);
#3253=FACE_OUTER_BOUND('',#4478,.T.);
#3254=FACE_OUTER_BOUND('',#4479,.T.);
#3255=FACE_OUTER_BOUND('',#4480,.T.);
#3256=FACE_OUTER_BOUND('',#4481,.T.);
#3257=FACE_OUTER_BOUND('',#4482,.T.);
#3258=FACE_OUTER_BOUND('',#4483,.T.);
#3259=FACE_OUTER_BOUND('',#4484,.T.);
#3260=FACE_OUTER_BOUND('',#4485,.T.);
#3261=FACE_OUTER_BOUND('',#4486,.T.);
#3262=FACE_OUTER_BOUND('',#4487,.T.);
#3263=FACE_OUTER_BOUND('',#4488,.T.);
#3264=FACE_OUTER_BOUND('',#4489,.T.);
#3265=FACE_OUTER_BOUND('',#4490,.T.);
#3266=FACE_OUTER_BOUND('',#4491,.T.);
#3267=FACE_OUTER_BOUND('',#4492,.T.);
#3268=FACE_OUTER_BOUND('',#4493,.T.);
#3269=FACE_OUTER_BOUND('',#4494,.T.);
#3270=FACE_OUTER_BOUND('',#4495,.T.);
#3271=FACE_OUTER_BOUND('',#4496,.T.);
#3272=FACE_OUTER_BOUND('',#4497,.T.);
#3273=FACE_OUTER_BOUND('',#4498,.T.);
#3274=FACE_OUTER_BOUND('',#4499,.T.);
#3275=FACE_OUTER_BOUND('',#4500,.T.);
#3276=FACE_OUTER_BOUND('',#4501,.T.);
#3277=FACE_OUTER_BOUND('',#4502,.T.);
#3278=FACE_OUTER_BOUND('',#4503,.T.);
#3279=FACE_OUTER_BOUND('',#4504,.T.);
#3280=FACE_OUTER_BOUND('',#4505,.T.);
#3281=FACE_OUTER_BOUND('',#4506,.T.);
#3282=FACE_OUTER_BOUND('',#4507,.T.);
#3283=FACE_OUTER_BOUND('',#4508,.T.);
#3284=FACE_OUTER_BOUND('',#4509,.T.);
#3285=FACE_OUTER_BOUND('',#4510,.T.);
#3286=FACE_OUTER_BOUND('',#4511,.T.);
#3287=FACE_OUTER_BOUND('',#4512,.T.);
#3288=FACE_OUTER_BOUND('',#4513,.T.);
#3289=FACE_OUTER_BOUND('',#4514,.T.);
#3290=FACE_OUTER_BOUND('',#4515,.T.);
#3291=FACE_OUTER_BOUND('',#4516,.T.);
#3292=FACE_OUTER_BOUND('',#4517,.T.);
#3293=FACE_OUTER_BOUND('',#4518,.T.);
#3294=FACE_OUTER_BOUND('',#4519,.T.);
#3295=FACE_OUTER_BOUND('',#4520,.T.);
#3296=FACE_OUTER_BOUND('',#4522,.T.);
#3297=FACE_OUTER_BOUND('',#4523,.T.);
#3298=FACE_OUTER_BOUND('',#4525,.T.);
#3299=FACE_OUTER_BOUND('',#4526,.T.);
#3300=FACE_OUTER_BOUND('',#4527,.T.);
#3301=FACE_OUTER_BOUND('',#4528,.T.);
#3302=FACE_OUTER_BOUND('',#4529,.T.);
#3303=FACE_OUTER_BOUND('',#4530,.T.);
#3304=FACE_OUTER_BOUND('',#4531,.T.);
#3305=FACE_OUTER_BOUND('',#4532,.T.);
#3306=FACE_OUTER_BOUND('',#4533,.T.);
#3307=FACE_OUTER_BOUND('',#4534,.T.);
#3308=FACE_OUTER_BOUND('',#4535,.T.);
#3309=FACE_OUTER_BOUND('',#4536,.T.);
#3310=FACE_OUTER_BOUND('',#4537,.T.);
#3311=FACE_OUTER_BOUND('',#4538,.T.);
#3312=FACE_OUTER_BOUND('',#4539,.T.);
#3313=FACE_OUTER_BOUND('',#4540,.T.);
#3314=FACE_OUTER_BOUND('',#4541,.T.);
#3315=FACE_OUTER_BOUND('',#4542,.T.);
#3316=FACE_OUTER_BOUND('',#4543,.T.);
#3317=FACE_OUTER_BOUND('',#4544,.T.);
#3318=FACE_OUTER_BOUND('',#4545,.T.);
#3319=FACE_OUTER_BOUND('',#4546,.T.);
#3320=FACE_OUTER_BOUND('',#4547,.T.);
#3321=FACE_OUTER_BOUND('',#4548,.T.);
#3322=FACE_OUTER_BOUND('',#4549,.T.);
#3323=FACE_OUTER_BOUND('',#4550,.T.);
#3324=FACE_OUTER_BOUND('',#4551,.T.);
#3325=FACE_OUTER_BOUND('',#4552,.T.);
#3326=FACE_OUTER_BOUND('',#4553,.T.);
#3327=FACE_OUTER_BOUND('',#4554,.T.);
#3328=FACE_OUTER_BOUND('',#4555,.T.);
#3329=FACE_OUTER_BOUND('',#4556,.T.);
#3330=FACE_OUTER_BOUND('',#4557,.T.);
#3331=FACE_OUTER_BOUND('',#4558,.T.);
#3332=FACE_OUTER_BOUND('',#4559,.T.);
#3333=FACE_OUTER_BOUND('',#4560,.T.);
#3334=FACE_OUTER_BOUND('',#4561,.T.);
#3335=FACE_OUTER_BOUND('',#4562,.T.);
#3336=FACE_OUTER_BOUND('',#4563,.T.);
#3337=FACE_OUTER_BOUND('',#4564,.T.);
#3338=FACE_OUTER_BOUND('',#4565,.T.);
#3339=FACE_OUTER_BOUND('',#4566,.T.);
#3340=FACE_OUTER_BOUND('',#4567,.T.);
#3341=FACE_OUTER_BOUND('',#4568,.T.);
#3342=FACE_OUTER_BOUND('',#4569,.T.);
#3343=FACE_OUTER_BOUND('',#4570,.T.);
#3344=FACE_OUTER_BOUND('',#4571,.T.);
#3345=FACE_OUTER_BOUND('',#4572,.T.);
#3346=FACE_OUTER_BOUND('',#4573,.T.);
#3347=FACE_OUTER_BOUND('',#4574,.T.);
#3348=FACE_OUTER_BOUND('',#4575,.T.);
#3349=FACE_OUTER_BOUND('',#4576,.T.);
#3350=FACE_OUTER_BOUND('',#4577,.T.);
#3351=FACE_OUTER_BOUND('',#4578,.T.);
#3352=FACE_OUTER_BOUND('',#4579,.T.);
#3353=FACE_OUTER_BOUND('',#4580,.T.);
#3354=FACE_OUTER_BOUND('',#4581,.T.);
#3355=FACE_OUTER_BOUND('',#4582,.T.);
#3356=FACE_OUTER_BOUND('',#4583,.T.);
#3357=FACE_OUTER_BOUND('',#4584,.T.);
#3358=FACE_OUTER_BOUND('',#4585,.T.);
#3359=FACE_OUTER_BOUND('',#4586,.T.);
#3360=FACE_OUTER_BOUND('',#4587,.T.);
#3361=FACE_OUTER_BOUND('',#4588,.T.);
#3362=FACE_OUTER_BOUND('',#4589,.T.);
#3363=FACE_OUTER_BOUND('',#4590,.T.);
#3364=FACE_OUTER_BOUND('',#4591,.T.);
#3365=FACE_OUTER_BOUND('',#4592,.T.);
#3366=FACE_OUTER_BOUND('',#4593,.T.);
#3367=FACE_OUTER_BOUND('',#4594,.T.);
#3368=FACE_OUTER_BOUND('',#4595,.T.);
#3369=FACE_OUTER_BOUND('',#4596,.T.);
#3370=FACE_OUTER_BOUND('',#4597,.T.);
#3371=FACE_OUTER_BOUND('',#4598,.T.);
#3372=FACE_OUTER_BOUND('',#4599,.T.);
#3373=FACE_OUTER_BOUND('',#4600,.T.);
#3374=FACE_OUTER_BOUND('',#4601,.T.);
#3375=FACE_OUTER_BOUND('',#4602,.T.);
#3376=FACE_OUTER_BOUND('',#4603,.T.);
#3377=FACE_OUTER_BOUND('',#4604,.T.);
#3378=FACE_OUTER_BOUND('',#4605,.T.);
#3379=FACE_OUTER_BOUND('',#4606,.T.);
#3380=FACE_OUTER_BOUND('',#4607,.T.);
#3381=FACE_OUTER_BOUND('',#4608,.T.);
#3382=FACE_OUTER_BOUND('',#4609,.T.);
#3383=FACE_OUTER_BOUND('',#4610,.T.);
#3384=FACE_OUTER_BOUND('',#4611,.T.);
#3385=FACE_OUTER_BOUND('',#4612,.T.);
#3386=FACE_OUTER_BOUND('',#4613,.T.);
#3387=FACE_OUTER_BOUND('',#4614,.T.);
#3388=FACE_OUTER_BOUND('',#4615,.T.);
#3389=FACE_OUTER_BOUND('',#4616,.T.);
#3390=FACE_OUTER_BOUND('',#4617,.T.);
#3391=FACE_OUTER_BOUND('',#4618,.T.);
#3392=FACE_OUTER_BOUND('',#4619,.T.);
#3393=FACE_OUTER_BOUND('',#4620,.T.);
#3394=FACE_OUTER_BOUND('',#4621,.T.);
#3395=FACE_OUTER_BOUND('',#4622,.T.);
#3396=FACE_OUTER_BOUND('',#4623,.T.);
#3397=FACE_OUTER_BOUND('',#4624,.T.);
#3398=FACE_OUTER_BOUND('',#4625,.T.);
#3399=FACE_OUTER_BOUND('',#4626,.T.);
#3400=FACE_OUTER_BOUND('',#4627,.T.);
#3401=FACE_OUTER_BOUND('',#4628,.T.);
#3402=FACE_OUTER_BOUND('',#4629,.T.);
#3403=FACE_OUTER_BOUND('',#4630,.T.);
#3404=FACE_OUTER_BOUND('',#4631,.T.);
#3405=FACE_OUTER_BOUND('',#4632,.T.);
#3406=FACE_OUTER_BOUND('',#4633,.T.);
#3407=FACE_OUTER_BOUND('',#4634,.T.);
#3408=FACE_OUTER_BOUND('',#4635,.T.);
#3409=FACE_OUTER_BOUND('',#4636,.T.);
#3410=FACE_OUTER_BOUND('',#4637,.T.);
#3411=FACE_OUTER_BOUND('',#4638,.T.);
#3412=FACE_OUTER_BOUND('',#4639,.T.);
#3413=FACE_OUTER_BOUND('',#4640,.T.);
#3414=FACE_OUTER_BOUND('',#4641,.T.);
#3415=FACE_OUTER_BOUND('',#4642,.T.);
#3416=FACE_OUTER_BOUND('',#4643,.T.);
#3417=FACE_OUTER_BOUND('',#4644,.T.);
#3418=FACE_OUTER_BOUND('',#4645,.T.);
#3419=FACE_OUTER_BOUND('',#4646,.T.);
#3420=FACE_OUTER_BOUND('',#4647,.T.);
#3421=FACE_OUTER_BOUND('',#4648,.T.);
#3422=FACE_OUTER_BOUND('',#4649,.T.);
#3423=FACE_OUTER_BOUND('',#4650,.T.);
#3424=FACE_OUTER_BOUND('',#4651,.T.);
#3425=FACE_OUTER_BOUND('',#4652,.T.);
#3426=FACE_OUTER_BOUND('',#4653,.T.);
#3427=FACE_OUTER_BOUND('',#4654,.T.);
#3428=FACE_OUTER_BOUND('',#4655,.T.);
#3429=FACE_OUTER_BOUND('',#4656,.T.);
#3430=FACE_OUTER_BOUND('',#4657,.T.);
#3431=FACE_OUTER_BOUND('',#4658,.T.);
#3432=FACE_OUTER_BOUND('',#4659,.T.);
#3433=FACE_OUTER_BOUND('',#4660,.T.);
#3434=FACE_OUTER_BOUND('',#4661,.T.);
#3435=FACE_OUTER_BOUND('',#4662,.T.);
#3436=FACE_OUTER_BOUND('',#4663,.T.);
#3437=FACE_OUTER_BOUND('',#4664,.T.);
#3438=FACE_OUTER_BOUND('',#4665,.T.);
#3439=FACE_OUTER_BOUND('',#4666,.T.);
#3440=FACE_OUTER_BOUND('',#4667,.T.);
#3441=FACE_OUTER_BOUND('',#4668,.T.);
#3442=FACE_OUTER_BOUND('',#4669,.T.);
#3443=FACE_OUTER_BOUND('',#4670,.T.);
#3444=FACE_OUTER_BOUND('',#4671,.T.);
#3445=FACE_OUTER_BOUND('',#4672,.T.);
#3446=FACE_OUTER_BOUND('',#4673,.T.);
#3447=FACE_OUTER_BOUND('',#4674,.T.);
#3448=FACE_OUTER_BOUND('',#4675,.T.);
#3449=FACE_OUTER_BOUND('',#4676,.T.);
#3450=FACE_OUTER_BOUND('',#4677,.T.);
#3451=FACE_OUTER_BOUND('',#4678,.T.);
#3452=FACE_OUTER_BOUND('',#4679,.T.);
#3453=FACE_OUTER_BOUND('',#4680,.T.);
#3454=FACE_OUTER_BOUND('',#4681,.T.);
#3455=FACE_OUTER_BOUND('',#4682,.T.);
#3456=FACE_OUTER_BOUND('',#4683,.T.);
#3457=FACE_OUTER_BOUND('',#4684,.T.);
#3458=FACE_OUTER_BOUND('',#4685,.T.);
#3459=FACE_OUTER_BOUND('',#4686,.T.);
#3460=FACE_OUTER_BOUND('',#4687,.T.);
#3461=FACE_OUTER_BOUND('',#4688,.T.);
#3462=FACE_OUTER_BOUND('',#4689,.T.);
#3463=FACE_OUTER_BOUND('',#4690,.T.);
#3464=FACE_OUTER_BOUND('',#4691,.T.);
#3465=FACE_OUTER_BOUND('',#4692,.T.);
#3466=FACE_OUTER_BOUND('',#4693,.T.);
#3467=FACE_OUTER_BOUND('',#4694,.T.);
#3468=FACE_OUTER_BOUND('',#4695,.T.);
#3469=FACE_OUTER_BOUND('',#4696,.T.);
#3470=FACE_OUTER_BOUND('',#4697,.T.);
#3471=FACE_OUTER_BOUND('',#4698,.T.);
#3472=FACE_OUTER_BOUND('',#4699,.T.);
#3473=FACE_OUTER_BOUND('',#4700,.T.);
#3474=FACE_OUTER_BOUND('',#4701,.T.);
#3475=FACE_OUTER_BOUND('',#4702,.T.);
#3476=FACE_OUTER_BOUND('',#4703,.T.);
#3477=FACE_OUTER_BOUND('',#4704,.T.);
#3478=FACE_OUTER_BOUND('',#4705,.T.);
#3479=FACE_OUTER_BOUND('',#4706,.T.);
#3480=FACE_OUTER_BOUND('',#4707,.T.);
#3481=FACE_OUTER_BOUND('',#4708,.T.);
#3482=FACE_OUTER_BOUND('',#4709,.T.);
#3483=FACE_OUTER_BOUND('',#4710,.T.);
#3484=FACE_OUTER_BOUND('',#4711,.T.);
#3485=FACE_OUTER_BOUND('',#4712,.T.);
#3486=FACE_OUTER_BOUND('',#4713,.T.);
#3487=FACE_OUTER_BOUND('',#4714,.T.);
#3488=FACE_OUTER_BOUND('',#4715,.T.);
#3489=FACE_OUTER_BOUND('',#4716,.T.);
#3490=FACE_OUTER_BOUND('',#4717,.T.);
#3491=FACE_OUTER_BOUND('',#4718,.T.);
#3492=FACE_OUTER_BOUND('',#4719,.T.);
#3493=FACE_OUTER_BOUND('',#4720,.T.);
#3494=FACE_OUTER_BOUND('',#4721,.T.);
#3495=FACE_OUTER_BOUND('',#4722,.T.);
#3496=FACE_OUTER_BOUND('',#4723,.T.);
#3497=FACE_OUTER_BOUND('',#4724,.T.);
#3498=FACE_OUTER_BOUND('',#4725,.T.);
#3499=FACE_OUTER_BOUND('',#4726,.T.);
#3500=FACE_OUTER_BOUND('',#4727,.T.);
#3501=FACE_OUTER_BOUND('',#4728,.T.);
#3502=FACE_OUTER_BOUND('',#4729,.T.);
#3503=FACE_OUTER_BOUND('',#4730,.T.);
#3504=FACE_OUTER_BOUND('',#4731,.T.);
#3505=FACE_OUTER_BOUND('',#4732,.T.);
#3506=FACE_OUTER_BOUND('',#4733,.T.);
#3507=FACE_OUTER_BOUND('',#4734,.T.);
#3508=FACE_OUTER_BOUND('',#4735,.T.);
#3509=FACE_OUTER_BOUND('',#4736,.T.);
#3510=FACE_OUTER_BOUND('',#4737,.T.);
#3511=FACE_OUTER_BOUND('',#4738,.T.);
#3512=FACE_OUTER_BOUND('',#4739,.T.);
#3513=FACE_OUTER_BOUND('',#4740,.T.);
#3514=FACE_OUTER_BOUND('',#4741,.T.);
#3515=FACE_OUTER_BOUND('',#4742,.T.);
#3516=FACE_OUTER_BOUND('',#4743,.T.);
#3517=FACE_OUTER_BOUND('',#4744,.T.);
#3518=FACE_OUTER_BOUND('',#4745,.T.);
#3519=FACE_OUTER_BOUND('',#4746,.T.);
#3520=FACE_OUTER_BOUND('',#4747,.T.);
#3521=FACE_OUTER_BOUND('',#4748,.T.);
#3522=FACE_OUTER_BOUND('',#4749,.T.);
#3523=FACE_OUTER_BOUND('',#4750,.T.);
#3524=FACE_OUTER_BOUND('',#4751,.T.);
#3525=FACE_OUTER_BOUND('',#4752,.T.);
#3526=FACE_OUTER_BOUND('',#4753,.T.);
#3527=FACE_OUTER_BOUND('',#4754,.T.);
#3528=FACE_OUTER_BOUND('',#4755,.T.);
#3529=FACE_OUTER_BOUND('',#4756,.T.);
#3530=FACE_OUTER_BOUND('',#4757,.T.);
#3531=FACE_OUTER_BOUND('',#4758,.T.);
#3532=FACE_OUTER_BOUND('',#4759,.T.);
#3533=FACE_OUTER_BOUND('',#4760,.T.);
#3534=FACE_OUTER_BOUND('',#4761,.T.);
#3535=FACE_OUTER_BOUND('',#4762,.T.);
#3536=FACE_OUTER_BOUND('',#4763,.T.);
#3537=FACE_OUTER_BOUND('',#4764,.T.);
#3538=FACE_OUTER_BOUND('',#4765,.T.);
#3539=FACE_OUTER_BOUND('',#4766,.T.);
#3540=FACE_OUTER_BOUND('',#4767,.T.);
#3541=FACE_OUTER_BOUND('',#4768,.T.);
#3542=FACE_OUTER_BOUND('',#4769,.T.);
#3543=FACE_OUTER_BOUND('',#4776,.T.);
#3544=FACE_OUTER_BOUND('',#4777,.T.);
#3545=FACE_OUTER_BOUND('',#4778,.T.);
#3546=FACE_OUTER_BOUND('',#4779,.T.);
#3547=FACE_OUTER_BOUND('',#4780,.T.);
#3548=FACE_OUTER_BOUND('',#4781,.T.);
#3549=FACE_OUTER_BOUND('',#4782,.T.);
#3550=FACE_OUTER_BOUND('',#4783,.T.);
#3551=FACE_OUTER_BOUND('',#4784,.T.);
#3552=FACE_OUTER_BOUND('',#4785,.T.);
#3553=FACE_OUTER_BOUND('',#4786,.T.);
#3554=FACE_OUTER_BOUND('',#4787,.T.);
#3555=FACE_OUTER_BOUND('',#4788,.T.);
#3556=FACE_OUTER_BOUND('',#4789,.T.);
#3557=FACE_OUTER_BOUND('',#4790,.T.);
#3558=FACE_OUTER_BOUND('',#4791,.T.);
#3559=FACE_OUTER_BOUND('',#4792,.T.);
#3560=FACE_OUTER_BOUND('',#4793,.T.);
#3561=FACE_OUTER_BOUND('',#4794,.T.);
#3562=FACE_OUTER_BOUND('',#4795,.T.);
#3563=FACE_OUTER_BOUND('',#4796,.T.);
#3564=FACE_OUTER_BOUND('',#4797,.T.);
#3565=FACE_OUTER_BOUND('',#4798,.T.);
#3566=FACE_OUTER_BOUND('',#4799,.T.);
#3567=FACE_OUTER_BOUND('',#4800,.T.);
#3568=FACE_OUTER_BOUND('',#4801,.T.);
#3569=FACE_OUTER_BOUND('',#4808,.T.);
#3570=FACE_OUTER_BOUND('',#4809,.T.);
#3571=FACE_OUTER_BOUND('',#4810,.T.);
#3572=FACE_OUTER_BOUND('',#4811,.T.);
#3573=FACE_OUTER_BOUND('',#4812,.T.);
#3574=FACE_OUTER_BOUND('',#4813,.T.);
#3575=FACE_OUTER_BOUND('',#4814,.T.);
#3576=FACE_OUTER_BOUND('',#4815,.T.);
#3577=FACE_OUTER_BOUND('',#4816,.T.);
#3578=FACE_OUTER_BOUND('',#4817,.T.);
#3579=FACE_OUTER_BOUND('',#4818,.T.);
#3580=FACE_OUTER_BOUND('',#4819,.T.);
#3581=FACE_OUTER_BOUND('',#4820,.T.);
#3582=FACE_OUTER_BOUND('',#4821,.T.);
#3583=FACE_OUTER_BOUND('',#4822,.T.);
#3584=FACE_OUTER_BOUND('',#4823,.T.);
#3585=FACE_OUTER_BOUND('',#4824,.T.);
#3586=FACE_OUTER_BOUND('',#4825,.T.);
#3587=FACE_OUTER_BOUND('',#4826,.T.);
#3588=FACE_OUTER_BOUND('',#4827,.T.);
#3589=FACE_OUTER_BOUND('',#4828,.T.);
#3590=FACE_OUTER_BOUND('',#4829,.T.);
#3591=FACE_OUTER_BOUND('',#4830,.T.);
#3592=FACE_OUTER_BOUND('',#4831,.T.);
#3593=FACE_OUTER_BOUND('',#4832,.T.);
#3594=FACE_OUTER_BOUND('',#4833,.T.);
#3595=FACE_OUTER_BOUND('',#4834,.T.);
#3596=FACE_OUTER_BOUND('',#4835,.T.);
#3597=FACE_OUTER_BOUND('',#4836,.T.);
#3598=FACE_OUTER_BOUND('',#4837,.T.);
#3599=FACE_OUTER_BOUND('',#4838,.T.);
#3600=FACE_OUTER_BOUND('',#4839,.T.);
#3601=FACE_OUTER_BOUND('',#4840,.T.);
#3602=FACE_OUTER_BOUND('',#4841,.T.);
#3603=FACE_OUTER_BOUND('',#4842,.T.);
#3604=FACE_OUTER_BOUND('',#4843,.T.);
#3605=FACE_OUTER_BOUND('',#4844,.T.);
#3606=FACE_OUTER_BOUND('',#4845,.T.);
#3607=FACE_OUTER_BOUND('',#4846,.T.);
#3608=FACE_OUTER_BOUND('',#4847,.T.);
#3609=FACE_OUTER_BOUND('',#4848,.T.);
#3610=FACE_OUTER_BOUND('',#4849,.T.);
#3611=FACE_OUTER_BOUND('',#4850,.T.);
#3612=FACE_OUTER_BOUND('',#4851,.T.);
#3613=FACE_OUTER_BOUND('',#4852,.T.);
#3614=FACE_OUTER_BOUND('',#4853,.T.);
#3615=FACE_OUTER_BOUND('',#4854,.T.);
#3616=FACE_OUTER_BOUND('',#4855,.T.);
#3617=FACE_OUTER_BOUND('',#4856,.T.);
#3618=FACE_OUTER_BOUND('',#4857,.T.);
#3619=FACE_OUTER_BOUND('',#4858,.T.);
#3620=FACE_OUTER_BOUND('',#4859,.T.);
#3621=FACE_OUTER_BOUND('',#4860,.T.);
#3622=FACE_OUTER_BOUND('',#4861,.T.);
#3623=FACE_OUTER_BOUND('',#4862,.T.);
#3624=FACE_OUTER_BOUND('',#4863,.T.);
#3625=FACE_OUTER_BOUND('',#4864,.T.);
#3626=FACE_OUTER_BOUND('',#4865,.T.);
#3627=FACE_OUTER_BOUND('',#4866,.T.);
#3628=FACE_OUTER_BOUND('',#4867,.T.);
#3629=FACE_OUTER_BOUND('',#4868,.T.);
#3630=FACE_OUTER_BOUND('',#4869,.T.);
#3631=FACE_OUTER_BOUND('',#4870,.T.);
#3632=FACE_OUTER_BOUND('',#4871,.T.);
#3633=FACE_OUTER_BOUND('',#4872,.T.);
#3634=FACE_OUTER_BOUND('',#4873,.T.);
#3635=FACE_OUTER_BOUND('',#4874,.T.);
#3636=FACE_OUTER_BOUND('',#4875,.T.);
#3637=FACE_OUTER_BOUND('',#4876,.T.);
#3638=FACE_OUTER_BOUND('',#4877,.T.);
#3639=FACE_OUTER_BOUND('',#4878,.T.);
#3640=FACE_OUTER_BOUND('',#4879,.T.);
#3641=FACE_OUTER_BOUND('',#4880,.T.);
#3642=FACE_OUTER_BOUND('',#4881,.T.);
#3643=FACE_OUTER_BOUND('',#4882,.T.);
#3644=FACE_OUTER_BOUND('',#4883,.T.);
#3645=FACE_OUTER_BOUND('',#4884,.T.);
#3646=FACE_OUTER_BOUND('',#4885,.T.);
#3647=FACE_OUTER_BOUND('',#4886,.T.);
#3648=FACE_OUTER_BOUND('',#4887,.T.);
#3649=FACE_OUTER_BOUND('',#4888,.T.);
#3650=FACE_OUTER_BOUND('',#4889,.T.);
#3651=FACE_OUTER_BOUND('',#4890,.T.);
#3652=FACE_OUTER_BOUND('',#4891,.T.);
#3653=FACE_OUTER_BOUND('',#4892,.T.);
#3654=FACE_OUTER_BOUND('',#4893,.T.);
#3655=FACE_OUTER_BOUND('',#4894,.T.);
#3656=FACE_OUTER_BOUND('',#4895,.T.);
#3657=FACE_OUTER_BOUND('',#4896,.T.);
#3658=FACE_OUTER_BOUND('',#4897,.T.);
#3659=FACE_OUTER_BOUND('',#4898,.T.);
#3660=FACE_OUTER_BOUND('',#4899,.T.);
#3661=FACE_OUTER_BOUND('',#4900,.T.);
#3662=FACE_OUTER_BOUND('',#4901,.T.);
#3663=FACE_OUTER_BOUND('',#4902,.T.);
#3664=FACE_OUTER_BOUND('',#4903,.T.);
#3665=FACE_OUTER_BOUND('',#4904,.T.);
#3666=FACE_OUTER_BOUND('',#4905,.T.);
#3667=FACE_OUTER_BOUND('',#4906,.T.);
#3668=FACE_OUTER_BOUND('',#4907,.T.);
#3669=FACE_OUTER_BOUND('',#4908,.T.);
#3670=FACE_OUTER_BOUND('',#4909,.T.);
#3671=FACE_OUTER_BOUND('',#4910,.T.);
#3672=FACE_OUTER_BOUND('',#4911,.T.);
#3673=FACE_OUTER_BOUND('',#4912,.T.);
#3674=FACE_OUTER_BOUND('',#4913,.T.);
#3675=FACE_OUTER_BOUND('',#4914,.T.);
#3676=FACE_OUTER_BOUND('',#4915,.T.);
#3677=FACE_OUTER_BOUND('',#4916,.T.);
#3678=FACE_OUTER_BOUND('',#4917,.T.);
#3679=FACE_OUTER_BOUND('',#4918,.T.);
#3680=FACE_OUTER_BOUND('',#4920,.T.);
#3681=FACE_OUTER_BOUND('',#4921,.T.);
#3682=FACE_OUTER_BOUND('',#4923,.T.);
#3683=FACE_OUTER_BOUND('',#4924,.T.);
#3684=FACE_OUTER_BOUND('',#4925,.T.);
#3685=FACE_OUTER_BOUND('',#4926,.T.);
#3686=FACE_OUTER_BOUND('',#4928,.T.);
#3687=FACE_OUTER_BOUND('',#4930,.T.);
#3688=FACE_OUTER_BOUND('',#4931,.T.);
#3689=FACE_OUTER_BOUND('',#4932,.T.);
#3690=FACE_OUTER_BOUND('',#4934,.T.);
#3691=EDGE_LOOP('',(#13112,#13113,#13114,#13115));
#3692=EDGE_LOOP('',(#13116,#13117,#13118,#13119));
#3693=EDGE_LOOP('',(#13120,#13121,#13122,#13123));
#3694=EDGE_LOOP('',(#13124,#13125,#13126,#13127));
#3695=EDGE_LOOP('',(#13128,#13129,#13130,#13131));
#3696=EDGE_LOOP('',(#13132,#13133,#13134,#13135));
#3697=EDGE_LOOP('',(#13136,#13137,#13138,#13139));
#3698=EDGE_LOOP('',(#13140,#13141,#13142,#13143));
#3699=EDGE_LOOP('',(#13144));
#3700=EDGE_LOOP('',(#13145));
#3701=EDGE_LOOP('',(#13146));
#3702=EDGE_LOOP('',(#13147,#13148,#13149,#13150));
#3703=EDGE_LOOP('',(#13151,#13152,#13153,#13154));
#3704=EDGE_LOOP('',(#13155));
#3705=EDGE_LOOP('',(#13156));
#3706=EDGE_LOOP('',(#13157));
#3707=EDGE_LOOP('',(#13158,#13159,#13160,#13161));
#3708=EDGE_LOOP('',(#13162,#13163,#13164,#13165));
#3709=EDGE_LOOP('',(#13166));
#3710=EDGE_LOOP('',(#13167));
#3711=EDGE_LOOP('',(#13168));
#3712=EDGE_LOOP('',(#13169,#13170,#13171,#13172));
#3713=EDGE_LOOP('',(#13173,#13174,#13175,#13176));
#3714=EDGE_LOOP('',(#13177));
#3715=EDGE_LOOP('',(#13178));
#3716=EDGE_LOOP('',(#13179));
#3717=EDGE_LOOP('',(#13180,#13181,#13182,#13183));
#3718=EDGE_LOOP('',(#13184,#13185,#13186,#13187));
#3719=EDGE_LOOP('',(#13188,#13189,#13190,#13191));
#3720=EDGE_LOOP('',(#13192,#13193,#13194,#13195));
#3721=EDGE_LOOP('',(#13196,#13197,#13198,#13199));
#3722=EDGE_LOOP('',(#13200,#13201,#13202,#13203));
#3723=EDGE_LOOP('',(#13204,#13205,#13206,#13207));
#3724=EDGE_LOOP('',(#13208,#13209,#13210,#13211));
#3725=EDGE_LOOP('',(#13212,#13213,#13214,#13215));
#3726=EDGE_LOOP('',(#13216,#13217,#13218,#13219));
#3727=EDGE_LOOP('',(#13220,#13221,#13222,#13223));
#3728=EDGE_LOOP('',(#13224,#13225,#13226,#13227));
#3729=EDGE_LOOP('',(#13228,#13229,#13230,#13231));
#3730=EDGE_LOOP('',(#13232,#13233,#13234,#13235));
#3731=EDGE_LOOP('',(#13236,#13237,#13238,#13239));
#3732=EDGE_LOOP('',(#13240,#13241,#13242,#13243));
#3733=EDGE_LOOP('',(#13244,#13245,#13246,#13247));
#3734=EDGE_LOOP('',(#13248,#13249,#13250,#13251));
#3735=EDGE_LOOP('',(#13252,#13253,#13254,#13255));
#3736=EDGE_LOOP('',(#13256,#13257,#13258,#13259));
#3737=EDGE_LOOP('',(#13260,#13261,#13262,#13263));
#3738=EDGE_LOOP('',(#13264,#13265,#13266,#13267));
#3739=EDGE_LOOP('',(#13268,#13269,#13270,#13271));
#3740=EDGE_LOOP('',(#13272,#13273,#13274,#13275));
#3741=EDGE_LOOP('',(#13276,#13277,#13278,#13279));
#3742=EDGE_LOOP('',(#13280,#13281,#13282,#13283));
#3743=EDGE_LOOP('',(#13284,#13285,#13286,#13287));
#3744=EDGE_LOOP('',(#13288,#13289,#13290,#13291));
#3745=EDGE_LOOP('',(#13292,#13293,#13294,#13295));
#3746=EDGE_LOOP('',(#13296,#13297,#13298,#13299));
#3747=EDGE_LOOP('',(#13300,#13301,#13302,#13303));
#3748=EDGE_LOOP('',(#13304,#13305,#13306,#13307));
#3749=EDGE_LOOP('',(#13308,#13309,#13310,#13311));
#3750=EDGE_LOOP('',(#13312,#13313,#13314,#13315));
#3751=EDGE_LOOP('',(#13316,#13317,#13318,#13319));
#3752=EDGE_LOOP('',(#13320,#13321,#13322,#13323));
#3753=EDGE_LOOP('',(#13324,#13325,#13326,#13327));
#3754=EDGE_LOOP('',(#13328,#13329,#13330,#13331));
#3755=EDGE_LOOP('',(#13332,#13333,#13334,#13335));
#3756=EDGE_LOOP('',(#13336,#13337,#13338,#13339));
#3757=EDGE_LOOP('',(#13340,#13341,#13342,#13343));
#3758=EDGE_LOOP('',(#13344,#13345,#13346,#13347));
#3759=EDGE_LOOP('',(#13348,#13349,#13350,#13351));
#3760=EDGE_LOOP('',(#13352,#13353,#13354,#13355));
#3761=EDGE_LOOP('',(#13356,#13357,#13358,#13359));
#3762=EDGE_LOOP('',(#13360,#13361,#13362,#13363));
#3763=EDGE_LOOP('',(#13364,#13365,#13366,#13367));
#3764=EDGE_LOOP('',(#13368,#13369,#13370,#13371));
#3765=EDGE_LOOP('',(#13372,#13373,#13374,#13375));
#3766=EDGE_LOOP('',(#13376,#13377,#13378,#13379));
#3767=EDGE_LOOP('',(#13380,#13381,#13382,#13383));
#3768=EDGE_LOOP('',(#13384,#13385,#13386,#13387));
#3769=EDGE_LOOP('',(#13388,#13389,#13390,#13391));
#3770=EDGE_LOOP('',(#13392,#13393,#13394,#13395));
#3771=EDGE_LOOP('',(#13396,#13397,#13398,#13399));
#3772=EDGE_LOOP('',(#13400,#13401,#13402,#13403));
#3773=EDGE_LOOP('',(#13404,#13405,#13406,#13407));
#3774=EDGE_LOOP('',(#13408,#13409,#13410,#13411));
#3775=EDGE_LOOP('',(#13412,#13413,#13414,#13415));
#3776=EDGE_LOOP('',(#13416,#13417,#13418,#13419));
#3777=EDGE_LOOP('',(#13420,#13421,#13422,#13423));
#3778=EDGE_LOOP('',(#13424,#13425,#13426,#13427));
#3779=EDGE_LOOP('',(#13428,#13429,#13430,#13431));
#3780=EDGE_LOOP('',(#13432,#13433,#13434,#13435));
#3781=EDGE_LOOP('',(#13436,#13437,#13438,#13439));
#3782=EDGE_LOOP('',(#13440,#13441,#13442,#13443));
#3783=EDGE_LOOP('',(#13444,#13445,#13446,#13447));
#3784=EDGE_LOOP('',(#13448,#13449,#13450,#13451));
#3785=EDGE_LOOP('',(#13452,#13453,#13454,#13455));
#3786=EDGE_LOOP('',(#13456,#13457,#13458,#13459));
#3787=EDGE_LOOP('',(#13460,#13461,#13462,#13463));
#3788=EDGE_LOOP('',(#13464,#13465,#13466,#13467));
#3789=EDGE_LOOP('',(#13468,#13469,#13470,#13471));
#3790=EDGE_LOOP('',(#13472,#13473,#13474,#13475));
#3791=EDGE_LOOP('',(#13476,#13477,#13478,#13479));
#3792=EDGE_LOOP('',(#13480,#13481,#13482,#13483));
#3793=EDGE_LOOP('',(#13484,#13485,#13486,#13487));
#3794=EDGE_LOOP('',(#13488,#13489,#13490,#13491));
#3795=EDGE_LOOP('',(#13492,#13493,#13494,#13495));
#3796=EDGE_LOOP('',(#13496,#13497,#13498,#13499));
#3797=EDGE_LOOP('',(#13500,#13501,#13502,#13503));
#3798=EDGE_LOOP('',(#13504,#13505,#13506,#13507,#13508,#13509,#13510,#13511,
#13512,#13513,#13514,#13515,#13516,#13517,#13518,#13519,#13520,#13521,#13522,
#13523));
#3799=EDGE_LOOP('',(#13524,#13525,#13526,#13527,#13528,#13529,#13530,#13531,
#13532,#13533,#13534,#13535,#13536,#13537,#13538,#13539,#13540,#13541,#13542,
#13543));
#3800=EDGE_LOOP('',(#13544,#13545,#13546,#13547));
#3801=EDGE_LOOP('',(#13548,#13549,#13550,#13551));
#3802=EDGE_LOOP('',(#13552,#13553,#13554,#13555));
#3803=EDGE_LOOP('',(#13556,#13557,#13558,#13559));
#3804=EDGE_LOOP('',(#13560,#13561,#13562,#13563));
#3805=EDGE_LOOP('',(#13564,#13565,#13566,#13567));
#3806=EDGE_LOOP('',(#13568,#13569,#13570,#13571,#13572,#13573,#13574,#13575,
#13576,#13577,#13578,#13579,#13580,#13581,#13582,#13583,#13584,#13585,#13586,
#13587));
#3807=EDGE_LOOP('',(#13588,#13589,#13590,#13591,#13592,#13593,#13594,#13595,
#13596,#13597,#13598,#13599,#13600,#13601,#13602,#13603,#13604,#13605,#13606,
#13607));
#3808=EDGE_LOOP('',(#13608,#13609,#13610,#13611));
#3809=EDGE_LOOP('',(#13612,#13613,#13614,#13615,#13616,#13617,#13618,#13619,
#13620,#13621,#13622,#13623,#13624,#13625,#13626,#13627,#13628,#13629,#13630,
#13631));
#3810=EDGE_LOOP('',(#13632,#13633,#13634,#13635,#13636,#13637,#13638,#13639,
#13640,#13641,#13642,#13643,#13644,#13645,#13646,#13647,#13648,#13649,#13650,
#13651));
#3811=EDGE_LOOP('',(#13652,#13653,#13654,#13655));
#3812=EDGE_LOOP('',(#13656,#13657,#13658,#13659,#13660,#13661,#13662,#13663,
#13664,#13665,#13666,#13667,#13668,#13669,#13670,#13671,#13672,#13673,#13674,
#13675));
#3813=EDGE_LOOP('',(#13676,#13677,#13678,#13679,#13680,#13681,#13682,#13683,
#13684,#13685,#13686,#13687,#13688,#13689,#13690,#13691,#13692,#13693,#13694,
#13695));
#3814=EDGE_LOOP('',(#13696,#13697,#13698,#13699));
#3815=EDGE_LOOP('',(#13700,#13701,#13702,#13703));
#3816=EDGE_LOOP('',(#13704,#13705,#13706,#13707));
#3817=EDGE_LOOP('',(#13708,#13709,#13710,#13711));
#3818=EDGE_LOOP('',(#13712,#13713,#13714,#13715));
#3819=EDGE_LOOP('',(#13716,#13717,#13718,#13719));
#3820=EDGE_LOOP('',(#13720,#13721,#13722,#13723));
#3821=EDGE_LOOP('',(#13724,#13725,#13726,#13727));
#3822=EDGE_LOOP('',(#13728,#13729,#13730,#13731));
#3823=EDGE_LOOP('',(#13732,#13733,#13734,#13735));
#3824=EDGE_LOOP('',(#13736,#13737,#13738,#13739));
#3825=EDGE_LOOP('',(#13740,#13741,#13742,#13743));
#3826=EDGE_LOOP('',(#13744,#13745,#13746,#13747));
#3827=EDGE_LOOP('',(#13748,#13749,#13750,#13751));
#3828=EDGE_LOOP('',(#13752,#13753,#13754,#13755));
#3829=EDGE_LOOP('',(#13756,#13757,#13758,#13759));
#3830=EDGE_LOOP('',(#13760,#13761,#13762,#13763));
#3831=EDGE_LOOP('',(#13764,#13765,#13766,#13767));
#3832=EDGE_LOOP('',(#13768,#13769,#13770,#13771));
#3833=EDGE_LOOP('',(#13772,#13773,#13774,#13775));
#3834=EDGE_LOOP('',(#13776,#13777,#13778,#13779));
#3835=EDGE_LOOP('',(#13780,#13781,#13782,#13783));
#3836=EDGE_LOOP('',(#13784,#13785,#13786,#13787));
#3837=EDGE_LOOP('',(#13788,#13789,#13790,#13791));
#3838=EDGE_LOOP('',(#13792,#13793,#13794,#13795));
#3839=EDGE_LOOP('',(#13796,#13797,#13798,#13799));
#3840=EDGE_LOOP('',(#13800,#13801,#13802,#13803));
#3841=EDGE_LOOP('',(#13804,#13805,#13806,#13807));
#3842=EDGE_LOOP('',(#13808,#13809,#13810,#13811));
#3843=EDGE_LOOP('',(#13812,#13813,#13814,#13815));
#3844=EDGE_LOOP('',(#13816,#13817,#13818,#13819));
#3845=EDGE_LOOP('',(#13820,#13821,#13822,#13823));
#3846=EDGE_LOOP('',(#13824,#13825,#13826,#13827));
#3847=EDGE_LOOP('',(#13828,#13829,#13830,#13831));
#3848=EDGE_LOOP('',(#13832,#13833,#13834,#13835));
#3849=EDGE_LOOP('',(#13836,#13837,#13838,#13839));
#3850=EDGE_LOOP('',(#13840,#13841,#13842,#13843));
#3851=EDGE_LOOP('',(#13844,#13845,#13846,#13847));
#3852=EDGE_LOOP('',(#13848,#13849,#13850,#13851));
#3853=EDGE_LOOP('',(#13852,#13853,#13854,#13855));
#3854=EDGE_LOOP('',(#13856,#13857,#13858,#13859));
#3855=EDGE_LOOP('',(#13860,#13861,#13862,#13863));
#3856=EDGE_LOOP('',(#13864,#13865,#13866,#13867));
#3857=EDGE_LOOP('',(#13868,#13869,#13870,#13871));
#3858=EDGE_LOOP('',(#13872,#13873,#13874,#13875));
#3859=EDGE_LOOP('',(#13876,#13877,#13878,#13879));
#3860=EDGE_LOOP('',(#13880,#13881,#13882,#13883));
#3861=EDGE_LOOP('',(#13884,#13885,#13886,#13887));
#3862=EDGE_LOOP('',(#13888,#13889,#13890,#13891));
#3863=EDGE_LOOP('',(#13892,#13893,#13894,#13895));
#3864=EDGE_LOOP('',(#13896,#13897,#13898,#13899));
#3865=EDGE_LOOP('',(#13900,#13901,#13902,#13903));
#3866=EDGE_LOOP('',(#13904,#13905,#13906,#13907));
#3867=EDGE_LOOP('',(#13908,#13909,#13910,#13911));
#3868=EDGE_LOOP('',(#13912,#13913,#13914,#13915));
#3869=EDGE_LOOP('',(#13916,#13917,#13918,#13919));
#3870=EDGE_LOOP('',(#13920,#13921,#13922,#13923));
#3871=EDGE_LOOP('',(#13924,#13925,#13926,#13927));
#3872=EDGE_LOOP('',(#13928,#13929,#13930,#13931));
#3873=EDGE_LOOP('',(#13932,#13933,#13934,#13935));
#3874=EDGE_LOOP('',(#13936,#13937,#13938,#13939));
#3875=EDGE_LOOP('',(#13940,#13941,#13942,#13943,#13944,#13945,#13946,#13947));
#3876=EDGE_LOOP('',(#13948,#13949,#13950,#13951,#13952,#13953,#13954,#13955,
#13956,#13957,#13958,#13959,#13960,#13961,#13962,#13963,#13964,#13965,#13966,
#13967,#13968,#13969,#13970,#13971,#13972,#13973,#13974,#13975,#13976,#13977,
#13978,#13979,#13980,#13981,#13982,#13983,#13984,#13985,#13986,#13987,#13988,
#13989,#13990,#13991,#13992,#13993,#13994,#13995,#13996,#13997,#13998,#13999));
#3877=EDGE_LOOP('',(#14000,#14001,#14002,#14003));
#3878=EDGE_LOOP('',(#14004,#14005,#14006,#14007,#14008,#14009,#14010,#14011,
#14012,#14013,#14014,#14015,#14016,#14017,#14018,#14019,#14020,#14021,#14022,
#14023,#14024,#14025,#14026,#14027,#14028,#14029,#14030,#14031,#14032,#14033,
#14034,#14035,#14036,#14037,#14038,#14039,#14040,#14041,#14042,#14043,#14044,
#14045,#14046,#14047,#14048,#14049,#14050,#14051,#14052,#14053,#14054,#14055,
#14056));
#3879=EDGE_LOOP('',(#14057,#14058,#14059,#14060));
#3880=EDGE_LOOP('',(#14061,#14062,#14063,#14064));
#3881=EDGE_LOOP('',(#14065,#14066,#14067,#14068));
#3882=EDGE_LOOP('',(#14069,#14070,#14071,#14072));
#3883=EDGE_LOOP('',(#14073,#14074,#14075,#14076));
#3884=EDGE_LOOP('',(#14077,#14078,#14079,#14080));
#3885=EDGE_LOOP('',(#14081,#14082,#14083,#14084));
#3886=EDGE_LOOP('',(#14085,#14086,#14087,#14088,#14089,#14090));
#3887=EDGE_LOOP('',(#14091));
#3888=EDGE_LOOP('',(#14092,#14093,#14094,#14095));
#3889=EDGE_LOOP('',(#14096,#14097,#14098,#14099));
#3890=EDGE_LOOP('',(#14100));
#3891=EDGE_LOOP('',(#14101,#14102,#14103,#14104,#14105,#14106));
#3892=EDGE_LOOP('',(#14107));
#3893=EDGE_LOOP('',(#14108,#14109,#14110,#14111));
#3894=EDGE_LOOP('',(#14112,#14113,#14114,#14115));
#3895=EDGE_LOOP('',(#14116));
#3896=EDGE_LOOP('',(#14117));
#3897=EDGE_LOOP('',(#14118));
#3898=EDGE_LOOP('',(#14119));
#3899=EDGE_LOOP('',(#14120,#14121,#14122,#14123,#14124,#14125,#14126,#14127));
#3900=EDGE_LOOP('',(#14128,#14129,#14130,#14131));
#3901=EDGE_LOOP('',(#14132,#14133,#14134,#14135));
#3902=EDGE_LOOP('',(#14136,#14137,#14138,#14139));
#3903=EDGE_LOOP('',(#14140,#14141,#14142,#14143));
#3904=EDGE_LOOP('',(#14144,#14145,#14146,#14147));
#3905=EDGE_LOOP('',(#14148,#14149,#14150,#14151));
#3906=EDGE_LOOP('',(#14152,#14153,#14154,#14155));
#3907=EDGE_LOOP('',(#14156,#14157,#14158,#14159));
#3908=EDGE_LOOP('',(#14160,#14161,#14162,#14163));
#3909=EDGE_LOOP('',(#14164,#14165,#14166,#14167));
#3910=EDGE_LOOP('',(#14168,#14169,#14170,#14171));
#3911=EDGE_LOOP('',(#14172,#14173,#14174,#14175));
#3912=EDGE_LOOP('',(#14176,#14177,#14178,#14179));
#3913=EDGE_LOOP('',(#14180,#14181,#14182,#14183));
#3914=EDGE_LOOP('',(#14184,#14185,#14186,#14187));
#3915=EDGE_LOOP('',(#14188,#14189,#14190,#14191));
#3916=EDGE_LOOP('',(#14192,#14193,#14194,#14195));
#3917=EDGE_LOOP('',(#14196,#14197,#14198,#14199));
#3918=EDGE_LOOP('',(#14200,#14201,#14202,#14203));
#3919=EDGE_LOOP('',(#14204,#14205,#14206,#14207));
#3920=EDGE_LOOP('',(#14208,#14209,#14210,#14211));
#3921=EDGE_LOOP('',(#14212,#14213,#14214,#14215));
#3922=EDGE_LOOP('',(#14216,#14217,#14218,#14219));
#3923=EDGE_LOOP('',(#14220,#14221,#14222,#14223));
#3924=EDGE_LOOP('',(#14224,#14225,#14226,#14227));
#3925=EDGE_LOOP('',(#14228,#14229,#14230,#14231));
#3926=EDGE_LOOP('',(#14232,#14233,#14234,#14235));
#3927=EDGE_LOOP('',(#14236,#14237,#14238,#14239));
#3928=EDGE_LOOP('',(#14240,#14241,#14242,#14243));
#3929=EDGE_LOOP('',(#14244,#14245,#14246,#14247));
#3930=EDGE_LOOP('',(#14248,#14249,#14250,#14251));
#3931=EDGE_LOOP('',(#14252,#14253,#14254,#14255));
#3932=EDGE_LOOP('',(#14256,#14257,#14258,#14259));
#3933=EDGE_LOOP('',(#14260,#14261,#14262,#14263));
#3934=EDGE_LOOP('',(#14264,#14265,#14266,#14267));
#3935=EDGE_LOOP('',(#14268,#14269,#14270,#14271));
#3936=EDGE_LOOP('',(#14272,#14273,#14274,#14275));
#3937=EDGE_LOOP('',(#14276,#14277,#14278,#14279));
#3938=EDGE_LOOP('',(#14280,#14281,#14282,#14283));
#3939=EDGE_LOOP('',(#14284,#14285,#14286,#14287));
#3940=EDGE_LOOP('',(#14288,#14289,#14290,#14291));
#3941=EDGE_LOOP('',(#14292,#14293,#14294,#14295));
#3942=EDGE_LOOP('',(#14296,#14297,#14298,#14299));
#3943=EDGE_LOOP('',(#14300,#14301,#14302,#14303));
#3944=EDGE_LOOP('',(#14304,#14305,#14306,#14307));
#3945=EDGE_LOOP('',(#14308,#14309,#14310,#14311));
#3946=EDGE_LOOP('',(#14312,#14313,#14314,#14315));
#3947=EDGE_LOOP('',(#14316,#14317,#14318,#14319));
#3948=EDGE_LOOP('',(#14320,#14321,#14322,#14323));
#3949=EDGE_LOOP('',(#14324,#14325,#14326,#14327,#14328,#14329,#14330,#14331));
#3950=EDGE_LOOP('',(#14332,#14333,#14334,#14335));
#3951=EDGE_LOOP('',(#14336,#14337,#14338,#14339));
#3952=EDGE_LOOP('',(#14340,#14341,#14342,#14343));
#3953=EDGE_LOOP('',(#14344,#14345,#14346,#14347));
#3954=EDGE_LOOP('',(#14348,#14349,#14350,#14351));
#3955=EDGE_LOOP('',(#14352,#14353,#14354,#14355));
#3956=EDGE_LOOP('',(#14356,#14357,#14358,#14359));
#3957=EDGE_LOOP('',(#14360,#14361,#14362,#14363));
#3958=EDGE_LOOP('',(#14364,#14365,#14366,#14367));
#3959=EDGE_LOOP('',(#14368,#14369,#14370,#14371));
#3960=EDGE_LOOP('',(#14372,#14373,#14374,#14375));
#3961=EDGE_LOOP('',(#14376,#14377,#14378,#14379));
#3962=EDGE_LOOP('',(#14380,#14381,#14382,#14383));
#3963=EDGE_LOOP('',(#14384,#14385,#14386,#14387));
#3964=EDGE_LOOP('',(#14388,#14389,#14390,#14391));
#3965=EDGE_LOOP('',(#14392,#14393,#14394,#14395));
#3966=EDGE_LOOP('',(#14396,#14397,#14398,#14399));
#3967=EDGE_LOOP('',(#14400,#14401,#14402,#14403));
#3968=EDGE_LOOP('',(#14404,#14405,#14406,#14407));
#3969=EDGE_LOOP('',(#14408,#14409,#14410,#14411));
#3970=EDGE_LOOP('',(#14412,#14413,#14414,#14415));
#3971=EDGE_LOOP('',(#14416,#14417,#14418,#14419));
#3972=EDGE_LOOP('',(#14420,#14421,#14422,#14423));
#3973=EDGE_LOOP('',(#14424,#14425,#14426,#14427));
#3974=EDGE_LOOP('',(#14428,#14429,#14430,#14431));
#3975=EDGE_LOOP('',(#14432,#14433,#14434,#14435));
#3976=EDGE_LOOP('',(#14436,#14437,#14438,#14439));
#3977=EDGE_LOOP('',(#14440,#14441,#14442,#14443));
#3978=EDGE_LOOP('',(#14444,#14445,#14446,#14447));
#3979=EDGE_LOOP('',(#14448,#14449,#14450,#14451));
#3980=EDGE_LOOP('',(#14452,#14453,#14454,#14455));
#3981=EDGE_LOOP('',(#14456,#14457,#14458,#14459));
#3982=EDGE_LOOP('',(#14460,#14461,#14462,#14463));
#3983=EDGE_LOOP('',(#14464,#14465,#14466,#14467));
#3984=EDGE_LOOP('',(#14468,#14469,#14470,#14471));
#3985=EDGE_LOOP('',(#14472,#14473,#14474,#14475));
#3986=EDGE_LOOP('',(#14476,#14477,#14478,#14479));
#3987=EDGE_LOOP('',(#14480,#14481,#14482,#14483));
#3988=EDGE_LOOP('',(#14484,#14485,#14486,#14487));
#3989=EDGE_LOOP('',(#14488,#14489,#14490,#14491));
#3990=EDGE_LOOP('',(#14492,#14493,#14494,#14495));
#3991=EDGE_LOOP('',(#14496,#14497,#14498,#14499));
#3992=EDGE_LOOP('',(#14500,#14501,#14502,#14503));
#3993=EDGE_LOOP('',(#14504,#14505,#14506,#14507));
#3994=EDGE_LOOP('',(#14508,#14509,#14510,#14511));
#3995=EDGE_LOOP('',(#14512,#14513,#14514,#14515));
#3996=EDGE_LOOP('',(#14516,#14517,#14518,#14519));
#3997=EDGE_LOOP('',(#14520,#14521,#14522,#14523));
#3998=EDGE_LOOP('',(#14524,#14525,#14526,#14527));
#3999=EDGE_LOOP('',(#14528,#14529,#14530,#14531));
#4000=EDGE_LOOP('',(#14532,#14533,#14534,#14535));
#4001=EDGE_LOOP('',(#14536,#14537,#14538,#14539));
#4002=EDGE_LOOP('',(#14540,#14541,#14542,#14543));
#4003=EDGE_LOOP('',(#14544,#14545,#14546,#14547));
#4004=EDGE_LOOP('',(#14548,#14549,#14550,#14551));
#4005=EDGE_LOOP('',(#14552,#14553,#14554,#14555));
#4006=EDGE_LOOP('',(#14556,#14557,#14558,#14559));
#4007=EDGE_LOOP('',(#14560,#14561,#14562,#14563));
#4008=EDGE_LOOP('',(#14564,#14565,#14566,#14567));
#4009=EDGE_LOOP('',(#14568,#14569,#14570,#14571));
#4010=EDGE_LOOP('',(#14572,#14573,#14574,#14575));
#4011=EDGE_LOOP('',(#14576,#14577,#14578,#14579));
#4012=EDGE_LOOP('',(#14580,#14581,#14582,#14583));
#4013=EDGE_LOOP('',(#14584,#14585,#14586,#14587));
#4014=EDGE_LOOP('',(#14588,#14589,#14590,#14591));
#4015=EDGE_LOOP('',(#14592,#14593,#14594,#14595));
#4016=EDGE_LOOP('',(#14596,#14597,#14598,#14599));
#4017=EDGE_LOOP('',(#14600,#14601,#14602,#14603));
#4018=EDGE_LOOP('',(#14604,#14605,#14606,#14607));
#4019=EDGE_LOOP('',(#14608,#14609,#14610,#14611));
#4020=EDGE_LOOP('',(#14612,#14613,#14614,#14615));
#4021=EDGE_LOOP('',(#14616,#14617,#14618,#14619));
#4022=EDGE_LOOP('',(#14620,#14621,#14622,#14623));
#4023=EDGE_LOOP('',(#14624,#14625,#14626,#14627));
#4024=EDGE_LOOP('',(#14628,#14629,#14630,#14631));
#4025=EDGE_LOOP('',(#14632,#14633,#14634,#14635));
#4026=EDGE_LOOP('',(#14636,#14637,#14638,#14639));
#4027=EDGE_LOOP('',(#14640,#14641,#14642,#14643));
#4028=EDGE_LOOP('',(#14644,#14645,#14646,#14647));
#4029=EDGE_LOOP('',(#14648,#14649,#14650,#14651,#14652));
#4030=EDGE_LOOP('',(#14653,#14654,#14655,#14656));
#4031=EDGE_LOOP('',(#14657,#14658,#14659,#14660,#14661,#14662,#14663,#14664,
#14665,#14666,#14667,#14668,#14669,#14670,#14671,#14672,#14673,#14674,#14675,
#14676,#14677,#14678,#14679,#14680,#14681,#14682,#14683,#14684,#14685,#14686,
#14687,#14688,#14689,#14690,#14691,#14692,#14693,#14694,#14695,#14696,#14697,
#14698,#14699,#14700,#14701,#14702,#14703,#14704,#14705,#14706,#14707,#14708,
#14709,#14710,#14711,#14712,#14713,#14714,#14715,#14716,#14717,#14718,#14719,
#14720,#14721,#14722,#14723,#14724,#14725,#14726,#14727,#14728,#14729,#14730,
#14731,#14732,#14733,#14734,#14735,#14736,#14737,#14738,#14739,#14740));
#4032=EDGE_LOOP('',(#14741,#14742,#14743,#14744,#14745,#14746,#14747,#14748,
#14749,#14750,#14751,#14752,#14753,#14754,#14755,#14756,#14757,#14758,#14759,
#14760,#14761,#14762,#14763,#14764,#14765,#14766,#14767,#14768,#14769,#14770,
#14771,#14772,#14773,#14774,#14775,#14776,#14777,#14778,#14779,#14780,#14781,
#14782,#14783,#14784,#14785,#14786,#14787,#14788,#14789,#14790,#14791,#14792,
#14793,#14794,#14795,#14796,#14797,#14798,#14799,#14800,#14801,#14802,#14803,
#14804,#14805,#14806,#14807,#14808,#14809,#14810,#14811,#14812,#14813,#14814,
#14815,#14816,#14817,#14818,#14819,#14820,#14821,#14822,#14823,#14824));
#4033=EDGE_LOOP('',(#14825,#14826,#14827,#14828));
#4034=EDGE_LOOP('',(#14829));
#4035=EDGE_LOOP('',(#14830));
#4036=EDGE_LOOP('',(#14831,#14832,#14833,#14834,#14835));
#4037=EDGE_LOOP('',(#14836,#14837,#14838,#14839));
#4038=EDGE_LOOP('',(#14840,#14841,#14842,#14843,#14844,#14845,#14846,#14847,
#14848,#14849,#14850,#14851,#14852,#14853,#14854,#14855,#14856,#14857,#14858,
#14859,#14860,#14861,#14862,#14863,#14864,#14865,#14866,#14867,#14868,#14869,
#14870,#14871,#14872,#14873,#14874,#14875,#14876,#14877,#14878,#14879,#14880,
#14881,#14882,#14883,#14884,#14885,#14886,#14887,#14888,#14889,#14890,#14891,
#14892,#14893));
#4039=EDGE_LOOP('',(#14894,#14895,#14896,#14897,#14898,#14899,#14900,#14901,
#14902,#14903,#14904,#14905,#14906,#14907,#14908,#14909,#14910,#14911,#14912,
#14913,#14914,#14915,#14916,#14917,#14918,#14919,#14920,#14921,#14922,#14923,
#14924,#14925,#14926,#14927,#14928,#14929,#14930,#14931,#14932,#14933,#14934,
#14935,#14936,#14937,#14938,#14939,#14940,#14941,#14942,#14943,#14944,#14945,
#14946,#14947));
#4040=EDGE_LOOP('',(#14948,#14949,#14950,#14951));
#4041=EDGE_LOOP('',(#14952));
#4042=EDGE_LOOP('',(#14953));
#4043=EDGE_LOOP('',(#14954,#14955,#14956,#14957));
#4044=EDGE_LOOP('',(#14958,#14959,#14960,#14961));
#4045=EDGE_LOOP('',(#14962,#14963,#14964,#14965,#14966,#14967,#14968,#14969,
#14970,#14971,#14972,#14973,#14974,#14975,#14976,#14977,#14978,#14979,#14980,
#14981,#14982,#14983,#14984,#14985,#14986,#14987,#14988,#14989,#14990,#14991,
#14992,#14993,#14994,#14995,#14996,#14997,#14998,#14999,#15000,#15001,#15002,
#15003,#15004,#15005,#15006,#15007,#15008,#15009,#15010,#15011,#15012,#15013,
#15014,#15015,#15016,#15017,#15018,#15019,#15020,#15021,#15022,#15023,#15024,
#15025,#15026,#15027,#15028,#15029,#15030,#15031,#15032,#15033));
#4046=EDGE_LOOP('',(#15034,#15035,#15036,#15037));
#4047=EDGE_LOOP('',(#15038));
#4048=EDGE_LOOP('',(#15039));
#4049=EDGE_LOOP('',(#15040));
#4050=EDGE_LOOP('',(#15041));
#4051=EDGE_LOOP('',(#15042,#15043,#15044,#15045));
#4052=EDGE_LOOP('',(#15046,#15047,#15048,#15049));
#4053=EDGE_LOOP('',(#15050,#15051,#15052,#15053));
#4054=EDGE_LOOP('',(#15054,#15055,#15056,#15057));
#4055=EDGE_LOOP('',(#15058,#15059,#15060,#15061));
#4056=EDGE_LOOP('',(#15062,#15063,#15064,#15065));
#4057=EDGE_LOOP('',(#15066,#15067,#15068,#15069));
#4058=EDGE_LOOP('',(#15070,#15071,#15072,#15073));
#4059=EDGE_LOOP('',(#15074,#15075,#15076,#15077));
#4060=EDGE_LOOP('',(#15078,#15079,#15080,#15081));
#4061=EDGE_LOOP('',(#15082,#15083,#15084,#15085));
#4062=EDGE_LOOP('',(#15086,#15087,#15088,#15089));
#4063=EDGE_LOOP('',(#15090,#15091,#15092,#15093));
#4064=EDGE_LOOP('',(#15094,#15095,#15096,#15097));
#4065=EDGE_LOOP('',(#15098,#15099,#15100,#15101));
#4066=EDGE_LOOP('',(#15102,#15103,#15104,#15105));
#4067=EDGE_LOOP('',(#15106,#15107,#15108,#15109));
#4068=EDGE_LOOP('',(#15110,#15111,#15112,#15113));
#4069=EDGE_LOOP('',(#15114,#15115,#15116,#15117));
#4070=EDGE_LOOP('',(#15118,#15119,#15120,#15121));
#4071=EDGE_LOOP('',(#15122,#15123,#15124,#15125));
#4072=EDGE_LOOP('',(#15126,#15127,#15128,#15129));
#4073=EDGE_LOOP('',(#15130,#15131,#15132,#15133));
#4074=EDGE_LOOP('',(#15134,#15135,#15136,#15137));
#4075=EDGE_LOOP('',(#15138,#15139,#15140,#15141));
#4076=EDGE_LOOP('',(#15142,#15143,#15144,#15145));
#4077=EDGE_LOOP('',(#15146,#15147,#15148,#15149));
#4078=EDGE_LOOP('',(#15150,#15151,#15152,#15153));
#4079=EDGE_LOOP('',(#15154,#15155,#15156,#15157));
#4080=EDGE_LOOP('',(#15158,#15159,#15160,#15161));
#4081=EDGE_LOOP('',(#15162,#15163,#15164,#15165));
#4082=EDGE_LOOP('',(#15166,#15167,#15168,#15169));
#4083=EDGE_LOOP('',(#15170,#15171,#15172,#15173));
#4084=EDGE_LOOP('',(#15174,#15175,#15176,#15177));
#4085=EDGE_LOOP('',(#15178,#15179,#15180,#15181));
#4086=EDGE_LOOP('',(#15182,#15183,#15184,#15185));
#4087=EDGE_LOOP('',(#15186,#15187,#15188,#15189));
#4088=EDGE_LOOP('',(#15190,#15191,#15192,#15193));
#4089=EDGE_LOOP('',(#15194,#15195,#15196,#15197));
#4090=EDGE_LOOP('',(#15198,#15199,#15200,#15201));
#4091=EDGE_LOOP('',(#15202,#15203,#15204,#15205));
#4092=EDGE_LOOP('',(#15206,#15207,#15208,#15209));
#4093=EDGE_LOOP('',(#15210,#15211,#15212,#15213));
#4094=EDGE_LOOP('',(#15214,#15215,#15216,#15217));
#4095=EDGE_LOOP('',(#15218,#15219,#15220,#15221));
#4096=EDGE_LOOP('',(#15222,#15223,#15224,#15225));
#4097=EDGE_LOOP('',(#15226,#15227,#15228,#15229));
#4098=EDGE_LOOP('',(#15230,#15231,#15232,#15233));
#4099=EDGE_LOOP('',(#15234,#15235,#15236,#15237));
#4100=EDGE_LOOP('',(#15238,#15239,#15240,#15241));
#4101=EDGE_LOOP('',(#15242,#15243,#15244,#15245));
#4102=EDGE_LOOP('',(#15246,#15247,#15248,#15249));
#4103=EDGE_LOOP('',(#15250,#15251,#15252,#15253));
#4104=EDGE_LOOP('',(#15254,#15255,#15256,#15257));
#4105=EDGE_LOOP('',(#15258,#15259,#15260,#15261));
#4106=EDGE_LOOP('',(#15262,#15263,#15264,#15265));
#4107=EDGE_LOOP('',(#15266,#15267,#15268,#15269));
#4108=EDGE_LOOP('',(#15270,#15271,#15272,#15273));
#4109=EDGE_LOOP('',(#15274,#15275,#15276,#15277));
#4110=EDGE_LOOP('',(#15278,#15279,#15280,#15281));
#4111=EDGE_LOOP('',(#15282,#15283,#15284,#15285));
#4112=EDGE_LOOP('',(#15286,#15287,#15288,#15289));
#4113=EDGE_LOOP('',(#15290,#15291,#15292,#15293));
#4114=EDGE_LOOP('',(#15294,#15295,#15296,#15297));
#4115=EDGE_LOOP('',(#15298,#15299,#15300,#15301));
#4116=EDGE_LOOP('',(#15302,#15303,#15304,#15305));
#4117=EDGE_LOOP('',(#15306,#15307,#15308,#15309));
#4118=EDGE_LOOP('',(#15310,#15311,#15312,#15313));
#4119=EDGE_LOOP('',(#15314,#15315,#15316,#15317));
#4120=EDGE_LOOP('',(#15318,#15319,#15320,#15321));
#4121=EDGE_LOOP('',(#15322,#15323,#15324,#15325));
#4122=EDGE_LOOP('',(#15326,#15327,#15328,#15329));
#4123=EDGE_LOOP('',(#15330,#15331,#15332,#15333));
#4124=EDGE_LOOP('',(#15334,#15335,#15336,#15337));
#4125=EDGE_LOOP('',(#15338,#15339,#15340,#15341));
#4126=EDGE_LOOP('',(#15342,#15343,#15344,#15345,#15346,#15347,#15348,#15349,
#15350,#15351,#15352,#15353,#15354,#15355,#15356,#15357,#15358,#15359,#15360,
#15361,#15362,#15363,#15364,#15365,#15366,#15367,#15368,#15369,#15370,#15371,
#15372,#15373,#15374,#15375,#15376,#15377,#15378,#15379,#15380,#15381,#15382,
#15383,#15384,#15385,#15386,#15387,#15388,#15389,#15390,#15391,#15392,#15393,
#15394,#15395,#15396,#15397,#15398,#15399,#15400,#15401,#15402,#15403,#15404,
#15405,#15406,#15407,#15408,#15409,#15410,#15411,#15412,#15413));
#4127=EDGE_LOOP('',(#15414,#15415,#15416,#15417));
#4128=EDGE_LOOP('',(#15418));
#4129=EDGE_LOOP('',(#15419));
#4130=EDGE_LOOP('',(#15420));
#4131=EDGE_LOOP('',(#15421));
#4132=EDGE_LOOP('',(#15422));
#4133=EDGE_LOOP('',(#15423));
#4134=EDGE_LOOP('',(#15424,#15425,#15426,#15427));
#4135=EDGE_LOOP('',(#15428,#15429,#15430,#15431));
#4136=EDGE_LOOP('',(#15432,#15433,#15434,#15435));
#4137=EDGE_LOOP('',(#15436,#15437,#15438,#15439));
#4138=EDGE_LOOP('',(#15440,#15441,#15442,#15443));
#4139=EDGE_LOOP('',(#15444,#15445,#15446,#15447));
#4140=EDGE_LOOP('',(#15448,#15449,#15450,#15451));
#4141=EDGE_LOOP('',(#15452,#15453,#15454,#15455));
#4142=EDGE_LOOP('',(#15456,#15457,#15458,#15459));
#4143=EDGE_LOOP('',(#15460,#15461,#15462,#15463));
#4144=EDGE_LOOP('',(#15464,#15465,#15466,#15467));
#4145=EDGE_LOOP('',(#15468));
#4146=EDGE_LOOP('',(#15469));
#4147=EDGE_LOOP('',(#15470));
#4148=EDGE_LOOP('',(#15471));
#4149=EDGE_LOOP('',(#15472));
#4150=EDGE_LOOP('',(#15473,#15474,#15475,#15476));
#4151=EDGE_LOOP('',(#15477));
#4152=EDGE_LOOP('',(#15478));
#4153=EDGE_LOOP('',(#15479));
#4154=EDGE_LOOP('',(#15480));
#4155=EDGE_LOOP('',(#15481));
#4156=EDGE_LOOP('',(#15482,#15483,#15484,#15485));
#4157=EDGE_LOOP('',(#15486,#15487,#15488,#15489));
#4158=EDGE_LOOP('',(#15490,#15491,#15492,#15493));
#4159=EDGE_LOOP('',(#15494,#15495,#15496,#15497));
#4160=EDGE_LOOP('',(#15498,#15499,#15500,#15501));
#4161=EDGE_LOOP('',(#15502,#15503,#15504,#15505));
#4162=EDGE_LOOP('',(#15506,#15507,#15508,#15509));
#4163=EDGE_LOOP('',(#15510,#15511,#15512,#15513));
#4164=EDGE_LOOP('',(#15514,#15515,#15516,#15517));
#4165=EDGE_LOOP('',(#15518,#15519,#15520,#15521));
#4166=EDGE_LOOP('',(#15522,#15523,#15524,#15525));
#4167=EDGE_LOOP('',(#15526,#15527,#15528,#15529));
#4168=EDGE_LOOP('',(#15530,#15531,#15532,#15533));
#4169=EDGE_LOOP('',(#15534,#15535,#15536,#15537));
#4170=EDGE_LOOP('',(#15538,#15539,#15540,#15541));
#4171=EDGE_LOOP('',(#15542,#15543,#15544,#15545));
#4172=EDGE_LOOP('',(#15546,#15547,#15548,#15549));
#4173=EDGE_LOOP('',(#15550,#15551,#15552,#15553));
#4174=EDGE_LOOP('',(#15554,#15555,#15556,#15557));
#4175=EDGE_LOOP('',(#15558,#15559,#15560,#15561));
#4176=EDGE_LOOP('',(#15562,#15563,#15564,#15565));
#4177=EDGE_LOOP('',(#15566,#15567,#15568,#15569));
#4178=EDGE_LOOP('',(#15570,#15571,#15572,#15573));
#4179=EDGE_LOOP('',(#15574,#15575,#15576,#15577));
#4180=EDGE_LOOP('',(#15578,#15579,#15580,#15581));
#4181=EDGE_LOOP('',(#15582,#15583,#15584,#15585));
#4182=EDGE_LOOP('',(#15586,#15587,#15588,#15589));
#4183=EDGE_LOOP('',(#15590,#15591,#15592,#15593));
#4184=EDGE_LOOP('',(#15594,#15595,#15596,#15597));
#4185=EDGE_LOOP('',(#15598,#15599,#15600,#15601));
#4186=EDGE_LOOP('',(#15602,#15603,#15604,#15605));
#4187=EDGE_LOOP('',(#15606,#15607,#15608,#15609));
#4188=EDGE_LOOP('',(#15610,#15611,#15612,#15613));
#4189=EDGE_LOOP('',(#15614,#15615,#15616,#15617));
#4190=EDGE_LOOP('',(#15618,#15619,#15620,#15621));
#4191=EDGE_LOOP('',(#15622,#15623,#15624,#15625));
#4192=EDGE_LOOP('',(#15626,#15627,#15628,#15629));
#4193=EDGE_LOOP('',(#15630,#15631,#15632,#15633));
#4194=EDGE_LOOP('',(#15634,#15635,#15636,#15637,#15638,#15639,#15640,#15641));
#4195=EDGE_LOOP('',(#15642,#15643,#15644,#15645,#15646,#15647,#15648,#15649,
#15650,#15651,#15652,#15653,#15654,#15655,#15656,#15657,#15658,#15659,#15660,
#15661,#15662,#15663,#15664,#15665,#15666,#15667,#15668,#15669,#15670,#15671,
#15672,#15673,#15674,#15675,#15676,#15677,#15678,#15679,#15680,#15681,#15682,
#15683));
#4196=EDGE_LOOP('',(#15684,#15685,#15686,#15687));
#4197=EDGE_LOOP('',(#15688,#15689,#15690,#15691,#15692,#15693,#15694,#15695,
#15696,#15697,#15698,#15699,#15700,#15701,#15702,#15703,#15704,#15705,#15706,
#15707,#15708,#15709,#15710,#15711,#15712,#15713,#15714,#15715,#15716,#15717,
#15718,#15719,#15720,#15721,#15722,#15723,#15724,#15725,#15726,#15727,#15728,
#15729,#15730));
#4198=EDGE_LOOP('',(#15731,#15732,#15733,#15734));
#4199=EDGE_LOOP('',(#15735,#15736,#15737,#15738));
#4200=EDGE_LOOP('',(#15739,#15740,#15741,#15742));
#4201=EDGE_LOOP('',(#15743,#15744,#15745,#15746));
#4202=EDGE_LOOP('',(#15747,#15748,#15749,#15750));
#4203=EDGE_LOOP('',(#15751,#15752,#15753,#15754));
#4204=EDGE_LOOP('',(#15755,#15756,#15757,#15758));
#4205=EDGE_LOOP('',(#15759,#15760,#15761,#15762,#15763,#15764));
#4206=EDGE_LOOP('',(#15765));
#4207=EDGE_LOOP('',(#15766,#15767,#15768,#15769));
#4208=EDGE_LOOP('',(#15770,#15771,#15772,#15773));
#4209=EDGE_LOOP('',(#15774));
#4210=EDGE_LOOP('',(#15775,#15776,#15777,#15778,#15779,#15780));
#4211=EDGE_LOOP('',(#15781));
#4212=EDGE_LOOP('',(#15782,#15783,#15784,#15785));
#4213=EDGE_LOOP('',(#15786));
#4214=EDGE_LOOP('',(#15787));
#4215=EDGE_LOOP('',(#15788,#15789,#15790,#15791,#15792,#15793,#15794,#15795));
#4216=EDGE_LOOP('',(#15796,#15797,#15798,#15799));
#4217=EDGE_LOOP('',(#15800,#15801,#15802,#15803));
#4218=EDGE_LOOP('',(#15804,#15805,#15806,#15807));
#4219=EDGE_LOOP('',(#15808,#15809,#15810,#15811));
#4220=EDGE_LOOP('',(#15812,#15813,#15814,#15815));
#4221=EDGE_LOOP('',(#15816,#15817,#15818,#15819));
#4222=EDGE_LOOP('',(#15820,#15821,#15822,#15823));
#4223=EDGE_LOOP('',(#15824,#15825,#15826,#15827));
#4224=EDGE_LOOP('',(#15828,#15829,#15830,#15831));
#4225=EDGE_LOOP('',(#15832,#15833,#15834,#15835));
#4226=EDGE_LOOP('',(#15836,#15837,#15838,#15839));
#4227=EDGE_LOOP('',(#15840,#15841,#15842,#15843));
#4228=EDGE_LOOP('',(#15844,#15845,#15846,#15847));
#4229=EDGE_LOOP('',(#15848,#15849,#15850,#15851));
#4230=EDGE_LOOP('',(#15852,#15853,#15854,#15855));
#4231=EDGE_LOOP('',(#15856,#15857,#15858,#15859,#15860,#15861,#15862,#15863));
#4232=EDGE_LOOP('',(#15864,#15865,#15866,#15867));
#4233=EDGE_LOOP('',(#15868,#15869,#15870,#15871));
#4234=EDGE_LOOP('',(#15872,#15873,#15874,#15875));
#4235=EDGE_LOOP('',(#15876,#15877,#15878,#15879));
#4236=EDGE_LOOP('',(#15880,#15881,#15882,#15883));
#4237=EDGE_LOOP('',(#15884,#15885,#15886,#15887));
#4238=EDGE_LOOP('',(#15888,#15889,#15890,#15891));
#4239=EDGE_LOOP('',(#15892,#15893,#15894,#15895));
#4240=EDGE_LOOP('',(#15896,#15897,#15898,#15899));
#4241=EDGE_LOOP('',(#15900,#15901,#15902,#15903));
#4242=EDGE_LOOP('',(#15904,#15905,#15906,#15907));
#4243=EDGE_LOOP('',(#15908,#15909,#15910,#15911));
#4244=EDGE_LOOP('',(#15912,#15913,#15914,#15915));
#4245=EDGE_LOOP('',(#15916,#15917,#15918,#15919));
#4246=EDGE_LOOP('',(#15920,#15921,#15922,#15923));
#4247=EDGE_LOOP('',(#15924,#15925,#15926,#15927,#15928,#15929,#15930,#15931));
#4248=EDGE_LOOP('',(#15932,#15933,#15934,#15935));
#4249=EDGE_LOOP('',(#15936,#15937,#15938,#15939));
#4250=EDGE_LOOP('',(#15940,#15941,#15942,#15943));
#4251=EDGE_LOOP('',(#15944,#15945,#15946,#15947));
#4252=EDGE_LOOP('',(#15948,#15949,#15950,#15951));
#4253=EDGE_LOOP('',(#15952,#15953,#15954,#15955));
#4254=EDGE_LOOP('',(#15956,#15957,#15958,#15959));
#4255=EDGE_LOOP('',(#15960,#15961,#15962,#15963));
#4256=EDGE_LOOP('',(#15964,#15965,#15966,#15967));
#4257=EDGE_LOOP('',(#15968,#15969,#15970,#15971));
#4258=EDGE_LOOP('',(#15972,#15973,#15974,#15975));
#4259=EDGE_LOOP('',(#15976,#15977,#15978,#15979));
#4260=EDGE_LOOP('',(#15980,#15981,#15982,#15983));
#4261=EDGE_LOOP('',(#15984,#15985,#15986,#15987));
#4262=EDGE_LOOP('',(#15988,#15989,#15990,#15991));
#4263=EDGE_LOOP('',(#15992,#15993,#15994,#15995,#15996));
#4264=EDGE_LOOP('',(#15997,#15998,#15999,#16000));
#4265=EDGE_LOOP('',(#16001,#16002,#16003,#16004,#16005,#16006,#16007,#16008,
#16009,#16010,#16011,#16012,#16013,#16014,#16015,#16016,#16017,#16018,#16019,
#16020));
#4266=EDGE_LOOP('',(#16021,#16022,#16023,#16024,#16025,#16026,#16027,#16028,
#16029,#16030,#16031,#16032,#16033,#16034,#16035,#16036,#16037,#16038,#16039,
#16040));
#4267=EDGE_LOOP('',(#16041,#16042,#16043,#16044));
#4268=EDGE_LOOP('',(#16045,#16046,#16047,#16048,#16049));
#4269=EDGE_LOOP('',(#16050,#16051,#16052,#16053));
#4270=EDGE_LOOP('',(#16054,#16055,#16056,#16057,#16058,#16059,#16060,#16061,
#16062,#16063,#16064,#16065,#16066,#16067,#16068,#16069,#16070,#16071,#16072,
#16073));
#4271=EDGE_LOOP('',(#16074,#16075,#16076,#16077,#16078,#16079,#16080,#16081,
#16082,#16083,#16084,#16085,#16086,#16087,#16088,#16089,#16090,#16091,#16092,
#16093));
#4272=EDGE_LOOP('',(#16094,#16095,#16096,#16097));
#4273=EDGE_LOOP('',(#16098,#16099,#16100,#16101,#16102));
#4274=EDGE_LOOP('',(#16103,#16104,#16105,#16106));
#4275=EDGE_LOOP('',(#16107,#16108,#16109,#16110,#16111,#16112,#16113,#16114,
#16115,#16116,#16117,#16118,#16119,#16120,#16121,#16122,#16123,#16124,#16125,
#16126));
#4276=EDGE_LOOP('',(#16127,#16128,#16129,#16130,#16131,#16132,#16133,#16134,
#16135,#16136,#16137,#16138,#16139,#16140,#16141,#16142,#16143,#16144,#16145,
#16146));
#4277=EDGE_LOOP('',(#16147,#16148,#16149,#16150));
#4278=EDGE_LOOP('',(#16151));
#4279=EDGE_LOOP('',(#16152));
#4280=EDGE_LOOP('',(#16153));
#4281=EDGE_LOOP('',(#16154,#16155,#16156));
#4282=EDGE_LOOP('',(#16157,#16158,#16159,#16160));
#4283=EDGE_LOOP('',(#16161));
#4284=EDGE_LOOP('',(#16162,#16163,#16164,#16165));
#4285=EDGE_LOOP('',(#16166,#16167,#16168,#16169));
#4286=EDGE_LOOP('',(#16170,#16171,#16172,#16173));
#4287=EDGE_LOOP('',(#16174));
#4288=EDGE_LOOP('',(#16175));
#4289=EDGE_LOOP('',(#16176,#16177,#16178,#16179));
#4290=EDGE_LOOP('',(#16180,#16181,#16182,#16183));
#4291=EDGE_LOOP('',(#16184,#16185,#16186,#16187));
#4292=EDGE_LOOP('',(#16188,#16189,#16190,#16191));
#4293=EDGE_LOOP('',(#16192,#16193,#16194,#16195));
#4294=EDGE_LOOP('',(#16196,#16197,#16198,#16199));
#4295=EDGE_LOOP('',(#16200));
#4296=EDGE_LOOP('',(#16201));
#4297=EDGE_LOOP('',(#16202));
#4298=EDGE_LOOP('',(#16203));
#4299=EDGE_LOOP('',(#16204));
#4300=EDGE_LOOP('',(#16205));
#4301=EDGE_LOOP('',(#16206));
#4302=EDGE_LOOP('',(#16207));
#4303=EDGE_LOOP('',(#16208));
#4304=EDGE_LOOP('',(#16209));
#4305=EDGE_LOOP('',(#16210,#16211,#16212,#16213));
#4306=EDGE_LOOP('',(#16214,#16215,#16216,#16217));
#4307=EDGE_LOOP('',(#16218,#16219,#16220,#16221));
#4308=EDGE_LOOP('',(#16222,#16223,#16224,#16225));
#4309=EDGE_LOOP('',(#16226,#16227,#16228,#16229));
#4310=EDGE_LOOP('',(#16230,#16231,#16232,#16233));
#4311=EDGE_LOOP('',(#16234,#16235,#16236,#16237));
#4312=EDGE_LOOP('',(#16238,#16239,#16240,#16241));
#4313=EDGE_LOOP('',(#16242,#16243,#16244,#16245));
#4314=EDGE_LOOP('',(#16246,#16247,#16248,#16249));
#4315=EDGE_LOOP('',(#16250,#16251,#16252,#16253));
#4316=EDGE_LOOP('',(#16254,#16255,#16256,#16257));
#4317=EDGE_LOOP('',(#16258,#16259,#16260,#16261));
#4318=EDGE_LOOP('',(#16262,#16263,#16264,#16265));
#4319=EDGE_LOOP('',(#16266,#16267,#16268,#16269));
#4320=EDGE_LOOP('',(#16270,#16271,#16272,#16273));
#4321=EDGE_LOOP('',(#16274,#16275,#16276,#16277));
#4322=EDGE_LOOP('',(#16278,#16279,#16280,#16281));
#4323=EDGE_LOOP('',(#16282,#16283,#16284,#16285));
#4324=EDGE_LOOP('',(#16286,#16287,#16288,#16289));
#4325=EDGE_LOOP('',(#16290,#16291,#16292,#16293));
#4326=EDGE_LOOP('',(#16294,#16295,#16296,#16297));
#4327=EDGE_LOOP('',(#16298,#16299,#16300,#16301));
#4328=EDGE_LOOP('',(#16302,#16303,#16304,#16305));
#4329=EDGE_LOOP('',(#16306,#16307,#16308,#16309));
#4330=EDGE_LOOP('',(#16310,#16311,#16312,#16313));
#4331=EDGE_LOOP('',(#16314,#16315,#16316,#16317));
#4332=EDGE_LOOP('',(#16318,#16319,#16320,#16321));
#4333=EDGE_LOOP('',(#16322,#16323,#16324,#16325));
#4334=EDGE_LOOP('',(#16326,#16327,#16328,#16329));
#4335=EDGE_LOOP('',(#16330,#16331,#16332,#16333));
#4336=EDGE_LOOP('',(#16334,#16335,#16336,#16337));
#4337=EDGE_LOOP('',(#16338,#16339,#16340,#16341));
#4338=EDGE_LOOP('',(#16342,#16343,#16344,#16345));
#4339=EDGE_LOOP('',(#16346,#16347,#16348,#16349));
#4340=EDGE_LOOP('',(#16350,#16351,#16352,#16353));
#4341=EDGE_LOOP('',(#16354,#16355,#16356,#16357));
#4342=EDGE_LOOP('',(#16358,#16359,#16360,#16361));
#4343=EDGE_LOOP('',(#16362,#16363,#16364,#16365));
#4344=EDGE_LOOP('',(#16366,#16367,#16368,#16369));
#4345=EDGE_LOOP('',(#16370,#16371,#16372,#16373));
#4346=EDGE_LOOP('',(#16374,#16375,#16376,#16377));
#4347=EDGE_LOOP('',(#16378,#16379,#16380,#16381));
#4348=EDGE_LOOP('',(#16382,#16383,#16384,#16385));
#4349=EDGE_LOOP('',(#16386,#16387,#16388,#16389));
#4350=EDGE_LOOP('',(#16390,#16391,#16392,#16393));
#4351=EDGE_LOOP('',(#16394,#16395,#16396,#16397));
#4352=EDGE_LOOP('',(#16398,#16399,#16400,#16401));
#4353=EDGE_LOOP('',(#16402,#16403,#16404,#16405));
#4354=EDGE_LOOP('',(#16406,#16407,#16408,#16409));
#4355=EDGE_LOOP('',(#16410,#16411,#16412,#16413));
#4356=EDGE_LOOP('',(#16414,#16415,#16416,#16417));
#4357=EDGE_LOOP('',(#16418,#16419,#16420,#16421));
#4358=EDGE_LOOP('',(#16422,#16423,#16424,#16425));
#4359=EDGE_LOOP('',(#16426,#16427,#16428,#16429));
#4360=EDGE_LOOP('',(#16430,#16431,#16432,#16433));
#4361=EDGE_LOOP('',(#16434,#16435,#16436,#16437));
#4362=EDGE_LOOP('',(#16438,#16439,#16440,#16441));
#4363=EDGE_LOOP('',(#16442,#16443,#16444,#16445));
#4364=EDGE_LOOP('',(#16446,#16447,#16448,#16449));
#4365=EDGE_LOOP('',(#16450,#16451,#16452,#16453));
#4366=EDGE_LOOP('',(#16454,#16455,#16456,#16457));
#4367=EDGE_LOOP('',(#16458,#16459,#16460,#16461));
#4368=EDGE_LOOP('',(#16462,#16463,#16464,#16465));
#4369=EDGE_LOOP('',(#16466,#16467,#16468,#16469));
#4370=EDGE_LOOP('',(#16470,#16471,#16472,#16473));
#4371=EDGE_LOOP('',(#16474,#16475,#16476,#16477));
#4372=EDGE_LOOP('',(#16478,#16479,#16480,#16481));
#4373=EDGE_LOOP('',(#16482,#16483,#16484,#16485));
#4374=EDGE_LOOP('',(#16486,#16487,#16488,#16489));
#4375=EDGE_LOOP('',(#16490,#16491,#16492,#16493));
#4376=EDGE_LOOP('',(#16494,#16495,#16496,#16497));
#4377=EDGE_LOOP('',(#16498,#16499,#16500,#16501));
#4378=EDGE_LOOP('',(#16502,#16503,#16504,#16505));
#4379=EDGE_LOOP('',(#16506,#16507,#16508,#16509));
#4380=EDGE_LOOP('',(#16510,#16511,#16512,#16513));
#4381=EDGE_LOOP('',(#16514,#16515,#16516,#16517));
#4382=EDGE_LOOP('',(#16518,#16519,#16520,#16521));
#4383=EDGE_LOOP('',(#16522,#16523,#16524,#16525));
#4384=EDGE_LOOP('',(#16526,#16527,#16528,#16529));
#4385=EDGE_LOOP('',(#16530,#16531,#16532,#16533));
#4386=EDGE_LOOP('',(#16534,#16535,#16536,#16537));
#4387=EDGE_LOOP('',(#16538,#16539,#16540,#16541));
#4388=EDGE_LOOP('',(#16542,#16543,#16544,#16545));
#4389=EDGE_LOOP('',(#16546,#16547,#16548,#16549));
#4390=EDGE_LOOP('',(#16550,#16551,#16552,#16553));
#4391=EDGE_LOOP('',(#16554,#16555,#16556,#16557));
#4392=EDGE_LOOP('',(#16558,#16559,#16560,#16561));
#4393=EDGE_LOOP('',(#16562,#16563,#16564,#16565));
#4394=EDGE_LOOP('',(#16566,#16567,#16568,#16569));
#4395=EDGE_LOOP('',(#16570,#16571,#16572,#16573));
#4396=EDGE_LOOP('',(#16574,#16575,#16576,#16577));
#4397=EDGE_LOOP('',(#16578,#16579,#16580,#16581));
#4398=EDGE_LOOP('',(#16582,#16583,#16584,#16585));
#4399=EDGE_LOOP('',(#16586,#16587,#16588,#16589));
#4400=EDGE_LOOP('',(#16590,#16591,#16592,#16593));
#4401=EDGE_LOOP('',(#16594,#16595,#16596,#16597));
#4402=EDGE_LOOP('',(#16598,#16599,#16600,#16601));
#4403=EDGE_LOOP('',(#16602,#16603,#16604,#16605));
#4404=EDGE_LOOP('',(#16606,#16607,#16608,#16609));
#4405=EDGE_LOOP('',(#16610,#16611,#16612,#16613));
#4406=EDGE_LOOP('',(#16614,#16615,#16616,#16617));
#4407=EDGE_LOOP('',(#16618,#16619,#16620,#16621));
#4408=EDGE_LOOP('',(#16622,#16623,#16624,#16625));
#4409=EDGE_LOOP('',(#16626,#16627,#16628,#16629));
#4410=EDGE_LOOP('',(#16630,#16631,#16632,#16633));
#4411=EDGE_LOOP('',(#16634,#16635,#16636,#16637));
#4412=EDGE_LOOP('',(#16638,#16639,#16640,#16641));
#4413=EDGE_LOOP('',(#16642,#16643,#16644,#16645));
#4414=EDGE_LOOP('',(#16646,#16647,#16648,#16649));
#4415=EDGE_LOOP('',(#16650,#16651,#16652,#16653));
#4416=EDGE_LOOP('',(#16654,#16655,#16656,#16657));
#4417=EDGE_LOOP('',(#16658,#16659,#16660,#16661));
#4418=EDGE_LOOP('',(#16662,#16663,#16664,#16665));
#4419=EDGE_LOOP('',(#16666,#16667,#16668,#16669));
#4420=EDGE_LOOP('',(#16670,#16671,#16672,#16673));
#4421=EDGE_LOOP('',(#16674,#16675,#16676,#16677));
#4422=EDGE_LOOP('',(#16678,#16679,#16680,#16681));
#4423=EDGE_LOOP('',(#16682,#16683,#16684,#16685));
#4424=EDGE_LOOP('',(#16686,#16687,#16688,#16689));
#4425=EDGE_LOOP('',(#16690,#16691,#16692,#16693,#16694,#16695,#16696,#16697,
#16698,#16699,#16700,#16701,#16702,#16703,#16704,#16705,#16706,#16707,#16708,
#16709,#16710,#16711,#16712,#16713,#16714,#16715,#16716,#16717,#16718,#16719,
#16720,#16721,#16722,#16723,#16724,#16725,#16726,#16727,#16728,#16729,#16730,
#16731,#16732,#16733,#16734,#16735,#16736,#16737,#16738,#16739,#16740,#16741,
#16742,#16743,#16744,#16745,#16746,#16747,#16748,#16749,#16750,#16751,#16752,
#16753,#16754,#16755,#16756,#16757,#16758,#16759,#16760,#16761,#16762,#16763,
#16764,#16765,#16766,#16767,#16768,#16769,#16770,#16771,#16772,#16773,#16774,
#16775,#16776,#16777,#16778,#16779,#16780,#16781,#16782,#16783,#16784,#16785,
#16786,#16787,#16788,#16789,#16790,#16791,#16792,#16793,#16794,#16795,#16796,
#16797,#16798,#16799,#16800,#16801,#16802,#16803,#16804,#16805,#16806,#16807,
#16808,#16809,#16810,#16811,#16812,#16813));
#4426=EDGE_LOOP('',(#16814,#16815,#16816,#16817));
#4427=EDGE_LOOP('',(#16818,#16819,#16820,#16821,#16822,#16823,#16824,#16825,
#16826,#16827,#16828,#16829,#16830,#16831,#16832,#16833,#16834,#16835,#16836,
#16837,#16838,#16839,#16840,#16841,#16842,#16843,#16844,#16845,#16846,#16847,
#16848,#16849,#16850,#16851,#16852,#16853,#16854,#16855,#16856,#16857,#16858,
#16859,#16860,#16861,#16862,#16863,#16864,#16865,#16866,#16867,#16868,#16869,
#16870,#16871,#16872,#16873,#16874,#16875,#16876,#16877,#16878,#16879,#16880,
#16881,#16882,#16883,#16884,#16885,#16886,#16887,#16888,#16889,#16890,#16891,
#16892,#16893,#16894,#16895,#16896,#16897,#16898,#16899,#16900,#16901,#16902,
#16903,#16904,#16905,#16906,#16907,#16908,#16909,#16910,#16911,#16912,#16913,
#16914,#16915,#16916,#16917,#16918,#16919,#16920,#16921,#16922,#16923,#16924,
#16925,#16926,#16927,#16928,#16929,#16930,#16931,#16932,#16933,#16934,#16935,
#16936,#16937,#16938,#16939,#16940,#16941));
#4428=EDGE_LOOP('',(#16942,#16943,#16944,#16945));
#4429=EDGE_LOOP('',(#16946,#16947,#16948,#16949,#16950,#16951));
#4430=EDGE_LOOP('',(#16952,#16953,#16954,#16955));
#4431=EDGE_LOOP('',(#16956,#16957,#16958,#16959,#16960,#16961));
#4432=EDGE_LOOP('',(#16962));
#4433=EDGE_LOOP('',(#16963,#16964,#16965,#16966));
#4434=EDGE_LOOP('',(#16967,#16968,#16969,#16970));
#4435=EDGE_LOOP('',(#16971,#16972,#16973,#16974));
#4436=EDGE_LOOP('',(#16975,#16976,#16977,#16978));
#4437=EDGE_LOOP('',(#16979,#16980,#16981,#16982));
#4438=EDGE_LOOP('',(#16983,#16984,#16985,#16986));
#4439=EDGE_LOOP('',(#16987,#16988,#16989,#16990));
#4440=EDGE_LOOP('',(#16991,#16992,#16993,#16994));
#4441=EDGE_LOOP('',(#16995,#16996,#16997));
#4442=EDGE_LOOP('',(#16998,#16999,#17000,#17001));
#4443=EDGE_LOOP('',(#17002,#17003,#17004,#17005));
#4444=EDGE_LOOP('',(#17006,#17007,#17008,#17009));
#4445=EDGE_LOOP('',(#17010,#17011,#17012,#17013));
#4446=EDGE_LOOP('',(#17014,#17015,#17016,#17017));
#4447=EDGE_LOOP('',(#17018,#17019,#17020,#17021));
#4448=EDGE_LOOP('',(#17022,#17023,#17024,#17025));
#4449=EDGE_LOOP('',(#17026,#17027,#17028,#17029));
#4450=EDGE_LOOP('',(#17030,#17031,#17032,#17033));
#4451=EDGE_LOOP('',(#17034,#17035,#17036,#17037));
#4452=EDGE_LOOP('',(#17038,#17039,#17040,#17041));
#4453=EDGE_LOOP('',(#17042,#17043,#17044,#17045));
#4454=EDGE_LOOP('',(#17046,#17047,#17048,#17049));
#4455=EDGE_LOOP('',(#17050,#17051,#17052,#17053));
#4456=EDGE_LOOP('',(#17054,#17055,#17056,#17057));
#4457=EDGE_LOOP('',(#17058,#17059,#17060,#17061));
#4458=EDGE_LOOP('',(#17062,#17063,#17064,#17065));
#4459=EDGE_LOOP('',(#17066,#17067,#17068,#17069,#17070,#17071,#17072,#17073,
#17074,#17075,#17076,#17077,#17078,#17079,#17080,#17081,#17082,#17083,#17084,
#17085));
#4460=EDGE_LOOP('',(#17086,#17087,#17088,#17089,#17090,#17091,#17092,#17093,
#17094,#17095,#17096,#17097,#17098,#17099,#17100,#17101,#17102,#17103,#17104,
#17105));
#4461=EDGE_LOOP('',(#17106,#17107,#17108,#17109,#17110,#17111));
#4462=EDGE_LOOP('',(#17112,#17113,#17114,#17115));
#4463=EDGE_LOOP('',(#17116,#17117,#17118,#17119));
#4464=EDGE_LOOP('',(#17120,#17121,#17122,#17123));
#4465=EDGE_LOOP('',(#17124,#17125,#17126,#17127));
#4466=EDGE_LOOP('',(#17128,#17129,#17130,#17131));
#4467=EDGE_LOOP('',(#17132,#17133,#17134,#17135));
#4468=EDGE_LOOP('',(#17136,#17137,#17138,#17139));
#4469=EDGE_LOOP('',(#17140,#17141,#17142,#17143));
#4470=EDGE_LOOP('',(#17144,#17145,#17146,#17147,#17148,#17149));
#4471=EDGE_LOOP('',(#17150,#17151,#17152,#17153));
#4472=EDGE_LOOP('',(#17154,#17155,#17156,#17157));
#4473=EDGE_LOOP('',(#17158,#17159,#17160,#17161));
#4474=EDGE_LOOP('',(#17162));
#4475=EDGE_LOOP('',(#17163));
#4476=EDGE_LOOP('',(#17164));
#4477=EDGE_LOOP('',(#17165));
#4478=EDGE_LOOP('',(#17166,#17167,#17168,#17169));
#4479=EDGE_LOOP('',(#17170,#17171,#17172,#17173));
#4480=EDGE_LOOP('',(#17174,#17175,#17176,#17177));
#4481=EDGE_LOOP('',(#17178,#17179,#17180,#17181));
#4482=EDGE_LOOP('',(#17182,#17183,#17184,#17185));
#4483=EDGE_LOOP('',(#17186,#17187,#17188,#17189));
#4484=EDGE_LOOP('',(#17190,#17191,#17192,#17193));
#4485=EDGE_LOOP('',(#17194,#17195,#17196,#17197));
#4486=EDGE_LOOP('',(#17198,#17199,#17200,#17201));
#4487=EDGE_LOOP('',(#17202,#17203,#17204,#17205));
#4488=EDGE_LOOP('',(#17206,#17207,#17208,#17209));
#4489=EDGE_LOOP('',(#17210,#17211,#17212,#17213));
#4490=EDGE_LOOP('',(#17214,#17215,#17216,#17217));
#4491=EDGE_LOOP('',(#17218,#17219,#17220,#17221));
#4492=EDGE_LOOP('',(#17222,#17223,#17224,#17225));
#4493=EDGE_LOOP('',(#17226,#17227,#17228,#17229));
#4494=EDGE_LOOP('',(#17230,#17231,#17232,#17233));
#4495=EDGE_LOOP('',(#17234,#17235,#17236,#17237));
#4496=EDGE_LOOP('',(#17238,#17239,#17240,#17241));
#4497=EDGE_LOOP('',(#17242,#17243,#17244,#17245));
#4498=EDGE_LOOP('',(#17246,#17247,#17248,#17249));
#4499=EDGE_LOOP('',(#17250,#17251,#17252,#17253));
#4500=EDGE_LOOP('',(#17254,#17255,#17256,#17257));
#4501=EDGE_LOOP('',(#17258,#17259,#17260,#17261));
#4502=EDGE_LOOP('',(#17262,#17263,#17264,#17265));
#4503=EDGE_LOOP('',(#17266,#17267,#17268,#17269));
#4504=EDGE_LOOP('',(#17270,#17271,#17272,#17273));
#4505=EDGE_LOOP('',(#17274,#17275,#17276,#17277));
#4506=EDGE_LOOP('',(#17278,#17279,#17280,#17281));
#4507=EDGE_LOOP('',(#17282,#17283,#17284,#17285));
#4508=EDGE_LOOP('',(#17286,#17287,#17288,#17289,#17290,#17291,#17292,#17293));
#4509=EDGE_LOOP('',(#17294,#17295,#17296,#17297,#17298,#17299,#17300,#17301,
#17302,#17303,#17304,#17305,#17306,#17307,#17308,#17309,#17310,#17311,#17312,
#17313,#17314,#17315,#17316,#17317,#17318,#17319,#17320,#17321,#17322,#17323,
#17324,#17325,#17326,#17327));
#4510=EDGE_LOOP('',(#17328,#17329,#17330,#17331));
#4511=EDGE_LOOP('',(#17332,#17333,#17334,#17335,#17336,#17337,#17338,#17339,
#17340,#17341,#17342,#17343,#17344,#17345,#17346,#17347,#17348,#17349,#17350,
#17351,#17352,#17353,#17354,#17355,#17356,#17357,#17358,#17359,#17360,#17361,
#17362,#17363,#17364,#17365,#17366));
#4512=EDGE_LOOP('',(#17367,#17368,#17369,#17370));
#4513=EDGE_LOOP('',(#17371,#17372,#17373,#17374));
#4514=EDGE_LOOP('',(#17375,#17376,#17377,#17378));
#4515=EDGE_LOOP('',(#17379,#17380,#17381,#17382));
#4516=EDGE_LOOP('',(#17383,#17384,#17385,#17386));
#4517=EDGE_LOOP('',(#17387,#17388,#17389,#17390));
#4518=EDGE_LOOP('',(#17391,#17392,#17393,#17394));
#4519=EDGE_LOOP('',(#17395,#17396,#17397,#17398,#17399,#17400));
#4520=EDGE_LOOP('',(#17401));
#4521=EDGE_LOOP('',(#17402,#17403,#17404,#17405));
#4522=EDGE_LOOP('',(#17406,#17407,#17408,#17409));
#4523=EDGE_LOOP('',(#17410));
#4524=EDGE_LOOP('',(#17411,#17412,#17413,#17414,#17415,#17416));
#4525=EDGE_LOOP('',(#17417));
#4526=EDGE_LOOP('',(#17418,#17419,#17420,#17421));
#4527=EDGE_LOOP('',(#17422,#17423,#17424,#17425));
#4528=EDGE_LOOP('',(#17426,#17427,#17428,#17429));
#4529=EDGE_LOOP('',(#17430,#17431,#17432,#17433));
#4530=EDGE_LOOP('',(#17434,#17435,#17436,#17437));
#4531=EDGE_LOOP('',(#17438,#17439,#17440,#17441));
#4532=EDGE_LOOP('',(#17442,#17443,#17444,#17445));
#4533=EDGE_LOOP('',(#17446,#17447,#17448,#17449));
#4534=EDGE_LOOP('',(#17450,#17451,#17452,#17453));
#4535=EDGE_LOOP('',(#17454,#17455,#17456,#17457));
#4536=EDGE_LOOP('',(#17458,#17459,#17460,#17461));
#4537=EDGE_LOOP('',(#17462,#17463,#17464,#17465));
#4538=EDGE_LOOP('',(#17466,#17467,#17468,#17469));
#4539=EDGE_LOOP('',(#17470,#17471,#17472,#17473));
#4540=EDGE_LOOP('',(#17474,#17475,#17476,#17477));
#4541=EDGE_LOOP('',(#17478,#17479,#17480,#17481));
#4542=EDGE_LOOP('',(#17482,#17483,#17484,#17485));
#4543=EDGE_LOOP('',(#17486,#17487,#17488,#17489));
#4544=EDGE_LOOP('',(#17490,#17491,#17492,#17493));
#4545=EDGE_LOOP('',(#17494,#17495,#17496,#17497));
#4546=EDGE_LOOP('',(#17498,#17499,#17500,#17501));
#4547=EDGE_LOOP('',(#17502,#17503,#17504,#17505));
#4548=EDGE_LOOP('',(#17506,#17507,#17508,#17509));
#4549=EDGE_LOOP('',(#17510,#17511,#17512,#17513));
#4550=EDGE_LOOP('',(#17514,#17515,#17516,#17517));
#4551=EDGE_LOOP('',(#17518,#17519,#17520,#17521));
#4552=EDGE_LOOP('',(#17522,#17523,#17524,#17525));
#4553=EDGE_LOOP('',(#17526,#17527,#17528,#17529));
#4554=EDGE_LOOP('',(#17530,#17531,#17532,#17533));
#4555=EDGE_LOOP('',(#17534,#17535,#17536,#17537));
#4556=EDGE_LOOP('',(#17538,#17539,#17540,#17541));
#4557=EDGE_LOOP('',(#17542,#17543,#17544,#17545));
#4558=EDGE_LOOP('',(#17546,#17547,#17548,#17549));
#4559=EDGE_LOOP('',(#17550,#17551,#17552,#17553));
#4560=EDGE_LOOP('',(#17554,#17555,#17556,#17557));
#4561=EDGE_LOOP('',(#17558,#17559,#17560,#17561));
#4562=EDGE_LOOP('',(#17562,#17563,#17564,#17565));
#4563=EDGE_LOOP('',(#17566,#17567,#17568,#17569));
#4564=EDGE_LOOP('',(#17570,#17571,#17572,#17573));
#4565=EDGE_LOOP('',(#17574,#17575,#17576,#17577));
#4566=EDGE_LOOP('',(#17578,#17579,#17580,#17581));
#4567=EDGE_LOOP('',(#17582,#17583,#17584,#17585));
#4568=EDGE_LOOP('',(#17586,#17587,#17588,#17589));
#4569=EDGE_LOOP('',(#17590,#17591,#17592,#17593));
#4570=EDGE_LOOP('',(#17594,#17595,#17596,#17597));
#4571=EDGE_LOOP('',(#17598,#17599,#17600,#17601));
#4572=EDGE_LOOP('',(#17602,#17603,#17604,#17605));
#4573=EDGE_LOOP('',(#17606,#17607,#17608,#17609));
#4574=EDGE_LOOP('',(#17610,#17611,#17612,#17613));
#4575=EDGE_LOOP('',(#17614,#17615,#17616,#17617));
#4576=EDGE_LOOP('',(#17618,#17619,#17620,#17621));
#4577=EDGE_LOOP('',(#17622,#17623,#17624,#17625));
#4578=EDGE_LOOP('',(#17626,#17627,#17628,#17629));
#4579=EDGE_LOOP('',(#17630,#17631,#17632,#17633));
#4580=EDGE_LOOP('',(#17634,#17635,#17636,#17637));
#4581=EDGE_LOOP('',(#17638,#17639,#17640,#17641));
#4582=EDGE_LOOP('',(#17642,#17643,#17644,#17645));
#4583=EDGE_LOOP('',(#17646,#17647,#17648,#17649));
#4584=EDGE_LOOP('',(#17650,#17651,#17652,#17653));
#4585=EDGE_LOOP('',(#17654,#17655,#17656,#17657));
#4586=EDGE_LOOP('',(#17658,#17659,#17660,#17661));
#4587=EDGE_LOOP('',(#17662,#17663,#17664,#17665));
#4588=EDGE_LOOP('',(#17666,#17667,#17668,#17669));
#4589=EDGE_LOOP('',(#17670,#17671,#17672,#17673));
#4590=EDGE_LOOP('',(#17674,#17675,#17676,#17677));
#4591=EDGE_LOOP('',(#17678,#17679,#17680,#17681));
#4592=EDGE_LOOP('',(#17682,#17683,#17684,#17685));
#4593=EDGE_LOOP('',(#17686,#17687,#17688,#17689));
#4594=EDGE_LOOP('',(#17690,#17691,#17692,#17693));
#4595=EDGE_LOOP('',(#17694,#17695,#17696,#17697));
#4596=EDGE_LOOP('',(#17698,#17699,#17700,#17701));
#4597=EDGE_LOOP('',(#17702,#17703,#17704,#17705));
#4598=EDGE_LOOP('',(#17706,#17707,#17708,#17709));
#4599=EDGE_LOOP('',(#17710,#17711,#17712,#17713));
#4600=EDGE_LOOP('',(#17714,#17715,#17716,#17717));
#4601=EDGE_LOOP('',(#17718,#17719,#17720,#17721));
#4602=EDGE_LOOP('',(#17722,#17723,#17724,#17725));
#4603=EDGE_LOOP('',(#17726,#17727,#17728,#17729));
#4604=EDGE_LOOP('',(#17730,#17731,#17732,#17733));
#4605=EDGE_LOOP('',(#17734,#17735,#17736,#17737));
#4606=EDGE_LOOP('',(#17738,#17739,#17740,#17741));
#4607=EDGE_LOOP('',(#17742,#17743,#17744,#17745));
#4608=EDGE_LOOP('',(#17746,#17747,#17748,#17749));
#4609=EDGE_LOOP('',(#17750,#17751,#17752,#17753));
#4610=EDGE_LOOP('',(#17754,#17755,#17756,#17757));
#4611=EDGE_LOOP('',(#17758,#17759,#17760,#17761));
#4612=EDGE_LOOP('',(#17762,#17763,#17764,#17765));
#4613=EDGE_LOOP('',(#17766,#17767,#17768,#17769));
#4614=EDGE_LOOP('',(#17770,#17771,#17772,#17773));
#4615=EDGE_LOOP('',(#17774,#17775,#17776,#17777));
#4616=EDGE_LOOP('',(#17778,#17779,#17780,#17781));
#4617=EDGE_LOOP('',(#17782,#17783,#17784,#17785));
#4618=EDGE_LOOP('',(#17786,#17787,#17788,#17789));
#4619=EDGE_LOOP('',(#17790,#17791,#17792,#17793));
#4620=EDGE_LOOP('',(#17794,#17795,#17796,#17797));
#4621=EDGE_LOOP('',(#17798,#17799,#17800,#17801));
#4622=EDGE_LOOP('',(#17802,#17803,#17804,#17805));
#4623=EDGE_LOOP('',(#17806,#17807,#17808,#17809));
#4624=EDGE_LOOP('',(#17810,#17811,#17812,#17813));
#4625=EDGE_LOOP('',(#17814,#17815,#17816,#17817));
#4626=EDGE_LOOP('',(#17818,#17819,#17820,#17821));
#4627=EDGE_LOOP('',(#17822,#17823,#17824,#17825));
#4628=EDGE_LOOP('',(#17826,#17827,#17828,#17829));
#4629=EDGE_LOOP('',(#17830,#17831,#17832,#17833));
#4630=EDGE_LOOP('',(#17834,#17835,#17836,#17837));
#4631=EDGE_LOOP('',(#17838,#17839,#17840,#17841));
#4632=EDGE_LOOP('',(#17842,#17843,#17844,#17845));
#4633=EDGE_LOOP('',(#17846,#17847,#17848,#17849));
#4634=EDGE_LOOP('',(#17850,#17851,#17852,#17853));
#4635=EDGE_LOOP('',(#17854,#17855,#17856,#17857));
#4636=EDGE_LOOP('',(#17858,#17859,#17860,#17861));
#4637=EDGE_LOOP('',(#17862,#17863,#17864,#17865));
#4638=EDGE_LOOP('',(#17866,#17867,#17868,#17869));
#4639=EDGE_LOOP('',(#17870,#17871,#17872,#17873));
#4640=EDGE_LOOP('',(#17874,#17875,#17876,#17877));
#4641=EDGE_LOOP('',(#17878,#17879,#17880,#17881));
#4642=EDGE_LOOP('',(#17882,#17883,#17884,#17885));
#4643=EDGE_LOOP('',(#17886,#17887,#17888,#17889));
#4644=EDGE_LOOP('',(#17890,#17891,#17892,#17893));
#4645=EDGE_LOOP('',(#17894,#17895,#17896,#17897));
#4646=EDGE_LOOP('',(#17898,#17899,#17900,#17901));
#4647=EDGE_LOOP('',(#17902,#17903,#17904,#17905));
#4648=EDGE_LOOP('',(#17906,#17907,#17908,#17909));
#4649=EDGE_LOOP('',(#17910,#17911,#17912,#17913));
#4650=EDGE_LOOP('',(#17914,#17915,#17916,#17917));
#4651=EDGE_LOOP('',(#17918,#17919,#17920,#17921));
#4652=EDGE_LOOP('',(#17922,#17923,#17924,#17925));
#4653=EDGE_LOOP('',(#17926,#17927,#17928,#17929));
#4654=EDGE_LOOP('',(#17930,#17931,#17932,#17933));
#4655=EDGE_LOOP('',(#17934,#17935,#17936,#17937));
#4656=EDGE_LOOP('',(#17938,#17939,#17940,#17941));
#4657=EDGE_LOOP('',(#17942,#17943,#17944,#17945));
#4658=EDGE_LOOP('',(#17946,#17947,#17948,#17949));
#4659=EDGE_LOOP('',(#17950,#17951,#17952,#17953));
#4660=EDGE_LOOP('',(#17954,#17955,#17956,#17957));
#4661=EDGE_LOOP('',(#17958,#17959,#17960,#17961));
#4662=EDGE_LOOP('',(#17962,#17963,#17964,#17965));
#4663=EDGE_LOOP('',(#17966,#17967,#17968,#17969));
#4664=EDGE_LOOP('',(#17970,#17971,#17972,#17973));
#4665=EDGE_LOOP('',(#17974,#17975,#17976,#17977));
#4666=EDGE_LOOP('',(#17978,#17979,#17980,#17981));
#4667=EDGE_LOOP('',(#17982,#17983,#17984,#17985));
#4668=EDGE_LOOP('',(#17986,#17987,#17988,#17989));
#4669=EDGE_LOOP('',(#17990,#17991,#17992,#17993));
#4670=EDGE_LOOP('',(#17994,#17995,#17996,#17997));
#4671=EDGE_LOOP('',(#17998,#17999,#18000,#18001));
#4672=EDGE_LOOP('',(#18002,#18003,#18004,#18005));
#4673=EDGE_LOOP('',(#18006,#18007,#18008,#18009));
#4674=EDGE_LOOP('',(#18010,#18011,#18012,#18013));
#4675=EDGE_LOOP('',(#18014,#18015,#18016,#18017));
#4676=EDGE_LOOP('',(#18018,#18019,#18020,#18021));
#4677=EDGE_LOOP('',(#18022,#18023,#18024,#18025));
#4678=EDGE_LOOP('',(#18026,#18027,#18028,#18029));
#4679=EDGE_LOOP('',(#18030,#18031,#18032,#18033));
#4680=EDGE_LOOP('',(#18034,#18035,#18036,#18037));
#4681=EDGE_LOOP('',(#18038,#18039,#18040,#18041));
#4682=EDGE_LOOP('',(#18042,#18043,#18044,#18045));
#4683=EDGE_LOOP('',(#18046,#18047,#18048,#18049));
#4684=EDGE_LOOP('',(#18050,#18051,#18052,#18053));
#4685=EDGE_LOOP('',(#18054,#18055,#18056,#18057));
#4686=EDGE_LOOP('',(#18058,#18059,#18060,#18061));
#4687=EDGE_LOOP('',(#18062,#18063,#18064,#18065));
#4688=EDGE_LOOP('',(#18066,#18067,#18068,#18069));
#4689=EDGE_LOOP('',(#18070,#18071,#18072,#18073));
#4690=EDGE_LOOP('',(#18074,#18075,#18076,#18077));
#4691=EDGE_LOOP('',(#18078,#18079,#18080,#18081));
#4692=EDGE_LOOP('',(#18082,#18083,#18084,#18085));
#4693=EDGE_LOOP('',(#18086,#18087,#18088,#18089));
#4694=EDGE_LOOP('',(#18090,#18091,#18092,#18093));
#4695=EDGE_LOOP('',(#18094,#18095,#18096,#18097));
#4696=EDGE_LOOP('',(#18098,#18099,#18100,#18101));
#4697=EDGE_LOOP('',(#18102,#18103,#18104,#18105));
#4698=EDGE_LOOP('',(#18106,#18107,#18108,#18109));
#4699=EDGE_LOOP('',(#18110,#18111,#18112,#18113));
#4700=EDGE_LOOP('',(#18114,#18115,#18116,#18117));
#4701=EDGE_LOOP('',(#18118,#18119,#18120,#18121));
#4702=EDGE_LOOP('',(#18122,#18123,#18124,#18125));
#4703=EDGE_LOOP('',(#18126,#18127,#18128,#18129));
#4704=EDGE_LOOP('',(#18130,#18131,#18132,#18133));
#4705=EDGE_LOOP('',(#18134,#18135,#18136,#18137));
#4706=EDGE_LOOP('',(#18138,#18139,#18140,#18141));
#4707=EDGE_LOOP('',(#18142,#18143,#18144,#18145));
#4708=EDGE_LOOP('',(#18146,#18147,#18148,#18149));
#4709=EDGE_LOOP('',(#18150,#18151,#18152,#18153));
#4710=EDGE_LOOP('',(#18154,#18155,#18156,#18157));
#4711=EDGE_LOOP('',(#18158,#18159,#18160,#18161));
#4712=EDGE_LOOP('',(#18162,#18163,#18164,#18165));
#4713=EDGE_LOOP('',(#18166,#18167,#18168,#18169));
#4714=EDGE_LOOP('',(#18170,#18171,#18172,#18173));
#4715=EDGE_LOOP('',(#18174,#18175,#18176,#18177));
#4716=EDGE_LOOP('',(#18178,#18179,#18180,#18181));
#4717=EDGE_LOOP('',(#18182,#18183,#18184,#18185));
#4718=EDGE_LOOP('',(#18186,#18187,#18188,#18189));
#4719=EDGE_LOOP('',(#18190,#18191,#18192,#18193));
#4720=EDGE_LOOP('',(#18194,#18195,#18196,#18197));
#4721=EDGE_LOOP('',(#18198,#18199,#18200,#18201));
#4722=EDGE_LOOP('',(#18202,#18203,#18204,#18205));
#4723=EDGE_LOOP('',(#18206,#18207,#18208,#18209));
#4724=EDGE_LOOP('',(#18210,#18211,#18212,#18213));
#4725=EDGE_LOOP('',(#18214,#18215,#18216,#18217));
#4726=EDGE_LOOP('',(#18218,#18219,#18220,#18221));
#4727=EDGE_LOOP('',(#18222,#18223,#18224,#18225));
#4728=EDGE_LOOP('',(#18226,#18227,#18228,#18229));
#4729=EDGE_LOOP('',(#18230,#18231,#18232,#18233));
#4730=EDGE_LOOP('',(#18234,#18235,#18236,#18237));
#4731=EDGE_LOOP('',(#18238,#18239,#18240,#18241));
#4732=EDGE_LOOP('',(#18242,#18243,#18244,#18245));
#4733=EDGE_LOOP('',(#18246,#18247,#18248,#18249));
#4734=EDGE_LOOP('',(#18250,#18251,#18252,#18253));
#4735=EDGE_LOOP('',(#18254,#18255,#18256,#18257));
#4736=EDGE_LOOP('',(#18258,#18259,#18260,#18261));
#4737=EDGE_LOOP('',(#18262,#18263,#18264,#18265));
#4738=EDGE_LOOP('',(#18266,#18267,#18268,#18269));
#4739=EDGE_LOOP('',(#18270,#18271,#18272,#18273));
#4740=EDGE_LOOP('',(#18274,#18275,#18276,#18277));
#4741=EDGE_LOOP('',(#18278,#18279,#18280,#18281));
#4742=EDGE_LOOP('',(#18282,#18283,#18284,#18285));
#4743=EDGE_LOOP('',(#18286,#18287,#18288,#18289));
#4744=EDGE_LOOP('',(#18290,#18291,#18292,#18293));
#4745=EDGE_LOOP('',(#18294,#18295,#18296,#18297));
#4746=EDGE_LOOP('',(#18298,#18299,#18300,#18301));
#4747=EDGE_LOOP('',(#18302,#18303,#18304,#18305));
#4748=EDGE_LOOP('',(#18306,#18307,#18308,#18309));
#4749=EDGE_LOOP('',(#18310,#18311,#18312,#18313));
#4750=EDGE_LOOP('',(#18314,#18315,#18316,#18317));
#4751=EDGE_LOOP('',(#18318,#18319,#18320,#18321));
#4752=EDGE_LOOP('',(#18322,#18323,#18324,#18325));
#4753=EDGE_LOOP('',(#18326,#18327,#18328,#18329));
#4754=EDGE_LOOP('',(#18330,#18331,#18332,#18333));
#4755=EDGE_LOOP('',(#18334,#18335,#18336,#18337));
#4756=EDGE_LOOP('',(#18338,#18339,#18340,#18341));
#4757=EDGE_LOOP('',(#18342,#18343,#18344,#18345));
#4758=EDGE_LOOP('',(#18346,#18347,#18348,#18349));
#4759=EDGE_LOOP('',(#18350,#18351,#18352,#18353));
#4760=EDGE_LOOP('',(#18354,#18355,#18356,#18357));
#4761=EDGE_LOOP('',(#18358,#18359,#18360,#18361));
#4762=EDGE_LOOP('',(#18362,#18363,#18364,#18365));
#4763=EDGE_LOOP('',(#18366,#18367,#18368,#18369));
#4764=EDGE_LOOP('',(#18370,#18371,#18372,#18373));
#4765=EDGE_LOOP('',(#18374,#18375,#18376,#18377));
#4766=EDGE_LOOP('',(#18378,#18379,#18380,#18381));
#4767=EDGE_LOOP('',(#18382,#18383,#18384,#18385,#18386,#18387,#18388,#18389,
#18390,#18391,#18392,#18393,#18394,#18395,#18396,#18397,#18398,#18399,#18400,
#18401,#18402,#18403,#18404,#18405,#18406,#18407,#18408,#18409,#18410,#18411,
#18412,#18413,#18414,#18415,#18416,#18417,#18418,#18419,#18420,#18421,#18422,
#18423,#18424,#18425));
#4768=EDGE_LOOP('',(#18426,#18427,#18428,#18429,#18430,#18431,#18432,#18433,
#18434,#18435,#18436,#18437,#18438,#18439,#18440,#18441,#18442,#18443,#18444,
#18445,#18446,#18447,#18448,#18449,#18450,#18451,#18452,#18453,#18454,#18455,
#18456,#18457,#18458,#18459,#18460,#18461,#18462,#18463,#18464,#18465,#18466,
#18467,#18468,#18469));
#4769=EDGE_LOOP('',(#18470,#18471,#18472,#18473));
#4770=EDGE_LOOP('',(#18474,#18475,#18476,#18477));
#4771=EDGE_LOOP('',(#18478,#18479,#18480,#18481));
#4772=EDGE_LOOP('',(#18482,#18483,#18484,#18485));
#4773=EDGE_LOOP('',(#18486,#18487,#18488,#18489));
#4774=EDGE_LOOP('',(#18490,#18491,#18492,#18493));
#4775=EDGE_LOOP('',(#18494,#18495,#18496,#18497));
#4776=EDGE_LOOP('',(#18498,#18499,#18500,#18501));
#4777=EDGE_LOOP('',(#18502,#18503,#18504,#18505,#18506,#18507,#18508,#18509,
#18510,#18511,#18512,#18513,#18514,#18515,#18516,#18517,#18518,#18519,#18520,
#18521,#18522,#18523,#18524,#18525,#18526,#18527,#18528,#18529,#18530,#18531,
#18532,#18533,#18534,#18535,#18536,#18537,#18538,#18539,#18540,#18541,#18542,
#18543,#18544,#18545));
#4778=EDGE_LOOP('',(#18546,#18547,#18548,#18549,#18550,#18551,#18552,#18553,
#18554,#18555,#18556,#18557,#18558,#18559,#18560,#18561,#18562,#18563,#18564,
#18565,#18566,#18567,#18568,#18569,#18570,#18571,#18572,#18573,#18574,#18575,
#18576,#18577,#18578,#18579,#18580,#18581,#18582,#18583,#18584,#18585,#18586,
#18587,#18588,#18589));
#4779=EDGE_LOOP('',(#18590,#18591,#18592,#18593));
#4780=EDGE_LOOP('',(#18594,#18595,#18596,#18597,#18598,#18599,#18600,#18601,
#18602,#18603,#18604,#18605,#18606,#18607,#18608,#18609,#18610,#18611,#18612,
#18613,#18614,#18615,#18616,#18617,#18618,#18619,#18620,#18621,#18622,#18623,
#18624,#18625,#18626,#18627,#18628,#18629,#18630,#18631,#18632,#18633,#18634,
#18635,#18636,#18637));
#4781=EDGE_LOOP('',(#18638,#18639,#18640,#18641,#18642,#18643,#18644,#18645,
#18646,#18647,#18648,#18649,#18650,#18651,#18652,#18653,#18654,#18655,#18656,
#18657,#18658,#18659,#18660,#18661,#18662,#18663,#18664,#18665,#18666,#18667,
#18668,#18669,#18670,#18671,#18672,#18673,#18674,#18675,#18676,#18677,#18678,
#18679,#18680,#18681));
#4782=EDGE_LOOP('',(#18682,#18683,#18684,#18685));
#4783=EDGE_LOOP('',(#18686,#18687,#18688,#18689,#18690,#18691,#18692,#18693,
#18694,#18695,#18696,#18697,#18698,#18699,#18700,#18701,#18702,#18703,#18704,
#18705,#18706,#18707,#18708,#18709,#18710,#18711,#18712,#18713,#18714,#18715,
#18716,#18717,#18718,#18719,#18720,#18721,#18722,#18723,#18724,#18725,#18726,
#18727,#18728,#18729));
#4784=EDGE_LOOP('',(#18730,#18731,#18732,#18733,#18734,#18735,#18736,#18737,
#18738,#18739,#18740,#18741,#18742,#18743,#18744,#18745,#18746,#18747,#18748,
#18749,#18750,#18751,#18752,#18753,#18754,#18755,#18756,#18757,#18758,#18759,
#18760,#18761,#18762,#18763,#18764,#18765,#18766,#18767,#18768,#18769,#18770,
#18771,#18772,#18773));
#4785=EDGE_LOOP('',(#18774,#18775,#18776,#18777));
#4786=EDGE_LOOP('',(#18778,#18779,#18780,#18781,#18782,#18783,#18784,#18785,
#18786,#18787,#18788,#18789,#18790,#18791,#18792,#18793,#18794,#18795,#18796,
#18797,#18798,#18799,#18800,#18801,#18802,#18803,#18804,#18805,#18806,#18807,
#18808,#18809,#18810,#18811,#18812,#18813,#18814,#18815,#18816,#18817,#18818,
#18819,#18820,#18821));
#4787=EDGE_LOOP('',(#18822,#18823,#18824,#18825,#18826,#18827,#18828,#18829,
#18830,#18831,#18832,#18833,#18834,#18835,#18836,#18837,#18838,#18839,#18840,
#18841,#18842,#18843,#18844,#18845,#18846,#18847,#18848,#18849,#18850,#18851,
#18852,#18853,#18854,#18855,#18856,#18857,#18858,#18859,#18860,#18861,#18862,
#18863,#18864,#18865));
#4788=EDGE_LOOP('',(#18866,#18867,#18868,#18869));
#4789=EDGE_LOOP('',(#18870,#18871,#18872,#18873,#18874,#18875,#18876,#18877,
#18878,#18879,#18880,#18881,#18882,#18883,#18884,#18885,#18886,#18887,#18888,
#18889,#18890,#18891,#18892,#18893,#18894,#18895,#18896,#18897,#18898,#18899,
#18900,#18901,#18902,#18903,#18904,#18905,#18906,#18907,#18908,#18909,#18910,
#18911,#18912,#18913));
#4790=EDGE_LOOP('',(#18914,#18915,#18916,#18917,#18918,#18919,#18920,#18921,
#18922,#18923,#18924,#18925,#18926,#18927,#18928,#18929,#18930,#18931,#18932,
#18933,#18934,#18935,#18936,#18937,#18938,#18939,#18940,#18941,#18942,#18943,
#18944,#18945,#18946,#18947,#18948,#18949,#18950,#18951,#18952,#18953,#18954,
#18955,#18956,#18957));
#4791=EDGE_LOOP('',(#18958,#18959,#18960,#18961));
#4792=EDGE_LOOP('',(#18962,#18963,#18964,#18965));
#4793=EDGE_LOOP('',(#18966,#18967,#18968,#18969));
#4794=EDGE_LOOP('',(#18970,#18971,#18972,#18973));
#4795=EDGE_LOOP('',(#18974,#18975,#18976,#18977));
#4796=EDGE_LOOP('',(#18978,#18979,#18980,#18981));
#4797=EDGE_LOOP('',(#18982,#18983,#18984,#18985));
#4798=EDGE_LOOP('',(#18986,#18987,#18988,#18989));
#4799=EDGE_LOOP('',(#18990,#18991,#18992,#18993));
#4800=EDGE_LOOP('',(#18994,#18995,#18996,#18997));
#4801=EDGE_LOOP('',(#18998,#18999,#19000,#19001));
#4802=EDGE_LOOP('',(#19002,#19003,#19004,#19005));
#4803=EDGE_LOOP('',(#19006,#19007,#19008,#19009));
#4804=EDGE_LOOP('',(#19010,#19011,#19012,#19013));
#4805=EDGE_LOOP('',(#19014,#19015,#19016,#19017));
#4806=EDGE_LOOP('',(#19018,#19019,#19020,#19021));
#4807=EDGE_LOOP('',(#19022,#19023,#19024,#19025));
#4808=EDGE_LOOP('',(#19026,#19027,#19028,#19029));
#4809=EDGE_LOOP('',(#19030,#19031,#19032,#19033));
#4810=EDGE_LOOP('',(#19034,#19035,#19036,#19037));
#4811=EDGE_LOOP('',(#19038,#19039,#19040,#19041));
#4812=EDGE_LOOP('',(#19042,#19043,#19044,#19045));
#4813=EDGE_LOOP('',(#19046,#19047,#19048,#19049));
#4814=EDGE_LOOP('',(#19050,#19051,#19052,#19053));
#4815=EDGE_LOOP('',(#19054,#19055,#19056,#19057));
#4816=EDGE_LOOP('',(#19058,#19059,#19060,#19061));
#4817=EDGE_LOOP('',(#19062,#19063,#19064,#19065));
#4818=EDGE_LOOP('',(#19066,#19067,#19068,#19069));
#4819=EDGE_LOOP('',(#19070,#19071,#19072,#19073));
#4820=EDGE_LOOP('',(#19074,#19075,#19076,#19077));
#4821=EDGE_LOOP('',(#19078,#19079,#19080,#19081));
#4822=EDGE_LOOP('',(#19082,#19083,#19084,#19085));
#4823=EDGE_LOOP('',(#19086,#19087,#19088,#19089));
#4824=EDGE_LOOP('',(#19090,#19091,#19092,#19093));
#4825=EDGE_LOOP('',(#19094,#19095,#19096,#19097));
#4826=EDGE_LOOP('',(#19098,#19099,#19100,#19101));
#4827=EDGE_LOOP('',(#19102,#19103,#19104,#19105));
#4828=EDGE_LOOP('',(#19106,#19107,#19108,#19109));
#4829=EDGE_LOOP('',(#19110,#19111,#19112,#19113));
#4830=EDGE_LOOP('',(#19114,#19115,#19116,#19117));
#4831=EDGE_LOOP('',(#19118,#19119,#19120,#19121));
#4832=EDGE_LOOP('',(#19122,#19123,#19124,#19125));
#4833=EDGE_LOOP('',(#19126,#19127,#19128,#19129));
#4834=EDGE_LOOP('',(#19130,#19131,#19132,#19133));
#4835=EDGE_LOOP('',(#19134,#19135,#19136,#19137));
#4836=EDGE_LOOP('',(#19138,#19139,#19140,#19141));
#4837=EDGE_LOOP('',(#19142,#19143,#19144,#19145));
#4838=EDGE_LOOP('',(#19146,#19147,#19148,#19149));
#4839=EDGE_LOOP('',(#19150,#19151,#19152,#19153));
#4840=EDGE_LOOP('',(#19154,#19155,#19156,#19157));
#4841=EDGE_LOOP('',(#19158,#19159,#19160,#19161));
#4842=EDGE_LOOP('',(#19162,#19163,#19164,#19165));
#4843=EDGE_LOOP('',(#19166,#19167,#19168,#19169));
#4844=EDGE_LOOP('',(#19170,#19171,#19172,#19173));
#4845=EDGE_LOOP('',(#19174,#19175,#19176,#19177));
#4846=EDGE_LOOP('',(#19178,#19179,#19180,#19181));
#4847=EDGE_LOOP('',(#19182,#19183,#19184,#19185));
#4848=EDGE_LOOP('',(#19186,#19187,#19188,#19189));
#4849=EDGE_LOOP('',(#19190,#19191,#19192,#19193));
#4850=EDGE_LOOP('',(#19194,#19195,#19196,#19197));
#4851=EDGE_LOOP('',(#19198,#19199,#19200,#19201));
#4852=EDGE_LOOP('',(#19202,#19203,#19204,#19205));
#4853=EDGE_LOOP('',(#19206,#19207,#19208,#19209));
#4854=EDGE_LOOP('',(#19210,#19211,#19212,#19213));
#4855=EDGE_LOOP('',(#19214,#19215,#19216,#19217));
#4856=EDGE_LOOP('',(#19218,#19219,#19220,#19221));
#4857=EDGE_LOOP('',(#19222,#19223,#19224,#19225));
#4858=EDGE_LOOP('',(#19226,#19227,#19228,#19229));
#4859=EDGE_LOOP('',(#19230,#19231,#19232,#19233));
#4860=EDGE_LOOP('',(#19234,#19235,#19236,#19237));
#4861=EDGE_LOOP('',(#19238,#19239,#19240,#19241));
#4862=EDGE_LOOP('',(#19242,#19243,#19244,#19245));
#4863=EDGE_LOOP('',(#19246,#19247,#19248,#19249));
#4864=EDGE_LOOP('',(#19250,#19251,#19252,#19253));
#4865=EDGE_LOOP('',(#19254,#19255,#19256,#19257));
#4866=EDGE_LOOP('',(#19258,#19259,#19260,#19261));
#4867=EDGE_LOOP('',(#19262,#19263,#19264,#19265));
#4868=EDGE_LOOP('',(#19266,#19267,#19268,#19269));
#4869=EDGE_LOOP('',(#19270,#19271,#19272,#19273));
#4870=EDGE_LOOP('',(#19274,#19275,#19276,#19277));
#4871=EDGE_LOOP('',(#19278,#19279,#19280,#19281));
#4872=EDGE_LOOP('',(#19282,#19283,#19284,#19285));
#4873=EDGE_LOOP('',(#19286,#19287,#19288,#19289));
#4874=EDGE_LOOP('',(#19290,#19291,#19292,#19293));
#4875=EDGE_LOOP('',(#19294,#19295,#19296,#19297));
#4876=EDGE_LOOP('',(#19298,#19299,#19300,#19301));
#4877=EDGE_LOOP('',(#19302,#19303,#19304,#19305));
#4878=EDGE_LOOP('',(#19306,#19307,#19308,#19309));
#4879=EDGE_LOOP('',(#19310,#19311,#19312,#19313));
#4880=EDGE_LOOP('',(#19314,#19315,#19316,#19317));
#4881=EDGE_LOOP('',(#19318,#19319,#19320,#19321));
#4882=EDGE_LOOP('',(#19322,#19323,#19324,#19325));
#4883=EDGE_LOOP('',(#19326,#19327,#19328,#19329));
#4884=EDGE_LOOP('',(#19330,#19331,#19332,#19333));
#4885=EDGE_LOOP('',(#19334,#19335,#19336,#19337));
#4886=EDGE_LOOP('',(#19338,#19339,#19340,#19341));
#4887=EDGE_LOOP('',(#19342,#19343,#19344,#19345));
#4888=EDGE_LOOP('',(#19346,#19347,#19348,#19349));
#4889=EDGE_LOOP('',(#19350,#19351,#19352,#19353));
#4890=EDGE_LOOP('',(#19354,#19355,#19356,#19357));
#4891=EDGE_LOOP('',(#19358,#19359,#19360,#19361));
#4892=EDGE_LOOP('',(#19362,#19363,#19364,#19365));
#4893=EDGE_LOOP('',(#19366,#19367,#19368,#19369));
#4894=EDGE_LOOP('',(#19370,#19371,#19372,#19373));
#4895=EDGE_LOOP('',(#19374,#19375,#19376,#19377));
#4896=EDGE_LOOP('',(#19378,#19379,#19380,#19381));
#4897=EDGE_LOOP('',(#19382,#19383,#19384,#19385));
#4898=EDGE_LOOP('',(#19386,#19387,#19388,#19389));
#4899=EDGE_LOOP('',(#19390,#19391,#19392,#19393));
#4900=EDGE_LOOP('',(#19394,#19395,#19396,#19397));
#4901=EDGE_LOOP('',(#19398,#19399,#19400,#19401));
#4902=EDGE_LOOP('',(#19402,#19403,#19404,#19405));
#4903=EDGE_LOOP('',(#19406,#19407,#19408,#19409));
#4904=EDGE_LOOP('',(#19410,#19411,#19412,#19413));
#4905=EDGE_LOOP('',(#19414,#19415,#19416,#19417));
#4906=EDGE_LOOP('',(#19418,#19419,#19420,#19421,#19422,#19423,#19424,#19425));
#4907=EDGE_LOOP('',(#19426,#19427,#19428,#19429,#19430,#19431,#19432,#19433,
#19434,#19435,#19436,#19437,#19438,#19439,#19440,#19441,#19442,#19443,#19444,
#19445,#19446,#19447,#19448,#19449,#19450,#19451,#19452,#19453,#19454,#19455,
#19456,#19457,#19458,#19459,#19460,#19461,#19462,#19463,#19464,#19465,#19466,
#19467,#19468,#19469,#19470,#19471,#19472,#19473,#19474,#19475,#19476,#19477,
#19478,#19479,#19480,#19481,#19482,#19483,#19484,#19485,#19486,#19487,#19488,
#19489,#19490,#19491,#19492,#19493,#19494,#19495,#19496,#19497,#19498,#19499,
#19500,#19501,#19502,#19503,#19504,#19505,#19506,#19507,#19508,#19509,#19510,
#19511,#19512,#19513,#19514,#19515,#19516,#19517,#19518,#19519,#19520,#19521,
#19522,#19523,#19524,#19525,#19526,#19527));
#4908=EDGE_LOOP('',(#19528,#19529,#19530,#19531));
#4909=EDGE_LOOP('',(#19532,#19533,#19534,#19535,#19536,#19537,#19538,#19539,
#19540,#19541,#19542,#19543,#19544,#19545,#19546,#19547,#19548,#19549,#19550,
#19551,#19552,#19553,#19554,#19555,#19556,#19557,#19558,#19559,#19560,#19561,
#19562,#19563,#19564,#19565,#19566,#19567,#19568,#19569,#19570,#19571,#19572,
#19573,#19574,#19575,#19576,#19577,#19578,#19579,#19580,#19581,#19582,#19583,
#19584,#19585,#19586,#19587,#19588,#19589,#19590,#19591,#19592,#19593,#19594,
#19595,#19596,#19597,#19598,#19599,#19600,#19601,#19602,#19603,#19604,#19605,
#19606,#19607,#19608,#19609,#19610,#19611,#19612,#19613,#19614,#19615,#19616,
#19617,#19618,#19619,#19620,#19621,#19622,#19623,#19624,#19625,#19626,#19627,
#19628,#19629,#19630,#19631,#19632,#19633,#19634));
#4910=EDGE_LOOP('',(#19635,#19636,#19637,#19638));
#4911=EDGE_LOOP('',(#19639,#19640,#19641,#19642));
#4912=EDGE_LOOP('',(#19643,#19644,#19645,#19646));
#4913=EDGE_LOOP('',(#19647,#19648,#19649,#19650));
#4914=EDGE_LOOP('',(#19651,#19652,#19653,#19654));
#4915=EDGE_LOOP('',(#19655,#19656,#19657,#19658));
#4916=EDGE_LOOP('',(#19659,#19660,#19661,#19662));
#4917=EDGE_LOOP('',(#19663,#19664,#19665,#19666,#19667,#19668));
#4918=EDGE_LOOP('',(#19669));
#4919=EDGE_LOOP('',(#19670,#19671,#19672,#19673));
#4920=EDGE_LOOP('',(#19674,#19675,#19676,#19677));
#4921=EDGE_LOOP('',(#19678));
#4922=EDGE_LOOP('',(#19679,#19680,#19681,#19682,#19683,#19684));
#4923=EDGE_LOOP('',(#19685));
#4924=EDGE_LOOP('',(#19686,#19687,#19688,#19689));
#4925=EDGE_LOOP('',(#19690,#19691,#19692,#19693));
#4926=EDGE_LOOP('',(#19694));
#4927=EDGE_LOOP('',(#19695));
#4928=EDGE_LOOP('',(#19696));
#4929=EDGE_LOOP('',(#19697));
#4930=EDGE_LOOP('',(#19698,#19699,#19700,#19701));
#4931=EDGE_LOOP('',(#19702,#19703,#19704,#19705));
#4932=EDGE_LOOP('',(#19706));
#4933=EDGE_LOOP('',(#19707));
#4934=EDGE_LOOP('',(#19708));
#4935=EDGE_LOOP('',(#19709));
#4936=LINE('',#27647,#6150);
#4937=LINE('',#27653,#6151);
#4938=LINE('',#27659,#6152);
#4939=LINE('',#27665,#6153);
#4940=LINE('',#27671,#6154);
#4941=LINE('',#27677,#6155);
#4942=LINE('',#27682,#6156);
#4943=LINE('',#27684,#6157);
#4944=LINE('',#27686,#6158);
#4945=LINE('',#27687,#6159);
#4946=LINE('',#27690,#6160);
#4947=LINE('',#27692,#6161);
#4948=LINE('',#27693,#6162);
#4949=LINE('',#27696,#6163);
#4950=LINE('',#27698,#6164);
#4951=LINE('',#27699,#6165);
#4952=LINE('',#27701,#6166);
#4953=LINE('',#27702,#6167);
#4954=LINE('',#27706,#6168);
#4955=LINE('',#27708,#6169);
#4956=LINE('',#27710,#6170);
#4957=LINE('',#27711,#6171);
#4958=LINE('',#27714,#6172);
#4959=LINE('',#27716,#6173);
#4960=LINE('',#27717,#6174);
#4961=LINE('',#27720,#6175);
#4962=LINE('',#27722,#6176);
#4963=LINE('',#27723,#6177);
#4964=LINE('',#27725,#6178);
#4965=LINE('',#27726,#6179);
#4966=LINE('',#27733,#6180);
#4967=LINE('',#27735,#6181);
#4968=LINE('',#27737,#6182);
#4969=LINE('',#27738,#6183);
#4970=LINE('',#27741,#6184);
#4971=LINE('',#27743,#6185);
#4972=LINE('',#27744,#6186);
#4973=LINE('',#27747,#6187);
#4974=LINE('',#27749,#6188);
#4975=LINE('',#27750,#6189);
#4976=LINE('',#27752,#6190);
#4977=LINE('',#27753,#6191);
#4978=LINE('',#27757,#6192);
#4979=LINE('',#27759,#6193);
#4980=LINE('',#27761,#6194);
#4981=LINE('',#27762,#6195);
#4982=LINE('',#27765,#6196);
#4983=LINE('',#27767,#6197);
#4984=LINE('',#27768,#6198);
#4985=LINE('',#27771,#6199);
#4986=LINE('',#27773,#6200);
#4987=LINE('',#27774,#6201);
#4988=LINE('',#27776,#6202);
#4989=LINE('',#27777,#6203);
#4990=LINE('',#27784,#6204);
#4991=LINE('',#27805,#6205);
#4992=LINE('',#27856,#6206);
#4993=LINE('',#27907,#6207);
#4994=LINE('',#27955,#6208);
#4995=LINE('',#28006,#6209);
#4996=LINE('',#28057,#6210);
#4997=LINE('',#28105,#6211);
#4998=LINE('',#28144,#6212);
#4999=LINE('',#28165,#6213);
#5000=LINE('',#28216,#6214);
#5001=LINE('',#28267,#6215);
#5002=LINE('',#28315,#6216);
#5003=LINE('',#28366,#6217);
#5004=LINE('',#28417,#6218);
#5005=LINE('',#28465,#6219);
#5006=LINE('',#28504,#6220);
#5007=LINE('',#28525,#6221);
#5008=LINE('',#28576,#6222);
#5009=LINE('',#28627,#6223);
#5010=LINE('',#28675,#6224);
#5011=LINE('',#28726,#6225);
#5012=LINE('',#28777,#6226);
#5013=LINE('',#28825,#6227);
#5014=LINE('',#28864,#6228);
#5015=LINE('',#28885,#6229);
#5016=LINE('',#28936,#6230);
#5017=LINE('',#28987,#6231);
#5018=LINE('',#29035,#6232);
#5019=LINE('',#29086,#6233);
#5020=LINE('',#29137,#6234);
#5021=LINE('',#29185,#6235);
#5022=LINE('',#29224,#6236);
#5023=LINE('',#29248,#6237);
#5024=LINE('',#29272,#6238);
#5025=LINE('',#29297,#6239);
#5026=LINE('',#29322,#6240);
#5027=LINE('',#29346,#6241);
#5028=LINE('',#29371,#6242);
#5029=LINE('',#29396,#6243);
#5030=LINE('',#29413,#6244);
#5031=LINE('',#29437,#6245);
#5032=LINE('',#29461,#6246);
#5033=LINE('',#29486,#6247);
#5034=LINE('',#29511,#6248);
#5035=LINE('',#29535,#6249);
#5036=LINE('',#29560,#6250);
#5037=LINE('',#29585,#6251);
#5038=LINE('',#29602,#6252);
#5039=LINE('',#29626,#6253);
#5040=LINE('',#29650,#6254);
#5041=LINE('',#29675,#6255);
#5042=LINE('',#29700,#6256);
#5043=LINE('',#29724,#6257);
#5044=LINE('',#29749,#6258);
#5045=LINE('',#29774,#6259);
#5046=LINE('',#29791,#6260);
#5047=LINE('',#29815,#6261);
#5048=LINE('',#29839,#6262);
#5049=LINE('',#29864,#6263);
#5050=LINE('',#29889,#6264);
#5051=LINE('',#29913,#6265);
#5052=LINE('',#29938,#6266);
#5053=LINE('',#29963,#6267);
#5054=LINE('',#30882,#6268);
#5055=LINE('',#30884,#6269);
#5056=LINE('',#30886,#6270);
#5057=LINE('',#30887,#6271);
#5058=LINE('',#33601,#6272);
#5059=LINE('',#33602,#6273);
#5060=LINE('',#33603,#6274);
#5061=LINE('',#33606,#6275);
#5062=LINE('',#33607,#6276);
#5063=LINE('',#33610,#6277);
#5064=LINE('',#33611,#6278);
#5065=LINE('',#33613,#6279);
#5066=LINE('',#33619,#6280);
#5067=LINE('',#33643,#6281);
#5068=LINE('',#33691,#6282);
#5069=LINE('',#33739,#6283);
#5070=LINE('',#33787,#6284);
#5071=LINE('',#33841,#6285);
#5072=LINE('',#33889,#6286);
#5073=LINE('',#33937,#6287);
#5074=LINE('',#33991,#6288);
#5075=LINE('',#34039,#6289);
#5076=LINE('',#34087,#6290);
#5077=LINE('',#34141,#6291);
#5078=LINE('',#34189,#6292);
#5079=LINE('',#34237,#6293);
#5080=LINE('',#34285,#6294);
#5081=LINE('',#34339,#6295);
#5082=LINE('',#34387,#6296);
#5083=LINE('',#34435,#6297);
#5084=LINE('',#34489,#6298);
#5085=LINE('',#34537,#6299);
#5086=LINE('',#34585,#6300);
#5087=LINE('',#34633,#6301);
#5088=LINE('',#34687,#6302);
#5089=LINE('',#34735,#6303);
#5090=LINE('',#34783,#6304);
#5091=LINE('',#34808,#6305);
#5092=LINE('',#34833,#6306);
#5093=LINE('',#34857,#6307);
#5094=LINE('',#34882,#6308);
#5095=LINE('',#34907,#6309);
#5096=LINE('',#34931,#6310);
#5097=LINE('',#34955,#6311);
#5098=LINE('',#34980,#6312);
#5099=LINE('',#35005,#6313);
#5100=LINE('',#35029,#6314);
#5101=LINE('',#35054,#6315);
#5102=LINE('',#35079,#6316);
#5103=LINE('',#35103,#6317);
#5104=LINE('',#35127,#6318);
#5105=LINE('',#35152,#6319);
#5106=LINE('',#35177,#6320);
#5107=LINE('',#35201,#6321);
#5108=LINE('',#35226,#6322);
#5109=LINE('',#35251,#6323);
#5110=LINE('',#35275,#6324);
#5111=LINE('',#35300,#6325);
#5112=LINE('',#35325,#6326);
#5113=LINE('',#35349,#6327);
#5114=LINE('',#35706,#6328);
#5115=LINE('',#37240,#6329);
#5116=LINE('',#37242,#6330);
#5117=LINE('',#37244,#6331);
#5118=LINE('',#37245,#6332);
#5119=LINE('',#37248,#6333);
#5120=LINE('',#37250,#6334);
#5121=LINE('',#37251,#6335);
#5122=LINE('',#37254,#6336);
#5123=LINE('',#37256,#6337);
#5124=LINE('',#37257,#6338);
#5125=LINE('',#37260,#6339);
#5126=LINE('',#37262,#6340);
#5127=LINE('',#37263,#6341);
#5128=LINE('',#37266,#6342);
#5129=LINE('',#37268,#6343);
#5130=LINE('',#37269,#6344);
#5131=LINE('',#37271,#6345);
#5132=LINE('',#37272,#6346);
#5133=LINE('',#37279,#6347);
#5134=LINE('',#37288,#6348);
#5135=LINE('',#37294,#6349);
#5136=LINE('',#37343,#6350);
#5137=LINE('',#37355,#6351);
#5138=LINE('',#37378,#6352);
#5139=LINE('',#37468,#6353);
#5140=LINE('',#37555,#6354);
#5141=LINE('',#37642,#6355);
#5142=LINE('',#37729,#6356);
#5143=LINE('',#37819,#6357);
#5144=LINE('',#37906,#6358);
#5145=LINE('',#37993,#6359);
#5146=LINE('',#38083,#6360);
#5147=LINE('',#38170,#6361);
#5148=LINE('',#38257,#6362);
#5149=LINE('',#38344,#6363);
#5150=LINE('',#38434,#6364);
#5151=LINE('',#38521,#6365);
#5152=LINE('',#38608,#6366);
#5153=LINE('',#38695,#6367);
#5154=LINE('',#38785,#6368);
#5155=LINE('',#38872,#6369);
#5156=LINE('',#38959,#6370);
#5157=LINE('',#39049,#6371);
#5158=LINE('',#39136,#6372);
#5159=LINE('',#39223,#6373);
#5160=LINE('',#39310,#6374);
#5161=LINE('',#39400,#6375);
#5162=LINE('',#39469,#6376);
#5163=LINE('',#39502,#6377);
#5164=LINE('',#39539,#6378);
#5165=LINE('',#39577,#6379);
#5166=LINE('',#39613,#6380);
#5167=LINE('',#39651,#6381);
#5168=LINE('',#39689,#6382);
#5169=LINE('',#39725,#6383);
#5170=LINE('',#39763,#6384);
#5171=LINE('',#39801,#6385);
#5172=LINE('',#39837,#6386);
#5173=LINE('',#39875,#6387);
#5174=LINE('',#39912,#6388);
#5175=LINE('',#39949,#6389);
#5176=LINE('',#39987,#6390);
#5177=LINE('',#40023,#6391);
#5178=LINE('',#40061,#6392);
#5179=LINE('',#40099,#6393);
#5180=LINE('',#40135,#6394);
#5181=LINE('',#40173,#6395);
#5182=LINE('',#40211,#6396);
#5183=LINE('',#40247,#6397);
#5184=LINE('',#40285,#6398);
#5185=LINE('',#40322,#6399);
#5186=LINE('',#40359,#6400);
#5187=LINE('',#40379,#6401);
#5188=LINE('',#40391,#6402);
#5189=LINE('',#40414,#6403);
#5190=LINE('',#40504,#6404);
#5191=LINE('',#40591,#6405);
#5192=LINE('',#40678,#6406);
#5193=LINE('',#40765,#6407);
#5194=LINE('',#40852,#6408);
#5195=LINE('',#40942,#6409);
#5196=LINE('',#41029,#6410);
#5197=LINE('',#41116,#6411);
#5198=LINE('',#41203,#6412);
#5199=LINE('',#41290,#6413);
#5200=LINE('',#41380,#6414);
#5201=LINE('',#41467,#6415);
#5202=LINE('',#41554,#6416);
#5203=LINE('',#41641,#6417);
#5204=LINE('',#41728,#6418);
#5205=LINE('',#41815,#6419);
#5206=LINE('',#41902,#6420);
#5207=LINE('',#41989,#6421);
#5208=LINE('',#42064,#6422);
#5209=LINE('',#42112,#6423);
#5210=LINE('',#42169,#6424);
#5211=LINE('',#42256,#6425);
#5212=LINE('',#42343,#6426);
#5213=LINE('',#42430,#6427);
#5214=LINE('',#42517,#6428);
#5215=LINE('',#42604,#6429);
#5216=LINE('',#42694,#6430);
#5217=LINE('',#42781,#6431);
#5218=LINE('',#42868,#6432);
#5219=LINE('',#42955,#6433);
#5220=LINE('',#43042,#6434);
#5221=LINE('',#43132,#6435);
#5222=LINE('',#43219,#6436);
#5223=LINE('',#43306,#6437);
#5224=LINE('',#43393,#6438);
#5225=LINE('',#43480,#6439);
#5226=LINE('',#43570,#6440);
#5227=LINE('',#43657,#6441);
#5228=LINE('',#43726,#6442);
#5229=LINE('',#43759,#6443);
#5230=LINE('',#43796,#6444);
#5231=LINE('',#43834,#6445);
#5232=LINE('',#43870,#6446);
#5233=LINE('',#43908,#6447);
#5234=LINE('',#43945,#6448);
#5235=LINE('',#43982,#6449);
#5236=LINE('',#44020,#6450);
#5237=LINE('',#44056,#6451);
#5238=LINE('',#44094,#6452);
#5239=LINE('',#44131,#6453);
#5240=LINE('',#44168,#6454);
#5241=LINE('',#44206,#6455);
#5242=LINE('',#44242,#6456);
#5243=LINE('',#44280,#6457);
#5244=LINE('',#44317,#6458);
#5245=LINE('',#44354,#6459);
#5246=LINE('',#44392,#6460);
#5247=LINE('',#44428,#6461);
#5248=LINE('',#44455,#6462);
#5249=LINE('',#44479,#6463);
#5250=LINE('',#44512,#6464);
#5251=LINE('',#44550,#6465);
#5252=LINE('',#44586,#6466);
#5253=LINE('',#44624,#6467);
#5254=LINE('',#44660,#6468);
#5255=LINE('',#44698,#6469);
#5256=LINE('',#44736,#6470);
#5257=LINE('',#44772,#6471);
#5258=LINE('',#44810,#6472);
#5259=LINE('',#44846,#6473);
#5260=LINE('',#44884,#6474);
#5261=LINE('',#44922,#6475);
#5262=LINE('',#44958,#6476);
#5263=LINE('',#44996,#6477);
#5264=LINE('',#45032,#6478);
#5265=LINE('',#45070,#6479);
#5266=LINE('',#45108,#6480);
#5267=LINE('',#45144,#6481);
#5268=LINE('',#52811,#6482);
#5269=LINE('',#52814,#6483);
#5270=LINE('',#52817,#6484);
#5271=LINE('',#52819,#6485);
#5272=LINE('',#52820,#6486);
#5273=LINE('',#52823,#6487);
#5274=LINE('',#52827,#6488);
#5275=LINE('',#52831,#6489);
#5276=LINE('',#52835,#6490);
#5277=LINE('',#52839,#6491);
#5278=LINE('',#52843,#6492);
#5279=LINE('',#52847,#6493);
#5280=LINE('',#52851,#6494);
#5281=LINE('',#52855,#6495);
#5282=LINE('',#52859,#6496);
#5283=LINE('',#52863,#6497);
#5284=LINE('',#52867,#6498);
#5285=LINE('',#52871,#6499);
#5286=LINE('',#52875,#6500);
#5287=LINE('',#52879,#6501);
#5288=LINE('',#52883,#6502);
#5289=LINE('',#52887,#6503);
#5290=LINE('',#52891,#6504);
#5291=LINE('',#52895,#6505);
#5292=LINE('',#52899,#6506);
#5293=LINE('',#52903,#6507);
#5294=LINE('',#52907,#6508);
#5295=LINE('',#52911,#6509);
#5296=LINE('',#52915,#6510);
#5297=LINE('',#52919,#6511);
#5298=LINE('',#52923,#6512);
#5299=LINE('',#52927,#6513);
#5300=LINE('',#52931,#6514);
#5301=LINE('',#52935,#6515);
#5302=LINE('',#52939,#6516);
#5303=LINE('',#52943,#6517);
#5304=LINE('',#52947,#6518);
#5305=LINE('',#52951,#6519);
#5306=LINE('',#52955,#6520);
#5307=LINE('',#52959,#6521);
#5308=LINE('',#52973,#6522);
#5309=LINE('',#52974,#6523);
#5310=LINE('',#52977,#6524);
#5311=LINE('',#52978,#6525);
#5312=LINE('',#52982,#6526);
#5313=LINE('',#52985,#6527);
#5314=LINE('',#52986,#6528);
#5315=LINE('',#52990,#6529);
#5316=LINE('',#52993,#6530);
#5317=LINE('',#52994,#6531);
#5318=LINE('',#52998,#6532);
#5319=LINE('',#53001,#6533);
#5320=LINE('',#53002,#6534);
#5321=LINE('',#53006,#6535);
#5322=LINE('',#53009,#6536);
#5323=LINE('',#53012,#6537);
#5324=LINE('',#53015,#6538);
#5325=LINE('',#53016,#6539);
#5326=LINE('',#53020,#6540);
#5327=LINE('',#53023,#6541);
#5328=LINE('',#53026,#6542);
#5329=LINE('',#53029,#6543);
#5330=LINE('',#53030,#6544);
#5331=LINE('',#53034,#6545);
#5332=LINE('',#53039,#6546);
#5333=LINE('',#53040,#6547);
#5334=LINE('',#53043,#6548);
#5335=LINE('',#53044,#6549);
#5336=LINE('',#53048,#6550);
#5337=LINE('',#53051,#6551);
#5338=LINE('',#53052,#6552);
#5339=LINE('',#53056,#6553);
#5340=LINE('',#53059,#6554);
#5341=LINE('',#53060,#6555);
#5342=LINE('',#53064,#6556);
#5343=LINE('',#53067,#6557);
#5344=LINE('',#53068,#6558);
#5345=LINE('',#53072,#6559);
#5346=LINE('',#53075,#6560);
#5347=LINE('',#53078,#6561);
#5348=LINE('',#53081,#6562);
#5349=LINE('',#53082,#6563);
#5350=LINE('',#53086,#6564);
#5351=LINE('',#53089,#6565);
#5352=LINE('',#53092,#6566);
#5353=LINE('',#53095,#6567);
#5354=LINE('',#53096,#6568);
#5355=LINE('',#53100,#6569);
#5356=LINE('',#53105,#6570);
#5357=LINE('',#53106,#6571);
#5358=LINE('',#53109,#6572);
#5359=LINE('',#53110,#6573);
#5360=LINE('',#53114,#6574);
#5361=LINE('',#53117,#6575);
#5362=LINE('',#53118,#6576);
#5363=LINE('',#53122,#6577);
#5364=LINE('',#53125,#6578);
#5365=LINE('',#53126,#6579);
#5366=LINE('',#53130,#6580);
#5367=LINE('',#53133,#6581);
#5368=LINE('',#53134,#6582);
#5369=LINE('',#53138,#6583);
#5370=LINE('',#53141,#6584);
#5371=LINE('',#53144,#6585);
#5372=LINE('',#53147,#6586);
#5373=LINE('',#53148,#6587);
#5374=LINE('',#53152,#6588);
#5375=LINE('',#53155,#6589);
#5376=LINE('',#53158,#6590);
#5377=LINE('',#53161,#6591);
#5378=LINE('',#53162,#6592);
#5379=LINE('',#53166,#6593);
#5380=LINE('',#53171,#6594);
#5381=LINE('',#53172,#6595);
#5382=LINE('',#53175,#6596);
#5383=LINE('',#53176,#6597);
#5384=LINE('',#53180,#6598);
#5385=LINE('',#53183,#6599);
#5386=LINE('',#53184,#6600);
#5387=LINE('',#53188,#6601);
#5388=LINE('',#53191,#6602);
#5389=LINE('',#53192,#6603);
#5390=LINE('',#53196,#6604);
#5391=LINE('',#53199,#6605);
#5392=LINE('',#53200,#6606);
#5393=LINE('',#53204,#6607);
#5394=LINE('',#53207,#6608);
#5395=LINE('',#53210,#6609);
#5396=LINE('',#53213,#6610);
#5397=LINE('',#53214,#6611);
#5398=LINE('',#53218,#6612);
#5399=LINE('',#53221,#6613);
#5400=LINE('',#53225,#6614);
#5401=LINE('',#53229,#6615);
#5402=LINE('',#53232,#6616);
#5403=LINE('',#53235,#6617);
#5404=LINE('',#53239,#6618);
#5405=LINE('',#53242,#6619);
#5406=LINE('',#53244,#6620);
#5407=LINE('',#53246,#6621);
#5408=LINE('',#53248,#6622);
#5409=LINE('',#53250,#6623);
#5410=LINE('',#53252,#6624);
#5411=LINE('',#53254,#6625);
#5412=LINE('',#53256,#6626);
#5413=LINE('',#53258,#6627);
#5414=LINE('',#53260,#6628);
#5415=LINE('',#53262,#6629);
#5416=LINE('',#53264,#6630);
#5417=LINE('',#53275,#6631);
#5418=LINE('',#53278,#6632);
#5419=LINE('',#53284,#6633);
#5420=LINE('',#53290,#6634);
#5421=LINE('',#53296,#6635);
#5422=LINE('',#53302,#6636);
#5423=LINE('',#53307,#6637);
#5424=LINE('',#53309,#6638);
#5425=LINE('',#53311,#6639);
#5426=LINE('',#53312,#6640);
#5427=LINE('',#53315,#6641);
#5428=LINE('',#53317,#6642);
#5429=LINE('',#53318,#6643);
#5430=LINE('',#53321,#6644);
#5431=LINE('',#53323,#6645);
#5432=LINE('',#53324,#6646);
#5433=LINE('',#53326,#6647);
#5434=LINE('',#53327,#6648);
#5435=LINE('',#53334,#6649);
#5436=LINE('',#53361,#6650);
#5437=LINE('',#53409,#6651);
#5438=LINE('',#53457,#6652);
#5439=LINE('',#53511,#6653);
#5440=LINE('',#53559,#6654);
#5441=LINE('',#53607,#6655);
#5442=LINE('',#53661,#6656);
#5443=LINE('',#53709,#6657);
#5444=LINE('',#53757,#6658);
#5445=LINE('',#53805,#6659);
#5446=LINE('',#53859,#6660);
#5447=LINE('',#53907,#6661);
#5448=LINE('',#53955,#6662);
#5449=LINE('',#54009,#6663);
#5450=LINE('',#54057,#6664);
#5451=LINE('',#54105,#6665);
#5452=LINE('',#54159,#6666);
#5453=LINE('',#54207,#6667);
#5454=LINE('',#54255,#6668);
#5455=LINE('',#54282,#6669);
#5456=LINE('',#54307,#6670);
#5457=LINE('',#54331,#6671);
#5458=LINE('',#54356,#6672);
#5459=LINE('',#54381,#6673);
#5460=LINE('',#54405,#6674);
#5461=LINE('',#54430,#6675);
#5462=LINE('',#54455,#6676);
#5463=LINE('',#54479,#6677);
#5464=LINE('',#54504,#6678);
#5465=LINE('',#54529,#6679);
#5466=LINE('',#54553,#6680);
#5467=LINE('',#54577,#6681);
#5468=LINE('',#54602,#6682);
#5469=LINE('',#54627,#6683);
#5470=LINE('',#54651,#6684);
#5471=LINE('',#54676,#6685);
#5472=LINE('',#54701,#6686);
#5473=LINE('',#55082,#6687);
#5474=LINE('',#56400,#6688);
#5475=LINE('',#56402,#6689);
#5476=LINE('',#56404,#6690);
#5477=LINE('',#56405,#6691);
#5478=LINE('',#56408,#6692);
#5479=LINE('',#56410,#6693);
#5480=LINE('',#56411,#6694);
#5481=LINE('',#56414,#6695);
#5482=LINE('',#56416,#6696);
#5483=LINE('',#56417,#6697);
#5484=LINE('',#56420,#6698);
#5485=LINE('',#56422,#6699);
#5486=LINE('',#56423,#6700);
#5487=LINE('',#56426,#6701);
#5488=LINE('',#56428,#6702);
#5489=LINE('',#56429,#6703);
#5490=LINE('',#56431,#6704);
#5491=LINE('',#56432,#6705);
#5492=LINE('',#56439,#6706);
#5493=LINE('',#56448,#6707);
#5494=LINE('',#56456,#6708);
#5495=LINE('',#56465,#6709);
#5496=LINE('',#56482,#6710);
#5497=LINE('',#56533,#6711);
#5498=LINE('',#56584,#6712);
#5499=LINE('',#56632,#6713);
#5500=LINE('',#56683,#6714);
#5501=LINE('',#56734,#6715);
#5502=LINE('',#56782,#6716);
#5503=LINE('',#56821,#6717);
#5504=LINE('',#56845,#6718);
#5505=LINE('',#56869,#6719);
#5506=LINE('',#56894,#6720);
#5507=LINE('',#56919,#6721);
#5508=LINE('',#56943,#6722);
#5509=LINE('',#56968,#6723);
#5510=LINE('',#56993,#6724);
#5511=LINE('',#57010,#6725);
#5512=LINE('',#57019,#6726);
#5513=LINE('',#57036,#6727);
#5514=LINE('',#57087,#6728);
#5515=LINE('',#57138,#6729);
#5516=LINE('',#57186,#6730);
#5517=LINE('',#57237,#6731);
#5518=LINE('',#57288,#6732);
#5519=LINE('',#57336,#6733);
#5520=LINE('',#57375,#6734);
#5521=LINE('',#57399,#6735);
#5522=LINE('',#57423,#6736);
#5523=LINE('',#57448,#6737);
#5524=LINE('',#57473,#6738);
#5525=LINE('',#57497,#6739);
#5526=LINE('',#57522,#6740);
#5527=LINE('',#57547,#6741);
#5528=LINE('',#57564,#6742);
#5529=LINE('',#57573,#6743);
#5530=LINE('',#57590,#6744);
#5531=LINE('',#57641,#6745);
#5532=LINE('',#57692,#6746);
#5533=LINE('',#57740,#6747);
#5534=LINE('',#57791,#6748);
#5535=LINE('',#57842,#6749);
#5536=LINE('',#57890,#6750);
#5537=LINE('',#57929,#6751);
#5538=LINE('',#57953,#6752);
#5539=LINE('',#57977,#6753);
#5540=LINE('',#58002,#6754);
#5541=LINE('',#58027,#6755);
#5542=LINE('',#58051,#6756);
#5543=LINE('',#58076,#6757);
#5544=LINE('',#58101,#6758);
#5545=LINE('',#60803,#6759);
#5546=LINE('',#60812,#6760);
#5547=LINE('',#60818,#6761);
#5548=LINE('',#60824,#6762);
#5549=LINE('',#60835,#6763);
#5550=LINE('',#60840,#6764);
#5551=LINE('',#60848,#6765);
#5552=LINE('',#60875,#6766);
#5553=LINE('',#60923,#6767);
#5554=LINE('',#60971,#6768);
#5555=LINE('',#61022,#6769);
#5556=LINE('',#61070,#6770);
#5557=LINE('',#61118,#6771);
#5558=LINE('',#61166,#6772);
#5559=LINE('',#61220,#6773);
#5560=LINE('',#61268,#6774);
#5561=LINE('',#61316,#6775);
#5562=LINE('',#61370,#6776);
#5563=LINE('',#61418,#6777);
#5564=LINE('',#61466,#6778);
#5565=LINE('',#61517,#6779);
#5566=LINE('',#61568,#6780);
#5567=LINE('',#61616,#6781);
#5568=LINE('',#61664,#6782);
#5569=LINE('',#61718,#6783);
#5570=LINE('',#61766,#6784);
#5571=LINE('',#61814,#6785);
#5572=LINE('',#61868,#6786);
#5573=LINE('',#61916,#6787);
#5574=LINE('',#61964,#6788);
#5575=LINE('',#62012,#6789);
#5576=LINE('',#62066,#6790);
#5577=LINE('',#62114,#6791);
#5578=LINE('',#62162,#6792);
#5579=LINE('',#62216,#6793);
#5580=LINE('',#62264,#6794);
#5581=LINE('',#62312,#6795);
#5582=LINE('',#62366,#6796);
#5583=LINE('',#62414,#6797);
#5584=LINE('',#62462,#6798);
#5585=LINE('',#62510,#6799);
#5586=LINE('',#62564,#6800);
#5587=LINE('',#62612,#6801);
#5588=LINE('',#62660,#6802);
#5589=LINE('',#62714,#6803);
#5590=LINE('',#62762,#6804);
#5591=LINE('',#62810,#6805);
#5592=LINE('',#62864,#6806);
#5593=LINE('',#62912,#6807);
#5594=LINE('',#62960,#6808);
#5595=LINE('',#63008,#6809);
#5596=LINE('',#63062,#6810);
#5597=LINE('',#63110,#6811);
#5598=LINE('',#63158,#6812);
#5599=LINE('',#63212,#6813);
#5600=LINE('',#63260,#6814);
#5601=LINE('',#63308,#6815);
#5602=LINE('',#63362,#6816);
#5603=LINE('',#63410,#6817);
#5604=LINE('',#63458,#6818);
#5605=LINE('',#63506,#6819);
#5606=LINE('',#63560,#6820);
#5607=LINE('',#63608,#6821);
#5608=LINE('',#63656,#6822);
#5609=LINE('',#63710,#6823);
#5610=LINE('',#63758,#6824);
#5611=LINE('',#63806,#6825);
#5612=LINE('',#63824,#6826);
#5613=LINE('',#63849,#6827);
#5614=LINE('',#63873,#6828);
#5615=LINE('',#63898,#6829);
#5616=LINE('',#63923,#6830);
#5617=LINE('',#63947,#6831);
#5618=LINE('',#63972,#6832);
#5619=LINE('',#63997,#6833);
#5620=LINE('',#64021,#6834);
#5621=LINE('',#64045,#6835);
#5622=LINE('',#64070,#6836);
#5623=LINE('',#64095,#6837);
#5624=LINE('',#64119,#6838);
#5625=LINE('',#64144,#6839);
#5626=LINE('',#64169,#6840);
#5627=LINE('',#64193,#6841);
#5628=LINE('',#64218,#6842);
#5629=LINE('',#64243,#6843);
#5630=LINE('',#64267,#6844);
#5631=LINE('',#64291,#6845);
#5632=LINE('',#64316,#6846);
#5633=LINE('',#64341,#6847);
#5634=LINE('',#64365,#6848);
#5635=LINE('',#64390,#6849);
#5636=LINE('',#64415,#6850);
#5637=LINE('',#64439,#6851);
#5638=LINE('',#64464,#6852);
#5639=LINE('',#64489,#6853);
#5640=LINE('',#64513,#6854);
#5641=LINE('',#64537,#6855);
#5642=LINE('',#64562,#6856);
#5643=LINE('',#64587,#6857);
#5644=LINE('',#64611,#6858);
#5645=LINE('',#64636,#6859);
#5646=LINE('',#64661,#6860);
#5647=LINE('',#64685,#6861);
#5648=LINE('',#64710,#6862);
#5649=LINE('',#64735,#6863);
#5650=LINE('',#64759,#6864);
#5651=LINE('',#64783,#6865);
#5652=LINE('',#64808,#6866);
#5653=LINE('',#64833,#6867);
#5654=LINE('',#64857,#6868);
#5655=LINE('',#64882,#6869);
#5656=LINE('',#64907,#6870);
#5657=LINE('',#64931,#6871);
#5658=LINE('',#64956,#6872);
#5659=LINE('',#64980,#6873);
#5660=LINE('',#65005,#6874);
#5661=LINE('',#65029,#6875);
#5662=LINE('',#65054,#6876);
#5663=LINE('',#65079,#6877);
#5664=LINE('',#65103,#6878);
#5665=LINE('',#65128,#6879);
#5666=LINE('',#65153,#6880);
#5667=LINE('',#65177,#6881);
#5668=LINE('',#65202,#6882);
#5669=LINE('',#65226,#6883);
#5670=LINE('',#65251,#6884);
#5671=LINE('',#68846,#6885);
#5672=LINE('',#68848,#6886);
#5673=LINE('',#68850,#6887);
#5674=LINE('',#68852,#6888);
#5675=LINE('',#68854,#6889);
#5676=LINE('',#68855,#6890);
#5677=LINE('',#68859,#6891);
#5678=LINE('',#68861,#6892);
#5679=LINE('',#68863,#6893);
#5680=LINE('',#68865,#6894);
#5681=LINE('',#68867,#6895);
#5682=LINE('',#68868,#6896);
#5683=LINE('',#68872,#6897);
#5684=LINE('',#68873,#6898);
#5685=LINE('',#68875,#6899);
#5686=LINE('',#68877,#6900);
#5687=LINE('',#68879,#6901);
#5688=LINE('',#68881,#6902);
#5689=LINE('',#68885,#6903);
#5690=LINE('',#68895,#6904);
#5691=LINE('',#68919,#6905);
#5692=LINE('',#68970,#6906);
#5693=LINE('',#69021,#6907);
#5694=LINE('',#69069,#6908);
#5695=LINE('',#69120,#6909);
#5696=LINE('',#69171,#6910);
#5697=LINE('',#69219,#6911);
#5698=LINE('',#69261,#6912);
#5699=LINE('',#69286,#6913);
#5700=LINE('',#69310,#6914);
#5701=LINE('',#69335,#6915);
#5702=LINE('',#69360,#6916);
#5703=LINE('',#69384,#6917);
#5704=LINE('',#69409,#6918);
#5705=LINE('',#69434,#6919);
#5706=LINE('',#70406,#6920);
#5707=LINE('',#70408,#6921);
#5708=LINE('',#70410,#6922);
#5709=LINE('',#70412,#6923);
#5710=LINE('',#70414,#6924);
#5711=LINE('',#70415,#6925);
#5712=LINE('',#70420,#6926);
#5713=LINE('',#70421,#6927);
#5714=LINE('',#70422,#6928);
#5715=LINE('',#70425,#6929);
#5716=LINE('',#70426,#6930);
#5717=LINE('',#70429,#6931);
#5718=LINE('',#70430,#6932);
#5719=LINE('',#70433,#6933);
#5720=LINE('',#70434,#6934);
#5721=LINE('',#70437,#6935);
#5722=LINE('',#70438,#6936);
#5723=LINE('',#70440,#6937);
#5724=LINE('',#70447,#6938);
#5725=LINE('',#70453,#6939);
#5726=LINE('',#70461,#6940);
#5727=LINE('',#70485,#6941);
#5728=LINE('',#70533,#6942);
#5729=LINE('',#70581,#6943);
#5730=LINE('',#70635,#6944);
#5731=LINE('',#70683,#6945);
#5732=LINE('',#70731,#6946);
#5733=LINE('',#70785,#6947);
#5734=LINE('',#70833,#6948);
#5735=LINE('',#70881,#6949);
#5736=LINE('',#70935,#6950);
#5737=LINE('',#70983,#6951);
#5738=LINE('',#71031,#6952);
#5739=LINE('',#71085,#6953);
#5740=LINE('',#71133,#6954);
#5741=LINE('',#71181,#6955);
#5742=LINE('',#71206,#6956);
#5743=LINE('',#71231,#6957);
#5744=LINE('',#71255,#6958);
#5745=LINE('',#71280,#6959);
#5746=LINE('',#71305,#6960);
#5747=LINE('',#71329,#6961);
#5748=LINE('',#71354,#6962);
#5749=LINE('',#71379,#6963);
#5750=LINE('',#71403,#6964);
#5751=LINE('',#71428,#6965);
#5752=LINE('',#71453,#6966);
#5753=LINE('',#71477,#6967);
#5754=LINE('',#71502,#6968);
#5755=LINE('',#71527,#6969);
#5756=LINE('',#71869,#6970);
#5757=LINE('',#72937,#6971);
#5758=LINE('',#72939,#6972);
#5759=LINE('',#72941,#6973);
#5760=LINE('',#72942,#6974);
#5761=LINE('',#72945,#6975);
#5762=LINE('',#72947,#6976);
#5763=LINE('',#72948,#6977);
#5764=LINE('',#72951,#6978);
#5765=LINE('',#72953,#6979);
#5766=LINE('',#72954,#6980);
#5767=LINE('',#72957,#6981);
#5768=LINE('',#72959,#6982);
#5769=LINE('',#72960,#6983);
#5770=LINE('',#72963,#6984);
#5771=LINE('',#72965,#6985);
#5772=LINE('',#72966,#6986);
#5773=LINE('',#72968,#6987);
#5774=LINE('',#72969,#6988);
#5775=LINE('',#72976,#6989);
#5776=LINE('',#72984,#6990);
#5777=LINE('',#73005,#6991);
#5778=LINE('',#73056,#6992);
#5779=LINE('',#73107,#6993);
#5780=LINE('',#73155,#6994);
#5781=LINE('',#73203,#6995);
#5782=LINE('',#73254,#6996);
#5783=LINE('',#73305,#6997);
#5784=LINE('',#73353,#6998);
#5785=LINE('',#73404,#6999);
#5786=LINE('',#73455,#7000);
#5787=LINE('',#73503,#7001);
#5788=LINE('',#73551,#7002);
#5789=LINE('',#73605,#7003);
#5790=LINE('',#73653,#7004);
#5791=LINE('',#73701,#7005);
#5792=LINE('',#73752,#7006);
#5793=LINE('',#73803,#7007);
#5794=LINE('',#73851,#7008);
#5795=LINE('',#73902,#7009);
#5796=LINE('',#73941,#7010);
#5797=LINE('',#73962,#7011);
#5798=LINE('',#74013,#7012);
#5799=LINE('',#74064,#7013);
#5800=LINE('',#74112,#7014);
#5801=LINE('',#74160,#7015);
#5802=LINE('',#74211,#7016);
#5803=LINE('',#74262,#7017);
#5804=LINE('',#74310,#7018);
#5805=LINE('',#74361,#7019);
#5806=LINE('',#74412,#7020);
#5807=LINE('',#74460,#7021);
#5808=LINE('',#74508,#7022);
#5809=LINE('',#74562,#7023);
#5810=LINE('',#74610,#7024);
#5811=LINE('',#74658,#7025);
#5812=LINE('',#74709,#7026);
#5813=LINE('',#74760,#7027);
#5814=LINE('',#74808,#7028);
#5815=LINE('',#74859,#7029);
#5816=LINE('',#74898,#7030);
#5817=LINE('',#74919,#7031);
#5818=LINE('',#74970,#7032);
#5819=LINE('',#75021,#7033);
#5820=LINE('',#75069,#7034);
#5821=LINE('',#75117,#7035);
#5822=LINE('',#75168,#7036);
#5823=LINE('',#75219,#7037);
#5824=LINE('',#75267,#7038);
#5825=LINE('',#75318,#7039);
#5826=LINE('',#75369,#7040);
#5827=LINE('',#75417,#7041);
#5828=LINE('',#75465,#7042);
#5829=LINE('',#75519,#7043);
#5830=LINE('',#75567,#7044);
#5831=LINE('',#75615,#7045);
#5832=LINE('',#75666,#7046);
#5833=LINE('',#75717,#7047);
#5834=LINE('',#75765,#7048);
#5835=LINE('',#75816,#7049);
#5836=LINE('',#75855,#7050);
#5837=LINE('',#75876,#7051);
#5838=LINE('',#75927,#7052);
#5839=LINE('',#75978,#7053);
#5840=LINE('',#76026,#7054);
#5841=LINE('',#76074,#7055);
#5842=LINE('',#76125,#7056);
#5843=LINE('',#76176,#7057);
#5844=LINE('',#76224,#7058);
#5845=LINE('',#76275,#7059);
#5846=LINE('',#76326,#7060);
#5847=LINE('',#76374,#7061);
#5848=LINE('',#76422,#7062);
#5849=LINE('',#76476,#7063);
#5850=LINE('',#76524,#7064);
#5851=LINE('',#76572,#7065);
#5852=LINE('',#76623,#7066);
#5853=LINE('',#76674,#7067);
#5854=LINE('',#76722,#7068);
#5855=LINE('',#76773,#7069);
#5856=LINE('',#76812,#7070);
#5857=LINE('',#76833,#7071);
#5858=LINE('',#76884,#7072);
#5859=LINE('',#76935,#7073);
#5860=LINE('',#76983,#7074);
#5861=LINE('',#77031,#7075);
#5862=LINE('',#77082,#7076);
#5863=LINE('',#77133,#7077);
#5864=LINE('',#77181,#7078);
#5865=LINE('',#77232,#7079);
#5866=LINE('',#77283,#7080);
#5867=LINE('',#77331,#7081);
#5868=LINE('',#77379,#7082);
#5869=LINE('',#77433,#7083);
#5870=LINE('',#77481,#7084);
#5871=LINE('',#77529,#7085);
#5872=LINE('',#77580,#7086);
#5873=LINE('',#77631,#7087);
#5874=LINE('',#77679,#7088);
#5875=LINE('',#77730,#7089);
#5876=LINE('',#77769,#7090);
#5877=LINE('',#77790,#7091);
#5878=LINE('',#77841,#7092);
#5879=LINE('',#77892,#7093);
#5880=LINE('',#77940,#7094);
#5881=LINE('',#77988,#7095);
#5882=LINE('',#78039,#7096);
#5883=LINE('',#78090,#7097);
#5884=LINE('',#78138,#7098);
#5885=LINE('',#78189,#7099);
#5886=LINE('',#78240,#7100);
#5887=LINE('',#78288,#7101);
#5888=LINE('',#78336,#7102);
#5889=LINE('',#78390,#7103);
#5890=LINE('',#78438,#7104);
#5891=LINE('',#78486,#7105);
#5892=LINE('',#78537,#7106);
#5893=LINE('',#78588,#7107);
#5894=LINE('',#78636,#7108);
#5895=LINE('',#78687,#7109);
#5896=LINE('',#78726,#7110);
#5897=LINE('',#78750,#7111);
#5898=LINE('',#78774,#7112);
#5899=LINE('',#78799,#7113);
#5900=LINE('',#78823,#7114);
#5901=LINE('',#78848,#7115);
#5902=LINE('',#78872,#7116);
#5903=LINE('',#78897,#7117);
#5904=LINE('',#78922,#7118);
#5905=LINE('',#78946,#7119);
#5906=LINE('',#78971,#7120);
#5907=LINE('',#78995,#7121);
#5908=LINE('',#79020,#7122);
#5909=LINE('',#79045,#7123);
#5910=LINE('',#79069,#7124);
#5911=LINE('',#79094,#7125);
#5912=LINE('',#79118,#7126);
#5913=LINE('',#79143,#7127);
#5914=LINE('',#79168,#7128);
#5915=LINE('',#79192,#7129);
#5916=LINE('',#79209,#7130);
#5917=LINE('',#79233,#7131);
#5918=LINE('',#79257,#7132);
#5919=LINE('',#79282,#7133);
#5920=LINE('',#79306,#7134);
#5921=LINE('',#79331,#7135);
#5922=LINE('',#79355,#7136);
#5923=LINE('',#79380,#7137);
#5924=LINE('',#79405,#7138);
#5925=LINE('',#79429,#7139);
#5926=LINE('',#79454,#7140);
#5927=LINE('',#79478,#7141);
#5928=LINE('',#79503,#7142);
#5929=LINE('',#79528,#7143);
#5930=LINE('',#79552,#7144);
#5931=LINE('',#79577,#7145);
#5932=LINE('',#79601,#7146);
#5933=LINE('',#79626,#7147);
#5934=LINE('',#79651,#7148);
#5935=LINE('',#79675,#7149);
#5936=LINE('',#79692,#7150);
#5937=LINE('',#79716,#7151);
#5938=LINE('',#79740,#7152);
#5939=LINE('',#79765,#7153);
#5940=LINE('',#79789,#7154);
#5941=LINE('',#79814,#7155);
#5942=LINE('',#79838,#7156);
#5943=LINE('',#79863,#7157);
#5944=LINE('',#79888,#7158);
#5945=LINE('',#79912,#7159);
#5946=LINE('',#79937,#7160);
#5947=LINE('',#79961,#7161);
#5948=LINE('',#79986,#7162);
#5949=LINE('',#80011,#7163);
#5950=LINE('',#80035,#7164);
#5951=LINE('',#80060,#7165);
#5952=LINE('',#80084,#7166);
#5953=LINE('',#80109,#7167);
#5954=LINE('',#80134,#7168);
#5955=LINE('',#80158,#7169);
#5956=LINE('',#80175,#7170);
#5957=LINE('',#80199,#7171);
#5958=LINE('',#80223,#7172);
#5959=LINE('',#80248,#7173);
#5960=LINE('',#80272,#7174);
#5961=LINE('',#80297,#7175);
#5962=LINE('',#80321,#7176);
#5963=LINE('',#80346,#7177);
#5964=LINE('',#80371,#7178);
#5965=LINE('',#80395,#7179);
#5966=LINE('',#80420,#7180);
#5967=LINE('',#80444,#7181);
#5968=LINE('',#80469,#7182);
#5969=LINE('',#80494,#7183);
#5970=LINE('',#80518,#7184);
#5971=LINE('',#80543,#7185);
#5972=LINE('',#80567,#7186);
#5973=LINE('',#80592,#7187);
#5974=LINE('',#80617,#7188);
#5975=LINE('',#80641,#7189);
#5976=LINE('',#80658,#7190);
#5977=LINE('',#80682,#7191);
#5978=LINE('',#80706,#7192);
#5979=LINE('',#80731,#7193);
#5980=LINE('',#80755,#7194);
#5981=LINE('',#80780,#7195);
#5982=LINE('',#80804,#7196);
#5983=LINE('',#80829,#7197);
#5984=LINE('',#80854,#7198);
#5985=LINE('',#80878,#7199);
#5986=LINE('',#80903,#7200);
#5987=LINE('',#80927,#7201);
#5988=LINE('',#80952,#7202);
#5989=LINE('',#80977,#7203);
#5990=LINE('',#81001,#7204);
#5991=LINE('',#81026,#7205);
#5992=LINE('',#81050,#7206);
#5993=LINE('',#81075,#7207);
#5994=LINE('',#81100,#7208);
#5995=LINE('',#81124,#7209);
#5996=LINE('',#81141,#7210);
#5997=LINE('',#81165,#7211);
#5998=LINE('',#81189,#7212);
#5999=LINE('',#81214,#7213);
#6000=LINE('',#81238,#7214);
#6001=LINE('',#81263,#7215);
#6002=LINE('',#81287,#7216);
#6003=LINE('',#81312,#7217);
#6004=LINE('',#81337,#7218);
#6005=LINE('',#81361,#7219);
#6006=LINE('',#81386,#7220);
#6007=LINE('',#81410,#7221);
#6008=LINE('',#81435,#7222);
#6009=LINE('',#81460,#7223);
#6010=LINE('',#81484,#7224);
#6011=LINE('',#81509,#7225);
#6012=LINE('',#81533,#7226);
#6013=LINE('',#81558,#7227);
#6014=LINE('',#81583,#7228);
#6015=LINE('',#81607,#7229);
#6016=LINE('',#83117,#7230);
#6017=LINE('',#83119,#7231);
#6018=LINE('',#83121,#7232);
#6019=LINE('',#83122,#7233);
#6020=LINE('',#90597,#7234);
#6021=LINE('',#90598,#7235);
#6022=LINE('',#90599,#7236);
#6023=LINE('',#90602,#7237);
#6024=LINE('',#90603,#7238);
#6025=LINE('',#90606,#7239);
#6026=LINE('',#90607,#7240);
#6027=LINE('',#90609,#7241);
#6028=LINE('',#90615,#7242);
#6029=LINE('',#90639,#7243);
#6030=LINE('',#90687,#7244);
#6031=LINE('',#90735,#7245);
#6032=LINE('',#90783,#7246);
#6033=LINE('',#90837,#7247);
#6034=LINE('',#90885,#7248);
#6035=LINE('',#90933,#7249);
#6036=LINE('',#90987,#7250);
#6037=LINE('',#91035,#7251);
#6038=LINE('',#91083,#7252);
#6039=LINE('',#91131,#7253);
#6040=LINE('',#91185,#7254);
#6041=LINE('',#91233,#7255);
#6042=LINE('',#91281,#7256);
#6043=LINE('',#91335,#7257);
#6044=LINE('',#91383,#7258);
#6045=LINE('',#91431,#7259);
#6046=LINE('',#91479,#7260);
#6047=LINE('',#91533,#7261);
#6048=LINE('',#91581,#7262);
#6049=LINE('',#91629,#7263);
#6050=LINE('',#91683,#7264);
#6051=LINE('',#91731,#7265);
#6052=LINE('',#91779,#7266);
#6053=LINE('',#91827,#7267);
#6054=LINE('',#91881,#7268);
#6055=LINE('',#91929,#7269);
#6056=LINE('',#91977,#7270);
#6057=LINE('',#92031,#7271);
#6058=LINE('',#92079,#7272);
#6059=LINE('',#92127,#7273);
#6060=LINE('',#92175,#7274);
#6061=LINE('',#92229,#7275);
#6062=LINE('',#92277,#7276);
#6063=LINE('',#92325,#7277);
#6064=LINE('',#92379,#7278);
#6065=LINE('',#92427,#7279);
#6066=LINE('',#92475,#7280);
#6067=LINE('',#92523,#7281);
#6068=LINE('',#92577,#7282);
#6069=LINE('',#92625,#7283);
#6070=LINE('',#92673,#7284);
#6071=LINE('',#92727,#7285);
#6072=LINE('',#92775,#7286);
#6073=LINE('',#92823,#7287);
#6074=LINE('',#92871,#7288);
#6075=LINE('',#92922,#7289);
#6076=LINE('',#92970,#7290);
#6077=LINE('',#93018,#7291);
#6078=LINE('',#93043,#7292);
#6079=LINE('',#93068,#7293);
#6080=LINE('',#93092,#7294);
#6081=LINE('',#93117,#7295);
#6082=LINE('',#93142,#7296);
#6083=LINE('',#93166,#7297);
#6084=LINE('',#93190,#7298);
#6085=LINE('',#93215,#7299);
#6086=LINE('',#93240,#7300);
#6087=LINE('',#93264,#7301);
#6088=LINE('',#93289,#7302);
#6089=LINE('',#93314,#7303);
#6090=LINE('',#93338,#7304);
#6091=LINE('',#93362,#7305);
#6092=LINE('',#93387,#7306);
#6093=LINE('',#93412,#7307);
#6094=LINE('',#93436,#7308);
#6095=LINE('',#93461,#7309);
#6096=LINE('',#93486,#7310);
#6097=LINE('',#93510,#7311);
#6098=LINE('',#93534,#7312);
#6099=LINE('',#93559,#7313);
#6100=LINE('',#93584,#7314);
#6101=LINE('',#93608,#7315);
#6102=LINE('',#93633,#7316);
#6103=LINE('',#93658,#7317);
#6104=LINE('',#93682,#7318);
#6105=LINE('',#93706,#7319);
#6106=LINE('',#93731,#7320);
#6107=LINE('',#93756,#7321);
#6108=LINE('',#93780,#7322);
#6109=LINE('',#93805,#7323);
#6110=LINE('',#93830,#7324);
#6111=LINE('',#93854,#7325);
#6112=LINE('',#93878,#7326);
#6113=LINE('',#93903,#7327);
#6114=LINE('',#93928,#7328);
#6115=LINE('',#93952,#7329);
#6116=LINE('',#93977,#7330);
#6117=LINE('',#94002,#7331);
#6118=LINE('',#94026,#7332);
#6119=LINE('',#94050,#7333);
#6120=LINE('',#94075,#7334);
#6121=LINE('',#94100,#7335);
#6122=LINE('',#94124,#7336);
#6123=LINE('',#94149,#7337);
#6124=LINE('',#94174,#7338);
#6125=LINE('',#94198,#7339);
#6126=LINE('',#94540,#7340);
#6127=LINE('',#97318,#7341);
#6128=LINE('',#97320,#7342);
#6129=LINE('',#97322,#7343);
#6130=LINE('',#97323,#7344);
#6131=LINE('',#97326,#7345);
#6132=LINE('',#97328,#7346);
#6133=LINE('',#97329,#7347);
#6134=LINE('',#97332,#7348);
#6135=LINE('',#97334,#7349);
#6136=LINE('',#97335,#7350);
#6137=LINE('',#97338,#7351);
#6138=LINE('',#97340,#7352);
#6139=LINE('',#97341,#7353);
#6140=LINE('',#97344,#7354);
#6141=LINE('',#97346,#7355);
#6142=LINE('',#97347,#7356);
#6143=LINE('',#97349,#7357);
#6144=LINE('',#97350,#7358);
#6145=LINE('',#97357,#7359);
#6146=LINE('',#97366,#7360);
#6147=LINE('',#97372,#7361);
#6148=LINE('',#97381,#7362);
#6149=LINE('',#97387,#7363);
#6150=VECTOR('',#23512,3.5);
#6151=VECTOR('',#23519,3.5);
#6152=VECTOR('',#23526,3.5);
#6153=VECTOR('',#23533,3.5);
#6154=VECTOR('',#23540,3.5);
#6155=VECTOR('',#23547,3.5);
#6156=VECTOR('',#23552,10.);
#6157=VECTOR('',#23553,10.);
#6158=VECTOR('',#23554,10.);
#6159=VECTOR('',#23555,10.);
#6160=VECTOR('',#23558,10.);
#6161=VECTOR('',#23559,10.);
#6162=VECTOR('',#23560,10.);
#6163=VECTOR('',#23563,10.);
#6164=VECTOR('',#23564,10.);
#6165=VECTOR('',#23565,10.);
#6166=VECTOR('',#23568,10.);
#6167=VECTOR('',#23569,10.);
#6168=VECTOR('',#23572,10.);
#6169=VECTOR('',#23573,10.);
#6170=VECTOR('',#23574,10.);
#6171=VECTOR('',#23575,10.);
#6172=VECTOR('',#23578,10.);
#6173=VECTOR('',#23579,10.);
#6174=VECTOR('',#23580,10.);
#6175=VECTOR('',#23583,10.);
#6176=VECTOR('',#23584,10.);
#6177=VECTOR('',#23585,10.);
#6178=VECTOR('',#23588,10.);
#6179=VECTOR('',#23589,10.);
#6180=VECTOR('',#23598,10.);
#6181=VECTOR('',#23599,10.);
#6182=VECTOR('',#23600,10.);
#6183=VECTOR('',#23601,10.);
#6184=VECTOR('',#23604,10.);
#6185=VECTOR('',#23605,10.);
#6186=VECTOR('',#23606,10.);
#6187=VECTOR('',#23609,10.);
#6188=VECTOR('',#23610,10.);
#6189=VECTOR('',#23611,10.);
#6190=VECTOR('',#23614,10.);
#6191=VECTOR('',#23615,10.);
#6192=VECTOR('',#23618,10.);
#6193=VECTOR('',#23619,10.);
#6194=VECTOR('',#23620,10.);
#6195=VECTOR('',#23621,10.);
#6196=VECTOR('',#23624,10.);
#6197=VECTOR('',#23625,10.);
#6198=VECTOR('',#23626,10.);
#6199=VECTOR('',#23629,10.);
#6200=VECTOR('',#23630,10.);
#6201=VECTOR('',#23631,10.);
#6202=VECTOR('',#23634,10.);
#6203=VECTOR('',#23635,10.);
#6204=VECTOR('',#23644,4.);
#6205=VECTOR('',#23649,4.);
#6206=VECTOR('',#23652,4.);
#6207=VECTOR('',#23655,4.);
#6208=VECTOR('',#23658,4.);
#6209=VECTOR('',#23661,4.);
#6210=VECTOR('',#23664,4.);
#6211=VECTOR('',#23667,4.);
#6212=VECTOR('',#23672,4.);
#6213=VECTOR('',#23677,4.);
#6214=VECTOR('',#23680,4.);
#6215=VECTOR('',#23683,4.);
#6216=VECTOR('',#23686,4.);
#6217=VECTOR('',#23689,4.);
#6218=VECTOR('',#23692,4.);
#6219=VECTOR('',#23695,4.);
#6220=VECTOR('',#23700,4.);
#6221=VECTOR('',#23705,4.);
#6222=VECTOR('',#23708,4.);
#6223=VECTOR('',#23711,4.);
#6224=VECTOR('',#23714,4.);
#6225=VECTOR('',#23717,4.);
#6226=VECTOR('',#23720,4.);
#6227=VECTOR('',#23723,4.);
#6228=VECTOR('',#23728,4.);
#6229=VECTOR('',#23733,4.);
#6230=VECTOR('',#23736,4.);
#6231=VECTOR('',#23739,4.);
#6232=VECTOR('',#23742,4.);
#6233=VECTOR('',#23745,4.);
#6234=VECTOR('',#23748,4.);
#6235=VECTOR('',#23751,4.);
#6236=VECTOR('',#23756,4.07350000000001);
#6237=VECTOR('',#23761,4.07350000000001);
#6238=VECTOR('',#23764,4.07350000000001);
#6239=VECTOR('',#23767,4.07350000000001);
#6240=VECTOR('',#23770,4.07350000000001);
#6241=VECTOR('',#23773,4.07350000000001);
#6242=VECTOR('',#23776,4.07350000000001);
#6243=VECTOR('',#23779,4.07350000000001);
#6244=VECTOR('',#23784,4.0735);
#6245=VECTOR('',#23789,4.0735);
#6246=VECTOR('',#23792,4.0735);
#6247=VECTOR('',#23795,4.0735);
#6248=VECTOR('',#23798,4.0735);
#6249=VECTOR('',#23801,4.0735);
#6250=VECTOR('',#23804,4.0735);
#6251=VECTOR('',#23807,4.0735);
#6252=VECTOR('',#23812,4.0735);
#6253=VECTOR('',#23817,4.0735);
#6254=VECTOR('',#23820,4.0735);
#6255=VECTOR('',#23823,4.0735);
#6256=VECTOR('',#23826,4.0735);
#6257=VECTOR('',#23829,4.0735);
#6258=VECTOR('',#23832,4.0735);
#6259=VECTOR('',#23835,4.0735);
#6260=VECTOR('',#23840,4.07350000000001);
#6261=VECTOR('',#23845,4.07350000000001);
#6262=VECTOR('',#23848,4.07350000000001);
#6263=VECTOR('',#23851,4.07350000000001);
#6264=VECTOR('',#23854,4.07350000000001);
#6265=VECTOR('',#23857,4.07350000000001);
#6266=VECTOR('',#23860,4.07350000000001);
#6267=VECTOR('',#23863,4.07350000000001);
#6268=VECTOR('',#23870,10.);
#6269=VECTOR('',#23871,10.);
#6270=VECTOR('',#23872,10.);
#6271=VECTOR('',#23873,10.);
#6272=VECTOR('',#23890,10.);
#6273=VECTOR('',#23891,10.);
#6274=VECTOR('',#23892,10.);
#6275=VECTOR('',#23895,10.);
#6276=VECTOR('',#23896,10.);
#6277=VECTOR('',#23899,10.);
#6278=VECTOR('',#23900,10.);
#6279=VECTOR('',#23903,10.);
#6280=VECTOR('',#23910,4.);
#6281=VECTOR('',#23915,4.);
#6282=VECTOR('',#23918,4.);
#6283=VECTOR('',#23921,4.);
#6284=VECTOR('',#23924,4.);
#6285=VECTOR('',#23927,4.);
#6286=VECTOR('',#23930,4.);
#6287=VECTOR('',#23933,4.);
#6288=VECTOR('',#23936,4.);
#6289=VECTOR('',#23939,4.);
#6290=VECTOR('',#23942,4.);
#6291=VECTOR('',#23945,4.);
#6292=VECTOR('',#23948,4.);
#6293=VECTOR('',#23951,4.);
#6294=VECTOR('',#23954,4.);
#6295=VECTOR('',#23957,4.);
#6296=VECTOR('',#23960,4.);
#6297=VECTOR('',#23963,4.);
#6298=VECTOR('',#23966,4.);
#6299=VECTOR('',#23969,4.);
#6300=VECTOR('',#23972,4.);
#6301=VECTOR('',#23975,4.);
#6302=VECTOR('',#23978,4.);
#6303=VECTOR('',#23981,4.);
#6304=VECTOR('',#23984,3.37175);
#6305=VECTOR('',#23989,3.37175);
#6306=VECTOR('',#23992,3.37175);
#6307=VECTOR('',#23995,3.37175);
#6308=VECTOR('',#23998,3.37175);
#6309=VECTOR('',#24001,3.37175);
#6310=VECTOR('',#24004,3.37175);
#6311=VECTOR('',#24007,3.37175);
#6312=VECTOR('',#24010,3.37175);
#6313=VECTOR('',#24013,3.37175);
#6314=VECTOR('',#24016,3.37175);
#6315=VECTOR('',#24019,3.37175);
#6316=VECTOR('',#24022,3.37175);
#6317=VECTOR('',#24025,3.37175);
#6318=VECTOR('',#24028,3.37175);
#6319=VECTOR('',#24031,3.37175);
#6320=VECTOR('',#24034,3.37175);
#6321=VECTOR('',#24037,3.37175);
#6322=VECTOR('',#24040,3.37175);
#6323=VECTOR('',#24043,3.37175);
#6324=VECTOR('',#24046,3.37175);
#6325=VECTOR('',#24049,3.37175);
#6326=VECTOR('',#24052,3.37175);
#6327=VECTOR('',#24055,3.37175);
#6328=VECTOR('',#24060,3.5);
#6329=VECTOR('',#24071,10.);
#6330=VECTOR('',#24072,10.);
#6331=VECTOR('',#24073,10.);
#6332=VECTOR('',#24074,10.);
#6333=VECTOR('',#24077,10.);
#6334=VECTOR('',#24078,10.);
#6335=VECTOR('',#24079,10.);
#6336=VECTOR('',#24082,10.);
#6337=VECTOR('',#24083,10.);
#6338=VECTOR('',#24084,10.);
#6339=VECTOR('',#24087,10.);
#6340=VECTOR('',#24088,10.);
#6341=VECTOR('',#24089,10.);
#6342=VECTOR('',#24092,10.);
#6343=VECTOR('',#24093,10.);
#6344=VECTOR('',#24094,10.);
#6345=VECTOR('',#24097,10.);
#6346=VECTOR('',#24098,10.);
#6347=VECTOR('',#24107,6.5);
#6348=VECTOR('',#24120,4.5);
#6349=VECTOR('',#24127,9.);
#6350=VECTOR('',#24220,5.);
#6351=VECTOR('',#24223,5.);
#6352=VECTOR('',#24230,5.);
#6353=VECTOR('',#24233,5.);
#6354=VECTOR('',#24236,5.);
#6355=VECTOR('',#24239,5.);
#6356=VECTOR('',#24242,5.);
#6357=VECTOR('',#24245,5.);
#6358=VECTOR('',#24248,5.);
#6359=VECTOR('',#24251,5.);
#6360=VECTOR('',#24254,5.);
#6361=VECTOR('',#24257,5.);
#6362=VECTOR('',#24260,5.);
#6363=VECTOR('',#24263,5.);
#6364=VECTOR('',#24266,5.);
#6365=VECTOR('',#24269,5.);
#6366=VECTOR('',#24272,5.);
#6367=VECTOR('',#24275,5.);
#6368=VECTOR('',#24278,5.);
#6369=VECTOR('',#24281,5.);
#6370=VECTOR('',#24284,5.);
#6371=VECTOR('',#24287,5.);
#6372=VECTOR('',#24290,5.);
#6373=VECTOR('',#24293,5.);
#6374=VECTOR('',#24296,5.);
#6375=VECTOR('',#24299,5.);
#6376=VECTOR('',#24304,5.0736);
#6377=VECTOR('',#24309,5.0736);
#6378=VECTOR('',#24312,5.0736);
#6379=VECTOR('',#24315,5.0736);
#6380=VECTOR('',#24318,5.0736);
#6381=VECTOR('',#24321,5.0736);
#6382=VECTOR('',#24324,5.0736);
#6383=VECTOR('',#24327,5.0736);
#6384=VECTOR('',#24330,5.0736);
#6385=VECTOR('',#24333,5.0736);
#6386=VECTOR('',#24336,5.0736);
#6387=VECTOR('',#24339,5.0736);
#6388=VECTOR('',#24342,5.0736);
#6389=VECTOR('',#24345,5.0736);
#6390=VECTOR('',#24348,5.0736);
#6391=VECTOR('',#24351,5.0736);
#6392=VECTOR('',#24354,5.0736);
#6393=VECTOR('',#24357,5.0736);
#6394=VECTOR('',#24360,5.0736);
#6395=VECTOR('',#24363,5.0736);
#6396=VECTOR('',#24366,5.0736);
#6397=VECTOR('',#24369,5.0736);
#6398=VECTOR('',#24372,5.0736);
#6399=VECTOR('',#24375,5.0736);
#6400=VECTOR('',#24378,5.0736);
#6401=VECTOR('',#24383,5.);
#6402=VECTOR('',#24386,5.);
#6403=VECTOR('',#24393,5.);
#6404=VECTOR('',#24396,5.);
#6405=VECTOR('',#24399,5.);
#6406=VECTOR('',#24402,5.);
#6407=VECTOR('',#24405,5.);
#6408=VECTOR('',#24408,5.);
#6409=VECTOR('',#24411,5.);
#6410=VECTOR('',#24414,5.);
#6411=VECTOR('',#24417,5.);
#6412=VECTOR('',#24420,5.);
#6413=VECTOR('',#24423,5.);
#6414=VECTOR('',#24426,5.);
#6415=VECTOR('',#24429,5.);
#6416=VECTOR('',#24432,5.);
#6417=VECTOR('',#24435,5.);
#6418=VECTOR('',#24438,5.);
#6419=VECTOR('',#24441,5.);
#6420=VECTOR('',#24444,5.);
#6421=VECTOR('',#24447,5.);
#6422=VECTOR('',#24450,5.);
#6423=VECTOR('',#24453,5.);
#6424=VECTOR('',#24456,5.);
#6425=VECTOR('',#24459,5.);
#6426=VECTOR('',#24462,5.);
#6427=VECTOR('',#24465,5.);
#6428=VECTOR('',#24468,5.);
#6429=VECTOR('',#24471,5.);
#6430=VECTOR('',#24474,5.);
#6431=VECTOR('',#24477,5.);
#6432=VECTOR('',#24480,5.);
#6433=VECTOR('',#24483,5.);
#6434=VECTOR('',#24486,5.);
#6435=VECTOR('',#24489,5.);
#6436=VECTOR('',#24492,5.);
#6437=VECTOR('',#24495,5.);
#6438=VECTOR('',#24498,5.);
#6439=VECTOR('',#24501,5.);
#6440=VECTOR('',#24504,5.);
#6441=VECTOR('',#24507,5.);
#6442=VECTOR('',#24512,5.0736);
#6443=VECTOR('',#24517,5.0736);
#6444=VECTOR('',#24520,5.0736);
#6445=VECTOR('',#24523,5.0736);
#6446=VECTOR('',#24526,5.0736);
#6447=VECTOR('',#24529,5.0736);
#6448=VECTOR('',#24532,5.0736);
#6449=VECTOR('',#24535,5.0736);
#6450=VECTOR('',#24538,5.0736);
#6451=VECTOR('',#24541,5.0736);
#6452=VECTOR('',#24544,5.0736);
#6453=VECTOR('',#24547,5.0736);
#6454=VECTOR('',#24550,5.0736);
#6455=VECTOR('',#24553,5.0736);
#6456=VECTOR('',#24556,5.0736);
#6457=VECTOR('',#24559,5.0736);
#6458=VECTOR('',#24562,5.0736);
#6459=VECTOR('',#24565,5.0736);
#6460=VECTOR('',#24568,5.0736);
#6461=VECTOR('',#24571,5.0736);
#6462=VECTOR('',#24574,5.0736);
#6463=VECTOR('',#24577,5.0736);
#6464=VECTOR('',#24580,5.0736);
#6465=VECTOR('',#24583,5.0736);
#6466=VECTOR('',#24586,5.0736);
#6467=VECTOR('',#24589,5.0736);
#6468=VECTOR('',#24592,5.0736);
#6469=VECTOR('',#24595,5.0736);
#6470=VECTOR('',#24598,5.0736);
#6471=VECTOR('',#24601,5.0736);
#6472=VECTOR('',#24604,5.0736);
#6473=VECTOR('',#24607,5.0736);
#6474=VECTOR('',#24610,5.0736);
#6475=VECTOR('',#24613,5.0736);
#6476=VECTOR('',#24616,5.0736);
#6477=VECTOR('',#24619,5.0736);
#6478=VECTOR('',#24622,5.0736);
#6479=VECTOR('',#24625,5.0736);
#6480=VECTOR('',#24628,5.0736);
#6481=VECTOR('',#24631,5.0736);
#6482=VECTOR('',#24658,10.);
#6483=VECTOR('',#24661,10.);
#6484=VECTOR('',#24664,10.);
#6485=VECTOR('',#24665,10.);
#6486=VECTOR('',#24666,10.);
#6487=VECTOR('',#24669,10.);
#6488=VECTOR('',#24672,10.);
#6489=VECTOR('',#24675,10.);
#6490=VECTOR('',#24678,10.);
#6491=VECTOR('',#24681,10.);
#6492=VECTOR('',#24684,10.);
#6493=VECTOR('',#24687,10.);
#6494=VECTOR('',#24690,10.);
#6495=VECTOR('',#24693,10.);
#6496=VECTOR('',#24696,10.);
#6497=VECTOR('',#24699,10.);
#6498=VECTOR('',#24702,10.);
#6499=VECTOR('',#24705,10.);
#6500=VECTOR('',#24708,10.);
#6501=VECTOR('',#24711,10.);
#6502=VECTOR('',#24714,10.);
#6503=VECTOR('',#24717,10.);
#6504=VECTOR('',#24720,10.);
#6505=VECTOR('',#24723,10.);
#6506=VECTOR('',#24726,10.);
#6507=VECTOR('',#24729,10.);
#6508=VECTOR('',#24732,10.);
#6509=VECTOR('',#24735,10.);
#6510=VECTOR('',#24738,10.);
#6511=VECTOR('',#24741,10.);
#6512=VECTOR('',#24744,10.);
#6513=VECTOR('',#24747,10.);
#6514=VECTOR('',#24750,10.);
#6515=VECTOR('',#24753,10.);
#6516=VECTOR('',#24756,10.);
#6517=VECTOR('',#24759,10.);
#6518=VECTOR('',#24762,10.);
#6519=VECTOR('',#24765,10.);
#6520=VECTOR('',#24768,10.);
#6521=VECTOR('',#24771,10.);
#6522=VECTOR('',#24786,10.);
#6523=VECTOR('',#24787,10.);
#6524=VECTOR('',#24790,10.);
#6525=VECTOR('',#24791,10.);
#6526=VECTOR('',#24796,10.);
#6527=VECTOR('',#24799,10.);
#6528=VECTOR('',#24800,10.);
#6529=VECTOR('',#24805,10.);
#6530=VECTOR('',#24808,10.);
#6531=VECTOR('',#24809,10.);
#6532=VECTOR('',#24814,10.);
#6533=VECTOR('',#24817,10.);
#6534=VECTOR('',#24818,10.);
#6535=VECTOR('',#24823,10.);
#6536=VECTOR('',#24826,10.);
#6537=VECTOR('',#24829,10.);
#6538=VECTOR('',#24832,10.);
#6539=VECTOR('',#24833,10.);
#6540=VECTOR('',#24838,10.);
#6541=VECTOR('',#24841,10.);
#6542=VECTOR('',#24844,10.);
#6543=VECTOR('',#24847,10.);
#6544=VECTOR('',#24848,10.);
#6545=VECTOR('',#24853,10.);
#6546=VECTOR('',#24858,10.);
#6547=VECTOR('',#24859,10.);
#6548=VECTOR('',#24862,10.);
#6549=VECTOR('',#24863,10.);
#6550=VECTOR('',#24868,10.);
#6551=VECTOR('',#24871,10.);
#6552=VECTOR('',#24872,10.);
#6553=VECTOR('',#24877,10.);
#6554=VECTOR('',#24880,10.);
#6555=VECTOR('',#24881,10.);
#6556=VECTOR('',#24886,10.);
#6557=VECTOR('',#24889,10.);
#6558=VECTOR('',#24890,10.);
#6559=VECTOR('',#24895,10.);
#6560=VECTOR('',#24898,10.);
#6561=VECTOR('',#24901,10.);
#6562=VECTOR('',#24904,10.);
#6563=VECTOR('',#24905,10.);
#6564=VECTOR('',#24910,10.);
#6565=VECTOR('',#24913,10.);
#6566=VECTOR('',#24916,10.);
#6567=VECTOR('',#24919,10.);
#6568=VECTOR('',#24920,10.);
#6569=VECTOR('',#24925,10.);
#6570=VECTOR('',#24930,10.);
#6571=VECTOR('',#24931,10.);
#6572=VECTOR('',#24934,10.);
#6573=VECTOR('',#24935,10.);
#6574=VECTOR('',#24940,10.);
#6575=VECTOR('',#24943,10.);
#6576=VECTOR('',#24944,10.);
#6577=VECTOR('',#24949,10.);
#6578=VECTOR('',#24952,10.);
#6579=VECTOR('',#24953,10.);
#6580=VECTOR('',#24958,10.);
#6581=VECTOR('',#24961,10.);
#6582=VECTOR('',#24962,10.);
#6583=VECTOR('',#24967,10.);
#6584=VECTOR('',#24970,10.);
#6585=VECTOR('',#24973,10.);
#6586=VECTOR('',#24976,10.);
#6587=VECTOR('',#24977,10.);
#6588=VECTOR('',#24982,10.);
#6589=VECTOR('',#24985,10.);
#6590=VECTOR('',#24988,10.);
#6591=VECTOR('',#24991,10.);
#6592=VECTOR('',#24992,10.);
#6593=VECTOR('',#24997,10.);
#6594=VECTOR('',#25002,10.);
#6595=VECTOR('',#25003,10.);
#6596=VECTOR('',#25006,10.);
#6597=VECTOR('',#25007,10.);
#6598=VECTOR('',#25012,10.);
#6599=VECTOR('',#25015,10.);
#6600=VECTOR('',#25016,10.);
#6601=VECTOR('',#25021,10.);
#6602=VECTOR('',#25024,10.);
#6603=VECTOR('',#25025,10.);
#6604=VECTOR('',#25030,10.);
#6605=VECTOR('',#25033,10.);
#6606=VECTOR('',#25034,10.);
#6607=VECTOR('',#25039,10.);
#6608=VECTOR('',#25042,10.);
#6609=VECTOR('',#25045,10.);
#6610=VECTOR('',#25048,10.);
#6611=VECTOR('',#25049,10.);
#6612=VECTOR('',#25054,10.);
#6613=VECTOR('',#25057,10.);
#6614=VECTOR('',#25062,3.);
#6615=VECTOR('',#25067,3.);
#6616=VECTOR('',#25072,4.);
#6617=VECTOR('',#25075,3.);
#6618=VECTOR('',#25080,3.);
#6619=VECTOR('',#25085,10.);
#6620=VECTOR('',#25088,10.);
#6621=VECTOR('',#25091,10.);
#6622=VECTOR('',#25094,10.);
#6623=VECTOR('',#25097,10.);
#6624=VECTOR('',#25100,10.);
#6625=VECTOR('',#25103,10.);
#6626=VECTOR('',#25106,10.);
#6627=VECTOR('',#25109,10.);
#6628=VECTOR('',#25112,10.);
#6629=VECTOR('',#25115,10.);
#6630=VECTOR('',#25118,10.);
#6631=VECTOR('',#25133,8.5);
#6632=VECTOR('',#25136,5.5);
#6633=VECTOR('',#25143,4.5);
#6634=VECTOR('',#25150,4.5);
#6635=VECTOR('',#25157,4.5);
#6636=VECTOR('',#25164,4.5);
#6637=VECTOR('',#25169,10.);
#6638=VECTOR('',#25170,10.);
#6639=VECTOR('',#25171,10.);
#6640=VECTOR('',#25172,10.);
#6641=VECTOR('',#25175,10.);
#6642=VECTOR('',#25176,10.);
#6643=VECTOR('',#25177,10.);
#6644=VECTOR('',#25180,10.);
#6645=VECTOR('',#25181,10.);
#6646=VECTOR('',#25182,10.);
#6647=VECTOR('',#25185,10.);
#6648=VECTOR('',#25186,10.);
#6649=VECTOR('',#25195,5.);
#6650=VECTOR('',#25200,5.);
#6651=VECTOR('',#25203,5.);
#6652=VECTOR('',#25206,5.);
#6653=VECTOR('',#25209,5.);
#6654=VECTOR('',#25212,5.);
#6655=VECTOR('',#25215,5.);
#6656=VECTOR('',#25218,5.);
#6657=VECTOR('',#25221,5.);
#6658=VECTOR('',#25224,5.);
#6659=VECTOR('',#25227,5.);
#6660=VECTOR('',#25230,5.);
#6661=VECTOR('',#25233,5.);
#6662=VECTOR('',#25236,5.);
#6663=VECTOR('',#25239,5.);
#6664=VECTOR('',#25242,5.);
#6665=VECTOR('',#25245,5.);
#6666=VECTOR('',#25248,5.);
#6667=VECTOR('',#25251,5.);
#6668=VECTOR('',#25254,4.372);
#6669=VECTOR('',#25259,4.372);
#6670=VECTOR('',#25262,4.372);
#6671=VECTOR('',#25265,4.372);
#6672=VECTOR('',#25268,4.372);
#6673=VECTOR('',#25271,4.372);
#6674=VECTOR('',#25274,4.372);
#6675=VECTOR('',#25277,4.372);
#6676=VECTOR('',#25280,4.372);
#6677=VECTOR('',#25283,4.372);
#6678=VECTOR('',#25286,4.372);
#6679=VECTOR('',#25289,4.372);
#6680=VECTOR('',#25292,4.372);
#6681=VECTOR('',#25295,4.372);
#6682=VECTOR('',#25298,4.372);
#6683=VECTOR('',#25301,4.372);
#6684=VECTOR('',#25304,4.372);
#6685=VECTOR('',#25307,4.372);
#6686=VECTOR('',#25310,4.372);
#6687=VECTOR('',#25315,4.5);
#6688=VECTOR('',#25326,10.);
#6689=VECTOR('',#25327,10.);
#6690=VECTOR('',#25328,10.);
#6691=VECTOR('',#25329,10.);
#6692=VECTOR('',#25332,10.);
#6693=VECTOR('',#25333,10.);
#6694=VECTOR('',#25334,10.);
#6695=VECTOR('',#25337,10.);
#6696=VECTOR('',#25338,10.);
#6697=VECTOR('',#25339,10.);
#6698=VECTOR('',#25342,10.);
#6699=VECTOR('',#25343,10.);
#6700=VECTOR('',#25344,10.);
#6701=VECTOR('',#25347,10.);
#6702=VECTOR('',#25348,10.);
#6703=VECTOR('',#25349,10.);
#6704=VECTOR('',#25352,10.);
#6705=VECTOR('',#25353,10.);
#6706=VECTOR('',#25362,8.);
#6707=VECTOR('',#25375,30.);
#6708=VECTOR('',#25386,3.);
#6709=VECTOR('',#25389,3.);
#6710=VECTOR('',#25396,3.);
#6711=VECTOR('',#25399,3.);
#6712=VECTOR('',#25402,3.);
#6713=VECTOR('',#25405,3.);
#6714=VECTOR('',#25408,3.);
#6715=VECTOR('',#25411,3.);
#6716=VECTOR('',#25414,3.);
#6717=VECTOR('',#25419,3.0735);
#6718=VECTOR('',#25424,3.0735);
#6719=VECTOR('',#25427,3.0735);
#6720=VECTOR('',#25430,3.0735);
#6721=VECTOR('',#25433,3.0735);
#6722=VECTOR('',#25436,3.0735);
#6723=VECTOR('',#25439,3.0735);
#6724=VECTOR('',#25442,3.0735);
#6725=VECTOR('',#25447,3.);
#6726=VECTOR('',#25450,3.);
#6727=VECTOR('',#25457,3.);
#6728=VECTOR('',#25460,3.);
#6729=VECTOR('',#25463,3.);
#6730=VECTOR('',#25466,3.);
#6731=VECTOR('',#25469,3.);
#6732=VECTOR('',#25472,3.);
#6733=VECTOR('',#25475,3.);
#6734=VECTOR('',#25480,3.0735);
#6735=VECTOR('',#25485,3.0735);
#6736=VECTOR('',#25488,3.0735);
#6737=VECTOR('',#25491,3.0735);
#6738=VECTOR('',#25494,3.0735);
#6739=VECTOR('',#25497,3.0735);
#6740=VECTOR('',#25500,3.0735);
#6741=VECTOR('',#25503,3.0735);
#6742=VECTOR('',#25508,3.);
#6743=VECTOR('',#25511,3.);
#6744=VECTOR('',#25518,3.);
#6745=VECTOR('',#25521,3.);
#6746=VECTOR('',#25524,3.);
#6747=VECTOR('',#25527,3.);
#6748=VECTOR('',#25530,3.);
#6749=VECTOR('',#25533,3.);
#6750=VECTOR('',#25536,3.);
#6751=VECTOR('',#25541,3.0735);
#6752=VECTOR('',#25546,3.0735);
#6753=VECTOR('',#25549,3.0735);
#6754=VECTOR('',#25552,3.0735);
#6755=VECTOR('',#25555,3.0735);
#6756=VECTOR('',#25558,3.0735);
#6757=VECTOR('',#25561,3.0735);
#6758=VECTOR('',#25564,3.0735);
#6759=VECTOR('',#25601,30.);
#6760=VECTOR('',#25614,3.5);
#6761=VECTOR('',#25621,3.5);
#6762=VECTOR('',#25628,3.5);
#6763=VECTOR('',#25643,5.5);
#6764=VECTOR('',#25648,22.);
#6765=VECTOR('',#25659,5.);
#6766=VECTOR('',#25664,5.);
#6767=VECTOR('',#25667,5.);
#6768=VECTOR('',#25670,5.);
#6769=VECTOR('',#25673,5.);
#6770=VECTOR('',#25676,5.);
#6771=VECTOR('',#25679,5.);
#6772=VECTOR('',#25682,5.);
#6773=VECTOR('',#25685,5.);
#6774=VECTOR('',#25688,5.);
#6775=VECTOR('',#25691,5.);
#6776=VECTOR('',#25694,5.);
#6777=VECTOR('',#25697,5.);
#6778=VECTOR('',#25700,5.);
#6779=VECTOR('',#25703,5.);
#6780=VECTOR('',#25706,5.);
#6781=VECTOR('',#25709,5.);
#6782=VECTOR('',#25712,5.);
#6783=VECTOR('',#25715,5.);
#6784=VECTOR('',#25718,5.);
#6785=VECTOR('',#25721,5.);
#6786=VECTOR('',#25724,5.);
#6787=VECTOR('',#25727,5.);
#6788=VECTOR('',#25730,5.);
#6789=VECTOR('',#25733,5.);
#6790=VECTOR('',#25736,5.);
#6791=VECTOR('',#25739,5.);
#6792=VECTOR('',#25742,5.);
#6793=VECTOR('',#25745,5.);
#6794=VECTOR('',#25748,5.);
#6795=VECTOR('',#25751,5.);
#6796=VECTOR('',#25754,5.);
#6797=VECTOR('',#25757,5.);
#6798=VECTOR('',#25760,5.);
#6799=VECTOR('',#25763,5.);
#6800=VECTOR('',#25766,5.);
#6801=VECTOR('',#25769,5.);
#6802=VECTOR('',#25772,5.);
#6803=VECTOR('',#25775,5.);
#6804=VECTOR('',#25778,5.);
#6805=VECTOR('',#25781,5.);
#6806=VECTOR('',#25784,5.);
#6807=VECTOR('',#25787,5.);
#6808=VECTOR('',#25790,5.);
#6809=VECTOR('',#25793,5.);
#6810=VECTOR('',#25796,5.);
#6811=VECTOR('',#25799,5.);
#6812=VECTOR('',#25802,5.);
#6813=VECTOR('',#25805,5.);
#6814=VECTOR('',#25808,5.);
#6815=VECTOR('',#25811,5.);
#6816=VECTOR('',#25814,5.);
#6817=VECTOR('',#25817,5.);
#6818=VECTOR('',#25820,5.);
#6819=VECTOR('',#25823,5.);
#6820=VECTOR('',#25826,5.);
#6821=VECTOR('',#25829,5.);
#6822=VECTOR('',#25832,5.);
#6823=VECTOR('',#25835,5.);
#6824=VECTOR('',#25838,5.);
#6825=VECTOR('',#25841,4.372);
#6826=VECTOR('',#25846,4.372);
#6827=VECTOR('',#25849,4.372);
#6828=VECTOR('',#25852,4.372);
#6829=VECTOR('',#25855,4.372);
#6830=VECTOR('',#25858,4.372);
#6831=VECTOR('',#25861,4.372);
#6832=VECTOR('',#25864,4.372);
#6833=VECTOR('',#25867,4.372);
#6834=VECTOR('',#25870,4.372);
#6835=VECTOR('',#25873,4.372);
#6836=VECTOR('',#25876,4.372);
#6837=VECTOR('',#25879,4.372);
#6838=VECTOR('',#25882,4.372);
#6839=VECTOR('',#25885,4.372);
#6840=VECTOR('',#25888,4.372);
#6841=VECTOR('',#25891,4.372);
#6842=VECTOR('',#25894,4.372);
#6843=VECTOR('',#25897,4.372);
#6844=VECTOR('',#25900,4.372);
#6845=VECTOR('',#25903,4.372);
#6846=VECTOR('',#25906,4.372);
#6847=VECTOR('',#25909,4.372);
#6848=VECTOR('',#25912,4.372);
#6849=VECTOR('',#25915,4.372);
#6850=VECTOR('',#25918,4.372);
#6851=VECTOR('',#25921,4.372);
#6852=VECTOR('',#25924,4.372);
#6853=VECTOR('',#25927,4.372);
#6854=VECTOR('',#25930,4.372);
#6855=VECTOR('',#25933,4.372);
#6856=VECTOR('',#25936,4.372);
#6857=VECTOR('',#25939,4.372);
#6858=VECTOR('',#25942,4.372);
#6859=VECTOR('',#25945,4.372);
#6860=VECTOR('',#25948,4.372);
#6861=VECTOR('',#25951,4.372);
#6862=VECTOR('',#25954,4.372);
#6863=VECTOR('',#25957,4.372);
#6864=VECTOR('',#25960,4.372);
#6865=VECTOR('',#25963,4.372);
#6866=VECTOR('',#25966,4.372);
#6867=VECTOR('',#25969,4.372);
#6868=VECTOR('',#25972,4.372);
#6869=VECTOR('',#25975,4.372);
#6870=VECTOR('',#25978,4.372);
#6871=VECTOR('',#25981,4.372);
#6872=VECTOR('',#25984,4.372);
#6873=VECTOR('',#25987,4.372);
#6874=VECTOR('',#25990,4.372);
#6875=VECTOR('',#25993,4.372);
#6876=VECTOR('',#25996,4.372);
#6877=VECTOR('',#25999,4.372);
#6878=VECTOR('',#26002,4.372);
#6879=VECTOR('',#26005,4.372);
#6880=VECTOR('',#26008,4.372);
#6881=VECTOR('',#26011,4.372);
#6882=VECTOR('',#26014,4.372);
#6883=VECTOR('',#26017,4.372);
#6884=VECTOR('',#26020,4.372);
#6885=VECTOR('',#26031,10.);
#6886=VECTOR('',#26032,10.);
#6887=VECTOR('',#26033,10.);
#6888=VECTOR('',#26034,10.);
#6889=VECTOR('',#26035,10.);
#6890=VECTOR('',#26036,10.);
#6891=VECTOR('',#26039,10.);
#6892=VECTOR('',#26040,10.);
#6893=VECTOR('',#26041,10.);
#6894=VECTOR('',#26042,10.);
#6895=VECTOR('',#26043,10.);
#6896=VECTOR('',#26044,10.);
#6897=VECTOR('',#26049,10.);
#6898=VECTOR('',#26050,10.);
#6899=VECTOR('',#26053,10.);
#6900=VECTOR('',#26056,10.);
#6901=VECTOR('',#26059,10.);
#6902=VECTOR('',#26062,10.);
#6903=VECTOR('',#26067,5.);
#6904=VECTOR('',#26080,5.);
#6905=VECTOR('',#26085,5.);
#6906=VECTOR('',#26088,5.);
#6907=VECTOR('',#26091,5.);
#6908=VECTOR('',#26094,5.);
#6909=VECTOR('',#26097,5.);
#6910=VECTOR('',#26100,5.);
#6911=VECTOR('',#26103,5.);
#6912=VECTOR('',#26108,5.0736);
#6913=VECTOR('',#26113,5.0736);
#6914=VECTOR('',#26116,5.0736);
#6915=VECTOR('',#26119,5.0736);
#6916=VECTOR('',#26122,5.0736);
#6917=VECTOR('',#26125,5.0736);
#6918=VECTOR('',#26128,5.0736);
#6919=VECTOR('',#26131,5.0736);
#6920=VECTOR('',#26138,10.);
#6921=VECTOR('',#26139,10.);
#6922=VECTOR('',#26140,10.);
#6923=VECTOR('',#26141,10.);
#6924=VECTOR('',#26142,10.);
#6925=VECTOR('',#26143,10.);
#6926=VECTOR('',#26148,10.);
#6927=VECTOR('',#26149,10.);
#6928=VECTOR('',#26150,10.);
#6929=VECTOR('',#26153,10.);
#6930=VECTOR('',#26154,10.);
#6931=VECTOR('',#26157,10.);
#6932=VECTOR('',#26158,10.);
#6933=VECTOR('',#26161,10.);
#6934=VECTOR('',#26162,10.);
#6935=VECTOR('',#26165,10.);
#6936=VECTOR('',#26166,10.);
#6937=VECTOR('',#26169,10.);
#6938=VECTOR('',#26178,5.5);
#6939=VECTOR('',#26185,11.);
#6940=VECTOR('',#26196,3.);
#6941=VECTOR('',#26201,3.);
#6942=VECTOR('',#26204,3.);
#6943=VECTOR('',#26207,3.);
#6944=VECTOR('',#26210,3.);
#6945=VECTOR('',#26213,3.);
#6946=VECTOR('',#26216,3.);
#6947=VECTOR('',#26219,3.);
#6948=VECTOR('',#26222,3.);
#6949=VECTOR('',#26225,3.);
#6950=VECTOR('',#26228,3.);
#6951=VECTOR('',#26231,3.);
#6952=VECTOR('',#26234,3.);
#6953=VECTOR('',#26237,3.);
#6954=VECTOR('',#26240,3.);
#6955=VECTOR('',#26243,2.37175);
#6956=VECTOR('',#26248,2.37175);
#6957=VECTOR('',#26251,2.37175);
#6958=VECTOR('',#26254,2.37175);
#6959=VECTOR('',#26257,2.37175);
#6960=VECTOR('',#26260,2.37175);
#6961=VECTOR('',#26263,2.37175);
#6962=VECTOR('',#26266,2.37175);
#6963=VECTOR('',#26269,2.37175);
#6964=VECTOR('',#26272,2.37175);
#6965=VECTOR('',#26275,2.37175);
#6966=VECTOR('',#26278,2.37175);
#6967=VECTOR('',#26281,2.37175);
#6968=VECTOR('',#26284,2.37175);
#6969=VECTOR('',#26287,2.37175);
#6970=VECTOR('',#26292,2.5);
#6971=VECTOR('',#26303,10.);
#6972=VECTOR('',#26304,10.);
#6973=VECTOR('',#26305,10.);
#6974=VECTOR('',#26306,10.);
#6975=VECTOR('',#26309,10.);
#6976=VECTOR('',#26310,10.);
#6977=VECTOR('',#26311,10.);
#6978=VECTOR('',#26314,10.);
#6979=VECTOR('',#26315,10.);
#6980=VECTOR('',#26316,10.);
#6981=VECTOR('',#26319,10.);
#6982=VECTOR('',#26320,10.);
#6983=VECTOR('',#26321,10.);
#6984=VECTOR('',#26324,10.);
#6985=VECTOR('',#26325,10.);
#6986=VECTOR('',#26326,10.);
#6987=VECTOR('',#26329,10.);
#6988=VECTOR('',#26330,10.);
#6989=VECTOR('',#26339,5.);
#6990=VECTOR('',#26350,3.);
#6991=VECTOR('',#26355,3.);
#6992=VECTOR('',#26358,3.);
#6993=VECTOR('',#26361,3.);
#6994=VECTOR('',#26364,3.);
#6995=VECTOR('',#26367,3.);
#6996=VECTOR('',#26370,3.);
#6997=VECTOR('',#26373,3.);
#6998=VECTOR('',#26376,3.);
#6999=VECTOR('',#26379,3.);
#7000=VECTOR('',#26382,3.);
#7001=VECTOR('',#26385,3.);
#7002=VECTOR('',#26388,3.);
#7003=VECTOR('',#26391,3.);
#7004=VECTOR('',#26394,3.);
#7005=VECTOR('',#26397,3.);
#7006=VECTOR('',#26400,3.);
#7007=VECTOR('',#26403,3.);
#7008=VECTOR('',#26406,3.);
#7009=VECTOR('',#26409,3.);
#7010=VECTOR('',#26414,3.);
#7011=VECTOR('',#26419,3.);
#7012=VECTOR('',#26422,3.);
#7013=VECTOR('',#26425,3.);
#7014=VECTOR('',#26428,3.);
#7015=VECTOR('',#26431,3.);
#7016=VECTOR('',#26434,3.);
#7017=VECTOR('',#26437,3.);
#7018=VECTOR('',#26440,3.);
#7019=VECTOR('',#26443,3.);
#7020=VECTOR('',#26446,3.);
#7021=VECTOR('',#26449,3.);
#7022=VECTOR('',#26452,3.);
#7023=VECTOR('',#26455,3.);
#7024=VECTOR('',#26458,3.);
#7025=VECTOR('',#26461,3.);
#7026=VECTOR('',#26464,3.);
#7027=VECTOR('',#26467,3.);
#7028=VECTOR('',#26470,3.);
#7029=VECTOR('',#26473,3.);
#7030=VECTOR('',#26478,3.);
#7031=VECTOR('',#26483,3.);
#7032=VECTOR('',#26486,3.);
#7033=VECTOR('',#26489,3.);
#7034=VECTOR('',#26492,3.);
#7035=VECTOR('',#26495,3.);
#7036=VECTOR('',#26498,3.);
#7037=VECTOR('',#26501,3.);
#7038=VECTOR('',#26504,3.);
#7039=VECTOR('',#26507,3.);
#7040=VECTOR('',#26510,3.);
#7041=VECTOR('',#26513,3.);
#7042=VECTOR('',#26516,3.);
#7043=VECTOR('',#26519,3.);
#7044=VECTOR('',#26522,3.);
#7045=VECTOR('',#26525,3.);
#7046=VECTOR('',#26528,3.);
#7047=VECTOR('',#26531,3.);
#7048=VECTOR('',#26534,3.);
#7049=VECTOR('',#26537,3.);
#7050=VECTOR('',#26542,3.);
#7051=VECTOR('',#26547,3.);
#7052=VECTOR('',#26550,3.);
#7053=VECTOR('',#26553,3.);
#7054=VECTOR('',#26556,3.);
#7055=VECTOR('',#26559,3.);
#7056=VECTOR('',#26562,3.);
#7057=VECTOR('',#26565,3.);
#7058=VECTOR('',#26568,3.);
#7059=VECTOR('',#26571,3.);
#7060=VECTOR('',#26574,3.);
#7061=VECTOR('',#26577,3.);
#7062=VECTOR('',#26580,3.);
#7063=VECTOR('',#26583,3.);
#7064=VECTOR('',#26586,3.);
#7065=VECTOR('',#26589,3.);
#7066=VECTOR('',#26592,3.);
#7067=VECTOR('',#26595,3.);
#7068=VECTOR('',#26598,3.);
#7069=VECTOR('',#26601,3.);
#7070=VECTOR('',#26606,3.);
#7071=VECTOR('',#26611,3.);
#7072=VECTOR('',#26614,3.);
#7073=VECTOR('',#26617,3.);
#7074=VECTOR('',#26620,3.);
#7075=VECTOR('',#26623,3.);
#7076=VECTOR('',#26626,3.);
#7077=VECTOR('',#26629,3.);
#7078=VECTOR('',#26632,3.);
#7079=VECTOR('',#26635,3.);
#7080=VECTOR('',#26638,3.);
#7081=VECTOR('',#26641,3.);
#7082=VECTOR('',#26644,3.);
#7083=VECTOR('',#26647,3.);
#7084=VECTOR('',#26650,3.);
#7085=VECTOR('',#26653,3.);
#7086=VECTOR('',#26656,3.);
#7087=VECTOR('',#26659,3.);
#7088=VECTOR('',#26662,3.);
#7089=VECTOR('',#26665,3.);
#7090=VECTOR('',#26670,3.);
#7091=VECTOR('',#26675,3.);
#7092=VECTOR('',#26678,3.);
#7093=VECTOR('',#26681,3.);
#7094=VECTOR('',#26684,3.);
#7095=VECTOR('',#26687,3.);
#7096=VECTOR('',#26690,3.);
#7097=VECTOR('',#26693,3.);
#7098=VECTOR('',#26696,3.);
#7099=VECTOR('',#26699,3.);
#7100=VECTOR('',#26702,3.);
#7101=VECTOR('',#26705,3.);
#7102=VECTOR('',#26708,3.);
#7103=VECTOR('',#26711,3.);
#7104=VECTOR('',#26714,3.);
#7105=VECTOR('',#26717,3.);
#7106=VECTOR('',#26720,3.);
#7107=VECTOR('',#26723,3.);
#7108=VECTOR('',#26726,3.);
#7109=VECTOR('',#26729,3.);
#7110=VECTOR('',#26734,3.0735);
#7111=VECTOR('',#26739,3.0735);
#7112=VECTOR('',#26742,3.0735);
#7113=VECTOR('',#26745,3.0735);
#7114=VECTOR('',#26748,3.0735);
#7115=VECTOR('',#26751,3.0735);
#7116=VECTOR('',#26754,3.0735);
#7117=VECTOR('',#26757,3.0735);
#7118=VECTOR('',#26760,3.0735);
#7119=VECTOR('',#26763,3.0735);
#7120=VECTOR('',#26766,3.0735);
#7121=VECTOR('',#26769,3.0735);
#7122=VECTOR('',#26772,3.0735);
#7123=VECTOR('',#26775,3.0735);
#7124=VECTOR('',#26778,3.0735);
#7125=VECTOR('',#26781,3.0735);
#7126=VECTOR('',#26784,3.0735);
#7127=VECTOR('',#26787,3.0735);
#7128=VECTOR('',#26790,3.0735);
#7129=VECTOR('',#26793,3.0735);
#7130=VECTOR('',#26798,3.0735);
#7131=VECTOR('',#26803,3.0735);
#7132=VECTOR('',#26806,3.0735);
#7133=VECTOR('',#26809,3.0735);
#7134=VECTOR('',#26812,3.0735);
#7135=VECTOR('',#26815,3.0735);
#7136=VECTOR('',#26818,3.0735);
#7137=VECTOR('',#26821,3.0735);
#7138=VECTOR('',#26824,3.0735);
#7139=VECTOR('',#26827,3.0735);
#7140=VECTOR('',#26830,3.0735);
#7141=VECTOR('',#26833,3.0735);
#7142=VECTOR('',#26836,3.0735);
#7143=VECTOR('',#26839,3.0735);
#7144=VECTOR('',#26842,3.0735);
#7145=VECTOR('',#26845,3.0735);
#7146=VECTOR('',#26848,3.0735);
#7147=VECTOR('',#26851,3.0735);
#7148=VECTOR('',#26854,3.0735);
#7149=VECTOR('',#26857,3.0735);
#7150=VECTOR('',#26862,3.07349999999996);
#7151=VECTOR('',#26867,3.07349999999996);
#7152=VECTOR('',#26870,3.07349999999996);
#7153=VECTOR('',#26873,3.07349999999996);
#7154=VECTOR('',#26876,3.07349999999996);
#7155=VECTOR('',#26879,3.07349999999996);
#7156=VECTOR('',#26882,3.07349999999996);
#7157=VECTOR('',#26885,3.07349999999996);
#7158=VECTOR('',#26888,3.07349999999996);
#7159=VECTOR('',#26891,3.07349999999996);
#7160=VECTOR('',#26894,3.07349999999996);
#7161=VECTOR('',#26897,3.07349999999996);
#7162=VECTOR('',#26900,3.07349999999996);
#7163=VECTOR('',#26903,3.07349999999996);
#7164=VECTOR('',#26906,3.07349999999996);
#7165=VECTOR('',#26909,3.07349999999996);
#7166=VECTOR('',#26912,3.07349999999996);
#7167=VECTOR('',#26915,3.07349999999996);
#7168=VECTOR('',#26918,3.07349999999996);
#7169=VECTOR('',#26921,3.07349999999996);
#7170=VECTOR('',#26926,3.07349999999996);
#7171=VECTOR('',#26931,3.07349999999996);
#7172=VECTOR('',#26934,3.07349999999996);
#7173=VECTOR('',#26937,3.07349999999996);
#7174=VECTOR('',#26940,3.07349999999996);
#7175=VECTOR('',#26943,3.07349999999996);
#7176=VECTOR('',#26946,3.07349999999996);
#7177=VECTOR('',#26949,3.07349999999996);
#7178=VECTOR('',#26952,3.07349999999996);
#7179=VECTOR('',#26955,3.07349999999996);
#7180=VECTOR('',#26958,3.07349999999996);
#7181=VECTOR('',#26961,3.07349999999996);
#7182=VECTOR('',#26964,3.07349999999996);
#7183=VECTOR('',#26967,3.07349999999996);
#7184=VECTOR('',#26970,3.07349999999996);
#7185=VECTOR('',#26973,3.07349999999996);
#7186=VECTOR('',#26976,3.07349999999996);
#7187=VECTOR('',#26979,3.07349999999996);
#7188=VECTOR('',#26982,3.07349999999996);
#7189=VECTOR('',#26985,3.07349999999996);
#7190=VECTOR('',#26990,3.0735);
#7191=VECTOR('',#26995,3.0735);
#7192=VECTOR('',#26998,3.0735);
#7193=VECTOR('',#27001,3.0735);
#7194=VECTOR('',#27004,3.0735);
#7195=VECTOR('',#27007,3.0735);
#7196=VECTOR('',#27010,3.0735);
#7197=VECTOR('',#27013,3.0735);
#7198=VECTOR('',#27016,3.0735);
#7199=VECTOR('',#27019,3.0735);
#7200=VECTOR('',#27022,3.0735);
#7201=VECTOR('',#27025,3.0735);
#7202=VECTOR('',#27028,3.0735);
#7203=VECTOR('',#27031,3.0735);
#7204=VECTOR('',#27034,3.0735);
#7205=VECTOR('',#27037,3.0735);
#7206=VECTOR('',#27040,3.0735);
#7207=VECTOR('',#27043,3.0735);
#7208=VECTOR('',#27046,3.0735);
#7209=VECTOR('',#27049,3.0735);
#7210=VECTOR('',#27054,3.0735);
#7211=VECTOR('',#27059,3.0735);
#7212=VECTOR('',#27062,3.0735);
#7213=VECTOR('',#27065,3.0735);
#7214=VECTOR('',#27068,3.0735);
#7215=VECTOR('',#27071,3.0735);
#7216=VECTOR('',#27074,3.0735);
#7217=VECTOR('',#27077,3.0735);
#7218=VECTOR('',#27080,3.0735);
#7219=VECTOR('',#27083,3.0735);
#7220=VECTOR('',#27086,3.0735);
#7221=VECTOR('',#27089,3.0735);
#7222=VECTOR('',#27092,3.0735);
#7223=VECTOR('',#27095,3.0735);
#7224=VECTOR('',#27098,3.0735);
#7225=VECTOR('',#27101,3.0735);
#7226=VECTOR('',#27104,3.0735);
#7227=VECTOR('',#27107,3.0735);
#7228=VECTOR('',#27110,3.0735);
#7229=VECTOR('',#27113,3.0735);
#7230=VECTOR('',#27120,10.);
#7231=VECTOR('',#27121,10.);
#7232=VECTOR('',#27122,10.);
#7233=VECTOR('',#27123,10.);
#7234=VECTOR('',#27148,10.);
#7235=VECTOR('',#27149,10.);
#7236=VECTOR('',#27150,10.);
#7237=VECTOR('',#27153,10.);
#7238=VECTOR('',#27154,10.);
#7239=VECTOR('',#27157,10.);
#7240=VECTOR('',#27158,10.);
#7241=VECTOR('',#27161,10.);
#7242=VECTOR('',#27168,3.);
#7243=VECTOR('',#27173,3.);
#7244=VECTOR('',#27176,3.);
#7245=VECTOR('',#27179,3.);
#7246=VECTOR('',#27182,3.);
#7247=VECTOR('',#27185,3.);
#7248=VECTOR('',#27188,3.);
#7249=VECTOR('',#27191,3.);
#7250=VECTOR('',#27194,3.);
#7251=VECTOR('',#27197,3.);
#7252=VECTOR('',#27200,3.);
#7253=VECTOR('',#27203,3.);
#7254=VECTOR('',#27206,3.);
#7255=VECTOR('',#27209,3.);
#7256=VECTOR('',#27212,3.);
#7257=VECTOR('',#27215,3.);
#7258=VECTOR('',#27218,3.);
#7259=VECTOR('',#27221,3.);
#7260=VECTOR('',#27224,3.);
#7261=VECTOR('',#27227,3.);
#7262=VECTOR('',#27230,3.);
#7263=VECTOR('',#27233,3.);
#7264=VECTOR('',#27236,3.);
#7265=VECTOR('',#27239,3.);
#7266=VECTOR('',#27242,3.);
#7267=VECTOR('',#27245,3.);
#7268=VECTOR('',#27248,3.);
#7269=VECTOR('',#27251,3.);
#7270=VECTOR('',#27254,3.);
#7271=VECTOR('',#27257,3.);
#7272=VECTOR('',#27260,3.);
#7273=VECTOR('',#27263,3.);
#7274=VECTOR('',#27266,3.);
#7275=VECTOR('',#27269,3.);
#7276=VECTOR('',#27272,3.);
#7277=VECTOR('',#27275,3.);
#7278=VECTOR('',#27278,3.);
#7279=VECTOR('',#27281,3.);
#7280=VECTOR('',#27284,3.);
#7281=VECTOR('',#27287,3.);
#7282=VECTOR('',#27290,3.);
#7283=VECTOR('',#27293,3.);
#7284=VECTOR('',#27296,3.);
#7285=VECTOR('',#27299,3.);
#7286=VECTOR('',#27302,3.);
#7287=VECTOR('',#27305,3.);
#7288=VECTOR('',#27308,3.);
#7289=VECTOR('',#27311,3.);
#7290=VECTOR('',#27314,3.);
#7291=VECTOR('',#27317,2.37175);
#7292=VECTOR('',#27322,2.37175);
#7293=VECTOR('',#27325,2.37175);
#7294=VECTOR('',#27328,2.37175);
#7295=VECTOR('',#27331,2.37175);
#7296=VECTOR('',#27334,2.37175);
#7297=VECTOR('',#27337,2.37175);
#7298=VECTOR('',#27340,2.37175);
#7299=VECTOR('',#27343,2.37175);
#7300=VECTOR('',#27346,2.37175);
#7301=VECTOR('',#27349,2.37175);
#7302=VECTOR('',#27352,2.37175);
#7303=VECTOR('',#27355,2.37175);
#7304=VECTOR('',#27358,2.37175);
#7305=VECTOR('',#27361,2.37175);
#7306=VECTOR('',#27364,2.37175);
#7307=VECTOR('',#27367,2.37175);
#7308=VECTOR('',#27370,2.37175);
#7309=VECTOR('',#27373,2.37175);
#7310=VECTOR('',#27376,2.37175);
#7311=VECTOR('',#27379,2.37175);
#7312=VECTOR('',#27382,2.37175);
#7313=VECTOR('',#27385,2.37175);
#7314=VECTOR('',#27388,2.37175);
#7315=VECTOR('',#27391,2.37175);
#7316=VECTOR('',#27394,2.37175);
#7317=VECTOR('',#27397,2.37175);
#7318=VECTOR('',#27400,2.37175);
#7319=VECTOR('',#27403,2.37175);
#7320=VECTOR('',#27406,2.37175);
#7321=VECTOR('',#27409,2.37175);
#7322=VECTOR('',#27412,2.37175);
#7323=VECTOR('',#27415,2.37175);
#7324=VECTOR('',#27418,2.37175);
#7325=VECTOR('',#27421,2.37175);
#7326=VECTOR('',#27424,2.37175);
#7327=VECTOR('',#27427,2.37175);
#7328=VECTOR('',#27430,2.37175);
#7329=VECTOR('',#27433,2.37175);
#7330=VECTOR('',#27436,2.37175);
#7331=VECTOR('',#27439,2.37175);
#7332=VECTOR('',#27442,2.37175);
#7333=VECTOR('',#27445,2.37175);
#7334=VECTOR('',#27448,2.37175);
#7335=VECTOR('',#27451,2.37175);
#7336=VECTOR('',#27454,2.37175);
#7337=VECTOR('',#27457,2.37175);
#7338=VECTOR('',#27460,2.37175);
#7339=VECTOR('',#27463,2.37175);
#7340=VECTOR('',#27468,2.5);
#7341=VECTOR('',#27479,10.);
#7342=VECTOR('',#27480,10.);
#7343=VECTOR('',#27481,10.);
#7344=VECTOR('',#27482,10.);
#7345=VECTOR('',#27485,10.);
#7346=VECTOR('',#27486,10.);
#7347=VECTOR('',#27487,10.);
#7348=VECTOR('',#27490,10.);
#7349=VECTOR('',#27491,10.);
#7350=VECTOR('',#27492,10.);
#7351=VECTOR('',#27495,10.);
#7352=VECTOR('',#27496,10.);
#7353=VECTOR('',#27497,10.);
#7354=VECTOR('',#27500,10.);
#7355=VECTOR('',#27501,10.);
#7356=VECTOR('',#27502,10.);
#7357=VECTOR('',#27505,10.);
#7358=VECTOR('',#27506,10.);
#7359=VECTOR('',#27515,5.);
#7360=VECTOR('',#27528,3.5);
#7361=VECTOR('',#27535,6.);
#7362=VECTOR('',#27548,3.5);
#7363=VECTOR('',#27555,7.);
#7364=CIRCLE('',#22044,3.5);
#7365=CIRCLE('',#22045,3.5);
#7366=CIRCLE('',#22047,3.5);
#7367=CIRCLE('',#22048,3.5);
#7368=CIRCLE('',#22050,3.5);
#7369=CIRCLE('',#22051,3.5);
#7370=CIRCLE('',#22053,3.5);
#7371=CIRCLE('',#22054,3.5);
#7372=CIRCLE('',#22056,3.5);
#7373=CIRCLE('',#22057,3.5);
#7374=CIRCLE('',#22059,3.5);
#7375=CIRCLE('',#22060,3.5);
#7376=CIRCLE('',#22084,3.5175);
#7377=CIRCLE('',#22092,3.5175);
#7378=CIRCLE('',#22094,3.5175);
#7379=CIRCLE('',#22102,3.5175);
#7380=CIRCLE('',#22104,3.5175);
#7381=CIRCLE('',#22112,3.5175);
#7382=CIRCLE('',#22114,3.5175);
#7383=CIRCLE('',#22122,3.5175);
#7384=CIRCLE('',#22124,4.0735);
#7385=CIRCLE('',#22132,4.07350000000001);
#7386=CIRCLE('',#22134,4.0735);
#7387=CIRCLE('',#22142,4.0735);
#7388=CIRCLE('',#22144,4.0735);
#7389=CIRCLE('',#22152,4.0735);
#7390=CIRCLE('',#22154,4.0735);
#7391=CIRCLE('',#22162,4.07350000000001);
#7392=CIRCLE('',#22179,3.942);
#7393=CIRCLE('',#22204,3.37175);
#7394=CIRCLE('',#22229,3.942);
#7395=CIRCLE('',#22230,3.);
#7396=CIRCLE('',#22232,3.37175);
#7397=CIRCLE('',#22242,6.5);
#7398=CIRCLE('',#22244,6.5);
#7399=CIRCLE('',#22249,4.5);
#7400=CIRCLE('',#22250,4.5);
#7401=CIRCLE('',#22252,9.);
#7402=CIRCLE('',#22253,9.);
#7403=CIRCLE('',#22299,4.51775);
#7404=CIRCLE('',#22300,4.51775);
#7405=CIRCLE('',#22301,4.51775);
#7406=CIRCLE('',#22326,4.51775);
#7407=CIRCLE('',#22328,5.0736);
#7408=CIRCLE('',#22353,5.0736);
#7409=CIRCLE('',#22355,4.51775);
#7410=CIRCLE('',#22356,4.51775);
#7411=CIRCLE('',#22357,4.51775);
#7412=CIRCLE('',#22397,4.51775);
#7413=CIRCLE('',#22399,5.07359999999999);
#7414=CIRCLE('',#22439,5.0736);
#7415=CIRCLE('',#22444,4.);
#7416=CIRCLE('',#22449,4.);
#7417=CIRCLE('',#22451,1.);
#7418=CIRCLE('',#22452,1.);
#7419=CIRCLE('',#22455,1.);
#7420=CIRCLE('',#22456,1.);
#7421=CIRCLE('',#22457,1.);
#7422=CIRCLE('',#22458,1.);
#7423=CIRCLE('',#22459,1.);
#7424=CIRCLE('',#22460,1.);
#7425=CIRCLE('',#22461,1.);
#7426=CIRCLE('',#22462,1.);
#7427=CIRCLE('',#22463,1.);
#7428=CIRCLE('',#22464,1.);
#7429=CIRCLE('',#22465,1.);
#7430=CIRCLE('',#22466,1.);
#7431=CIRCLE('',#22467,1.);
#7432=CIRCLE('',#22468,1.);
#7433=CIRCLE('',#22469,1.);
#7434=CIRCLE('',#22470,1.);
#7435=CIRCLE('',#22471,1.);
#7436=CIRCLE('',#22472,1.);
#7437=CIRCLE('',#22473,1.);
#7438=CIRCLE('',#22474,1.);
#7439=CIRCLE('',#22475,1.);
#7440=CIRCLE('',#22476,1.);
#7441=CIRCLE('',#22477,1.);
#7442=CIRCLE('',#22478,1.);
#7443=CIRCLE('',#22479,1.);
#7444=CIRCLE('',#22480,1.);
#7445=CIRCLE('',#22481,1.);
#7446=CIRCLE('',#22482,1.);
#7447=CIRCLE('',#22483,1.);
#7448=CIRCLE('',#22484,1.);
#7449=CIRCLE('',#22485,1.);
#7450=CIRCLE('',#22486,1.);
#7451=CIRCLE('',#22487,1.);
#7452=CIRCLE('',#22488,1.);
#7453=CIRCLE('',#22489,1.);
#7454=CIRCLE('',#22490,3.);
#7455=CIRCLE('',#22491,3.);
#7456=CIRCLE('',#22492,3.);
#7457=CIRCLE('',#22493,3.);
#7458=CIRCLE('',#22495,1.);
#7459=CIRCLE('',#22498,1.);
#7460=CIRCLE('',#22501,1.);
#7461=CIRCLE('',#22504,1.);
#7462=CIRCLE('',#22507,1.);
#7463=CIRCLE('',#22509,1.);
#7464=CIRCLE('',#22512,1.);
#7465=CIRCLE('',#22514,1.);
#7466=CIRCLE('',#22517,1.);
#7467=CIRCLE('',#22519,1.);
#7468=CIRCLE('',#22522,1.);
#7469=CIRCLE('',#22525,1.);
#7470=CIRCLE('',#22528,1.);
#7471=CIRCLE('',#22531,1.);
#7472=CIRCLE('',#22533,1.);
#7473=CIRCLE('',#22536,1.);
#7474=CIRCLE('',#22538,1.);
#7475=CIRCLE('',#22541,1.);
#7476=CIRCLE('',#22543,1.);
#7477=CIRCLE('',#22546,1.);
#7478=CIRCLE('',#22549,1.);
#7479=CIRCLE('',#22552,1.);
#7480=CIRCLE('',#22555,1.);
#7481=CIRCLE('',#22557,1.);
#7482=CIRCLE('',#22560,1.);
#7483=CIRCLE('',#22562,1.);
#7484=CIRCLE('',#22565,1.);
#7485=CIRCLE('',#22567,1.);
#7486=CIRCLE('',#22570,1.);
#7487=CIRCLE('',#22573,1.);
#7488=CIRCLE('',#22576,1.);
#7489=CIRCLE('',#22579,1.);
#7490=CIRCLE('',#22581,1.);
#7491=CIRCLE('',#22584,1.);
#7492=CIRCLE('',#22586,1.);
#7493=CIRCLE('',#22588,3.);
#7494=CIRCLE('',#22590,3.);
#7495=CIRCLE('',#22593,3.);
#7496=CIRCLE('',#22595,3.);
#7497=CIRCLE('',#22611,8.5);
#7498=CIRCLE('',#22612,5.5);
#7499=CIRCLE('',#22614,8.5);
#7500=CIRCLE('',#22616,5.5);
#7501=CIRCLE('',#22618,4.5);
#7502=CIRCLE('',#22619,4.5);
#7503=CIRCLE('',#22621,4.5);
#7504=CIRCLE('',#22622,4.5);
#7505=CIRCLE('',#22624,4.5);
#7506=CIRCLE('',#22625,4.5);
#7507=CIRCLE('',#22627,4.5);
#7508=CIRCLE('',#22628,4.5);
#7509=CIRCLE('',#22637,4.942);
#7510=CIRCLE('',#22657,4.372);
#7511=CIRCLE('',#22677,4.942);
#7512=CIRCLE('',#22678,4.);
#7513=CIRCLE('',#22680,4.372);
#7514=CIRCLE('',#22690,8.);
#7515=CIRCLE('',#22692,8.);
#7516=CIRCLE('',#22697,30.);
#7517=CIRCLE('',#22698,30.);
#7518=CIRCLE('',#22703,2.5175);
#7519=CIRCLE('',#22704,2.5175);
#7520=CIRCLE('',#22705,2.5175);
#7521=CIRCLE('',#22713,2.5175);
#7522=CIRCLE('',#22715,3.0735);
#7523=CIRCLE('',#22723,3.0735);
#7524=CIRCLE('',#22725,2.5175);
#7525=CIRCLE('',#22726,2.5175);
#7526=CIRCLE('',#22727,2.5175);
#7527=CIRCLE('',#22735,2.5175);
#7528=CIRCLE('',#22737,3.0735);
#7529=CIRCLE('',#22745,3.0735);
#7530=CIRCLE('',#22747,2.5175);
#7531=CIRCLE('',#22748,2.5175);
#7532=CIRCLE('',#22749,2.5175);
#7533=CIRCLE('',#22757,2.5175);
#7534=CIRCLE('',#22759,3.0735);
#7535=CIRCLE('',#22767,3.0735);
#7536=CIRCLE('',#22781,5.65685424949238);
#7537=CIRCLE('',#22782,6.);
#7538=CIRCLE('',#22784,30.);
#7539=CIRCLE('',#22785,30.);
#7540=CIRCLE('',#22790,3.5);
#7541=CIRCLE('',#22791,3.5);
#7542=CIRCLE('',#22793,3.5);
#7543=CIRCLE('',#22794,3.5);
#7544=CIRCLE('',#22796,3.5);
#7545=CIRCLE('',#22797,3.5);
#7546=CIRCLE('',#22799,5.65685424949238);
#7547=CIRCLE('',#22800,6.);
#7548=CIRCLE('',#22801,5.5);
#7549=CIRCLE('',#22803,5.5);
#7550=CIRCLE('',#22805,22.);
#7551=CIRCLE('',#22806,22.);
#7552=CIRCLE('',#22811,4.942);
#7553=CIRCLE('',#22872,4.372);
#7554=CIRCLE('',#22933,4.372);
#7555=CIRCLE('',#22935,4.942);
#7556=CIRCLE('',#22938,5.);
#7557=CIRCLE('',#22946,5.);
#7558=CIRCLE('',#22949,6.);
#7559=CIRCLE('',#22952,4.51775);
#7560=CIRCLE('',#22960,4.51775);
#7561=CIRCLE('',#22962,5.0736);
#7562=CIRCLE('',#22970,5.0736);
#7563=CIRCLE('',#22983,5.5);
#7564=CIRCLE('',#22984,5.5);
#7565=CIRCLE('',#22986,11.);
#7566=CIRCLE('',#22987,11.);
#7567=CIRCLE('',#22992,2.942);
#7568=CIRCLE('',#23008,2.37175);
#7569=CIRCLE('',#23024,2.942);
#7570=CIRCLE('',#23025,2.);
#7571=CIRCLE('',#23027,2.37175);
#7572=CIRCLE('',#23037,5.);
#7573=CIRCLE('',#23039,5.);
#7574=CIRCLE('',#23044,2.5175);
#7575=CIRCLE('',#23064,2.5175);
#7576=CIRCLE('',#23066,2.5175);
#7577=CIRCLE('',#23086,2.5175);
#7578=CIRCLE('',#23088,2.5175);
#7579=CIRCLE('',#23108,2.5175);
#7580=CIRCLE('',#23110,2.5175);
#7581=CIRCLE('',#23130,2.5175);
#7582=CIRCLE('',#23132,2.5175);
#7583=CIRCLE('',#23152,2.5175);
#7584=CIRCLE('',#23154,2.5175);
#7585=CIRCLE('',#23174,2.5175);
#7586=CIRCLE('',#23176,3.0735);
#7587=CIRCLE('',#23196,3.0735);
#7588=CIRCLE('',#23198,3.07349999999999);
#7589=CIRCLE('',#23218,3.0735);
#7590=CIRCLE('',#23220,3.07349999999996);
#7591=CIRCLE('',#23240,3.07349999999996);
#7592=CIRCLE('',#23242,3.07349999999996);
#7593=CIRCLE('',#23262,3.07349999999996);
#7594=CIRCLE('',#23264,3.07349999999999);
#7595=CIRCLE('',#23284,3.0735);
#7596=CIRCLE('',#23286,3.0735);
#7597=CIRCLE('',#23306,3.0735);
#7598=CIRCLE('',#23327,2.942);
#7599=CIRCLE('',#23377,2.37175);
#7600=CIRCLE('',#23427,2.942);
#7601=CIRCLE('',#23428,2.);
#7602=CIRCLE('',#23430,2.37175);
#7603=CIRCLE('',#23440,5.);
#7604=CIRCLE('',#23442,5.);
#7605=CIRCLE('',#23447,3.5);
#7606=CIRCLE('',#23448,3.5);
#7607=CIRCLE('',#23450,6.);
#7608=CIRCLE('',#23451,6.);
#7609=CIRCLE('',#23456,3.5);
#7610=CIRCLE('',#23457,3.5);
#7611=CIRCLE('',#23459,7.);
#7612=CIRCLE('',#23460,7.);
#7613=VERTEX_POINT('',#27644);
#7614=VERTEX_POINT('',#27646);
#7615=VERTEX_POINT('',#27650);
#7616=VERTEX_POINT('',#27652);
#7617=VERTEX_POINT('',#27656);
#7618=VERTEX_POINT('',#27658);
#7619=VERTEX_POINT('',#27662);
#7620=VERTEX_POINT('',#27664);
#7621=VERTEX_POINT('',#27668);
#7622=VERTEX_POINT('',#27670);
#7623=VERTEX_POINT('',#27674);
#7624=VERTEX_POINT('',#27676);
#7625=VERTEX_POINT('',#27680);
#7626=VERTEX_POINT('',#27681);
#7627=VERTEX_POINT('',#27683);
#7628=VERTEX_POINT('',#27685);
#7629=VERTEX_POINT('',#27689);
#7630=VERTEX_POINT('',#27691);
#7631=VERTEX_POINT('',#27695);
#7632=VERTEX_POINT('',#27697);
#7633=VERTEX_POINT('',#27704);
#7634=VERTEX_POINT('',#27705);
#7635=VERTEX_POINT('',#27707);
#7636=VERTEX_POINT('',#27709);
#7637=VERTEX_POINT('',#27713);
#7638=VERTEX_POINT('',#27715);
#7639=VERTEX_POINT('',#27719);
#7640=VERTEX_POINT('',#27721);
#7641=VERTEX_POINT('',#27731);
#7642=VERTEX_POINT('',#27732);
#7643=VERTEX_POINT('',#27734);
#7644=VERTEX_POINT('',#27736);
#7645=VERTEX_POINT('',#27740);
#7646=VERTEX_POINT('',#27742);
#7647=VERTEX_POINT('',#27746);
#7648=VERTEX_POINT('',#27748);
#7649=VERTEX_POINT('',#27755);
#7650=VERTEX_POINT('',#27756);
#7651=VERTEX_POINT('',#27758);
#7652=VERTEX_POINT('',#27760);
#7653=VERTEX_POINT('',#27764);
#7654=VERTEX_POINT('',#27766);
#7655=VERTEX_POINT('',#27770);
#7656=VERTEX_POINT('',#27772);
#7657=VERTEX_POINT('',#27782);
#7658=VERTEX_POINT('',#27783);
#7659=VERTEX_POINT('',#27785);
#7660=VERTEX_POINT('',#27790);
#7661=VERTEX_POINT('',#27803);
#7662=VERTEX_POINT('',#27804);
#7663=VERTEX_POINT('',#27854);
#7664=VERTEX_POINT('',#27855);
#7665=VERTEX_POINT('',#27905);
#7666=VERTEX_POINT('',#27906);
#7667=VERTEX_POINT('',#27953);
#7668=VERTEX_POINT('',#27954);
#7669=VERTEX_POINT('',#28004);
#7670=VERTEX_POINT('',#28005);
#7671=VERTEX_POINT('',#28055);
#7672=VERTEX_POINT('',#28056);
#7673=VERTEX_POINT('',#28103);
#7674=VERTEX_POINT('',#28104);
#7675=VERTEX_POINT('',#28106);
#7676=VERTEX_POINT('',#28120);
#7677=VERTEX_POINT('',#28142);
#7678=VERTEX_POINT('',#28143);
#7679=VERTEX_POINT('',#28145);
#7680=VERTEX_POINT('',#28150);
#7681=VERTEX_POINT('',#28163);
#7682=VERTEX_POINT('',#28164);
#7683=VERTEX_POINT('',#28214);
#7684=VERTEX_POINT('',#28215);
#7685=VERTEX_POINT('',#28265);
#7686=VERTEX_POINT('',#28266);
#7687=VERTEX_POINT('',#28313);
#7688=VERTEX_POINT('',#28314);
#7689=VERTEX_POINT('',#28364);
#7690=VERTEX_POINT('',#28365);
#7691=VERTEX_POINT('',#28415);
#7692=VERTEX_POINT('',#28416);
#7693=VERTEX_POINT('',#28463);
#7694=VERTEX_POINT('',#28464);
#7695=VERTEX_POINT('',#28466);
#7696=VERTEX_POINT('',#28480);
#7697=VERTEX_POINT('',#28502);
#7698=VERTEX_POINT('',#28503);
#7699=VERTEX_POINT('',#28505);
#7700=VERTEX_POINT('',#28510);
#7701=VERTEX_POINT('',#28523);
#7702=VERTEX_POINT('',#28524);
#7703=VERTEX_POINT('',#28574);
#7704=VERTEX_POINT('',#28575);
#7705=VERTEX_POINT('',#28625);
#7706=VERTEX_POINT('',#28626);
#7707=VERTEX_POINT('',#28673);
#7708=VERTEX_POINT('',#28674);
#7709=VERTEX_POINT('',#28724);
#7710=VERTEX_POINT('',#28725);
#7711=VERTEX_POINT('',#28775);
#7712=VERTEX_POINT('',#28776);
#7713=VERTEX_POINT('',#28823);
#7714=VERTEX_POINT('',#28824);
#7715=VERTEX_POINT('',#28826);
#7716=VERTEX_POINT('',#28840);
#7717=VERTEX_POINT('',#28862);
#7718=VERTEX_POINT('',#28863);
#7719=VERTEX_POINT('',#28865);
#7720=VERTEX_POINT('',#28870);
#7721=VERTEX_POINT('',#28883);
#7722=VERTEX_POINT('',#28884);
#7723=VERTEX_POINT('',#28934);
#7724=VERTEX_POINT('',#28935);
#7725=VERTEX_POINT('',#28985);
#7726=VERTEX_POINT('',#28986);
#7727=VERTEX_POINT('',#29033);
#7728=VERTEX_POINT('',#29034);
#7729=VERTEX_POINT('',#29084);
#7730=VERTEX_POINT('',#29085);
#7731=VERTEX_POINT('',#29135);
#7732=VERTEX_POINT('',#29136);
#7733=VERTEX_POINT('',#29183);
#7734=VERTEX_POINT('',#29184);
#7735=VERTEX_POINT('',#29186);
#7736=VERTEX_POINT('',#29200);
#7737=VERTEX_POINT('',#29222);
#7738=VERTEX_POINT('',#29223);
#7739=VERTEX_POINT('',#29225);
#7740=VERTEX_POINT('',#29234);
#7741=VERTEX_POINT('',#29246);
#7742=VERTEX_POINT('',#29247);
#7743=VERTEX_POINT('',#29270);
#7744=VERTEX_POINT('',#29271);
#7745=VERTEX_POINT('',#29295);
#7746=VERTEX_POINT('',#29296);
#7747=VERTEX_POINT('',#29320);
#7748=VERTEX_POINT('',#29321);
#7749=VERTEX_POINT('',#29344);
#7750=VERTEX_POINT('',#29345);
#7751=VERTEX_POINT('',#29369);
#7752=VERTEX_POINT('',#29370);
#7753=VERTEX_POINT('',#29394);
#7754=VERTEX_POINT('',#29395);
#7755=VERTEX_POINT('',#29397);
#7756=VERTEX_POINT('',#29403);
#7757=VERTEX_POINT('',#29411);
#7758=VERTEX_POINT('',#29412);
#7759=VERTEX_POINT('',#29414);
#7760=VERTEX_POINT('',#29423);
#7761=VERTEX_POINT('',#29435);
#7762=VERTEX_POINT('',#29436);
#7763=VERTEX_POINT('',#29459);
#7764=VERTEX_POINT('',#29460);
#7765=VERTEX_POINT('',#29484);
#7766=VERTEX_POINT('',#29485);
#7767=VERTEX_POINT('',#29509);
#7768=VERTEX_POINT('',#29510);
#7769=VERTEX_POINT('',#29533);
#7770=VERTEX_POINT('',#29534);
#7771=VERTEX_POINT('',#29558);
#7772=VERTEX_POINT('',#29559);
#7773=VERTEX_POINT('',#29583);
#7774=VERTEX_POINT('',#29584);
#7775=VERTEX_POINT('',#29586);
#7776=VERTEX_POINT('',#29592);
#7777=VERTEX_POINT('',#29600);
#7778=VERTEX_POINT('',#29601);
#7779=VERTEX_POINT('',#29603);
#7780=VERTEX_POINT('',#29612);
#7781=VERTEX_POINT('',#29624);
#7782=VERTEX_POINT('',#29625);
#7783=VERTEX_POINT('',#29648);
#7784=VERTEX_POINT('',#29649);
#7785=VERTEX_POINT('',#29673);
#7786=VERTEX_POINT('',#29674);
#7787=VERTEX_POINT('',#29698);
#7788=VERTEX_POINT('',#29699);
#7789=VERTEX_POINT('',#29722);
#7790=VERTEX_POINT('',#29723);
#7791=VERTEX_POINT('',#29747);
#7792=VERTEX_POINT('',#29748);
#7793=VERTEX_POINT('',#29772);
#7794=VERTEX_POINT('',#29773);
#7795=VERTEX_POINT('',#29775);
#7796=VERTEX_POINT('',#29781);
#7797=VERTEX_POINT('',#29789);
#7798=VERTEX_POINT('',#29790);
#7799=VERTEX_POINT('',#29792);
#7800=VERTEX_POINT('',#29801);
#7801=VERTEX_POINT('',#29813);
#7802=VERTEX_POINT('',#29814);
#7803=VERTEX_POINT('',#29837);
#7804=VERTEX_POINT('',#29838);
#7805=VERTEX_POINT('',#29862);
#7806=VERTEX_POINT('',#29863);
#7807=VERTEX_POINT('',#29887);
#7808=VERTEX_POINT('',#29888);
#7809=VERTEX_POINT('',#29911);
#7810=VERTEX_POINT('',#29912);
#7811=VERTEX_POINT('',#29936);
#7812=VERTEX_POINT('',#29937);
#7813=VERTEX_POINT('',#29961);
#7814=VERTEX_POINT('',#29962);
#7815=VERTEX_POINT('',#29964);
#7816=VERTEX_POINT('',#29970);
#7817=VERTEX_POINT('',#30880);
#7818=VERTEX_POINT('',#30881);
#7819=VERTEX_POINT('',#30883);
#7820=VERTEX_POINT('',#30885);
#7821=VERTEX_POINT('',#33599);
#7822=VERTEX_POINT('',#33600);
#7823=VERTEX_POINT('',#33605);
#7824=VERTEX_POINT('',#33609);
#7825=VERTEX_POINT('',#33617);
#7826=VERTEX_POINT('',#33618);
#7827=VERTEX_POINT('',#33620);
#7828=VERTEX_POINT('',#33631);
#7829=VERTEX_POINT('',#33641);
#7830=VERTEX_POINT('',#33642);
#7831=VERTEX_POINT('',#33689);
#7832=VERTEX_POINT('',#33690);
#7833=VERTEX_POINT('',#33737);
#7834=VERTEX_POINT('',#33738);
#7835=VERTEX_POINT('',#33785);
#7836=VERTEX_POINT('',#33786);
#7837=VERTEX_POINT('',#33839);
#7838=VERTEX_POINT('',#33840);
#7839=VERTEX_POINT('',#33887);
#7840=VERTEX_POINT('',#33888);
#7841=VERTEX_POINT('',#33935);
#7842=VERTEX_POINT('',#33936);
#7843=VERTEX_POINT('',#33989);
#7844=VERTEX_POINT('',#33990);
#7845=VERTEX_POINT('',#34037);
#7846=VERTEX_POINT('',#34038);
#7847=VERTEX_POINT('',#34085);
#7848=VERTEX_POINT('',#34086);
#7849=VERTEX_POINT('',#34139);
#7850=VERTEX_POINT('',#34140);
#7851=VERTEX_POINT('',#34187);
#7852=VERTEX_POINT('',#34188);
#7853=VERTEX_POINT('',#34235);
#7854=VERTEX_POINT('',#34236);
#7855=VERTEX_POINT('',#34283);
#7856=VERTEX_POINT('',#34284);
#7857=VERTEX_POINT('',#34337);
#7858=VERTEX_POINT('',#34338);
#7859=VERTEX_POINT('',#34385);
#7860=VERTEX_POINT('',#34386);
#7861=VERTEX_POINT('',#34433);
#7862=VERTEX_POINT('',#34434);
#7863=VERTEX_POINT('',#34487);
#7864=VERTEX_POINT('',#34488);
#7865=VERTEX_POINT('',#34535);
#7866=VERTEX_POINT('',#34536);
#7867=VERTEX_POINT('',#34583);
#7868=VERTEX_POINT('',#34584);
#7869=VERTEX_POINT('',#34631);
#7870=VERTEX_POINT('',#34632);
#7871=VERTEX_POINT('',#34685);
#7872=VERTEX_POINT('',#34686);
#7873=VERTEX_POINT('',#34733);
#7874=VERTEX_POINT('',#34734);
#7875=VERTEX_POINT('',#34781);
#7876=VERTEX_POINT('',#34782);
#7877=VERTEX_POINT('',#34784);
#7878=VERTEX_POINT('',#34795);
#7879=VERTEX_POINT('',#34806);
#7880=VERTEX_POINT('',#34807);
#7881=VERTEX_POINT('',#34831);
#7882=VERTEX_POINT('',#34832);
#7883=VERTEX_POINT('',#34855);
#7884=VERTEX_POINT('',#34856);
#7885=VERTEX_POINT('',#34880);
#7886=VERTEX_POINT('',#34881);
#7887=VERTEX_POINT('',#34905);
#7888=VERTEX_POINT('',#34906);
#7889=VERTEX_POINT('',#34929);
#7890=VERTEX_POINT('',#34930);
#7891=VERTEX_POINT('',#34953);
#7892=VERTEX_POINT('',#34954);
#7893=VERTEX_POINT('',#34978);
#7894=VERTEX_POINT('',#34979);
#7895=VERTEX_POINT('',#35003);
#7896=VERTEX_POINT('',#35004);
#7897=VERTEX_POINT('',#35027);
#7898=VERTEX_POINT('',#35028);
#7899=VERTEX_POINT('',#35052);
#7900=VERTEX_POINT('',#35053);
#7901=VERTEX_POINT('',#35077);
#7902=VERTEX_POINT('',#35078);
#7903=VERTEX_POINT('',#35101);
#7904=VERTEX_POINT('',#35102);
#7905=VERTEX_POINT('',#35125);
#7906=VERTEX_POINT('',#35126);
#7907=VERTEX_POINT('',#35150);
#7908=VERTEX_POINT('',#35151);
#7909=VERTEX_POINT('',#35175);
#7910=VERTEX_POINT('',#35176);
#7911=VERTEX_POINT('',#35199);
#7912=VERTEX_POINT('',#35200);
#7913=VERTEX_POINT('',#35224);
#7914=VERTEX_POINT('',#35225);
#7915=VERTEX_POINT('',#35249);
#7916=VERTEX_POINT('',#35250);
#7917=VERTEX_POINT('',#35273);
#7918=VERTEX_POINT('',#35274);
#7919=VERTEX_POINT('',#35298);
#7920=VERTEX_POINT('',#35299);
#7921=VERTEX_POINT('',#35323);
#7922=VERTEX_POINT('',#35324);
#7923=VERTEX_POINT('',#35347);
#7924=VERTEX_POINT('',#35348);
#7925=VERTEX_POINT('',#35371);
#7926=VERTEX_POINT('',#35604);
#7927=VERTEX_POINT('',#35672);
#7928=VERTEX_POINT('',#35705);
#7929=VERTEX_POINT('',#36340);
#7930=VERTEX_POINT('',#36466);
#7931=VERTEX_POINT('',#37238);
#7932=VERTEX_POINT('',#37239);
#7933=VERTEX_POINT('',#37241);
#7934=VERTEX_POINT('',#37243);
#7935=VERTEX_POINT('',#37247);
#7936=VERTEX_POINT('',#37249);
#7937=VERTEX_POINT('',#37253);
#7938=VERTEX_POINT('',#37255);
#7939=VERTEX_POINT('',#37259);
#7940=VERTEX_POINT('',#37261);
#7941=VERTEX_POINT('',#37265);
#7942=VERTEX_POINT('',#37267);
#7943=VERTEX_POINT('',#37275);
#7944=VERTEX_POINT('',#37278);
#7945=VERTEX_POINT('',#37285);
#7946=VERTEX_POINT('',#37287);
#7947=VERTEX_POINT('',#37291);
#7948=VERTEX_POINT('',#37293);
#7949=VERTEX_POINT('',#37341);
#7950=VERTEX_POINT('',#37342);
#7951=VERTEX_POINT('',#37344);
#7952=VERTEX_POINT('',#37352);
#7953=VERTEX_POINT('',#37354);
#7954=VERTEX_POINT('',#37357);
#7955=VERTEX_POINT('',#37376);
#7956=VERTEX_POINT('',#37377);
#7957=VERTEX_POINT('',#37466);
#7958=VERTEX_POINT('',#37467);
#7959=VERTEX_POINT('',#37553);
#7960=VERTEX_POINT('',#37554);
#7961=VERTEX_POINT('',#37640);
#7962=VERTEX_POINT('',#37641);
#7963=VERTEX_POINT('',#37727);
#7964=VERTEX_POINT('',#37728);
#7965=VERTEX_POINT('',#37817);
#7966=VERTEX_POINT('',#37818);
#7967=VERTEX_POINT('',#37904);
#7968=VERTEX_POINT('',#37905);
#7969=VERTEX_POINT('',#37991);
#7970=VERTEX_POINT('',#37992);
#7971=VERTEX_POINT('',#38081);
#7972=VERTEX_POINT('',#38082);
#7973=VERTEX_POINT('',#38168);
#7974=VERTEX_POINT('',#38169);
#7975=VERTEX_POINT('',#38255);
#7976=VERTEX_POINT('',#38256);
#7977=VERTEX_POINT('',#38342);
#7978=VERTEX_POINT('',#38343);
#7979=VERTEX_POINT('',#38432);
#7980=VERTEX_POINT('',#38433);
#7981=VERTEX_POINT('',#38519);
#7982=VERTEX_POINT('',#38520);
#7983=VERTEX_POINT('',#38606);
#7984=VERTEX_POINT('',#38607);
#7985=VERTEX_POINT('',#38693);
#7986=VERTEX_POINT('',#38694);
#7987=VERTEX_POINT('',#38783);
#7988=VERTEX_POINT('',#38784);
#7989=VERTEX_POINT('',#38870);
#7990=VERTEX_POINT('',#38871);
#7991=VERTEX_POINT('',#38957);
#7992=VERTEX_POINT('',#38958);
#7993=VERTEX_POINT('',#39047);
#7994=VERTEX_POINT('',#39048);
#7995=VERTEX_POINT('',#39134);
#7996=VERTEX_POINT('',#39135);
#7997=VERTEX_POINT('',#39221);
#7998=VERTEX_POINT('',#39222);
#7999=VERTEX_POINT('',#39308);
#8000=VERTEX_POINT('',#39309);
#8001=VERTEX_POINT('',#39398);
#8002=VERTEX_POINT('',#39399);
#8003=VERTEX_POINT('',#39401);
#8004=VERTEX_POINT('',#39427);
#8005=VERTEX_POINT('',#39467);
#8006=VERTEX_POINT('',#39468);
#8007=VERTEX_POINT('',#39470);
#8008=VERTEX_POINT('',#39483);
#8009=VERTEX_POINT('',#39500);
#8010=VERTEX_POINT('',#39501);
#8011=VERTEX_POINT('',#39537);
#8012=VERTEX_POINT('',#39538);
#8013=VERTEX_POINT('',#39575);
#8014=VERTEX_POINT('',#39576);
#8015=VERTEX_POINT('',#39611);
#8016=VERTEX_POINT('',#39612);
#8017=VERTEX_POINT('',#39649);
#8018=VERTEX_POINT('',#39650);
#8019=VERTEX_POINT('',#39687);
#8020=VERTEX_POINT('',#39688);
#8021=VERTEX_POINT('',#39723);
#8022=VERTEX_POINT('',#39724);
#8023=VERTEX_POINT('',#39761);
#8024=VERTEX_POINT('',#39762);
#8025=VERTEX_POINT('',#39799);
#8026=VERTEX_POINT('',#39800);
#8027=VERTEX_POINT('',#39835);
#8028=VERTEX_POINT('',#39836);
#8029=VERTEX_POINT('',#39873);
#8030=VERTEX_POINT('',#39874);
#8031=VERTEX_POINT('',#39910);
#8032=VERTEX_POINT('',#39911);
#8033=VERTEX_POINT('',#39947);
#8034=VERTEX_POINT('',#39948);
#8035=VERTEX_POINT('',#39985);
#8036=VERTEX_POINT('',#39986);
#8037=VERTEX_POINT('',#40021);
#8038=VERTEX_POINT('',#40022);
#8039=VERTEX_POINT('',#40059);
#8040=VERTEX_POINT('',#40060);
#8041=VERTEX_POINT('',#40097);
#8042=VERTEX_POINT('',#40098);
#8043=VERTEX_POINT('',#40133);
#8044=VERTEX_POINT('',#40134);
#8045=VERTEX_POINT('',#40171);
#8046=VERTEX_POINT('',#40172);
#8047=VERTEX_POINT('',#40209);
#8048=VERTEX_POINT('',#40210);
#8049=VERTEX_POINT('',#40245);
#8050=VERTEX_POINT('',#40246);
#8051=VERTEX_POINT('',#40283);
#8052=VERTEX_POINT('',#40284);
#8053=VERTEX_POINT('',#40320);
#8054=VERTEX_POINT('',#40321);
#8055=VERTEX_POINT('',#40357);
#8056=VERTEX_POINT('',#40358);
#8057=VERTEX_POINT('',#40360);
#8058=VERTEX_POINT('',#40367);
#8059=VERTEX_POINT('',#40377);
#8060=VERTEX_POINT('',#40378);
#8061=VERTEX_POINT('',#40380);
#8062=VERTEX_POINT('',#40388);
#8063=VERTEX_POINT('',#40390);
#8064=VERTEX_POINT('',#40393);
#8065=VERTEX_POINT('',#40412);
#8066=VERTEX_POINT('',#40413);
#8067=VERTEX_POINT('',#40502);
#8068=VERTEX_POINT('',#40503);
#8069=VERTEX_POINT('',#40589);
#8070=VERTEX_POINT('',#40590);
#8071=VERTEX_POINT('',#40676);
#8072=VERTEX_POINT('',#40677);
#8073=VERTEX_POINT('',#40763);
#8074=VERTEX_POINT('',#40764);
#8075=VERTEX_POINT('',#40850);
#8076=VERTEX_POINT('',#40851);
#8077=VERTEX_POINT('',#40940);
#8078=VERTEX_POINT('',#40941);
#8079=VERTEX_POINT('',#41027);
#8080=VERTEX_POINT('',#41028);
#8081=VERTEX_POINT('',#41114);
#8082=VERTEX_POINT('',#41115);
#8083=VERTEX_POINT('',#41201);
#8084=VERTEX_POINT('',#41202);
#8085=VERTEX_POINT('',#41288);
#8086=VERTEX_POINT('',#41289);
#8087=VERTEX_POINT('',#41378);
#8088=VERTEX_POINT('',#41379);
#8089=VERTEX_POINT('',#41465);
#8090=VERTEX_POINT('',#41466);
#8091=VERTEX_POINT('',#41552);
#8092=VERTEX_POINT('',#41553);
#8093=VERTEX_POINT('',#41639);
#8094=VERTEX_POINT('',#41640);
#8095=VERTEX_POINT('',#41726);
#8096=VERTEX_POINT('',#41727);
#8097=VERTEX_POINT('',#41813);
#8098=VERTEX_POINT('',#41814);
#8099=VERTEX_POINT('',#41900);
#8100=VERTEX_POINT('',#41901);
#8101=VERTEX_POINT('',#41987);
#8102=VERTEX_POINT('',#41988);
#8103=VERTEX_POINT('',#42062);
#8104=VERTEX_POINT('',#42063);
#8105=VERTEX_POINT('',#42110);
#8106=VERTEX_POINT('',#42111);
#8107=VERTEX_POINT('',#42167);
#8108=VERTEX_POINT('',#42168);
#8109=VERTEX_POINT('',#42254);
#8110=VERTEX_POINT('',#42255);
#8111=VERTEX_POINT('',#42341);
#8112=VERTEX_POINT('',#42342);
#8113=VERTEX_POINT('',#42428);
#8114=VERTEX_POINT('',#42429);
#8115=VERTEX_POINT('',#42515);
#8116=VERTEX_POINT('',#42516);
#8117=VERTEX_POINT('',#42602);
#8118=VERTEX_POINT('',#42603);
#8119=VERTEX_POINT('',#42692);
#8120=VERTEX_POINT('',#42693);
#8121=VERTEX_POINT('',#42779);
#8122=VERTEX_POINT('',#42780);
#8123=VERTEX_POINT('',#42866);
#8124=VERTEX_POINT('',#42867);
#8125=VERTEX_POINT('',#42953);
#8126=VERTEX_POINT('',#42954);
#8127=VERTEX_POINT('',#43040);
#8128=VERTEX_POINT('',#43041);
#8129=VERTEX_POINT('',#43130);
#8130=VERTEX_POINT('',#43131);
#8131=VERTEX_POINT('',#43217);
#8132=VERTEX_POINT('',#43218);
#8133=VERTEX_POINT('',#43304);
#8134=VERTEX_POINT('',#43305);
#8135=VERTEX_POINT('',#43391);
#8136=VERTEX_POINT('',#43392);
#8137=VERTEX_POINT('',#43478);
#8138=VERTEX_POINT('',#43479);
#8139=VERTEX_POINT('',#43568);
#8140=VERTEX_POINT('',#43569);
#8141=VERTEX_POINT('',#43655);
#8142=VERTEX_POINT('',#43656);
#8143=VERTEX_POINT('',#43658);
#8144=VERTEX_POINT('',#43684);
#8145=VERTEX_POINT('',#43724);
#8146=VERTEX_POINT('',#43725);
#8147=VERTEX_POINT('',#43727);
#8148=VERTEX_POINT('',#43740);
#8149=VERTEX_POINT('',#43757);
#8150=VERTEX_POINT('',#43758);
#8151=VERTEX_POINT('',#43794);
#8152=VERTEX_POINT('',#43795);
#8153=VERTEX_POINT('',#43832);
#8154=VERTEX_POINT('',#43833);
#8155=VERTEX_POINT('',#43868);
#8156=VERTEX_POINT('',#43869);
#8157=VERTEX_POINT('',#43906);
#8158=VERTEX_POINT('',#43907);
#8159=VERTEX_POINT('',#43943);
#8160=VERTEX_POINT('',#43944);
#8161=VERTEX_POINT('',#43980);
#8162=VERTEX_POINT('',#43981);
#8163=VERTEX_POINT('',#44018);
#8164=VERTEX_POINT('',#44019);
#8165=VERTEX_POINT('',#44054);
#8166=VERTEX_POINT('',#44055);
#8167=VERTEX_POINT('',#44092);
#8168=VERTEX_POINT('',#44093);
#8169=VERTEX_POINT('',#44129);
#8170=VERTEX_POINT('',#44130);
#8171=VERTEX_POINT('',#44166);
#8172=VERTEX_POINT('',#44167);
#8173=VERTEX_POINT('',#44204);
#8174=VERTEX_POINT('',#44205);
#8175=VERTEX_POINT('',#44240);
#8176=VERTEX_POINT('',#44241);
#8177=VERTEX_POINT('',#44278);
#8178=VERTEX_POINT('',#44279);
#8179=VERTEX_POINT('',#44315);
#8180=VERTEX_POINT('',#44316);
#8181=VERTEX_POINT('',#44352);
#8182=VERTEX_POINT('',#44353);
#8183=VERTEX_POINT('',#44390);
#8184=VERTEX_POINT('',#44391);
#8185=VERTEX_POINT('',#44426);
#8186=VERTEX_POINT('',#44427);
#8187=VERTEX_POINT('',#44453);
#8188=VERTEX_POINT('',#44454);
#8189=VERTEX_POINT('',#44477);
#8190=VERTEX_POINT('',#44478);
#8191=VERTEX_POINT('',#44510);
#8192=VERTEX_POINT('',#44511);
#8193=VERTEX_POINT('',#44548);
#8194=VERTEX_POINT('',#44549);
#8195=VERTEX_POINT('',#44584);
#8196=VERTEX_POINT('',#44585);
#8197=VERTEX_POINT('',#44622);
#8198=VERTEX_POINT('',#44623);
#8199=VERTEX_POINT('',#44658);
#8200=VERTEX_POINT('',#44659);
#8201=VERTEX_POINT('',#44696);
#8202=VERTEX_POINT('',#44697);
#8203=VERTEX_POINT('',#44734);
#8204=VERTEX_POINT('',#44735);
#8205=VERTEX_POINT('',#44770);
#8206=VERTEX_POINT('',#44771);
#8207=VERTEX_POINT('',#44808);
#8208=VERTEX_POINT('',#44809);
#8209=VERTEX_POINT('',#44844);
#8210=VERTEX_POINT('',#44845);
#8211=VERTEX_POINT('',#44882);
#8212=VERTEX_POINT('',#44883);
#8213=VERTEX_POINT('',#44920);
#8214=VERTEX_POINT('',#44921);
#8215=VERTEX_POINT('',#44956);
#8216=VERTEX_POINT('',#44957);
#8217=VERTEX_POINT('',#44994);
#8218=VERTEX_POINT('',#44995);
#8219=VERTEX_POINT('',#45030);
#8220=VERTEX_POINT('',#45031);
#8221=VERTEX_POINT('',#45068);
#8222=VERTEX_POINT('',#45069);
#8223=VERTEX_POINT('',#45106);
#8224=VERTEX_POINT('',#45107);
#8225=VERTEX_POINT('',#45142);
#8226=VERTEX_POINT('',#45143);
#8227=VERTEX_POINT('',#45145);
#8228=VERTEX_POINT('',#45152);
#8229=VERTEX_POINT('',#49679);
#8230=VERTEX_POINT('',#52804);
#8231=VERTEX_POINT('',#52807);
#8232=VERTEX_POINT('',#52808);
#8233=VERTEX_POINT('',#52810);
#8234=VERTEX_POINT('',#52812);
#8235=VERTEX_POINT('',#52816);
#8236=VERTEX_POINT('',#52818);
#8237=VERTEX_POINT('',#52822);
#8238=VERTEX_POINT('',#52824);
#8239=VERTEX_POINT('',#52826);
#8240=VERTEX_POINT('',#52828);
#8241=VERTEX_POINT('',#52830);
#8242=VERTEX_POINT('',#52832);
#8243=VERTEX_POINT('',#52834);
#8244=VERTEX_POINT('',#52836);
#8245=VERTEX_POINT('',#52838);
#8246=VERTEX_POINT('',#52840);
#8247=VERTEX_POINT('',#52842);
#8248=VERTEX_POINT('',#52844);
#8249=VERTEX_POINT('',#52846);
#8250=VERTEX_POINT('',#52848);
#8251=VERTEX_POINT('',#52850);
#8252=VERTEX_POINT('',#52852);
#8253=VERTEX_POINT('',#52854);
#8254=VERTEX_POINT('',#52856);
#8255=VERTEX_POINT('',#52858);
#8256=VERTEX_POINT('',#52860);
#8257=VERTEX_POINT('',#52862);
#8258=VERTEX_POINT('',#52864);
#8259=VERTEX_POINT('',#52866);
#8260=VERTEX_POINT('',#52868);
#8261=VERTEX_POINT('',#52870);
#8262=VERTEX_POINT('',#52872);
#8263=VERTEX_POINT('',#52874);
#8264=VERTEX_POINT('',#52876);
#8265=VERTEX_POINT('',#52878);
#8266=VERTEX_POINT('',#52880);
#8267=VERTEX_POINT('',#52882);
#8268=VERTEX_POINT('',#52884);
#8269=VERTEX_POINT('',#52886);
#8270=VERTEX_POINT('',#52888);
#8271=VERTEX_POINT('',#52890);
#8272=VERTEX_POINT('',#52892);
#8273=VERTEX_POINT('',#52894);
#8274=VERTEX_POINT('',#52896);
#8275=VERTEX_POINT('',#52898);
#8276=VERTEX_POINT('',#52900);
#8277=VERTEX_POINT('',#52902);
#8278=VERTEX_POINT('',#52904);
#8279=VERTEX_POINT('',#52906);
#8280=VERTEX_POINT('',#52908);
#8281=VERTEX_POINT('',#52910);
#8282=VERTEX_POINT('',#52912);
#8283=VERTEX_POINT('',#52914);
#8284=VERTEX_POINT('',#52916);
#8285=VERTEX_POINT('',#52918);
#8286=VERTEX_POINT('',#52920);
#8287=VERTEX_POINT('',#52922);
#8288=VERTEX_POINT('',#52924);
#8289=VERTEX_POINT('',#52926);
#8290=VERTEX_POINT('',#52928);
#8291=VERTEX_POINT('',#52930);
#8292=VERTEX_POINT('',#52932);
#8293=VERTEX_POINT('',#52934);
#8294=VERTEX_POINT('',#52936);
#8295=VERTEX_POINT('',#52938);
#8296=VERTEX_POINT('',#52940);
#8297=VERTEX_POINT('',#52942);
#8298=VERTEX_POINT('',#52944);
#8299=VERTEX_POINT('',#52946);
#8300=VERTEX_POINT('',#52948);
#8301=VERTEX_POINT('',#52950);
#8302=VERTEX_POINT('',#52952);
#8303=VERTEX_POINT('',#52954);
#8304=VERTEX_POINT('',#52956);
#8305=VERTEX_POINT('',#52958);
#8306=VERTEX_POINT('',#52961);
#8307=VERTEX_POINT('',#52963);
#8308=VERTEX_POINT('',#52965);
#8309=VERTEX_POINT('',#52967);
#8310=VERTEX_POINT('',#52970);
#8311=VERTEX_POINT('',#52971);
#8312=VERTEX_POINT('',#52976);
#8313=VERTEX_POINT('',#52980);
#8314=VERTEX_POINT('',#52984);
#8315=VERTEX_POINT('',#52988);
#8316=VERTEX_POINT('',#52992);
#8317=VERTEX_POINT('',#52996);
#8318=VERTEX_POINT('',#53000);
#8319=VERTEX_POINT('',#53004);
#8320=VERTEX_POINT('',#53008);
#8321=VERTEX_POINT('',#53010);
#8322=VERTEX_POINT('',#53014);
#8323=VERTEX_POINT('',#53018);
#8324=VERTEX_POINT('',#53022);
#8325=VERTEX_POINT('',#53024);
#8326=VERTEX_POINT('',#53028);
#8327=VERTEX_POINT('',#53032);
#8328=VERTEX_POINT('',#53036);
#8329=VERTEX_POINT('',#53037);
#8330=VERTEX_POINT('',#53042);
#8331=VERTEX_POINT('',#53046);
#8332=VERTEX_POINT('',#53050);
#8333=VERTEX_POINT('',#53054);
#8334=VERTEX_POINT('',#53058);
#8335=VERTEX_POINT('',#53062);
#8336=VERTEX_POINT('',#53066);
#8337=VERTEX_POINT('',#53070);
#8338=VERTEX_POINT('',#53074);
#8339=VERTEX_POINT('',#53076);
#8340=VERTEX_POINT('',#53080);
#8341=VERTEX_POINT('',#53084);
#8342=VERTEX_POINT('',#53088);
#8343=VERTEX_POINT('',#53090);
#8344=VERTEX_POINT('',#53094);
#8345=VERTEX_POINT('',#53098);
#8346=VERTEX_POINT('',#53102);
#8347=VERTEX_POINT('',#53103);
#8348=VERTEX_POINT('',#53108);
#8349=VERTEX_POINT('',#53112);
#8350=VERTEX_POINT('',#53116);
#8351=VERTEX_POINT('',#53120);
#8352=VERTEX_POINT('',#53124);
#8353=VERTEX_POINT('',#53128);
#8354=VERTEX_POINT('',#53132);
#8355=VERTEX_POINT('',#53136);
#8356=VERTEX_POINT('',#53140);
#8357=VERTEX_POINT('',#53142);
#8358=VERTEX_POINT('',#53146);
#8359=VERTEX_POINT('',#53150);
#8360=VERTEX_POINT('',#53154);
#8361=VERTEX_POINT('',#53156);
#8362=VERTEX_POINT('',#53160);
#8363=VERTEX_POINT('',#53164);
#8364=VERTEX_POINT('',#53168);
#8365=VERTEX_POINT('',#53169);
#8366=VERTEX_POINT('',#53174);
#8367=VERTEX_POINT('',#53178);
#8368=VERTEX_POINT('',#53182);
#8369=VERTEX_POINT('',#53186);
#8370=VERTEX_POINT('',#53190);
#8371=VERTEX_POINT('',#53194);
#8372=VERTEX_POINT('',#53198);
#8373=VERTEX_POINT('',#53202);
#8374=VERTEX_POINT('',#53206);
#8375=VERTEX_POINT('',#53208);
#8376=VERTEX_POINT('',#53212);
#8377=VERTEX_POINT('',#53216);
#8378=VERTEX_POINT('',#53220);
#8379=VERTEX_POINT('',#53224);
#8380=VERTEX_POINT('',#53228);
#8381=VERTEX_POINT('',#53234);
#8382=VERTEX_POINT('',#53238);
#8383=VERTEX_POINT('',#53268);
#8384=VERTEX_POINT('',#53270);
#8385=VERTEX_POINT('',#53273);
#8386=VERTEX_POINT('',#53277);
#8387=VERTEX_POINT('',#53281);
#8388=VERTEX_POINT('',#53283);
#8389=VERTEX_POINT('',#53287);
#8390=VERTEX_POINT('',#53289);
#8391=VERTEX_POINT('',#53293);
#8392=VERTEX_POINT('',#53295);
#8393=VERTEX_POINT('',#53299);
#8394=VERTEX_POINT('',#53301);
#8395=VERTEX_POINT('',#53305);
#8396=VERTEX_POINT('',#53306);
#8397=VERTEX_POINT('',#53308);
#8398=VERTEX_POINT('',#53310);
#8399=VERTEX_POINT('',#53314);
#8400=VERTEX_POINT('',#53316);
#8401=VERTEX_POINT('',#53320);
#8402=VERTEX_POINT('',#53322);
#8403=VERTEX_POINT('',#53332);
#8404=VERTEX_POINT('',#53333);
#8405=VERTEX_POINT('',#53335);
#8406=VERTEX_POINT('',#53346);
#8407=VERTEX_POINT('',#53359);
#8408=VERTEX_POINT('',#53360);
#8409=VERTEX_POINT('',#53407);
#8410=VERTEX_POINT('',#53408);
#8411=VERTEX_POINT('',#53455);
#8412=VERTEX_POINT('',#53456);
#8413=VERTEX_POINT('',#53509);
#8414=VERTEX_POINT('',#53510);
#8415=VERTEX_POINT('',#53557);
#8416=VERTEX_POINT('',#53558);
#8417=VERTEX_POINT('',#53605);
#8418=VERTEX_POINT('',#53606);
#8419=VERTEX_POINT('',#53659);
#8420=VERTEX_POINT('',#53660);
#8421=VERTEX_POINT('',#53707);
#8422=VERTEX_POINT('',#53708);
#8423=VERTEX_POINT('',#53755);
#8424=VERTEX_POINT('',#53756);
#8425=VERTEX_POINT('',#53803);
#8426=VERTEX_POINT('',#53804);
#8427=VERTEX_POINT('',#53857);
#8428=VERTEX_POINT('',#53858);
#8429=VERTEX_POINT('',#53905);
#8430=VERTEX_POINT('',#53906);
#8431=VERTEX_POINT('',#53953);
#8432=VERTEX_POINT('',#53954);
#8433=VERTEX_POINT('',#54007);
#8434=VERTEX_POINT('',#54008);
#8435=VERTEX_POINT('',#54055);
#8436=VERTEX_POINT('',#54056);
#8437=VERTEX_POINT('',#54103);
#8438=VERTEX_POINT('',#54104);
#8439=VERTEX_POINT('',#54157);
#8440=VERTEX_POINT('',#54158);
#8441=VERTEX_POINT('',#54205);
#8442=VERTEX_POINT('',#54206);
#8443=VERTEX_POINT('',#54253);
#8444=VERTEX_POINT('',#54254);
#8445=VERTEX_POINT('',#54256);
#8446=VERTEX_POINT('',#54268);
#8447=VERTEX_POINT('',#54280);
#8448=VERTEX_POINT('',#54281);
#8449=VERTEX_POINT('',#54305);
#8450=VERTEX_POINT('',#54306);
#8451=VERTEX_POINT('',#54329);
#8452=VERTEX_POINT('',#54330);
#8453=VERTEX_POINT('',#54354);
#8454=VERTEX_POINT('',#54355);
#8455=VERTEX_POINT('',#54379);
#8456=VERTEX_POINT('',#54380);
#8457=VERTEX_POINT('',#54403);
#8458=VERTEX_POINT('',#54404);
#8459=VERTEX_POINT('',#54428);
#8460=VERTEX_POINT('',#54429);
#8461=VERTEX_POINT('',#54453);
#8462=VERTEX_POINT('',#54454);
#8463=VERTEX_POINT('',#54477);
#8464=VERTEX_POINT('',#54478);
#8465=VERTEX_POINT('',#54502);
#8466=VERTEX_POINT('',#54503);
#8467=VERTEX_POINT('',#54527);
#8468=VERTEX_POINT('',#54528);
#8469=VERTEX_POINT('',#54551);
#8470=VERTEX_POINT('',#54552);
#8471=VERTEX_POINT('',#54575);
#8472=VERTEX_POINT('',#54576);
#8473=VERTEX_POINT('',#54600);
#8474=VERTEX_POINT('',#54601);
#8475=VERTEX_POINT('',#54625);
#8476=VERTEX_POINT('',#54626);
#8477=VERTEX_POINT('',#54649);
#8478=VERTEX_POINT('',#54650);
#8479=VERTEX_POINT('',#54674);
#8480=VERTEX_POINT('',#54675);
#8481=VERTEX_POINT('',#54699);
#8482=VERTEX_POINT('',#54700);
#8483=VERTEX_POINT('',#54723);
#8484=VERTEX_POINT('',#54968);
#8485=VERTEX_POINT('',#55042);
#8486=VERTEX_POINT('',#55081);
#8487=VERTEX_POINT('',#55600);
#8488=VERTEX_POINT('',#55733);
#8489=VERTEX_POINT('',#56398);
#8490=VERTEX_POINT('',#56399);
#8491=VERTEX_POINT('',#56401);
#8492=VERTEX_POINT('',#56403);
#8493=VERTEX_POINT('',#56407);
#8494=VERTEX_POINT('',#56409);
#8495=VERTEX_POINT('',#56413);
#8496=VERTEX_POINT('',#56415);
#8497=VERTEX_POINT('',#56419);
#8498=VERTEX_POINT('',#56421);
#8499=VERTEX_POINT('',#56425);
#8500=VERTEX_POINT('',#56427);
#8501=VERTEX_POINT('',#56435);
#8502=VERTEX_POINT('',#56438);
#8503=VERTEX_POINT('',#56445);
#8504=VERTEX_POINT('',#56447);
#8505=VERTEX_POINT('',#56454);
#8506=VERTEX_POINT('',#56455);
#8507=VERTEX_POINT('',#56457);
#8508=VERTEX_POINT('',#56462);
#8509=VERTEX_POINT('',#56464);
#8510=VERTEX_POINT('',#56467);
#8511=VERTEX_POINT('',#56480);
#8512=VERTEX_POINT('',#56481);
#8513=VERTEX_POINT('',#56531);
#8514=VERTEX_POINT('',#56532);
#8515=VERTEX_POINT('',#56582);
#8516=VERTEX_POINT('',#56583);
#8517=VERTEX_POINT('',#56630);
#8518=VERTEX_POINT('',#56631);
#8519=VERTEX_POINT('',#56681);
#8520=VERTEX_POINT('',#56682);
#8521=VERTEX_POINT('',#56732);
#8522=VERTEX_POINT('',#56733);
#8523=VERTEX_POINT('',#56780);
#8524=VERTEX_POINT('',#56781);
#8525=VERTEX_POINT('',#56783);
#8526=VERTEX_POINT('',#56797);
#8527=VERTEX_POINT('',#56819);
#8528=VERTEX_POINT('',#56820);
#8529=VERTEX_POINT('',#56822);
#8530=VERTEX_POINT('',#56831);
#8531=VERTEX_POINT('',#56843);
#8532=VERTEX_POINT('',#56844);
#8533=VERTEX_POINT('',#56867);
#8534=VERTEX_POINT('',#56868);
#8535=VERTEX_POINT('',#56892);
#8536=VERTEX_POINT('',#56893);
#8537=VERTEX_POINT('',#56917);
#8538=VERTEX_POINT('',#56918);
#8539=VERTEX_POINT('',#56941);
#8540=VERTEX_POINT('',#56942);
#8541=VERTEX_POINT('',#56966);
#8542=VERTEX_POINT('',#56967);
#8543=VERTEX_POINT('',#56991);
#8544=VERTEX_POINT('',#56992);
#8545=VERTEX_POINT('',#56994);
#8546=VERTEX_POINT('',#57000);
#8547=VERTEX_POINT('',#57008);
#8548=VERTEX_POINT('',#57009);
#8549=VERTEX_POINT('',#57011);
#8550=VERTEX_POINT('',#57016);
#8551=VERTEX_POINT('',#57018);
#8552=VERTEX_POINT('',#57021);
#8553=VERTEX_POINT('',#57034);
#8554=VERTEX_POINT('',#57035);
#8555=VERTEX_POINT('',#57085);
#8556=VERTEX_POINT('',#57086);
#8557=VERTEX_POINT('',#57136);
#8558=VERTEX_POINT('',#57137);
#8559=VERTEX_POINT('',#57184);
#8560=VERTEX_POINT('',#57185);
#8561=VERTEX_POINT('',#57235);
#8562=VERTEX_POINT('',#57236);
#8563=VERTEX_POINT('',#57286);
#8564=VERTEX_POINT('',#57287);
#8565=VERTEX_POINT('',#57334);
#8566=VERTEX_POINT('',#57335);
#8567=VERTEX_POINT('',#57337);
#8568=VERTEX_POINT('',#57351);
#8569=VERTEX_POINT('',#57373);
#8570=VERTEX_POINT('',#57374);
#8571=VERTEX_POINT('',#57376);
#8572=VERTEX_POINT('',#57385);
#8573=VERTEX_POINT('',#57397);
#8574=VERTEX_POINT('',#57398);
#8575=VERTEX_POINT('',#57421);
#8576=VERTEX_POINT('',#57422);
#8577=VERTEX_POINT('',#57446);
#8578=VERTEX_POINT('',#57447);
#8579=VERTEX_POINT('',#57471);
#8580=VERTEX_POINT('',#57472);
#8581=VERTEX_POINT('',#57495);
#8582=VERTEX_POINT('',#57496);
#8583=VERTEX_POINT('',#57520);
#8584=VERTEX_POINT('',#57521);
#8585=VERTEX_POINT('',#57545);
#8586=VERTEX_POINT('',#57546);
#8587=VERTEX_POINT('',#57548);
#8588=VERTEX_POINT('',#57554);
#8589=VERTEX_POINT('',#57562);
#8590=VERTEX_POINT('',#57563);
#8591=VERTEX_POINT('',#57565);
#8592=VERTEX_POINT('',#57570);
#8593=VERTEX_POINT('',#57572);
#8594=VERTEX_POINT('',#57575);
#8595=VERTEX_POINT('',#57588);
#8596=VERTEX_POINT('',#57589);
#8597=VERTEX_POINT('',#57639);
#8598=VERTEX_POINT('',#57640);
#8599=VERTEX_POINT('',#57690);
#8600=VERTEX_POINT('',#57691);
#8601=VERTEX_POINT('',#57738);
#8602=VERTEX_POINT('',#57739);
#8603=VERTEX_POINT('',#57789);
#8604=VERTEX_POINT('',#57790);
#8605=VERTEX_POINT('',#57840);
#8606=VERTEX_POINT('',#57841);
#8607=VERTEX_POINT('',#57888);
#8608=VERTEX_POINT('',#57889);
#8609=VERTEX_POINT('',#57891);
#8610=VERTEX_POINT('',#57905);
#8611=VERTEX_POINT('',#57927);
#8612=VERTEX_POINT('',#57928);
#8613=VERTEX_POINT('',#57930);
#8614=VERTEX_POINT('',#57939);
#8615=VERTEX_POINT('',#57951);
#8616=VERTEX_POINT('',#57952);
#8617=VERTEX_POINT('',#57975);
#8618=VERTEX_POINT('',#57976);
#8619=VERTEX_POINT('',#58000);
#8620=VERTEX_POINT('',#58001);
#8621=VERTEX_POINT('',#58025);
#8622=VERTEX_POINT('',#58026);
#8623=VERTEX_POINT('',#58049);
#8624=VERTEX_POINT('',#58050);
#8625=VERTEX_POINT('',#58074);
#8626=VERTEX_POINT('',#58075);
#8627=VERTEX_POINT('',#58099);
#8628=VERTEX_POINT('',#58100);
#8629=VERTEX_POINT('',#58102);
#8630=VERTEX_POINT('',#58108);
#8631=VERTEX_POINT('',#60795);
#8632=VERTEX_POINT('',#60797);
#8633=VERTEX_POINT('',#60800);
#8634=VERTEX_POINT('',#60802);
#8635=VERTEX_POINT('',#60809);
#8636=VERTEX_POINT('',#60811);
#8637=VERTEX_POINT('',#60815);
#8638=VERTEX_POINT('',#60817);
#8639=VERTEX_POINT('',#60821);
#8640=VERTEX_POINT('',#60823);
#8641=VERTEX_POINT('',#60827);
#8642=VERTEX_POINT('',#60829);
#8643=VERTEX_POINT('',#60833);
#8644=VERTEX_POINT('',#60837);
#8645=VERTEX_POINT('',#60839);
#8646=VERTEX_POINT('',#60846);
#8647=VERTEX_POINT('',#60847);
#8648=VERTEX_POINT('',#60849);
#8649=VERTEX_POINT('',#60860);
#8650=VERTEX_POINT('',#60873);
#8651=VERTEX_POINT('',#60874);
#8652=VERTEX_POINT('',#60921);
#8653=VERTEX_POINT('',#60922);
#8654=VERTEX_POINT('',#60969);
#8655=VERTEX_POINT('',#60970);
#8656=VERTEX_POINT('',#61020);
#8657=VERTEX_POINT('',#61021);
#8658=VERTEX_POINT('',#61068);
#8659=VERTEX_POINT('',#61069);
#8660=VERTEX_POINT('',#61116);
#8661=VERTEX_POINT('',#61117);
#8662=VERTEX_POINT('',#61164);
#8663=VERTEX_POINT('',#61165);
#8664=VERTEX_POINT('',#61218);
#8665=VERTEX_POINT('',#61219);
#8666=VERTEX_POINT('',#61266);
#8667=VERTEX_POINT('',#61267);
#8668=VERTEX_POINT('',#61314);
#8669=VERTEX_POINT('',#61315);
#8670=VERTEX_POINT('',#61368);
#8671=VERTEX_POINT('',#61369);
#8672=VERTEX_POINT('',#61416);
#8673=VERTEX_POINT('',#61417);
#8674=VERTEX_POINT('',#61464);
#8675=VERTEX_POINT('',#61465);
#8676=VERTEX_POINT('',#61515);
#8677=VERTEX_POINT('',#61516);
#8678=VERTEX_POINT('',#61566);
#8679=VERTEX_POINT('',#61567);
#8680=VERTEX_POINT('',#61614);
#8681=VERTEX_POINT('',#61615);
#8682=VERTEX_POINT('',#61662);
#8683=VERTEX_POINT('',#61663);
#8684=VERTEX_POINT('',#61716);
#8685=VERTEX_POINT('',#61717);
#8686=VERTEX_POINT('',#61764);
#8687=VERTEX_POINT('',#61765);
#8688=VERTEX_POINT('',#61812);
#8689=VERTEX_POINT('',#61813);
#8690=VERTEX_POINT('',#61866);
#8691=VERTEX_POINT('',#61867);
#8692=VERTEX_POINT('',#61914);
#8693=VERTEX_POINT('',#61915);
#8694=VERTEX_POINT('',#61962);
#8695=VERTEX_POINT('',#61963);
#8696=VERTEX_POINT('',#62010);
#8697=VERTEX_POINT('',#62011);
#8698=VERTEX_POINT('',#62064);
#8699=VERTEX_POINT('',#62065);
#8700=VERTEX_POINT('',#62112);
#8701=VERTEX_POINT('',#62113);
#8702=VERTEX_POINT('',#62160);
#8703=VERTEX_POINT('',#62161);
#8704=VERTEX_POINT('',#62214);
#8705=VERTEX_POINT('',#62215);
#8706=VERTEX_POINT('',#62262);
#8707=VERTEX_POINT('',#62263);
#8708=VERTEX_POINT('',#62310);
#8709=VERTEX_POINT('',#62311);
#8710=VERTEX_POINT('',#62364);
#8711=VERTEX_POINT('',#62365);
#8712=VERTEX_POINT('',#62412);
#8713=VERTEX_POINT('',#62413);
#8714=VERTEX_POINT('',#62460);
#8715=VERTEX_POINT('',#62461);
#8716=VERTEX_POINT('',#62508);
#8717=VERTEX_POINT('',#62509);
#8718=VERTEX_POINT('',#62562);
#8719=VERTEX_POINT('',#62563);
#8720=VERTEX_POINT('',#62610);
#8721=VERTEX_POINT('',#62611);
#8722=VERTEX_POINT('',#62658);
#8723=VERTEX_POINT('',#62659);
#8724=VERTEX_POINT('',#62712);
#8725=VERTEX_POINT('',#62713);
#8726=VERTEX_POINT('',#62760);
#8727=VERTEX_POINT('',#62761);
#8728=VERTEX_POINT('',#62808);
#8729=VERTEX_POINT('',#62809);
#8730=VERTEX_POINT('',#62862);
#8731=VERTEX_POINT('',#62863);
#8732=VERTEX_POINT('',#62910);
#8733=VERTEX_POINT('',#62911);
#8734=VERTEX_POINT('',#62958);
#8735=VERTEX_POINT('',#62959);
#8736=VERTEX_POINT('',#63006);
#8737=VERTEX_POINT('',#63007);
#8738=VERTEX_POINT('',#63060);
#8739=VERTEX_POINT('',#63061);
#8740=VERTEX_POINT('',#63108);
#8741=VERTEX_POINT('',#63109);
#8742=VERTEX_POINT('',#63156);
#8743=VERTEX_POINT('',#63157);
#8744=VERTEX_POINT('',#63210);
#8745=VERTEX_POINT('',#63211);
#8746=VERTEX_POINT('',#63258);
#8747=VERTEX_POINT('',#63259);
#8748=VERTEX_POINT('',#63306);
#8749=VERTEX_POINT('',#63307);
#8750=VERTEX_POINT('',#63360);
#8751=VERTEX_POINT('',#63361);
#8752=VERTEX_POINT('',#63408);
#8753=VERTEX_POINT('',#63409);
#8754=VERTEX_POINT('',#63456);
#8755=VERTEX_POINT('',#63457);
#8756=VERTEX_POINT('',#63504);
#8757=VERTEX_POINT('',#63505);
#8758=VERTEX_POINT('',#63558);
#8759=VERTEX_POINT('',#63559);
#8760=VERTEX_POINT('',#63606);
#8761=VERTEX_POINT('',#63607);
#8762=VERTEX_POINT('',#63654);
#8763=VERTEX_POINT('',#63655);
#8764=VERTEX_POINT('',#63708);
#8765=VERTEX_POINT('',#63709);
#8766=VERTEX_POINT('',#63756);
#8767=VERTEX_POINT('',#63757);
#8768=VERTEX_POINT('',#63804);
#8769=VERTEX_POINT('',#63805);
#8770=VERTEX_POINT('',#63807);
#8771=VERTEX_POINT('',#63814);
#8772=VERTEX_POINT('',#63822);
#8773=VERTEX_POINT('',#63823);
#8774=VERTEX_POINT('',#63847);
#8775=VERTEX_POINT('',#63848);
#8776=VERTEX_POINT('',#63871);
#8777=VERTEX_POINT('',#63872);
#8778=VERTEX_POINT('',#63896);
#8779=VERTEX_POINT('',#63897);
#8780=VERTEX_POINT('',#63921);
#8781=VERTEX_POINT('',#63922);
#8782=VERTEX_POINT('',#63945);
#8783=VERTEX_POINT('',#63946);
#8784=VERTEX_POINT('',#63970);
#8785=VERTEX_POINT('',#63971);
#8786=VERTEX_POINT('',#63995);
#8787=VERTEX_POINT('',#63996);
#8788=VERTEX_POINT('',#64019);
#8789=VERTEX_POINT('',#64020);
#8790=VERTEX_POINT('',#64043);
#8791=VERTEX_POINT('',#64044);
#8792=VERTEX_POINT('',#64068);
#8793=VERTEX_POINT('',#64069);
#8794=VERTEX_POINT('',#64093);
#8795=VERTEX_POINT('',#64094);
#8796=VERTEX_POINT('',#64117);
#8797=VERTEX_POINT('',#64118);
#8798=VERTEX_POINT('',#64142);
#8799=VERTEX_POINT('',#64143);
#8800=VERTEX_POINT('',#64167);
#8801=VERTEX_POINT('',#64168);
#8802=VERTEX_POINT('',#64191);
#8803=VERTEX_POINT('',#64192);
#8804=VERTEX_POINT('',#64216);
#8805=VERTEX_POINT('',#64217);
#8806=VERTEX_POINT('',#64241);
#8807=VERTEX_POINT('',#64242);
#8808=VERTEX_POINT('',#64265);
#8809=VERTEX_POINT('',#64266);
#8810=VERTEX_POINT('',#64289);
#8811=VERTEX_POINT('',#64290);
#8812=VERTEX_POINT('',#64314);
#8813=VERTEX_POINT('',#64315);
#8814=VERTEX_POINT('',#64339);
#8815=VERTEX_POINT('',#64340);
#8816=VERTEX_POINT('',#64363);
#8817=VERTEX_POINT('',#64364);
#8818=VERTEX_POINT('',#64388);
#8819=VERTEX_POINT('',#64389);
#8820=VERTEX_POINT('',#64413);
#8821=VERTEX_POINT('',#64414);
#8822=VERTEX_POINT('',#64437);
#8823=VERTEX_POINT('',#64438);
#8824=VERTEX_POINT('',#64462);
#8825=VERTEX_POINT('',#64463);
#8826=VERTEX_POINT('',#64487);
#8827=VERTEX_POINT('',#64488);
#8828=VERTEX_POINT('',#64511);
#8829=VERTEX_POINT('',#64512);
#8830=VERTEX_POINT('',#64535);
#8831=VERTEX_POINT('',#64536);
#8832=VERTEX_POINT('',#64560);
#8833=VERTEX_POINT('',#64561);
#8834=VERTEX_POINT('',#64585);
#8835=VERTEX_POINT('',#64586);
#8836=VERTEX_POINT('',#64609);
#8837=VERTEX_POINT('',#64610);
#8838=VERTEX_POINT('',#64634);
#8839=VERTEX_POINT('',#64635);
#8840=VERTEX_POINT('',#64659);
#8841=VERTEX_POINT('',#64660);
#8842=VERTEX_POINT('',#64683);
#8843=VERTEX_POINT('',#64684);
#8844=VERTEX_POINT('',#64708);
#8845=VERTEX_POINT('',#64709);
#8846=VERTEX_POINT('',#64733);
#8847=VERTEX_POINT('',#64734);
#8848=VERTEX_POINT('',#64757);
#8849=VERTEX_POINT('',#64758);
#8850=VERTEX_POINT('',#64781);
#8851=VERTEX_POINT('',#64782);
#8852=VERTEX_POINT('',#64806);
#8853=VERTEX_POINT('',#64807);
#8854=VERTEX_POINT('',#64831);
#8855=VERTEX_POINT('',#64832);
#8856=VERTEX_POINT('',#64855);
#8857=VERTEX_POINT('',#64856);
#8858=VERTEX_POINT('',#64880);
#8859=VERTEX_POINT('',#64881);
#8860=VERTEX_POINT('',#64905);
#8861=VERTEX_POINT('',#64906);
#8862=VERTEX_POINT('',#64929);
#8863=VERTEX_POINT('',#64930);
#8864=VERTEX_POINT('',#64954);
#8865=VERTEX_POINT('',#64955);
#8866=VERTEX_POINT('',#64978);
#8867=VERTEX_POINT('',#64979);
#8868=VERTEX_POINT('',#65003);
#8869=VERTEX_POINT('',#65004);
#8870=VERTEX_POINT('',#65027);
#8871=VERTEX_POINT('',#65028);
#8872=VERTEX_POINT('',#65052);
#8873=VERTEX_POINT('',#65053);
#8874=VERTEX_POINT('',#65077);
#8875=VERTEX_POINT('',#65078);
#8876=VERTEX_POINT('',#65101);
#8877=VERTEX_POINT('',#65102);
#8878=VERTEX_POINT('',#65126);
#8879=VERTEX_POINT('',#65127);
#8880=VERTEX_POINT('',#65151);
#8881=VERTEX_POINT('',#65152);
#8882=VERTEX_POINT('',#65175);
#8883=VERTEX_POINT('',#65176);
#8884=VERTEX_POINT('',#65200);
#8885=VERTEX_POINT('',#65201);
#8886=VERTEX_POINT('',#65224);
#8887=VERTEX_POINT('',#65225);
#8888=VERTEX_POINT('',#65249);
#8889=VERTEX_POINT('',#65250);
#8890=VERTEX_POINT('',#66812);
#8891=VERTEX_POINT('',#66941);
#8892=VERTEX_POINT('',#67058);
#8893=VERTEX_POINT('',#68609);
#8894=VERTEX_POINT('',#68844);
#8895=VERTEX_POINT('',#68845);
#8896=VERTEX_POINT('',#68847);
#8897=VERTEX_POINT('',#68849);
#8898=VERTEX_POINT('',#68851);
#8899=VERTEX_POINT('',#68853);
#8900=VERTEX_POINT('',#68857);
#8901=VERTEX_POINT('',#68858);
#8902=VERTEX_POINT('',#68860);
#8903=VERTEX_POINT('',#68862);
#8904=VERTEX_POINT('',#68864);
#8905=VERTEX_POINT('',#68866);
#8906=VERTEX_POINT('',#68869);
#8907=VERTEX_POINT('',#68884);
#8908=VERTEX_POINT('',#68889);
#8909=VERTEX_POINT('',#68893);
#8910=VERTEX_POINT('',#68894);
#8911=VERTEX_POINT('',#68896);
#8912=VERTEX_POINT('',#68904);
#8913=VERTEX_POINT('',#68917);
#8914=VERTEX_POINT('',#68918);
#8915=VERTEX_POINT('',#68968);
#8916=VERTEX_POINT('',#68969);
#8917=VERTEX_POINT('',#69019);
#8918=VERTEX_POINT('',#69020);
#8919=VERTEX_POINT('',#69067);
#8920=VERTEX_POINT('',#69068);
#8921=VERTEX_POINT('',#69118);
#8922=VERTEX_POINT('',#69119);
#8923=VERTEX_POINT('',#69169);
#8924=VERTEX_POINT('',#69170);
#8925=VERTEX_POINT('',#69217);
#8926=VERTEX_POINT('',#69218);
#8927=VERTEX_POINT('',#69220);
#8928=VERTEX_POINT('',#69237);
#8929=VERTEX_POINT('',#69259);
#8930=VERTEX_POINT('',#69260);
#8931=VERTEX_POINT('',#69262);
#8932=VERTEX_POINT('',#69272);
#8933=VERTEX_POINT('',#69284);
#8934=VERTEX_POINT('',#69285);
#8935=VERTEX_POINT('',#69308);
#8936=VERTEX_POINT('',#69309);
#8937=VERTEX_POINT('',#69333);
#8938=VERTEX_POINT('',#69334);
#8939=VERTEX_POINT('',#69358);
#8940=VERTEX_POINT('',#69359);
#8941=VERTEX_POINT('',#69382);
#8942=VERTEX_POINT('',#69383);
#8943=VERTEX_POINT('',#69407);
#8944=VERTEX_POINT('',#69408);
#8945=VERTEX_POINT('',#69432);
#8946=VERTEX_POINT('',#69433);
#8947=VERTEX_POINT('',#69435);
#8948=VERTEX_POINT('',#69442);
#8949=VERTEX_POINT('',#70404);
#8950=VERTEX_POINT('',#70405);
#8951=VERTEX_POINT('',#70407);
#8952=VERTEX_POINT('',#70409);
#8953=VERTEX_POINT('',#70411);
#8954=VERTEX_POINT('',#70413);
#8955=VERTEX_POINT('',#70418);
#8956=VERTEX_POINT('',#70419);
#8957=VERTEX_POINT('',#70424);
#8958=VERTEX_POINT('',#70428);
#8959=VERTEX_POINT('',#70432);
#8960=VERTEX_POINT('',#70436);
#8961=VERTEX_POINT('',#70444);
#8962=VERTEX_POINT('',#70446);
#8963=VERTEX_POINT('',#70450);
#8964=VERTEX_POINT('',#70452);
#8965=VERTEX_POINT('',#70459);
#8966=VERTEX_POINT('',#70460);
#8967=VERTEX_POINT('',#70462);
#8968=VERTEX_POINT('',#70473);
#8969=VERTEX_POINT('',#70483);
#8970=VERTEX_POINT('',#70484);
#8971=VERTEX_POINT('',#70531);
#8972=VERTEX_POINT('',#70532);
#8973=VERTEX_POINT('',#70579);
#8974=VERTEX_POINT('',#70580);
#8975=VERTEX_POINT('',#70633);
#8976=VERTEX_POINT('',#70634);
#8977=VERTEX_POINT('',#70681);
#8978=VERTEX_POINT('',#70682);
#8979=VERTEX_POINT('',#70729);
#8980=VERTEX_POINT('',#70730);
#8981=VERTEX_POINT('',#70783);
#8982=VERTEX_POINT('',#70784);
#8983=VERTEX_POINT('',#70831);
#8984=VERTEX_POINT('',#70832);
#8985=VERTEX_POINT('',#70879);
#8986=VERTEX_POINT('',#70880);
#8987=VERTEX_POINT('',#70933);
#8988=VERTEX_POINT('',#70934);
#8989=VERTEX_POINT('',#70981);
#8990=VERTEX_POINT('',#70982);
#8991=VERTEX_POINT('',#71029);
#8992=VERTEX_POINT('',#71030);
#8993=VERTEX_POINT('',#71083);
#8994=VERTEX_POINT('',#71084);
#8995=VERTEX_POINT('',#71131);
#8996=VERTEX_POINT('',#71132);
#8997=VERTEX_POINT('',#71179);
#8998=VERTEX_POINT('',#71180);
#8999=VERTEX_POINT('',#71182);
#9000=VERTEX_POINT('',#71193);
#9001=VERTEX_POINT('',#71204);
#9002=VERTEX_POINT('',#71205);
#9003=VERTEX_POINT('',#71229);
#9004=VERTEX_POINT('',#71230);
#9005=VERTEX_POINT('',#71253);
#9006=VERTEX_POINT('',#71254);
#9007=VERTEX_POINT('',#71278);
#9008=VERTEX_POINT('',#71279);
#9009=VERTEX_POINT('',#71303);
#9010=VERTEX_POINT('',#71304);
#9011=VERTEX_POINT('',#71327);
#9012=VERTEX_POINT('',#71328);
#9013=VERTEX_POINT('',#71352);
#9014=VERTEX_POINT('',#71353);
#9015=VERTEX_POINT('',#71377);
#9016=VERTEX_POINT('',#71378);
#9017=VERTEX_POINT('',#71401);
#9018=VERTEX_POINT('',#71402);
#9019=VERTEX_POINT('',#71426);
#9020=VERTEX_POINT('',#71427);
#9021=VERTEX_POINT('',#71451);
#9022=VERTEX_POINT('',#71452);
#9023=VERTEX_POINT('',#71475);
#9024=VERTEX_POINT('',#71476);
#9025=VERTEX_POINT('',#71500);
#9026=VERTEX_POINT('',#71501);
#9027=VERTEX_POINT('',#71525);
#9028=VERTEX_POINT('',#71526);
#9029=VERTEX_POINT('',#71549);
#9030=VERTEX_POINT('',#71770);
#9031=VERTEX_POINT('',#71835);
#9032=VERTEX_POINT('',#71868);
#9033=VERTEX_POINT('',#72279);
#9034=VERTEX_POINT('',#72396);
#9035=VERTEX_POINT('',#72935);
#9036=VERTEX_POINT('',#72936);
#9037=VERTEX_POINT('',#72938);
#9038=VERTEX_POINT('',#72940);
#9039=VERTEX_POINT('',#72944);
#9040=VERTEX_POINT('',#72946);
#9041=VERTEX_POINT('',#72950);
#9042=VERTEX_POINT('',#72952);
#9043=VERTEX_POINT('',#72956);
#9044=VERTEX_POINT('',#72958);
#9045=VERTEX_POINT('',#72962);
#9046=VERTEX_POINT('',#72964);
#9047=VERTEX_POINT('',#72972);
#9048=VERTEX_POINT('',#72975);
#9049=VERTEX_POINT('',#72982);
#9050=VERTEX_POINT('',#72983);
#9051=VERTEX_POINT('',#72985);
#9052=VERTEX_POINT('',#72990);
#9053=VERTEX_POINT('',#73003);
#9054=VERTEX_POINT('',#73004);
#9055=VERTEX_POINT('',#73054);
#9056=VERTEX_POINT('',#73055);
#9057=VERTEX_POINT('',#73105);
#9058=VERTEX_POINT('',#73106);
#9059=VERTEX_POINT('',#73153);
#9060=VERTEX_POINT('',#73154);
#9061=VERTEX_POINT('',#73201);
#9062=VERTEX_POINT('',#73202);
#9063=VERTEX_POINT('',#73252);
#9064=VERTEX_POINT('',#73253);
#9065=VERTEX_POINT('',#73303);
#9066=VERTEX_POINT('',#73304);
#9067=VERTEX_POINT('',#73351);
#9068=VERTEX_POINT('',#73352);
#9069=VERTEX_POINT('',#73402);
#9070=VERTEX_POINT('',#73403);
#9071=VERTEX_POINT('',#73453);
#9072=VERTEX_POINT('',#73454);
#9073=VERTEX_POINT('',#73501);
#9074=VERTEX_POINT('',#73502);
#9075=VERTEX_POINT('',#73549);
#9076=VERTEX_POINT('',#73550);
#9077=VERTEX_POINT('',#73603);
#9078=VERTEX_POINT('',#73604);
#9079=VERTEX_POINT('',#73651);
#9080=VERTEX_POINT('',#73652);
#9081=VERTEX_POINT('',#73699);
#9082=VERTEX_POINT('',#73700);
#9083=VERTEX_POINT('',#73750);
#9084=VERTEX_POINT('',#73751);
#9085=VERTEX_POINT('',#73801);
#9086=VERTEX_POINT('',#73802);
#9087=VERTEX_POINT('',#73849);
#9088=VERTEX_POINT('',#73850);
#9089=VERTEX_POINT('',#73900);
#9090=VERTEX_POINT('',#73901);
#9091=VERTEX_POINT('',#73903);
#9092=VERTEX_POINT('',#73917);
#9093=VERTEX_POINT('',#73939);
#9094=VERTEX_POINT('',#73940);
#9095=VERTEX_POINT('',#73942);
#9096=VERTEX_POINT('',#73947);
#9097=VERTEX_POINT('',#73960);
#9098=VERTEX_POINT('',#73961);
#9099=VERTEX_POINT('',#74011);
#9100=VERTEX_POINT('',#74012);
#9101=VERTEX_POINT('',#74062);
#9102=VERTEX_POINT('',#74063);
#9103=VERTEX_POINT('',#74110);
#9104=VERTEX_POINT('',#74111);
#9105=VERTEX_POINT('',#74158);
#9106=VERTEX_POINT('',#74159);
#9107=VERTEX_POINT('',#74209);
#9108=VERTEX_POINT('',#74210);
#9109=VERTEX_POINT('',#74260);
#9110=VERTEX_POINT('',#74261);
#9111=VERTEX_POINT('',#74308);
#9112=VERTEX_POINT('',#74309);
#9113=VERTEX_POINT('',#74359);
#9114=VERTEX_POINT('',#74360);
#9115=VERTEX_POINT('',#74410);
#9116=VERTEX_POINT('',#74411);
#9117=VERTEX_POINT('',#74458);
#9118=VERTEX_POINT('',#74459);
#9119=VERTEX_POINT('',#74506);
#9120=VERTEX_POINT('',#74507);
#9121=VERTEX_POINT('',#74560);
#9122=VERTEX_POINT('',#74561);
#9123=VERTEX_POINT('',#74608);
#9124=VERTEX_POINT('',#74609);
#9125=VERTEX_POINT('',#74656);
#9126=VERTEX_POINT('',#74657);
#9127=VERTEX_POINT('',#74707);
#9128=VERTEX_POINT('',#74708);
#9129=VERTEX_POINT('',#74758);
#9130=VERTEX_POINT('',#74759);
#9131=VERTEX_POINT('',#74806);
#9132=VERTEX_POINT('',#74807);
#9133=VERTEX_POINT('',#74857);
#9134=VERTEX_POINT('',#74858);
#9135=VERTEX_POINT('',#74860);
#9136=VERTEX_POINT('',#74874);
#9137=VERTEX_POINT('',#74896);
#9138=VERTEX_POINT('',#74897);
#9139=VERTEX_POINT('',#74899);
#9140=VERTEX_POINT('',#74904);
#9141=VERTEX_POINT('',#74917);
#9142=VERTEX_POINT('',#74918);
#9143=VERTEX_POINT('',#74968);
#9144=VERTEX_POINT('',#74969);
#9145=VERTEX_POINT('',#75019);
#9146=VERTEX_POINT('',#75020);
#9147=VERTEX_POINT('',#75067);
#9148=VERTEX_POINT('',#75068);
#9149=VERTEX_POINT('',#75115);
#9150=VERTEX_POINT('',#75116);
#9151=VERTEX_POINT('',#75166);
#9152=VERTEX_POINT('',#75167);
#9153=VERTEX_POINT('',#75217);
#9154=VERTEX_POINT('',#75218);
#9155=VERTEX_POINT('',#75265);
#9156=VERTEX_POINT('',#75266);
#9157=VERTEX_POINT('',#75316);
#9158=VERTEX_POINT('',#75317);
#9159=VERTEX_POINT('',#75367);
#9160=VERTEX_POINT('',#75368);
#9161=VERTEX_POINT('',#75415);
#9162=VERTEX_POINT('',#75416);
#9163=VERTEX_POINT('',#75463);
#9164=VERTEX_POINT('',#75464);
#9165=VERTEX_POINT('',#75517);
#9166=VERTEX_POINT('',#75518);
#9167=VERTEX_POINT('',#75565);
#9168=VERTEX_POINT('',#75566);
#9169=VERTEX_POINT('',#75613);
#9170=VERTEX_POINT('',#75614);
#9171=VERTEX_POINT('',#75664);
#9172=VERTEX_POINT('',#75665);
#9173=VERTEX_POINT('',#75715);
#9174=VERTEX_POINT('',#75716);
#9175=VERTEX_POINT('',#75763);
#9176=VERTEX_POINT('',#75764);
#9177=VERTEX_POINT('',#75814);
#9178=VERTEX_POINT('',#75815);
#9179=VERTEX_POINT('',#75817);
#9180=VERTEX_POINT('',#75831);
#9181=VERTEX_POINT('',#75853);
#9182=VERTEX_POINT('',#75854);
#9183=VERTEX_POINT('',#75856);
#9184=VERTEX_POINT('',#75861);
#9185=VERTEX_POINT('',#75874);
#9186=VERTEX_POINT('',#75875);
#9187=VERTEX_POINT('',#75925);
#9188=VERTEX_POINT('',#75926);
#9189=VERTEX_POINT('',#75976);
#9190=VERTEX_POINT('',#75977);
#9191=VERTEX_POINT('',#76024);
#9192=VERTEX_POINT('',#76025);
#9193=VERTEX_POINT('',#76072);
#9194=VERTEX_POINT('',#76073);
#9195=VERTEX_POINT('',#76123);
#9196=VERTEX_POINT('',#76124);
#9197=VERTEX_POINT('',#76174);
#9198=VERTEX_POINT('',#76175);
#9199=VERTEX_POINT('',#76222);
#9200=VERTEX_POINT('',#76223);
#9201=VERTEX_POINT('',#76273);
#9202=VERTEX_POINT('',#76274);
#9203=VERTEX_POINT('',#76324);
#9204=VERTEX_POINT('',#76325);
#9205=VERTEX_POINT('',#76372);
#9206=VERTEX_POINT('',#76373);
#9207=VERTEX_POINT('',#76420);
#9208=VERTEX_POINT('',#76421);
#9209=VERTEX_POINT('',#76474);
#9210=VERTEX_POINT('',#76475);
#9211=VERTEX_POINT('',#76522);
#9212=VERTEX_POINT('',#76523);
#9213=VERTEX_POINT('',#76570);
#9214=VERTEX_POINT('',#76571);
#9215=VERTEX_POINT('',#76621);
#9216=VERTEX_POINT('',#76622);
#9217=VERTEX_POINT('',#76672);
#9218=VERTEX_POINT('',#76673);
#9219=VERTEX_POINT('',#76720);
#9220=VERTEX_POINT('',#76721);
#9221=VERTEX_POINT('',#76771);
#9222=VERTEX_POINT('',#76772);
#9223=VERTEX_POINT('',#76774);
#9224=VERTEX_POINT('',#76788);
#9225=VERTEX_POINT('',#76810);
#9226=VERTEX_POINT('',#76811);
#9227=VERTEX_POINT('',#76813);
#9228=VERTEX_POINT('',#76818);
#9229=VERTEX_POINT('',#76831);
#9230=VERTEX_POINT('',#76832);
#9231=VERTEX_POINT('',#76882);
#9232=VERTEX_POINT('',#76883);
#9233=VERTEX_POINT('',#76933);
#9234=VERTEX_POINT('',#76934);
#9235=VERTEX_POINT('',#76981);
#9236=VERTEX_POINT('',#76982);
#9237=VERTEX_POINT('',#77029);
#9238=VERTEX_POINT('',#77030);
#9239=VERTEX_POINT('',#77080);
#9240=VERTEX_POINT('',#77081);
#9241=VERTEX_POINT('',#77131);
#9242=VERTEX_POINT('',#77132);
#9243=VERTEX_POINT('',#77179);
#9244=VERTEX_POINT('',#77180);
#9245=VERTEX_POINT('',#77230);
#9246=VERTEX_POINT('',#77231);
#9247=VERTEX_POINT('',#77281);
#9248=VERTEX_POINT('',#77282);
#9249=VERTEX_POINT('',#77329);
#9250=VERTEX_POINT('',#77330);
#9251=VERTEX_POINT('',#77377);
#9252=VERTEX_POINT('',#77378);
#9253=VERTEX_POINT('',#77431);
#9254=VERTEX_POINT('',#77432);
#9255=VERTEX_POINT('',#77479);
#9256=VERTEX_POINT('',#77480);
#9257=VERTEX_POINT('',#77527);
#9258=VERTEX_POINT('',#77528);
#9259=VERTEX_POINT('',#77578);
#9260=VERTEX_POINT('',#77579);
#9261=VERTEX_POINT('',#77629);
#9262=VERTEX_POINT('',#77630);
#9263=VERTEX_POINT('',#77677);
#9264=VERTEX_POINT('',#77678);
#9265=VERTEX_POINT('',#77728);
#9266=VERTEX_POINT('',#77729);
#9267=VERTEX_POINT('',#77731);
#9268=VERTEX_POINT('',#77745);
#9269=VERTEX_POINT('',#77767);
#9270=VERTEX_POINT('',#77768);
#9271=VERTEX_POINT('',#77770);
#9272=VERTEX_POINT('',#77775);
#9273=VERTEX_POINT('',#77788);
#9274=VERTEX_POINT('',#77789);
#9275=VERTEX_POINT('',#77839);
#9276=VERTEX_POINT('',#77840);
#9277=VERTEX_POINT('',#77890);
#9278=VERTEX_POINT('',#77891);
#9279=VERTEX_POINT('',#77938);
#9280=VERTEX_POINT('',#77939);
#9281=VERTEX_POINT('',#77986);
#9282=VERTEX_POINT('',#77987);
#9283=VERTEX_POINT('',#78037);
#9284=VERTEX_POINT('',#78038);
#9285=VERTEX_POINT('',#78088);
#9286=VERTEX_POINT('',#78089);
#9287=VERTEX_POINT('',#78136);
#9288=VERTEX_POINT('',#78137);
#9289=VERTEX_POINT('',#78187);
#9290=VERTEX_POINT('',#78188);
#9291=VERTEX_POINT('',#78238);
#9292=VERTEX_POINT('',#78239);
#9293=VERTEX_POINT('',#78286);
#9294=VERTEX_POINT('',#78287);
#9295=VERTEX_POINT('',#78334);
#9296=VERTEX_POINT('',#78335);
#9297=VERTEX_POINT('',#78388);
#9298=VERTEX_POINT('',#78389);
#9299=VERTEX_POINT('',#78436);
#9300=VERTEX_POINT('',#78437);
#9301=VERTEX_POINT('',#78484);
#9302=VERTEX_POINT('',#78485);
#9303=VERTEX_POINT('',#78535);
#9304=VERTEX_POINT('',#78536);
#9305=VERTEX_POINT('',#78586);
#9306=VERTEX_POINT('',#78587);
#9307=VERTEX_POINT('',#78634);
#9308=VERTEX_POINT('',#78635);
#9309=VERTEX_POINT('',#78685);
#9310=VERTEX_POINT('',#78686);
#9311=VERTEX_POINT('',#78688);
#9312=VERTEX_POINT('',#78702);
#9313=VERTEX_POINT('',#78724);
#9314=VERTEX_POINT('',#78725);
#9315=VERTEX_POINT('',#78727);
#9316=VERTEX_POINT('',#78736);
#9317=VERTEX_POINT('',#78748);
#9318=VERTEX_POINT('',#78749);
#9319=VERTEX_POINT('',#78772);
#9320=VERTEX_POINT('',#78773);
#9321=VERTEX_POINT('',#78797);
#9322=VERTEX_POINT('',#78798);
#9323=VERTEX_POINT('',#78821);
#9324=VERTEX_POINT('',#78822);
#9325=VERTEX_POINT('',#78846);
#9326=VERTEX_POINT('',#78847);
#9327=VERTEX_POINT('',#78870);
#9328=VERTEX_POINT('',#78871);
#9329=VERTEX_POINT('',#78895);
#9330=VERTEX_POINT('',#78896);
#9331=VERTEX_POINT('',#78920);
#9332=VERTEX_POINT('',#78921);
#9333=VERTEX_POINT('',#78944);
#9334=VERTEX_POINT('',#78945);
#9335=VERTEX_POINT('',#78969);
#9336=VERTEX_POINT('',#78970);
#9337=VERTEX_POINT('',#78993);
#9338=VERTEX_POINT('',#78994);
#9339=VERTEX_POINT('',#79018);
#9340=VERTEX_POINT('',#79019);
#9341=VERTEX_POINT('',#79043);
#9342=VERTEX_POINT('',#79044);
#9343=VERTEX_POINT('',#79067);
#9344=VERTEX_POINT('',#79068);
#9345=VERTEX_POINT('',#79092);
#9346=VERTEX_POINT('',#79093);
#9347=VERTEX_POINT('',#79116);
#9348=VERTEX_POINT('',#79117);
#9349=VERTEX_POINT('',#79141);
#9350=VERTEX_POINT('',#79142);
#9351=VERTEX_POINT('',#79166);
#9352=VERTEX_POINT('',#79167);
#9353=VERTEX_POINT('',#79190);
#9354=VERTEX_POINT('',#79191);
#9355=VERTEX_POINT('',#79193);
#9356=VERTEX_POINT('',#79199);
#9357=VERTEX_POINT('',#79207);
#9358=VERTEX_POINT('',#79208);
#9359=VERTEX_POINT('',#79210);
#9360=VERTEX_POINT('',#79219);
#9361=VERTEX_POINT('',#79231);
#9362=VERTEX_POINT('',#79232);
#9363=VERTEX_POINT('',#79255);
#9364=VERTEX_POINT('',#79256);
#9365=VERTEX_POINT('',#79280);
#9366=VERTEX_POINT('',#79281);
#9367=VERTEX_POINT('',#79304);
#9368=VERTEX_POINT('',#79305);
#9369=VERTEX_POINT('',#79329);
#9370=VERTEX_POINT('',#79330);
#9371=VERTEX_POINT('',#79353);
#9372=VERTEX_POINT('',#79354);
#9373=VERTEX_POINT('',#79378);
#9374=VERTEX_POINT('',#79379);
#9375=VERTEX_POINT('',#79403);
#9376=VERTEX_POINT('',#79404);
#9377=VERTEX_POINT('',#79427);
#9378=VERTEX_POINT('',#79428);
#9379=VERTEX_POINT('',#79452);
#9380=VERTEX_POINT('',#79453);
#9381=VERTEX_POINT('',#79476);
#9382=VERTEX_POINT('',#79477);
#9383=VERTEX_POINT('',#79501);
#9384=VERTEX_POINT('',#79502);
#9385=VERTEX_POINT('',#79526);
#9386=VERTEX_POINT('',#79527);
#9387=VERTEX_POINT('',#79550);
#9388=VERTEX_POINT('',#79551);
#9389=VERTEX_POINT('',#79575);
#9390=VERTEX_POINT('',#79576);
#9391=VERTEX_POINT('',#79599);
#9392=VERTEX_POINT('',#79600);
#9393=VERTEX_POINT('',#79624);
#9394=VERTEX_POINT('',#79625);
#9395=VERTEX_POINT('',#79649);
#9396=VERTEX_POINT('',#79650);
#9397=VERTEX_POINT('',#79673);
#9398=VERTEX_POINT('',#79674);
#9399=VERTEX_POINT('',#79676);
#9400=VERTEX_POINT('',#79682);
#9401=VERTEX_POINT('',#79690);
#9402=VERTEX_POINT('',#79691);
#9403=VERTEX_POINT('',#79693);
#9404=VERTEX_POINT('',#79702);
#9405=VERTEX_POINT('',#79714);
#9406=VERTEX_POINT('',#79715);
#9407=VERTEX_POINT('',#79738);
#9408=VERTEX_POINT('',#79739);
#9409=VERTEX_POINT('',#79763);
#9410=VERTEX_POINT('',#79764);
#9411=VERTEX_POINT('',#79787);
#9412=VERTEX_POINT('',#79788);
#9413=VERTEX_POINT('',#79812);
#9414=VERTEX_POINT('',#79813);
#9415=VERTEX_POINT('',#79836);
#9416=VERTEX_POINT('',#79837);
#9417=VERTEX_POINT('',#79861);
#9418=VERTEX_POINT('',#79862);
#9419=VERTEX_POINT('',#79886);
#9420=VERTEX_POINT('',#79887);
#9421=VERTEX_POINT('',#79910);
#9422=VERTEX_POINT('',#79911);
#9423=VERTEX_POINT('',#79935);
#9424=VERTEX_POINT('',#79936);
#9425=VERTEX_POINT('',#79959);
#9426=VERTEX_POINT('',#79960);
#9427=VERTEX_POINT('',#79984);
#9428=VERTEX_POINT('',#79985);
#9429=VERTEX_POINT('',#80009);
#9430=VERTEX_POINT('',#80010);
#9431=VERTEX_POINT('',#80033);
#9432=VERTEX_POINT('',#80034);
#9433=VERTEX_POINT('',#80058);
#9434=VERTEX_POINT('',#80059);
#9435=VERTEX_POINT('',#80082);
#9436=VERTEX_POINT('',#80083);
#9437=VERTEX_POINT('',#80107);
#9438=VERTEX_POINT('',#80108);
#9439=VERTEX_POINT('',#80132);
#9440=VERTEX_POINT('',#80133);
#9441=VERTEX_POINT('',#80156);
#9442=VERTEX_POINT('',#80157);
#9443=VERTEX_POINT('',#80159);
#9444=VERTEX_POINT('',#80165);
#9445=VERTEX_POINT('',#80173);
#9446=VERTEX_POINT('',#80174);
#9447=VERTEX_POINT('',#80176);
#9448=VERTEX_POINT('',#80185);
#9449=VERTEX_POINT('',#80197);
#9450=VERTEX_POINT('',#80198);
#9451=VERTEX_POINT('',#80221);
#9452=VERTEX_POINT('',#80222);
#9453=VERTEX_POINT('',#80246);
#9454=VERTEX_POINT('',#80247);
#9455=VERTEX_POINT('',#80270);
#9456=VERTEX_POINT('',#80271);
#9457=VERTEX_POINT('',#80295);
#9458=VERTEX_POINT('',#80296);
#9459=VERTEX_POINT('',#80319);
#9460=VERTEX_POINT('',#80320);
#9461=VERTEX_POINT('',#80344);
#9462=VERTEX_POINT('',#80345);
#9463=VERTEX_POINT('',#80369);
#9464=VERTEX_POINT('',#80370);
#9465=VERTEX_POINT('',#80393);
#9466=VERTEX_POINT('',#80394);
#9467=VERTEX_POINT('',#80418);
#9468=VERTEX_POINT('',#80419);
#9469=VERTEX_POINT('',#80442);
#9470=VERTEX_POINT('',#80443);
#9471=VERTEX_POINT('',#80467);
#9472=VERTEX_POINT('',#80468);
#9473=VERTEX_POINT('',#80492);
#9474=VERTEX_POINT('',#80493);
#9475=VERTEX_POINT('',#80516);
#9476=VERTEX_POINT('',#80517);
#9477=VERTEX_POINT('',#80541);
#9478=VERTEX_POINT('',#80542);
#9479=VERTEX_POINT('',#80565);
#9480=VERTEX_POINT('',#80566);
#9481=VERTEX_POINT('',#80590);
#9482=VERTEX_POINT('',#80591);
#9483=VERTEX_POINT('',#80615);
#9484=VERTEX_POINT('',#80616);
#9485=VERTEX_POINT('',#80639);
#9486=VERTEX_POINT('',#80640);
#9487=VERTEX_POINT('',#80642);
#9488=VERTEX_POINT('',#80648);
#9489=VERTEX_POINT('',#80656);
#9490=VERTEX_POINT('',#80657);
#9491=VERTEX_POINT('',#80659);
#9492=VERTEX_POINT('',#80668);
#9493=VERTEX_POINT('',#80680);
#9494=VERTEX_POINT('',#80681);
#9495=VERTEX_POINT('',#80704);
#9496=VERTEX_POINT('',#80705);
#9497=VERTEX_POINT('',#80729);
#9498=VERTEX_POINT('',#80730);
#9499=VERTEX_POINT('',#80753);
#9500=VERTEX_POINT('',#80754);
#9501=VERTEX_POINT('',#80778);
#9502=VERTEX_POINT('',#80779);
#9503=VERTEX_POINT('',#80802);
#9504=VERTEX_POINT('',#80803);
#9505=VERTEX_POINT('',#80827);
#9506=VERTEX_POINT('',#80828);
#9507=VERTEX_POINT('',#80852);
#9508=VERTEX_POINT('',#80853);
#9509=VERTEX_POINT('',#80876);
#9510=VERTEX_POINT('',#80877);
#9511=VERTEX_POINT('',#80901);
#9512=VERTEX_POINT('',#80902);
#9513=VERTEX_POINT('',#80925);
#9514=VERTEX_POINT('',#80926);
#9515=VERTEX_POINT('',#80950);
#9516=VERTEX_POINT('',#80951);
#9517=VERTEX_POINT('',#80975);
#9518=VERTEX_POINT('',#80976);
#9519=VERTEX_POINT('',#80999);
#9520=VERTEX_POINT('',#81000);
#9521=VERTEX_POINT('',#81024);
#9522=VERTEX_POINT('',#81025);
#9523=VERTEX_POINT('',#81048);
#9524=VERTEX_POINT('',#81049);
#9525=VERTEX_POINT('',#81073);
#9526=VERTEX_POINT('',#81074);
#9527=VERTEX_POINT('',#81098);
#9528=VERTEX_POINT('',#81099);
#9529=VERTEX_POINT('',#81122);
#9530=VERTEX_POINT('',#81123);
#9531=VERTEX_POINT('',#81125);
#9532=VERTEX_POINT('',#81131);
#9533=VERTEX_POINT('',#81139);
#9534=VERTEX_POINT('',#81140);
#9535=VERTEX_POINT('',#81142);
#9536=VERTEX_POINT('',#81151);
#9537=VERTEX_POINT('',#81163);
#9538=VERTEX_POINT('',#81164);
#9539=VERTEX_POINT('',#81187);
#9540=VERTEX_POINT('',#81188);
#9541=VERTEX_POINT('',#81212);
#9542=VERTEX_POINT('',#81213);
#9543=VERTEX_POINT('',#81236);
#9544=VERTEX_POINT('',#81237);
#9545=VERTEX_POINT('',#81261);
#9546=VERTEX_POINT('',#81262);
#9547=VERTEX_POINT('',#81285);
#9548=VERTEX_POINT('',#81286);
#9549=VERTEX_POINT('',#81310);
#9550=VERTEX_POINT('',#81311);
#9551=VERTEX_POINT('',#81335);
#9552=VERTEX_POINT('',#81336);
#9553=VERTEX_POINT('',#81359);
#9554=VERTEX_POINT('',#81360);
#9555=VERTEX_POINT('',#81384);
#9556=VERTEX_POINT('',#81385);
#9557=VERTEX_POINT('',#81408);
#9558=VERTEX_POINT('',#81409);
#9559=VERTEX_POINT('',#81433);
#9560=VERTEX_POINT('',#81434);
#9561=VERTEX_POINT('',#81458);
#9562=VERTEX_POINT('',#81459);
#9563=VERTEX_POINT('',#81482);
#9564=VERTEX_POINT('',#81483);
#9565=VERTEX_POINT('',#81507);
#9566=VERTEX_POINT('',#81508);
#9567=VERTEX_POINT('',#81531);
#9568=VERTEX_POINT('',#81532);
#9569=VERTEX_POINT('',#81556);
#9570=VERTEX_POINT('',#81557);
#9571=VERTEX_POINT('',#81581);
#9572=VERTEX_POINT('',#81582);
#9573=VERTEX_POINT('',#81605);
#9574=VERTEX_POINT('',#81606);
#9575=VERTEX_POINT('',#81608);
#9576=VERTEX_POINT('',#81614);
#9577=VERTEX_POINT('',#83115);
#9578=VERTEX_POINT('',#83116);
#9579=VERTEX_POINT('',#83118);
#9580=VERTEX_POINT('',#83120);
#9581=VERTEX_POINT('',#90595);
#9582=VERTEX_POINT('',#90596);
#9583=VERTEX_POINT('',#90601);
#9584=VERTEX_POINT('',#90605);
#9585=VERTEX_POINT('',#90613);
#9586=VERTEX_POINT('',#90614);
#9587=VERTEX_POINT('',#90616);
#9588=VERTEX_POINT('',#90627);
#9589=VERTEX_POINT('',#90637);
#9590=VERTEX_POINT('',#90638);
#9591=VERTEX_POINT('',#90685);
#9592=VERTEX_POINT('',#90686);
#9593=VERTEX_POINT('',#90733);
#9594=VERTEX_POINT('',#90734);
#9595=VERTEX_POINT('',#90781);
#9596=VERTEX_POINT('',#90782);
#9597=VERTEX_POINT('',#90835);
#9598=VERTEX_POINT('',#90836);
#9599=VERTEX_POINT('',#90883);
#9600=VERTEX_POINT('',#90884);
#9601=VERTEX_POINT('',#90931);
#9602=VERTEX_POINT('',#90932);
#9603=VERTEX_POINT('',#90985);
#9604=VERTEX_POINT('',#90986);
#9605=VERTEX_POINT('',#91033);
#9606=VERTEX_POINT('',#91034);
#9607=VERTEX_POINT('',#91081);
#9608=VERTEX_POINT('',#91082);
#9609=VERTEX_POINT('',#91129);
#9610=VERTEX_POINT('',#91130);
#9611=VERTEX_POINT('',#91183);
#9612=VERTEX_POINT('',#91184);
#9613=VERTEX_POINT('',#91231);
#9614=VERTEX_POINT('',#91232);
#9615=VERTEX_POINT('',#91279);
#9616=VERTEX_POINT('',#91280);
#9617=VERTEX_POINT('',#91333);
#9618=VERTEX_POINT('',#91334);
#9619=VERTEX_POINT('',#91381);
#9620=VERTEX_POINT('',#91382);
#9621=VERTEX_POINT('',#91429);
#9622=VERTEX_POINT('',#91430);
#9623=VERTEX_POINT('',#91477);
#9624=VERTEX_POINT('',#91478);
#9625=VERTEX_POINT('',#91531);
#9626=VERTEX_POINT('',#91532);
#9627=VERTEX_POINT('',#91579);
#9628=VERTEX_POINT('',#91580);
#9629=VERTEX_POINT('',#91627);
#9630=VERTEX_POINT('',#91628);
#9631=VERTEX_POINT('',#91681);
#9632=VERTEX_POINT('',#91682);
#9633=VERTEX_POINT('',#91729);
#9634=VERTEX_POINT('',#91730);
#9635=VERTEX_POINT('',#91777);
#9636=VERTEX_POINT('',#91778);
#9637=VERTEX_POINT('',#91825);
#9638=VERTEX_POINT('',#91826);
#9639=VERTEX_POINT('',#91879);
#9640=VERTEX_POINT('',#91880);
#9641=VERTEX_POINT('',#91927);
#9642=VERTEX_POINT('',#91928);
#9643=VERTEX_POINT('',#91975);
#9644=VERTEX_POINT('',#91976);
#9645=VERTEX_POINT('',#92029);
#9646=VERTEX_POINT('',#92030);
#9647=VERTEX_POINT('',#92077);
#9648=VERTEX_POINT('',#92078);
#9649=VERTEX_POINT('',#92125);
#9650=VERTEX_POINT('',#92126);
#9651=VERTEX_POINT('',#92173);
#9652=VERTEX_POINT('',#92174);
#9653=VERTEX_POINT('',#92227);
#9654=VERTEX_POINT('',#92228);
#9655=VERTEX_POINT('',#92275);
#9656=VERTEX_POINT('',#92276);
#9657=VERTEX_POINT('',#92323);
#9658=VERTEX_POINT('',#92324);
#9659=VERTEX_POINT('',#92377);
#9660=VERTEX_POINT('',#92378);
#9661=VERTEX_POINT('',#92425);
#9662=VERTEX_POINT('',#92426);
#9663=VERTEX_POINT('',#92473);
#9664=VERTEX_POINT('',#92474);
#9665=VERTEX_POINT('',#92521);
#9666=VERTEX_POINT('',#92522);
#9667=VERTEX_POINT('',#92575);
#9668=VERTEX_POINT('',#92576);
#9669=VERTEX_POINT('',#92623);
#9670=VERTEX_POINT('',#92624);
#9671=VERTEX_POINT('',#92671);
#9672=VERTEX_POINT('',#92672);
#9673=VERTEX_POINT('',#92725);
#9674=VERTEX_POINT('',#92726);
#9675=VERTEX_POINT('',#92773);
#9676=VERTEX_POINT('',#92774);
#9677=VERTEX_POINT('',#92821);
#9678=VERTEX_POINT('',#92822);
#9679=VERTEX_POINT('',#92869);
#9680=VERTEX_POINT('',#92870);
#9681=VERTEX_POINT('',#92920);
#9682=VERTEX_POINT('',#92921);
#9683=VERTEX_POINT('',#92968);
#9684=VERTEX_POINT('',#92969);
#9685=VERTEX_POINT('',#93016);
#9686=VERTEX_POINT('',#93017);
#9687=VERTEX_POINT('',#93019);
#9688=VERTEX_POINT('',#93030);
#9689=VERTEX_POINT('',#93041);
#9690=VERTEX_POINT('',#93042);
#9691=VERTEX_POINT('',#93066);
#9692=VERTEX_POINT('',#93067);
#9693=VERTEX_POINT('',#93090);
#9694=VERTEX_POINT('',#93091);
#9695=VERTEX_POINT('',#93115);
#9696=VERTEX_POINT('',#93116);
#9697=VERTEX_POINT('',#93140);
#9698=VERTEX_POINT('',#93141);
#9699=VERTEX_POINT('',#93164);
#9700=VERTEX_POINT('',#93165);
#9701=VERTEX_POINT('',#93188);
#9702=VERTEX_POINT('',#93189);
#9703=VERTEX_POINT('',#93213);
#9704=VERTEX_POINT('',#93214);
#9705=VERTEX_POINT('',#93238);
#9706=VERTEX_POINT('',#93239);
#9707=VERTEX_POINT('',#93262);
#9708=VERTEX_POINT('',#93263);
#9709=VERTEX_POINT('',#93287);
#9710=VERTEX_POINT('',#93288);
#9711=VERTEX_POINT('',#93312);
#9712=VERTEX_POINT('',#93313);
#9713=VERTEX_POINT('',#93336);
#9714=VERTEX_POINT('',#93337);
#9715=VERTEX_POINT('',#93360);
#9716=VERTEX_POINT('',#93361);
#9717=VERTEX_POINT('',#93385);
#9718=VERTEX_POINT('',#93386);
#9719=VERTEX_POINT('',#93410);
#9720=VERTEX_POINT('',#93411);
#9721=VERTEX_POINT('',#93434);
#9722=VERTEX_POINT('',#93435);
#9723=VERTEX_POINT('',#93459);
#9724=VERTEX_POINT('',#93460);
#9725=VERTEX_POINT('',#93484);
#9726=VERTEX_POINT('',#93485);
#9727=VERTEX_POINT('',#93508);
#9728=VERTEX_POINT('',#93509);
#9729=VERTEX_POINT('',#93532);
#9730=VERTEX_POINT('',#93533);
#9731=VERTEX_POINT('',#93557);
#9732=VERTEX_POINT('',#93558);
#9733=VERTEX_POINT('',#93582);
#9734=VERTEX_POINT('',#93583);
#9735=VERTEX_POINT('',#93606);
#9736=VERTEX_POINT('',#93607);
#9737=VERTEX_POINT('',#93631);
#9738=VERTEX_POINT('',#93632);
#9739=VERTEX_POINT('',#93656);
#9740=VERTEX_POINT('',#93657);
#9741=VERTEX_POINT('',#93680);
#9742=VERTEX_POINT('',#93681);
#9743=VERTEX_POINT('',#93704);
#9744=VERTEX_POINT('',#93705);
#9745=VERTEX_POINT('',#93729);
#9746=VERTEX_POINT('',#93730);
#9747=VERTEX_POINT('',#93754);
#9748=VERTEX_POINT('',#93755);
#9749=VERTEX_POINT('',#93778);
#9750=VERTEX_POINT('',#93779);
#9751=VERTEX_POINT('',#93803);
#9752=VERTEX_POINT('',#93804);
#9753=VERTEX_POINT('',#93828);
#9754=VERTEX_POINT('',#93829);
#9755=VERTEX_POINT('',#93852);
#9756=VERTEX_POINT('',#93853);
#9757=VERTEX_POINT('',#93876);
#9758=VERTEX_POINT('',#93877);
#9759=VERTEX_POINT('',#93901);
#9760=VERTEX_POINT('',#93902);
#9761=VERTEX_POINT('',#93926);
#9762=VERTEX_POINT('',#93927);
#9763=VERTEX_POINT('',#93950);
#9764=VERTEX_POINT('',#93951);
#9765=VERTEX_POINT('',#93975);
#9766=VERTEX_POINT('',#93976);
#9767=VERTEX_POINT('',#94000);
#9768=VERTEX_POINT('',#94001);
#9769=VERTEX_POINT('',#94024);
#9770=VERTEX_POINT('',#94025);
#9771=VERTEX_POINT('',#94048);
#9772=VERTEX_POINT('',#94049);
#9773=VERTEX_POINT('',#94073);
#9774=VERTEX_POINT('',#94074);
#9775=VERTEX_POINT('',#94098);
#9776=VERTEX_POINT('',#94099);
#9777=VERTEX_POINT('',#94122);
#9778=VERTEX_POINT('',#94123);
#9779=VERTEX_POINT('',#94147);
#9780=VERTEX_POINT('',#94148);
#9781=VERTEX_POINT('',#94172);
#9782=VERTEX_POINT('',#94173);
#9783=VERTEX_POINT('',#94196);
#9784=VERTEX_POINT('',#94197);
#9785=VERTEX_POINT('',#94220);
#9786=VERTEX_POINT('',#94441);
#9787=VERTEX_POINT('',#94506);
#9788=VERTEX_POINT('',#94539);
#9789=VERTEX_POINT('',#95802);
#9790=VERTEX_POINT('',#95925);
#9791=VERTEX_POINT('',#97316);
#9792=VERTEX_POINT('',#97317);
#9793=VERTEX_POINT('',#97319);
#9794=VERTEX_POINT('',#97321);
#9795=VERTEX_POINT('',#97325);
#9796=VERTEX_POINT('',#97327);
#9797=VERTEX_POINT('',#97331);
#9798=VERTEX_POINT('',#97333);
#9799=VERTEX_POINT('',#97337);
#9800=VERTEX_POINT('',#97339);
#9801=VERTEX_POINT('',#97343);
#9802=VERTEX_POINT('',#97345);
#9803=VERTEX_POINT('',#97353);
#9804=VERTEX_POINT('',#97356);
#9805=VERTEX_POINT('',#97363);
#9806=VERTEX_POINT('',#97365);
#9807=VERTEX_POINT('',#97369);
#9808=VERTEX_POINT('',#97371);
#9809=VERTEX_POINT('',#97378);
#9810=VERTEX_POINT('',#97380);
#9811=VERTEX_POINT('',#97384);
#9812=VERTEX_POINT('',#97386);
#9813=EDGE_CURVE('',#7613,#7613,#7364,.T.);
#9814=EDGE_CURVE('',#7613,#7614,#4936,.T.);
#9815=EDGE_CURVE('',#7614,#7614,#7365,.T.);
#9816=EDGE_CURVE('',#7615,#7615,#7366,.T.);
#9817=EDGE_CURVE('',#7615,#7616,#4937,.T.);
#9818=EDGE_CURVE('',#7616,#7616,#7367,.T.);
#9819=EDGE_CURVE('',#7617,#7617,#7368,.T.);
#9820=EDGE_CURVE('',#7617,#7618,#4938,.T.);
#9821=EDGE_CURVE('',#7618,#7618,#7369,.T.);
#9822=EDGE_CURVE('',#7619,#7619,#7370,.T.);
#9823=EDGE_CURVE('',#7619,#7620,#4939,.T.);
#9824=EDGE_CURVE('',#7620,#7620,#7371,.T.);
#9825=EDGE_CURVE('',#7621,#7621,#7372,.T.);
#9826=EDGE_CURVE('',#7621,#7622,#4940,.T.);
#9827=EDGE_CURVE('',#7622,#7622,#7373,.T.);
#9828=EDGE_CURVE('',#7623,#7623,#7374,.T.);
#9829=EDGE_CURVE('',#7623,#7624,#4941,.T.);
#9830=EDGE_CURVE('',#7624,#7624,#7375,.T.);
#9831=EDGE_CURVE('',#7625,#7626,#4942,.T.);
#9832=EDGE_CURVE('',#7626,#7627,#4943,.T.);
#9833=EDGE_CURVE('',#7628,#7627,#4944,.T.);
#9834=EDGE_CURVE('',#7625,#7628,#4945,.T.);
#9835=EDGE_CURVE('',#7629,#7625,#4946,.T.);
#9836=EDGE_CURVE('',#7630,#7628,#4947,.T.);
#9837=EDGE_CURVE('',#7629,#7630,#4948,.T.);
#9838=EDGE_CURVE('',#7631,#7629,#4949,.T.);
#9839=EDGE_CURVE('',#7632,#7630,#4950,.T.);
#9840=EDGE_CURVE('',#7631,#7632,#4951,.T.);
#9841=EDGE_CURVE('',#7626,#7631,#4952,.T.);
#9842=EDGE_CURVE('',#7627,#7632,#4953,.T.);
#9843=EDGE_CURVE('',#7633,#7634,#4954,.T.);
#9844=EDGE_CURVE('',#7634,#7635,#4955,.T.);
#9845=EDGE_CURVE('',#7636,#7635,#4956,.T.);
#9846=EDGE_CURVE('',#7633,#7636,#4957,.T.);
#9847=EDGE_CURVE('',#7637,#7633,#4958,.T.);
#9848=EDGE_CURVE('',#7638,#7636,#4959,.T.);
#9849=EDGE_CURVE('',#7637,#7638,#4960,.T.);
#9850=EDGE_CURVE('',#7639,#7637,#4961,.T.);
#9851=EDGE_CURVE('',#7640,#7638,#4962,.T.);
#9852=EDGE_CURVE('',#7639,#7640,#4963,.T.);
#9853=EDGE_CURVE('',#7634,#7639,#4964,.T.);
#9854=EDGE_CURVE('',#7635,#7640,#4965,.T.);
#9855=EDGE_CURVE('',#7641,#7642,#4966,.T.);
#9856=EDGE_CURVE('',#7642,#7643,#4967,.T.);
#9857=EDGE_CURVE('',#7644,#7643,#4968,.T.);
#9858=EDGE_CURVE('',#7641,#7644,#4969,.T.);
#9859=EDGE_CURVE('',#7645,#7641,#4970,.T.);
#9860=EDGE_CURVE('',#7646,#7644,#4971,.T.);
#9861=EDGE_CURVE('',#7645,#7646,#4972,.T.);
#9862=EDGE_CURVE('',#7647,#7645,#4973,.T.);
#9863=EDGE_CURVE('',#7648,#7646,#4974,.T.);
#9864=EDGE_CURVE('',#7647,#7648,#4975,.T.);
#9865=EDGE_CURVE('',#7642,#7647,#4976,.T.);
#9866=EDGE_CURVE('',#7643,#7648,#4977,.T.);
#9867=EDGE_CURVE('',#7649,#7650,#4978,.T.);
#9868=EDGE_CURVE('',#7650,#7651,#4979,.T.);
#9869=EDGE_CURVE('',#7652,#7651,#4980,.T.);
#9870=EDGE_CURVE('',#7649,#7652,#4981,.T.);
#9871=EDGE_CURVE('',#7653,#7649,#4982,.T.);
#9872=EDGE_CURVE('',#7654,#7652,#4983,.T.);
#9873=EDGE_CURVE('',#7653,#7654,#4984,.T.);
#9874=EDGE_CURVE('',#7655,#7653,#4985,.T.);
#9875=EDGE_CURVE('',#7656,#7654,#4986,.T.);
#9876=EDGE_CURVE('',#7655,#7656,#4987,.T.);
#9877=EDGE_CURVE('',#7650,#7655,#4988,.T.);
#9878=EDGE_CURVE('',#7651,#7656,#4989,.T.);
#9879=EDGE_CURVE('',#7657,#7658,#4990,.T.);
#9880=EDGE_CURVE('',#7658,#7659,#376,.T.);
#9881=EDGE_CURVE('',#7660,#7659,#7376,.F.);
#9882=EDGE_CURVE('',#7660,#7657,#377,.T.);
#9883=EDGE_CURVE('',#7661,#7662,#4991,.T.);
#9884=EDGE_CURVE('',#7662,#7658,#378,.T.);
#9885=EDGE_CURVE('',#7657,#7661,#379,.T.);
#9886=EDGE_CURVE('',#7663,#7664,#4992,.T.);
#9887=EDGE_CURVE('',#7664,#7662,#380,.T.);
#9888=EDGE_CURVE('',#7661,#7663,#381,.T.);
#9889=EDGE_CURVE('',#7665,#7666,#4993,.T.);
#9890=EDGE_CURVE('',#7666,#7664,#382,.T.);
#9891=EDGE_CURVE('',#7663,#7665,#383,.T.);
#9892=EDGE_CURVE('',#7667,#7668,#4994,.T.);
#9893=EDGE_CURVE('',#7668,#7666,#384,.T.);
#9894=EDGE_CURVE('',#7665,#7667,#385,.T.);
#9895=EDGE_CURVE('',#7669,#7670,#4995,.T.);
#9896=EDGE_CURVE('',#7670,#7668,#386,.T.);
#9897=EDGE_CURVE('',#7667,#7669,#387,.T.);
#9898=EDGE_CURVE('',#7671,#7672,#4996,.T.);
#9899=EDGE_CURVE('',#7672,#7670,#388,.T.);
#9900=EDGE_CURVE('',#7669,#7671,#389,.T.);
#9901=EDGE_CURVE('',#7673,#7674,#4997,.T.);
#9902=EDGE_CURVE('',#7673,#7675,#390,.T.);
#9903=EDGE_CURVE('',#7676,#7675,#7377,.T.);
#9904=EDGE_CURVE('',#7676,#7674,#391,.T.);
#9905=EDGE_CURVE('',#7677,#7678,#4998,.T.);
#9906=EDGE_CURVE('',#7678,#7679,#392,.T.);
#9907=EDGE_CURVE('',#7680,#7679,#7378,.F.);
#9908=EDGE_CURVE('',#7680,#7677,#393,.T.);
#9909=EDGE_CURVE('',#7681,#7682,#4999,.T.);
#9910=EDGE_CURVE('',#7682,#7678,#394,.T.);
#9911=EDGE_CURVE('',#7677,#7681,#395,.T.);
#9912=EDGE_CURVE('',#7683,#7684,#5000,.T.);
#9913=EDGE_CURVE('',#7684,#7682,#396,.T.);
#9914=EDGE_CURVE('',#7681,#7683,#397,.T.);
#9915=EDGE_CURVE('',#7685,#7686,#5001,.T.);
#9916=EDGE_CURVE('',#7686,#7684,#398,.T.);
#9917=EDGE_CURVE('',#7683,#7685,#399,.T.);
#9918=EDGE_CURVE('',#7687,#7688,#5002,.T.);
#9919=EDGE_CURVE('',#7688,#7686,#400,.T.);
#9920=EDGE_CURVE('',#7685,#7687,#401,.T.);
#9921=EDGE_CURVE('',#7689,#7690,#5003,.T.);
#9922=EDGE_CURVE('',#7690,#7688,#402,.T.);
#9923=EDGE_CURVE('',#7687,#7689,#403,.T.);
#9924=EDGE_CURVE('',#7691,#7692,#5004,.T.);
#9925=EDGE_CURVE('',#7692,#7690,#404,.T.);
#9926=EDGE_CURVE('',#7689,#7691,#405,.T.);
#9927=EDGE_CURVE('',#7693,#7694,#5005,.T.);
#9928=EDGE_CURVE('',#7693,#7695,#406,.T.);
#9929=EDGE_CURVE('',#7696,#7695,#7379,.T.);
#9930=EDGE_CURVE('',#7696,#7694,#407,.T.);
#9931=EDGE_CURVE('',#7697,#7698,#5006,.T.);
#9932=EDGE_CURVE('',#7698,#7699,#408,.T.);
#9933=EDGE_CURVE('',#7700,#7699,#7380,.F.);
#9934=EDGE_CURVE('',#7700,#7697,#409,.T.);
#9935=EDGE_CURVE('',#7701,#7702,#5007,.T.);
#9936=EDGE_CURVE('',#7702,#7698,#410,.T.);
#9937=EDGE_CURVE('',#7697,#7701,#411,.T.);
#9938=EDGE_CURVE('',#7703,#7704,#5008,.T.);
#9939=EDGE_CURVE('',#7704,#7702,#412,.T.);
#9940=EDGE_CURVE('',#7701,#7703,#413,.T.);
#9941=EDGE_CURVE('',#7705,#7706,#5009,.T.);
#9942=EDGE_CURVE('',#7706,#7704,#414,.T.);
#9943=EDGE_CURVE('',#7703,#7705,#415,.T.);
#9944=EDGE_CURVE('',#7707,#7708,#5010,.T.);
#9945=EDGE_CURVE('',#7708,#7706,#416,.T.);
#9946=EDGE_CURVE('',#7705,#7707,#417,.T.);
#9947=EDGE_CURVE('',#7709,#7710,#5011,.T.);
#9948=EDGE_CURVE('',#7710,#7708,#418,.T.);
#9949=EDGE_CURVE('',#7707,#7709,#419,.T.);
#9950=EDGE_CURVE('',#7711,#7712,#5012,.T.);
#9951=EDGE_CURVE('',#7712,#7710,#420,.T.);
#9952=EDGE_CURVE('',#7709,#7711,#421,.T.);
#9953=EDGE_CURVE('',#7713,#7714,#5013,.T.);
#9954=EDGE_CURVE('',#7713,#7715,#422,.T.);
#9955=EDGE_CURVE('',#7716,#7715,#7381,.T.);
#9956=EDGE_CURVE('',#7716,#7714,#423,.T.);
#9957=EDGE_CURVE('',#7717,#7718,#5014,.T.);
#9958=EDGE_CURVE('',#7718,#7719,#424,.T.);
#9959=EDGE_CURVE('',#7720,#7719,#7382,.F.);
#9960=EDGE_CURVE('',#7720,#7717,#425,.T.);
#9961=EDGE_CURVE('',#7721,#7722,#5015,.T.);
#9962=EDGE_CURVE('',#7722,#7718,#426,.T.);
#9963=EDGE_CURVE('',#7717,#7721,#427,.T.);
#9964=EDGE_CURVE('',#7723,#7724,#5016,.T.);
#9965=EDGE_CURVE('',#7724,#7722,#428,.T.);
#9966=EDGE_CURVE('',#7721,#7723,#429,.T.);
#9967=EDGE_CURVE('',#7725,#7726,#5017,.T.);
#9968=EDGE_CURVE('',#7726,#7724,#430,.T.);
#9969=EDGE_CURVE('',#7723,#7725,#431,.T.);
#9970=EDGE_CURVE('',#7727,#7728,#5018,.T.);
#9971=EDGE_CURVE('',#7728,#7726,#432,.T.);
#9972=EDGE_CURVE('',#7725,#7727,#433,.T.);
#9973=EDGE_CURVE('',#7729,#7730,#5019,.T.);
#9974=EDGE_CURVE('',#7730,#7728,#434,.T.);
#9975=EDGE_CURVE('',#7727,#7729,#435,.T.);
#9976=EDGE_CURVE('',#7731,#7732,#5020,.T.);
#9977=EDGE_CURVE('',#7732,#7730,#436,.T.);
#9978=EDGE_CURVE('',#7729,#7731,#437,.T.);
#9979=EDGE_CURVE('',#7733,#7734,#5021,.T.);
#9980=EDGE_CURVE('',#7733,#7735,#438,.T.);
#9981=EDGE_CURVE('',#7736,#7735,#7383,.T.);
#9982=EDGE_CURVE('',#7736,#7734,#439,.T.);
#9983=EDGE_CURVE('',#7737,#7738,#5022,.T.);
#9984=EDGE_CURVE('',#7738,#7739,#440,.T.);
#9985=EDGE_CURVE('',#7740,#7739,#7384,.T.);
#9986=EDGE_CURVE('',#7737,#7740,#441,.T.);
#9987=EDGE_CURVE('',#7741,#7742,#5023,.T.);
#9988=EDGE_CURVE('',#7742,#7738,#442,.T.);
#9989=EDGE_CURVE('',#7741,#7737,#443,.T.);
#9990=EDGE_CURVE('',#7743,#7744,#5024,.T.);
#9991=EDGE_CURVE('',#7744,#7742,#444,.T.);
#9992=EDGE_CURVE('',#7743,#7741,#445,.T.);
#9993=EDGE_CURVE('',#7745,#7746,#5025,.T.);
#9994=EDGE_CURVE('',#7746,#7744,#446,.T.);
#9995=EDGE_CURVE('',#7745,#7743,#447,.T.);
#9996=EDGE_CURVE('',#7747,#7748,#5026,.T.);
#9997=EDGE_CURVE('',#7748,#7746,#448,.T.);
#9998=EDGE_CURVE('',#7747,#7745,#449,.T.);
#9999=EDGE_CURVE('',#7749,#7750,#5027,.T.);
#10000=EDGE_CURVE('',#7750,#7748,#450,.T.);
#10001=EDGE_CURVE('',#7749,#7747,#451,.T.);
#10002=EDGE_CURVE('',#7751,#7752,#5028,.T.);
#10003=EDGE_CURVE('',#7752,#7750,#452,.T.);
#10004=EDGE_CURVE('',#7751,#7749,#453,.T.);
#10005=EDGE_CURVE('',#7753,#7754,#5029,.T.);
#10006=EDGE_CURVE('',#7755,#7753,#454,.T.);
#10007=EDGE_CURVE('',#7756,#7755,#7385,.T.);
#10008=EDGE_CURVE('',#7756,#7754,#455,.T.);
#10009=EDGE_CURVE('',#7757,#7758,#5030,.T.);
#10010=EDGE_CURVE('',#7758,#7759,#456,.T.);
#10011=EDGE_CURVE('',#7760,#7759,#7386,.T.);
#10012=EDGE_CURVE('',#7757,#7760,#457,.T.);
#10013=EDGE_CURVE('',#7761,#7762,#5031,.T.);
#10014=EDGE_CURVE('',#7762,#7758,#458,.T.);
#10015=EDGE_CURVE('',#7761,#7757,#459,.T.);
#10016=EDGE_CURVE('',#7763,#7764,#5032,.T.);
#10017=EDGE_CURVE('',#7764,#7762,#460,.T.);
#10018=EDGE_CURVE('',#7763,#7761,#461,.T.);
#10019=EDGE_CURVE('',#7765,#7766,#5033,.T.);
#10020=EDGE_CURVE('',#7766,#7764,#462,.T.);
#10021=EDGE_CURVE('',#7765,#7763,#463,.T.);
#10022=EDGE_CURVE('',#7767,#7768,#5034,.T.);
#10023=EDGE_CURVE('',#7768,#7766,#464,.T.);
#10024=EDGE_CURVE('',#7767,#7765,#465,.T.);
#10025=EDGE_CURVE('',#7769,#7770,#5035,.T.);
#10026=EDGE_CURVE('',#7770,#7768,#466,.T.);
#10027=EDGE_CURVE('',#7769,#7767,#467,.T.);
#10028=EDGE_CURVE('',#7771,#7772,#5036,.T.);
#10029=EDGE_CURVE('',#7772,#7770,#468,.T.);
#10030=EDGE_CURVE('',#7771,#7769,#469,.T.);
#10031=EDGE_CURVE('',#7773,#7774,#5037,.T.);
#10032=EDGE_CURVE('',#7775,#7773,#470,.T.);
#10033=EDGE_CURVE('',#7776,#7775,#7387,.T.);
#10034=EDGE_CURVE('',#7776,#7774,#471,.T.);
#10035=EDGE_CURVE('',#7777,#7778,#5038,.T.);
#10036=EDGE_CURVE('',#7778,#7779,#472,.T.);
#10037=EDGE_CURVE('',#7780,#7779,#7388,.T.);
#10038=EDGE_CURVE('',#7777,#7780,#473,.T.);
#10039=EDGE_CURVE('',#7781,#7782,#5039,.T.);
#10040=EDGE_CURVE('',#7782,#7778,#474,.T.);
#10041=EDGE_CURVE('',#7781,#7777,#475,.T.);
#10042=EDGE_CURVE('',#7783,#7784,#5040,.T.);
#10043=EDGE_CURVE('',#7784,#7782,#476,.T.);
#10044=EDGE_CURVE('',#7783,#7781,#477,.T.);
#10045=EDGE_CURVE('',#7785,#7786,#5041,.T.);
#10046=EDGE_CURVE('',#7786,#7784,#478,.T.);
#10047=EDGE_CURVE('',#7785,#7783,#479,.T.);
#10048=EDGE_CURVE('',#7787,#7788,#5042,.T.);
#10049=EDGE_CURVE('',#7788,#7786,#480,.T.);
#10050=EDGE_CURVE('',#7787,#7785,#481,.T.);
#10051=EDGE_CURVE('',#7789,#7790,#5043,.T.);
#10052=EDGE_CURVE('',#7790,#7788,#482,.T.);
#10053=EDGE_CURVE('',#7789,#7787,#483,.T.);
#10054=EDGE_CURVE('',#7791,#7792,#5044,.T.);
#10055=EDGE_CURVE('',#7792,#7790,#484,.T.);
#10056=EDGE_CURVE('',#7791,#7789,#485,.T.);
#10057=EDGE_CURVE('',#7793,#7794,#5045,.T.);
#10058=EDGE_CURVE('',#7795,#7793,#486,.T.);
#10059=EDGE_CURVE('',#7796,#7795,#7389,.T.);
#10060=EDGE_CURVE('',#7796,#7794,#487,.T.);
#10061=EDGE_CURVE('',#7797,#7798,#5046,.T.);
#10062=EDGE_CURVE('',#7798,#7799,#488,.T.);
#10063=EDGE_CURVE('',#7800,#7799,#7390,.T.);
#10064=EDGE_CURVE('',#7797,#7800,#489,.T.);
#10065=EDGE_CURVE('',#7801,#7802,#5047,.T.);
#10066=EDGE_CURVE('',#7802,#7798,#490,.T.);
#10067=EDGE_CURVE('',#7801,#7797,#491,.T.);
#10068=EDGE_CURVE('',#7803,#7804,#5048,.T.);
#10069=EDGE_CURVE('',#7804,#7802,#492,.T.);
#10070=EDGE_CURVE('',#7803,#7801,#493,.T.);
#10071=EDGE_CURVE('',#7805,#7806,#5049,.T.);
#10072=EDGE_CURVE('',#7806,#7804,#494,.T.);
#10073=EDGE_CURVE('',#7805,#7803,#495,.T.);
#10074=EDGE_CURVE('',#7807,#7808,#5050,.T.);
#10075=EDGE_CURVE('',#7808,#7806,#496,.T.);
#10076=EDGE_CURVE('',#7807,#7805,#497,.T.);
#10077=EDGE_CURVE('',#7809,#7810,#5051,.T.);
#10078=EDGE_CURVE('',#7810,#7808,#498,.T.);
#10079=EDGE_CURVE('',#7809,#7807,#499,.T.);
#10080=EDGE_CURVE('',#7811,#7812,#5052,.T.);
#10081=EDGE_CURVE('',#7812,#7810,#500,.T.);
#10082=EDGE_CURVE('',#7811,#7809,#501,.T.);
#10083=EDGE_CURVE('',#7813,#7814,#5053,.T.);
#10084=EDGE_CURVE('',#7815,#7813,#502,.T.);
#10085=EDGE_CURVE('',#7816,#7815,#7391,.T.);
#10086=EDGE_CURVE('',#7816,#7814,#503,.T.);
#10087=EDGE_CURVE('',#7814,#7812,#504,.T.);
#10088=EDGE_CURVE('',#7813,#7811,#505,.T.);
#10089=EDGE_CURVE('',#7799,#7660,#506,.T.);
#10090=EDGE_CURVE('',#7675,#7816,#507,.T.);
#10091=EDGE_CURVE('',#7671,#7673,#508,.T.);
#10092=EDGE_CURVE('',#7659,#7800,#509,.T.);
#10093=EDGE_CURVE('',#7674,#7672,#510,.T.);
#10094=EDGE_CURVE('',#7815,#7676,#511,.T.);
#10095=EDGE_CURVE('',#7817,#7818,#5054,.T.);
#10096=EDGE_CURVE('',#7818,#7819,#5055,.T.);
#10097=EDGE_CURVE('',#7819,#7820,#5056,.T.);
#10098=EDGE_CURVE('',#7820,#7817,#5057,.T.);
#10099=EDGE_CURVE('',#7735,#7776,#512,.T.);
#10100=EDGE_CURVE('',#7775,#7736,#513,.T.);
#10101=EDGE_CURVE('',#7715,#7796,#514,.T.);
#10102=EDGE_CURVE('',#7795,#7716,#515,.T.);
#10103=EDGE_CURVE('',#7695,#7756,#516,.T.);
#10104=EDGE_CURVE('',#7755,#7696,#517,.T.);
#10105=EDGE_CURVE('',#7794,#7792,#518,.T.);
#10106=EDGE_CURVE('',#7793,#7791,#519,.T.);
#10107=EDGE_CURVE('',#7779,#7700,#520,.T.);
#10108=EDGE_CURVE('',#7711,#7713,#521,.T.);
#10109=EDGE_CURVE('',#7699,#7780,#522,.T.);
#10110=EDGE_CURVE('',#7714,#7712,#523,.T.);
#10111=EDGE_CURVE('',#7774,#7772,#524,.T.);
#10112=EDGE_CURVE('',#7773,#7771,#525,.T.);
#10113=EDGE_CURVE('',#7759,#7720,#526,.T.);
#10114=EDGE_CURVE('',#7731,#7733,#527,.T.);
#10115=EDGE_CURVE('',#7719,#7760,#528,.T.);
#10116=EDGE_CURVE('',#7734,#7732,#529,.T.);
#10117=EDGE_CURVE('',#7754,#7752,#530,.T.);
#10118=EDGE_CURVE('',#7753,#7751,#531,.T.);
#10119=EDGE_CURVE('',#7739,#7680,#532,.T.);
#10120=EDGE_CURVE('',#7691,#7693,#533,.T.);
#10121=EDGE_CURVE('',#7679,#7740,#534,.T.);
#10122=EDGE_CURVE('',#7694,#7692,#535,.T.);
#10123=EDGE_CURVE('',#7821,#7822,#5058,.T.);
#10124=EDGE_CURVE('',#7822,#7817,#5059,.T.);
#10125=EDGE_CURVE('',#7821,#7820,#5060,.T.);
#10126=EDGE_CURVE('',#7823,#7821,#5061,.T.);
#10127=EDGE_CURVE('',#7823,#7819,#5062,.T.);
#10128=EDGE_CURVE('',#7824,#7823,#5063,.T.);
#10129=EDGE_CURVE('',#7824,#7818,#5064,.T.);
#10130=EDGE_CURVE('',#7822,#7824,#5065,.T.);
#10131=EDGE_CURVE('',#7825,#7826,#5066,.T.);
#10132=EDGE_CURVE('',#7825,#7827,#536,.T.);
#10133=EDGE_CURVE('',#7827,#7828,#7392,.F.);
#10134=EDGE_CURVE('',#7828,#7826,#537,.T.);
#10135=EDGE_CURVE('',#7829,#7830,#5067,.T.);
#10136=EDGE_CURVE('',#7829,#7825,#538,.T.);
#10137=EDGE_CURVE('',#7826,#7830,#539,.T.);
#10138=EDGE_CURVE('',#7831,#7832,#5068,.T.);
#10139=EDGE_CURVE('',#7831,#7829,#540,.T.);
#10140=EDGE_CURVE('',#7830,#7832,#541,.T.);
#10141=EDGE_CURVE('',#7833,#7834,#5069,.T.);
#10142=EDGE_CURVE('',#7833,#7831,#542,.T.);
#10143=EDGE_CURVE('',#7832,#7834,#543,.T.);
#10144=EDGE_CURVE('',#7835,#7836,#5070,.T.);
#10145=EDGE_CURVE('',#7835,#7833,#544,.T.);
#10146=EDGE_CURVE('',#7834,#7836,#545,.T.);
#10147=EDGE_CURVE('',#7837,#7838,#5071,.T.);
#10148=EDGE_CURVE('',#7837,#7835,#546,.T.);
#10149=EDGE_CURVE('',#7836,#7838,#547,.T.);
#10150=EDGE_CURVE('',#7839,#7840,#5072,.T.);
#10151=EDGE_CURVE('',#7839,#7837,#548,.T.);
#10152=EDGE_CURVE('',#7838,#7840,#549,.T.);
#10153=EDGE_CURVE('',#7841,#7842,#5073,.T.);
#10154=EDGE_CURVE('',#7841,#7839,#550,.T.);
#10155=EDGE_CURVE('',#7840,#7842,#551,.T.);
#10156=EDGE_CURVE('',#7843,#7844,#5074,.T.);
#10157=EDGE_CURVE('',#7843,#7841,#552,.T.);
#10158=EDGE_CURVE('',#7842,#7844,#553,.T.);
#10159=EDGE_CURVE('',#7845,#7846,#5075,.T.);
#10160=EDGE_CURVE('',#7845,#7843,#554,.T.);
#10161=EDGE_CURVE('',#7844,#7846,#555,.T.);
#10162=EDGE_CURVE('',#7847,#7848,#5076,.T.);
#10163=EDGE_CURVE('',#7847,#7845,#556,.T.);
#10164=EDGE_CURVE('',#7846,#7848,#557,.T.);
#10165=EDGE_CURVE('',#7849,#7850,#5077,.T.);
#10166=EDGE_CURVE('',#7849,#7847,#558,.T.);
#10167=EDGE_CURVE('',#7848,#7850,#559,.T.);
#10168=EDGE_CURVE('',#7851,#7852,#5078,.T.);
#10169=EDGE_CURVE('',#7851,#7849,#560,.T.);
#10170=EDGE_CURVE('',#7850,#7852,#561,.T.);
#10171=EDGE_CURVE('',#7853,#7854,#5079,.T.);
#10172=EDGE_CURVE('',#7853,#7851,#562,.T.);
#10173=EDGE_CURVE('',#7852,#7854,#563,.T.);
#10174=EDGE_CURVE('',#7855,#7856,#5080,.T.);
#10175=EDGE_CURVE('',#7855,#7853,#564,.T.);
#10176=EDGE_CURVE('',#7854,#7856,#565,.T.);
#10177=EDGE_CURVE('',#7857,#7858,#5081,.T.);
#10178=EDGE_CURVE('',#7857,#7855,#566,.T.);
#10179=EDGE_CURVE('',#7856,#7858,#567,.T.);
#10180=EDGE_CURVE('',#7859,#7860,#5082,.T.);
#10181=EDGE_CURVE('',#7859,#7857,#568,.T.);
#10182=EDGE_CURVE('',#7858,#7860,#569,.T.);
#10183=EDGE_CURVE('',#7861,#7862,#5083,.T.);
#10184=EDGE_CURVE('',#7861,#7859,#570,.T.);
#10185=EDGE_CURVE('',#7860,#7862,#571,.T.);
#10186=EDGE_CURVE('',#7863,#7864,#5084,.T.);
#10187=EDGE_CURVE('',#7863,#7861,#572,.T.);
#10188=EDGE_CURVE('',#7862,#7864,#573,.T.);
#10189=EDGE_CURVE('',#7865,#7866,#5085,.T.);
#10190=EDGE_CURVE('',#7865,#7863,#574,.T.);
#10191=EDGE_CURVE('',#7864,#7866,#575,.T.);
#10192=EDGE_CURVE('',#7867,#7868,#5086,.T.);
#10193=EDGE_CURVE('',#7867,#7865,#576,.T.);
#10194=EDGE_CURVE('',#7866,#7868,#577,.T.);
#10195=EDGE_CURVE('',#7869,#7870,#5087,.T.);
#10196=EDGE_CURVE('',#7869,#7867,#578,.T.);
#10197=EDGE_CURVE('',#7868,#7870,#579,.T.);
#10198=EDGE_CURVE('',#7871,#7872,#5088,.T.);
#10199=EDGE_CURVE('',#7871,#7869,#580,.T.);
#10200=EDGE_CURVE('',#7870,#7872,#581,.T.);
#10201=EDGE_CURVE('',#7873,#7874,#5089,.T.);
#10202=EDGE_CURVE('',#7873,#7871,#582,.T.);
#10203=EDGE_CURVE('',#7872,#7874,#583,.T.);
#10204=EDGE_CURVE('',#7875,#7876,#5090,.T.);
#10205=EDGE_CURVE('',#7875,#7877,#584,.T.);
#10206=EDGE_CURVE('',#7877,#7878,#7393,.T.);
#10207=EDGE_CURVE('',#7876,#7878,#585,.T.);
#10208=EDGE_CURVE('',#7879,#7880,#5091,.T.);
#10209=EDGE_CURVE('',#7879,#7875,#586,.T.);
#10210=EDGE_CURVE('',#7880,#7876,#587,.T.);
#10211=EDGE_CURVE('',#7881,#7882,#5092,.T.);
#10212=EDGE_CURVE('',#7881,#7879,#588,.T.);
#10213=EDGE_CURVE('',#7882,#7880,#589,.T.);
#10214=EDGE_CURVE('',#7883,#7884,#5093,.T.);
#10215=EDGE_CURVE('',#7883,#7881,#590,.T.);
#10216=EDGE_CURVE('',#7884,#7882,#591,.T.);
#10217=EDGE_CURVE('',#7885,#7886,#5094,.T.);
#10218=EDGE_CURVE('',#7885,#7883,#592,.T.);
#10219=EDGE_CURVE('',#7886,#7884,#593,.T.);
#10220=EDGE_CURVE('',#7887,#7888,#5095,.T.);
#10221=EDGE_CURVE('',#7887,#7885,#594,.T.);
#10222=EDGE_CURVE('',#7888,#7886,#595,.T.);
#10223=EDGE_CURVE('',#7889,#7890,#5096,.T.);
#10224=EDGE_CURVE('',#7889,#7887,#596,.T.);
#10225=EDGE_CURVE('',#7890,#7888,#597,.T.);
#10226=EDGE_CURVE('',#7891,#7892,#5097,.T.);
#10227=EDGE_CURVE('',#7891,#7889,#598,.T.);
#10228=EDGE_CURVE('',#7892,#7890,#599,.T.);
#10229=EDGE_CURVE('',#7893,#7894,#5098,.T.);
#10230=EDGE_CURVE('',#7893,#7891,#600,.T.);
#10231=EDGE_CURVE('',#7894,#7892,#601,.T.);
#10232=EDGE_CURVE('',#7895,#7896,#5099,.T.);
#10233=EDGE_CURVE('',#7895,#7893,#602,.T.);
#10234=EDGE_CURVE('',#7896,#7894,#603,.T.);
#10235=EDGE_CURVE('',#7897,#7898,#5100,.T.);
#10236=EDGE_CURVE('',#7897,#7895,#604,.T.);
#10237=EDGE_CURVE('',#7898,#7896,#605,.T.);
#10238=EDGE_CURVE('',#7899,#7900,#5101,.T.);
#10239=EDGE_CURVE('',#7899,#7897,#606,.T.);
#10240=EDGE_CURVE('',#7900,#7898,#607,.T.);
#10241=EDGE_CURVE('',#7901,#7902,#5102,.T.);
#10242=EDGE_CURVE('',#7901,#7899,#608,.T.);
#10243=EDGE_CURVE('',#7902,#7900,#609,.T.);
#10244=EDGE_CURVE('',#7903,#7904,#5103,.T.);
#10245=EDGE_CURVE('',#7903,#7901,#610,.T.);
#10246=EDGE_CURVE('',#7904,#7902,#611,.T.);
#10247=EDGE_CURVE('',#7905,#7906,#5104,.T.);
#10248=EDGE_CURVE('',#7905,#7903,#612,.T.);
#10249=EDGE_CURVE('',#7906,#7904,#613,.T.);
#10250=EDGE_CURVE('',#7907,#7908,#5105,.T.);
#10251=EDGE_CURVE('',#7907,#7905,#614,.T.);
#10252=EDGE_CURVE('',#7908,#7906,#615,.T.);
#10253=EDGE_CURVE('',#7909,#7910,#5106,.T.);
#10254=EDGE_CURVE('',#7909,#7907,#616,.T.);
#10255=EDGE_CURVE('',#7910,#7908,#617,.T.);
#10256=EDGE_CURVE('',#7911,#7912,#5107,.T.);
#10257=EDGE_CURVE('',#7911,#7909,#618,.T.);
#10258=EDGE_CURVE('',#7912,#7910,#619,.T.);
#10259=EDGE_CURVE('',#7913,#7914,#5108,.T.);
#10260=EDGE_CURVE('',#7913,#7911,#620,.T.);
#10261=EDGE_CURVE('',#7914,#7912,#621,.T.);
#10262=EDGE_CURVE('',#7915,#7916,#5109,.T.);
#10263=EDGE_CURVE('',#7915,#7913,#622,.T.);
#10264=EDGE_CURVE('',#7916,#7914,#623,.T.);
#10265=EDGE_CURVE('',#7917,#7918,#5110,.T.);
#10266=EDGE_CURVE('',#7917,#7915,#624,.T.);
#10267=EDGE_CURVE('',#7918,#7916,#625,.T.);
#10268=EDGE_CURVE('',#7919,#7920,#5111,.T.);
#10269=EDGE_CURVE('',#7919,#7917,#626,.T.);
#10270=EDGE_CURVE('',#7920,#7918,#627,.T.);
#10271=EDGE_CURVE('',#7921,#7922,#5112,.T.);
#10272=EDGE_CURVE('',#7921,#7919,#628,.T.);
#10273=EDGE_CURVE('',#7922,#7920,#629,.T.);
#10274=EDGE_CURVE('',#7923,#7924,#5113,.T.);
#10275=EDGE_CURVE('',#7923,#7921,#630,.T.);
#10276=EDGE_CURVE('',#7924,#7922,#631,.T.);
#10277=EDGE_CURVE('',#7878,#7925,#632,.T.);
#10278=EDGE_CURVE('',#7926,#7877,#633,.T.);
#10279=EDGE_CURVE('',#7927,#7926,#7394,.T.);
#10280=EDGE_CURVE('',#7925,#7927,#634,.T.);
#10281=EDGE_CURVE('',#7925,#7928,#5114,.T.);
#10282=EDGE_CURVE('',#7928,#7928,#7395,.T.);
#10283=EDGE_CURVE('',#7929,#7923,#635,.T.);
#10284=EDGE_CURVE('',#7827,#7929,#636,.T.);
#10285=EDGE_CURVE('',#7926,#7873,#637,.T.);
#10286=EDGE_CURVE('',#7930,#7924,#638,.T.);
#10287=EDGE_CURVE('',#7929,#7930,#7396,.T.);
#10288=EDGE_CURVE('',#7874,#7927,#639,.T.);
#10289=EDGE_CURVE('',#7930,#7828,#640,.T.);
#10290=EDGE_CURVE('',#7931,#7932,#5115,.T.);
#10291=EDGE_CURVE('',#7931,#7933,#5116,.T.);
#10292=EDGE_CURVE('',#7933,#7934,#5117,.T.);
#10293=EDGE_CURVE('',#7932,#7934,#5118,.T.);
#10294=EDGE_CURVE('',#7935,#7931,#5119,.T.);
#10295=EDGE_CURVE('',#7935,#7936,#5120,.T.);
#10296=EDGE_CURVE('',#7936,#7933,#5121,.T.);
#10297=EDGE_CURVE('',#7937,#7935,#5122,.T.);
#10298=EDGE_CURVE('',#7937,#7938,#5123,.T.);
#10299=EDGE_CURVE('',#7938,#7936,#5124,.T.);
#10300=EDGE_CURVE('',#7939,#7937,#5125,.T.);
#10301=EDGE_CURVE('',#7939,#7940,#5126,.T.);
#10302=EDGE_CURVE('',#7940,#7938,#5127,.T.);
#10303=EDGE_CURVE('',#7941,#7939,#5128,.T.);
#10304=EDGE_CURVE('',#7941,#7942,#5129,.T.);
#10305=EDGE_CURVE('',#7942,#7940,#5130,.T.);
#10306=EDGE_CURVE('',#7932,#7941,#5131,.T.);
#10307=EDGE_CURVE('',#7934,#7942,#5132,.T.);
#10308=EDGE_CURVE('',#7943,#7943,#7397,.T.);
#10309=EDGE_CURVE('',#7943,#7944,#5133,.T.);
#10310=EDGE_CURVE('',#7944,#7944,#7398,.T.);
#10311=EDGE_CURVE('',#7945,#7945,#7399,.T.);
#10312=EDGE_CURVE('',#7945,#7946,#5134,.T.);
#10313=EDGE_CURVE('',#7946,#7946,#7400,.T.);
#10314=EDGE_CURVE('',#7947,#7947,#7401,.T.);
#10315=EDGE_CURVE('',#7947,#7948,#5135,.T.);
#10316=EDGE_CURVE('',#7948,#7948,#7402,.T.);
#10317=EDGE_CURVE('',#7949,#7950,#5136,.T.);
#10318=EDGE_CURVE('',#7950,#7951,#641,.T.);
#10319=EDGE_CURVE('',#7951,#7952,#7403,.T.);
#10320=EDGE_CURVE('',#7952,#7953,#5137,.T.);
#10321=EDGE_CURVE('',#7953,#7953,#7404,.F.);
#10322=EDGE_CURVE('',#7952,#7954,#7405,.T.);
#10323=EDGE_CURVE('',#7954,#7949,#642,.T.);
#10324=EDGE_CURVE('',#7955,#7956,#5138,.T.);
#10325=EDGE_CURVE('',#7956,#7950,#643,.T.);
#10326=EDGE_CURVE('',#7949,#7955,#644,.T.);
#10327=EDGE_CURVE('',#7957,#7958,#5139,.T.);
#10328=EDGE_CURVE('',#7958,#7956,#645,.T.);
#10329=EDGE_CURVE('',#7955,#7957,#646,.T.);
#10330=EDGE_CURVE('',#7959,#7960,#5140,.T.);
#10331=EDGE_CURVE('',#7960,#7958,#647,.T.);
#10332=EDGE_CURVE('',#7957,#7959,#648,.T.);
#10333=EDGE_CURVE('',#7961,#7962,#5141,.T.);
#10334=EDGE_CURVE('',#7962,#7960,#649,.T.);
#10335=EDGE_CURVE('',#7959,#7961,#650,.T.);
#10336=EDGE_CURVE('',#7963,#7964,#5142,.T.);
#10337=EDGE_CURVE('',#7964,#7962,#651,.T.);
#10338=EDGE_CURVE('',#7961,#7963,#652,.T.);
#10339=EDGE_CURVE('',#7965,#7966,#5143,.T.);
#10340=EDGE_CURVE('',#7966,#7964,#653,.T.);
#10341=EDGE_CURVE('',#7963,#7965,#654,.T.);
#10342=EDGE_CURVE('',#7967,#7968,#5144,.T.);
#10343=EDGE_CURVE('',#7968,#7966,#655,.T.);
#10344=EDGE_CURVE('',#7965,#7967,#656,.T.);
#10345=EDGE_CURVE('',#7969,#7970,#5145,.T.);
#10346=EDGE_CURVE('',#7970,#7968,#657,.T.);
#10347=EDGE_CURVE('',#7967,#7969,#658,.T.);
#10348=EDGE_CURVE('',#7971,#7972,#5146,.T.);
#10349=EDGE_CURVE('',#7972,#7970,#659,.T.);
#10350=EDGE_CURVE('',#7969,#7971,#660,.T.);
#10351=EDGE_CURVE('',#7973,#7974,#5147,.T.);
#10352=EDGE_CURVE('',#7974,#7972,#661,.T.);
#10353=EDGE_CURVE('',#7971,#7973,#662,.T.);
#10354=EDGE_CURVE('',#7975,#7976,#5148,.T.);
#10355=EDGE_CURVE('',#7976,#7974,#663,.T.);
#10356=EDGE_CURVE('',#7973,#7975,#664,.T.);
#10357=EDGE_CURVE('',#7977,#7978,#5149,.T.);
#10358=EDGE_CURVE('',#7978,#7976,#665,.T.);
#10359=EDGE_CURVE('',#7975,#7977,#666,.T.);
#10360=EDGE_CURVE('',#7979,#7980,#5150,.T.);
#10361=EDGE_CURVE('',#7980,#7978,#667,.T.);
#10362=EDGE_CURVE('',#7977,#7979,#668,.T.);
#10363=EDGE_CURVE('',#7981,#7982,#5151,.T.);
#10364=EDGE_CURVE('',#7982,#7980,#669,.T.);
#10365=EDGE_CURVE('',#7979,#7981,#670,.T.);
#10366=EDGE_CURVE('',#7983,#7984,#5152,.T.);
#10367=EDGE_CURVE('',#7984,#7982,#671,.T.);
#10368=EDGE_CURVE('',#7981,#7983,#672,.T.);
#10369=EDGE_CURVE('',#7985,#7986,#5153,.T.);
#10370=EDGE_CURVE('',#7986,#7984,#673,.T.);
#10371=EDGE_CURVE('',#7983,#7985,#674,.T.);
#10372=EDGE_CURVE('',#7987,#7988,#5154,.T.);
#10373=EDGE_CURVE('',#7988,#7986,#675,.T.);
#10374=EDGE_CURVE('',#7985,#7987,#676,.T.);
#10375=EDGE_CURVE('',#7989,#7990,#5155,.T.);
#10376=EDGE_CURVE('',#7990,#7988,#677,.T.);
#10377=EDGE_CURVE('',#7987,#7989,#678,.T.);
#10378=EDGE_CURVE('',#7991,#7992,#5156,.T.);
#10379=EDGE_CURVE('',#7992,#7990,#679,.T.);
#10380=EDGE_CURVE('',#7989,#7991,#680,.T.);
#10381=EDGE_CURVE('',#7993,#7994,#5157,.T.);
#10382=EDGE_CURVE('',#7994,#7992,#681,.T.);
#10383=EDGE_CURVE('',#7991,#7993,#682,.T.);
#10384=EDGE_CURVE('',#7995,#7996,#5158,.T.);
#10385=EDGE_CURVE('',#7996,#7994,#683,.T.);
#10386=EDGE_CURVE('',#7993,#7995,#684,.T.);
#10387=EDGE_CURVE('',#7997,#7998,#5159,.T.);
#10388=EDGE_CURVE('',#7998,#7996,#685,.T.);
#10389=EDGE_CURVE('',#7995,#7997,#686,.T.);
#10390=EDGE_CURVE('',#7999,#8000,#5160,.T.);
#10391=EDGE_CURVE('',#8000,#7998,#687,.T.);
#10392=EDGE_CURVE('',#7997,#7999,#688,.T.);
#10393=EDGE_CURVE('',#8001,#8002,#5161,.T.);
#10394=EDGE_CURVE('',#8001,#8003,#689,.T.);
#10395=EDGE_CURVE('',#8004,#8003,#7406,.T.);
#10396=EDGE_CURVE('',#8004,#8002,#690,.T.);
#10397=EDGE_CURVE('',#8005,#8006,#5162,.T.);
#10398=EDGE_CURVE('',#8006,#8007,#691,.T.);
#10399=EDGE_CURVE('',#8008,#8007,#7407,.T.);
#10400=EDGE_CURVE('',#8005,#8008,#692,.T.);
#10401=EDGE_CURVE('',#8009,#8010,#5163,.T.);
#10402=EDGE_CURVE('',#8010,#8006,#693,.T.);
#10403=EDGE_CURVE('',#8009,#8005,#694,.T.);
#10404=EDGE_CURVE('',#8011,#8012,#5164,.T.);
#10405=EDGE_CURVE('',#8012,#8010,#695,.T.);
#10406=EDGE_CURVE('',#8011,#8009,#696,.T.);
#10407=EDGE_CURVE('',#8013,#8014,#5165,.T.);
#10408=EDGE_CURVE('',#8014,#8012,#697,.T.);
#10409=EDGE_CURVE('',#8013,#8011,#698,.T.);
#10410=EDGE_CURVE('',#8015,#8016,#5166,.T.);
#10411=EDGE_CURVE('',#8016,#8014,#699,.T.);
#10412=EDGE_CURVE('',#8015,#8013,#700,.T.);
#10413=EDGE_CURVE('',#8017,#8018,#5167,.T.);
#10414=EDGE_CURVE('',#8018,#8016,#701,.T.);
#10415=EDGE_CURVE('',#8017,#8015,#702,.T.);
#10416=EDGE_CURVE('',#8019,#8020,#5168,.T.);
#10417=EDGE_CURVE('',#8020,#8018,#703,.T.);
#10418=EDGE_CURVE('',#8019,#8017,#704,.T.);
#10419=EDGE_CURVE('',#8021,#8022,#5169,.T.);
#10420=EDGE_CURVE('',#8022,#8020,#705,.T.);
#10421=EDGE_CURVE('',#8021,#8019,#706,.T.);
#10422=EDGE_CURVE('',#8023,#8024,#5170,.T.);
#10423=EDGE_CURVE('',#8024,#8022,#707,.T.);
#10424=EDGE_CURVE('',#8023,#8021,#708,.T.);
#10425=EDGE_CURVE('',#8025,#8026,#5171,.T.);
#10426=EDGE_CURVE('',#8026,#8024,#709,.T.);
#10427=EDGE_CURVE('',#8025,#8023,#710,.T.);
#10428=EDGE_CURVE('',#8027,#8028,#5172,.T.);
#10429=EDGE_CURVE('',#8028,#8026,#711,.T.);
#10430=EDGE_CURVE('',#8027,#8025,#712,.T.);
#10431=EDGE_CURVE('',#8029,#8030,#5173,.T.);
#10432=EDGE_CURVE('',#8030,#8028,#713,.T.);
#10433=EDGE_CURVE('',#8029,#8027,#714,.T.);
#10434=EDGE_CURVE('',#8031,#8032,#5174,.T.);
#10435=EDGE_CURVE('',#8032,#8030,#715,.T.);
#10436=EDGE_CURVE('',#8031,#8029,#716,.T.);
#10437=EDGE_CURVE('',#8033,#8034,#5175,.T.);
#10438=EDGE_CURVE('',#8034,#8032,#717,.T.);
#10439=EDGE_CURVE('',#8033,#8031,#718,.T.);
#10440=EDGE_CURVE('',#8035,#8036,#5176,.T.);
#10441=EDGE_CURVE('',#8036,#8034,#719,.T.);
#10442=EDGE_CURVE('',#8035,#8033,#720,.T.);
#10443=EDGE_CURVE('',#8037,#8038,#5177,.T.);
#10444=EDGE_CURVE('',#8038,#8036,#721,.T.);
#10445=EDGE_CURVE('',#8037,#8035,#722,.T.);
#10446=EDGE_CURVE('',#8039,#8040,#5178,.T.);
#10447=EDGE_CURVE('',#8040,#8038,#723,.T.);
#10448=EDGE_CURVE('',#8039,#8037,#724,.T.);
#10449=EDGE_CURVE('',#8041,#8042,#5179,.T.);
#10450=EDGE_CURVE('',#8042,#8040,#725,.T.);
#10451=EDGE_CURVE('',#8041,#8039,#726,.T.);
#10452=EDGE_CURVE('',#8043,#8044,#5180,.T.);
#10453=EDGE_CURVE('',#8044,#8042,#727,.T.);
#10454=EDGE_CURVE('',#8043,#8041,#728,.T.);
#10455=EDGE_CURVE('',#8045,#8046,#5181,.T.);
#10456=EDGE_CURVE('',#8046,#8044,#729,.T.);
#10457=EDGE_CURVE('',#8045,#8043,#730,.T.);
#10458=EDGE_CURVE('',#8047,#8048,#5182,.T.);
#10459=EDGE_CURVE('',#8048,#8046,#731,.T.);
#10460=EDGE_CURVE('',#8047,#8045,#732,.T.);
#10461=EDGE_CURVE('',#8049,#8050,#5183,.T.);
#10462=EDGE_CURVE('',#8050,#8048,#733,.T.);
#10463=EDGE_CURVE('',#8049,#8047,#734,.T.);
#10464=EDGE_CURVE('',#8051,#8052,#5184,.T.);
#10465=EDGE_CURVE('',#8052,#8050,#735,.T.);
#10466=EDGE_CURVE('',#8051,#8049,#736,.T.);
#10467=EDGE_CURVE('',#8053,#8054,#5185,.T.);
#10468=EDGE_CURVE('',#8054,#8052,#737,.T.);
#10469=EDGE_CURVE('',#8053,#8051,#738,.T.);
#10470=EDGE_CURVE('',#8055,#8056,#5186,.T.);
#10471=EDGE_CURVE('',#8057,#8055,#739,.T.);
#10472=EDGE_CURVE('',#8058,#8057,#7408,.T.);
#10473=EDGE_CURVE('',#8058,#8056,#740,.T.);
#10474=EDGE_CURVE('',#8059,#8060,#5187,.T.);
#10475=EDGE_CURVE('',#8060,#8061,#741,.T.);
#10476=EDGE_CURVE('',#8061,#8062,#7409,.T.);
#10477=EDGE_CURVE('',#8062,#8063,#5188,.T.);
#10478=EDGE_CURVE('',#8063,#8063,#7410,.F.);
#10479=EDGE_CURVE('',#8062,#8064,#7411,.T.);
#10480=EDGE_CURVE('',#8064,#8059,#742,.T.);
#10481=EDGE_CURVE('',#8065,#8066,#5189,.T.);
#10482=EDGE_CURVE('',#8066,#8060,#743,.T.);
#10483=EDGE_CURVE('',#8059,#8065,#744,.T.);
#10484=EDGE_CURVE('',#8067,#8068,#5190,.T.);
#10485=EDGE_CURVE('',#8068,#8066,#745,.T.);
#10486=EDGE_CURVE('',#8065,#8067,#746,.T.);
#10487=EDGE_CURVE('',#8069,#8070,#5191,.T.);
#10488=EDGE_CURVE('',#8070,#8068,#747,.T.);
#10489=EDGE_CURVE('',#8067,#8069,#748,.T.);
#10490=EDGE_CURVE('',#8071,#8072,#5192,.T.);
#10491=EDGE_CURVE('',#8072,#8070,#749,.T.);
#10492=EDGE_CURVE('',#8069,#8071,#750,.T.);
#10493=EDGE_CURVE('',#8073,#8074,#5193,.T.);
#10494=EDGE_CURVE('',#8074,#8072,#751,.T.);
#10495=EDGE_CURVE('',#8071,#8073,#752,.T.);
#10496=EDGE_CURVE('',#8075,#8076,#5194,.T.);
#10497=EDGE_CURVE('',#8076,#8074,#753,.T.);
#10498=EDGE_CURVE('',#8073,#8075,#754,.T.);
#10499=EDGE_CURVE('',#8077,#8078,#5195,.T.);
#10500=EDGE_CURVE('',#8078,#8076,#755,.T.);
#10501=EDGE_CURVE('',#8075,#8077,#756,.T.);
#10502=EDGE_CURVE('',#8079,#8080,#5196,.T.);
#10503=EDGE_CURVE('',#8080,#8078,#757,.T.);
#10504=EDGE_CURVE('',#8077,#8079,#758,.T.);
#10505=EDGE_CURVE('',#8081,#8082,#5197,.T.);
#10506=EDGE_CURVE('',#8082,#8080,#759,.T.);
#10507=EDGE_CURVE('',#8079,#8081,#760,.T.);
#10508=EDGE_CURVE('',#8083,#8084,#5198,.T.);
#10509=EDGE_CURVE('',#8084,#8082,#761,.T.);
#10510=EDGE_CURVE('',#8081,#8083,#762,.T.);
#10511=EDGE_CURVE('',#8085,#8086,#5199,.T.);
#10512=EDGE_CURVE('',#8086,#8084,#763,.T.);
#10513=EDGE_CURVE('',#8083,#8085,#764,.T.);
#10514=EDGE_CURVE('',#8087,#8088,#5200,.T.);
#10515=EDGE_CURVE('',#8088,#8086,#765,.T.);
#10516=EDGE_CURVE('',#8085,#8087,#766,.T.);
#10517=EDGE_CURVE('',#8089,#8090,#5201,.T.);
#10518=EDGE_CURVE('',#8090,#8088,#767,.T.);
#10519=EDGE_CURVE('',#8087,#8089,#768,.T.);
#10520=EDGE_CURVE('',#8091,#8092,#5202,.T.);
#10521=EDGE_CURVE('',#8092,#8090,#769,.T.);
#10522=EDGE_CURVE('',#8089,#8091,#770,.T.);
#10523=EDGE_CURVE('',#8093,#8094,#5203,.T.);
#10524=EDGE_CURVE('',#8094,#8092,#771,.T.);
#10525=EDGE_CURVE('',#8091,#8093,#772,.T.);
#10526=EDGE_CURVE('',#8095,#8096,#5204,.T.);
#10527=EDGE_CURVE('',#8096,#8094,#773,.T.);
#10528=EDGE_CURVE('',#8093,#8095,#774,.T.);
#10529=EDGE_CURVE('',#8097,#8098,#5205,.T.);
#10530=EDGE_CURVE('',#8098,#8096,#775,.T.);
#10531=EDGE_CURVE('',#8095,#8097,#776,.T.);
#10532=EDGE_CURVE('',#8099,#8100,#5206,.T.);
#10533=EDGE_CURVE('',#8100,#8098,#777,.T.);
#10534=EDGE_CURVE('',#8097,#8099,#778,.T.);
#10535=EDGE_CURVE('',#8101,#8102,#5207,.T.);
#10536=EDGE_CURVE('',#8102,#8100,#779,.T.);
#10537=EDGE_CURVE('',#8099,#8101,#780,.T.);
#10538=EDGE_CURVE('',#8103,#8104,#5208,.T.);
#10539=EDGE_CURVE('',#8104,#8102,#781,.T.);
#10540=EDGE_CURVE('',#8101,#8103,#782,.T.);
#10541=EDGE_CURVE('',#8105,#8106,#5209,.T.);
#10542=EDGE_CURVE('',#8106,#8104,#783,.T.);
#10543=EDGE_CURVE('',#8103,#8105,#784,.T.);
#10544=EDGE_CURVE('',#8107,#8108,#5210,.T.);
#10545=EDGE_CURVE('',#8108,#8106,#785,.T.);
#10546=EDGE_CURVE('',#8105,#8107,#786,.T.);
#10547=EDGE_CURVE('',#8109,#8110,#5211,.T.);
#10548=EDGE_CURVE('',#8110,#8108,#787,.T.);
#10549=EDGE_CURVE('',#8107,#8109,#788,.T.);
#10550=EDGE_CURVE('',#8111,#8112,#5212,.T.);
#10551=EDGE_CURVE('',#8112,#8110,#789,.T.);
#10552=EDGE_CURVE('',#8109,#8111,#790,.T.);
#10553=EDGE_CURVE('',#8113,#8114,#5213,.T.);
#10554=EDGE_CURVE('',#8114,#8112,#791,.T.);
#10555=EDGE_CURVE('',#8111,#8113,#792,.T.);
#10556=EDGE_CURVE('',#8115,#8116,#5214,.T.);
#10557=EDGE_CURVE('',#8116,#8114,#793,.T.);
#10558=EDGE_CURVE('',#8113,#8115,#794,.T.);
#10559=EDGE_CURVE('',#8117,#8118,#5215,.T.);
#10560=EDGE_CURVE('',#8118,#8116,#795,.T.);
#10561=EDGE_CURVE('',#8115,#8117,#796,.T.);
#10562=EDGE_CURVE('',#8119,#8120,#5216,.T.);
#10563=EDGE_CURVE('',#8120,#8118,#797,.T.);
#10564=EDGE_CURVE('',#8117,#8119,#798,.T.);
#10565=EDGE_CURVE('',#8121,#8122,#5217,.T.);
#10566=EDGE_CURVE('',#8122,#8120,#799,.T.);
#10567=EDGE_CURVE('',#8119,#8121,#800,.T.);
#10568=EDGE_CURVE('',#8123,#8124,#5218,.T.);
#10569=EDGE_CURVE('',#8124,#8122,#801,.T.);
#10570=EDGE_CURVE('',#8121,#8123,#802,.T.);
#10571=EDGE_CURVE('',#8125,#8126,#5219,.T.);
#10572=EDGE_CURVE('',#8126,#8124,#803,.T.);
#10573=EDGE_CURVE('',#8123,#8125,#804,.T.);
#10574=EDGE_CURVE('',#8127,#8128,#5220,.T.);
#10575=EDGE_CURVE('',#8128,#8126,#805,.T.);
#10576=EDGE_CURVE('',#8125,#8127,#806,.T.);
#10577=EDGE_CURVE('',#8129,#8130,#5221,.T.);
#10578=EDGE_CURVE('',#8130,#8128,#807,.T.);
#10579=EDGE_CURVE('',#8127,#8129,#808,.T.);
#10580=EDGE_CURVE('',#8131,#8132,#5222,.T.);
#10581=EDGE_CURVE('',#8132,#8130,#809,.T.);
#10582=EDGE_CURVE('',#8129,#8131,#810,.T.);
#10583=EDGE_CURVE('',#8133,#8134,#5223,.T.);
#10584=EDGE_CURVE('',#8134,#8132,#811,.T.);
#10585=EDGE_CURVE('',#8131,#8133,#812,.T.);
#10586=EDGE_CURVE('',#8135,#8136,#5224,.T.);
#10587=EDGE_CURVE('',#8136,#8134,#813,.T.);
#10588=EDGE_CURVE('',#8133,#8135,#814,.T.);
#10589=EDGE_CURVE('',#8137,#8138,#5225,.T.);
#10590=EDGE_CURVE('',#8138,#8136,#815,.T.);
#10591=EDGE_CURVE('',#8135,#8137,#816,.T.);
#10592=EDGE_CURVE('',#8139,#8140,#5226,.T.);
#10593=EDGE_CURVE('',#8140,#8138,#817,.T.);
#10594=EDGE_CURVE('',#8137,#8139,#818,.T.);
#10595=EDGE_CURVE('',#8141,#8142,#5227,.T.);
#10596=EDGE_CURVE('',#8141,#8143,#819,.T.);
#10597=EDGE_CURVE('',#8144,#8143,#7412,.F.);
#10598=EDGE_CURVE('',#8144,#8142,#820,.T.);
#10599=EDGE_CURVE('',#8145,#8146,#5228,.T.);
#10600=EDGE_CURVE('',#8146,#8147,#821,.T.);
#10601=EDGE_CURVE('',#8148,#8147,#7413,.T.);
#10602=EDGE_CURVE('',#8145,#8148,#822,.T.);
#10603=EDGE_CURVE('',#8149,#8150,#5229,.T.);
#10604=EDGE_CURVE('',#8150,#8146,#823,.T.);
#10605=EDGE_CURVE('',#8149,#8145,#824,.T.);
#10606=EDGE_CURVE('',#8151,#8152,#5230,.T.);
#10607=EDGE_CURVE('',#8152,#8150,#825,.T.);
#10608=EDGE_CURVE('',#8151,#8149,#826,.T.);
#10609=EDGE_CURVE('',#8153,#8154,#5231,.T.);
#10610=EDGE_CURVE('',#8154,#8152,#827,.T.);
#10611=EDGE_CURVE('',#8153,#8151,#828,.T.);
#10612=EDGE_CURVE('',#8155,#8156,#5232,.T.);
#10613=EDGE_CURVE('',#8156,#8154,#829,.T.);
#10614=EDGE_CURVE('',#8155,#8153,#830,.T.);
#10615=EDGE_CURVE('',#8157,#8158,#5233,.T.);
#10616=EDGE_CURVE('',#8158,#8156,#831,.T.);
#10617=EDGE_CURVE('',#8157,#8155,#832,.T.);
#10618=EDGE_CURVE('',#8159,#8160,#5234,.T.);
#10619=EDGE_CURVE('',#8160,#8158,#833,.T.);
#10620=EDGE_CURVE('',#8159,#8157,#834,.T.);
#10621=EDGE_CURVE('',#8161,#8162,#5235,.T.);
#10622=EDGE_CURVE('',#8162,#8160,#835,.T.);
#10623=EDGE_CURVE('',#8161,#8159,#836,.T.);
#10624=EDGE_CURVE('',#8163,#8164,#5236,.T.);
#10625=EDGE_CURVE('',#8164,#8162,#837,.T.);
#10626=EDGE_CURVE('',#8163,#8161,#838,.T.);
#10627=EDGE_CURVE('',#8165,#8166,#5237,.T.);
#10628=EDGE_CURVE('',#8166,#8164,#839,.T.);
#10629=EDGE_CURVE('',#8165,#8163,#840,.T.);
#10630=EDGE_CURVE('',#8167,#8168,#5238,.T.);
#10631=EDGE_CURVE('',#8168,#8166,#841,.T.);
#10632=EDGE_CURVE('',#8167,#8165,#842,.T.);
#10633=EDGE_CURVE('',#8169,#8170,#5239,.T.);
#10634=EDGE_CURVE('',#8170,#8168,#843,.T.);
#10635=EDGE_CURVE('',#8169,#8167,#844,.T.);
#10636=EDGE_CURVE('',#8171,#8172,#5240,.T.);
#10637=EDGE_CURVE('',#8172,#8170,#845,.T.);
#10638=EDGE_CURVE('',#8171,#8169,#846,.T.);
#10639=EDGE_CURVE('',#8173,#8174,#5241,.T.);
#10640=EDGE_CURVE('',#8174,#8172,#847,.T.);
#10641=EDGE_CURVE('',#8173,#8171,#848,.T.);
#10642=EDGE_CURVE('',#8175,#8176,#5242,.T.);
#10643=EDGE_CURVE('',#8176,#8174,#849,.T.);
#10644=EDGE_CURVE('',#8175,#8173,#850,.T.);
#10645=EDGE_CURVE('',#8177,#8178,#5243,.T.);
#10646=EDGE_CURVE('',#8178,#8176,#851,.T.);
#10647=EDGE_CURVE('',#8177,#8175,#852,.T.);
#10648=EDGE_CURVE('',#8179,#8180,#5244,.T.);
#10649=EDGE_CURVE('',#8180,#8178,#853,.T.);
#10650=EDGE_CURVE('',#8179,#8177,#854,.T.);
#10651=EDGE_CURVE('',#8181,#8182,#5245,.T.);
#10652=EDGE_CURVE('',#8182,#8180,#855,.T.);
#10653=EDGE_CURVE('',#8181,#8179,#856,.T.);
#10654=EDGE_CURVE('',#8183,#8184,#5246,.T.);
#10655=EDGE_CURVE('',#8184,#8182,#857,.T.);
#10656=EDGE_CURVE('',#8183,#8181,#858,.T.);
#10657=EDGE_CURVE('',#8185,#8186,#5247,.T.);
#10658=EDGE_CURVE('',#8186,#8184,#859,.T.);
#10659=EDGE_CURVE('',#8185,#8183,#860,.T.);
#10660=EDGE_CURVE('',#8187,#8188,#5248,.T.);
#10661=EDGE_CURVE('',#8188,#8186,#861,.T.);
#10662=EDGE_CURVE('',#8187,#8185,#862,.T.);
#10663=EDGE_CURVE('',#8189,#8190,#5249,.T.);
#10664=EDGE_CURVE('',#8190,#8188,#863,.T.);
#10665=EDGE_CURVE('',#8189,#8187,#864,.T.);
#10666=EDGE_CURVE('',#8191,#8192,#5250,.T.);
#10667=EDGE_CURVE('',#8192,#8190,#865,.T.);
#10668=EDGE_CURVE('',#8191,#8189,#866,.T.);
#10669=EDGE_CURVE('',#8193,#8194,#5251,.T.);
#10670=EDGE_CURVE('',#8194,#8192,#867,.T.);
#10671=EDGE_CURVE('',#8193,#8191,#868,.T.);
#10672=EDGE_CURVE('',#8195,#8196,#5252,.T.);
#10673=EDGE_CURVE('',#8196,#8194,#869,.T.);
#10674=EDGE_CURVE('',#8195,#8193,#870,.T.);
#10675=EDGE_CURVE('',#8197,#8198,#5253,.T.);
#10676=EDGE_CURVE('',#8198,#8196,#871,.T.);
#10677=EDGE_CURVE('',#8197,#8195,#872,.T.);
#10678=EDGE_CURVE('',#8199,#8200,#5254,.T.);
#10679=EDGE_CURVE('',#8200,#8198,#873,.T.);
#10680=EDGE_CURVE('',#8199,#8197,#874,.T.);
#10681=EDGE_CURVE('',#8201,#8202,#5255,.T.);
#10682=EDGE_CURVE('',#8202,#8200,#875,.T.);
#10683=EDGE_CURVE('',#8201,#8199,#876,.T.);
#10684=EDGE_CURVE('',#8203,#8204,#5256,.T.);
#10685=EDGE_CURVE('',#8204,#8202,#877,.T.);
#10686=EDGE_CURVE('',#8203,#8201,#878,.T.);
#10687=EDGE_CURVE('',#8205,#8206,#5257,.T.);
#10688=EDGE_CURVE('',#8206,#8204,#879,.T.);
#10689=EDGE_CURVE('',#8205,#8203,#880,.T.);
#10690=EDGE_CURVE('',#8207,#8208,#5258,.T.);
#10691=EDGE_CURVE('',#8208,#8206,#881,.T.);
#10692=EDGE_CURVE('',#8207,#8205,#882,.T.);
#10693=EDGE_CURVE('',#8209,#8210,#5259,.T.);
#10694=EDGE_CURVE('',#8210,#8208,#883,.T.);
#10695=EDGE_CURVE('',#8209,#8207,#884,.T.);
#10696=EDGE_CURVE('',#8211,#8212,#5260,.T.);
#10697=EDGE_CURVE('',#8212,#8210,#885,.T.);
#10698=EDGE_CURVE('',#8211,#8209,#886,.T.);
#10699=EDGE_CURVE('',#8213,#8214,#5261,.T.);
#10700=EDGE_CURVE('',#8214,#8212,#887,.T.);
#10701=EDGE_CURVE('',#8213,#8211,#888,.T.);
#10702=EDGE_CURVE('',#8215,#8216,#5262,.T.);
#10703=EDGE_CURVE('',#8216,#8214,#889,.T.);
#10704=EDGE_CURVE('',#8215,#8213,#890,.T.);
#10705=EDGE_CURVE('',#8217,#8218,#5263,.T.);
#10706=EDGE_CURVE('',#8218,#8216,#891,.T.);
#10707=EDGE_CURVE('',#8217,#8215,#892,.T.);
#10708=EDGE_CURVE('',#8219,#8220,#5264,.T.);
#10709=EDGE_CURVE('',#8220,#8218,#893,.T.);
#10710=EDGE_CURVE('',#8219,#8217,#894,.T.);
#10711=EDGE_CURVE('',#8221,#8222,#5265,.T.);
#10712=EDGE_CURVE('',#8222,#8220,#895,.T.);
#10713=EDGE_CURVE('',#8221,#8219,#896,.T.);
#10714=EDGE_CURVE('',#8223,#8224,#5266,.T.);
#10715=EDGE_CURVE('',#8224,#8222,#897,.T.);
#10716=EDGE_CURVE('',#8223,#8221,#898,.T.);
#10717=EDGE_CURVE('',#8225,#8226,#5267,.T.);
#10718=EDGE_CURVE('',#8227,#8225,#899,.T.);
#10719=EDGE_CURVE('',#8228,#8227,#7414,.T.);
#10720=EDGE_CURVE('',#8228,#8226,#900,.T.);
#10721=EDGE_CURVE('',#8061,#8148,#901,.T.);
#10722=EDGE_CURVE('',#8147,#8064,#902,.T.);
#10723=EDGE_CURVE('',#8226,#8224,#903,.T.);
#10724=EDGE_CURVE('',#8225,#8223,#904,.T.);
#10725=EDGE_CURVE('',#8143,#8228,#905,.T.);
#10726=EDGE_CURVE('',#8139,#8141,#906,.T.);
#10727=EDGE_CURVE('',#8142,#8140,#907,.T.);
#10728=EDGE_CURVE('',#8227,#8144,#908,.T.);
#10729=EDGE_CURVE('',#8229,#8229,#7415,.T.);
#10730=EDGE_CURVE('',#7951,#8008,#909,.T.);
#10731=EDGE_CURVE('',#8007,#7954,#910,.T.);
#10732=EDGE_CURVE('',#8056,#8054,#911,.T.);
#10733=EDGE_CURVE('',#8055,#8053,#912,.T.);
#10734=EDGE_CURVE('',#8003,#8058,#913,.T.);
#10735=EDGE_CURVE('',#7999,#8001,#914,.T.);
#10736=EDGE_CURVE('',#8002,#8000,#915,.T.);
#10737=EDGE_CURVE('',#8057,#8004,#916,.T.);
#10738=EDGE_CURVE('',#8230,#8230,#7416,.T.);
#10739=EDGE_CURVE('',#8231,#8232,#7417,.T.);
#10740=EDGE_CURVE('',#8232,#8233,#5268,.T.);
#10741=EDGE_CURVE('',#8233,#8234,#7418,.T.);
#10742=EDGE_CURVE('',#8234,#8231,#5269,.T.);
#10743=EDGE_CURVE('',#8235,#8232,#5270,.T.);
#10744=EDGE_CURVE('',#8236,#8235,#5271,.T.);
#10745=EDGE_CURVE('',#8233,#8236,#5272,.T.);
#10746=EDGE_CURVE('',#8231,#8237,#5273,.T.);
#10747=EDGE_CURVE('',#8238,#8237,#7419,.T.);
#10748=EDGE_CURVE('',#8238,#8239,#5274,.T.);
#10749=EDGE_CURVE('',#8240,#8239,#7420,.T.);
#10750=EDGE_CURVE('',#8240,#8241,#5275,.T.);
#10751=EDGE_CURVE('',#8242,#8241,#7421,.T.);
#10752=EDGE_CURVE('',#8242,#8243,#5276,.T.);
#10753=EDGE_CURVE('',#8244,#8243,#7422,.T.);
#10754=EDGE_CURVE('',#8244,#8245,#5277,.T.);
#10755=EDGE_CURVE('',#8246,#8245,#7423,.T.);
#10756=EDGE_CURVE('',#8246,#8247,#5278,.T.);
#10757=EDGE_CURVE('',#8248,#8247,#7424,.T.);
#10758=EDGE_CURVE('',#8248,#8249,#5279,.T.);
#10759=EDGE_CURVE('',#8250,#8249,#7425,.T.);
#10760=EDGE_CURVE('',#8250,#8251,#5280,.T.);
#10761=EDGE_CURVE('',#8252,#8251,#7426,.T.);
#10762=EDGE_CURVE('',#8252,#8253,#5281,.T.);
#10763=EDGE_CURVE('',#8254,#8253,#7427,.T.);
#10764=EDGE_CURVE('',#8254,#8255,#5282,.T.);
#10765=EDGE_CURVE('',#8256,#8255,#7428,.T.);
#10766=EDGE_CURVE('',#8256,#8257,#5283,.T.);
#10767=EDGE_CURVE('',#8258,#8257,#7429,.T.);
#10768=EDGE_CURVE('',#8258,#8259,#5284,.T.);
#10769=EDGE_CURVE('',#8260,#8259,#7430,.T.);
#10770=EDGE_CURVE('',#8260,#8261,#5285,.T.);
#10771=EDGE_CURVE('',#8262,#8261,#7431,.T.);
#10772=EDGE_CURVE('',#8262,#8263,#5286,.T.);
#10773=EDGE_CURVE('',#8264,#8263,#7432,.T.);
#10774=EDGE_CURVE('',#8264,#8265,#5287,.T.);
#10775=EDGE_CURVE('',#8266,#8265,#7433,.T.);
#10776=EDGE_CURVE('',#8266,#8267,#5288,.T.);
#10777=EDGE_CURVE('',#8268,#8267,#7434,.T.);
#10778=EDGE_CURVE('',#8268,#8269,#5289,.T.);
#10779=EDGE_CURVE('',#8270,#8269,#7435,.T.);
#10780=EDGE_CURVE('',#8270,#8271,#5290,.T.);
#10781=EDGE_CURVE('',#8272,#8271,#7436,.T.);
#10782=EDGE_CURVE('',#8272,#8273,#5291,.T.);
#10783=EDGE_CURVE('',#8274,#8273,#7437,.T.);
#10784=EDGE_CURVE('',#8274,#8275,#5292,.T.);
#10785=EDGE_CURVE('',#8276,#8275,#7438,.T.);
#10786=EDGE_CURVE('',#8276,#8277,#5293,.T.);
#10787=EDGE_CURVE('',#8278,#8277,#7439,.T.);
#10788=EDGE_CURVE('',#8278,#8279,#5294,.T.);
#10789=EDGE_CURVE('',#8280,#8279,#7440,.T.);
#10790=EDGE_CURVE('',#8280,#8281,#5295,.T.);
#10791=EDGE_CURVE('',#8282,#8281,#7441,.T.);
#10792=EDGE_CURVE('',#8282,#8283,#5296,.T.);
#10793=EDGE_CURVE('',#8284,#8283,#7442,.T.);
#10794=EDGE_CURVE('',#8284,#8285,#5297,.T.);
#10795=EDGE_CURVE('',#8286,#8285,#7443,.T.);
#10796=EDGE_CURVE('',#8286,#8287,#5298,.T.);
#10797=EDGE_CURVE('',#8288,#8287,#7444,.T.);
#10798=EDGE_CURVE('',#8288,#8289,#5299,.T.);
#10799=EDGE_CURVE('',#8290,#8289,#7445,.T.);
#10800=EDGE_CURVE('',#8290,#8291,#5300,.T.);
#10801=EDGE_CURVE('',#8292,#8291,#7446,.T.);
#10802=EDGE_CURVE('',#8292,#8293,#5301,.T.);
#10803=EDGE_CURVE('',#8294,#8293,#7447,.T.);
#10804=EDGE_CURVE('',#8294,#8295,#5302,.T.);
#10805=EDGE_CURVE('',#8296,#8295,#7448,.T.);
#10806=EDGE_CURVE('',#8296,#8297,#5303,.T.);
#10807=EDGE_CURVE('',#8298,#8297,#7449,.T.);
#10808=EDGE_CURVE('',#8298,#8299,#5304,.T.);
#10809=EDGE_CURVE('',#8300,#8299,#7450,.T.);
#10810=EDGE_CURVE('',#8300,#8301,#5305,.T.);
#10811=EDGE_CURVE('',#8302,#8301,#7451,.T.);
#10812=EDGE_CURVE('',#8302,#8303,#5306,.T.);
#10813=EDGE_CURVE('',#8304,#8303,#7452,.T.);
#10814=EDGE_CURVE('',#8304,#8305,#5307,.T.);
#10815=EDGE_CURVE('',#8235,#8305,#7453,.T.);
#10816=EDGE_CURVE('',#8306,#8306,#7454,.T.);
#10817=EDGE_CURVE('',#8307,#8307,#7455,.T.);
#10818=EDGE_CURVE('',#8308,#8308,#7456,.T.);
#10819=EDGE_CURVE('',#8309,#8309,#7457,.T.);
#10820=EDGE_CURVE('',#8310,#8311,#7458,.T.);
#10821=EDGE_CURVE('',#8311,#8238,#5308,.T.);
#10822=EDGE_CURVE('',#8237,#8310,#5309,.T.);
#10823=EDGE_CURVE('',#8312,#8311,#5310,.T.);
#10824=EDGE_CURVE('',#8239,#8312,#5311,.T.);
#10825=EDGE_CURVE('',#8312,#8313,#7459,.T.);
#10826=EDGE_CURVE('',#8313,#8240,#5312,.T.);
#10827=EDGE_CURVE('',#8314,#8313,#5313,.T.);
#10828=EDGE_CURVE('',#8241,#8314,#5314,.T.);
#10829=EDGE_CURVE('',#8314,#8315,#7460,.T.);
#10830=EDGE_CURVE('',#8315,#8242,#5315,.T.);
#10831=EDGE_CURVE('',#8316,#8315,#5316,.T.);
#10832=EDGE_CURVE('',#8243,#8316,#5317,.T.);
#10833=EDGE_CURVE('',#8316,#8317,#7461,.T.);
#10834=EDGE_CURVE('',#8317,#8244,#5318,.T.);
#10835=EDGE_CURVE('',#8318,#8317,#5319,.T.);
#10836=EDGE_CURVE('',#8245,#8318,#5320,.T.);
#10837=EDGE_CURVE('',#8318,#8319,#7462,.T.);
#10838=EDGE_CURVE('',#8319,#8246,#5321,.T.);
#10839=EDGE_CURVE('',#8247,#8320,#5322,.T.);
#10840=EDGE_CURVE('',#8320,#8321,#7463,.T.);
#10841=EDGE_CURVE('',#8321,#8248,#5323,.T.);
#10842=EDGE_CURVE('',#8322,#8321,#5324,.T.);
#10843=EDGE_CURVE('',#8249,#8322,#5325,.T.);
#10844=EDGE_CURVE('',#8322,#8323,#7464,.T.);
#10845=EDGE_CURVE('',#8323,#8250,#5326,.T.);
#10846=EDGE_CURVE('',#8251,#8324,#5327,.T.);
#10847=EDGE_CURVE('',#8324,#8325,#7465,.T.);
#10848=EDGE_CURVE('',#8325,#8252,#5328,.T.);
#10849=EDGE_CURVE('',#8326,#8325,#5329,.T.);
#10850=EDGE_CURVE('',#8253,#8326,#5330,.T.);
#10851=EDGE_CURVE('',#8326,#8327,#7466,.T.);
#10852=EDGE_CURVE('',#8327,#8254,#5331,.T.);
#10853=EDGE_CURVE('',#8328,#8329,#7467,.T.);
#10854=EDGE_CURVE('',#8329,#8256,#5332,.T.);
#10855=EDGE_CURVE('',#8255,#8328,#5333,.T.);
#10856=EDGE_CURVE('',#8330,#8329,#5334,.T.);
#10857=EDGE_CURVE('',#8257,#8330,#5335,.T.);
#10858=EDGE_CURVE('',#8330,#8331,#7468,.T.);
#10859=EDGE_CURVE('',#8331,#8258,#5336,.T.);
#10860=EDGE_CURVE('',#8332,#8331,#5337,.T.);
#10861=EDGE_CURVE('',#8259,#8332,#5338,.T.);
#10862=EDGE_CURVE('',#8332,#8333,#7469,.T.);
#10863=EDGE_CURVE('',#8333,#8260,#5339,.T.);
#10864=EDGE_CURVE('',#8334,#8333,#5340,.T.);
#10865=EDGE_CURVE('',#8261,#8334,#5341,.T.);
#10866=EDGE_CURVE('',#8334,#8335,#7470,.T.);
#10867=EDGE_CURVE('',#8335,#8262,#5342,.T.);
#10868=EDGE_CURVE('',#8336,#8335,#5343,.T.);
#10869=EDGE_CURVE('',#8263,#8336,#5344,.T.);
#10870=EDGE_CURVE('',#8336,#8337,#7471,.T.);
#10871=EDGE_CURVE('',#8337,#8264,#5345,.T.);
#10872=EDGE_CURVE('',#8265,#8338,#5346,.T.);
#10873=EDGE_CURVE('',#8338,#8339,#7472,.T.);
#10874=EDGE_CURVE('',#8339,#8266,#5347,.T.);
#10875=EDGE_CURVE('',#8340,#8339,#5348,.T.);
#10876=EDGE_CURVE('',#8267,#8340,#5349,.T.);
#10877=EDGE_CURVE('',#8340,#8341,#7473,.T.);
#10878=EDGE_CURVE('',#8341,#8268,#5350,.T.);
#10879=EDGE_CURVE('',#8269,#8342,#5351,.T.);
#10880=EDGE_CURVE('',#8342,#8343,#7474,.T.);
#10881=EDGE_CURVE('',#8343,#8270,#5352,.T.);
#10882=EDGE_CURVE('',#8344,#8343,#5353,.T.);
#10883=EDGE_CURVE('',#8271,#8344,#5354,.T.);
#10884=EDGE_CURVE('',#8344,#8345,#7475,.T.);
#10885=EDGE_CURVE('',#8345,#8272,#5355,.T.);
#10886=EDGE_CURVE('',#8346,#8347,#7476,.T.);
#10887=EDGE_CURVE('',#8347,#8274,#5356,.T.);
#10888=EDGE_CURVE('',#8273,#8346,#5357,.T.);
#10889=EDGE_CURVE('',#8348,#8347,#5358,.T.);
#10890=EDGE_CURVE('',#8275,#8348,#5359,.T.);
#10891=EDGE_CURVE('',#8348,#8349,#7477,.T.);
#10892=EDGE_CURVE('',#8349,#8276,#5360,.T.);
#10893=EDGE_CURVE('',#8350,#8349,#5361,.T.);
#10894=EDGE_CURVE('',#8277,#8350,#5362,.T.);
#10895=EDGE_CURVE('',#8350,#8351,#7478,.T.);
#10896=EDGE_CURVE('',#8351,#8278,#5363,.T.);
#10897=EDGE_CURVE('',#8352,#8351,#5364,.T.);
#10898=EDGE_CURVE('',#8279,#8352,#5365,.T.);
#10899=EDGE_CURVE('',#8352,#8353,#7479,.T.);
#10900=EDGE_CURVE('',#8353,#8280,#5366,.T.);
#10901=EDGE_CURVE('',#8354,#8353,#5367,.T.);
#10902=EDGE_CURVE('',#8281,#8354,#5368,.T.);
#10903=EDGE_CURVE('',#8354,#8355,#7480,.T.);
#10904=EDGE_CURVE('',#8355,#8282,#5369,.T.);
#10905=EDGE_CURVE('',#8283,#8356,#5370,.T.);
#10906=EDGE_CURVE('',#8356,#8357,#7481,.T.);
#10907=EDGE_CURVE('',#8357,#8284,#5371,.T.);
#10908=EDGE_CURVE('',#8358,#8357,#5372,.T.);
#10909=EDGE_CURVE('',#8285,#8358,#5373,.T.);
#10910=EDGE_CURVE('',#8358,#8359,#7482,.T.);
#10911=EDGE_CURVE('',#8359,#8286,#5374,.T.);
#10912=EDGE_CURVE('',#8287,#8360,#5375,.T.);
#10913=EDGE_CURVE('',#8360,#8361,#7483,.T.);
#10914=EDGE_CURVE('',#8361,#8288,#5376,.T.);
#10915=EDGE_CURVE('',#8362,#8361,#5377,.T.);
#10916=EDGE_CURVE('',#8289,#8362,#5378,.T.);
#10917=EDGE_CURVE('',#8362,#8363,#7484,.T.);
#10918=EDGE_CURVE('',#8363,#8290,#5379,.T.);
#10919=EDGE_CURVE('',#8364,#8365,#7485,.T.);
#10920=EDGE_CURVE('',#8365,#8292,#5380,.T.);
#10921=EDGE_CURVE('',#8291,#8364,#5381,.T.);
#10922=EDGE_CURVE('',#8366,#8365,#5382,.T.);
#10923=EDGE_CURVE('',#8293,#8366,#5383,.T.);
#10924=EDGE_CURVE('',#8366,#8367,#7486,.T.);
#10925=EDGE_CURVE('',#8367,#8294,#5384,.T.);
#10926=EDGE_CURVE('',#8368,#8367,#5385,.T.);
#10927=EDGE_CURVE('',#8295,#8368,#5386,.T.);
#10928=EDGE_CURVE('',#8368,#8369,#7487,.T.);
#10929=EDGE_CURVE('',#8369,#8296,#5387,.T.);
#10930=EDGE_CURVE('',#8370,#8369,#5388,.T.);
#10931=EDGE_CURVE('',#8297,#8370,#5389,.T.);
#10932=EDGE_CURVE('',#8370,#8371,#7488,.T.);
#10933=EDGE_CURVE('',#8371,#8298,#5390,.T.);
#10934=EDGE_CURVE('',#8372,#8371,#5391,.T.);
#10935=EDGE_CURVE('',#8299,#8372,#5392,.T.);
#10936=EDGE_CURVE('',#8372,#8373,#7489,.T.);
#10937=EDGE_CURVE('',#8373,#8300,#5393,.T.);
#10938=EDGE_CURVE('',#8301,#8374,#5394,.T.);
#10939=EDGE_CURVE('',#8374,#8375,#7490,.T.);
#10940=EDGE_CURVE('',#8375,#8302,#5395,.T.);
#10941=EDGE_CURVE('',#8376,#8375,#5396,.T.);
#10942=EDGE_CURVE('',#8303,#8376,#5397,.T.);
#10943=EDGE_CURVE('',#8376,#8377,#7491,.T.);
#10944=EDGE_CURVE('',#8377,#8304,#5398,.T.);
#10945=EDGE_CURVE('',#8305,#8378,#5399,.T.);
#10946=EDGE_CURVE('',#8378,#8236,#7492,.T.);
#10947=EDGE_CURVE('',#8309,#8379,#5400,.T.);
#10948=EDGE_CURVE('',#8379,#8379,#7493,.T.);
#10949=EDGE_CURVE('',#8308,#8380,#5401,.T.);
#10950=EDGE_CURVE('',#8380,#8380,#7494,.T.);
#10951=EDGE_CURVE('',#8230,#8229,#5402,.T.);
#10952=EDGE_CURVE('',#8307,#8381,#5403,.T.);
#10953=EDGE_CURVE('',#8381,#8381,#7495,.T.);
#10954=EDGE_CURVE('',#8306,#8382,#5404,.T.);
#10955=EDGE_CURVE('',#8382,#8382,#7496,.T.);
#10956=EDGE_CURVE('',#8378,#8377,#5405,.T.);
#10957=EDGE_CURVE('',#8374,#8373,#5406,.T.);
#10958=EDGE_CURVE('',#8364,#8363,#5407,.T.);
#10959=EDGE_CURVE('',#8360,#8359,#5408,.T.);
#10960=EDGE_CURVE('',#8356,#8355,#5409,.T.);
#10961=EDGE_CURVE('',#8346,#8345,#5410,.T.);
#10962=EDGE_CURVE('',#8342,#8341,#5411,.T.);
#10963=EDGE_CURVE('',#8338,#8337,#5412,.T.);
#10964=EDGE_CURVE('',#8328,#8327,#5413,.T.);
#10965=EDGE_CURVE('',#8324,#8323,#5414,.T.);
#10966=EDGE_CURVE('',#8320,#8319,#5415,.T.);
#10967=EDGE_CURVE('',#8310,#8234,#5416,.T.);
#10968=EDGE_CURVE('',#8383,#8383,#7497,.T.);
#10969=EDGE_CURVE('',#8384,#8384,#7498,.T.);
#10970=EDGE_CURVE('',#8385,#8385,#7499,.T.);
#10971=EDGE_CURVE('',#8385,#8383,#5417,.T.);
#10972=EDGE_CURVE('',#8384,#8386,#5418,.T.);
#10973=EDGE_CURVE('',#8386,#8386,#7500,.T.);
#10974=EDGE_CURVE('',#8387,#8387,#7501,.T.);
#10975=EDGE_CURVE('',#8387,#8388,#5419,.T.);
#10976=EDGE_CURVE('',#8388,#8388,#7502,.T.);
#10977=EDGE_CURVE('',#8389,#8389,#7503,.T.);
#10978=EDGE_CURVE('',#8389,#8390,#5420,.T.);
#10979=EDGE_CURVE('',#8390,#8390,#7504,.T.);
#10980=EDGE_CURVE('',#8391,#8391,#7505,.T.);
#10981=EDGE_CURVE('',#8391,#8392,#5421,.T.);
#10982=EDGE_CURVE('',#8392,#8392,#7506,.T.);
#10983=EDGE_CURVE('',#8393,#8393,#7507,.T.);
#10984=EDGE_CURVE('',#8393,#8394,#5422,.T.);
#10985=EDGE_CURVE('',#8394,#8394,#7508,.T.);
#10986=EDGE_CURVE('',#8395,#8396,#5423,.T.);
#10987=EDGE_CURVE('',#8396,#8397,#5424,.T.);
#10988=EDGE_CURVE('',#8398,#8397,#5425,.T.);
#10989=EDGE_CURVE('',#8395,#8398,#5426,.T.);
#10990=EDGE_CURVE('',#8399,#8395,#5427,.T.);
#10991=EDGE_CURVE('',#8400,#8398,#5428,.T.);
#10992=EDGE_CURVE('',#8399,#8400,#5429,.T.);
#10993=EDGE_CURVE('',#8401,#8399,#5430,.T.);
#10994=EDGE_CURVE('',#8402,#8400,#5431,.T.);
#10995=EDGE_CURVE('',#8401,#8402,#5432,.T.);
#10996=EDGE_CURVE('',#8396,#8401,#5433,.T.);
#10997=EDGE_CURVE('',#8397,#8402,#5434,.T.);
#10998=EDGE_CURVE('',#8403,#8404,#5435,.T.);
#10999=EDGE_CURVE('',#8403,#8405,#917,.T.);
#11000=EDGE_CURVE('',#8405,#8406,#7509,.F.);
#11001=EDGE_CURVE('',#8406,#8404,#918,.T.);
#11002=EDGE_CURVE('',#8407,#8408,#5436,.T.);
#11003=EDGE_CURVE('',#8407,#8403,#919,.T.);
#11004=EDGE_CURVE('',#8404,#8408,#920,.T.);
#11005=EDGE_CURVE('',#8409,#8410,#5437,.T.);
#11006=EDGE_CURVE('',#8409,#8407,#921,.T.);
#11007=EDGE_CURVE('',#8408,#8410,#922,.T.);
#11008=EDGE_CURVE('',#8411,#8412,#5438,.T.);
#11009=EDGE_CURVE('',#8411,#8409,#923,.T.);
#11010=EDGE_CURVE('',#8410,#8412,#924,.T.);
#11011=EDGE_CURVE('',#8413,#8414,#5439,.T.);
#11012=EDGE_CURVE('',#8413,#8411,#925,.T.);
#11013=EDGE_CURVE('',#8412,#8414,#926,.T.);
#11014=EDGE_CURVE('',#8415,#8416,#5440,.T.);
#11015=EDGE_CURVE('',#8415,#8413,#927,.T.);
#11016=EDGE_CURVE('',#8414,#8416,#928,.T.);
#11017=EDGE_CURVE('',#8417,#8418,#5441,.T.);
#11018=EDGE_CURVE('',#8417,#8415,#929,.T.);
#11019=EDGE_CURVE('',#8416,#8418,#930,.T.);
#11020=EDGE_CURVE('',#8419,#8420,#5442,.T.);
#11021=EDGE_CURVE('',#8419,#8417,#931,.T.);
#11022=EDGE_CURVE('',#8418,#8420,#932,.T.);
#11023=EDGE_CURVE('',#8421,#8422,#5443,.T.);
#11024=EDGE_CURVE('',#8421,#8419,#933,.T.);
#11025=EDGE_CURVE('',#8420,#8422,#934,.T.);
#11026=EDGE_CURVE('',#8423,#8424,#5444,.T.);
#11027=EDGE_CURVE('',#8423,#8421,#935,.T.);
#11028=EDGE_CURVE('',#8422,#8424,#936,.T.);
#11029=EDGE_CURVE('',#8425,#8426,#5445,.T.);
#11030=EDGE_CURVE('',#8425,#8423,#937,.T.);
#11031=EDGE_CURVE('',#8424,#8426,#938,.T.);
#11032=EDGE_CURVE('',#8427,#8428,#5446,.T.);
#11033=EDGE_CURVE('',#8427,#8425,#939,.T.);
#11034=EDGE_CURVE('',#8426,#8428,#940,.T.);
#11035=EDGE_CURVE('',#8429,#8430,#5447,.T.);
#11036=EDGE_CURVE('',#8429,#8427,#941,.T.);
#11037=EDGE_CURVE('',#8428,#8430,#942,.T.);
#11038=EDGE_CURVE('',#8431,#8432,#5448,.T.);
#11039=EDGE_CURVE('',#8431,#8429,#943,.T.);
#11040=EDGE_CURVE('',#8430,#8432,#944,.T.);
#11041=EDGE_CURVE('',#8433,#8434,#5449,.T.);
#11042=EDGE_CURVE('',#8433,#8431,#945,.T.);
#11043=EDGE_CURVE('',#8432,#8434,#946,.T.);
#11044=EDGE_CURVE('',#8435,#8436,#5450,.T.);
#11045=EDGE_CURVE('',#8435,#8433,#947,.T.);
#11046=EDGE_CURVE('',#8434,#8436,#948,.T.);
#11047=EDGE_CURVE('',#8437,#8438,#5451,.T.);
#11048=EDGE_CURVE('',#8437,#8435,#949,.T.);
#11049=EDGE_CURVE('',#8436,#8438,#950,.T.);
#11050=EDGE_CURVE('',#8439,#8440,#5452,.T.);
#11051=EDGE_CURVE('',#8439,#8437,#951,.T.);
#11052=EDGE_CURVE('',#8438,#8440,#952,.T.);
#11053=EDGE_CURVE('',#8441,#8442,#5453,.T.);
#11054=EDGE_CURVE('',#8441,#8439,#953,.T.);
#11055=EDGE_CURVE('',#8440,#8442,#954,.T.);
#11056=EDGE_CURVE('',#8443,#8444,#5454,.T.);
#11057=EDGE_CURVE('',#8443,#8445,#955,.T.);
#11058=EDGE_CURVE('',#8445,#8446,#7510,.T.);
#11059=EDGE_CURVE('',#8444,#8446,#956,.T.);
#11060=EDGE_CURVE('',#8447,#8448,#5455,.T.);
#11061=EDGE_CURVE('',#8447,#8443,#957,.T.);
#11062=EDGE_CURVE('',#8448,#8444,#958,.T.);
#11063=EDGE_CURVE('',#8449,#8450,#5456,.T.);
#11064=EDGE_CURVE('',#8449,#8447,#959,.T.);
#11065=EDGE_CURVE('',#8450,#8448,#960,.T.);
#11066=EDGE_CURVE('',#8451,#8452,#5457,.T.);
#11067=EDGE_CURVE('',#8451,#8449,#961,.T.);
#11068=EDGE_CURVE('',#8452,#8450,#962,.T.);
#11069=EDGE_CURVE('',#8453,#8454,#5458,.T.);
#11070=EDGE_CURVE('',#8453,#8451,#963,.T.);
#11071=EDGE_CURVE('',#8454,#8452,#964,.T.);
#11072=EDGE_CURVE('',#8455,#8456,#5459,.T.);
#11073=EDGE_CURVE('',#8455,#8453,#965,.T.);
#11074=EDGE_CURVE('',#8456,#8454,#966,.T.);
#11075=EDGE_CURVE('',#8457,#8458,#5460,.T.);
#11076=EDGE_CURVE('',#8457,#8455,#967,.T.);
#11077=EDGE_CURVE('',#8458,#8456,#968,.T.);
#11078=EDGE_CURVE('',#8459,#8460,#5461,.T.);
#11079=EDGE_CURVE('',#8459,#8457,#969,.T.);
#11080=EDGE_CURVE('',#8460,#8458,#970,.T.);
#11081=EDGE_CURVE('',#8461,#8462,#5462,.T.);
#11082=EDGE_CURVE('',#8461,#8459,#971,.T.);
#11083=EDGE_CURVE('',#8462,#8460,#972,.T.);
#11084=EDGE_CURVE('',#8463,#8464,#5463,.T.);
#11085=EDGE_CURVE('',#8463,#8461,#973,.T.);
#11086=EDGE_CURVE('',#8464,#8462,#974,.T.);
#11087=EDGE_CURVE('',#8465,#8466,#5464,.T.);
#11088=EDGE_CURVE('',#8465,#8463,#975,.T.);
#11089=EDGE_CURVE('',#8466,#8464,#976,.T.);
#11090=EDGE_CURVE('',#8467,#8468,#5465,.T.);
#11091=EDGE_CURVE('',#8467,#8465,#977,.T.);
#11092=EDGE_CURVE('',#8468,#8466,#978,.T.);
#11093=EDGE_CURVE('',#8469,#8470,#5466,.T.);
#11094=EDGE_CURVE('',#8469,#8467,#979,.T.);
#11095=EDGE_CURVE('',#8470,#8468,#980,.T.);
#11096=EDGE_CURVE('',#8471,#8472,#5467,.T.);
#11097=EDGE_CURVE('',#8471,#8469,#981,.T.);
#11098=EDGE_CURVE('',#8472,#8470,#982,.T.);
#11099=EDGE_CURVE('',#8473,#8474,#5468,.T.);
#11100=EDGE_CURVE('',#8473,#8471,#983,.T.);
#11101=EDGE_CURVE('',#8474,#8472,#984,.T.);
#11102=EDGE_CURVE('',#8475,#8476,#5469,.T.);
#11103=EDGE_CURVE('',#8475,#8473,#985,.T.);
#11104=EDGE_CURVE('',#8476,#8474,#986,.T.);
#11105=EDGE_CURVE('',#8477,#8478,#5470,.T.);
#11106=EDGE_CURVE('',#8477,#8475,#987,.T.);
#11107=EDGE_CURVE('',#8478,#8476,#988,.T.);
#11108=EDGE_CURVE('',#8479,#8480,#5471,.T.);
#11109=EDGE_CURVE('',#8479,#8477,#989,.T.);
#11110=EDGE_CURVE('',#8480,#8478,#990,.T.);
#11111=EDGE_CURVE('',#8481,#8482,#5472,.T.);
#11112=EDGE_CURVE('',#8481,#8479,#991,.T.);
#11113=EDGE_CURVE('',#8482,#8480,#992,.T.);
#11114=EDGE_CURVE('',#8446,#8483,#993,.T.);
#11115=EDGE_CURVE('',#8484,#8445,#994,.T.);
#11116=EDGE_CURVE('',#8485,#8484,#7511,.T.);
#11117=EDGE_CURVE('',#8483,#8485,#995,.T.);
#11118=EDGE_CURVE('',#8483,#8486,#5473,.T.);
#11119=EDGE_CURVE('',#8486,#8486,#7512,.T.);
#11120=EDGE_CURVE('',#8487,#8481,#996,.T.);
#11121=EDGE_CURVE('',#8405,#8487,#997,.T.);
#11122=EDGE_CURVE('',#8484,#8441,#998,.T.);
#11123=EDGE_CURVE('',#8488,#8482,#999,.T.);
#11124=EDGE_CURVE('',#8487,#8488,#7513,.T.);
#11125=EDGE_CURVE('',#8442,#8485,#1000,.T.);
#11126=EDGE_CURVE('',#8488,#8406,#1001,.T.);
#11127=EDGE_CURVE('',#8489,#8490,#5474,.T.);
#11128=EDGE_CURVE('',#8489,#8491,#5475,.T.);
#11129=EDGE_CURVE('',#8491,#8492,#5476,.T.);
#11130=EDGE_CURVE('',#8490,#8492,#5477,.T.);
#11131=EDGE_CURVE('',#8493,#8489,#5478,.T.);
#11132=EDGE_CURVE('',#8493,#8494,#5479,.T.);
#11133=EDGE_CURVE('',#8494,#8491,#5480,.T.);
#11134=EDGE_CURVE('',#8495,#8493,#5481,.T.);
#11135=EDGE_CURVE('',#8495,#8496,#5482,.T.);
#11136=EDGE_CURVE('',#8496,#8494,#5483,.T.);
#11137=EDGE_CURVE('',#8497,#8495,#5484,.T.);
#11138=EDGE_CURVE('',#8497,#8498,#5485,.T.);
#11139=EDGE_CURVE('',#8498,#8496,#5486,.T.);
#11140=EDGE_CURVE('',#8499,#8497,#5487,.T.);
#11141=EDGE_CURVE('',#8499,#8500,#5488,.T.);
#11142=EDGE_CURVE('',#8500,#8498,#5489,.T.);
#11143=EDGE_CURVE('',#8490,#8499,#5490,.T.);
#11144=EDGE_CURVE('',#8492,#8500,#5491,.T.);
#11145=EDGE_CURVE('',#8501,#8501,#7514,.T.);
#11146=EDGE_CURVE('',#8501,#8502,#5492,.T.);
#11147=EDGE_CURVE('',#8502,#8502,#7515,.T.);
#11148=EDGE_CURVE('',#8503,#8503,#7516,.T.);
#11149=EDGE_CURVE('',#8503,#8504,#5493,.T.);
#11150=EDGE_CURVE('',#8504,#8504,#7517,.T.);
#11151=EDGE_CURVE('',#8505,#8506,#5494,.T.);
#11152=EDGE_CURVE('',#8506,#8507,#1002,.T.);
#11153=EDGE_CURVE('',#8507,#8508,#7518,.T.);
#11154=EDGE_CURVE('',#8508,#8509,#5495,.T.);
#11155=EDGE_CURVE('',#8509,#8509,#7519,.F.);
#11156=EDGE_CURVE('',#8508,#8510,#7520,.T.);
#11157=EDGE_CURVE('',#8510,#8505,#1003,.T.);
#11158=EDGE_CURVE('',#8511,#8512,#5496,.T.);
#11159=EDGE_CURVE('',#8512,#8506,#1004,.T.);
#11160=EDGE_CURVE('',#8505,#8511,#1005,.T.);
#11161=EDGE_CURVE('',#8513,#8514,#5497,.T.);
#11162=EDGE_CURVE('',#8514,#8512,#1006,.T.);
#11163=EDGE_CURVE('',#8511,#8513,#1007,.T.);
#11164=EDGE_CURVE('',#8515,#8516,#5498,.T.);
#11165=EDGE_CURVE('',#8516,#8514,#1008,.T.);
#11166=EDGE_CURVE('',#8513,#8515,#1009,.T.);
#11167=EDGE_CURVE('',#8517,#8518,#5499,.T.);
#11168=EDGE_CURVE('',#8518,#8516,#1010,.T.);
#11169=EDGE_CURVE('',#8515,#8517,#1011,.T.);
#11170=EDGE_CURVE('',#8519,#8520,#5500,.T.);
#11171=EDGE_CURVE('',#8520,#8518,#1012,.T.);
#11172=EDGE_CURVE('',#8517,#8519,#1013,.T.);
#11173=EDGE_CURVE('',#8521,#8522,#5501,.T.);
#11174=EDGE_CURVE('',#8522,#8520,#1014,.T.);
#11175=EDGE_CURVE('',#8519,#8521,#1015,.T.);
#11176=EDGE_CURVE('',#8523,#8524,#5502,.T.);
#11177=EDGE_CURVE('',#8523,#8525,#1016,.T.);
#11178=EDGE_CURVE('',#8526,#8525,#7521,.T.);
#11179=EDGE_CURVE('',#8526,#8524,#1017,.T.);
#11180=EDGE_CURVE('',#8527,#8528,#5503,.T.);
#11181=EDGE_CURVE('',#8528,#8529,#1018,.T.);
#11182=EDGE_CURVE('',#8530,#8529,#7522,.T.);
#11183=EDGE_CURVE('',#8527,#8530,#1019,.T.);
#11184=EDGE_CURVE('',#8531,#8532,#5504,.T.);
#11185=EDGE_CURVE('',#8532,#8528,#1020,.T.);
#11186=EDGE_CURVE('',#8531,#8527,#1021,.T.);
#11187=EDGE_CURVE('',#8533,#8534,#5505,.T.);
#11188=EDGE_CURVE('',#8534,#8532,#1022,.T.);
#11189=EDGE_CURVE('',#8533,#8531,#1023,.T.);
#11190=EDGE_CURVE('',#8535,#8536,#5506,.T.);
#11191=EDGE_CURVE('',#8536,#8534,#1024,.T.);
#11192=EDGE_CURVE('',#8535,#8533,#1025,.T.);
#11193=EDGE_CURVE('',#8537,#8538,#5507,.T.);
#11194=EDGE_CURVE('',#8538,#8536,#1026,.T.);
#11195=EDGE_CURVE('',#8537,#8535,#1027,.T.);
#11196=EDGE_CURVE('',#8539,#8540,#5508,.T.);
#11197=EDGE_CURVE('',#8540,#8538,#1028,.T.);
#11198=EDGE_CURVE('',#8539,#8537,#1029,.T.);
#11199=EDGE_CURVE('',#8541,#8542,#5509,.T.);
#11200=EDGE_CURVE('',#8542,#8540,#1030,.T.);
#11201=EDGE_CURVE('',#8541,#8539,#1031,.T.);
#11202=EDGE_CURVE('',#8543,#8544,#5510,.T.);
#11203=EDGE_CURVE('',#8545,#8543,#1032,.T.);
#11204=EDGE_CURVE('',#8546,#8545,#7523,.T.);
#11205=EDGE_CURVE('',#8546,#8544,#1033,.T.);
#11206=EDGE_CURVE('',#8547,#8548,#5511,.T.);
#11207=EDGE_CURVE('',#8548,#8549,#1034,.T.);
#11208=EDGE_CURVE('',#8549,#8550,#7524,.T.);
#11209=EDGE_CURVE('',#8550,#8551,#5512,.T.);
#11210=EDGE_CURVE('',#8551,#8551,#7525,.F.);
#11211=EDGE_CURVE('',#8550,#8552,#7526,.T.);
#11212=EDGE_CURVE('',#8552,#8547,#1035,.T.);
#11213=EDGE_CURVE('',#8553,#8554,#5513,.T.);
#11214=EDGE_CURVE('',#8554,#8548,#1036,.T.);
#11215=EDGE_CURVE('',#8547,#8553,#1037,.T.);
#11216=EDGE_CURVE('',#8555,#8556,#5514,.T.);
#11217=EDGE_CURVE('',#8556,#8554,#1038,.T.);
#11218=EDGE_CURVE('',#8553,#8555,#1039,.T.);
#11219=EDGE_CURVE('',#8557,#8558,#5515,.T.);
#11220=EDGE_CURVE('',#8558,#8556,#1040,.T.);
#11221=EDGE_CURVE('',#8555,#8557,#1041,.T.);
#11222=EDGE_CURVE('',#8559,#8560,#5516,.T.);
#11223=EDGE_CURVE('',#8560,#8558,#1042,.T.);
#11224=EDGE_CURVE('',#8557,#8559,#1043,.T.);
#11225=EDGE_CURVE('',#8561,#8562,#5517,.T.);
#11226=EDGE_CURVE('',#8562,#8560,#1044,.T.);
#11227=EDGE_CURVE('',#8559,#8561,#1045,.T.);
#11228=EDGE_CURVE('',#8563,#8564,#5518,.T.);
#11229=EDGE_CURVE('',#8564,#8562,#1046,.T.);
#11230=EDGE_CURVE('',#8561,#8563,#1047,.T.);
#11231=EDGE_CURVE('',#8565,#8566,#5519,.T.);
#11232=EDGE_CURVE('',#8565,#8567,#1048,.T.);
#11233=EDGE_CURVE('',#8568,#8567,#7527,.T.);
#11234=EDGE_CURVE('',#8568,#8566,#1049,.T.);
#11235=EDGE_CURVE('',#8569,#8570,#5520,.T.);
#11236=EDGE_CURVE('',#8570,#8571,#1050,.T.);
#11237=EDGE_CURVE('',#8572,#8571,#7528,.T.);
#11238=EDGE_CURVE('',#8569,#8572,#1051,.T.);
#11239=EDGE_CURVE('',#8573,#8574,#5521,.T.);
#11240=EDGE_CURVE('',#8574,#8570,#1052,.T.);
#11241=EDGE_CURVE('',#8573,#8569,#1053,.T.);
#11242=EDGE_CURVE('',#8575,#8576,#5522,.T.);
#11243=EDGE_CURVE('',#8576,#8574,#1054,.T.);
#11244=EDGE_CURVE('',#8575,#8573,#1055,.T.);
#11245=EDGE_CURVE('',#8577,#8578,#5523,.T.);
#11246=EDGE_CURVE('',#8578,#8576,#1056,.T.);
#11247=EDGE_CURVE('',#8577,#8575,#1057,.T.);
#11248=EDGE_CURVE('',#8579,#8580,#5524,.T.);
#11249=EDGE_CURVE('',#8580,#8578,#1058,.T.);
#11250=EDGE_CURVE('',#8579,#8577,#1059,.T.);
#11251=EDGE_CURVE('',#8581,#8582,#5525,.T.);
#11252=EDGE_CURVE('',#8582,#8580,#1060,.T.);
#11253=EDGE_CURVE('',#8581,#8579,#1061,.T.);
#11254=EDGE_CURVE('',#8583,#8584,#5526,.T.);
#11255=EDGE_CURVE('',#8584,#8582,#1062,.T.);
#11256=EDGE_CURVE('',#8583,#8581,#1063,.T.);
#11257=EDGE_CURVE('',#8585,#8586,#5527,.T.);
#11258=EDGE_CURVE('',#8587,#8585,#1064,.T.);
#11259=EDGE_CURVE('',#8588,#8587,#7529,.T.);
#11260=EDGE_CURVE('',#8588,#8586,#1065,.T.);
#11261=EDGE_CURVE('',#8589,#8590,#5528,.T.);
#11262=EDGE_CURVE('',#8590,#8591,#1066,.T.);
#11263=EDGE_CURVE('',#8591,#8592,#7530,.T.);
#11264=EDGE_CURVE('',#8592,#8593,#5529,.T.);
#11265=EDGE_CURVE('',#8593,#8593,#7531,.F.);
#11266=EDGE_CURVE('',#8592,#8594,#7532,.T.);
#11267=EDGE_CURVE('',#8594,#8589,#1067,.T.);
#11268=EDGE_CURVE('',#8595,#8596,#5530,.T.);
#11269=EDGE_CURVE('',#8596,#8590,#1068,.T.);
#11270=EDGE_CURVE('',#8589,#8595,#1069,.T.);
#11271=EDGE_CURVE('',#8597,#8598,#5531,.T.);
#11272=EDGE_CURVE('',#8598,#8596,#1070,.T.);
#11273=EDGE_CURVE('',#8595,#8597,#1071,.T.);
#11274=EDGE_CURVE('',#8599,#8600,#5532,.T.);
#11275=EDGE_CURVE('',#8600,#8598,#1072,.T.);
#11276=EDGE_CURVE('',#8597,#8599,#1073,.T.);
#11277=EDGE_CURVE('',#8601,#8602,#5533,.T.);
#11278=EDGE_CURVE('',#8602,#8600,#1074,.T.);
#11279=EDGE_CURVE('',#8599,#8601,#1075,.T.);
#11280=EDGE_CURVE('',#8603,#8604,#5534,.T.);
#11281=EDGE_CURVE('',#8604,#8602,#1076,.T.);
#11282=EDGE_CURVE('',#8601,#8603,#1077,.T.);
#11283=EDGE_CURVE('',#8605,#8606,#5535,.T.);
#11284=EDGE_CURVE('',#8606,#8604,#1078,.T.);
#11285=EDGE_CURVE('',#8603,#8605,#1079,.T.);
#11286=EDGE_CURVE('',#8607,#8608,#5536,.T.);
#11287=EDGE_CURVE('',#8607,#8609,#1080,.T.);
#11288=EDGE_CURVE('',#8610,#8609,#7533,.T.);
#11289=EDGE_CURVE('',#8610,#8608,#1081,.T.);
#11290=EDGE_CURVE('',#8611,#8612,#5537,.T.);
#11291=EDGE_CURVE('',#8612,#8613,#1082,.T.);
#11292=EDGE_CURVE('',#8614,#8613,#7534,.T.);
#11293=EDGE_CURVE('',#8611,#8614,#1083,.T.);
#11294=EDGE_CURVE('',#8615,#8616,#5538,.T.);
#11295=EDGE_CURVE('',#8616,#8612,#1084,.T.);
#11296=EDGE_CURVE('',#8615,#8611,#1085,.T.);
#11297=EDGE_CURVE('',#8617,#8618,#5539,.T.);
#11298=EDGE_CURVE('',#8618,#8616,#1086,.T.);
#11299=EDGE_CURVE('',#8617,#8615,#1087,.T.);
#11300=EDGE_CURVE('',#8619,#8620,#5540,.T.);
#11301=EDGE_CURVE('',#8620,#8618,#1088,.T.);
#11302=EDGE_CURVE('',#8619,#8617,#1089,.T.);
#11303=EDGE_CURVE('',#8621,#8622,#5541,.T.);
#11304=EDGE_CURVE('',#8622,#8620,#1090,.T.);
#11305=EDGE_CURVE('',#8621,#8619,#1091,.T.);
#11306=EDGE_CURVE('',#8623,#8624,#5542,.T.);
#11307=EDGE_CURVE('',#8624,#8622,#1092,.T.);
#11308=EDGE_CURVE('',#8623,#8621,#1093,.T.);
#11309=EDGE_CURVE('',#8625,#8626,#5543,.T.);
#11310=EDGE_CURVE('',#8626,#8624,#1094,.T.);
#11311=EDGE_CURVE('',#8625,#8623,#1095,.T.);
#11312=EDGE_CURVE('',#8627,#8628,#5544,.T.);
#11313=EDGE_CURVE('',#8629,#8627,#1096,.T.);
#11314=EDGE_CURVE('',#8630,#8629,#7535,.T.);
#11315=EDGE_CURVE('',#8630,#8628,#1097,.T.);
#11316=EDGE_CURVE('',#8591,#8614,#1098,.T.);
#11317=EDGE_CURVE('',#8613,#8594,#1099,.T.);
#11318=EDGE_CURVE('',#8628,#8626,#1100,.T.);
#11319=EDGE_CURVE('',#8627,#8625,#1101,.T.);
#11320=EDGE_CURVE('',#8609,#8630,#1102,.T.);
#11321=EDGE_CURVE('',#8605,#8607,#1103,.T.);
#11322=EDGE_CURVE('',#8608,#8606,#1104,.T.);
#11323=EDGE_CURVE('',#8629,#8610,#1105,.T.);
#11324=EDGE_CURVE('',#8549,#8572,#1106,.T.);
#11325=EDGE_CURVE('',#8571,#8552,#1107,.T.);
#11326=EDGE_CURVE('',#8586,#8584,#1108,.T.);
#11327=EDGE_CURVE('',#8585,#8583,#1109,.T.);
#11328=EDGE_CURVE('',#8567,#8588,#1110,.T.);
#11329=EDGE_CURVE('',#8563,#8565,#1111,.T.);
#11330=EDGE_CURVE('',#8566,#8564,#1112,.T.);
#11331=EDGE_CURVE('',#8587,#8568,#1113,.T.);
#11332=EDGE_CURVE('',#8507,#8530,#1114,.T.);
#11333=EDGE_CURVE('',#8529,#8510,#1115,.T.);
#11334=EDGE_CURVE('',#8544,#8542,#1116,.T.);
#11335=EDGE_CURVE('',#8543,#8541,#1117,.T.);
#11336=EDGE_CURVE('',#8525,#8546,#1118,.T.);
#11337=EDGE_CURVE('',#8521,#8523,#1119,.T.);
#11338=EDGE_CURVE('',#8524,#8522,#1120,.T.);
#11339=EDGE_CURVE('',#8545,#8526,#1121,.T.);
#11340=EDGE_CURVE('',#8631,#8631,#7536,.T.);
#11341=EDGE_CURVE('',#8632,#8631,#7537,.T.);
#11342=EDGE_CURVE('',#8633,#8633,#7538,.T.);
#11343=EDGE_CURVE('',#8633,#8634,#5545,.T.);
#11344=EDGE_CURVE('',#8634,#8634,#7539,.T.);
#11345=EDGE_CURVE('',#8635,#8635,#7540,.T.);
#11346=EDGE_CURVE('',#8635,#8636,#5546,.T.);
#11347=EDGE_CURVE('',#8636,#8636,#7541,.T.);
#11348=EDGE_CURVE('',#8637,#8637,#7542,.T.);
#11349=EDGE_CURVE('',#8637,#8638,#5547,.T.);
#11350=EDGE_CURVE('',#8638,#8638,#7543,.T.);
#11351=EDGE_CURVE('',#8639,#8639,#7544,.T.);
#11352=EDGE_CURVE('',#8639,#8640,#5548,.T.);
#11353=EDGE_CURVE('',#8640,#8640,#7545,.T.);
#11354=EDGE_CURVE('',#8641,#8641,#7546,.T.);
#11355=EDGE_CURVE('',#8641,#8642,#7547,.T.);
#11356=EDGE_CURVE('',#8642,#8642,#7548,.T.);
#11357=EDGE_CURVE('',#8643,#8643,#7549,.T.);
#11358=EDGE_CURVE('',#8643,#8642,#5549,.T.);
#11359=EDGE_CURVE('',#8644,#8644,#7550,.T.);
#11360=EDGE_CURVE('',#8644,#8645,#5550,.T.);
#11361=EDGE_CURVE('',#8645,#8645,#7551,.T.);
#11362=EDGE_CURVE('',#8646,#8647,#5551,.T.);
#11363=EDGE_CURVE('',#8646,#8648,#1122,.T.);
#11364=EDGE_CURVE('',#8648,#8649,#7552,.F.);
#11365=EDGE_CURVE('',#8649,#8647,#1123,.T.);
#11366=EDGE_CURVE('',#8650,#8651,#5552,.T.);
#11367=EDGE_CURVE('',#8650,#8646,#1124,.T.);
#11368=EDGE_CURVE('',#8647,#8651,#1125,.T.);
#11369=EDGE_CURVE('',#8652,#8653,#5553,.T.);
#11370=EDGE_CURVE('',#8652,#8650,#1126,.T.);
#11371=EDGE_CURVE('',#8651,#8653,#1127,.T.);
#11372=EDGE_CURVE('',#8654,#8655,#5554,.T.);
#11373=EDGE_CURVE('',#8654,#8652,#1128,.T.);
#11374=EDGE_CURVE('',#8653,#8655,#1129,.T.);
#11375=EDGE_CURVE('',#8656,#8657,#5555,.T.);
#11376=EDGE_CURVE('',#8656,#8654,#1130,.T.);
#11377=EDGE_CURVE('',#8655,#8657,#1131,.T.);
#11378=EDGE_CURVE('',#8658,#8659,#5556,.T.);
#11379=EDGE_CURVE('',#8658,#8656,#1132,.T.);
#11380=EDGE_CURVE('',#8657,#8659,#1133,.T.);
#11381=EDGE_CURVE('',#8660,#8661,#5557,.T.);
#11382=EDGE_CURVE('',#8660,#8658,#1134,.T.);
#11383=EDGE_CURVE('',#8659,#8661,#1135,.T.);
#11384=EDGE_CURVE('',#8662,#8663,#5558,.T.);
#11385=EDGE_CURVE('',#8662,#8660,#1136,.T.);
#11386=EDGE_CURVE('',#8661,#8663,#1137,.T.);
#11387=EDGE_CURVE('',#8664,#8665,#5559,.T.);
#11388=EDGE_CURVE('',#8664,#8662,#1138,.T.);
#11389=EDGE_CURVE('',#8663,#8665,#1139,.T.);
#11390=EDGE_CURVE('',#8666,#8667,#5560,.T.);
#11391=EDGE_CURVE('',#8666,#8664,#1140,.T.);
#11392=EDGE_CURVE('',#8665,#8667,#1141,.T.);
#11393=EDGE_CURVE('',#8668,#8669,#5561,.T.);
#11394=EDGE_CURVE('',#8668,#8666,#1142,.T.);
#11395=EDGE_CURVE('',#8667,#8669,#1143,.T.);
#11396=EDGE_CURVE('',#8670,#8671,#5562,.T.);
#11397=EDGE_CURVE('',#8670,#8668,#1144,.T.);
#11398=EDGE_CURVE('',#8669,#8671,#1145,.T.);
#11399=EDGE_CURVE('',#8672,#8673,#5563,.T.);
#11400=EDGE_CURVE('',#8672,#8670,#1146,.T.);
#11401=EDGE_CURVE('',#8671,#8673,#1147,.T.);
#11402=EDGE_CURVE('',#8674,#8675,#5564,.T.);
#11403=EDGE_CURVE('',#8674,#8672,#1148,.T.);
#11404=EDGE_CURVE('',#8673,#8675,#1149,.T.);
#11405=EDGE_CURVE('',#8676,#8677,#5565,.T.);
#11406=EDGE_CURVE('',#8676,#8674,#1150,.T.);
#11407=EDGE_CURVE('',#8675,#8677,#1151,.T.);
#11408=EDGE_CURVE('',#8678,#8679,#5566,.T.);
#11409=EDGE_CURVE('',#8678,#8676,#1152,.T.);
#11410=EDGE_CURVE('',#8677,#8679,#1153,.T.);
#11411=EDGE_CURVE('',#8680,#8681,#5567,.T.);
#11412=EDGE_CURVE('',#8680,#8678,#1154,.T.);
#11413=EDGE_CURVE('',#8679,#8681,#1155,.T.);
#11414=EDGE_CURVE('',#8682,#8683,#5568,.T.);
#11415=EDGE_CURVE('',#8682,#8680,#1156,.T.);
#11416=EDGE_CURVE('',#8681,#8683,#1157,.T.);
#11417=EDGE_CURVE('',#8684,#8685,#5569,.T.);
#11418=EDGE_CURVE('',#8684,#8682,#1158,.T.);
#11419=EDGE_CURVE('',#8683,#8685,#1159,.T.);
#11420=EDGE_CURVE('',#8686,#8687,#5570,.T.);
#11421=EDGE_CURVE('',#8686,#8684,#1160,.T.);
#11422=EDGE_CURVE('',#8685,#8687,#1161,.T.);
#11423=EDGE_CURVE('',#8688,#8689,#5571,.T.);
#11424=EDGE_CURVE('',#8688,#8686,#1162,.T.);
#11425=EDGE_CURVE('',#8687,#8689,#1163,.T.);
#11426=EDGE_CURVE('',#8690,#8691,#5572,.T.);
#11427=EDGE_CURVE('',#8690,#8688,#1164,.T.);
#11428=EDGE_CURVE('',#8689,#8691,#1165,.T.);
#11429=EDGE_CURVE('',#8692,#8693,#5573,.T.);
#11430=EDGE_CURVE('',#8692,#8690,#1166,.T.);
#11431=EDGE_CURVE('',#8691,#8693,#1167,.T.);
#11432=EDGE_CURVE('',#8694,#8695,#5574,.T.);
#11433=EDGE_CURVE('',#8694,#8692,#1168,.T.);
#11434=EDGE_CURVE('',#8693,#8695,#1169,.T.);
#11435=EDGE_CURVE('',#8696,#8697,#5575,.T.);
#11436=EDGE_CURVE('',#8696,#8694,#1170,.T.);
#11437=EDGE_CURVE('',#8695,#8697,#1171,.T.);
#11438=EDGE_CURVE('',#8698,#8699,#5576,.T.);
#11439=EDGE_CURVE('',#8698,#8696,#1172,.T.);
#11440=EDGE_CURVE('',#8697,#8699,#1173,.T.);
#11441=EDGE_CURVE('',#8700,#8701,#5577,.T.);
#11442=EDGE_CURVE('',#8700,#8698,#1174,.T.);
#11443=EDGE_CURVE('',#8699,#8701,#1175,.T.);
#11444=EDGE_CURVE('',#8702,#8703,#5578,.T.);
#11445=EDGE_CURVE('',#8702,#8700,#1176,.T.);
#11446=EDGE_CURVE('',#8701,#8703,#1177,.T.);
#11447=EDGE_CURVE('',#8704,#8705,#5579,.T.);
#11448=EDGE_CURVE('',#8704,#8702,#1178,.T.);
#11449=EDGE_CURVE('',#8703,#8705,#1179,.T.);
#11450=EDGE_CURVE('',#8706,#8707,#5580,.T.);
#11451=EDGE_CURVE('',#8706,#8704,#1180,.T.);
#11452=EDGE_CURVE('',#8705,#8707,#1181,.T.);
#11453=EDGE_CURVE('',#8708,#8709,#5581,.T.);
#11454=EDGE_CURVE('',#8708,#8706,#1182,.T.);
#11455=EDGE_CURVE('',#8707,#8709,#1183,.T.);
#11456=EDGE_CURVE('',#8710,#8711,#5582,.T.);
#11457=EDGE_CURVE('',#8710,#8708,#1184,.T.);
#11458=EDGE_CURVE('',#8709,#8711,#1185,.T.);
#11459=EDGE_CURVE('',#8712,#8713,#5583,.T.);
#11460=EDGE_CURVE('',#8712,#8710,#1186,.T.);
#11461=EDGE_CURVE('',#8711,#8713,#1187,.T.);
#11462=EDGE_CURVE('',#8714,#8715,#5584,.T.);
#11463=EDGE_CURVE('',#8714,#8712,#1188,.T.);
#11464=EDGE_CURVE('',#8713,#8715,#1189,.T.);
#11465=EDGE_CURVE('',#8716,#8717,#5585,.T.);
#11466=EDGE_CURVE('',#8716,#8714,#1190,.T.);
#11467=EDGE_CURVE('',#8715,#8717,#1191,.T.);
#11468=EDGE_CURVE('',#8718,#8719,#5586,.T.);
#11469=EDGE_CURVE('',#8718,#8716,#1192,.T.);
#11470=EDGE_CURVE('',#8717,#8719,#1193,.T.);
#11471=EDGE_CURVE('',#8720,#8721,#5587,.T.);
#11472=EDGE_CURVE('',#8720,#8718,#1194,.T.);
#11473=EDGE_CURVE('',#8719,#8721,#1195,.T.);
#11474=EDGE_CURVE('',#8722,#8723,#5588,.T.);
#11475=EDGE_CURVE('',#8722,#8720,#1196,.T.);
#11476=EDGE_CURVE('',#8721,#8723,#1197,.T.);
#11477=EDGE_CURVE('',#8724,#8725,#5589,.T.);
#11478=EDGE_CURVE('',#8724,#8722,#1198,.T.);
#11479=EDGE_CURVE('',#8723,#8725,#1199,.T.);
#11480=EDGE_CURVE('',#8726,#8727,#5590,.T.);
#11481=EDGE_CURVE('',#8726,#8724,#1200,.T.);
#11482=EDGE_CURVE('',#8725,#8727,#1201,.T.);
#11483=EDGE_CURVE('',#8728,#8729,#5591,.T.);
#11484=EDGE_CURVE('',#8728,#8726,#1202,.T.);
#11485=EDGE_CURVE('',#8727,#8729,#1203,.T.);
#11486=EDGE_CURVE('',#8730,#8731,#5592,.T.);
#11487=EDGE_CURVE('',#8730,#8728,#1204,.T.);
#11488=EDGE_CURVE('',#8729,#8731,#1205,.T.);
#11489=EDGE_CURVE('',#8732,#8733,#5593,.T.);
#11490=EDGE_CURVE('',#8732,#8730,#1206,.T.);
#11491=EDGE_CURVE('',#8731,#8733,#1207,.T.);
#11492=EDGE_CURVE('',#8734,#8735,#5594,.T.);
#11493=EDGE_CURVE('',#8734,#8732,#1208,.T.);
#11494=EDGE_CURVE('',#8733,#8735,#1209,.T.);
#11495=EDGE_CURVE('',#8736,#8737,#5595,.T.);
#11496=EDGE_CURVE('',#8736,#8734,#1210,.T.);
#11497=EDGE_CURVE('',#8735,#8737,#1211,.T.);
#11498=EDGE_CURVE('',#8738,#8739,#5596,.T.);
#11499=EDGE_CURVE('',#8738,#8736,#1212,.T.);
#11500=EDGE_CURVE('',#8737,#8739,#1213,.T.);
#11501=EDGE_CURVE('',#8740,#8741,#5597,.T.);
#11502=EDGE_CURVE('',#8740,#8738,#1214,.T.);
#11503=EDGE_CURVE('',#8739,#8741,#1215,.T.);
#11504=EDGE_CURVE('',#8742,#8743,#5598,.T.);
#11505=EDGE_CURVE('',#8742,#8740,#1216,.T.);
#11506=EDGE_CURVE('',#8741,#8743,#1217,.T.);
#11507=EDGE_CURVE('',#8744,#8745,#5599,.T.);
#11508=EDGE_CURVE('',#8744,#8742,#1218,.T.);
#11509=EDGE_CURVE('',#8743,#8745,#1219,.T.);
#11510=EDGE_CURVE('',#8746,#8747,#5600,.T.);
#11511=EDGE_CURVE('',#8746,#8744,#1220,.T.);
#11512=EDGE_CURVE('',#8745,#8747,#1221,.T.);
#11513=EDGE_CURVE('',#8748,#8749,#5601,.T.);
#11514=EDGE_CURVE('',#8748,#8746,#1222,.T.);
#11515=EDGE_CURVE('',#8747,#8749,#1223,.T.);
#11516=EDGE_CURVE('',#8750,#8751,#5602,.T.);
#11517=EDGE_CURVE('',#8750,#8748,#1224,.T.);
#11518=EDGE_CURVE('',#8749,#8751,#1225,.T.);
#11519=EDGE_CURVE('',#8752,#8753,#5603,.T.);
#11520=EDGE_CURVE('',#8752,#8750,#1226,.T.);
#11521=EDGE_CURVE('',#8751,#8753,#1227,.T.);
#11522=EDGE_CURVE('',#8754,#8755,#5604,.T.);
#11523=EDGE_CURVE('',#8754,#8752,#1228,.T.);
#11524=EDGE_CURVE('',#8753,#8755,#1229,.T.);
#11525=EDGE_CURVE('',#8756,#8757,#5605,.T.);
#11526=EDGE_CURVE('',#8756,#8754,#1230,.T.);
#11527=EDGE_CURVE('',#8755,#8757,#1231,.T.);
#11528=EDGE_CURVE('',#8758,#8759,#5606,.T.);
#11529=EDGE_CURVE('',#8758,#8756,#1232,.T.);
#11530=EDGE_CURVE('',#8757,#8759,#1233,.T.);
#11531=EDGE_CURVE('',#8760,#8761,#5607,.T.);
#11532=EDGE_CURVE('',#8760,#8758,#1234,.T.);
#11533=EDGE_CURVE('',#8759,#8761,#1235,.T.);
#11534=EDGE_CURVE('',#8762,#8763,#5608,.T.);
#11535=EDGE_CURVE('',#8762,#8760,#1236,.T.);
#11536=EDGE_CURVE('',#8761,#8763,#1237,.T.);
#11537=EDGE_CURVE('',#8764,#8765,#5609,.T.);
#11538=EDGE_CURVE('',#8764,#8762,#1238,.T.);
#11539=EDGE_CURVE('',#8763,#8765,#1239,.T.);
#11540=EDGE_CURVE('',#8766,#8767,#5610,.T.);
#11541=EDGE_CURVE('',#8766,#8764,#1240,.T.);
#11542=EDGE_CURVE('',#8765,#8767,#1241,.T.);
#11543=EDGE_CURVE('',#8768,#8769,#5611,.T.);
#11544=EDGE_CURVE('',#8768,#8770,#1242,.T.);
#11545=EDGE_CURVE('',#8771,#8770,#7553,.T.);
#11546=EDGE_CURVE('',#8769,#8771,#1243,.T.);
#11547=EDGE_CURVE('',#8772,#8773,#5612,.T.);
#11548=EDGE_CURVE('',#8772,#8768,#1244,.T.);
#11549=EDGE_CURVE('',#8773,#8769,#1245,.T.);
#11550=EDGE_CURVE('',#8774,#8775,#5613,.T.);
#11551=EDGE_CURVE('',#8774,#8772,#1246,.T.);
#11552=EDGE_CURVE('',#8775,#8773,#1247,.T.);
#11553=EDGE_CURVE('',#8776,#8777,#5614,.T.);
#11554=EDGE_CURVE('',#8776,#8774,#1248,.T.);
#11555=EDGE_CURVE('',#8777,#8775,#1249,.T.);
#11556=EDGE_CURVE('',#8778,#8779,#5615,.T.);
#11557=EDGE_CURVE('',#8778,#8776,#1250,.T.);
#11558=EDGE_CURVE('',#8779,#8777,#1251,.T.);
#11559=EDGE_CURVE('',#8780,#8781,#5616,.T.);
#11560=EDGE_CURVE('',#8780,#8778,#1252,.T.);
#11561=EDGE_CURVE('',#8781,#8779,#1253,.T.);
#11562=EDGE_CURVE('',#8782,#8783,#5617,.T.);
#11563=EDGE_CURVE('',#8782,#8780,#1254,.T.);
#11564=EDGE_CURVE('',#8783,#8781,#1255,.T.);
#11565=EDGE_CURVE('',#8784,#8785,#5618,.T.);
#11566=EDGE_CURVE('',#8784,#8782,#1256,.T.);
#11567=EDGE_CURVE('',#8785,#8783,#1257,.T.);
#11568=EDGE_CURVE('',#8786,#8787,#5619,.T.);
#11569=EDGE_CURVE('',#8786,#8784,#1258,.T.);
#11570=EDGE_CURVE('',#8787,#8785,#1259,.T.);
#11571=EDGE_CURVE('',#8788,#8789,#5620,.T.);
#11572=EDGE_CURVE('',#8788,#8786,#1260,.T.);
#11573=EDGE_CURVE('',#8789,#8787,#1261,.T.);
#11574=EDGE_CURVE('',#8790,#8791,#5621,.T.);
#11575=EDGE_CURVE('',#8790,#8788,#1262,.T.);
#11576=EDGE_CURVE('',#8791,#8789,#1263,.T.);
#11577=EDGE_CURVE('',#8792,#8793,#5622,.T.);
#11578=EDGE_CURVE('',#8792,#8790,#1264,.T.);
#11579=EDGE_CURVE('',#8793,#8791,#1265,.T.);
#11580=EDGE_CURVE('',#8794,#8795,#5623,.T.);
#11581=EDGE_CURVE('',#8794,#8792,#1266,.T.);
#11582=EDGE_CURVE('',#8795,#8793,#1267,.T.);
#11583=EDGE_CURVE('',#8796,#8797,#5624,.T.);
#11584=EDGE_CURVE('',#8796,#8794,#1268,.T.);
#11585=EDGE_CURVE('',#8797,#8795,#1269,.T.);
#11586=EDGE_CURVE('',#8798,#8799,#5625,.T.);
#11587=EDGE_CURVE('',#8798,#8796,#1270,.T.);
#11588=EDGE_CURVE('',#8799,#8797,#1271,.T.);
#11589=EDGE_CURVE('',#8800,#8801,#5626,.T.);
#11590=EDGE_CURVE('',#8800,#8798,#1272,.T.);
#11591=EDGE_CURVE('',#8801,#8799,#1273,.T.);
#11592=EDGE_CURVE('',#8802,#8803,#5627,.T.);
#11593=EDGE_CURVE('',#8802,#8800,#1274,.T.);
#11594=EDGE_CURVE('',#8803,#8801,#1275,.T.);
#11595=EDGE_CURVE('',#8804,#8805,#5628,.T.);
#11596=EDGE_CURVE('',#8804,#8802,#1276,.T.);
#11597=EDGE_CURVE('',#8805,#8803,#1277,.T.);
#11598=EDGE_CURVE('',#8806,#8807,#5629,.T.);
#11599=EDGE_CURVE('',#8806,#8804,#1278,.T.);
#11600=EDGE_CURVE('',#8807,#8805,#1279,.T.);
#11601=EDGE_CURVE('',#8808,#8809,#5630,.T.);
#11602=EDGE_CURVE('',#8808,#8806,#1280,.T.);
#11603=EDGE_CURVE('',#8809,#8807,#1281,.T.);
#11604=EDGE_CURVE('',#8810,#8811,#5631,.T.);
#11605=EDGE_CURVE('',#8810,#8808,#1282,.T.);
#11606=EDGE_CURVE('',#8811,#8809,#1283,.T.);
#11607=EDGE_CURVE('',#8812,#8813,#5632,.T.);
#11608=EDGE_CURVE('',#8812,#8810,#1284,.T.);
#11609=EDGE_CURVE('',#8813,#8811,#1285,.T.);
#11610=EDGE_CURVE('',#8814,#8815,#5633,.T.);
#11611=EDGE_CURVE('',#8814,#8812,#1286,.T.);
#11612=EDGE_CURVE('',#8815,#8813,#1287,.T.);
#11613=EDGE_CURVE('',#8816,#8817,#5634,.T.);
#11614=EDGE_CURVE('',#8816,#8814,#1288,.T.);
#11615=EDGE_CURVE('',#8817,#8815,#1289,.T.);
#11616=EDGE_CURVE('',#8818,#8819,#5635,.T.);
#11617=EDGE_CURVE('',#8818,#8816,#1290,.T.);
#11618=EDGE_CURVE('',#8819,#8817,#1291,.T.);
#11619=EDGE_CURVE('',#8820,#8821,#5636,.T.);
#11620=EDGE_CURVE('',#8820,#8818,#1292,.T.);
#11621=EDGE_CURVE('',#8821,#8819,#1293,.T.);
#11622=EDGE_CURVE('',#8822,#8823,#5637,.T.);
#11623=EDGE_CURVE('',#8822,#8820,#1294,.T.);
#11624=EDGE_CURVE('',#8823,#8821,#1295,.T.);
#11625=EDGE_CURVE('',#8824,#8825,#5638,.T.);
#11626=EDGE_CURVE('',#8824,#8822,#1296,.T.);
#11627=EDGE_CURVE('',#8825,#8823,#1297,.T.);
#11628=EDGE_CURVE('',#8826,#8827,#5639,.T.);
#11629=EDGE_CURVE('',#8826,#8824,#1298,.T.);
#11630=EDGE_CURVE('',#8827,#8825,#1299,.T.);
#11631=EDGE_CURVE('',#8828,#8829,#5640,.T.);
#11632=EDGE_CURVE('',#8828,#8826,#1300,.T.);
#11633=EDGE_CURVE('',#8829,#8827,#1301,.T.);
#11634=EDGE_CURVE('',#8830,#8831,#5641,.T.);
#11635=EDGE_CURVE('',#8830,#8828,#1302,.T.);
#11636=EDGE_CURVE('',#8831,#8829,#1303,.T.);
#11637=EDGE_CURVE('',#8832,#8833,#5642,.T.);
#11638=EDGE_CURVE('',#8832,#8830,#1304,.T.);
#11639=EDGE_CURVE('',#8833,#8831,#1305,.T.);
#11640=EDGE_CURVE('',#8834,#8835,#5643,.T.);
#11641=EDGE_CURVE('',#8834,#8832,#1306,.T.);
#11642=EDGE_CURVE('',#8835,#8833,#1307,.T.);
#11643=EDGE_CURVE('',#8836,#8837,#5644,.T.);
#11644=EDGE_CURVE('',#8836,#8834,#1308,.T.);
#11645=EDGE_CURVE('',#8837,#8835,#1309,.T.);
#11646=EDGE_CURVE('',#8838,#8839,#5645,.T.);
#11647=EDGE_CURVE('',#8838,#8836,#1310,.T.);
#11648=EDGE_CURVE('',#8839,#8837,#1311,.T.);
#11649=EDGE_CURVE('',#8840,#8841,#5646,.T.);
#11650=EDGE_CURVE('',#8840,#8838,#1312,.T.);
#11651=EDGE_CURVE('',#8841,#8839,#1313,.T.);
#11652=EDGE_CURVE('',#8842,#8843,#5647,.T.);
#11653=EDGE_CURVE('',#8842,#8840,#1314,.T.);
#11654=EDGE_CURVE('',#8843,#8841,#1315,.T.);
#11655=EDGE_CURVE('',#8844,#8845,#5648,.T.);
#11656=EDGE_CURVE('',#8844,#8842,#1316,.T.);
#11657=EDGE_CURVE('',#8845,#8843,#1317,.T.);
#11658=EDGE_CURVE('',#8846,#8847,#5649,.T.);
#11659=EDGE_CURVE('',#8846,#8844,#1318,.T.);
#11660=EDGE_CURVE('',#8847,#8845,#1319,.T.);
#11661=EDGE_CURVE('',#8848,#8849,#5650,.T.);
#11662=EDGE_CURVE('',#8848,#8846,#1320,.T.);
#11663=EDGE_CURVE('',#8849,#8847,#1321,.T.);
#11664=EDGE_CURVE('',#8850,#8851,#5651,.T.);
#11665=EDGE_CURVE('',#8850,#8848,#1322,.T.);
#11666=EDGE_CURVE('',#8851,#8849,#1323,.T.);
#11667=EDGE_CURVE('',#8852,#8853,#5652,.T.);
#11668=EDGE_CURVE('',#8852,#8850,#1324,.T.);
#11669=EDGE_CURVE('',#8853,#8851,#1325,.T.);
#11670=EDGE_CURVE('',#8854,#8855,#5653,.T.);
#11671=EDGE_CURVE('',#8854,#8852,#1326,.T.);
#11672=EDGE_CURVE('',#8855,#8853,#1327,.T.);
#11673=EDGE_CURVE('',#8856,#8857,#5654,.T.);
#11674=EDGE_CURVE('',#8856,#8854,#1328,.T.);
#11675=EDGE_CURVE('',#8857,#8855,#1329,.T.);
#11676=EDGE_CURVE('',#8858,#8859,#5655,.T.);
#11677=EDGE_CURVE('',#8858,#8856,#1330,.T.);
#11678=EDGE_CURVE('',#8859,#8857,#1331,.T.);
#11679=EDGE_CURVE('',#8860,#8861,#5656,.T.);
#11680=EDGE_CURVE('',#8860,#8858,#1332,.T.);
#11681=EDGE_CURVE('',#8861,#8859,#1333,.T.);
#11682=EDGE_CURVE('',#8862,#8863,#5657,.T.);
#11683=EDGE_CURVE('',#8862,#8860,#1334,.T.);
#11684=EDGE_CURVE('',#8863,#8861,#1335,.T.);
#11685=EDGE_CURVE('',#8864,#8865,#5658,.T.);
#11686=EDGE_CURVE('',#8864,#8862,#1336,.T.);
#11687=EDGE_CURVE('',#8865,#8863,#1337,.T.);
#11688=EDGE_CURVE('',#8866,#8867,#5659,.T.);
#11689=EDGE_CURVE('',#8866,#8864,#1338,.T.);
#11690=EDGE_CURVE('',#8867,#8865,#1339,.T.);
#11691=EDGE_CURVE('',#8868,#8869,#5660,.T.);
#11692=EDGE_CURVE('',#8868,#8866,#1340,.T.);
#11693=EDGE_CURVE('',#8869,#8867,#1341,.T.);
#11694=EDGE_CURVE('',#8870,#8871,#5661,.T.);
#11695=EDGE_CURVE('',#8870,#8868,#1342,.T.);
#11696=EDGE_CURVE('',#8871,#8869,#1343,.T.);
#11697=EDGE_CURVE('',#8872,#8873,#5662,.T.);
#11698=EDGE_CURVE('',#8872,#8870,#1344,.T.);
#11699=EDGE_CURVE('',#8873,#8871,#1345,.T.);
#11700=EDGE_CURVE('',#8874,#8875,#5663,.T.);
#11701=EDGE_CURVE('',#8874,#8872,#1346,.T.);
#11702=EDGE_CURVE('',#8875,#8873,#1347,.T.);
#11703=EDGE_CURVE('',#8876,#8877,#5664,.T.);
#11704=EDGE_CURVE('',#8876,#8874,#1348,.T.);
#11705=EDGE_CURVE('',#8877,#8875,#1349,.T.);
#11706=EDGE_CURVE('',#8878,#8879,#5665,.T.);
#11707=EDGE_CURVE('',#8878,#8876,#1350,.T.);
#11708=EDGE_CURVE('',#8879,#8877,#1351,.T.);
#11709=EDGE_CURVE('',#8880,#8881,#5666,.T.);
#11710=EDGE_CURVE('',#8880,#8878,#1352,.T.);
#11711=EDGE_CURVE('',#8881,#8879,#1353,.T.);
#11712=EDGE_CURVE('',#8882,#8883,#5667,.T.);
#11713=EDGE_CURVE('',#8882,#8880,#1354,.T.);
#11714=EDGE_CURVE('',#8883,#8881,#1355,.T.);
#11715=EDGE_CURVE('',#8884,#8885,#5668,.T.);
#11716=EDGE_CURVE('',#8884,#8882,#1356,.T.);
#11717=EDGE_CURVE('',#8885,#8883,#1357,.T.);
#11718=EDGE_CURVE('',#8886,#8887,#5669,.T.);
#11719=EDGE_CURVE('',#8886,#8884,#1358,.T.);
#11720=EDGE_CURVE('',#8887,#8885,#1359,.T.);
#11721=EDGE_CURVE('',#8888,#8889,#5670,.T.);
#11722=EDGE_CURVE('',#8888,#8886,#1360,.T.);
#11723=EDGE_CURVE('',#8889,#8887,#1361,.T.);
#11724=EDGE_CURVE('',#8890,#8771,#1362,.T.);
#11725=EDGE_CURVE('',#8767,#8890,#1363,.T.);
#11726=EDGE_CURVE('',#8891,#8649,#1364,.T.);
#11727=EDGE_CURVE('',#8891,#8889,#1365,.T.);
#11728=EDGE_CURVE('',#8892,#8891,#7554,.T.);
#11729=EDGE_CURVE('',#8892,#8888,#1366,.T.);
#11730=EDGE_CURVE('',#8770,#8893,#1367,.T.);
#11731=EDGE_CURVE('',#8648,#8892,#1368,.T.);
#11732=EDGE_CURVE('',#8893,#8766,#1369,.T.);
#11733=EDGE_CURVE('',#8893,#8890,#7555,.F.);
#11734=EDGE_CURVE('',#8894,#8895,#5671,.T.);
#11735=EDGE_CURVE('',#8895,#8896,#5672,.T.);
#11736=EDGE_CURVE('',#8896,#8897,#5673,.T.);
#11737=EDGE_CURVE('',#8897,#8898,#5674,.T.);
#11738=EDGE_CURVE('',#8898,#8899,#5675,.T.);
#11739=EDGE_CURVE('',#8899,#8894,#5676,.T.);
#11740=EDGE_CURVE('',#8900,#8901,#5677,.T.);
#11741=EDGE_CURVE('',#8902,#8900,#5678,.T.);
#11742=EDGE_CURVE('',#8903,#8902,#5679,.T.);
#11743=EDGE_CURVE('',#8904,#8903,#5680,.T.);
#11744=EDGE_CURVE('',#8905,#8904,#5681,.T.);
#11745=EDGE_CURVE('',#8901,#8905,#5682,.T.);
#11746=EDGE_CURVE('',#8906,#8906,#7556,.T.);
#11747=EDGE_CURVE('',#8900,#8894,#5683,.T.);
#11748=EDGE_CURVE('',#8902,#8899,#5684,.T.);
#11749=EDGE_CURVE('',#8903,#8898,#5685,.T.);
#11750=EDGE_CURVE('',#8904,#8897,#5686,.T.);
#11751=EDGE_CURVE('',#8905,#8896,#5687,.T.);
#11752=EDGE_CURVE('',#8901,#8895,#5688,.T.);
#11753=EDGE_CURVE('',#8906,#8907,#5689,.T.);
#11754=EDGE_CURVE('',#8907,#8907,#7557,.T.);
#11755=EDGE_CURVE('',#8907,#8908,#7558,.T.);
#11756=EDGE_CURVE('',#8909,#8910,#5690,.T.);
#11757=EDGE_CURVE('',#8910,#8911,#1370,.T.);
#11758=EDGE_CURVE('',#8912,#8911,#7559,.F.);
#11759=EDGE_CURVE('',#8912,#8909,#1371,.T.);
#11760=EDGE_CURVE('',#8913,#8914,#5691,.T.);
#11761=EDGE_CURVE('',#8914,#8910,#1372,.T.);
#11762=EDGE_CURVE('',#8909,#8913,#1373,.T.);
#11763=EDGE_CURVE('',#8915,#8916,#5692,.T.);
#11764=EDGE_CURVE('',#8916,#8914,#1374,.T.);
#11765=EDGE_CURVE('',#8913,#8915,#1375,.T.);
#11766=EDGE_CURVE('',#8917,#8918,#5693,.T.);
#11767=EDGE_CURVE('',#8918,#8916,#1376,.T.);
#11768=EDGE_CURVE('',#8915,#8917,#1377,.T.);
#11769=EDGE_CURVE('',#8919,#8920,#5694,.T.);
#11770=EDGE_CURVE('',#8920,#8918,#1378,.T.);
#11771=EDGE_CURVE('',#8917,#8919,#1379,.T.);
#11772=EDGE_CURVE('',#8921,#8922,#5695,.T.);
#11773=EDGE_CURVE('',#8922,#8920,#1380,.T.);
#11774=EDGE_CURVE('',#8919,#8921,#1381,.T.);
#11775=EDGE_CURVE('',#8923,#8924,#5696,.T.);
#11776=EDGE_CURVE('',#8924,#8922,#1382,.T.);
#11777=EDGE_CURVE('',#8921,#8923,#1383,.T.);
#11778=EDGE_CURVE('',#8925,#8926,#5697,.T.);
#11779=EDGE_CURVE('',#8925,#8927,#1384,.T.);
#11780=EDGE_CURVE('',#8928,#8927,#7560,.T.);
#11781=EDGE_CURVE('',#8928,#8926,#1385,.T.);
#11782=EDGE_CURVE('',#8929,#8930,#5698,.T.);
#11783=EDGE_CURVE('',#8930,#8931,#1386,.T.);
#11784=EDGE_CURVE('',#8932,#8931,#7561,.T.);
#11785=EDGE_CURVE('',#8929,#8932,#1387,.T.);
#11786=EDGE_CURVE('',#8933,#8934,#5699,.T.);
#11787=EDGE_CURVE('',#8934,#8930,#1388,.T.);
#11788=EDGE_CURVE('',#8933,#8929,#1389,.T.);
#11789=EDGE_CURVE('',#8935,#8936,#5700,.T.);
#11790=EDGE_CURVE('',#8936,#8934,#1390,.T.);
#11791=EDGE_CURVE('',#8935,#8933,#1391,.T.);
#11792=EDGE_CURVE('',#8937,#8938,#5701,.T.);
#11793=EDGE_CURVE('',#8938,#8936,#1392,.T.);
#11794=EDGE_CURVE('',#8937,#8935,#1393,.T.);
#11795=EDGE_CURVE('',#8939,#8940,#5702,.T.);
#11796=EDGE_CURVE('',#8940,#8938,#1394,.T.);
#11797=EDGE_CURVE('',#8939,#8937,#1395,.T.);
#11798=EDGE_CURVE('',#8941,#8942,#5703,.T.);
#11799=EDGE_CURVE('',#8942,#8940,#1396,.T.);
#11800=EDGE_CURVE('',#8941,#8939,#1397,.T.);
#11801=EDGE_CURVE('',#8943,#8944,#5704,.T.);
#11802=EDGE_CURVE('',#8944,#8942,#1398,.T.);
#11803=EDGE_CURVE('',#8943,#8941,#1399,.T.);
#11804=EDGE_CURVE('',#8945,#8946,#5705,.T.);
#11805=EDGE_CURVE('',#8947,#8945,#1400,.T.);
#11806=EDGE_CURVE('',#8948,#8947,#7562,.T.);
#11807=EDGE_CURVE('',#8948,#8946,#1401,.T.);
#11808=EDGE_CURVE('',#8946,#8944,#1402,.T.);
#11809=EDGE_CURVE('',#8945,#8943,#1403,.T.);
#11810=EDGE_CURVE('',#8931,#8912,#1404,.T.);
#11811=EDGE_CURVE('',#8927,#8948,#1405,.T.);
#11812=EDGE_CURVE('',#8923,#8925,#1406,.T.);
#11813=EDGE_CURVE('',#8911,#8932,#1407,.T.);
#11814=EDGE_CURVE('',#8926,#8924,#1408,.T.);
#11815=EDGE_CURVE('',#8947,#8928,#1409,.T.);
#11816=EDGE_CURVE('',#8949,#8950,#5706,.T.);
#11817=EDGE_CURVE('',#8950,#8951,#5707,.T.);
#11818=EDGE_CURVE('',#8951,#8952,#5708,.T.);
#11819=EDGE_CURVE('',#8952,#8953,#5709,.T.);
#11820=EDGE_CURVE('',#8953,#8954,#5710,.T.);
#11821=EDGE_CURVE('',#8954,#8949,#5711,.T.);
#11822=EDGE_CURVE('',#8955,#8956,#5712,.T.);
#11823=EDGE_CURVE('',#8956,#8949,#5713,.T.);
#11824=EDGE_CURVE('',#8955,#8954,#5714,.T.);
#11825=EDGE_CURVE('',#8957,#8955,#5715,.T.);
#11826=EDGE_CURVE('',#8957,#8953,#5716,.T.);
#11827=EDGE_CURVE('',#8958,#8957,#5717,.T.);
#11828=EDGE_CURVE('',#8958,#8952,#5718,.T.);
#11829=EDGE_CURVE('',#8959,#8958,#5719,.T.);
#11830=EDGE_CURVE('',#8959,#8951,#5720,.T.);
#11831=EDGE_CURVE('',#8960,#8959,#5721,.T.);
#11832=EDGE_CURVE('',#8960,#8950,#5722,.T.);
#11833=EDGE_CURVE('',#8956,#8960,#5723,.T.);
#11834=EDGE_CURVE('',#8961,#8961,#7563,.T.);
#11835=EDGE_CURVE('',#8961,#8962,#5724,.T.);
#11836=EDGE_CURVE('',#8962,#8962,#7564,.T.);
#11837=EDGE_CURVE('',#8963,#8963,#7565,.T.);
#11838=EDGE_CURVE('',#8963,#8964,#5725,.T.);
#11839=EDGE_CURVE('',#8964,#8964,#7566,.T.);
#11840=EDGE_CURVE('',#8965,#8966,#5726,.T.);
#11841=EDGE_CURVE('',#8965,#8967,#1410,.T.);
#11842=EDGE_CURVE('',#8967,#8968,#7567,.F.);
#11843=EDGE_CURVE('',#8968,#8966,#1411,.T.);
#11844=EDGE_CURVE('',#8969,#8970,#5727,.T.);
#11845=EDGE_CURVE('',#8969,#8965,#1412,.T.);
#11846=EDGE_CURVE('',#8966,#8970,#1413,.T.);
#11847=EDGE_CURVE('',#8971,#8972,#5728,.T.);
#11848=EDGE_CURVE('',#8971,#8969,#1414,.T.);
#11849=EDGE_CURVE('',#8970,#8972,#1415,.T.);
#11850=EDGE_CURVE('',#8973,#8974,#5729,.T.);
#11851=EDGE_CURVE('',#8973,#8971,#1416,.T.);
#11852=EDGE_CURVE('',#8972,#8974,#1417,.T.);
#11853=EDGE_CURVE('',#8975,#8976,#5730,.T.);
#11854=EDGE_CURVE('',#8975,#8973,#1418,.T.);
#11855=EDGE_CURVE('',#8974,#8976,#1419,.T.);
#11856=EDGE_CURVE('',#8977,#8978,#5731,.T.);
#11857=EDGE_CURVE('',#8977,#8975,#1420,.T.);
#11858=EDGE_CURVE('',#8976,#8978,#1421,.T.);
#11859=EDGE_CURVE('',#8979,#8980,#5732,.T.);
#11860=EDGE_CURVE('',#8979,#8977,#1422,.T.);
#11861=EDGE_CURVE('',#8978,#8980,#1423,.T.);
#11862=EDGE_CURVE('',#8981,#8982,#5733,.T.);
#11863=EDGE_CURVE('',#8981,#8979,#1424,.T.);
#11864=EDGE_CURVE('',#8980,#8982,#1425,.T.);
#11865=EDGE_CURVE('',#8983,#8984,#5734,.T.);
#11866=EDGE_CURVE('',#8983,#8981,#1426,.T.);
#11867=EDGE_CURVE('',#8982,#8984,#1427,.T.);
#11868=EDGE_CURVE('',#8985,#8986,#5735,.T.);
#11869=EDGE_CURVE('',#8985,#8983,#1428,.T.);
#11870=EDGE_CURVE('',#8984,#8986,#1429,.T.);
#11871=EDGE_CURVE('',#8987,#8988,#5736,.T.);
#11872=EDGE_CURVE('',#8987,#8985,#1430,.T.);
#11873=EDGE_CURVE('',#8986,#8988,#1431,.T.);
#11874=EDGE_CURVE('',#8989,#8990,#5737,.T.);
#11875=EDGE_CURVE('',#8989,#8987,#1432,.T.);
#11876=EDGE_CURVE('',#8988,#8990,#1433,.T.);
#11877=EDGE_CURVE('',#8991,#8992,#5738,.T.);
#11878=EDGE_CURVE('',#8991,#8989,#1434,.T.);
#11879=EDGE_CURVE('',#8990,#8992,#1435,.T.);
#11880=EDGE_CURVE('',#8993,#8994,#5739,.T.);
#11881=EDGE_CURVE('',#8993,#8991,#1436,.T.);
#11882=EDGE_CURVE('',#8992,#8994,#1437,.T.);
#11883=EDGE_CURVE('',#8995,#8996,#5740,.T.);
#11884=EDGE_CURVE('',#8995,#8993,#1438,.T.);
#11885=EDGE_CURVE('',#8994,#8996,#1439,.T.);
#11886=EDGE_CURVE('',#8997,#8998,#5741,.T.);
#11887=EDGE_CURVE('',#8997,#8999,#1440,.T.);
#11888=EDGE_CURVE('',#8999,#9000,#7568,.T.);
#11889=EDGE_CURVE('',#8998,#9000,#1441,.T.);
#11890=EDGE_CURVE('',#9001,#9002,#5742,.T.);
#11891=EDGE_CURVE('',#9001,#8997,#1442,.T.);
#11892=EDGE_CURVE('',#9002,#8998,#1443,.T.);
#11893=EDGE_CURVE('',#9003,#9004,#5743,.T.);
#11894=EDGE_CURVE('',#9003,#9001,#1444,.T.);
#11895=EDGE_CURVE('',#9004,#9002,#1445,.T.);
#11896=EDGE_CURVE('',#9005,#9006,#5744,.T.);
#11897=EDGE_CURVE('',#9005,#9003,#1446,.T.);
#11898=EDGE_CURVE('',#9006,#9004,#1447,.T.);
#11899=EDGE_CURVE('',#9007,#9008,#5745,.T.);
#11900=EDGE_CURVE('',#9007,#9005,#1448,.T.);
#11901=EDGE_CURVE('',#9008,#9006,#1449,.T.);
#11902=EDGE_CURVE('',#9009,#9010,#5746,.T.);
#11903=EDGE_CURVE('',#9009,#9007,#1450,.T.);
#11904=EDGE_CURVE('',#9010,#9008,#1451,.T.);
#11905=EDGE_CURVE('',#9011,#9012,#5747,.T.);
#11906=EDGE_CURVE('',#9011,#9009,#1452,.T.);
#11907=EDGE_CURVE('',#9012,#9010,#1453,.T.);
#11908=EDGE_CURVE('',#9013,#9014,#5748,.T.);
#11909=EDGE_CURVE('',#9013,#9011,#1454,.T.);
#11910=EDGE_CURVE('',#9014,#9012,#1455,.T.);
#11911=EDGE_CURVE('',#9015,#9016,#5749,.T.);
#11912=EDGE_CURVE('',#9015,#9013,#1456,.T.);
#11913=EDGE_CURVE('',#9016,#9014,#1457,.T.);
#11914=EDGE_CURVE('',#9017,#9018,#5750,.T.);
#11915=EDGE_CURVE('',#9017,#9015,#1458,.T.);
#11916=EDGE_CURVE('',#9018,#9016,#1459,.T.);
#11917=EDGE_CURVE('',#9019,#9020,#5751,.T.);
#11918=EDGE_CURVE('',#9019,#9017,#1460,.T.);
#11919=EDGE_CURVE('',#9020,#9018,#1461,.T.);
#11920=EDGE_CURVE('',#9021,#9022,#5752,.T.);
#11921=EDGE_CURVE('',#9021,#9019,#1462,.T.);
#11922=EDGE_CURVE('',#9022,#9020,#1463,.T.);
#11923=EDGE_CURVE('',#9023,#9024,#5753,.T.);
#11924=EDGE_CURVE('',#9023,#9021,#1464,.T.);
#11925=EDGE_CURVE('',#9024,#9022,#1465,.T.);
#11926=EDGE_CURVE('',#9025,#9026,#5754,.T.);
#11927=EDGE_CURVE('',#9025,#9023,#1466,.T.);
#11928=EDGE_CURVE('',#9026,#9024,#1467,.T.);
#11929=EDGE_CURVE('',#9027,#9028,#5755,.T.);
#11930=EDGE_CURVE('',#9027,#9025,#1468,.T.);
#11931=EDGE_CURVE('',#9028,#9026,#1469,.T.);
#11932=EDGE_CURVE('',#9000,#9029,#1470,.T.);
#11933=EDGE_CURVE('',#9030,#8999,#1471,.T.);
#11934=EDGE_CURVE('',#9031,#9030,#7569,.T.);
#11935=EDGE_CURVE('',#9029,#9031,#1472,.T.);
#11936=EDGE_CURVE('',#9029,#9032,#5756,.T.);
#11937=EDGE_CURVE('',#9032,#9032,#7570,.T.);
#11938=EDGE_CURVE('',#9033,#9027,#1473,.T.);
#11939=EDGE_CURVE('',#8967,#9033,#1474,.T.);
#11940=EDGE_CURVE('',#9030,#8995,#1475,.T.);
#11941=EDGE_CURVE('',#9034,#9028,#1476,.T.);
#11942=EDGE_CURVE('',#9033,#9034,#7571,.T.);
#11943=EDGE_CURVE('',#8996,#9031,#1477,.T.);
#11944=EDGE_CURVE('',#9034,#8968,#1478,.T.);
#11945=EDGE_CURVE('',#9035,#9036,#5757,.T.);
#11946=EDGE_CURVE('',#9035,#9037,#5758,.T.);
#11947=EDGE_CURVE('',#9037,#9038,#5759,.T.);
#11948=EDGE_CURVE('',#9036,#9038,#5760,.T.);
#11949=EDGE_CURVE('',#9039,#9035,#5761,.T.);
#11950=EDGE_CURVE('',#9039,#9040,#5762,.T.);
#11951=EDGE_CURVE('',#9040,#9037,#5763,.T.);
#11952=EDGE_CURVE('',#9041,#9039,#5764,.T.);
#11953=EDGE_CURVE('',#9041,#9042,#5765,.T.);
#11954=EDGE_CURVE('',#9042,#9040,#5766,.T.);
#11955=EDGE_CURVE('',#9043,#9041,#5767,.T.);
#11956=EDGE_CURVE('',#9043,#9044,#5768,.T.);
#11957=EDGE_CURVE('',#9044,#9042,#5769,.T.);
#11958=EDGE_CURVE('',#9045,#9043,#5770,.T.);
#11959=EDGE_CURVE('',#9045,#9046,#5771,.T.);
#11960=EDGE_CURVE('',#9046,#9044,#5772,.T.);
#11961=EDGE_CURVE('',#9036,#9045,#5773,.T.);
#11962=EDGE_CURVE('',#9038,#9046,#5774,.T.);
#11963=EDGE_CURVE('',#9047,#9047,#7572,.T.);
#11964=EDGE_CURVE('',#9047,#9048,#5775,.T.);
#11965=EDGE_CURVE('',#9048,#9048,#7573,.T.);
#11966=EDGE_CURVE('',#9049,#9050,#5776,.T.);
#11967=EDGE_CURVE('',#9050,#9051,#1479,.T.);
#11968=EDGE_CURVE('',#9052,#9051,#7574,.F.);
#11969=EDGE_CURVE('',#9052,#9049,#1480,.T.);
#11970=EDGE_CURVE('',#9053,#9054,#5777,.T.);
#11971=EDGE_CURVE('',#9054,#9050,#1481,.T.);
#11972=EDGE_CURVE('',#9049,#9053,#1482,.T.);
#11973=EDGE_CURVE('',#9055,#9056,#5778,.T.);
#11974=EDGE_CURVE('',#9056,#9054,#1483,.T.);
#11975=EDGE_CURVE('',#9053,#9055,#1484,.T.);
#11976=EDGE_CURVE('',#9057,#9058,#5779,.T.);
#11977=EDGE_CURVE('',#9058,#9056,#1485,.T.);
#11978=EDGE_CURVE('',#9055,#9057,#1486,.T.);
#11979=EDGE_CURVE('',#9059,#9060,#5780,.T.);
#11980=EDGE_CURVE('',#9060,#9058,#1487,.T.);
#11981=EDGE_CURVE('',#9057,#9059,#1488,.T.);
#11982=EDGE_CURVE('',#9061,#9062,#5781,.T.);
#11983=EDGE_CURVE('',#9062,#9060,#1489,.T.);
#11984=EDGE_CURVE('',#9059,#9061,#1490,.T.);
#11985=EDGE_CURVE('',#9063,#9064,#5782,.T.);
#11986=EDGE_CURVE('',#9064,#9062,#1491,.T.);
#11987=EDGE_CURVE('',#9061,#9063,#1492,.T.);
#11988=EDGE_CURVE('',#9065,#9066,#5783,.T.);
#11989=EDGE_CURVE('',#9066,#9064,#1493,.T.);
#11990=EDGE_CURVE('',#9063,#9065,#1494,.T.);
#11991=EDGE_CURVE('',#9067,#9068,#5784,.T.);
#11992=EDGE_CURVE('',#9068,#9066,#1495,.T.);
#11993=EDGE_CURVE('',#9065,#9067,#1496,.T.);
#11994=EDGE_CURVE('',#9069,#9070,#5785,.T.);
#11995=EDGE_CURVE('',#9070,#9068,#1497,.T.);
#11996=EDGE_CURVE('',#9067,#9069,#1498,.T.);
#11997=EDGE_CURVE('',#9071,#9072,#5786,.T.);
#11998=EDGE_CURVE('',#9072,#9070,#1499,.T.);
#11999=EDGE_CURVE('',#9069,#9071,#1500,.T.);
#12000=EDGE_CURVE('',#9073,#9074,#5787,.T.);
#12001=EDGE_CURVE('',#9074,#9072,#1501,.T.);
#12002=EDGE_CURVE('',#9071,#9073,#1502,.T.);
#12003=EDGE_CURVE('',#9075,#9076,#5788,.T.);
#12004=EDGE_CURVE('',#9076,#9074,#1503,.T.);
#12005=EDGE_CURVE('',#9073,#9075,#1504,.T.);
#12006=EDGE_CURVE('',#9077,#9078,#5789,.T.);
#12007=EDGE_CURVE('',#9078,#9076,#1505,.T.);
#12008=EDGE_CURVE('',#9075,#9077,#1506,.T.);
#12009=EDGE_CURVE('',#9079,#9080,#5790,.T.);
#12010=EDGE_CURVE('',#9080,#9078,#1507,.T.);
#12011=EDGE_CURVE('',#9077,#9079,#1508,.T.);
#12012=EDGE_CURVE('',#9081,#9082,#5791,.T.);
#12013=EDGE_CURVE('',#9082,#9080,#1509,.T.);
#12014=EDGE_CURVE('',#9079,#9081,#1510,.T.);
#12015=EDGE_CURVE('',#9083,#9084,#5792,.T.);
#12016=EDGE_CURVE('',#9084,#9082,#1511,.T.);
#12017=EDGE_CURVE('',#9081,#9083,#1512,.T.);
#12018=EDGE_CURVE('',#9085,#9086,#5793,.T.);
#12019=EDGE_CURVE('',#9086,#9084,#1513,.T.);
#12020=EDGE_CURVE('',#9083,#9085,#1514,.T.);
#12021=EDGE_CURVE('',#9087,#9088,#5794,.T.);
#12022=EDGE_CURVE('',#9088,#9086,#1515,.T.);
#12023=EDGE_CURVE('',#9085,#9087,#1516,.T.);
#12024=EDGE_CURVE('',#9089,#9090,#5795,.T.);
#12025=EDGE_CURVE('',#9089,#9091,#1517,.T.);
#12026=EDGE_CURVE('',#9092,#9091,#7575,.T.);
#12027=EDGE_CURVE('',#9092,#9090,#1518,.T.);
#12028=EDGE_CURVE('',#9093,#9094,#5796,.T.);
#12029=EDGE_CURVE('',#9094,#9095,#1519,.T.);
#12030=EDGE_CURVE('',#9096,#9095,#7576,.F.);
#12031=EDGE_CURVE('',#9096,#9093,#1520,.T.);
#12032=EDGE_CURVE('',#9097,#9098,#5797,.T.);
#12033=EDGE_CURVE('',#9098,#9094,#1521,.T.);
#12034=EDGE_CURVE('',#9093,#9097,#1522,.T.);
#12035=EDGE_CURVE('',#9099,#9100,#5798,.T.);
#12036=EDGE_CURVE('',#9100,#9098,#1523,.T.);
#12037=EDGE_CURVE('',#9097,#9099,#1524,.T.);
#12038=EDGE_CURVE('',#9101,#9102,#5799,.T.);
#12039=EDGE_CURVE('',#9102,#9100,#1525,.T.);
#12040=EDGE_CURVE('',#9099,#9101,#1526,.T.);
#12041=EDGE_CURVE('',#9103,#9104,#5800,.T.);
#12042=EDGE_CURVE('',#9104,#9102,#1527,.T.);
#12043=EDGE_CURVE('',#9101,#9103,#1528,.T.);
#12044=EDGE_CURVE('',#9105,#9106,#5801,.T.);
#12045=EDGE_CURVE('',#9106,#9104,#1529,.T.);
#12046=EDGE_CURVE('',#9103,#9105,#1530,.T.);
#12047=EDGE_CURVE('',#9107,#9108,#5802,.T.);
#12048=EDGE_CURVE('',#9108,#9106,#1531,.T.);
#12049=EDGE_CURVE('',#9105,#9107,#1532,.T.);
#12050=EDGE_CURVE('',#9109,#9110,#5803,.T.);
#12051=EDGE_CURVE('',#9110,#9108,#1533,.T.);
#12052=EDGE_CURVE('',#9107,#9109,#1534,.T.);
#12053=EDGE_CURVE('',#9111,#9112,#5804,.T.);
#12054=EDGE_CURVE('',#9112,#9110,#1535,.T.);
#12055=EDGE_CURVE('',#9109,#9111,#1536,.T.);
#12056=EDGE_CURVE('',#9113,#9114,#5805,.T.);
#12057=EDGE_CURVE('',#9114,#9112,#1537,.T.);
#12058=EDGE_CURVE('',#9111,#9113,#1538,.T.);
#12059=EDGE_CURVE('',#9115,#9116,#5806,.T.);
#12060=EDGE_CURVE('',#9116,#9114,#1539,.T.);
#12061=EDGE_CURVE('',#9113,#9115,#1540,.T.);
#12062=EDGE_CURVE('',#9117,#9118,#5807,.T.);
#12063=EDGE_CURVE('',#9118,#9116,#1541,.T.);
#12064=EDGE_CURVE('',#9115,#9117,#1542,.T.);
#12065=EDGE_CURVE('',#9119,#9120,#5808,.T.);
#12066=EDGE_CURVE('',#9120,#9118,#1543,.T.);
#12067=EDGE_CURVE('',#9117,#9119,#1544,.T.);
#12068=EDGE_CURVE('',#9121,#9122,#5809,.T.);
#12069=EDGE_CURVE('',#9122,#9120,#1545,.T.);
#12070=EDGE_CURVE('',#9119,#9121,#1546,.T.);
#12071=EDGE_CURVE('',#9123,#9124,#5810,.T.);
#12072=EDGE_CURVE('',#9124,#9122,#1547,.T.);
#12073=EDGE_CURVE('',#9121,#9123,#1548,.T.);
#12074=EDGE_CURVE('',#9125,#9126,#5811,.T.);
#12075=EDGE_CURVE('',#9126,#9124,#1549,.T.);
#12076=EDGE_CURVE('',#9123,#9125,#1550,.T.);
#12077=EDGE_CURVE('',#9127,#9128,#5812,.T.);
#12078=EDGE_CURVE('',#9128,#9126,#1551,.T.);
#12079=EDGE_CURVE('',#9125,#9127,#1552,.T.);
#12080=EDGE_CURVE('',#9129,#9130,#5813,.T.);
#12081=EDGE_CURVE('',#9130,#9128,#1553,.T.);
#12082=EDGE_CURVE('',#9127,#9129,#1554,.T.);
#12083=EDGE_CURVE('',#9131,#9132,#5814,.T.);
#12084=EDGE_CURVE('',#9132,#9130,#1555,.T.);
#12085=EDGE_CURVE('',#9129,#9131,#1556,.T.);
#12086=EDGE_CURVE('',#9133,#9134,#5815,.T.);
#12087=EDGE_CURVE('',#9133,#9135,#1557,.T.);
#12088=EDGE_CURVE('',#9136,#9135,#7577,.T.);
#12089=EDGE_CURVE('',#9136,#9134,#1558,.T.);
#12090=EDGE_CURVE('',#9137,#9138,#5816,.T.);
#12091=EDGE_CURVE('',#9138,#9139,#1559,.T.);
#12092=EDGE_CURVE('',#9140,#9139,#7578,.F.);
#12093=EDGE_CURVE('',#9140,#9137,#1560,.T.);
#12094=EDGE_CURVE('',#9141,#9142,#5817,.T.);
#12095=EDGE_CURVE('',#9142,#9138,#1561,.T.);
#12096=EDGE_CURVE('',#9137,#9141,#1562,.T.);
#12097=EDGE_CURVE('',#9143,#9144,#5818,.T.);
#12098=EDGE_CURVE('',#9144,#9142,#1563,.T.);
#12099=EDGE_CURVE('',#9141,#9143,#1564,.T.);
#12100=EDGE_CURVE('',#9145,#9146,#5819,.T.);
#12101=EDGE_CURVE('',#9146,#9144,#1565,.T.);
#12102=EDGE_CURVE('',#9143,#9145,#1566,.T.);
#12103=EDGE_CURVE('',#9147,#9148,#5820,.T.);
#12104=EDGE_CURVE('',#9148,#9146,#1567,.T.);
#12105=EDGE_CURVE('',#9145,#9147,#1568,.T.);
#12106=EDGE_CURVE('',#9149,#9150,#5821,.T.);
#12107=EDGE_CURVE('',#9150,#9148,#1569,.T.);
#12108=EDGE_CURVE('',#9147,#9149,#1570,.T.);
#12109=EDGE_CURVE('',#9151,#9152,#5822,.T.);
#12110=EDGE_CURVE('',#9152,#9150,#1571,.T.);
#12111=EDGE_CURVE('',#9149,#9151,#1572,.T.);
#12112=EDGE_CURVE('',#9153,#9154,#5823,.T.);
#12113=EDGE_CURVE('',#9154,#9152,#1573,.T.);
#12114=EDGE_CURVE('',#9151,#9153,#1574,.T.);
#12115=EDGE_CURVE('',#9155,#9156,#5824,.T.);
#12116=EDGE_CURVE('',#9156,#9154,#1575,.T.);
#12117=EDGE_CURVE('',#9153,#9155,#1576,.T.);
#12118=EDGE_CURVE('',#9157,#9158,#5825,.T.);
#12119=EDGE_CURVE('',#9158,#9156,#1577,.T.);
#12120=EDGE_CURVE('',#9155,#9157,#1578,.T.);
#12121=EDGE_CURVE('',#9159,#9160,#5826,.T.);
#12122=EDGE_CURVE('',#9160,#9158,#1579,.T.);
#12123=EDGE_CURVE('',#9157,#9159,#1580,.T.);
#12124=EDGE_CURVE('',#9161,#9162,#5827,.T.);
#12125=EDGE_CURVE('',#9162,#9160,#1581,.T.);
#12126=EDGE_CURVE('',#9159,#9161,#1582,.T.);
#12127=EDGE_CURVE('',#9163,#9164,#5828,.T.);
#12128=EDGE_CURVE('',#9164,#9162,#1583,.T.);
#12129=EDGE_CURVE('',#9161,#9163,#1584,.T.);
#12130=EDGE_CURVE('',#9165,#9166,#5829,.T.);
#12131=EDGE_CURVE('',#9166,#9164,#1585,.T.);
#12132=EDGE_CURVE('',#9163,#9165,#1586,.T.);
#12133=EDGE_CURVE('',#9167,#9168,#5830,.T.);
#12134=EDGE_CURVE('',#9168,#9166,#1587,.T.);
#12135=EDGE_CURVE('',#9165,#9167,#1588,.T.);
#12136=EDGE_CURVE('',#9169,#9170,#5831,.T.);
#12137=EDGE_CURVE('',#9170,#9168,#1589,.T.);
#12138=EDGE_CURVE('',#9167,#9169,#1590,.T.);
#12139=EDGE_CURVE('',#9171,#9172,#5832,.T.);
#12140=EDGE_CURVE('',#9172,#9170,#1591,.T.);
#12141=EDGE_CURVE('',#9169,#9171,#1592,.T.);
#12142=EDGE_CURVE('',#9173,#9174,#5833,.T.);
#12143=EDGE_CURVE('',#9174,#9172,#1593,.T.);
#12144=EDGE_CURVE('',#9171,#9173,#1594,.T.);
#12145=EDGE_CURVE('',#9175,#9176,#5834,.T.);
#12146=EDGE_CURVE('',#9176,#9174,#1595,.T.);
#12147=EDGE_CURVE('',#9173,#9175,#1596,.T.);
#12148=EDGE_CURVE('',#9177,#9178,#5835,.T.);
#12149=EDGE_CURVE('',#9177,#9179,#1597,.T.);
#12150=EDGE_CURVE('',#9180,#9179,#7579,.T.);
#12151=EDGE_CURVE('',#9180,#9178,#1598,.T.);
#12152=EDGE_CURVE('',#9181,#9182,#5836,.T.);
#12153=EDGE_CURVE('',#9182,#9183,#1599,.T.);
#12154=EDGE_CURVE('',#9184,#9183,#7580,.F.);
#12155=EDGE_CURVE('',#9184,#9181,#1600,.T.);
#12156=EDGE_CURVE('',#9185,#9186,#5837,.T.);
#12157=EDGE_CURVE('',#9186,#9182,#1601,.T.);
#12158=EDGE_CURVE('',#9181,#9185,#1602,.T.);
#12159=EDGE_CURVE('',#9187,#9188,#5838,.T.);
#12160=EDGE_CURVE('',#9188,#9186,#1603,.T.);
#12161=EDGE_CURVE('',#9185,#9187,#1604,.T.);
#12162=EDGE_CURVE('',#9189,#9190,#5839,.T.);
#12163=EDGE_CURVE('',#9190,#9188,#1605,.T.);
#12164=EDGE_CURVE('',#9187,#9189,#1606,.T.);
#12165=EDGE_CURVE('',#9191,#9192,#5840,.T.);
#12166=EDGE_CURVE('',#9192,#9190,#1607,.T.);
#12167=EDGE_CURVE('',#9189,#9191,#1608,.T.);
#12168=EDGE_CURVE('',#9193,#9194,#5841,.T.);
#12169=EDGE_CURVE('',#9194,#9192,#1609,.T.);
#12170=EDGE_CURVE('',#9191,#9193,#1610,.T.);
#12171=EDGE_CURVE('',#9195,#9196,#5842,.T.);
#12172=EDGE_CURVE('',#9196,#9194,#1611,.T.);
#12173=EDGE_CURVE('',#9193,#9195,#1612,.T.);
#12174=EDGE_CURVE('',#9197,#9198,#5843,.T.);
#12175=EDGE_CURVE('',#9198,#9196,#1613,.T.);
#12176=EDGE_CURVE('',#9195,#9197,#1614,.T.);
#12177=EDGE_CURVE('',#9199,#9200,#5844,.T.);
#12178=EDGE_CURVE('',#9200,#9198,#1615,.T.);
#12179=EDGE_CURVE('',#9197,#9199,#1616,.T.);
#12180=EDGE_CURVE('',#9201,#9202,#5845,.T.);
#12181=EDGE_CURVE('',#9202,#9200,#1617,.T.);
#12182=EDGE_CURVE('',#9199,#9201,#1618,.T.);
#12183=EDGE_CURVE('',#9203,#9204,#5846,.T.);
#12184=EDGE_CURVE('',#9204,#9202,#1619,.T.);
#12185=EDGE_CURVE('',#9201,#9203,#1620,.T.);
#12186=EDGE_CURVE('',#9205,#9206,#5847,.T.);
#12187=EDGE_CURVE('',#9206,#9204,#1621,.T.);
#12188=EDGE_CURVE('',#9203,#9205,#1622,.T.);
#12189=EDGE_CURVE('',#9207,#9208,#5848,.T.);
#12190=EDGE_CURVE('',#9208,#9206,#1623,.T.);
#12191=EDGE_CURVE('',#9205,#9207,#1624,.T.);
#12192=EDGE_CURVE('',#9209,#9210,#5849,.T.);
#12193=EDGE_CURVE('',#9210,#9208,#1625,.T.);
#12194=EDGE_CURVE('',#9207,#9209,#1626,.T.);
#12195=EDGE_CURVE('',#9211,#9212,#5850,.T.);
#12196=EDGE_CURVE('',#9212,#9210,#1627,.T.);
#12197=EDGE_CURVE('',#9209,#9211,#1628,.T.);
#12198=EDGE_CURVE('',#9213,#9214,#5851,.T.);
#12199=EDGE_CURVE('',#9214,#9212,#1629,.T.);
#12200=EDGE_CURVE('',#9211,#9213,#1630,.T.);
#12201=EDGE_CURVE('',#9215,#9216,#5852,.T.);
#12202=EDGE_CURVE('',#9216,#9214,#1631,.T.);
#12203=EDGE_CURVE('',#9213,#9215,#1632,.T.);
#12204=EDGE_CURVE('',#9217,#9218,#5853,.T.);
#12205=EDGE_CURVE('',#9218,#9216,#1633,.T.);
#12206=EDGE_CURVE('',#9215,#9217,#1634,.T.);
#12207=EDGE_CURVE('',#9219,#9220,#5854,.T.);
#12208=EDGE_CURVE('',#9220,#9218,#1635,.T.);
#12209=EDGE_CURVE('',#9217,#9219,#1636,.T.);
#12210=EDGE_CURVE('',#9221,#9222,#5855,.T.);
#12211=EDGE_CURVE('',#9221,#9223,#1637,.T.);
#12212=EDGE_CURVE('',#9224,#9223,#7581,.T.);
#12213=EDGE_CURVE('',#9224,#9222,#1638,.T.);
#12214=EDGE_CURVE('',#9225,#9226,#5856,.T.);
#12215=EDGE_CURVE('',#9226,#9227,#1639,.T.);
#12216=EDGE_CURVE('',#9228,#9227,#7582,.F.);
#12217=EDGE_CURVE('',#9228,#9225,#1640,.T.);
#12218=EDGE_CURVE('',#9229,#9230,#5857,.T.);
#12219=EDGE_CURVE('',#9230,#9226,#1641,.T.);
#12220=EDGE_CURVE('',#9225,#9229,#1642,.T.);
#12221=EDGE_CURVE('',#9231,#9232,#5858,.T.);
#12222=EDGE_CURVE('',#9232,#9230,#1643,.T.);
#12223=EDGE_CURVE('',#9229,#9231,#1644,.T.);
#12224=EDGE_CURVE('',#9233,#9234,#5859,.T.);
#12225=EDGE_CURVE('',#9234,#9232,#1645,.T.);
#12226=EDGE_CURVE('',#9231,#9233,#1646,.T.);
#12227=EDGE_CURVE('',#9235,#9236,#5860,.T.);
#12228=EDGE_CURVE('',#9236,#9234,#1647,.T.);
#12229=EDGE_CURVE('',#9233,#9235,#1648,.T.);
#12230=EDGE_CURVE('',#9237,#9238,#5861,.T.);
#12231=EDGE_CURVE('',#9238,#9236,#1649,.T.);
#12232=EDGE_CURVE('',#9235,#9237,#1650,.T.);
#12233=EDGE_CURVE('',#9239,#9240,#5862,.T.);
#12234=EDGE_CURVE('',#9240,#9238,#1651,.T.);
#12235=EDGE_CURVE('',#9237,#9239,#1652,.T.);
#12236=EDGE_CURVE('',#9241,#9242,#5863,.T.);
#12237=EDGE_CURVE('',#9242,#9240,#1653,.T.);
#12238=EDGE_CURVE('',#9239,#9241,#1654,.T.);
#12239=EDGE_CURVE('',#9243,#9244,#5864,.T.);
#12240=EDGE_CURVE('',#9244,#9242,#1655,.T.);
#12241=EDGE_CURVE('',#9241,#9243,#1656,.T.);
#12242=EDGE_CURVE('',#9245,#9246,#5865,.T.);
#12243=EDGE_CURVE('',#9246,#9244,#1657,.T.);
#12244=EDGE_CURVE('',#9243,#9245,#1658,.T.);
#12245=EDGE_CURVE('',#9247,#9248,#5866,.T.);
#12246=EDGE_CURVE('',#9248,#9246,#1659,.T.);
#12247=EDGE_CURVE('',#9245,#9247,#1660,.T.);
#12248=EDGE_CURVE('',#9249,#9250,#5867,.T.);
#12249=EDGE_CURVE('',#9250,#9248,#1661,.T.);
#12250=EDGE_CURVE('',#9247,#9249,#1662,.T.);
#12251=EDGE_CURVE('',#9251,#9252,#5868,.T.);
#12252=EDGE_CURVE('',#9252,#9250,#1663,.T.);
#12253=EDGE_CURVE('',#9249,#9251,#1664,.T.);
#12254=EDGE_CURVE('',#9253,#9254,#5869,.T.);
#12255=EDGE_CURVE('',#9254,#9252,#1665,.T.);
#12256=EDGE_CURVE('',#9251,#9253,#1666,.T.);
#12257=EDGE_CURVE('',#9255,#9256,#5870,.T.);
#12258=EDGE_CURVE('',#9256,#9254,#1667,.T.);
#12259=EDGE_CURVE('',#9253,#9255,#1668,.T.);
#12260=EDGE_CURVE('',#9257,#9258,#5871,.T.);
#12261=EDGE_CURVE('',#9258,#9256,#1669,.T.);
#12262=EDGE_CURVE('',#9255,#9257,#1670,.T.);
#12263=EDGE_CURVE('',#9259,#9260,#5872,.T.);
#12264=EDGE_CURVE('',#9260,#9258,#1671,.T.);
#12265=EDGE_CURVE('',#9257,#9259,#1672,.T.);
#12266=EDGE_CURVE('',#9261,#9262,#5873,.T.);
#12267=EDGE_CURVE('',#9262,#9260,#1673,.T.);
#12268=EDGE_CURVE('',#9259,#9261,#1674,.T.);
#12269=EDGE_CURVE('',#9263,#9264,#5874,.T.);
#12270=EDGE_CURVE('',#9264,#9262,#1675,.T.);
#12271=EDGE_CURVE('',#9261,#9263,#1676,.T.);
#12272=EDGE_CURVE('',#9265,#9266,#5875,.T.);
#12273=EDGE_CURVE('',#9265,#9267,#1677,.T.);
#12274=EDGE_CURVE('',#9268,#9267,#7583,.T.);
#12275=EDGE_CURVE('',#9268,#9266,#1678,.T.);
#12276=EDGE_CURVE('',#9269,#9270,#5876,.T.);
#12277=EDGE_CURVE('',#9270,#9271,#1679,.T.);
#12278=EDGE_CURVE('',#9272,#9271,#7584,.F.);
#12279=EDGE_CURVE('',#9272,#9269,#1680,.T.);
#12280=EDGE_CURVE('',#9273,#9274,#5877,.T.);
#12281=EDGE_CURVE('',#9274,#9270,#1681,.T.);
#12282=EDGE_CURVE('',#9269,#9273,#1682,.T.);
#12283=EDGE_CURVE('',#9275,#9276,#5878,.T.);
#12284=EDGE_CURVE('',#9276,#9274,#1683,.T.);
#12285=EDGE_CURVE('',#9273,#9275,#1684,.T.);
#12286=EDGE_CURVE('',#9277,#9278,#5879,.T.);
#12287=EDGE_CURVE('',#9278,#9276,#1685,.T.);
#12288=EDGE_CURVE('',#9275,#9277,#1686,.T.);
#12289=EDGE_CURVE('',#9279,#9280,#5880,.T.);
#12290=EDGE_CURVE('',#9280,#9278,#1687,.T.);
#12291=EDGE_CURVE('',#9277,#9279,#1688,.T.);
#12292=EDGE_CURVE('',#9281,#9282,#5881,.T.);
#12293=EDGE_CURVE('',#9282,#9280,#1689,.T.);
#12294=EDGE_CURVE('',#9279,#9281,#1690,.T.);
#12295=EDGE_CURVE('',#9283,#9284,#5882,.T.);
#12296=EDGE_CURVE('',#9284,#9282,#1691,.T.);
#12297=EDGE_CURVE('',#9281,#9283,#1692,.T.);
#12298=EDGE_CURVE('',#9285,#9286,#5883,.T.);
#12299=EDGE_CURVE('',#9286,#9284,#1693,.T.);
#12300=EDGE_CURVE('',#9283,#9285,#1694,.T.);
#12301=EDGE_CURVE('',#9287,#9288,#5884,.T.);
#12302=EDGE_CURVE('',#9288,#9286,#1695,.T.);
#12303=EDGE_CURVE('',#9285,#9287,#1696,.T.);
#12304=EDGE_CURVE('',#9289,#9290,#5885,.T.);
#12305=EDGE_CURVE('',#9290,#9288,#1697,.T.);
#12306=EDGE_CURVE('',#9287,#9289,#1698,.T.);
#12307=EDGE_CURVE('',#9291,#9292,#5886,.T.);
#12308=EDGE_CURVE('',#9292,#9290,#1699,.T.);
#12309=EDGE_CURVE('',#9289,#9291,#1700,.T.);
#12310=EDGE_CURVE('',#9293,#9294,#5887,.T.);
#12311=EDGE_CURVE('',#9294,#9292,#1701,.T.);
#12312=EDGE_CURVE('',#9291,#9293,#1702,.T.);
#12313=EDGE_CURVE('',#9295,#9296,#5888,.T.);
#12314=EDGE_CURVE('',#9296,#9294,#1703,.T.);
#12315=EDGE_CURVE('',#9293,#9295,#1704,.T.);
#12316=EDGE_CURVE('',#9297,#9298,#5889,.T.);
#12317=EDGE_CURVE('',#9298,#9296,#1705,.T.);
#12318=EDGE_CURVE('',#9295,#9297,#1706,.T.);
#12319=EDGE_CURVE('',#9299,#9300,#5890,.T.);
#12320=EDGE_CURVE('',#9300,#9298,#1707,.T.);
#12321=EDGE_CURVE('',#9297,#9299,#1708,.T.);
#12322=EDGE_CURVE('',#9301,#9302,#5891,.T.);
#12323=EDGE_CURVE('',#9302,#9300,#1709,.T.);
#12324=EDGE_CURVE('',#9299,#9301,#1710,.T.);
#12325=EDGE_CURVE('',#9303,#9304,#5892,.T.);
#12326=EDGE_CURVE('',#9304,#9302,#1711,.T.);
#12327=EDGE_CURVE('',#9301,#9303,#1712,.T.);
#12328=EDGE_CURVE('',#9305,#9306,#5893,.T.);
#12329=EDGE_CURVE('',#9306,#9304,#1713,.T.);
#12330=EDGE_CURVE('',#9303,#9305,#1714,.T.);
#12331=EDGE_CURVE('',#9307,#9308,#5894,.T.);
#12332=EDGE_CURVE('',#9308,#9306,#1715,.T.);
#12333=EDGE_CURVE('',#9305,#9307,#1716,.T.);
#12334=EDGE_CURVE('',#9309,#9310,#5895,.T.);
#12335=EDGE_CURVE('',#9309,#9311,#1717,.T.);
#12336=EDGE_CURVE('',#9312,#9311,#7585,.T.);
#12337=EDGE_CURVE('',#9312,#9310,#1718,.T.);
#12338=EDGE_CURVE('',#9313,#9314,#5896,.T.);
#12339=EDGE_CURVE('',#9314,#9315,#1719,.T.);
#12340=EDGE_CURVE('',#9316,#9315,#7586,.T.);
#12341=EDGE_CURVE('',#9313,#9316,#1720,.T.);
#12342=EDGE_CURVE('',#9317,#9318,#5897,.T.);
#12343=EDGE_CURVE('',#9318,#9314,#1721,.T.);
#12344=EDGE_CURVE('',#9317,#9313,#1722,.T.);
#12345=EDGE_CURVE('',#9319,#9320,#5898,.T.);
#12346=EDGE_CURVE('',#9320,#9318,#1723,.T.);
#12347=EDGE_CURVE('',#9319,#9317,#1724,.T.);
#12348=EDGE_CURVE('',#9321,#9322,#5899,.T.);
#12349=EDGE_CURVE('',#9322,#9320,#1725,.T.);
#12350=EDGE_CURVE('',#9321,#9319,#1726,.T.);
#12351=EDGE_CURVE('',#9323,#9324,#5900,.T.);
#12352=EDGE_CURVE('',#9324,#9322,#1727,.T.);
#12353=EDGE_CURVE('',#9323,#9321,#1728,.T.);
#12354=EDGE_CURVE('',#9325,#9326,#5901,.T.);
#12355=EDGE_CURVE('',#9326,#9324,#1729,.T.);
#12356=EDGE_CURVE('',#9325,#9323,#1730,.T.);
#12357=EDGE_CURVE('',#9327,#9328,#5902,.T.);
#12358=EDGE_CURVE('',#9328,#9326,#1731,.T.);
#12359=EDGE_CURVE('',#9327,#9325,#1732,.T.);
#12360=EDGE_CURVE('',#9329,#9330,#5903,.T.);
#12361=EDGE_CURVE('',#9330,#9328,#1733,.T.);
#12362=EDGE_CURVE('',#9329,#9327,#1734,.T.);
#12363=EDGE_CURVE('',#9331,#9332,#5904,.T.);
#12364=EDGE_CURVE('',#9332,#9330,#1735,.T.);
#12365=EDGE_CURVE('',#9331,#9329,#1736,.T.);
#12366=EDGE_CURVE('',#9333,#9334,#5905,.T.);
#12367=EDGE_CURVE('',#9334,#9332,#1737,.T.);
#12368=EDGE_CURVE('',#9333,#9331,#1738,.T.);
#12369=EDGE_CURVE('',#9335,#9336,#5906,.T.);
#12370=EDGE_CURVE('',#9336,#9334,#1739,.T.);
#12371=EDGE_CURVE('',#9335,#9333,#1740,.T.);
#12372=EDGE_CURVE('',#9337,#9338,#5907,.T.);
#12373=EDGE_CURVE('',#9338,#9336,#1741,.T.);
#12374=EDGE_CURVE('',#9337,#9335,#1742,.T.);
#12375=EDGE_CURVE('',#9339,#9340,#5908,.T.);
#12376=EDGE_CURVE('',#9340,#9338,#1743,.T.);
#12377=EDGE_CURVE('',#9339,#9337,#1744,.T.);
#12378=EDGE_CURVE('',#9341,#9342,#5909,.T.);
#12379=EDGE_CURVE('',#9342,#9340,#1745,.T.);
#12380=EDGE_CURVE('',#9341,#9339,#1746,.T.);
#12381=EDGE_CURVE('',#9343,#9344,#5910,.T.);
#12382=EDGE_CURVE('',#9344,#9342,#1747,.T.);
#12383=EDGE_CURVE('',#9343,#9341,#1748,.T.);
#12384=EDGE_CURVE('',#9345,#9346,#5911,.T.);
#12385=EDGE_CURVE('',#9346,#9344,#1749,.T.);
#12386=EDGE_CURVE('',#9345,#9343,#1750,.T.);
#12387=EDGE_CURVE('',#9347,#9348,#5912,.T.);
#12388=EDGE_CURVE('',#9348,#9346,#1751,.T.);
#12389=EDGE_CURVE('',#9347,#9345,#1752,.T.);
#12390=EDGE_CURVE('',#9349,#9350,#5913,.T.);
#12391=EDGE_CURVE('',#9350,#9348,#1753,.T.);
#12392=EDGE_CURVE('',#9349,#9347,#1754,.T.);
#12393=EDGE_CURVE('',#9351,#9352,#5914,.T.);
#12394=EDGE_CURVE('',#9352,#9350,#1755,.T.);
#12395=EDGE_CURVE('',#9351,#9349,#1756,.T.);
#12396=EDGE_CURVE('',#9353,#9354,#5915,.T.);
#12397=EDGE_CURVE('',#9355,#9353,#1757,.T.);
#12398=EDGE_CURVE('',#9356,#9355,#7587,.T.);
#12399=EDGE_CURVE('',#9356,#9354,#1758,.T.);
#12400=EDGE_CURVE('',#9357,#9358,#5916,.T.);
#12401=EDGE_CURVE('',#9358,#9359,#1759,.T.);
#12402=EDGE_CURVE('',#9360,#9359,#7588,.T.);
#12403=EDGE_CURVE('',#9357,#9360,#1760,.T.);
#12404=EDGE_CURVE('',#9361,#9362,#5917,.T.);
#12405=EDGE_CURVE('',#9362,#9358,#1761,.T.);
#12406=EDGE_CURVE('',#9361,#9357,#1762,.T.);
#12407=EDGE_CURVE('',#9363,#9364,#5918,.T.);
#12408=EDGE_CURVE('',#9364,#9362,#1763,.T.);
#12409=EDGE_CURVE('',#9363,#9361,#1764,.T.);
#12410=EDGE_CURVE('',#9365,#9366,#5919,.T.);
#12411=EDGE_CURVE('',#9366,#9364,#1765,.T.);
#12412=EDGE_CURVE('',#9365,#9363,#1766,.T.);
#12413=EDGE_CURVE('',#9367,#9368,#5920,.T.);
#12414=EDGE_CURVE('',#9368,#9366,#1767,.T.);
#12415=EDGE_CURVE('',#9367,#9365,#1768,.T.);
#12416=EDGE_CURVE('',#9369,#9370,#5921,.T.);
#12417=EDGE_CURVE('',#9370,#9368,#1769,.T.);
#12418=EDGE_CURVE('',#9369,#9367,#1770,.T.);
#12419=EDGE_CURVE('',#9371,#9372,#5922,.T.);
#12420=EDGE_CURVE('',#9372,#9370,#1771,.T.);
#12421=EDGE_CURVE('',#9371,#9369,#1772,.T.);
#12422=EDGE_CURVE('',#9373,#9374,#5923,.T.);
#12423=EDGE_CURVE('',#9374,#9372,#1773,.T.);
#12424=EDGE_CURVE('',#9373,#9371,#1774,.T.);
#12425=EDGE_CURVE('',#9375,#9376,#5924,.T.);
#12426=EDGE_CURVE('',#9376,#9374,#1775,.T.);
#12427=EDGE_CURVE('',#9375,#9373,#1776,.T.);
#12428=EDGE_CURVE('',#9377,#9378,#5925,.T.);
#12429=EDGE_CURVE('',#9378,#9376,#1777,.T.);
#12430=EDGE_CURVE('',#9377,#9375,#1778,.T.);
#12431=EDGE_CURVE('',#9379,#9380,#5926,.T.);
#12432=EDGE_CURVE('',#9380,#9378,#1779,.T.);
#12433=EDGE_CURVE('',#9379,#9377,#1780,.T.);
#12434=EDGE_CURVE('',#9381,#9382,#5927,.T.);
#12435=EDGE_CURVE('',#9382,#9380,#1781,.T.);
#12436=EDGE_CURVE('',#9381,#9379,#1782,.T.);
#12437=EDGE_CURVE('',#9383,#9384,#5928,.T.);
#12438=EDGE_CURVE('',#9384,#9382,#1783,.T.);
#12439=EDGE_CURVE('',#9383,#9381,#1784,.T.);
#12440=EDGE_CURVE('',#9385,#9386,#5929,.T.);
#12441=EDGE_CURVE('',#9386,#9384,#1785,.T.);
#12442=EDGE_CURVE('',#9385,#9383,#1786,.T.);
#12443=EDGE_CURVE('',#9387,#9388,#5930,.T.);
#12444=EDGE_CURVE('',#9388,#9386,#1787,.T.);
#12445=EDGE_CURVE('',#9387,#9385,#1788,.T.);
#12446=EDGE_CURVE('',#9389,#9390,#5931,.T.);
#12447=EDGE_CURVE('',#9390,#9388,#1789,.T.);
#12448=EDGE_CURVE('',#9389,#9387,#1790,.T.);
#12449=EDGE_CURVE('',#9391,#9392,#5932,.T.);
#12450=EDGE_CURVE('',#9392,#9390,#1791,.T.);
#12451=EDGE_CURVE('',#9391,#9389,#1792,.T.);
#12452=EDGE_CURVE('',#9393,#9394,#5933,.T.);
#12453=EDGE_CURVE('',#9394,#9392,#1793,.T.);
#12454=EDGE_CURVE('',#9393,#9391,#1794,.T.);
#12455=EDGE_CURVE('',#9395,#9396,#5934,.T.);
#12456=EDGE_CURVE('',#9396,#9394,#1795,.T.);
#12457=EDGE_CURVE('',#9395,#9393,#1796,.T.);
#12458=EDGE_CURVE('',#9397,#9398,#5935,.T.);
#12459=EDGE_CURVE('',#9399,#9397,#1797,.T.);
#12460=EDGE_CURVE('',#9400,#9399,#7589,.T.);
#12461=EDGE_CURVE('',#9400,#9398,#1798,.T.);
#12462=EDGE_CURVE('',#9401,#9402,#5936,.T.);
#12463=EDGE_CURVE('',#9402,#9403,#1799,.T.);
#12464=EDGE_CURVE('',#9404,#9403,#7590,.T.);
#12465=EDGE_CURVE('',#9401,#9404,#1800,.T.);
#12466=EDGE_CURVE('',#9405,#9406,#5937,.T.);
#12467=EDGE_CURVE('',#9406,#9402,#1801,.T.);
#12468=EDGE_CURVE('',#9405,#9401,#1802,.T.);
#12469=EDGE_CURVE('',#9407,#9408,#5938,.T.);
#12470=EDGE_CURVE('',#9408,#9406,#1803,.T.);
#12471=EDGE_CURVE('',#9407,#9405,#1804,.T.);
#12472=EDGE_CURVE('',#9409,#9410,#5939,.T.);
#12473=EDGE_CURVE('',#9410,#9408,#1805,.T.);
#12474=EDGE_CURVE('',#9409,#9407,#1806,.T.);
#12475=EDGE_CURVE('',#9411,#9412,#5940,.T.);
#12476=EDGE_CURVE('',#9412,#9410,#1807,.T.);
#12477=EDGE_CURVE('',#9411,#9409,#1808,.T.);
#12478=EDGE_CURVE('',#9413,#9414,#5941,.T.);
#12479=EDGE_CURVE('',#9414,#9412,#1809,.T.);
#12480=EDGE_CURVE('',#9413,#9411,#1810,.T.);
#12481=EDGE_CURVE('',#9415,#9416,#5942,.T.);
#12482=EDGE_CURVE('',#9416,#9414,#1811,.T.);
#12483=EDGE_CURVE('',#9415,#9413,#1812,.T.);
#12484=EDGE_CURVE('',#9417,#9418,#5943,.T.);
#12485=EDGE_CURVE('',#9418,#9416,#1813,.T.);
#12486=EDGE_CURVE('',#9417,#9415,#1814,.T.);
#12487=EDGE_CURVE('',#9419,#9420,#5944,.T.);
#12488=EDGE_CURVE('',#9420,#9418,#1815,.T.);
#12489=EDGE_CURVE('',#9419,#9417,#1816,.T.);
#12490=EDGE_CURVE('',#9421,#9422,#5945,.T.);
#12491=EDGE_CURVE('',#9422,#9420,#1817,.T.);
#12492=EDGE_CURVE('',#9421,#9419,#1818,.T.);
#12493=EDGE_CURVE('',#9423,#9424,#5946,.T.);
#12494=EDGE_CURVE('',#9424,#9422,#1819,.T.);
#12495=EDGE_CURVE('',#9423,#9421,#1820,.T.);
#12496=EDGE_CURVE('',#9425,#9426,#5947,.T.);
#12497=EDGE_CURVE('',#9426,#9424,#1821,.T.);
#12498=EDGE_CURVE('',#9425,#9423,#1822,.T.);
#12499=EDGE_CURVE('',#9427,#9428,#5948,.T.);
#12500=EDGE_CURVE('',#9428,#9426,#1823,.T.);
#12501=EDGE_CURVE('',#9427,#9425,#1824,.T.);
#12502=EDGE_CURVE('',#9429,#9430,#5949,.T.);
#12503=EDGE_CURVE('',#9430,#9428,#1825,.T.);
#12504=EDGE_CURVE('',#9429,#9427,#1826,.T.);
#12505=EDGE_CURVE('',#9431,#9432,#5950,.T.);
#12506=EDGE_CURVE('',#9432,#9430,#1827,.T.);
#12507=EDGE_CURVE('',#9431,#9429,#1828,.T.);
#12508=EDGE_CURVE('',#9433,#9434,#5951,.T.);
#12509=EDGE_CURVE('',#9434,#9432,#1829,.T.);
#12510=EDGE_CURVE('',#9433,#9431,#1830,.T.);
#12511=EDGE_CURVE('',#9435,#9436,#5952,.T.);
#12512=EDGE_CURVE('',#9436,#9434,#1831,.T.);
#12513=EDGE_CURVE('',#9435,#9433,#1832,.T.);
#12514=EDGE_CURVE('',#9437,#9438,#5953,.T.);
#12515=EDGE_CURVE('',#9438,#9436,#1833,.T.);
#12516=EDGE_CURVE('',#9437,#9435,#1834,.T.);
#12517=EDGE_CURVE('',#9439,#9440,#5954,.T.);
#12518=EDGE_CURVE('',#9440,#9438,#1835,.T.);
#12519=EDGE_CURVE('',#9439,#9437,#1836,.T.);
#12520=EDGE_CURVE('',#9441,#9442,#5955,.T.);
#12521=EDGE_CURVE('',#9443,#9441,#1837,.T.);
#12522=EDGE_CURVE('',#9444,#9443,#7591,.T.);
#12523=EDGE_CURVE('',#9444,#9442,#1838,.T.);
#12524=EDGE_CURVE('',#9445,#9446,#5956,.T.);
#12525=EDGE_CURVE('',#9446,#9447,#1839,.T.);
#12526=EDGE_CURVE('',#9448,#9447,#7592,.T.);
#12527=EDGE_CURVE('',#9445,#9448,#1840,.T.);
#12528=EDGE_CURVE('',#9449,#9450,#5957,.T.);
#12529=EDGE_CURVE('',#9450,#9446,#1841,.T.);
#12530=EDGE_CURVE('',#9449,#9445,#1842,.T.);
#12531=EDGE_CURVE('',#9451,#9452,#5958,.T.);
#12532=EDGE_CURVE('',#9452,#9450,#1843,.T.);
#12533=EDGE_CURVE('',#9451,#9449,#1844,.T.);
#12534=EDGE_CURVE('',#9453,#9454,#5959,.T.);
#12535=EDGE_CURVE('',#9454,#9452,#1845,.T.);
#12536=EDGE_CURVE('',#9453,#9451,#1846,.T.);
#12537=EDGE_CURVE('',#9455,#9456,#5960,.T.);
#12538=EDGE_CURVE('',#9456,#9454,#1847,.T.);
#12539=EDGE_CURVE('',#9455,#9453,#1848,.T.);
#12540=EDGE_CURVE('',#9457,#9458,#5961,.T.);
#12541=EDGE_CURVE('',#9458,#9456,#1849,.T.);
#12542=EDGE_CURVE('',#9457,#9455,#1850,.T.);
#12543=EDGE_CURVE('',#9459,#9460,#5962,.T.);
#12544=EDGE_CURVE('',#9460,#9458,#1851,.T.);
#12545=EDGE_CURVE('',#9459,#9457,#1852,.T.);
#12546=EDGE_CURVE('',#9461,#9462,#5963,.T.);
#12547=EDGE_CURVE('',#9462,#9460,#1853,.T.);
#12548=EDGE_CURVE('',#9461,#9459,#1854,.T.);
#12549=EDGE_CURVE('',#9463,#9464,#5964,.T.);
#12550=EDGE_CURVE('',#9464,#9462,#1855,.T.);
#12551=EDGE_CURVE('',#9463,#9461,#1856,.T.);
#12552=EDGE_CURVE('',#9465,#9466,#5965,.T.);
#12553=EDGE_CURVE('',#9466,#9464,#1857,.T.);
#12554=EDGE_CURVE('',#9465,#9463,#1858,.T.);
#12555=EDGE_CURVE('',#9467,#9468,#5966,.T.);
#12556=EDGE_CURVE('',#9468,#9466,#1859,.T.);
#12557=EDGE_CURVE('',#9467,#9465,#1860,.T.);
#12558=EDGE_CURVE('',#9469,#9470,#5967,.T.);
#12559=EDGE_CURVE('',#9470,#9468,#1861,.T.);
#12560=EDGE_CURVE('',#9469,#9467,#1862,.T.);
#12561=EDGE_CURVE('',#9471,#9472,#5968,.T.);
#12562=EDGE_CURVE('',#9472,#9470,#1863,.T.);
#12563=EDGE_CURVE('',#9471,#9469,#1864,.T.);
#12564=EDGE_CURVE('',#9473,#9474,#5969,.T.);
#12565=EDGE_CURVE('',#9474,#9472,#1865,.T.);
#12566=EDGE_CURVE('',#9473,#9471,#1866,.T.);
#12567=EDGE_CURVE('',#9475,#9476,#5970,.T.);
#12568=EDGE_CURVE('',#9476,#9474,#1867,.T.);
#12569=EDGE_CURVE('',#9475,#9473,#1868,.T.);
#12570=EDGE_CURVE('',#9477,#9478,#5971,.T.);
#12571=EDGE_CURVE('',#9478,#9476,#1869,.T.);
#12572=EDGE_CURVE('',#9477,#9475,#1870,.T.);
#12573=EDGE_CURVE('',#9479,#9480,#5972,.T.);
#12574=EDGE_CURVE('',#9480,#9478,#1871,.T.);
#12575=EDGE_CURVE('',#9479,#9477,#1872,.T.);
#12576=EDGE_CURVE('',#9481,#9482,#5973,.T.);
#12577=EDGE_CURVE('',#9482,#9480,#1873,.T.);
#12578=EDGE_CURVE('',#9481,#9479,#1874,.T.);
#12579=EDGE_CURVE('',#9483,#9484,#5974,.T.);
#12580=EDGE_CURVE('',#9484,#9482,#1875,.T.);
#12581=EDGE_CURVE('',#9483,#9481,#1876,.T.);
#12582=EDGE_CURVE('',#9485,#9486,#5975,.T.);
#12583=EDGE_CURVE('',#9487,#9485,#1877,.T.);
#12584=EDGE_CURVE('',#9488,#9487,#7593,.T.);
#12585=EDGE_CURVE('',#9488,#9486,#1878,.T.);
#12586=EDGE_CURVE('',#9489,#9490,#5976,.T.);
#12587=EDGE_CURVE('',#9490,#9491,#1879,.T.);
#12588=EDGE_CURVE('',#9492,#9491,#7594,.T.);
#12589=EDGE_CURVE('',#9489,#9492,#1880,.T.);
#12590=EDGE_CURVE('',#9493,#9494,#5977,.T.);
#12591=EDGE_CURVE('',#9494,#9490,#1881,.T.);
#12592=EDGE_CURVE('',#9493,#9489,#1882,.T.);
#12593=EDGE_CURVE('',#9495,#9496,#5978,.T.);
#12594=EDGE_CURVE('',#9496,#9494,#1883,.T.);
#12595=EDGE_CURVE('',#9495,#9493,#1884,.T.);
#12596=EDGE_CURVE('',#9497,#9498,#5979,.T.);
#12597=EDGE_CURVE('',#9498,#9496,#1885,.T.);
#12598=EDGE_CURVE('',#9497,#9495,#1886,.T.);
#12599=EDGE_CURVE('',#9499,#9500,#5980,.T.);
#12600=EDGE_CURVE('',#9500,#9498,#1887,.T.);
#12601=EDGE_CURVE('',#9499,#9497,#1888,.T.);
#12602=EDGE_CURVE('',#9501,#9502,#5981,.T.);
#12603=EDGE_CURVE('',#9502,#9500,#1889,.T.);
#12604=EDGE_CURVE('',#9501,#9499,#1890,.T.);
#12605=EDGE_CURVE('',#9503,#9504,#5982,.T.);
#12606=EDGE_CURVE('',#9504,#9502,#1891,.T.);
#12607=EDGE_CURVE('',#9503,#9501,#1892,.T.);
#12608=EDGE_CURVE('',#9505,#9506,#5983,.T.);
#12609=EDGE_CURVE('',#9506,#9504,#1893,.T.);
#12610=EDGE_CURVE('',#9505,#9503,#1894,.T.);
#12611=EDGE_CURVE('',#9507,#9508,#5984,.T.);
#12612=EDGE_CURVE('',#9508,#9506,#1895,.T.);
#12613=EDGE_CURVE('',#9507,#9505,#1896,.T.);
#12614=EDGE_CURVE('',#9509,#9510,#5985,.T.);
#12615=EDGE_CURVE('',#9510,#9508,#1897,.T.);
#12616=EDGE_CURVE('',#9509,#9507,#1898,.T.);
#12617=EDGE_CURVE('',#9511,#9512,#5986,.T.);
#12618=EDGE_CURVE('',#9512,#9510,#1899,.T.);
#12619=EDGE_CURVE('',#9511,#9509,#1900,.T.);
#12620=EDGE_CURVE('',#9513,#9514,#5987,.T.);
#12621=EDGE_CURVE('',#9514,#9512,#1901,.T.);
#12622=EDGE_CURVE('',#9513,#9511,#1902,.T.);
#12623=EDGE_CURVE('',#9515,#9516,#5988,.T.);
#12624=EDGE_CURVE('',#9516,#9514,#1903,.T.);
#12625=EDGE_CURVE('',#9515,#9513,#1904,.T.);
#12626=EDGE_CURVE('',#9517,#9518,#5989,.T.);
#12627=EDGE_CURVE('',#9518,#9516,#1905,.T.);
#12628=EDGE_CURVE('',#9517,#9515,#1906,.T.);
#12629=EDGE_CURVE('',#9519,#9520,#5990,.T.);
#12630=EDGE_CURVE('',#9520,#9518,#1907,.T.);
#12631=EDGE_CURVE('',#9519,#9517,#1908,.T.);
#12632=EDGE_CURVE('',#9521,#9522,#5991,.T.);
#12633=EDGE_CURVE('',#9522,#9520,#1909,.T.);
#12634=EDGE_CURVE('',#9521,#9519,#1910,.T.);
#12635=EDGE_CURVE('',#9523,#9524,#5992,.T.);
#12636=EDGE_CURVE('',#9524,#9522,#1911,.T.);
#12637=EDGE_CURVE('',#9523,#9521,#1912,.T.);
#12638=EDGE_CURVE('',#9525,#9526,#5993,.T.);
#12639=EDGE_CURVE('',#9526,#9524,#1913,.T.);
#12640=EDGE_CURVE('',#9525,#9523,#1914,.T.);
#12641=EDGE_CURVE('',#9527,#9528,#5994,.T.);
#12642=EDGE_CURVE('',#9528,#9526,#1915,.T.);
#12643=EDGE_CURVE('',#9527,#9525,#1916,.T.);
#12644=EDGE_CURVE('',#9529,#9530,#5995,.T.);
#12645=EDGE_CURVE('',#9531,#9529,#1917,.T.);
#12646=EDGE_CURVE('',#9532,#9531,#7595,.T.);
#12647=EDGE_CURVE('',#9532,#9530,#1918,.T.);
#12648=EDGE_CURVE('',#9533,#9534,#5996,.T.);
#12649=EDGE_CURVE('',#9534,#9535,#1919,.T.);
#12650=EDGE_CURVE('',#9536,#9535,#7596,.T.);
#12651=EDGE_CURVE('',#9533,#9536,#1920,.T.);
#12652=EDGE_CURVE('',#9537,#9538,#5997,.T.);
#12653=EDGE_CURVE('',#9538,#9534,#1921,.T.);
#12654=EDGE_CURVE('',#9537,#9533,#1922,.T.);
#12655=EDGE_CURVE('',#9539,#9540,#5998,.T.);
#12656=EDGE_CURVE('',#9540,#9538,#1923,.T.);
#12657=EDGE_CURVE('',#9539,#9537,#1924,.T.);
#12658=EDGE_CURVE('',#9541,#9542,#5999,.T.);
#12659=EDGE_CURVE('',#9542,#9540,#1925,.T.);
#12660=EDGE_CURVE('',#9541,#9539,#1926,.T.);
#12661=EDGE_CURVE('',#9543,#9544,#6000,.T.);
#12662=EDGE_CURVE('',#9544,#9542,#1927,.T.);
#12663=EDGE_CURVE('',#9543,#9541,#1928,.T.);
#12664=EDGE_CURVE('',#9545,#9546,#6001,.T.);
#12665=EDGE_CURVE('',#9546,#9544,#1929,.T.);
#12666=EDGE_CURVE('',#9545,#9543,#1930,.T.);
#12667=EDGE_CURVE('',#9547,#9548,#6002,.T.);
#12668=EDGE_CURVE('',#9548,#9546,#1931,.T.);
#12669=EDGE_CURVE('',#9547,#9545,#1932,.T.);
#12670=EDGE_CURVE('',#9549,#9550,#6003,.T.);
#12671=EDGE_CURVE('',#9550,#9548,#1933,.T.);
#12672=EDGE_CURVE('',#9549,#9547,#1934,.T.);
#12673=EDGE_CURVE('',#9551,#9552,#6004,.T.);
#12674=EDGE_CURVE('',#9552,#9550,#1935,.T.);
#12675=EDGE_CURVE('',#9551,#9549,#1936,.T.);
#12676=EDGE_CURVE('',#9553,#9554,#6005,.T.);
#12677=EDGE_CURVE('',#9554,#9552,#1937,.T.);
#12678=EDGE_CURVE('',#9553,#9551,#1938,.T.);
#12679=EDGE_CURVE('',#9555,#9556,#6006,.T.);
#12680=EDGE_CURVE('',#9556,#9554,#1939,.T.);
#12681=EDGE_CURVE('',#9555,#9553,#1940,.T.);
#12682=EDGE_CURVE('',#9557,#9558,#6007,.T.);
#12683=EDGE_CURVE('',#9558,#9556,#1941,.T.);
#12684=EDGE_CURVE('',#9557,#9555,#1942,.T.);
#12685=EDGE_CURVE('',#9559,#9560,#6008,.T.);
#12686=EDGE_CURVE('',#9560,#9558,#1943,.T.);
#12687=EDGE_CURVE('',#9559,#9557,#1944,.T.);
#12688=EDGE_CURVE('',#9561,#9562,#6009,.T.);
#12689=EDGE_CURVE('',#9562,#9560,#1945,.T.);
#12690=EDGE_CURVE('',#9561,#9559,#1946,.T.);
#12691=EDGE_CURVE('',#9563,#9564,#6010,.T.);
#12692=EDGE_CURVE('',#9564,#9562,#1947,.T.);
#12693=EDGE_CURVE('',#9563,#9561,#1948,.T.);
#12694=EDGE_CURVE('',#9565,#9566,#6011,.T.);
#12695=EDGE_CURVE('',#9566,#9564,#1949,.T.);
#12696=EDGE_CURVE('',#9565,#9563,#1950,.T.);
#12697=EDGE_CURVE('',#9567,#9568,#6012,.T.);
#12698=EDGE_CURVE('',#9568,#9566,#1951,.T.);
#12699=EDGE_CURVE('',#9567,#9565,#1952,.T.);
#12700=EDGE_CURVE('',#9569,#9570,#6013,.T.);
#12701=EDGE_CURVE('',#9570,#9568,#1953,.T.);
#12702=EDGE_CURVE('',#9569,#9567,#1954,.T.);
#12703=EDGE_CURVE('',#9571,#9572,#6014,.T.);
#12704=EDGE_CURVE('',#9572,#9570,#1955,.T.);
#12705=EDGE_CURVE('',#9571,#9569,#1956,.T.);
#12706=EDGE_CURVE('',#9573,#9574,#6015,.T.);
#12707=EDGE_CURVE('',#9575,#9573,#1957,.T.);
#12708=EDGE_CURVE('',#9576,#9575,#7597,.T.);
#12709=EDGE_CURVE('',#9576,#9574,#1958,.T.);
#12710=EDGE_CURVE('',#9574,#9572,#1959,.T.);
#12711=EDGE_CURVE('',#9573,#9571,#1960,.T.);
#12712=EDGE_CURVE('',#9535,#9140,#1961,.T.);
#12713=EDGE_CURVE('',#9179,#9576,#1962,.T.);
#12714=EDGE_CURVE('',#9175,#9177,#1963,.T.);
#12715=EDGE_CURVE('',#9139,#9536,#1964,.T.);
#12716=EDGE_CURVE('',#9178,#9176,#1965,.T.);
#12717=EDGE_CURVE('',#9575,#9180,#1966,.T.);
#12718=EDGE_CURVE('',#9577,#9578,#6016,.T.);
#12719=EDGE_CURVE('',#9578,#9579,#6017,.T.);
#12720=EDGE_CURVE('',#9579,#9580,#6018,.T.);
#12721=EDGE_CURVE('',#9580,#9577,#6019,.T.);
#12722=EDGE_CURVE('',#9091,#9400,#1967,.T.);
#12723=EDGE_CURVE('',#9399,#9092,#1968,.T.);
#12724=EDGE_CURVE('',#9135,#9444,#1969,.T.);
#12725=EDGE_CURVE('',#9443,#9136,#1970,.T.);
#12726=EDGE_CURVE('',#9223,#9488,#1971,.T.);
#12727=EDGE_CURVE('',#9487,#9224,#1972,.T.);
#12728=EDGE_CURVE('',#9267,#9532,#1973,.T.);
#12729=EDGE_CURVE('',#9531,#9268,#1974,.T.);
#12730=EDGE_CURVE('',#9311,#9356,#1975,.T.);
#12731=EDGE_CURVE('',#9355,#9312,#1976,.T.);
#12732=EDGE_CURVE('',#9530,#9528,#1977,.T.);
#12733=EDGE_CURVE('',#9529,#9527,#1978,.T.);
#12734=EDGE_CURVE('',#9491,#9228,#1979,.T.);
#12735=EDGE_CURVE('',#9263,#9265,#1980,.T.);
#12736=EDGE_CURVE('',#9227,#9492,#1981,.T.);
#12737=EDGE_CURVE('',#9266,#9264,#1982,.T.);
#12738=EDGE_CURVE('',#9486,#9484,#1983,.T.);
#12739=EDGE_CURVE('',#9485,#9483,#1984,.T.);
#12740=EDGE_CURVE('',#9447,#9184,#1985,.T.);
#12741=EDGE_CURVE('',#9219,#9221,#1986,.T.);
#12742=EDGE_CURVE('',#9183,#9448,#1987,.T.);
#12743=EDGE_CURVE('',#9222,#9220,#1988,.T.);
#12744=EDGE_CURVE('',#9442,#9440,#1989,.T.);
#12745=EDGE_CURVE('',#9441,#9439,#1990,.T.);
#12746=EDGE_CURVE('',#9403,#9096,#1991,.T.);
#12747=EDGE_CURVE('',#9131,#9133,#1992,.T.);
#12748=EDGE_CURVE('',#9095,#9404,#1993,.T.);
#12749=EDGE_CURVE('',#9134,#9132,#1994,.T.);
#12750=EDGE_CURVE('',#9398,#9396,#1995,.T.);
#12751=EDGE_CURVE('',#9397,#9395,#1996,.T.);
#12752=EDGE_CURVE('',#9359,#9052,#1997,.T.);
#12753=EDGE_CURVE('',#9087,#9089,#1998,.T.);
#12754=EDGE_CURVE('',#9051,#9360,#1999,.T.);
#12755=EDGE_CURVE('',#9090,#9088,#2000,.T.);
#12756=EDGE_CURVE('',#9354,#9352,#2001,.T.);
#12757=EDGE_CURVE('',#9353,#9351,#2002,.T.);
#12758=EDGE_CURVE('',#9315,#9272,#2003,.T.);
#12759=EDGE_CURVE('',#9307,#9309,#2004,.T.);
#12760=EDGE_CURVE('',#9271,#9316,#2005,.T.);
#12761=EDGE_CURVE('',#9310,#9308,#2006,.T.);
#12762=EDGE_CURVE('',#9581,#9582,#6020,.T.);
#12763=EDGE_CURVE('',#9582,#9577,#6021,.T.);
#12764=EDGE_CURVE('',#9581,#9580,#6022,.T.);
#12765=EDGE_CURVE('',#9583,#9581,#6023,.T.);
#12766=EDGE_CURVE('',#9583,#9579,#6024,.T.);
#12767=EDGE_CURVE('',#9584,#9583,#6025,.T.);
#12768=EDGE_CURVE('',#9584,#9578,#6026,.T.);
#12769=EDGE_CURVE('',#9582,#9584,#6027,.T.);
#12770=EDGE_CURVE('',#9585,#9586,#6028,.T.);
#12771=EDGE_CURVE('',#9585,#9587,#2007,.T.);
#12772=EDGE_CURVE('',#9587,#9588,#7598,.F.);
#12773=EDGE_CURVE('',#9588,#9586,#2008,.T.);
#12774=EDGE_CURVE('',#9589,#9590,#6029,.T.);
#12775=EDGE_CURVE('',#9589,#9585,#2009,.T.);
#12776=EDGE_CURVE('',#9586,#9590,#2010,.T.);
#12777=EDGE_CURVE('',#9591,#9592,#6030,.T.);
#12778=EDGE_CURVE('',#9591,#9589,#2011,.T.);
#12779=EDGE_CURVE('',#9590,#9592,#2012,.T.);
#12780=EDGE_CURVE('',#9593,#9594,#6031,.T.);
#12781=EDGE_CURVE('',#9593,#9591,#2013,.T.);
#12782=EDGE_CURVE('',#9592,#9594,#2014,.T.);
#12783=EDGE_CURVE('',#9595,#9596,#6032,.T.);
#12784=EDGE_CURVE('',#9595,#9593,#2015,.T.);
#12785=EDGE_CURVE('',#9594,#9596,#2016,.T.);
#12786=EDGE_CURVE('',#9597,#9598,#6033,.T.);
#12787=EDGE_CURVE('',#9597,#9595,#2017,.T.);
#12788=EDGE_CURVE('',#9596,#9598,#2018,.T.);
#12789=EDGE_CURVE('',#9599,#9600,#6034,.T.);
#12790=EDGE_CURVE('',#9599,#9597,#2019,.T.);
#12791=EDGE_CURVE('',#9598,#9600,#2020,.T.);
#12792=EDGE_CURVE('',#9601,#9602,#6035,.T.);
#12793=EDGE_CURVE('',#9601,#9599,#2021,.T.);
#12794=EDGE_CURVE('',#9600,#9602,#2022,.T.);
#12795=EDGE_CURVE('',#9603,#9604,#6036,.T.);
#12796=EDGE_CURVE('',#9603,#9601,#2023,.T.);
#12797=EDGE_CURVE('',#9602,#9604,#2024,.T.);
#12798=EDGE_CURVE('',#9605,#9606,#6037,.T.);
#12799=EDGE_CURVE('',#9605,#9603,#2025,.T.);
#12800=EDGE_CURVE('',#9604,#9606,#2026,.T.);
#12801=EDGE_CURVE('',#9607,#9608,#6038,.T.);
#12802=EDGE_CURVE('',#9607,#9605,#2027,.T.);
#12803=EDGE_CURVE('',#9606,#9608,#2028,.T.);
#12804=EDGE_CURVE('',#9609,#9610,#6039,.T.);
#12805=EDGE_CURVE('',#9609,#9607,#2029,.T.);
#12806=EDGE_CURVE('',#9608,#9610,#2030,.T.);
#12807=EDGE_CURVE('',#9611,#9612,#6040,.T.);
#12808=EDGE_CURVE('',#9611,#9609,#2031,.T.);
#12809=EDGE_CURVE('',#9610,#9612,#2032,.T.);
#12810=EDGE_CURVE('',#9613,#9614,#6041,.T.);
#12811=EDGE_CURVE('',#9613,#9611,#2033,.T.);
#12812=EDGE_CURVE('',#9612,#9614,#2034,.T.);
#12813=EDGE_CURVE('',#9615,#9616,#6042,.T.);
#12814=EDGE_CURVE('',#9615,#9613,#2035,.T.);
#12815=EDGE_CURVE('',#9614,#9616,#2036,.T.);
#12816=EDGE_CURVE('',#9617,#9618,#6043,.T.);
#12817=EDGE_CURVE('',#9617,#9615,#2037,.T.);
#12818=EDGE_CURVE('',#9616,#9618,#2038,.T.);
#12819=EDGE_CURVE('',#9619,#9620,#6044,.T.);
#12820=EDGE_CURVE('',#9619,#9617,#2039,.T.);
#12821=EDGE_CURVE('',#9618,#9620,#2040,.T.);
#12822=EDGE_CURVE('',#9621,#9622,#6045,.T.);
#12823=EDGE_CURVE('',#9621,#9619,#2041,.T.);
#12824=EDGE_CURVE('',#9620,#9622,#2042,.T.);
#12825=EDGE_CURVE('',#9623,#9624,#6046,.T.);
#12826=EDGE_CURVE('',#9623,#9621,#2043,.T.);
#12827=EDGE_CURVE('',#9622,#9624,#2044,.T.);
#12828=EDGE_CURVE('',#9625,#9626,#6047,.T.);
#12829=EDGE_CURVE('',#9625,#9623,#2045,.T.);
#12830=EDGE_CURVE('',#9624,#9626,#2046,.T.);
#12831=EDGE_CURVE('',#9627,#9628,#6048,.T.);
#12832=EDGE_CURVE('',#9627,#9625,#2047,.T.);
#12833=EDGE_CURVE('',#9626,#9628,#2048,.T.);
#12834=EDGE_CURVE('',#9629,#9630,#6049,.T.);
#12835=EDGE_CURVE('',#9629,#9627,#2049,.T.);
#12836=EDGE_CURVE('',#9628,#9630,#2050,.T.);
#12837=EDGE_CURVE('',#9631,#9632,#6050,.T.);
#12838=EDGE_CURVE('',#9631,#9629,#2051,.T.);
#12839=EDGE_CURVE('',#9630,#9632,#2052,.T.);
#12840=EDGE_CURVE('',#9633,#9634,#6051,.T.);
#12841=EDGE_CURVE('',#9633,#9631,#2053,.T.);
#12842=EDGE_CURVE('',#9632,#9634,#2054,.T.);
#12843=EDGE_CURVE('',#9635,#9636,#6052,.T.);
#12844=EDGE_CURVE('',#9635,#9633,#2055,.T.);
#12845=EDGE_CURVE('',#9634,#9636,#2056,.T.);
#12846=EDGE_CURVE('',#9637,#9638,#6053,.T.);
#12847=EDGE_CURVE('',#9637,#9635,#2057,.T.);
#12848=EDGE_CURVE('',#9636,#9638,#2058,.T.);
#12849=EDGE_CURVE('',#9639,#9640,#6054,.T.);
#12850=EDGE_CURVE('',#9639,#9637,#2059,.T.);
#12851=EDGE_CURVE('',#9638,#9640,#2060,.T.);
#12852=EDGE_CURVE('',#9641,#9642,#6055,.T.);
#12853=EDGE_CURVE('',#9641,#9639,#2061,.T.);
#12854=EDGE_CURVE('',#9640,#9642,#2062,.T.);
#12855=EDGE_CURVE('',#9643,#9644,#6056,.T.);
#12856=EDGE_CURVE('',#9643,#9641,#2063,.T.);
#12857=EDGE_CURVE('',#9642,#9644,#2064,.T.);
#12858=EDGE_CURVE('',#9645,#9646,#6057,.T.);
#12859=EDGE_CURVE('',#9645,#9643,#2065,.T.);
#12860=EDGE_CURVE('',#9644,#9646,#2066,.T.);
#12861=EDGE_CURVE('',#9647,#9648,#6058,.T.);
#12862=EDGE_CURVE('',#9647,#9645,#2067,.T.);
#12863=EDGE_CURVE('',#9646,#9648,#2068,.T.);
#12864=EDGE_CURVE('',#9649,#9650,#6059,.T.);
#12865=EDGE_CURVE('',#9649,#9647,#2069,.T.);
#12866=EDGE_CURVE('',#9648,#9650,#2070,.T.);
#12867=EDGE_CURVE('',#9651,#9652,#6060,.T.);
#12868=EDGE_CURVE('',#9651,#9649,#2071,.T.);
#12869=EDGE_CURVE('',#9650,#9652,#2072,.T.);
#12870=EDGE_CURVE('',#9653,#9654,#6061,.T.);
#12871=EDGE_CURVE('',#9653,#9651,#2073,.T.);
#12872=EDGE_CURVE('',#9652,#9654,#2074,.T.);
#12873=EDGE_CURVE('',#9655,#9656,#6062,.T.);
#12874=EDGE_CURVE('',#9655,#9653,#2075,.T.);
#12875=EDGE_CURVE('',#9654,#9656,#2076,.T.);
#12876=EDGE_CURVE('',#9657,#9658,#6063,.T.);
#12877=EDGE_CURVE('',#9657,#9655,#2077,.T.);
#12878=EDGE_CURVE('',#9656,#9658,#2078,.T.);
#12879=EDGE_CURVE('',#9659,#9660,#6064,.T.);
#12880=EDGE_CURVE('',#9659,#9657,#2079,.T.);
#12881=EDGE_CURVE('',#9658,#9660,#2080,.T.);
#12882=EDGE_CURVE('',#9661,#9662,#6065,.T.);
#12883=EDGE_CURVE('',#9661,#9659,#2081,.T.);
#12884=EDGE_CURVE('',#9660,#9662,#2082,.T.);
#12885=EDGE_CURVE('',#9663,#9664,#6066,.T.);
#12886=EDGE_CURVE('',#9663,#9661,#2083,.T.);
#12887=EDGE_CURVE('',#9662,#9664,#2084,.T.);
#12888=EDGE_CURVE('',#9665,#9666,#6067,.T.);
#12889=EDGE_CURVE('',#9665,#9663,#2085,.T.);
#12890=EDGE_CURVE('',#9664,#9666,#2086,.T.);
#12891=EDGE_CURVE('',#9667,#9668,#6068,.T.);
#12892=EDGE_CURVE('',#9667,#9665,#2087,.T.);
#12893=EDGE_CURVE('',#9666,#9668,#2088,.T.);
#12894=EDGE_CURVE('',#9669,#9670,#6069,.T.);
#12895=EDGE_CURVE('',#9669,#9667,#2089,.T.);
#12896=EDGE_CURVE('',#9668,#9670,#2090,.T.);
#12897=EDGE_CURVE('',#9671,#9672,#6070,.T.);
#12898=EDGE_CURVE('',#9671,#9669,#2091,.T.);
#12899=EDGE_CURVE('',#9670,#9672,#2092,.T.);
#12900=EDGE_CURVE('',#9673,#9674,#6071,.T.);
#12901=EDGE_CURVE('',#9673,#9671,#2093,.T.);
#12902=EDGE_CURVE('',#9672,#9674,#2094,.T.);
#12903=EDGE_CURVE('',#9675,#9676,#6072,.T.);
#12904=EDGE_CURVE('',#9675,#9673,#2095,.T.);
#12905=EDGE_CURVE('',#9674,#9676,#2096,.T.);
#12906=EDGE_CURVE('',#9677,#9678,#6073,.T.);
#12907=EDGE_CURVE('',#9677,#9675,#2097,.T.);
#12908=EDGE_CURVE('',#9676,#9678,#2098,.T.);
#12909=EDGE_CURVE('',#9679,#9680,#6074,.T.);
#12910=EDGE_CURVE('',#9679,#9677,#2099,.T.);
#12911=EDGE_CURVE('',#9678,#9680,#2100,.T.);
#12912=EDGE_CURVE('',#9681,#9682,#6075,.T.);
#12913=EDGE_CURVE('',#9681,#9679,#2101,.T.);
#12914=EDGE_CURVE('',#9680,#9682,#2102,.T.);
#12915=EDGE_CURVE('',#9683,#9684,#6076,.T.);
#12916=EDGE_CURVE('',#9683,#9681,#2103,.T.);
#12917=EDGE_CURVE('',#9682,#9684,#2104,.T.);
#12918=EDGE_CURVE('',#9685,#9686,#6077,.T.);
#12919=EDGE_CURVE('',#9685,#9687,#2105,.T.);
#12920=EDGE_CURVE('',#9687,#9688,#7599,.T.);
#12921=EDGE_CURVE('',#9686,#9688,#2106,.T.);
#12922=EDGE_CURVE('',#9689,#9690,#6078,.T.);
#12923=EDGE_CURVE('',#9689,#9685,#2107,.T.);
#12924=EDGE_CURVE('',#9690,#9686,#2108,.T.);
#12925=EDGE_CURVE('',#9691,#9692,#6079,.T.);
#12926=EDGE_CURVE('',#9691,#9689,#2109,.T.);
#12927=EDGE_CURVE('',#9692,#9690,#2110,.T.);
#12928=EDGE_CURVE('',#9693,#9694,#6080,.T.);
#12929=EDGE_CURVE('',#9693,#9691,#2111,.T.);
#12930=EDGE_CURVE('',#9694,#9692,#2112,.T.);
#12931=EDGE_CURVE('',#9695,#9696,#6081,.T.);
#12932=EDGE_CURVE('',#9695,#9693,#2113,.T.);
#12933=EDGE_CURVE('',#9696,#9694,#2114,.T.);
#12934=EDGE_CURVE('',#9697,#9698,#6082,.T.);
#12935=EDGE_CURVE('',#9697,#9695,#2115,.T.);
#12936=EDGE_CURVE('',#9698,#9696,#2116,.T.);
#12937=EDGE_CURVE('',#9699,#9700,#6083,.T.);
#12938=EDGE_CURVE('',#9699,#9697,#2117,.T.);
#12939=EDGE_CURVE('',#9700,#9698,#2118,.T.);
#12940=EDGE_CURVE('',#9701,#9702,#6084,.T.);
#12941=EDGE_CURVE('',#9701,#9699,#2119,.T.);
#12942=EDGE_CURVE('',#9702,#9700,#2120,.T.);
#12943=EDGE_CURVE('',#9703,#9704,#6085,.T.);
#12944=EDGE_CURVE('',#9703,#9701,#2121,.T.);
#12945=EDGE_CURVE('',#9704,#9702,#2122,.T.);
#12946=EDGE_CURVE('',#9705,#9706,#6086,.T.);
#12947=EDGE_CURVE('',#9705,#9703,#2123,.T.);
#12948=EDGE_CURVE('',#9706,#9704,#2124,.T.);
#12949=EDGE_CURVE('',#9707,#9708,#6087,.T.);
#12950=EDGE_CURVE('',#9707,#9705,#2125,.T.);
#12951=EDGE_CURVE('',#9708,#9706,#2126,.T.);
#12952=EDGE_CURVE('',#9709,#9710,#6088,.T.);
#12953=EDGE_CURVE('',#9709,#9707,#2127,.T.);
#12954=EDGE_CURVE('',#9710,#9708,#2128,.T.);
#12955=EDGE_CURVE('',#9711,#9712,#6089,.T.);
#12956=EDGE_CURVE('',#9711,#9709,#2129,.T.);
#12957=EDGE_CURVE('',#9712,#9710,#2130,.T.);
#12958=EDGE_CURVE('',#9713,#9714,#6090,.T.);
#12959=EDGE_CURVE('',#9713,#9711,#2131,.T.);
#12960=EDGE_CURVE('',#9714,#9712,#2132,.T.);
#12961=EDGE_CURVE('',#9715,#9716,#6091,.T.);
#12962=EDGE_CURVE('',#9715,#9713,#2133,.T.);
#12963=EDGE_CURVE('',#9716,#9714,#2134,.T.);
#12964=EDGE_CURVE('',#9717,#9718,#6092,.T.);
#12965=EDGE_CURVE('',#9717,#9715,#2135,.T.);
#12966=EDGE_CURVE('',#9718,#9716,#2136,.T.);
#12967=EDGE_CURVE('',#9719,#9720,#6093,.T.);
#12968=EDGE_CURVE('',#9719,#9717,#2137,.T.);
#12969=EDGE_CURVE('',#9720,#9718,#2138,.T.);
#12970=EDGE_CURVE('',#9721,#9722,#6094,.T.);
#12971=EDGE_CURVE('',#9721,#9719,#2139,.T.);
#12972=EDGE_CURVE('',#9722,#9720,#2140,.T.);
#12973=EDGE_CURVE('',#9723,#9724,#6095,.T.);
#12974=EDGE_CURVE('',#9723,#9721,#2141,.T.);
#12975=EDGE_CURVE('',#9724,#9722,#2142,.T.);
#12976=EDGE_CURVE('',#9725,#9726,#6096,.T.);
#12977=EDGE_CURVE('',#9725,#9723,#2143,.T.);
#12978=EDGE_CURVE('',#9726,#9724,#2144,.T.);
#12979=EDGE_CURVE('',#9727,#9728,#6097,.T.);
#12980=EDGE_CURVE('',#9727,#9725,#2145,.T.);
#12981=EDGE_CURVE('',#9728,#9726,#2146,.T.);
#12982=EDGE_CURVE('',#9729,#9730,#6098,.T.);
#12983=EDGE_CURVE('',#9729,#9727,#2147,.T.);
#12984=EDGE_CURVE('',#9730,#9728,#2148,.T.);
#12985=EDGE_CURVE('',#9731,#9732,#6099,.T.);
#12986=EDGE_CURVE('',#9731,#9729,#2149,.T.);
#12987=EDGE_CURVE('',#9732,#9730,#2150,.T.);
#12988=EDGE_CURVE('',#9733,#9734,#6100,.T.);
#12989=EDGE_CURVE('',#9733,#9731,#2151,.T.);
#12990=EDGE_CURVE('',#9734,#9732,#2152,.T.);
#12991=EDGE_CURVE('',#9735,#9736,#6101,.T.);
#12992=EDGE_CURVE('',#9735,#9733,#2153,.T.);
#12993=EDGE_CURVE('',#9736,#9734,#2154,.T.);
#12994=EDGE_CURVE('',#9737,#9738,#6102,.T.);
#12995=EDGE_CURVE('',#9737,#9735,#2155,.T.);
#12996=EDGE_CURVE('',#9738,#9736,#2156,.T.);
#12997=EDGE_CURVE('',#9739,#9740,#6103,.T.);
#12998=EDGE_CURVE('',#9739,#9737,#2157,.T.);
#12999=EDGE_CURVE('',#9740,#9738,#2158,.T.);
#13000=EDGE_CURVE('',#9741,#9742,#6104,.T.);
#13001=EDGE_CURVE('',#9741,#9739,#2159,.T.);
#13002=EDGE_CURVE('',#9742,#9740,#2160,.T.);
#13003=EDGE_CURVE('',#9743,#9744,#6105,.T.);
#13004=EDGE_CURVE('',#9743,#9741,#2161,.T.);
#13005=EDGE_CURVE('',#9744,#9742,#2162,.T.);
#13006=EDGE_CURVE('',#9745,#9746,#6106,.T.);
#13007=EDGE_CURVE('',#9745,#9743,#2163,.T.);
#13008=EDGE_CURVE('',#9746,#9744,#2164,.T.);
#13009=EDGE_CURVE('',#9747,#9748,#6107,.T.);
#13010=EDGE_CURVE('',#9747,#9745,#2165,.T.);
#13011=EDGE_CURVE('',#9748,#9746,#2166,.T.);
#13012=EDGE_CURVE('',#9749,#9750,#6108,.T.);
#13013=EDGE_CURVE('',#9749,#9747,#2167,.T.);
#13014=EDGE_CURVE('',#9750,#9748,#2168,.T.);
#13015=EDGE_CURVE('',#9751,#9752,#6109,.T.);
#13016=EDGE_CURVE('',#9751,#9749,#2169,.T.);
#13017=EDGE_CURVE('',#9752,#9750,#2170,.T.);
#13018=EDGE_CURVE('',#9753,#9754,#6110,.T.);
#13019=EDGE_CURVE('',#9753,#9751,#2171,.T.);
#13020=EDGE_CURVE('',#9754,#9752,#2172,.T.);
#13021=EDGE_CURVE('',#9755,#9756,#6111,.T.);
#13022=EDGE_CURVE('',#9755,#9753,#2173,.T.);
#13023=EDGE_CURVE('',#9756,#9754,#2174,.T.);
#13024=EDGE_CURVE('',#9757,#9758,#6112,.T.);
#13025=EDGE_CURVE('',#9757,#9755,#2175,.T.);
#13026=EDGE_CURVE('',#9758,#9756,#2176,.T.);
#13027=EDGE_CURVE('',#9759,#9760,#6113,.T.);
#13028=EDGE_CURVE('',#9759,#9757,#2177,.T.);
#13029=EDGE_CURVE('',#9760,#9758,#2178,.T.);
#13030=EDGE_CURVE('',#9761,#9762,#6114,.T.);
#13031=EDGE_CURVE('',#9761,#9759,#2179,.T.);
#13032=EDGE_CURVE('',#9762,#9760,#2180,.T.);
#13033=EDGE_CURVE('',#9763,#9764,#6115,.T.);
#13034=EDGE_CURVE('',#9763,#9761,#2181,.T.);
#13035=EDGE_CURVE('',#9764,#9762,#2182,.T.);
#13036=EDGE_CURVE('',#9765,#9766,#6116,.T.);
#13037=EDGE_CURVE('',#9765,#9763,#2183,.T.);
#13038=EDGE_CURVE('',#9766,#9764,#2184,.T.);
#13039=EDGE_CURVE('',#9767,#9768,#6117,.T.);
#13040=EDGE_CURVE('',#9767,#9765,#2185,.T.);
#13041=EDGE_CURVE('',#9768,#9766,#2186,.T.);
#13042=EDGE_CURVE('',#9769,#9770,#6118,.T.);
#13043=EDGE_CURVE('',#9769,#9767,#2187,.T.);
#13044=EDGE_CURVE('',#9770,#9768,#2188,.T.);
#13045=EDGE_CURVE('',#9771,#9772,#6119,.T.);
#13046=EDGE_CURVE('',#9771,#9769,#2189,.T.);
#13047=EDGE_CURVE('',#9772,#9770,#2190,.T.);
#13048=EDGE_CURVE('',#9773,#9774,#6120,.T.);
#13049=EDGE_CURVE('',#9773,#9771,#2191,.T.);
#13050=EDGE_CURVE('',#9774,#9772,#2192,.T.);
#13051=EDGE_CURVE('',#9775,#9776,#6121,.T.);
#13052=EDGE_CURVE('',#9775,#9773,#2193,.T.);
#13053=EDGE_CURVE('',#9776,#9774,#2194,.T.);
#13054=EDGE_CURVE('',#9777,#9778,#6122,.T.);
#13055=EDGE_CURVE('',#9777,#9775,#2195,.T.);
#13056=EDGE_CURVE('',#9778,#9776,#2196,.T.);
#13057=EDGE_CURVE('',#9779,#9780,#6123,.T.);
#13058=EDGE_CURVE('',#9779,#9777,#2197,.T.);
#13059=EDGE_CURVE('',#9780,#9778,#2198,.T.);
#13060=EDGE_CURVE('',#9781,#9782,#6124,.T.);
#13061=EDGE_CURVE('',#9781,#9779,#2199,.T.);
#13062=EDGE_CURVE('',#9782,#9780,#2200,.T.);
#13063=EDGE_CURVE('',#9783,#9784,#6125,.T.);
#13064=EDGE_CURVE('',#9783,#9781,#2201,.T.);
#13065=EDGE_CURVE('',#9784,#9782,#2202,.T.);
#13066=EDGE_CURVE('',#9688,#9785,#2203,.T.);
#13067=EDGE_CURVE('',#9786,#9687,#2204,.T.);
#13068=EDGE_CURVE('',#9787,#9786,#7600,.T.);
#13069=EDGE_CURVE('',#9785,#9787,#2205,.T.);
#13070=EDGE_CURVE('',#9785,#9788,#6126,.T.);
#13071=EDGE_CURVE('',#9788,#9788,#7601,.T.);
#13072=EDGE_CURVE('',#9789,#9783,#2206,.T.);
#13073=EDGE_CURVE('',#9587,#9789,#2207,.T.);
#13074=EDGE_CURVE('',#9786,#9683,#2208,.T.);
#13075=EDGE_CURVE('',#9790,#9784,#2209,.T.);
#13076=EDGE_CURVE('',#9789,#9790,#7602,.T.);
#13077=EDGE_CURVE('',#9684,#9787,#2210,.T.);
#13078=EDGE_CURVE('',#9790,#9588,#2211,.T.);
#13079=EDGE_CURVE('',#9791,#9792,#6127,.T.);
#13080=EDGE_CURVE('',#9791,#9793,#6128,.T.);
#13081=EDGE_CURVE('',#9793,#9794,#6129,.T.);
#13082=EDGE_CURVE('',#9792,#9794,#6130,.T.);
#13083=EDGE_CURVE('',#9795,#9791,#6131,.T.);
#13084=EDGE_CURVE('',#9795,#9796,#6132,.T.);
#13085=EDGE_CURVE('',#9796,#9793,#6133,.T.);
#13086=EDGE_CURVE('',#9797,#9795,#6134,.T.);
#13087=EDGE_CURVE('',#9797,#9798,#6135,.T.);
#13088=EDGE_CURVE('',#9798,#9796,#6136,.T.);
#13089=EDGE_CURVE('',#9799,#9797,#6137,.T.);
#13090=EDGE_CURVE('',#9799,#9800,#6138,.T.);
#13091=EDGE_CURVE('',#9800,#9798,#6139,.T.);
#13092=EDGE_CURVE('',#9801,#9799,#6140,.T.);
#13093=EDGE_CURVE('',#9801,#9802,#6141,.T.);
#13094=EDGE_CURVE('',#9802,#9800,#6142,.T.);
#13095=EDGE_CURVE('',#9792,#9801,#6143,.T.);
#13096=EDGE_CURVE('',#9794,#9802,#6144,.T.);
#13097=EDGE_CURVE('',#9803,#9803,#7603,.T.);
#13098=EDGE_CURVE('',#9803,#9804,#6145,.T.);
#13099=EDGE_CURVE('',#9804,#9804,#7604,.T.);
#13100=EDGE_CURVE('',#9805,#9805,#7605,.T.);
#13101=EDGE_CURVE('',#9805,#9806,#6146,.T.);
#13102=EDGE_CURVE('',#9806,#9806,#7606,.T.);
#13103=EDGE_CURVE('',#9807,#9807,#7607,.T.);
#13104=EDGE_CURVE('',#9807,#9808,#6147,.T.);
#13105=EDGE_CURVE('',#9808,#9808,#7608,.T.);
#13106=EDGE_CURVE('',#9809,#9809,#7609,.T.);
#13107=EDGE_CURVE('',#9809,#9810,#6148,.T.);
#13108=EDGE_CURVE('',#9810,#9810,#7610,.T.);
#13109=EDGE_CURVE('',#9811,#9811,#7611,.T.);
#13110=EDGE_CURVE('',#9811,#9812,#6149,.T.);
#13111=EDGE_CURVE('',#9812,#9812,#7612,.T.);
#13112=ORIENTED_EDGE('',*,*,#9813,.F.);
#13113=ORIENTED_EDGE('',*,*,#9814,.T.);
#13114=ORIENTED_EDGE('',*,*,#9815,.F.);
#13115=ORIENTED_EDGE('',*,*,#9814,.F.);
#13116=ORIENTED_EDGE('',*,*,#9816,.F.);
#13117=ORIENTED_EDGE('',*,*,#9817,.T.);
#13118=ORIENTED_EDGE('',*,*,#9818,.F.);
#13119=ORIENTED_EDGE('',*,*,#9817,.F.);
#13120=ORIENTED_EDGE('',*,*,#9819,.F.);
#13121=ORIENTED_EDGE('',*,*,#9820,.T.);
#13122=ORIENTED_EDGE('',*,*,#9821,.F.);
#13123=ORIENTED_EDGE('',*,*,#9820,.F.);
#13124=ORIENTED_EDGE('',*,*,#9822,.F.);
#13125=ORIENTED_EDGE('',*,*,#9823,.T.);
#13126=ORIENTED_EDGE('',*,*,#9824,.F.);
#13127=ORIENTED_EDGE('',*,*,#9823,.F.);
#13128=ORIENTED_EDGE('',*,*,#9825,.F.);
#13129=ORIENTED_EDGE('',*,*,#9826,.T.);
#13130=ORIENTED_EDGE('',*,*,#9827,.F.);
#13131=ORIENTED_EDGE('',*,*,#9826,.F.);
#13132=ORIENTED_EDGE('',*,*,#9828,.F.);
#13133=ORIENTED_EDGE('',*,*,#9829,.T.);
#13134=ORIENTED_EDGE('',*,*,#9830,.F.);
#13135=ORIENTED_EDGE('',*,*,#9829,.F.);
#13136=ORIENTED_EDGE('',*,*,#9831,.T.);
#13137=ORIENTED_EDGE('',*,*,#9832,.T.);
#13138=ORIENTED_EDGE('',*,*,#9833,.F.);
#13139=ORIENTED_EDGE('',*,*,#9834,.F.);
#13140=ORIENTED_EDGE('',*,*,#9835,.T.);
#13141=ORIENTED_EDGE('',*,*,#9834,.T.);
#13142=ORIENTED_EDGE('',*,*,#9836,.F.);
#13143=ORIENTED_EDGE('',*,*,#9837,.F.);
#13144=ORIENTED_EDGE('',*,*,#9818,.T.);
#13145=ORIENTED_EDGE('',*,*,#9824,.T.);
#13146=ORIENTED_EDGE('',*,*,#9830,.T.);
#13147=ORIENTED_EDGE('',*,*,#9838,.T.);
#13148=ORIENTED_EDGE('',*,*,#9837,.T.);
#13149=ORIENTED_EDGE('',*,*,#9839,.F.);
#13150=ORIENTED_EDGE('',*,*,#9840,.F.);
#13151=ORIENTED_EDGE('',*,*,#9841,.T.);
#13152=ORIENTED_EDGE('',*,*,#9840,.T.);
#13153=ORIENTED_EDGE('',*,*,#9842,.F.);
#13154=ORIENTED_EDGE('',*,*,#9832,.F.);
#13155=ORIENTED_EDGE('',*,*,#9813,.T.);
#13156=ORIENTED_EDGE('',*,*,#9819,.T.);
#13157=ORIENTED_EDGE('',*,*,#9825,.T.);
#13158=ORIENTED_EDGE('',*,*,#9843,.T.);
#13159=ORIENTED_EDGE('',*,*,#9844,.T.);
#13160=ORIENTED_EDGE('',*,*,#9845,.F.);
#13161=ORIENTED_EDGE('',*,*,#9846,.F.);
#13162=ORIENTED_EDGE('',*,*,#9847,.T.);
#13163=ORIENTED_EDGE('',*,*,#9846,.T.);
#13164=ORIENTED_EDGE('',*,*,#9848,.F.);
#13165=ORIENTED_EDGE('',*,*,#9849,.F.);
#13166=ORIENTED_EDGE('',*,*,#9816,.T.);
#13167=ORIENTED_EDGE('',*,*,#9822,.T.);
#13168=ORIENTED_EDGE('',*,*,#9828,.T.);
#13169=ORIENTED_EDGE('',*,*,#9850,.T.);
#13170=ORIENTED_EDGE('',*,*,#9849,.T.);
#13171=ORIENTED_EDGE('',*,*,#9851,.F.);
#13172=ORIENTED_EDGE('',*,*,#9852,.F.);
#13173=ORIENTED_EDGE('',*,*,#9853,.T.);
#13174=ORIENTED_EDGE('',*,*,#9852,.T.);
#13175=ORIENTED_EDGE('',*,*,#9854,.F.);
#13176=ORIENTED_EDGE('',*,*,#9844,.F.);
#13177=ORIENTED_EDGE('',*,*,#9815,.T.);
#13178=ORIENTED_EDGE('',*,*,#9821,.T.);
#13179=ORIENTED_EDGE('',*,*,#9827,.T.);
#13180=ORIENTED_EDGE('',*,*,#9854,.T.);
#13181=ORIENTED_EDGE('',*,*,#9851,.T.);
#13182=ORIENTED_EDGE('',*,*,#9848,.T.);
#13183=ORIENTED_EDGE('',*,*,#9845,.T.);
#13184=ORIENTED_EDGE('',*,*,#9842,.T.);
#13185=ORIENTED_EDGE('',*,*,#9839,.T.);
#13186=ORIENTED_EDGE('',*,*,#9836,.T.);
#13187=ORIENTED_EDGE('',*,*,#9833,.T.);
#13188=ORIENTED_EDGE('',*,*,#9853,.F.);
#13189=ORIENTED_EDGE('',*,*,#9843,.F.);
#13190=ORIENTED_EDGE('',*,*,#9847,.F.);
#13191=ORIENTED_EDGE('',*,*,#9850,.F.);
#13192=ORIENTED_EDGE('',*,*,#9841,.F.);
#13193=ORIENTED_EDGE('',*,*,#9831,.F.);
#13194=ORIENTED_EDGE('',*,*,#9835,.F.);
#13195=ORIENTED_EDGE('',*,*,#9838,.F.);
#13196=ORIENTED_EDGE('',*,*,#9855,.T.);
#13197=ORIENTED_EDGE('',*,*,#9856,.T.);
#13198=ORIENTED_EDGE('',*,*,#9857,.F.);
#13199=ORIENTED_EDGE('',*,*,#9858,.F.);
#13200=ORIENTED_EDGE('',*,*,#9859,.T.);
#13201=ORIENTED_EDGE('',*,*,#9858,.T.);
#13202=ORIENTED_EDGE('',*,*,#9860,.F.);
#13203=ORIENTED_EDGE('',*,*,#9861,.F.);
#13204=ORIENTED_EDGE('',*,*,#9862,.T.);
#13205=ORIENTED_EDGE('',*,*,#9861,.T.);
#13206=ORIENTED_EDGE('',*,*,#9863,.F.);
#13207=ORIENTED_EDGE('',*,*,#9864,.F.);
#13208=ORIENTED_EDGE('',*,*,#9865,.T.);
#13209=ORIENTED_EDGE('',*,*,#9864,.T.);
#13210=ORIENTED_EDGE('',*,*,#9866,.F.);
#13211=ORIENTED_EDGE('',*,*,#9856,.F.);
#13212=ORIENTED_EDGE('',*,*,#9867,.T.);
#13213=ORIENTED_EDGE('',*,*,#9868,.T.);
#13214=ORIENTED_EDGE('',*,*,#9869,.F.);
#13215=ORIENTED_EDGE('',*,*,#9870,.F.);
#13216=ORIENTED_EDGE('',*,*,#9871,.T.);
#13217=ORIENTED_EDGE('',*,*,#9870,.T.);
#13218=ORIENTED_EDGE('',*,*,#9872,.F.);
#13219=ORIENTED_EDGE('',*,*,#9873,.F.);
#13220=ORIENTED_EDGE('',*,*,#9874,.T.);
#13221=ORIENTED_EDGE('',*,*,#9873,.T.);
#13222=ORIENTED_EDGE('',*,*,#9875,.F.);
#13223=ORIENTED_EDGE('',*,*,#9876,.F.);
#13224=ORIENTED_EDGE('',*,*,#9877,.T.);
#13225=ORIENTED_EDGE('',*,*,#9876,.T.);
#13226=ORIENTED_EDGE('',*,*,#9878,.F.);
#13227=ORIENTED_EDGE('',*,*,#9868,.F.);
#13228=ORIENTED_EDGE('',*,*,#9878,.T.);
#13229=ORIENTED_EDGE('',*,*,#9875,.T.);
#13230=ORIENTED_EDGE('',*,*,#9872,.T.);
#13231=ORIENTED_EDGE('',*,*,#9869,.T.);
#13232=ORIENTED_EDGE('',*,*,#9866,.T.);
#13233=ORIENTED_EDGE('',*,*,#9863,.T.);
#13234=ORIENTED_EDGE('',*,*,#9860,.T.);
#13235=ORIENTED_EDGE('',*,*,#9857,.T.);
#13236=ORIENTED_EDGE('',*,*,#9877,.F.);
#13237=ORIENTED_EDGE('',*,*,#9867,.F.);
#13238=ORIENTED_EDGE('',*,*,#9871,.F.);
#13239=ORIENTED_EDGE('',*,*,#9874,.F.);
#13240=ORIENTED_EDGE('',*,*,#9865,.F.);
#13241=ORIENTED_EDGE('',*,*,#9855,.F.);
#13242=ORIENTED_EDGE('',*,*,#9859,.F.);
#13243=ORIENTED_EDGE('',*,*,#9862,.F.);
#13244=ORIENTED_EDGE('',*,*,#9879,.T.);
#13245=ORIENTED_EDGE('',*,*,#9880,.T.);
#13246=ORIENTED_EDGE('',*,*,#9881,.F.);
#13247=ORIENTED_EDGE('',*,*,#9882,.T.);
#13248=ORIENTED_EDGE('',*,*,#9883,.T.);
#13249=ORIENTED_EDGE('',*,*,#9884,.T.);
#13250=ORIENTED_EDGE('',*,*,#9879,.F.);
#13251=ORIENTED_EDGE('',*,*,#9885,.T.);
#13252=ORIENTED_EDGE('',*,*,#9886,.T.);
#13253=ORIENTED_EDGE('',*,*,#9887,.T.);
#13254=ORIENTED_EDGE('',*,*,#9883,.F.);
#13255=ORIENTED_EDGE('',*,*,#9888,.T.);
#13256=ORIENTED_EDGE('',*,*,#9889,.T.);
#13257=ORIENTED_EDGE('',*,*,#9890,.T.);
#13258=ORIENTED_EDGE('',*,*,#9886,.F.);
#13259=ORIENTED_EDGE('',*,*,#9891,.T.);
#13260=ORIENTED_EDGE('',*,*,#9892,.T.);
#13261=ORIENTED_EDGE('',*,*,#9893,.T.);
#13262=ORIENTED_EDGE('',*,*,#9889,.F.);
#13263=ORIENTED_EDGE('',*,*,#9894,.T.);
#13264=ORIENTED_EDGE('',*,*,#9895,.T.);
#13265=ORIENTED_EDGE('',*,*,#9896,.T.);
#13266=ORIENTED_EDGE('',*,*,#9892,.F.);
#13267=ORIENTED_EDGE('',*,*,#9897,.T.);
#13268=ORIENTED_EDGE('',*,*,#9898,.T.);
#13269=ORIENTED_EDGE('',*,*,#9899,.T.);
#13270=ORIENTED_EDGE('',*,*,#9895,.F.);
#13271=ORIENTED_EDGE('',*,*,#9900,.T.);
#13272=ORIENTED_EDGE('',*,*,#9901,.F.);
#13273=ORIENTED_EDGE('',*,*,#9902,.T.);
#13274=ORIENTED_EDGE('',*,*,#9903,.F.);
#13275=ORIENTED_EDGE('',*,*,#9904,.T.);
#13276=ORIENTED_EDGE('',*,*,#9905,.T.);
#13277=ORIENTED_EDGE('',*,*,#9906,.T.);
#13278=ORIENTED_EDGE('',*,*,#9907,.F.);
#13279=ORIENTED_EDGE('',*,*,#9908,.T.);
#13280=ORIENTED_EDGE('',*,*,#9909,.T.);
#13281=ORIENTED_EDGE('',*,*,#9910,.T.);
#13282=ORIENTED_EDGE('',*,*,#9905,.F.);
#13283=ORIENTED_EDGE('',*,*,#9911,.T.);
#13284=ORIENTED_EDGE('',*,*,#9912,.T.);
#13285=ORIENTED_EDGE('',*,*,#9913,.T.);
#13286=ORIENTED_EDGE('',*,*,#9909,.F.);
#13287=ORIENTED_EDGE('',*,*,#9914,.T.);
#13288=ORIENTED_EDGE('',*,*,#9915,.T.);
#13289=ORIENTED_EDGE('',*,*,#9916,.T.);
#13290=ORIENTED_EDGE('',*,*,#9912,.F.);
#13291=ORIENTED_EDGE('',*,*,#9917,.T.);
#13292=ORIENTED_EDGE('',*,*,#9918,.T.);
#13293=ORIENTED_EDGE('',*,*,#9919,.T.);
#13294=ORIENTED_EDGE('',*,*,#9915,.F.);
#13295=ORIENTED_EDGE('',*,*,#9920,.T.);
#13296=ORIENTED_EDGE('',*,*,#9921,.T.);
#13297=ORIENTED_EDGE('',*,*,#9922,.T.);
#13298=ORIENTED_EDGE('',*,*,#9918,.F.);
#13299=ORIENTED_EDGE('',*,*,#9923,.T.);
#13300=ORIENTED_EDGE('',*,*,#9924,.T.);
#13301=ORIENTED_EDGE('',*,*,#9925,.T.);
#13302=ORIENTED_EDGE('',*,*,#9921,.F.);
#13303=ORIENTED_EDGE('',*,*,#9926,.T.);
#13304=ORIENTED_EDGE('',*,*,#9927,.F.);
#13305=ORIENTED_EDGE('',*,*,#9928,.T.);
#13306=ORIENTED_EDGE('',*,*,#9929,.F.);
#13307=ORIENTED_EDGE('',*,*,#9930,.T.);
#13308=ORIENTED_EDGE('',*,*,#9931,.T.);
#13309=ORIENTED_EDGE('',*,*,#9932,.T.);
#13310=ORIENTED_EDGE('',*,*,#9933,.F.);
#13311=ORIENTED_EDGE('',*,*,#9934,.T.);
#13312=ORIENTED_EDGE('',*,*,#9935,.T.);
#13313=ORIENTED_EDGE('',*,*,#9936,.T.);
#13314=ORIENTED_EDGE('',*,*,#9931,.F.);
#13315=ORIENTED_EDGE('',*,*,#9937,.T.);
#13316=ORIENTED_EDGE('',*,*,#9938,.T.);
#13317=ORIENTED_EDGE('',*,*,#9939,.T.);
#13318=ORIENTED_EDGE('',*,*,#9935,.F.);
#13319=ORIENTED_EDGE('',*,*,#9940,.T.);
#13320=ORIENTED_EDGE('',*,*,#9941,.T.);
#13321=ORIENTED_EDGE('',*,*,#9942,.T.);
#13322=ORIENTED_EDGE('',*,*,#9938,.F.);
#13323=ORIENTED_EDGE('',*,*,#9943,.T.);
#13324=ORIENTED_EDGE('',*,*,#9944,.T.);
#13325=ORIENTED_EDGE('',*,*,#9945,.T.);
#13326=ORIENTED_EDGE('',*,*,#9941,.F.);
#13327=ORIENTED_EDGE('',*,*,#9946,.T.);
#13328=ORIENTED_EDGE('',*,*,#9947,.T.);
#13329=ORIENTED_EDGE('',*,*,#9948,.T.);
#13330=ORIENTED_EDGE('',*,*,#9944,.F.);
#13331=ORIENTED_EDGE('',*,*,#9949,.T.);
#13332=ORIENTED_EDGE('',*,*,#9950,.T.);
#13333=ORIENTED_EDGE('',*,*,#9951,.T.);
#13334=ORIENTED_EDGE('',*,*,#9947,.F.);
#13335=ORIENTED_EDGE('',*,*,#9952,.T.);
#13336=ORIENTED_EDGE('',*,*,#9953,.F.);
#13337=ORIENTED_EDGE('',*,*,#9954,.T.);
#13338=ORIENTED_EDGE('',*,*,#9955,.F.);
#13339=ORIENTED_EDGE('',*,*,#9956,.T.);
#13340=ORIENTED_EDGE('',*,*,#9957,.T.);
#13341=ORIENTED_EDGE('',*,*,#9958,.T.);
#13342=ORIENTED_EDGE('',*,*,#9959,.F.);
#13343=ORIENTED_EDGE('',*,*,#9960,.T.);
#13344=ORIENTED_EDGE('',*,*,#9961,.T.);
#13345=ORIENTED_EDGE('',*,*,#9962,.T.);
#13346=ORIENTED_EDGE('',*,*,#9957,.F.);
#13347=ORIENTED_EDGE('',*,*,#9963,.T.);
#13348=ORIENTED_EDGE('',*,*,#9964,.T.);
#13349=ORIENTED_EDGE('',*,*,#9965,.T.);
#13350=ORIENTED_EDGE('',*,*,#9961,.F.);
#13351=ORIENTED_EDGE('',*,*,#9966,.T.);
#13352=ORIENTED_EDGE('',*,*,#9967,.T.);
#13353=ORIENTED_EDGE('',*,*,#9968,.T.);
#13354=ORIENTED_EDGE('',*,*,#9964,.F.);
#13355=ORIENTED_EDGE('',*,*,#9969,.T.);
#13356=ORIENTED_EDGE('',*,*,#9970,.T.);
#13357=ORIENTED_EDGE('',*,*,#9971,.T.);
#13358=ORIENTED_EDGE('',*,*,#9967,.F.);
#13359=ORIENTED_EDGE('',*,*,#9972,.T.);
#13360=ORIENTED_EDGE('',*,*,#9973,.T.);
#13361=ORIENTED_EDGE('',*,*,#9974,.T.);
#13362=ORIENTED_EDGE('',*,*,#9970,.F.);
#13363=ORIENTED_EDGE('',*,*,#9975,.T.);
#13364=ORIENTED_EDGE('',*,*,#9976,.T.);
#13365=ORIENTED_EDGE('',*,*,#9977,.T.);
#13366=ORIENTED_EDGE('',*,*,#9973,.F.);
#13367=ORIENTED_EDGE('',*,*,#9978,.T.);
#13368=ORIENTED_EDGE('',*,*,#9979,.F.);
#13369=ORIENTED_EDGE('',*,*,#9980,.T.);
#13370=ORIENTED_EDGE('',*,*,#9981,.F.);
#13371=ORIENTED_EDGE('',*,*,#9982,.T.);
#13372=ORIENTED_EDGE('',*,*,#9983,.T.);
#13373=ORIENTED_EDGE('',*,*,#9984,.T.);
#13374=ORIENTED_EDGE('',*,*,#9985,.F.);
#13375=ORIENTED_EDGE('',*,*,#9986,.F.);
#13376=ORIENTED_EDGE('',*,*,#9987,.T.);
#13377=ORIENTED_EDGE('',*,*,#9988,.T.);
#13378=ORIENTED_EDGE('',*,*,#9983,.F.);
#13379=ORIENTED_EDGE('',*,*,#9989,.F.);
#13380=ORIENTED_EDGE('',*,*,#9990,.T.);
#13381=ORIENTED_EDGE('',*,*,#9991,.T.);
#13382=ORIENTED_EDGE('',*,*,#9987,.F.);
#13383=ORIENTED_EDGE('',*,*,#9992,.F.);
#13384=ORIENTED_EDGE('',*,*,#9993,.T.);
#13385=ORIENTED_EDGE('',*,*,#9994,.T.);
#13386=ORIENTED_EDGE('',*,*,#9990,.F.);
#13387=ORIENTED_EDGE('',*,*,#9995,.F.);
#13388=ORIENTED_EDGE('',*,*,#9996,.T.);
#13389=ORIENTED_EDGE('',*,*,#9997,.T.);
#13390=ORIENTED_EDGE('',*,*,#9993,.F.);
#13391=ORIENTED_EDGE('',*,*,#9998,.F.);
#13392=ORIENTED_EDGE('',*,*,#9999,.T.);
#13393=ORIENTED_EDGE('',*,*,#10000,.T.);
#13394=ORIENTED_EDGE('',*,*,#9996,.F.);
#13395=ORIENTED_EDGE('',*,*,#10001,.F.);
#13396=ORIENTED_EDGE('',*,*,#10002,.T.);
#13397=ORIENTED_EDGE('',*,*,#10003,.T.);
#13398=ORIENTED_EDGE('',*,*,#9999,.F.);
#13399=ORIENTED_EDGE('',*,*,#10004,.F.);
#13400=ORIENTED_EDGE('',*,*,#10005,.F.);
#13401=ORIENTED_EDGE('',*,*,#10006,.F.);
#13402=ORIENTED_EDGE('',*,*,#10007,.F.);
#13403=ORIENTED_EDGE('',*,*,#10008,.T.);
#13404=ORIENTED_EDGE('',*,*,#10009,.T.);
#13405=ORIENTED_EDGE('',*,*,#10010,.T.);
#13406=ORIENTED_EDGE('',*,*,#10011,.F.);
#13407=ORIENTED_EDGE('',*,*,#10012,.F.);
#13408=ORIENTED_EDGE('',*,*,#10013,.T.);
#13409=ORIENTED_EDGE('',*,*,#10014,.T.);
#13410=ORIENTED_EDGE('',*,*,#10009,.F.);
#13411=ORIENTED_EDGE('',*,*,#10015,.F.);
#13412=ORIENTED_EDGE('',*,*,#10016,.T.);
#13413=ORIENTED_EDGE('',*,*,#10017,.T.);
#13414=ORIENTED_EDGE('',*,*,#10013,.F.);
#13415=ORIENTED_EDGE('',*,*,#10018,.F.);
#13416=ORIENTED_EDGE('',*,*,#10019,.T.);
#13417=ORIENTED_EDGE('',*,*,#10020,.T.);
#13418=ORIENTED_EDGE('',*,*,#10016,.F.);
#13419=ORIENTED_EDGE('',*,*,#10021,.F.);
#13420=ORIENTED_EDGE('',*,*,#10022,.T.);
#13421=ORIENTED_EDGE('',*,*,#10023,.T.);
#13422=ORIENTED_EDGE('',*,*,#10019,.F.);
#13423=ORIENTED_EDGE('',*,*,#10024,.F.);
#13424=ORIENTED_EDGE('',*,*,#10025,.T.);
#13425=ORIENTED_EDGE('',*,*,#10026,.T.);
#13426=ORIENTED_EDGE('',*,*,#10022,.F.);
#13427=ORIENTED_EDGE('',*,*,#10027,.F.);
#13428=ORIENTED_EDGE('',*,*,#10028,.T.);
#13429=ORIENTED_EDGE('',*,*,#10029,.T.);
#13430=ORIENTED_EDGE('',*,*,#10025,.F.);
#13431=ORIENTED_EDGE('',*,*,#10030,.F.);
#13432=ORIENTED_EDGE('',*,*,#10031,.F.);
#13433=ORIENTED_EDGE('',*,*,#10032,.F.);
#13434=ORIENTED_EDGE('',*,*,#10033,.F.);
#13435=ORIENTED_EDGE('',*,*,#10034,.T.);
#13436=ORIENTED_EDGE('',*,*,#10035,.T.);
#13437=ORIENTED_EDGE('',*,*,#10036,.T.);
#13438=ORIENTED_EDGE('',*,*,#10037,.F.);
#13439=ORIENTED_EDGE('',*,*,#10038,.F.);
#13440=ORIENTED_EDGE('',*,*,#10039,.T.);
#13441=ORIENTED_EDGE('',*,*,#10040,.T.);
#13442=ORIENTED_EDGE('',*,*,#10035,.F.);
#13443=ORIENTED_EDGE('',*,*,#10041,.F.);
#13444=ORIENTED_EDGE('',*,*,#10042,.T.);
#13445=ORIENTED_EDGE('',*,*,#10043,.T.);
#13446=ORIENTED_EDGE('',*,*,#10039,.F.);
#13447=ORIENTED_EDGE('',*,*,#10044,.F.);
#13448=ORIENTED_EDGE('',*,*,#10045,.T.);
#13449=ORIENTED_EDGE('',*,*,#10046,.T.);
#13450=ORIENTED_EDGE('',*,*,#10042,.F.);
#13451=ORIENTED_EDGE('',*,*,#10047,.F.);
#13452=ORIENTED_EDGE('',*,*,#10048,.T.);
#13453=ORIENTED_EDGE('',*,*,#10049,.T.);
#13454=ORIENTED_EDGE('',*,*,#10045,.F.);
#13455=ORIENTED_EDGE('',*,*,#10050,.F.);
#13456=ORIENTED_EDGE('',*,*,#10051,.T.);
#13457=ORIENTED_EDGE('',*,*,#10052,.T.);
#13458=ORIENTED_EDGE('',*,*,#10048,.F.);
#13459=ORIENTED_EDGE('',*,*,#10053,.F.);
#13460=ORIENTED_EDGE('',*,*,#10054,.T.);
#13461=ORIENTED_EDGE('',*,*,#10055,.T.);
#13462=ORIENTED_EDGE('',*,*,#10051,.F.);
#13463=ORIENTED_EDGE('',*,*,#10056,.F.);
#13464=ORIENTED_EDGE('',*,*,#10057,.F.);
#13465=ORIENTED_EDGE('',*,*,#10058,.F.);
#13466=ORIENTED_EDGE('',*,*,#10059,.F.);
#13467=ORIENTED_EDGE('',*,*,#10060,.T.);
#13468=ORIENTED_EDGE('',*,*,#10061,.T.);
#13469=ORIENTED_EDGE('',*,*,#10062,.T.);
#13470=ORIENTED_EDGE('',*,*,#10063,.F.);
#13471=ORIENTED_EDGE('',*,*,#10064,.F.);
#13472=ORIENTED_EDGE('',*,*,#10065,.T.);
#13473=ORIENTED_EDGE('',*,*,#10066,.T.);
#13474=ORIENTED_EDGE('',*,*,#10061,.F.);
#13475=ORIENTED_EDGE('',*,*,#10067,.F.);
#13476=ORIENTED_EDGE('',*,*,#10068,.T.);
#13477=ORIENTED_EDGE('',*,*,#10069,.T.);
#13478=ORIENTED_EDGE('',*,*,#10065,.F.);
#13479=ORIENTED_EDGE('',*,*,#10070,.F.);
#13480=ORIENTED_EDGE('',*,*,#10071,.T.);
#13481=ORIENTED_EDGE('',*,*,#10072,.T.);
#13482=ORIENTED_EDGE('',*,*,#10068,.F.);
#13483=ORIENTED_EDGE('',*,*,#10073,.F.);
#13484=ORIENTED_EDGE('',*,*,#10074,.T.);
#13485=ORIENTED_EDGE('',*,*,#10075,.T.);
#13486=ORIENTED_EDGE('',*,*,#10071,.F.);
#13487=ORIENTED_EDGE('',*,*,#10076,.F.);
#13488=ORIENTED_EDGE('',*,*,#10077,.T.);
#13489=ORIENTED_EDGE('',*,*,#10078,.T.);
#13490=ORIENTED_EDGE('',*,*,#10074,.F.);
#13491=ORIENTED_EDGE('',*,*,#10079,.F.);
#13492=ORIENTED_EDGE('',*,*,#10080,.T.);
#13493=ORIENTED_EDGE('',*,*,#10081,.T.);
#13494=ORIENTED_EDGE('',*,*,#10077,.F.);
#13495=ORIENTED_EDGE('',*,*,#10082,.F.);
#13496=ORIENTED_EDGE('',*,*,#10083,.F.);
#13497=ORIENTED_EDGE('',*,*,#10084,.F.);
#13498=ORIENTED_EDGE('',*,*,#10085,.F.);
#13499=ORIENTED_EDGE('',*,*,#10086,.T.);
#13500=ORIENTED_EDGE('',*,*,#10083,.T.);
#13501=ORIENTED_EDGE('',*,*,#10087,.T.);
#13502=ORIENTED_EDGE('',*,*,#10080,.F.);
#13503=ORIENTED_EDGE('',*,*,#10088,.F.);
#13504=ORIENTED_EDGE('',*,*,#10089,.F.);
#13505=ORIENTED_EDGE('',*,*,#10062,.F.);
#13506=ORIENTED_EDGE('',*,*,#10066,.F.);
#13507=ORIENTED_EDGE('',*,*,#10069,.F.);
#13508=ORIENTED_EDGE('',*,*,#10072,.F.);
#13509=ORIENTED_EDGE('',*,*,#10075,.F.);
#13510=ORIENTED_EDGE('',*,*,#10078,.F.);
#13511=ORIENTED_EDGE('',*,*,#10081,.F.);
#13512=ORIENTED_EDGE('',*,*,#10087,.F.);
#13513=ORIENTED_EDGE('',*,*,#10086,.F.);
#13514=ORIENTED_EDGE('',*,*,#10090,.F.);
#13515=ORIENTED_EDGE('',*,*,#9902,.F.);
#13516=ORIENTED_EDGE('',*,*,#10091,.F.);
#13517=ORIENTED_EDGE('',*,*,#9900,.F.);
#13518=ORIENTED_EDGE('',*,*,#9897,.F.);
#13519=ORIENTED_EDGE('',*,*,#9894,.F.);
#13520=ORIENTED_EDGE('',*,*,#9891,.F.);
#13521=ORIENTED_EDGE('',*,*,#9888,.F.);
#13522=ORIENTED_EDGE('',*,*,#9885,.F.);
#13523=ORIENTED_EDGE('',*,*,#9882,.F.);
#13524=ORIENTED_EDGE('',*,*,#10092,.F.);
#13525=ORIENTED_EDGE('',*,*,#9880,.F.);
#13526=ORIENTED_EDGE('',*,*,#9884,.F.);
#13527=ORIENTED_EDGE('',*,*,#9887,.F.);
#13528=ORIENTED_EDGE('',*,*,#9890,.F.);
#13529=ORIENTED_EDGE('',*,*,#9893,.F.);
#13530=ORIENTED_EDGE('',*,*,#9896,.F.);
#13531=ORIENTED_EDGE('',*,*,#9899,.F.);
#13532=ORIENTED_EDGE('',*,*,#10093,.F.);
#13533=ORIENTED_EDGE('',*,*,#9904,.F.);
#13534=ORIENTED_EDGE('',*,*,#10094,.F.);
#13535=ORIENTED_EDGE('',*,*,#10084,.T.);
#13536=ORIENTED_EDGE('',*,*,#10088,.T.);
#13537=ORIENTED_EDGE('',*,*,#10082,.T.);
#13538=ORIENTED_EDGE('',*,*,#10079,.T.);
#13539=ORIENTED_EDGE('',*,*,#10076,.T.);
#13540=ORIENTED_EDGE('',*,*,#10073,.T.);
#13541=ORIENTED_EDGE('',*,*,#10070,.T.);
#13542=ORIENTED_EDGE('',*,*,#10067,.T.);
#13543=ORIENTED_EDGE('',*,*,#10064,.T.);
#13544=ORIENTED_EDGE('',*,*,#10095,.T.);
#13545=ORIENTED_EDGE('',*,*,#10096,.T.);
#13546=ORIENTED_EDGE('',*,*,#10097,.T.);
#13547=ORIENTED_EDGE('',*,*,#10098,.T.);
#13548=ORIENTED_EDGE('',*,*,#10099,.T.);
#13549=ORIENTED_EDGE('',*,*,#10033,.T.);
#13550=ORIENTED_EDGE('',*,*,#10100,.T.);
#13551=ORIENTED_EDGE('',*,*,#9981,.T.);
#13552=ORIENTED_EDGE('',*,*,#10101,.T.);
#13553=ORIENTED_EDGE('',*,*,#10059,.T.);
#13554=ORIENTED_EDGE('',*,*,#10102,.T.);
#13555=ORIENTED_EDGE('',*,*,#9955,.T.);
#13556=ORIENTED_EDGE('',*,*,#10103,.T.);
#13557=ORIENTED_EDGE('',*,*,#10007,.T.);
#13558=ORIENTED_EDGE('',*,*,#10104,.T.);
#13559=ORIENTED_EDGE('',*,*,#9929,.T.);
#13560=ORIENTED_EDGE('',*,*,#10090,.T.);
#13561=ORIENTED_EDGE('',*,*,#10085,.T.);
#13562=ORIENTED_EDGE('',*,*,#10094,.T.);
#13563=ORIENTED_EDGE('',*,*,#9903,.T.);
#13564=ORIENTED_EDGE('',*,*,#10057,.T.);
#13565=ORIENTED_EDGE('',*,*,#10105,.T.);
#13566=ORIENTED_EDGE('',*,*,#10054,.F.);
#13567=ORIENTED_EDGE('',*,*,#10106,.F.);
#13568=ORIENTED_EDGE('',*,*,#10107,.F.);
#13569=ORIENTED_EDGE('',*,*,#10036,.F.);
#13570=ORIENTED_EDGE('',*,*,#10040,.F.);
#13571=ORIENTED_EDGE('',*,*,#10043,.F.);
#13572=ORIENTED_EDGE('',*,*,#10046,.F.);
#13573=ORIENTED_EDGE('',*,*,#10049,.F.);
#13574=ORIENTED_EDGE('',*,*,#10052,.F.);
#13575=ORIENTED_EDGE('',*,*,#10055,.F.);
#13576=ORIENTED_EDGE('',*,*,#10105,.F.);
#13577=ORIENTED_EDGE('',*,*,#10060,.F.);
#13578=ORIENTED_EDGE('',*,*,#10101,.F.);
#13579=ORIENTED_EDGE('',*,*,#9954,.F.);
#13580=ORIENTED_EDGE('',*,*,#10108,.F.);
#13581=ORIENTED_EDGE('',*,*,#9952,.F.);
#13582=ORIENTED_EDGE('',*,*,#9949,.F.);
#13583=ORIENTED_EDGE('',*,*,#9946,.F.);
#13584=ORIENTED_EDGE('',*,*,#9943,.F.);
#13585=ORIENTED_EDGE('',*,*,#9940,.F.);
#13586=ORIENTED_EDGE('',*,*,#9937,.F.);
#13587=ORIENTED_EDGE('',*,*,#9934,.F.);
#13588=ORIENTED_EDGE('',*,*,#10109,.F.);
#13589=ORIENTED_EDGE('',*,*,#9932,.F.);
#13590=ORIENTED_EDGE('',*,*,#9936,.F.);
#13591=ORIENTED_EDGE('',*,*,#9939,.F.);
#13592=ORIENTED_EDGE('',*,*,#9942,.F.);
#13593=ORIENTED_EDGE('',*,*,#9945,.F.);
#13594=ORIENTED_EDGE('',*,*,#9948,.F.);
#13595=ORIENTED_EDGE('',*,*,#9951,.F.);
#13596=ORIENTED_EDGE('',*,*,#10110,.F.);
#13597=ORIENTED_EDGE('',*,*,#9956,.F.);
#13598=ORIENTED_EDGE('',*,*,#10102,.F.);
#13599=ORIENTED_EDGE('',*,*,#10058,.T.);
#13600=ORIENTED_EDGE('',*,*,#10106,.T.);
#13601=ORIENTED_EDGE('',*,*,#10056,.T.);
#13602=ORIENTED_EDGE('',*,*,#10053,.T.);
#13603=ORIENTED_EDGE('',*,*,#10050,.T.);
#13604=ORIENTED_EDGE('',*,*,#10047,.T.);
#13605=ORIENTED_EDGE('',*,*,#10044,.T.);
#13606=ORIENTED_EDGE('',*,*,#10041,.T.);
#13607=ORIENTED_EDGE('',*,*,#10038,.T.);
#13608=ORIENTED_EDGE('',*,*,#10031,.T.);
#13609=ORIENTED_EDGE('',*,*,#10111,.T.);
#13610=ORIENTED_EDGE('',*,*,#10028,.F.);
#13611=ORIENTED_EDGE('',*,*,#10112,.F.);
#13612=ORIENTED_EDGE('',*,*,#10113,.F.);
#13613=ORIENTED_EDGE('',*,*,#10010,.F.);
#13614=ORIENTED_EDGE('',*,*,#10014,.F.);
#13615=ORIENTED_EDGE('',*,*,#10017,.F.);
#13616=ORIENTED_EDGE('',*,*,#10020,.F.);
#13617=ORIENTED_EDGE('',*,*,#10023,.F.);
#13618=ORIENTED_EDGE('',*,*,#10026,.F.);
#13619=ORIENTED_EDGE('',*,*,#10029,.F.);
#13620=ORIENTED_EDGE('',*,*,#10111,.F.);
#13621=ORIENTED_EDGE('',*,*,#10034,.F.);
#13622=ORIENTED_EDGE('',*,*,#10099,.F.);
#13623=ORIENTED_EDGE('',*,*,#9980,.F.);
#13624=ORIENTED_EDGE('',*,*,#10114,.F.);
#13625=ORIENTED_EDGE('',*,*,#9978,.F.);
#13626=ORIENTED_EDGE('',*,*,#9975,.F.);
#13627=ORIENTED_EDGE('',*,*,#9972,.F.);
#13628=ORIENTED_EDGE('',*,*,#9969,.F.);
#13629=ORIENTED_EDGE('',*,*,#9966,.F.);
#13630=ORIENTED_EDGE('',*,*,#9963,.F.);
#13631=ORIENTED_EDGE('',*,*,#9960,.F.);
#13632=ORIENTED_EDGE('',*,*,#10115,.F.);
#13633=ORIENTED_EDGE('',*,*,#9958,.F.);
#13634=ORIENTED_EDGE('',*,*,#9962,.F.);
#13635=ORIENTED_EDGE('',*,*,#9965,.F.);
#13636=ORIENTED_EDGE('',*,*,#9968,.F.);
#13637=ORIENTED_EDGE('',*,*,#9971,.F.);
#13638=ORIENTED_EDGE('',*,*,#9974,.F.);
#13639=ORIENTED_EDGE('',*,*,#9977,.F.);
#13640=ORIENTED_EDGE('',*,*,#10116,.F.);
#13641=ORIENTED_EDGE('',*,*,#9982,.F.);
#13642=ORIENTED_EDGE('',*,*,#10100,.F.);
#13643=ORIENTED_EDGE('',*,*,#10032,.T.);
#13644=ORIENTED_EDGE('',*,*,#10112,.T.);
#13645=ORIENTED_EDGE('',*,*,#10030,.T.);
#13646=ORIENTED_EDGE('',*,*,#10027,.T.);
#13647=ORIENTED_EDGE('',*,*,#10024,.T.);
#13648=ORIENTED_EDGE('',*,*,#10021,.T.);
#13649=ORIENTED_EDGE('',*,*,#10018,.T.);
#13650=ORIENTED_EDGE('',*,*,#10015,.T.);
#13651=ORIENTED_EDGE('',*,*,#10012,.T.);
#13652=ORIENTED_EDGE('',*,*,#10005,.T.);
#13653=ORIENTED_EDGE('',*,*,#10117,.T.);
#13654=ORIENTED_EDGE('',*,*,#10002,.F.);
#13655=ORIENTED_EDGE('',*,*,#10118,.F.);
#13656=ORIENTED_EDGE('',*,*,#10119,.F.);
#13657=ORIENTED_EDGE('',*,*,#9984,.F.);
#13658=ORIENTED_EDGE('',*,*,#9988,.F.);
#13659=ORIENTED_EDGE('',*,*,#9991,.F.);
#13660=ORIENTED_EDGE('',*,*,#9994,.F.);
#13661=ORIENTED_EDGE('',*,*,#9997,.F.);
#13662=ORIENTED_EDGE('',*,*,#10000,.F.);
#13663=ORIENTED_EDGE('',*,*,#10003,.F.);
#13664=ORIENTED_EDGE('',*,*,#10117,.F.);
#13665=ORIENTED_EDGE('',*,*,#10008,.F.);
#13666=ORIENTED_EDGE('',*,*,#10103,.F.);
#13667=ORIENTED_EDGE('',*,*,#9928,.F.);
#13668=ORIENTED_EDGE('',*,*,#10120,.F.);
#13669=ORIENTED_EDGE('',*,*,#9926,.F.);
#13670=ORIENTED_EDGE('',*,*,#9923,.F.);
#13671=ORIENTED_EDGE('',*,*,#9920,.F.);
#13672=ORIENTED_EDGE('',*,*,#9917,.F.);
#13673=ORIENTED_EDGE('',*,*,#9914,.F.);
#13674=ORIENTED_EDGE('',*,*,#9911,.F.);
#13675=ORIENTED_EDGE('',*,*,#9908,.F.);
#13676=ORIENTED_EDGE('',*,*,#10121,.F.);
#13677=ORIENTED_EDGE('',*,*,#9906,.F.);
#13678=ORIENTED_EDGE('',*,*,#9910,.F.);
#13679=ORIENTED_EDGE('',*,*,#9913,.F.);
#13680=ORIENTED_EDGE('',*,*,#9916,.F.);
#13681=ORIENTED_EDGE('',*,*,#9919,.F.);
#13682=ORIENTED_EDGE('',*,*,#9922,.F.);
#13683=ORIENTED_EDGE('',*,*,#9925,.F.);
#13684=ORIENTED_EDGE('',*,*,#10122,.F.);
#13685=ORIENTED_EDGE('',*,*,#9930,.F.);
#13686=ORIENTED_EDGE('',*,*,#10104,.F.);
#13687=ORIENTED_EDGE('',*,*,#10006,.T.);
#13688=ORIENTED_EDGE('',*,*,#10118,.T.);
#13689=ORIENTED_EDGE('',*,*,#10004,.T.);
#13690=ORIENTED_EDGE('',*,*,#10001,.T.);
#13691=ORIENTED_EDGE('',*,*,#9998,.T.);
#13692=ORIENTED_EDGE('',*,*,#9995,.T.);
#13693=ORIENTED_EDGE('',*,*,#9992,.T.);
#13694=ORIENTED_EDGE('',*,*,#9989,.T.);
#13695=ORIENTED_EDGE('',*,*,#9986,.T.);
#13696=ORIENTED_EDGE('',*,*,#9979,.T.);
#13697=ORIENTED_EDGE('',*,*,#10116,.T.);
#13698=ORIENTED_EDGE('',*,*,#9976,.F.);
#13699=ORIENTED_EDGE('',*,*,#10114,.T.);
#13700=ORIENTED_EDGE('',*,*,#9953,.T.);
#13701=ORIENTED_EDGE('',*,*,#10110,.T.);
#13702=ORIENTED_EDGE('',*,*,#9950,.F.);
#13703=ORIENTED_EDGE('',*,*,#10108,.T.);
#13704=ORIENTED_EDGE('',*,*,#9927,.T.);
#13705=ORIENTED_EDGE('',*,*,#10122,.T.);
#13706=ORIENTED_EDGE('',*,*,#9924,.F.);
#13707=ORIENTED_EDGE('',*,*,#10120,.T.);
#13708=ORIENTED_EDGE('',*,*,#9901,.T.);
#13709=ORIENTED_EDGE('',*,*,#10093,.T.);
#13710=ORIENTED_EDGE('',*,*,#9898,.F.);
#13711=ORIENTED_EDGE('',*,*,#10091,.T.);
#13712=ORIENTED_EDGE('',*,*,#10123,.T.);
#13713=ORIENTED_EDGE('',*,*,#10124,.T.);
#13714=ORIENTED_EDGE('',*,*,#10098,.F.);
#13715=ORIENTED_EDGE('',*,*,#10125,.F.);
#13716=ORIENTED_EDGE('',*,*,#10126,.T.);
#13717=ORIENTED_EDGE('',*,*,#10125,.T.);
#13718=ORIENTED_EDGE('',*,*,#10097,.F.);
#13719=ORIENTED_EDGE('',*,*,#10127,.F.);
#13720=ORIENTED_EDGE('',*,*,#10128,.T.);
#13721=ORIENTED_EDGE('',*,*,#10127,.T.);
#13722=ORIENTED_EDGE('',*,*,#10096,.F.);
#13723=ORIENTED_EDGE('',*,*,#10129,.F.);
#13724=ORIENTED_EDGE('',*,*,#10130,.T.);
#13725=ORIENTED_EDGE('',*,*,#10129,.T.);
#13726=ORIENTED_EDGE('',*,*,#10095,.F.);
#13727=ORIENTED_EDGE('',*,*,#10124,.F.);
#13728=ORIENTED_EDGE('',*,*,#10130,.F.);
#13729=ORIENTED_EDGE('',*,*,#10123,.F.);
#13730=ORIENTED_EDGE('',*,*,#10126,.F.);
#13731=ORIENTED_EDGE('',*,*,#10128,.F.);
#13732=ORIENTED_EDGE('',*,*,#10089,.T.);
#13733=ORIENTED_EDGE('',*,*,#9881,.T.);
#13734=ORIENTED_EDGE('',*,*,#10092,.T.);
#13735=ORIENTED_EDGE('',*,*,#10063,.T.);
#13736=ORIENTED_EDGE('',*,*,#10107,.T.);
#13737=ORIENTED_EDGE('',*,*,#9933,.T.);
#13738=ORIENTED_EDGE('',*,*,#10109,.T.);
#13739=ORIENTED_EDGE('',*,*,#10037,.T.);
#13740=ORIENTED_EDGE('',*,*,#10113,.T.);
#13741=ORIENTED_EDGE('',*,*,#9959,.T.);
#13742=ORIENTED_EDGE('',*,*,#10115,.T.);
#13743=ORIENTED_EDGE('',*,*,#10011,.T.);
#13744=ORIENTED_EDGE('',*,*,#10119,.T.);
#13745=ORIENTED_EDGE('',*,*,#9907,.T.);
#13746=ORIENTED_EDGE('',*,*,#10121,.T.);
#13747=ORIENTED_EDGE('',*,*,#9985,.T.);
#13748=ORIENTED_EDGE('',*,*,#10131,.F.);
#13749=ORIENTED_EDGE('',*,*,#10132,.T.);
#13750=ORIENTED_EDGE('',*,*,#10133,.T.);
#13751=ORIENTED_EDGE('',*,*,#10134,.T.);
#13752=ORIENTED_EDGE('',*,*,#10135,.F.);
#13753=ORIENTED_EDGE('',*,*,#10136,.T.);
#13754=ORIENTED_EDGE('',*,*,#10131,.T.);
#13755=ORIENTED_EDGE('',*,*,#10137,.T.);
#13756=ORIENTED_EDGE('',*,*,#10138,.F.);
#13757=ORIENTED_EDGE('',*,*,#10139,.T.);
#13758=ORIENTED_EDGE('',*,*,#10135,.T.);
#13759=ORIENTED_EDGE('',*,*,#10140,.T.);
#13760=ORIENTED_EDGE('',*,*,#10141,.F.);
#13761=ORIENTED_EDGE('',*,*,#10142,.T.);
#13762=ORIENTED_EDGE('',*,*,#10138,.T.);
#13763=ORIENTED_EDGE('',*,*,#10143,.T.);
#13764=ORIENTED_EDGE('',*,*,#10144,.F.);
#13765=ORIENTED_EDGE('',*,*,#10145,.T.);
#13766=ORIENTED_EDGE('',*,*,#10141,.T.);
#13767=ORIENTED_EDGE('',*,*,#10146,.T.);
#13768=ORIENTED_EDGE('',*,*,#10147,.F.);
#13769=ORIENTED_EDGE('',*,*,#10148,.T.);
#13770=ORIENTED_EDGE('',*,*,#10144,.T.);
#13771=ORIENTED_EDGE('',*,*,#10149,.T.);
#13772=ORIENTED_EDGE('',*,*,#10150,.F.);
#13773=ORIENTED_EDGE('',*,*,#10151,.T.);
#13774=ORIENTED_EDGE('',*,*,#10147,.T.);
#13775=ORIENTED_EDGE('',*,*,#10152,.T.);
#13776=ORIENTED_EDGE('',*,*,#10153,.F.);
#13777=ORIENTED_EDGE('',*,*,#10154,.T.);
#13778=ORIENTED_EDGE('',*,*,#10150,.T.);
#13779=ORIENTED_EDGE('',*,*,#10155,.T.);
#13780=ORIENTED_EDGE('',*,*,#10156,.F.);
#13781=ORIENTED_EDGE('',*,*,#10157,.T.);
#13782=ORIENTED_EDGE('',*,*,#10153,.T.);
#13783=ORIENTED_EDGE('',*,*,#10158,.T.);
#13784=ORIENTED_EDGE('',*,*,#10159,.F.);
#13785=ORIENTED_EDGE('',*,*,#10160,.T.);
#13786=ORIENTED_EDGE('',*,*,#10156,.T.);
#13787=ORIENTED_EDGE('',*,*,#10161,.T.);
#13788=ORIENTED_EDGE('',*,*,#10162,.F.);
#13789=ORIENTED_EDGE('',*,*,#10163,.T.);
#13790=ORIENTED_EDGE('',*,*,#10159,.T.);
#13791=ORIENTED_EDGE('',*,*,#10164,.T.);
#13792=ORIENTED_EDGE('',*,*,#10165,.F.);
#13793=ORIENTED_EDGE('',*,*,#10166,.T.);
#13794=ORIENTED_EDGE('',*,*,#10162,.T.);
#13795=ORIENTED_EDGE('',*,*,#10167,.T.);
#13796=ORIENTED_EDGE('',*,*,#10168,.F.);
#13797=ORIENTED_EDGE('',*,*,#10169,.T.);
#13798=ORIENTED_EDGE('',*,*,#10165,.T.);
#13799=ORIENTED_EDGE('',*,*,#10170,.T.);
#13800=ORIENTED_EDGE('',*,*,#10171,.F.);
#13801=ORIENTED_EDGE('',*,*,#10172,.T.);
#13802=ORIENTED_EDGE('',*,*,#10168,.T.);
#13803=ORIENTED_EDGE('',*,*,#10173,.T.);
#13804=ORIENTED_EDGE('',*,*,#10174,.F.);
#13805=ORIENTED_EDGE('',*,*,#10175,.T.);
#13806=ORIENTED_EDGE('',*,*,#10171,.T.);
#13807=ORIENTED_EDGE('',*,*,#10176,.T.);
#13808=ORIENTED_EDGE('',*,*,#10177,.F.);
#13809=ORIENTED_EDGE('',*,*,#10178,.T.);
#13810=ORIENTED_EDGE('',*,*,#10174,.T.);
#13811=ORIENTED_EDGE('',*,*,#10179,.T.);
#13812=ORIENTED_EDGE('',*,*,#10180,.F.);
#13813=ORIENTED_EDGE('',*,*,#10181,.T.);
#13814=ORIENTED_EDGE('',*,*,#10177,.T.);
#13815=ORIENTED_EDGE('',*,*,#10182,.T.);
#13816=ORIENTED_EDGE('',*,*,#10183,.F.);
#13817=ORIENTED_EDGE('',*,*,#10184,.T.);
#13818=ORIENTED_EDGE('',*,*,#10180,.T.);
#13819=ORIENTED_EDGE('',*,*,#10185,.T.);
#13820=ORIENTED_EDGE('',*,*,#10186,.F.);
#13821=ORIENTED_EDGE('',*,*,#10187,.T.);
#13822=ORIENTED_EDGE('',*,*,#10183,.T.);
#13823=ORIENTED_EDGE('',*,*,#10188,.T.);
#13824=ORIENTED_EDGE('',*,*,#10189,.F.);
#13825=ORIENTED_EDGE('',*,*,#10190,.T.);
#13826=ORIENTED_EDGE('',*,*,#10186,.T.);
#13827=ORIENTED_EDGE('',*,*,#10191,.T.);
#13828=ORIENTED_EDGE('',*,*,#10192,.F.);
#13829=ORIENTED_EDGE('',*,*,#10193,.T.);
#13830=ORIENTED_EDGE('',*,*,#10189,.T.);
#13831=ORIENTED_EDGE('',*,*,#10194,.T.);
#13832=ORIENTED_EDGE('',*,*,#10195,.F.);
#13833=ORIENTED_EDGE('',*,*,#10196,.T.);
#13834=ORIENTED_EDGE('',*,*,#10192,.T.);
#13835=ORIENTED_EDGE('',*,*,#10197,.T.);
#13836=ORIENTED_EDGE('',*,*,#10198,.F.);
#13837=ORIENTED_EDGE('',*,*,#10199,.T.);
#13838=ORIENTED_EDGE('',*,*,#10195,.T.);
#13839=ORIENTED_EDGE('',*,*,#10200,.T.);
#13840=ORIENTED_EDGE('',*,*,#10201,.F.);
#13841=ORIENTED_EDGE('',*,*,#10202,.T.);
#13842=ORIENTED_EDGE('',*,*,#10198,.T.);
#13843=ORIENTED_EDGE('',*,*,#10203,.T.);
#13844=ORIENTED_EDGE('',*,*,#10204,.F.);
#13845=ORIENTED_EDGE('',*,*,#10205,.T.);
#13846=ORIENTED_EDGE('',*,*,#10206,.T.);
#13847=ORIENTED_EDGE('',*,*,#10207,.F.);
#13848=ORIENTED_EDGE('',*,*,#10208,.F.);
#13849=ORIENTED_EDGE('',*,*,#10209,.T.);
#13850=ORIENTED_EDGE('',*,*,#10204,.T.);
#13851=ORIENTED_EDGE('',*,*,#10210,.F.);
#13852=ORIENTED_EDGE('',*,*,#10211,.F.);
#13853=ORIENTED_EDGE('',*,*,#10212,.T.);
#13854=ORIENTED_EDGE('',*,*,#10208,.T.);
#13855=ORIENTED_EDGE('',*,*,#10213,.F.);
#13856=ORIENTED_EDGE('',*,*,#10214,.F.);
#13857=ORIENTED_EDGE('',*,*,#10215,.T.);
#13858=ORIENTED_EDGE('',*,*,#10211,.T.);
#13859=ORIENTED_EDGE('',*,*,#10216,.F.);
#13860=ORIENTED_EDGE('',*,*,#10217,.F.);
#13861=ORIENTED_EDGE('',*,*,#10218,.T.);
#13862=ORIENTED_EDGE('',*,*,#10214,.T.);
#13863=ORIENTED_EDGE('',*,*,#10219,.F.);
#13864=ORIENTED_EDGE('',*,*,#10220,.F.);
#13865=ORIENTED_EDGE('',*,*,#10221,.T.);
#13866=ORIENTED_EDGE('',*,*,#10217,.T.);
#13867=ORIENTED_EDGE('',*,*,#10222,.F.);
#13868=ORIENTED_EDGE('',*,*,#10223,.F.);
#13869=ORIENTED_EDGE('',*,*,#10224,.T.);
#13870=ORIENTED_EDGE('',*,*,#10220,.T.);
#13871=ORIENTED_EDGE('',*,*,#10225,.F.);
#13872=ORIENTED_EDGE('',*,*,#10226,.F.);
#13873=ORIENTED_EDGE('',*,*,#10227,.T.);
#13874=ORIENTED_EDGE('',*,*,#10223,.T.);
#13875=ORIENTED_EDGE('',*,*,#10228,.F.);
#13876=ORIENTED_EDGE('',*,*,#10229,.F.);
#13877=ORIENTED_EDGE('',*,*,#10230,.T.);
#13878=ORIENTED_EDGE('',*,*,#10226,.T.);
#13879=ORIENTED_EDGE('',*,*,#10231,.F.);
#13880=ORIENTED_EDGE('',*,*,#10232,.F.);
#13881=ORIENTED_EDGE('',*,*,#10233,.T.);
#13882=ORIENTED_EDGE('',*,*,#10229,.T.);
#13883=ORIENTED_EDGE('',*,*,#10234,.F.);
#13884=ORIENTED_EDGE('',*,*,#10235,.F.);
#13885=ORIENTED_EDGE('',*,*,#10236,.T.);
#13886=ORIENTED_EDGE('',*,*,#10232,.T.);
#13887=ORIENTED_EDGE('',*,*,#10237,.F.);
#13888=ORIENTED_EDGE('',*,*,#10238,.F.);
#13889=ORIENTED_EDGE('',*,*,#10239,.T.);
#13890=ORIENTED_EDGE('',*,*,#10235,.T.);
#13891=ORIENTED_EDGE('',*,*,#10240,.F.);
#13892=ORIENTED_EDGE('',*,*,#10241,.F.);
#13893=ORIENTED_EDGE('',*,*,#10242,.T.);
#13894=ORIENTED_EDGE('',*,*,#10238,.T.);
#13895=ORIENTED_EDGE('',*,*,#10243,.F.);
#13896=ORIENTED_EDGE('',*,*,#10244,.F.);
#13897=ORIENTED_EDGE('',*,*,#10245,.T.);
#13898=ORIENTED_EDGE('',*,*,#10241,.T.);
#13899=ORIENTED_EDGE('',*,*,#10246,.F.);
#13900=ORIENTED_EDGE('',*,*,#10247,.F.);
#13901=ORIENTED_EDGE('',*,*,#10248,.T.);
#13902=ORIENTED_EDGE('',*,*,#10244,.T.);
#13903=ORIENTED_EDGE('',*,*,#10249,.F.);
#13904=ORIENTED_EDGE('',*,*,#10250,.F.);
#13905=ORIENTED_EDGE('',*,*,#10251,.T.);
#13906=ORIENTED_EDGE('',*,*,#10247,.T.);
#13907=ORIENTED_EDGE('',*,*,#10252,.F.);
#13908=ORIENTED_EDGE('',*,*,#10253,.F.);
#13909=ORIENTED_EDGE('',*,*,#10254,.T.);
#13910=ORIENTED_EDGE('',*,*,#10250,.T.);
#13911=ORIENTED_EDGE('',*,*,#10255,.F.);
#13912=ORIENTED_EDGE('',*,*,#10256,.F.);
#13913=ORIENTED_EDGE('',*,*,#10257,.T.);
#13914=ORIENTED_EDGE('',*,*,#10253,.T.);
#13915=ORIENTED_EDGE('',*,*,#10258,.F.);
#13916=ORIENTED_EDGE('',*,*,#10259,.F.);
#13917=ORIENTED_EDGE('',*,*,#10260,.T.);
#13918=ORIENTED_EDGE('',*,*,#10256,.T.);
#13919=ORIENTED_EDGE('',*,*,#10261,.F.);
#13920=ORIENTED_EDGE('',*,*,#10262,.F.);
#13921=ORIENTED_EDGE('',*,*,#10263,.T.);
#13922=ORIENTED_EDGE('',*,*,#10259,.T.);
#13923=ORIENTED_EDGE('',*,*,#10264,.F.);
#13924=ORIENTED_EDGE('',*,*,#10265,.F.);
#13925=ORIENTED_EDGE('',*,*,#10266,.T.);
#13926=ORIENTED_EDGE('',*,*,#10262,.T.);
#13927=ORIENTED_EDGE('',*,*,#10267,.F.);
#13928=ORIENTED_EDGE('',*,*,#10268,.F.);
#13929=ORIENTED_EDGE('',*,*,#10269,.T.);
#13930=ORIENTED_EDGE('',*,*,#10265,.T.);
#13931=ORIENTED_EDGE('',*,*,#10270,.F.);
#13932=ORIENTED_EDGE('',*,*,#10271,.F.);
#13933=ORIENTED_EDGE('',*,*,#10272,.T.);
#13934=ORIENTED_EDGE('',*,*,#10268,.T.);
#13935=ORIENTED_EDGE('',*,*,#10273,.F.);
#13936=ORIENTED_EDGE('',*,*,#10274,.F.);
#13937=ORIENTED_EDGE('',*,*,#10275,.T.);
#13938=ORIENTED_EDGE('',*,*,#10271,.T.);
#13939=ORIENTED_EDGE('',*,*,#10276,.F.);
#13940=ORIENTED_EDGE('',*,*,#10277,.F.);
#13941=ORIENTED_EDGE('',*,*,#10206,.F.);
#13942=ORIENTED_EDGE('',*,*,#10278,.F.);
#13943=ORIENTED_EDGE('',*,*,#10279,.F.);
#13944=ORIENTED_EDGE('',*,*,#10280,.F.);
#13945=ORIENTED_EDGE('',*,*,#10281,.T.);
#13946=ORIENTED_EDGE('',*,*,#10282,.F.);
#13947=ORIENTED_EDGE('',*,*,#10281,.F.);
#13948=ORIENTED_EDGE('',*,*,#10278,.T.);
#13949=ORIENTED_EDGE('',*,*,#10205,.F.);
#13950=ORIENTED_EDGE('',*,*,#10209,.F.);
#13951=ORIENTED_EDGE('',*,*,#10212,.F.);
#13952=ORIENTED_EDGE('',*,*,#10215,.F.);
#13953=ORIENTED_EDGE('',*,*,#10218,.F.);
#13954=ORIENTED_EDGE('',*,*,#10221,.F.);
#13955=ORIENTED_EDGE('',*,*,#10224,.F.);
#13956=ORIENTED_EDGE('',*,*,#10227,.F.);
#13957=ORIENTED_EDGE('',*,*,#10230,.F.);
#13958=ORIENTED_EDGE('',*,*,#10233,.F.);
#13959=ORIENTED_EDGE('',*,*,#10236,.F.);
#13960=ORIENTED_EDGE('',*,*,#10239,.F.);
#13961=ORIENTED_EDGE('',*,*,#10242,.F.);
#13962=ORIENTED_EDGE('',*,*,#10245,.F.);
#13963=ORIENTED_EDGE('',*,*,#10248,.F.);
#13964=ORIENTED_EDGE('',*,*,#10251,.F.);
#13965=ORIENTED_EDGE('',*,*,#10254,.F.);
#13966=ORIENTED_EDGE('',*,*,#10257,.F.);
#13967=ORIENTED_EDGE('',*,*,#10260,.F.);
#13968=ORIENTED_EDGE('',*,*,#10263,.F.);
#13969=ORIENTED_EDGE('',*,*,#10266,.F.);
#13970=ORIENTED_EDGE('',*,*,#10269,.F.);
#13971=ORIENTED_EDGE('',*,*,#10272,.F.);
#13972=ORIENTED_EDGE('',*,*,#10275,.F.);
#13973=ORIENTED_EDGE('',*,*,#10283,.F.);
#13974=ORIENTED_EDGE('',*,*,#10284,.F.);
#13975=ORIENTED_EDGE('',*,*,#10132,.F.);
#13976=ORIENTED_EDGE('',*,*,#10136,.F.);
#13977=ORIENTED_EDGE('',*,*,#10139,.F.);
#13978=ORIENTED_EDGE('',*,*,#10142,.F.);
#13979=ORIENTED_EDGE('',*,*,#10145,.F.);
#13980=ORIENTED_EDGE('',*,*,#10148,.F.);
#13981=ORIENTED_EDGE('',*,*,#10151,.F.);
#13982=ORIENTED_EDGE('',*,*,#10154,.F.);
#13983=ORIENTED_EDGE('',*,*,#10157,.F.);
#13984=ORIENTED_EDGE('',*,*,#10160,.F.);
#13985=ORIENTED_EDGE('',*,*,#10163,.F.);
#13986=ORIENTED_EDGE('',*,*,#10166,.F.);
#13987=ORIENTED_EDGE('',*,*,#10169,.F.);
#13988=ORIENTED_EDGE('',*,*,#10172,.F.);
#13989=ORIENTED_EDGE('',*,*,#10175,.F.);
#13990=ORIENTED_EDGE('',*,*,#10178,.F.);
#13991=ORIENTED_EDGE('',*,*,#10181,.F.);
#13992=ORIENTED_EDGE('',*,*,#10184,.F.);
#13993=ORIENTED_EDGE('',*,*,#10187,.F.);
#13994=ORIENTED_EDGE('',*,*,#10190,.F.);
#13995=ORIENTED_EDGE('',*,*,#10193,.F.);
#13996=ORIENTED_EDGE('',*,*,#10196,.F.);
#13997=ORIENTED_EDGE('',*,*,#10199,.F.);
#13998=ORIENTED_EDGE('',*,*,#10202,.F.);
#13999=ORIENTED_EDGE('',*,*,#10285,.F.);
#14000=ORIENTED_EDGE('',*,*,#10274,.T.);
#14001=ORIENTED_EDGE('',*,*,#10286,.F.);
#14002=ORIENTED_EDGE('',*,*,#10287,.F.);
#14003=ORIENTED_EDGE('',*,*,#10283,.T.);
#14004=ORIENTED_EDGE('',*,*,#10277,.T.);
#14005=ORIENTED_EDGE('',*,*,#10280,.T.);
#14006=ORIENTED_EDGE('',*,*,#10288,.F.);
#14007=ORIENTED_EDGE('',*,*,#10203,.F.);
#14008=ORIENTED_EDGE('',*,*,#10200,.F.);
#14009=ORIENTED_EDGE('',*,*,#10197,.F.);
#14010=ORIENTED_EDGE('',*,*,#10194,.F.);
#14011=ORIENTED_EDGE('',*,*,#10191,.F.);
#14012=ORIENTED_EDGE('',*,*,#10188,.F.);
#14013=ORIENTED_EDGE('',*,*,#10185,.F.);
#14014=ORIENTED_EDGE('',*,*,#10182,.F.);
#14015=ORIENTED_EDGE('',*,*,#10179,.F.);
#14016=ORIENTED_EDGE('',*,*,#10176,.F.);
#14017=ORIENTED_EDGE('',*,*,#10173,.F.);
#14018=ORIENTED_EDGE('',*,*,#10170,.F.);
#14019=ORIENTED_EDGE('',*,*,#10167,.F.);
#14020=ORIENTED_EDGE('',*,*,#10164,.F.);
#14021=ORIENTED_EDGE('',*,*,#10161,.F.);
#14022=ORIENTED_EDGE('',*,*,#10158,.F.);
#14023=ORIENTED_EDGE('',*,*,#10155,.F.);
#14024=ORIENTED_EDGE('',*,*,#10152,.F.);
#14025=ORIENTED_EDGE('',*,*,#10149,.F.);
#14026=ORIENTED_EDGE('',*,*,#10146,.F.);
#14027=ORIENTED_EDGE('',*,*,#10143,.F.);
#14028=ORIENTED_EDGE('',*,*,#10140,.F.);
#14029=ORIENTED_EDGE('',*,*,#10137,.F.);
#14030=ORIENTED_EDGE('',*,*,#10134,.F.);
#14031=ORIENTED_EDGE('',*,*,#10289,.F.);
#14032=ORIENTED_EDGE('',*,*,#10286,.T.);
#14033=ORIENTED_EDGE('',*,*,#10276,.T.);
#14034=ORIENTED_EDGE('',*,*,#10273,.T.);
#14035=ORIENTED_EDGE('',*,*,#10270,.T.);
#14036=ORIENTED_EDGE('',*,*,#10267,.T.);
#14037=ORIENTED_EDGE('',*,*,#10264,.T.);
#14038=ORIENTED_EDGE('',*,*,#10261,.T.);
#14039=ORIENTED_EDGE('',*,*,#10258,.T.);
#14040=ORIENTED_EDGE('',*,*,#10255,.T.);
#14041=ORIENTED_EDGE('',*,*,#10252,.T.);
#14042=ORIENTED_EDGE('',*,*,#10249,.T.);
#14043=ORIENTED_EDGE('',*,*,#10246,.T.);
#14044=ORIENTED_EDGE('',*,*,#10243,.T.);
#14045=ORIENTED_EDGE('',*,*,#10240,.T.);
#14046=ORIENTED_EDGE('',*,*,#10237,.T.);
#14047=ORIENTED_EDGE('',*,*,#10234,.T.);
#14048=ORIENTED_EDGE('',*,*,#10231,.T.);
#14049=ORIENTED_EDGE('',*,*,#10228,.T.);
#14050=ORIENTED_EDGE('',*,*,#10225,.T.);
#14051=ORIENTED_EDGE('',*,*,#10222,.T.);
#14052=ORIENTED_EDGE('',*,*,#10219,.T.);
#14053=ORIENTED_EDGE('',*,*,#10216,.T.);
#14054=ORIENTED_EDGE('',*,*,#10213,.T.);
#14055=ORIENTED_EDGE('',*,*,#10210,.T.);
#14056=ORIENTED_EDGE('',*,*,#10207,.T.);
#14057=ORIENTED_EDGE('',*,*,#10201,.T.);
#14058=ORIENTED_EDGE('',*,*,#10288,.T.);
#14059=ORIENTED_EDGE('',*,*,#10279,.T.);
#14060=ORIENTED_EDGE('',*,*,#10285,.T.);
#14061=ORIENTED_EDGE('',*,*,#10290,.F.);
#14062=ORIENTED_EDGE('',*,*,#10291,.T.);
#14063=ORIENTED_EDGE('',*,*,#10292,.T.);
#14064=ORIENTED_EDGE('',*,*,#10293,.F.);
#14065=ORIENTED_EDGE('',*,*,#10294,.F.);
#14066=ORIENTED_EDGE('',*,*,#10295,.T.);
#14067=ORIENTED_EDGE('',*,*,#10296,.T.);
#14068=ORIENTED_EDGE('',*,*,#10291,.F.);
#14069=ORIENTED_EDGE('',*,*,#10297,.F.);
#14070=ORIENTED_EDGE('',*,*,#10298,.T.);
#14071=ORIENTED_EDGE('',*,*,#10299,.T.);
#14072=ORIENTED_EDGE('',*,*,#10295,.F.);
#14073=ORIENTED_EDGE('',*,*,#10300,.F.);
#14074=ORIENTED_EDGE('',*,*,#10301,.T.);
#14075=ORIENTED_EDGE('',*,*,#10302,.T.);
#14076=ORIENTED_EDGE('',*,*,#10298,.F.);
#14077=ORIENTED_EDGE('',*,*,#10303,.F.);
#14078=ORIENTED_EDGE('',*,*,#10304,.T.);
#14079=ORIENTED_EDGE('',*,*,#10305,.T.);
#14080=ORIENTED_EDGE('',*,*,#10301,.F.);
#14081=ORIENTED_EDGE('',*,*,#10306,.F.);
#14082=ORIENTED_EDGE('',*,*,#10293,.T.);
#14083=ORIENTED_EDGE('',*,*,#10307,.T.);
#14084=ORIENTED_EDGE('',*,*,#10304,.F.);
#14085=ORIENTED_EDGE('',*,*,#10307,.F.);
#14086=ORIENTED_EDGE('',*,*,#10292,.F.);
#14087=ORIENTED_EDGE('',*,*,#10296,.F.);
#14088=ORIENTED_EDGE('',*,*,#10299,.F.);
#14089=ORIENTED_EDGE('',*,*,#10302,.F.);
#14090=ORIENTED_EDGE('',*,*,#10305,.F.);
#14091=ORIENTED_EDGE('',*,*,#10308,.T.);
#14092=ORIENTED_EDGE('',*,*,#10284,.T.);
#14093=ORIENTED_EDGE('',*,*,#10287,.T.);
#14094=ORIENTED_EDGE('',*,*,#10289,.T.);
#14095=ORIENTED_EDGE('',*,*,#10133,.F.);
#14096=ORIENTED_EDGE('',*,*,#10308,.F.);
#14097=ORIENTED_EDGE('',*,*,#10309,.T.);
#14098=ORIENTED_EDGE('',*,*,#10310,.T.);
#14099=ORIENTED_EDGE('',*,*,#10309,.F.);
#14100=ORIENTED_EDGE('',*,*,#10310,.F.);
#14101=ORIENTED_EDGE('',*,*,#10290,.T.);
#14102=ORIENTED_EDGE('',*,*,#10306,.T.);
#14103=ORIENTED_EDGE('',*,*,#10303,.T.);
#14104=ORIENTED_EDGE('',*,*,#10300,.T.);
#14105=ORIENTED_EDGE('',*,*,#10297,.T.);
#14106=ORIENTED_EDGE('',*,*,#10294,.T.);
#14107=ORIENTED_EDGE('',*,*,#10282,.T.);
#14108=ORIENTED_EDGE('',*,*,#10311,.F.);
#14109=ORIENTED_EDGE('',*,*,#10312,.T.);
#14110=ORIENTED_EDGE('',*,*,#10313,.T.);
#14111=ORIENTED_EDGE('',*,*,#10312,.F.);
#14112=ORIENTED_EDGE('',*,*,#10314,.F.);
#14113=ORIENTED_EDGE('',*,*,#10315,.T.);
#14114=ORIENTED_EDGE('',*,*,#10316,.T.);
#14115=ORIENTED_EDGE('',*,*,#10315,.F.);
#14116=ORIENTED_EDGE('',*,*,#10314,.T.);
#14117=ORIENTED_EDGE('',*,*,#10311,.T.);
#14118=ORIENTED_EDGE('',*,*,#10316,.F.);
#14119=ORIENTED_EDGE('',*,*,#10313,.F.);
#14120=ORIENTED_EDGE('',*,*,#10317,.T.);
#14121=ORIENTED_EDGE('',*,*,#10318,.T.);
#14122=ORIENTED_EDGE('',*,*,#10319,.T.);
#14123=ORIENTED_EDGE('',*,*,#10320,.T.);
#14124=ORIENTED_EDGE('',*,*,#10321,.T.);
#14125=ORIENTED_EDGE('',*,*,#10320,.F.);
#14126=ORIENTED_EDGE('',*,*,#10322,.T.);
#14127=ORIENTED_EDGE('',*,*,#10323,.T.);
#14128=ORIENTED_EDGE('',*,*,#10324,.T.);
#14129=ORIENTED_EDGE('',*,*,#10325,.T.);
#14130=ORIENTED_EDGE('',*,*,#10317,.F.);
#14131=ORIENTED_EDGE('',*,*,#10326,.T.);
#14132=ORIENTED_EDGE('',*,*,#10327,.T.);
#14133=ORIENTED_EDGE('',*,*,#10328,.T.);
#14134=ORIENTED_EDGE('',*,*,#10324,.F.);
#14135=ORIENTED_EDGE('',*,*,#10329,.T.);
#14136=ORIENTED_EDGE('',*,*,#10330,.T.);
#14137=ORIENTED_EDGE('',*,*,#10331,.T.);
#14138=ORIENTED_EDGE('',*,*,#10327,.F.);
#14139=ORIENTED_EDGE('',*,*,#10332,.T.);
#14140=ORIENTED_EDGE('',*,*,#10333,.T.);
#14141=ORIENTED_EDGE('',*,*,#10334,.T.);
#14142=ORIENTED_EDGE('',*,*,#10330,.F.);
#14143=ORIENTED_EDGE('',*,*,#10335,.T.);
#14144=ORIENTED_EDGE('',*,*,#10336,.T.);
#14145=ORIENTED_EDGE('',*,*,#10337,.T.);
#14146=ORIENTED_EDGE('',*,*,#10333,.F.);
#14147=ORIENTED_EDGE('',*,*,#10338,.T.);
#14148=ORIENTED_EDGE('',*,*,#10339,.T.);
#14149=ORIENTED_EDGE('',*,*,#10340,.T.);
#14150=ORIENTED_EDGE('',*,*,#10336,.F.);
#14151=ORIENTED_EDGE('',*,*,#10341,.T.);
#14152=ORIENTED_EDGE('',*,*,#10342,.T.);
#14153=ORIENTED_EDGE('',*,*,#10343,.T.);
#14154=ORIENTED_EDGE('',*,*,#10339,.F.);
#14155=ORIENTED_EDGE('',*,*,#10344,.T.);
#14156=ORIENTED_EDGE('',*,*,#10345,.T.);
#14157=ORIENTED_EDGE('',*,*,#10346,.T.);
#14158=ORIENTED_EDGE('',*,*,#10342,.F.);
#14159=ORIENTED_EDGE('',*,*,#10347,.T.);
#14160=ORIENTED_EDGE('',*,*,#10348,.T.);
#14161=ORIENTED_EDGE('',*,*,#10349,.T.);
#14162=ORIENTED_EDGE('',*,*,#10345,.F.);
#14163=ORIENTED_EDGE('',*,*,#10350,.T.);
#14164=ORIENTED_EDGE('',*,*,#10351,.T.);
#14165=ORIENTED_EDGE('',*,*,#10352,.T.);
#14166=ORIENTED_EDGE('',*,*,#10348,.F.);
#14167=ORIENTED_EDGE('',*,*,#10353,.T.);
#14168=ORIENTED_EDGE('',*,*,#10354,.T.);
#14169=ORIENTED_EDGE('',*,*,#10355,.T.);
#14170=ORIENTED_EDGE('',*,*,#10351,.F.);
#14171=ORIENTED_EDGE('',*,*,#10356,.T.);
#14172=ORIENTED_EDGE('',*,*,#10357,.T.);
#14173=ORIENTED_EDGE('',*,*,#10358,.T.);
#14174=ORIENTED_EDGE('',*,*,#10354,.F.);
#14175=ORIENTED_EDGE('',*,*,#10359,.T.);
#14176=ORIENTED_EDGE('',*,*,#10360,.T.);
#14177=ORIENTED_EDGE('',*,*,#10361,.T.);
#14178=ORIENTED_EDGE('',*,*,#10357,.F.);
#14179=ORIENTED_EDGE('',*,*,#10362,.T.);
#14180=ORIENTED_EDGE('',*,*,#10363,.T.);
#14181=ORIENTED_EDGE('',*,*,#10364,.T.);
#14182=ORIENTED_EDGE('',*,*,#10360,.F.);
#14183=ORIENTED_EDGE('',*,*,#10365,.T.);
#14184=ORIENTED_EDGE('',*,*,#10366,.T.);
#14185=ORIENTED_EDGE('',*,*,#10367,.T.);
#14186=ORIENTED_EDGE('',*,*,#10363,.F.);
#14187=ORIENTED_EDGE('',*,*,#10368,.T.);
#14188=ORIENTED_EDGE('',*,*,#10369,.T.);
#14189=ORIENTED_EDGE('',*,*,#10370,.T.);
#14190=ORIENTED_EDGE('',*,*,#10366,.F.);
#14191=ORIENTED_EDGE('',*,*,#10371,.T.);
#14192=ORIENTED_EDGE('',*,*,#10372,.T.);
#14193=ORIENTED_EDGE('',*,*,#10373,.T.);
#14194=ORIENTED_EDGE('',*,*,#10369,.F.);
#14195=ORIENTED_EDGE('',*,*,#10374,.T.);
#14196=ORIENTED_EDGE('',*,*,#10375,.T.);
#14197=ORIENTED_EDGE('',*,*,#10376,.T.);
#14198=ORIENTED_EDGE('',*,*,#10372,.F.);
#14199=ORIENTED_EDGE('',*,*,#10377,.T.);
#14200=ORIENTED_EDGE('',*,*,#10378,.T.);
#14201=ORIENTED_EDGE('',*,*,#10379,.T.);
#14202=ORIENTED_EDGE('',*,*,#10375,.F.);
#14203=ORIENTED_EDGE('',*,*,#10380,.T.);
#14204=ORIENTED_EDGE('',*,*,#10381,.T.);
#14205=ORIENTED_EDGE('',*,*,#10382,.T.);
#14206=ORIENTED_EDGE('',*,*,#10378,.F.);
#14207=ORIENTED_EDGE('',*,*,#10383,.T.);
#14208=ORIENTED_EDGE('',*,*,#10384,.T.);
#14209=ORIENTED_EDGE('',*,*,#10385,.T.);
#14210=ORIENTED_EDGE('',*,*,#10381,.F.);
#14211=ORIENTED_EDGE('',*,*,#10386,.T.);
#14212=ORIENTED_EDGE('',*,*,#10387,.T.);
#14213=ORIENTED_EDGE('',*,*,#10388,.T.);
#14214=ORIENTED_EDGE('',*,*,#10384,.F.);
#14215=ORIENTED_EDGE('',*,*,#10389,.T.);
#14216=ORIENTED_EDGE('',*,*,#10390,.T.);
#14217=ORIENTED_EDGE('',*,*,#10391,.T.);
#14218=ORIENTED_EDGE('',*,*,#10387,.F.);
#14219=ORIENTED_EDGE('',*,*,#10392,.T.);
#14220=ORIENTED_EDGE('',*,*,#10393,.F.);
#14221=ORIENTED_EDGE('',*,*,#10394,.T.);
#14222=ORIENTED_EDGE('',*,*,#10395,.F.);
#14223=ORIENTED_EDGE('',*,*,#10396,.T.);
#14224=ORIENTED_EDGE('',*,*,#10397,.T.);
#14225=ORIENTED_EDGE('',*,*,#10398,.T.);
#14226=ORIENTED_EDGE('',*,*,#10399,.F.);
#14227=ORIENTED_EDGE('',*,*,#10400,.F.);
#14228=ORIENTED_EDGE('',*,*,#10401,.T.);
#14229=ORIENTED_EDGE('',*,*,#10402,.T.);
#14230=ORIENTED_EDGE('',*,*,#10397,.F.);
#14231=ORIENTED_EDGE('',*,*,#10403,.F.);
#14232=ORIENTED_EDGE('',*,*,#10404,.T.);
#14233=ORIENTED_EDGE('',*,*,#10405,.T.);
#14234=ORIENTED_EDGE('',*,*,#10401,.F.);
#14235=ORIENTED_EDGE('',*,*,#10406,.F.);
#14236=ORIENTED_EDGE('',*,*,#10407,.T.);
#14237=ORIENTED_EDGE('',*,*,#10408,.T.);
#14238=ORIENTED_EDGE('',*,*,#10404,.F.);
#14239=ORIENTED_EDGE('',*,*,#10409,.F.);
#14240=ORIENTED_EDGE('',*,*,#10410,.T.);
#14241=ORIENTED_EDGE('',*,*,#10411,.T.);
#14242=ORIENTED_EDGE('',*,*,#10407,.F.);
#14243=ORIENTED_EDGE('',*,*,#10412,.F.);
#14244=ORIENTED_EDGE('',*,*,#10413,.T.);
#14245=ORIENTED_EDGE('',*,*,#10414,.T.);
#14246=ORIENTED_EDGE('',*,*,#10410,.F.);
#14247=ORIENTED_EDGE('',*,*,#10415,.F.);
#14248=ORIENTED_EDGE('',*,*,#10416,.T.);
#14249=ORIENTED_EDGE('',*,*,#10417,.T.);
#14250=ORIENTED_EDGE('',*,*,#10413,.F.);
#14251=ORIENTED_EDGE('',*,*,#10418,.F.);
#14252=ORIENTED_EDGE('',*,*,#10419,.T.);
#14253=ORIENTED_EDGE('',*,*,#10420,.T.);
#14254=ORIENTED_EDGE('',*,*,#10416,.F.);
#14255=ORIENTED_EDGE('',*,*,#10421,.F.);
#14256=ORIENTED_EDGE('',*,*,#10422,.T.);
#14257=ORIENTED_EDGE('',*,*,#10423,.T.);
#14258=ORIENTED_EDGE('',*,*,#10419,.F.);
#14259=ORIENTED_EDGE('',*,*,#10424,.F.);
#14260=ORIENTED_EDGE('',*,*,#10425,.T.);
#14261=ORIENTED_EDGE('',*,*,#10426,.T.);
#14262=ORIENTED_EDGE('',*,*,#10422,.F.);
#14263=ORIENTED_EDGE('',*,*,#10427,.F.);
#14264=ORIENTED_EDGE('',*,*,#10428,.T.);
#14265=ORIENTED_EDGE('',*,*,#10429,.T.);
#14266=ORIENTED_EDGE('',*,*,#10425,.F.);
#14267=ORIENTED_EDGE('',*,*,#10430,.F.);
#14268=ORIENTED_EDGE('',*,*,#10431,.T.);
#14269=ORIENTED_EDGE('',*,*,#10432,.T.);
#14270=ORIENTED_EDGE('',*,*,#10428,.F.);
#14271=ORIENTED_EDGE('',*,*,#10433,.F.);
#14272=ORIENTED_EDGE('',*,*,#10434,.T.);
#14273=ORIENTED_EDGE('',*,*,#10435,.T.);
#14274=ORIENTED_EDGE('',*,*,#10431,.F.);
#14275=ORIENTED_EDGE('',*,*,#10436,.F.);
#14276=ORIENTED_EDGE('',*,*,#10437,.T.);
#14277=ORIENTED_EDGE('',*,*,#10438,.T.);
#14278=ORIENTED_EDGE('',*,*,#10434,.F.);
#14279=ORIENTED_EDGE('',*,*,#10439,.F.);
#14280=ORIENTED_EDGE('',*,*,#10440,.T.);
#14281=ORIENTED_EDGE('',*,*,#10441,.T.);
#14282=ORIENTED_EDGE('',*,*,#10437,.F.);
#14283=ORIENTED_EDGE('',*,*,#10442,.F.);
#14284=ORIENTED_EDGE('',*,*,#10443,.T.);
#14285=ORIENTED_EDGE('',*,*,#10444,.T.);
#14286=ORIENTED_EDGE('',*,*,#10440,.F.);
#14287=ORIENTED_EDGE('',*,*,#10445,.F.);
#14288=ORIENTED_EDGE('',*,*,#10446,.T.);
#14289=ORIENTED_EDGE('',*,*,#10447,.T.);
#14290=ORIENTED_EDGE('',*,*,#10443,.F.);
#14291=ORIENTED_EDGE('',*,*,#10448,.F.);
#14292=ORIENTED_EDGE('',*,*,#10449,.T.);
#14293=ORIENTED_EDGE('',*,*,#10450,.T.);
#14294=ORIENTED_EDGE('',*,*,#10446,.F.);
#14295=ORIENTED_EDGE('',*,*,#10451,.F.);
#14296=ORIENTED_EDGE('',*,*,#10452,.T.);
#14297=ORIENTED_EDGE('',*,*,#10453,.T.);
#14298=ORIENTED_EDGE('',*,*,#10449,.F.);
#14299=ORIENTED_EDGE('',*,*,#10454,.F.);
#14300=ORIENTED_EDGE('',*,*,#10455,.T.);
#14301=ORIENTED_EDGE('',*,*,#10456,.T.);
#14302=ORIENTED_EDGE('',*,*,#10452,.F.);
#14303=ORIENTED_EDGE('',*,*,#10457,.F.);
#14304=ORIENTED_EDGE('',*,*,#10458,.T.);
#14305=ORIENTED_EDGE('',*,*,#10459,.T.);
#14306=ORIENTED_EDGE('',*,*,#10455,.F.);
#14307=ORIENTED_EDGE('',*,*,#10460,.F.);
#14308=ORIENTED_EDGE('',*,*,#10461,.T.);
#14309=ORIENTED_EDGE('',*,*,#10462,.T.);
#14310=ORIENTED_EDGE('',*,*,#10458,.F.);
#14311=ORIENTED_EDGE('',*,*,#10463,.F.);
#14312=ORIENTED_EDGE('',*,*,#10464,.T.);
#14313=ORIENTED_EDGE('',*,*,#10465,.T.);
#14314=ORIENTED_EDGE('',*,*,#10461,.F.);
#14315=ORIENTED_EDGE('',*,*,#10466,.F.);
#14316=ORIENTED_EDGE('',*,*,#10467,.T.);
#14317=ORIENTED_EDGE('',*,*,#10468,.T.);
#14318=ORIENTED_EDGE('',*,*,#10464,.F.);
#14319=ORIENTED_EDGE('',*,*,#10469,.F.);
#14320=ORIENTED_EDGE('',*,*,#10470,.F.);
#14321=ORIENTED_EDGE('',*,*,#10471,.F.);
#14322=ORIENTED_EDGE('',*,*,#10472,.F.);
#14323=ORIENTED_EDGE('',*,*,#10473,.T.);
#14324=ORIENTED_EDGE('',*,*,#10474,.T.);
#14325=ORIENTED_EDGE('',*,*,#10475,.T.);
#14326=ORIENTED_EDGE('',*,*,#10476,.T.);
#14327=ORIENTED_EDGE('',*,*,#10477,.T.);
#14328=ORIENTED_EDGE('',*,*,#10478,.T.);
#14329=ORIENTED_EDGE('',*,*,#10477,.F.);
#14330=ORIENTED_EDGE('',*,*,#10479,.T.);
#14331=ORIENTED_EDGE('',*,*,#10480,.T.);
#14332=ORIENTED_EDGE('',*,*,#10481,.T.);
#14333=ORIENTED_EDGE('',*,*,#10482,.T.);
#14334=ORIENTED_EDGE('',*,*,#10474,.F.);
#14335=ORIENTED_EDGE('',*,*,#10483,.T.);
#14336=ORIENTED_EDGE('',*,*,#10484,.T.);
#14337=ORIENTED_EDGE('',*,*,#10485,.T.);
#14338=ORIENTED_EDGE('',*,*,#10481,.F.);
#14339=ORIENTED_EDGE('',*,*,#10486,.T.);
#14340=ORIENTED_EDGE('',*,*,#10487,.T.);
#14341=ORIENTED_EDGE('',*,*,#10488,.T.);
#14342=ORIENTED_EDGE('',*,*,#10484,.F.);
#14343=ORIENTED_EDGE('',*,*,#10489,.T.);
#14344=ORIENTED_EDGE('',*,*,#10490,.T.);
#14345=ORIENTED_EDGE('',*,*,#10491,.T.);
#14346=ORIENTED_EDGE('',*,*,#10487,.F.);
#14347=ORIENTED_EDGE('',*,*,#10492,.T.);
#14348=ORIENTED_EDGE('',*,*,#10493,.T.);
#14349=ORIENTED_EDGE('',*,*,#10494,.T.);
#14350=ORIENTED_EDGE('',*,*,#10490,.F.);
#14351=ORIENTED_EDGE('',*,*,#10495,.T.);
#14352=ORIENTED_EDGE('',*,*,#10496,.T.);
#14353=ORIENTED_EDGE('',*,*,#10497,.T.);
#14354=ORIENTED_EDGE('',*,*,#10493,.F.);
#14355=ORIENTED_EDGE('',*,*,#10498,.T.);
#14356=ORIENTED_EDGE('',*,*,#10499,.T.);
#14357=ORIENTED_EDGE('',*,*,#10500,.T.);
#14358=ORIENTED_EDGE('',*,*,#10496,.F.);
#14359=ORIENTED_EDGE('',*,*,#10501,.T.);
#14360=ORIENTED_EDGE('',*,*,#10502,.T.);
#14361=ORIENTED_EDGE('',*,*,#10503,.T.);
#14362=ORIENTED_EDGE('',*,*,#10499,.F.);
#14363=ORIENTED_EDGE('',*,*,#10504,.T.);
#14364=ORIENTED_EDGE('',*,*,#10505,.T.);
#14365=ORIENTED_EDGE('',*,*,#10506,.T.);
#14366=ORIENTED_EDGE('',*,*,#10502,.F.);
#14367=ORIENTED_EDGE('',*,*,#10507,.T.);
#14368=ORIENTED_EDGE('',*,*,#10508,.T.);
#14369=ORIENTED_EDGE('',*,*,#10509,.T.);
#14370=ORIENTED_EDGE('',*,*,#10505,.F.);
#14371=ORIENTED_EDGE('',*,*,#10510,.T.);
#14372=ORIENTED_EDGE('',*,*,#10511,.T.);
#14373=ORIENTED_EDGE('',*,*,#10512,.T.);
#14374=ORIENTED_EDGE('',*,*,#10508,.F.);
#14375=ORIENTED_EDGE('',*,*,#10513,.T.);
#14376=ORIENTED_EDGE('',*,*,#10514,.T.);
#14377=ORIENTED_EDGE('',*,*,#10515,.T.);
#14378=ORIENTED_EDGE('',*,*,#10511,.F.);
#14379=ORIENTED_EDGE('',*,*,#10516,.T.);
#14380=ORIENTED_EDGE('',*,*,#10517,.T.);
#14381=ORIENTED_EDGE('',*,*,#10518,.T.);
#14382=ORIENTED_EDGE('',*,*,#10514,.F.);
#14383=ORIENTED_EDGE('',*,*,#10519,.T.);
#14384=ORIENTED_EDGE('',*,*,#10520,.T.);
#14385=ORIENTED_EDGE('',*,*,#10521,.T.);
#14386=ORIENTED_EDGE('',*,*,#10517,.F.);
#14387=ORIENTED_EDGE('',*,*,#10522,.T.);
#14388=ORIENTED_EDGE('',*,*,#10523,.T.);
#14389=ORIENTED_EDGE('',*,*,#10524,.T.);
#14390=ORIENTED_EDGE('',*,*,#10520,.F.);
#14391=ORIENTED_EDGE('',*,*,#10525,.T.);
#14392=ORIENTED_EDGE('',*,*,#10526,.T.);
#14393=ORIENTED_EDGE('',*,*,#10527,.T.);
#14394=ORIENTED_EDGE('',*,*,#10523,.F.);
#14395=ORIENTED_EDGE('',*,*,#10528,.T.);
#14396=ORIENTED_EDGE('',*,*,#10529,.T.);
#14397=ORIENTED_EDGE('',*,*,#10530,.T.);
#14398=ORIENTED_EDGE('',*,*,#10526,.F.);
#14399=ORIENTED_EDGE('',*,*,#10531,.T.);
#14400=ORIENTED_EDGE('',*,*,#10532,.T.);
#14401=ORIENTED_EDGE('',*,*,#10533,.T.);
#14402=ORIENTED_EDGE('',*,*,#10529,.F.);
#14403=ORIENTED_EDGE('',*,*,#10534,.T.);
#14404=ORIENTED_EDGE('',*,*,#10535,.T.);
#14405=ORIENTED_EDGE('',*,*,#10536,.T.);
#14406=ORIENTED_EDGE('',*,*,#10532,.F.);
#14407=ORIENTED_EDGE('',*,*,#10537,.T.);
#14408=ORIENTED_EDGE('',*,*,#10538,.T.);
#14409=ORIENTED_EDGE('',*,*,#10539,.T.);
#14410=ORIENTED_EDGE('',*,*,#10535,.F.);
#14411=ORIENTED_EDGE('',*,*,#10540,.T.);
#14412=ORIENTED_EDGE('',*,*,#10541,.T.);
#14413=ORIENTED_EDGE('',*,*,#10542,.T.);
#14414=ORIENTED_EDGE('',*,*,#10538,.F.);
#14415=ORIENTED_EDGE('',*,*,#10543,.T.);
#14416=ORIENTED_EDGE('',*,*,#10544,.T.);
#14417=ORIENTED_EDGE('',*,*,#10545,.T.);
#14418=ORIENTED_EDGE('',*,*,#10541,.F.);
#14419=ORIENTED_EDGE('',*,*,#10546,.T.);
#14420=ORIENTED_EDGE('',*,*,#10547,.T.);
#14421=ORIENTED_EDGE('',*,*,#10548,.T.);
#14422=ORIENTED_EDGE('',*,*,#10544,.F.);
#14423=ORIENTED_EDGE('',*,*,#10549,.T.);
#14424=ORIENTED_EDGE('',*,*,#10550,.T.);
#14425=ORIENTED_EDGE('',*,*,#10551,.T.);
#14426=ORIENTED_EDGE('',*,*,#10547,.F.);
#14427=ORIENTED_EDGE('',*,*,#10552,.T.);
#14428=ORIENTED_EDGE('',*,*,#10553,.T.);
#14429=ORIENTED_EDGE('',*,*,#10554,.T.);
#14430=ORIENTED_EDGE('',*,*,#10550,.F.);
#14431=ORIENTED_EDGE('',*,*,#10555,.T.);
#14432=ORIENTED_EDGE('',*,*,#10556,.T.);
#14433=ORIENTED_EDGE('',*,*,#10557,.T.);
#14434=ORIENTED_EDGE('',*,*,#10553,.F.);
#14435=ORIENTED_EDGE('',*,*,#10558,.T.);
#14436=ORIENTED_EDGE('',*,*,#10559,.T.);
#14437=ORIENTED_EDGE('',*,*,#10560,.T.);
#14438=ORIENTED_EDGE('',*,*,#10556,.F.);
#14439=ORIENTED_EDGE('',*,*,#10561,.T.);
#14440=ORIENTED_EDGE('',*,*,#10562,.T.);
#14441=ORIENTED_EDGE('',*,*,#10563,.T.);
#14442=ORIENTED_EDGE('',*,*,#10559,.F.);
#14443=ORIENTED_EDGE('',*,*,#10564,.T.);
#14444=ORIENTED_EDGE('',*,*,#10565,.T.);
#14445=ORIENTED_EDGE('',*,*,#10566,.T.);
#14446=ORIENTED_EDGE('',*,*,#10562,.F.);
#14447=ORIENTED_EDGE('',*,*,#10567,.T.);
#14448=ORIENTED_EDGE('',*,*,#10568,.T.);
#14449=ORIENTED_EDGE('',*,*,#10569,.T.);
#14450=ORIENTED_EDGE('',*,*,#10565,.F.);
#14451=ORIENTED_EDGE('',*,*,#10570,.T.);
#14452=ORIENTED_EDGE('',*,*,#10571,.T.);
#14453=ORIENTED_EDGE('',*,*,#10572,.T.);
#14454=ORIENTED_EDGE('',*,*,#10568,.F.);
#14455=ORIENTED_EDGE('',*,*,#10573,.T.);
#14456=ORIENTED_EDGE('',*,*,#10574,.T.);
#14457=ORIENTED_EDGE('',*,*,#10575,.T.);
#14458=ORIENTED_EDGE('',*,*,#10571,.F.);
#14459=ORIENTED_EDGE('',*,*,#10576,.T.);
#14460=ORIENTED_EDGE('',*,*,#10577,.T.);
#14461=ORIENTED_EDGE('',*,*,#10578,.T.);
#14462=ORIENTED_EDGE('',*,*,#10574,.F.);
#14463=ORIENTED_EDGE('',*,*,#10579,.T.);
#14464=ORIENTED_EDGE('',*,*,#10580,.T.);
#14465=ORIENTED_EDGE('',*,*,#10581,.T.);
#14466=ORIENTED_EDGE('',*,*,#10577,.F.);
#14467=ORIENTED_EDGE('',*,*,#10582,.T.);
#14468=ORIENTED_EDGE('',*,*,#10583,.T.);
#14469=ORIENTED_EDGE('',*,*,#10584,.T.);
#14470=ORIENTED_EDGE('',*,*,#10580,.F.);
#14471=ORIENTED_EDGE('',*,*,#10585,.T.);
#14472=ORIENTED_EDGE('',*,*,#10586,.T.);
#14473=ORIENTED_EDGE('',*,*,#10587,.T.);
#14474=ORIENTED_EDGE('',*,*,#10583,.F.);
#14475=ORIENTED_EDGE('',*,*,#10588,.T.);
#14476=ORIENTED_EDGE('',*,*,#10589,.T.);
#14477=ORIENTED_EDGE('',*,*,#10590,.T.);
#14478=ORIENTED_EDGE('',*,*,#10586,.F.);
#14479=ORIENTED_EDGE('',*,*,#10591,.T.);
#14480=ORIENTED_EDGE('',*,*,#10592,.T.);
#14481=ORIENTED_EDGE('',*,*,#10593,.T.);
#14482=ORIENTED_EDGE('',*,*,#10589,.F.);
#14483=ORIENTED_EDGE('',*,*,#10594,.T.);
#14484=ORIENTED_EDGE('',*,*,#10595,.F.);
#14485=ORIENTED_EDGE('',*,*,#10596,.T.);
#14486=ORIENTED_EDGE('',*,*,#10597,.F.);
#14487=ORIENTED_EDGE('',*,*,#10598,.T.);
#14488=ORIENTED_EDGE('',*,*,#10599,.T.);
#14489=ORIENTED_EDGE('',*,*,#10600,.T.);
#14490=ORIENTED_EDGE('',*,*,#10601,.F.);
#14491=ORIENTED_EDGE('',*,*,#10602,.F.);
#14492=ORIENTED_EDGE('',*,*,#10603,.T.);
#14493=ORIENTED_EDGE('',*,*,#10604,.T.);
#14494=ORIENTED_EDGE('',*,*,#10599,.F.);
#14495=ORIENTED_EDGE('',*,*,#10605,.F.);
#14496=ORIENTED_EDGE('',*,*,#10606,.T.);
#14497=ORIENTED_EDGE('',*,*,#10607,.T.);
#14498=ORIENTED_EDGE('',*,*,#10603,.F.);
#14499=ORIENTED_EDGE('',*,*,#10608,.F.);
#14500=ORIENTED_EDGE('',*,*,#10609,.T.);
#14501=ORIENTED_EDGE('',*,*,#10610,.T.);
#14502=ORIENTED_EDGE('',*,*,#10606,.F.);
#14503=ORIENTED_EDGE('',*,*,#10611,.F.);
#14504=ORIENTED_EDGE('',*,*,#10612,.T.);
#14505=ORIENTED_EDGE('',*,*,#10613,.T.);
#14506=ORIENTED_EDGE('',*,*,#10609,.F.);
#14507=ORIENTED_EDGE('',*,*,#10614,.F.);
#14508=ORIENTED_EDGE('',*,*,#10615,.T.);
#14509=ORIENTED_EDGE('',*,*,#10616,.T.);
#14510=ORIENTED_EDGE('',*,*,#10612,.F.);
#14511=ORIENTED_EDGE('',*,*,#10617,.F.);
#14512=ORIENTED_EDGE('',*,*,#10618,.T.);
#14513=ORIENTED_EDGE('',*,*,#10619,.T.);
#14514=ORIENTED_EDGE('',*,*,#10615,.F.);
#14515=ORIENTED_EDGE('',*,*,#10620,.F.);
#14516=ORIENTED_EDGE('',*,*,#10621,.T.);
#14517=ORIENTED_EDGE('',*,*,#10622,.T.);
#14518=ORIENTED_EDGE('',*,*,#10618,.F.);
#14519=ORIENTED_EDGE('',*,*,#10623,.F.);
#14520=ORIENTED_EDGE('',*,*,#10624,.T.);
#14521=ORIENTED_EDGE('',*,*,#10625,.T.);
#14522=ORIENTED_EDGE('',*,*,#10621,.F.);
#14523=ORIENTED_EDGE('',*,*,#10626,.F.);
#14524=ORIENTED_EDGE('',*,*,#10627,.T.);
#14525=ORIENTED_EDGE('',*,*,#10628,.T.);
#14526=ORIENTED_EDGE('',*,*,#10624,.F.);
#14527=ORIENTED_EDGE('',*,*,#10629,.F.);
#14528=ORIENTED_EDGE('',*,*,#10630,.T.);
#14529=ORIENTED_EDGE('',*,*,#10631,.T.);
#14530=ORIENTED_EDGE('',*,*,#10627,.F.);
#14531=ORIENTED_EDGE('',*,*,#10632,.F.);
#14532=ORIENTED_EDGE('',*,*,#10633,.T.);
#14533=ORIENTED_EDGE('',*,*,#10634,.T.);
#14534=ORIENTED_EDGE('',*,*,#10630,.F.);
#14535=ORIENTED_EDGE('',*,*,#10635,.F.);
#14536=ORIENTED_EDGE('',*,*,#10636,.T.);
#14537=ORIENTED_EDGE('',*,*,#10637,.T.);
#14538=ORIENTED_EDGE('',*,*,#10633,.F.);
#14539=ORIENTED_EDGE('',*,*,#10638,.F.);
#14540=ORIENTED_EDGE('',*,*,#10639,.T.);
#14541=ORIENTED_EDGE('',*,*,#10640,.T.);
#14542=ORIENTED_EDGE('',*,*,#10636,.F.);
#14543=ORIENTED_EDGE('',*,*,#10641,.F.);
#14544=ORIENTED_EDGE('',*,*,#10642,.T.);
#14545=ORIENTED_EDGE('',*,*,#10643,.T.);
#14546=ORIENTED_EDGE('',*,*,#10639,.F.);
#14547=ORIENTED_EDGE('',*,*,#10644,.F.);
#14548=ORIENTED_EDGE('',*,*,#10645,.T.);
#14549=ORIENTED_EDGE('',*,*,#10646,.T.);
#14550=ORIENTED_EDGE('',*,*,#10642,.F.);
#14551=ORIENTED_EDGE('',*,*,#10647,.F.);
#14552=ORIENTED_EDGE('',*,*,#10648,.T.);
#14553=ORIENTED_EDGE('',*,*,#10649,.T.);
#14554=ORIENTED_EDGE('',*,*,#10645,.F.);
#14555=ORIENTED_EDGE('',*,*,#10650,.F.);
#14556=ORIENTED_EDGE('',*,*,#10651,.T.);
#14557=ORIENTED_EDGE('',*,*,#10652,.T.);
#14558=ORIENTED_EDGE('',*,*,#10648,.F.);
#14559=ORIENTED_EDGE('',*,*,#10653,.F.);
#14560=ORIENTED_EDGE('',*,*,#10654,.T.);
#14561=ORIENTED_EDGE('',*,*,#10655,.T.);
#14562=ORIENTED_EDGE('',*,*,#10651,.F.);
#14563=ORIENTED_EDGE('',*,*,#10656,.F.);
#14564=ORIENTED_EDGE('',*,*,#10657,.T.);
#14565=ORIENTED_EDGE('',*,*,#10658,.T.);
#14566=ORIENTED_EDGE('',*,*,#10654,.F.);
#14567=ORIENTED_EDGE('',*,*,#10659,.F.);
#14568=ORIENTED_EDGE('',*,*,#10660,.T.);
#14569=ORIENTED_EDGE('',*,*,#10661,.T.);
#14570=ORIENTED_EDGE('',*,*,#10657,.F.);
#14571=ORIENTED_EDGE('',*,*,#10662,.F.);
#14572=ORIENTED_EDGE('',*,*,#10663,.T.);
#14573=ORIENTED_EDGE('',*,*,#10664,.T.);
#14574=ORIENTED_EDGE('',*,*,#10660,.F.);
#14575=ORIENTED_EDGE('',*,*,#10665,.F.);
#14576=ORIENTED_EDGE('',*,*,#10666,.T.);
#14577=ORIENTED_EDGE('',*,*,#10667,.T.);
#14578=ORIENTED_EDGE('',*,*,#10663,.F.);
#14579=ORIENTED_EDGE('',*,*,#10668,.F.);
#14580=ORIENTED_EDGE('',*,*,#10669,.T.);
#14581=ORIENTED_EDGE('',*,*,#10670,.T.);
#14582=ORIENTED_EDGE('',*,*,#10666,.F.);
#14583=ORIENTED_EDGE('',*,*,#10671,.F.);
#14584=ORIENTED_EDGE('',*,*,#10672,.T.);
#14585=ORIENTED_EDGE('',*,*,#10673,.T.);
#14586=ORIENTED_EDGE('',*,*,#10669,.F.);
#14587=ORIENTED_EDGE('',*,*,#10674,.F.);
#14588=ORIENTED_EDGE('',*,*,#10675,.T.);
#14589=ORIENTED_EDGE('',*,*,#10676,.T.);
#14590=ORIENTED_EDGE('',*,*,#10672,.F.);
#14591=ORIENTED_EDGE('',*,*,#10677,.F.);
#14592=ORIENTED_EDGE('',*,*,#10678,.T.);
#14593=ORIENTED_EDGE('',*,*,#10679,.T.);
#14594=ORIENTED_EDGE('',*,*,#10675,.F.);
#14595=ORIENTED_EDGE('',*,*,#10680,.F.);
#14596=ORIENTED_EDGE('',*,*,#10681,.T.);
#14597=ORIENTED_EDGE('',*,*,#10682,.T.);
#14598=ORIENTED_EDGE('',*,*,#10678,.F.);
#14599=ORIENTED_EDGE('',*,*,#10683,.F.);
#14600=ORIENTED_EDGE('',*,*,#10684,.T.);
#14601=ORIENTED_EDGE('',*,*,#10685,.T.);
#14602=ORIENTED_EDGE('',*,*,#10681,.F.);
#14603=ORIENTED_EDGE('',*,*,#10686,.F.);
#14604=ORIENTED_EDGE('',*,*,#10687,.T.);
#14605=ORIENTED_EDGE('',*,*,#10688,.T.);
#14606=ORIENTED_EDGE('',*,*,#10684,.F.);
#14607=ORIENTED_EDGE('',*,*,#10689,.F.);
#14608=ORIENTED_EDGE('',*,*,#10690,.T.);
#14609=ORIENTED_EDGE('',*,*,#10691,.T.);
#14610=ORIENTED_EDGE('',*,*,#10687,.F.);
#14611=ORIENTED_EDGE('',*,*,#10692,.F.);
#14612=ORIENTED_EDGE('',*,*,#10693,.T.);
#14613=ORIENTED_EDGE('',*,*,#10694,.T.);
#14614=ORIENTED_EDGE('',*,*,#10690,.F.);
#14615=ORIENTED_EDGE('',*,*,#10695,.F.);
#14616=ORIENTED_EDGE('',*,*,#10696,.T.);
#14617=ORIENTED_EDGE('',*,*,#10697,.T.);
#14618=ORIENTED_EDGE('',*,*,#10693,.F.);
#14619=ORIENTED_EDGE('',*,*,#10698,.F.);
#14620=ORIENTED_EDGE('',*,*,#10699,.T.);
#14621=ORIENTED_EDGE('',*,*,#10700,.T.);
#14622=ORIENTED_EDGE('',*,*,#10696,.F.);
#14623=ORIENTED_EDGE('',*,*,#10701,.F.);
#14624=ORIENTED_EDGE('',*,*,#10702,.T.);
#14625=ORIENTED_EDGE('',*,*,#10703,.T.);
#14626=ORIENTED_EDGE('',*,*,#10699,.F.);
#14627=ORIENTED_EDGE('',*,*,#10704,.F.);
#14628=ORIENTED_EDGE('',*,*,#10705,.T.);
#14629=ORIENTED_EDGE('',*,*,#10706,.T.);
#14630=ORIENTED_EDGE('',*,*,#10702,.F.);
#14631=ORIENTED_EDGE('',*,*,#10707,.F.);
#14632=ORIENTED_EDGE('',*,*,#10708,.T.);
#14633=ORIENTED_EDGE('',*,*,#10709,.T.);
#14634=ORIENTED_EDGE('',*,*,#10705,.F.);
#14635=ORIENTED_EDGE('',*,*,#10710,.F.);
#14636=ORIENTED_EDGE('',*,*,#10711,.T.);
#14637=ORIENTED_EDGE('',*,*,#10712,.T.);
#14638=ORIENTED_EDGE('',*,*,#10708,.F.);
#14639=ORIENTED_EDGE('',*,*,#10713,.F.);
#14640=ORIENTED_EDGE('',*,*,#10714,.T.);
#14641=ORIENTED_EDGE('',*,*,#10715,.T.);
#14642=ORIENTED_EDGE('',*,*,#10711,.F.);
#14643=ORIENTED_EDGE('',*,*,#10716,.F.);
#14644=ORIENTED_EDGE('',*,*,#10717,.F.);
#14645=ORIENTED_EDGE('',*,*,#10718,.F.);
#14646=ORIENTED_EDGE('',*,*,#10719,.F.);
#14647=ORIENTED_EDGE('',*,*,#10720,.T.);
#14648=ORIENTED_EDGE('',*,*,#10476,.F.);
#14649=ORIENTED_EDGE('',*,*,#10721,.T.);
#14650=ORIENTED_EDGE('',*,*,#10601,.T.);
#14651=ORIENTED_EDGE('',*,*,#10722,.T.);
#14652=ORIENTED_EDGE('',*,*,#10479,.F.);
#14653=ORIENTED_EDGE('',*,*,#10717,.T.);
#14654=ORIENTED_EDGE('',*,*,#10723,.T.);
#14655=ORIENTED_EDGE('',*,*,#10714,.F.);
#14656=ORIENTED_EDGE('',*,*,#10724,.F.);
#14657=ORIENTED_EDGE('',*,*,#10722,.F.);
#14658=ORIENTED_EDGE('',*,*,#10600,.F.);
#14659=ORIENTED_EDGE('',*,*,#10604,.F.);
#14660=ORIENTED_EDGE('',*,*,#10607,.F.);
#14661=ORIENTED_EDGE('',*,*,#10610,.F.);
#14662=ORIENTED_EDGE('',*,*,#10613,.F.);
#14663=ORIENTED_EDGE('',*,*,#10616,.F.);
#14664=ORIENTED_EDGE('',*,*,#10619,.F.);
#14665=ORIENTED_EDGE('',*,*,#10622,.F.);
#14666=ORIENTED_EDGE('',*,*,#10625,.F.);
#14667=ORIENTED_EDGE('',*,*,#10628,.F.);
#14668=ORIENTED_EDGE('',*,*,#10631,.F.);
#14669=ORIENTED_EDGE('',*,*,#10634,.F.);
#14670=ORIENTED_EDGE('',*,*,#10637,.F.);
#14671=ORIENTED_EDGE('',*,*,#10640,.F.);
#14672=ORIENTED_EDGE('',*,*,#10643,.F.);
#14673=ORIENTED_EDGE('',*,*,#10646,.F.);
#14674=ORIENTED_EDGE('',*,*,#10649,.F.);
#14675=ORIENTED_EDGE('',*,*,#10652,.F.);
#14676=ORIENTED_EDGE('',*,*,#10655,.F.);
#14677=ORIENTED_EDGE('',*,*,#10658,.F.);
#14678=ORIENTED_EDGE('',*,*,#10661,.F.);
#14679=ORIENTED_EDGE('',*,*,#10664,.F.);
#14680=ORIENTED_EDGE('',*,*,#10667,.F.);
#14681=ORIENTED_EDGE('',*,*,#10670,.F.);
#14682=ORIENTED_EDGE('',*,*,#10673,.F.);
#14683=ORIENTED_EDGE('',*,*,#10676,.F.);
#14684=ORIENTED_EDGE('',*,*,#10679,.F.);
#14685=ORIENTED_EDGE('',*,*,#10682,.F.);
#14686=ORIENTED_EDGE('',*,*,#10685,.F.);
#14687=ORIENTED_EDGE('',*,*,#10688,.F.);
#14688=ORIENTED_EDGE('',*,*,#10691,.F.);
#14689=ORIENTED_EDGE('',*,*,#10694,.F.);
#14690=ORIENTED_EDGE('',*,*,#10697,.F.);
#14691=ORIENTED_EDGE('',*,*,#10700,.F.);
#14692=ORIENTED_EDGE('',*,*,#10703,.F.);
#14693=ORIENTED_EDGE('',*,*,#10706,.F.);
#14694=ORIENTED_EDGE('',*,*,#10709,.F.);
#14695=ORIENTED_EDGE('',*,*,#10712,.F.);
#14696=ORIENTED_EDGE('',*,*,#10715,.F.);
#14697=ORIENTED_EDGE('',*,*,#10723,.F.);
#14698=ORIENTED_EDGE('',*,*,#10720,.F.);
#14699=ORIENTED_EDGE('',*,*,#10725,.F.);
#14700=ORIENTED_EDGE('',*,*,#10596,.F.);
#14701=ORIENTED_EDGE('',*,*,#10726,.F.);
#14702=ORIENTED_EDGE('',*,*,#10594,.F.);
#14703=ORIENTED_EDGE('',*,*,#10591,.F.);
#14704=ORIENTED_EDGE('',*,*,#10588,.F.);
#14705=ORIENTED_EDGE('',*,*,#10585,.F.);
#14706=ORIENTED_EDGE('',*,*,#10582,.F.);
#14707=ORIENTED_EDGE('',*,*,#10579,.F.);
#14708=ORIENTED_EDGE('',*,*,#10576,.F.);
#14709=ORIENTED_EDGE('',*,*,#10573,.F.);
#14710=ORIENTED_EDGE('',*,*,#10570,.F.);
#14711=ORIENTED_EDGE('',*,*,#10567,.F.);
#14712=ORIENTED_EDGE('',*,*,#10564,.F.);
#14713=ORIENTED_EDGE('',*,*,#10561,.F.);
#14714=ORIENTED_EDGE('',*,*,#10558,.F.);
#14715=ORIENTED_EDGE('',*,*,#10555,.F.);
#14716=ORIENTED_EDGE('',*,*,#10552,.F.);
#14717=ORIENTED_EDGE('',*,*,#10549,.F.);
#14718=ORIENTED_EDGE('',*,*,#10546,.F.);
#14719=ORIENTED_EDGE('',*,*,#10543,.F.);
#14720=ORIENTED_EDGE('',*,*,#10540,.F.);
#14721=ORIENTED_EDGE('',*,*,#10537,.F.);
#14722=ORIENTED_EDGE('',*,*,#10534,.F.);
#14723=ORIENTED_EDGE('',*,*,#10531,.F.);
#14724=ORIENTED_EDGE('',*,*,#10528,.F.);
#14725=ORIENTED_EDGE('',*,*,#10525,.F.);
#14726=ORIENTED_EDGE('',*,*,#10522,.F.);
#14727=ORIENTED_EDGE('',*,*,#10519,.F.);
#14728=ORIENTED_EDGE('',*,*,#10516,.F.);
#14729=ORIENTED_EDGE('',*,*,#10513,.F.);
#14730=ORIENTED_EDGE('',*,*,#10510,.F.);
#14731=ORIENTED_EDGE('',*,*,#10507,.F.);
#14732=ORIENTED_EDGE('',*,*,#10504,.F.);
#14733=ORIENTED_EDGE('',*,*,#10501,.F.);
#14734=ORIENTED_EDGE('',*,*,#10498,.F.);
#14735=ORIENTED_EDGE('',*,*,#10495,.F.);
#14736=ORIENTED_EDGE('',*,*,#10492,.F.);
#14737=ORIENTED_EDGE('',*,*,#10489,.F.);
#14738=ORIENTED_EDGE('',*,*,#10486,.F.);
#14739=ORIENTED_EDGE('',*,*,#10483,.F.);
#14740=ORIENTED_EDGE('',*,*,#10480,.F.);
#14741=ORIENTED_EDGE('',*,*,#10721,.F.);
#14742=ORIENTED_EDGE('',*,*,#10475,.F.);
#14743=ORIENTED_EDGE('',*,*,#10482,.F.);
#14744=ORIENTED_EDGE('',*,*,#10485,.F.);
#14745=ORIENTED_EDGE('',*,*,#10488,.F.);
#14746=ORIENTED_EDGE('',*,*,#10491,.F.);
#14747=ORIENTED_EDGE('',*,*,#10494,.F.);
#14748=ORIENTED_EDGE('',*,*,#10497,.F.);
#14749=ORIENTED_EDGE('',*,*,#10500,.F.);
#14750=ORIENTED_EDGE('',*,*,#10503,.F.);
#14751=ORIENTED_EDGE('',*,*,#10506,.F.);
#14752=ORIENTED_EDGE('',*,*,#10509,.F.);
#14753=ORIENTED_EDGE('',*,*,#10512,.F.);
#14754=ORIENTED_EDGE('',*,*,#10515,.F.);
#14755=ORIENTED_EDGE('',*,*,#10518,.F.);
#14756=ORIENTED_EDGE('',*,*,#10521,.F.);
#14757=ORIENTED_EDGE('',*,*,#10524,.F.);
#14758=ORIENTED_EDGE('',*,*,#10527,.F.);
#14759=ORIENTED_EDGE('',*,*,#10530,.F.);
#14760=ORIENTED_EDGE('',*,*,#10533,.F.);
#14761=ORIENTED_EDGE('',*,*,#10536,.F.);
#14762=ORIENTED_EDGE('',*,*,#10539,.F.);
#14763=ORIENTED_EDGE('',*,*,#10542,.F.);
#14764=ORIENTED_EDGE('',*,*,#10545,.F.);
#14765=ORIENTED_EDGE('',*,*,#10548,.F.);
#14766=ORIENTED_EDGE('',*,*,#10551,.F.);
#14767=ORIENTED_EDGE('',*,*,#10554,.F.);
#14768=ORIENTED_EDGE('',*,*,#10557,.F.);
#14769=ORIENTED_EDGE('',*,*,#10560,.F.);
#14770=ORIENTED_EDGE('',*,*,#10563,.F.);
#14771=ORIENTED_EDGE('',*,*,#10566,.F.);
#14772=ORIENTED_EDGE('',*,*,#10569,.F.);
#14773=ORIENTED_EDGE('',*,*,#10572,.F.);
#14774=ORIENTED_EDGE('',*,*,#10575,.F.);
#14775=ORIENTED_EDGE('',*,*,#10578,.F.);
#14776=ORIENTED_EDGE('',*,*,#10581,.F.);
#14777=ORIENTED_EDGE('',*,*,#10584,.F.);
#14778=ORIENTED_EDGE('',*,*,#10587,.F.);
#14779=ORIENTED_EDGE('',*,*,#10590,.F.);
#14780=ORIENTED_EDGE('',*,*,#10593,.F.);
#14781=ORIENTED_EDGE('',*,*,#10727,.F.);
#14782=ORIENTED_EDGE('',*,*,#10598,.F.);
#14783=ORIENTED_EDGE('',*,*,#10728,.F.);
#14784=ORIENTED_EDGE('',*,*,#10718,.T.);
#14785=ORIENTED_EDGE('',*,*,#10724,.T.);
#14786=ORIENTED_EDGE('',*,*,#10716,.T.);
#14787=ORIENTED_EDGE('',*,*,#10713,.T.);
#14788=ORIENTED_EDGE('',*,*,#10710,.T.);
#14789=ORIENTED_EDGE('',*,*,#10707,.T.);
#14790=ORIENTED_EDGE('',*,*,#10704,.T.);
#14791=ORIENTED_EDGE('',*,*,#10701,.T.);
#14792=ORIENTED_EDGE('',*,*,#10698,.T.);
#14793=ORIENTED_EDGE('',*,*,#10695,.T.);
#14794=ORIENTED_EDGE('',*,*,#10692,.T.);
#14795=ORIENTED_EDGE('',*,*,#10689,.T.);
#14796=ORIENTED_EDGE('',*,*,#10686,.T.);
#14797=ORIENTED_EDGE('',*,*,#10683,.T.);
#14798=ORIENTED_EDGE('',*,*,#10680,.T.);
#14799=ORIENTED_EDGE('',*,*,#10677,.T.);
#14800=ORIENTED_EDGE('',*,*,#10674,.T.);
#14801=ORIENTED_EDGE('',*,*,#10671,.T.);
#14802=ORIENTED_EDGE('',*,*,#10668,.T.);
#14803=ORIENTED_EDGE('',*,*,#10665,.T.);
#14804=ORIENTED_EDGE('',*,*,#10662,.T.);
#14805=ORIENTED_EDGE('',*,*,#10659,.T.);
#14806=ORIENTED_EDGE('',*,*,#10656,.T.);
#14807=ORIENTED_EDGE('',*,*,#10653,.T.);
#14808=ORIENTED_EDGE('',*,*,#10650,.T.);
#14809=ORIENTED_EDGE('',*,*,#10647,.T.);
#14810=ORIENTED_EDGE('',*,*,#10644,.T.);
#14811=ORIENTED_EDGE('',*,*,#10641,.T.);
#14812=ORIENTED_EDGE('',*,*,#10638,.T.);
#14813=ORIENTED_EDGE('',*,*,#10635,.T.);
#14814=ORIENTED_EDGE('',*,*,#10632,.T.);
#14815=ORIENTED_EDGE('',*,*,#10629,.T.);
#14816=ORIENTED_EDGE('',*,*,#10626,.T.);
#14817=ORIENTED_EDGE('',*,*,#10623,.T.);
#14818=ORIENTED_EDGE('',*,*,#10620,.T.);
#14819=ORIENTED_EDGE('',*,*,#10617,.T.);
#14820=ORIENTED_EDGE('',*,*,#10614,.T.);
#14821=ORIENTED_EDGE('',*,*,#10611,.T.);
#14822=ORIENTED_EDGE('',*,*,#10608,.T.);
#14823=ORIENTED_EDGE('',*,*,#10605,.T.);
#14824=ORIENTED_EDGE('',*,*,#10602,.T.);
#14825=ORIENTED_EDGE('',*,*,#10595,.T.);
#14826=ORIENTED_EDGE('',*,*,#10727,.T.);
#14827=ORIENTED_EDGE('',*,*,#10592,.F.);
#14828=ORIENTED_EDGE('',*,*,#10726,.T.);
#14829=ORIENTED_EDGE('',*,*,#10478,.F.);
#14830=ORIENTED_EDGE('',*,*,#10729,.F.);
#14831=ORIENTED_EDGE('',*,*,#10319,.F.);
#14832=ORIENTED_EDGE('',*,*,#10730,.T.);
#14833=ORIENTED_EDGE('',*,*,#10399,.T.);
#14834=ORIENTED_EDGE('',*,*,#10731,.T.);
#14835=ORIENTED_EDGE('',*,*,#10322,.F.);
#14836=ORIENTED_EDGE('',*,*,#10470,.T.);
#14837=ORIENTED_EDGE('',*,*,#10732,.T.);
#14838=ORIENTED_EDGE('',*,*,#10467,.F.);
#14839=ORIENTED_EDGE('',*,*,#10733,.F.);
#14840=ORIENTED_EDGE('',*,*,#10731,.F.);
#14841=ORIENTED_EDGE('',*,*,#10398,.F.);
#14842=ORIENTED_EDGE('',*,*,#10402,.F.);
#14843=ORIENTED_EDGE('',*,*,#10405,.F.);
#14844=ORIENTED_EDGE('',*,*,#10408,.F.);
#14845=ORIENTED_EDGE('',*,*,#10411,.F.);
#14846=ORIENTED_EDGE('',*,*,#10414,.F.);
#14847=ORIENTED_EDGE('',*,*,#10417,.F.);
#14848=ORIENTED_EDGE('',*,*,#10420,.F.);
#14849=ORIENTED_EDGE('',*,*,#10423,.F.);
#14850=ORIENTED_EDGE('',*,*,#10426,.F.);
#14851=ORIENTED_EDGE('',*,*,#10429,.F.);
#14852=ORIENTED_EDGE('',*,*,#10432,.F.);
#14853=ORIENTED_EDGE('',*,*,#10435,.F.);
#14854=ORIENTED_EDGE('',*,*,#10438,.F.);
#14855=ORIENTED_EDGE('',*,*,#10441,.F.);
#14856=ORIENTED_EDGE('',*,*,#10444,.F.);
#14857=ORIENTED_EDGE('',*,*,#10447,.F.);
#14858=ORIENTED_EDGE('',*,*,#10450,.F.);
#14859=ORIENTED_EDGE('',*,*,#10453,.F.);
#14860=ORIENTED_EDGE('',*,*,#10456,.F.);
#14861=ORIENTED_EDGE('',*,*,#10459,.F.);
#14862=ORIENTED_EDGE('',*,*,#10462,.F.);
#14863=ORIENTED_EDGE('',*,*,#10465,.F.);
#14864=ORIENTED_EDGE('',*,*,#10468,.F.);
#14865=ORIENTED_EDGE('',*,*,#10732,.F.);
#14866=ORIENTED_EDGE('',*,*,#10473,.F.);
#14867=ORIENTED_EDGE('',*,*,#10734,.F.);
#14868=ORIENTED_EDGE('',*,*,#10394,.F.);
#14869=ORIENTED_EDGE('',*,*,#10735,.F.);
#14870=ORIENTED_EDGE('',*,*,#10392,.F.);
#14871=ORIENTED_EDGE('',*,*,#10389,.F.);
#14872=ORIENTED_EDGE('',*,*,#10386,.F.);
#14873=ORIENTED_EDGE('',*,*,#10383,.F.);
#14874=ORIENTED_EDGE('',*,*,#10380,.F.);
#14875=ORIENTED_EDGE('',*,*,#10377,.F.);
#14876=ORIENTED_EDGE('',*,*,#10374,.F.);
#14877=ORIENTED_EDGE('',*,*,#10371,.F.);
#14878=ORIENTED_EDGE('',*,*,#10368,.F.);
#14879=ORIENTED_EDGE('',*,*,#10365,.F.);
#14880=ORIENTED_EDGE('',*,*,#10362,.F.);
#14881=ORIENTED_EDGE('',*,*,#10359,.F.);
#14882=ORIENTED_EDGE('',*,*,#10356,.F.);
#14883=ORIENTED_EDGE('',*,*,#10353,.F.);
#14884=ORIENTED_EDGE('',*,*,#10350,.F.);
#14885=ORIENTED_EDGE('',*,*,#10347,.F.);
#14886=ORIENTED_EDGE('',*,*,#10344,.F.);
#14887=ORIENTED_EDGE('',*,*,#10341,.F.);
#14888=ORIENTED_EDGE('',*,*,#10338,.F.);
#14889=ORIENTED_EDGE('',*,*,#10335,.F.);
#14890=ORIENTED_EDGE('',*,*,#10332,.F.);
#14891=ORIENTED_EDGE('',*,*,#10329,.F.);
#14892=ORIENTED_EDGE('',*,*,#10326,.F.);
#14893=ORIENTED_EDGE('',*,*,#10323,.F.);
#14894=ORIENTED_EDGE('',*,*,#10730,.F.);
#14895=ORIENTED_EDGE('',*,*,#10318,.F.);
#14896=ORIENTED_EDGE('',*,*,#10325,.F.);
#14897=ORIENTED_EDGE('',*,*,#10328,.F.);
#14898=ORIENTED_EDGE('',*,*,#10331,.F.);
#14899=ORIENTED_EDGE('',*,*,#10334,.F.);
#14900=ORIENTED_EDGE('',*,*,#10337,.F.);
#14901=ORIENTED_EDGE('',*,*,#10340,.F.);
#14902=ORIENTED_EDGE('',*,*,#10343,.F.);
#14903=ORIENTED_EDGE('',*,*,#10346,.F.);
#14904=ORIENTED_EDGE('',*,*,#10349,.F.);
#14905=ORIENTED_EDGE('',*,*,#10352,.F.);
#14906=ORIENTED_EDGE('',*,*,#10355,.F.);
#14907=ORIENTED_EDGE('',*,*,#10358,.F.);
#14908=ORIENTED_EDGE('',*,*,#10361,.F.);
#14909=ORIENTED_EDGE('',*,*,#10364,.F.);
#14910=ORIENTED_EDGE('',*,*,#10367,.F.);
#14911=ORIENTED_EDGE('',*,*,#10370,.F.);
#14912=ORIENTED_EDGE('',*,*,#10373,.F.);
#14913=ORIENTED_EDGE('',*,*,#10376,.F.);
#14914=ORIENTED_EDGE('',*,*,#10379,.F.);
#14915=ORIENTED_EDGE('',*,*,#10382,.F.);
#14916=ORIENTED_EDGE('',*,*,#10385,.F.);
#14917=ORIENTED_EDGE('',*,*,#10388,.F.);
#14918=ORIENTED_EDGE('',*,*,#10391,.F.);
#14919=ORIENTED_EDGE('',*,*,#10736,.F.);
#14920=ORIENTED_EDGE('',*,*,#10396,.F.);
#14921=ORIENTED_EDGE('',*,*,#10737,.F.);
#14922=ORIENTED_EDGE('',*,*,#10471,.T.);
#14923=ORIENTED_EDGE('',*,*,#10733,.T.);
#14924=ORIENTED_EDGE('',*,*,#10469,.T.);
#14925=ORIENTED_EDGE('',*,*,#10466,.T.);
#14926=ORIENTED_EDGE('',*,*,#10463,.T.);
#14927=ORIENTED_EDGE('',*,*,#10460,.T.);
#14928=ORIENTED_EDGE('',*,*,#10457,.T.);
#14929=ORIENTED_EDGE('',*,*,#10454,.T.);
#14930=ORIENTED_EDGE('',*,*,#10451,.T.);
#14931=ORIENTED_EDGE('',*,*,#10448,.T.);
#14932=ORIENTED_EDGE('',*,*,#10445,.T.);
#14933=ORIENTED_EDGE('',*,*,#10442,.T.);
#14934=ORIENTED_EDGE('',*,*,#10439,.T.);
#14935=ORIENTED_EDGE('',*,*,#10436,.T.);
#14936=ORIENTED_EDGE('',*,*,#10433,.T.);
#14937=ORIENTED_EDGE('',*,*,#10430,.T.);
#14938=ORIENTED_EDGE('',*,*,#10427,.T.);
#14939=ORIENTED_EDGE('',*,*,#10424,.T.);
#14940=ORIENTED_EDGE('',*,*,#10421,.T.);
#14941=ORIENTED_EDGE('',*,*,#10418,.T.);
#14942=ORIENTED_EDGE('',*,*,#10415,.T.);
#14943=ORIENTED_EDGE('',*,*,#10412,.T.);
#14944=ORIENTED_EDGE('',*,*,#10409,.T.);
#14945=ORIENTED_EDGE('',*,*,#10406,.T.);
#14946=ORIENTED_EDGE('',*,*,#10403,.T.);
#14947=ORIENTED_EDGE('',*,*,#10400,.T.);
#14948=ORIENTED_EDGE('',*,*,#10393,.T.);
#14949=ORIENTED_EDGE('',*,*,#10736,.T.);
#14950=ORIENTED_EDGE('',*,*,#10390,.F.);
#14951=ORIENTED_EDGE('',*,*,#10735,.T.);
#14952=ORIENTED_EDGE('',*,*,#10321,.F.);
#14953=ORIENTED_EDGE('',*,*,#10738,.F.);
#14954=ORIENTED_EDGE('',*,*,#10739,.T.);
#14955=ORIENTED_EDGE('',*,*,#10740,.T.);
#14956=ORIENTED_EDGE('',*,*,#10741,.T.);
#14957=ORIENTED_EDGE('',*,*,#10742,.T.);
#14958=ORIENTED_EDGE('',*,*,#10740,.F.);
#14959=ORIENTED_EDGE('',*,*,#10743,.F.);
#14960=ORIENTED_EDGE('',*,*,#10744,.F.);
#14961=ORIENTED_EDGE('',*,*,#10745,.F.);
#14962=ORIENTED_EDGE('',*,*,#10739,.F.);
#14963=ORIENTED_EDGE('',*,*,#10746,.T.);
#14964=ORIENTED_EDGE('',*,*,#10747,.F.);
#14965=ORIENTED_EDGE('',*,*,#10748,.T.);
#14966=ORIENTED_EDGE('',*,*,#10749,.F.);
#14967=ORIENTED_EDGE('',*,*,#10750,.T.);
#14968=ORIENTED_EDGE('',*,*,#10751,.F.);
#14969=ORIENTED_EDGE('',*,*,#10752,.T.);
#14970=ORIENTED_EDGE('',*,*,#10753,.F.);
#14971=ORIENTED_EDGE('',*,*,#10754,.T.);
#14972=ORIENTED_EDGE('',*,*,#10755,.F.);
#14973=ORIENTED_EDGE('',*,*,#10756,.T.);
#14974=ORIENTED_EDGE('',*,*,#10757,.F.);
#14975=ORIENTED_EDGE('',*,*,#10758,.T.);
#14976=ORIENTED_EDGE('',*,*,#10759,.F.);
#14977=ORIENTED_EDGE('',*,*,#10760,.T.);
#14978=ORIENTED_EDGE('',*,*,#10761,.F.);
#14979=ORIENTED_EDGE('',*,*,#10762,.T.);
#14980=ORIENTED_EDGE('',*,*,#10763,.F.);
#14981=ORIENTED_EDGE('',*,*,#10764,.T.);
#14982=ORIENTED_EDGE('',*,*,#10765,.F.);
#14983=ORIENTED_EDGE('',*,*,#10766,.T.);
#14984=ORIENTED_EDGE('',*,*,#10767,.F.);
#14985=ORIENTED_EDGE('',*,*,#10768,.T.);
#14986=ORIENTED_EDGE('',*,*,#10769,.F.);
#14987=ORIENTED_EDGE('',*,*,#10770,.T.);
#14988=ORIENTED_EDGE('',*,*,#10771,.F.);
#14989=ORIENTED_EDGE('',*,*,#10772,.T.);
#14990=ORIENTED_EDGE('',*,*,#10773,.F.);
#14991=ORIENTED_EDGE('',*,*,#10774,.T.);
#14992=ORIENTED_EDGE('',*,*,#10775,.F.);
#14993=ORIENTED_EDGE('',*,*,#10776,.T.);
#14994=ORIENTED_EDGE('',*,*,#10777,.F.);
#14995=ORIENTED_EDGE('',*,*,#10778,.T.);
#14996=ORIENTED_EDGE('',*,*,#10779,.F.);
#14997=ORIENTED_EDGE('',*,*,#10780,.T.);
#14998=ORIENTED_EDGE('',*,*,#10781,.F.);
#14999=ORIENTED_EDGE('',*,*,#10782,.T.);
#15000=ORIENTED_EDGE('',*,*,#10783,.F.);
#15001=ORIENTED_EDGE('',*,*,#10784,.T.);
#15002=ORIENTED_EDGE('',*,*,#10785,.F.);
#15003=ORIENTED_EDGE('',*,*,#10786,.T.);
#15004=ORIENTED_EDGE('',*,*,#10787,.F.);
#15005=ORIENTED_EDGE('',*,*,#10788,.T.);
#15006=ORIENTED_EDGE('',*,*,#10789,.F.);
#15007=ORIENTED_EDGE('',*,*,#10790,.T.);
#15008=ORIENTED_EDGE('',*,*,#10791,.F.);
#15009=ORIENTED_EDGE('',*,*,#10792,.T.);
#15010=ORIENTED_EDGE('',*,*,#10793,.F.);
#15011=ORIENTED_EDGE('',*,*,#10794,.T.);
#15012=ORIENTED_EDGE('',*,*,#10795,.F.);
#15013=ORIENTED_EDGE('',*,*,#10796,.T.);
#15014=ORIENTED_EDGE('',*,*,#10797,.F.);
#15015=ORIENTED_EDGE('',*,*,#10798,.T.);
#15016=ORIENTED_EDGE('',*,*,#10799,.F.);
#15017=ORIENTED_EDGE('',*,*,#10800,.T.);
#15018=ORIENTED_EDGE('',*,*,#10801,.F.);
#15019=ORIENTED_EDGE('',*,*,#10802,.T.);
#15020=ORIENTED_EDGE('',*,*,#10803,.F.);
#15021=ORIENTED_EDGE('',*,*,#10804,.T.);
#15022=ORIENTED_EDGE('',*,*,#10805,.F.);
#15023=ORIENTED_EDGE('',*,*,#10806,.T.);
#15024=ORIENTED_EDGE('',*,*,#10807,.F.);
#15025=ORIENTED_EDGE('',*,*,#10808,.T.);
#15026=ORIENTED_EDGE('',*,*,#10809,.F.);
#15027=ORIENTED_EDGE('',*,*,#10810,.T.);
#15028=ORIENTED_EDGE('',*,*,#10811,.F.);
#15029=ORIENTED_EDGE('',*,*,#10812,.T.);
#15030=ORIENTED_EDGE('',*,*,#10813,.F.);
#15031=ORIENTED_EDGE('',*,*,#10814,.T.);
#15032=ORIENTED_EDGE('',*,*,#10815,.F.);
#15033=ORIENTED_EDGE('',*,*,#10743,.T.);
#15034=ORIENTED_EDGE('',*,*,#10737,.T.);
#15035=ORIENTED_EDGE('',*,*,#10395,.T.);
#15036=ORIENTED_EDGE('',*,*,#10734,.T.);
#15037=ORIENTED_EDGE('',*,*,#10472,.T.);
#15038=ORIENTED_EDGE('',*,*,#10816,.T.);
#15039=ORIENTED_EDGE('',*,*,#10817,.T.);
#15040=ORIENTED_EDGE('',*,*,#10818,.T.);
#15041=ORIENTED_EDGE('',*,*,#10819,.T.);
#15042=ORIENTED_EDGE('',*,*,#10820,.T.);
#15043=ORIENTED_EDGE('',*,*,#10821,.T.);
#15044=ORIENTED_EDGE('',*,*,#10747,.T.);
#15045=ORIENTED_EDGE('',*,*,#10822,.T.);
#15046=ORIENTED_EDGE('',*,*,#10821,.F.);
#15047=ORIENTED_EDGE('',*,*,#10823,.F.);
#15048=ORIENTED_EDGE('',*,*,#10824,.F.);
#15049=ORIENTED_EDGE('',*,*,#10748,.F.);
#15050=ORIENTED_EDGE('',*,*,#10825,.T.);
#15051=ORIENTED_EDGE('',*,*,#10826,.T.);
#15052=ORIENTED_EDGE('',*,*,#10749,.T.);
#15053=ORIENTED_EDGE('',*,*,#10824,.T.);
#15054=ORIENTED_EDGE('',*,*,#10826,.F.);
#15055=ORIENTED_EDGE('',*,*,#10827,.F.);
#15056=ORIENTED_EDGE('',*,*,#10828,.F.);
#15057=ORIENTED_EDGE('',*,*,#10750,.F.);
#15058=ORIENTED_EDGE('',*,*,#10829,.T.);
#15059=ORIENTED_EDGE('',*,*,#10830,.T.);
#15060=ORIENTED_EDGE('',*,*,#10751,.T.);
#15061=ORIENTED_EDGE('',*,*,#10828,.T.);
#15062=ORIENTED_EDGE('',*,*,#10830,.F.);
#15063=ORIENTED_EDGE('',*,*,#10831,.F.);
#15064=ORIENTED_EDGE('',*,*,#10832,.F.);
#15065=ORIENTED_EDGE('',*,*,#10752,.F.);
#15066=ORIENTED_EDGE('',*,*,#10833,.T.);
#15067=ORIENTED_EDGE('',*,*,#10834,.T.);
#15068=ORIENTED_EDGE('',*,*,#10753,.T.);
#15069=ORIENTED_EDGE('',*,*,#10832,.T.);
#15070=ORIENTED_EDGE('',*,*,#10834,.F.);
#15071=ORIENTED_EDGE('',*,*,#10835,.F.);
#15072=ORIENTED_EDGE('',*,*,#10836,.F.);
#15073=ORIENTED_EDGE('',*,*,#10754,.F.);
#15074=ORIENTED_EDGE('',*,*,#10755,.T.);
#15075=ORIENTED_EDGE('',*,*,#10836,.T.);
#15076=ORIENTED_EDGE('',*,*,#10837,.T.);
#15077=ORIENTED_EDGE('',*,*,#10838,.T.);
#15078=ORIENTED_EDGE('',*,*,#10757,.T.);
#15079=ORIENTED_EDGE('',*,*,#10839,.T.);
#15080=ORIENTED_EDGE('',*,*,#10840,.T.);
#15081=ORIENTED_EDGE('',*,*,#10841,.T.);
#15082=ORIENTED_EDGE('',*,*,#10841,.F.);
#15083=ORIENTED_EDGE('',*,*,#10842,.F.);
#15084=ORIENTED_EDGE('',*,*,#10843,.F.);
#15085=ORIENTED_EDGE('',*,*,#10758,.F.);
#15086=ORIENTED_EDGE('',*,*,#10759,.T.);
#15087=ORIENTED_EDGE('',*,*,#10843,.T.);
#15088=ORIENTED_EDGE('',*,*,#10844,.T.);
#15089=ORIENTED_EDGE('',*,*,#10845,.T.);
#15090=ORIENTED_EDGE('',*,*,#10761,.T.);
#15091=ORIENTED_EDGE('',*,*,#10846,.T.);
#15092=ORIENTED_EDGE('',*,*,#10847,.T.);
#15093=ORIENTED_EDGE('',*,*,#10848,.T.);
#15094=ORIENTED_EDGE('',*,*,#10848,.F.);
#15095=ORIENTED_EDGE('',*,*,#10849,.F.);
#15096=ORIENTED_EDGE('',*,*,#10850,.F.);
#15097=ORIENTED_EDGE('',*,*,#10762,.F.);
#15098=ORIENTED_EDGE('',*,*,#10763,.T.);
#15099=ORIENTED_EDGE('',*,*,#10850,.T.);
#15100=ORIENTED_EDGE('',*,*,#10851,.T.);
#15101=ORIENTED_EDGE('',*,*,#10852,.T.);
#15102=ORIENTED_EDGE('',*,*,#10853,.T.);
#15103=ORIENTED_EDGE('',*,*,#10854,.T.);
#15104=ORIENTED_EDGE('',*,*,#10765,.T.);
#15105=ORIENTED_EDGE('',*,*,#10855,.T.);
#15106=ORIENTED_EDGE('',*,*,#10854,.F.);
#15107=ORIENTED_EDGE('',*,*,#10856,.F.);
#15108=ORIENTED_EDGE('',*,*,#10857,.F.);
#15109=ORIENTED_EDGE('',*,*,#10766,.F.);
#15110=ORIENTED_EDGE('',*,*,#10858,.T.);
#15111=ORIENTED_EDGE('',*,*,#10859,.T.);
#15112=ORIENTED_EDGE('',*,*,#10767,.T.);
#15113=ORIENTED_EDGE('',*,*,#10857,.T.);
#15114=ORIENTED_EDGE('',*,*,#10859,.F.);
#15115=ORIENTED_EDGE('',*,*,#10860,.F.);
#15116=ORIENTED_EDGE('',*,*,#10861,.F.);
#15117=ORIENTED_EDGE('',*,*,#10768,.F.);
#15118=ORIENTED_EDGE('',*,*,#10862,.T.);
#15119=ORIENTED_EDGE('',*,*,#10863,.T.);
#15120=ORIENTED_EDGE('',*,*,#10769,.T.);
#15121=ORIENTED_EDGE('',*,*,#10861,.T.);
#15122=ORIENTED_EDGE('',*,*,#10863,.F.);
#15123=ORIENTED_EDGE('',*,*,#10864,.F.);
#15124=ORIENTED_EDGE('',*,*,#10865,.F.);
#15125=ORIENTED_EDGE('',*,*,#10770,.F.);
#15126=ORIENTED_EDGE('',*,*,#10866,.T.);
#15127=ORIENTED_EDGE('',*,*,#10867,.T.);
#15128=ORIENTED_EDGE('',*,*,#10771,.T.);
#15129=ORIENTED_EDGE('',*,*,#10865,.T.);
#15130=ORIENTED_EDGE('',*,*,#10867,.F.);
#15131=ORIENTED_EDGE('',*,*,#10868,.F.);
#15132=ORIENTED_EDGE('',*,*,#10869,.F.);
#15133=ORIENTED_EDGE('',*,*,#10772,.F.);
#15134=ORIENTED_EDGE('',*,*,#10773,.T.);
#15135=ORIENTED_EDGE('',*,*,#10869,.T.);
#15136=ORIENTED_EDGE('',*,*,#10870,.T.);
#15137=ORIENTED_EDGE('',*,*,#10871,.T.);
#15138=ORIENTED_EDGE('',*,*,#10775,.T.);
#15139=ORIENTED_EDGE('',*,*,#10872,.T.);
#15140=ORIENTED_EDGE('',*,*,#10873,.T.);
#15141=ORIENTED_EDGE('',*,*,#10874,.T.);
#15142=ORIENTED_EDGE('',*,*,#10874,.F.);
#15143=ORIENTED_EDGE('',*,*,#10875,.F.);
#15144=ORIENTED_EDGE('',*,*,#10876,.F.);
#15145=ORIENTED_EDGE('',*,*,#10776,.F.);
#15146=ORIENTED_EDGE('',*,*,#10777,.T.);
#15147=ORIENTED_EDGE('',*,*,#10876,.T.);
#15148=ORIENTED_EDGE('',*,*,#10877,.T.);
#15149=ORIENTED_EDGE('',*,*,#10878,.T.);
#15150=ORIENTED_EDGE('',*,*,#10779,.T.);
#15151=ORIENTED_EDGE('',*,*,#10879,.T.);
#15152=ORIENTED_EDGE('',*,*,#10880,.T.);
#15153=ORIENTED_EDGE('',*,*,#10881,.T.);
#15154=ORIENTED_EDGE('',*,*,#10881,.F.);
#15155=ORIENTED_EDGE('',*,*,#10882,.F.);
#15156=ORIENTED_EDGE('',*,*,#10883,.F.);
#15157=ORIENTED_EDGE('',*,*,#10780,.F.);
#15158=ORIENTED_EDGE('',*,*,#10781,.T.);
#15159=ORIENTED_EDGE('',*,*,#10883,.T.);
#15160=ORIENTED_EDGE('',*,*,#10884,.T.);
#15161=ORIENTED_EDGE('',*,*,#10885,.T.);
#15162=ORIENTED_EDGE('',*,*,#10886,.T.);
#15163=ORIENTED_EDGE('',*,*,#10887,.T.);
#15164=ORIENTED_EDGE('',*,*,#10783,.T.);
#15165=ORIENTED_EDGE('',*,*,#10888,.T.);
#15166=ORIENTED_EDGE('',*,*,#10887,.F.);
#15167=ORIENTED_EDGE('',*,*,#10889,.F.);
#15168=ORIENTED_EDGE('',*,*,#10890,.F.);
#15169=ORIENTED_EDGE('',*,*,#10784,.F.);
#15170=ORIENTED_EDGE('',*,*,#10891,.T.);
#15171=ORIENTED_EDGE('',*,*,#10892,.T.);
#15172=ORIENTED_EDGE('',*,*,#10785,.T.);
#15173=ORIENTED_EDGE('',*,*,#10890,.T.);
#15174=ORIENTED_EDGE('',*,*,#10892,.F.);
#15175=ORIENTED_EDGE('',*,*,#10893,.F.);
#15176=ORIENTED_EDGE('',*,*,#10894,.F.);
#15177=ORIENTED_EDGE('',*,*,#10786,.F.);
#15178=ORIENTED_EDGE('',*,*,#10895,.T.);
#15179=ORIENTED_EDGE('',*,*,#10896,.T.);
#15180=ORIENTED_EDGE('',*,*,#10787,.T.);
#15181=ORIENTED_EDGE('',*,*,#10894,.T.);
#15182=ORIENTED_EDGE('',*,*,#10896,.F.);
#15183=ORIENTED_EDGE('',*,*,#10897,.F.);
#15184=ORIENTED_EDGE('',*,*,#10898,.F.);
#15185=ORIENTED_EDGE('',*,*,#10788,.F.);
#15186=ORIENTED_EDGE('',*,*,#10899,.T.);
#15187=ORIENTED_EDGE('',*,*,#10900,.T.);
#15188=ORIENTED_EDGE('',*,*,#10789,.T.);
#15189=ORIENTED_EDGE('',*,*,#10898,.T.);
#15190=ORIENTED_EDGE('',*,*,#10900,.F.);
#15191=ORIENTED_EDGE('',*,*,#10901,.F.);
#15192=ORIENTED_EDGE('',*,*,#10902,.F.);
#15193=ORIENTED_EDGE('',*,*,#10790,.F.);
#15194=ORIENTED_EDGE('',*,*,#10791,.T.);
#15195=ORIENTED_EDGE('',*,*,#10902,.T.);
#15196=ORIENTED_EDGE('',*,*,#10903,.T.);
#15197=ORIENTED_EDGE('',*,*,#10904,.T.);
#15198=ORIENTED_EDGE('',*,*,#10793,.T.);
#15199=ORIENTED_EDGE('',*,*,#10905,.T.);
#15200=ORIENTED_EDGE('',*,*,#10906,.T.);
#15201=ORIENTED_EDGE('',*,*,#10907,.T.);
#15202=ORIENTED_EDGE('',*,*,#10907,.F.);
#15203=ORIENTED_EDGE('',*,*,#10908,.F.);
#15204=ORIENTED_EDGE('',*,*,#10909,.F.);
#15205=ORIENTED_EDGE('',*,*,#10794,.F.);
#15206=ORIENTED_EDGE('',*,*,#10795,.T.);
#15207=ORIENTED_EDGE('',*,*,#10909,.T.);
#15208=ORIENTED_EDGE('',*,*,#10910,.T.);
#15209=ORIENTED_EDGE('',*,*,#10911,.T.);
#15210=ORIENTED_EDGE('',*,*,#10797,.T.);
#15211=ORIENTED_EDGE('',*,*,#10912,.T.);
#15212=ORIENTED_EDGE('',*,*,#10913,.T.);
#15213=ORIENTED_EDGE('',*,*,#10914,.T.);
#15214=ORIENTED_EDGE('',*,*,#10914,.F.);
#15215=ORIENTED_EDGE('',*,*,#10915,.F.);
#15216=ORIENTED_EDGE('',*,*,#10916,.F.);
#15217=ORIENTED_EDGE('',*,*,#10798,.F.);
#15218=ORIENTED_EDGE('',*,*,#10799,.T.);
#15219=ORIENTED_EDGE('',*,*,#10916,.T.);
#15220=ORIENTED_EDGE('',*,*,#10917,.T.);
#15221=ORIENTED_EDGE('',*,*,#10918,.T.);
#15222=ORIENTED_EDGE('',*,*,#10919,.T.);
#15223=ORIENTED_EDGE('',*,*,#10920,.T.);
#15224=ORIENTED_EDGE('',*,*,#10801,.T.);
#15225=ORIENTED_EDGE('',*,*,#10921,.T.);
#15226=ORIENTED_EDGE('',*,*,#10920,.F.);
#15227=ORIENTED_EDGE('',*,*,#10922,.F.);
#15228=ORIENTED_EDGE('',*,*,#10923,.F.);
#15229=ORIENTED_EDGE('',*,*,#10802,.F.);
#15230=ORIENTED_EDGE('',*,*,#10924,.T.);
#15231=ORIENTED_EDGE('',*,*,#10925,.T.);
#15232=ORIENTED_EDGE('',*,*,#10803,.T.);
#15233=ORIENTED_EDGE('',*,*,#10923,.T.);
#15234=ORIENTED_EDGE('',*,*,#10925,.F.);
#15235=ORIENTED_EDGE('',*,*,#10926,.F.);
#15236=ORIENTED_EDGE('',*,*,#10927,.F.);
#15237=ORIENTED_EDGE('',*,*,#10804,.F.);
#15238=ORIENTED_EDGE('',*,*,#10928,.T.);
#15239=ORIENTED_EDGE('',*,*,#10929,.T.);
#15240=ORIENTED_EDGE('',*,*,#10805,.T.);
#15241=ORIENTED_EDGE('',*,*,#10927,.T.);
#15242=ORIENTED_EDGE('',*,*,#10929,.F.);
#15243=ORIENTED_EDGE('',*,*,#10930,.F.);
#15244=ORIENTED_EDGE('',*,*,#10931,.F.);
#15245=ORIENTED_EDGE('',*,*,#10806,.F.);
#15246=ORIENTED_EDGE('',*,*,#10932,.T.);
#15247=ORIENTED_EDGE('',*,*,#10933,.T.);
#15248=ORIENTED_EDGE('',*,*,#10807,.T.);
#15249=ORIENTED_EDGE('',*,*,#10931,.T.);
#15250=ORIENTED_EDGE('',*,*,#10933,.F.);
#15251=ORIENTED_EDGE('',*,*,#10934,.F.);
#15252=ORIENTED_EDGE('',*,*,#10935,.F.);
#15253=ORIENTED_EDGE('',*,*,#10808,.F.);
#15254=ORIENTED_EDGE('',*,*,#10809,.T.);
#15255=ORIENTED_EDGE('',*,*,#10935,.T.);
#15256=ORIENTED_EDGE('',*,*,#10936,.T.);
#15257=ORIENTED_EDGE('',*,*,#10937,.T.);
#15258=ORIENTED_EDGE('',*,*,#10811,.T.);
#15259=ORIENTED_EDGE('',*,*,#10938,.T.);
#15260=ORIENTED_EDGE('',*,*,#10939,.T.);
#15261=ORIENTED_EDGE('',*,*,#10940,.T.);
#15262=ORIENTED_EDGE('',*,*,#10940,.F.);
#15263=ORIENTED_EDGE('',*,*,#10941,.F.);
#15264=ORIENTED_EDGE('',*,*,#10942,.F.);
#15265=ORIENTED_EDGE('',*,*,#10812,.F.);
#15266=ORIENTED_EDGE('',*,*,#10813,.T.);
#15267=ORIENTED_EDGE('',*,*,#10942,.T.);
#15268=ORIENTED_EDGE('',*,*,#10943,.T.);
#15269=ORIENTED_EDGE('',*,*,#10944,.T.);
#15270=ORIENTED_EDGE('',*,*,#10815,.T.);
#15271=ORIENTED_EDGE('',*,*,#10945,.T.);
#15272=ORIENTED_EDGE('',*,*,#10946,.T.);
#15273=ORIENTED_EDGE('',*,*,#10744,.T.);
#15274=ORIENTED_EDGE('',*,*,#10819,.F.);
#15275=ORIENTED_EDGE('',*,*,#10947,.T.);
#15276=ORIENTED_EDGE('',*,*,#10948,.T.);
#15277=ORIENTED_EDGE('',*,*,#10947,.F.);
#15278=ORIENTED_EDGE('',*,*,#10818,.F.);
#15279=ORIENTED_EDGE('',*,*,#10949,.T.);
#15280=ORIENTED_EDGE('',*,*,#10950,.T.);
#15281=ORIENTED_EDGE('',*,*,#10949,.F.);
#15282=ORIENTED_EDGE('',*,*,#10738,.T.);
#15283=ORIENTED_EDGE('',*,*,#10951,.T.);
#15284=ORIENTED_EDGE('',*,*,#10729,.T.);
#15285=ORIENTED_EDGE('',*,*,#10951,.F.);
#15286=ORIENTED_EDGE('',*,*,#10817,.F.);
#15287=ORIENTED_EDGE('',*,*,#10952,.T.);
#15288=ORIENTED_EDGE('',*,*,#10953,.T.);
#15289=ORIENTED_EDGE('',*,*,#10952,.F.);
#15290=ORIENTED_EDGE('',*,*,#10816,.F.);
#15291=ORIENTED_EDGE('',*,*,#10954,.T.);
#15292=ORIENTED_EDGE('',*,*,#10955,.T.);
#15293=ORIENTED_EDGE('',*,*,#10954,.F.);
#15294=ORIENTED_EDGE('',*,*,#10944,.F.);
#15295=ORIENTED_EDGE('',*,*,#10956,.F.);
#15296=ORIENTED_EDGE('',*,*,#10945,.F.);
#15297=ORIENTED_EDGE('',*,*,#10814,.F.);
#15298=ORIENTED_EDGE('',*,*,#10937,.F.);
#15299=ORIENTED_EDGE('',*,*,#10957,.F.);
#15300=ORIENTED_EDGE('',*,*,#10938,.F.);
#15301=ORIENTED_EDGE('',*,*,#10810,.F.);
#15302=ORIENTED_EDGE('',*,*,#10918,.F.);
#15303=ORIENTED_EDGE('',*,*,#10958,.F.);
#15304=ORIENTED_EDGE('',*,*,#10921,.F.);
#15305=ORIENTED_EDGE('',*,*,#10800,.F.);
#15306=ORIENTED_EDGE('',*,*,#10911,.F.);
#15307=ORIENTED_EDGE('',*,*,#10959,.F.);
#15308=ORIENTED_EDGE('',*,*,#10912,.F.);
#15309=ORIENTED_EDGE('',*,*,#10796,.F.);
#15310=ORIENTED_EDGE('',*,*,#10904,.F.);
#15311=ORIENTED_EDGE('',*,*,#10960,.F.);
#15312=ORIENTED_EDGE('',*,*,#10905,.F.);
#15313=ORIENTED_EDGE('',*,*,#10792,.F.);
#15314=ORIENTED_EDGE('',*,*,#10885,.F.);
#15315=ORIENTED_EDGE('',*,*,#10961,.F.);
#15316=ORIENTED_EDGE('',*,*,#10888,.F.);
#15317=ORIENTED_EDGE('',*,*,#10782,.F.);
#15318=ORIENTED_EDGE('',*,*,#10878,.F.);
#15319=ORIENTED_EDGE('',*,*,#10962,.F.);
#15320=ORIENTED_EDGE('',*,*,#10879,.F.);
#15321=ORIENTED_EDGE('',*,*,#10778,.F.);
#15322=ORIENTED_EDGE('',*,*,#10871,.F.);
#15323=ORIENTED_EDGE('',*,*,#10963,.F.);
#15324=ORIENTED_EDGE('',*,*,#10872,.F.);
#15325=ORIENTED_EDGE('',*,*,#10774,.F.);
#15326=ORIENTED_EDGE('',*,*,#10852,.F.);
#15327=ORIENTED_EDGE('',*,*,#10964,.F.);
#15328=ORIENTED_EDGE('',*,*,#10855,.F.);
#15329=ORIENTED_EDGE('',*,*,#10764,.F.);
#15330=ORIENTED_EDGE('',*,*,#10845,.F.);
#15331=ORIENTED_EDGE('',*,*,#10965,.F.);
#15332=ORIENTED_EDGE('',*,*,#10846,.F.);
#15333=ORIENTED_EDGE('',*,*,#10760,.F.);
#15334=ORIENTED_EDGE('',*,*,#10838,.F.);
#15335=ORIENTED_EDGE('',*,*,#10966,.F.);
#15336=ORIENTED_EDGE('',*,*,#10839,.F.);
#15337=ORIENTED_EDGE('',*,*,#10756,.F.);
#15338=ORIENTED_EDGE('',*,*,#10742,.F.);
#15339=ORIENTED_EDGE('',*,*,#10967,.F.);
#15340=ORIENTED_EDGE('',*,*,#10822,.F.);
#15341=ORIENTED_EDGE('',*,*,#10746,.F.);
#15342=ORIENTED_EDGE('',*,*,#10741,.F.);
#15343=ORIENTED_EDGE('',*,*,#10745,.T.);
#15344=ORIENTED_EDGE('',*,*,#10946,.F.);
#15345=ORIENTED_EDGE('',*,*,#10956,.T.);
#15346=ORIENTED_EDGE('',*,*,#10943,.F.);
#15347=ORIENTED_EDGE('',*,*,#10941,.T.);
#15348=ORIENTED_EDGE('',*,*,#10939,.F.);
#15349=ORIENTED_EDGE('',*,*,#10957,.T.);
#15350=ORIENTED_EDGE('',*,*,#10936,.F.);
#15351=ORIENTED_EDGE('',*,*,#10934,.T.);
#15352=ORIENTED_EDGE('',*,*,#10932,.F.);
#15353=ORIENTED_EDGE('',*,*,#10930,.T.);
#15354=ORIENTED_EDGE('',*,*,#10928,.F.);
#15355=ORIENTED_EDGE('',*,*,#10926,.T.);
#15356=ORIENTED_EDGE('',*,*,#10924,.F.);
#15357=ORIENTED_EDGE('',*,*,#10922,.T.);
#15358=ORIENTED_EDGE('',*,*,#10919,.F.);
#15359=ORIENTED_EDGE('',*,*,#10958,.T.);
#15360=ORIENTED_EDGE('',*,*,#10917,.F.);
#15361=ORIENTED_EDGE('',*,*,#10915,.T.);
#15362=ORIENTED_EDGE('',*,*,#10913,.F.);
#15363=ORIENTED_EDGE('',*,*,#10959,.T.);
#15364=ORIENTED_EDGE('',*,*,#10910,.F.);
#15365=ORIENTED_EDGE('',*,*,#10908,.T.);
#15366=ORIENTED_EDGE('',*,*,#10906,.F.);
#15367=ORIENTED_EDGE('',*,*,#10960,.T.);
#15368=ORIENTED_EDGE('',*,*,#10903,.F.);
#15369=ORIENTED_EDGE('',*,*,#10901,.T.);
#15370=ORIENTED_EDGE('',*,*,#10899,.F.);
#15371=ORIENTED_EDGE('',*,*,#10897,.T.);
#15372=ORIENTED_EDGE('',*,*,#10895,.F.);
#15373=ORIENTED_EDGE('',*,*,#10893,.T.);
#15374=ORIENTED_EDGE('',*,*,#10891,.F.);
#15375=ORIENTED_EDGE('',*,*,#10889,.T.);
#15376=ORIENTED_EDGE('',*,*,#10886,.F.);
#15377=ORIENTED_EDGE('',*,*,#10961,.T.);
#15378=ORIENTED_EDGE('',*,*,#10884,.F.);
#15379=ORIENTED_EDGE('',*,*,#10882,.T.);
#15380=ORIENTED_EDGE('',*,*,#10880,.F.);
#15381=ORIENTED_EDGE('',*,*,#10962,.T.);
#15382=ORIENTED_EDGE('',*,*,#10877,.F.);
#15383=ORIENTED_EDGE('',*,*,#10875,.T.);
#15384=ORIENTED_EDGE('',*,*,#10873,.F.);
#15385=ORIENTED_EDGE('',*,*,#10963,.T.);
#15386=ORIENTED_EDGE('',*,*,#10870,.F.);
#15387=ORIENTED_EDGE('',*,*,#10868,.T.);
#15388=ORIENTED_EDGE('',*,*,#10866,.F.);
#15389=ORIENTED_EDGE('',*,*,#10864,.T.);
#15390=ORIENTED_EDGE('',*,*,#10862,.F.);
#15391=ORIENTED_EDGE('',*,*,#10860,.T.);
#15392=ORIENTED_EDGE('',*,*,#10858,.F.);
#15393=ORIENTED_EDGE('',*,*,#10856,.T.);
#15394=ORIENTED_EDGE('',*,*,#10853,.F.);
#15395=ORIENTED_EDGE('',*,*,#10964,.T.);
#15396=ORIENTED_EDGE('',*,*,#10851,.F.);
#15397=ORIENTED_EDGE('',*,*,#10849,.T.);
#15398=ORIENTED_EDGE('',*,*,#10847,.F.);
#15399=ORIENTED_EDGE('',*,*,#10965,.T.);
#15400=ORIENTED_EDGE('',*,*,#10844,.F.);
#15401=ORIENTED_EDGE('',*,*,#10842,.T.);
#15402=ORIENTED_EDGE('',*,*,#10840,.F.);
#15403=ORIENTED_EDGE('',*,*,#10966,.T.);
#15404=ORIENTED_EDGE('',*,*,#10837,.F.);
#15405=ORIENTED_EDGE('',*,*,#10835,.T.);
#15406=ORIENTED_EDGE('',*,*,#10833,.F.);
#15407=ORIENTED_EDGE('',*,*,#10831,.T.);
#15408=ORIENTED_EDGE('',*,*,#10829,.F.);
#15409=ORIENTED_EDGE('',*,*,#10827,.T.);
#15410=ORIENTED_EDGE('',*,*,#10825,.F.);
#15411=ORIENTED_EDGE('',*,*,#10823,.T.);
#15412=ORIENTED_EDGE('',*,*,#10820,.F.);
#15413=ORIENTED_EDGE('',*,*,#10967,.T.);
#15414=ORIENTED_EDGE('',*,*,#10728,.T.);
#15415=ORIENTED_EDGE('',*,*,#10597,.T.);
#15416=ORIENTED_EDGE('',*,*,#10725,.T.);
#15417=ORIENTED_EDGE('',*,*,#10719,.T.);
#15418=ORIENTED_EDGE('',*,*,#10955,.F.);
#15419=ORIENTED_EDGE('',*,*,#10953,.F.);
#15420=ORIENTED_EDGE('',*,*,#10950,.F.);
#15421=ORIENTED_EDGE('',*,*,#10948,.F.);
#15422=ORIENTED_EDGE('',*,*,#10968,.F.);
#15423=ORIENTED_EDGE('',*,*,#10969,.T.);
#15424=ORIENTED_EDGE('',*,*,#10970,.F.);
#15425=ORIENTED_EDGE('',*,*,#10971,.T.);
#15426=ORIENTED_EDGE('',*,*,#10968,.T.);
#15427=ORIENTED_EDGE('',*,*,#10971,.F.);
#15428=ORIENTED_EDGE('',*,*,#10969,.F.);
#15429=ORIENTED_EDGE('',*,*,#10972,.T.);
#15430=ORIENTED_EDGE('',*,*,#10973,.F.);
#15431=ORIENTED_EDGE('',*,*,#10972,.F.);
#15432=ORIENTED_EDGE('',*,*,#10974,.F.);
#15433=ORIENTED_EDGE('',*,*,#10975,.T.);
#15434=ORIENTED_EDGE('',*,*,#10976,.F.);
#15435=ORIENTED_EDGE('',*,*,#10975,.F.);
#15436=ORIENTED_EDGE('',*,*,#10977,.F.);
#15437=ORIENTED_EDGE('',*,*,#10978,.T.);
#15438=ORIENTED_EDGE('',*,*,#10979,.F.);
#15439=ORIENTED_EDGE('',*,*,#10978,.F.);
#15440=ORIENTED_EDGE('',*,*,#10980,.F.);
#15441=ORIENTED_EDGE('',*,*,#10981,.T.);
#15442=ORIENTED_EDGE('',*,*,#10982,.F.);
#15443=ORIENTED_EDGE('',*,*,#10981,.F.);
#15444=ORIENTED_EDGE('',*,*,#10983,.F.);
#15445=ORIENTED_EDGE('',*,*,#10984,.T.);
#15446=ORIENTED_EDGE('',*,*,#10985,.F.);
#15447=ORIENTED_EDGE('',*,*,#10984,.F.);
#15448=ORIENTED_EDGE('',*,*,#10986,.T.);
#15449=ORIENTED_EDGE('',*,*,#10987,.T.);
#15450=ORIENTED_EDGE('',*,*,#10988,.F.);
#15451=ORIENTED_EDGE('',*,*,#10989,.F.);
#15452=ORIENTED_EDGE('',*,*,#10990,.T.);
#15453=ORIENTED_EDGE('',*,*,#10989,.T.);
#15454=ORIENTED_EDGE('',*,*,#10991,.F.);
#15455=ORIENTED_EDGE('',*,*,#10992,.F.);
#15456=ORIENTED_EDGE('',*,*,#10993,.T.);
#15457=ORIENTED_EDGE('',*,*,#10992,.T.);
#15458=ORIENTED_EDGE('',*,*,#10994,.F.);
#15459=ORIENTED_EDGE('',*,*,#10995,.F.);
#15460=ORIENTED_EDGE('',*,*,#10996,.T.);
#15461=ORIENTED_EDGE('',*,*,#10995,.T.);
#15462=ORIENTED_EDGE('',*,*,#10997,.F.);
#15463=ORIENTED_EDGE('',*,*,#10987,.F.);
#15464=ORIENTED_EDGE('',*,*,#10997,.T.);
#15465=ORIENTED_EDGE('',*,*,#10994,.T.);
#15466=ORIENTED_EDGE('',*,*,#10991,.T.);
#15467=ORIENTED_EDGE('',*,*,#10988,.T.);
#15468=ORIENTED_EDGE('',*,*,#10970,.T.);
#15469=ORIENTED_EDGE('',*,*,#10974,.T.);
#15470=ORIENTED_EDGE('',*,*,#10977,.T.);
#15471=ORIENTED_EDGE('',*,*,#10980,.T.);
#15472=ORIENTED_EDGE('',*,*,#10983,.T.);
#15473=ORIENTED_EDGE('',*,*,#10996,.F.);
#15474=ORIENTED_EDGE('',*,*,#10986,.F.);
#15475=ORIENTED_EDGE('',*,*,#10990,.F.);
#15476=ORIENTED_EDGE('',*,*,#10993,.F.);
#15477=ORIENTED_EDGE('',*,*,#10973,.T.);
#15478=ORIENTED_EDGE('',*,*,#10976,.T.);
#15479=ORIENTED_EDGE('',*,*,#10979,.T.);
#15480=ORIENTED_EDGE('',*,*,#10982,.T.);
#15481=ORIENTED_EDGE('',*,*,#10985,.T.);
#15482=ORIENTED_EDGE('',*,*,#10998,.F.);
#15483=ORIENTED_EDGE('',*,*,#10999,.T.);
#15484=ORIENTED_EDGE('',*,*,#11000,.T.);
#15485=ORIENTED_EDGE('',*,*,#11001,.T.);
#15486=ORIENTED_EDGE('',*,*,#11002,.F.);
#15487=ORIENTED_EDGE('',*,*,#11003,.T.);
#15488=ORIENTED_EDGE('',*,*,#10998,.T.);
#15489=ORIENTED_EDGE('',*,*,#11004,.T.);
#15490=ORIENTED_EDGE('',*,*,#11005,.F.);
#15491=ORIENTED_EDGE('',*,*,#11006,.T.);
#15492=ORIENTED_EDGE('',*,*,#11002,.T.);
#15493=ORIENTED_EDGE('',*,*,#11007,.T.);
#15494=ORIENTED_EDGE('',*,*,#11008,.F.);
#15495=ORIENTED_EDGE('',*,*,#11009,.T.);
#15496=ORIENTED_EDGE('',*,*,#11005,.T.);
#15497=ORIENTED_EDGE('',*,*,#11010,.T.);
#15498=ORIENTED_EDGE('',*,*,#11011,.F.);
#15499=ORIENTED_EDGE('',*,*,#11012,.T.);
#15500=ORIENTED_EDGE('',*,*,#11008,.T.);
#15501=ORIENTED_EDGE('',*,*,#11013,.T.);
#15502=ORIENTED_EDGE('',*,*,#11014,.F.);
#15503=ORIENTED_EDGE('',*,*,#11015,.T.);
#15504=ORIENTED_EDGE('',*,*,#11011,.T.);
#15505=ORIENTED_EDGE('',*,*,#11016,.T.);
#15506=ORIENTED_EDGE('',*,*,#11017,.F.);
#15507=ORIENTED_EDGE('',*,*,#11018,.T.);
#15508=ORIENTED_EDGE('',*,*,#11014,.T.);
#15509=ORIENTED_EDGE('',*,*,#11019,.T.);
#15510=ORIENTED_EDGE('',*,*,#11020,.F.);
#15511=ORIENTED_EDGE('',*,*,#11021,.T.);
#15512=ORIENTED_EDGE('',*,*,#11017,.T.);
#15513=ORIENTED_EDGE('',*,*,#11022,.T.);
#15514=ORIENTED_EDGE('',*,*,#11023,.F.);
#15515=ORIENTED_EDGE('',*,*,#11024,.T.);
#15516=ORIENTED_EDGE('',*,*,#11020,.T.);
#15517=ORIENTED_EDGE('',*,*,#11025,.T.);
#15518=ORIENTED_EDGE('',*,*,#11026,.F.);
#15519=ORIENTED_EDGE('',*,*,#11027,.T.);
#15520=ORIENTED_EDGE('',*,*,#11023,.T.);
#15521=ORIENTED_EDGE('',*,*,#11028,.T.);
#15522=ORIENTED_EDGE('',*,*,#11029,.F.);
#15523=ORIENTED_EDGE('',*,*,#11030,.T.);
#15524=ORIENTED_EDGE('',*,*,#11026,.T.);
#15525=ORIENTED_EDGE('',*,*,#11031,.T.);
#15526=ORIENTED_EDGE('',*,*,#11032,.F.);
#15527=ORIENTED_EDGE('',*,*,#11033,.T.);
#15528=ORIENTED_EDGE('',*,*,#11029,.T.);
#15529=ORIENTED_EDGE('',*,*,#11034,.T.);
#15530=ORIENTED_EDGE('',*,*,#11035,.F.);
#15531=ORIENTED_EDGE('',*,*,#11036,.T.);
#15532=ORIENTED_EDGE('',*,*,#11032,.T.);
#15533=ORIENTED_EDGE('',*,*,#11037,.T.);
#15534=ORIENTED_EDGE('',*,*,#11038,.F.);
#15535=ORIENTED_EDGE('',*,*,#11039,.T.);
#15536=ORIENTED_EDGE('',*,*,#11035,.T.);
#15537=ORIENTED_EDGE('',*,*,#11040,.T.);
#15538=ORIENTED_EDGE('',*,*,#11041,.F.);
#15539=ORIENTED_EDGE('',*,*,#11042,.T.);
#15540=ORIENTED_EDGE('',*,*,#11038,.T.);
#15541=ORIENTED_EDGE('',*,*,#11043,.T.);
#15542=ORIENTED_EDGE('',*,*,#11044,.F.);
#15543=ORIENTED_EDGE('',*,*,#11045,.T.);
#15544=ORIENTED_EDGE('',*,*,#11041,.T.);
#15545=ORIENTED_EDGE('',*,*,#11046,.T.);
#15546=ORIENTED_EDGE('',*,*,#11047,.F.);
#15547=ORIENTED_EDGE('',*,*,#11048,.T.);
#15548=ORIENTED_EDGE('',*,*,#11044,.T.);
#15549=ORIENTED_EDGE('',*,*,#11049,.T.);
#15550=ORIENTED_EDGE('',*,*,#11050,.F.);
#15551=ORIENTED_EDGE('',*,*,#11051,.T.);
#15552=ORIENTED_EDGE('',*,*,#11047,.T.);
#15553=ORIENTED_EDGE('',*,*,#11052,.T.);
#15554=ORIENTED_EDGE('',*,*,#11053,.F.);
#15555=ORIENTED_EDGE('',*,*,#11054,.T.);
#15556=ORIENTED_EDGE('',*,*,#11050,.T.);
#15557=ORIENTED_EDGE('',*,*,#11055,.T.);
#15558=ORIENTED_EDGE('',*,*,#11056,.F.);
#15559=ORIENTED_EDGE('',*,*,#11057,.T.);
#15560=ORIENTED_EDGE('',*,*,#11058,.T.);
#15561=ORIENTED_EDGE('',*,*,#11059,.F.);
#15562=ORIENTED_EDGE('',*,*,#11060,.F.);
#15563=ORIENTED_EDGE('',*,*,#11061,.T.);
#15564=ORIENTED_EDGE('',*,*,#11056,.T.);
#15565=ORIENTED_EDGE('',*,*,#11062,.F.);
#15566=ORIENTED_EDGE('',*,*,#11063,.F.);
#15567=ORIENTED_EDGE('',*,*,#11064,.T.);
#15568=ORIENTED_EDGE('',*,*,#11060,.T.);
#15569=ORIENTED_EDGE('',*,*,#11065,.F.);
#15570=ORIENTED_EDGE('',*,*,#11066,.F.);
#15571=ORIENTED_EDGE('',*,*,#11067,.T.);
#15572=ORIENTED_EDGE('',*,*,#11063,.T.);
#15573=ORIENTED_EDGE('',*,*,#11068,.F.);
#15574=ORIENTED_EDGE('',*,*,#11069,.F.);
#15575=ORIENTED_EDGE('',*,*,#11070,.T.);
#15576=ORIENTED_EDGE('',*,*,#11066,.T.);
#15577=ORIENTED_EDGE('',*,*,#11071,.F.);
#15578=ORIENTED_EDGE('',*,*,#11072,.F.);
#15579=ORIENTED_EDGE('',*,*,#11073,.T.);
#15580=ORIENTED_EDGE('',*,*,#11069,.T.);
#15581=ORIENTED_EDGE('',*,*,#11074,.F.);
#15582=ORIENTED_EDGE('',*,*,#11075,.F.);
#15583=ORIENTED_EDGE('',*,*,#11076,.T.);
#15584=ORIENTED_EDGE('',*,*,#11072,.T.);
#15585=ORIENTED_EDGE('',*,*,#11077,.F.);
#15586=ORIENTED_EDGE('',*,*,#11078,.F.);
#15587=ORIENTED_EDGE('',*,*,#11079,.T.);
#15588=ORIENTED_EDGE('',*,*,#11075,.T.);
#15589=ORIENTED_EDGE('',*,*,#11080,.F.);
#15590=ORIENTED_EDGE('',*,*,#11081,.F.);
#15591=ORIENTED_EDGE('',*,*,#11082,.T.);
#15592=ORIENTED_EDGE('',*,*,#11078,.T.);
#15593=ORIENTED_EDGE('',*,*,#11083,.F.);
#15594=ORIENTED_EDGE('',*,*,#11084,.F.);
#15595=ORIENTED_EDGE('',*,*,#11085,.T.);
#15596=ORIENTED_EDGE('',*,*,#11081,.T.);
#15597=ORIENTED_EDGE('',*,*,#11086,.F.);
#15598=ORIENTED_EDGE('',*,*,#11087,.F.);
#15599=ORIENTED_EDGE('',*,*,#11088,.T.);
#15600=ORIENTED_EDGE('',*,*,#11084,.T.);
#15601=ORIENTED_EDGE('',*,*,#11089,.F.);
#15602=ORIENTED_EDGE('',*,*,#11090,.F.);
#15603=ORIENTED_EDGE('',*,*,#11091,.T.);
#15604=ORIENTED_EDGE('',*,*,#11087,.T.);
#15605=ORIENTED_EDGE('',*,*,#11092,.F.);
#15606=ORIENTED_EDGE('',*,*,#11093,.F.);
#15607=ORIENTED_EDGE('',*,*,#11094,.T.);
#15608=ORIENTED_EDGE('',*,*,#11090,.T.);
#15609=ORIENTED_EDGE('',*,*,#11095,.F.);
#15610=ORIENTED_EDGE('',*,*,#11096,.F.);
#15611=ORIENTED_EDGE('',*,*,#11097,.T.);
#15612=ORIENTED_EDGE('',*,*,#11093,.T.);
#15613=ORIENTED_EDGE('',*,*,#11098,.F.);
#15614=ORIENTED_EDGE('',*,*,#11099,.F.);
#15615=ORIENTED_EDGE('',*,*,#11100,.T.);
#15616=ORIENTED_EDGE('',*,*,#11096,.T.);
#15617=ORIENTED_EDGE('',*,*,#11101,.F.);
#15618=ORIENTED_EDGE('',*,*,#11102,.F.);
#15619=ORIENTED_EDGE('',*,*,#11103,.T.);
#15620=ORIENTED_EDGE('',*,*,#11099,.T.);
#15621=ORIENTED_EDGE('',*,*,#11104,.F.);
#15622=ORIENTED_EDGE('',*,*,#11105,.F.);
#15623=ORIENTED_EDGE('',*,*,#11106,.T.);
#15624=ORIENTED_EDGE('',*,*,#11102,.T.);
#15625=ORIENTED_EDGE('',*,*,#11107,.F.);
#15626=ORIENTED_EDGE('',*,*,#11108,.F.);
#15627=ORIENTED_EDGE('',*,*,#11109,.T.);
#15628=ORIENTED_EDGE('',*,*,#11105,.T.);
#15629=ORIENTED_EDGE('',*,*,#11110,.F.);
#15630=ORIENTED_EDGE('',*,*,#11111,.F.);
#15631=ORIENTED_EDGE('',*,*,#11112,.T.);
#15632=ORIENTED_EDGE('',*,*,#11108,.T.);
#15633=ORIENTED_EDGE('',*,*,#11113,.F.);
#15634=ORIENTED_EDGE('',*,*,#11114,.F.);
#15635=ORIENTED_EDGE('',*,*,#11058,.F.);
#15636=ORIENTED_EDGE('',*,*,#11115,.F.);
#15637=ORIENTED_EDGE('',*,*,#11116,.F.);
#15638=ORIENTED_EDGE('',*,*,#11117,.F.);
#15639=ORIENTED_EDGE('',*,*,#11118,.T.);
#15640=ORIENTED_EDGE('',*,*,#11119,.F.);
#15641=ORIENTED_EDGE('',*,*,#11118,.F.);
#15642=ORIENTED_EDGE('',*,*,#11115,.T.);
#15643=ORIENTED_EDGE('',*,*,#11057,.F.);
#15644=ORIENTED_EDGE('',*,*,#11061,.F.);
#15645=ORIENTED_EDGE('',*,*,#11064,.F.);
#15646=ORIENTED_EDGE('',*,*,#11067,.F.);
#15647=ORIENTED_EDGE('',*,*,#11070,.F.);
#15648=ORIENTED_EDGE('',*,*,#11073,.F.);
#15649=ORIENTED_EDGE('',*,*,#11076,.F.);
#15650=ORIENTED_EDGE('',*,*,#11079,.F.);
#15651=ORIENTED_EDGE('',*,*,#11082,.F.);
#15652=ORIENTED_EDGE('',*,*,#11085,.F.);
#15653=ORIENTED_EDGE('',*,*,#11088,.F.);
#15654=ORIENTED_EDGE('',*,*,#11091,.F.);
#15655=ORIENTED_EDGE('',*,*,#11094,.F.);
#15656=ORIENTED_EDGE('',*,*,#11097,.F.);
#15657=ORIENTED_EDGE('',*,*,#11100,.F.);
#15658=ORIENTED_EDGE('',*,*,#11103,.F.);
#15659=ORIENTED_EDGE('',*,*,#11106,.F.);
#15660=ORIENTED_EDGE('',*,*,#11109,.F.);
#15661=ORIENTED_EDGE('',*,*,#11112,.F.);
#15662=ORIENTED_EDGE('',*,*,#11120,.F.);
#15663=ORIENTED_EDGE('',*,*,#11121,.F.);
#15664=ORIENTED_EDGE('',*,*,#10999,.F.);
#15665=ORIENTED_EDGE('',*,*,#11003,.F.);
#15666=ORIENTED_EDGE('',*,*,#11006,.F.);
#15667=ORIENTED_EDGE('',*,*,#11009,.F.);
#15668=ORIENTED_EDGE('',*,*,#11012,.F.);
#15669=ORIENTED_EDGE('',*,*,#11015,.F.);
#15670=ORIENTED_EDGE('',*,*,#11018,.F.);
#15671=ORIENTED_EDGE('',*,*,#11021,.F.);
#15672=ORIENTED_EDGE('',*,*,#11024,.F.);
#15673=ORIENTED_EDGE('',*,*,#11027,.F.);
#15674=ORIENTED_EDGE('',*,*,#11030,.F.);
#15675=ORIENTED_EDGE('',*,*,#11033,.F.);
#15676=ORIENTED_EDGE('',*,*,#11036,.F.);
#15677=ORIENTED_EDGE('',*,*,#11039,.F.);
#15678=ORIENTED_EDGE('',*,*,#11042,.F.);
#15679=ORIENTED_EDGE('',*,*,#11045,.F.);
#15680=ORIENTED_EDGE('',*,*,#11048,.F.);
#15681=ORIENTED_EDGE('',*,*,#11051,.F.);
#15682=ORIENTED_EDGE('',*,*,#11054,.F.);
#15683=ORIENTED_EDGE('',*,*,#11122,.F.);
#15684=ORIENTED_EDGE('',*,*,#11111,.T.);
#15685=ORIENTED_EDGE('',*,*,#11123,.F.);
#15686=ORIENTED_EDGE('',*,*,#11124,.F.);
#15687=ORIENTED_EDGE('',*,*,#11120,.T.);
#15688=ORIENTED_EDGE('',*,*,#11114,.T.);
#15689=ORIENTED_EDGE('',*,*,#11117,.T.);
#15690=ORIENTED_EDGE('',*,*,#11125,.F.);
#15691=ORIENTED_EDGE('',*,*,#11055,.F.);
#15692=ORIENTED_EDGE('',*,*,#11052,.F.);
#15693=ORIENTED_EDGE('',*,*,#11049,.F.);
#15694=ORIENTED_EDGE('',*,*,#11046,.F.);
#15695=ORIENTED_EDGE('',*,*,#11043,.F.);
#15696=ORIENTED_EDGE('',*,*,#11040,.F.);
#15697=ORIENTED_EDGE('',*,*,#11037,.F.);
#15698=ORIENTED_EDGE('',*,*,#11034,.F.);
#15699=ORIENTED_EDGE('',*,*,#11031,.F.);
#15700=ORIENTED_EDGE('',*,*,#11028,.F.);
#15701=ORIENTED_EDGE('',*,*,#11025,.F.);
#15702=ORIENTED_EDGE('',*,*,#11022,.F.);
#15703=ORIENTED_EDGE('',*,*,#11019,.F.);
#15704=ORIENTED_EDGE('',*,*,#11016,.F.);
#15705=ORIENTED_EDGE('',*,*,#11013,.F.);
#15706=ORIENTED_EDGE('',*,*,#11010,.F.);
#15707=ORIENTED_EDGE('',*,*,#11007,.F.);
#15708=ORIENTED_EDGE('',*,*,#11004,.F.);
#15709=ORIENTED_EDGE('',*,*,#11001,.F.);
#15710=ORIENTED_EDGE('',*,*,#11126,.F.);
#15711=ORIENTED_EDGE('',*,*,#11123,.T.);
#15712=ORIENTED_EDGE('',*,*,#11113,.T.);
#15713=ORIENTED_EDGE('',*,*,#11110,.T.);
#15714=ORIENTED_EDGE('',*,*,#11107,.T.);
#15715=ORIENTED_EDGE('',*,*,#11104,.T.);
#15716=ORIENTED_EDGE('',*,*,#11101,.T.);
#15717=ORIENTED_EDGE('',*,*,#11098,.T.);
#15718=ORIENTED_EDGE('',*,*,#11095,.T.);
#15719=ORIENTED_EDGE('',*,*,#11092,.T.);
#15720=ORIENTED_EDGE('',*,*,#11089,.T.);
#15721=ORIENTED_EDGE('',*,*,#11086,.T.);
#15722=ORIENTED_EDGE('',*,*,#11083,.T.);
#15723=ORIENTED_EDGE('',*,*,#11080,.T.);
#15724=ORIENTED_EDGE('',*,*,#11077,.T.);
#15725=ORIENTED_EDGE('',*,*,#11074,.T.);
#15726=ORIENTED_EDGE('',*,*,#11071,.T.);
#15727=ORIENTED_EDGE('',*,*,#11068,.T.);
#15728=ORIENTED_EDGE('',*,*,#11065,.T.);
#15729=ORIENTED_EDGE('',*,*,#11062,.T.);
#15730=ORIENTED_EDGE('',*,*,#11059,.T.);
#15731=ORIENTED_EDGE('',*,*,#11053,.T.);
#15732=ORIENTED_EDGE('',*,*,#11125,.T.);
#15733=ORIENTED_EDGE('',*,*,#11116,.T.);
#15734=ORIENTED_EDGE('',*,*,#11122,.T.);
#15735=ORIENTED_EDGE('',*,*,#11127,.F.);
#15736=ORIENTED_EDGE('',*,*,#11128,.T.);
#15737=ORIENTED_EDGE('',*,*,#11129,.T.);
#15738=ORIENTED_EDGE('',*,*,#11130,.F.);
#15739=ORIENTED_EDGE('',*,*,#11131,.F.);
#15740=ORIENTED_EDGE('',*,*,#11132,.T.);
#15741=ORIENTED_EDGE('',*,*,#11133,.T.);
#15742=ORIENTED_EDGE('',*,*,#11128,.F.);
#15743=ORIENTED_EDGE('',*,*,#11134,.F.);
#15744=ORIENTED_EDGE('',*,*,#11135,.T.);
#15745=ORIENTED_EDGE('',*,*,#11136,.T.);
#15746=ORIENTED_EDGE('',*,*,#11132,.F.);
#15747=ORIENTED_EDGE('',*,*,#11137,.F.);
#15748=ORIENTED_EDGE('',*,*,#11138,.T.);
#15749=ORIENTED_EDGE('',*,*,#11139,.T.);
#15750=ORIENTED_EDGE('',*,*,#11135,.F.);
#15751=ORIENTED_EDGE('',*,*,#11140,.F.);
#15752=ORIENTED_EDGE('',*,*,#11141,.T.);
#15753=ORIENTED_EDGE('',*,*,#11142,.T.);
#15754=ORIENTED_EDGE('',*,*,#11138,.F.);
#15755=ORIENTED_EDGE('',*,*,#11143,.F.);
#15756=ORIENTED_EDGE('',*,*,#11130,.T.);
#15757=ORIENTED_EDGE('',*,*,#11144,.T.);
#15758=ORIENTED_EDGE('',*,*,#11141,.F.);
#15759=ORIENTED_EDGE('',*,*,#11144,.F.);
#15760=ORIENTED_EDGE('',*,*,#11129,.F.);
#15761=ORIENTED_EDGE('',*,*,#11133,.F.);
#15762=ORIENTED_EDGE('',*,*,#11136,.F.);
#15763=ORIENTED_EDGE('',*,*,#11139,.F.);
#15764=ORIENTED_EDGE('',*,*,#11142,.F.);
#15765=ORIENTED_EDGE('',*,*,#11145,.T.);
#15766=ORIENTED_EDGE('',*,*,#11121,.T.);
#15767=ORIENTED_EDGE('',*,*,#11124,.T.);
#15768=ORIENTED_EDGE('',*,*,#11126,.T.);
#15769=ORIENTED_EDGE('',*,*,#11000,.F.);
#15770=ORIENTED_EDGE('',*,*,#11145,.F.);
#15771=ORIENTED_EDGE('',*,*,#11146,.T.);
#15772=ORIENTED_EDGE('',*,*,#11147,.T.);
#15773=ORIENTED_EDGE('',*,*,#11146,.F.);
#15774=ORIENTED_EDGE('',*,*,#11147,.F.);
#15775=ORIENTED_EDGE('',*,*,#11127,.T.);
#15776=ORIENTED_EDGE('',*,*,#11143,.T.);
#15777=ORIENTED_EDGE('',*,*,#11140,.T.);
#15778=ORIENTED_EDGE('',*,*,#11137,.T.);
#15779=ORIENTED_EDGE('',*,*,#11134,.T.);
#15780=ORIENTED_EDGE('',*,*,#11131,.T.);
#15781=ORIENTED_EDGE('',*,*,#11119,.T.);
#15782=ORIENTED_EDGE('',*,*,#11148,.F.);
#15783=ORIENTED_EDGE('',*,*,#11149,.T.);
#15784=ORIENTED_EDGE('',*,*,#11150,.T.);
#15785=ORIENTED_EDGE('',*,*,#11149,.F.);
#15786=ORIENTED_EDGE('',*,*,#11148,.T.);
#15787=ORIENTED_EDGE('',*,*,#11150,.F.);
#15788=ORIENTED_EDGE('',*,*,#11151,.T.);
#15789=ORIENTED_EDGE('',*,*,#11152,.T.);
#15790=ORIENTED_EDGE('',*,*,#11153,.T.);
#15791=ORIENTED_EDGE('',*,*,#11154,.T.);
#15792=ORIENTED_EDGE('',*,*,#11155,.T.);
#15793=ORIENTED_EDGE('',*,*,#11154,.F.);
#15794=ORIENTED_EDGE('',*,*,#11156,.T.);
#15795=ORIENTED_EDGE('',*,*,#11157,.T.);
#15796=ORIENTED_EDGE('',*,*,#11158,.T.);
#15797=ORIENTED_EDGE('',*,*,#11159,.T.);
#15798=ORIENTED_EDGE('',*,*,#11151,.F.);
#15799=ORIENTED_EDGE('',*,*,#11160,.T.);
#15800=ORIENTED_EDGE('',*,*,#11161,.T.);
#15801=ORIENTED_EDGE('',*,*,#11162,.T.);
#15802=ORIENTED_EDGE('',*,*,#11158,.F.);
#15803=ORIENTED_EDGE('',*,*,#11163,.T.);
#15804=ORIENTED_EDGE('',*,*,#11164,.T.);
#15805=ORIENTED_EDGE('',*,*,#11165,.T.);
#15806=ORIENTED_EDGE('',*,*,#11161,.F.);
#15807=ORIENTED_EDGE('',*,*,#11166,.T.);
#15808=ORIENTED_EDGE('',*,*,#11167,.T.);
#15809=ORIENTED_EDGE('',*,*,#11168,.T.);
#15810=ORIENTED_EDGE('',*,*,#11164,.F.);
#15811=ORIENTED_EDGE('',*,*,#11169,.T.);
#15812=ORIENTED_EDGE('',*,*,#11170,.T.);
#15813=ORIENTED_EDGE('',*,*,#11171,.T.);
#15814=ORIENTED_EDGE('',*,*,#11167,.F.);
#15815=ORIENTED_EDGE('',*,*,#11172,.T.);
#15816=ORIENTED_EDGE('',*,*,#11173,.T.);
#15817=ORIENTED_EDGE('',*,*,#11174,.T.);
#15818=ORIENTED_EDGE('',*,*,#11170,.F.);
#15819=ORIENTED_EDGE('',*,*,#11175,.T.);
#15820=ORIENTED_EDGE('',*,*,#11176,.F.);
#15821=ORIENTED_EDGE('',*,*,#11177,.T.);
#15822=ORIENTED_EDGE('',*,*,#11178,.F.);
#15823=ORIENTED_EDGE('',*,*,#11179,.T.);
#15824=ORIENTED_EDGE('',*,*,#11180,.T.);
#15825=ORIENTED_EDGE('',*,*,#11181,.T.);
#15826=ORIENTED_EDGE('',*,*,#11182,.F.);
#15827=ORIENTED_EDGE('',*,*,#11183,.F.);
#15828=ORIENTED_EDGE('',*,*,#11184,.T.);
#15829=ORIENTED_EDGE('',*,*,#11185,.T.);
#15830=ORIENTED_EDGE('',*,*,#11180,.F.);
#15831=ORIENTED_EDGE('',*,*,#11186,.F.);
#15832=ORIENTED_EDGE('',*,*,#11187,.T.);
#15833=ORIENTED_EDGE('',*,*,#11188,.T.);
#15834=ORIENTED_EDGE('',*,*,#11184,.F.);
#15835=ORIENTED_EDGE('',*,*,#11189,.F.);
#15836=ORIENTED_EDGE('',*,*,#11190,.T.);
#15837=ORIENTED_EDGE('',*,*,#11191,.T.);
#15838=ORIENTED_EDGE('',*,*,#11187,.F.);
#15839=ORIENTED_EDGE('',*,*,#11192,.F.);
#15840=ORIENTED_EDGE('',*,*,#11193,.T.);
#15841=ORIENTED_EDGE('',*,*,#11194,.T.);
#15842=ORIENTED_EDGE('',*,*,#11190,.F.);
#15843=ORIENTED_EDGE('',*,*,#11195,.F.);
#15844=ORIENTED_EDGE('',*,*,#11196,.T.);
#15845=ORIENTED_EDGE('',*,*,#11197,.T.);
#15846=ORIENTED_EDGE('',*,*,#11193,.F.);
#15847=ORIENTED_EDGE('',*,*,#11198,.F.);
#15848=ORIENTED_EDGE('',*,*,#11199,.T.);
#15849=ORIENTED_EDGE('',*,*,#11200,.T.);
#15850=ORIENTED_EDGE('',*,*,#11196,.F.);
#15851=ORIENTED_EDGE('',*,*,#11201,.F.);
#15852=ORIENTED_EDGE('',*,*,#11202,.F.);
#15853=ORIENTED_EDGE('',*,*,#11203,.F.);
#15854=ORIENTED_EDGE('',*,*,#11204,.F.);
#15855=ORIENTED_EDGE('',*,*,#11205,.T.);
#15856=ORIENTED_EDGE('',*,*,#11206,.T.);
#15857=ORIENTED_EDGE('',*,*,#11207,.T.);
#15858=ORIENTED_EDGE('',*,*,#11208,.T.);
#15859=ORIENTED_EDGE('',*,*,#11209,.T.);
#15860=ORIENTED_EDGE('',*,*,#11210,.T.);
#15861=ORIENTED_EDGE('',*,*,#11209,.F.);
#15862=ORIENTED_EDGE('',*,*,#11211,.T.);
#15863=ORIENTED_EDGE('',*,*,#11212,.T.);
#15864=ORIENTED_EDGE('',*,*,#11213,.T.);
#15865=ORIENTED_EDGE('',*,*,#11214,.T.);
#15866=ORIENTED_EDGE('',*,*,#11206,.F.);
#15867=ORIENTED_EDGE('',*,*,#11215,.T.);
#15868=ORIENTED_EDGE('',*,*,#11216,.T.);
#15869=ORIENTED_EDGE('',*,*,#11217,.T.);
#15870=ORIENTED_EDGE('',*,*,#11213,.F.);
#15871=ORIENTED_EDGE('',*,*,#11218,.T.);
#15872=ORIENTED_EDGE('',*,*,#11219,.T.);
#15873=ORIENTED_EDGE('',*,*,#11220,.T.);
#15874=ORIENTED_EDGE('',*,*,#11216,.F.);
#15875=ORIENTED_EDGE('',*,*,#11221,.T.);
#15876=ORIENTED_EDGE('',*,*,#11222,.T.);
#15877=ORIENTED_EDGE('',*,*,#11223,.T.);
#15878=ORIENTED_EDGE('',*,*,#11219,.F.);
#15879=ORIENTED_EDGE('',*,*,#11224,.T.);
#15880=ORIENTED_EDGE('',*,*,#11225,.T.);
#15881=ORIENTED_EDGE('',*,*,#11226,.T.);
#15882=ORIENTED_EDGE('',*,*,#11222,.F.);
#15883=ORIENTED_EDGE('',*,*,#11227,.T.);
#15884=ORIENTED_EDGE('',*,*,#11228,.T.);
#15885=ORIENTED_EDGE('',*,*,#11229,.T.);
#15886=ORIENTED_EDGE('',*,*,#11225,.F.);
#15887=ORIENTED_EDGE('',*,*,#11230,.T.);
#15888=ORIENTED_EDGE('',*,*,#11231,.F.);
#15889=ORIENTED_EDGE('',*,*,#11232,.T.);
#15890=ORIENTED_EDGE('',*,*,#11233,.F.);
#15891=ORIENTED_EDGE('',*,*,#11234,.T.);
#15892=ORIENTED_EDGE('',*,*,#11235,.T.);
#15893=ORIENTED_EDGE('',*,*,#11236,.T.);
#15894=ORIENTED_EDGE('',*,*,#11237,.F.);
#15895=ORIENTED_EDGE('',*,*,#11238,.F.);
#15896=ORIENTED_EDGE('',*,*,#11239,.T.);
#15897=ORIENTED_EDGE('',*,*,#11240,.T.);
#15898=ORIENTED_EDGE('',*,*,#11235,.F.);
#15899=ORIENTED_EDGE('',*,*,#11241,.F.);
#15900=ORIENTED_EDGE('',*,*,#11242,.T.);
#15901=ORIENTED_EDGE('',*,*,#11243,.T.);
#15902=ORIENTED_EDGE('',*,*,#11239,.F.);
#15903=ORIENTED_EDGE('',*,*,#11244,.F.);
#15904=ORIENTED_EDGE('',*,*,#11245,.T.);
#15905=ORIENTED_EDGE('',*,*,#11246,.T.);
#15906=ORIENTED_EDGE('',*,*,#11242,.F.);
#15907=ORIENTED_EDGE('',*,*,#11247,.F.);
#15908=ORIENTED_EDGE('',*,*,#11248,.T.);
#15909=ORIENTED_EDGE('',*,*,#11249,.T.);
#15910=ORIENTED_EDGE('',*,*,#11245,.F.);
#15911=ORIENTED_EDGE('',*,*,#11250,.F.);
#15912=ORIENTED_EDGE('',*,*,#11251,.T.);
#15913=ORIENTED_EDGE('',*,*,#11252,.T.);
#15914=ORIENTED_EDGE('',*,*,#11248,.F.);
#15915=ORIENTED_EDGE('',*,*,#11253,.F.);
#15916=ORIENTED_EDGE('',*,*,#11254,.T.);
#15917=ORIENTED_EDGE('',*,*,#11255,.T.);
#15918=ORIENTED_EDGE('',*,*,#11251,.F.);
#15919=ORIENTED_EDGE('',*,*,#11256,.F.);
#15920=ORIENTED_EDGE('',*,*,#11257,.F.);
#15921=ORIENTED_EDGE('',*,*,#11258,.F.);
#15922=ORIENTED_EDGE('',*,*,#11259,.F.);
#15923=ORIENTED_EDGE('',*,*,#11260,.T.);
#15924=ORIENTED_EDGE('',*,*,#11261,.T.);
#15925=ORIENTED_EDGE('',*,*,#11262,.T.);
#15926=ORIENTED_EDGE('',*,*,#11263,.T.);
#15927=ORIENTED_EDGE('',*,*,#11264,.T.);
#15928=ORIENTED_EDGE('',*,*,#11265,.T.);
#15929=ORIENTED_EDGE('',*,*,#11264,.F.);
#15930=ORIENTED_EDGE('',*,*,#11266,.T.);
#15931=ORIENTED_EDGE('',*,*,#11267,.T.);
#15932=ORIENTED_EDGE('',*,*,#11268,.T.);
#15933=ORIENTED_EDGE('',*,*,#11269,.T.);
#15934=ORIENTED_EDGE('',*,*,#11261,.F.);
#15935=ORIENTED_EDGE('',*,*,#11270,.T.);
#15936=ORIENTED_EDGE('',*,*,#11271,.T.);
#15937=ORIENTED_EDGE('',*,*,#11272,.T.);
#15938=ORIENTED_EDGE('',*,*,#11268,.F.);
#15939=ORIENTED_EDGE('',*,*,#11273,.T.);
#15940=ORIENTED_EDGE('',*,*,#11274,.T.);
#15941=ORIENTED_EDGE('',*,*,#11275,.T.);
#15942=ORIENTED_EDGE('',*,*,#11271,.F.);
#15943=ORIENTED_EDGE('',*,*,#11276,.T.);
#15944=ORIENTED_EDGE('',*,*,#11277,.T.);
#15945=ORIENTED_EDGE('',*,*,#11278,.T.);
#15946=ORIENTED_EDGE('',*,*,#11274,.F.);
#15947=ORIENTED_EDGE('',*,*,#11279,.T.);
#15948=ORIENTED_EDGE('',*,*,#11280,.T.);
#15949=ORIENTED_EDGE('',*,*,#11281,.T.);
#15950=ORIENTED_EDGE('',*,*,#11277,.F.);
#15951=ORIENTED_EDGE('',*,*,#11282,.T.);
#15952=ORIENTED_EDGE('',*,*,#11283,.T.);
#15953=ORIENTED_EDGE('',*,*,#11284,.T.);
#15954=ORIENTED_EDGE('',*,*,#11280,.F.);
#15955=ORIENTED_EDGE('',*,*,#11285,.T.);
#15956=ORIENTED_EDGE('',*,*,#11286,.F.);
#15957=ORIENTED_EDGE('',*,*,#11287,.T.);
#15958=ORIENTED_EDGE('',*,*,#11288,.F.);
#15959=ORIENTED_EDGE('',*,*,#11289,.T.);
#15960=ORIENTED_EDGE('',*,*,#11290,.T.);
#15961=ORIENTED_EDGE('',*,*,#11291,.T.);
#15962=ORIENTED_EDGE('',*,*,#11292,.F.);
#15963=ORIENTED_EDGE('',*,*,#11293,.F.);
#15964=ORIENTED_EDGE('',*,*,#11294,.T.);
#15965=ORIENTED_EDGE('',*,*,#11295,.T.);
#15966=ORIENTED_EDGE('',*,*,#11290,.F.);
#15967=ORIENTED_EDGE('',*,*,#11296,.F.);
#15968=ORIENTED_EDGE('',*,*,#11297,.T.);
#15969=ORIENTED_EDGE('',*,*,#11298,.T.);
#15970=ORIENTED_EDGE('',*,*,#11294,.F.);
#15971=ORIENTED_EDGE('',*,*,#11299,.F.);
#15972=ORIENTED_EDGE('',*,*,#11300,.T.);
#15973=ORIENTED_EDGE('',*,*,#11301,.T.);
#15974=ORIENTED_EDGE('',*,*,#11297,.F.);
#15975=ORIENTED_EDGE('',*,*,#11302,.F.);
#15976=ORIENTED_EDGE('',*,*,#11303,.T.);
#15977=ORIENTED_EDGE('',*,*,#11304,.T.);
#15978=ORIENTED_EDGE('',*,*,#11300,.F.);
#15979=ORIENTED_EDGE('',*,*,#11305,.F.);
#15980=ORIENTED_EDGE('',*,*,#11306,.T.);
#15981=ORIENTED_EDGE('',*,*,#11307,.T.);
#15982=ORIENTED_EDGE('',*,*,#11303,.F.);
#15983=ORIENTED_EDGE('',*,*,#11308,.F.);
#15984=ORIENTED_EDGE('',*,*,#11309,.T.);
#15985=ORIENTED_EDGE('',*,*,#11310,.T.);
#15986=ORIENTED_EDGE('',*,*,#11306,.F.);
#15987=ORIENTED_EDGE('',*,*,#11311,.F.);
#15988=ORIENTED_EDGE('',*,*,#11312,.F.);
#15989=ORIENTED_EDGE('',*,*,#11313,.F.);
#15990=ORIENTED_EDGE('',*,*,#11314,.F.);
#15991=ORIENTED_EDGE('',*,*,#11315,.T.);
#15992=ORIENTED_EDGE('',*,*,#11263,.F.);
#15993=ORIENTED_EDGE('',*,*,#11316,.T.);
#15994=ORIENTED_EDGE('',*,*,#11292,.T.);
#15995=ORIENTED_EDGE('',*,*,#11317,.T.);
#15996=ORIENTED_EDGE('',*,*,#11266,.F.);
#15997=ORIENTED_EDGE('',*,*,#11312,.T.);
#15998=ORIENTED_EDGE('',*,*,#11318,.T.);
#15999=ORIENTED_EDGE('',*,*,#11309,.F.);
#16000=ORIENTED_EDGE('',*,*,#11319,.F.);
#16001=ORIENTED_EDGE('',*,*,#11317,.F.);
#16002=ORIENTED_EDGE('',*,*,#11291,.F.);
#16003=ORIENTED_EDGE('',*,*,#11295,.F.);
#16004=ORIENTED_EDGE('',*,*,#11298,.F.);
#16005=ORIENTED_EDGE('',*,*,#11301,.F.);
#16006=ORIENTED_EDGE('',*,*,#11304,.F.);
#16007=ORIENTED_EDGE('',*,*,#11307,.F.);
#16008=ORIENTED_EDGE('',*,*,#11310,.F.);
#16009=ORIENTED_EDGE('',*,*,#11318,.F.);
#16010=ORIENTED_EDGE('',*,*,#11315,.F.);
#16011=ORIENTED_EDGE('',*,*,#11320,.F.);
#16012=ORIENTED_EDGE('',*,*,#11287,.F.);
#16013=ORIENTED_EDGE('',*,*,#11321,.F.);
#16014=ORIENTED_EDGE('',*,*,#11285,.F.);
#16015=ORIENTED_EDGE('',*,*,#11282,.F.);
#16016=ORIENTED_EDGE('',*,*,#11279,.F.);
#16017=ORIENTED_EDGE('',*,*,#11276,.F.);
#16018=ORIENTED_EDGE('',*,*,#11273,.F.);
#16019=ORIENTED_EDGE('',*,*,#11270,.F.);
#16020=ORIENTED_EDGE('',*,*,#11267,.F.);
#16021=ORIENTED_EDGE('',*,*,#11316,.F.);
#16022=ORIENTED_EDGE('',*,*,#11262,.F.);
#16023=ORIENTED_EDGE('',*,*,#11269,.F.);
#16024=ORIENTED_EDGE('',*,*,#11272,.F.);
#16025=ORIENTED_EDGE('',*,*,#11275,.F.);
#16026=ORIENTED_EDGE('',*,*,#11278,.F.);
#16027=ORIENTED_EDGE('',*,*,#11281,.F.);
#16028=ORIENTED_EDGE('',*,*,#11284,.F.);
#16029=ORIENTED_EDGE('',*,*,#11322,.F.);
#16030=ORIENTED_EDGE('',*,*,#11289,.F.);
#16031=ORIENTED_EDGE('',*,*,#11323,.F.);
#16032=ORIENTED_EDGE('',*,*,#11313,.T.);
#16033=ORIENTED_EDGE('',*,*,#11319,.T.);
#16034=ORIENTED_EDGE('',*,*,#11311,.T.);
#16035=ORIENTED_EDGE('',*,*,#11308,.T.);
#16036=ORIENTED_EDGE('',*,*,#11305,.T.);
#16037=ORIENTED_EDGE('',*,*,#11302,.T.);
#16038=ORIENTED_EDGE('',*,*,#11299,.T.);
#16039=ORIENTED_EDGE('',*,*,#11296,.T.);
#16040=ORIENTED_EDGE('',*,*,#11293,.T.);
#16041=ORIENTED_EDGE('',*,*,#11286,.T.);
#16042=ORIENTED_EDGE('',*,*,#11322,.T.);
#16043=ORIENTED_EDGE('',*,*,#11283,.F.);
#16044=ORIENTED_EDGE('',*,*,#11321,.T.);
#16045=ORIENTED_EDGE('',*,*,#11208,.F.);
#16046=ORIENTED_EDGE('',*,*,#11324,.T.);
#16047=ORIENTED_EDGE('',*,*,#11237,.T.);
#16048=ORIENTED_EDGE('',*,*,#11325,.T.);
#16049=ORIENTED_EDGE('',*,*,#11211,.F.);
#16050=ORIENTED_EDGE('',*,*,#11257,.T.);
#16051=ORIENTED_EDGE('',*,*,#11326,.T.);
#16052=ORIENTED_EDGE('',*,*,#11254,.F.);
#16053=ORIENTED_EDGE('',*,*,#11327,.F.);
#16054=ORIENTED_EDGE('',*,*,#11325,.F.);
#16055=ORIENTED_EDGE('',*,*,#11236,.F.);
#16056=ORIENTED_EDGE('',*,*,#11240,.F.);
#16057=ORIENTED_EDGE('',*,*,#11243,.F.);
#16058=ORIENTED_EDGE('',*,*,#11246,.F.);
#16059=ORIENTED_EDGE('',*,*,#11249,.F.);
#16060=ORIENTED_EDGE('',*,*,#11252,.F.);
#16061=ORIENTED_EDGE('',*,*,#11255,.F.);
#16062=ORIENTED_EDGE('',*,*,#11326,.F.);
#16063=ORIENTED_EDGE('',*,*,#11260,.F.);
#16064=ORIENTED_EDGE('',*,*,#11328,.F.);
#16065=ORIENTED_EDGE('',*,*,#11232,.F.);
#16066=ORIENTED_EDGE('',*,*,#11329,.F.);
#16067=ORIENTED_EDGE('',*,*,#11230,.F.);
#16068=ORIENTED_EDGE('',*,*,#11227,.F.);
#16069=ORIENTED_EDGE('',*,*,#11224,.F.);
#16070=ORIENTED_EDGE('',*,*,#11221,.F.);
#16071=ORIENTED_EDGE('',*,*,#11218,.F.);
#16072=ORIENTED_EDGE('',*,*,#11215,.F.);
#16073=ORIENTED_EDGE('',*,*,#11212,.F.);
#16074=ORIENTED_EDGE('',*,*,#11324,.F.);
#16075=ORIENTED_EDGE('',*,*,#11207,.F.);
#16076=ORIENTED_EDGE('',*,*,#11214,.F.);
#16077=ORIENTED_EDGE('',*,*,#11217,.F.);
#16078=ORIENTED_EDGE('',*,*,#11220,.F.);
#16079=ORIENTED_EDGE('',*,*,#11223,.F.);
#16080=ORIENTED_EDGE('',*,*,#11226,.F.);
#16081=ORIENTED_EDGE('',*,*,#11229,.F.);
#16082=ORIENTED_EDGE('',*,*,#11330,.F.);
#16083=ORIENTED_EDGE('',*,*,#11234,.F.);
#16084=ORIENTED_EDGE('',*,*,#11331,.F.);
#16085=ORIENTED_EDGE('',*,*,#11258,.T.);
#16086=ORIENTED_EDGE('',*,*,#11327,.T.);
#16087=ORIENTED_EDGE('',*,*,#11256,.T.);
#16088=ORIENTED_EDGE('',*,*,#11253,.T.);
#16089=ORIENTED_EDGE('',*,*,#11250,.T.);
#16090=ORIENTED_EDGE('',*,*,#11247,.T.);
#16091=ORIENTED_EDGE('',*,*,#11244,.T.);
#16092=ORIENTED_EDGE('',*,*,#11241,.T.);
#16093=ORIENTED_EDGE('',*,*,#11238,.T.);
#16094=ORIENTED_EDGE('',*,*,#11231,.T.);
#16095=ORIENTED_EDGE('',*,*,#11330,.T.);
#16096=ORIENTED_EDGE('',*,*,#11228,.F.);
#16097=ORIENTED_EDGE('',*,*,#11329,.T.);
#16098=ORIENTED_EDGE('',*,*,#11153,.F.);
#16099=ORIENTED_EDGE('',*,*,#11332,.T.);
#16100=ORIENTED_EDGE('',*,*,#11182,.T.);
#16101=ORIENTED_EDGE('',*,*,#11333,.T.);
#16102=ORIENTED_EDGE('',*,*,#11156,.F.);
#16103=ORIENTED_EDGE('',*,*,#11202,.T.);
#16104=ORIENTED_EDGE('',*,*,#11334,.T.);
#16105=ORIENTED_EDGE('',*,*,#11199,.F.);
#16106=ORIENTED_EDGE('',*,*,#11335,.F.);
#16107=ORIENTED_EDGE('',*,*,#11333,.F.);
#16108=ORIENTED_EDGE('',*,*,#11181,.F.);
#16109=ORIENTED_EDGE('',*,*,#11185,.F.);
#16110=ORIENTED_EDGE('',*,*,#11188,.F.);
#16111=ORIENTED_EDGE('',*,*,#11191,.F.);
#16112=ORIENTED_EDGE('',*,*,#11194,.F.);
#16113=ORIENTED_EDGE('',*,*,#11197,.F.);
#16114=ORIENTED_EDGE('',*,*,#11200,.F.);
#16115=ORIENTED_EDGE('',*,*,#11334,.F.);
#16116=ORIENTED_EDGE('',*,*,#11205,.F.);
#16117=ORIENTED_EDGE('',*,*,#11336,.F.);
#16118=ORIENTED_EDGE('',*,*,#11177,.F.);
#16119=ORIENTED_EDGE('',*,*,#11337,.F.);
#16120=ORIENTED_EDGE('',*,*,#11175,.F.);
#16121=ORIENTED_EDGE('',*,*,#11172,.F.);
#16122=ORIENTED_EDGE('',*,*,#11169,.F.);
#16123=ORIENTED_EDGE('',*,*,#11166,.F.);
#16124=ORIENTED_EDGE('',*,*,#11163,.F.);
#16125=ORIENTED_EDGE('',*,*,#11160,.F.);
#16126=ORIENTED_EDGE('',*,*,#11157,.F.);
#16127=ORIENTED_EDGE('',*,*,#11332,.F.);
#16128=ORIENTED_EDGE('',*,*,#11152,.F.);
#16129=ORIENTED_EDGE('',*,*,#11159,.F.);
#16130=ORIENTED_EDGE('',*,*,#11162,.F.);
#16131=ORIENTED_EDGE('',*,*,#11165,.F.);
#16132=ORIENTED_EDGE('',*,*,#11168,.F.);
#16133=ORIENTED_EDGE('',*,*,#11171,.F.);
#16134=ORIENTED_EDGE('',*,*,#11174,.F.);
#16135=ORIENTED_EDGE('',*,*,#11338,.F.);
#16136=ORIENTED_EDGE('',*,*,#11179,.F.);
#16137=ORIENTED_EDGE('',*,*,#11339,.F.);
#16138=ORIENTED_EDGE('',*,*,#11203,.T.);
#16139=ORIENTED_EDGE('',*,*,#11335,.T.);
#16140=ORIENTED_EDGE('',*,*,#11201,.T.);
#16141=ORIENTED_EDGE('',*,*,#11198,.T.);
#16142=ORIENTED_EDGE('',*,*,#11195,.T.);
#16143=ORIENTED_EDGE('',*,*,#11192,.T.);
#16144=ORIENTED_EDGE('',*,*,#11189,.T.);
#16145=ORIENTED_EDGE('',*,*,#11186,.T.);
#16146=ORIENTED_EDGE('',*,*,#11183,.T.);
#16147=ORIENTED_EDGE('',*,*,#11176,.T.);
#16148=ORIENTED_EDGE('',*,*,#11338,.T.);
#16149=ORIENTED_EDGE('',*,*,#11173,.F.);
#16150=ORIENTED_EDGE('',*,*,#11337,.T.);
#16151=ORIENTED_EDGE('',*,*,#11210,.F.);
#16152=ORIENTED_EDGE('',*,*,#11155,.F.);
#16153=ORIENTED_EDGE('',*,*,#11265,.F.);
#16154=ORIENTED_EDGE('',*,*,#11340,.F.);
#16155=ORIENTED_EDGE('',*,*,#11341,.F.);
#16156=ORIENTED_EDGE('',*,*,#11341,.T.);
#16157=ORIENTED_EDGE('',*,*,#11342,.F.);
#16158=ORIENTED_EDGE('',*,*,#11343,.T.);
#16159=ORIENTED_EDGE('',*,*,#11344,.T.);
#16160=ORIENTED_EDGE('',*,*,#11343,.F.);
#16161=ORIENTED_EDGE('',*,*,#11342,.T.);
#16162=ORIENTED_EDGE('',*,*,#11323,.T.);
#16163=ORIENTED_EDGE('',*,*,#11288,.T.);
#16164=ORIENTED_EDGE('',*,*,#11320,.T.);
#16165=ORIENTED_EDGE('',*,*,#11314,.T.);
#16166=ORIENTED_EDGE('',*,*,#11331,.T.);
#16167=ORIENTED_EDGE('',*,*,#11233,.T.);
#16168=ORIENTED_EDGE('',*,*,#11328,.T.);
#16169=ORIENTED_EDGE('',*,*,#11259,.T.);
#16170=ORIENTED_EDGE('',*,*,#11339,.T.);
#16171=ORIENTED_EDGE('',*,*,#11178,.T.);
#16172=ORIENTED_EDGE('',*,*,#11336,.T.);
#16173=ORIENTED_EDGE('',*,*,#11204,.T.);
#16174=ORIENTED_EDGE('',*,*,#11340,.T.);
#16175=ORIENTED_EDGE('',*,*,#11344,.F.);
#16176=ORIENTED_EDGE('',*,*,#11345,.F.);
#16177=ORIENTED_EDGE('',*,*,#11346,.T.);
#16178=ORIENTED_EDGE('',*,*,#11347,.F.);
#16179=ORIENTED_EDGE('',*,*,#11346,.F.);
#16180=ORIENTED_EDGE('',*,*,#11348,.F.);
#16181=ORIENTED_EDGE('',*,*,#11349,.T.);
#16182=ORIENTED_EDGE('',*,*,#11350,.F.);
#16183=ORIENTED_EDGE('',*,*,#11349,.F.);
#16184=ORIENTED_EDGE('',*,*,#11351,.F.);
#16185=ORIENTED_EDGE('',*,*,#11352,.T.);
#16186=ORIENTED_EDGE('',*,*,#11353,.F.);
#16187=ORIENTED_EDGE('',*,*,#11352,.F.);
#16188=ORIENTED_EDGE('',*,*,#11354,.F.);
#16189=ORIENTED_EDGE('',*,*,#11355,.T.);
#16190=ORIENTED_EDGE('',*,*,#11356,.F.);
#16191=ORIENTED_EDGE('',*,*,#11355,.F.);
#16192=ORIENTED_EDGE('',*,*,#11357,.F.);
#16193=ORIENTED_EDGE('',*,*,#11358,.T.);
#16194=ORIENTED_EDGE('',*,*,#11356,.T.);
#16195=ORIENTED_EDGE('',*,*,#11358,.F.);
#16196=ORIENTED_EDGE('',*,*,#11359,.F.);
#16197=ORIENTED_EDGE('',*,*,#11360,.T.);
#16198=ORIENTED_EDGE('',*,*,#11361,.T.);
#16199=ORIENTED_EDGE('',*,*,#11360,.F.);
#16200=ORIENTED_EDGE('',*,*,#11359,.T.);
#16201=ORIENTED_EDGE('',*,*,#11345,.T.);
#16202=ORIENTED_EDGE('',*,*,#11348,.T.);
#16203=ORIENTED_EDGE('',*,*,#11351,.T.);
#16204=ORIENTED_EDGE('',*,*,#11357,.T.);
#16205=ORIENTED_EDGE('',*,*,#11361,.F.);
#16206=ORIENTED_EDGE('',*,*,#11347,.T.);
#16207=ORIENTED_EDGE('',*,*,#11350,.T.);
#16208=ORIENTED_EDGE('',*,*,#11353,.T.);
#16209=ORIENTED_EDGE('',*,*,#11354,.T.);
#16210=ORIENTED_EDGE('',*,*,#11362,.F.);
#16211=ORIENTED_EDGE('',*,*,#11363,.T.);
#16212=ORIENTED_EDGE('',*,*,#11364,.T.);
#16213=ORIENTED_EDGE('',*,*,#11365,.T.);
#16214=ORIENTED_EDGE('',*,*,#11366,.F.);
#16215=ORIENTED_EDGE('',*,*,#11367,.T.);
#16216=ORIENTED_EDGE('',*,*,#11362,.T.);
#16217=ORIENTED_EDGE('',*,*,#11368,.T.);
#16218=ORIENTED_EDGE('',*,*,#11369,.F.);
#16219=ORIENTED_EDGE('',*,*,#11370,.T.);
#16220=ORIENTED_EDGE('',*,*,#11366,.T.);
#16221=ORIENTED_EDGE('',*,*,#11371,.T.);
#16222=ORIENTED_EDGE('',*,*,#11372,.F.);
#16223=ORIENTED_EDGE('',*,*,#11373,.T.);
#16224=ORIENTED_EDGE('',*,*,#11369,.T.);
#16225=ORIENTED_EDGE('',*,*,#11374,.T.);
#16226=ORIENTED_EDGE('',*,*,#11375,.F.);
#16227=ORIENTED_EDGE('',*,*,#11376,.T.);
#16228=ORIENTED_EDGE('',*,*,#11372,.T.);
#16229=ORIENTED_EDGE('',*,*,#11377,.T.);
#16230=ORIENTED_EDGE('',*,*,#11378,.F.);
#16231=ORIENTED_EDGE('',*,*,#11379,.T.);
#16232=ORIENTED_EDGE('',*,*,#11375,.T.);
#16233=ORIENTED_EDGE('',*,*,#11380,.T.);
#16234=ORIENTED_EDGE('',*,*,#11381,.F.);
#16235=ORIENTED_EDGE('',*,*,#11382,.T.);
#16236=ORIENTED_EDGE('',*,*,#11378,.T.);
#16237=ORIENTED_EDGE('',*,*,#11383,.T.);
#16238=ORIENTED_EDGE('',*,*,#11384,.F.);
#16239=ORIENTED_EDGE('',*,*,#11385,.T.);
#16240=ORIENTED_EDGE('',*,*,#11381,.T.);
#16241=ORIENTED_EDGE('',*,*,#11386,.T.);
#16242=ORIENTED_EDGE('',*,*,#11387,.F.);
#16243=ORIENTED_EDGE('',*,*,#11388,.T.);
#16244=ORIENTED_EDGE('',*,*,#11384,.T.);
#16245=ORIENTED_EDGE('',*,*,#11389,.T.);
#16246=ORIENTED_EDGE('',*,*,#11390,.F.);
#16247=ORIENTED_EDGE('',*,*,#11391,.T.);
#16248=ORIENTED_EDGE('',*,*,#11387,.T.);
#16249=ORIENTED_EDGE('',*,*,#11392,.T.);
#16250=ORIENTED_EDGE('',*,*,#11393,.F.);
#16251=ORIENTED_EDGE('',*,*,#11394,.T.);
#16252=ORIENTED_EDGE('',*,*,#11390,.T.);
#16253=ORIENTED_EDGE('',*,*,#11395,.T.);
#16254=ORIENTED_EDGE('',*,*,#11396,.F.);
#16255=ORIENTED_EDGE('',*,*,#11397,.T.);
#16256=ORIENTED_EDGE('',*,*,#11393,.T.);
#16257=ORIENTED_EDGE('',*,*,#11398,.T.);
#16258=ORIENTED_EDGE('',*,*,#11399,.F.);
#16259=ORIENTED_EDGE('',*,*,#11400,.T.);
#16260=ORIENTED_EDGE('',*,*,#11396,.T.);
#16261=ORIENTED_EDGE('',*,*,#11401,.T.);
#16262=ORIENTED_EDGE('',*,*,#11402,.F.);
#16263=ORIENTED_EDGE('',*,*,#11403,.T.);
#16264=ORIENTED_EDGE('',*,*,#11399,.T.);
#16265=ORIENTED_EDGE('',*,*,#11404,.T.);
#16266=ORIENTED_EDGE('',*,*,#11405,.F.);
#16267=ORIENTED_EDGE('',*,*,#11406,.T.);
#16268=ORIENTED_EDGE('',*,*,#11402,.T.);
#16269=ORIENTED_EDGE('',*,*,#11407,.T.);
#16270=ORIENTED_EDGE('',*,*,#11408,.F.);
#16271=ORIENTED_EDGE('',*,*,#11409,.T.);
#16272=ORIENTED_EDGE('',*,*,#11405,.T.);
#16273=ORIENTED_EDGE('',*,*,#11410,.T.);
#16274=ORIENTED_EDGE('',*,*,#11411,.F.);
#16275=ORIENTED_EDGE('',*,*,#11412,.T.);
#16276=ORIENTED_EDGE('',*,*,#11408,.T.);
#16277=ORIENTED_EDGE('',*,*,#11413,.T.);
#16278=ORIENTED_EDGE('',*,*,#11414,.F.);
#16279=ORIENTED_EDGE('',*,*,#11415,.T.);
#16280=ORIENTED_EDGE('',*,*,#11411,.T.);
#16281=ORIENTED_EDGE('',*,*,#11416,.T.);
#16282=ORIENTED_EDGE('',*,*,#11417,.F.);
#16283=ORIENTED_EDGE('',*,*,#11418,.T.);
#16284=ORIENTED_EDGE('',*,*,#11414,.T.);
#16285=ORIENTED_EDGE('',*,*,#11419,.T.);
#16286=ORIENTED_EDGE('',*,*,#11420,.F.);
#16287=ORIENTED_EDGE('',*,*,#11421,.T.);
#16288=ORIENTED_EDGE('',*,*,#11417,.T.);
#16289=ORIENTED_EDGE('',*,*,#11422,.T.);
#16290=ORIENTED_EDGE('',*,*,#11423,.F.);
#16291=ORIENTED_EDGE('',*,*,#11424,.T.);
#16292=ORIENTED_EDGE('',*,*,#11420,.T.);
#16293=ORIENTED_EDGE('',*,*,#11425,.T.);
#16294=ORIENTED_EDGE('',*,*,#11426,.F.);
#16295=ORIENTED_EDGE('',*,*,#11427,.T.);
#16296=ORIENTED_EDGE('',*,*,#11423,.T.);
#16297=ORIENTED_EDGE('',*,*,#11428,.T.);
#16298=ORIENTED_EDGE('',*,*,#11429,.F.);
#16299=ORIENTED_EDGE('',*,*,#11430,.T.);
#16300=ORIENTED_EDGE('',*,*,#11426,.T.);
#16301=ORIENTED_EDGE('',*,*,#11431,.T.);
#16302=ORIENTED_EDGE('',*,*,#11432,.F.);
#16303=ORIENTED_EDGE('',*,*,#11433,.T.);
#16304=ORIENTED_EDGE('',*,*,#11429,.T.);
#16305=ORIENTED_EDGE('',*,*,#11434,.T.);
#16306=ORIENTED_EDGE('',*,*,#11435,.F.);
#16307=ORIENTED_EDGE('',*,*,#11436,.T.);
#16308=ORIENTED_EDGE('',*,*,#11432,.T.);
#16309=ORIENTED_EDGE('',*,*,#11437,.T.);
#16310=ORIENTED_EDGE('',*,*,#11438,.F.);
#16311=ORIENTED_EDGE('',*,*,#11439,.T.);
#16312=ORIENTED_EDGE('',*,*,#11435,.T.);
#16313=ORIENTED_EDGE('',*,*,#11440,.T.);
#16314=ORIENTED_EDGE('',*,*,#11441,.F.);
#16315=ORIENTED_EDGE('',*,*,#11442,.T.);
#16316=ORIENTED_EDGE('',*,*,#11438,.T.);
#16317=ORIENTED_EDGE('',*,*,#11443,.T.);
#16318=ORIENTED_EDGE('',*,*,#11444,.F.);
#16319=ORIENTED_EDGE('',*,*,#11445,.T.);
#16320=ORIENTED_EDGE('',*,*,#11441,.T.);
#16321=ORIENTED_EDGE('',*,*,#11446,.T.);
#16322=ORIENTED_EDGE('',*,*,#11447,.F.);
#16323=ORIENTED_EDGE('',*,*,#11448,.T.);
#16324=ORIENTED_EDGE('',*,*,#11444,.T.);
#16325=ORIENTED_EDGE('',*,*,#11449,.T.);
#16326=ORIENTED_EDGE('',*,*,#11450,.F.);
#16327=ORIENTED_EDGE('',*,*,#11451,.T.);
#16328=ORIENTED_EDGE('',*,*,#11447,.T.);
#16329=ORIENTED_EDGE('',*,*,#11452,.T.);
#16330=ORIENTED_EDGE('',*,*,#11453,.F.);
#16331=ORIENTED_EDGE('',*,*,#11454,.T.);
#16332=ORIENTED_EDGE('',*,*,#11450,.T.);
#16333=ORIENTED_EDGE('',*,*,#11455,.T.);
#16334=ORIENTED_EDGE('',*,*,#11456,.F.);
#16335=ORIENTED_EDGE('',*,*,#11457,.T.);
#16336=ORIENTED_EDGE('',*,*,#11453,.T.);
#16337=ORIENTED_EDGE('',*,*,#11458,.T.);
#16338=ORIENTED_EDGE('',*,*,#11459,.F.);
#16339=ORIENTED_EDGE('',*,*,#11460,.T.);
#16340=ORIENTED_EDGE('',*,*,#11456,.T.);
#16341=ORIENTED_EDGE('',*,*,#11461,.T.);
#16342=ORIENTED_EDGE('',*,*,#11462,.F.);
#16343=ORIENTED_EDGE('',*,*,#11463,.T.);
#16344=ORIENTED_EDGE('',*,*,#11459,.T.);
#16345=ORIENTED_EDGE('',*,*,#11464,.T.);
#16346=ORIENTED_EDGE('',*,*,#11465,.F.);
#16347=ORIENTED_EDGE('',*,*,#11466,.T.);
#16348=ORIENTED_EDGE('',*,*,#11462,.T.);
#16349=ORIENTED_EDGE('',*,*,#11467,.T.);
#16350=ORIENTED_EDGE('',*,*,#11468,.F.);
#16351=ORIENTED_EDGE('',*,*,#11469,.T.);
#16352=ORIENTED_EDGE('',*,*,#11465,.T.);
#16353=ORIENTED_EDGE('',*,*,#11470,.T.);
#16354=ORIENTED_EDGE('',*,*,#11471,.F.);
#16355=ORIENTED_EDGE('',*,*,#11472,.T.);
#16356=ORIENTED_EDGE('',*,*,#11468,.T.);
#16357=ORIENTED_EDGE('',*,*,#11473,.T.);
#16358=ORIENTED_EDGE('',*,*,#11474,.F.);
#16359=ORIENTED_EDGE('',*,*,#11475,.T.);
#16360=ORIENTED_EDGE('',*,*,#11471,.T.);
#16361=ORIENTED_EDGE('',*,*,#11476,.T.);
#16362=ORIENTED_EDGE('',*,*,#11477,.F.);
#16363=ORIENTED_EDGE('',*,*,#11478,.T.);
#16364=ORIENTED_EDGE('',*,*,#11474,.T.);
#16365=ORIENTED_EDGE('',*,*,#11479,.T.);
#16366=ORIENTED_EDGE('',*,*,#11480,.F.);
#16367=ORIENTED_EDGE('',*,*,#11481,.T.);
#16368=ORIENTED_EDGE('',*,*,#11477,.T.);
#16369=ORIENTED_EDGE('',*,*,#11482,.T.);
#16370=ORIENTED_EDGE('',*,*,#11483,.F.);
#16371=ORIENTED_EDGE('',*,*,#11484,.T.);
#16372=ORIENTED_EDGE('',*,*,#11480,.T.);
#16373=ORIENTED_EDGE('',*,*,#11485,.T.);
#16374=ORIENTED_EDGE('',*,*,#11486,.F.);
#16375=ORIENTED_EDGE('',*,*,#11487,.T.);
#16376=ORIENTED_EDGE('',*,*,#11483,.T.);
#16377=ORIENTED_EDGE('',*,*,#11488,.T.);
#16378=ORIENTED_EDGE('',*,*,#11489,.F.);
#16379=ORIENTED_EDGE('',*,*,#11490,.T.);
#16380=ORIENTED_EDGE('',*,*,#11486,.T.);
#16381=ORIENTED_EDGE('',*,*,#11491,.T.);
#16382=ORIENTED_EDGE('',*,*,#11492,.F.);
#16383=ORIENTED_EDGE('',*,*,#11493,.T.);
#16384=ORIENTED_EDGE('',*,*,#11489,.T.);
#16385=ORIENTED_EDGE('',*,*,#11494,.T.);
#16386=ORIENTED_EDGE('',*,*,#11495,.F.);
#16387=ORIENTED_EDGE('',*,*,#11496,.T.);
#16388=ORIENTED_EDGE('',*,*,#11492,.T.);
#16389=ORIENTED_EDGE('',*,*,#11497,.T.);
#16390=ORIENTED_EDGE('',*,*,#11498,.F.);
#16391=ORIENTED_EDGE('',*,*,#11499,.T.);
#16392=ORIENTED_EDGE('',*,*,#11495,.T.);
#16393=ORIENTED_EDGE('',*,*,#11500,.T.);
#16394=ORIENTED_EDGE('',*,*,#11501,.F.);
#16395=ORIENTED_EDGE('',*,*,#11502,.T.);
#16396=ORIENTED_EDGE('',*,*,#11498,.T.);
#16397=ORIENTED_EDGE('',*,*,#11503,.T.);
#16398=ORIENTED_EDGE('',*,*,#11504,.F.);
#16399=ORIENTED_EDGE('',*,*,#11505,.T.);
#16400=ORIENTED_EDGE('',*,*,#11501,.T.);
#16401=ORIENTED_EDGE('',*,*,#11506,.T.);
#16402=ORIENTED_EDGE('',*,*,#11507,.F.);
#16403=ORIENTED_EDGE('',*,*,#11508,.T.);
#16404=ORIENTED_EDGE('',*,*,#11504,.T.);
#16405=ORIENTED_EDGE('',*,*,#11509,.T.);
#16406=ORIENTED_EDGE('',*,*,#11510,.F.);
#16407=ORIENTED_EDGE('',*,*,#11511,.T.);
#16408=ORIENTED_EDGE('',*,*,#11507,.T.);
#16409=ORIENTED_EDGE('',*,*,#11512,.T.);
#16410=ORIENTED_EDGE('',*,*,#11513,.F.);
#16411=ORIENTED_EDGE('',*,*,#11514,.T.);
#16412=ORIENTED_EDGE('',*,*,#11510,.T.);
#16413=ORIENTED_EDGE('',*,*,#11515,.T.);
#16414=ORIENTED_EDGE('',*,*,#11516,.F.);
#16415=ORIENTED_EDGE('',*,*,#11517,.T.);
#16416=ORIENTED_EDGE('',*,*,#11513,.T.);
#16417=ORIENTED_EDGE('',*,*,#11518,.T.);
#16418=ORIENTED_EDGE('',*,*,#11519,.F.);
#16419=ORIENTED_EDGE('',*,*,#11520,.T.);
#16420=ORIENTED_EDGE('',*,*,#11516,.T.);
#16421=ORIENTED_EDGE('',*,*,#11521,.T.);
#16422=ORIENTED_EDGE('',*,*,#11522,.F.);
#16423=ORIENTED_EDGE('',*,*,#11523,.T.);
#16424=ORIENTED_EDGE('',*,*,#11519,.T.);
#16425=ORIENTED_EDGE('',*,*,#11524,.T.);
#16426=ORIENTED_EDGE('',*,*,#11525,.F.);
#16427=ORIENTED_EDGE('',*,*,#11526,.T.);
#16428=ORIENTED_EDGE('',*,*,#11522,.T.);
#16429=ORIENTED_EDGE('',*,*,#11527,.T.);
#16430=ORIENTED_EDGE('',*,*,#11528,.F.);
#16431=ORIENTED_EDGE('',*,*,#11529,.T.);
#16432=ORIENTED_EDGE('',*,*,#11525,.T.);
#16433=ORIENTED_EDGE('',*,*,#11530,.T.);
#16434=ORIENTED_EDGE('',*,*,#11531,.F.);
#16435=ORIENTED_EDGE('',*,*,#11532,.T.);
#16436=ORIENTED_EDGE('',*,*,#11528,.T.);
#16437=ORIENTED_EDGE('',*,*,#11533,.T.);
#16438=ORIENTED_EDGE('',*,*,#11534,.F.);
#16439=ORIENTED_EDGE('',*,*,#11535,.T.);
#16440=ORIENTED_EDGE('',*,*,#11531,.T.);
#16441=ORIENTED_EDGE('',*,*,#11536,.T.);
#16442=ORIENTED_EDGE('',*,*,#11537,.F.);
#16443=ORIENTED_EDGE('',*,*,#11538,.T.);
#16444=ORIENTED_EDGE('',*,*,#11534,.T.);
#16445=ORIENTED_EDGE('',*,*,#11539,.T.);
#16446=ORIENTED_EDGE('',*,*,#11540,.F.);
#16447=ORIENTED_EDGE('',*,*,#11541,.T.);
#16448=ORIENTED_EDGE('',*,*,#11537,.T.);
#16449=ORIENTED_EDGE('',*,*,#11542,.T.);
#16450=ORIENTED_EDGE('',*,*,#11543,.F.);
#16451=ORIENTED_EDGE('',*,*,#11544,.T.);
#16452=ORIENTED_EDGE('',*,*,#11545,.F.);
#16453=ORIENTED_EDGE('',*,*,#11546,.F.);
#16454=ORIENTED_EDGE('',*,*,#11547,.F.);
#16455=ORIENTED_EDGE('',*,*,#11548,.T.);
#16456=ORIENTED_EDGE('',*,*,#11543,.T.);
#16457=ORIENTED_EDGE('',*,*,#11549,.F.);
#16458=ORIENTED_EDGE('',*,*,#11550,.F.);
#16459=ORIENTED_EDGE('',*,*,#11551,.T.);
#16460=ORIENTED_EDGE('',*,*,#11547,.T.);
#16461=ORIENTED_EDGE('',*,*,#11552,.F.);
#16462=ORIENTED_EDGE('',*,*,#11553,.F.);
#16463=ORIENTED_EDGE('',*,*,#11554,.T.);
#16464=ORIENTED_EDGE('',*,*,#11550,.T.);
#16465=ORIENTED_EDGE('',*,*,#11555,.F.);
#16466=ORIENTED_EDGE('',*,*,#11556,.F.);
#16467=ORIENTED_EDGE('',*,*,#11557,.T.);
#16468=ORIENTED_EDGE('',*,*,#11553,.T.);
#16469=ORIENTED_EDGE('',*,*,#11558,.F.);
#16470=ORIENTED_EDGE('',*,*,#11559,.F.);
#16471=ORIENTED_EDGE('',*,*,#11560,.T.);
#16472=ORIENTED_EDGE('',*,*,#11556,.T.);
#16473=ORIENTED_EDGE('',*,*,#11561,.F.);
#16474=ORIENTED_EDGE('',*,*,#11562,.F.);
#16475=ORIENTED_EDGE('',*,*,#11563,.T.);
#16476=ORIENTED_EDGE('',*,*,#11559,.T.);
#16477=ORIENTED_EDGE('',*,*,#11564,.F.);
#16478=ORIENTED_EDGE('',*,*,#11565,.F.);
#16479=ORIENTED_EDGE('',*,*,#11566,.T.);
#16480=ORIENTED_EDGE('',*,*,#11562,.T.);
#16481=ORIENTED_EDGE('',*,*,#11567,.F.);
#16482=ORIENTED_EDGE('',*,*,#11568,.F.);
#16483=ORIENTED_EDGE('',*,*,#11569,.T.);
#16484=ORIENTED_EDGE('',*,*,#11565,.T.);
#16485=ORIENTED_EDGE('',*,*,#11570,.F.);
#16486=ORIENTED_EDGE('',*,*,#11571,.F.);
#16487=ORIENTED_EDGE('',*,*,#11572,.T.);
#16488=ORIENTED_EDGE('',*,*,#11568,.T.);
#16489=ORIENTED_EDGE('',*,*,#11573,.F.);
#16490=ORIENTED_EDGE('',*,*,#11574,.F.);
#16491=ORIENTED_EDGE('',*,*,#11575,.T.);
#16492=ORIENTED_EDGE('',*,*,#11571,.T.);
#16493=ORIENTED_EDGE('',*,*,#11576,.F.);
#16494=ORIENTED_EDGE('',*,*,#11577,.F.);
#16495=ORIENTED_EDGE('',*,*,#11578,.T.);
#16496=ORIENTED_EDGE('',*,*,#11574,.T.);
#16497=ORIENTED_EDGE('',*,*,#11579,.F.);
#16498=ORIENTED_EDGE('',*,*,#11580,.F.);
#16499=ORIENTED_EDGE('',*,*,#11581,.T.);
#16500=ORIENTED_EDGE('',*,*,#11577,.T.);
#16501=ORIENTED_EDGE('',*,*,#11582,.F.);
#16502=ORIENTED_EDGE('',*,*,#11583,.F.);
#16503=ORIENTED_EDGE('',*,*,#11584,.T.);
#16504=ORIENTED_EDGE('',*,*,#11580,.T.);
#16505=ORIENTED_EDGE('',*,*,#11585,.F.);
#16506=ORIENTED_EDGE('',*,*,#11586,.F.);
#16507=ORIENTED_EDGE('',*,*,#11587,.T.);
#16508=ORIENTED_EDGE('',*,*,#11583,.T.);
#16509=ORIENTED_EDGE('',*,*,#11588,.F.);
#16510=ORIENTED_EDGE('',*,*,#11589,.F.);
#16511=ORIENTED_EDGE('',*,*,#11590,.T.);
#16512=ORIENTED_EDGE('',*,*,#11586,.T.);
#16513=ORIENTED_EDGE('',*,*,#11591,.F.);
#16514=ORIENTED_EDGE('',*,*,#11592,.F.);
#16515=ORIENTED_EDGE('',*,*,#11593,.T.);
#16516=ORIENTED_EDGE('',*,*,#11589,.T.);
#16517=ORIENTED_EDGE('',*,*,#11594,.F.);
#16518=ORIENTED_EDGE('',*,*,#11595,.F.);
#16519=ORIENTED_EDGE('',*,*,#11596,.T.);
#16520=ORIENTED_EDGE('',*,*,#11592,.T.);
#16521=ORIENTED_EDGE('',*,*,#11597,.F.);
#16522=ORIENTED_EDGE('',*,*,#11598,.F.);
#16523=ORIENTED_EDGE('',*,*,#11599,.T.);
#16524=ORIENTED_EDGE('',*,*,#11595,.T.);
#16525=ORIENTED_EDGE('',*,*,#11600,.F.);
#16526=ORIENTED_EDGE('',*,*,#11601,.F.);
#16527=ORIENTED_EDGE('',*,*,#11602,.T.);
#16528=ORIENTED_EDGE('',*,*,#11598,.T.);
#16529=ORIENTED_EDGE('',*,*,#11603,.F.);
#16530=ORIENTED_EDGE('',*,*,#11604,.F.);
#16531=ORIENTED_EDGE('',*,*,#11605,.T.);
#16532=ORIENTED_EDGE('',*,*,#11601,.T.);
#16533=ORIENTED_EDGE('',*,*,#11606,.F.);
#16534=ORIENTED_EDGE('',*,*,#11607,.F.);
#16535=ORIENTED_EDGE('',*,*,#11608,.T.);
#16536=ORIENTED_EDGE('',*,*,#11604,.T.);
#16537=ORIENTED_EDGE('',*,*,#11609,.F.);
#16538=ORIENTED_EDGE('',*,*,#11610,.F.);
#16539=ORIENTED_EDGE('',*,*,#11611,.T.);
#16540=ORIENTED_EDGE('',*,*,#11607,.T.);
#16541=ORIENTED_EDGE('',*,*,#11612,.F.);
#16542=ORIENTED_EDGE('',*,*,#11613,.F.);
#16543=ORIENTED_EDGE('',*,*,#11614,.T.);
#16544=ORIENTED_EDGE('',*,*,#11610,.T.);
#16545=ORIENTED_EDGE('',*,*,#11615,.F.);
#16546=ORIENTED_EDGE('',*,*,#11616,.F.);
#16547=ORIENTED_EDGE('',*,*,#11617,.T.);
#16548=ORIENTED_EDGE('',*,*,#11613,.T.);
#16549=ORIENTED_EDGE('',*,*,#11618,.F.);
#16550=ORIENTED_EDGE('',*,*,#11619,.F.);
#16551=ORIENTED_EDGE('',*,*,#11620,.T.);
#16552=ORIENTED_EDGE('',*,*,#11616,.T.);
#16553=ORIENTED_EDGE('',*,*,#11621,.F.);
#16554=ORIENTED_EDGE('',*,*,#11622,.F.);
#16555=ORIENTED_EDGE('',*,*,#11623,.T.);
#16556=ORIENTED_EDGE('',*,*,#11619,.T.);
#16557=ORIENTED_EDGE('',*,*,#11624,.F.);
#16558=ORIENTED_EDGE('',*,*,#11625,.F.);
#16559=ORIENTED_EDGE('',*,*,#11626,.T.);
#16560=ORIENTED_EDGE('',*,*,#11622,.T.);
#16561=ORIENTED_EDGE('',*,*,#11627,.F.);
#16562=ORIENTED_EDGE('',*,*,#11628,.F.);
#16563=ORIENTED_EDGE('',*,*,#11629,.T.);
#16564=ORIENTED_EDGE('',*,*,#11625,.T.);
#16565=ORIENTED_EDGE('',*,*,#11630,.F.);
#16566=ORIENTED_EDGE('',*,*,#11631,.F.);
#16567=ORIENTED_EDGE('',*,*,#11632,.T.);
#16568=ORIENTED_EDGE('',*,*,#11628,.T.);
#16569=ORIENTED_EDGE('',*,*,#11633,.F.);
#16570=ORIENTED_EDGE('',*,*,#11634,.F.);
#16571=ORIENTED_EDGE('',*,*,#11635,.T.);
#16572=ORIENTED_EDGE('',*,*,#11631,.T.);
#16573=ORIENTED_EDGE('',*,*,#11636,.F.);
#16574=ORIENTED_EDGE('',*,*,#11637,.F.);
#16575=ORIENTED_EDGE('',*,*,#11638,.T.);
#16576=ORIENTED_EDGE('',*,*,#11634,.T.);
#16577=ORIENTED_EDGE('',*,*,#11639,.F.);
#16578=ORIENTED_EDGE('',*,*,#11640,.F.);
#16579=ORIENTED_EDGE('',*,*,#11641,.T.);
#16580=ORIENTED_EDGE('',*,*,#11637,.T.);
#16581=ORIENTED_EDGE('',*,*,#11642,.F.);
#16582=ORIENTED_EDGE('',*,*,#11643,.F.);
#16583=ORIENTED_EDGE('',*,*,#11644,.T.);
#16584=ORIENTED_EDGE('',*,*,#11640,.T.);
#16585=ORIENTED_EDGE('',*,*,#11645,.F.);
#16586=ORIENTED_EDGE('',*,*,#11646,.F.);
#16587=ORIENTED_EDGE('',*,*,#11647,.T.);
#16588=ORIENTED_EDGE('',*,*,#11643,.T.);
#16589=ORIENTED_EDGE('',*,*,#11648,.F.);
#16590=ORIENTED_EDGE('',*,*,#11649,.F.);
#16591=ORIENTED_EDGE('',*,*,#11650,.T.);
#16592=ORIENTED_EDGE('',*,*,#11646,.T.);
#16593=ORIENTED_EDGE('',*,*,#11651,.F.);
#16594=ORIENTED_EDGE('',*,*,#11652,.F.);
#16595=ORIENTED_EDGE('',*,*,#11653,.T.);
#16596=ORIENTED_EDGE('',*,*,#11649,.T.);
#16597=ORIENTED_EDGE('',*,*,#11654,.F.);
#16598=ORIENTED_EDGE('',*,*,#11655,.F.);
#16599=ORIENTED_EDGE('',*,*,#11656,.T.);
#16600=ORIENTED_EDGE('',*,*,#11652,.T.);
#16601=ORIENTED_EDGE('',*,*,#11657,.F.);
#16602=ORIENTED_EDGE('',*,*,#11658,.F.);
#16603=ORIENTED_EDGE('',*,*,#11659,.T.);
#16604=ORIENTED_EDGE('',*,*,#11655,.T.);
#16605=ORIENTED_EDGE('',*,*,#11660,.F.);
#16606=ORIENTED_EDGE('',*,*,#11661,.F.);
#16607=ORIENTED_EDGE('',*,*,#11662,.T.);
#16608=ORIENTED_EDGE('',*,*,#11658,.T.);
#16609=ORIENTED_EDGE('',*,*,#11663,.F.);
#16610=ORIENTED_EDGE('',*,*,#11664,.F.);
#16611=ORIENTED_EDGE('',*,*,#11665,.T.);
#16612=ORIENTED_EDGE('',*,*,#11661,.T.);
#16613=ORIENTED_EDGE('',*,*,#11666,.F.);
#16614=ORIENTED_EDGE('',*,*,#11667,.F.);
#16615=ORIENTED_EDGE('',*,*,#11668,.T.);
#16616=ORIENTED_EDGE('',*,*,#11664,.T.);
#16617=ORIENTED_EDGE('',*,*,#11669,.F.);
#16618=ORIENTED_EDGE('',*,*,#11670,.F.);
#16619=ORIENTED_EDGE('',*,*,#11671,.T.);
#16620=ORIENTED_EDGE('',*,*,#11667,.T.);
#16621=ORIENTED_EDGE('',*,*,#11672,.F.);
#16622=ORIENTED_EDGE('',*,*,#11673,.F.);
#16623=ORIENTED_EDGE('',*,*,#11674,.T.);
#16624=ORIENTED_EDGE('',*,*,#11670,.T.);
#16625=ORIENTED_EDGE('',*,*,#11675,.F.);
#16626=ORIENTED_EDGE('',*,*,#11676,.F.);
#16627=ORIENTED_EDGE('',*,*,#11677,.T.);
#16628=ORIENTED_EDGE('',*,*,#11673,.T.);
#16629=ORIENTED_EDGE('',*,*,#11678,.F.);
#16630=ORIENTED_EDGE('',*,*,#11679,.F.);
#16631=ORIENTED_EDGE('',*,*,#11680,.T.);
#16632=ORIENTED_EDGE('',*,*,#11676,.T.);
#16633=ORIENTED_EDGE('',*,*,#11681,.F.);
#16634=ORIENTED_EDGE('',*,*,#11682,.F.);
#16635=ORIENTED_EDGE('',*,*,#11683,.T.);
#16636=ORIENTED_EDGE('',*,*,#11679,.T.);
#16637=ORIENTED_EDGE('',*,*,#11684,.F.);
#16638=ORIENTED_EDGE('',*,*,#11685,.F.);
#16639=ORIENTED_EDGE('',*,*,#11686,.T.);
#16640=ORIENTED_EDGE('',*,*,#11682,.T.);
#16641=ORIENTED_EDGE('',*,*,#11687,.F.);
#16642=ORIENTED_EDGE('',*,*,#11688,.F.);
#16643=ORIENTED_EDGE('',*,*,#11689,.T.);
#16644=ORIENTED_EDGE('',*,*,#11685,.T.);
#16645=ORIENTED_EDGE('',*,*,#11690,.F.);
#16646=ORIENTED_EDGE('',*,*,#11691,.F.);
#16647=ORIENTED_EDGE('',*,*,#11692,.T.);
#16648=ORIENTED_EDGE('',*,*,#11688,.T.);
#16649=ORIENTED_EDGE('',*,*,#11693,.F.);
#16650=ORIENTED_EDGE('',*,*,#11694,.F.);
#16651=ORIENTED_EDGE('',*,*,#11695,.T.);
#16652=ORIENTED_EDGE('',*,*,#11691,.T.);
#16653=ORIENTED_EDGE('',*,*,#11696,.F.);
#16654=ORIENTED_EDGE('',*,*,#11697,.F.);
#16655=ORIENTED_EDGE('',*,*,#11698,.T.);
#16656=ORIENTED_EDGE('',*,*,#11694,.T.);
#16657=ORIENTED_EDGE('',*,*,#11699,.F.);
#16658=ORIENTED_EDGE('',*,*,#11700,.F.);
#16659=ORIENTED_EDGE('',*,*,#11701,.T.);
#16660=ORIENTED_EDGE('',*,*,#11697,.T.);
#16661=ORIENTED_EDGE('',*,*,#11702,.F.);
#16662=ORIENTED_EDGE('',*,*,#11703,.F.);
#16663=ORIENTED_EDGE('',*,*,#11704,.T.);
#16664=ORIENTED_EDGE('',*,*,#11700,.T.);
#16665=ORIENTED_EDGE('',*,*,#11705,.F.);
#16666=ORIENTED_EDGE('',*,*,#11706,.F.);
#16667=ORIENTED_EDGE('',*,*,#11707,.T.);
#16668=ORIENTED_EDGE('',*,*,#11703,.T.);
#16669=ORIENTED_EDGE('',*,*,#11708,.F.);
#16670=ORIENTED_EDGE('',*,*,#11709,.F.);
#16671=ORIENTED_EDGE('',*,*,#11710,.T.);
#16672=ORIENTED_EDGE('',*,*,#11706,.T.);
#16673=ORIENTED_EDGE('',*,*,#11711,.F.);
#16674=ORIENTED_EDGE('',*,*,#11712,.F.);
#16675=ORIENTED_EDGE('',*,*,#11713,.T.);
#16676=ORIENTED_EDGE('',*,*,#11709,.T.);
#16677=ORIENTED_EDGE('',*,*,#11714,.F.);
#16678=ORIENTED_EDGE('',*,*,#11715,.F.);
#16679=ORIENTED_EDGE('',*,*,#11716,.T.);
#16680=ORIENTED_EDGE('',*,*,#11712,.T.);
#16681=ORIENTED_EDGE('',*,*,#11717,.F.);
#16682=ORIENTED_EDGE('',*,*,#11718,.F.);
#16683=ORIENTED_EDGE('',*,*,#11719,.T.);
#16684=ORIENTED_EDGE('',*,*,#11715,.T.);
#16685=ORIENTED_EDGE('',*,*,#11720,.F.);
#16686=ORIENTED_EDGE('',*,*,#11721,.F.);
#16687=ORIENTED_EDGE('',*,*,#11722,.T.);
#16688=ORIENTED_EDGE('',*,*,#11718,.T.);
#16689=ORIENTED_EDGE('',*,*,#11723,.F.);
#16690=ORIENTED_EDGE('',*,*,#11724,.F.);
#16691=ORIENTED_EDGE('',*,*,#11725,.F.);
#16692=ORIENTED_EDGE('',*,*,#11542,.F.);
#16693=ORIENTED_EDGE('',*,*,#11539,.F.);
#16694=ORIENTED_EDGE('',*,*,#11536,.F.);
#16695=ORIENTED_EDGE('',*,*,#11533,.F.);
#16696=ORIENTED_EDGE('',*,*,#11530,.F.);
#16697=ORIENTED_EDGE('',*,*,#11527,.F.);
#16698=ORIENTED_EDGE('',*,*,#11524,.F.);
#16699=ORIENTED_EDGE('',*,*,#11521,.F.);
#16700=ORIENTED_EDGE('',*,*,#11518,.F.);
#16701=ORIENTED_EDGE('',*,*,#11515,.F.);
#16702=ORIENTED_EDGE('',*,*,#11512,.F.);
#16703=ORIENTED_EDGE('',*,*,#11509,.F.);
#16704=ORIENTED_EDGE('',*,*,#11506,.F.);
#16705=ORIENTED_EDGE('',*,*,#11503,.F.);
#16706=ORIENTED_EDGE('',*,*,#11500,.F.);
#16707=ORIENTED_EDGE('',*,*,#11497,.F.);
#16708=ORIENTED_EDGE('',*,*,#11494,.F.);
#16709=ORIENTED_EDGE('',*,*,#11491,.F.);
#16710=ORIENTED_EDGE('',*,*,#11488,.F.);
#16711=ORIENTED_EDGE('',*,*,#11485,.F.);
#16712=ORIENTED_EDGE('',*,*,#11482,.F.);
#16713=ORIENTED_EDGE('',*,*,#11479,.F.);
#16714=ORIENTED_EDGE('',*,*,#11476,.F.);
#16715=ORIENTED_EDGE('',*,*,#11473,.F.);
#16716=ORIENTED_EDGE('',*,*,#11470,.F.);
#16717=ORIENTED_EDGE('',*,*,#11467,.F.);
#16718=ORIENTED_EDGE('',*,*,#11464,.F.);
#16719=ORIENTED_EDGE('',*,*,#11461,.F.);
#16720=ORIENTED_EDGE('',*,*,#11458,.F.);
#16721=ORIENTED_EDGE('',*,*,#11455,.F.);
#16722=ORIENTED_EDGE('',*,*,#11452,.F.);
#16723=ORIENTED_EDGE('',*,*,#11449,.F.);
#16724=ORIENTED_EDGE('',*,*,#11446,.F.);
#16725=ORIENTED_EDGE('',*,*,#11443,.F.);
#16726=ORIENTED_EDGE('',*,*,#11440,.F.);
#16727=ORIENTED_EDGE('',*,*,#11437,.F.);
#16728=ORIENTED_EDGE('',*,*,#11434,.F.);
#16729=ORIENTED_EDGE('',*,*,#11431,.F.);
#16730=ORIENTED_EDGE('',*,*,#11428,.F.);
#16731=ORIENTED_EDGE('',*,*,#11425,.F.);
#16732=ORIENTED_EDGE('',*,*,#11422,.F.);
#16733=ORIENTED_EDGE('',*,*,#11419,.F.);
#16734=ORIENTED_EDGE('',*,*,#11416,.F.);
#16735=ORIENTED_EDGE('',*,*,#11413,.F.);
#16736=ORIENTED_EDGE('',*,*,#11410,.F.);
#16737=ORIENTED_EDGE('',*,*,#11407,.F.);
#16738=ORIENTED_EDGE('',*,*,#11404,.F.);
#16739=ORIENTED_EDGE('',*,*,#11401,.F.);
#16740=ORIENTED_EDGE('',*,*,#11398,.F.);
#16741=ORIENTED_EDGE('',*,*,#11395,.F.);
#16742=ORIENTED_EDGE('',*,*,#11392,.F.);
#16743=ORIENTED_EDGE('',*,*,#11389,.F.);
#16744=ORIENTED_EDGE('',*,*,#11386,.F.);
#16745=ORIENTED_EDGE('',*,*,#11383,.F.);
#16746=ORIENTED_EDGE('',*,*,#11380,.F.);
#16747=ORIENTED_EDGE('',*,*,#11377,.F.);
#16748=ORIENTED_EDGE('',*,*,#11374,.F.);
#16749=ORIENTED_EDGE('',*,*,#11371,.F.);
#16750=ORIENTED_EDGE('',*,*,#11368,.F.);
#16751=ORIENTED_EDGE('',*,*,#11365,.F.);
#16752=ORIENTED_EDGE('',*,*,#11726,.F.);
#16753=ORIENTED_EDGE('',*,*,#11727,.T.);
#16754=ORIENTED_EDGE('',*,*,#11723,.T.);
#16755=ORIENTED_EDGE('',*,*,#11720,.T.);
#16756=ORIENTED_EDGE('',*,*,#11717,.T.);
#16757=ORIENTED_EDGE('',*,*,#11714,.T.);
#16758=ORIENTED_EDGE('',*,*,#11711,.T.);
#16759=ORIENTED_EDGE('',*,*,#11708,.T.);
#16760=ORIENTED_EDGE('',*,*,#11705,.T.);
#16761=ORIENTED_EDGE('',*,*,#11702,.T.);
#16762=ORIENTED_EDGE('',*,*,#11699,.T.);
#16763=ORIENTED_EDGE('',*,*,#11696,.T.);
#16764=ORIENTED_EDGE('',*,*,#11693,.T.);
#16765=ORIENTED_EDGE('',*,*,#11690,.T.);
#16766=ORIENTED_EDGE('',*,*,#11687,.T.);
#16767=ORIENTED_EDGE('',*,*,#11684,.T.);
#16768=ORIENTED_EDGE('',*,*,#11681,.T.);
#16769=ORIENTED_EDGE('',*,*,#11678,.T.);
#16770=ORIENTED_EDGE('',*,*,#11675,.T.);
#16771=ORIENTED_EDGE('',*,*,#11672,.T.);
#16772=ORIENTED_EDGE('',*,*,#11669,.T.);
#16773=ORIENTED_EDGE('',*,*,#11666,.T.);
#16774=ORIENTED_EDGE('',*,*,#11663,.T.);
#16775=ORIENTED_EDGE('',*,*,#11660,.T.);
#16776=ORIENTED_EDGE('',*,*,#11657,.T.);
#16777=ORIENTED_EDGE('',*,*,#11654,.T.);
#16778=ORIENTED_EDGE('',*,*,#11651,.T.);
#16779=ORIENTED_EDGE('',*,*,#11648,.T.);
#16780=ORIENTED_EDGE('',*,*,#11645,.T.);
#16781=ORIENTED_EDGE('',*,*,#11642,.T.);
#16782=ORIENTED_EDGE('',*,*,#11639,.T.);
#16783=ORIENTED_EDGE('',*,*,#11636,.T.);
#16784=ORIENTED_EDGE('',*,*,#11633,.T.);
#16785=ORIENTED_EDGE('',*,*,#11630,.T.);
#16786=ORIENTED_EDGE('',*,*,#11627,.T.);
#16787=ORIENTED_EDGE('',*,*,#11624,.T.);
#16788=ORIENTED_EDGE('',*,*,#11621,.T.);
#16789=ORIENTED_EDGE('',*,*,#11618,.T.);
#16790=ORIENTED_EDGE('',*,*,#11615,.T.);
#16791=ORIENTED_EDGE('',*,*,#11612,.T.);
#16792=ORIENTED_EDGE('',*,*,#11609,.T.);
#16793=ORIENTED_EDGE('',*,*,#11606,.T.);
#16794=ORIENTED_EDGE('',*,*,#11603,.T.);
#16795=ORIENTED_EDGE('',*,*,#11600,.T.);
#16796=ORIENTED_EDGE('',*,*,#11597,.T.);
#16797=ORIENTED_EDGE('',*,*,#11594,.T.);
#16798=ORIENTED_EDGE('',*,*,#11591,.T.);
#16799=ORIENTED_EDGE('',*,*,#11588,.T.);
#16800=ORIENTED_EDGE('',*,*,#11585,.T.);
#16801=ORIENTED_EDGE('',*,*,#11582,.T.);
#16802=ORIENTED_EDGE('',*,*,#11579,.T.);
#16803=ORIENTED_EDGE('',*,*,#11576,.T.);
#16804=ORIENTED_EDGE('',*,*,#11573,.T.);
#16805=ORIENTED_EDGE('',*,*,#11570,.T.);
#16806=ORIENTED_EDGE('',*,*,#11567,.T.);
#16807=ORIENTED_EDGE('',*,*,#11564,.T.);
#16808=ORIENTED_EDGE('',*,*,#11561,.T.);
#16809=ORIENTED_EDGE('',*,*,#11558,.T.);
#16810=ORIENTED_EDGE('',*,*,#11555,.T.);
#16811=ORIENTED_EDGE('',*,*,#11552,.T.);
#16812=ORIENTED_EDGE('',*,*,#11549,.T.);
#16813=ORIENTED_EDGE('',*,*,#11546,.T.);
#16814=ORIENTED_EDGE('',*,*,#11721,.T.);
#16815=ORIENTED_EDGE('',*,*,#11727,.F.);
#16816=ORIENTED_EDGE('',*,*,#11728,.F.);
#16817=ORIENTED_EDGE('',*,*,#11729,.T.);
#16818=ORIENTED_EDGE('',*,*,#11730,.F.);
#16819=ORIENTED_EDGE('',*,*,#11544,.F.);
#16820=ORIENTED_EDGE('',*,*,#11548,.F.);
#16821=ORIENTED_EDGE('',*,*,#11551,.F.);
#16822=ORIENTED_EDGE('',*,*,#11554,.F.);
#16823=ORIENTED_EDGE('',*,*,#11557,.F.);
#16824=ORIENTED_EDGE('',*,*,#11560,.F.);
#16825=ORIENTED_EDGE('',*,*,#11563,.F.);
#16826=ORIENTED_EDGE('',*,*,#11566,.F.);
#16827=ORIENTED_EDGE('',*,*,#11569,.F.);
#16828=ORIENTED_EDGE('',*,*,#11572,.F.);
#16829=ORIENTED_EDGE('',*,*,#11575,.F.);
#16830=ORIENTED_EDGE('',*,*,#11578,.F.);
#16831=ORIENTED_EDGE('',*,*,#11581,.F.);
#16832=ORIENTED_EDGE('',*,*,#11584,.F.);
#16833=ORIENTED_EDGE('',*,*,#11587,.F.);
#16834=ORIENTED_EDGE('',*,*,#11590,.F.);
#16835=ORIENTED_EDGE('',*,*,#11593,.F.);
#16836=ORIENTED_EDGE('',*,*,#11596,.F.);
#16837=ORIENTED_EDGE('',*,*,#11599,.F.);
#16838=ORIENTED_EDGE('',*,*,#11602,.F.);
#16839=ORIENTED_EDGE('',*,*,#11605,.F.);
#16840=ORIENTED_EDGE('',*,*,#11608,.F.);
#16841=ORIENTED_EDGE('',*,*,#11611,.F.);
#16842=ORIENTED_EDGE('',*,*,#11614,.F.);
#16843=ORIENTED_EDGE('',*,*,#11617,.F.);
#16844=ORIENTED_EDGE('',*,*,#11620,.F.);
#16845=ORIENTED_EDGE('',*,*,#11623,.F.);
#16846=ORIENTED_EDGE('',*,*,#11626,.F.);
#16847=ORIENTED_EDGE('',*,*,#11629,.F.);
#16848=ORIENTED_EDGE('',*,*,#11632,.F.);
#16849=ORIENTED_EDGE('',*,*,#11635,.F.);
#16850=ORIENTED_EDGE('',*,*,#11638,.F.);
#16851=ORIENTED_EDGE('',*,*,#11641,.F.);
#16852=ORIENTED_EDGE('',*,*,#11644,.F.);
#16853=ORIENTED_EDGE('',*,*,#11647,.F.);
#16854=ORIENTED_EDGE('',*,*,#11650,.F.);
#16855=ORIENTED_EDGE('',*,*,#11653,.F.);
#16856=ORIENTED_EDGE('',*,*,#11656,.F.);
#16857=ORIENTED_EDGE('',*,*,#11659,.F.);
#16858=ORIENTED_EDGE('',*,*,#11662,.F.);
#16859=ORIENTED_EDGE('',*,*,#11665,.F.);
#16860=ORIENTED_EDGE('',*,*,#11668,.F.);
#16861=ORIENTED_EDGE('',*,*,#11671,.F.);
#16862=ORIENTED_EDGE('',*,*,#11674,.F.);
#16863=ORIENTED_EDGE('',*,*,#11677,.F.);
#16864=ORIENTED_EDGE('',*,*,#11680,.F.);
#16865=ORIENTED_EDGE('',*,*,#11683,.F.);
#16866=ORIENTED_EDGE('',*,*,#11686,.F.);
#16867=ORIENTED_EDGE('',*,*,#11689,.F.);
#16868=ORIENTED_EDGE('',*,*,#11692,.F.);
#16869=ORIENTED_EDGE('',*,*,#11695,.F.);
#16870=ORIENTED_EDGE('',*,*,#11698,.F.);
#16871=ORIENTED_EDGE('',*,*,#11701,.F.);
#16872=ORIENTED_EDGE('',*,*,#11704,.F.);
#16873=ORIENTED_EDGE('',*,*,#11707,.F.);
#16874=ORIENTED_EDGE('',*,*,#11710,.F.);
#16875=ORIENTED_EDGE('',*,*,#11713,.F.);
#16876=ORIENTED_EDGE('',*,*,#11716,.F.);
#16877=ORIENTED_EDGE('',*,*,#11719,.F.);
#16878=ORIENTED_EDGE('',*,*,#11722,.F.);
#16879=ORIENTED_EDGE('',*,*,#11729,.F.);
#16880=ORIENTED_EDGE('',*,*,#11731,.F.);
#16881=ORIENTED_EDGE('',*,*,#11363,.F.);
#16882=ORIENTED_EDGE('',*,*,#11367,.F.);
#16883=ORIENTED_EDGE('',*,*,#11370,.F.);
#16884=ORIENTED_EDGE('',*,*,#11373,.F.);
#16885=ORIENTED_EDGE('',*,*,#11376,.F.);
#16886=ORIENTED_EDGE('',*,*,#11379,.F.);
#16887=ORIENTED_EDGE('',*,*,#11382,.F.);
#16888=ORIENTED_EDGE('',*,*,#11385,.F.);
#16889=ORIENTED_EDGE('',*,*,#11388,.F.);
#16890=ORIENTED_EDGE('',*,*,#11391,.F.);
#16891=ORIENTED_EDGE('',*,*,#11394,.F.);
#16892=ORIENTED_EDGE('',*,*,#11397,.F.);
#16893=ORIENTED_EDGE('',*,*,#11400,.F.);
#16894=ORIENTED_EDGE('',*,*,#11403,.F.);
#16895=ORIENTED_EDGE('',*,*,#11406,.F.);
#16896=ORIENTED_EDGE('',*,*,#11409,.F.);
#16897=ORIENTED_EDGE('',*,*,#11412,.F.);
#16898=ORIENTED_EDGE('',*,*,#11415,.F.);
#16899=ORIENTED_EDGE('',*,*,#11418,.F.);
#16900=ORIENTED_EDGE('',*,*,#11421,.F.);
#16901=ORIENTED_EDGE('',*,*,#11424,.F.);
#16902=ORIENTED_EDGE('',*,*,#11427,.F.);
#16903=ORIENTED_EDGE('',*,*,#11430,.F.);
#16904=ORIENTED_EDGE('',*,*,#11433,.F.);
#16905=ORIENTED_EDGE('',*,*,#11436,.F.);
#16906=ORIENTED_EDGE('',*,*,#11439,.F.);
#16907=ORIENTED_EDGE('',*,*,#11442,.F.);
#16908=ORIENTED_EDGE('',*,*,#11445,.F.);
#16909=ORIENTED_EDGE('',*,*,#11448,.F.);
#16910=ORIENTED_EDGE('',*,*,#11451,.F.);
#16911=ORIENTED_EDGE('',*,*,#11454,.F.);
#16912=ORIENTED_EDGE('',*,*,#11457,.F.);
#16913=ORIENTED_EDGE('',*,*,#11460,.F.);
#16914=ORIENTED_EDGE('',*,*,#11463,.F.);
#16915=ORIENTED_EDGE('',*,*,#11466,.F.);
#16916=ORIENTED_EDGE('',*,*,#11469,.F.);
#16917=ORIENTED_EDGE('',*,*,#11472,.F.);
#16918=ORIENTED_EDGE('',*,*,#11475,.F.);
#16919=ORIENTED_EDGE('',*,*,#11478,.F.);
#16920=ORIENTED_EDGE('',*,*,#11481,.F.);
#16921=ORIENTED_EDGE('',*,*,#11484,.F.);
#16922=ORIENTED_EDGE('',*,*,#11487,.F.);
#16923=ORIENTED_EDGE('',*,*,#11490,.F.);
#16924=ORIENTED_EDGE('',*,*,#11493,.F.);
#16925=ORIENTED_EDGE('',*,*,#11496,.F.);
#16926=ORIENTED_EDGE('',*,*,#11499,.F.);
#16927=ORIENTED_EDGE('',*,*,#11502,.F.);
#16928=ORIENTED_EDGE('',*,*,#11505,.F.);
#16929=ORIENTED_EDGE('',*,*,#11508,.F.);
#16930=ORIENTED_EDGE('',*,*,#11511,.F.);
#16931=ORIENTED_EDGE('',*,*,#11514,.F.);
#16932=ORIENTED_EDGE('',*,*,#11517,.F.);
#16933=ORIENTED_EDGE('',*,*,#11520,.F.);
#16934=ORIENTED_EDGE('',*,*,#11523,.F.);
#16935=ORIENTED_EDGE('',*,*,#11526,.F.);
#16936=ORIENTED_EDGE('',*,*,#11529,.F.);
#16937=ORIENTED_EDGE('',*,*,#11532,.F.);
#16938=ORIENTED_EDGE('',*,*,#11535,.F.);
#16939=ORIENTED_EDGE('',*,*,#11538,.F.);
#16940=ORIENTED_EDGE('',*,*,#11541,.F.);
#16941=ORIENTED_EDGE('',*,*,#11732,.F.);
#16942=ORIENTED_EDGE('',*,*,#11540,.T.);
#16943=ORIENTED_EDGE('',*,*,#11725,.T.);
#16944=ORIENTED_EDGE('',*,*,#11733,.F.);
#16945=ORIENTED_EDGE('',*,*,#11732,.T.);
#16946=ORIENTED_EDGE('',*,*,#11734,.T.);
#16947=ORIENTED_EDGE('',*,*,#11735,.T.);
#16948=ORIENTED_EDGE('',*,*,#11736,.T.);
#16949=ORIENTED_EDGE('',*,*,#11737,.T.);
#16950=ORIENTED_EDGE('',*,*,#11738,.T.);
#16951=ORIENTED_EDGE('',*,*,#11739,.T.);
#16952=ORIENTED_EDGE('',*,*,#11731,.T.);
#16953=ORIENTED_EDGE('',*,*,#11728,.T.);
#16954=ORIENTED_EDGE('',*,*,#11726,.T.);
#16955=ORIENTED_EDGE('',*,*,#11364,.F.);
#16956=ORIENTED_EDGE('',*,*,#11740,.F.);
#16957=ORIENTED_EDGE('',*,*,#11741,.F.);
#16958=ORIENTED_EDGE('',*,*,#11742,.F.);
#16959=ORIENTED_EDGE('',*,*,#11743,.F.);
#16960=ORIENTED_EDGE('',*,*,#11744,.F.);
#16961=ORIENTED_EDGE('',*,*,#11745,.F.);
#16962=ORIENTED_EDGE('',*,*,#11746,.F.);
#16963=ORIENTED_EDGE('',*,*,#11741,.T.);
#16964=ORIENTED_EDGE('',*,*,#11747,.T.);
#16965=ORIENTED_EDGE('',*,*,#11739,.F.);
#16966=ORIENTED_EDGE('',*,*,#11748,.F.);
#16967=ORIENTED_EDGE('',*,*,#11742,.T.);
#16968=ORIENTED_EDGE('',*,*,#11748,.T.);
#16969=ORIENTED_EDGE('',*,*,#11738,.F.);
#16970=ORIENTED_EDGE('',*,*,#11749,.F.);
#16971=ORIENTED_EDGE('',*,*,#11743,.T.);
#16972=ORIENTED_EDGE('',*,*,#11749,.T.);
#16973=ORIENTED_EDGE('',*,*,#11737,.F.);
#16974=ORIENTED_EDGE('',*,*,#11750,.F.);
#16975=ORIENTED_EDGE('',*,*,#11744,.T.);
#16976=ORIENTED_EDGE('',*,*,#11750,.T.);
#16977=ORIENTED_EDGE('',*,*,#11736,.F.);
#16978=ORIENTED_EDGE('',*,*,#11751,.F.);
#16979=ORIENTED_EDGE('',*,*,#11745,.T.);
#16980=ORIENTED_EDGE('',*,*,#11751,.T.);
#16981=ORIENTED_EDGE('',*,*,#11735,.F.);
#16982=ORIENTED_EDGE('',*,*,#11752,.F.);
#16983=ORIENTED_EDGE('',*,*,#11740,.T.);
#16984=ORIENTED_EDGE('',*,*,#11752,.T.);
#16985=ORIENTED_EDGE('',*,*,#11734,.F.);
#16986=ORIENTED_EDGE('',*,*,#11747,.F.);
#16987=ORIENTED_EDGE('',*,*,#11746,.T.);
#16988=ORIENTED_EDGE('',*,*,#11753,.T.);
#16989=ORIENTED_EDGE('',*,*,#11754,.F.);
#16990=ORIENTED_EDGE('',*,*,#11753,.F.);
#16991=ORIENTED_EDGE('',*,*,#11730,.T.);
#16992=ORIENTED_EDGE('',*,*,#11733,.T.);
#16993=ORIENTED_EDGE('',*,*,#11724,.T.);
#16994=ORIENTED_EDGE('',*,*,#11545,.T.);
#16995=ORIENTED_EDGE('',*,*,#11754,.T.);
#16996=ORIENTED_EDGE('',*,*,#11755,.T.);
#16997=ORIENTED_EDGE('',*,*,#11755,.F.);
#16998=ORIENTED_EDGE('',*,*,#11756,.T.);
#16999=ORIENTED_EDGE('',*,*,#11757,.T.);
#17000=ORIENTED_EDGE('',*,*,#11758,.F.);
#17001=ORIENTED_EDGE('',*,*,#11759,.T.);
#17002=ORIENTED_EDGE('',*,*,#11760,.T.);
#17003=ORIENTED_EDGE('',*,*,#11761,.T.);
#17004=ORIENTED_EDGE('',*,*,#11756,.F.);
#17005=ORIENTED_EDGE('',*,*,#11762,.T.);
#17006=ORIENTED_EDGE('',*,*,#11763,.T.);
#17007=ORIENTED_EDGE('',*,*,#11764,.T.);
#17008=ORIENTED_EDGE('',*,*,#11760,.F.);
#17009=ORIENTED_EDGE('',*,*,#11765,.T.);
#17010=ORIENTED_EDGE('',*,*,#11766,.T.);
#17011=ORIENTED_EDGE('',*,*,#11767,.T.);
#17012=ORIENTED_EDGE('',*,*,#11763,.F.);
#17013=ORIENTED_EDGE('',*,*,#11768,.T.);
#17014=ORIENTED_EDGE('',*,*,#11769,.T.);
#17015=ORIENTED_EDGE('',*,*,#11770,.T.);
#17016=ORIENTED_EDGE('',*,*,#11766,.F.);
#17017=ORIENTED_EDGE('',*,*,#11771,.T.);
#17018=ORIENTED_EDGE('',*,*,#11772,.T.);
#17019=ORIENTED_EDGE('',*,*,#11773,.T.);
#17020=ORIENTED_EDGE('',*,*,#11769,.F.);
#17021=ORIENTED_EDGE('',*,*,#11774,.T.);
#17022=ORIENTED_EDGE('',*,*,#11775,.T.);
#17023=ORIENTED_EDGE('',*,*,#11776,.T.);
#17024=ORIENTED_EDGE('',*,*,#11772,.F.);
#17025=ORIENTED_EDGE('',*,*,#11777,.T.);
#17026=ORIENTED_EDGE('',*,*,#11778,.F.);
#17027=ORIENTED_EDGE('',*,*,#11779,.T.);
#17028=ORIENTED_EDGE('',*,*,#11780,.F.);
#17029=ORIENTED_EDGE('',*,*,#11781,.T.);
#17030=ORIENTED_EDGE('',*,*,#11782,.T.);
#17031=ORIENTED_EDGE('',*,*,#11783,.T.);
#17032=ORIENTED_EDGE('',*,*,#11784,.F.);
#17033=ORIENTED_EDGE('',*,*,#11785,.F.);
#17034=ORIENTED_EDGE('',*,*,#11786,.T.);
#17035=ORIENTED_EDGE('',*,*,#11787,.T.);
#17036=ORIENTED_EDGE('',*,*,#11782,.F.);
#17037=ORIENTED_EDGE('',*,*,#11788,.F.);
#17038=ORIENTED_EDGE('',*,*,#11789,.T.);
#17039=ORIENTED_EDGE('',*,*,#11790,.T.);
#17040=ORIENTED_EDGE('',*,*,#11786,.F.);
#17041=ORIENTED_EDGE('',*,*,#11791,.F.);
#17042=ORIENTED_EDGE('',*,*,#11792,.T.);
#17043=ORIENTED_EDGE('',*,*,#11793,.T.);
#17044=ORIENTED_EDGE('',*,*,#11789,.F.);
#17045=ORIENTED_EDGE('',*,*,#11794,.F.);
#17046=ORIENTED_EDGE('',*,*,#11795,.T.);
#17047=ORIENTED_EDGE('',*,*,#11796,.T.);
#17048=ORIENTED_EDGE('',*,*,#11792,.F.);
#17049=ORIENTED_EDGE('',*,*,#11797,.F.);
#17050=ORIENTED_EDGE('',*,*,#11798,.T.);
#17051=ORIENTED_EDGE('',*,*,#11799,.T.);
#17052=ORIENTED_EDGE('',*,*,#11795,.F.);
#17053=ORIENTED_EDGE('',*,*,#11800,.F.);
#17054=ORIENTED_EDGE('',*,*,#11801,.T.);
#17055=ORIENTED_EDGE('',*,*,#11802,.T.);
#17056=ORIENTED_EDGE('',*,*,#11798,.F.);
#17057=ORIENTED_EDGE('',*,*,#11803,.F.);
#17058=ORIENTED_EDGE('',*,*,#11804,.F.);
#17059=ORIENTED_EDGE('',*,*,#11805,.F.);
#17060=ORIENTED_EDGE('',*,*,#11806,.F.);
#17061=ORIENTED_EDGE('',*,*,#11807,.T.);
#17062=ORIENTED_EDGE('',*,*,#11804,.T.);
#17063=ORIENTED_EDGE('',*,*,#11808,.T.);
#17064=ORIENTED_EDGE('',*,*,#11801,.F.);
#17065=ORIENTED_EDGE('',*,*,#11809,.F.);
#17066=ORIENTED_EDGE('',*,*,#11810,.F.);
#17067=ORIENTED_EDGE('',*,*,#11783,.F.);
#17068=ORIENTED_EDGE('',*,*,#11787,.F.);
#17069=ORIENTED_EDGE('',*,*,#11790,.F.);
#17070=ORIENTED_EDGE('',*,*,#11793,.F.);
#17071=ORIENTED_EDGE('',*,*,#11796,.F.);
#17072=ORIENTED_EDGE('',*,*,#11799,.F.);
#17073=ORIENTED_EDGE('',*,*,#11802,.F.);
#17074=ORIENTED_EDGE('',*,*,#11808,.F.);
#17075=ORIENTED_EDGE('',*,*,#11807,.F.);
#17076=ORIENTED_EDGE('',*,*,#11811,.F.);
#17077=ORIENTED_EDGE('',*,*,#11779,.F.);
#17078=ORIENTED_EDGE('',*,*,#11812,.F.);
#17079=ORIENTED_EDGE('',*,*,#11777,.F.);
#17080=ORIENTED_EDGE('',*,*,#11774,.F.);
#17081=ORIENTED_EDGE('',*,*,#11771,.F.);
#17082=ORIENTED_EDGE('',*,*,#11768,.F.);
#17083=ORIENTED_EDGE('',*,*,#11765,.F.);
#17084=ORIENTED_EDGE('',*,*,#11762,.F.);
#17085=ORIENTED_EDGE('',*,*,#11759,.F.);
#17086=ORIENTED_EDGE('',*,*,#11813,.F.);
#17087=ORIENTED_EDGE('',*,*,#11757,.F.);
#17088=ORIENTED_EDGE('',*,*,#11761,.F.);
#17089=ORIENTED_EDGE('',*,*,#11764,.F.);
#17090=ORIENTED_EDGE('',*,*,#11767,.F.);
#17091=ORIENTED_EDGE('',*,*,#11770,.F.);
#17092=ORIENTED_EDGE('',*,*,#11773,.F.);
#17093=ORIENTED_EDGE('',*,*,#11776,.F.);
#17094=ORIENTED_EDGE('',*,*,#11814,.F.);
#17095=ORIENTED_EDGE('',*,*,#11781,.F.);
#17096=ORIENTED_EDGE('',*,*,#11815,.F.);
#17097=ORIENTED_EDGE('',*,*,#11805,.T.);
#17098=ORIENTED_EDGE('',*,*,#11809,.T.);
#17099=ORIENTED_EDGE('',*,*,#11803,.T.);
#17100=ORIENTED_EDGE('',*,*,#11800,.T.);
#17101=ORIENTED_EDGE('',*,*,#11797,.T.);
#17102=ORIENTED_EDGE('',*,*,#11794,.T.);
#17103=ORIENTED_EDGE('',*,*,#11791,.T.);
#17104=ORIENTED_EDGE('',*,*,#11788,.T.);
#17105=ORIENTED_EDGE('',*,*,#11785,.T.);
#17106=ORIENTED_EDGE('',*,*,#11816,.T.);
#17107=ORIENTED_EDGE('',*,*,#11817,.T.);
#17108=ORIENTED_EDGE('',*,*,#11818,.T.);
#17109=ORIENTED_EDGE('',*,*,#11819,.T.);
#17110=ORIENTED_EDGE('',*,*,#11820,.T.);
#17111=ORIENTED_EDGE('',*,*,#11821,.T.);
#17112=ORIENTED_EDGE('',*,*,#11811,.T.);
#17113=ORIENTED_EDGE('',*,*,#11806,.T.);
#17114=ORIENTED_EDGE('',*,*,#11815,.T.);
#17115=ORIENTED_EDGE('',*,*,#11780,.T.);
#17116=ORIENTED_EDGE('',*,*,#11778,.T.);
#17117=ORIENTED_EDGE('',*,*,#11814,.T.);
#17118=ORIENTED_EDGE('',*,*,#11775,.F.);
#17119=ORIENTED_EDGE('',*,*,#11812,.T.);
#17120=ORIENTED_EDGE('',*,*,#11822,.T.);
#17121=ORIENTED_EDGE('',*,*,#11823,.T.);
#17122=ORIENTED_EDGE('',*,*,#11821,.F.);
#17123=ORIENTED_EDGE('',*,*,#11824,.F.);
#17124=ORIENTED_EDGE('',*,*,#11825,.T.);
#17125=ORIENTED_EDGE('',*,*,#11824,.T.);
#17126=ORIENTED_EDGE('',*,*,#11820,.F.);
#17127=ORIENTED_EDGE('',*,*,#11826,.F.);
#17128=ORIENTED_EDGE('',*,*,#11827,.T.);
#17129=ORIENTED_EDGE('',*,*,#11826,.T.);
#17130=ORIENTED_EDGE('',*,*,#11819,.F.);
#17131=ORIENTED_EDGE('',*,*,#11828,.F.);
#17132=ORIENTED_EDGE('',*,*,#11829,.T.);
#17133=ORIENTED_EDGE('',*,*,#11828,.T.);
#17134=ORIENTED_EDGE('',*,*,#11818,.F.);
#17135=ORIENTED_EDGE('',*,*,#11830,.F.);
#17136=ORIENTED_EDGE('',*,*,#11831,.T.);
#17137=ORIENTED_EDGE('',*,*,#11830,.T.);
#17138=ORIENTED_EDGE('',*,*,#11817,.F.);
#17139=ORIENTED_EDGE('',*,*,#11832,.F.);
#17140=ORIENTED_EDGE('',*,*,#11833,.T.);
#17141=ORIENTED_EDGE('',*,*,#11832,.T.);
#17142=ORIENTED_EDGE('',*,*,#11816,.F.);
#17143=ORIENTED_EDGE('',*,*,#11823,.F.);
#17144=ORIENTED_EDGE('',*,*,#11833,.F.);
#17145=ORIENTED_EDGE('',*,*,#11822,.F.);
#17146=ORIENTED_EDGE('',*,*,#11825,.F.);
#17147=ORIENTED_EDGE('',*,*,#11827,.F.);
#17148=ORIENTED_EDGE('',*,*,#11829,.F.);
#17149=ORIENTED_EDGE('',*,*,#11831,.F.);
#17150=ORIENTED_EDGE('',*,*,#11810,.T.);
#17151=ORIENTED_EDGE('',*,*,#11758,.T.);
#17152=ORIENTED_EDGE('',*,*,#11813,.T.);
#17153=ORIENTED_EDGE('',*,*,#11784,.T.);
#17154=ORIENTED_EDGE('',*,*,#11834,.F.);
#17155=ORIENTED_EDGE('',*,*,#11835,.T.);
#17156=ORIENTED_EDGE('',*,*,#11836,.T.);
#17157=ORIENTED_EDGE('',*,*,#11835,.F.);
#17158=ORIENTED_EDGE('',*,*,#11837,.F.);
#17159=ORIENTED_EDGE('',*,*,#11838,.T.);
#17160=ORIENTED_EDGE('',*,*,#11839,.T.);
#17161=ORIENTED_EDGE('',*,*,#11838,.F.);
#17162=ORIENTED_EDGE('',*,*,#11837,.T.);
#17163=ORIENTED_EDGE('',*,*,#11834,.T.);
#17164=ORIENTED_EDGE('',*,*,#11839,.F.);
#17165=ORIENTED_EDGE('',*,*,#11836,.F.);
#17166=ORIENTED_EDGE('',*,*,#11840,.F.);
#17167=ORIENTED_EDGE('',*,*,#11841,.T.);
#17168=ORIENTED_EDGE('',*,*,#11842,.T.);
#17169=ORIENTED_EDGE('',*,*,#11843,.T.);
#17170=ORIENTED_EDGE('',*,*,#11844,.F.);
#17171=ORIENTED_EDGE('',*,*,#11845,.T.);
#17172=ORIENTED_EDGE('',*,*,#11840,.T.);
#17173=ORIENTED_EDGE('',*,*,#11846,.T.);
#17174=ORIENTED_EDGE('',*,*,#11847,.F.);
#17175=ORIENTED_EDGE('',*,*,#11848,.T.);
#17176=ORIENTED_EDGE('',*,*,#11844,.T.);
#17177=ORIENTED_EDGE('',*,*,#11849,.T.);
#17178=ORIENTED_EDGE('',*,*,#11850,.F.);
#17179=ORIENTED_EDGE('',*,*,#11851,.T.);
#17180=ORIENTED_EDGE('',*,*,#11847,.T.);
#17181=ORIENTED_EDGE('',*,*,#11852,.T.);
#17182=ORIENTED_EDGE('',*,*,#11853,.F.);
#17183=ORIENTED_EDGE('',*,*,#11854,.T.);
#17184=ORIENTED_EDGE('',*,*,#11850,.T.);
#17185=ORIENTED_EDGE('',*,*,#11855,.T.);
#17186=ORIENTED_EDGE('',*,*,#11856,.F.);
#17187=ORIENTED_EDGE('',*,*,#11857,.T.);
#17188=ORIENTED_EDGE('',*,*,#11853,.T.);
#17189=ORIENTED_EDGE('',*,*,#11858,.T.);
#17190=ORIENTED_EDGE('',*,*,#11859,.F.);
#17191=ORIENTED_EDGE('',*,*,#11860,.T.);
#17192=ORIENTED_EDGE('',*,*,#11856,.T.);
#17193=ORIENTED_EDGE('',*,*,#11861,.T.);
#17194=ORIENTED_EDGE('',*,*,#11862,.F.);
#17195=ORIENTED_EDGE('',*,*,#11863,.T.);
#17196=ORIENTED_EDGE('',*,*,#11859,.T.);
#17197=ORIENTED_EDGE('',*,*,#11864,.T.);
#17198=ORIENTED_EDGE('',*,*,#11865,.F.);
#17199=ORIENTED_EDGE('',*,*,#11866,.T.);
#17200=ORIENTED_EDGE('',*,*,#11862,.T.);
#17201=ORIENTED_EDGE('',*,*,#11867,.T.);
#17202=ORIENTED_EDGE('',*,*,#11868,.F.);
#17203=ORIENTED_EDGE('',*,*,#11869,.T.);
#17204=ORIENTED_EDGE('',*,*,#11865,.T.);
#17205=ORIENTED_EDGE('',*,*,#11870,.T.);
#17206=ORIENTED_EDGE('',*,*,#11871,.F.);
#17207=ORIENTED_EDGE('',*,*,#11872,.T.);
#17208=ORIENTED_EDGE('',*,*,#11868,.T.);
#17209=ORIENTED_EDGE('',*,*,#11873,.T.);
#17210=ORIENTED_EDGE('',*,*,#11874,.F.);
#17211=ORIENTED_EDGE('',*,*,#11875,.T.);
#17212=ORIENTED_EDGE('',*,*,#11871,.T.);
#17213=ORIENTED_EDGE('',*,*,#11876,.T.);
#17214=ORIENTED_EDGE('',*,*,#11877,.F.);
#17215=ORIENTED_EDGE('',*,*,#11878,.T.);
#17216=ORIENTED_EDGE('',*,*,#11874,.T.);
#17217=ORIENTED_EDGE('',*,*,#11879,.T.);
#17218=ORIENTED_EDGE('',*,*,#11880,.F.);
#17219=ORIENTED_EDGE('',*,*,#11881,.T.);
#17220=ORIENTED_EDGE('',*,*,#11877,.T.);
#17221=ORIENTED_EDGE('',*,*,#11882,.T.);
#17222=ORIENTED_EDGE('',*,*,#11883,.F.);
#17223=ORIENTED_EDGE('',*,*,#11884,.T.);
#17224=ORIENTED_EDGE('',*,*,#11880,.T.);
#17225=ORIENTED_EDGE('',*,*,#11885,.T.);
#17226=ORIENTED_EDGE('',*,*,#11886,.F.);
#17227=ORIENTED_EDGE('',*,*,#11887,.T.);
#17228=ORIENTED_EDGE('',*,*,#11888,.T.);
#17229=ORIENTED_EDGE('',*,*,#11889,.F.);
#17230=ORIENTED_EDGE('',*,*,#11890,.F.);
#17231=ORIENTED_EDGE('',*,*,#11891,.T.);
#17232=ORIENTED_EDGE('',*,*,#11886,.T.);
#17233=ORIENTED_EDGE('',*,*,#11892,.F.);
#17234=ORIENTED_EDGE('',*,*,#11893,.F.);
#17235=ORIENTED_EDGE('',*,*,#11894,.T.);
#17236=ORIENTED_EDGE('',*,*,#11890,.T.);
#17237=ORIENTED_EDGE('',*,*,#11895,.F.);
#17238=ORIENTED_EDGE('',*,*,#11896,.F.);
#17239=ORIENTED_EDGE('',*,*,#11897,.T.);
#17240=ORIENTED_EDGE('',*,*,#11893,.T.);
#17241=ORIENTED_EDGE('',*,*,#11898,.F.);
#17242=ORIENTED_EDGE('',*,*,#11899,.F.);
#17243=ORIENTED_EDGE('',*,*,#11900,.T.);
#17244=ORIENTED_EDGE('',*,*,#11896,.T.);
#17245=ORIENTED_EDGE('',*,*,#11901,.F.);
#17246=ORIENTED_EDGE('',*,*,#11902,.F.);
#17247=ORIENTED_EDGE('',*,*,#11903,.T.);
#17248=ORIENTED_EDGE('',*,*,#11899,.T.);
#17249=ORIENTED_EDGE('',*,*,#11904,.F.);
#17250=ORIENTED_EDGE('',*,*,#11905,.F.);
#17251=ORIENTED_EDGE('',*,*,#11906,.T.);
#17252=ORIENTED_EDGE('',*,*,#11902,.T.);
#17253=ORIENTED_EDGE('',*,*,#11907,.F.);
#17254=ORIENTED_EDGE('',*,*,#11908,.F.);
#17255=ORIENTED_EDGE('',*,*,#11909,.T.);
#17256=ORIENTED_EDGE('',*,*,#11905,.T.);
#17257=ORIENTED_EDGE('',*,*,#11910,.F.);
#17258=ORIENTED_EDGE('',*,*,#11911,.F.);
#17259=ORIENTED_EDGE('',*,*,#11912,.T.);
#17260=ORIENTED_EDGE('',*,*,#11908,.T.);
#17261=ORIENTED_EDGE('',*,*,#11913,.F.);
#17262=ORIENTED_EDGE('',*,*,#11914,.F.);
#17263=ORIENTED_EDGE('',*,*,#11915,.T.);
#17264=ORIENTED_EDGE('',*,*,#11911,.T.);
#17265=ORIENTED_EDGE('',*,*,#11916,.F.);
#17266=ORIENTED_EDGE('',*,*,#11917,.F.);
#17267=ORIENTED_EDGE('',*,*,#11918,.T.);
#17268=ORIENTED_EDGE('',*,*,#11914,.T.);
#17269=ORIENTED_EDGE('',*,*,#11919,.F.);
#17270=ORIENTED_EDGE('',*,*,#11920,.F.);
#17271=ORIENTED_EDGE('',*,*,#11921,.T.);
#17272=ORIENTED_EDGE('',*,*,#11917,.T.);
#17273=ORIENTED_EDGE('',*,*,#11922,.F.);
#17274=ORIENTED_EDGE('',*,*,#11923,.F.);
#17275=ORIENTED_EDGE('',*,*,#11924,.T.);
#17276=ORIENTED_EDGE('',*,*,#11920,.T.);
#17277=ORIENTED_EDGE('',*,*,#11925,.F.);
#17278=ORIENTED_EDGE('',*,*,#11926,.F.);
#17279=ORIENTED_EDGE('',*,*,#11927,.T.);
#17280=ORIENTED_EDGE('',*,*,#11923,.T.);
#17281=ORIENTED_EDGE('',*,*,#11928,.F.);
#17282=ORIENTED_EDGE('',*,*,#11929,.F.);
#17283=ORIENTED_EDGE('',*,*,#11930,.T.);
#17284=ORIENTED_EDGE('',*,*,#11926,.T.);
#17285=ORIENTED_EDGE('',*,*,#11931,.F.);
#17286=ORIENTED_EDGE('',*,*,#11932,.F.);
#17287=ORIENTED_EDGE('',*,*,#11888,.F.);
#17288=ORIENTED_EDGE('',*,*,#11933,.F.);
#17289=ORIENTED_EDGE('',*,*,#11934,.F.);
#17290=ORIENTED_EDGE('',*,*,#11935,.F.);
#17291=ORIENTED_EDGE('',*,*,#11936,.T.);
#17292=ORIENTED_EDGE('',*,*,#11937,.F.);
#17293=ORIENTED_EDGE('',*,*,#11936,.F.);
#17294=ORIENTED_EDGE('',*,*,#11933,.T.);
#17295=ORIENTED_EDGE('',*,*,#11887,.F.);
#17296=ORIENTED_EDGE('',*,*,#11891,.F.);
#17297=ORIENTED_EDGE('',*,*,#11894,.F.);
#17298=ORIENTED_EDGE('',*,*,#11897,.F.);
#17299=ORIENTED_EDGE('',*,*,#11900,.F.);
#17300=ORIENTED_EDGE('',*,*,#11903,.F.);
#17301=ORIENTED_EDGE('',*,*,#11906,.F.);
#17302=ORIENTED_EDGE('',*,*,#11909,.F.);
#17303=ORIENTED_EDGE('',*,*,#11912,.F.);
#17304=ORIENTED_EDGE('',*,*,#11915,.F.);
#17305=ORIENTED_EDGE('',*,*,#11918,.F.);
#17306=ORIENTED_EDGE('',*,*,#11921,.F.);
#17307=ORIENTED_EDGE('',*,*,#11924,.F.);
#17308=ORIENTED_EDGE('',*,*,#11927,.F.);
#17309=ORIENTED_EDGE('',*,*,#11930,.F.);
#17310=ORIENTED_EDGE('',*,*,#11938,.F.);
#17311=ORIENTED_EDGE('',*,*,#11939,.F.);
#17312=ORIENTED_EDGE('',*,*,#11841,.F.);
#17313=ORIENTED_EDGE('',*,*,#11845,.F.);
#17314=ORIENTED_EDGE('',*,*,#11848,.F.);
#17315=ORIENTED_EDGE('',*,*,#11851,.F.);
#17316=ORIENTED_EDGE('',*,*,#11854,.F.);
#17317=ORIENTED_EDGE('',*,*,#11857,.F.);
#17318=ORIENTED_EDGE('',*,*,#11860,.F.);
#17319=ORIENTED_EDGE('',*,*,#11863,.F.);
#17320=ORIENTED_EDGE('',*,*,#11866,.F.);
#17321=ORIENTED_EDGE('',*,*,#11869,.F.);
#17322=ORIENTED_EDGE('',*,*,#11872,.F.);
#17323=ORIENTED_EDGE('',*,*,#11875,.F.);
#17324=ORIENTED_EDGE('',*,*,#11878,.F.);
#17325=ORIENTED_EDGE('',*,*,#11881,.F.);
#17326=ORIENTED_EDGE('',*,*,#11884,.F.);
#17327=ORIENTED_EDGE('',*,*,#11940,.F.);
#17328=ORIENTED_EDGE('',*,*,#11929,.T.);
#17329=ORIENTED_EDGE('',*,*,#11941,.F.);
#17330=ORIENTED_EDGE('',*,*,#11942,.F.);
#17331=ORIENTED_EDGE('',*,*,#11938,.T.);
#17332=ORIENTED_EDGE('',*,*,#11932,.T.);
#17333=ORIENTED_EDGE('',*,*,#11935,.T.);
#17334=ORIENTED_EDGE('',*,*,#11943,.F.);
#17335=ORIENTED_EDGE('',*,*,#11885,.F.);
#17336=ORIENTED_EDGE('',*,*,#11882,.F.);
#17337=ORIENTED_EDGE('',*,*,#11879,.F.);
#17338=ORIENTED_EDGE('',*,*,#11876,.F.);
#17339=ORIENTED_EDGE('',*,*,#11873,.F.);
#17340=ORIENTED_EDGE('',*,*,#11870,.F.);
#17341=ORIENTED_EDGE('',*,*,#11867,.F.);
#17342=ORIENTED_EDGE('',*,*,#11864,.F.);
#17343=ORIENTED_EDGE('',*,*,#11861,.F.);
#17344=ORIENTED_EDGE('',*,*,#11858,.F.);
#17345=ORIENTED_EDGE('',*,*,#11855,.F.);
#17346=ORIENTED_EDGE('',*,*,#11852,.F.);
#17347=ORIENTED_EDGE('',*,*,#11849,.F.);
#17348=ORIENTED_EDGE('',*,*,#11846,.F.);
#17349=ORIENTED_EDGE('',*,*,#11843,.F.);
#17350=ORIENTED_EDGE('',*,*,#11944,.F.);
#17351=ORIENTED_EDGE('',*,*,#11941,.T.);
#17352=ORIENTED_EDGE('',*,*,#11931,.T.);
#17353=ORIENTED_EDGE('',*,*,#11928,.T.);
#17354=ORIENTED_EDGE('',*,*,#11925,.T.);
#17355=ORIENTED_EDGE('',*,*,#11922,.T.);
#17356=ORIENTED_EDGE('',*,*,#11919,.T.);
#17357=ORIENTED_EDGE('',*,*,#11916,.T.);
#17358=ORIENTED_EDGE('',*,*,#11913,.T.);
#17359=ORIENTED_EDGE('',*,*,#11910,.T.);
#17360=ORIENTED_EDGE('',*,*,#11907,.T.);
#17361=ORIENTED_EDGE('',*,*,#11904,.T.);
#17362=ORIENTED_EDGE('',*,*,#11901,.T.);
#17363=ORIENTED_EDGE('',*,*,#11898,.T.);
#17364=ORIENTED_EDGE('',*,*,#11895,.T.);
#17365=ORIENTED_EDGE('',*,*,#11892,.T.);
#17366=ORIENTED_EDGE('',*,*,#11889,.T.);
#17367=ORIENTED_EDGE('',*,*,#11883,.T.);
#17368=ORIENTED_EDGE('',*,*,#11943,.T.);
#17369=ORIENTED_EDGE('',*,*,#11934,.T.);
#17370=ORIENTED_EDGE('',*,*,#11940,.T.);
#17371=ORIENTED_EDGE('',*,*,#11945,.F.);
#17372=ORIENTED_EDGE('',*,*,#11946,.T.);
#17373=ORIENTED_EDGE('',*,*,#11947,.T.);
#17374=ORIENTED_EDGE('',*,*,#11948,.F.);
#17375=ORIENTED_EDGE('',*,*,#11949,.F.);
#17376=ORIENTED_EDGE('',*,*,#11950,.T.);
#17377=ORIENTED_EDGE('',*,*,#11951,.T.);
#17378=ORIENTED_EDGE('',*,*,#11946,.F.);
#17379=ORIENTED_EDGE('',*,*,#11952,.F.);
#17380=ORIENTED_EDGE('',*,*,#11953,.T.);
#17381=ORIENTED_EDGE('',*,*,#11954,.T.);
#17382=ORIENTED_EDGE('',*,*,#11950,.F.);
#17383=ORIENTED_EDGE('',*,*,#11955,.F.);
#17384=ORIENTED_EDGE('',*,*,#11956,.T.);
#17385=ORIENTED_EDGE('',*,*,#11957,.T.);
#17386=ORIENTED_EDGE('',*,*,#11953,.F.);
#17387=ORIENTED_EDGE('',*,*,#11958,.F.);
#17388=ORIENTED_EDGE('',*,*,#11959,.T.);
#17389=ORIENTED_EDGE('',*,*,#11960,.T.);
#17390=ORIENTED_EDGE('',*,*,#11956,.F.);
#17391=ORIENTED_EDGE('',*,*,#11961,.F.);
#17392=ORIENTED_EDGE('',*,*,#11948,.T.);
#17393=ORIENTED_EDGE('',*,*,#11962,.T.);
#17394=ORIENTED_EDGE('',*,*,#11959,.F.);
#17395=ORIENTED_EDGE('',*,*,#11962,.F.);
#17396=ORIENTED_EDGE('',*,*,#11947,.F.);
#17397=ORIENTED_EDGE('',*,*,#11951,.F.);
#17398=ORIENTED_EDGE('',*,*,#11954,.F.);
#17399=ORIENTED_EDGE('',*,*,#11957,.F.);
#17400=ORIENTED_EDGE('',*,*,#11960,.F.);
#17401=ORIENTED_EDGE('',*,*,#11963,.T.);
#17402=ORIENTED_EDGE('',*,*,#11939,.T.);
#17403=ORIENTED_EDGE('',*,*,#11942,.T.);
#17404=ORIENTED_EDGE('',*,*,#11944,.T.);
#17405=ORIENTED_EDGE('',*,*,#11842,.F.);
#17406=ORIENTED_EDGE('',*,*,#11963,.F.);
#17407=ORIENTED_EDGE('',*,*,#11964,.T.);
#17408=ORIENTED_EDGE('',*,*,#11965,.T.);
#17409=ORIENTED_EDGE('',*,*,#11964,.F.);
#17410=ORIENTED_EDGE('',*,*,#11965,.F.);
#17411=ORIENTED_EDGE('',*,*,#11945,.T.);
#17412=ORIENTED_EDGE('',*,*,#11961,.T.);
#17413=ORIENTED_EDGE('',*,*,#11958,.T.);
#17414=ORIENTED_EDGE('',*,*,#11955,.T.);
#17415=ORIENTED_EDGE('',*,*,#11952,.T.);
#17416=ORIENTED_EDGE('',*,*,#11949,.T.);
#17417=ORIENTED_EDGE('',*,*,#11937,.T.);
#17418=ORIENTED_EDGE('',*,*,#11966,.T.);
#17419=ORIENTED_EDGE('',*,*,#11967,.T.);
#17420=ORIENTED_EDGE('',*,*,#11968,.F.);
#17421=ORIENTED_EDGE('',*,*,#11969,.T.);
#17422=ORIENTED_EDGE('',*,*,#11970,.T.);
#17423=ORIENTED_EDGE('',*,*,#11971,.T.);
#17424=ORIENTED_EDGE('',*,*,#11966,.F.);
#17425=ORIENTED_EDGE('',*,*,#11972,.T.);
#17426=ORIENTED_EDGE('',*,*,#11973,.T.);
#17427=ORIENTED_EDGE('',*,*,#11974,.T.);
#17428=ORIENTED_EDGE('',*,*,#11970,.F.);
#17429=ORIENTED_EDGE('',*,*,#11975,.T.);
#17430=ORIENTED_EDGE('',*,*,#11976,.T.);
#17431=ORIENTED_EDGE('',*,*,#11977,.T.);
#17432=ORIENTED_EDGE('',*,*,#11973,.F.);
#17433=ORIENTED_EDGE('',*,*,#11978,.T.);
#17434=ORIENTED_EDGE('',*,*,#11979,.T.);
#17435=ORIENTED_EDGE('',*,*,#11980,.T.);
#17436=ORIENTED_EDGE('',*,*,#11976,.F.);
#17437=ORIENTED_EDGE('',*,*,#11981,.T.);
#17438=ORIENTED_EDGE('',*,*,#11982,.T.);
#17439=ORIENTED_EDGE('',*,*,#11983,.T.);
#17440=ORIENTED_EDGE('',*,*,#11979,.F.);
#17441=ORIENTED_EDGE('',*,*,#11984,.T.);
#17442=ORIENTED_EDGE('',*,*,#11985,.T.);
#17443=ORIENTED_EDGE('',*,*,#11986,.T.);
#17444=ORIENTED_EDGE('',*,*,#11982,.F.);
#17445=ORIENTED_EDGE('',*,*,#11987,.T.);
#17446=ORIENTED_EDGE('',*,*,#11988,.T.);
#17447=ORIENTED_EDGE('',*,*,#11989,.T.);
#17448=ORIENTED_EDGE('',*,*,#11985,.F.);
#17449=ORIENTED_EDGE('',*,*,#11990,.T.);
#17450=ORIENTED_EDGE('',*,*,#11991,.T.);
#17451=ORIENTED_EDGE('',*,*,#11992,.T.);
#17452=ORIENTED_EDGE('',*,*,#11988,.F.);
#17453=ORIENTED_EDGE('',*,*,#11993,.T.);
#17454=ORIENTED_EDGE('',*,*,#11994,.T.);
#17455=ORIENTED_EDGE('',*,*,#11995,.T.);
#17456=ORIENTED_EDGE('',*,*,#11991,.F.);
#17457=ORIENTED_EDGE('',*,*,#11996,.T.);
#17458=ORIENTED_EDGE('',*,*,#11997,.T.);
#17459=ORIENTED_EDGE('',*,*,#11998,.T.);
#17460=ORIENTED_EDGE('',*,*,#11994,.F.);
#17461=ORIENTED_EDGE('',*,*,#11999,.T.);
#17462=ORIENTED_EDGE('',*,*,#12000,.T.);
#17463=ORIENTED_EDGE('',*,*,#12001,.T.);
#17464=ORIENTED_EDGE('',*,*,#11997,.F.);
#17465=ORIENTED_EDGE('',*,*,#12002,.T.);
#17466=ORIENTED_EDGE('',*,*,#12003,.T.);
#17467=ORIENTED_EDGE('',*,*,#12004,.T.);
#17468=ORIENTED_EDGE('',*,*,#12000,.F.);
#17469=ORIENTED_EDGE('',*,*,#12005,.T.);
#17470=ORIENTED_EDGE('',*,*,#12006,.T.);
#17471=ORIENTED_EDGE('',*,*,#12007,.T.);
#17472=ORIENTED_EDGE('',*,*,#12003,.F.);
#17473=ORIENTED_EDGE('',*,*,#12008,.T.);
#17474=ORIENTED_EDGE('',*,*,#12009,.T.);
#17475=ORIENTED_EDGE('',*,*,#12010,.T.);
#17476=ORIENTED_EDGE('',*,*,#12006,.F.);
#17477=ORIENTED_EDGE('',*,*,#12011,.T.);
#17478=ORIENTED_EDGE('',*,*,#12012,.T.);
#17479=ORIENTED_EDGE('',*,*,#12013,.T.);
#17480=ORIENTED_EDGE('',*,*,#12009,.F.);
#17481=ORIENTED_EDGE('',*,*,#12014,.T.);
#17482=ORIENTED_EDGE('',*,*,#12015,.T.);
#17483=ORIENTED_EDGE('',*,*,#12016,.T.);
#17484=ORIENTED_EDGE('',*,*,#12012,.F.);
#17485=ORIENTED_EDGE('',*,*,#12017,.T.);
#17486=ORIENTED_EDGE('',*,*,#12018,.T.);
#17487=ORIENTED_EDGE('',*,*,#12019,.T.);
#17488=ORIENTED_EDGE('',*,*,#12015,.F.);
#17489=ORIENTED_EDGE('',*,*,#12020,.T.);
#17490=ORIENTED_EDGE('',*,*,#12021,.T.);
#17491=ORIENTED_EDGE('',*,*,#12022,.T.);
#17492=ORIENTED_EDGE('',*,*,#12018,.F.);
#17493=ORIENTED_EDGE('',*,*,#12023,.T.);
#17494=ORIENTED_EDGE('',*,*,#12024,.F.);
#17495=ORIENTED_EDGE('',*,*,#12025,.T.);
#17496=ORIENTED_EDGE('',*,*,#12026,.F.);
#17497=ORIENTED_EDGE('',*,*,#12027,.T.);
#17498=ORIENTED_EDGE('',*,*,#12028,.T.);
#17499=ORIENTED_EDGE('',*,*,#12029,.T.);
#17500=ORIENTED_EDGE('',*,*,#12030,.F.);
#17501=ORIENTED_EDGE('',*,*,#12031,.T.);
#17502=ORIENTED_EDGE('',*,*,#12032,.T.);
#17503=ORIENTED_EDGE('',*,*,#12033,.T.);
#17504=ORIENTED_EDGE('',*,*,#12028,.F.);
#17505=ORIENTED_EDGE('',*,*,#12034,.T.);
#17506=ORIENTED_EDGE('',*,*,#12035,.T.);
#17507=ORIENTED_EDGE('',*,*,#12036,.T.);
#17508=ORIENTED_EDGE('',*,*,#12032,.F.);
#17509=ORIENTED_EDGE('',*,*,#12037,.T.);
#17510=ORIENTED_EDGE('',*,*,#12038,.T.);
#17511=ORIENTED_EDGE('',*,*,#12039,.T.);
#17512=ORIENTED_EDGE('',*,*,#12035,.F.);
#17513=ORIENTED_EDGE('',*,*,#12040,.T.);
#17514=ORIENTED_EDGE('',*,*,#12041,.T.);
#17515=ORIENTED_EDGE('',*,*,#12042,.T.);
#17516=ORIENTED_EDGE('',*,*,#12038,.F.);
#17517=ORIENTED_EDGE('',*,*,#12043,.T.);
#17518=ORIENTED_EDGE('',*,*,#12044,.T.);
#17519=ORIENTED_EDGE('',*,*,#12045,.T.);
#17520=ORIENTED_EDGE('',*,*,#12041,.F.);
#17521=ORIENTED_EDGE('',*,*,#12046,.T.);
#17522=ORIENTED_EDGE('',*,*,#12047,.T.);
#17523=ORIENTED_EDGE('',*,*,#12048,.T.);
#17524=ORIENTED_EDGE('',*,*,#12044,.F.);
#17525=ORIENTED_EDGE('',*,*,#12049,.T.);
#17526=ORIENTED_EDGE('',*,*,#12050,.T.);
#17527=ORIENTED_EDGE('',*,*,#12051,.T.);
#17528=ORIENTED_EDGE('',*,*,#12047,.F.);
#17529=ORIENTED_EDGE('',*,*,#12052,.T.);
#17530=ORIENTED_EDGE('',*,*,#12053,.T.);
#17531=ORIENTED_EDGE('',*,*,#12054,.T.);
#17532=ORIENTED_EDGE('',*,*,#12050,.F.);
#17533=ORIENTED_EDGE('',*,*,#12055,.T.);
#17534=ORIENTED_EDGE('',*,*,#12056,.T.);
#17535=ORIENTED_EDGE('',*,*,#12057,.T.);
#17536=ORIENTED_EDGE('',*,*,#12053,.F.);
#17537=ORIENTED_EDGE('',*,*,#12058,.T.);
#17538=ORIENTED_EDGE('',*,*,#12059,.T.);
#17539=ORIENTED_EDGE('',*,*,#12060,.T.);
#17540=ORIENTED_EDGE('',*,*,#12056,.F.);
#17541=ORIENTED_EDGE('',*,*,#12061,.T.);
#17542=ORIENTED_EDGE('',*,*,#12062,.T.);
#17543=ORIENTED_EDGE('',*,*,#12063,.T.);
#17544=ORIENTED_EDGE('',*,*,#12059,.F.);
#17545=ORIENTED_EDGE('',*,*,#12064,.T.);
#17546=ORIENTED_EDGE('',*,*,#12065,.T.);
#17547=ORIENTED_EDGE('',*,*,#12066,.T.);
#17548=ORIENTED_EDGE('',*,*,#12062,.F.);
#17549=ORIENTED_EDGE('',*,*,#12067,.T.);
#17550=ORIENTED_EDGE('',*,*,#12068,.T.);
#17551=ORIENTED_EDGE('',*,*,#12069,.T.);
#17552=ORIENTED_EDGE('',*,*,#12065,.F.);
#17553=ORIENTED_EDGE('',*,*,#12070,.T.);
#17554=ORIENTED_EDGE('',*,*,#12071,.T.);
#17555=ORIENTED_EDGE('',*,*,#12072,.T.);
#17556=ORIENTED_EDGE('',*,*,#12068,.F.);
#17557=ORIENTED_EDGE('',*,*,#12073,.T.);
#17558=ORIENTED_EDGE('',*,*,#12074,.T.);
#17559=ORIENTED_EDGE('',*,*,#12075,.T.);
#17560=ORIENTED_EDGE('',*,*,#12071,.F.);
#17561=ORIENTED_EDGE('',*,*,#12076,.T.);
#17562=ORIENTED_EDGE('',*,*,#12077,.T.);
#17563=ORIENTED_EDGE('',*,*,#12078,.T.);
#17564=ORIENTED_EDGE('',*,*,#12074,.F.);
#17565=ORIENTED_EDGE('',*,*,#12079,.T.);
#17566=ORIENTED_EDGE('',*,*,#12080,.T.);
#17567=ORIENTED_EDGE('',*,*,#12081,.T.);
#17568=ORIENTED_EDGE('',*,*,#12077,.F.);
#17569=ORIENTED_EDGE('',*,*,#12082,.T.);
#17570=ORIENTED_EDGE('',*,*,#12083,.T.);
#17571=ORIENTED_EDGE('',*,*,#12084,.T.);
#17572=ORIENTED_EDGE('',*,*,#12080,.F.);
#17573=ORIENTED_EDGE('',*,*,#12085,.T.);
#17574=ORIENTED_EDGE('',*,*,#12086,.F.);
#17575=ORIENTED_EDGE('',*,*,#12087,.T.);
#17576=ORIENTED_EDGE('',*,*,#12088,.F.);
#17577=ORIENTED_EDGE('',*,*,#12089,.T.);
#17578=ORIENTED_EDGE('',*,*,#12090,.T.);
#17579=ORIENTED_EDGE('',*,*,#12091,.T.);
#17580=ORIENTED_EDGE('',*,*,#12092,.F.);
#17581=ORIENTED_EDGE('',*,*,#12093,.T.);
#17582=ORIENTED_EDGE('',*,*,#12094,.T.);
#17583=ORIENTED_EDGE('',*,*,#12095,.T.);
#17584=ORIENTED_EDGE('',*,*,#12090,.F.);
#17585=ORIENTED_EDGE('',*,*,#12096,.T.);
#17586=ORIENTED_EDGE('',*,*,#12097,.T.);
#17587=ORIENTED_EDGE('',*,*,#12098,.T.);
#17588=ORIENTED_EDGE('',*,*,#12094,.F.);
#17589=ORIENTED_EDGE('',*,*,#12099,.T.);
#17590=ORIENTED_EDGE('',*,*,#12100,.T.);
#17591=ORIENTED_EDGE('',*,*,#12101,.T.);
#17592=ORIENTED_EDGE('',*,*,#12097,.F.);
#17593=ORIENTED_EDGE('',*,*,#12102,.T.);
#17594=ORIENTED_EDGE('',*,*,#12103,.T.);
#17595=ORIENTED_EDGE('',*,*,#12104,.T.);
#17596=ORIENTED_EDGE('',*,*,#12100,.F.);
#17597=ORIENTED_EDGE('',*,*,#12105,.T.);
#17598=ORIENTED_EDGE('',*,*,#12106,.T.);
#17599=ORIENTED_EDGE('',*,*,#12107,.T.);
#17600=ORIENTED_EDGE('',*,*,#12103,.F.);
#17601=ORIENTED_EDGE('',*,*,#12108,.T.);
#17602=ORIENTED_EDGE('',*,*,#12109,.T.);
#17603=ORIENTED_EDGE('',*,*,#12110,.T.);
#17604=ORIENTED_EDGE('',*,*,#12106,.F.);
#17605=ORIENTED_EDGE('',*,*,#12111,.T.);
#17606=ORIENTED_EDGE('',*,*,#12112,.T.);
#17607=ORIENTED_EDGE('',*,*,#12113,.T.);
#17608=ORIENTED_EDGE('',*,*,#12109,.F.);
#17609=ORIENTED_EDGE('',*,*,#12114,.T.);
#17610=ORIENTED_EDGE('',*,*,#12115,.T.);
#17611=ORIENTED_EDGE('',*,*,#12116,.T.);
#17612=ORIENTED_EDGE('',*,*,#12112,.F.);
#17613=ORIENTED_EDGE('',*,*,#12117,.T.);
#17614=ORIENTED_EDGE('',*,*,#12118,.T.);
#17615=ORIENTED_EDGE('',*,*,#12119,.T.);
#17616=ORIENTED_EDGE('',*,*,#12115,.F.);
#17617=ORIENTED_EDGE('',*,*,#12120,.T.);
#17618=ORIENTED_EDGE('',*,*,#12121,.T.);
#17619=ORIENTED_EDGE('',*,*,#12122,.T.);
#17620=ORIENTED_EDGE('',*,*,#12118,.F.);
#17621=ORIENTED_EDGE('',*,*,#12123,.T.);
#17622=ORIENTED_EDGE('',*,*,#12124,.T.);
#17623=ORIENTED_EDGE('',*,*,#12125,.T.);
#17624=ORIENTED_EDGE('',*,*,#12121,.F.);
#17625=ORIENTED_EDGE('',*,*,#12126,.T.);
#17626=ORIENTED_EDGE('',*,*,#12127,.T.);
#17627=ORIENTED_EDGE('',*,*,#12128,.T.);
#17628=ORIENTED_EDGE('',*,*,#12124,.F.);
#17629=ORIENTED_EDGE('',*,*,#12129,.T.);
#17630=ORIENTED_EDGE('',*,*,#12130,.T.);
#17631=ORIENTED_EDGE('',*,*,#12131,.T.);
#17632=ORIENTED_EDGE('',*,*,#12127,.F.);
#17633=ORIENTED_EDGE('',*,*,#12132,.T.);
#17634=ORIENTED_EDGE('',*,*,#12133,.T.);
#17635=ORIENTED_EDGE('',*,*,#12134,.T.);
#17636=ORIENTED_EDGE('',*,*,#12130,.F.);
#17637=ORIENTED_EDGE('',*,*,#12135,.T.);
#17638=ORIENTED_EDGE('',*,*,#12136,.T.);
#17639=ORIENTED_EDGE('',*,*,#12137,.T.);
#17640=ORIENTED_EDGE('',*,*,#12133,.F.);
#17641=ORIENTED_EDGE('',*,*,#12138,.T.);
#17642=ORIENTED_EDGE('',*,*,#12139,.T.);
#17643=ORIENTED_EDGE('',*,*,#12140,.T.);
#17644=ORIENTED_EDGE('',*,*,#12136,.F.);
#17645=ORIENTED_EDGE('',*,*,#12141,.T.);
#17646=ORIENTED_EDGE('',*,*,#12142,.T.);
#17647=ORIENTED_EDGE('',*,*,#12143,.T.);
#17648=ORIENTED_EDGE('',*,*,#12139,.F.);
#17649=ORIENTED_EDGE('',*,*,#12144,.T.);
#17650=ORIENTED_EDGE('',*,*,#12145,.T.);
#17651=ORIENTED_EDGE('',*,*,#12146,.T.);
#17652=ORIENTED_EDGE('',*,*,#12142,.F.);
#17653=ORIENTED_EDGE('',*,*,#12147,.T.);
#17654=ORIENTED_EDGE('',*,*,#12148,.F.);
#17655=ORIENTED_EDGE('',*,*,#12149,.T.);
#17656=ORIENTED_EDGE('',*,*,#12150,.F.);
#17657=ORIENTED_EDGE('',*,*,#12151,.T.);
#17658=ORIENTED_EDGE('',*,*,#12152,.T.);
#17659=ORIENTED_EDGE('',*,*,#12153,.T.);
#17660=ORIENTED_EDGE('',*,*,#12154,.F.);
#17661=ORIENTED_EDGE('',*,*,#12155,.T.);
#17662=ORIENTED_EDGE('',*,*,#12156,.T.);
#17663=ORIENTED_EDGE('',*,*,#12157,.T.);
#17664=ORIENTED_EDGE('',*,*,#12152,.F.);
#17665=ORIENTED_EDGE('',*,*,#12158,.T.);
#17666=ORIENTED_EDGE('',*,*,#12159,.T.);
#17667=ORIENTED_EDGE('',*,*,#12160,.T.);
#17668=ORIENTED_EDGE('',*,*,#12156,.F.);
#17669=ORIENTED_EDGE('',*,*,#12161,.T.);
#17670=ORIENTED_EDGE('',*,*,#12162,.T.);
#17671=ORIENTED_EDGE('',*,*,#12163,.T.);
#17672=ORIENTED_EDGE('',*,*,#12159,.F.);
#17673=ORIENTED_EDGE('',*,*,#12164,.T.);
#17674=ORIENTED_EDGE('',*,*,#12165,.T.);
#17675=ORIENTED_EDGE('',*,*,#12166,.T.);
#17676=ORIENTED_EDGE('',*,*,#12162,.F.);
#17677=ORIENTED_EDGE('',*,*,#12167,.T.);
#17678=ORIENTED_EDGE('',*,*,#12168,.T.);
#17679=ORIENTED_EDGE('',*,*,#12169,.T.);
#17680=ORIENTED_EDGE('',*,*,#12165,.F.);
#17681=ORIENTED_EDGE('',*,*,#12170,.T.);
#17682=ORIENTED_EDGE('',*,*,#12171,.T.);
#17683=ORIENTED_EDGE('',*,*,#12172,.T.);
#17684=ORIENTED_EDGE('',*,*,#12168,.F.);
#17685=ORIENTED_EDGE('',*,*,#12173,.T.);
#17686=ORIENTED_EDGE('',*,*,#12174,.T.);
#17687=ORIENTED_EDGE('',*,*,#12175,.T.);
#17688=ORIENTED_EDGE('',*,*,#12171,.F.);
#17689=ORIENTED_EDGE('',*,*,#12176,.T.);
#17690=ORIENTED_EDGE('',*,*,#12177,.T.);
#17691=ORIENTED_EDGE('',*,*,#12178,.T.);
#17692=ORIENTED_EDGE('',*,*,#12174,.F.);
#17693=ORIENTED_EDGE('',*,*,#12179,.T.);
#17694=ORIENTED_EDGE('',*,*,#12180,.T.);
#17695=ORIENTED_EDGE('',*,*,#12181,.T.);
#17696=ORIENTED_EDGE('',*,*,#12177,.F.);
#17697=ORIENTED_EDGE('',*,*,#12182,.T.);
#17698=ORIENTED_EDGE('',*,*,#12183,.T.);
#17699=ORIENTED_EDGE('',*,*,#12184,.T.);
#17700=ORIENTED_EDGE('',*,*,#12180,.F.);
#17701=ORIENTED_EDGE('',*,*,#12185,.T.);
#17702=ORIENTED_EDGE('',*,*,#12186,.T.);
#17703=ORIENTED_EDGE('',*,*,#12187,.T.);
#17704=ORIENTED_EDGE('',*,*,#12183,.F.);
#17705=ORIENTED_EDGE('',*,*,#12188,.T.);
#17706=ORIENTED_EDGE('',*,*,#12189,.T.);
#17707=ORIENTED_EDGE('',*,*,#12190,.T.);
#17708=ORIENTED_EDGE('',*,*,#12186,.F.);
#17709=ORIENTED_EDGE('',*,*,#12191,.T.);
#17710=ORIENTED_EDGE('',*,*,#12192,.T.);
#17711=ORIENTED_EDGE('',*,*,#12193,.T.);
#17712=ORIENTED_EDGE('',*,*,#12189,.F.);
#17713=ORIENTED_EDGE('',*,*,#12194,.T.);
#17714=ORIENTED_EDGE('',*,*,#12195,.T.);
#17715=ORIENTED_EDGE('',*,*,#12196,.T.);
#17716=ORIENTED_EDGE('',*,*,#12192,.F.);
#17717=ORIENTED_EDGE('',*,*,#12197,.T.);
#17718=ORIENTED_EDGE('',*,*,#12198,.T.);
#17719=ORIENTED_EDGE('',*,*,#12199,.T.);
#17720=ORIENTED_EDGE('',*,*,#12195,.F.);
#17721=ORIENTED_EDGE('',*,*,#12200,.T.);
#17722=ORIENTED_EDGE('',*,*,#12201,.T.);
#17723=ORIENTED_EDGE('',*,*,#12202,.T.);
#17724=ORIENTED_EDGE('',*,*,#12198,.F.);
#17725=ORIENTED_EDGE('',*,*,#12203,.T.);
#17726=ORIENTED_EDGE('',*,*,#12204,.T.);
#17727=ORIENTED_EDGE('',*,*,#12205,.T.);
#17728=ORIENTED_EDGE('',*,*,#12201,.F.);
#17729=ORIENTED_EDGE('',*,*,#12206,.T.);
#17730=ORIENTED_EDGE('',*,*,#12207,.T.);
#17731=ORIENTED_EDGE('',*,*,#12208,.T.);
#17732=ORIENTED_EDGE('',*,*,#12204,.F.);
#17733=ORIENTED_EDGE('',*,*,#12209,.T.);
#17734=ORIENTED_EDGE('',*,*,#12210,.F.);
#17735=ORIENTED_EDGE('',*,*,#12211,.T.);
#17736=ORIENTED_EDGE('',*,*,#12212,.F.);
#17737=ORIENTED_EDGE('',*,*,#12213,.T.);
#17738=ORIENTED_EDGE('',*,*,#12214,.T.);
#17739=ORIENTED_EDGE('',*,*,#12215,.T.);
#17740=ORIENTED_EDGE('',*,*,#12216,.F.);
#17741=ORIENTED_EDGE('',*,*,#12217,.T.);
#17742=ORIENTED_EDGE('',*,*,#12218,.T.);
#17743=ORIENTED_EDGE('',*,*,#12219,.T.);
#17744=ORIENTED_EDGE('',*,*,#12214,.F.);
#17745=ORIENTED_EDGE('',*,*,#12220,.T.);
#17746=ORIENTED_EDGE('',*,*,#12221,.T.);
#17747=ORIENTED_EDGE('',*,*,#12222,.T.);
#17748=ORIENTED_EDGE('',*,*,#12218,.F.);
#17749=ORIENTED_EDGE('',*,*,#12223,.T.);
#17750=ORIENTED_EDGE('',*,*,#12224,.T.);
#17751=ORIENTED_EDGE('',*,*,#12225,.T.);
#17752=ORIENTED_EDGE('',*,*,#12221,.F.);
#17753=ORIENTED_EDGE('',*,*,#12226,.T.);
#17754=ORIENTED_EDGE('',*,*,#12227,.T.);
#17755=ORIENTED_EDGE('',*,*,#12228,.T.);
#17756=ORIENTED_EDGE('',*,*,#12224,.F.);
#17757=ORIENTED_EDGE('',*,*,#12229,.T.);
#17758=ORIENTED_EDGE('',*,*,#12230,.T.);
#17759=ORIENTED_EDGE('',*,*,#12231,.T.);
#17760=ORIENTED_EDGE('',*,*,#12227,.F.);
#17761=ORIENTED_EDGE('',*,*,#12232,.T.);
#17762=ORIENTED_EDGE('',*,*,#12233,.T.);
#17763=ORIENTED_EDGE('',*,*,#12234,.T.);
#17764=ORIENTED_EDGE('',*,*,#12230,.F.);
#17765=ORIENTED_EDGE('',*,*,#12235,.T.);
#17766=ORIENTED_EDGE('',*,*,#12236,.T.);
#17767=ORIENTED_EDGE('',*,*,#12237,.T.);
#17768=ORIENTED_EDGE('',*,*,#12233,.F.);
#17769=ORIENTED_EDGE('',*,*,#12238,.T.);
#17770=ORIENTED_EDGE('',*,*,#12239,.T.);
#17771=ORIENTED_EDGE('',*,*,#12240,.T.);
#17772=ORIENTED_EDGE('',*,*,#12236,.F.);
#17773=ORIENTED_EDGE('',*,*,#12241,.T.);
#17774=ORIENTED_EDGE('',*,*,#12242,.T.);
#17775=ORIENTED_EDGE('',*,*,#12243,.T.);
#17776=ORIENTED_EDGE('',*,*,#12239,.F.);
#17777=ORIENTED_EDGE('',*,*,#12244,.T.);
#17778=ORIENTED_EDGE('',*,*,#12245,.T.);
#17779=ORIENTED_EDGE('',*,*,#12246,.T.);
#17780=ORIENTED_EDGE('',*,*,#12242,.F.);
#17781=ORIENTED_EDGE('',*,*,#12247,.T.);
#17782=ORIENTED_EDGE('',*,*,#12248,.T.);
#17783=ORIENTED_EDGE('',*,*,#12249,.T.);
#17784=ORIENTED_EDGE('',*,*,#12245,.F.);
#17785=ORIENTED_EDGE('',*,*,#12250,.T.);
#17786=ORIENTED_EDGE('',*,*,#12251,.T.);
#17787=ORIENTED_EDGE('',*,*,#12252,.T.);
#17788=ORIENTED_EDGE('',*,*,#12248,.F.);
#17789=ORIENTED_EDGE('',*,*,#12253,.T.);
#17790=ORIENTED_EDGE('',*,*,#12254,.T.);
#17791=ORIENTED_EDGE('',*,*,#12255,.T.);
#17792=ORIENTED_EDGE('',*,*,#12251,.F.);
#17793=ORIENTED_EDGE('',*,*,#12256,.T.);
#17794=ORIENTED_EDGE('',*,*,#12257,.T.);
#17795=ORIENTED_EDGE('',*,*,#12258,.T.);
#17796=ORIENTED_EDGE('',*,*,#12254,.F.);
#17797=ORIENTED_EDGE('',*,*,#12259,.T.);
#17798=ORIENTED_EDGE('',*,*,#12260,.T.);
#17799=ORIENTED_EDGE('',*,*,#12261,.T.);
#17800=ORIENTED_EDGE('',*,*,#12257,.F.);
#17801=ORIENTED_EDGE('',*,*,#12262,.T.);
#17802=ORIENTED_EDGE('',*,*,#12263,.T.);
#17803=ORIENTED_EDGE('',*,*,#12264,.T.);
#17804=ORIENTED_EDGE('',*,*,#12260,.F.);
#17805=ORIENTED_EDGE('',*,*,#12265,.T.);
#17806=ORIENTED_EDGE('',*,*,#12266,.T.);
#17807=ORIENTED_EDGE('',*,*,#12267,.T.);
#17808=ORIENTED_EDGE('',*,*,#12263,.F.);
#17809=ORIENTED_EDGE('',*,*,#12268,.T.);
#17810=ORIENTED_EDGE('',*,*,#12269,.T.);
#17811=ORIENTED_EDGE('',*,*,#12270,.T.);
#17812=ORIENTED_EDGE('',*,*,#12266,.F.);
#17813=ORIENTED_EDGE('',*,*,#12271,.T.);
#17814=ORIENTED_EDGE('',*,*,#12272,.F.);
#17815=ORIENTED_EDGE('',*,*,#12273,.T.);
#17816=ORIENTED_EDGE('',*,*,#12274,.F.);
#17817=ORIENTED_EDGE('',*,*,#12275,.T.);
#17818=ORIENTED_EDGE('',*,*,#12276,.T.);
#17819=ORIENTED_EDGE('',*,*,#12277,.T.);
#17820=ORIENTED_EDGE('',*,*,#12278,.F.);
#17821=ORIENTED_EDGE('',*,*,#12279,.T.);
#17822=ORIENTED_EDGE('',*,*,#12280,.T.);
#17823=ORIENTED_EDGE('',*,*,#12281,.T.);
#17824=ORIENTED_EDGE('',*,*,#12276,.F.);
#17825=ORIENTED_EDGE('',*,*,#12282,.T.);
#17826=ORIENTED_EDGE('',*,*,#12283,.T.);
#17827=ORIENTED_EDGE('',*,*,#12284,.T.);
#17828=ORIENTED_EDGE('',*,*,#12280,.F.);
#17829=ORIENTED_EDGE('',*,*,#12285,.T.);
#17830=ORIENTED_EDGE('',*,*,#12286,.T.);
#17831=ORIENTED_EDGE('',*,*,#12287,.T.);
#17832=ORIENTED_EDGE('',*,*,#12283,.F.);
#17833=ORIENTED_EDGE('',*,*,#12288,.T.);
#17834=ORIENTED_EDGE('',*,*,#12289,.T.);
#17835=ORIENTED_EDGE('',*,*,#12290,.T.);
#17836=ORIENTED_EDGE('',*,*,#12286,.F.);
#17837=ORIENTED_EDGE('',*,*,#12291,.T.);
#17838=ORIENTED_EDGE('',*,*,#12292,.T.);
#17839=ORIENTED_EDGE('',*,*,#12293,.T.);
#17840=ORIENTED_EDGE('',*,*,#12289,.F.);
#17841=ORIENTED_EDGE('',*,*,#12294,.T.);
#17842=ORIENTED_EDGE('',*,*,#12295,.T.);
#17843=ORIENTED_EDGE('',*,*,#12296,.T.);
#17844=ORIENTED_EDGE('',*,*,#12292,.F.);
#17845=ORIENTED_EDGE('',*,*,#12297,.T.);
#17846=ORIENTED_EDGE('',*,*,#12298,.T.);
#17847=ORIENTED_EDGE('',*,*,#12299,.T.);
#17848=ORIENTED_EDGE('',*,*,#12295,.F.);
#17849=ORIENTED_EDGE('',*,*,#12300,.T.);
#17850=ORIENTED_EDGE('',*,*,#12301,.T.);
#17851=ORIENTED_EDGE('',*,*,#12302,.T.);
#17852=ORIENTED_EDGE('',*,*,#12298,.F.);
#17853=ORIENTED_EDGE('',*,*,#12303,.T.);
#17854=ORIENTED_EDGE('',*,*,#12304,.T.);
#17855=ORIENTED_EDGE('',*,*,#12305,.T.);
#17856=ORIENTED_EDGE('',*,*,#12301,.F.);
#17857=ORIENTED_EDGE('',*,*,#12306,.T.);
#17858=ORIENTED_EDGE('',*,*,#12307,.T.);
#17859=ORIENTED_EDGE('',*,*,#12308,.T.);
#17860=ORIENTED_EDGE('',*,*,#12304,.F.);
#17861=ORIENTED_EDGE('',*,*,#12309,.T.);
#17862=ORIENTED_EDGE('',*,*,#12310,.T.);
#17863=ORIENTED_EDGE('',*,*,#12311,.T.);
#17864=ORIENTED_EDGE('',*,*,#12307,.F.);
#17865=ORIENTED_EDGE('',*,*,#12312,.T.);
#17866=ORIENTED_EDGE('',*,*,#12313,.T.);
#17867=ORIENTED_EDGE('',*,*,#12314,.T.);
#17868=ORIENTED_EDGE('',*,*,#12310,.F.);
#17869=ORIENTED_EDGE('',*,*,#12315,.T.);
#17870=ORIENTED_EDGE('',*,*,#12316,.T.);
#17871=ORIENTED_EDGE('',*,*,#12317,.T.);
#17872=ORIENTED_EDGE('',*,*,#12313,.F.);
#17873=ORIENTED_EDGE('',*,*,#12318,.T.);
#17874=ORIENTED_EDGE('',*,*,#12319,.T.);
#17875=ORIENTED_EDGE('',*,*,#12320,.T.);
#17876=ORIENTED_EDGE('',*,*,#12316,.F.);
#17877=ORIENTED_EDGE('',*,*,#12321,.T.);
#17878=ORIENTED_EDGE('',*,*,#12322,.T.);
#17879=ORIENTED_EDGE('',*,*,#12323,.T.);
#17880=ORIENTED_EDGE('',*,*,#12319,.F.);
#17881=ORIENTED_EDGE('',*,*,#12324,.T.);
#17882=ORIENTED_EDGE('',*,*,#12325,.T.);
#17883=ORIENTED_EDGE('',*,*,#12326,.T.);
#17884=ORIENTED_EDGE('',*,*,#12322,.F.);
#17885=ORIENTED_EDGE('',*,*,#12327,.T.);
#17886=ORIENTED_EDGE('',*,*,#12328,.T.);
#17887=ORIENTED_EDGE('',*,*,#12329,.T.);
#17888=ORIENTED_EDGE('',*,*,#12325,.F.);
#17889=ORIENTED_EDGE('',*,*,#12330,.T.);
#17890=ORIENTED_EDGE('',*,*,#12331,.T.);
#17891=ORIENTED_EDGE('',*,*,#12332,.T.);
#17892=ORIENTED_EDGE('',*,*,#12328,.F.);
#17893=ORIENTED_EDGE('',*,*,#12333,.T.);
#17894=ORIENTED_EDGE('',*,*,#12334,.F.);
#17895=ORIENTED_EDGE('',*,*,#12335,.T.);
#17896=ORIENTED_EDGE('',*,*,#12336,.F.);
#17897=ORIENTED_EDGE('',*,*,#12337,.T.);
#17898=ORIENTED_EDGE('',*,*,#12338,.T.);
#17899=ORIENTED_EDGE('',*,*,#12339,.T.);
#17900=ORIENTED_EDGE('',*,*,#12340,.F.);
#17901=ORIENTED_EDGE('',*,*,#12341,.F.);
#17902=ORIENTED_EDGE('',*,*,#12342,.T.);
#17903=ORIENTED_EDGE('',*,*,#12343,.T.);
#17904=ORIENTED_EDGE('',*,*,#12338,.F.);
#17905=ORIENTED_EDGE('',*,*,#12344,.F.);
#17906=ORIENTED_EDGE('',*,*,#12345,.T.);
#17907=ORIENTED_EDGE('',*,*,#12346,.T.);
#17908=ORIENTED_EDGE('',*,*,#12342,.F.);
#17909=ORIENTED_EDGE('',*,*,#12347,.F.);
#17910=ORIENTED_EDGE('',*,*,#12348,.T.);
#17911=ORIENTED_EDGE('',*,*,#12349,.T.);
#17912=ORIENTED_EDGE('',*,*,#12345,.F.);
#17913=ORIENTED_EDGE('',*,*,#12350,.F.);
#17914=ORIENTED_EDGE('',*,*,#12351,.T.);
#17915=ORIENTED_EDGE('',*,*,#12352,.T.);
#17916=ORIENTED_EDGE('',*,*,#12348,.F.);
#17917=ORIENTED_EDGE('',*,*,#12353,.F.);
#17918=ORIENTED_EDGE('',*,*,#12354,.T.);
#17919=ORIENTED_EDGE('',*,*,#12355,.T.);
#17920=ORIENTED_EDGE('',*,*,#12351,.F.);
#17921=ORIENTED_EDGE('',*,*,#12356,.F.);
#17922=ORIENTED_EDGE('',*,*,#12357,.T.);
#17923=ORIENTED_EDGE('',*,*,#12358,.T.);
#17924=ORIENTED_EDGE('',*,*,#12354,.F.);
#17925=ORIENTED_EDGE('',*,*,#12359,.F.);
#17926=ORIENTED_EDGE('',*,*,#12360,.T.);
#17927=ORIENTED_EDGE('',*,*,#12361,.T.);
#17928=ORIENTED_EDGE('',*,*,#12357,.F.);
#17929=ORIENTED_EDGE('',*,*,#12362,.F.);
#17930=ORIENTED_EDGE('',*,*,#12363,.T.);
#17931=ORIENTED_EDGE('',*,*,#12364,.T.);
#17932=ORIENTED_EDGE('',*,*,#12360,.F.);
#17933=ORIENTED_EDGE('',*,*,#12365,.F.);
#17934=ORIENTED_EDGE('',*,*,#12366,.T.);
#17935=ORIENTED_EDGE('',*,*,#12367,.T.);
#17936=ORIENTED_EDGE('',*,*,#12363,.F.);
#17937=ORIENTED_EDGE('',*,*,#12368,.F.);
#17938=ORIENTED_EDGE('',*,*,#12369,.T.);
#17939=ORIENTED_EDGE('',*,*,#12370,.T.);
#17940=ORIENTED_EDGE('',*,*,#12366,.F.);
#17941=ORIENTED_EDGE('',*,*,#12371,.F.);
#17942=ORIENTED_EDGE('',*,*,#12372,.T.);
#17943=ORIENTED_EDGE('',*,*,#12373,.T.);
#17944=ORIENTED_EDGE('',*,*,#12369,.F.);
#17945=ORIENTED_EDGE('',*,*,#12374,.F.);
#17946=ORIENTED_EDGE('',*,*,#12375,.T.);
#17947=ORIENTED_EDGE('',*,*,#12376,.T.);
#17948=ORIENTED_EDGE('',*,*,#12372,.F.);
#17949=ORIENTED_EDGE('',*,*,#12377,.F.);
#17950=ORIENTED_EDGE('',*,*,#12378,.T.);
#17951=ORIENTED_EDGE('',*,*,#12379,.T.);
#17952=ORIENTED_EDGE('',*,*,#12375,.F.);
#17953=ORIENTED_EDGE('',*,*,#12380,.F.);
#17954=ORIENTED_EDGE('',*,*,#12381,.T.);
#17955=ORIENTED_EDGE('',*,*,#12382,.T.);
#17956=ORIENTED_EDGE('',*,*,#12378,.F.);
#17957=ORIENTED_EDGE('',*,*,#12383,.F.);
#17958=ORIENTED_EDGE('',*,*,#12384,.T.);
#17959=ORIENTED_EDGE('',*,*,#12385,.T.);
#17960=ORIENTED_EDGE('',*,*,#12381,.F.);
#17961=ORIENTED_EDGE('',*,*,#12386,.F.);
#17962=ORIENTED_EDGE('',*,*,#12387,.T.);
#17963=ORIENTED_EDGE('',*,*,#12388,.T.);
#17964=ORIENTED_EDGE('',*,*,#12384,.F.);
#17965=ORIENTED_EDGE('',*,*,#12389,.F.);
#17966=ORIENTED_EDGE('',*,*,#12390,.T.);
#17967=ORIENTED_EDGE('',*,*,#12391,.T.);
#17968=ORIENTED_EDGE('',*,*,#12387,.F.);
#17969=ORIENTED_EDGE('',*,*,#12392,.F.);
#17970=ORIENTED_EDGE('',*,*,#12393,.T.);
#17971=ORIENTED_EDGE('',*,*,#12394,.T.);
#17972=ORIENTED_EDGE('',*,*,#12390,.F.);
#17973=ORIENTED_EDGE('',*,*,#12395,.F.);
#17974=ORIENTED_EDGE('',*,*,#12396,.F.);
#17975=ORIENTED_EDGE('',*,*,#12397,.F.);
#17976=ORIENTED_EDGE('',*,*,#12398,.F.);
#17977=ORIENTED_EDGE('',*,*,#12399,.T.);
#17978=ORIENTED_EDGE('',*,*,#12400,.T.);
#17979=ORIENTED_EDGE('',*,*,#12401,.T.);
#17980=ORIENTED_EDGE('',*,*,#12402,.F.);
#17981=ORIENTED_EDGE('',*,*,#12403,.F.);
#17982=ORIENTED_EDGE('',*,*,#12404,.T.);
#17983=ORIENTED_EDGE('',*,*,#12405,.T.);
#17984=ORIENTED_EDGE('',*,*,#12400,.F.);
#17985=ORIENTED_EDGE('',*,*,#12406,.F.);
#17986=ORIENTED_EDGE('',*,*,#12407,.T.);
#17987=ORIENTED_EDGE('',*,*,#12408,.T.);
#17988=ORIENTED_EDGE('',*,*,#12404,.F.);
#17989=ORIENTED_EDGE('',*,*,#12409,.F.);
#17990=ORIENTED_EDGE('',*,*,#12410,.T.);
#17991=ORIENTED_EDGE('',*,*,#12411,.T.);
#17992=ORIENTED_EDGE('',*,*,#12407,.F.);
#17993=ORIENTED_EDGE('',*,*,#12412,.F.);
#17994=ORIENTED_EDGE('',*,*,#12413,.T.);
#17995=ORIENTED_EDGE('',*,*,#12414,.T.);
#17996=ORIENTED_EDGE('',*,*,#12410,.F.);
#17997=ORIENTED_EDGE('',*,*,#12415,.F.);
#17998=ORIENTED_EDGE('',*,*,#12416,.T.);
#17999=ORIENTED_EDGE('',*,*,#12417,.T.);
#18000=ORIENTED_EDGE('',*,*,#12413,.F.);
#18001=ORIENTED_EDGE('',*,*,#12418,.F.);
#18002=ORIENTED_EDGE('',*,*,#12419,.T.);
#18003=ORIENTED_EDGE('',*,*,#12420,.T.);
#18004=ORIENTED_EDGE('',*,*,#12416,.F.);
#18005=ORIENTED_EDGE('',*,*,#12421,.F.);
#18006=ORIENTED_EDGE('',*,*,#12422,.T.);
#18007=ORIENTED_EDGE('',*,*,#12423,.T.);
#18008=ORIENTED_EDGE('',*,*,#12419,.F.);
#18009=ORIENTED_EDGE('',*,*,#12424,.F.);
#18010=ORIENTED_EDGE('',*,*,#12425,.T.);
#18011=ORIENTED_EDGE('',*,*,#12426,.T.);
#18012=ORIENTED_EDGE('',*,*,#12422,.F.);
#18013=ORIENTED_EDGE('',*,*,#12427,.F.);
#18014=ORIENTED_EDGE('',*,*,#12428,.T.);
#18015=ORIENTED_EDGE('',*,*,#12429,.T.);
#18016=ORIENTED_EDGE('',*,*,#12425,.F.);
#18017=ORIENTED_EDGE('',*,*,#12430,.F.);
#18018=ORIENTED_EDGE('',*,*,#12431,.T.);
#18019=ORIENTED_EDGE('',*,*,#12432,.T.);
#18020=ORIENTED_EDGE('',*,*,#12428,.F.);
#18021=ORIENTED_EDGE('',*,*,#12433,.F.);
#18022=ORIENTED_EDGE('',*,*,#12434,.T.);
#18023=ORIENTED_EDGE('',*,*,#12435,.T.);
#18024=ORIENTED_EDGE('',*,*,#12431,.F.);
#18025=ORIENTED_EDGE('',*,*,#12436,.F.);
#18026=ORIENTED_EDGE('',*,*,#12437,.T.);
#18027=ORIENTED_EDGE('',*,*,#12438,.T.);
#18028=ORIENTED_EDGE('',*,*,#12434,.F.);
#18029=ORIENTED_EDGE('',*,*,#12439,.F.);
#18030=ORIENTED_EDGE('',*,*,#12440,.T.);
#18031=ORIENTED_EDGE('',*,*,#12441,.T.);
#18032=ORIENTED_EDGE('',*,*,#12437,.F.);
#18033=ORIENTED_EDGE('',*,*,#12442,.F.);
#18034=ORIENTED_EDGE('',*,*,#12443,.T.);
#18035=ORIENTED_EDGE('',*,*,#12444,.T.);
#18036=ORIENTED_EDGE('',*,*,#12440,.F.);
#18037=ORIENTED_EDGE('',*,*,#12445,.F.);
#18038=ORIENTED_EDGE('',*,*,#12446,.T.);
#18039=ORIENTED_EDGE('',*,*,#12447,.T.);
#18040=ORIENTED_EDGE('',*,*,#12443,.F.);
#18041=ORIENTED_EDGE('',*,*,#12448,.F.);
#18042=ORIENTED_EDGE('',*,*,#12449,.T.);
#18043=ORIENTED_EDGE('',*,*,#12450,.T.);
#18044=ORIENTED_EDGE('',*,*,#12446,.F.);
#18045=ORIENTED_EDGE('',*,*,#12451,.F.);
#18046=ORIENTED_EDGE('',*,*,#12452,.T.);
#18047=ORIENTED_EDGE('',*,*,#12453,.T.);
#18048=ORIENTED_EDGE('',*,*,#12449,.F.);
#18049=ORIENTED_EDGE('',*,*,#12454,.F.);
#18050=ORIENTED_EDGE('',*,*,#12455,.T.);
#18051=ORIENTED_EDGE('',*,*,#12456,.T.);
#18052=ORIENTED_EDGE('',*,*,#12452,.F.);
#18053=ORIENTED_EDGE('',*,*,#12457,.F.);
#18054=ORIENTED_EDGE('',*,*,#12458,.F.);
#18055=ORIENTED_EDGE('',*,*,#12459,.F.);
#18056=ORIENTED_EDGE('',*,*,#12460,.F.);
#18057=ORIENTED_EDGE('',*,*,#12461,.T.);
#18058=ORIENTED_EDGE('',*,*,#12462,.T.);
#18059=ORIENTED_EDGE('',*,*,#12463,.T.);
#18060=ORIENTED_EDGE('',*,*,#12464,.F.);
#18061=ORIENTED_EDGE('',*,*,#12465,.F.);
#18062=ORIENTED_EDGE('',*,*,#12466,.T.);
#18063=ORIENTED_EDGE('',*,*,#12467,.T.);
#18064=ORIENTED_EDGE('',*,*,#12462,.F.);
#18065=ORIENTED_EDGE('',*,*,#12468,.F.);
#18066=ORIENTED_EDGE('',*,*,#12469,.T.);
#18067=ORIENTED_EDGE('',*,*,#12470,.T.);
#18068=ORIENTED_EDGE('',*,*,#12466,.F.);
#18069=ORIENTED_EDGE('',*,*,#12471,.F.);
#18070=ORIENTED_EDGE('',*,*,#12472,.T.);
#18071=ORIENTED_EDGE('',*,*,#12473,.T.);
#18072=ORIENTED_EDGE('',*,*,#12469,.F.);
#18073=ORIENTED_EDGE('',*,*,#12474,.F.);
#18074=ORIENTED_EDGE('',*,*,#12475,.T.);
#18075=ORIENTED_EDGE('',*,*,#12476,.T.);
#18076=ORIENTED_EDGE('',*,*,#12472,.F.);
#18077=ORIENTED_EDGE('',*,*,#12477,.F.);
#18078=ORIENTED_EDGE('',*,*,#12478,.T.);
#18079=ORIENTED_EDGE('',*,*,#12479,.T.);
#18080=ORIENTED_EDGE('',*,*,#12475,.F.);
#18081=ORIENTED_EDGE('',*,*,#12480,.F.);
#18082=ORIENTED_EDGE('',*,*,#12481,.T.);
#18083=ORIENTED_EDGE('',*,*,#12482,.T.);
#18084=ORIENTED_EDGE('',*,*,#12478,.F.);
#18085=ORIENTED_EDGE('',*,*,#12483,.F.);
#18086=ORIENTED_EDGE('',*,*,#12484,.T.);
#18087=ORIENTED_EDGE('',*,*,#12485,.T.);
#18088=ORIENTED_EDGE('',*,*,#12481,.F.);
#18089=ORIENTED_EDGE('',*,*,#12486,.F.);
#18090=ORIENTED_EDGE('',*,*,#12487,.T.);
#18091=ORIENTED_EDGE('',*,*,#12488,.T.);
#18092=ORIENTED_EDGE('',*,*,#12484,.F.);
#18093=ORIENTED_EDGE('',*,*,#12489,.F.);
#18094=ORIENTED_EDGE('',*,*,#12490,.T.);
#18095=ORIENTED_EDGE('',*,*,#12491,.T.);
#18096=ORIENTED_EDGE('',*,*,#12487,.F.);
#18097=ORIENTED_EDGE('',*,*,#12492,.F.);
#18098=ORIENTED_EDGE('',*,*,#12493,.T.);
#18099=ORIENTED_EDGE('',*,*,#12494,.T.);
#18100=ORIENTED_EDGE('',*,*,#12490,.F.);
#18101=ORIENTED_EDGE('',*,*,#12495,.F.);
#18102=ORIENTED_EDGE('',*,*,#12496,.T.);
#18103=ORIENTED_EDGE('',*,*,#12497,.T.);
#18104=ORIENTED_EDGE('',*,*,#12493,.F.);
#18105=ORIENTED_EDGE('',*,*,#12498,.F.);
#18106=ORIENTED_EDGE('',*,*,#12499,.T.);
#18107=ORIENTED_EDGE('',*,*,#12500,.T.);
#18108=ORIENTED_EDGE('',*,*,#12496,.F.);
#18109=ORIENTED_EDGE('',*,*,#12501,.F.);
#18110=ORIENTED_EDGE('',*,*,#12502,.T.);
#18111=ORIENTED_EDGE('',*,*,#12503,.T.);
#18112=ORIENTED_EDGE('',*,*,#12499,.F.);
#18113=ORIENTED_EDGE('',*,*,#12504,.F.);
#18114=ORIENTED_EDGE('',*,*,#12505,.T.);
#18115=ORIENTED_EDGE('',*,*,#12506,.T.);
#18116=ORIENTED_EDGE('',*,*,#12502,.F.);
#18117=ORIENTED_EDGE('',*,*,#12507,.F.);
#18118=ORIENTED_EDGE('',*,*,#12508,.T.);
#18119=ORIENTED_EDGE('',*,*,#12509,.T.);
#18120=ORIENTED_EDGE('',*,*,#12505,.F.);
#18121=ORIENTED_EDGE('',*,*,#12510,.F.);
#18122=ORIENTED_EDGE('',*,*,#12511,.T.);
#18123=ORIENTED_EDGE('',*,*,#12512,.T.);
#18124=ORIENTED_EDGE('',*,*,#12508,.F.);
#18125=ORIENTED_EDGE('',*,*,#12513,.F.);
#18126=ORIENTED_EDGE('',*,*,#12514,.T.);
#18127=ORIENTED_EDGE('',*,*,#12515,.T.);
#18128=ORIENTED_EDGE('',*,*,#12511,.F.);
#18129=ORIENTED_EDGE('',*,*,#12516,.F.);
#18130=ORIENTED_EDGE('',*,*,#12517,.T.);
#18131=ORIENTED_EDGE('',*,*,#12518,.T.);
#18132=ORIENTED_EDGE('',*,*,#12514,.F.);
#18133=ORIENTED_EDGE('',*,*,#12519,.F.);
#18134=ORIENTED_EDGE('',*,*,#12520,.F.);
#18135=ORIENTED_EDGE('',*,*,#12521,.F.);
#18136=ORIENTED_EDGE('',*,*,#12522,.F.);
#18137=ORIENTED_EDGE('',*,*,#12523,.T.);
#18138=ORIENTED_EDGE('',*,*,#12524,.T.);
#18139=ORIENTED_EDGE('',*,*,#12525,.T.);
#18140=ORIENTED_EDGE('',*,*,#12526,.F.);
#18141=ORIENTED_EDGE('',*,*,#12527,.F.);
#18142=ORIENTED_EDGE('',*,*,#12528,.T.);
#18143=ORIENTED_EDGE('',*,*,#12529,.T.);
#18144=ORIENTED_EDGE('',*,*,#12524,.F.);
#18145=ORIENTED_EDGE('',*,*,#12530,.F.);
#18146=ORIENTED_EDGE('',*,*,#12531,.T.);
#18147=ORIENTED_EDGE('',*,*,#12532,.T.);
#18148=ORIENTED_EDGE('',*,*,#12528,.F.);
#18149=ORIENTED_EDGE('',*,*,#12533,.F.);
#18150=ORIENTED_EDGE('',*,*,#12534,.T.);
#18151=ORIENTED_EDGE('',*,*,#12535,.T.);
#18152=ORIENTED_EDGE('',*,*,#12531,.F.);
#18153=ORIENTED_EDGE('',*,*,#12536,.F.);
#18154=ORIENTED_EDGE('',*,*,#12537,.T.);
#18155=ORIENTED_EDGE('',*,*,#12538,.T.);
#18156=ORIENTED_EDGE('',*,*,#12534,.F.);
#18157=ORIENTED_EDGE('',*,*,#12539,.F.);
#18158=ORIENTED_EDGE('',*,*,#12540,.T.);
#18159=ORIENTED_EDGE('',*,*,#12541,.T.);
#18160=ORIENTED_EDGE('',*,*,#12537,.F.);
#18161=ORIENTED_EDGE('',*,*,#12542,.F.);
#18162=ORIENTED_EDGE('',*,*,#12543,.T.);
#18163=ORIENTED_EDGE('',*,*,#12544,.T.);
#18164=ORIENTED_EDGE('',*,*,#12540,.F.);
#18165=ORIENTED_EDGE('',*,*,#12545,.F.);
#18166=ORIENTED_EDGE('',*,*,#12546,.T.);
#18167=ORIENTED_EDGE('',*,*,#12547,.T.);
#18168=ORIENTED_EDGE('',*,*,#12543,.F.);
#18169=ORIENTED_EDGE('',*,*,#12548,.F.);
#18170=ORIENTED_EDGE('',*,*,#12549,.T.);
#18171=ORIENTED_EDGE('',*,*,#12550,.T.);
#18172=ORIENTED_EDGE('',*,*,#12546,.F.);
#18173=ORIENTED_EDGE('',*,*,#12551,.F.);
#18174=ORIENTED_EDGE('',*,*,#12552,.T.);
#18175=ORIENTED_EDGE('',*,*,#12553,.T.);
#18176=ORIENTED_EDGE('',*,*,#12549,.F.);
#18177=ORIENTED_EDGE('',*,*,#12554,.F.);
#18178=ORIENTED_EDGE('',*,*,#12555,.T.);
#18179=ORIENTED_EDGE('',*,*,#12556,.T.);
#18180=ORIENTED_EDGE('',*,*,#12552,.F.);
#18181=ORIENTED_EDGE('',*,*,#12557,.F.);
#18182=ORIENTED_EDGE('',*,*,#12558,.T.);
#18183=ORIENTED_EDGE('',*,*,#12559,.T.);
#18184=ORIENTED_EDGE('',*,*,#12555,.F.);
#18185=ORIENTED_EDGE('',*,*,#12560,.F.);
#18186=ORIENTED_EDGE('',*,*,#12561,.T.);
#18187=ORIENTED_EDGE('',*,*,#12562,.T.);
#18188=ORIENTED_EDGE('',*,*,#12558,.F.);
#18189=ORIENTED_EDGE('',*,*,#12563,.F.);
#18190=ORIENTED_EDGE('',*,*,#12564,.T.);
#18191=ORIENTED_EDGE('',*,*,#12565,.T.);
#18192=ORIENTED_EDGE('',*,*,#12561,.F.);
#18193=ORIENTED_EDGE('',*,*,#12566,.F.);
#18194=ORIENTED_EDGE('',*,*,#12567,.T.);
#18195=ORIENTED_EDGE('',*,*,#12568,.T.);
#18196=ORIENTED_EDGE('',*,*,#12564,.F.);
#18197=ORIENTED_EDGE('',*,*,#12569,.F.);
#18198=ORIENTED_EDGE('',*,*,#12570,.T.);
#18199=ORIENTED_EDGE('',*,*,#12571,.T.);
#18200=ORIENTED_EDGE('',*,*,#12567,.F.);
#18201=ORIENTED_EDGE('',*,*,#12572,.F.);
#18202=ORIENTED_EDGE('',*,*,#12573,.T.);
#18203=ORIENTED_EDGE('',*,*,#12574,.T.);
#18204=ORIENTED_EDGE('',*,*,#12570,.F.);
#18205=ORIENTED_EDGE('',*,*,#12575,.F.);
#18206=ORIENTED_EDGE('',*,*,#12576,.T.);
#18207=ORIENTED_EDGE('',*,*,#12577,.T.);
#18208=ORIENTED_EDGE('',*,*,#12573,.F.);
#18209=ORIENTED_EDGE('',*,*,#12578,.F.);
#18210=ORIENTED_EDGE('',*,*,#12579,.T.);
#18211=ORIENTED_EDGE('',*,*,#12580,.T.);
#18212=ORIENTED_EDGE('',*,*,#12576,.F.);
#18213=ORIENTED_EDGE('',*,*,#12581,.F.);
#18214=ORIENTED_EDGE('',*,*,#12582,.F.);
#18215=ORIENTED_EDGE('',*,*,#12583,.F.);
#18216=ORIENTED_EDGE('',*,*,#12584,.F.);
#18217=ORIENTED_EDGE('',*,*,#12585,.T.);
#18218=ORIENTED_EDGE('',*,*,#12586,.T.);
#18219=ORIENTED_EDGE('',*,*,#12587,.T.);
#18220=ORIENTED_EDGE('',*,*,#12588,.F.);
#18221=ORIENTED_EDGE('',*,*,#12589,.F.);
#18222=ORIENTED_EDGE('',*,*,#12590,.T.);
#18223=ORIENTED_EDGE('',*,*,#12591,.T.);
#18224=ORIENTED_EDGE('',*,*,#12586,.F.);
#18225=ORIENTED_EDGE('',*,*,#12592,.F.);
#18226=ORIENTED_EDGE('',*,*,#12593,.T.);
#18227=ORIENTED_EDGE('',*,*,#12594,.T.);
#18228=ORIENTED_EDGE('',*,*,#12590,.F.);
#18229=ORIENTED_EDGE('',*,*,#12595,.F.);
#18230=ORIENTED_EDGE('',*,*,#12596,.T.);
#18231=ORIENTED_EDGE('',*,*,#12597,.T.);
#18232=ORIENTED_EDGE('',*,*,#12593,.F.);
#18233=ORIENTED_EDGE('',*,*,#12598,.F.);
#18234=ORIENTED_EDGE('',*,*,#12599,.T.);
#18235=ORIENTED_EDGE('',*,*,#12600,.T.);
#18236=ORIENTED_EDGE('',*,*,#12596,.F.);
#18237=ORIENTED_EDGE('',*,*,#12601,.F.);
#18238=ORIENTED_EDGE('',*,*,#12602,.T.);
#18239=ORIENTED_EDGE('',*,*,#12603,.T.);
#18240=ORIENTED_EDGE('',*,*,#12599,.F.);
#18241=ORIENTED_EDGE('',*,*,#12604,.F.);
#18242=ORIENTED_EDGE('',*,*,#12605,.T.);
#18243=ORIENTED_EDGE('',*,*,#12606,.T.);
#18244=ORIENTED_EDGE('',*,*,#12602,.F.);
#18245=ORIENTED_EDGE('',*,*,#12607,.F.);
#18246=ORIENTED_EDGE('',*,*,#12608,.T.);
#18247=ORIENTED_EDGE('',*,*,#12609,.T.);
#18248=ORIENTED_EDGE('',*,*,#12605,.F.);
#18249=ORIENTED_EDGE('',*,*,#12610,.F.);
#18250=ORIENTED_EDGE('',*,*,#12611,.T.);
#18251=ORIENTED_EDGE('',*,*,#12612,.T.);
#18252=ORIENTED_EDGE('',*,*,#12608,.F.);
#18253=ORIENTED_EDGE('',*,*,#12613,.F.);
#18254=ORIENTED_EDGE('',*,*,#12614,.T.);
#18255=ORIENTED_EDGE('',*,*,#12615,.T.);
#18256=ORIENTED_EDGE('',*,*,#12611,.F.);
#18257=ORIENTED_EDGE('',*,*,#12616,.F.);
#18258=ORIENTED_EDGE('',*,*,#12617,.T.);
#18259=ORIENTED_EDGE('',*,*,#12618,.T.);
#18260=ORIENTED_EDGE('',*,*,#12614,.F.);
#18261=ORIENTED_EDGE('',*,*,#12619,.F.);
#18262=ORIENTED_EDGE('',*,*,#12620,.T.);
#18263=ORIENTED_EDGE('',*,*,#12621,.T.);
#18264=ORIENTED_EDGE('',*,*,#12617,.F.);
#18265=ORIENTED_EDGE('',*,*,#12622,.F.);
#18266=ORIENTED_EDGE('',*,*,#12623,.T.);
#18267=ORIENTED_EDGE('',*,*,#12624,.T.);
#18268=ORIENTED_EDGE('',*,*,#12620,.F.);
#18269=ORIENTED_EDGE('',*,*,#12625,.F.);
#18270=ORIENTED_EDGE('',*,*,#12626,.T.);
#18271=ORIENTED_EDGE('',*,*,#12627,.T.);
#18272=ORIENTED_EDGE('',*,*,#12623,.F.);
#18273=ORIENTED_EDGE('',*,*,#12628,.F.);
#18274=ORIENTED_EDGE('',*,*,#12629,.T.);
#18275=ORIENTED_EDGE('',*,*,#12630,.T.);
#18276=ORIENTED_EDGE('',*,*,#12626,.F.);
#18277=ORIENTED_EDGE('',*,*,#12631,.F.);
#18278=ORIENTED_EDGE('',*,*,#12632,.T.);
#18279=ORIENTED_EDGE('',*,*,#12633,.T.);
#18280=ORIENTED_EDGE('',*,*,#12629,.F.);
#18281=ORIENTED_EDGE('',*,*,#12634,.F.);
#18282=ORIENTED_EDGE('',*,*,#12635,.T.);
#18283=ORIENTED_EDGE('',*,*,#12636,.T.);
#18284=ORIENTED_EDGE('',*,*,#12632,.F.);
#18285=ORIENTED_EDGE('',*,*,#12637,.F.);
#18286=ORIENTED_EDGE('',*,*,#12638,.T.);
#18287=ORIENTED_EDGE('',*,*,#12639,.T.);
#18288=ORIENTED_EDGE('',*,*,#12635,.F.);
#18289=ORIENTED_EDGE('',*,*,#12640,.F.);
#18290=ORIENTED_EDGE('',*,*,#12641,.T.);
#18291=ORIENTED_EDGE('',*,*,#12642,.T.);
#18292=ORIENTED_EDGE('',*,*,#12638,.F.);
#18293=ORIENTED_EDGE('',*,*,#12643,.F.);
#18294=ORIENTED_EDGE('',*,*,#12644,.F.);
#18295=ORIENTED_EDGE('',*,*,#12645,.F.);
#18296=ORIENTED_EDGE('',*,*,#12646,.F.);
#18297=ORIENTED_EDGE('',*,*,#12647,.T.);
#18298=ORIENTED_EDGE('',*,*,#12648,.T.);
#18299=ORIENTED_EDGE('',*,*,#12649,.T.);
#18300=ORIENTED_EDGE('',*,*,#12650,.F.);
#18301=ORIENTED_EDGE('',*,*,#12651,.F.);
#18302=ORIENTED_EDGE('',*,*,#12652,.T.);
#18303=ORIENTED_EDGE('',*,*,#12653,.T.);
#18304=ORIENTED_EDGE('',*,*,#12648,.F.);
#18305=ORIENTED_EDGE('',*,*,#12654,.F.);
#18306=ORIENTED_EDGE('',*,*,#12655,.T.);
#18307=ORIENTED_EDGE('',*,*,#12656,.T.);
#18308=ORIENTED_EDGE('',*,*,#12652,.F.);
#18309=ORIENTED_EDGE('',*,*,#12657,.F.);
#18310=ORIENTED_EDGE('',*,*,#12658,.T.);
#18311=ORIENTED_EDGE('',*,*,#12659,.T.);
#18312=ORIENTED_EDGE('',*,*,#12655,.F.);
#18313=ORIENTED_EDGE('',*,*,#12660,.F.);
#18314=ORIENTED_EDGE('',*,*,#12661,.T.);
#18315=ORIENTED_EDGE('',*,*,#12662,.T.);
#18316=ORIENTED_EDGE('',*,*,#12658,.F.);
#18317=ORIENTED_EDGE('',*,*,#12663,.F.);
#18318=ORIENTED_EDGE('',*,*,#12664,.T.);
#18319=ORIENTED_EDGE('',*,*,#12665,.T.);
#18320=ORIENTED_EDGE('',*,*,#12661,.F.);
#18321=ORIENTED_EDGE('',*,*,#12666,.F.);
#18322=ORIENTED_EDGE('',*,*,#12667,.T.);
#18323=ORIENTED_EDGE('',*,*,#12668,.T.);
#18324=ORIENTED_EDGE('',*,*,#12664,.F.);
#18325=ORIENTED_EDGE('',*,*,#12669,.F.);
#18326=ORIENTED_EDGE('',*,*,#12670,.T.);
#18327=ORIENTED_EDGE('',*,*,#12671,.T.);
#18328=ORIENTED_EDGE('',*,*,#12667,.F.);
#18329=ORIENTED_EDGE('',*,*,#12672,.F.);
#18330=ORIENTED_EDGE('',*,*,#12673,.T.);
#18331=ORIENTED_EDGE('',*,*,#12674,.T.);
#18332=ORIENTED_EDGE('',*,*,#12670,.F.);
#18333=ORIENTED_EDGE('',*,*,#12675,.F.);
#18334=ORIENTED_EDGE('',*,*,#12676,.T.);
#18335=ORIENTED_EDGE('',*,*,#12677,.T.);
#18336=ORIENTED_EDGE('',*,*,#12673,.F.);
#18337=ORIENTED_EDGE('',*,*,#12678,.F.);
#18338=ORIENTED_EDGE('',*,*,#12679,.T.);
#18339=ORIENTED_EDGE('',*,*,#12680,.T.);
#18340=ORIENTED_EDGE('',*,*,#12676,.F.);
#18341=ORIENTED_EDGE('',*,*,#12681,.F.);
#18342=ORIENTED_EDGE('',*,*,#12682,.T.);
#18343=ORIENTED_EDGE('',*,*,#12683,.T.);
#18344=ORIENTED_EDGE('',*,*,#12679,.F.);
#18345=ORIENTED_EDGE('',*,*,#12684,.F.);
#18346=ORIENTED_EDGE('',*,*,#12685,.T.);
#18347=ORIENTED_EDGE('',*,*,#12686,.T.);
#18348=ORIENTED_EDGE('',*,*,#12682,.F.);
#18349=ORIENTED_EDGE('',*,*,#12687,.F.);
#18350=ORIENTED_EDGE('',*,*,#12688,.T.);
#18351=ORIENTED_EDGE('',*,*,#12689,.T.);
#18352=ORIENTED_EDGE('',*,*,#12685,.F.);
#18353=ORIENTED_EDGE('',*,*,#12690,.F.);
#18354=ORIENTED_EDGE('',*,*,#12691,.T.);
#18355=ORIENTED_EDGE('',*,*,#12692,.T.);
#18356=ORIENTED_EDGE('',*,*,#12688,.F.);
#18357=ORIENTED_EDGE('',*,*,#12693,.F.);
#18358=ORIENTED_EDGE('',*,*,#12694,.T.);
#18359=ORIENTED_EDGE('',*,*,#12695,.T.);
#18360=ORIENTED_EDGE('',*,*,#12691,.F.);
#18361=ORIENTED_EDGE('',*,*,#12696,.F.);
#18362=ORIENTED_EDGE('',*,*,#12697,.T.);
#18363=ORIENTED_EDGE('',*,*,#12698,.T.);
#18364=ORIENTED_EDGE('',*,*,#12694,.F.);
#18365=ORIENTED_EDGE('',*,*,#12699,.F.);
#18366=ORIENTED_EDGE('',*,*,#12700,.T.);
#18367=ORIENTED_EDGE('',*,*,#12701,.T.);
#18368=ORIENTED_EDGE('',*,*,#12697,.F.);
#18369=ORIENTED_EDGE('',*,*,#12702,.F.);
#18370=ORIENTED_EDGE('',*,*,#12703,.T.);
#18371=ORIENTED_EDGE('',*,*,#12704,.T.);
#18372=ORIENTED_EDGE('',*,*,#12700,.F.);
#18373=ORIENTED_EDGE('',*,*,#12705,.F.);
#18374=ORIENTED_EDGE('',*,*,#12706,.F.);
#18375=ORIENTED_EDGE('',*,*,#12707,.F.);
#18376=ORIENTED_EDGE('',*,*,#12708,.F.);
#18377=ORIENTED_EDGE('',*,*,#12709,.T.);
#18378=ORIENTED_EDGE('',*,*,#12706,.T.);
#18379=ORIENTED_EDGE('',*,*,#12710,.T.);
#18380=ORIENTED_EDGE('',*,*,#12703,.F.);
#18381=ORIENTED_EDGE('',*,*,#12711,.F.);
#18382=ORIENTED_EDGE('',*,*,#12712,.F.);
#18383=ORIENTED_EDGE('',*,*,#12649,.F.);
#18384=ORIENTED_EDGE('',*,*,#12653,.F.);
#18385=ORIENTED_EDGE('',*,*,#12656,.F.);
#18386=ORIENTED_EDGE('',*,*,#12659,.F.);
#18387=ORIENTED_EDGE('',*,*,#12662,.F.);
#18388=ORIENTED_EDGE('',*,*,#12665,.F.);
#18389=ORIENTED_EDGE('',*,*,#12668,.F.);
#18390=ORIENTED_EDGE('',*,*,#12671,.F.);
#18391=ORIENTED_EDGE('',*,*,#12674,.F.);
#18392=ORIENTED_EDGE('',*,*,#12677,.F.);
#18393=ORIENTED_EDGE('',*,*,#12680,.F.);
#18394=ORIENTED_EDGE('',*,*,#12683,.F.);
#18395=ORIENTED_EDGE('',*,*,#12686,.F.);
#18396=ORIENTED_EDGE('',*,*,#12689,.F.);
#18397=ORIENTED_EDGE('',*,*,#12692,.F.);
#18398=ORIENTED_EDGE('',*,*,#12695,.F.);
#18399=ORIENTED_EDGE('',*,*,#12698,.F.);
#18400=ORIENTED_EDGE('',*,*,#12701,.F.);
#18401=ORIENTED_EDGE('',*,*,#12704,.F.);
#18402=ORIENTED_EDGE('',*,*,#12710,.F.);
#18403=ORIENTED_EDGE('',*,*,#12709,.F.);
#18404=ORIENTED_EDGE('',*,*,#12713,.F.);
#18405=ORIENTED_EDGE('',*,*,#12149,.F.);
#18406=ORIENTED_EDGE('',*,*,#12714,.F.);
#18407=ORIENTED_EDGE('',*,*,#12147,.F.);
#18408=ORIENTED_EDGE('',*,*,#12144,.F.);
#18409=ORIENTED_EDGE('',*,*,#12141,.F.);
#18410=ORIENTED_EDGE('',*,*,#12138,.F.);
#18411=ORIENTED_EDGE('',*,*,#12135,.F.);
#18412=ORIENTED_EDGE('',*,*,#12132,.F.);
#18413=ORIENTED_EDGE('',*,*,#12129,.F.);
#18414=ORIENTED_EDGE('',*,*,#12126,.F.);
#18415=ORIENTED_EDGE('',*,*,#12123,.F.);
#18416=ORIENTED_EDGE('',*,*,#12120,.F.);
#18417=ORIENTED_EDGE('',*,*,#12117,.F.);
#18418=ORIENTED_EDGE('',*,*,#12114,.F.);
#18419=ORIENTED_EDGE('',*,*,#12111,.F.);
#18420=ORIENTED_EDGE('',*,*,#12108,.F.);
#18421=ORIENTED_EDGE('',*,*,#12105,.F.);
#18422=ORIENTED_EDGE('',*,*,#12102,.F.);
#18423=ORIENTED_EDGE('',*,*,#12099,.F.);
#18424=ORIENTED_EDGE('',*,*,#12096,.F.);
#18425=ORIENTED_EDGE('',*,*,#12093,.F.);
#18426=ORIENTED_EDGE('',*,*,#12715,.F.);
#18427=ORIENTED_EDGE('',*,*,#12091,.F.);
#18428=ORIENTED_EDGE('',*,*,#12095,.F.);
#18429=ORIENTED_EDGE('',*,*,#12098,.F.);
#18430=ORIENTED_EDGE('',*,*,#12101,.F.);
#18431=ORIENTED_EDGE('',*,*,#12104,.F.);
#18432=ORIENTED_EDGE('',*,*,#12107,.F.);
#18433=ORIENTED_EDGE('',*,*,#12110,.F.);
#18434=ORIENTED_EDGE('',*,*,#12113,.F.);
#18435=ORIENTED_EDGE('',*,*,#12116,.F.);
#18436=ORIENTED_EDGE('',*,*,#12119,.F.);
#18437=ORIENTED_EDGE('',*,*,#12122,.F.);
#18438=ORIENTED_EDGE('',*,*,#12125,.F.);
#18439=ORIENTED_EDGE('',*,*,#12128,.F.);
#18440=ORIENTED_EDGE('',*,*,#12131,.F.);
#18441=ORIENTED_EDGE('',*,*,#12134,.F.);
#18442=ORIENTED_EDGE('',*,*,#12137,.F.);
#18443=ORIENTED_EDGE('',*,*,#12140,.F.);
#18444=ORIENTED_EDGE('',*,*,#12143,.F.);
#18445=ORIENTED_EDGE('',*,*,#12146,.F.);
#18446=ORIENTED_EDGE('',*,*,#12716,.F.);
#18447=ORIENTED_EDGE('',*,*,#12151,.F.);
#18448=ORIENTED_EDGE('',*,*,#12717,.F.);
#18449=ORIENTED_EDGE('',*,*,#12707,.T.);
#18450=ORIENTED_EDGE('',*,*,#12711,.T.);
#18451=ORIENTED_EDGE('',*,*,#12705,.T.);
#18452=ORIENTED_EDGE('',*,*,#12702,.T.);
#18453=ORIENTED_EDGE('',*,*,#12699,.T.);
#18454=ORIENTED_EDGE('',*,*,#12696,.T.);
#18455=ORIENTED_EDGE('',*,*,#12693,.T.);
#18456=ORIENTED_EDGE('',*,*,#12690,.T.);
#18457=ORIENTED_EDGE('',*,*,#12687,.T.);
#18458=ORIENTED_EDGE('',*,*,#12684,.T.);
#18459=ORIENTED_EDGE('',*,*,#12681,.T.);
#18460=ORIENTED_EDGE('',*,*,#12678,.T.);
#18461=ORIENTED_EDGE('',*,*,#12675,.T.);
#18462=ORIENTED_EDGE('',*,*,#12672,.T.);
#18463=ORIENTED_EDGE('',*,*,#12669,.T.);
#18464=ORIENTED_EDGE('',*,*,#12666,.T.);
#18465=ORIENTED_EDGE('',*,*,#12663,.T.);
#18466=ORIENTED_EDGE('',*,*,#12660,.T.);
#18467=ORIENTED_EDGE('',*,*,#12657,.T.);
#18468=ORIENTED_EDGE('',*,*,#12654,.T.);
#18469=ORIENTED_EDGE('',*,*,#12651,.T.);
#18470=ORIENTED_EDGE('',*,*,#12718,.T.);
#18471=ORIENTED_EDGE('',*,*,#12719,.T.);
#18472=ORIENTED_EDGE('',*,*,#12720,.T.);
#18473=ORIENTED_EDGE('',*,*,#12721,.T.);
#18474=ORIENTED_EDGE('',*,*,#12722,.T.);
#18475=ORIENTED_EDGE('',*,*,#12460,.T.);
#18476=ORIENTED_EDGE('',*,*,#12723,.T.);
#18477=ORIENTED_EDGE('',*,*,#12026,.T.);
#18478=ORIENTED_EDGE('',*,*,#12724,.T.);
#18479=ORIENTED_EDGE('',*,*,#12522,.T.);
#18480=ORIENTED_EDGE('',*,*,#12725,.T.);
#18481=ORIENTED_EDGE('',*,*,#12088,.T.);
#18482=ORIENTED_EDGE('',*,*,#12713,.T.);
#18483=ORIENTED_EDGE('',*,*,#12708,.T.);
#18484=ORIENTED_EDGE('',*,*,#12717,.T.);
#18485=ORIENTED_EDGE('',*,*,#12150,.T.);
#18486=ORIENTED_EDGE('',*,*,#12726,.T.);
#18487=ORIENTED_EDGE('',*,*,#12584,.T.);
#18488=ORIENTED_EDGE('',*,*,#12727,.T.);
#18489=ORIENTED_EDGE('',*,*,#12212,.T.);
#18490=ORIENTED_EDGE('',*,*,#12728,.T.);
#18491=ORIENTED_EDGE('',*,*,#12646,.T.);
#18492=ORIENTED_EDGE('',*,*,#12729,.T.);
#18493=ORIENTED_EDGE('',*,*,#12274,.T.);
#18494=ORIENTED_EDGE('',*,*,#12730,.T.);
#18495=ORIENTED_EDGE('',*,*,#12398,.T.);
#18496=ORIENTED_EDGE('',*,*,#12731,.T.);
#18497=ORIENTED_EDGE('',*,*,#12336,.T.);
#18498=ORIENTED_EDGE('',*,*,#12644,.T.);
#18499=ORIENTED_EDGE('',*,*,#12732,.T.);
#18500=ORIENTED_EDGE('',*,*,#12641,.F.);
#18501=ORIENTED_EDGE('',*,*,#12733,.F.);
#18502=ORIENTED_EDGE('',*,*,#12734,.F.);
#18503=ORIENTED_EDGE('',*,*,#12587,.F.);
#18504=ORIENTED_EDGE('',*,*,#12591,.F.);
#18505=ORIENTED_EDGE('',*,*,#12594,.F.);
#18506=ORIENTED_EDGE('',*,*,#12597,.F.);
#18507=ORIENTED_EDGE('',*,*,#12600,.F.);
#18508=ORIENTED_EDGE('',*,*,#12603,.F.);
#18509=ORIENTED_EDGE('',*,*,#12606,.F.);
#18510=ORIENTED_EDGE('',*,*,#12609,.F.);
#18511=ORIENTED_EDGE('',*,*,#12612,.F.);
#18512=ORIENTED_EDGE('',*,*,#12615,.F.);
#18513=ORIENTED_EDGE('',*,*,#12618,.F.);
#18514=ORIENTED_EDGE('',*,*,#12621,.F.);
#18515=ORIENTED_EDGE('',*,*,#12624,.F.);
#18516=ORIENTED_EDGE('',*,*,#12627,.F.);
#18517=ORIENTED_EDGE('',*,*,#12630,.F.);
#18518=ORIENTED_EDGE('',*,*,#12633,.F.);
#18519=ORIENTED_EDGE('',*,*,#12636,.F.);
#18520=ORIENTED_EDGE('',*,*,#12639,.F.);
#18521=ORIENTED_EDGE('',*,*,#12642,.F.);
#18522=ORIENTED_EDGE('',*,*,#12732,.F.);
#18523=ORIENTED_EDGE('',*,*,#12647,.F.);
#18524=ORIENTED_EDGE('',*,*,#12728,.F.);
#18525=ORIENTED_EDGE('',*,*,#12273,.F.);
#18526=ORIENTED_EDGE('',*,*,#12735,.F.);
#18527=ORIENTED_EDGE('',*,*,#12271,.F.);
#18528=ORIENTED_EDGE('',*,*,#12268,.F.);
#18529=ORIENTED_EDGE('',*,*,#12265,.F.);
#18530=ORIENTED_EDGE('',*,*,#12262,.F.);
#18531=ORIENTED_EDGE('',*,*,#12259,.F.);
#18532=ORIENTED_EDGE('',*,*,#12256,.F.);
#18533=ORIENTED_EDGE('',*,*,#12253,.F.);
#18534=ORIENTED_EDGE('',*,*,#12250,.F.);
#18535=ORIENTED_EDGE('',*,*,#12247,.F.);
#18536=ORIENTED_EDGE('',*,*,#12244,.F.);
#18537=ORIENTED_EDGE('',*,*,#12241,.F.);
#18538=ORIENTED_EDGE('',*,*,#12238,.F.);
#18539=ORIENTED_EDGE('',*,*,#12235,.F.);
#18540=ORIENTED_EDGE('',*,*,#12232,.F.);
#18541=ORIENTED_EDGE('',*,*,#12229,.F.);
#18542=ORIENTED_EDGE('',*,*,#12226,.F.);
#18543=ORIENTED_EDGE('',*,*,#12223,.F.);
#18544=ORIENTED_EDGE('',*,*,#12220,.F.);
#18545=ORIENTED_EDGE('',*,*,#12217,.F.);
#18546=ORIENTED_EDGE('',*,*,#12736,.F.);
#18547=ORIENTED_EDGE('',*,*,#12215,.F.);
#18548=ORIENTED_EDGE('',*,*,#12219,.F.);
#18549=ORIENTED_EDGE('',*,*,#12222,.F.);
#18550=ORIENTED_EDGE('',*,*,#12225,.F.);
#18551=ORIENTED_EDGE('',*,*,#12228,.F.);
#18552=ORIENTED_EDGE('',*,*,#12231,.F.);
#18553=ORIENTED_EDGE('',*,*,#12234,.F.);
#18554=ORIENTED_EDGE('',*,*,#12237,.F.);
#18555=ORIENTED_EDGE('',*,*,#12240,.F.);
#18556=ORIENTED_EDGE('',*,*,#12243,.F.);
#18557=ORIENTED_EDGE('',*,*,#12246,.F.);
#18558=ORIENTED_EDGE('',*,*,#12249,.F.);
#18559=ORIENTED_EDGE('',*,*,#12252,.F.);
#18560=ORIENTED_EDGE('',*,*,#12255,.F.);
#18561=ORIENTED_EDGE('',*,*,#12258,.F.);
#18562=ORIENTED_EDGE('',*,*,#12261,.F.);
#18563=ORIENTED_EDGE('',*,*,#12264,.F.);
#18564=ORIENTED_EDGE('',*,*,#12267,.F.);
#18565=ORIENTED_EDGE('',*,*,#12270,.F.);
#18566=ORIENTED_EDGE('',*,*,#12737,.F.);
#18567=ORIENTED_EDGE('',*,*,#12275,.F.);
#18568=ORIENTED_EDGE('',*,*,#12729,.F.);
#18569=ORIENTED_EDGE('',*,*,#12645,.T.);
#18570=ORIENTED_EDGE('',*,*,#12733,.T.);
#18571=ORIENTED_EDGE('',*,*,#12643,.T.);
#18572=ORIENTED_EDGE('',*,*,#12640,.T.);
#18573=ORIENTED_EDGE('',*,*,#12637,.T.);
#18574=ORIENTED_EDGE('',*,*,#12634,.T.);
#18575=ORIENTED_EDGE('',*,*,#12631,.T.);
#18576=ORIENTED_EDGE('',*,*,#12628,.T.);
#18577=ORIENTED_EDGE('',*,*,#12625,.T.);
#18578=ORIENTED_EDGE('',*,*,#12622,.T.);
#18579=ORIENTED_EDGE('',*,*,#12619,.T.);
#18580=ORIENTED_EDGE('',*,*,#12616,.T.);
#18581=ORIENTED_EDGE('',*,*,#12613,.T.);
#18582=ORIENTED_EDGE('',*,*,#12610,.T.);
#18583=ORIENTED_EDGE('',*,*,#12607,.T.);
#18584=ORIENTED_EDGE('',*,*,#12604,.T.);
#18585=ORIENTED_EDGE('',*,*,#12601,.T.);
#18586=ORIENTED_EDGE('',*,*,#12598,.T.);
#18587=ORIENTED_EDGE('',*,*,#12595,.T.);
#18588=ORIENTED_EDGE('',*,*,#12592,.T.);
#18589=ORIENTED_EDGE('',*,*,#12589,.T.);
#18590=ORIENTED_EDGE('',*,*,#12582,.T.);
#18591=ORIENTED_EDGE('',*,*,#12738,.T.);
#18592=ORIENTED_EDGE('',*,*,#12579,.F.);
#18593=ORIENTED_EDGE('',*,*,#12739,.F.);
#18594=ORIENTED_EDGE('',*,*,#12740,.F.);
#18595=ORIENTED_EDGE('',*,*,#12525,.F.);
#18596=ORIENTED_EDGE('',*,*,#12529,.F.);
#18597=ORIENTED_EDGE('',*,*,#12532,.F.);
#18598=ORIENTED_EDGE('',*,*,#12535,.F.);
#18599=ORIENTED_EDGE('',*,*,#12538,.F.);
#18600=ORIENTED_EDGE('',*,*,#12541,.F.);
#18601=ORIENTED_EDGE('',*,*,#12544,.F.);
#18602=ORIENTED_EDGE('',*,*,#12547,.F.);
#18603=ORIENTED_EDGE('',*,*,#12550,.F.);
#18604=ORIENTED_EDGE('',*,*,#12553,.F.);
#18605=ORIENTED_EDGE('',*,*,#12556,.F.);
#18606=ORIENTED_EDGE('',*,*,#12559,.F.);
#18607=ORIENTED_EDGE('',*,*,#12562,.F.);
#18608=ORIENTED_EDGE('',*,*,#12565,.F.);
#18609=ORIENTED_EDGE('',*,*,#12568,.F.);
#18610=ORIENTED_EDGE('',*,*,#12571,.F.);
#18611=ORIENTED_EDGE('',*,*,#12574,.F.);
#18612=ORIENTED_EDGE('',*,*,#12577,.F.);
#18613=ORIENTED_EDGE('',*,*,#12580,.F.);
#18614=ORIENTED_EDGE('',*,*,#12738,.F.);
#18615=ORIENTED_EDGE('',*,*,#12585,.F.);
#18616=ORIENTED_EDGE('',*,*,#12726,.F.);
#18617=ORIENTED_EDGE('',*,*,#12211,.F.);
#18618=ORIENTED_EDGE('',*,*,#12741,.F.);
#18619=ORIENTED_EDGE('',*,*,#12209,.F.);
#18620=ORIENTED_EDGE('',*,*,#12206,.F.);
#18621=ORIENTED_EDGE('',*,*,#12203,.F.);
#18622=ORIENTED_EDGE('',*,*,#12200,.F.);
#18623=ORIENTED_EDGE('',*,*,#12197,.F.);
#18624=ORIENTED_EDGE('',*,*,#12194,.F.);
#18625=ORIENTED_EDGE('',*,*,#12191,.F.);
#18626=ORIENTED_EDGE('',*,*,#12188,.F.);
#18627=ORIENTED_EDGE('',*,*,#12185,.F.);
#18628=ORIENTED_EDGE('',*,*,#12182,.F.);
#18629=ORIENTED_EDGE('',*,*,#12179,.F.);
#18630=ORIENTED_EDGE('',*,*,#12176,.F.);
#18631=ORIENTED_EDGE('',*,*,#12173,.F.);
#18632=ORIENTED_EDGE('',*,*,#12170,.F.);
#18633=ORIENTED_EDGE('',*,*,#12167,.F.);
#18634=ORIENTED_EDGE('',*,*,#12164,.F.);
#18635=ORIENTED_EDGE('',*,*,#12161,.F.);
#18636=ORIENTED_EDGE('',*,*,#12158,.F.);
#18637=ORIENTED_EDGE('',*,*,#12155,.F.);
#18638=ORIENTED_EDGE('',*,*,#12742,.F.);
#18639=ORIENTED_EDGE('',*,*,#12153,.F.);
#18640=ORIENTED_EDGE('',*,*,#12157,.F.);
#18641=ORIENTED_EDGE('',*,*,#12160,.F.);
#18642=ORIENTED_EDGE('',*,*,#12163,.F.);
#18643=ORIENTED_EDGE('',*,*,#12166,.F.);
#18644=ORIENTED_EDGE('',*,*,#12169,.F.);
#18645=ORIENTED_EDGE('',*,*,#12172,.F.);
#18646=ORIENTED_EDGE('',*,*,#12175,.F.);
#18647=ORIENTED_EDGE('',*,*,#12178,.F.);
#18648=ORIENTED_EDGE('',*,*,#12181,.F.);
#18649=ORIENTED_EDGE('',*,*,#12184,.F.);
#18650=ORIENTED_EDGE('',*,*,#12187,.F.);
#18651=ORIENTED_EDGE('',*,*,#12190,.F.);
#18652=ORIENTED_EDGE('',*,*,#12193,.F.);
#18653=ORIENTED_EDGE('',*,*,#12196,.F.);
#18654=ORIENTED_EDGE('',*,*,#12199,.F.);
#18655=ORIENTED_EDGE('',*,*,#12202,.F.);
#18656=ORIENTED_EDGE('',*,*,#12205,.F.);
#18657=ORIENTED_EDGE('',*,*,#12208,.F.);
#18658=ORIENTED_EDGE('',*,*,#12743,.F.);
#18659=ORIENTED_EDGE('',*,*,#12213,.F.);
#18660=ORIENTED_EDGE('',*,*,#12727,.F.);
#18661=ORIENTED_EDGE('',*,*,#12583,.T.);
#18662=ORIENTED_EDGE('',*,*,#12739,.T.);
#18663=ORIENTED_EDGE('',*,*,#12581,.T.);
#18664=ORIENTED_EDGE('',*,*,#12578,.T.);
#18665=ORIENTED_EDGE('',*,*,#12575,.T.);
#18666=ORIENTED_EDGE('',*,*,#12572,.T.);
#18667=ORIENTED_EDGE('',*,*,#12569,.T.);
#18668=ORIENTED_EDGE('',*,*,#12566,.T.);
#18669=ORIENTED_EDGE('',*,*,#12563,.T.);
#18670=ORIENTED_EDGE('',*,*,#12560,.T.);
#18671=ORIENTED_EDGE('',*,*,#12557,.T.);
#18672=ORIENTED_EDGE('',*,*,#12554,.T.);
#18673=ORIENTED_EDGE('',*,*,#12551,.T.);
#18674=ORIENTED_EDGE('',*,*,#12548,.T.);
#18675=ORIENTED_EDGE('',*,*,#12545,.T.);
#18676=ORIENTED_EDGE('',*,*,#12542,.T.);
#18677=ORIENTED_EDGE('',*,*,#12539,.T.);
#18678=ORIENTED_EDGE('',*,*,#12536,.T.);
#18679=ORIENTED_EDGE('',*,*,#12533,.T.);
#18680=ORIENTED_EDGE('',*,*,#12530,.T.);
#18681=ORIENTED_EDGE('',*,*,#12527,.T.);
#18682=ORIENTED_EDGE('',*,*,#12520,.T.);
#18683=ORIENTED_EDGE('',*,*,#12744,.T.);
#18684=ORIENTED_EDGE('',*,*,#12517,.F.);
#18685=ORIENTED_EDGE('',*,*,#12745,.F.);
#18686=ORIENTED_EDGE('',*,*,#12746,.F.);
#18687=ORIENTED_EDGE('',*,*,#12463,.F.);
#18688=ORIENTED_EDGE('',*,*,#12467,.F.);
#18689=ORIENTED_EDGE('',*,*,#12470,.F.);
#18690=ORIENTED_EDGE('',*,*,#12473,.F.);
#18691=ORIENTED_EDGE('',*,*,#12476,.F.);
#18692=ORIENTED_EDGE('',*,*,#12479,.F.);
#18693=ORIENTED_EDGE('',*,*,#12482,.F.);
#18694=ORIENTED_EDGE('',*,*,#12485,.F.);
#18695=ORIENTED_EDGE('',*,*,#12488,.F.);
#18696=ORIENTED_EDGE('',*,*,#12491,.F.);
#18697=ORIENTED_EDGE('',*,*,#12494,.F.);
#18698=ORIENTED_EDGE('',*,*,#12497,.F.);
#18699=ORIENTED_EDGE('',*,*,#12500,.F.);
#18700=ORIENTED_EDGE('',*,*,#12503,.F.);
#18701=ORIENTED_EDGE('',*,*,#12506,.F.);
#18702=ORIENTED_EDGE('',*,*,#12509,.F.);
#18703=ORIENTED_EDGE('',*,*,#12512,.F.);
#18704=ORIENTED_EDGE('',*,*,#12515,.F.);
#18705=ORIENTED_EDGE('',*,*,#12518,.F.);
#18706=ORIENTED_EDGE('',*,*,#12744,.F.);
#18707=ORIENTED_EDGE('',*,*,#12523,.F.);
#18708=ORIENTED_EDGE('',*,*,#12724,.F.);
#18709=ORIENTED_EDGE('',*,*,#12087,.F.);
#18710=ORIENTED_EDGE('',*,*,#12747,.F.);
#18711=ORIENTED_EDGE('',*,*,#12085,.F.);
#18712=ORIENTED_EDGE('',*,*,#12082,.F.);
#18713=ORIENTED_EDGE('',*,*,#12079,.F.);
#18714=ORIENTED_EDGE('',*,*,#12076,.F.);
#18715=ORIENTED_EDGE('',*,*,#12073,.F.);
#18716=ORIENTED_EDGE('',*,*,#12070,.F.);
#18717=ORIENTED_EDGE('',*,*,#12067,.F.);
#18718=ORIENTED_EDGE('',*,*,#12064,.F.);
#18719=ORIENTED_EDGE('',*,*,#12061,.F.);
#18720=ORIENTED_EDGE('',*,*,#12058,.F.);
#18721=ORIENTED_EDGE('',*,*,#12055,.F.);
#18722=ORIENTED_EDGE('',*,*,#12052,.F.);
#18723=ORIENTED_EDGE('',*,*,#12049,.F.);
#18724=ORIENTED_EDGE('',*,*,#12046,.F.);
#18725=ORIENTED_EDGE('',*,*,#12043,.F.);
#18726=ORIENTED_EDGE('',*,*,#12040,.F.);
#18727=ORIENTED_EDGE('',*,*,#12037,.F.);
#18728=ORIENTED_EDGE('',*,*,#12034,.F.);
#18729=ORIENTED_EDGE('',*,*,#12031,.F.);
#18730=ORIENTED_EDGE('',*,*,#12748,.F.);
#18731=ORIENTED_EDGE('',*,*,#12029,.F.);
#18732=ORIENTED_EDGE('',*,*,#12033,.F.);
#18733=ORIENTED_EDGE('',*,*,#12036,.F.);
#18734=ORIENTED_EDGE('',*,*,#12039,.F.);
#18735=ORIENTED_EDGE('',*,*,#12042,.F.);
#18736=ORIENTED_EDGE('',*,*,#12045,.F.);
#18737=ORIENTED_EDGE('',*,*,#12048,.F.);
#18738=ORIENTED_EDGE('',*,*,#12051,.F.);
#18739=ORIENTED_EDGE('',*,*,#12054,.F.);
#18740=ORIENTED_EDGE('',*,*,#12057,.F.);
#18741=ORIENTED_EDGE('',*,*,#12060,.F.);
#18742=ORIENTED_EDGE('',*,*,#12063,.F.);
#18743=ORIENTED_EDGE('',*,*,#12066,.F.);
#18744=ORIENTED_EDGE('',*,*,#12069,.F.);
#18745=ORIENTED_EDGE('',*,*,#12072,.F.);
#18746=ORIENTED_EDGE('',*,*,#12075,.F.);
#18747=ORIENTED_EDGE('',*,*,#12078,.F.);
#18748=ORIENTED_EDGE('',*,*,#12081,.F.);
#18749=ORIENTED_EDGE('',*,*,#12084,.F.);
#18750=ORIENTED_EDGE('',*,*,#12749,.F.);
#18751=ORIENTED_EDGE('',*,*,#12089,.F.);
#18752=ORIENTED_EDGE('',*,*,#12725,.F.);
#18753=ORIENTED_EDGE('',*,*,#12521,.T.);
#18754=ORIENTED_EDGE('',*,*,#12745,.T.);
#18755=ORIENTED_EDGE('',*,*,#12519,.T.);
#18756=ORIENTED_EDGE('',*,*,#12516,.T.);
#18757=ORIENTED_EDGE('',*,*,#12513,.T.);
#18758=ORIENTED_EDGE('',*,*,#12510,.T.);
#18759=ORIENTED_EDGE('',*,*,#12507,.T.);
#18760=ORIENTED_EDGE('',*,*,#12504,.T.);
#18761=ORIENTED_EDGE('',*,*,#12501,.T.);
#18762=ORIENTED_EDGE('',*,*,#12498,.T.);
#18763=ORIENTED_EDGE('',*,*,#12495,.T.);
#18764=ORIENTED_EDGE('',*,*,#12492,.T.);
#18765=ORIENTED_EDGE('',*,*,#12489,.T.);
#18766=ORIENTED_EDGE('',*,*,#12486,.T.);
#18767=ORIENTED_EDGE('',*,*,#12483,.T.);
#18768=ORIENTED_EDGE('',*,*,#12480,.T.);
#18769=ORIENTED_EDGE('',*,*,#12477,.T.);
#18770=ORIENTED_EDGE('',*,*,#12474,.T.);
#18771=ORIENTED_EDGE('',*,*,#12471,.T.);
#18772=ORIENTED_EDGE('',*,*,#12468,.T.);
#18773=ORIENTED_EDGE('',*,*,#12465,.T.);
#18774=ORIENTED_EDGE('',*,*,#12458,.T.);
#18775=ORIENTED_EDGE('',*,*,#12750,.T.);
#18776=ORIENTED_EDGE('',*,*,#12455,.F.);
#18777=ORIENTED_EDGE('',*,*,#12751,.F.);
#18778=ORIENTED_EDGE('',*,*,#12752,.F.);
#18779=ORIENTED_EDGE('',*,*,#12401,.F.);
#18780=ORIENTED_EDGE('',*,*,#12405,.F.);
#18781=ORIENTED_EDGE('',*,*,#12408,.F.);
#18782=ORIENTED_EDGE('',*,*,#12411,.F.);
#18783=ORIENTED_EDGE('',*,*,#12414,.F.);
#18784=ORIENTED_EDGE('',*,*,#12417,.F.);
#18785=ORIENTED_EDGE('',*,*,#12420,.F.);
#18786=ORIENTED_EDGE('',*,*,#12423,.F.);
#18787=ORIENTED_EDGE('',*,*,#12426,.F.);
#18788=ORIENTED_EDGE('',*,*,#12429,.F.);
#18789=ORIENTED_EDGE('',*,*,#12432,.F.);
#18790=ORIENTED_EDGE('',*,*,#12435,.F.);
#18791=ORIENTED_EDGE('',*,*,#12438,.F.);
#18792=ORIENTED_EDGE('',*,*,#12441,.F.);
#18793=ORIENTED_EDGE('',*,*,#12444,.F.);
#18794=ORIENTED_EDGE('',*,*,#12447,.F.);
#18795=ORIENTED_EDGE('',*,*,#12450,.F.);
#18796=ORIENTED_EDGE('',*,*,#12453,.F.);
#18797=ORIENTED_EDGE('',*,*,#12456,.F.);
#18798=ORIENTED_EDGE('',*,*,#12750,.F.);
#18799=ORIENTED_EDGE('',*,*,#12461,.F.);
#18800=ORIENTED_EDGE('',*,*,#12722,.F.);
#18801=ORIENTED_EDGE('',*,*,#12025,.F.);
#18802=ORIENTED_EDGE('',*,*,#12753,.F.);
#18803=ORIENTED_EDGE('',*,*,#12023,.F.);
#18804=ORIENTED_EDGE('',*,*,#12020,.F.);
#18805=ORIENTED_EDGE('',*,*,#12017,.F.);
#18806=ORIENTED_EDGE('',*,*,#12014,.F.);
#18807=ORIENTED_EDGE('',*,*,#12011,.F.);
#18808=ORIENTED_EDGE('',*,*,#12008,.F.);
#18809=ORIENTED_EDGE('',*,*,#12005,.F.);
#18810=ORIENTED_EDGE('',*,*,#12002,.F.);
#18811=ORIENTED_EDGE('',*,*,#11999,.F.);
#18812=ORIENTED_EDGE('',*,*,#11996,.F.);
#18813=ORIENTED_EDGE('',*,*,#11993,.F.);
#18814=ORIENTED_EDGE('',*,*,#11990,.F.);
#18815=ORIENTED_EDGE('',*,*,#11987,.F.);
#18816=ORIENTED_EDGE('',*,*,#11984,.F.);
#18817=ORIENTED_EDGE('',*,*,#11981,.F.);
#18818=ORIENTED_EDGE('',*,*,#11978,.F.);
#18819=ORIENTED_EDGE('',*,*,#11975,.F.);
#18820=ORIENTED_EDGE('',*,*,#11972,.F.);
#18821=ORIENTED_EDGE('',*,*,#11969,.F.);
#18822=ORIENTED_EDGE('',*,*,#12754,.F.);
#18823=ORIENTED_EDGE('',*,*,#11967,.F.);
#18824=ORIENTED_EDGE('',*,*,#11971,.F.);
#18825=ORIENTED_EDGE('',*,*,#11974,.F.);
#18826=ORIENTED_EDGE('',*,*,#11977,.F.);
#18827=ORIENTED_EDGE('',*,*,#11980,.F.);
#18828=ORIENTED_EDGE('',*,*,#11983,.F.);
#18829=ORIENTED_EDGE('',*,*,#11986,.F.);
#18830=ORIENTED_EDGE('',*,*,#11989,.F.);
#18831=ORIENTED_EDGE('',*,*,#11992,.F.);
#18832=ORIENTED_EDGE('',*,*,#11995,.F.);
#18833=ORIENTED_EDGE('',*,*,#11998,.F.);
#18834=ORIENTED_EDGE('',*,*,#12001,.F.);
#18835=ORIENTED_EDGE('',*,*,#12004,.F.);
#18836=ORIENTED_EDGE('',*,*,#12007,.F.);
#18837=ORIENTED_EDGE('',*,*,#12010,.F.);
#18838=ORIENTED_EDGE('',*,*,#12013,.F.);
#18839=ORIENTED_EDGE('',*,*,#12016,.F.);
#18840=ORIENTED_EDGE('',*,*,#12019,.F.);
#18841=ORIENTED_EDGE('',*,*,#12022,.F.);
#18842=ORIENTED_EDGE('',*,*,#12755,.F.);
#18843=ORIENTED_EDGE('',*,*,#12027,.F.);
#18844=ORIENTED_EDGE('',*,*,#12723,.F.);
#18845=ORIENTED_EDGE('',*,*,#12459,.T.);
#18846=ORIENTED_EDGE('',*,*,#12751,.T.);
#18847=ORIENTED_EDGE('',*,*,#12457,.T.);
#18848=ORIENTED_EDGE('',*,*,#12454,.T.);
#18849=ORIENTED_EDGE('',*,*,#12451,.T.);
#18850=ORIENTED_EDGE('',*,*,#12448,.T.);
#18851=ORIENTED_EDGE('',*,*,#12445,.T.);
#18852=ORIENTED_EDGE('',*,*,#12442,.T.);
#18853=ORIENTED_EDGE('',*,*,#12439,.T.);
#18854=ORIENTED_EDGE('',*,*,#12436,.T.);
#18855=ORIENTED_EDGE('',*,*,#12433,.T.);
#18856=ORIENTED_EDGE('',*,*,#12430,.T.);
#18857=ORIENTED_EDGE('',*,*,#12427,.T.);
#18858=ORIENTED_EDGE('',*,*,#12424,.T.);
#18859=ORIENTED_EDGE('',*,*,#12421,.T.);
#18860=ORIENTED_EDGE('',*,*,#12418,.T.);
#18861=ORIENTED_EDGE('',*,*,#12415,.T.);
#18862=ORIENTED_EDGE('',*,*,#12412,.T.);
#18863=ORIENTED_EDGE('',*,*,#12409,.T.);
#18864=ORIENTED_EDGE('',*,*,#12406,.T.);
#18865=ORIENTED_EDGE('',*,*,#12403,.T.);
#18866=ORIENTED_EDGE('',*,*,#12396,.T.);
#18867=ORIENTED_EDGE('',*,*,#12756,.T.);
#18868=ORIENTED_EDGE('',*,*,#12393,.F.);
#18869=ORIENTED_EDGE('',*,*,#12757,.F.);
#18870=ORIENTED_EDGE('',*,*,#12758,.F.);
#18871=ORIENTED_EDGE('',*,*,#12339,.F.);
#18872=ORIENTED_EDGE('',*,*,#12343,.F.);
#18873=ORIENTED_EDGE('',*,*,#12346,.F.);
#18874=ORIENTED_EDGE('',*,*,#12349,.F.);
#18875=ORIENTED_EDGE('',*,*,#12352,.F.);
#18876=ORIENTED_EDGE('',*,*,#12355,.F.);
#18877=ORIENTED_EDGE('',*,*,#12358,.F.);
#18878=ORIENTED_EDGE('',*,*,#12361,.F.);
#18879=ORIENTED_EDGE('',*,*,#12364,.F.);
#18880=ORIENTED_EDGE('',*,*,#12367,.F.);
#18881=ORIENTED_EDGE('',*,*,#12370,.F.);
#18882=ORIENTED_EDGE('',*,*,#12373,.F.);
#18883=ORIENTED_EDGE('',*,*,#12376,.F.);
#18884=ORIENTED_EDGE('',*,*,#12379,.F.);
#18885=ORIENTED_EDGE('',*,*,#12382,.F.);
#18886=ORIENTED_EDGE('',*,*,#12385,.F.);
#18887=ORIENTED_EDGE('',*,*,#12388,.F.);
#18888=ORIENTED_EDGE('',*,*,#12391,.F.);
#18889=ORIENTED_EDGE('',*,*,#12394,.F.);
#18890=ORIENTED_EDGE('',*,*,#12756,.F.);
#18891=ORIENTED_EDGE('',*,*,#12399,.F.);
#18892=ORIENTED_EDGE('',*,*,#12730,.F.);
#18893=ORIENTED_EDGE('',*,*,#12335,.F.);
#18894=ORIENTED_EDGE('',*,*,#12759,.F.);
#18895=ORIENTED_EDGE('',*,*,#12333,.F.);
#18896=ORIENTED_EDGE('',*,*,#12330,.F.);
#18897=ORIENTED_EDGE('',*,*,#12327,.F.);
#18898=ORIENTED_EDGE('',*,*,#12324,.F.);
#18899=ORIENTED_EDGE('',*,*,#12321,.F.);
#18900=ORIENTED_EDGE('',*,*,#12318,.F.);
#18901=ORIENTED_EDGE('',*,*,#12315,.F.);
#18902=ORIENTED_EDGE('',*,*,#12312,.F.);
#18903=ORIENTED_EDGE('',*,*,#12309,.F.);
#18904=ORIENTED_EDGE('',*,*,#12306,.F.);
#18905=ORIENTED_EDGE('',*,*,#12303,.F.);
#18906=ORIENTED_EDGE('',*,*,#12300,.F.);
#18907=ORIENTED_EDGE('',*,*,#12297,.F.);
#18908=ORIENTED_EDGE('',*,*,#12294,.F.);
#18909=ORIENTED_EDGE('',*,*,#12291,.F.);
#18910=ORIENTED_EDGE('',*,*,#12288,.F.);
#18911=ORIENTED_EDGE('',*,*,#12285,.F.);
#18912=ORIENTED_EDGE('',*,*,#12282,.F.);
#18913=ORIENTED_EDGE('',*,*,#12279,.F.);
#18914=ORIENTED_EDGE('',*,*,#12760,.F.);
#18915=ORIENTED_EDGE('',*,*,#12277,.F.);
#18916=ORIENTED_EDGE('',*,*,#12281,.F.);
#18917=ORIENTED_EDGE('',*,*,#12284,.F.);
#18918=ORIENTED_EDGE('',*,*,#12287,.F.);
#18919=ORIENTED_EDGE('',*,*,#12290,.F.);
#18920=ORIENTED_EDGE('',*,*,#12293,.F.);
#18921=ORIENTED_EDGE('',*,*,#12296,.F.);
#18922=ORIENTED_EDGE('',*,*,#12299,.F.);
#18923=ORIENTED_EDGE('',*,*,#12302,.F.);
#18924=ORIENTED_EDGE('',*,*,#12305,.F.);
#18925=ORIENTED_EDGE('',*,*,#12308,.F.);
#18926=ORIENTED_EDGE('',*,*,#12311,.F.);
#18927=ORIENTED_EDGE('',*,*,#12314,.F.);
#18928=ORIENTED_EDGE('',*,*,#12317,.F.);
#18929=ORIENTED_EDGE('',*,*,#12320,.F.);
#18930=ORIENTED_EDGE('',*,*,#12323,.F.);
#18931=ORIENTED_EDGE('',*,*,#12326,.F.);
#18932=ORIENTED_EDGE('',*,*,#12329,.F.);
#18933=ORIENTED_EDGE('',*,*,#12332,.F.);
#18934=ORIENTED_EDGE('',*,*,#12761,.F.);
#18935=ORIENTED_EDGE('',*,*,#12337,.F.);
#18936=ORIENTED_EDGE('',*,*,#12731,.F.);
#18937=ORIENTED_EDGE('',*,*,#12397,.T.);
#18938=ORIENTED_EDGE('',*,*,#12757,.T.);
#18939=ORIENTED_EDGE('',*,*,#12395,.T.);
#18940=ORIENTED_EDGE('',*,*,#12392,.T.);
#18941=ORIENTED_EDGE('',*,*,#12389,.T.);
#18942=ORIENTED_EDGE('',*,*,#12386,.T.);
#18943=ORIENTED_EDGE('',*,*,#12383,.T.);
#18944=ORIENTED_EDGE('',*,*,#12380,.T.);
#18945=ORIENTED_EDGE('',*,*,#12377,.T.);
#18946=ORIENTED_EDGE('',*,*,#12374,.T.);
#18947=ORIENTED_EDGE('',*,*,#12371,.T.);
#18948=ORIENTED_EDGE('',*,*,#12368,.T.);
#18949=ORIENTED_EDGE('',*,*,#12365,.T.);
#18950=ORIENTED_EDGE('',*,*,#12362,.T.);
#18951=ORIENTED_EDGE('',*,*,#12359,.T.);
#18952=ORIENTED_EDGE('',*,*,#12356,.T.);
#18953=ORIENTED_EDGE('',*,*,#12353,.T.);
#18954=ORIENTED_EDGE('',*,*,#12350,.T.);
#18955=ORIENTED_EDGE('',*,*,#12347,.T.);
#18956=ORIENTED_EDGE('',*,*,#12344,.T.);
#18957=ORIENTED_EDGE('',*,*,#12341,.T.);
#18958=ORIENTED_EDGE('',*,*,#12334,.T.);
#18959=ORIENTED_EDGE('',*,*,#12761,.T.);
#18960=ORIENTED_EDGE('',*,*,#12331,.F.);
#18961=ORIENTED_EDGE('',*,*,#12759,.T.);
#18962=ORIENTED_EDGE('',*,*,#12272,.T.);
#18963=ORIENTED_EDGE('',*,*,#12737,.T.);
#18964=ORIENTED_EDGE('',*,*,#12269,.F.);
#18965=ORIENTED_EDGE('',*,*,#12735,.T.);
#18966=ORIENTED_EDGE('',*,*,#12210,.T.);
#18967=ORIENTED_EDGE('',*,*,#12743,.T.);
#18968=ORIENTED_EDGE('',*,*,#12207,.F.);
#18969=ORIENTED_EDGE('',*,*,#12741,.T.);
#18970=ORIENTED_EDGE('',*,*,#12148,.T.);
#18971=ORIENTED_EDGE('',*,*,#12716,.T.);
#18972=ORIENTED_EDGE('',*,*,#12145,.F.);
#18973=ORIENTED_EDGE('',*,*,#12714,.T.);
#18974=ORIENTED_EDGE('',*,*,#12086,.T.);
#18975=ORIENTED_EDGE('',*,*,#12749,.T.);
#18976=ORIENTED_EDGE('',*,*,#12083,.F.);
#18977=ORIENTED_EDGE('',*,*,#12747,.T.);
#18978=ORIENTED_EDGE('',*,*,#12024,.T.);
#18979=ORIENTED_EDGE('',*,*,#12755,.T.);
#18980=ORIENTED_EDGE('',*,*,#12021,.F.);
#18981=ORIENTED_EDGE('',*,*,#12753,.T.);
#18982=ORIENTED_EDGE('',*,*,#12762,.T.);
#18983=ORIENTED_EDGE('',*,*,#12763,.T.);
#18984=ORIENTED_EDGE('',*,*,#12721,.F.);
#18985=ORIENTED_EDGE('',*,*,#12764,.F.);
#18986=ORIENTED_EDGE('',*,*,#12765,.T.);
#18987=ORIENTED_EDGE('',*,*,#12764,.T.);
#18988=ORIENTED_EDGE('',*,*,#12720,.F.);
#18989=ORIENTED_EDGE('',*,*,#12766,.F.);
#18990=ORIENTED_EDGE('',*,*,#12767,.T.);
#18991=ORIENTED_EDGE('',*,*,#12766,.T.);
#18992=ORIENTED_EDGE('',*,*,#12719,.F.);
#18993=ORIENTED_EDGE('',*,*,#12768,.F.);
#18994=ORIENTED_EDGE('',*,*,#12769,.T.);
#18995=ORIENTED_EDGE('',*,*,#12768,.T.);
#18996=ORIENTED_EDGE('',*,*,#12718,.F.);
#18997=ORIENTED_EDGE('',*,*,#12763,.F.);
#18998=ORIENTED_EDGE('',*,*,#12769,.F.);
#18999=ORIENTED_EDGE('',*,*,#12762,.F.);
#19000=ORIENTED_EDGE('',*,*,#12765,.F.);
#19001=ORIENTED_EDGE('',*,*,#12767,.F.);
#19002=ORIENTED_EDGE('',*,*,#12712,.T.);
#19003=ORIENTED_EDGE('',*,*,#12092,.T.);
#19004=ORIENTED_EDGE('',*,*,#12715,.T.);
#19005=ORIENTED_EDGE('',*,*,#12650,.T.);
#19006=ORIENTED_EDGE('',*,*,#12734,.T.);
#19007=ORIENTED_EDGE('',*,*,#12216,.T.);
#19008=ORIENTED_EDGE('',*,*,#12736,.T.);
#19009=ORIENTED_EDGE('',*,*,#12588,.T.);
#19010=ORIENTED_EDGE('',*,*,#12740,.T.);
#19011=ORIENTED_EDGE('',*,*,#12154,.T.);
#19012=ORIENTED_EDGE('',*,*,#12742,.T.);
#19013=ORIENTED_EDGE('',*,*,#12526,.T.);
#19014=ORIENTED_EDGE('',*,*,#12746,.T.);
#19015=ORIENTED_EDGE('',*,*,#12030,.T.);
#19016=ORIENTED_EDGE('',*,*,#12748,.T.);
#19017=ORIENTED_EDGE('',*,*,#12464,.T.);
#19018=ORIENTED_EDGE('',*,*,#12752,.T.);
#19019=ORIENTED_EDGE('',*,*,#11968,.T.);
#19020=ORIENTED_EDGE('',*,*,#12754,.T.);
#19021=ORIENTED_EDGE('',*,*,#12402,.T.);
#19022=ORIENTED_EDGE('',*,*,#12758,.T.);
#19023=ORIENTED_EDGE('',*,*,#12278,.T.);
#19024=ORIENTED_EDGE('',*,*,#12760,.T.);
#19025=ORIENTED_EDGE('',*,*,#12340,.T.);
#19026=ORIENTED_EDGE('',*,*,#12770,.F.);
#19027=ORIENTED_EDGE('',*,*,#12771,.T.);
#19028=ORIENTED_EDGE('',*,*,#12772,.T.);
#19029=ORIENTED_EDGE('',*,*,#12773,.T.);
#19030=ORIENTED_EDGE('',*,*,#12774,.F.);
#19031=ORIENTED_EDGE('',*,*,#12775,.T.);
#19032=ORIENTED_EDGE('',*,*,#12770,.T.);
#19033=ORIENTED_EDGE('',*,*,#12776,.T.);
#19034=ORIENTED_EDGE('',*,*,#12777,.F.);
#19035=ORIENTED_EDGE('',*,*,#12778,.T.);
#19036=ORIENTED_EDGE('',*,*,#12774,.T.);
#19037=ORIENTED_EDGE('',*,*,#12779,.T.);
#19038=ORIENTED_EDGE('',*,*,#12780,.F.);
#19039=ORIENTED_EDGE('',*,*,#12781,.T.);
#19040=ORIENTED_EDGE('',*,*,#12777,.T.);
#19041=ORIENTED_EDGE('',*,*,#12782,.T.);
#19042=ORIENTED_EDGE('',*,*,#12783,.F.);
#19043=ORIENTED_EDGE('',*,*,#12784,.T.);
#19044=ORIENTED_EDGE('',*,*,#12780,.T.);
#19045=ORIENTED_EDGE('',*,*,#12785,.T.);
#19046=ORIENTED_EDGE('',*,*,#12786,.F.);
#19047=ORIENTED_EDGE('',*,*,#12787,.T.);
#19048=ORIENTED_EDGE('',*,*,#12783,.T.);
#19049=ORIENTED_EDGE('',*,*,#12788,.T.);
#19050=ORIENTED_EDGE('',*,*,#12789,.F.);
#19051=ORIENTED_EDGE('',*,*,#12790,.T.);
#19052=ORIENTED_EDGE('',*,*,#12786,.T.);
#19053=ORIENTED_EDGE('',*,*,#12791,.T.);
#19054=ORIENTED_EDGE('',*,*,#12792,.F.);
#19055=ORIENTED_EDGE('',*,*,#12793,.T.);
#19056=ORIENTED_EDGE('',*,*,#12789,.T.);
#19057=ORIENTED_EDGE('',*,*,#12794,.T.);
#19058=ORIENTED_EDGE('',*,*,#12795,.F.);
#19059=ORIENTED_EDGE('',*,*,#12796,.T.);
#19060=ORIENTED_EDGE('',*,*,#12792,.T.);
#19061=ORIENTED_EDGE('',*,*,#12797,.T.);
#19062=ORIENTED_EDGE('',*,*,#12798,.F.);
#19063=ORIENTED_EDGE('',*,*,#12799,.T.);
#19064=ORIENTED_EDGE('',*,*,#12795,.T.);
#19065=ORIENTED_EDGE('',*,*,#12800,.T.);
#19066=ORIENTED_EDGE('',*,*,#12801,.F.);
#19067=ORIENTED_EDGE('',*,*,#12802,.T.);
#19068=ORIENTED_EDGE('',*,*,#12798,.T.);
#19069=ORIENTED_EDGE('',*,*,#12803,.T.);
#19070=ORIENTED_EDGE('',*,*,#12804,.F.);
#19071=ORIENTED_EDGE('',*,*,#12805,.T.);
#19072=ORIENTED_EDGE('',*,*,#12801,.T.);
#19073=ORIENTED_EDGE('',*,*,#12806,.T.);
#19074=ORIENTED_EDGE('',*,*,#12807,.F.);
#19075=ORIENTED_EDGE('',*,*,#12808,.T.);
#19076=ORIENTED_EDGE('',*,*,#12804,.T.);
#19077=ORIENTED_EDGE('',*,*,#12809,.T.);
#19078=ORIENTED_EDGE('',*,*,#12810,.F.);
#19079=ORIENTED_EDGE('',*,*,#12811,.T.);
#19080=ORIENTED_EDGE('',*,*,#12807,.T.);
#19081=ORIENTED_EDGE('',*,*,#12812,.T.);
#19082=ORIENTED_EDGE('',*,*,#12813,.F.);
#19083=ORIENTED_EDGE('',*,*,#12814,.T.);
#19084=ORIENTED_EDGE('',*,*,#12810,.T.);
#19085=ORIENTED_EDGE('',*,*,#12815,.T.);
#19086=ORIENTED_EDGE('',*,*,#12816,.F.);
#19087=ORIENTED_EDGE('',*,*,#12817,.T.);
#19088=ORIENTED_EDGE('',*,*,#12813,.T.);
#19089=ORIENTED_EDGE('',*,*,#12818,.T.);
#19090=ORIENTED_EDGE('',*,*,#12819,.F.);
#19091=ORIENTED_EDGE('',*,*,#12820,.T.);
#19092=ORIENTED_EDGE('',*,*,#12816,.T.);
#19093=ORIENTED_EDGE('',*,*,#12821,.T.);
#19094=ORIENTED_EDGE('',*,*,#12822,.F.);
#19095=ORIENTED_EDGE('',*,*,#12823,.T.);
#19096=ORIENTED_EDGE('',*,*,#12819,.T.);
#19097=ORIENTED_EDGE('',*,*,#12824,.T.);
#19098=ORIENTED_EDGE('',*,*,#12825,.F.);
#19099=ORIENTED_EDGE('',*,*,#12826,.T.);
#19100=ORIENTED_EDGE('',*,*,#12822,.T.);
#19101=ORIENTED_EDGE('',*,*,#12827,.T.);
#19102=ORIENTED_EDGE('',*,*,#12828,.F.);
#19103=ORIENTED_EDGE('',*,*,#12829,.T.);
#19104=ORIENTED_EDGE('',*,*,#12825,.T.);
#19105=ORIENTED_EDGE('',*,*,#12830,.T.);
#19106=ORIENTED_EDGE('',*,*,#12831,.F.);
#19107=ORIENTED_EDGE('',*,*,#12832,.T.);
#19108=ORIENTED_EDGE('',*,*,#12828,.T.);
#19109=ORIENTED_EDGE('',*,*,#12833,.T.);
#19110=ORIENTED_EDGE('',*,*,#12834,.F.);
#19111=ORIENTED_EDGE('',*,*,#12835,.T.);
#19112=ORIENTED_EDGE('',*,*,#12831,.T.);
#19113=ORIENTED_EDGE('',*,*,#12836,.T.);
#19114=ORIENTED_EDGE('',*,*,#12837,.F.);
#19115=ORIENTED_EDGE('',*,*,#12838,.T.);
#19116=ORIENTED_EDGE('',*,*,#12834,.T.);
#19117=ORIENTED_EDGE('',*,*,#12839,.T.);
#19118=ORIENTED_EDGE('',*,*,#12840,.F.);
#19119=ORIENTED_EDGE('',*,*,#12841,.T.);
#19120=ORIENTED_EDGE('',*,*,#12837,.T.);
#19121=ORIENTED_EDGE('',*,*,#12842,.T.);
#19122=ORIENTED_EDGE('',*,*,#12843,.F.);
#19123=ORIENTED_EDGE('',*,*,#12844,.T.);
#19124=ORIENTED_EDGE('',*,*,#12840,.T.);
#19125=ORIENTED_EDGE('',*,*,#12845,.T.);
#19126=ORIENTED_EDGE('',*,*,#12846,.F.);
#19127=ORIENTED_EDGE('',*,*,#12847,.T.);
#19128=ORIENTED_EDGE('',*,*,#12843,.T.);
#19129=ORIENTED_EDGE('',*,*,#12848,.T.);
#19130=ORIENTED_EDGE('',*,*,#12849,.F.);
#19131=ORIENTED_EDGE('',*,*,#12850,.T.);
#19132=ORIENTED_EDGE('',*,*,#12846,.T.);
#19133=ORIENTED_EDGE('',*,*,#12851,.T.);
#19134=ORIENTED_EDGE('',*,*,#12852,.F.);
#19135=ORIENTED_EDGE('',*,*,#12853,.T.);
#19136=ORIENTED_EDGE('',*,*,#12849,.T.);
#19137=ORIENTED_EDGE('',*,*,#12854,.T.);
#19138=ORIENTED_EDGE('',*,*,#12855,.F.);
#19139=ORIENTED_EDGE('',*,*,#12856,.T.);
#19140=ORIENTED_EDGE('',*,*,#12852,.T.);
#19141=ORIENTED_EDGE('',*,*,#12857,.T.);
#19142=ORIENTED_EDGE('',*,*,#12858,.F.);
#19143=ORIENTED_EDGE('',*,*,#12859,.T.);
#19144=ORIENTED_EDGE('',*,*,#12855,.T.);
#19145=ORIENTED_EDGE('',*,*,#12860,.T.);
#19146=ORIENTED_EDGE('',*,*,#12861,.F.);
#19147=ORIENTED_EDGE('',*,*,#12862,.T.);
#19148=ORIENTED_EDGE('',*,*,#12858,.T.);
#19149=ORIENTED_EDGE('',*,*,#12863,.T.);
#19150=ORIENTED_EDGE('',*,*,#12864,.F.);
#19151=ORIENTED_EDGE('',*,*,#12865,.T.);
#19152=ORIENTED_EDGE('',*,*,#12861,.T.);
#19153=ORIENTED_EDGE('',*,*,#12866,.T.);
#19154=ORIENTED_EDGE('',*,*,#12867,.F.);
#19155=ORIENTED_EDGE('',*,*,#12868,.T.);
#19156=ORIENTED_EDGE('',*,*,#12864,.T.);
#19157=ORIENTED_EDGE('',*,*,#12869,.T.);
#19158=ORIENTED_EDGE('',*,*,#12870,.F.);
#19159=ORIENTED_EDGE('',*,*,#12871,.T.);
#19160=ORIENTED_EDGE('',*,*,#12867,.T.);
#19161=ORIENTED_EDGE('',*,*,#12872,.T.);
#19162=ORIENTED_EDGE('',*,*,#12873,.F.);
#19163=ORIENTED_EDGE('',*,*,#12874,.T.);
#19164=ORIENTED_EDGE('',*,*,#12870,.T.);
#19165=ORIENTED_EDGE('',*,*,#12875,.T.);
#19166=ORIENTED_EDGE('',*,*,#12876,.F.);
#19167=ORIENTED_EDGE('',*,*,#12877,.T.);
#19168=ORIENTED_EDGE('',*,*,#12873,.T.);
#19169=ORIENTED_EDGE('',*,*,#12878,.T.);
#19170=ORIENTED_EDGE('',*,*,#12879,.F.);
#19171=ORIENTED_EDGE('',*,*,#12880,.T.);
#19172=ORIENTED_EDGE('',*,*,#12876,.T.);
#19173=ORIENTED_EDGE('',*,*,#12881,.T.);
#19174=ORIENTED_EDGE('',*,*,#12882,.F.);
#19175=ORIENTED_EDGE('',*,*,#12883,.T.);
#19176=ORIENTED_EDGE('',*,*,#12879,.T.);
#19177=ORIENTED_EDGE('',*,*,#12884,.T.);
#19178=ORIENTED_EDGE('',*,*,#12885,.F.);
#19179=ORIENTED_EDGE('',*,*,#12886,.T.);
#19180=ORIENTED_EDGE('',*,*,#12882,.T.);
#19181=ORIENTED_EDGE('',*,*,#12887,.T.);
#19182=ORIENTED_EDGE('',*,*,#12888,.F.);
#19183=ORIENTED_EDGE('',*,*,#12889,.T.);
#19184=ORIENTED_EDGE('',*,*,#12885,.T.);
#19185=ORIENTED_EDGE('',*,*,#12890,.T.);
#19186=ORIENTED_EDGE('',*,*,#12891,.F.);
#19187=ORIENTED_EDGE('',*,*,#12892,.T.);
#19188=ORIENTED_EDGE('',*,*,#12888,.T.);
#19189=ORIENTED_EDGE('',*,*,#12893,.T.);
#19190=ORIENTED_EDGE('',*,*,#12894,.F.);
#19191=ORIENTED_EDGE('',*,*,#12895,.T.);
#19192=ORIENTED_EDGE('',*,*,#12891,.T.);
#19193=ORIENTED_EDGE('',*,*,#12896,.T.);
#19194=ORIENTED_EDGE('',*,*,#12897,.F.);
#19195=ORIENTED_EDGE('',*,*,#12898,.T.);
#19196=ORIENTED_EDGE('',*,*,#12894,.T.);
#19197=ORIENTED_EDGE('',*,*,#12899,.T.);
#19198=ORIENTED_EDGE('',*,*,#12900,.F.);
#19199=ORIENTED_EDGE('',*,*,#12901,.T.);
#19200=ORIENTED_EDGE('',*,*,#12897,.T.);
#19201=ORIENTED_EDGE('',*,*,#12902,.T.);
#19202=ORIENTED_EDGE('',*,*,#12903,.F.);
#19203=ORIENTED_EDGE('',*,*,#12904,.T.);
#19204=ORIENTED_EDGE('',*,*,#12900,.T.);
#19205=ORIENTED_EDGE('',*,*,#12905,.T.);
#19206=ORIENTED_EDGE('',*,*,#12906,.F.);
#19207=ORIENTED_EDGE('',*,*,#12907,.T.);
#19208=ORIENTED_EDGE('',*,*,#12903,.T.);
#19209=ORIENTED_EDGE('',*,*,#12908,.T.);
#19210=ORIENTED_EDGE('',*,*,#12909,.F.);
#19211=ORIENTED_EDGE('',*,*,#12910,.T.);
#19212=ORIENTED_EDGE('',*,*,#12906,.T.);
#19213=ORIENTED_EDGE('',*,*,#12911,.T.);
#19214=ORIENTED_EDGE('',*,*,#12912,.F.);
#19215=ORIENTED_EDGE('',*,*,#12913,.T.);
#19216=ORIENTED_EDGE('',*,*,#12909,.T.);
#19217=ORIENTED_EDGE('',*,*,#12914,.T.);
#19218=ORIENTED_EDGE('',*,*,#12915,.F.);
#19219=ORIENTED_EDGE('',*,*,#12916,.T.);
#19220=ORIENTED_EDGE('',*,*,#12912,.T.);
#19221=ORIENTED_EDGE('',*,*,#12917,.T.);
#19222=ORIENTED_EDGE('',*,*,#12918,.F.);
#19223=ORIENTED_EDGE('',*,*,#12919,.T.);
#19224=ORIENTED_EDGE('',*,*,#12920,.T.);
#19225=ORIENTED_EDGE('',*,*,#12921,.F.);
#19226=ORIENTED_EDGE('',*,*,#12922,.F.);
#19227=ORIENTED_EDGE('',*,*,#12923,.T.);
#19228=ORIENTED_EDGE('',*,*,#12918,.T.);
#19229=ORIENTED_EDGE('',*,*,#12924,.F.);
#19230=ORIENTED_EDGE('',*,*,#12925,.F.);
#19231=ORIENTED_EDGE('',*,*,#12926,.T.);
#19232=ORIENTED_EDGE('',*,*,#12922,.T.);
#19233=ORIENTED_EDGE('',*,*,#12927,.F.);
#19234=ORIENTED_EDGE('',*,*,#12928,.F.);
#19235=ORIENTED_EDGE('',*,*,#12929,.T.);
#19236=ORIENTED_EDGE('',*,*,#12925,.T.);
#19237=ORIENTED_EDGE('',*,*,#12930,.F.);
#19238=ORIENTED_EDGE('',*,*,#12931,.F.);
#19239=ORIENTED_EDGE('',*,*,#12932,.T.);
#19240=ORIENTED_EDGE('',*,*,#12928,.T.);
#19241=ORIENTED_EDGE('',*,*,#12933,.F.);
#19242=ORIENTED_EDGE('',*,*,#12934,.F.);
#19243=ORIENTED_EDGE('',*,*,#12935,.T.);
#19244=ORIENTED_EDGE('',*,*,#12931,.T.);
#19245=ORIENTED_EDGE('',*,*,#12936,.F.);
#19246=ORIENTED_EDGE('',*,*,#12937,.F.);
#19247=ORIENTED_EDGE('',*,*,#12938,.T.);
#19248=ORIENTED_EDGE('',*,*,#12934,.T.);
#19249=ORIENTED_EDGE('',*,*,#12939,.F.);
#19250=ORIENTED_EDGE('',*,*,#12940,.F.);
#19251=ORIENTED_EDGE('',*,*,#12941,.T.);
#19252=ORIENTED_EDGE('',*,*,#12937,.T.);
#19253=ORIENTED_EDGE('',*,*,#12942,.F.);
#19254=ORIENTED_EDGE('',*,*,#12943,.F.);
#19255=ORIENTED_EDGE('',*,*,#12944,.T.);
#19256=ORIENTED_EDGE('',*,*,#12940,.T.);
#19257=ORIENTED_EDGE('',*,*,#12945,.F.);
#19258=ORIENTED_EDGE('',*,*,#12946,.F.);
#19259=ORIENTED_EDGE('',*,*,#12947,.T.);
#19260=ORIENTED_EDGE('',*,*,#12943,.T.);
#19261=ORIENTED_EDGE('',*,*,#12948,.F.);
#19262=ORIENTED_EDGE('',*,*,#12949,.F.);
#19263=ORIENTED_EDGE('',*,*,#12950,.T.);
#19264=ORIENTED_EDGE('',*,*,#12946,.T.);
#19265=ORIENTED_EDGE('',*,*,#12951,.F.);
#19266=ORIENTED_EDGE('',*,*,#12952,.F.);
#19267=ORIENTED_EDGE('',*,*,#12953,.T.);
#19268=ORIENTED_EDGE('',*,*,#12949,.T.);
#19269=ORIENTED_EDGE('',*,*,#12954,.F.);
#19270=ORIENTED_EDGE('',*,*,#12955,.F.);
#19271=ORIENTED_EDGE('',*,*,#12956,.T.);
#19272=ORIENTED_EDGE('',*,*,#12952,.T.);
#19273=ORIENTED_EDGE('',*,*,#12957,.F.);
#19274=ORIENTED_EDGE('',*,*,#12958,.F.);
#19275=ORIENTED_EDGE('',*,*,#12959,.T.);
#19276=ORIENTED_EDGE('',*,*,#12955,.T.);
#19277=ORIENTED_EDGE('',*,*,#12960,.F.);
#19278=ORIENTED_EDGE('',*,*,#12961,.F.);
#19279=ORIENTED_EDGE('',*,*,#12962,.T.);
#19280=ORIENTED_EDGE('',*,*,#12958,.T.);
#19281=ORIENTED_EDGE('',*,*,#12963,.F.);
#19282=ORIENTED_EDGE('',*,*,#12964,.F.);
#19283=ORIENTED_EDGE('',*,*,#12965,.T.);
#19284=ORIENTED_EDGE('',*,*,#12961,.T.);
#19285=ORIENTED_EDGE('',*,*,#12966,.F.);
#19286=ORIENTED_EDGE('',*,*,#12967,.F.);
#19287=ORIENTED_EDGE('',*,*,#12968,.T.);
#19288=ORIENTED_EDGE('',*,*,#12964,.T.);
#19289=ORIENTED_EDGE('',*,*,#12969,.F.);
#19290=ORIENTED_EDGE('',*,*,#12970,.F.);
#19291=ORIENTED_EDGE('',*,*,#12971,.T.);
#19292=ORIENTED_EDGE('',*,*,#12967,.T.);
#19293=ORIENTED_EDGE('',*,*,#12972,.F.);
#19294=ORIENTED_EDGE('',*,*,#12973,.F.);
#19295=ORIENTED_EDGE('',*,*,#12974,.T.);
#19296=ORIENTED_EDGE('',*,*,#12970,.T.);
#19297=ORIENTED_EDGE('',*,*,#12975,.F.);
#19298=ORIENTED_EDGE('',*,*,#12976,.F.);
#19299=ORIENTED_EDGE('',*,*,#12977,.T.);
#19300=ORIENTED_EDGE('',*,*,#12973,.T.);
#19301=ORIENTED_EDGE('',*,*,#12978,.F.);
#19302=ORIENTED_EDGE('',*,*,#12979,.F.);
#19303=ORIENTED_EDGE('',*,*,#12980,.T.);
#19304=ORIENTED_EDGE('',*,*,#12976,.T.);
#19305=ORIENTED_EDGE('',*,*,#12981,.F.);
#19306=ORIENTED_EDGE('',*,*,#12982,.F.);
#19307=ORIENTED_EDGE('',*,*,#12983,.T.);
#19308=ORIENTED_EDGE('',*,*,#12979,.T.);
#19309=ORIENTED_EDGE('',*,*,#12984,.F.);
#19310=ORIENTED_EDGE('',*,*,#12985,.F.);
#19311=ORIENTED_EDGE('',*,*,#12986,.T.);
#19312=ORIENTED_EDGE('',*,*,#12982,.T.);
#19313=ORIENTED_EDGE('',*,*,#12987,.F.);
#19314=ORIENTED_EDGE('',*,*,#12988,.F.);
#19315=ORIENTED_EDGE('',*,*,#12989,.T.);
#19316=ORIENTED_EDGE('',*,*,#12985,.T.);
#19317=ORIENTED_EDGE('',*,*,#12990,.F.);
#19318=ORIENTED_EDGE('',*,*,#12991,.F.);
#19319=ORIENTED_EDGE('',*,*,#12992,.T.);
#19320=ORIENTED_EDGE('',*,*,#12988,.T.);
#19321=ORIENTED_EDGE('',*,*,#12993,.F.);
#19322=ORIENTED_EDGE('',*,*,#12994,.F.);
#19323=ORIENTED_EDGE('',*,*,#12995,.T.);
#19324=ORIENTED_EDGE('',*,*,#12991,.T.);
#19325=ORIENTED_EDGE('',*,*,#12996,.F.);
#19326=ORIENTED_EDGE('',*,*,#12997,.F.);
#19327=ORIENTED_EDGE('',*,*,#12998,.T.);
#19328=ORIENTED_EDGE('',*,*,#12994,.T.);
#19329=ORIENTED_EDGE('',*,*,#12999,.F.);
#19330=ORIENTED_EDGE('',*,*,#13000,.F.);
#19331=ORIENTED_EDGE('',*,*,#13001,.T.);
#19332=ORIENTED_EDGE('',*,*,#12997,.T.);
#19333=ORIENTED_EDGE('',*,*,#13002,.F.);
#19334=ORIENTED_EDGE('',*,*,#13003,.F.);
#19335=ORIENTED_EDGE('',*,*,#13004,.T.);
#19336=ORIENTED_EDGE('',*,*,#13000,.T.);
#19337=ORIENTED_EDGE('',*,*,#13005,.F.);
#19338=ORIENTED_EDGE('',*,*,#13006,.F.);
#19339=ORIENTED_EDGE('',*,*,#13007,.T.);
#19340=ORIENTED_EDGE('',*,*,#13003,.T.);
#19341=ORIENTED_EDGE('',*,*,#13008,.F.);
#19342=ORIENTED_EDGE('',*,*,#13009,.F.);
#19343=ORIENTED_EDGE('',*,*,#13010,.T.);
#19344=ORIENTED_EDGE('',*,*,#13006,.T.);
#19345=ORIENTED_EDGE('',*,*,#13011,.F.);
#19346=ORIENTED_EDGE('',*,*,#13012,.F.);
#19347=ORIENTED_EDGE('',*,*,#13013,.T.);
#19348=ORIENTED_EDGE('',*,*,#13009,.T.);
#19349=ORIENTED_EDGE('',*,*,#13014,.F.);
#19350=ORIENTED_EDGE('',*,*,#13015,.F.);
#19351=ORIENTED_EDGE('',*,*,#13016,.T.);
#19352=ORIENTED_EDGE('',*,*,#13012,.T.);
#19353=ORIENTED_EDGE('',*,*,#13017,.F.);
#19354=ORIENTED_EDGE('',*,*,#13018,.F.);
#19355=ORIENTED_EDGE('',*,*,#13019,.T.);
#19356=ORIENTED_EDGE('',*,*,#13015,.T.);
#19357=ORIENTED_EDGE('',*,*,#13020,.F.);
#19358=ORIENTED_EDGE('',*,*,#13021,.F.);
#19359=ORIENTED_EDGE('',*,*,#13022,.T.);
#19360=ORIENTED_EDGE('',*,*,#13018,.T.);
#19361=ORIENTED_EDGE('',*,*,#13023,.F.);
#19362=ORIENTED_EDGE('',*,*,#13024,.F.);
#19363=ORIENTED_EDGE('',*,*,#13025,.T.);
#19364=ORIENTED_EDGE('',*,*,#13021,.T.);
#19365=ORIENTED_EDGE('',*,*,#13026,.F.);
#19366=ORIENTED_EDGE('',*,*,#13027,.F.);
#19367=ORIENTED_EDGE('',*,*,#13028,.T.);
#19368=ORIENTED_EDGE('',*,*,#13024,.T.);
#19369=ORIENTED_EDGE('',*,*,#13029,.F.);
#19370=ORIENTED_EDGE('',*,*,#13030,.F.);
#19371=ORIENTED_EDGE('',*,*,#13031,.T.);
#19372=ORIENTED_EDGE('',*,*,#13027,.T.);
#19373=ORIENTED_EDGE('',*,*,#13032,.F.);
#19374=ORIENTED_EDGE('',*,*,#13033,.F.);
#19375=ORIENTED_EDGE('',*,*,#13034,.T.);
#19376=ORIENTED_EDGE('',*,*,#13030,.T.);
#19377=ORIENTED_EDGE('',*,*,#13035,.F.);
#19378=ORIENTED_EDGE('',*,*,#13036,.F.);
#19379=ORIENTED_EDGE('',*,*,#13037,.T.);
#19380=ORIENTED_EDGE('',*,*,#13033,.T.);
#19381=ORIENTED_EDGE('',*,*,#13038,.F.);
#19382=ORIENTED_EDGE('',*,*,#13039,.F.);
#19383=ORIENTED_EDGE('',*,*,#13040,.T.);
#19384=ORIENTED_EDGE('',*,*,#13036,.T.);
#19385=ORIENTED_EDGE('',*,*,#13041,.F.);
#19386=ORIENTED_EDGE('',*,*,#13042,.F.);
#19387=ORIENTED_EDGE('',*,*,#13043,.T.);
#19388=ORIENTED_EDGE('',*,*,#13039,.T.);
#19389=ORIENTED_EDGE('',*,*,#13044,.F.);
#19390=ORIENTED_EDGE('',*,*,#13045,.F.);
#19391=ORIENTED_EDGE('',*,*,#13046,.T.);
#19392=ORIENTED_EDGE('',*,*,#13042,.T.);
#19393=ORIENTED_EDGE('',*,*,#13047,.F.);
#19394=ORIENTED_EDGE('',*,*,#13048,.F.);
#19395=ORIENTED_EDGE('',*,*,#13049,.T.);
#19396=ORIENTED_EDGE('',*,*,#13045,.T.);
#19397=ORIENTED_EDGE('',*,*,#13050,.F.);
#19398=ORIENTED_EDGE('',*,*,#13051,.F.);
#19399=ORIENTED_EDGE('',*,*,#13052,.T.);
#19400=ORIENTED_EDGE('',*,*,#13048,.T.);
#19401=ORIENTED_EDGE('',*,*,#13053,.F.);
#19402=ORIENTED_EDGE('',*,*,#13054,.F.);
#19403=ORIENTED_EDGE('',*,*,#13055,.T.);
#19404=ORIENTED_EDGE('',*,*,#13051,.T.);
#19405=ORIENTED_EDGE('',*,*,#13056,.F.);
#19406=ORIENTED_EDGE('',*,*,#13057,.F.);
#19407=ORIENTED_EDGE('',*,*,#13058,.T.);
#19408=ORIENTED_EDGE('',*,*,#13054,.T.);
#19409=ORIENTED_EDGE('',*,*,#13059,.F.);
#19410=ORIENTED_EDGE('',*,*,#13060,.F.);
#19411=ORIENTED_EDGE('',*,*,#13061,.T.);
#19412=ORIENTED_EDGE('',*,*,#13057,.T.);
#19413=ORIENTED_EDGE('',*,*,#13062,.F.);
#19414=ORIENTED_EDGE('',*,*,#13063,.F.);
#19415=ORIENTED_EDGE('',*,*,#13064,.T.);
#19416=ORIENTED_EDGE('',*,*,#13060,.T.);
#19417=ORIENTED_EDGE('',*,*,#13065,.F.);
#19418=ORIENTED_EDGE('',*,*,#13066,.F.);
#19419=ORIENTED_EDGE('',*,*,#12920,.F.);
#19420=ORIENTED_EDGE('',*,*,#13067,.F.);
#19421=ORIENTED_EDGE('',*,*,#13068,.F.);
#19422=ORIENTED_EDGE('',*,*,#13069,.F.);
#19423=ORIENTED_EDGE('',*,*,#13070,.T.);
#19424=ORIENTED_EDGE('',*,*,#13071,.F.);
#19425=ORIENTED_EDGE('',*,*,#13070,.F.);
#19426=ORIENTED_EDGE('',*,*,#13067,.T.);
#19427=ORIENTED_EDGE('',*,*,#12919,.F.);
#19428=ORIENTED_EDGE('',*,*,#12923,.F.);
#19429=ORIENTED_EDGE('',*,*,#12926,.F.);
#19430=ORIENTED_EDGE('',*,*,#12929,.F.);
#19431=ORIENTED_EDGE('',*,*,#12932,.F.);
#19432=ORIENTED_EDGE('',*,*,#12935,.F.);
#19433=ORIENTED_EDGE('',*,*,#12938,.F.);
#19434=ORIENTED_EDGE('',*,*,#12941,.F.);
#19435=ORIENTED_EDGE('',*,*,#12944,.F.);
#19436=ORIENTED_EDGE('',*,*,#12947,.F.);
#19437=ORIENTED_EDGE('',*,*,#12950,.F.);
#19438=ORIENTED_EDGE('',*,*,#12953,.F.);
#19439=ORIENTED_EDGE('',*,*,#12956,.F.);
#19440=ORIENTED_EDGE('',*,*,#12959,.F.);
#19441=ORIENTED_EDGE('',*,*,#12962,.F.);
#19442=ORIENTED_EDGE('',*,*,#12965,.F.);
#19443=ORIENTED_EDGE('',*,*,#12968,.F.);
#19444=ORIENTED_EDGE('',*,*,#12971,.F.);
#19445=ORIENTED_EDGE('',*,*,#12974,.F.);
#19446=ORIENTED_EDGE('',*,*,#12977,.F.);
#19447=ORIENTED_EDGE('',*,*,#12980,.F.);
#19448=ORIENTED_EDGE('',*,*,#12983,.F.);
#19449=ORIENTED_EDGE('',*,*,#12986,.F.);
#19450=ORIENTED_EDGE('',*,*,#12989,.F.);
#19451=ORIENTED_EDGE('',*,*,#12992,.F.);
#19452=ORIENTED_EDGE('',*,*,#12995,.F.);
#19453=ORIENTED_EDGE('',*,*,#12998,.F.);
#19454=ORIENTED_EDGE('',*,*,#13001,.F.);
#19455=ORIENTED_EDGE('',*,*,#13004,.F.);
#19456=ORIENTED_EDGE('',*,*,#13007,.F.);
#19457=ORIENTED_EDGE('',*,*,#13010,.F.);
#19458=ORIENTED_EDGE('',*,*,#13013,.F.);
#19459=ORIENTED_EDGE('',*,*,#13016,.F.);
#19460=ORIENTED_EDGE('',*,*,#13019,.F.);
#19461=ORIENTED_EDGE('',*,*,#13022,.F.);
#19462=ORIENTED_EDGE('',*,*,#13025,.F.);
#19463=ORIENTED_EDGE('',*,*,#13028,.F.);
#19464=ORIENTED_EDGE('',*,*,#13031,.F.);
#19465=ORIENTED_EDGE('',*,*,#13034,.F.);
#19466=ORIENTED_EDGE('',*,*,#13037,.F.);
#19467=ORIENTED_EDGE('',*,*,#13040,.F.);
#19468=ORIENTED_EDGE('',*,*,#13043,.F.);
#19469=ORIENTED_EDGE('',*,*,#13046,.F.);
#19470=ORIENTED_EDGE('',*,*,#13049,.F.);
#19471=ORIENTED_EDGE('',*,*,#13052,.F.);
#19472=ORIENTED_EDGE('',*,*,#13055,.F.);
#19473=ORIENTED_EDGE('',*,*,#13058,.F.);
#19474=ORIENTED_EDGE('',*,*,#13061,.F.);
#19475=ORIENTED_EDGE('',*,*,#13064,.F.);
#19476=ORIENTED_EDGE('',*,*,#13072,.F.);
#19477=ORIENTED_EDGE('',*,*,#13073,.F.);
#19478=ORIENTED_EDGE('',*,*,#12771,.F.);
#19479=ORIENTED_EDGE('',*,*,#12775,.F.);
#19480=ORIENTED_EDGE('',*,*,#12778,.F.);
#19481=ORIENTED_EDGE('',*,*,#12781,.F.);
#19482=ORIENTED_EDGE('',*,*,#12784,.F.);
#19483=ORIENTED_EDGE('',*,*,#12787,.F.);
#19484=ORIENTED_EDGE('',*,*,#12790,.F.);
#19485=ORIENTED_EDGE('',*,*,#12793,.F.);
#19486=ORIENTED_EDGE('',*,*,#12796,.F.);
#19487=ORIENTED_EDGE('',*,*,#12799,.F.);
#19488=ORIENTED_EDGE('',*,*,#12802,.F.);
#19489=ORIENTED_EDGE('',*,*,#12805,.F.);
#19490=ORIENTED_EDGE('',*,*,#12808,.F.);
#19491=ORIENTED_EDGE('',*,*,#12811,.F.);
#19492=ORIENTED_EDGE('',*,*,#12814,.F.);
#19493=ORIENTED_EDGE('',*,*,#12817,.F.);
#19494=ORIENTED_EDGE('',*,*,#12820,.F.);
#19495=ORIENTED_EDGE('',*,*,#12823,.F.);
#19496=ORIENTED_EDGE('',*,*,#12826,.F.);
#19497=ORIENTED_EDGE('',*,*,#12829,.F.);
#19498=ORIENTED_EDGE('',*,*,#12832,.F.);
#19499=ORIENTED_EDGE('',*,*,#12835,.F.);
#19500=ORIENTED_EDGE('',*,*,#12838,.F.);
#19501=ORIENTED_EDGE('',*,*,#12841,.F.);
#19502=ORIENTED_EDGE('',*,*,#12844,.F.);
#19503=ORIENTED_EDGE('',*,*,#12847,.F.);
#19504=ORIENTED_EDGE('',*,*,#12850,.F.);
#19505=ORIENTED_EDGE('',*,*,#12853,.F.);
#19506=ORIENTED_EDGE('',*,*,#12856,.F.);
#19507=ORIENTED_EDGE('',*,*,#12859,.F.);
#19508=ORIENTED_EDGE('',*,*,#12862,.F.);
#19509=ORIENTED_EDGE('',*,*,#12865,.F.);
#19510=ORIENTED_EDGE('',*,*,#12868,.F.);
#19511=ORIENTED_EDGE('',*,*,#12871,.F.);
#19512=ORIENTED_EDGE('',*,*,#12874,.F.);
#19513=ORIENTED_EDGE('',*,*,#12877,.F.);
#19514=ORIENTED_EDGE('',*,*,#12880,.F.);
#19515=ORIENTED_EDGE('',*,*,#12883,.F.);
#19516=ORIENTED_EDGE('',*,*,#12886,.F.);
#19517=ORIENTED_EDGE('',*,*,#12889,.F.);
#19518=ORIENTED_EDGE('',*,*,#12892,.F.);
#19519=ORIENTED_EDGE('',*,*,#12895,.F.);
#19520=ORIENTED_EDGE('',*,*,#12898,.F.);
#19521=ORIENTED_EDGE('',*,*,#12901,.F.);
#19522=ORIENTED_EDGE('',*,*,#12904,.F.);
#19523=ORIENTED_EDGE('',*,*,#12907,.F.);
#19524=ORIENTED_EDGE('',*,*,#12910,.F.);
#19525=ORIENTED_EDGE('',*,*,#12913,.F.);
#19526=ORIENTED_EDGE('',*,*,#12916,.F.);
#19527=ORIENTED_EDGE('',*,*,#13074,.F.);
#19528=ORIENTED_EDGE('',*,*,#13063,.T.);
#19529=ORIENTED_EDGE('',*,*,#13075,.F.);
#19530=ORIENTED_EDGE('',*,*,#13076,.F.);
#19531=ORIENTED_EDGE('',*,*,#13072,.T.);
#19532=ORIENTED_EDGE('',*,*,#13066,.T.);
#19533=ORIENTED_EDGE('',*,*,#13069,.T.);
#19534=ORIENTED_EDGE('',*,*,#13077,.F.);
#19535=ORIENTED_EDGE('',*,*,#12917,.F.);
#19536=ORIENTED_EDGE('',*,*,#12914,.F.);
#19537=ORIENTED_EDGE('',*,*,#12911,.F.);
#19538=ORIENTED_EDGE('',*,*,#12908,.F.);
#19539=ORIENTED_EDGE('',*,*,#12905,.F.);
#19540=ORIENTED_EDGE('',*,*,#12902,.F.);
#19541=ORIENTED_EDGE('',*,*,#12899,.F.);
#19542=ORIENTED_EDGE('',*,*,#12896,.F.);
#19543=ORIENTED_EDGE('',*,*,#12893,.F.);
#19544=ORIENTED_EDGE('',*,*,#12890,.F.);
#19545=ORIENTED_EDGE('',*,*,#12887,.F.);
#19546=ORIENTED_EDGE('',*,*,#12884,.F.);
#19547=ORIENTED_EDGE('',*,*,#12881,.F.);
#19548=ORIENTED_EDGE('',*,*,#12878,.F.);
#19549=ORIENTED_EDGE('',*,*,#12875,.F.);
#19550=ORIENTED_EDGE('',*,*,#12872,.F.);
#19551=ORIENTED_EDGE('',*,*,#12869,.F.);
#19552=ORIENTED_EDGE('',*,*,#12866,.F.);
#19553=ORIENTED_EDGE('',*,*,#12863,.F.);
#19554=ORIENTED_EDGE('',*,*,#12860,.F.);
#19555=ORIENTED_EDGE('',*,*,#12857,.F.);
#19556=ORIENTED_EDGE('',*,*,#12854,.F.);
#19557=ORIENTED_EDGE('',*,*,#12851,.F.);
#19558=ORIENTED_EDGE('',*,*,#12848,.F.);
#19559=ORIENTED_EDGE('',*,*,#12845,.F.);
#19560=ORIENTED_EDGE('',*,*,#12842,.F.);
#19561=ORIENTED_EDGE('',*,*,#12839,.F.);
#19562=ORIENTED_EDGE('',*,*,#12836,.F.);
#19563=ORIENTED_EDGE('',*,*,#12833,.F.);
#19564=ORIENTED_EDGE('',*,*,#12830,.F.);
#19565=ORIENTED_EDGE('',*,*,#12827,.F.);
#19566=ORIENTED_EDGE('',*,*,#12824,.F.);
#19567=ORIENTED_EDGE('',*,*,#12821,.F.);
#19568=ORIENTED_EDGE('',*,*,#12818,.F.);
#19569=ORIENTED_EDGE('',*,*,#12815,.F.);
#19570=ORIENTED_EDGE('',*,*,#12812,.F.);
#19571=ORIENTED_EDGE('',*,*,#12809,.F.);
#19572=ORIENTED_EDGE('',*,*,#12806,.F.);
#19573=ORIENTED_EDGE('',*,*,#12803,.F.);
#19574=ORIENTED_EDGE('',*,*,#12800,.F.);
#19575=ORIENTED_EDGE('',*,*,#12797,.F.);
#19576=ORIENTED_EDGE('',*,*,#12794,.F.);
#19577=ORIENTED_EDGE('',*,*,#12791,.F.);
#19578=ORIENTED_EDGE('',*,*,#12788,.F.);
#19579=ORIENTED_EDGE('',*,*,#12785,.F.);
#19580=ORIENTED_EDGE('',*,*,#12782,.F.);
#19581=ORIENTED_EDGE('',*,*,#12779,.F.);
#19582=ORIENTED_EDGE('',*,*,#12776,.F.);
#19583=ORIENTED_EDGE('',*,*,#12773,.F.);
#19584=ORIENTED_EDGE('',*,*,#13078,.F.);
#19585=ORIENTED_EDGE('',*,*,#13075,.T.);
#19586=ORIENTED_EDGE('',*,*,#13065,.T.);
#19587=ORIENTED_EDGE('',*,*,#13062,.T.);
#19588=ORIENTED_EDGE('',*,*,#13059,.T.);
#19589=ORIENTED_EDGE('',*,*,#13056,.T.);
#19590=ORIENTED_EDGE('',*,*,#13053,.T.);
#19591=ORIENTED_EDGE('',*,*,#13050,.T.);
#19592=ORIENTED_EDGE('',*,*,#13047,.T.);
#19593=ORIENTED_EDGE('',*,*,#13044,.T.);
#19594=ORIENTED_EDGE('',*,*,#13041,.T.);
#19595=ORIENTED_EDGE('',*,*,#13038,.T.);
#19596=ORIENTED_EDGE('',*,*,#13035,.T.);
#19597=ORIENTED_EDGE('',*,*,#13032,.T.);
#19598=ORIENTED_EDGE('',*,*,#13029,.T.);
#19599=ORIENTED_EDGE('',*,*,#13026,.T.);
#19600=ORIENTED_EDGE('',*,*,#13023,.T.);
#19601=ORIENTED_EDGE('',*,*,#13020,.T.);
#19602=ORIENTED_EDGE('',*,*,#13017,.T.);
#19603=ORIENTED_EDGE('',*,*,#13014,.T.);
#19604=ORIENTED_EDGE('',*,*,#13011,.T.);
#19605=ORIENTED_EDGE('',*,*,#13008,.T.);
#19606=ORIENTED_EDGE('',*,*,#13005,.T.);
#19607=ORIENTED_EDGE('',*,*,#13002,.T.);
#19608=ORIENTED_EDGE('',*,*,#12999,.T.);
#19609=ORIENTED_EDGE('',*,*,#12996,.T.);
#19610=ORIENTED_EDGE('',*,*,#12993,.T.);
#19611=ORIENTED_EDGE('',*,*,#12990,.T.);
#19612=ORIENTED_EDGE('',*,*,#12987,.T.);
#19613=ORIENTED_EDGE('',*,*,#12984,.T.);
#19614=ORIENTED_EDGE('',*,*,#12981,.T.);
#19615=ORIENTED_EDGE('',*,*,#12978,.T.);
#19616=ORIENTED_EDGE('',*,*,#12975,.T.);
#19617=ORIENTED_EDGE('',*,*,#12972,.T.);
#19618=ORIENTED_EDGE('',*,*,#12969,.T.);
#19619=ORIENTED_EDGE('',*,*,#12966,.T.);
#19620=ORIENTED_EDGE('',*,*,#12963,.T.);
#19621=ORIENTED_EDGE('',*,*,#12960,.T.);
#19622=ORIENTED_EDGE('',*,*,#12957,.T.);
#19623=ORIENTED_EDGE('',*,*,#12954,.T.);
#19624=ORIENTED_EDGE('',*,*,#12951,.T.);
#19625=ORIENTED_EDGE('',*,*,#12948,.T.);
#19626=ORIENTED_EDGE('',*,*,#12945,.T.);
#19627=ORIENTED_EDGE('',*,*,#12942,.T.);
#19628=ORIENTED_EDGE('',*,*,#12939,.T.);
#19629=ORIENTED_EDGE('',*,*,#12936,.T.);
#19630=ORIENTED_EDGE('',*,*,#12933,.T.);
#19631=ORIENTED_EDGE('',*,*,#12930,.T.);
#19632=ORIENTED_EDGE('',*,*,#12927,.T.);
#19633=ORIENTED_EDGE('',*,*,#12924,.T.);
#19634=ORIENTED_EDGE('',*,*,#12921,.T.);
#19635=ORIENTED_EDGE('',*,*,#12915,.T.);
#19636=ORIENTED_EDGE('',*,*,#13077,.T.);
#19637=ORIENTED_EDGE('',*,*,#13068,.T.);
#19638=ORIENTED_EDGE('',*,*,#13074,.T.);
#19639=ORIENTED_EDGE('',*,*,#13079,.F.);
#19640=ORIENTED_EDGE('',*,*,#13080,.T.);
#19641=ORIENTED_EDGE('',*,*,#13081,.T.);
#19642=ORIENTED_EDGE('',*,*,#13082,.F.);
#19643=ORIENTED_EDGE('',*,*,#13083,.F.);
#19644=ORIENTED_EDGE('',*,*,#13084,.T.);
#19645=ORIENTED_EDGE('',*,*,#13085,.T.);
#19646=ORIENTED_EDGE('',*,*,#13080,.F.);
#19647=ORIENTED_EDGE('',*,*,#13086,.F.);
#19648=ORIENTED_EDGE('',*,*,#13087,.T.);
#19649=ORIENTED_EDGE('',*,*,#13088,.T.);
#19650=ORIENTED_EDGE('',*,*,#13084,.F.);
#19651=ORIENTED_EDGE('',*,*,#13089,.F.);
#19652=ORIENTED_EDGE('',*,*,#13090,.T.);
#19653=ORIENTED_EDGE('',*,*,#13091,.T.);
#19654=ORIENTED_EDGE('',*,*,#13087,.F.);
#19655=ORIENTED_EDGE('',*,*,#13092,.F.);
#19656=ORIENTED_EDGE('',*,*,#13093,.T.);
#19657=ORIENTED_EDGE('',*,*,#13094,.T.);
#19658=ORIENTED_EDGE('',*,*,#13090,.F.);
#19659=ORIENTED_EDGE('',*,*,#13095,.F.);
#19660=ORIENTED_EDGE('',*,*,#13082,.T.);
#19661=ORIENTED_EDGE('',*,*,#13096,.T.);
#19662=ORIENTED_EDGE('',*,*,#13093,.F.);
#19663=ORIENTED_EDGE('',*,*,#13096,.F.);
#19664=ORIENTED_EDGE('',*,*,#13081,.F.);
#19665=ORIENTED_EDGE('',*,*,#13085,.F.);
#19666=ORIENTED_EDGE('',*,*,#13088,.F.);
#19667=ORIENTED_EDGE('',*,*,#13091,.F.);
#19668=ORIENTED_EDGE('',*,*,#13094,.F.);
#19669=ORIENTED_EDGE('',*,*,#13097,.T.);
#19670=ORIENTED_EDGE('',*,*,#13073,.T.);
#19671=ORIENTED_EDGE('',*,*,#13076,.T.);
#19672=ORIENTED_EDGE('',*,*,#13078,.T.);
#19673=ORIENTED_EDGE('',*,*,#12772,.F.);
#19674=ORIENTED_EDGE('',*,*,#13097,.F.);
#19675=ORIENTED_EDGE('',*,*,#13098,.T.);
#19676=ORIENTED_EDGE('',*,*,#13099,.T.);
#19677=ORIENTED_EDGE('',*,*,#13098,.F.);
#19678=ORIENTED_EDGE('',*,*,#13099,.F.);
#19679=ORIENTED_EDGE('',*,*,#13079,.T.);
#19680=ORIENTED_EDGE('',*,*,#13095,.T.);
#19681=ORIENTED_EDGE('',*,*,#13092,.T.);
#19682=ORIENTED_EDGE('',*,*,#13089,.T.);
#19683=ORIENTED_EDGE('',*,*,#13086,.T.);
#19684=ORIENTED_EDGE('',*,*,#13083,.T.);
#19685=ORIENTED_EDGE('',*,*,#13071,.T.);
#19686=ORIENTED_EDGE('',*,*,#13100,.F.);
#19687=ORIENTED_EDGE('',*,*,#13101,.T.);
#19688=ORIENTED_EDGE('',*,*,#13102,.T.);
#19689=ORIENTED_EDGE('',*,*,#13101,.F.);
#19690=ORIENTED_EDGE('',*,*,#13103,.F.);
#19691=ORIENTED_EDGE('',*,*,#13104,.T.);
#19692=ORIENTED_EDGE('',*,*,#13105,.T.);
#19693=ORIENTED_EDGE('',*,*,#13104,.F.);
#19694=ORIENTED_EDGE('',*,*,#13103,.T.);
#19695=ORIENTED_EDGE('',*,*,#13100,.T.);
#19696=ORIENTED_EDGE('',*,*,#13105,.F.);
#19697=ORIENTED_EDGE('',*,*,#13102,.F.);
#19698=ORIENTED_EDGE('',*,*,#13106,.F.);
#19699=ORIENTED_EDGE('',*,*,#13107,.T.);
#19700=ORIENTED_EDGE('',*,*,#13108,.T.);
#19701=ORIENTED_EDGE('',*,*,#13107,.F.);
#19702=ORIENTED_EDGE('',*,*,#13109,.F.);
#19703=ORIENTED_EDGE('',*,*,#13110,.T.);
#19704=ORIENTED_EDGE('',*,*,#13111,.T.);
#19705=ORIENTED_EDGE('',*,*,#13110,.F.);
#19706=ORIENTED_EDGE('',*,*,#13109,.T.);
#19707=ORIENTED_EDGE('',*,*,#13106,.T.);
#19708=ORIENTED_EDGE('',*,*,#13111,.F.);
#19709=ORIENTED_EDGE('',*,*,#13108,.F.);
#19710=CYLINDRICAL_SURFACE('',#22043,3.5);
#19711=CYLINDRICAL_SURFACE('',#22046,3.5);
#19712=CYLINDRICAL_SURFACE('',#22049,3.5);
#19713=CYLINDRICAL_SURFACE('',#22052,3.5);
#19714=CYLINDRICAL_SURFACE('',#22055,3.5);
#19715=CYLINDRICAL_SURFACE('',#22058,3.5);
#19716=CYLINDRICAL_SURFACE('',#22083,3.5175);
#19717=CYLINDRICAL_SURFACE('',#22085,3.5175);
#19718=CYLINDRICAL_SURFACE('',#22086,3.5175);
#19719=CYLINDRICAL_SURFACE('',#22087,3.5175);
#19720=CYLINDRICAL_SURFACE('',#22088,3.5175);
#19721=CYLINDRICAL_SURFACE('',#22089,3.5175);
#19722=CYLINDRICAL_SURFACE('',#22090,3.5175);
#19723=CYLINDRICAL_SURFACE('',#22091,3.5175);
#19724=CYLINDRICAL_SURFACE('',#22093,3.5175);
#19725=CYLINDRICAL_SURFACE('',#22095,3.5175);
#19726=CYLINDRICAL_SURFACE('',#22096,3.5175);
#19727=CYLINDRICAL_SURFACE('',#22097,3.5175);
#19728=CYLINDRICAL_SURFACE('',#22098,3.5175);
#19729=CYLINDRICAL_SURFACE('',#22099,3.5175);
#19730=CYLINDRICAL_SURFACE('',#22100,3.5175);
#19731=CYLINDRICAL_SURFACE('',#22101,3.5175);
#19732=CYLINDRICAL_SURFACE('',#22103,3.5175);
#19733=CYLINDRICAL_SURFACE('',#22105,3.5175);
#19734=CYLINDRICAL_SURFACE('',#22106,3.5175);
#19735=CYLINDRICAL_SURFACE('',#22107,3.5175);
#19736=CYLINDRICAL_SURFACE('',#22108,3.5175);
#19737=CYLINDRICAL_SURFACE('',#22109,3.5175);
#19738=CYLINDRICAL_SURFACE('',#22110,3.5175);
#19739=CYLINDRICAL_SURFACE('',#22111,3.5175);
#19740=CYLINDRICAL_SURFACE('',#22113,3.5175);
#19741=CYLINDRICAL_SURFACE('',#22115,3.5175);
#19742=CYLINDRICAL_SURFACE('',#22116,3.5175);
#19743=CYLINDRICAL_SURFACE('',#22117,3.5175);
#19744=CYLINDRICAL_SURFACE('',#22118,3.5175);
#19745=CYLINDRICAL_SURFACE('',#22119,3.5175);
#19746=CYLINDRICAL_SURFACE('',#22120,3.5175);
#19747=CYLINDRICAL_SURFACE('',#22121,3.5175);
#19748=CYLINDRICAL_SURFACE('',#22123,4.07350000000001);
#19749=CYLINDRICAL_SURFACE('',#22125,4.07350000000001);
#19750=CYLINDRICAL_SURFACE('',#22126,4.07350000000001);
#19751=CYLINDRICAL_SURFACE('',#22127,4.07350000000001);
#19752=CYLINDRICAL_SURFACE('',#22128,4.07350000000001);
#19753=CYLINDRICAL_SURFACE('',#22129,4.07350000000001);
#19754=CYLINDRICAL_SURFACE('',#22130,4.07350000000001);
#19755=CYLINDRICAL_SURFACE('',#22131,4.07350000000001);
#19756=CYLINDRICAL_SURFACE('',#22133,4.0735);
#19757=CYLINDRICAL_SURFACE('',#22135,4.0735);
#19758=CYLINDRICAL_SURFACE('',#22136,4.0735);
#19759=CYLINDRICAL_SURFACE('',#22137,4.0735);
#19760=CYLINDRICAL_SURFACE('',#22138,4.0735);
#19761=CYLINDRICAL_SURFACE('',#22139,4.0735);
#19762=CYLINDRICAL_SURFACE('',#22140,4.0735);
#19763=CYLINDRICAL_SURFACE('',#22141,4.0735);
#19764=CYLINDRICAL_SURFACE('',#22143,4.0735);
#19765=CYLINDRICAL_SURFACE('',#22145,4.0735);
#19766=CYLINDRICAL_SURFACE('',#22146,4.0735);
#19767=CYLINDRICAL_SURFACE('',#22147,4.0735);
#19768=CYLINDRICAL_SURFACE('',#22148,4.0735);
#19769=CYLINDRICAL_SURFACE('',#22149,4.0735);
#19770=CYLINDRICAL_SURFACE('',#22150,4.0735);
#19771=CYLINDRICAL_SURFACE('',#22151,4.0735);
#19772=CYLINDRICAL_SURFACE('',#22153,4.07350000000001);
#19773=CYLINDRICAL_SURFACE('',#22155,4.07350000000001);
#19774=CYLINDRICAL_SURFACE('',#22156,4.07350000000001);
#19775=CYLINDRICAL_SURFACE('',#22157,4.07350000000001);
#19776=CYLINDRICAL_SURFACE('',#22158,4.07350000000001);
#19777=CYLINDRICAL_SURFACE('',#22159,4.07350000000001);
#19778=CYLINDRICAL_SURFACE('',#22160,4.07350000000001);
#19779=CYLINDRICAL_SURFACE('',#22161,4.07350000000001);
#19780=CYLINDRICAL_SURFACE('',#22163,4.07350000000001);
#19781=CYLINDRICAL_SURFACE('',#22165,4.0735);
#19782=CYLINDRICAL_SURFACE('',#22166,4.0735);
#19783=CYLINDRICAL_SURFACE('',#22167,4.07350000000001);
#19784=CYLINDRICAL_SURFACE('',#22168,3.5175);
#19785=CYLINDRICAL_SURFACE('',#22169,3.5175);
#19786=CYLINDRICAL_SURFACE('',#22170,3.5175);
#19787=CYLINDRICAL_SURFACE('',#22171,3.5175);
#19788=CYLINDRICAL_SURFACE('',#22178,3.942);
#19789=CYLINDRICAL_SURFACE('',#22180,3.942);
#19790=CYLINDRICAL_SURFACE('',#22181,3.942);
#19791=CYLINDRICAL_SURFACE('',#22182,3.942);
#19792=CYLINDRICAL_SURFACE('',#22183,3.942);
#19793=CYLINDRICAL_SURFACE('',#22184,3.942);
#19794=CYLINDRICAL_SURFACE('',#22185,3.942);
#19795=CYLINDRICAL_SURFACE('',#22186,3.942);
#19796=CYLINDRICAL_SURFACE('',#22187,3.942);
#19797=CYLINDRICAL_SURFACE('',#22188,3.942);
#19798=CYLINDRICAL_SURFACE('',#22189,3.942);
#19799=CYLINDRICAL_SURFACE('',#22190,3.942);
#19800=CYLINDRICAL_SURFACE('',#22191,3.942);
#19801=CYLINDRICAL_SURFACE('',#22192,3.942);
#19802=CYLINDRICAL_SURFACE('',#22193,3.942);
#19803=CYLINDRICAL_SURFACE('',#22194,3.942);
#19804=CYLINDRICAL_SURFACE('',#22195,3.942);
#19805=CYLINDRICAL_SURFACE('',#22196,3.942);
#19806=CYLINDRICAL_SURFACE('',#22197,3.942);
#19807=CYLINDRICAL_SURFACE('',#22198,3.942);
#19808=CYLINDRICAL_SURFACE('',#22199,3.942);
#19809=CYLINDRICAL_SURFACE('',#22200,3.942);
#19810=CYLINDRICAL_SURFACE('',#22201,3.942);
#19811=CYLINDRICAL_SURFACE('',#22202,3.942);
#19812=CYLINDRICAL_SURFACE('',#22203,3.37175);
#19813=CYLINDRICAL_SURFACE('',#22205,3.37175);
#19814=CYLINDRICAL_SURFACE('',#22206,3.37175);
#19815=CYLINDRICAL_SURFACE('',#22207,3.37175);
#19816=CYLINDRICAL_SURFACE('',#22208,3.37175);
#19817=CYLINDRICAL_SURFACE('',#22209,3.37175);
#19818=CYLINDRICAL_SURFACE('',#22210,3.37175);
#19819=CYLINDRICAL_SURFACE('',#22211,3.37175);
#19820=CYLINDRICAL_SURFACE('',#22212,3.37175);
#19821=CYLINDRICAL_SURFACE('',#22213,3.37175);
#19822=CYLINDRICAL_SURFACE('',#22214,3.37175);
#19823=CYLINDRICAL_SURFACE('',#22215,3.37175);
#19824=CYLINDRICAL_SURFACE('',#22216,3.37175);
#19825=CYLINDRICAL_SURFACE('',#22217,3.37175);
#19826=CYLINDRICAL_SURFACE('',#22218,3.37175);
#19827=CYLINDRICAL_SURFACE('',#22219,3.37175);
#19828=CYLINDRICAL_SURFACE('',#22220,3.37175);
#19829=CYLINDRICAL_SURFACE('',#22221,3.37175);
#19830=CYLINDRICAL_SURFACE('',#22222,3.37175);
#19831=CYLINDRICAL_SURFACE('',#22223,3.37175);
#19832=CYLINDRICAL_SURFACE('',#22224,3.37175);
#19833=CYLINDRICAL_SURFACE('',#22225,3.37175);
#19834=CYLINDRICAL_SURFACE('',#22226,3.37175);
#19835=CYLINDRICAL_SURFACE('',#22227,3.37175);
#19836=CYLINDRICAL_SURFACE('',#22231,3.37175);
#19837=CYLINDRICAL_SURFACE('',#22233,3.942);
#19838=CYLINDRICAL_SURFACE('',#22243,6.5);
#19839=CYLINDRICAL_SURFACE('',#22248,4.5);
#19840=CYLINDRICAL_SURFACE('',#22251,9.);
#19841=CYLINDRICAL_SURFACE('',#22298,4.51775);
#19842=CYLINDRICAL_SURFACE('',#22302,4.51775);
#19843=CYLINDRICAL_SURFACE('',#22303,4.51775);
#19844=CYLINDRICAL_SURFACE('',#22304,4.51775);
#19845=CYLINDRICAL_SURFACE('',#22305,4.51775);
#19846=CYLINDRICAL_SURFACE('',#22306,4.51775);
#19847=CYLINDRICAL_SURFACE('',#22307,4.51775);
#19848=CYLINDRICAL_SURFACE('',#22308,4.51775);
#19849=CYLINDRICAL_SURFACE('',#22309,4.51775);
#19850=CYLINDRICAL_SURFACE('',#22310,4.51775);
#19851=CYLINDRICAL_SURFACE('',#22311,4.51775);
#19852=CYLINDRICAL_SURFACE('',#22312,4.51775);
#19853=CYLINDRICAL_SURFACE('',#22313,4.51775);
#19854=CYLINDRICAL_SURFACE('',#22314,4.51775);
#19855=CYLINDRICAL_SURFACE('',#22315,4.51775);
#19856=CYLINDRICAL_SURFACE('',#22316,4.51775);
#19857=CYLINDRICAL_SURFACE('',#22317,4.51775);
#19858=CYLINDRICAL_SURFACE('',#22318,4.51775);
#19859=CYLINDRICAL_SURFACE('',#22319,4.51775);
#19860=CYLINDRICAL_SURFACE('',#22320,4.51775);
#19861=CYLINDRICAL_SURFACE('',#22321,4.51775);
#19862=CYLINDRICAL_SURFACE('',#22322,4.51775);
#19863=CYLINDRICAL_SURFACE('',#22323,4.51775);
#19864=CYLINDRICAL_SURFACE('',#22324,4.51775);
#19865=CYLINDRICAL_SURFACE('',#22325,4.51775);
#19866=CYLINDRICAL_SURFACE('',#22327,5.0736);
#19867=CYLINDRICAL_SURFACE('',#22329,5.0736);
#19868=CYLINDRICAL_SURFACE('',#22330,5.0736);
#19869=CYLINDRICAL_SURFACE('',#22331,5.0736);
#19870=CYLINDRICAL_SURFACE('',#22332,5.0736);
#19871=CYLINDRICAL_SURFACE('',#22333,5.0736);
#19872=CYLINDRICAL_SURFACE('',#22334,5.0736);
#19873=CYLINDRICAL_SURFACE('',#22335,5.0736);
#19874=CYLINDRICAL_SURFACE('',#22336,5.0736);
#19875=CYLINDRICAL_SURFACE('',#22337,5.0736);
#19876=CYLINDRICAL_SURFACE('',#22338,5.0736);
#19877=CYLINDRICAL_SURFACE('',#22339,5.0736);
#19878=CYLINDRICAL_SURFACE('',#22340,5.0736);
#19879=CYLINDRICAL_SURFACE('',#22341,5.0736);
#19880=CYLINDRICAL_SURFACE('',#22342,5.0736);
#19881=CYLINDRICAL_SURFACE('',#22343,5.0736);
#19882=CYLINDRICAL_SURFACE('',#22344,5.0736);
#19883=CYLINDRICAL_SURFACE('',#22345,5.0736);
#19884=CYLINDRICAL_SURFACE('',#22346,5.0736);
#19885=CYLINDRICAL_SURFACE('',#22347,5.0736);
#19886=CYLINDRICAL_SURFACE('',#22348,5.0736);
#19887=CYLINDRICAL_SURFACE('',#22349,5.0736);
#19888=CYLINDRICAL_SURFACE('',#22350,5.0736);
#19889=CYLINDRICAL_SURFACE('',#22351,5.0736);
#19890=CYLINDRICAL_SURFACE('',#22352,5.0736);
#19891=CYLINDRICAL_SURFACE('',#22354,4.51775);
#19892=CYLINDRICAL_SURFACE('',#22358,4.51775);
#19893=CYLINDRICAL_SURFACE('',#22359,4.51775);
#19894=CYLINDRICAL_SURFACE('',#22360,4.51775);
#19895=CYLINDRICAL_SURFACE('',#22361,4.51775);
#19896=CYLINDRICAL_SURFACE('',#22362,4.51775);
#19897=CYLINDRICAL_SURFACE('',#22363,4.51775);
#19898=CYLINDRICAL_SURFACE('',#22364,4.51775);
#19899=CYLINDRICAL_SURFACE('',#22365,4.51775);
#19900=CYLINDRICAL_SURFACE('',#22366,4.51775);
#19901=CYLINDRICAL_SURFACE('',#22367,4.51775);
#19902=CYLINDRICAL_SURFACE('',#22368,4.51775);
#19903=CYLINDRICAL_SURFACE('',#22369,4.51775);
#19904=CYLINDRICAL_SURFACE('',#22370,4.51775);
#19905=CYLINDRICAL_SURFACE('',#22371,4.51775);
#19906=CYLINDRICAL_SURFACE('',#22372,4.51775);
#19907=CYLINDRICAL_SURFACE('',#22373,4.51775);
#19908=CYLINDRICAL_SURFACE('',#22374,4.51775);
#19909=CYLINDRICAL_SURFACE('',#22375,4.51775);
#19910=CYLINDRICAL_SURFACE('',#22376,4.51775);
#19911=CYLINDRICAL_SURFACE('',#22377,4.51775);
#19912=CYLINDRICAL_SURFACE('',#22378,4.51775);
#19913=CYLINDRICAL_SURFACE('',#22379,4.51775);
#19914=CYLINDRICAL_SURFACE('',#22380,4.51775);
#19915=CYLINDRICAL_SURFACE('',#22381,4.51775);
#19916=CYLINDRICAL_SURFACE('',#22382,4.51775);
#19917=CYLINDRICAL_SURFACE('',#22383,4.51775);
#19918=CYLINDRICAL_SURFACE('',#22384,4.51775);
#19919=CYLINDRICAL_SURFACE('',#22385,4.51775);
#19920=CYLINDRICAL_SURFACE('',#22386,4.51775);
#19921=CYLINDRICAL_SURFACE('',#22387,4.51775);
#19922=CYLINDRICAL_SURFACE('',#22388,4.51775);
#19923=CYLINDRICAL_SURFACE('',#22389,4.51775);
#19924=CYLINDRICAL_SURFACE('',#22390,4.51775);
#19925=CYLINDRICAL_SURFACE('',#22391,4.51775);
#19926=CYLINDRICAL_SURFACE('',#22392,4.51775);
#19927=CYLINDRICAL_SURFACE('',#22393,4.51775);
#19928=CYLINDRICAL_SURFACE('',#22394,4.51775);
#19929=CYLINDRICAL_SURFACE('',#22395,4.51775);
#19930=CYLINDRICAL_SURFACE('',#22396,4.51775);
#19931=CYLINDRICAL_SURFACE('',#22398,5.0736);
#19932=CYLINDRICAL_SURFACE('',#22400,5.0736);
#19933=CYLINDRICAL_SURFACE('',#22401,5.0736);
#19934=CYLINDRICAL_SURFACE('',#22402,5.0736);
#19935=CYLINDRICAL_SURFACE('',#22403,5.0736);
#19936=CYLINDRICAL_SURFACE('',#22404,5.0736);
#19937=CYLINDRICAL_SURFACE('',#22405,5.0736);
#19938=CYLINDRICAL_SURFACE('',#22406,5.0736);
#19939=CYLINDRICAL_SURFACE('',#22407,5.0736);
#19940=CYLINDRICAL_SURFACE('',#22408,5.0736);
#19941=CYLINDRICAL_SURFACE('',#22409,5.0736);
#19942=CYLINDRICAL_SURFACE('',#22410,5.0736);
#19943=CYLINDRICAL_SURFACE('',#22411,5.0736);
#19944=CYLINDRICAL_SURFACE('',#22412,5.0736);
#19945=CYLINDRICAL_SURFACE('',#22413,5.0736);
#19946=CYLINDRICAL_SURFACE('',#22414,5.0736);
#19947=CYLINDRICAL_SURFACE('',#22415,5.0736);
#19948=CYLINDRICAL_SURFACE('',#22416,5.0736);
#19949=CYLINDRICAL_SURFACE('',#22417,5.0736);
#19950=CYLINDRICAL_SURFACE('',#22418,5.0736);
#19951=CYLINDRICAL_SURFACE('',#22419,5.0736);
#19952=CYLINDRICAL_SURFACE('',#22420,5.0736);
#19953=CYLINDRICAL_SURFACE('',#22421,5.0736);
#19954=CYLINDRICAL_SURFACE('',#22422,5.0736);
#19955=CYLINDRICAL_SURFACE('',#22423,5.0736);
#19956=CYLINDRICAL_SURFACE('',#22424,5.0736);
#19957=CYLINDRICAL_SURFACE('',#22425,5.0736);
#19958=CYLINDRICAL_SURFACE('',#22426,5.0736);
#19959=CYLINDRICAL_SURFACE('',#22427,5.0736);
#19960=CYLINDRICAL_SURFACE('',#22428,5.0736);
#19961=CYLINDRICAL_SURFACE('',#22429,5.0736);
#19962=CYLINDRICAL_SURFACE('',#22430,5.0736);
#19963=CYLINDRICAL_SURFACE('',#22431,5.0736);
#19964=CYLINDRICAL_SURFACE('',#22432,5.0736);
#19965=CYLINDRICAL_SURFACE('',#22433,5.0736);
#19966=CYLINDRICAL_SURFACE('',#22434,5.0736);
#19967=CYLINDRICAL_SURFACE('',#22435,5.0736);
#19968=CYLINDRICAL_SURFACE('',#22436,5.0736);
#19969=CYLINDRICAL_SURFACE('',#22437,5.0736);
#19970=CYLINDRICAL_SURFACE('',#22438,5.0736);
#19971=CYLINDRICAL_SURFACE('',#22441,5.0736);
#19972=CYLINDRICAL_SURFACE('',#22442,4.51775);
#19973=CYLINDRICAL_SURFACE('',#22446,5.0736);
#19974=CYLINDRICAL_SURFACE('',#22447,4.51775);
#19975=CYLINDRICAL_SURFACE('',#22450,1.);
#19976=CYLINDRICAL_SURFACE('',#22494,1.);
#19977=CYLINDRICAL_SURFACE('',#22497,1.);
#19978=CYLINDRICAL_SURFACE('',#22500,1.);
#19979=CYLINDRICAL_SURFACE('',#22503,1.);
#19980=CYLINDRICAL_SURFACE('',#22506,1.);
#19981=CYLINDRICAL_SURFACE('',#22508,1.);
#19982=CYLINDRICAL_SURFACE('',#22511,1.);
#19983=CYLINDRICAL_SURFACE('',#22513,1.);
#19984=CYLINDRICAL_SURFACE('',#22516,1.);
#19985=CYLINDRICAL_SURFACE('',#22518,1.);
#19986=CYLINDRICAL_SURFACE('',#22521,1.);
#19987=CYLINDRICAL_SURFACE('',#22524,1.);
#19988=CYLINDRICAL_SURFACE('',#22527,1.);
#19989=CYLINDRICAL_SURFACE('',#22530,1.);
#19990=CYLINDRICAL_SURFACE('',#22532,1.);
#19991=CYLINDRICAL_SURFACE('',#22535,1.);
#19992=CYLINDRICAL_SURFACE('',#22537,1.);
#19993=CYLINDRICAL_SURFACE('',#22540,1.);
#19994=CYLINDRICAL_SURFACE('',#22542,1.);
#19995=CYLINDRICAL_SURFACE('',#22545,1.);
#19996=CYLINDRICAL_SURFACE('',#22548,1.);
#19997=CYLINDRICAL_SURFACE('',#22551,1.);
#19998=CYLINDRICAL_SURFACE('',#22554,1.);
#19999=CYLINDRICAL_SURFACE('',#22556,1.);
#20000=CYLINDRICAL_SURFACE('',#22559,1.);
#20001=CYLINDRICAL_SURFACE('',#22561,1.);
#20002=CYLINDRICAL_SURFACE('',#22564,1.);
#20003=CYLINDRICAL_SURFACE('',#22566,1.);
#20004=CYLINDRICAL_SURFACE('',#22569,1.);
#20005=CYLINDRICAL_SURFACE('',#22572,1.);
#20006=CYLINDRICAL_SURFACE('',#22575,1.);
#20007=CYLINDRICAL_SURFACE('',#22578,1.);
#20008=CYLINDRICAL_SURFACE('',#22580,1.);
#20009=CYLINDRICAL_SURFACE('',#22583,1.);
#20010=CYLINDRICAL_SURFACE('',#22585,1.);
#20011=CYLINDRICAL_SURFACE('',#22587,3.);
#20012=CYLINDRICAL_SURFACE('',#22589,3.);
#20013=CYLINDRICAL_SURFACE('',#22591,4.);
#20014=CYLINDRICAL_SURFACE('',#22592,3.);
#20015=CYLINDRICAL_SURFACE('',#22594,3.);
#20016=CYLINDRICAL_SURFACE('',#22613,8.5);
#20017=CYLINDRICAL_SURFACE('',#22615,5.5);
#20018=CYLINDRICAL_SURFACE('',#22617,4.5);
#20019=CYLINDRICAL_SURFACE('',#22620,4.5);
#20020=CYLINDRICAL_SURFACE('',#22623,4.5);
#20021=CYLINDRICAL_SURFACE('',#22626,4.5);
#20022=CYLINDRICAL_SURFACE('',#22636,4.942);
#20023=CYLINDRICAL_SURFACE('',#22638,4.942);
#20024=CYLINDRICAL_SURFACE('',#22639,4.942);
#20025=CYLINDRICAL_SURFACE('',#22640,4.942);
#20026=CYLINDRICAL_SURFACE('',#22641,4.942);
#20027=CYLINDRICAL_SURFACE('',#22642,4.942);
#20028=CYLINDRICAL_SURFACE('',#22643,4.942);
#20029=CYLINDRICAL_SURFACE('',#22644,4.942);
#20030=CYLINDRICAL_SURFACE('',#22645,4.942);
#20031=CYLINDRICAL_SURFACE('',#22646,4.942);
#20032=CYLINDRICAL_SURFACE('',#22647,4.942);
#20033=CYLINDRICAL_SURFACE('',#22648,4.942);
#20034=CYLINDRICAL_SURFACE('',#22649,4.942);
#20035=CYLINDRICAL_SURFACE('',#22650,4.942);
#20036=CYLINDRICAL_SURFACE('',#22651,4.942);
#20037=CYLINDRICAL_SURFACE('',#22652,4.942);
#20038=CYLINDRICAL_SURFACE('',#22653,4.942);
#20039=CYLINDRICAL_SURFACE('',#22654,4.942);
#20040=CYLINDRICAL_SURFACE('',#22655,4.942);
#20041=CYLINDRICAL_SURFACE('',#22656,4.372);
#20042=CYLINDRICAL_SURFACE('',#22658,4.372);
#20043=CYLINDRICAL_SURFACE('',#22659,4.372);
#20044=CYLINDRICAL_SURFACE('',#22660,4.372);
#20045=CYLINDRICAL_SURFACE('',#22661,4.372);
#20046=CYLINDRICAL_SURFACE('',#22662,4.372);
#20047=CYLINDRICAL_SURFACE('',#22663,4.372);
#20048=CYLINDRICAL_SURFACE('',#22664,4.372);
#20049=CYLINDRICAL_SURFACE('',#22665,4.372);
#20050=CYLINDRICAL_SURFACE('',#22666,4.372);
#20051=CYLINDRICAL_SURFACE('',#22667,4.372);
#20052=CYLINDRICAL_SURFACE('',#22668,4.372);
#20053=CYLINDRICAL_SURFACE('',#22669,4.372);
#20054=CYLINDRICAL_SURFACE('',#22670,4.372);
#20055=CYLINDRICAL_SURFACE('',#22671,4.372);
#20056=CYLINDRICAL_SURFACE('',#22672,4.372);
#20057=CYLINDRICAL_SURFACE('',#22673,4.372);
#20058=CYLINDRICAL_SURFACE('',#22674,4.372);
#20059=CYLINDRICAL_SURFACE('',#22675,4.372);
#20060=CYLINDRICAL_SURFACE('',#22679,4.372);
#20061=CYLINDRICAL_SURFACE('',#22681,4.942);
#20062=CYLINDRICAL_SURFACE('',#22691,8.);
#20063=CYLINDRICAL_SURFACE('',#22696,30.);
#20064=CYLINDRICAL_SURFACE('',#22702,2.5175);
#20065=CYLINDRICAL_SURFACE('',#22706,2.5175);
#20066=CYLINDRICAL_SURFACE('',#22707,2.5175);
#20067=CYLINDRICAL_SURFACE('',#22708,2.5175);
#20068=CYLINDRICAL_SURFACE('',#22709,2.5175);
#20069=CYLINDRICAL_SURFACE('',#22710,2.5175);
#20070=CYLINDRICAL_SURFACE('',#22711,2.5175);
#20071=CYLINDRICAL_SURFACE('',#22712,2.5175);
#20072=CYLINDRICAL_SURFACE('',#22714,3.0735);
#20073=CYLINDRICAL_SURFACE('',#22716,3.0735);
#20074=CYLINDRICAL_SURFACE('',#22717,3.0735);
#20075=CYLINDRICAL_SURFACE('',#22718,3.0735);
#20076=CYLINDRICAL_SURFACE('',#22719,3.0735);
#20077=CYLINDRICAL_SURFACE('',#22720,3.0735);
#20078=CYLINDRICAL_SURFACE('',#22721,3.0735);
#20079=CYLINDRICAL_SURFACE('',#22722,3.0735);
#20080=CYLINDRICAL_SURFACE('',#22724,2.5175);
#20081=CYLINDRICAL_SURFACE('',#22728,2.5175);
#20082=CYLINDRICAL_SURFACE('',#22729,2.5175);
#20083=CYLINDRICAL_SURFACE('',#22730,2.5175);
#20084=CYLINDRICAL_SURFACE('',#22731,2.5175);
#20085=CYLINDRICAL_SURFACE('',#22732,2.5175);
#20086=CYLINDRICAL_SURFACE('',#22733,2.5175);
#20087=CYLINDRICAL_SURFACE('',#22734,2.5175);
#20088=CYLINDRICAL_SURFACE('',#22736,3.0735);
#20089=CYLINDRICAL_SURFACE('',#22738,3.0735);
#20090=CYLINDRICAL_SURFACE('',#22739,3.0735);
#20091=CYLINDRICAL_SURFACE('',#22740,3.0735);
#20092=CYLINDRICAL_SURFACE('',#22741,3.0735);
#20093=CYLINDRICAL_SURFACE('',#22742,3.0735);
#20094=CYLINDRICAL_SURFACE('',#22743,3.0735);
#20095=CYLINDRICAL_SURFACE('',#22744,3.0735);
#20096=CYLINDRICAL_SURFACE('',#22746,2.5175);
#20097=CYLINDRICAL_SURFACE('',#22750,2.5175);
#20098=CYLINDRICAL_SURFACE('',#22751,2.5175);
#20099=CYLINDRICAL_SURFACE('',#22752,2.5175);
#20100=CYLINDRICAL_SURFACE('',#22753,2.5175);
#20101=CYLINDRICAL_SURFACE('',#22754,2.5175);
#20102=CYLINDRICAL_SURFACE('',#22755,2.5175);
#20103=CYLINDRICAL_SURFACE('',#22756,2.5175);
#20104=CYLINDRICAL_SURFACE('',#22758,3.0735);
#20105=CYLINDRICAL_SURFACE('',#22760,3.0735);
#20106=CYLINDRICAL_SURFACE('',#22761,3.0735);
#20107=CYLINDRICAL_SURFACE('',#22762,3.0735);
#20108=CYLINDRICAL_SURFACE('',#22763,3.0735);
#20109=CYLINDRICAL_SURFACE('',#22764,3.0735);
#20110=CYLINDRICAL_SURFACE('',#22765,3.0735);
#20111=CYLINDRICAL_SURFACE('',#22766,3.0735);
#20112=CYLINDRICAL_SURFACE('',#22769,3.0735);
#20113=CYLINDRICAL_SURFACE('',#22770,2.5175);
#20114=CYLINDRICAL_SURFACE('',#22772,3.0735);
#20115=CYLINDRICAL_SURFACE('',#22773,2.5175);
#20116=CYLINDRICAL_SURFACE('',#22775,3.0735);
#20117=CYLINDRICAL_SURFACE('',#22776,2.5175);
#20118=CYLINDRICAL_SURFACE('',#22783,30.);
#20119=CYLINDRICAL_SURFACE('',#22789,3.5);
#20120=CYLINDRICAL_SURFACE('',#22792,3.5);
#20121=CYLINDRICAL_SURFACE('',#22795,3.5);
#20122=CYLINDRICAL_SURFACE('',#22802,5.5);
#20123=CYLINDRICAL_SURFACE('',#22804,22.);
#20124=CYLINDRICAL_SURFACE('',#22810,4.942);
#20125=CYLINDRICAL_SURFACE('',#22812,4.942);
#20126=CYLINDRICAL_SURFACE('',#22813,4.942);
#20127=CYLINDRICAL_SURFACE('',#22814,4.942);
#20128=CYLINDRICAL_SURFACE('',#22815,4.942);
#20129=CYLINDRICAL_SURFACE('',#22816,4.942);
#20130=CYLINDRICAL_SURFACE('',#22817,4.942);
#20131=CYLINDRICAL_SURFACE('',#22818,4.942);
#20132=CYLINDRICAL_SURFACE('',#22819,4.942);
#20133=CYLINDRICAL_SURFACE('',#22820,4.942);
#20134=CYLINDRICAL_SURFACE('',#22821,4.942);
#20135=CYLINDRICAL_SURFACE('',#22822,4.942);
#20136=CYLINDRICAL_SURFACE('',#22823,4.942);
#20137=CYLINDRICAL_SURFACE('',#22824,4.942);
#20138=CYLINDRICAL_SURFACE('',#22825,4.942);
#20139=CYLINDRICAL_SURFACE('',#22826,4.942);
#20140=CYLINDRICAL_SURFACE('',#22827,4.942);
#20141=CYLINDRICAL_SURFACE('',#22828,4.942);
#20142=CYLINDRICAL_SURFACE('',#22829,4.942);
#20143=CYLINDRICAL_SURFACE('',#22830,4.942);
#20144=CYLINDRICAL_SURFACE('',#22831,4.942);
#20145=CYLINDRICAL_SURFACE('',#22832,4.942);
#20146=CYLINDRICAL_SURFACE('',#22833,4.942);
#20147=CYLINDRICAL_SURFACE('',#22834,4.942);
#20148=CYLINDRICAL_SURFACE('',#22835,4.942);
#20149=CYLINDRICAL_SURFACE('',#22836,4.942);
#20150=CYLINDRICAL_SURFACE('',#22837,4.942);
#20151=CYLINDRICAL_SURFACE('',#22838,4.942);
#20152=CYLINDRICAL_SURFACE('',#22839,4.942);
#20153=CYLINDRICAL_SURFACE('',#22840,4.942);
#20154=CYLINDRICAL_SURFACE('',#22841,4.942);
#20155=CYLINDRICAL_SURFACE('',#22842,4.942);
#20156=CYLINDRICAL_SURFACE('',#22843,4.942);
#20157=CYLINDRICAL_SURFACE('',#22844,4.942);
#20158=CYLINDRICAL_SURFACE('',#22845,4.942);
#20159=CYLINDRICAL_SURFACE('',#22846,4.942);
#20160=CYLINDRICAL_SURFACE('',#22847,4.942);
#20161=CYLINDRICAL_SURFACE('',#22848,4.942);
#20162=CYLINDRICAL_SURFACE('',#22849,4.942);
#20163=CYLINDRICAL_SURFACE('',#22850,4.942);
#20164=CYLINDRICAL_SURFACE('',#22851,4.942);
#20165=CYLINDRICAL_SURFACE('',#22852,4.942);
#20166=CYLINDRICAL_SURFACE('',#22853,4.942);
#20167=CYLINDRICAL_SURFACE('',#22854,4.942);
#20168=CYLINDRICAL_SURFACE('',#22855,4.942);
#20169=CYLINDRICAL_SURFACE('',#22856,4.942);
#20170=CYLINDRICAL_SURFACE('',#22857,4.942);
#20171=CYLINDRICAL_SURFACE('',#22858,4.942);
#20172=CYLINDRICAL_SURFACE('',#22859,4.942);
#20173=CYLINDRICAL_SURFACE('',#22860,4.942);
#20174=CYLINDRICAL_SURFACE('',#22861,4.942);
#20175=CYLINDRICAL_SURFACE('',#22862,4.942);
#20176=CYLINDRICAL_SURFACE('',#22863,4.942);
#20177=CYLINDRICAL_SURFACE('',#22864,4.942);
#20178=CYLINDRICAL_SURFACE('',#22865,4.942);
#20179=CYLINDRICAL_SURFACE('',#22866,4.942);
#20180=CYLINDRICAL_SURFACE('',#22867,4.942);
#20181=CYLINDRICAL_SURFACE('',#22868,4.942);
#20182=CYLINDRICAL_SURFACE('',#22869,4.942);
#20183=CYLINDRICAL_SURFACE('',#22870,4.942);
#20184=CYLINDRICAL_SURFACE('',#22871,4.372);
#20185=CYLINDRICAL_SURFACE('',#22873,4.372);
#20186=CYLINDRICAL_SURFACE('',#22874,4.372);
#20187=CYLINDRICAL_SURFACE('',#22875,4.372);
#20188=CYLINDRICAL_SURFACE('',#22876,4.372);
#20189=CYLINDRICAL_SURFACE('',#22877,4.372);
#20190=CYLINDRICAL_SURFACE('',#22878,4.372);
#20191=CYLINDRICAL_SURFACE('',#22879,4.372);
#20192=CYLINDRICAL_SURFACE('',#22880,4.372);
#20193=CYLINDRICAL_SURFACE('',#22881,4.372);
#20194=CYLINDRICAL_SURFACE('',#22882,4.372);
#20195=CYLINDRICAL_SURFACE('',#22883,4.372);
#20196=CYLINDRICAL_SURFACE('',#22884,4.372);
#20197=CYLINDRICAL_SURFACE('',#22885,4.372);
#20198=CYLINDRICAL_SURFACE('',#22886,4.372);
#20199=CYLINDRICAL_SURFACE('',#22887,4.372);
#20200=CYLINDRICAL_SURFACE('',#22888,4.372);
#20201=CYLINDRICAL_SURFACE('',#22889,4.372);
#20202=CYLINDRICAL_SURFACE('',#22890,4.372);
#20203=CYLINDRICAL_SURFACE('',#22891,4.372);
#20204=CYLINDRICAL_SURFACE('',#22892,4.372);
#20205=CYLINDRICAL_SURFACE('',#22893,4.372);
#20206=CYLINDRICAL_SURFACE('',#22894,4.372);
#20207=CYLINDRICAL_SURFACE('',#22895,4.372);
#20208=CYLINDRICAL_SURFACE('',#22896,4.372);
#20209=CYLINDRICAL_SURFACE('',#22897,4.372);
#20210=CYLINDRICAL_SURFACE('',#22898,4.372);
#20211=CYLINDRICAL_SURFACE('',#22899,4.372);
#20212=CYLINDRICAL_SURFACE('',#22900,4.372);
#20213=CYLINDRICAL_SURFACE('',#22901,4.372);
#20214=CYLINDRICAL_SURFACE('',#22902,4.372);
#20215=CYLINDRICAL_SURFACE('',#22903,4.372);
#20216=CYLINDRICAL_SURFACE('',#22904,4.372);
#20217=CYLINDRICAL_SURFACE('',#22905,4.372);
#20218=CYLINDRICAL_SURFACE('',#22906,4.372);
#20219=CYLINDRICAL_SURFACE('',#22907,4.372);
#20220=CYLINDRICAL_SURFACE('',#22908,4.372);
#20221=CYLINDRICAL_SURFACE('',#22909,4.372);
#20222=CYLINDRICAL_SURFACE('',#22910,4.372);
#20223=CYLINDRICAL_SURFACE('',#22911,4.372);
#20224=CYLINDRICAL_SURFACE('',#22912,4.372);
#20225=CYLINDRICAL_SURFACE('',#22913,4.372);
#20226=CYLINDRICAL_SURFACE('',#22914,4.372);
#20227=CYLINDRICAL_SURFACE('',#22915,4.372);
#20228=CYLINDRICAL_SURFACE('',#22916,4.372);
#20229=CYLINDRICAL_SURFACE('',#22917,4.372);
#20230=CYLINDRICAL_SURFACE('',#22918,4.372);
#20231=CYLINDRICAL_SURFACE('',#22919,4.372);
#20232=CYLINDRICAL_SURFACE('',#22920,4.372);
#20233=CYLINDRICAL_SURFACE('',#22921,4.372);
#20234=CYLINDRICAL_SURFACE('',#22922,4.372);
#20235=CYLINDRICAL_SURFACE('',#22923,4.372);
#20236=CYLINDRICAL_SURFACE('',#22924,4.372);
#20237=CYLINDRICAL_SURFACE('',#22925,4.372);
#20238=CYLINDRICAL_SURFACE('',#22926,4.372);
#20239=CYLINDRICAL_SURFACE('',#22927,4.372);
#20240=CYLINDRICAL_SURFACE('',#22928,4.372);
#20241=CYLINDRICAL_SURFACE('',#22929,4.372);
#20242=CYLINDRICAL_SURFACE('',#22930,4.372);
#20243=CYLINDRICAL_SURFACE('',#22931,4.372);
#20244=CYLINDRICAL_SURFACE('',#22932,4.372);
#20245=CYLINDRICAL_SURFACE('',#22934,4.942);
#20246=CYLINDRICAL_SURFACE('',#22945,5.);
#20247=CYLINDRICAL_SURFACE('',#22951,4.51775);
#20248=CYLINDRICAL_SURFACE('',#22953,4.51775);
#20249=CYLINDRICAL_SURFACE('',#22954,4.51775);
#20250=CYLINDRICAL_SURFACE('',#22955,4.51775);
#20251=CYLINDRICAL_SURFACE('',#22956,4.51775);
#20252=CYLINDRICAL_SURFACE('',#22957,4.51775);
#20253=CYLINDRICAL_SURFACE('',#22958,4.51775);
#20254=CYLINDRICAL_SURFACE('',#22959,4.51775);
#20255=CYLINDRICAL_SURFACE('',#22961,5.0736);
#20256=CYLINDRICAL_SURFACE('',#22963,5.0736);
#20257=CYLINDRICAL_SURFACE('',#22964,5.0736);
#20258=CYLINDRICAL_SURFACE('',#22965,5.0736);
#20259=CYLINDRICAL_SURFACE('',#22966,5.0736);
#20260=CYLINDRICAL_SURFACE('',#22967,5.0736);
#20261=CYLINDRICAL_SURFACE('',#22968,5.0736);
#20262=CYLINDRICAL_SURFACE('',#22969,5.0736);
#20263=CYLINDRICAL_SURFACE('',#22971,5.0736);
#20264=CYLINDRICAL_SURFACE('',#22973,4.51775);
#20265=CYLINDRICAL_SURFACE('',#22982,5.5);
#20266=CYLINDRICAL_SURFACE('',#22985,11.);
#20267=CYLINDRICAL_SURFACE('',#22991,2.942);
#20268=CYLINDRICAL_SURFACE('',#22993,2.942);
#20269=CYLINDRICAL_SURFACE('',#22994,2.942);
#20270=CYLINDRICAL_SURFACE('',#22995,2.942);
#20271=CYLINDRICAL_SURFACE('',#22996,2.942);
#20272=CYLINDRICAL_SURFACE('',#22997,2.942);
#20273=CYLINDRICAL_SURFACE('',#22998,2.942);
#20274=CYLINDRICAL_SURFACE('',#22999,2.942);
#20275=CYLINDRICAL_SURFACE('',#23000,2.942);
#20276=CYLINDRICAL_SURFACE('',#23001,2.942);
#20277=CYLINDRICAL_SURFACE('',#23002,2.942);
#20278=CYLINDRICAL_SURFACE('',#23003,2.942);
#20279=CYLINDRICAL_SURFACE('',#23004,2.942);
#20280=CYLINDRICAL_SURFACE('',#23005,2.942);
#20281=CYLINDRICAL_SURFACE('',#23006,2.942);
#20282=CYLINDRICAL_SURFACE('',#23007,2.37175);
#20283=CYLINDRICAL_SURFACE('',#23009,2.37175);
#20284=CYLINDRICAL_SURFACE('',#23010,2.37175);
#20285=CYLINDRICAL_SURFACE('',#23011,2.37175);
#20286=CYLINDRICAL_SURFACE('',#23012,2.37175);
#20287=CYLINDRICAL_SURFACE('',#23013,2.37175);
#20288=CYLINDRICAL_SURFACE('',#23014,2.37175);
#20289=CYLINDRICAL_SURFACE('',#23015,2.37175);
#20290=CYLINDRICAL_SURFACE('',#23016,2.37175);
#20291=CYLINDRICAL_SURFACE('',#23017,2.37175);
#20292=CYLINDRICAL_SURFACE('',#23018,2.37175);
#20293=CYLINDRICAL_SURFACE('',#23019,2.37175);
#20294=CYLINDRICAL_SURFACE('',#23020,2.37175);
#20295=CYLINDRICAL_SURFACE('',#23021,2.37175);
#20296=CYLINDRICAL_SURFACE('',#23022,2.37175);
#20297=CYLINDRICAL_SURFACE('',#23026,2.37175);
#20298=CYLINDRICAL_SURFACE('',#23028,2.942);
#20299=CYLINDRICAL_SURFACE('',#23038,5.);
#20300=CYLINDRICAL_SURFACE('',#23043,2.5175);
#20301=CYLINDRICAL_SURFACE('',#23045,2.5175);
#20302=CYLINDRICAL_SURFACE('',#23046,2.5175);
#20303=CYLINDRICAL_SURFACE('',#23047,2.5175);
#20304=CYLINDRICAL_SURFACE('',#23048,2.5175);
#20305=CYLINDRICAL_SURFACE('',#23049,2.5175);
#20306=CYLINDRICAL_SURFACE('',#23050,2.5175);
#20307=CYLINDRICAL_SURFACE('',#23051,2.5175);
#20308=CYLINDRICAL_SURFACE('',#23052,2.5175);
#20309=CYLINDRICAL_SURFACE('',#23053,2.5175);
#20310=CYLINDRICAL_SURFACE('',#23054,2.5175);
#20311=CYLINDRICAL_SURFACE('',#23055,2.5175);
#20312=CYLINDRICAL_SURFACE('',#23056,2.5175);
#20313=CYLINDRICAL_SURFACE('',#23057,2.5175);
#20314=CYLINDRICAL_SURFACE('',#23058,2.5175);
#20315=CYLINDRICAL_SURFACE('',#23059,2.5175);
#20316=CYLINDRICAL_SURFACE('',#23060,2.5175);
#20317=CYLINDRICAL_SURFACE('',#23061,2.5175);
#20318=CYLINDRICAL_SURFACE('',#23062,2.5175);
#20319=CYLINDRICAL_SURFACE('',#23063,2.5175);
#20320=CYLINDRICAL_SURFACE('',#23065,2.5175);
#20321=CYLINDRICAL_SURFACE('',#23067,2.5175);
#20322=CYLINDRICAL_SURFACE('',#23068,2.5175);
#20323=CYLINDRICAL_SURFACE('',#23069,2.5175);
#20324=CYLINDRICAL_SURFACE('',#23070,2.5175);
#20325=CYLINDRICAL_SURFACE('',#23071,2.5175);
#20326=CYLINDRICAL_SURFACE('',#23072,2.5175);
#20327=CYLINDRICAL_SURFACE('',#23073,2.5175);
#20328=CYLINDRICAL_SURFACE('',#23074,2.5175);
#20329=CYLINDRICAL_SURFACE('',#23075,2.5175);
#20330=CYLINDRICAL_SURFACE('',#23076,2.5175);
#20331=CYLINDRICAL_SURFACE('',#23077,2.5175);
#20332=CYLINDRICAL_SURFACE('',#23078,2.5175);
#20333=CYLINDRICAL_SURFACE('',#23079,2.5175);
#20334=CYLINDRICAL_SURFACE('',#23080,2.5175);
#20335=CYLINDRICAL_SURFACE('',#23081,2.5175);
#20336=CYLINDRICAL_SURFACE('',#23082,2.5175);
#20337=CYLINDRICAL_SURFACE('',#23083,2.5175);
#20338=CYLINDRICAL_SURFACE('',#23084,2.5175);
#20339=CYLINDRICAL_SURFACE('',#23085,2.5175);
#20340=CYLINDRICAL_SURFACE('',#23087,2.5175);
#20341=CYLINDRICAL_SURFACE('',#23089,2.5175);
#20342=CYLINDRICAL_SURFACE('',#23090,2.5175);
#20343=CYLINDRICAL_SURFACE('',#23091,2.5175);
#20344=CYLINDRICAL_SURFACE('',#23092,2.5175);
#20345=CYLINDRICAL_SURFACE('',#23093,2.5175);
#20346=CYLINDRICAL_SURFACE('',#23094,2.5175);
#20347=CYLINDRICAL_SURFACE('',#23095,2.5175);
#20348=CYLINDRICAL_SURFACE('',#23096,2.5175);
#20349=CYLINDRICAL_SURFACE('',#23097,2.5175);
#20350=CYLINDRICAL_SURFACE('',#23098,2.5175);
#20351=CYLINDRICAL_SURFACE('',#23099,2.5175);
#20352=CYLINDRICAL_SURFACE('',#23100,2.5175);
#20353=CYLINDRICAL_SURFACE('',#23101,2.5175);
#20354=CYLINDRICAL_SURFACE('',#23102,2.5175);
#20355=CYLINDRICAL_SURFACE('',#23103,2.5175);
#20356=CYLINDRICAL_SURFACE('',#23104,2.5175);
#20357=CYLINDRICAL_SURFACE('',#23105,2.5175);
#20358=CYLINDRICAL_SURFACE('',#23106,2.5175);
#20359=CYLINDRICAL_SURFACE('',#23107,2.5175);
#20360=CYLINDRICAL_SURFACE('',#23109,2.5175);
#20361=CYLINDRICAL_SURFACE('',#23111,2.5175);
#20362=CYLINDRICAL_SURFACE('',#23112,2.5175);
#20363=CYLINDRICAL_SURFACE('',#23113,2.5175);
#20364=CYLINDRICAL_SURFACE('',#23114,2.5175);
#20365=CYLINDRICAL_SURFACE('',#23115,2.5175);
#20366=CYLINDRICAL_SURFACE('',#23116,2.5175);
#20367=CYLINDRICAL_SURFACE('',#23117,2.5175);
#20368=CYLINDRICAL_SURFACE('',#23118,2.5175);
#20369=CYLINDRICAL_SURFACE('',#23119,2.5175);
#20370=CYLINDRICAL_SURFACE('',#23120,2.5175);
#20371=CYLINDRICAL_SURFACE('',#23121,2.5175);
#20372=CYLINDRICAL_SURFACE('',#23122,2.5175);
#20373=CYLINDRICAL_SURFACE('',#23123,2.5175);
#20374=CYLINDRICAL_SURFACE('',#23124,2.5175);
#20375=CYLINDRICAL_SURFACE('',#23125,2.5175);
#20376=CYLINDRICAL_SURFACE('',#23126,2.5175);
#20377=CYLINDRICAL_SURFACE('',#23127,2.5175);
#20378=CYLINDRICAL_SURFACE('',#23128,2.5175);
#20379=CYLINDRICAL_SURFACE('',#23129,2.5175);
#20380=CYLINDRICAL_SURFACE('',#23131,2.5175);
#20381=CYLINDRICAL_SURFACE('',#23133,2.5175);
#20382=CYLINDRICAL_SURFACE('',#23134,2.5175);
#20383=CYLINDRICAL_SURFACE('',#23135,2.5175);
#20384=CYLINDRICAL_SURFACE('',#23136,2.5175);
#20385=CYLINDRICAL_SURFACE('',#23137,2.5175);
#20386=CYLINDRICAL_SURFACE('',#23138,2.5175);
#20387=CYLINDRICAL_SURFACE('',#23139,2.5175);
#20388=CYLINDRICAL_SURFACE('',#23140,2.5175);
#20389=CYLINDRICAL_SURFACE('',#23141,2.5175);
#20390=CYLINDRICAL_SURFACE('',#23142,2.5175);
#20391=CYLINDRICAL_SURFACE('',#23143,2.5175);
#20392=CYLINDRICAL_SURFACE('',#23144,2.5175);
#20393=CYLINDRICAL_SURFACE('',#23145,2.5175);
#20394=CYLINDRICAL_SURFACE('',#23146,2.5175);
#20395=CYLINDRICAL_SURFACE('',#23147,2.5175);
#20396=CYLINDRICAL_SURFACE('',#23148,2.5175);
#20397=CYLINDRICAL_SURFACE('',#23149,2.5175);
#20398=CYLINDRICAL_SURFACE('',#23150,2.5175);
#20399=CYLINDRICAL_SURFACE('',#23151,2.5175);
#20400=CYLINDRICAL_SURFACE('',#23153,2.5175);
#20401=CYLINDRICAL_SURFACE('',#23155,2.5175);
#20402=CYLINDRICAL_SURFACE('',#23156,2.5175);
#20403=CYLINDRICAL_SURFACE('',#23157,2.5175);
#20404=CYLINDRICAL_SURFACE('',#23158,2.5175);
#20405=CYLINDRICAL_SURFACE('',#23159,2.5175);
#20406=CYLINDRICAL_SURFACE('',#23160,2.5175);
#20407=CYLINDRICAL_SURFACE('',#23161,2.5175);
#20408=CYLINDRICAL_SURFACE('',#23162,2.5175);
#20409=CYLINDRICAL_SURFACE('',#23163,2.5175);
#20410=CYLINDRICAL_SURFACE('',#23164,2.5175);
#20411=CYLINDRICAL_SURFACE('',#23165,2.5175);
#20412=CYLINDRICAL_SURFACE('',#23166,2.5175);
#20413=CYLINDRICAL_SURFACE('',#23167,2.5175);
#20414=CYLINDRICAL_SURFACE('',#23168,2.5175);
#20415=CYLINDRICAL_SURFACE('',#23169,2.5175);
#20416=CYLINDRICAL_SURFACE('',#23170,2.5175);
#20417=CYLINDRICAL_SURFACE('',#23171,2.5175);
#20418=CYLINDRICAL_SURFACE('',#23172,2.5175);
#20419=CYLINDRICAL_SURFACE('',#23173,2.5175);
#20420=CYLINDRICAL_SURFACE('',#23175,3.0735);
#20421=CYLINDRICAL_SURFACE('',#23177,3.0735);
#20422=CYLINDRICAL_SURFACE('',#23178,3.0735);
#20423=CYLINDRICAL_SURFACE('',#23179,3.0735);
#20424=CYLINDRICAL_SURFACE('',#23180,3.0735);
#20425=CYLINDRICAL_SURFACE('',#23181,3.0735);
#20426=CYLINDRICAL_SURFACE('',#23182,3.0735);
#20427=CYLINDRICAL_SURFACE('',#23183,3.0735);
#20428=CYLINDRICAL_SURFACE('',#23184,3.0735);
#20429=CYLINDRICAL_SURFACE('',#23185,3.0735);
#20430=CYLINDRICAL_SURFACE('',#23186,3.0735);
#20431=CYLINDRICAL_SURFACE('',#23187,3.0735);
#20432=CYLINDRICAL_SURFACE('',#23188,3.0735);
#20433=CYLINDRICAL_SURFACE('',#23189,3.0735);
#20434=CYLINDRICAL_SURFACE('',#23190,3.0735);
#20435=CYLINDRICAL_SURFACE('',#23191,3.0735);
#20436=CYLINDRICAL_SURFACE('',#23192,3.0735);
#20437=CYLINDRICAL_SURFACE('',#23193,3.0735);
#20438=CYLINDRICAL_SURFACE('',#23194,3.0735);
#20439=CYLINDRICAL_SURFACE('',#23195,3.0735);
#20440=CYLINDRICAL_SURFACE('',#23197,3.0735);
#20441=CYLINDRICAL_SURFACE('',#23199,3.0735);
#20442=CYLINDRICAL_SURFACE('',#23200,3.0735);
#20443=CYLINDRICAL_SURFACE('',#23201,3.0735);
#20444=CYLINDRICAL_SURFACE('',#23202,3.0735);
#20445=CYLINDRICAL_SURFACE('',#23203,3.0735);
#20446=CYLINDRICAL_SURFACE('',#23204,3.0735);
#20447=CYLINDRICAL_SURFACE('',#23205,3.0735);
#20448=CYLINDRICAL_SURFACE('',#23206,3.0735);
#20449=CYLINDRICAL_SURFACE('',#23207,3.0735);
#20450=CYLINDRICAL_SURFACE('',#23208,3.0735);
#20451=CYLINDRICAL_SURFACE('',#23209,3.0735);
#20452=CYLINDRICAL_SURFACE('',#23210,3.0735);
#20453=CYLINDRICAL_SURFACE('',#23211,3.0735);
#20454=CYLINDRICAL_SURFACE('',#23212,3.0735);
#20455=CYLINDRICAL_SURFACE('',#23213,3.0735);
#20456=CYLINDRICAL_SURFACE('',#23214,3.0735);
#20457=CYLINDRICAL_SURFACE('',#23215,3.0735);
#20458=CYLINDRICAL_SURFACE('',#23216,3.0735);
#20459=CYLINDRICAL_SURFACE('',#23217,3.0735);
#20460=CYLINDRICAL_SURFACE('',#23219,3.07349999999996);
#20461=CYLINDRICAL_SURFACE('',#23221,3.07349999999996);
#20462=CYLINDRICAL_SURFACE('',#23222,3.07349999999996);
#20463=CYLINDRICAL_SURFACE('',#23223,3.07349999999996);
#20464=CYLINDRICAL_SURFACE('',#23224,3.07349999999996);
#20465=CYLINDRICAL_SURFACE('',#23225,3.07349999999996);
#20466=CYLINDRICAL_SURFACE('',#23226,3.07349999999996);
#20467=CYLINDRICAL_SURFACE('',#23227,3.07349999999996);
#20468=CYLINDRICAL_SURFACE('',#23228,3.07349999999996);
#20469=CYLINDRICAL_SURFACE('',#23229,3.07349999999996);
#20470=CYLINDRICAL_SURFACE('',#23230,3.07349999999996);
#20471=CYLINDRICAL_SURFACE('',#23231,3.07349999999996);
#20472=CYLINDRICAL_SURFACE('',#23232,3.07349999999996);
#20473=CYLINDRICAL_SURFACE('',#23233,3.07349999999996);
#20474=CYLINDRICAL_SURFACE('',#23234,3.07349999999996);
#20475=CYLINDRICAL_SURFACE('',#23235,3.07349999999996);
#20476=CYLINDRICAL_SURFACE('',#23236,3.07349999999996);
#20477=CYLINDRICAL_SURFACE('',#23237,3.07349999999996);
#20478=CYLINDRICAL_SURFACE('',#23238,3.07349999999996);
#20479=CYLINDRICAL_SURFACE('',#23239,3.07349999999996);
#20480=CYLINDRICAL_SURFACE('',#23241,3.07349999999996);
#20481=CYLINDRICAL_SURFACE('',#23243,3.07349999999996);
#20482=CYLINDRICAL_SURFACE('',#23244,3.07349999999996);
#20483=CYLINDRICAL_SURFACE('',#23245,3.07349999999996);
#20484=CYLINDRICAL_SURFACE('',#23246,3.07349999999996);
#20485=CYLINDRICAL_SURFACE('',#23247,3.07349999999996);
#20486=CYLINDRICAL_SURFACE('',#23248,3.07349999999996);
#20487=CYLINDRICAL_SURFACE('',#23249,3.07349999999996);
#20488=CYLINDRICAL_SURFACE('',#23250,3.07349999999996);
#20489=CYLINDRICAL_SURFACE('',#23251,3.07349999999996);
#20490=CYLINDRICAL_SURFACE('',#23252,3.07349999999996);
#20491=CYLINDRICAL_SURFACE('',#23253,3.07349999999996);
#20492=CYLINDRICAL_SURFACE('',#23254,3.07349999999996);
#20493=CYLINDRICAL_SURFACE('',#23255,3.07349999999996);
#20494=CYLINDRICAL_SURFACE('',#23256,3.07349999999996);
#20495=CYLINDRICAL_SURFACE('',#23257,3.07349999999996);
#20496=CYLINDRICAL_SURFACE('',#23258,3.07349999999996);
#20497=CYLINDRICAL_SURFACE('',#23259,3.07349999999996);
#20498=CYLINDRICAL_SURFACE('',#23260,3.07349999999996);
#20499=CYLINDRICAL_SURFACE('',#23261,3.07349999999996);
#20500=CYLINDRICAL_SURFACE('',#23263,3.0735);
#20501=CYLINDRICAL_SURFACE('',#23265,3.0735);
#20502=CYLINDRICAL_SURFACE('',#23266,3.0735);
#20503=CYLINDRICAL_SURFACE('',#23267,3.0735);
#20504=CYLINDRICAL_SURFACE('',#23268,3.0735);
#20505=CYLINDRICAL_SURFACE('',#23269,3.0735);
#20506=CYLINDRICAL_SURFACE('',#23270,3.0735);
#20507=CYLINDRICAL_SURFACE('',#23271,3.0735);
#20508=CYLINDRICAL_SURFACE('',#23272,3.0735);
#20509=CYLINDRICAL_SURFACE('',#23273,3.0735);
#20510=CYLINDRICAL_SURFACE('',#23274,3.0735);
#20511=CYLINDRICAL_SURFACE('',#23275,3.0735);
#20512=CYLINDRICAL_SURFACE('',#23276,3.0735);
#20513=CYLINDRICAL_SURFACE('',#23277,3.0735);
#20514=CYLINDRICAL_SURFACE('',#23278,3.0735);
#20515=CYLINDRICAL_SURFACE('',#23279,3.0735);
#20516=CYLINDRICAL_SURFACE('',#23280,3.0735);
#20517=CYLINDRICAL_SURFACE('',#23281,3.0735);
#20518=CYLINDRICAL_SURFACE('',#23282,3.0735);
#20519=CYLINDRICAL_SURFACE('',#23283,3.0735);
#20520=CYLINDRICAL_SURFACE('',#23285,3.0735);
#20521=CYLINDRICAL_SURFACE('',#23287,3.0735);
#20522=CYLINDRICAL_SURFACE('',#23288,3.0735);
#20523=CYLINDRICAL_SURFACE('',#23289,3.0735);
#20524=CYLINDRICAL_SURFACE('',#23290,3.0735);
#20525=CYLINDRICAL_SURFACE('',#23291,3.0735);
#20526=CYLINDRICAL_SURFACE('',#23292,3.0735);
#20527=CYLINDRICAL_SURFACE('',#23293,3.0735);
#20528=CYLINDRICAL_SURFACE('',#23294,3.0735);
#20529=CYLINDRICAL_SURFACE('',#23295,3.0735);
#20530=CYLINDRICAL_SURFACE('',#23296,3.0735);
#20531=CYLINDRICAL_SURFACE('',#23297,3.0735);
#20532=CYLINDRICAL_SURFACE('',#23298,3.0735);
#20533=CYLINDRICAL_SURFACE('',#23299,3.0735);
#20534=CYLINDRICAL_SURFACE('',#23300,3.0735);
#20535=CYLINDRICAL_SURFACE('',#23301,3.0735);
#20536=CYLINDRICAL_SURFACE('',#23302,3.0735);
#20537=CYLINDRICAL_SURFACE('',#23303,3.0735);
#20538=CYLINDRICAL_SURFACE('',#23304,3.0735);
#20539=CYLINDRICAL_SURFACE('',#23305,3.0735);
#20540=CYLINDRICAL_SURFACE('',#23307,3.0735);
#20541=CYLINDRICAL_SURFACE('',#23309,3.0735);
#20542=CYLINDRICAL_SURFACE('',#23310,3.07349999999996);
#20543=CYLINDRICAL_SURFACE('',#23311,3.07349999999996);
#20544=CYLINDRICAL_SURFACE('',#23312,3.0735);
#20545=CYLINDRICAL_SURFACE('',#23313,3.0735);
#20546=CYLINDRICAL_SURFACE('',#23314,2.5175);
#20547=CYLINDRICAL_SURFACE('',#23315,2.5175);
#20548=CYLINDRICAL_SURFACE('',#23316,2.5175);
#20549=CYLINDRICAL_SURFACE('',#23317,2.5175);
#20550=CYLINDRICAL_SURFACE('',#23318,2.5175);
#20551=CYLINDRICAL_SURFACE('',#23319,2.5175);
#20552=CYLINDRICAL_SURFACE('',#23326,2.942);
#20553=CYLINDRICAL_SURFACE('',#23328,2.942);
#20554=CYLINDRICAL_SURFACE('',#23329,2.942);
#20555=CYLINDRICAL_SURFACE('',#23330,2.942);
#20556=CYLINDRICAL_SURFACE('',#23331,2.942);
#20557=CYLINDRICAL_SURFACE('',#23332,2.942);
#20558=CYLINDRICAL_SURFACE('',#23333,2.942);
#20559=CYLINDRICAL_SURFACE('',#23334,2.942);
#20560=CYLINDRICAL_SURFACE('',#23335,2.942);
#20561=CYLINDRICAL_SURFACE('',#23336,2.942);
#20562=CYLINDRICAL_SURFACE('',#23337,2.942);
#20563=CYLINDRICAL_SURFACE('',#23338,2.942);
#20564=CYLINDRICAL_SURFACE('',#23339,2.942);
#20565=CYLINDRICAL_SURFACE('',#23340,2.942);
#20566=CYLINDRICAL_SURFACE('',#23341,2.942);
#20567=CYLINDRICAL_SURFACE('',#23342,2.942);
#20568=CYLINDRICAL_SURFACE('',#23343,2.942);
#20569=CYLINDRICAL_SURFACE('',#23344,2.942);
#20570=CYLINDRICAL_SURFACE('',#23345,2.942);
#20571=CYLINDRICAL_SURFACE('',#23346,2.942);
#20572=CYLINDRICAL_SURFACE('',#23347,2.942);
#20573=CYLINDRICAL_SURFACE('',#23348,2.942);
#20574=CYLINDRICAL_SURFACE('',#23349,2.942);
#20575=CYLINDRICAL_SURFACE('',#23350,2.942);
#20576=CYLINDRICAL_SURFACE('',#23351,2.942);
#20577=CYLINDRICAL_SURFACE('',#23352,2.942);
#20578=CYLINDRICAL_SURFACE('',#23353,2.942);
#20579=CYLINDRICAL_SURFACE('',#23354,2.942);
#20580=CYLINDRICAL_SURFACE('',#23355,2.942);
#20581=CYLINDRICAL_SURFACE('',#23356,2.942);
#20582=CYLINDRICAL_SURFACE('',#23357,2.942);
#20583=CYLINDRICAL_SURFACE('',#23358,2.942);
#20584=CYLINDRICAL_SURFACE('',#23359,2.942);
#20585=CYLINDRICAL_SURFACE('',#23360,2.942);
#20586=CYLINDRICAL_SURFACE('',#23361,2.942);
#20587=CYLINDRICAL_SURFACE('',#23362,2.942);
#20588=CYLINDRICAL_SURFACE('',#23363,2.942);
#20589=CYLINDRICAL_SURFACE('',#23364,2.942);
#20590=CYLINDRICAL_SURFACE('',#23365,2.942);
#20591=CYLINDRICAL_SURFACE('',#23366,2.942);
#20592=CYLINDRICAL_SURFACE('',#23367,2.942);
#20593=CYLINDRICAL_SURFACE('',#23368,2.942);
#20594=CYLINDRICAL_SURFACE('',#23369,2.942);
#20595=CYLINDRICAL_SURFACE('',#23370,2.942);
#20596=CYLINDRICAL_SURFACE('',#23371,2.942);
#20597=CYLINDRICAL_SURFACE('',#23372,2.942);
#20598=CYLINDRICAL_SURFACE('',#23373,2.942);
#20599=CYLINDRICAL_SURFACE('',#23374,2.942);
#20600=CYLINDRICAL_SURFACE('',#23375,2.942);
#20601=CYLINDRICAL_SURFACE('',#23376,2.37175);
#20602=CYLINDRICAL_SURFACE('',#23378,2.37175);
#20603=CYLINDRICAL_SURFACE('',#23379,2.37175);
#20604=CYLINDRICAL_SURFACE('',#23380,2.37175);
#20605=CYLINDRICAL_SURFACE('',#23381,2.37175);
#20606=CYLINDRICAL_SURFACE('',#23382,2.37175);
#20607=CYLINDRICAL_SURFACE('',#23383,2.37175);
#20608=CYLINDRICAL_SURFACE('',#23384,2.37175);
#20609=CYLINDRICAL_SURFACE('',#23385,2.37175);
#20610=CYLINDRICAL_SURFACE('',#23386,2.37175);
#20611=CYLINDRICAL_SURFACE('',#23387,2.37175);
#20612=CYLINDRICAL_SURFACE('',#23388,2.37175);
#20613=CYLINDRICAL_SURFACE('',#23389,2.37175);
#20614=CYLINDRICAL_SURFACE('',#23390,2.37175);
#20615=CYLINDRICAL_SURFACE('',#23391,2.37175);
#20616=CYLINDRICAL_SURFACE('',#23392,2.37175);
#20617=CYLINDRICAL_SURFACE('',#23393,2.37175);
#20618=CYLINDRICAL_SURFACE('',#23394,2.37175);
#20619=CYLINDRICAL_SURFACE('',#23395,2.37175);
#20620=CYLINDRICAL_SURFACE('',#23396,2.37175);
#20621=CYLINDRICAL_SURFACE('',#23397,2.37175);
#20622=CYLINDRICAL_SURFACE('',#23398,2.37175);
#20623=CYLINDRICAL_SURFACE('',#23399,2.37175);
#20624=CYLINDRICAL_SURFACE('',#23400,2.37175);
#20625=CYLINDRICAL_SURFACE('',#23401,2.37175);
#20626=CYLINDRICAL_SURFACE('',#23402,2.37175);
#20627=CYLINDRICAL_SURFACE('',#23403,2.37175);
#20628=CYLINDRICAL_SURFACE('',#23404,2.37175);
#20629=CYLINDRICAL_SURFACE('',#23405,2.37175);
#20630=CYLINDRICAL_SURFACE('',#23406,2.37175);
#20631=CYLINDRICAL_SURFACE('',#23407,2.37175);
#20632=CYLINDRICAL_SURFACE('',#23408,2.37175);
#20633=CYLINDRICAL_SURFACE('',#23409,2.37175);
#20634=CYLINDRICAL_SURFACE('',#23410,2.37175);
#20635=CYLINDRICAL_SURFACE('',#23411,2.37175);
#20636=CYLINDRICAL_SURFACE('',#23412,2.37175);
#20637=CYLINDRICAL_SURFACE('',#23413,2.37175);
#20638=CYLINDRICAL_SURFACE('',#23414,2.37175);
#20639=CYLINDRICAL_SURFACE('',#23415,2.37175);
#20640=CYLINDRICAL_SURFACE('',#23416,2.37175);
#20641=CYLINDRICAL_SURFACE('',#23417,2.37175);
#20642=CYLINDRICAL_SURFACE('',#23418,2.37175);
#20643=CYLINDRICAL_SURFACE('',#23419,2.37175);
#20644=CYLINDRICAL_SURFACE('',#23420,2.37175);
#20645=CYLINDRICAL_SURFACE('',#23421,2.37175);
#20646=CYLINDRICAL_SURFACE('',#23422,2.37175);
#20647=CYLINDRICAL_SURFACE('',#23423,2.37175);
#20648=CYLINDRICAL_SURFACE('',#23424,2.37175);
#20649=CYLINDRICAL_SURFACE('',#23425,2.37175);
#20650=CYLINDRICAL_SURFACE('',#23429,2.37175);
#20651=CYLINDRICAL_SURFACE('',#23431,2.942);
#20652=CYLINDRICAL_SURFACE('',#23441,5.);
#20653=CYLINDRICAL_SURFACE('',#23446,3.5);
#20654=CYLINDRICAL_SURFACE('',#23449,6.);
#20655=CYLINDRICAL_SURFACE('',#23455,3.5);
#20656=CYLINDRICAL_SURFACE('',#23458,7.);
#20657=ADVANCED_FACE('',(#2537),#19710,.F.);
#20658=ADVANCED_FACE('',(#2538),#19711,.F.);
#20659=ADVANCED_FACE('',(#2539),#19712,.F.);
#20660=ADVANCED_FACE('',(#2540),#19713,.F.);
#20661=ADVANCED_FACE('',(#2541),#19714,.F.);
#20662=ADVANCED_FACE('',(#2542),#19715,.F.);
#20663=ADVANCED_FACE('',(#2543),#2379,.T.);
#20664=ADVANCED_FACE('',(#2544,#2288,#2289,#2290),#2380,.T.);
#20665=ADVANCED_FACE('',(#2545),#2381,.T.);
#20666=ADVANCED_FACE('',(#2546,#2291,#2292,#2293),#2382,.T.);
#20667=ADVANCED_FACE('',(#2547),#2383,.T.);
#20668=ADVANCED_FACE('',(#2548,#2294,#2295,#2296),#2384,.T.);
#20669=ADVANCED_FACE('',(#2549),#2385,.T.);
#20670=ADVANCED_FACE('',(#2550,#2297,#2298,#2299),#2386,.T.);
#20671=ADVANCED_FACE('',(#2551,#2300),#2387,.T.);
#20672=ADVANCED_FACE('',(#2552,#2301),#2388,.F.);
#20673=ADVANCED_FACE('',(#2553),#2389,.T.);
#20674=ADVANCED_FACE('',(#2554),#2390,.T.);
#20675=ADVANCED_FACE('',(#2555),#2391,.T.);
#20676=ADVANCED_FACE('',(#2556),#2392,.T.);
#20677=ADVANCED_FACE('',(#2557),#2393,.T.);
#20678=ADVANCED_FACE('',(#2558),#2394,.T.);
#20679=ADVANCED_FACE('',(#2559),#2395,.T.);
#20680=ADVANCED_FACE('',(#2560),#2396,.T.);
#20681=ADVANCED_FACE('',(#2561,#2302),#2397,.T.);
#20682=ADVANCED_FACE('',(#2562,#2303),#2398,.F.);
#20683=ADVANCED_FACE('',(#2563),#19716,.F.);
#20684=ADVANCED_FACE('',(#2564),#19717,.F.);
#20685=ADVANCED_FACE('',(#2565),#19718,.F.);
#20686=ADVANCED_FACE('',(#2566),#19719,.F.);
#20687=ADVANCED_FACE('',(#2567),#19720,.F.);
#20688=ADVANCED_FACE('',(#2568),#19721,.F.);
#20689=ADVANCED_FACE('',(#2569),#19722,.F.);
#20690=ADVANCED_FACE('',(#2570),#19723,.F.);
#20691=ADVANCED_FACE('',(#2571),#19724,.F.);
#20692=ADVANCED_FACE('',(#2572),#19725,.F.);
#20693=ADVANCED_FACE('',(#2573),#19726,.F.);
#20694=ADVANCED_FACE('',(#2574),#19727,.F.);
#20695=ADVANCED_FACE('',(#2575),#19728,.F.);
#20696=ADVANCED_FACE('',(#2576),#19729,.F.);
#20697=ADVANCED_FACE('',(#2577),#19730,.F.);
#20698=ADVANCED_FACE('',(#2578),#19731,.F.);
#20699=ADVANCED_FACE('',(#2579),#19732,.F.);
#20700=ADVANCED_FACE('',(#2580),#19733,.F.);
#20701=ADVANCED_FACE('',(#2581),#19734,.F.);
#20702=ADVANCED_FACE('',(#2582),#19735,.F.);
#20703=ADVANCED_FACE('',(#2583),#19736,.F.);
#20704=ADVANCED_FACE('',(#2584),#19737,.F.);
#20705=ADVANCED_FACE('',(#2585),#19738,.F.);
#20706=ADVANCED_FACE('',(#2586),#19739,.F.);
#20707=ADVANCED_FACE('',(#2587),#19740,.F.);
#20708=ADVANCED_FACE('',(#2588),#19741,.F.);
#20709=ADVANCED_FACE('',(#2589),#19742,.F.);
#20710=ADVANCED_FACE('',(#2590),#19743,.F.);
#20711=ADVANCED_FACE('',(#2591),#19744,.F.);
#20712=ADVANCED_FACE('',(#2592),#19745,.F.);
#20713=ADVANCED_FACE('',(#2593),#19746,.F.);
#20714=ADVANCED_FACE('',(#2594),#19747,.F.);
#20715=ADVANCED_FACE('',(#2595),#19748,.F.);
#20716=ADVANCED_FACE('',(#2596),#19749,.F.);
#20717=ADVANCED_FACE('',(#2597),#19750,.F.);
#20718=ADVANCED_FACE('',(#2598),#19751,.F.);
#20719=ADVANCED_FACE('',(#2599),#19752,.F.);
#20720=ADVANCED_FACE('',(#2600),#19753,.F.);
#20721=ADVANCED_FACE('',(#2601),#19754,.F.);
#20722=ADVANCED_FACE('',(#2602),#19755,.F.);
#20723=ADVANCED_FACE('',(#2603),#19756,.F.);
#20724=ADVANCED_FACE('',(#2604),#19757,.F.);
#20725=ADVANCED_FACE('',(#2605),#19758,.F.);
#20726=ADVANCED_FACE('',(#2606),#19759,.F.);
#20727=ADVANCED_FACE('',(#2607),#19760,.F.);
#20728=ADVANCED_FACE('',(#2608),#19761,.F.);
#20729=ADVANCED_FACE('',(#2609),#19762,.F.);
#20730=ADVANCED_FACE('',(#2610),#19763,.F.);
#20731=ADVANCED_FACE('',(#2611),#19764,.F.);
#20732=ADVANCED_FACE('',(#2612),#19765,.F.);
#20733=ADVANCED_FACE('',(#2613),#19766,.F.);
#20734=ADVANCED_FACE('',(#2614),#19767,.F.);
#20735=ADVANCED_FACE('',(#2615),#19768,.F.);
#20736=ADVANCED_FACE('',(#2616),#19769,.F.);
#20737=ADVANCED_FACE('',(#2617),#19770,.F.);
#20738=ADVANCED_FACE('',(#2618),#19771,.F.);
#20739=ADVANCED_FACE('',(#2619),#19772,.F.);
#20740=ADVANCED_FACE('',(#2620),#19773,.F.);
#20741=ADVANCED_FACE('',(#2621),#19774,.F.);
#20742=ADVANCED_FACE('',(#2622),#19775,.F.);
#20743=ADVANCED_FACE('',(#2623),#19776,.F.);
#20744=ADVANCED_FACE('',(#2624),#19777,.F.);
#20745=ADVANCED_FACE('',(#2625),#19778,.F.);
#20746=ADVANCED_FACE('',(#2626),#19779,.F.);
#20747=ADVANCED_FACE('',(#2627),#19780,.F.);
#20748=ADVANCED_FACE('',(#2628),#334,.F.);
#20749=ADVANCED_FACE('',(#2629),#335,.F.);
#20750=ADVANCED_FACE('',(#2630,#2304,#2305,#2306,#2307),#2399,.T.);
#20751=ADVANCED_FACE('',(#2631),#19781,.F.);
#20752=ADVANCED_FACE('',(#2632),#336,.F.);
#20753=ADVANCED_FACE('',(#2633),#337,.F.);
#20754=ADVANCED_FACE('',(#2634),#19782,.F.);
#20755=ADVANCED_FACE('',(#2635),#338,.F.);
#20756=ADVANCED_FACE('',(#2636),#339,.F.);
#20757=ADVANCED_FACE('',(#2637),#19783,.F.);
#20758=ADVANCED_FACE('',(#2638),#340,.F.);
#20759=ADVANCED_FACE('',(#2639),#341,.F.);
#20760=ADVANCED_FACE('',(#2640),#19784,.F.);
#20761=ADVANCED_FACE('',(#2641),#19785,.F.);
#20762=ADVANCED_FACE('',(#2642),#19786,.F.);
#20763=ADVANCED_FACE('',(#2643),#19787,.F.);
#20764=ADVANCED_FACE('',(#2644),#2400,.T.);
#20765=ADVANCED_FACE('',(#2645),#2401,.T.);
#20766=ADVANCED_FACE('',(#2646),#2402,.T.);
#20767=ADVANCED_FACE('',(#2647),#2403,.T.);
#20768=ADVANCED_FACE('',(#2648,#2308,#2309,#2310,#2311),#2404,.F.);
#20769=ADVANCED_FACE('',(#2649),#19788,.T.);
#20770=ADVANCED_FACE('',(#2650),#19789,.T.);
#20771=ADVANCED_FACE('',(#2651),#19790,.T.);
#20772=ADVANCED_FACE('',(#2652),#19791,.T.);
#20773=ADVANCED_FACE('',(#2653),#19792,.T.);
#20774=ADVANCED_FACE('',(#2654),#19793,.T.);
#20775=ADVANCED_FACE('',(#2655),#19794,.T.);
#20776=ADVANCED_FACE('',(#2656),#19795,.T.);
#20777=ADVANCED_FACE('',(#2657),#19796,.T.);
#20778=ADVANCED_FACE('',(#2658),#19797,.T.);
#20779=ADVANCED_FACE('',(#2659),#19798,.T.);
#20780=ADVANCED_FACE('',(#2660),#19799,.T.);
#20781=ADVANCED_FACE('',(#2661),#19800,.T.);
#20782=ADVANCED_FACE('',(#2662),#19801,.T.);
#20783=ADVANCED_FACE('',(#2663),#19802,.T.);
#20784=ADVANCED_FACE('',(#2664),#19803,.T.);
#20785=ADVANCED_FACE('',(#2665),#19804,.T.);
#20786=ADVANCED_FACE('',(#2666),#19805,.T.);
#20787=ADVANCED_FACE('',(#2667),#19806,.T.);
#20788=ADVANCED_FACE('',(#2668),#19807,.T.);
#20789=ADVANCED_FACE('',(#2669),#19808,.T.);
#20790=ADVANCED_FACE('',(#2670),#19809,.T.);
#20791=ADVANCED_FACE('',(#2671),#19810,.T.);
#20792=ADVANCED_FACE('',(#2672),#19811,.T.);
#20793=ADVANCED_FACE('',(#2673),#19812,.T.);
#20794=ADVANCED_FACE('',(#2674),#19813,.T.);
#20795=ADVANCED_FACE('',(#2675),#19814,.T.);
#20796=ADVANCED_FACE('',(#2676),#19815,.T.);
#20797=ADVANCED_FACE('',(#2677),#19816,.T.);
#20798=ADVANCED_FACE('',(#2678),#19817,.T.);
#20799=ADVANCED_FACE('',(#2679),#19818,.T.);
#20800=ADVANCED_FACE('',(#2680),#19819,.T.);
#20801=ADVANCED_FACE('',(#2681),#19820,.T.);
#20802=ADVANCED_FACE('',(#2682),#19821,.T.);
#20803=ADVANCED_FACE('',(#2683),#19822,.T.);
#20804=ADVANCED_FACE('',(#2684),#19823,.T.);
#20805=ADVANCED_FACE('',(#2685),#19824,.T.);
#20806=ADVANCED_FACE('',(#2686),#19825,.T.);
#20807=ADVANCED_FACE('',(#2687),#19826,.T.);
#20808=ADVANCED_FACE('',(#2688),#19827,.T.);
#20809=ADVANCED_FACE('',(#2689),#19828,.T.);
#20810=ADVANCED_FACE('',(#2690),#19829,.T.);
#20811=ADVANCED_FACE('',(#2691),#19830,.T.);
#20812=ADVANCED_FACE('',(#2692),#19831,.T.);
#20813=ADVANCED_FACE('',(#2693),#19832,.T.);
#20814=ADVANCED_FACE('',(#2694),#19833,.T.);
#20815=ADVANCED_FACE('',(#2695),#19834,.T.);
#20816=ADVANCED_FACE('',(#2696),#19835,.T.);
#20817=ADVANCED_FACE('',(#2697),#330,.T.);
#20818=ADVANCED_FACE('',(#2698),#342,.F.);
#20819=ADVANCED_FACE('',(#2699),#19836,.T.);
#20820=ADVANCED_FACE('',(#2700),#343,.F.);
#20821=ADVANCED_FACE('',(#2701),#19837,.T.);
#20822=ADVANCED_FACE('',(#2702),#2405,.F.);
#20823=ADVANCED_FACE('',(#2703),#2406,.F.);
#20824=ADVANCED_FACE('',(#2704),#2407,.F.);
#20825=ADVANCED_FACE('',(#2705),#2408,.F.);
#20826=ADVANCED_FACE('',(#2706),#2409,.F.);
#20827=ADVANCED_FACE('',(#2707),#2410,.F.);
#20828=ADVANCED_FACE('',(#2708),#2411,.F.);
#20829=ADVANCED_FACE('',(#2709,#2312),#2412,.T.);
#20830=ADVANCED_FACE('',(#2710),#19838,.T.);
#20831=ADVANCED_FACE('',(#2711,#2313),#2413,.F.);
#20832=ADVANCED_FACE('',(#2712),#2414,.T.);
#20833=ADVANCED_FACE('',(#2713),#19839,.F.);
#20834=ADVANCED_FACE('',(#2714),#19840,.T.);
#20835=ADVANCED_FACE('',(#2715,#2314),#2415,.T.);
#20836=ADVANCED_FACE('',(#2716,#2315),#2416,.F.);
#20837=ADVANCED_FACE('',(#2717),#19841,.F.);
#20838=ADVANCED_FACE('',(#2718),#19842,.F.);
#20839=ADVANCED_FACE('',(#2719),#19843,.F.);
#20840=ADVANCED_FACE('',(#2720),#19844,.F.);
#20841=ADVANCED_FACE('',(#2721),#19845,.F.);
#20842=ADVANCED_FACE('',(#2722),#19846,.F.);
#20843=ADVANCED_FACE('',(#2723),#19847,.F.);
#20844=ADVANCED_FACE('',(#2724),#19848,.F.);
#20845=ADVANCED_FACE('',(#2725),#19849,.F.);
#20846=ADVANCED_FACE('',(#2726),#19850,.F.);
#20847=ADVANCED_FACE('',(#2727),#19851,.F.);
#20848=ADVANCED_FACE('',(#2728),#19852,.F.);
#20849=ADVANCED_FACE('',(#2729),#19853,.F.);
#20850=ADVANCED_FACE('',(#2730),#19854,.F.);
#20851=ADVANCED_FACE('',(#2731),#19855,.F.);
#20852=ADVANCED_FACE('',(#2732),#19856,.F.);
#20853=ADVANCED_FACE('',(#2733),#19857,.F.);
#20854=ADVANCED_FACE('',(#2734),#19858,.F.);
#20855=ADVANCED_FACE('',(#2735),#19859,.F.);
#20856=ADVANCED_FACE('',(#2736),#19860,.F.);
#20857=ADVANCED_FACE('',(#2737),#19861,.F.);
#20858=ADVANCED_FACE('',(#2738),#19862,.F.);
#20859=ADVANCED_FACE('',(#2739),#19863,.F.);
#20860=ADVANCED_FACE('',(#2740),#19864,.F.);
#20861=ADVANCED_FACE('',(#2741),#19865,.F.);
#20862=ADVANCED_FACE('',(#2742),#19866,.F.);
#20863=ADVANCED_FACE('',(#2743),#19867,.F.);
#20864=ADVANCED_FACE('',(#2744),#19868,.F.);
#20865=ADVANCED_FACE('',(#2745),#19869,.F.);
#20866=ADVANCED_FACE('',(#2746),#19870,.F.);
#20867=ADVANCED_FACE('',(#2747),#19871,.F.);
#20868=ADVANCED_FACE('',(#2748),#19872,.F.);
#20869=ADVANCED_FACE('',(#2749),#19873,.F.);
#20870=ADVANCED_FACE('',(#2750),#19874,.F.);
#20871=ADVANCED_FACE('',(#2751),#19875,.F.);
#20872=ADVANCED_FACE('',(#2752),#19876,.F.);
#20873=ADVANCED_FACE('',(#2753),#19877,.F.);
#20874=ADVANCED_FACE('',(#2754),#19878,.F.);
#20875=ADVANCED_FACE('',(#2755),#19879,.F.);
#20876=ADVANCED_FACE('',(#2756),#19880,.F.);
#20877=ADVANCED_FACE('',(#2757),#19881,.F.);
#20878=ADVANCED_FACE('',(#2758),#19882,.F.);
#20879=ADVANCED_FACE('',(#2759),#19883,.F.);
#20880=ADVANCED_FACE('',(#2760),#19884,.F.);
#20881=ADVANCED_FACE('',(#2761),#19885,.F.);
#20882=ADVANCED_FACE('',(#2762),#19886,.F.);
#20883=ADVANCED_FACE('',(#2763),#19887,.F.);
#20884=ADVANCED_FACE('',(#2764),#19888,.F.);
#20885=ADVANCED_FACE('',(#2765),#19889,.F.);
#20886=ADVANCED_FACE('',(#2766),#19890,.F.);
#20887=ADVANCED_FACE('',(#2767),#19891,.F.);
#20888=ADVANCED_FACE('',(#2768),#19892,.F.);
#20889=ADVANCED_FACE('',(#2769),#19893,.F.);
#20890=ADVANCED_FACE('',(#2770),#19894,.F.);
#20891=ADVANCED_FACE('',(#2771),#19895,.F.);
#20892=ADVANCED_FACE('',(#2772),#19896,.F.);
#20893=ADVANCED_FACE('',(#2773),#19897,.F.);
#20894=ADVANCED_FACE('',(#2774),#19898,.F.);
#20895=ADVANCED_FACE('',(#2775),#19899,.F.);
#20896=ADVANCED_FACE('',(#2776),#19900,.F.);
#20897=ADVANCED_FACE('',(#2777),#19901,.F.);
#20898=ADVANCED_FACE('',(#2778),#19902,.F.);
#20899=ADVANCED_FACE('',(#2779),#19903,.F.);
#20900=ADVANCED_FACE('',(#2780),#19904,.F.);
#20901=ADVANCED_FACE('',(#2781),#19905,.F.);
#20902=ADVANCED_FACE('',(#2782),#19906,.F.);
#20903=ADVANCED_FACE('',(#2783),#19907,.F.);
#20904=ADVANCED_FACE('',(#2784),#19908,.F.);
#20905=ADVANCED_FACE('',(#2785),#19909,.F.);
#20906=ADVANCED_FACE('',(#2786),#19910,.F.);
#20907=ADVANCED_FACE('',(#2787),#19911,.F.);
#20908=ADVANCED_FACE('',(#2788),#19912,.F.);
#20909=ADVANCED_FACE('',(#2789),#19913,.F.);
#20910=ADVANCED_FACE('',(#2790),#19914,.F.);
#20911=ADVANCED_FACE('',(#2791),#19915,.F.);
#20912=ADVANCED_FACE('',(#2792),#19916,.F.);
#20913=ADVANCED_FACE('',(#2793),#19917,.F.);
#20914=ADVANCED_FACE('',(#2794),#19918,.F.);
#20915=ADVANCED_FACE('',(#2795),#19919,.F.);
#20916=ADVANCED_FACE('',(#2796),#19920,.F.);
#20917=ADVANCED_FACE('',(#2797),#19921,.F.);
#20918=ADVANCED_FACE('',(#2798),#19922,.F.);
#20919=ADVANCED_FACE('',(#2799),#19923,.F.);
#20920=ADVANCED_FACE('',(#2800),#19924,.F.);
#20921=ADVANCED_FACE('',(#2801),#19925,.F.);
#20922=ADVANCED_FACE('',(#2802),#19926,.F.);
#20923=ADVANCED_FACE('',(#2803),#19927,.F.);
#20924=ADVANCED_FACE('',(#2804),#19928,.F.);
#20925=ADVANCED_FACE('',(#2805),#19929,.F.);
#20926=ADVANCED_FACE('',(#2806),#19930,.F.);
#20927=ADVANCED_FACE('',(#2807),#19931,.F.);
#20928=ADVANCED_FACE('',(#2808),#19932,.F.);
#20929=ADVANCED_FACE('',(#2809),#19933,.F.);
#20930=ADVANCED_FACE('',(#2810),#19934,.F.);
#20931=ADVANCED_FACE('',(#2811),#19935,.F.);
#20932=ADVANCED_FACE('',(#2812),#19936,.F.);
#20933=ADVANCED_FACE('',(#2813),#19937,.F.);
#20934=ADVANCED_FACE('',(#2814),#19938,.F.);
#20935=ADVANCED_FACE('',(#2815),#19939,.F.);
#20936=ADVANCED_FACE('',(#2816),#19940,.F.);
#20937=ADVANCED_FACE('',(#2817),#19941,.F.);
#20938=ADVANCED_FACE('',(#2818),#19942,.F.);
#20939=ADVANCED_FACE('',(#2819),#19943,.F.);
#20940=ADVANCED_FACE('',(#2820),#19944,.F.);
#20941=ADVANCED_FACE('',(#2821),#19945,.F.);
#20942=ADVANCED_FACE('',(#2822),#19946,.F.);
#20943=ADVANCED_FACE('',(#2823),#19947,.F.);
#20944=ADVANCED_FACE('',(#2824),#19948,.F.);
#20945=ADVANCED_FACE('',(#2825),#19949,.F.);
#20946=ADVANCED_FACE('',(#2826),#19950,.F.);
#20947=ADVANCED_FACE('',(#2827),#19951,.F.);
#20948=ADVANCED_FACE('',(#2828),#19952,.F.);
#20949=ADVANCED_FACE('',(#2829),#19953,.F.);
#20950=ADVANCED_FACE('',(#2830),#19954,.F.);
#20951=ADVANCED_FACE('',(#2831),#19955,.F.);
#20952=ADVANCED_FACE('',(#2832),#19956,.F.);
#20953=ADVANCED_FACE('',(#2833),#19957,.F.);
#20954=ADVANCED_FACE('',(#2834),#19958,.F.);
#20955=ADVANCED_FACE('',(#2835),#19959,.F.);
#20956=ADVANCED_FACE('',(#2836),#19960,.F.);
#20957=ADVANCED_FACE('',(#2837),#19961,.F.);
#20958=ADVANCED_FACE('',(#2838),#19962,.F.);
#20959=ADVANCED_FACE('',(#2839),#19963,.F.);
#20960=ADVANCED_FACE('',(#2840),#19964,.F.);
#20961=ADVANCED_FACE('',(#2841),#19965,.F.);
#20962=ADVANCED_FACE('',(#2842),#19966,.F.);
#20963=ADVANCED_FACE('',(#2843),#19967,.F.);
#20964=ADVANCED_FACE('',(#2844),#19968,.F.);
#20965=ADVANCED_FACE('',(#2845),#19969,.F.);
#20966=ADVANCED_FACE('',(#2846),#19970,.F.);
#20967=ADVANCED_FACE('',(#2847),#2417,.F.);
#20968=ADVANCED_FACE('',(#2848),#19971,.F.);
#20969=ADVANCED_FACE('',(#2849),#344,.F.);
#20970=ADVANCED_FACE('',(#2850),#345,.F.);
#20971=ADVANCED_FACE('',(#2851),#19972,.F.);
#20972=ADVANCED_FACE('',(#2852,#2316),#2418,.F.);
#20973=ADVANCED_FACE('',(#2853),#2419,.T.);
#20974=ADVANCED_FACE('',(#2854),#19973,.F.);
#20975=ADVANCED_FACE('',(#2855),#346,.F.);
#20976=ADVANCED_FACE('',(#2856),#347,.F.);
#20977=ADVANCED_FACE('',(#2857),#19974,.F.);
#20978=ADVANCED_FACE('',(#2858,#2317),#2420,.F.);
#20979=ADVANCED_FACE('',(#2859),#19975,.T.);
#20980=ADVANCED_FACE('',(#2860),#2421,.T.);
#20981=ADVANCED_FACE('',(#2861,#2318,#2319,#2320,#2321,#2322),#2422,.T.);
#20982=ADVANCED_FACE('',(#2862),#19976,.F.);
#20983=ADVANCED_FACE('',(#2863),#2423,.T.);
#20984=ADVANCED_FACE('',(#2864),#19977,.F.);
#20985=ADVANCED_FACE('',(#2865),#2424,.T.);
#20986=ADVANCED_FACE('',(#2866),#19978,.F.);
#20987=ADVANCED_FACE('',(#2867),#2425,.T.);
#20988=ADVANCED_FACE('',(#2868),#19979,.F.);
#20989=ADVANCED_FACE('',(#2869),#2426,.T.);
#20990=ADVANCED_FACE('',(#2870),#19980,.T.);
#20991=ADVANCED_FACE('',(#2871),#19981,.T.);
#20992=ADVANCED_FACE('',(#2872),#2427,.T.);
#20993=ADVANCED_FACE('',(#2873),#19982,.T.);
#20994=ADVANCED_FACE('',(#2874),#19983,.T.);
#20995=ADVANCED_FACE('',(#2875),#2428,.T.);
#20996=ADVANCED_FACE('',(#2876),#19984,.T.);
#20997=ADVANCED_FACE('',(#2877),#19985,.F.);
#20998=ADVANCED_FACE('',(#2878),#2429,.T.);
#20999=ADVANCED_FACE('',(#2879),#19986,.F.);
#21000=ADVANCED_FACE('',(#2880),#2430,.T.);
#21001=ADVANCED_FACE('',(#2881),#19987,.F.);
#21002=ADVANCED_FACE('',(#2882),#2431,.T.);
#21003=ADVANCED_FACE('',(#2883),#19988,.F.);
#21004=ADVANCED_FACE('',(#2884),#2432,.T.);
#21005=ADVANCED_FACE('',(#2885),#19989,.T.);
#21006=ADVANCED_FACE('',(#2886),#19990,.T.);
#21007=ADVANCED_FACE('',(#2887),#2433,.T.);
#21008=ADVANCED_FACE('',(#2888),#19991,.T.);
#21009=ADVANCED_FACE('',(#2889),#19992,.T.);
#21010=ADVANCED_FACE('',(#2890),#2434,.T.);
#21011=ADVANCED_FACE('',(#2891),#19993,.T.);
#21012=ADVANCED_FACE('',(#2892),#19994,.F.);
#21013=ADVANCED_FACE('',(#2893),#2435,.T.);
#21014=ADVANCED_FACE('',(#2894),#19995,.F.);
#21015=ADVANCED_FACE('',(#2895),#2436,.T.);
#21016=ADVANCED_FACE('',(#2896),#19996,.F.);
#21017=ADVANCED_FACE('',(#2897),#2437,.T.);
#21018=ADVANCED_FACE('',(#2898),#19997,.F.);
#21019=ADVANCED_FACE('',(#2899),#2438,.T.);
#21020=ADVANCED_FACE('',(#2900),#19998,.T.);
#21021=ADVANCED_FACE('',(#2901),#19999,.T.);
#21022=ADVANCED_FACE('',(#2902),#2439,.T.);
#21023=ADVANCED_FACE('',(#2903),#20000,.T.);
#21024=ADVANCED_FACE('',(#2904),#20001,.T.);
#21025=ADVANCED_FACE('',(#2905),#2440,.T.);
#21026=ADVANCED_FACE('',(#2906),#20002,.T.);
#21027=ADVANCED_FACE('',(#2907),#20003,.F.);
#21028=ADVANCED_FACE('',(#2908),#2441,.T.);
#21029=ADVANCED_FACE('',(#2909),#20004,.F.);
#21030=ADVANCED_FACE('',(#2910),#2442,.T.);
#21031=ADVANCED_FACE('',(#2911),#20005,.F.);
#21032=ADVANCED_FACE('',(#2912),#2443,.T.);
#21033=ADVANCED_FACE('',(#2913),#20006,.F.);
#21034=ADVANCED_FACE('',(#2914),#2444,.T.);
#21035=ADVANCED_FACE('',(#2915),#20007,.T.);
#21036=ADVANCED_FACE('',(#2916),#20008,.T.);
#21037=ADVANCED_FACE('',(#2917),#2445,.T.);
#21038=ADVANCED_FACE('',(#2918),#20009,.T.);
#21039=ADVANCED_FACE('',(#2919),#20010,.T.);
#21040=ADVANCED_FACE('',(#2920),#20011,.F.);
#21041=ADVANCED_FACE('',(#2921),#20012,.F.);
#21042=ADVANCED_FACE('',(#2922),#20013,.F.);
#21043=ADVANCED_FACE('',(#2923),#20014,.F.);
#21044=ADVANCED_FACE('',(#2924),#20015,.F.);
#21045=ADVANCED_FACE('',(#2925),#2446,.T.);
#21046=ADVANCED_FACE('',(#2926),#2447,.T.);
#21047=ADVANCED_FACE('',(#2927),#2448,.T.);
#21048=ADVANCED_FACE('',(#2928),#2449,.T.);
#21049=ADVANCED_FACE('',(#2929),#2450,.T.);
#21050=ADVANCED_FACE('',(#2930),#2451,.T.);
#21051=ADVANCED_FACE('',(#2931),#2452,.T.);
#21052=ADVANCED_FACE('',(#2932),#2453,.T.);
#21053=ADVANCED_FACE('',(#2933),#2454,.T.);
#21054=ADVANCED_FACE('',(#2934),#2455,.T.);
#21055=ADVANCED_FACE('',(#2935),#2456,.T.);
#21056=ADVANCED_FACE('',(#2936),#2457,.T.);
#21057=ADVANCED_FACE('',(#2937,#2323,#2324,#2325,#2326,#2327),#2458,.F.);
#21058=ADVANCED_FACE('',(#2938,#2328),#2459,.F.);
#21059=ADVANCED_FACE('',(#2939),#20016,.F.);
#21060=ADVANCED_FACE('',(#2940),#20017,.F.);
#21061=ADVANCED_FACE('',(#2941),#20018,.F.);
#21062=ADVANCED_FACE('',(#2942),#20019,.F.);
#21063=ADVANCED_FACE('',(#2943),#20020,.F.);
#21064=ADVANCED_FACE('',(#2944),#20021,.F.);
#21065=ADVANCED_FACE('',(#2945),#2460,.T.);
#21066=ADVANCED_FACE('',(#2946),#2461,.T.);
#21067=ADVANCED_FACE('',(#2947),#2462,.T.);
#21068=ADVANCED_FACE('',(#2948),#2463,.T.);
#21069=ADVANCED_FACE('',(#2949,#2329,#2330,#2331,#2332,#2333),#2464,.T.);
#21070=ADVANCED_FACE('',(#2950,#2334,#2335,#2336,#2337,#2338),#2465,.F.);
#21071=ADVANCED_FACE('',(#2951),#20022,.T.);
#21072=ADVANCED_FACE('',(#2952),#20023,.T.);
#21073=ADVANCED_FACE('',(#2953),#20024,.T.);
#21074=ADVANCED_FACE('',(#2954),#20025,.T.);
#21075=ADVANCED_FACE('',(#2955),#20026,.T.);
#21076=ADVANCED_FACE('',(#2956),#20027,.T.);
#21077=ADVANCED_FACE('',(#2957),#20028,.T.);
#21078=ADVANCED_FACE('',(#2958),#20029,.T.);
#21079=ADVANCED_FACE('',(#2959),#20030,.T.);
#21080=ADVANCED_FACE('',(#2960),#20031,.T.);
#21081=ADVANCED_FACE('',(#2961),#20032,.T.);
#21082=ADVANCED_FACE('',(#2962),#20033,.T.);
#21083=ADVANCED_FACE('',(#2963),#20034,.T.);
#21084=ADVANCED_FACE('',(#2964),#20035,.T.);
#21085=ADVANCED_FACE('',(#2965),#20036,.T.);
#21086=ADVANCED_FACE('',(#2966),#20037,.T.);
#21087=ADVANCED_FACE('',(#2967),#20038,.T.);
#21088=ADVANCED_FACE('',(#2968),#20039,.T.);
#21089=ADVANCED_FACE('',(#2969),#20040,.T.);
#21090=ADVANCED_FACE('',(#2970),#20041,.T.);
#21091=ADVANCED_FACE('',(#2971),#20042,.T.);
#21092=ADVANCED_FACE('',(#2972),#20043,.T.);
#21093=ADVANCED_FACE('',(#2973),#20044,.T.);
#21094=ADVANCED_FACE('',(#2974),#20045,.T.);
#21095=ADVANCED_FACE('',(#2975),#20046,.T.);
#21096=ADVANCED_FACE('',(#2976),#20047,.T.);
#21097=ADVANCED_FACE('',(#2977),#20048,.T.);
#21098=ADVANCED_FACE('',(#2978),#20049,.T.);
#21099=ADVANCED_FACE('',(#2979),#20050,.T.);
#21100=ADVANCED_FACE('',(#2980),#20051,.T.);
#21101=ADVANCED_FACE('',(#2981),#20052,.T.);
#21102=ADVANCED_FACE('',(#2982),#20053,.T.);
#21103=ADVANCED_FACE('',(#2983),#20054,.T.);
#21104=ADVANCED_FACE('',(#2984),#20055,.T.);
#21105=ADVANCED_FACE('',(#2985),#20056,.T.);
#21106=ADVANCED_FACE('',(#2986),#20057,.T.);
#21107=ADVANCED_FACE('',(#2987),#20058,.T.);
#21108=ADVANCED_FACE('',(#2988),#20059,.T.);
#21109=ADVANCED_FACE('',(#2989),#331,.T.);
#21110=ADVANCED_FACE('',(#2990),#348,.F.);
#21111=ADVANCED_FACE('',(#2991),#20060,.T.);
#21112=ADVANCED_FACE('',(#2992),#349,.F.);
#21113=ADVANCED_FACE('',(#2993),#20061,.T.);
#21114=ADVANCED_FACE('',(#2994),#2466,.F.);
#21115=ADVANCED_FACE('',(#2995),#2467,.F.);
#21116=ADVANCED_FACE('',(#2996),#2468,.F.);
#21117=ADVANCED_FACE('',(#2997),#2469,.F.);
#21118=ADVANCED_FACE('',(#2998),#2470,.F.);
#21119=ADVANCED_FACE('',(#2999),#2471,.F.);
#21120=ADVANCED_FACE('',(#3000),#2472,.F.);
#21121=ADVANCED_FACE('',(#3001,#2339),#2473,.T.);
#21122=ADVANCED_FACE('',(#3002),#20062,.T.);
#21123=ADVANCED_FACE('',(#3003,#2340),#2474,.F.);
#21124=ADVANCED_FACE('',(#3004),#2475,.T.);
#21125=ADVANCED_FACE('',(#3005),#20063,.T.);
#21126=ADVANCED_FACE('',(#3006),#2476,.T.);
#21127=ADVANCED_FACE('',(#3007),#2477,.F.);
#21128=ADVANCED_FACE('',(#3008),#20064,.F.);
#21129=ADVANCED_FACE('',(#3009),#20065,.F.);
#21130=ADVANCED_FACE('',(#3010),#20066,.F.);
#21131=ADVANCED_FACE('',(#3011),#20067,.F.);
#21132=ADVANCED_FACE('',(#3012),#20068,.F.);
#21133=ADVANCED_FACE('',(#3013),#20069,.F.);
#21134=ADVANCED_FACE('',(#3014),#20070,.F.);
#21135=ADVANCED_FACE('',(#3015),#20071,.F.);
#21136=ADVANCED_FACE('',(#3016),#20072,.F.);
#21137=ADVANCED_FACE('',(#3017),#20073,.F.);
#21138=ADVANCED_FACE('',(#3018),#20074,.F.);
#21139=ADVANCED_FACE('',(#3019),#20075,.F.);
#21140=ADVANCED_FACE('',(#3020),#20076,.F.);
#21141=ADVANCED_FACE('',(#3021),#20077,.F.);
#21142=ADVANCED_FACE('',(#3022),#20078,.F.);
#21143=ADVANCED_FACE('',(#3023),#20079,.F.);
#21144=ADVANCED_FACE('',(#3024),#20080,.F.);
#21145=ADVANCED_FACE('',(#3025),#20081,.F.);
#21146=ADVANCED_FACE('',(#3026),#20082,.F.);
#21147=ADVANCED_FACE('',(#3027),#20083,.F.);
#21148=ADVANCED_FACE('',(#3028),#20084,.F.);
#21149=ADVANCED_FACE('',(#3029),#20085,.F.);
#21150=ADVANCED_FACE('',(#3030),#20086,.F.);
#21151=ADVANCED_FACE('',(#3031),#20087,.F.);
#21152=ADVANCED_FACE('',(#3032),#20088,.F.);
#21153=ADVANCED_FACE('',(#3033),#20089,.F.);
#21154=ADVANCED_FACE('',(#3034),#20090,.F.);
#21155=ADVANCED_FACE('',(#3035),#20091,.F.);
#21156=ADVANCED_FACE('',(#3036),#20092,.F.);
#21157=ADVANCED_FACE('',(#3037),#20093,.F.);
#21158=ADVANCED_FACE('',(#3038),#20094,.F.);
#21159=ADVANCED_FACE('',(#3039),#20095,.F.);
#21160=ADVANCED_FACE('',(#3040),#20096,.F.);
#21161=ADVANCED_FACE('',(#3041),#20097,.F.);
#21162=ADVANCED_FACE('',(#3042),#20098,.F.);
#21163=ADVANCED_FACE('',(#3043),#20099,.F.);
#21164=ADVANCED_FACE('',(#3044),#20100,.F.);
#21165=ADVANCED_FACE('',(#3045),#20101,.F.);
#21166=ADVANCED_FACE('',(#3046),#20102,.F.);
#21167=ADVANCED_FACE('',(#3047),#20103,.F.);
#21168=ADVANCED_FACE('',(#3048),#20104,.F.);
#21169=ADVANCED_FACE('',(#3049),#20105,.F.);
#21170=ADVANCED_FACE('',(#3050),#20106,.F.);
#21171=ADVANCED_FACE('',(#3051),#20107,.F.);
#21172=ADVANCED_FACE('',(#3052),#20108,.F.);
#21173=ADVANCED_FACE('',(#3053),#20109,.F.);
#21174=ADVANCED_FACE('',(#3054),#20110,.F.);
#21175=ADVANCED_FACE('',(#3055),#20111,.F.);
#21176=ADVANCED_FACE('',(#3056),#2478,.T.);
#21177=ADVANCED_FACE('',(#3057),#20112,.F.);
#21178=ADVANCED_FACE('',(#3058),#350,.F.);
#21179=ADVANCED_FACE('',(#3059),#351,.F.);
#21180=ADVANCED_FACE('',(#3060),#20113,.F.);
#21181=ADVANCED_FACE('',(#3061),#2479,.T.);
#21182=ADVANCED_FACE('',(#3062),#20114,.F.);
#21183=ADVANCED_FACE('',(#3063),#352,.F.);
#21184=ADVANCED_FACE('',(#3064),#353,.F.);
#21185=ADVANCED_FACE('',(#3065),#20115,.F.);
#21186=ADVANCED_FACE('',(#3066),#2480,.T.);
#21187=ADVANCED_FACE('',(#3067),#20116,.F.);
#21188=ADVANCED_FACE('',(#3068),#354,.F.);
#21189=ADVANCED_FACE('',(#3069),#355,.F.);
#21190=ADVANCED_FACE('',(#3070),#20117,.F.);
#21191=ADVANCED_FACE('',(#3071),#2481,.F.);
#21192=ADVANCED_FACE('',(#3072),#2482,.F.);
#21193=ADVANCED_FACE('',(#3073),#2483,.F.);
#21194=ADVANCED_FACE('',(#3074),#11,.F.);
#21195=ADVANCED_FACE('',(#3075),#20118,.T.);
#21196=ADVANCED_FACE('',(#3076,#2341,#2342,#2343,#2344),#2484,.T.);
#21197=ADVANCED_FACE('',(#3077),#2485,.F.);
#21198=ADVANCED_FACE('',(#3078),#20119,.F.);
#21199=ADVANCED_FACE('',(#3079),#20120,.F.);
#21200=ADVANCED_FACE('',(#3080),#20121,.F.);
#21201=ADVANCED_FACE('',(#3081),#12,.F.);
#21202=ADVANCED_FACE('',(#3082),#20122,.F.);
#21203=ADVANCED_FACE('',(#3083),#20123,.T.);
#21204=ADVANCED_FACE('',(#3084,#2345,#2346,#2347,#2348),#2486,.T.);
#21205=ADVANCED_FACE('',(#3085,#2349,#2350,#2351,#2352),#2487,.F.);
#21206=ADVANCED_FACE('',(#3086),#20124,.T.);
#21207=ADVANCED_FACE('',(#3087),#20125,.T.);
#21208=ADVANCED_FACE('',(#3088),#20126,.T.);
#21209=ADVANCED_FACE('',(#3089),#20127,.T.);
#21210=ADVANCED_FACE('',(#3090),#20128,.T.);
#21211=ADVANCED_FACE('',(#3091),#20129,.T.);
#21212=ADVANCED_FACE('',(#3092),#20130,.T.);
#21213=ADVANCED_FACE('',(#3093),#20131,.T.);
#21214=ADVANCED_FACE('',(#3094),#20132,.T.);
#21215=ADVANCED_FACE('',(#3095),#20133,.T.);
#21216=ADVANCED_FACE('',(#3096),#20134,.T.);
#21217=ADVANCED_FACE('',(#3097),#20135,.T.);
#21218=ADVANCED_FACE('',(#3098),#20136,.T.);
#21219=ADVANCED_FACE('',(#3099),#20137,.T.);
#21220=ADVANCED_FACE('',(#3100),#20138,.T.);
#21221=ADVANCED_FACE('',(#3101),#20139,.T.);
#21222=ADVANCED_FACE('',(#3102),#20140,.T.);
#21223=ADVANCED_FACE('',(#3103),#20141,.T.);
#21224=ADVANCED_FACE('',(#3104),#20142,.T.);
#21225=ADVANCED_FACE('',(#3105),#20143,.T.);
#21226=ADVANCED_FACE('',(#3106),#20144,.T.);
#21227=ADVANCED_FACE('',(#3107),#20145,.T.);
#21228=ADVANCED_FACE('',(#3108),#20146,.T.);
#21229=ADVANCED_FACE('',(#3109),#20147,.T.);
#21230=ADVANCED_FACE('',(#3110),#20148,.T.);
#21231=ADVANCED_FACE('',(#3111),#20149,.T.);
#21232=ADVANCED_FACE('',(#3112),#20150,.T.);
#21233=ADVANCED_FACE('',(#3113),#20151,.T.);
#21234=ADVANCED_FACE('',(#3114),#20152,.T.);
#21235=ADVANCED_FACE('',(#3115),#20153,.T.);
#21236=ADVANCED_FACE('',(#3116),#20154,.T.);
#21237=ADVANCED_FACE('',(#3117),#20155,.T.);
#21238=ADVANCED_FACE('',(#3118),#20156,.T.);
#21239=ADVANCED_FACE('',(#3119),#20157,.T.);
#21240=ADVANCED_FACE('',(#3120),#20158,.T.);
#21241=ADVANCED_FACE('',(#3121),#20159,.T.);
#21242=ADVANCED_FACE('',(#3122),#20160,.T.);
#21243=ADVANCED_FACE('',(#3123),#20161,.T.);
#21244=ADVANCED_FACE('',(#3124),#20162,.T.);
#21245=ADVANCED_FACE('',(#3125),#20163,.T.);
#21246=ADVANCED_FACE('',(#3126),#20164,.T.);
#21247=ADVANCED_FACE('',(#3127),#20165,.T.);
#21248=ADVANCED_FACE('',(#3128),#20166,.T.);
#21249=ADVANCED_FACE('',(#3129),#20167,.T.);
#21250=ADVANCED_FACE('',(#3130),#20168,.T.);
#21251=ADVANCED_FACE('',(#3131),#20169,.T.);
#21252=ADVANCED_FACE('',(#3132),#20170,.T.);
#21253=ADVANCED_FACE('',(#3133),#20171,.T.);
#21254=ADVANCED_FACE('',(#3134),#20172,.T.);
#21255=ADVANCED_FACE('',(#3135),#20173,.T.);
#21256=ADVANCED_FACE('',(#3136),#20174,.T.);
#21257=ADVANCED_FACE('',(#3137),#20175,.T.);
#21258=ADVANCED_FACE('',(#3138),#20176,.T.);
#21259=ADVANCED_FACE('',(#3139),#20177,.T.);
#21260=ADVANCED_FACE('',(#3140),#20178,.T.);
#21261=ADVANCED_FACE('',(#3141),#20179,.T.);
#21262=ADVANCED_FACE('',(#3142),#20180,.T.);
#21263=ADVANCED_FACE('',(#3143),#20181,.T.);
#21264=ADVANCED_FACE('',(#3144),#20182,.T.);
#21265=ADVANCED_FACE('',(#3145),#20183,.T.);
#21266=ADVANCED_FACE('',(#3146),#20184,.T.);
#21267=ADVANCED_FACE('',(#3147),#20185,.T.);
#21268=ADVANCED_FACE('',(#3148),#20186,.T.);
#21269=ADVANCED_FACE('',(#3149),#20187,.T.);
#21270=ADVANCED_FACE('',(#3150),#20188,.T.);
#21271=ADVANCED_FACE('',(#3151),#20189,.T.);
#21272=ADVANCED_FACE('',(#3152),#20190,.T.);
#21273=ADVANCED_FACE('',(#3153),#20191,.T.);
#21274=ADVANCED_FACE('',(#3154),#20192,.T.);
#21275=ADVANCED_FACE('',(#3155),#20193,.T.);
#21276=ADVANCED_FACE('',(#3156),#20194,.T.);
#21277=ADVANCED_FACE('',(#3157),#20195,.T.);
#21278=ADVANCED_FACE('',(#3158),#20196,.T.);
#21279=ADVANCED_FACE('',(#3159),#20197,.T.);
#21280=ADVANCED_FACE('',(#3160),#20198,.T.);
#21281=ADVANCED_FACE('',(#3161),#20199,.T.);
#21282=ADVANCED_FACE('',(#3162),#20200,.T.);
#21283=ADVANCED_FACE('',(#3163),#20201,.T.);
#21284=ADVANCED_FACE('',(#3164),#20202,.T.);
#21285=ADVANCED_FACE('',(#3165),#20203,.T.);
#21286=ADVANCED_FACE('',(#3166),#20204,.T.);
#21287=ADVANCED_FACE('',(#3167),#20205,.T.);
#21288=ADVANCED_FACE('',(#3168),#20206,.T.);
#21289=ADVANCED_FACE('',(#3169),#20207,.T.);
#21290=ADVANCED_FACE('',(#3170),#20208,.T.);
#21291=ADVANCED_FACE('',(#3171),#20209,.T.);
#21292=ADVANCED_FACE('',(#3172),#20210,.T.);
#21293=ADVANCED_FACE('',(#3173),#20211,.T.);
#21294=ADVANCED_FACE('',(#3174),#20212,.T.);
#21295=ADVANCED_FACE('',(#3175),#20213,.T.);
#21296=ADVANCED_FACE('',(#3176),#20214,.T.);
#21297=ADVANCED_FACE('',(#3177),#20215,.T.);
#21298=ADVANCED_FACE('',(#3178),#20216,.T.);
#21299=ADVANCED_FACE('',(#3179),#20217,.T.);
#21300=ADVANCED_FACE('',(#3180),#20218,.T.);
#21301=ADVANCED_FACE('',(#3181),#20219,.T.);
#21302=ADVANCED_FACE('',(#3182),#20220,.T.);
#21303=ADVANCED_FACE('',(#3183),#20221,.T.);
#21304=ADVANCED_FACE('',(#3184),#20222,.T.);
#21305=ADVANCED_FACE('',(#3185),#20223,.T.);
#21306=ADVANCED_FACE('',(#3186),#20224,.T.);
#21307=ADVANCED_FACE('',(#3187),#20225,.T.);
#21308=ADVANCED_FACE('',(#3188),#20226,.T.);
#21309=ADVANCED_FACE('',(#3189),#20227,.T.);
#21310=ADVANCED_FACE('',(#3190),#20228,.T.);
#21311=ADVANCED_FACE('',(#3191),#20229,.T.);
#21312=ADVANCED_FACE('',(#3192),#20230,.T.);
#21313=ADVANCED_FACE('',(#3193),#20231,.T.);
#21314=ADVANCED_FACE('',(#3194),#20232,.T.);
#21315=ADVANCED_FACE('',(#3195),#20233,.T.);
#21316=ADVANCED_FACE('',(#3196),#20234,.T.);
#21317=ADVANCED_FACE('',(#3197),#20235,.T.);
#21318=ADVANCED_FACE('',(#3198),#20236,.T.);
#21319=ADVANCED_FACE('',(#3199),#20237,.T.);
#21320=ADVANCED_FACE('',(#3200),#20238,.T.);
#21321=ADVANCED_FACE('',(#3201),#20239,.T.);
#21322=ADVANCED_FACE('',(#3202),#20240,.T.);
#21323=ADVANCED_FACE('',(#3203),#20241,.T.);
#21324=ADVANCED_FACE('',(#3204),#20242,.T.);
#21325=ADVANCED_FACE('',(#3205),#20243,.T.);
#21326=ADVANCED_FACE('',(#3206),#356,.F.);
#21327=ADVANCED_FACE('',(#3207),#20244,.T.);
#21328=ADVANCED_FACE('',(#3208),#357,.F.);
#21329=ADVANCED_FACE('',(#3209),#20245,.T.);
#21330=ADVANCED_FACE('',(#3210,#2353),#2488,.T.);
#21331=ADVANCED_FACE('',(#3211,#2354),#2489,.F.);
#21332=ADVANCED_FACE('',(#3212),#2490,.T.);
#21333=ADVANCED_FACE('',(#3213),#2491,.T.);
#21334=ADVANCED_FACE('',(#3214),#2492,.T.);
#21335=ADVANCED_FACE('',(#3215),#2493,.T.);
#21336=ADVANCED_FACE('',(#3216),#2494,.T.);
#21337=ADVANCED_FACE('',(#3217),#2495,.T.);
#21338=ADVANCED_FACE('',(#3218),#20246,.T.);
#21339=ADVANCED_FACE('',(#3219),#2496,.T.);
#21340=ADVANCED_FACE('',(#3220),#13,.T.);
#21341=ADVANCED_FACE('',(#3221),#20247,.F.);
#21342=ADVANCED_FACE('',(#3222),#20248,.F.);
#21343=ADVANCED_FACE('',(#3223),#20249,.F.);
#21344=ADVANCED_FACE('',(#3224),#20250,.F.);
#21345=ADVANCED_FACE('',(#3225),#20251,.F.);
#21346=ADVANCED_FACE('',(#3226),#20252,.F.);
#21347=ADVANCED_FACE('',(#3227),#20253,.F.);
#21348=ADVANCED_FACE('',(#3228),#20254,.F.);
#21349=ADVANCED_FACE('',(#3229),#20255,.F.);
#21350=ADVANCED_FACE('',(#3230),#20256,.F.);
#21351=ADVANCED_FACE('',(#3231),#20257,.F.);
#21352=ADVANCED_FACE('',(#3232),#20258,.F.);
#21353=ADVANCED_FACE('',(#3233),#20259,.F.);
#21354=ADVANCED_FACE('',(#3234),#20260,.F.);
#21355=ADVANCED_FACE('',(#3235),#20261,.F.);
#21356=ADVANCED_FACE('',(#3236),#20262,.F.);
#21357=ADVANCED_FACE('',(#3237),#20263,.F.);
#21358=ADVANCED_FACE('',(#3238),#358,.F.);
#21359=ADVANCED_FACE('',(#3239),#359,.F.);
#21360=ADVANCED_FACE('',(#3240,#2355),#2497,.T.);
#21361=ADVANCED_FACE('',(#3241),#20264,.F.);
#21362=ADVANCED_FACE('',(#3242),#2498,.T.);
#21363=ADVANCED_FACE('',(#3243),#2499,.T.);
#21364=ADVANCED_FACE('',(#3244),#2500,.T.);
#21365=ADVANCED_FACE('',(#3245),#2501,.T.);
#21366=ADVANCED_FACE('',(#3246),#2502,.T.);
#21367=ADVANCED_FACE('',(#3247),#2503,.T.);
#21368=ADVANCED_FACE('',(#3248,#2356),#2504,.F.);
#21369=ADVANCED_FACE('',(#3249),#20265,.F.);
#21370=ADVANCED_FACE('',(#3250),#20266,.T.);
#21371=ADVANCED_FACE('',(#3251,#2357),#2505,.T.);
#21372=ADVANCED_FACE('',(#3252,#2358),#2506,.F.);
#21373=ADVANCED_FACE('',(#3253),#20267,.T.);
#21374=ADVANCED_FACE('',(#3254),#20268,.T.);
#21375=ADVANCED_FACE('',(#3255),#20269,.T.);
#21376=ADVANCED_FACE('',(#3256),#20270,.T.);
#21377=ADVANCED_FACE('',(#3257),#20271,.T.);
#21378=ADVANCED_FACE('',(#3258),#20272,.T.);
#21379=ADVANCED_FACE('',(#3259),#20273,.T.);
#21380=ADVANCED_FACE('',(#3260),#20274,.T.);
#21381=ADVANCED_FACE('',(#3261),#20275,.T.);
#21382=ADVANCED_FACE('',(#3262),#20276,.T.);
#21383=ADVANCED_FACE('',(#3263),#20277,.T.);
#21384=ADVANCED_FACE('',(#3264),#20278,.T.);
#21385=ADVANCED_FACE('',(#3265),#20279,.T.);
#21386=ADVANCED_FACE('',(#3266),#20280,.T.);
#21387=ADVANCED_FACE('',(#3267),#20281,.T.);
#21388=ADVANCED_FACE('',(#3268),#20282,.T.);
#21389=ADVANCED_FACE('',(#3269),#20283,.T.);
#21390=ADVANCED_FACE('',(#3270),#20284,.T.);
#21391=ADVANCED_FACE('',(#3271),#20285,.T.);
#21392=ADVANCED_FACE('',(#3272),#20286,.T.);
#21393=ADVANCED_FACE('',(#3273),#20287,.T.);
#21394=ADVANCED_FACE('',(#3274),#20288,.T.);
#21395=ADVANCED_FACE('',(#3275),#20289,.T.);
#21396=ADVANCED_FACE('',(#3276),#20290,.T.);
#21397=ADVANCED_FACE('',(#3277),#20291,.T.);
#21398=ADVANCED_FACE('',(#3278),#20292,.T.);
#21399=ADVANCED_FACE('',(#3279),#20293,.T.);
#21400=ADVANCED_FACE('',(#3280),#20294,.T.);
#21401=ADVANCED_FACE('',(#3281),#20295,.T.);
#21402=ADVANCED_FACE('',(#3282),#20296,.T.);
#21403=ADVANCED_FACE('',(#3283),#332,.T.);
#21404=ADVANCED_FACE('',(#3284),#360,.F.);
#21405=ADVANCED_FACE('',(#3285),#20297,.T.);
#21406=ADVANCED_FACE('',(#3286),#361,.F.);
#21407=ADVANCED_FACE('',(#3287),#20298,.T.);
#21408=ADVANCED_FACE('',(#3288),#2507,.F.);
#21409=ADVANCED_FACE('',(#3289),#2508,.F.);
#21410=ADVANCED_FACE('',(#3290),#2509,.F.);
#21411=ADVANCED_FACE('',(#3291),#2510,.F.);
#21412=ADVANCED_FACE('',(#3292),#2511,.F.);
#21413=ADVANCED_FACE('',(#3293),#2512,.F.);
#21414=ADVANCED_FACE('',(#3294),#2513,.F.);
#21415=ADVANCED_FACE('',(#3295,#2359),#2514,.T.);
#21416=ADVANCED_FACE('',(#3296),#20299,.T.);
#21417=ADVANCED_FACE('',(#3297,#2360),#2515,.F.);
#21418=ADVANCED_FACE('',(#3298),#2516,.T.);
#21419=ADVANCED_FACE('',(#3299),#20300,.F.);
#21420=ADVANCED_FACE('',(#3300),#20301,.F.);
#21421=ADVANCED_FACE('',(#3301),#20302,.F.);
#21422=ADVANCED_FACE('',(#3302),#20303,.F.);
#21423=ADVANCED_FACE('',(#3303),#20304,.F.);
#21424=ADVANCED_FACE('',(#3304),#20305,.F.);
#21425=ADVANCED_FACE('',(#3305),#20306,.F.);
#21426=ADVANCED_FACE('',(#3306),#20307,.F.);
#21427=ADVANCED_FACE('',(#3307),#20308,.F.);
#21428=ADVANCED_FACE('',(#3308),#20309,.F.);
#21429=ADVANCED_FACE('',(#3309),#20310,.F.);
#21430=ADVANCED_FACE('',(#3310),#20311,.F.);
#21431=ADVANCED_FACE('',(#3311),#20312,.F.);
#21432=ADVANCED_FACE('',(#3312),#20313,.F.);
#21433=ADVANCED_FACE('',(#3313),#20314,.F.);
#21434=ADVANCED_FACE('',(#3314),#20315,.F.);
#21435=ADVANCED_FACE('',(#3315),#20316,.F.);
#21436=ADVANCED_FACE('',(#3316),#20317,.F.);
#21437=ADVANCED_FACE('',(#3317),#20318,.F.);
#21438=ADVANCED_FACE('',(#3318),#20319,.F.);
#21439=ADVANCED_FACE('',(#3319),#20320,.F.);
#21440=ADVANCED_FACE('',(#3320),#20321,.F.);
#21441=ADVANCED_FACE('',(#3321),#20322,.F.);
#21442=ADVANCED_FACE('',(#3322),#20323,.F.);
#21443=ADVANCED_FACE('',(#3323),#20324,.F.);
#21444=ADVANCED_FACE('',(#3324),#20325,.F.);
#21445=ADVANCED_FACE('',(#3325),#20326,.F.);
#21446=ADVANCED_FACE('',(#3326),#20327,.F.);
#21447=ADVANCED_FACE('',(#3327),#20328,.F.);
#21448=ADVANCED_FACE('',(#3328),#20329,.F.);
#21449=ADVANCED_FACE('',(#3329),#20330,.F.);
#21450=ADVANCED_FACE('',(#3330),#20331,.F.);
#21451=ADVANCED_FACE('',(#3331),#20332,.F.);
#21452=ADVANCED_FACE('',(#3332),#20333,.F.);
#21453=ADVANCED_FACE('',(#3333),#20334,.F.);
#21454=ADVANCED_FACE('',(#3334),#20335,.F.);
#21455=ADVANCED_FACE('',(#3335),#20336,.F.);
#21456=ADVANCED_FACE('',(#3336),#20337,.F.);
#21457=ADVANCED_FACE('',(#3337),#20338,.F.);
#21458=ADVANCED_FACE('',(#3338),#20339,.F.);
#21459=ADVANCED_FACE('',(#3339),#20340,.F.);
#21460=ADVANCED_FACE('',(#3340),#20341,.F.);
#21461=ADVANCED_FACE('',(#3341),#20342,.F.);
#21462=ADVANCED_FACE('',(#3342),#20343,.F.);
#21463=ADVANCED_FACE('',(#3343),#20344,.F.);
#21464=ADVANCED_FACE('',(#3344),#20345,.F.);
#21465=ADVANCED_FACE('',(#3345),#20346,.F.);
#21466=ADVANCED_FACE('',(#3346),#20347,.F.);
#21467=ADVANCED_FACE('',(#3347),#20348,.F.);
#21468=ADVANCED_FACE('',(#3348),#20349,.F.);
#21469=ADVANCED_FACE('',(#3349),#20350,.F.);
#21470=ADVANCED_FACE('',(#3350),#20351,.F.);
#21471=ADVANCED_FACE('',(#3351),#20352,.F.);
#21472=ADVANCED_FACE('',(#3352),#20353,.F.);
#21473=ADVANCED_FACE('',(#3353),#20354,.F.);
#21474=ADVANCED_FACE('',(#3354),#20355,.F.);
#21475=ADVANCED_FACE('',(#3355),#20356,.F.);
#21476=ADVANCED_FACE('',(#3356),#20357,.F.);
#21477=ADVANCED_FACE('',(#3357),#20358,.F.);
#21478=ADVANCED_FACE('',(#3358),#20359,.F.);
#21479=ADVANCED_FACE('',(#3359),#20360,.F.);
#21480=ADVANCED_FACE('',(#3360),#20361,.F.);
#21481=ADVANCED_FACE('',(#3361),#20362,.F.);
#21482=ADVANCED_FACE('',(#3362),#20363,.F.);
#21483=ADVANCED_FACE('',(#3363),#20364,.F.);
#21484=ADVANCED_FACE('',(#3364),#20365,.F.);
#21485=ADVANCED_FACE('',(#3365),#20366,.F.);
#21486=ADVANCED_FACE('',(#3366),#20367,.F.);
#21487=ADVANCED_FACE('',(#3367),#20368,.F.);
#21488=ADVANCED_FACE('',(#3368),#20369,.F.);
#21489=ADVANCED_FACE('',(#3369),#20370,.F.);
#21490=ADVANCED_FACE('',(#3370),#20371,.F.);
#21491=ADVANCED_FACE('',(#3371),#20372,.F.);
#21492=ADVANCED_FACE('',(#3372),#20373,.F.);
#21493=ADVANCED_FACE('',(#3373),#20374,.F.);
#21494=ADVANCED_FACE('',(#3374),#20375,.F.);
#21495=ADVANCED_FACE('',(#3375),#20376,.F.);
#21496=ADVANCED_FACE('',(#3376),#20377,.F.);
#21497=ADVANCED_FACE('',(#3377),#20378,.F.);
#21498=ADVANCED_FACE('',(#3378),#20379,.F.);
#21499=ADVANCED_FACE('',(#3379),#20380,.F.);
#21500=ADVANCED_FACE('',(#3380),#20381,.F.);
#21501=ADVANCED_FACE('',(#3381),#20382,.F.);
#21502=ADVANCED_FACE('',(#3382),#20383,.F.);
#21503=ADVANCED_FACE('',(#3383),#20384,.F.);
#21504=ADVANCED_FACE('',(#3384),#20385,.F.);
#21505=ADVANCED_FACE('',(#3385),#20386,.F.);
#21506=ADVANCED_FACE('',(#3386),#20387,.F.);
#21507=ADVANCED_FACE('',(#3387),#20388,.F.);
#21508=ADVANCED_FACE('',(#3388),#20389,.F.);
#21509=ADVANCED_FACE('',(#3389),#20390,.F.);
#21510=ADVANCED_FACE('',(#3390),#20391,.F.);
#21511=ADVANCED_FACE('',(#3391),#20392,.F.);
#21512=ADVANCED_FACE('',(#3392),#20393,.F.);
#21513=ADVANCED_FACE('',(#3393),#20394,.F.);
#21514=ADVANCED_FACE('',(#3394),#20395,.F.);
#21515=ADVANCED_FACE('',(#3395),#20396,.F.);
#21516=ADVANCED_FACE('',(#3396),#20397,.F.);
#21517=ADVANCED_FACE('',(#3397),#20398,.F.);
#21518=ADVANCED_FACE('',(#3398),#20399,.F.);
#21519=ADVANCED_FACE('',(#3399),#20400,.F.);
#21520=ADVANCED_FACE('',(#3400),#20401,.F.);
#21521=ADVANCED_FACE('',(#3401),#20402,.F.);
#21522=ADVANCED_FACE('',(#3402),#20403,.F.);
#21523=ADVANCED_FACE('',(#3403),#20404,.F.);
#21524=ADVANCED_FACE('',(#3404),#20405,.F.);
#21525=ADVANCED_FACE('',(#3405),#20406,.F.);
#21526=ADVANCED_FACE('',(#3406),#20407,.F.);
#21527=ADVANCED_FACE('',(#3407),#20408,.F.);
#21528=ADVANCED_FACE('',(#3408),#20409,.F.);
#21529=ADVANCED_FACE('',(#3409),#20410,.F.);
#21530=ADVANCED_FACE('',(#3410),#20411,.F.);
#21531=ADVANCED_FACE('',(#3411),#20412,.F.);
#21532=ADVANCED_FACE('',(#3412),#20413,.F.);
#21533=ADVANCED_FACE('',(#3413),#20414,.F.);
#21534=ADVANCED_FACE('',(#3414),#20415,.F.);
#21535=ADVANCED_FACE('',(#3415),#20416,.F.);
#21536=ADVANCED_FACE('',(#3416),#20417,.F.);
#21537=ADVANCED_FACE('',(#3417),#20418,.F.);
#21538=ADVANCED_FACE('',(#3418),#20419,.F.);
#21539=ADVANCED_FACE('',(#3419),#20420,.F.);
#21540=ADVANCED_FACE('',(#3420),#20421,.F.);
#21541=ADVANCED_FACE('',(#3421),#20422,.F.);
#21542=ADVANCED_FACE('',(#3422),#20423,.F.);
#21543=ADVANCED_FACE('',(#3423),#20424,.F.);
#21544=ADVANCED_FACE('',(#3424),#20425,.F.);
#21545=ADVANCED_FACE('',(#3425),#20426,.F.);
#21546=ADVANCED_FACE('',(#3426),#20427,.F.);
#21547=ADVANCED_FACE('',(#3427),#20428,.F.);
#21548=ADVANCED_FACE('',(#3428),#20429,.F.);
#21549=ADVANCED_FACE('',(#3429),#20430,.F.);
#21550=ADVANCED_FACE('',(#3430),#20431,.F.);
#21551=ADVANCED_FACE('',(#3431),#20432,.F.);
#21552=ADVANCED_FACE('',(#3432),#20433,.F.);
#21553=ADVANCED_FACE('',(#3433),#20434,.F.);
#21554=ADVANCED_FACE('',(#3434),#20435,.F.);
#21555=ADVANCED_FACE('',(#3435),#20436,.F.);
#21556=ADVANCED_FACE('',(#3436),#20437,.F.);
#21557=ADVANCED_FACE('',(#3437),#20438,.F.);
#21558=ADVANCED_FACE('',(#3438),#20439,.F.);
#21559=ADVANCED_FACE('',(#3439),#20440,.F.);
#21560=ADVANCED_FACE('',(#3440),#20441,.F.);
#21561=ADVANCED_FACE('',(#3441),#20442,.F.);
#21562=ADVANCED_FACE('',(#3442),#20443,.F.);
#21563=ADVANCED_FACE('',(#3443),#20444,.F.);
#21564=ADVANCED_FACE('',(#3444),#20445,.F.);
#21565=ADVANCED_FACE('',(#3445),#20446,.F.);
#21566=ADVANCED_FACE('',(#3446),#20447,.F.);
#21567=ADVANCED_FACE('',(#3447),#20448,.F.);
#21568=ADVANCED_FACE('',(#3448),#20449,.F.);
#21569=ADVANCED_FACE('',(#3449),#20450,.F.);
#21570=ADVANCED_FACE('',(#3450),#20451,.F.);
#21571=ADVANCED_FACE('',(#3451),#20452,.F.);
#21572=ADVANCED_FACE('',(#3452),#20453,.F.);
#21573=ADVANCED_FACE('',(#3453),#20454,.F.);
#21574=ADVANCED_FACE('',(#3454),#20455,.F.);
#21575=ADVANCED_FACE('',(#3455),#20456,.F.);
#21576=ADVANCED_FACE('',(#3456),#20457,.F.);
#21577=ADVANCED_FACE('',(#3457),#20458,.F.);
#21578=ADVANCED_FACE('',(#3458),#20459,.F.);
#21579=ADVANCED_FACE('',(#3459),#20460,.F.);
#21580=ADVANCED_FACE('',(#3460),#20461,.F.);
#21581=ADVANCED_FACE('',(#3461),#20462,.F.);
#21582=ADVANCED_FACE('',(#3462),#20463,.F.);
#21583=ADVANCED_FACE('',(#3463),#20464,.F.);
#21584=ADVANCED_FACE('',(#3464),#20465,.F.);
#21585=ADVANCED_FACE('',(#3465),#20466,.F.);
#21586=ADVANCED_FACE('',(#3466),#20467,.F.);
#21587=ADVANCED_FACE('',(#3467),#20468,.F.);
#21588=ADVANCED_FACE('',(#3468),#20469,.F.);
#21589=ADVANCED_FACE('',(#3469),#20470,.F.);
#21590=ADVANCED_FACE('',(#3470),#20471,.F.);
#21591=ADVANCED_FACE('',(#3471),#20472,.F.);
#21592=ADVANCED_FACE('',(#3472),#20473,.F.);
#21593=ADVANCED_FACE('',(#3473),#20474,.F.);
#21594=ADVANCED_FACE('',(#3474),#20475,.F.);
#21595=ADVANCED_FACE('',(#3475),#20476,.F.);
#21596=ADVANCED_FACE('',(#3476),#20477,.F.);
#21597=ADVANCED_FACE('',(#3477),#20478,.F.);
#21598=ADVANCED_FACE('',(#3478),#20479,.F.);
#21599=ADVANCED_FACE('',(#3479),#20480,.F.);
#21600=ADVANCED_FACE('',(#3480),#20481,.F.);
#21601=ADVANCED_FACE('',(#3481),#20482,.F.);
#21602=ADVANCED_FACE('',(#3482),#20483,.F.);
#21603=ADVANCED_FACE('',(#3483),#20484,.F.);
#21604=ADVANCED_FACE('',(#3484),#20485,.F.);
#21605=ADVANCED_FACE('',(#3485),#20486,.F.);
#21606=ADVANCED_FACE('',(#3486),#20487,.F.);
#21607=ADVANCED_FACE('',(#3487),#20488,.F.);
#21608=ADVANCED_FACE('',(#3488),#20489,.F.);
#21609=ADVANCED_FACE('',(#3489),#20490,.F.);
#21610=ADVANCED_FACE('',(#3490),#20491,.F.);
#21611=ADVANCED_FACE('',(#3491),#20492,.F.);
#21612=ADVANCED_FACE('',(#3492),#20493,.F.);
#21613=ADVANCED_FACE('',(#3493),#20494,.F.);
#21614=ADVANCED_FACE('',(#3494),#20495,.F.);
#21615=ADVANCED_FACE('',(#3495),#20496,.F.);
#21616=ADVANCED_FACE('',(#3496),#20497,.F.);
#21617=ADVANCED_FACE('',(#3497),#20498,.F.);
#21618=ADVANCED_FACE('',(#3498),#20499,.F.);
#21619=ADVANCED_FACE('',(#3499),#20500,.F.);
#21620=ADVANCED_FACE('',(#3500),#20501,.F.);
#21621=ADVANCED_FACE('',(#3501),#20502,.F.);
#21622=ADVANCED_FACE('',(#3502),#20503,.F.);
#21623=ADVANCED_FACE('',(#3503),#20504,.F.);
#21624=ADVANCED_FACE('',(#3504),#20505,.F.);
#21625=ADVANCED_FACE('',(#3505),#20506,.F.);
#21626=ADVANCED_FACE('',(#3506),#20507,.F.);
#21627=ADVANCED_FACE('',(#3507),#20508,.F.);
#21628=ADVANCED_FACE('',(#3508),#20509,.F.);
#21629=ADVANCED_FACE('',(#3509),#20510,.F.);
#21630=ADVANCED_FACE('',(#3510),#20511,.F.);
#21631=ADVANCED_FACE('',(#3511),#20512,.F.);
#21632=ADVANCED_FACE('',(#3512),#20513,.F.);
#21633=ADVANCED_FACE('',(#3513),#20514,.F.);
#21634=ADVANCED_FACE('',(#3514),#20515,.F.);
#21635=ADVANCED_FACE('',(#3515),#20516,.F.);
#21636=ADVANCED_FACE('',(#3516),#20517,.F.);
#21637=ADVANCED_FACE('',(#3517),#20518,.F.);
#21638=ADVANCED_FACE('',(#3518),#20519,.F.);
#21639=ADVANCED_FACE('',(#3519),#20520,.F.);
#21640=ADVANCED_FACE('',(#3520),#20521,.F.);
#21641=ADVANCED_FACE('',(#3521),#20522,.F.);
#21642=ADVANCED_FACE('',(#3522),#20523,.F.);
#21643=ADVANCED_FACE('',(#3523),#20524,.F.);
#21644=ADVANCED_FACE('',(#3524),#20525,.F.);
#21645=ADVANCED_FACE('',(#3525),#20526,.F.);
#21646=ADVANCED_FACE('',(#3526),#20527,.F.);
#21647=ADVANCED_FACE('',(#3527),#20528,.F.);
#21648=ADVANCED_FACE('',(#3528),#20529,.F.);
#21649=ADVANCED_FACE('',(#3529),#20530,.F.);
#21650=ADVANCED_FACE('',(#3530),#20531,.F.);
#21651=ADVANCED_FACE('',(#3531),#20532,.F.);
#21652=ADVANCED_FACE('',(#3532),#20533,.F.);
#21653=ADVANCED_FACE('',(#3533),#20534,.F.);
#21654=ADVANCED_FACE('',(#3534),#20535,.F.);
#21655=ADVANCED_FACE('',(#3535),#20536,.F.);
#21656=ADVANCED_FACE('',(#3536),#20537,.F.);
#21657=ADVANCED_FACE('',(#3537),#20538,.F.);
#21658=ADVANCED_FACE('',(#3538),#20539,.F.);
#21659=ADVANCED_FACE('',(#3539),#20540,.F.);
#21660=ADVANCED_FACE('',(#3540),#362,.F.);
#21661=ADVANCED_FACE('',(#3541),#363,.F.);
#21662=ADVANCED_FACE('',(#3542,#2361,#2362,#2363,#2364,#2365,#2366),#2517,
 .T.);
#21663=ADVANCED_FACE('',(#3543),#20541,.F.);
#21664=ADVANCED_FACE('',(#3544),#364,.F.);
#21665=ADVANCED_FACE('',(#3545),#365,.F.);
#21666=ADVANCED_FACE('',(#3546),#20542,.F.);
#21667=ADVANCED_FACE('',(#3547),#366,.F.);
#21668=ADVANCED_FACE('',(#3548),#367,.F.);
#21669=ADVANCED_FACE('',(#3549),#20543,.F.);
#21670=ADVANCED_FACE('',(#3550),#368,.F.);
#21671=ADVANCED_FACE('',(#3551),#369,.F.);
#21672=ADVANCED_FACE('',(#3552),#20544,.F.);
#21673=ADVANCED_FACE('',(#3553),#370,.F.);
#21674=ADVANCED_FACE('',(#3554),#371,.F.);
#21675=ADVANCED_FACE('',(#3555),#20545,.F.);
#21676=ADVANCED_FACE('',(#3556),#372,.F.);
#21677=ADVANCED_FACE('',(#3557),#373,.F.);
#21678=ADVANCED_FACE('',(#3558),#20546,.F.);
#21679=ADVANCED_FACE('',(#3559),#20547,.F.);
#21680=ADVANCED_FACE('',(#3560),#20548,.F.);
#21681=ADVANCED_FACE('',(#3561),#20549,.F.);
#21682=ADVANCED_FACE('',(#3562),#20550,.F.);
#21683=ADVANCED_FACE('',(#3563),#20551,.F.);
#21684=ADVANCED_FACE('',(#3564),#2518,.T.);
#21685=ADVANCED_FACE('',(#3565),#2519,.T.);
#21686=ADVANCED_FACE('',(#3566),#2520,.T.);
#21687=ADVANCED_FACE('',(#3567),#2521,.T.);
#21688=ADVANCED_FACE('',(#3568,#2367,#2368,#2369,#2370,#2371,#2372),#2522,
 .F.);
#21689=ADVANCED_FACE('',(#3569),#20552,.T.);
#21690=ADVANCED_FACE('',(#3570),#20553,.T.);
#21691=ADVANCED_FACE('',(#3571),#20554,.T.);
#21692=ADVANCED_FACE('',(#3572),#20555,.T.);
#21693=ADVANCED_FACE('',(#3573),#20556,.T.);
#21694=ADVANCED_FACE('',(#3574),#20557,.T.);
#21695=ADVANCED_FACE('',(#3575),#20558,.T.);
#21696=ADVANCED_FACE('',(#3576),#20559,.T.);
#21697=ADVANCED_FACE('',(#3577),#20560,.T.);
#21698=ADVANCED_FACE('',(#3578),#20561,.T.);
#21699=ADVANCED_FACE('',(#3579),#20562,.T.);
#21700=ADVANCED_FACE('',(#3580),#20563,.T.);
#21701=ADVANCED_FACE('',(#3581),#20564,.T.);
#21702=ADVANCED_FACE('',(#3582),#20565,.T.);
#21703=ADVANCED_FACE('',(#3583),#20566,.T.);
#21704=ADVANCED_FACE('',(#3584),#20567,.T.);
#21705=ADVANCED_FACE('',(#3585),#20568,.T.);
#21706=ADVANCED_FACE('',(#3586),#20569,.T.);
#21707=ADVANCED_FACE('',(#3587),#20570,.T.);
#21708=ADVANCED_FACE('',(#3588),#20571,.T.);
#21709=ADVANCED_FACE('',(#3589),#20572,.T.);
#21710=ADVANCED_FACE('',(#3590),#20573,.T.);
#21711=ADVANCED_FACE('',(#3591),#20574,.T.);
#21712=ADVANCED_FACE('',(#3592),#20575,.T.);
#21713=ADVANCED_FACE('',(#3593),#20576,.T.);
#21714=ADVANCED_FACE('',(#3594),#20577,.T.);
#21715=ADVANCED_FACE('',(#3595),#20578,.T.);
#21716=ADVANCED_FACE('',(#3596),#20579,.T.);
#21717=ADVANCED_FACE('',(#3597),#20580,.T.);
#21718=ADVANCED_FACE('',(#3598),#20581,.T.);
#21719=ADVANCED_FACE('',(#3599),#20582,.T.);
#21720=ADVANCED_FACE('',(#3600),#20583,.T.);
#21721=ADVANCED_FACE('',(#3601),#20584,.T.);
#21722=ADVANCED_FACE('',(#3602),#20585,.T.);
#21723=ADVANCED_FACE('',(#3603),#20586,.T.);
#21724=ADVANCED_FACE('',(#3604),#20587,.T.);
#21725=ADVANCED_FACE('',(#3605),#20588,.T.);
#21726=ADVANCED_FACE('',(#3606),#20589,.T.);
#21727=ADVANCED_FACE('',(#3607),#20590,.T.);
#21728=ADVANCED_FACE('',(#3608),#20591,.T.);
#21729=ADVANCED_FACE('',(#3609),#20592,.T.);
#21730=ADVANCED_FACE('',(#3610),#20593,.T.);
#21731=ADVANCED_FACE('',(#3611),#20594,.T.);
#21732=ADVANCED_FACE('',(#3612),#20595,.T.);
#21733=ADVANCED_FACE('',(#3613),#20596,.T.);
#21734=ADVANCED_FACE('',(#3614),#20597,.T.);
#21735=ADVANCED_FACE('',(#3615),#20598,.T.);
#21736=ADVANCED_FACE('',(#3616),#20599,.T.);
#21737=ADVANCED_FACE('',(#3617),#20600,.T.);
#21738=ADVANCED_FACE('',(#3618),#20601,.T.);
#21739=ADVANCED_FACE('',(#3619),#20602,.T.);
#21740=ADVANCED_FACE('',(#3620),#20603,.T.);
#21741=ADVANCED_FACE('',(#3621),#20604,.T.);
#21742=ADVANCED_FACE('',(#3622),#20605,.T.);
#21743=ADVANCED_FACE('',(#3623),#20606,.T.);
#21744=ADVANCED_FACE('',(#3624),#20607,.T.);
#21745=ADVANCED_FACE('',(#3625),#20608,.T.);
#21746=ADVANCED_FACE('',(#3626),#20609,.T.);
#21747=ADVANCED_FACE('',(#3627),#20610,.T.);
#21748=ADVANCED_FACE('',(#3628),#20611,.T.);
#21749=ADVANCED_FACE('',(#3629),#20612,.T.);
#21750=ADVANCED_FACE('',(#3630),#20613,.T.);
#21751=ADVANCED_FACE('',(#3631),#20614,.T.);
#21752=ADVANCED_FACE('',(#3632),#20615,.T.);
#21753=ADVANCED_FACE('',(#3633),#20616,.T.);
#21754=ADVANCED_FACE('',(#3634),#20617,.T.);
#21755=ADVANCED_FACE('',(#3635),#20618,.T.);
#21756=ADVANCED_FACE('',(#3636),#20619,.T.);
#21757=ADVANCED_FACE('',(#3637),#20620,.T.);
#21758=ADVANCED_FACE('',(#3638),#20621,.T.);
#21759=ADVANCED_FACE('',(#3639),#20622,.T.);
#21760=ADVANCED_FACE('',(#3640),#20623,.T.);
#21761=ADVANCED_FACE('',(#3641),#20624,.T.);
#21762=ADVANCED_FACE('',(#3642),#20625,.T.);
#21763=ADVANCED_FACE('',(#3643),#20626,.T.);
#21764=ADVANCED_FACE('',(#3644),#20627,.T.);
#21765=ADVANCED_FACE('',(#3645),#20628,.T.);
#21766=ADVANCED_FACE('',(#3646),#20629,.T.);
#21767=ADVANCED_FACE('',(#3647),#20630,.T.);
#21768=ADVANCED_FACE('',(#3648),#20631,.T.);
#21769=ADVANCED_FACE('',(#3649),#20632,.T.);
#21770=ADVANCED_FACE('',(#3650),#20633,.T.);
#21771=ADVANCED_FACE('',(#3651),#20634,.T.);
#21772=ADVANCED_FACE('',(#3652),#20635,.T.);
#21773=ADVANCED_FACE('',(#3653),#20636,.T.);
#21774=ADVANCED_FACE('',(#3654),#20637,.T.);
#21775=ADVANCED_FACE('',(#3655),#20638,.T.);
#21776=ADVANCED_FACE('',(#3656),#20639,.T.);
#21777=ADVANCED_FACE('',(#3657),#20640,.T.);
#21778=ADVANCED_FACE('',(#3658),#20641,.T.);
#21779=ADVANCED_FACE('',(#3659),#20642,.T.);
#21780=ADVANCED_FACE('',(#3660),#20643,.T.);
#21781=ADVANCED_FACE('',(#3661),#20644,.T.);
#21782=ADVANCED_FACE('',(#3662),#20645,.T.);
#21783=ADVANCED_FACE('',(#3663),#20646,.T.);
#21784=ADVANCED_FACE('',(#3664),#20647,.T.);
#21785=ADVANCED_FACE('',(#3665),#20648,.T.);
#21786=ADVANCED_FACE('',(#3666),#20649,.T.);
#21787=ADVANCED_FACE('',(#3667),#333,.T.);
#21788=ADVANCED_FACE('',(#3668),#374,.F.);
#21789=ADVANCED_FACE('',(#3669),#20650,.T.);
#21790=ADVANCED_FACE('',(#3670),#375,.F.);
#21791=ADVANCED_FACE('',(#3671),#20651,.T.);
#21792=ADVANCED_FACE('',(#3672),#2523,.F.);
#21793=ADVANCED_FACE('',(#3673),#2524,.F.);
#21794=ADVANCED_FACE('',(#3674),#2525,.F.);
#21795=ADVANCED_FACE('',(#3675),#2526,.F.);
#21796=ADVANCED_FACE('',(#3676),#2527,.F.);
#21797=ADVANCED_FACE('',(#3677),#2528,.F.);
#21798=ADVANCED_FACE('',(#3678),#2529,.F.);
#21799=ADVANCED_FACE('',(#3679,#2373),#2530,.T.);
#21800=ADVANCED_FACE('',(#3680),#20652,.T.);
#21801=ADVANCED_FACE('',(#3681,#2374),#2531,.F.);
#21802=ADVANCED_FACE('',(#3682),#2532,.T.);
#21803=ADVANCED_FACE('',(#3683),#20653,.F.);
#21804=ADVANCED_FACE('',(#3684),#20654,.T.);
#21805=ADVANCED_FACE('',(#3685,#2375),#2533,.T.);
#21806=ADVANCED_FACE('',(#3686,#2376),#2534,.F.);
#21807=ADVANCED_FACE('',(#3687),#20655,.F.);
#21808=ADVANCED_FACE('',(#3688),#20656,.T.);
#21809=ADVANCED_FACE('',(#3689,#2377),#2535,.T.);
#21810=ADVANCED_FACE('',(#3690,#2378),#2536,.F.);
#21811=CLOSED_SHELL('',(#20657,#20658,#20659,#20660,#20661,#20662,#20663,
#20664,#20665,#20666,#20667,#20668,#20669,#20670,#20671,#20672));
#21812=CLOSED_SHELL('',(#20673,#20674,#20675,#20676,#20677,#20678,#20679,
#20680,#20681,#20682));
#21813=CLOSED_SHELL('',(#20683,#20684,#20685,#20686,#20687,#20688,#20689,
#20690,#20691,#20692,#20693,#20694,#20695,#20696,#20697,#20698,#20699,#20700,
#20701,#20702,#20703,#20704,#20705,#20706,#20707,#20708,#20709,#20710,#20711,
#20712,#20713,#20714,#20715,#20716,#20717,#20718,#20719,#20720,#20721,#20722,
#20723,#20724,#20725,#20726,#20727,#20728,#20729,#20730,#20731,#20732,#20733,
#20734,#20735,#20736,#20737,#20738,#20739,#20740,#20741,#20742,#20743,#20744,
#20745,#20746,#20747,#20748,#20749,#20750,#20751,#20752,#20753,#20754,#20755,
#20756,#20757,#20758,#20759,#20760,#20761,#20762,#20763,#20764,#20765,#20766,
#20767,#20768));
#21814=CLOSED_SHELL('',(#20769,#20770,#20771,#20772,#20773,#20774,#20775,
#20776,#20777,#20778,#20779,#20780,#20781,#20782,#20783,#20784,#20785,#20786,
#20787,#20788,#20789,#20790,#20791,#20792,#20793,#20794,#20795,#20796,#20797,
#20798,#20799,#20800,#20801,#20802,#20803,#20804,#20805,#20806,#20807,#20808,
#20809,#20810,#20811,#20812,#20813,#20814,#20815,#20816,#20817,#20818,#20819,
#20820,#20821,#20822,#20823,#20824,#20825,#20826,#20827,#20828,#20829,#20830,
#20831,#20832));
#21815=CLOSED_SHELL('',(#20833,#20834,#20835,#20836));
#21816=CLOSED_SHELL('',(#20837,#20838,#20839,#20840,#20841,#20842,#20843,
#20844,#20845,#20846,#20847,#20848,#20849,#20850,#20851,#20852,#20853,#20854,
#20855,#20856,#20857,#20858,#20859,#20860,#20861,#20862,#20863,#20864,#20865,
#20866,#20867,#20868,#20869,#20870,#20871,#20872,#20873,#20874,#20875,#20876,
#20877,#20878,#20879,#20880,#20881,#20882,#20883,#20884,#20885,#20886,#20887,
#20888,#20889,#20890,#20891,#20892,#20893,#20894,#20895,#20896,#20897,#20898,
#20899,#20900,#20901,#20902,#20903,#20904,#20905,#20906,#20907,#20908,#20909,
#20910,#20911,#20912,#20913,#20914,#20915,#20916,#20917,#20918,#20919,#20920,
#20921,#20922,#20923,#20924,#20925,#20926,#20927,#20928,#20929,#20930,#20931,
#20932,#20933,#20934,#20935,#20936,#20937,#20938,#20939,#20940,#20941,#20942,
#20943,#20944,#20945,#20946,#20947,#20948,#20949,#20950,#20951,#20952,#20953,
#20954,#20955,#20956,#20957,#20958,#20959,#20960,#20961,#20962,#20963,#20964,
#20965,#20966,#20967,#20968,#20969,#20970,#20971,#20972,#20973,#20974,#20975,
#20976,#20977,#20978,#20979,#20980,#20981,#20982,#20983,#20984,#20985,#20986,
#20987,#20988,#20989,#20990,#20991,#20992,#20993,#20994,#20995,#20996,#20997,
#20998,#20999,#21000,#21001,#21002,#21003,#21004,#21005,#21006,#21007,#21008,
#21009,#21010,#21011,#21012,#21013,#21014,#21015,#21016,#21017,#21018,#21019,
#21020,#21021,#21022,#21023,#21024,#21025,#21026,#21027,#21028,#21029,#21030,
#21031,#21032,#21033,#21034,#21035,#21036,#21037,#21038,#21039,#21040,#21041,
#21042,#21043,#21044,#21045,#21046,#21047,#21048,#21049,#21050,#21051,#21052,
#21053,#21054,#21055,#21056,#21057));
#21817=CLOSED_SHELL('',(#21058,#21059,#21060,#21061,#21062,#21063,#21064,
#21065,#21066,#21067,#21068,#21069,#21070));
#21818=CLOSED_SHELL('',(#21071,#21072,#21073,#21074,#21075,#21076,#21077,
#21078,#21079,#21080,#21081,#21082,#21083,#21084,#21085,#21086,#21087,#21088,
#21089,#21090,#21091,#21092,#21093,#21094,#21095,#21096,#21097,#21098,#21099,
#21100,#21101,#21102,#21103,#21104,#21105,#21106,#21107,#21108,#21109,#21110,
#21111,#21112,#21113,#21114,#21115,#21116,#21117,#21118,#21119,#21120,#21121,
#21122,#21123,#21124));
#21819=CLOSED_SHELL('',(#21125,#21126,#21127));
#21820=CLOSED_SHELL('',(#21128,#21129,#21130,#21131,#21132,#21133,#21134,
#21135,#21136,#21137,#21138,#21139,#21140,#21141,#21142,#21143,#21144,#21145,
#21146,#21147,#21148,#21149,#21150,#21151,#21152,#21153,#21154,#21155,#21156,
#21157,#21158,#21159,#21160,#21161,#21162,#21163,#21164,#21165,#21166,#21167,
#21168,#21169,#21170,#21171,#21172,#21173,#21174,#21175,#21176,#21177,#21178,
#21179,#21180,#21181,#21182,#21183,#21184,#21185,#21186,#21187,#21188,#21189,
#21190,#21191,#21192,#21193,#21194,#21195,#21196,#21197));
#21821=CLOSED_SHELL('',(#21198,#21199,#21200,#21201,#21202,#21203,#21204,
#21205));
#21822=CLOSED_SHELL('',(#21206,#21207,#21208,#21209,#21210,#21211,#21212,
#21213,#21214,#21215,#21216,#21217,#21218,#21219,#21220,#21221,#21222,#21223,
#21224,#21225,#21226,#21227,#21228,#21229,#21230,#21231,#21232,#21233,#21234,
#21235,#21236,#21237,#21238,#21239,#21240,#21241,#21242,#21243,#21244,#21245,
#21246,#21247,#21248,#21249,#21250,#21251,#21252,#21253,#21254,#21255,#21256,
#21257,#21258,#21259,#21260,#21261,#21262,#21263,#21264,#21265,#21266,#21267,
#21268,#21269,#21270,#21271,#21272,#21273,#21274,#21275,#21276,#21277,#21278,
#21279,#21280,#21281,#21282,#21283,#21284,#21285,#21286,#21287,#21288,#21289,
#21290,#21291,#21292,#21293,#21294,#21295,#21296,#21297,#21298,#21299,#21300,
#21301,#21302,#21303,#21304,#21305,#21306,#21307,#21308,#21309,#21310,#21311,
#21312,#21313,#21314,#21315,#21316,#21317,#21318,#21319,#21320,#21321,#21322,
#21323,#21324,#21325,#21326,#21327,#21328,#21329,#21330,#21331,#21332,#21333,
#21334,#21335,#21336,#21337,#21338,#21339,#21340));
#21823=CLOSED_SHELL('',(#21341,#21342,#21343,#21344,#21345,#21346,#21347,
#21348,#21349,#21350,#21351,#21352,#21353,#21354,#21355,#21356,#21357,#21358,
#21359,#21360,#21361,#21362,#21363,#21364,#21365,#21366,#21367,#21368));
#21824=CLOSED_SHELL('',(#21369,#21370,#21371,#21372));
#21825=CLOSED_SHELL('',(#21373,#21374,#21375,#21376,#21377,#21378,#21379,
#21380,#21381,#21382,#21383,#21384,#21385,#21386,#21387,#21388,#21389,#21390,
#21391,#21392,#21393,#21394,#21395,#21396,#21397,#21398,#21399,#21400,#21401,
#21402,#21403,#21404,#21405,#21406,#21407,#21408,#21409,#21410,#21411,#21412,
#21413,#21414,#21415,#21416,#21417,#21418));
#21826=CLOSED_SHELL('',(#21419,#21420,#21421,#21422,#21423,#21424,#21425,
#21426,#21427,#21428,#21429,#21430,#21431,#21432,#21433,#21434,#21435,#21436,
#21437,#21438,#21439,#21440,#21441,#21442,#21443,#21444,#21445,#21446,#21447,
#21448,#21449,#21450,#21451,#21452,#21453,#21454,#21455,#21456,#21457,#21458,
#21459,#21460,#21461,#21462,#21463,#21464,#21465,#21466,#21467,#21468,#21469,
#21470,#21471,#21472,#21473,#21474,#21475,#21476,#21477,#21478,#21479,#21480,
#21481,#21482,#21483,#21484,#21485,#21486,#21487,#21488,#21489,#21490,#21491,
#21492,#21493,#21494,#21495,#21496,#21497,#21498,#21499,#21500,#21501,#21502,
#21503,#21504,#21505,#21506,#21507,#21508,#21509,#21510,#21511,#21512,#21513,
#21514,#21515,#21516,#21517,#21518,#21519,#21520,#21521,#21522,#21523,#21524,
#21525,#21526,#21527,#21528,#21529,#21530,#21531,#21532,#21533,#21534,#21535,
#21536,#21537,#21538,#21539,#21540,#21541,#21542,#21543,#21544,#21545,#21546,
#21547,#21548,#21549,#21550,#21551,#21552,#21553,#21554,#21555,#21556,#21557,
#21558,#21559,#21560,#21561,#21562,#21563,#21564,#21565,#21566,#21567,#21568,
#21569,#21570,#21571,#21572,#21573,#21574,#21575,#21576,#21577,#21578,#21579,
#21580,#21581,#21582,#21583,#21584,#21585,#21586,#21587,#21588,#21589,#21590,
#21591,#21592,#21593,#21594,#21595,#21596,#21597,#21598,#21599,#21600,#21601,
#21602,#21603,#21604,#21605,#21606,#21607,#21608,#21609,#21610,#21611,#21612,
#21613,#21614,#21615,#21616,#21617,#21618,#21619,#21620,#21621,#21622,#21623,
#21624,#21625,#21626,#21627,#21628,#21629,#21630,#21631,#21632,#21633,#21634,
#21635,#21636,#21637,#21638,#21639,#21640,#21641,#21642,#21643,#21644,#21645,
#21646,#21647,#21648,#21649,#21650,#21651,#21652,#21653,#21654,#21655,#21656,
#21657,#21658,#21659,#21660,#21661,#21662,#21663,#21664,#21665,#21666,#21667,
#21668,#21669,#21670,#21671,#21672,#21673,#21674,#21675,#21676,#21677,#21678,
#21679,#21680,#21681,#21682,#21683,#21684,#21685,#21686,#21687,#21688));
#21827=CLOSED_SHELL('',(#21689,#21690,#21691,#21692,#21693,#21694,#21695,
#21696,#21697,#21698,#21699,#21700,#21701,#21702,#21703,#21704,#21705,#21706,
#21707,#21708,#21709,#21710,#21711,#21712,#21713,#21714,#21715,#21716,#21717,
#21718,#21719,#21720,#21721,#21722,#21723,#21724,#21725,#21726,#21727,#21728,
#21729,#21730,#21731,#21732,#21733,#21734,#21735,#21736,#21737,#21738,#21739,
#21740,#21741,#21742,#21743,#21744,#21745,#21746,#21747,#21748,#21749,#21750,
#21751,#21752,#21753,#21754,#21755,#21756,#21757,#21758,#21759,#21760,#21761,
#21762,#21763,#21764,#21765,#21766,#21767,#21768,#21769,#21770,#21771,#21772,
#21773,#21774,#21775,#21776,#21777,#21778,#21779,#21780,#21781,#21782,#21783,
#21784,#21785,#21786,#21787,#21788,#21789,#21790,#21791,#21792,#21793,#21794,
#21795,#21796,#21797,#21798,#21799,#21800,#21801,#21802));
#21828=CLOSED_SHELL('',(#21803,#21804,#21805,#21806));
#21829=CLOSED_SHELL('',(#21807,#21808,#21809,#21810));
#21830=DERIVED_UNIT_ELEMENT(#21868,1.);
#21831=DERIVED_UNIT_ELEMENT(#97477,-3.);
#21832=DERIVED_UNIT_ELEMENT(#21868,1.);
#21833=DERIVED_UNIT_ELEMENT(#97477,-3.);
#21834=DERIVED_UNIT_ELEMENT(#21868,1.);
#21835=DERIVED_UNIT_ELEMENT(#97477,-3.);
#21836=DERIVED_UNIT_ELEMENT(#21868,1.);
#21837=DERIVED_UNIT_ELEMENT(#97477,-3.);
#21838=DERIVED_UNIT_ELEMENT(#21868,1.);
#21839=DERIVED_UNIT_ELEMENT(#97477,-3.);
#21840=DERIVED_UNIT_ELEMENT(#21868,1.);
#21841=DERIVED_UNIT_ELEMENT(#97477,-3.);
#21842=DERIVED_UNIT_ELEMENT(#21868,1.);
#21843=DERIVED_UNIT_ELEMENT(#97477,-3.);
#21844=DERIVED_UNIT_ELEMENT(#21868,1.);
#21845=DERIVED_UNIT_ELEMENT(#97477,-3.);
#21846=DERIVED_UNIT_ELEMENT(#21868,1.);
#21847=DERIVED_UNIT_ELEMENT(#97477,-3.);
#21848=DERIVED_UNIT_ELEMENT(#21868,1.);
#21849=DERIVED_UNIT_ELEMENT(#97477,-3.);
#21850=DERIVED_UNIT_ELEMENT(#21868,1.);
#21851=DERIVED_UNIT_ELEMENT(#97477,-3.);
#21852=DERIVED_UNIT_ELEMENT(#21868,1.);
#21853=DERIVED_UNIT_ELEMENT(#97477,-3.);
#21854=DERIVED_UNIT_ELEMENT(#21868,1.);
#21855=DERIVED_UNIT_ELEMENT(#97477,-3.);
#21856=DERIVED_UNIT_ELEMENT(#21868,1.);
#21857=DERIVED_UNIT_ELEMENT(#97477,-3.);
#21858=DERIVED_UNIT_ELEMENT(#21868,1.);
#21859=DERIVED_UNIT_ELEMENT(#97477,-3.);
#21860=DERIVED_UNIT_ELEMENT(#21868,1.);
#21861=DERIVED_UNIT_ELEMENT(#97477,-3.);
#21862=DERIVED_UNIT_ELEMENT(#21868,1.);
#21863=DERIVED_UNIT_ELEMENT(#97477,-3.);
#21864=DERIVED_UNIT_ELEMENT(#21868,1.);
#21865=DERIVED_UNIT_ELEMENT(#97477,-3.);
#21866=DERIVED_UNIT_ELEMENT(#21868,1.);
#21867=DERIVED_UNIT_ELEMENT(#97477,-3.);
#21868=(
MASS_UNIT()
NAMED_UNIT(*)
SI_UNIT(.KILO.,.GRAM.)
);
#21869=DERIVED_UNIT((#21830,#21831));
#21870=DERIVED_UNIT((#21832,#21833));
#21871=DERIVED_UNIT((#21834,#21835));
#21872=DERIVED_UNIT((#21836,#21837));
#21873=DERIVED_UNIT((#21838,#21839));
#21874=DERIVED_UNIT((#21840,#21841));
#21875=DERIVED_UNIT((#21842,#21843));
#21876=DERIVED_UNIT((#21844,#21845));
#21877=DERIVED_UNIT((#21846,#21847));
#21878=DERIVED_UNIT((#21848,#21849));
#21879=DERIVED_UNIT((#21850,#21851));
#21880=DERIVED_UNIT((#21852,#21853));
#21881=DERIVED_UNIT((#21854,#21855));
#21882=DERIVED_UNIT((#21856,#21857));
#21883=DERIVED_UNIT((#21858,#21859));
#21884=DERIVED_UNIT((#21860,#21861));
#21885=DERIVED_UNIT((#21862,#21863));
#21886=DERIVED_UNIT((#21864,#21865));
#21887=DERIVED_UNIT((#21866,#21867));
#21888=MEASURE_REPRESENTATION_ITEM('density measure',
POSITIVE_RATIO_MEASURE(7850.),#21869);
#21889=MEASURE_REPRESENTATION_ITEM('density measure',
POSITIVE_RATIO_MEASURE(7850.),#21870);
#21890=MEASURE_REPRESENTATION_ITEM('density measure',
POSITIVE_RATIO_MEASURE(7850.),#21871);
#21891=MEASURE_REPRESENTATION_ITEM('density measure',
POSITIVE_RATIO_MEASURE(7850.),#21872);
#21892=MEASURE_REPRESENTATION_ITEM('density measure',
POSITIVE_RATIO_MEASURE(7850.),#21873);
#21893=MEASURE_REPRESENTATION_ITEM('density measure',
POSITIVE_RATIO_MEASURE(2700.),#21874);
#21894=MEASURE_REPRESENTATION_ITEM('density measure',
POSITIVE_RATIO_MEASURE(7850.),#21875);
#21895=MEASURE_REPRESENTATION_ITEM('density measure',
POSITIVE_RATIO_MEASURE(7850.),#21876);
#21896=MEASURE_REPRESENTATION_ITEM('density measure',
POSITIVE_RATIO_MEASURE(7850.),#21877);
#21897=MEASURE_REPRESENTATION_ITEM('density measure',
POSITIVE_RATIO_MEASURE(7850.),#21878);
#21898=MEASURE_REPRESENTATION_ITEM('density measure',
POSITIVE_RATIO_MEASURE(7850.),#21879);
#21899=MEASURE_REPRESENTATION_ITEM('density measure',
POSITIVE_RATIO_MEASURE(7850.),#21880);
#21900=MEASURE_REPRESENTATION_ITEM('density measure',
POSITIVE_RATIO_MEASURE(7850.),#21881);
#21901=MEASURE_REPRESENTATION_ITEM('density measure',
POSITIVE_RATIO_MEASURE(7850.),#21882);
#21902=MEASURE_REPRESENTATION_ITEM('density measure',
POSITIVE_RATIO_MEASURE(7850.),#21883);
#21903=MEASURE_REPRESENTATION_ITEM('density measure',
POSITIVE_RATIO_MEASURE(2700.),#21884);
#21904=MEASURE_REPRESENTATION_ITEM('density measure',
POSITIVE_RATIO_MEASURE(7850.),#21885);
#21905=MEASURE_REPRESENTATION_ITEM('density measure',
POSITIVE_RATIO_MEASURE(7850.),#21886);
#21906=MEASURE_REPRESENTATION_ITEM('density measure',
POSITIVE_RATIO_MEASURE(7850.),#21887);
#21907=PROPERTY_DEFINITION_REPRESENTATION(#22002,#21945);
#21908=PROPERTY_DEFINITION_REPRESENTATION(#22003,#21946);
#21909=PROPERTY_DEFINITION_REPRESENTATION(#22004,#21947);
#21910=PROPERTY_DEFINITION_REPRESENTATION(#22005,#21948);
#21911=PROPERTY_DEFINITION_REPRESENTATION(#22006,#21949);
#21912=PROPERTY_DEFINITION_REPRESENTATION(#22007,#21950);
#21913=PROPERTY_DEFINITION_REPRESENTATION(#22008,#21951);
#21914=PROPERTY_DEFINITION_REPRESENTATION(#22009,#21952);
#21915=PROPERTY_DEFINITION_REPRESENTATION(#22010,#21953);
#21916=PROPERTY_DEFINITION_REPRESENTATION(#22011,#21954);
#21917=PROPERTY_DEFINITION_REPRESENTATION(#22012,#21955);
#21918=PROPERTY_DEFINITION_REPRESENTATION(#22013,#21956);
#21919=PROPERTY_DEFINITION_REPRESENTATION(#22014,#21957);
#21920=PROPERTY_DEFINITION_REPRESENTATION(#22015,#21958);
#21921=PROPERTY_DEFINITION_REPRESENTATION(#22016,#21959);
#21922=PROPERTY_DEFINITION_REPRESENTATION(#22017,#21960);
#21923=PROPERTY_DEFINITION_REPRESENTATION(#22018,#21961);
#21924=PROPERTY_DEFINITION_REPRESENTATION(#22019,#21962);
#21925=PROPERTY_DEFINITION_REPRESENTATION(#22020,#21963);
#21926=PROPERTY_DEFINITION_REPRESENTATION(#22021,#21964);
#21927=PROPERTY_DEFINITION_REPRESENTATION(#22022,#21965);
#21928=PROPERTY_DEFINITION_REPRESENTATION(#22023,#21966);
#21929=PROPERTY_DEFINITION_REPRESENTATION(#22024,#21967);
#21930=PROPERTY_DEFINITION_REPRESENTATION(#22025,#21968);
#21931=PROPERTY_DEFINITION_REPRESENTATION(#22026,#21969);
#21932=PROPERTY_DEFINITION_REPRESENTATION(#22027,#21970);
#21933=PROPERTY_DEFINITION_REPRESENTATION(#22028,#21971);
#21934=PROPERTY_DEFINITION_REPRESENTATION(#22029,#21972);
#21935=PROPERTY_DEFINITION_REPRESENTATION(#22030,#21973);
#21936=PROPERTY_DEFINITION_REPRESENTATION(#22031,#21974);
#21937=PROPERTY_DEFINITION_REPRESENTATION(#22032,#21975);
#21938=PROPERTY_DEFINITION_REPRESENTATION(#22033,#21976);
#21939=PROPERTY_DEFINITION_REPRESENTATION(#22034,#21977);
#21940=PROPERTY_DEFINITION_REPRESENTATION(#22035,#21978);
#21941=PROPERTY_DEFINITION_REPRESENTATION(#22036,#21979);
#21942=PROPERTY_DEFINITION_REPRESENTATION(#22037,#21980);
#21943=PROPERTY_DEFINITION_REPRESENTATION(#22038,#21981);
#21944=PROPERTY_DEFINITION_REPRESENTATION(#22039,#21982);
#21945=REPRESENTATION('material name',(#21983),#97455);
#21946=REPRESENTATION('density',(#21888),#97455);
#21947=REPRESENTATION('material name',(#21984),#97456);
#21948=REPRESENTATION('density',(#21889),#97456);
#21949=REPRESENTATION('material name',(#21985),#97457);
#21950=REPRESENTATION('density',(#21890),#97457);
#21951=REPRESENTATION('material name',(#21986),#97458);
#21952=REPRESENTATION('density',(#21891),#97458);
#21953=REPRESENTATION('material name',(#21987),#97459);
#21954=REPRESENTATION('density',(#21892),#97459);
#21955=REPRESENTATION('material name',(#21988),#97461);
#21956=REPRESENTATION('density',(#21893),#97461);
#21957=REPRESENTATION('material name',(#21989),#97462);
#21958=REPRESENTATION('density',(#21894),#97462);
#21959=REPRESENTATION('material name',(#21990),#97463);
#21960=REPRESENTATION('density',(#21895),#97463);
#21961=REPRESENTATION('material name',(#21991),#97464);
#21962=REPRESENTATION('density',(#21896),#97464);
#21963=REPRESENTATION('material name',(#21992),#97465);
#21964=REPRESENTATION('density',(#21897),#97465);
#21965=REPRESENTATION('material name',(#21993),#97466);
#21966=REPRESENTATION('density',(#21898),#97466);
#21967=REPRESENTATION('material name',(#21994),#97467);
#21968=REPRESENTATION('density',(#21899),#97467);
#21969=REPRESENTATION('material name',(#21995),#97468);
#21970=REPRESENTATION('density',(#21900),#97468);
#21971=REPRESENTATION('material name',(#21996),#97469);
#21972=REPRESENTATION('density',(#21901),#97469);
#21973=REPRESENTATION('material name',(#21997),#97470);
#21974=REPRESENTATION('density',(#21902),#97470);
#21975=REPRESENTATION('material name',(#21998),#97471);
#21976=REPRESENTATION('density',(#21903),#97471);
#21977=REPRESENTATION('material name',(#21999),#97472);
#21978=REPRESENTATION('density',(#21904),#97472);
#21979=REPRESENTATION('material name',(#22000),#97473);
#21980=REPRESENTATION('density',(#21905),#97473);
#21981=REPRESENTATION('material name',(#22001),#97474);
#21982=REPRESENTATION('density',(#21906),#97474);
#21983=DESCRIPTIVE_REPRESENTATION_ITEM('Steel','Steel');
#21984=DESCRIPTIVE_REPRESENTATION_ITEM('Steel','Steel');
#21985=DESCRIPTIVE_REPRESENTATION_ITEM('Steel','Steel');
#21986=DESCRIPTIVE_REPRESENTATION_ITEM('Steel','Steel');
#21987=DESCRIPTIVE_REPRESENTATION_ITEM('Steel','Steel');
#21988=DESCRIPTIVE_REPRESENTATION_ITEM('Aluminum 6061','Aluminum 6061');
#21989=DESCRIPTIVE_REPRESENTATION_ITEM('Steel','Steel');
#21990=DESCRIPTIVE_REPRESENTATION_ITEM('Steel','Steel');
#21991=DESCRIPTIVE_REPRESENTATION_ITEM('Steel','Steel');
#21992=DESCRIPTIVE_REPRESENTATION_ITEM('Steel','Steel');
#21993=DESCRIPTIVE_REPRESENTATION_ITEM('Steel','Steel');
#21994=DESCRIPTIVE_REPRESENTATION_ITEM('Steel','Steel');
#21995=DESCRIPTIVE_REPRESENTATION_ITEM('Steel','Steel');
#21996=DESCRIPTIVE_REPRESENTATION_ITEM('Steel','Steel');
#21997=DESCRIPTIVE_REPRESENTATION_ITEM('Steel','Steel');
#21998=DESCRIPTIVE_REPRESENTATION_ITEM('Aluminum 6061','Aluminum 6061');
#21999=DESCRIPTIVE_REPRESENTATION_ITEM('Steel','Steel');
#22000=DESCRIPTIVE_REPRESENTATION_ITEM('Steel','Steel');
#22001=DESCRIPTIVE_REPRESENTATION_ITEM('Steel','Steel');
#22002=PROPERTY_DEFINITION('material property','material name',#97628);
#22003=PROPERTY_DEFINITION('material property','density of part',#97628);
#22004=PROPERTY_DEFINITION('material property','material name',#97629);
#22005=PROPERTY_DEFINITION('material property','density of part',#97629);
#22006=PROPERTY_DEFINITION('material property','material name',#97630);
#22007=PROPERTY_DEFINITION('material property','density of part',#97630);
#22008=PROPERTY_DEFINITION('material property','material name',#97631);
#22009=PROPERTY_DEFINITION('material property','density of part',#97631);
#22010=PROPERTY_DEFINITION('material property','material name',#97632);
#22011=PROPERTY_DEFINITION('material property','density of part',#97632);
#22012=PROPERTY_DEFINITION('material property','material name',#97634);
#22013=PROPERTY_DEFINITION('material property','density of part',#97634);
#22014=PROPERTY_DEFINITION('material property','material name',#97635);
#22015=PROPERTY_DEFINITION('material property','density of part',#97635);
#22016=PROPERTY_DEFINITION('material property','material name',#97636);
#22017=PROPERTY_DEFINITION('material property','density of part',#97636);
#22018=PROPERTY_DEFINITION('material property','material name',#97637);
#22019=PROPERTY_DEFINITION('material property','density of part',#97637);
#22020=PROPERTY_DEFINITION('material property','material name',#97638);
#22021=PROPERTY_DEFINITION('material property','density of part',#97638);
#22022=PROPERTY_DEFINITION('material property','material name',#97639);
#22023=PROPERTY_DEFINITION('material property','density of part',#97639);
#22024=PROPERTY_DEFINITION('material property','material name',#97640);
#22025=PROPERTY_DEFINITION('material property','density of part',#97640);
#22026=PROPERTY_DEFINITION('material property','material name',#97641);
#22027=PROPERTY_DEFINITION('material property','density of part',#97641);
#22028=PROPERTY_DEFINITION('material property','material name',#97642);
#22029=PROPERTY_DEFINITION('material property','density of part',#97642);
#22030=PROPERTY_DEFINITION('material property','material name',#97643);
#22031=PROPERTY_DEFINITION('material property','density of part',#97643);
#22032=PROPERTY_DEFINITION('material property','material name',#97644);
#22033=PROPERTY_DEFINITION('material property','density of part',#97644);
#22034=PROPERTY_DEFINITION('material property','material name',#97645);
#22035=PROPERTY_DEFINITION('material property','density of part',#97645);
#22036=PROPERTY_DEFINITION('material property','material name',#97646);
#22037=PROPERTY_DEFINITION('material property','density of part',#97646);
#22038=PROPERTY_DEFINITION('material property','material name',#97647);
#22039=PROPERTY_DEFINITION('material property','density of part',#97647);
#22040=AXIS2_PLACEMENT_3D('',#27640,#23502,#23503);
#22041=AXIS2_PLACEMENT_3D('',#27641,#23504,#23505);
#22042=AXIS2_PLACEMENT_3D('',#27642,#23506,#23507);
#22043=AXIS2_PLACEMENT_3D('',#27643,#23508,#23509);
#22044=AXIS2_PLACEMENT_3D('',#27645,#23510,#23511);
#22045=AXIS2_PLACEMENT_3D('',#27648,#23513,#23514);
#22046=AXIS2_PLACEMENT_3D('',#27649,#23515,#23516);
#22047=AXIS2_PLACEMENT_3D('',#27651,#23517,#23518);
#22048=AXIS2_PLACEMENT_3D('',#27654,#23520,#23521);
#22049=AXIS2_PLACEMENT_3D('',#27655,#23522,#23523);
#22050=AXIS2_PLACEMENT_3D('',#27657,#23524,#23525);
#22051=AXIS2_PLACEMENT_3D('',#27660,#23527,#23528);
#22052=AXIS2_PLACEMENT_3D('',#27661,#23529,#23530);
#22053=AXIS2_PLACEMENT_3D('',#27663,#23531,#23532);
#22054=AXIS2_PLACEMENT_3D('',#27666,#23534,#23535);
#22055=AXIS2_PLACEMENT_3D('',#27667,#23536,#23537);
#22056=AXIS2_PLACEMENT_3D('',#27669,#23538,#23539);
#22057=AXIS2_PLACEMENT_3D('',#27672,#23541,#23542);
#22058=AXIS2_PLACEMENT_3D('',#27673,#23543,#23544);
#22059=AXIS2_PLACEMENT_3D('',#27675,#23545,#23546);
#22060=AXIS2_PLACEMENT_3D('',#27678,#23548,#23549);
#22061=AXIS2_PLACEMENT_3D('',#27679,#23550,#23551);
#22062=AXIS2_PLACEMENT_3D('',#27688,#23556,#23557);
#22063=AXIS2_PLACEMENT_3D('',#27694,#23561,#23562);
#22064=AXIS2_PLACEMENT_3D('',#27700,#23566,#23567);
#22065=AXIS2_PLACEMENT_3D('',#27703,#23570,#23571);
#22066=AXIS2_PLACEMENT_3D('',#27712,#23576,#23577);
#22067=AXIS2_PLACEMENT_3D('',#27718,#23581,#23582);
#22068=AXIS2_PLACEMENT_3D('',#27724,#23586,#23587);
#22069=AXIS2_PLACEMENT_3D('',#27727,#23590,#23591);
#22070=AXIS2_PLACEMENT_3D('',#27728,#23592,#23593);
#22071=AXIS2_PLACEMENT_3D('',#27729,#23594,#23595);
#22072=AXIS2_PLACEMENT_3D('',#27730,#23596,#23597);
#22073=AXIS2_PLACEMENT_3D('',#27739,#23602,#23603);
#22074=AXIS2_PLACEMENT_3D('',#27745,#23607,#23608);
#22075=AXIS2_PLACEMENT_3D('',#27751,#23612,#23613);
#22076=AXIS2_PLACEMENT_3D('',#27754,#23616,#23617);
#22077=AXIS2_PLACEMENT_3D('',#27763,#23622,#23623);
#22078=AXIS2_PLACEMENT_3D('',#27769,#23627,#23628);
#22079=AXIS2_PLACEMENT_3D('',#27775,#23632,#23633);
#22080=AXIS2_PLACEMENT_3D('',#27778,#23636,#23637);
#22081=AXIS2_PLACEMENT_3D('',#27779,#23638,#23639);
#22082=AXIS2_PLACEMENT_3D('',#27780,#23640,#23641);
#22083=AXIS2_PLACEMENT_3D('',#27781,#23642,#23643);
#22084=AXIS2_PLACEMENT_3D('',#27791,#23645,#23646);
#22085=AXIS2_PLACEMENT_3D('',#27802,#23647,#23648);
#22086=AXIS2_PLACEMENT_3D('',#27853,#23650,#23651);
#22087=AXIS2_PLACEMENT_3D('',#27904,#23653,#23654);
#22088=AXIS2_PLACEMENT_3D('',#27952,#23656,#23657);
#22089=AXIS2_PLACEMENT_3D('',#28003,#23659,#23660);
#22090=AXIS2_PLACEMENT_3D('',#28054,#23662,#23663);
#22091=AXIS2_PLACEMENT_3D('',#28102,#23665,#23666);
#22092=AXIS2_PLACEMENT_3D('',#28121,#23668,#23669);
#22093=AXIS2_PLACEMENT_3D('',#28141,#23670,#23671);
#22094=AXIS2_PLACEMENT_3D('',#28151,#23673,#23674);
#22095=AXIS2_PLACEMENT_3D('',#28162,#23675,#23676);
#22096=AXIS2_PLACEMENT_3D('',#28213,#23678,#23679);
#22097=AXIS2_PLACEMENT_3D('',#28264,#23681,#23682);
#22098=AXIS2_PLACEMENT_3D('',#28312,#23684,#23685);
#22099=AXIS2_PLACEMENT_3D('',#28363,#23687,#23688);
#22100=AXIS2_PLACEMENT_3D('',#28414,#23690,#23691);
#22101=AXIS2_PLACEMENT_3D('',#28462,#23693,#23694);
#22102=AXIS2_PLACEMENT_3D('',#28481,#23696,#23697);
#22103=AXIS2_PLACEMENT_3D('',#28501,#23698,#23699);
#22104=AXIS2_PLACEMENT_3D('',#28511,#23701,#23702);
#22105=AXIS2_PLACEMENT_3D('',#28522,#23703,#23704);
#22106=AXIS2_PLACEMENT_3D('',#28573,#23706,#23707);
#22107=AXIS2_PLACEMENT_3D('',#28624,#23709,#23710);
#22108=AXIS2_PLACEMENT_3D('',#28672,#23712,#23713);
#22109=AXIS2_PLACEMENT_3D('',#28723,#23715,#23716);
#22110=AXIS2_PLACEMENT_3D('',#28774,#23718,#23719);
#22111=AXIS2_PLACEMENT_3D('',#28822,#23721,#23722);
#22112=AXIS2_PLACEMENT_3D('',#28841,#23724,#23725);
#22113=AXIS2_PLACEMENT_3D('',#28861,#23726,#23727);
#22114=AXIS2_PLACEMENT_3D('',#28871,#23729,#23730);
#22115=AXIS2_PLACEMENT_3D('',#28882,#23731,#23732);
#22116=AXIS2_PLACEMENT_3D('',#28933,#23734,#23735);
#22117=AXIS2_PLACEMENT_3D('',#28984,#23737,#23738);
#22118=AXIS2_PLACEMENT_3D('',#29032,#23740,#23741);
#22119=AXIS2_PLACEMENT_3D('',#29083,#23743,#23744);
#22120=AXIS2_PLACEMENT_3D('',#29134,#23746,#23747);
#22121=AXIS2_PLACEMENT_3D('',#29182,#23749,#23750);
#22122=AXIS2_PLACEMENT_3D('',#29201,#23752,#23753);
#22123=AXIS2_PLACEMENT_3D('',#29221,#23754,#23755);
#22124=AXIS2_PLACEMENT_3D('',#29235,#23757,#23758);
#22125=AXIS2_PLACEMENT_3D('',#29245,#23759,#23760);
#22126=AXIS2_PLACEMENT_3D('',#29269,#23762,#23763);
#22127=AXIS2_PLACEMENT_3D('',#29294,#23765,#23766);
#22128=AXIS2_PLACEMENT_3D('',#29319,#23768,#23769);
#22129=AXIS2_PLACEMENT_3D('',#29343,#23771,#23772);
#22130=AXIS2_PLACEMENT_3D('',#29368,#23774,#23775);
#22131=AXIS2_PLACEMENT_3D('',#29393,#23777,#23778);
#22132=AXIS2_PLACEMENT_3D('',#29404,#23780,#23781);
#22133=AXIS2_PLACEMENT_3D('',#29410,#23782,#23783);
#22134=AXIS2_PLACEMENT_3D('',#29424,#23785,#23786);
#22135=AXIS2_PLACEMENT_3D('',#29434,#23787,#23788);
#22136=AXIS2_PLACEMENT_3D('',#29458,#23790,#23791);
#22137=AXIS2_PLACEMENT_3D('',#29483,#23793,#23794);
#22138=AXIS2_PLACEMENT_3D('',#29508,#23796,#23797);
#22139=AXIS2_PLACEMENT_3D('',#29532,#23799,#23800);
#22140=AXIS2_PLACEMENT_3D('',#29557,#23802,#23803);
#22141=AXIS2_PLACEMENT_3D('',#29582,#23805,#23806);
#22142=AXIS2_PLACEMENT_3D('',#29593,#23808,#23809);
#22143=AXIS2_PLACEMENT_3D('',#29599,#23810,#23811);
#22144=AXIS2_PLACEMENT_3D('',#29613,#23813,#23814);
#22145=AXIS2_PLACEMENT_3D('',#29623,#23815,#23816);
#22146=AXIS2_PLACEMENT_3D('',#29647,#23818,#23819);
#22147=AXIS2_PLACEMENT_3D('',#29672,#23821,#23822);
#22148=AXIS2_PLACEMENT_3D('',#29697,#23824,#23825);
#22149=AXIS2_PLACEMENT_3D('',#29721,#23827,#23828);
#22150=AXIS2_PLACEMENT_3D('',#29746,#23830,#23831);
#22151=AXIS2_PLACEMENT_3D('',#29771,#23833,#23834);
#22152=AXIS2_PLACEMENT_3D('',#29782,#23836,#23837);
#22153=AXIS2_PLACEMENT_3D('',#29788,#23838,#23839);
#22154=AXIS2_PLACEMENT_3D('',#29802,#23841,#23842);
#22155=AXIS2_PLACEMENT_3D('',#29812,#23843,#23844);
#22156=AXIS2_PLACEMENT_3D('',#29836,#23846,#23847);
#22157=AXIS2_PLACEMENT_3D('',#29861,#23849,#23850);
#22158=AXIS2_PLACEMENT_3D('',#29886,#23852,#23853);
#22159=AXIS2_PLACEMENT_3D('',#29910,#23855,#23856);
#22160=AXIS2_PLACEMENT_3D('',#29935,#23858,#23859);
#22161=AXIS2_PLACEMENT_3D('',#29960,#23861,#23862);
#22162=AXIS2_PLACEMENT_3D('',#29971,#23864,#23865);
#22163=AXIS2_PLACEMENT_3D('',#29977,#23866,#23867);
#22164=AXIS2_PLACEMENT_3D('',#30879,#23868,#23869);
#22165=AXIS2_PLACEMENT_3D('',#31461,#23874,#23875);
#22166=AXIS2_PLACEMENT_3D('',#32172,#23876,#23877);
#22167=AXIS2_PLACEMENT_3D('',#32883,#23878,#23879);
#22168=AXIS2_PLACEMENT_3D('',#33594,#23880,#23881);
#22169=AXIS2_PLACEMENT_3D('',#33595,#23882,#23883);
#22170=AXIS2_PLACEMENT_3D('',#33596,#23884,#23885);
#22171=AXIS2_PLACEMENT_3D('',#33597,#23886,#23887);
#22172=AXIS2_PLACEMENT_3D('',#33598,#23888,#23889);
#22173=AXIS2_PLACEMENT_3D('',#33604,#23893,#23894);
#22174=AXIS2_PLACEMENT_3D('',#33608,#23897,#23898);
#22175=AXIS2_PLACEMENT_3D('',#33612,#23901,#23902);
#22176=AXIS2_PLACEMENT_3D('',#33614,#23904,#23905);
#22177=AXIS2_PLACEMENT_3D('',#33615,#23906,#23907);
#22178=AXIS2_PLACEMENT_3D('',#33616,#23908,#23909);
#22179=AXIS2_PLACEMENT_3D('',#33632,#23911,#23912);
#22180=AXIS2_PLACEMENT_3D('',#33640,#23913,#23914);
#22181=AXIS2_PLACEMENT_3D('',#33688,#23916,#23917);
#22182=AXIS2_PLACEMENT_3D('',#33736,#23919,#23920);
#22183=AXIS2_PLACEMENT_3D('',#33784,#23922,#23923);
#22184=AXIS2_PLACEMENT_3D('',#33838,#23925,#23926);
#22185=AXIS2_PLACEMENT_3D('',#33886,#23928,#23929);
#22186=AXIS2_PLACEMENT_3D('',#33934,#23931,#23932);
#22187=AXIS2_PLACEMENT_3D('',#33988,#23934,#23935);
#22188=AXIS2_PLACEMENT_3D('',#34036,#23937,#23938);
#22189=AXIS2_PLACEMENT_3D('',#34084,#23940,#23941);
#22190=AXIS2_PLACEMENT_3D('',#34138,#23943,#23944);
#22191=AXIS2_PLACEMENT_3D('',#34186,#23946,#23947);
#22192=AXIS2_PLACEMENT_3D('',#34234,#23949,#23950);
#22193=AXIS2_PLACEMENT_3D('',#34282,#23952,#23953);
#22194=AXIS2_PLACEMENT_3D('',#34336,#23955,#23956);
#22195=AXIS2_PLACEMENT_3D('',#34384,#23958,#23959);
#22196=AXIS2_PLACEMENT_3D('',#34432,#23961,#23962);
#22197=AXIS2_PLACEMENT_3D('',#34486,#23964,#23965);
#22198=AXIS2_PLACEMENT_3D('',#34534,#23967,#23968);
#22199=AXIS2_PLACEMENT_3D('',#34582,#23970,#23971);
#22200=AXIS2_PLACEMENT_3D('',#34630,#23973,#23974);
#22201=AXIS2_PLACEMENT_3D('',#34684,#23976,#23977);
#22202=AXIS2_PLACEMENT_3D('',#34732,#23979,#23980);
#22203=AXIS2_PLACEMENT_3D('',#34780,#23982,#23983);
#22204=AXIS2_PLACEMENT_3D('',#34796,#23985,#23986);
#22205=AXIS2_PLACEMENT_3D('',#34805,#23987,#23988);
#22206=AXIS2_PLACEMENT_3D('',#34830,#23990,#23991);
#22207=AXIS2_PLACEMENT_3D('',#34854,#23993,#23994);
#22208=AXIS2_PLACEMENT_3D('',#34879,#23996,#23997);
#22209=AXIS2_PLACEMENT_3D('',#34904,#23999,#24000);
#22210=AXIS2_PLACEMENT_3D('',#34928,#24002,#24003);
#22211=AXIS2_PLACEMENT_3D('',#34952,#24005,#24006);
#22212=AXIS2_PLACEMENT_3D('',#34977,#24008,#24009);
#22213=AXIS2_PLACEMENT_3D('',#35002,#24011,#24012);
#22214=AXIS2_PLACEMENT_3D('',#35026,#24014,#24015);
#22215=AXIS2_PLACEMENT_3D('',#35051,#24017,#24018);
#22216=AXIS2_PLACEMENT_3D('',#35076,#24020,#24021);
#22217=AXIS2_PLACEMENT_3D('',#35100,#24023,#24024);
#22218=AXIS2_PLACEMENT_3D('',#35124,#24026,#24027);
#22219=AXIS2_PLACEMENT_3D('',#35149,#24029,#24030);
#22220=AXIS2_PLACEMENT_3D('',#35174,#24032,#24033);
#22221=AXIS2_PLACEMENT_3D('',#35198,#24035,#24036);
#22222=AXIS2_PLACEMENT_3D('',#35223,#24038,#24039);
#22223=AXIS2_PLACEMENT_3D('',#35248,#24041,#24042);
#22224=AXIS2_PLACEMENT_3D('',#35272,#24044,#24045);
#22225=AXIS2_PLACEMENT_3D('',#35297,#24047,#24048);
#22226=AXIS2_PLACEMENT_3D('',#35322,#24050,#24051);
#22227=AXIS2_PLACEMENT_3D('',#35346,#24053,#24054);
#22228=AXIS2_PLACEMENT_3D('',#35370,#24056,#24057);
#22229=AXIS2_PLACEMENT_3D('',#35673,#24058,#24059);
#22230=AXIS2_PLACEMENT_3D('',#35707,#24061,#24062);
#22231=AXIS2_PLACEMENT_3D('',#36465,#24063,#24064);
#22232=AXIS2_PLACEMENT_3D('',#36476,#24065,#24066);
#22233=AXIS2_PLACEMENT_3D('',#37236,#24067,#24068);
#22234=AXIS2_PLACEMENT_3D('',#37237,#24069,#24070);
#22235=AXIS2_PLACEMENT_3D('',#37246,#24075,#24076);
#22236=AXIS2_PLACEMENT_3D('',#37252,#24080,#24081);
#22237=AXIS2_PLACEMENT_3D('',#37258,#24085,#24086);
#22238=AXIS2_PLACEMENT_3D('',#37264,#24090,#24091);
#22239=AXIS2_PLACEMENT_3D('',#37270,#24095,#24096);
#22240=AXIS2_PLACEMENT_3D('',#37273,#24099,#24100);
#22241=AXIS2_PLACEMENT_3D('',#37274,#24101,#24102);
#22242=AXIS2_PLACEMENT_3D('',#37276,#24103,#24104);
#22243=AXIS2_PLACEMENT_3D('',#37277,#24105,#24106);
#22244=AXIS2_PLACEMENT_3D('',#37280,#24108,#24109);
#22245=AXIS2_PLACEMENT_3D('',#37281,#24110,#24111);
#22246=AXIS2_PLACEMENT_3D('',#37282,#24112,#24113);
#22247=AXIS2_PLACEMENT_3D('',#37283,#24114,#24115);
#22248=AXIS2_PLACEMENT_3D('',#37284,#24116,#24117);
#22249=AXIS2_PLACEMENT_3D('',#37286,#24118,#24119);
#22250=AXIS2_PLACEMENT_3D('',#37289,#24121,#24122);
#22251=AXIS2_PLACEMENT_3D('',#37290,#24123,#24124);
#22252=AXIS2_PLACEMENT_3D('',#37292,#24125,#24126);
#22253=AXIS2_PLACEMENT_3D('',#37295,#24128,#24129);
#22254=AXIS2_PLACEMENT_3D('',#37296,#24130,#24131);
#22255=AXIS2_PLACEMENT_3D('',#37297,#24132,#24133);
#22256=AXIS2_PLACEMENT_3D('',#37298,#24134,#24135);
#22257=AXIS2_PLACEMENT_3D('',#37299,#24136,#24137);
#22258=AXIS2_PLACEMENT_3D('',#37300,#24138,#24139);
#22259=AXIS2_PLACEMENT_3D('',#37301,#24140,#24141);
#22260=AXIS2_PLACEMENT_3D('',#37302,#24142,#24143);
#22261=AXIS2_PLACEMENT_3D('',#37303,#24144,#24145);
#22262=AXIS2_PLACEMENT_3D('',#37304,#24146,#24147);
#22263=AXIS2_PLACEMENT_3D('',#37305,#24148,#24149);
#22264=AXIS2_PLACEMENT_3D('',#37306,#24150,#24151);
#22265=AXIS2_PLACEMENT_3D('',#37307,#24152,#24153);
#22266=AXIS2_PLACEMENT_3D('',#37308,#24154,#24155);
#22267=AXIS2_PLACEMENT_3D('',#37309,#24156,#24157);
#22268=AXIS2_PLACEMENT_3D('',#37310,#24158,#24159);
#22269=AXIS2_PLACEMENT_3D('',#37311,#24160,#24161);
#22270=AXIS2_PLACEMENT_3D('',#37312,#24162,#24163);
#22271=AXIS2_PLACEMENT_3D('',#37313,#24164,#24165);
#22272=AXIS2_PLACEMENT_3D('',#37314,#24166,#24167);
#22273=AXIS2_PLACEMENT_3D('',#37315,#24168,#24169);
#22274=AXIS2_PLACEMENT_3D('',#37316,#24170,#24171);
#22275=AXIS2_PLACEMENT_3D('',#37317,#24172,#24173);
#22276=AXIS2_PLACEMENT_3D('',#37318,#24174,#24175);
#22277=AXIS2_PLACEMENT_3D('',#37319,#24176,#24177);
#22278=AXIS2_PLACEMENT_3D('',#37320,#24178,#24179);
#22279=AXIS2_PLACEMENT_3D('',#37321,#24180,#24181);
#22280=AXIS2_PLACEMENT_3D('',#37322,#24182,#24183);
#22281=AXIS2_PLACEMENT_3D('',#37323,#24184,#24185);
#22282=AXIS2_PLACEMENT_3D('',#37324,#24186,#24187);
#22283=AXIS2_PLACEMENT_3D('',#37325,#24188,#24189);
#22284=AXIS2_PLACEMENT_3D('',#37326,#24190,#24191);
#22285=AXIS2_PLACEMENT_3D('',#37327,#24192,#24193);
#22286=AXIS2_PLACEMENT_3D('',#37328,#24194,#24195);
#22287=AXIS2_PLACEMENT_3D('',#37329,#24196,#24197);
#22288=AXIS2_PLACEMENT_3D('',#37330,#24198,#24199);
#22289=AXIS2_PLACEMENT_3D('',#37331,#24200,#24201);
#22290=AXIS2_PLACEMENT_3D('',#37332,#24202,#24203);
#22291=AXIS2_PLACEMENT_3D('',#37333,#24204,#24205);
#22292=AXIS2_PLACEMENT_3D('',#37334,#24206,#24207);
#22293=AXIS2_PLACEMENT_3D('',#37335,#24208,#24209);
#22294=AXIS2_PLACEMENT_3D('',#37336,#24210,#24211);
#22295=AXIS2_PLACEMENT_3D('',#37337,#24212,#24213);
#22296=AXIS2_PLACEMENT_3D('',#37338,#24214,#24215);
#22297=AXIS2_PLACEMENT_3D('',#37339,#24216,#24217);
#22298=AXIS2_PLACEMENT_3D('',#37340,#24218,#24219);
#22299=AXIS2_PLACEMENT_3D('',#37353,#24221,#24222);
#22300=AXIS2_PLACEMENT_3D('',#37356,#24224,#24225);
#22301=AXIS2_PLACEMENT_3D('',#37358,#24226,#24227);
#22302=AXIS2_PLACEMENT_3D('',#37375,#24228,#24229);
#22303=AXIS2_PLACEMENT_3D('',#37465,#24231,#24232);
#22304=AXIS2_PLACEMENT_3D('',#37552,#24234,#24235);
#22305=AXIS2_PLACEMENT_3D('',#37639,#24237,#24238);
#22306=AXIS2_PLACEMENT_3D('',#37726,#24240,#24241);
#22307=AXIS2_PLACEMENT_3D('',#37816,#24243,#24244);
#22308=AXIS2_PLACEMENT_3D('',#37903,#24246,#24247);
#22309=AXIS2_PLACEMENT_3D('',#37990,#24249,#24250);
#22310=AXIS2_PLACEMENT_3D('',#38080,#24252,#24253);
#22311=AXIS2_PLACEMENT_3D('',#38167,#24255,#24256);
#22312=AXIS2_PLACEMENT_3D('',#38254,#24258,#24259);
#22313=AXIS2_PLACEMENT_3D('',#38341,#24261,#24262);
#22314=AXIS2_PLACEMENT_3D('',#38431,#24264,#24265);
#22315=AXIS2_PLACEMENT_3D('',#38518,#24267,#24268);
#22316=AXIS2_PLACEMENT_3D('',#38605,#24270,#24271);
#22317=AXIS2_PLACEMENT_3D('',#38692,#24273,#24274);
#22318=AXIS2_PLACEMENT_3D('',#38782,#24276,#24277);
#22319=AXIS2_PLACEMENT_3D('',#38869,#24279,#24280);
#22320=AXIS2_PLACEMENT_3D('',#38956,#24282,#24283);
#22321=AXIS2_PLACEMENT_3D('',#39046,#24285,#24286);
#22322=AXIS2_PLACEMENT_3D('',#39133,#24288,#24289);
#22323=AXIS2_PLACEMENT_3D('',#39220,#24291,#24292);
#22324=AXIS2_PLACEMENT_3D('',#39307,#24294,#24295);
#22325=AXIS2_PLACEMENT_3D('',#39397,#24297,#24298);
#22326=AXIS2_PLACEMENT_3D('',#39428,#24300,#24301);
#22327=AXIS2_PLACEMENT_3D('',#39466,#24302,#24303);
#22328=AXIS2_PLACEMENT_3D('',#39484,#24305,#24306);
#22329=AXIS2_PLACEMENT_3D('',#39499,#24307,#24308);
#22330=AXIS2_PLACEMENT_3D('',#39536,#24310,#24311);
#22331=AXIS2_PLACEMENT_3D('',#39574,#24313,#24314);
#22332=AXIS2_PLACEMENT_3D('',#39610,#24316,#24317);
#22333=AXIS2_PLACEMENT_3D('',#39648,#24319,#24320);
#22334=AXIS2_PLACEMENT_3D('',#39686,#24322,#24323);
#22335=AXIS2_PLACEMENT_3D('',#39722,#24325,#24326);
#22336=AXIS2_PLACEMENT_3D('',#39760,#24328,#24329);
#22337=AXIS2_PLACEMENT_3D('',#39798,#24331,#24332);
#22338=AXIS2_PLACEMENT_3D('',#39834,#24334,#24335);
#22339=AXIS2_PLACEMENT_3D('',#39872,#24337,#24338);
#22340=AXIS2_PLACEMENT_3D('',#39909,#24340,#24341);
#22341=AXIS2_PLACEMENT_3D('',#39946,#24343,#24344);
#22342=AXIS2_PLACEMENT_3D('',#39984,#24346,#24347);
#22343=AXIS2_PLACEMENT_3D('',#40020,#24349,#24350);
#22344=AXIS2_PLACEMENT_3D('',#40058,#24352,#24353);
#22345=AXIS2_PLACEMENT_3D('',#40096,#24355,#24356);
#22346=AXIS2_PLACEMENT_3D('',#40132,#24358,#24359);
#22347=AXIS2_PLACEMENT_3D('',#40170,#24361,#24362);
#22348=AXIS2_PLACEMENT_3D('',#40208,#24364,#24365);
#22349=AXIS2_PLACEMENT_3D('',#40244,#24367,#24368);
#22350=AXIS2_PLACEMENT_3D('',#40282,#24370,#24371);
#22351=AXIS2_PLACEMENT_3D('',#40319,#24373,#24374);
#22352=AXIS2_PLACEMENT_3D('',#40356,#24376,#24377);
#22353=AXIS2_PLACEMENT_3D('',#40368,#24379,#24380);
#22354=AXIS2_PLACEMENT_3D('',#40376,#24381,#24382);
#22355=AXIS2_PLACEMENT_3D('',#40389,#24384,#24385);
#22356=AXIS2_PLACEMENT_3D('',#40392,#24387,#24388);
#22357=AXIS2_PLACEMENT_3D('',#40394,#24389,#24390);
#22358=AXIS2_PLACEMENT_3D('',#40411,#24391,#24392);
#22359=AXIS2_PLACEMENT_3D('',#40501,#24394,#24395);
#22360=AXIS2_PLACEMENT_3D('',#40588,#24397,#24398);
#22361=AXIS2_PLACEMENT_3D('',#40675,#24400,#24401);
#22362=AXIS2_PLACEMENT_3D('',#40762,#24403,#24404);
#22363=AXIS2_PLACEMENT_3D('',#40849,#24406,#24407);
#22364=AXIS2_PLACEMENT_3D('',#40939,#24409,#24410);
#22365=AXIS2_PLACEMENT_3D('',#41026,#24412,#24413);
#22366=AXIS2_PLACEMENT_3D('',#41113,#24415,#24416);
#22367=AXIS2_PLACEMENT_3D('',#41200,#24418,#24419);
#22368=AXIS2_PLACEMENT_3D('',#41287,#24421,#24422);
#22369=AXIS2_PLACEMENT_3D('',#41377,#24424,#24425);
#22370=AXIS2_PLACEMENT_3D('',#41464,#24427,#24428);
#22371=AXIS2_PLACEMENT_3D('',#41551,#24430,#24431);
#22372=AXIS2_PLACEMENT_3D('',#41638,#24433,#24434);
#22373=AXIS2_PLACEMENT_3D('',#41725,#24436,#24437);
#22374=AXIS2_PLACEMENT_3D('',#41812,#24439,#24440);
#22375=AXIS2_PLACEMENT_3D('',#41899,#24442,#24443);
#22376=AXIS2_PLACEMENT_3D('',#41986,#24445,#24446);
#22377=AXIS2_PLACEMENT_3D('',#42061,#24448,#24449);
#22378=AXIS2_PLACEMENT_3D('',#42109,#24451,#24452);
#22379=AXIS2_PLACEMENT_3D('',#42166,#24454,#24455);
#22380=AXIS2_PLACEMENT_3D('',#42253,#24457,#24458);
#22381=AXIS2_PLACEMENT_3D('',#42340,#24460,#24461);
#22382=AXIS2_PLACEMENT_3D('',#42427,#24463,#24464);
#22383=AXIS2_PLACEMENT_3D('',#42514,#24466,#24467);
#22384=AXIS2_PLACEMENT_3D('',#42601,#24469,#24470);
#22385=AXIS2_PLACEMENT_3D('',#42691,#24472,#24473);
#22386=AXIS2_PLACEMENT_3D('',#42778,#24475,#24476);
#22387=AXIS2_PLACEMENT_3D('',#42865,#24478,#24479);
#22388=AXIS2_PLACEMENT_3D('',#42952,#24481,#24482);
#22389=AXIS2_PLACEMENT_3D('',#43039,#24484,#24485);
#22390=AXIS2_PLACEMENT_3D('',#43129,#24487,#24488);
#22391=AXIS2_PLACEMENT_3D('',#43216,#24490,#24491);
#22392=AXIS2_PLACEMENT_3D('',#43303,#24493,#24494);
#22393=AXIS2_PLACEMENT_3D('',#43390,#24496,#24497);
#22394=AXIS2_PLACEMENT_3D('',#43477,#24499,#24500);
#22395=AXIS2_PLACEMENT_3D('',#43567,#24502,#24503);
#22396=AXIS2_PLACEMENT_3D('',#43654,#24505,#24506);
#22397=AXIS2_PLACEMENT_3D('',#43685,#24508,#24509);
#22398=AXIS2_PLACEMENT_3D('',#43723,#24510,#24511);
#22399=AXIS2_PLACEMENT_3D('',#43741,#24513,#24514);
#22400=AXIS2_PLACEMENT_3D('',#43756,#24515,#24516);
#22401=AXIS2_PLACEMENT_3D('',#43793,#24518,#24519);
#22402=AXIS2_PLACEMENT_3D('',#43831,#24521,#24522);
#22403=AXIS2_PLACEMENT_3D('',#43867,#24524,#24525);
#22404=AXIS2_PLACEMENT_3D('',#43905,#24527,#24528);
#22405=AXIS2_PLACEMENT_3D('',#43942,#24530,#24531);
#22406=AXIS2_PLACEMENT_3D('',#43979,#24533,#24534);
#22407=AXIS2_PLACEMENT_3D('',#44017,#24536,#24537);
#22408=AXIS2_PLACEMENT_3D('',#44053,#24539,#24540);
#22409=AXIS2_PLACEMENT_3D('',#44091,#24542,#24543);
#22410=AXIS2_PLACEMENT_3D('',#44128,#24545,#24546);
#22411=AXIS2_PLACEMENT_3D('',#44165,#24548,#24549);
#22412=AXIS2_PLACEMENT_3D('',#44203,#24551,#24552);
#22413=AXIS2_PLACEMENT_3D('',#44239,#24554,#24555);
#22414=AXIS2_PLACEMENT_3D('',#44277,#24557,#24558);
#22415=AXIS2_PLACEMENT_3D('',#44314,#24560,#24561);
#22416=AXIS2_PLACEMENT_3D('',#44351,#24563,#24564);
#22417=AXIS2_PLACEMENT_3D('',#44389,#24566,#24567);
#22418=AXIS2_PLACEMENT_3D('',#44425,#24569,#24570);
#22419=AXIS2_PLACEMENT_3D('',#44452,#24572,#24573);
#22420=AXIS2_PLACEMENT_3D('',#44476,#24575,#24576);
#22421=AXIS2_PLACEMENT_3D('',#44509,#24578,#24579);
#22422=AXIS2_PLACEMENT_3D('',#44547,#24581,#24582);
#22423=AXIS2_PLACEMENT_3D('',#44583,#24584,#24585);
#22424=AXIS2_PLACEMENT_3D('',#44621,#24587,#24588);
#22425=AXIS2_PLACEMENT_3D('',#44657,#24590,#24591);
#22426=AXIS2_PLACEMENT_3D('',#44695,#24593,#24594);
#22427=AXIS2_PLACEMENT_3D('',#44733,#24596,#24597);
#22428=AXIS2_PLACEMENT_3D('',#44769,#24599,#24600);
#22429=AXIS2_PLACEMENT_3D('',#44807,#24602,#24603);
#22430=AXIS2_PLACEMENT_3D('',#44843,#24605,#24606);
#22431=AXIS2_PLACEMENT_3D('',#44881,#24608,#24609);
#22432=AXIS2_PLACEMENT_3D('',#44919,#24611,#24612);
#22433=AXIS2_PLACEMENT_3D('',#44955,#24614,#24615);
#22434=AXIS2_PLACEMENT_3D('',#44993,#24617,#24618);
#22435=AXIS2_PLACEMENT_3D('',#45029,#24620,#24621);
#22436=AXIS2_PLACEMENT_3D('',#45067,#24623,#24624);
#22437=AXIS2_PLACEMENT_3D('',#45105,#24626,#24627);
#22438=AXIS2_PLACEMENT_3D('',#45141,#24629,#24630);
#22439=AXIS2_PLACEMENT_3D('',#45153,#24632,#24633);
#22440=AXIS2_PLACEMENT_3D('',#45161,#24634,#24635);
#22441=AXIS2_PLACEMENT_3D('',#45371,#24636,#24637);
#22442=AXIS2_PLACEMENT_3D('',#49677,#24638,#24639);
#22443=AXIS2_PLACEMENT_3D('',#49678,#24640,#24641);
#22444=AXIS2_PLACEMENT_3D('',#49680,#24642,#24643);
#22445=AXIS2_PLACEMENT_3D('',#49681,#24644,#24645);
#22446=AXIS2_PLACEMENT_3D('',#49888,#24646,#24647);
#22447=AXIS2_PLACEMENT_3D('',#52802,#24648,#24649);
#22448=AXIS2_PLACEMENT_3D('',#52803,#24650,#24651);
#22449=AXIS2_PLACEMENT_3D('',#52805,#24652,#24653);
#22450=AXIS2_PLACEMENT_3D('',#52806,#24654,#24655);
#22451=AXIS2_PLACEMENT_3D('',#52809,#24656,#24657);
#22452=AXIS2_PLACEMENT_3D('',#52813,#24659,#24660);
#22453=AXIS2_PLACEMENT_3D('',#52815,#24662,#24663);
#22454=AXIS2_PLACEMENT_3D('',#52821,#24667,#24668);
#22455=AXIS2_PLACEMENT_3D('',#52825,#24670,#24671);
#22456=AXIS2_PLACEMENT_3D('',#52829,#24673,#24674);
#22457=AXIS2_PLACEMENT_3D('',#52833,#24676,#24677);
#22458=AXIS2_PLACEMENT_3D('',#52837,#24679,#24680);
#22459=AXIS2_PLACEMENT_3D('',#52841,#24682,#24683);
#22460=AXIS2_PLACEMENT_3D('',#52845,#24685,#24686);
#22461=AXIS2_PLACEMENT_3D('',#52849,#24688,#24689);
#22462=AXIS2_PLACEMENT_3D('',#52853,#24691,#24692);
#22463=AXIS2_PLACEMENT_3D('',#52857,#24694,#24695);
#22464=AXIS2_PLACEMENT_3D('',#52861,#24697,#24698);
#22465=AXIS2_PLACEMENT_3D('',#52865,#24700,#24701);
#22466=AXIS2_PLACEMENT_3D('',#52869,#24703,#24704);
#22467=AXIS2_PLACEMENT_3D('',#52873,#24706,#24707);
#22468=AXIS2_PLACEMENT_3D('',#52877,#24709,#24710);
#22469=AXIS2_PLACEMENT_3D('',#52881,#24712,#24713);
#22470=AXIS2_PLACEMENT_3D('',#52885,#24715,#24716);
#22471=AXIS2_PLACEMENT_3D('',#52889,#24718,#24719);
#22472=AXIS2_PLACEMENT_3D('',#52893,#24721,#24722);
#22473=AXIS2_PLACEMENT_3D('',#52897,#24724,#24725);
#22474=AXIS2_PLACEMENT_3D('',#52901,#24727,#24728);
#22475=AXIS2_PLACEMENT_3D('',#52905,#24730,#24731);
#22476=AXIS2_PLACEMENT_3D('',#52909,#24733,#24734);
#22477=AXIS2_PLACEMENT_3D('',#52913,#24736,#24737);
#22478=AXIS2_PLACEMENT_3D('',#52917,#24739,#24740);
#22479=AXIS2_PLACEMENT_3D('',#52921,#24742,#24743);
#22480=AXIS2_PLACEMENT_3D('',#52925,#24745,#24746);
#22481=AXIS2_PLACEMENT_3D('',#52929,#24748,#24749);
#22482=AXIS2_PLACEMENT_3D('',#52933,#24751,#24752);
#22483=AXIS2_PLACEMENT_3D('',#52937,#24754,#24755);
#22484=AXIS2_PLACEMENT_3D('',#52941,#24757,#24758);
#22485=AXIS2_PLACEMENT_3D('',#52945,#24760,#24761);
#22486=AXIS2_PLACEMENT_3D('',#52949,#24763,#24764);
#22487=AXIS2_PLACEMENT_3D('',#52953,#24766,#24767);
#22488=AXIS2_PLACEMENT_3D('',#52957,#24769,#24770);
#22489=AXIS2_PLACEMENT_3D('',#52960,#24772,#24773);
#22490=AXIS2_PLACEMENT_3D('',#52962,#24774,#24775);
#22491=AXIS2_PLACEMENT_3D('',#52964,#24776,#24777);
#22492=AXIS2_PLACEMENT_3D('',#52966,#24778,#24779);
#22493=AXIS2_PLACEMENT_3D('',#52968,#24780,#24781);
#22494=AXIS2_PLACEMENT_3D('',#52969,#24782,#24783);
#22495=AXIS2_PLACEMENT_3D('',#52972,#24784,#24785);
#22496=AXIS2_PLACEMENT_3D('',#52975,#24788,#24789);
#22497=AXIS2_PLACEMENT_3D('',#52979,#24792,#24793);
#22498=AXIS2_PLACEMENT_3D('',#52981,#24794,#24795);
#22499=AXIS2_PLACEMENT_3D('',#52983,#24797,#24798);
#22500=AXIS2_PLACEMENT_3D('',#52987,#24801,#24802);
#22501=AXIS2_PLACEMENT_3D('',#52989,#24803,#24804);
#22502=AXIS2_PLACEMENT_3D('',#52991,#24806,#24807);
#22503=AXIS2_PLACEMENT_3D('',#52995,#24810,#24811);
#22504=AXIS2_PLACEMENT_3D('',#52997,#24812,#24813);
#22505=AXIS2_PLACEMENT_3D('',#52999,#24815,#24816);
#22506=AXIS2_PLACEMENT_3D('',#53003,#24819,#24820);
#22507=AXIS2_PLACEMENT_3D('',#53005,#24821,#24822);
#22508=AXIS2_PLACEMENT_3D('',#53007,#24824,#24825);
#22509=AXIS2_PLACEMENT_3D('',#53011,#24827,#24828);
#22510=AXIS2_PLACEMENT_3D('',#53013,#24830,#24831);
#22511=AXIS2_PLACEMENT_3D('',#53017,#24834,#24835);
#22512=AXIS2_PLACEMENT_3D('',#53019,#24836,#24837);
#22513=AXIS2_PLACEMENT_3D('',#53021,#24839,#24840);
#22514=AXIS2_PLACEMENT_3D('',#53025,#24842,#24843);
#22515=AXIS2_PLACEMENT_3D('',#53027,#24845,#24846);
#22516=AXIS2_PLACEMENT_3D('',#53031,#24849,#24850);
#22517=AXIS2_PLACEMENT_3D('',#53033,#24851,#24852);
#22518=AXIS2_PLACEMENT_3D('',#53035,#24854,#24855);
#22519=AXIS2_PLACEMENT_3D('',#53038,#24856,#24857);
#22520=AXIS2_PLACEMENT_3D('',#53041,#24860,#24861);
#22521=AXIS2_PLACEMENT_3D('',#53045,#24864,#24865);
#22522=AXIS2_PLACEMENT_3D('',#53047,#24866,#24867);
#22523=AXIS2_PLACEMENT_3D('',#53049,#24869,#24870);
#22524=AXIS2_PLACEMENT_3D('',#53053,#24873,#24874);
#22525=AXIS2_PLACEMENT_3D('',#53055,#24875,#24876);
#22526=AXIS2_PLACEMENT_3D('',#53057,#24878,#24879);
#22527=AXIS2_PLACEMENT_3D('',#53061,#24882,#24883);
#22528=AXIS2_PLACEMENT_3D('',#53063,#24884,#24885);
#22529=AXIS2_PLACEMENT_3D('',#53065,#24887,#24888);
#22530=AXIS2_PLACEMENT_3D('',#53069,#24891,#24892);
#22531=AXIS2_PLACEMENT_3D('',#53071,#24893,#24894);
#22532=AXIS2_PLACEMENT_3D('',#53073,#24896,#24897);
#22533=AXIS2_PLACEMENT_3D('',#53077,#24899,#24900);
#22534=AXIS2_PLACEMENT_3D('',#53079,#24902,#24903);
#22535=AXIS2_PLACEMENT_3D('',#53083,#24906,#24907);
#22536=AXIS2_PLACEMENT_3D('',#53085,#24908,#24909);
#22537=AXIS2_PLACEMENT_3D('',#53087,#24911,#24912);
#22538=AXIS2_PLACEMENT_3D('',#53091,#24914,#24915);
#22539=AXIS2_PLACEMENT_3D('',#53093,#24917,#24918);
#22540=AXIS2_PLACEMENT_3D('',#53097,#24921,#24922);
#22541=AXIS2_PLACEMENT_3D('',#53099,#24923,#24924);
#22542=AXIS2_PLACEMENT_3D('',#53101,#24926,#24927);
#22543=AXIS2_PLACEMENT_3D('',#53104,#24928,#24929);
#22544=AXIS2_PLACEMENT_3D('',#53107,#24932,#24933);
#22545=AXIS2_PLACEMENT_3D('',#53111,#24936,#24937);
#22546=AXIS2_PLACEMENT_3D('',#53113,#24938,#24939);
#22547=AXIS2_PLACEMENT_3D('',#53115,#24941,#24942);
#22548=AXIS2_PLACEMENT_3D('',#53119,#24945,#24946);
#22549=AXIS2_PLACEMENT_3D('',#53121,#24947,#24948);
#22550=AXIS2_PLACEMENT_3D('',#53123,#24950,#24951);
#22551=AXIS2_PLACEMENT_3D('',#53127,#24954,#24955);
#22552=AXIS2_PLACEMENT_3D('',#53129,#24956,#24957);
#22553=AXIS2_PLACEMENT_3D('',#53131,#24959,#24960);
#22554=AXIS2_PLACEMENT_3D('',#53135,#24963,#24964);
#22555=AXIS2_PLACEMENT_3D('',#53137,#24965,#24966);
#22556=AXIS2_PLACEMENT_3D('',#53139,#24968,#24969);
#22557=AXIS2_PLACEMENT_3D('',#53143,#24971,#24972);
#22558=AXIS2_PLACEMENT_3D('',#53145,#24974,#24975);
#22559=AXIS2_PLACEMENT_3D('',#53149,#24978,#24979);
#22560=AXIS2_PLACEMENT_3D('',#53151,#24980,#24981);
#22561=AXIS2_PLACEMENT_3D('',#53153,#24983,#24984);
#22562=AXIS2_PLACEMENT_3D('',#53157,#24986,#24987);
#22563=AXIS2_PLACEMENT_3D('',#53159,#24989,#24990);
#22564=AXIS2_PLACEMENT_3D('',#53163,#24993,#24994);
#22565=AXIS2_PLACEMENT_3D('',#53165,#24995,#24996);
#22566=AXIS2_PLACEMENT_3D('',#53167,#24998,#24999);
#22567=AXIS2_PLACEMENT_3D('',#53170,#25000,#25001);
#22568=AXIS2_PLACEMENT_3D('',#53173,#25004,#25005);
#22569=AXIS2_PLACEMENT_3D('',#53177,#25008,#25009);
#22570=AXIS2_PLACEMENT_3D('',#53179,#25010,#25011);
#22571=AXIS2_PLACEMENT_3D('',#53181,#25013,#25014);
#22572=AXIS2_PLACEMENT_3D('',#53185,#25017,#25018);
#22573=AXIS2_PLACEMENT_3D('',#53187,#25019,#25020);
#22574=AXIS2_PLACEMENT_3D('',#53189,#25022,#25023);
#22575=AXIS2_PLACEMENT_3D('',#53193,#25026,#25027);
#22576=AXIS2_PLACEMENT_3D('',#53195,#25028,#25029);
#22577=AXIS2_PLACEMENT_3D('',#53197,#25031,#25032);
#22578=AXIS2_PLACEMENT_3D('',#53201,#25035,#25036);
#22579=AXIS2_PLACEMENT_3D('',#53203,#25037,#25038);
#22580=AXIS2_PLACEMENT_3D('',#53205,#25040,#25041);
#22581=AXIS2_PLACEMENT_3D('',#53209,#25043,#25044);
#22582=AXIS2_PLACEMENT_3D('',#53211,#25046,#25047);
#22583=AXIS2_PLACEMENT_3D('',#53215,#25050,#25051);
#22584=AXIS2_PLACEMENT_3D('',#53217,#25052,#25053);
#22585=AXIS2_PLACEMENT_3D('',#53219,#25055,#25056);
#22586=AXIS2_PLACEMENT_3D('',#53222,#25058,#25059);
#22587=AXIS2_PLACEMENT_3D('',#53223,#25060,#25061);
#22588=AXIS2_PLACEMENT_3D('',#53226,#25063,#25064);
#22589=AXIS2_PLACEMENT_3D('',#53227,#25065,#25066);
#22590=AXIS2_PLACEMENT_3D('',#53230,#25068,#25069);
#22591=AXIS2_PLACEMENT_3D('',#53231,#25070,#25071);
#22592=AXIS2_PLACEMENT_3D('',#53233,#25073,#25074);
#22593=AXIS2_PLACEMENT_3D('',#53236,#25076,#25077);
#22594=AXIS2_PLACEMENT_3D('',#53237,#25078,#25079);
#22595=AXIS2_PLACEMENT_3D('',#53240,#25081,#25082);
#22596=AXIS2_PLACEMENT_3D('',#53241,#25083,#25084);
#22597=AXIS2_PLACEMENT_3D('',#53243,#25086,#25087);
#22598=AXIS2_PLACEMENT_3D('',#53245,#25089,#25090);
#22599=AXIS2_PLACEMENT_3D('',#53247,#25092,#25093);
#22600=AXIS2_PLACEMENT_3D('',#53249,#25095,#25096);
#22601=AXIS2_PLACEMENT_3D('',#53251,#25098,#25099);
#22602=AXIS2_PLACEMENT_3D('',#53253,#25101,#25102);
#22603=AXIS2_PLACEMENT_3D('',#53255,#25104,#25105);
#22604=AXIS2_PLACEMENT_3D('',#53257,#25107,#25108);
#22605=AXIS2_PLACEMENT_3D('',#53259,#25110,#25111);
#22606=AXIS2_PLACEMENT_3D('',#53261,#25113,#25114);
#22607=AXIS2_PLACEMENT_3D('',#53263,#25116,#25117);
#22608=AXIS2_PLACEMENT_3D('',#53265,#25119,#25120);
#22609=AXIS2_PLACEMENT_3D('',#53266,#25121,#25122);
#22610=AXIS2_PLACEMENT_3D('',#53267,#25123,#25124);
#22611=AXIS2_PLACEMENT_3D('',#53269,#25125,#25126);
#22612=AXIS2_PLACEMENT_3D('',#53271,#25127,#25128);
#22613=AXIS2_PLACEMENT_3D('',#53272,#25129,#25130);
#22614=AXIS2_PLACEMENT_3D('',#53274,#25131,#25132);
#22615=AXIS2_PLACEMENT_3D('',#53276,#25134,#25135);
#22616=AXIS2_PLACEMENT_3D('',#53279,#25137,#25138);
#22617=AXIS2_PLACEMENT_3D('',#53280,#25139,#25140);
#22618=AXIS2_PLACEMENT_3D('',#53282,#25141,#25142);
#22619=AXIS2_PLACEMENT_3D('',#53285,#25144,#25145);
#22620=AXIS2_PLACEMENT_3D('',#53286,#25146,#25147);
#22621=AXIS2_PLACEMENT_3D('',#53288,#25148,#25149);
#22622=AXIS2_PLACEMENT_3D('',#53291,#25151,#25152);
#22623=AXIS2_PLACEMENT_3D('',#53292,#25153,#25154);
#22624=AXIS2_PLACEMENT_3D('',#53294,#25155,#25156);
#22625=AXIS2_PLACEMENT_3D('',#53297,#25158,#25159);
#22626=AXIS2_PLACEMENT_3D('',#53298,#25160,#25161);
#22627=AXIS2_PLACEMENT_3D('',#53300,#25162,#25163);
#22628=AXIS2_PLACEMENT_3D('',#53303,#25165,#25166);
#22629=AXIS2_PLACEMENT_3D('',#53304,#25167,#25168);
#22630=AXIS2_PLACEMENT_3D('',#53313,#25173,#25174);
#22631=AXIS2_PLACEMENT_3D('',#53319,#25178,#25179);
#22632=AXIS2_PLACEMENT_3D('',#53325,#25183,#25184);
#22633=AXIS2_PLACEMENT_3D('',#53328,#25187,#25188);
#22634=AXIS2_PLACEMENT_3D('',#53329,#25189,#25190);
#22635=AXIS2_PLACEMENT_3D('',#53330,#25191,#25192);
#22636=AXIS2_PLACEMENT_3D('',#53331,#25193,#25194);
#22637=AXIS2_PLACEMENT_3D('',#53347,#25196,#25197);
#22638=AXIS2_PLACEMENT_3D('',#53358,#25198,#25199);
#22639=AXIS2_PLACEMENT_3D('',#53406,#25201,#25202);
#22640=AXIS2_PLACEMENT_3D('',#53454,#25204,#25205);
#22641=AXIS2_PLACEMENT_3D('',#53508,#25207,#25208);
#22642=AXIS2_PLACEMENT_3D('',#53556,#25210,#25211);
#22643=AXIS2_PLACEMENT_3D('',#53604,#25213,#25214);
#22644=AXIS2_PLACEMENT_3D('',#53658,#25216,#25217);
#22645=AXIS2_PLACEMENT_3D('',#53706,#25219,#25220);
#22646=AXIS2_PLACEMENT_3D('',#53754,#25222,#25223);
#22647=AXIS2_PLACEMENT_3D('',#53802,#25225,#25226);
#22648=AXIS2_PLACEMENT_3D('',#53856,#25228,#25229);
#22649=AXIS2_PLACEMENT_3D('',#53904,#25231,#25232);
#22650=AXIS2_PLACEMENT_3D('',#53952,#25234,#25235);
#22651=AXIS2_PLACEMENT_3D('',#54006,#25237,#25238);
#22652=AXIS2_PLACEMENT_3D('',#54054,#25240,#25241);
#22653=AXIS2_PLACEMENT_3D('',#54102,#25243,#25244);
#22654=AXIS2_PLACEMENT_3D('',#54156,#25246,#25247);
#22655=AXIS2_PLACEMENT_3D('',#54204,#25249,#25250);
#22656=AXIS2_PLACEMENT_3D('',#54252,#25252,#25253);
#22657=AXIS2_PLACEMENT_3D('',#54269,#25255,#25256);
#22658=AXIS2_PLACEMENT_3D('',#54279,#25257,#25258);
#22659=AXIS2_PLACEMENT_3D('',#54304,#25260,#25261);
#22660=AXIS2_PLACEMENT_3D('',#54328,#25263,#25264);
#22661=AXIS2_PLACEMENT_3D('',#54353,#25266,#25267);
#22662=AXIS2_PLACEMENT_3D('',#54378,#25269,#25270);
#22663=AXIS2_PLACEMENT_3D('',#54402,#25272,#25273);
#22664=AXIS2_PLACEMENT_3D('',#54427,#25275,#25276);
#22665=AXIS2_PLACEMENT_3D('',#54452,#25278,#25279);
#22666=AXIS2_PLACEMENT_3D('',#54476,#25281,#25282);
#22667=AXIS2_PLACEMENT_3D('',#54501,#25284,#25285);
#22668=AXIS2_PLACEMENT_3D('',#54526,#25287,#25288);
#22669=AXIS2_PLACEMENT_3D('',#54550,#25290,#25291);
#22670=AXIS2_PLACEMENT_3D('',#54574,#25293,#25294);
#22671=AXIS2_PLACEMENT_3D('',#54599,#25296,#25297);
#22672=AXIS2_PLACEMENT_3D('',#54624,#25299,#25300);
#22673=AXIS2_PLACEMENT_3D('',#54648,#25302,#25303);
#22674=AXIS2_PLACEMENT_3D('',#54673,#25305,#25306);
#22675=AXIS2_PLACEMENT_3D('',#54698,#25308,#25309);
#22676=AXIS2_PLACEMENT_3D('',#54722,#25311,#25312);
#22677=AXIS2_PLACEMENT_3D('',#55043,#25313,#25314);
#22678=AXIS2_PLACEMENT_3D('',#55083,#25316,#25317);
#22679=AXIS2_PLACEMENT_3D('',#55732,#25318,#25319);
#22680=AXIS2_PLACEMENT_3D('',#55743,#25320,#25321);
#22681=AXIS2_PLACEMENT_3D('',#56396,#25322,#25323);
#22682=AXIS2_PLACEMENT_3D('',#56397,#25324,#25325);
#22683=AXIS2_PLACEMENT_3D('',#56406,#25330,#25331);
#22684=AXIS2_PLACEMENT_3D('',#56412,#25335,#25336);
#22685=AXIS2_PLACEMENT_3D('',#56418,#25340,#25341);
#22686=AXIS2_PLACEMENT_3D('',#56424,#25345,#25346);
#22687=AXIS2_PLACEMENT_3D('',#56430,#25350,#25351);
#22688=AXIS2_PLACEMENT_3D('',#56433,#25354,#25355);
#22689=AXIS2_PLACEMENT_3D('',#56434,#25356,#25357);
#22690=AXIS2_PLACEMENT_3D('',#56436,#25358,#25359);
#22691=AXIS2_PLACEMENT_3D('',#56437,#25360,#25361);
#22692=AXIS2_PLACEMENT_3D('',#56440,#25363,#25364);
#22693=AXIS2_PLACEMENT_3D('',#56441,#25365,#25366);
#22694=AXIS2_PLACEMENT_3D('',#56442,#25367,#25368);
#22695=AXIS2_PLACEMENT_3D('',#56443,#25369,#25370);
#22696=AXIS2_PLACEMENT_3D('',#56444,#25371,#25372);
#22697=AXIS2_PLACEMENT_3D('',#56446,#25373,#25374);
#22698=AXIS2_PLACEMENT_3D('',#56449,#25376,#25377);
#22699=AXIS2_PLACEMENT_3D('',#56450,#25378,#25379);
#22700=AXIS2_PLACEMENT_3D('',#56451,#25380,#25381);
#22701=AXIS2_PLACEMENT_3D('',#56452,#25382,#25383);
#22702=AXIS2_PLACEMENT_3D('',#56453,#25384,#25385);
#22703=AXIS2_PLACEMENT_3D('',#56463,#25387,#25388);
#22704=AXIS2_PLACEMENT_3D('',#56466,#25390,#25391);
#22705=AXIS2_PLACEMENT_3D('',#56468,#25392,#25393);
#22706=AXIS2_PLACEMENT_3D('',#56479,#25394,#25395);
#22707=AXIS2_PLACEMENT_3D('',#56530,#25397,#25398);
#22708=AXIS2_PLACEMENT_3D('',#56581,#25400,#25401);
#22709=AXIS2_PLACEMENT_3D('',#56629,#25403,#25404);
#22710=AXIS2_PLACEMENT_3D('',#56680,#25406,#25407);
#22711=AXIS2_PLACEMENT_3D('',#56731,#25409,#25410);
#22712=AXIS2_PLACEMENT_3D('',#56779,#25412,#25413);
#22713=AXIS2_PLACEMENT_3D('',#56798,#25415,#25416);
#22714=AXIS2_PLACEMENT_3D('',#56818,#25417,#25418);
#22715=AXIS2_PLACEMENT_3D('',#56832,#25420,#25421);
#22716=AXIS2_PLACEMENT_3D('',#56842,#25422,#25423);
#22717=AXIS2_PLACEMENT_3D('',#56866,#25425,#25426);
#22718=AXIS2_PLACEMENT_3D('',#56891,#25428,#25429);
#22719=AXIS2_PLACEMENT_3D('',#56916,#25431,#25432);
#22720=AXIS2_PLACEMENT_3D('',#56940,#25434,#25435);
#22721=AXIS2_PLACEMENT_3D('',#56965,#25437,#25438);
#22722=AXIS2_PLACEMENT_3D('',#56990,#25440,#25441);
#22723=AXIS2_PLACEMENT_3D('',#57001,#25443,#25444);
#22724=AXIS2_PLACEMENT_3D('',#57007,#25445,#25446);
#22725=AXIS2_PLACEMENT_3D('',#57017,#25448,#25449);
#22726=AXIS2_PLACEMENT_3D('',#57020,#25451,#25452);
#22727=AXIS2_PLACEMENT_3D('',#57022,#25453,#25454);
#22728=AXIS2_PLACEMENT_3D('',#57033,#25455,#25456);
#22729=AXIS2_PLACEMENT_3D('',#57084,#25458,#25459);
#22730=AXIS2_PLACEMENT_3D('',#57135,#25461,#25462);
#22731=AXIS2_PLACEMENT_3D('',#57183,#25464,#25465);
#22732=AXIS2_PLACEMENT_3D('',#57234,#25467,#25468);
#22733=AXIS2_PLACEMENT_3D('',#57285,#25470,#25471);
#22734=AXIS2_PLACEMENT_3D('',#57333,#25473,#25474);
#22735=AXIS2_PLACEMENT_3D('',#57352,#25476,#25477);
#22736=AXIS2_PLACEMENT_3D('',#57372,#25478,#25479);
#22737=AXIS2_PLACEMENT_3D('',#57386,#25481,#25482);
#22738=AXIS2_PLACEMENT_3D('',#57396,#25483,#25484);
#22739=AXIS2_PLACEMENT_3D('',#57420,#25486,#25487);
#22740=AXIS2_PLACEMENT_3D('',#57445,#25489,#25490);
#22741=AXIS2_PLACEMENT_3D('',#57470,#25492,#25493);
#22742=AXIS2_PLACEMENT_3D('',#57494,#25495,#25496);
#22743=AXIS2_PLACEMENT_3D('',#57519,#25498,#25499);
#22744=AXIS2_PLACEMENT_3D('',#57544,#25501,#25502);
#22745=AXIS2_PLACEMENT_3D('',#57555,#25504,#25505);
#22746=AXIS2_PLACEMENT_3D('',#57561,#25506,#25507);
#22747=AXIS2_PLACEMENT_3D('',#57571,#25509,#25510);
#22748=AXIS2_PLACEMENT_3D('',#57574,#25512,#25513);
#22749=AXIS2_PLACEMENT_3D('',#57576,#25514,#25515);
#22750=AXIS2_PLACEMENT_3D('',#57587,#25516,#25517);
#22751=AXIS2_PLACEMENT_3D('',#57638,#25519,#25520);
#22752=AXIS2_PLACEMENT_3D('',#57689,#25522,#25523);
#22753=AXIS2_PLACEMENT_3D('',#57737,#25525,#25526);
#22754=AXIS2_PLACEMENT_3D('',#57788,#25528,#25529);
#22755=AXIS2_PLACEMENT_3D('',#57839,#25531,#25532);
#22756=AXIS2_PLACEMENT_3D('',#57887,#25534,#25535);
#22757=AXIS2_PLACEMENT_3D('',#57906,#25537,#25538);
#22758=AXIS2_PLACEMENT_3D('',#57926,#25539,#25540);
#22759=AXIS2_PLACEMENT_3D('',#57940,#25542,#25543);
#22760=AXIS2_PLACEMENT_3D('',#57950,#25544,#25545);
#22761=AXIS2_PLACEMENT_3D('',#57974,#25547,#25548);
#22762=AXIS2_PLACEMENT_3D('',#57999,#25550,#25551);
#22763=AXIS2_PLACEMENT_3D('',#58024,#25553,#25554);
#22764=AXIS2_PLACEMENT_3D('',#58048,#25556,#25557);
#22765=AXIS2_PLACEMENT_3D('',#58073,#25559,#25560);
#22766=AXIS2_PLACEMENT_3D('',#58098,#25562,#25563);
#22767=AXIS2_PLACEMENT_3D('',#58109,#25565,#25566);
#22768=AXIS2_PLACEMENT_3D('',#58115,#25567,#25568);
#22769=AXIS2_PLACEMENT_3D('',#58307,#25569,#25570);
#22770=AXIS2_PLACEMENT_3D('',#59006,#25571,#25572);
#22771=AXIS2_PLACEMENT_3D('',#59007,#25573,#25574);
#22772=AXIS2_PLACEMENT_3D('',#59199,#25575,#25576);
#22773=AXIS2_PLACEMENT_3D('',#59898,#25577,#25578);
#22774=AXIS2_PLACEMENT_3D('',#59899,#25579,#25580);
#22775=AXIS2_PLACEMENT_3D('',#60091,#25581,#25582);
#22776=AXIS2_PLACEMENT_3D('',#60790,#25583,#25584);
#22777=AXIS2_PLACEMENT_3D('',#60791,#25585,#25586);
#22778=AXIS2_PLACEMENT_3D('',#60792,#25587,#25588);
#22779=AXIS2_PLACEMENT_3D('',#60793,#25589,#25590);
#22780=AXIS2_PLACEMENT_3D('',#60794,#25591,#25592);
#22781=AXIS2_PLACEMENT_3D('',#60796,#25593,#25594);
#22782=AXIS2_PLACEMENT_3D('',#60798,#25595,#25596);
#22783=AXIS2_PLACEMENT_3D('',#60799,#25597,#25598);
#22784=AXIS2_PLACEMENT_3D('',#60801,#25599,#25600);
#22785=AXIS2_PLACEMENT_3D('',#60804,#25602,#25603);
#22786=AXIS2_PLACEMENT_3D('',#60805,#25604,#25605);
#22787=AXIS2_PLACEMENT_3D('',#60806,#25606,#25607);
#22788=AXIS2_PLACEMENT_3D('',#60807,#25608,#25609);
#22789=AXIS2_PLACEMENT_3D('',#60808,#25610,#25611);
#22790=AXIS2_PLACEMENT_3D('',#60810,#25612,#25613);
#22791=AXIS2_PLACEMENT_3D('',#60813,#25615,#25616);
#22792=AXIS2_PLACEMENT_3D('',#60814,#25617,#25618);
#22793=AXIS2_PLACEMENT_3D('',#60816,#25619,#25620);
#22794=AXIS2_PLACEMENT_3D('',#60819,#25622,#25623);
#22795=AXIS2_PLACEMENT_3D('',#60820,#25624,#25625);
#22796=AXIS2_PLACEMENT_3D('',#60822,#25626,#25627);
#22797=AXIS2_PLACEMENT_3D('',#60825,#25629,#25630);
#22798=AXIS2_PLACEMENT_3D('',#60826,#25631,#25632);
#22799=AXIS2_PLACEMENT_3D('',#60828,#25633,#25634);
#22800=AXIS2_PLACEMENT_3D('',#60830,#25635,#25636);
#22801=AXIS2_PLACEMENT_3D('',#60831,#25637,#25638);
#22802=AXIS2_PLACEMENT_3D('',#60832,#25639,#25640);
#22803=AXIS2_PLACEMENT_3D('',#60834,#25641,#25642);
#22804=AXIS2_PLACEMENT_3D('',#60836,#25644,#25645);
#22805=AXIS2_PLACEMENT_3D('',#60838,#25646,#25647);
#22806=AXIS2_PLACEMENT_3D('',#60841,#25649,#25650);
#22807=AXIS2_PLACEMENT_3D('',#60842,#25651,#25652);
#22808=AXIS2_PLACEMENT_3D('',#60843,#25653,#25654);
#22809=AXIS2_PLACEMENT_3D('',#60844,#25655,#25656);
#22810=AXIS2_PLACEMENT_3D('',#60845,#25657,#25658);
#22811=AXIS2_PLACEMENT_3D('',#60861,#25660,#25661);
#22812=AXIS2_PLACEMENT_3D('',#60872,#25662,#25663);
#22813=AXIS2_PLACEMENT_3D('',#60920,#25665,#25666);
#22814=AXIS2_PLACEMENT_3D('',#60968,#25668,#25669);
#22815=AXIS2_PLACEMENT_3D('',#61019,#25671,#25672);
#22816=AXIS2_PLACEMENT_3D('',#61067,#25674,#25675);
#22817=AXIS2_PLACEMENT_3D('',#61115,#25677,#25678);
#22818=AXIS2_PLACEMENT_3D('',#61163,#25680,#25681);
#22819=AXIS2_PLACEMENT_3D('',#61217,#25683,#25684);
#22820=AXIS2_PLACEMENT_3D('',#61265,#25686,#25687);
#22821=AXIS2_PLACEMENT_3D('',#61313,#25689,#25690);
#22822=AXIS2_PLACEMENT_3D('',#61367,#25692,#25693);
#22823=AXIS2_PLACEMENT_3D('',#61415,#25695,#25696);
#22824=AXIS2_PLACEMENT_3D('',#61463,#25698,#25699);
#22825=AXIS2_PLACEMENT_3D('',#61514,#25701,#25702);
#22826=AXIS2_PLACEMENT_3D('',#61565,#25704,#25705);
#22827=AXIS2_PLACEMENT_3D('',#61613,#25707,#25708);
#22828=AXIS2_PLACEMENT_3D('',#61661,#25710,#25711);
#22829=AXIS2_PLACEMENT_3D('',#61715,#25713,#25714);
#22830=AXIS2_PLACEMENT_3D('',#61763,#25716,#25717);
#22831=AXIS2_PLACEMENT_3D('',#61811,#25719,#25720);
#22832=AXIS2_PLACEMENT_3D('',#61865,#25722,#25723);
#22833=AXIS2_PLACEMENT_3D('',#61913,#25725,#25726);
#22834=AXIS2_PLACEMENT_3D('',#61961,#25728,#25729);
#22835=AXIS2_PLACEMENT_3D('',#62009,#25731,#25732);
#22836=AXIS2_PLACEMENT_3D('',#62063,#25734,#25735);
#22837=AXIS2_PLACEMENT_3D('',#62111,#25737,#25738);
#22838=AXIS2_PLACEMENT_3D('',#62159,#25740,#25741);
#22839=AXIS2_PLACEMENT_3D('',#62213,#25743,#25744);
#22840=AXIS2_PLACEMENT_3D('',#62261,#25746,#25747);
#22841=AXIS2_PLACEMENT_3D('',#62309,#25749,#25750);
#22842=AXIS2_PLACEMENT_3D('',#62363,#25752,#25753);
#22843=AXIS2_PLACEMENT_3D('',#62411,#25755,#25756);
#22844=AXIS2_PLACEMENT_3D('',#62459,#25758,#25759);
#22845=AXIS2_PLACEMENT_3D('',#62507,#25761,#25762);
#22846=AXIS2_PLACEMENT_3D('',#62561,#25764,#25765);
#22847=AXIS2_PLACEMENT_3D('',#62609,#25767,#25768);
#22848=AXIS2_PLACEMENT_3D('',#62657,#25770,#25771);
#22849=AXIS2_PLACEMENT_3D('',#62711,#25773,#25774);
#22850=AXIS2_PLACEMENT_3D('',#62759,#25776,#25777);
#22851=AXIS2_PLACEMENT_3D('',#62807,#25779,#25780);
#22852=AXIS2_PLACEMENT_3D('',#62861,#25782,#25783);
#22853=AXIS2_PLACEMENT_3D('',#62909,#25785,#25786);
#22854=AXIS2_PLACEMENT_3D('',#62957,#25788,#25789);
#22855=AXIS2_PLACEMENT_3D('',#63005,#25791,#25792);
#22856=AXIS2_PLACEMENT_3D('',#63059,#25794,#25795);
#22857=AXIS2_PLACEMENT_3D('',#63107,#25797,#25798);
#22858=AXIS2_PLACEMENT_3D('',#63155,#25800,#25801);
#22859=AXIS2_PLACEMENT_3D('',#63209,#25803,#25804);
#22860=AXIS2_PLACEMENT_3D('',#63257,#25806,#25807);
#22861=AXIS2_PLACEMENT_3D('',#63305,#25809,#25810);
#22862=AXIS2_PLACEMENT_3D('',#63359,#25812,#25813);
#22863=AXIS2_PLACEMENT_3D('',#63407,#25815,#25816);
#22864=AXIS2_PLACEMENT_3D('',#63455,#25818,#25819);
#22865=AXIS2_PLACEMENT_3D('',#63503,#25821,#25822);
#22866=AXIS2_PLACEMENT_3D('',#63557,#25824,#25825);
#22867=AXIS2_PLACEMENT_3D('',#63605,#25827,#25828);
#22868=AXIS2_PLACEMENT_3D('',#63653,#25830,#25831);
#22869=AXIS2_PLACEMENT_3D('',#63707,#25833,#25834);
#22870=AXIS2_PLACEMENT_3D('',#63755,#25836,#25837);
#22871=AXIS2_PLACEMENT_3D('',#63803,#25839,#25840);
#22872=AXIS2_PLACEMENT_3D('',#63815,#25842,#25843);
#22873=AXIS2_PLACEMENT_3D('',#63821,#25844,#25845);
#22874=AXIS2_PLACEMENT_3D('',#63846,#25847,#25848);
#22875=AXIS2_PLACEMENT_3D('',#63870,#25850,#25851);
#22876=AXIS2_PLACEMENT_3D('',#63895,#25853,#25854);
#22877=AXIS2_PLACEMENT_3D('',#63920,#25856,#25857);
#22878=AXIS2_PLACEMENT_3D('',#63944,#25859,#25860);
#22879=AXIS2_PLACEMENT_3D('',#63969,#25862,#25863);
#22880=AXIS2_PLACEMENT_3D('',#63994,#25865,#25866);
#22881=AXIS2_PLACEMENT_3D('',#64018,#25868,#25869);
#22882=AXIS2_PLACEMENT_3D('',#64042,#25871,#25872);
#22883=AXIS2_PLACEMENT_3D('',#64067,#25874,#25875);
#22884=AXIS2_PLACEMENT_3D('',#64092,#25877,#25878);
#22885=AXIS2_PLACEMENT_3D('',#64116,#25880,#25881);
#22886=AXIS2_PLACEMENT_3D('',#64141,#25883,#25884);
#22887=AXIS2_PLACEMENT_3D('',#64166,#25886,#25887);
#22888=AXIS2_PLACEMENT_3D('',#64190,#25889,#25890);
#22889=AXIS2_PLACEMENT_3D('',#64215,#25892,#25893);
#22890=AXIS2_PLACEMENT_3D('',#64240,#25895,#25896);
#22891=AXIS2_PLACEMENT_3D('',#64264,#25898,#25899);
#22892=AXIS2_PLACEMENT_3D('',#64288,#25901,#25902);
#22893=AXIS2_PLACEMENT_3D('',#64313,#25904,#25905);
#22894=AXIS2_PLACEMENT_3D('',#64338,#25907,#25908);
#22895=AXIS2_PLACEMENT_3D('',#64362,#25910,#25911);
#22896=AXIS2_PLACEMENT_3D('',#64387,#25913,#25914);
#22897=AXIS2_PLACEMENT_3D('',#64412,#25916,#25917);
#22898=AXIS2_PLACEMENT_3D('',#64436,#25919,#25920);
#22899=AXIS2_PLACEMENT_3D('',#64461,#25922,#25923);
#22900=AXIS2_PLACEMENT_3D('',#64486,#25925,#25926);
#22901=AXIS2_PLACEMENT_3D('',#64510,#25928,#25929);
#22902=AXIS2_PLACEMENT_3D('',#64534,#25931,#25932);
#22903=AXIS2_PLACEMENT_3D('',#64559,#25934,#25935);
#22904=AXIS2_PLACEMENT_3D('',#64584,#25937,#25938);
#22905=AXIS2_PLACEMENT_3D('',#64608,#25940,#25941);
#22906=AXIS2_PLACEMENT_3D('',#64633,#25943,#25944);
#22907=AXIS2_PLACEMENT_3D('',#64658,#25946,#25947);
#22908=AXIS2_PLACEMENT_3D('',#64682,#25949,#25950);
#22909=AXIS2_PLACEMENT_3D('',#64707,#25952,#25953);
#22910=AXIS2_PLACEMENT_3D('',#64732,#25955,#25956);
#22911=AXIS2_PLACEMENT_3D('',#64756,#25958,#25959);
#22912=AXIS2_PLACEMENT_3D('',#64780,#25961,#25962);
#22913=AXIS2_PLACEMENT_3D('',#64805,#25964,#25965);
#22914=AXIS2_PLACEMENT_3D('',#64830,#25967,#25968);
#22915=AXIS2_PLACEMENT_3D('',#64854,#25970,#25971);
#22916=AXIS2_PLACEMENT_3D('',#64879,#25973,#25974);
#22917=AXIS2_PLACEMENT_3D('',#64904,#25976,#25977);
#22918=AXIS2_PLACEMENT_3D('',#64928,#25979,#25980);
#22919=AXIS2_PLACEMENT_3D('',#64953,#25982,#25983);
#22920=AXIS2_PLACEMENT_3D('',#64977,#25985,#25986);
#22921=AXIS2_PLACEMENT_3D('',#65002,#25988,#25989);
#22922=AXIS2_PLACEMENT_3D('',#65026,#25991,#25992);
#22923=AXIS2_PLACEMENT_3D('',#65051,#25994,#25995);
#22924=AXIS2_PLACEMENT_3D('',#65076,#25997,#25998);
#22925=AXIS2_PLACEMENT_3D('',#65100,#26000,#26001);
#22926=AXIS2_PLACEMENT_3D('',#65125,#26003,#26004);
#22927=AXIS2_PLACEMENT_3D('',#65150,#26006,#26007);
#22928=AXIS2_PLACEMENT_3D('',#65174,#26009,#26010);
#22929=AXIS2_PLACEMENT_3D('',#65199,#26012,#26013);
#22930=AXIS2_PLACEMENT_3D('',#65223,#26015,#26016);
#22931=AXIS2_PLACEMENT_3D('',#65248,#26018,#26019);
#22932=AXIS2_PLACEMENT_3D('',#67057,#26021,#26022);
#22933=AXIS2_PLACEMENT_3D('',#67059,#26023,#26024);
#22934=AXIS2_PLACEMENT_3D('',#68841,#26025,#26026);
#22935=AXIS2_PLACEMENT_3D('',#68842,#26027,#26028);
#22936=AXIS2_PLACEMENT_3D('',#68843,#26029,#26030);
#22937=AXIS2_PLACEMENT_3D('',#68856,#26037,#26038);
#22938=AXIS2_PLACEMENT_3D('',#68870,#26045,#26046);
#22939=AXIS2_PLACEMENT_3D('',#68871,#26047,#26048);
#22940=AXIS2_PLACEMENT_3D('',#68874,#26051,#26052);
#22941=AXIS2_PLACEMENT_3D('',#68876,#26054,#26055);
#22942=AXIS2_PLACEMENT_3D('',#68878,#26057,#26058);
#22943=AXIS2_PLACEMENT_3D('',#68880,#26060,#26061);
#22944=AXIS2_PLACEMENT_3D('',#68882,#26063,#26064);
#22945=AXIS2_PLACEMENT_3D('',#68883,#26065,#26066);
#22946=AXIS2_PLACEMENT_3D('',#68886,#26068,#26069);
#22947=AXIS2_PLACEMENT_3D('',#68887,#26070,#26071);
#22948=AXIS2_PLACEMENT_3D('',#68888,#26072,#26073);
#22949=AXIS2_PLACEMENT_3D('',#68890,#26074,#26075);
#22950=AXIS2_PLACEMENT_3D('',#68891,#26076,#26077);
#22951=AXIS2_PLACEMENT_3D('',#68892,#26078,#26079);
#22952=AXIS2_PLACEMENT_3D('',#68905,#26081,#26082);
#22953=AXIS2_PLACEMENT_3D('',#68916,#26083,#26084);
#22954=AXIS2_PLACEMENT_3D('',#68967,#26086,#26087);
#22955=AXIS2_PLACEMENT_3D('',#69018,#26089,#26090);
#22956=AXIS2_PLACEMENT_3D('',#69066,#26092,#26093);
#22957=AXIS2_PLACEMENT_3D('',#69117,#26095,#26096);
#22958=AXIS2_PLACEMENT_3D('',#69168,#26098,#26099);
#22959=AXIS2_PLACEMENT_3D('',#69216,#26101,#26102);
#22960=AXIS2_PLACEMENT_3D('',#69238,#26104,#26105);
#22961=AXIS2_PLACEMENT_3D('',#69258,#26106,#26107);
#22962=AXIS2_PLACEMENT_3D('',#69273,#26109,#26110);
#22963=AXIS2_PLACEMENT_3D('',#69283,#26111,#26112);
#22964=AXIS2_PLACEMENT_3D('',#69307,#26114,#26115);
#22965=AXIS2_PLACEMENT_3D('',#69332,#26117,#26118);
#22966=AXIS2_PLACEMENT_3D('',#69357,#26120,#26121);
#22967=AXIS2_PLACEMENT_3D('',#69381,#26123,#26124);
#22968=AXIS2_PLACEMENT_3D('',#69406,#26126,#26127);
#22969=AXIS2_PLACEMENT_3D('',#69431,#26129,#26130);
#22970=AXIS2_PLACEMENT_3D('',#69443,#26132,#26133);
#22971=AXIS2_PLACEMENT_3D('',#69449,#26134,#26135);
#22972=AXIS2_PLACEMENT_3D('',#70403,#26136,#26137);
#22973=AXIS2_PLACEMENT_3D('',#70416,#26144,#26145);
#22974=AXIS2_PLACEMENT_3D('',#70417,#26146,#26147);
#22975=AXIS2_PLACEMENT_3D('',#70423,#26151,#26152);
#22976=AXIS2_PLACEMENT_3D('',#70427,#26155,#26156);
#22977=AXIS2_PLACEMENT_3D('',#70431,#26159,#26160);
#22978=AXIS2_PLACEMENT_3D('',#70435,#26163,#26164);
#22979=AXIS2_PLACEMENT_3D('',#70439,#26167,#26168);
#22980=AXIS2_PLACEMENT_3D('',#70441,#26170,#26171);
#22981=AXIS2_PLACEMENT_3D('',#70442,#26172,#26173);
#22982=AXIS2_PLACEMENT_3D('',#70443,#26174,#26175);
#22983=AXIS2_PLACEMENT_3D('',#70445,#26176,#26177);
#22984=AXIS2_PLACEMENT_3D('',#70448,#26179,#26180);
#22985=AXIS2_PLACEMENT_3D('',#70449,#26181,#26182);
#22986=AXIS2_PLACEMENT_3D('',#70451,#26183,#26184);
#22987=AXIS2_PLACEMENT_3D('',#70454,#26186,#26187);
#22988=AXIS2_PLACEMENT_3D('',#70455,#26188,#26189);
#22989=AXIS2_PLACEMENT_3D('',#70456,#26190,#26191);
#22990=AXIS2_PLACEMENT_3D('',#70457,#26192,#26193);
#22991=AXIS2_PLACEMENT_3D('',#70458,#26194,#26195);
#22992=AXIS2_PLACEMENT_3D('',#70474,#26197,#26198);
#22993=AXIS2_PLACEMENT_3D('',#70482,#26199,#26200);
#22994=AXIS2_PLACEMENT_3D('',#70530,#26202,#26203);
#22995=AXIS2_PLACEMENT_3D('',#70578,#26205,#26206);
#22996=AXIS2_PLACEMENT_3D('',#70632,#26208,#26209);
#22997=AXIS2_PLACEMENT_3D('',#70680,#26211,#26212);
#22998=AXIS2_PLACEMENT_3D('',#70728,#26214,#26215);
#22999=AXIS2_PLACEMENT_3D('',#70782,#26217,#26218);
#23000=AXIS2_PLACEMENT_3D('',#70830,#26220,#26221);
#23001=AXIS2_PLACEMENT_3D('',#70878,#26223,#26224);
#23002=AXIS2_PLACEMENT_3D('',#70932,#26226,#26227);
#23003=AXIS2_PLACEMENT_3D('',#70980,#26229,#26230);
#23004=AXIS2_PLACEMENT_3D('',#71028,#26232,#26233);
#23005=AXIS2_PLACEMENT_3D('',#71082,#26235,#26236);
#23006=AXIS2_PLACEMENT_3D('',#71130,#26238,#26239);
#23007=AXIS2_PLACEMENT_3D('',#71178,#26241,#26242);
#23008=AXIS2_PLACEMENT_3D('',#71194,#26244,#26245);
#23009=AXIS2_PLACEMENT_3D('',#71203,#26246,#26247);
#23010=AXIS2_PLACEMENT_3D('',#71228,#26249,#26250);
#23011=AXIS2_PLACEMENT_3D('',#71252,#26252,#26253);
#23012=AXIS2_PLACEMENT_3D('',#71277,#26255,#26256);
#23013=AXIS2_PLACEMENT_3D('',#71302,#26258,#26259);
#23014=AXIS2_PLACEMENT_3D('',#71326,#26261,#26262);
#23015=AXIS2_PLACEMENT_3D('',#71351,#26264,#26265);
#23016=AXIS2_PLACEMENT_3D('',#71376,#26267,#26268);
#23017=AXIS2_PLACEMENT_3D('',#71400,#26270,#26271);
#23018=AXIS2_PLACEMENT_3D('',#71425,#26273,#26274);
#23019=AXIS2_PLACEMENT_3D('',#71450,#26276,#26277);
#23020=AXIS2_PLACEMENT_3D('',#71474,#26279,#26280);
#23021=AXIS2_PLACEMENT_3D('',#71499,#26282,#26283);
#23022=AXIS2_PLACEMENT_3D('',#71524,#26285,#26286);
#23023=AXIS2_PLACEMENT_3D('',#71548,#26288,#26289);
#23024=AXIS2_PLACEMENT_3D('',#71836,#26290,#26291);
#23025=AXIS2_PLACEMENT_3D('',#71870,#26293,#26294);
#23026=AXIS2_PLACEMENT_3D('',#72395,#26295,#26296);
#23027=AXIS2_PLACEMENT_3D('',#72406,#26297,#26298);
#23028=AXIS2_PLACEMENT_3D('',#72933,#26299,#26300);
#23029=AXIS2_PLACEMENT_3D('',#72934,#26301,#26302);
#23030=AXIS2_PLACEMENT_3D('',#72943,#26307,#26308);
#23031=AXIS2_PLACEMENT_3D('',#72949,#26312,#26313);
#23032=AXIS2_PLACEMENT_3D('',#72955,#26317,#26318);
#23033=AXIS2_PLACEMENT_3D('',#72961,#26322,#26323);
#23034=AXIS2_PLACEMENT_3D('',#72967,#26327,#26328);
#23035=AXIS2_PLACEMENT_3D('',#72970,#26331,#26332);
#23036=AXIS2_PLACEMENT_3D('',#72971,#26333,#26334);
#23037=AXIS2_PLACEMENT_3D('',#72973,#26335,#26336);
#23038=AXIS2_PLACEMENT_3D('',#72974,#26337,#26338);
#23039=AXIS2_PLACEMENT_3D('',#72977,#26340,#26341);
#23040=AXIS2_PLACEMENT_3D('',#72978,#26342,#26343);
#23041=AXIS2_PLACEMENT_3D('',#72979,#26344,#26345);
#23042=AXIS2_PLACEMENT_3D('',#72980,#26346,#26347);
#23043=AXIS2_PLACEMENT_3D('',#72981,#26348,#26349);
#23044=AXIS2_PLACEMENT_3D('',#72991,#26351,#26352);
#23045=AXIS2_PLACEMENT_3D('',#73002,#26353,#26354);
#23046=AXIS2_PLACEMENT_3D('',#73053,#26356,#26357);
#23047=AXIS2_PLACEMENT_3D('',#73104,#26359,#26360);
#23048=AXIS2_PLACEMENT_3D('',#73152,#26362,#26363);
#23049=AXIS2_PLACEMENT_3D('',#73200,#26365,#26366);
#23050=AXIS2_PLACEMENT_3D('',#73251,#26368,#26369);
#23051=AXIS2_PLACEMENT_3D('',#73302,#26371,#26372);
#23052=AXIS2_PLACEMENT_3D('',#73350,#26374,#26375);
#23053=AXIS2_PLACEMENT_3D('',#73401,#26377,#26378);
#23054=AXIS2_PLACEMENT_3D('',#73452,#26380,#26381);
#23055=AXIS2_PLACEMENT_3D('',#73500,#26383,#26384);
#23056=AXIS2_PLACEMENT_3D('',#73548,#26386,#26387);
#23057=AXIS2_PLACEMENT_3D('',#73602,#26389,#26390);
#23058=AXIS2_PLACEMENT_3D('',#73650,#26392,#26393);
#23059=AXIS2_PLACEMENT_3D('',#73698,#26395,#26396);
#23060=AXIS2_PLACEMENT_3D('',#73749,#26398,#26399);
#23061=AXIS2_PLACEMENT_3D('',#73800,#26401,#26402);
#23062=AXIS2_PLACEMENT_3D('',#73848,#26404,#26405);
#23063=AXIS2_PLACEMENT_3D('',#73899,#26407,#26408);
#23064=AXIS2_PLACEMENT_3D('',#73918,#26410,#26411);
#23065=AXIS2_PLACEMENT_3D('',#73938,#26412,#26413);
#23066=AXIS2_PLACEMENT_3D('',#73948,#26415,#26416);
#23067=AXIS2_PLACEMENT_3D('',#73959,#26417,#26418);
#23068=AXIS2_PLACEMENT_3D('',#74010,#26420,#26421);
#23069=AXIS2_PLACEMENT_3D('',#74061,#26423,#26424);
#23070=AXIS2_PLACEMENT_3D('',#74109,#26426,#26427);
#23071=AXIS2_PLACEMENT_3D('',#74157,#26429,#26430);
#23072=AXIS2_PLACEMENT_3D('',#74208,#26432,#26433);
#23073=AXIS2_PLACEMENT_3D('',#74259,#26435,#26436);
#23074=AXIS2_PLACEMENT_3D('',#74307,#26438,#26439);
#23075=AXIS2_PLACEMENT_3D('',#74358,#26441,#26442);
#23076=AXIS2_PLACEMENT_3D('',#74409,#26444,#26445);
#23077=AXIS2_PLACEMENT_3D('',#74457,#26447,#26448);
#23078=AXIS2_PLACEMENT_3D('',#74505,#26450,#26451);
#23079=AXIS2_PLACEMENT_3D('',#74559,#26453,#26454);
#23080=AXIS2_PLACEMENT_3D('',#74607,#26456,#26457);
#23081=AXIS2_PLACEMENT_3D('',#74655,#26459,#26460);
#23082=AXIS2_PLACEMENT_3D('',#74706,#26462,#26463);
#23083=AXIS2_PLACEMENT_3D('',#74757,#26465,#26466);
#23084=AXIS2_PLACEMENT_3D('',#74805,#26468,#26469);
#23085=AXIS2_PLACEMENT_3D('',#74856,#26471,#26472);
#23086=AXIS2_PLACEMENT_3D('',#74875,#26474,#26475);
#23087=AXIS2_PLACEMENT_3D('',#74895,#26476,#26477);
#23088=AXIS2_PLACEMENT_3D('',#74905,#26479,#26480);
#23089=AXIS2_PLACEMENT_3D('',#74916,#26481,#26482);
#23090=AXIS2_PLACEMENT_3D('',#74967,#26484,#26485);
#23091=AXIS2_PLACEMENT_3D('',#75018,#26487,#26488);
#23092=AXIS2_PLACEMENT_3D('',#75066,#26490,#26491);
#23093=AXIS2_PLACEMENT_3D('',#75114,#26493,#26494);
#23094=AXIS2_PLACEMENT_3D('',#75165,#26496,#26497);
#23095=AXIS2_PLACEMENT_3D('',#75216,#26499,#26500);
#23096=AXIS2_PLACEMENT_3D('',#75264,#26502,#26503);
#23097=AXIS2_PLACEMENT_3D('',#75315,#26505,#26506);
#23098=AXIS2_PLACEMENT_3D('',#75366,#26508,#26509);
#23099=AXIS2_PLACEMENT_3D('',#75414,#26511,#26512);
#23100=AXIS2_PLACEMENT_3D('',#75462,#26514,#26515);
#23101=AXIS2_PLACEMENT_3D('',#75516,#26517,#26518);
#23102=AXIS2_PLACEMENT_3D('',#75564,#26520,#26521);
#23103=AXIS2_PLACEMENT_3D('',#75612,#26523,#26524);
#23104=AXIS2_PLACEMENT_3D('',#75663,#26526,#26527);
#23105=AXIS2_PLACEMENT_3D('',#75714,#26529,#26530);
#23106=AXIS2_PLACEMENT_3D('',#75762,#26532,#26533);
#23107=AXIS2_PLACEMENT_3D('',#75813,#26535,#26536);
#23108=AXIS2_PLACEMENT_3D('',#75832,#26538,#26539);
#23109=AXIS2_PLACEMENT_3D('',#75852,#26540,#26541);
#23110=AXIS2_PLACEMENT_3D('',#75862,#26543,#26544);
#23111=AXIS2_PLACEMENT_3D('',#75873,#26545,#26546);
#23112=AXIS2_PLACEMENT_3D('',#75924,#26548,#26549);
#23113=AXIS2_PLACEMENT_3D('',#75975,#26551,#26552);
#23114=AXIS2_PLACEMENT_3D('',#76023,#26554,#26555);
#23115=AXIS2_PLACEMENT_3D('',#76071,#26557,#26558);
#23116=AXIS2_PLACEMENT_3D('',#76122,#26560,#26561);
#23117=AXIS2_PLACEMENT_3D('',#76173,#26563,#26564);
#23118=AXIS2_PLACEMENT_3D('',#76221,#26566,#26567);
#23119=AXIS2_PLACEMENT_3D('',#76272,#26569,#26570);
#23120=AXIS2_PLACEMENT_3D('',#76323,#26572,#26573);
#23121=AXIS2_PLACEMENT_3D('',#76371,#26575,#26576);
#23122=AXIS2_PLACEMENT_3D('',#76419,#26578,#26579);
#23123=AXIS2_PLACEMENT_3D('',#76473,#26581,#26582);
#23124=AXIS2_PLACEMENT_3D('',#76521,#26584,#26585);
#23125=AXIS2_PLACEMENT_3D('',#76569,#26587,#26588);
#23126=AXIS2_PLACEMENT_3D('',#76620,#26590,#26591);
#23127=AXIS2_PLACEMENT_3D('',#76671,#26593,#26594);
#23128=AXIS2_PLACEMENT_3D('',#76719,#26596,#26597);
#23129=AXIS2_PLACEMENT_3D('',#76770,#26599,#26600);
#23130=AXIS2_PLACEMENT_3D('',#76789,#26602,#26603);
#23131=AXIS2_PLACEMENT_3D('',#76809,#26604,#26605);
#23132=AXIS2_PLACEMENT_3D('',#76819,#26607,#26608);
#23133=AXIS2_PLACEMENT_3D('',#76830,#26609,#26610);
#23134=AXIS2_PLACEMENT_3D('',#76881,#26612,#26613);
#23135=AXIS2_PLACEMENT_3D('',#76932,#26615,#26616);
#23136=AXIS2_PLACEMENT_3D('',#76980,#26618,#26619);
#23137=AXIS2_PLACEMENT_3D('',#77028,#26621,#26622);
#23138=AXIS2_PLACEMENT_3D('',#77079,#26624,#26625);
#23139=AXIS2_PLACEMENT_3D('',#77130,#26627,#26628);
#23140=AXIS2_PLACEMENT_3D('',#77178,#26630,#26631);
#23141=AXIS2_PLACEMENT_3D('',#77229,#26633,#26634);
#23142=AXIS2_PLACEMENT_3D('',#77280,#26636,#26637);
#23143=AXIS2_PLACEMENT_3D('',#77328,#26639,#26640);
#23144=AXIS2_PLACEMENT_3D('',#77376,#26642,#26643);
#23145=AXIS2_PLACEMENT_3D('',#77430,#26645,#26646);
#23146=AXIS2_PLACEMENT_3D('',#77478,#26648,#26649);
#23147=AXIS2_PLACEMENT_3D('',#77526,#26651,#26652);
#23148=AXIS2_PLACEMENT_3D('',#77577,#26654,#26655);
#23149=AXIS2_PLACEMENT_3D('',#77628,#26657,#26658);
#23150=AXIS2_PLACEMENT_3D('',#77676,#26660,#26661);
#23151=AXIS2_PLACEMENT_3D('',#77727,#26663,#26664);
#23152=AXIS2_PLACEMENT_3D('',#77746,#26666,#26667);
#23153=AXIS2_PLACEMENT_3D('',#77766,#26668,#26669);
#23154=AXIS2_PLACEMENT_3D('',#77776,#26671,#26672);
#23155=AXIS2_PLACEMENT_3D('',#77787,#26673,#26674);
#23156=AXIS2_PLACEMENT_3D('',#77838,#26676,#26677);
#23157=AXIS2_PLACEMENT_3D('',#77889,#26679,#26680);
#23158=AXIS2_PLACEMENT_3D('',#77937,#26682,#26683);
#23159=AXIS2_PLACEMENT_3D('',#77985,#26685,#26686);
#23160=AXIS2_PLACEMENT_3D('',#78036,#26688,#26689);
#23161=AXIS2_PLACEMENT_3D('',#78087,#26691,#26692);
#23162=AXIS2_PLACEMENT_3D('',#78135,#26694,#26695);
#23163=AXIS2_PLACEMENT_3D('',#78186,#26697,#26698);
#23164=AXIS2_PLACEMENT_3D('',#78237,#26700,#26701);
#23165=AXIS2_PLACEMENT_3D('',#78285,#26703,#26704);
#23166=AXIS2_PLACEMENT_3D('',#78333,#26706,#26707);
#23167=AXIS2_PLACEMENT_3D('',#78387,#26709,#26710);
#23168=AXIS2_PLACEMENT_3D('',#78435,#26712,#26713);
#23169=AXIS2_PLACEMENT_3D('',#78483,#26715,#26716);
#23170=AXIS2_PLACEMENT_3D('',#78534,#26718,#26719);
#23171=AXIS2_PLACEMENT_3D('',#78585,#26721,#26722);
#23172=AXIS2_PLACEMENT_3D('',#78633,#26724,#26725);
#23173=AXIS2_PLACEMENT_3D('',#78684,#26727,#26728);
#23174=AXIS2_PLACEMENT_3D('',#78703,#26730,#26731);
#23175=AXIS2_PLACEMENT_3D('',#78723,#26732,#26733);
#23176=AXIS2_PLACEMENT_3D('',#78737,#26735,#26736);
#23177=AXIS2_PLACEMENT_3D('',#78747,#26737,#26738);
#23178=AXIS2_PLACEMENT_3D('',#78771,#26740,#26741);
#23179=AXIS2_PLACEMENT_3D('',#78796,#26743,#26744);
#23180=AXIS2_PLACEMENT_3D('',#78820,#26746,#26747);
#23181=AXIS2_PLACEMENT_3D('',#78845,#26749,#26750);
#23182=AXIS2_PLACEMENT_3D('',#78869,#26752,#26753);
#23183=AXIS2_PLACEMENT_3D('',#78894,#26755,#26756);
#23184=AXIS2_PLACEMENT_3D('',#78919,#26758,#26759);
#23185=AXIS2_PLACEMENT_3D('',#78943,#26761,#26762);
#23186=AXIS2_PLACEMENT_3D('',#78968,#26764,#26765);
#23187=AXIS2_PLACEMENT_3D('',#78992,#26767,#26768);
#23188=AXIS2_PLACEMENT_3D('',#79017,#26770,#26771);
#23189=AXIS2_PLACEMENT_3D('',#79042,#26773,#26774);
#23190=AXIS2_PLACEMENT_3D('',#79066,#26776,#26777);
#23191=AXIS2_PLACEMENT_3D('',#79091,#26779,#26780);
#23192=AXIS2_PLACEMENT_3D('',#79115,#26782,#26783);
#23193=AXIS2_PLACEMENT_3D('',#79140,#26785,#26786);
#23194=AXIS2_PLACEMENT_3D('',#79165,#26788,#26789);
#23195=AXIS2_PLACEMENT_3D('',#79189,#26791,#26792);
#23196=AXIS2_PLACEMENT_3D('',#79200,#26794,#26795);
#23197=AXIS2_PLACEMENT_3D('',#79206,#26796,#26797);
#23198=AXIS2_PLACEMENT_3D('',#79220,#26799,#26800);
#23199=AXIS2_PLACEMENT_3D('',#79230,#26801,#26802);
#23200=AXIS2_PLACEMENT_3D('',#79254,#26804,#26805);
#23201=AXIS2_PLACEMENT_3D('',#79279,#26807,#26808);
#23202=AXIS2_PLACEMENT_3D('',#79303,#26810,#26811);
#23203=AXIS2_PLACEMENT_3D('',#79328,#26813,#26814);
#23204=AXIS2_PLACEMENT_3D('',#79352,#26816,#26817);
#23205=AXIS2_PLACEMENT_3D('',#79377,#26819,#26820);
#23206=AXIS2_PLACEMENT_3D('',#79402,#26822,#26823);
#23207=AXIS2_PLACEMENT_3D('',#79426,#26825,#26826);
#23208=AXIS2_PLACEMENT_3D('',#79451,#26828,#26829);
#23209=AXIS2_PLACEMENT_3D('',#79475,#26831,#26832);
#23210=AXIS2_PLACEMENT_3D('',#79500,#26834,#26835);
#23211=AXIS2_PLACEMENT_3D('',#79525,#26837,#26838);
#23212=AXIS2_PLACEMENT_3D('',#79549,#26840,#26841);
#23213=AXIS2_PLACEMENT_3D('',#79574,#26843,#26844);
#23214=AXIS2_PLACEMENT_3D('',#79598,#26846,#26847);
#23215=AXIS2_PLACEMENT_3D('',#79623,#26849,#26850);
#23216=AXIS2_PLACEMENT_3D('',#79648,#26852,#26853);
#23217=AXIS2_PLACEMENT_3D('',#79672,#26855,#26856);
#23218=AXIS2_PLACEMENT_3D('',#79683,#26858,#26859);
#23219=AXIS2_PLACEMENT_3D('',#79689,#26860,#26861);
#23220=AXIS2_PLACEMENT_3D('',#79703,#26863,#26864);
#23221=AXIS2_PLACEMENT_3D('',#79713,#26865,#26866);
#23222=AXIS2_PLACEMENT_3D('',#79737,#26868,#26869);
#23223=AXIS2_PLACEMENT_3D('',#79762,#26871,#26872);
#23224=AXIS2_PLACEMENT_3D('',#79786,#26874,#26875);
#23225=AXIS2_PLACEMENT_3D('',#79811,#26877,#26878);
#23226=AXIS2_PLACEMENT_3D('',#79835,#26880,#26881);
#23227=AXIS2_PLACEMENT_3D('',#79860,#26883,#26884);
#23228=AXIS2_PLACEMENT_3D('',#79885,#26886,#26887);
#23229=AXIS2_PLACEMENT_3D('',#79909,#26889,#26890);
#23230=AXIS2_PLACEMENT_3D('',#79934,#26892,#26893);
#23231=AXIS2_PLACEMENT_3D('',#79958,#26895,#26896);
#23232=AXIS2_PLACEMENT_3D('',#79983,#26898,#26899);
#23233=AXIS2_PLACEMENT_3D('',#80008,#26901,#26902);
#23234=AXIS2_PLACEMENT_3D('',#80032,#26904,#26905);
#23235=AXIS2_PLACEMENT_3D('',#80057,#26907,#26908);
#23236=AXIS2_PLACEMENT_3D('',#80081,#26910,#26911);
#23237=AXIS2_PLACEMENT_3D('',#80106,#26913,#26914);
#23238=AXIS2_PLACEMENT_3D('',#80131,#26916,#26917);
#23239=AXIS2_PLACEMENT_3D('',#80155,#26919,#26920);
#23240=AXIS2_PLACEMENT_3D('',#80166,#26922,#26923);
#23241=AXIS2_PLACEMENT_3D('',#80172,#26924,#26925);
#23242=AXIS2_PLACEMENT_3D('',#80186,#26927,#26928);
#23243=AXIS2_PLACEMENT_3D('',#80196,#26929,#26930);
#23244=AXIS2_PLACEMENT_3D('',#80220,#26932,#26933);
#23245=AXIS2_PLACEMENT_3D('',#80245,#26935,#26936);
#23246=AXIS2_PLACEMENT_3D('',#80269,#26938,#26939);
#23247=AXIS2_PLACEMENT_3D('',#80294,#26941,#26942);
#23248=AXIS2_PLACEMENT_3D('',#80318,#26944,#26945);
#23249=AXIS2_PLACEMENT_3D('',#80343,#26947,#26948);
#23250=AXIS2_PLACEMENT_3D('',#80368,#26950,#26951);
#23251=AXIS2_PLACEMENT_3D('',#80392,#26953,#26954);
#23252=AXIS2_PLACEMENT_3D('',#80417,#26956,#26957);
#23253=AXIS2_PLACEMENT_3D('',#80441,#26959,#26960);
#23254=AXIS2_PLACEMENT_3D('',#80466,#26962,#26963);
#23255=AXIS2_PLACEMENT_3D('',#80491,#26965,#26966);
#23256=AXIS2_PLACEMENT_3D('',#80515,#26968,#26969);
#23257=AXIS2_PLACEMENT_3D('',#80540,#26971,#26972);
#23258=AXIS2_PLACEMENT_3D('',#80564,#26974,#26975);
#23259=AXIS2_PLACEMENT_3D('',#80589,#26977,#26978);
#23260=AXIS2_PLACEMENT_3D('',#80614,#26980,#26981);
#23261=AXIS2_PLACEMENT_3D('',#80638,#26983,#26984);
#23262=AXIS2_PLACEMENT_3D('',#80649,#26986,#26987);
#23263=AXIS2_PLACEMENT_3D('',#80655,#26988,#26989);
#23264=AXIS2_PLACEMENT_3D('',#80669,#26991,#26992);
#23265=AXIS2_PLACEMENT_3D('',#80679,#26993,#26994);
#23266=AXIS2_PLACEMENT_3D('',#80703,#26996,#26997);
#23267=AXIS2_PLACEMENT_3D('',#80728,#26999,#27000);
#23268=AXIS2_PLACEMENT_3D('',#80752,#27002,#27003);
#23269=AXIS2_PLACEMENT_3D('',#80777,#27005,#27006);
#23270=AXIS2_PLACEMENT_3D('',#80801,#27008,#27009);
#23271=AXIS2_PLACEMENT_3D('',#80826,#27011,#27012);
#23272=AXIS2_PLACEMENT_3D('',#80851,#27014,#27015);
#23273=AXIS2_PLACEMENT_3D('',#80875,#27017,#27018);
#23274=AXIS2_PLACEMENT_3D('',#80900,#27020,#27021);
#23275=AXIS2_PLACEMENT_3D('',#80924,#27023,#27024);
#23276=AXIS2_PLACEMENT_3D('',#80949,#27026,#27027);
#23277=AXIS2_PLACEMENT_3D('',#80974,#27029,#27030);
#23278=AXIS2_PLACEMENT_3D('',#80998,#27032,#27033);
#23279=AXIS2_PLACEMENT_3D('',#81023,#27035,#27036);
#23280=AXIS2_PLACEMENT_3D('',#81047,#27038,#27039);
#23281=AXIS2_PLACEMENT_3D('',#81072,#27041,#27042);
#23282=AXIS2_PLACEMENT_3D('',#81097,#27044,#27045);
#23283=AXIS2_PLACEMENT_3D('',#81121,#27047,#27048);
#23284=AXIS2_PLACEMENT_3D('',#81132,#27050,#27051);
#23285=AXIS2_PLACEMENT_3D('',#81138,#27052,#27053);
#23286=AXIS2_PLACEMENT_3D('',#81152,#27055,#27056);
#23287=AXIS2_PLACEMENT_3D('',#81162,#27057,#27058);
#23288=AXIS2_PLACEMENT_3D('',#81186,#27060,#27061);
#23289=AXIS2_PLACEMENT_3D('',#81211,#27063,#27064);
#23290=AXIS2_PLACEMENT_3D('',#81235,#27066,#27067);
#23291=AXIS2_PLACEMENT_3D('',#81260,#27069,#27070);
#23292=AXIS2_PLACEMENT_3D('',#81284,#27072,#27073);
#23293=AXIS2_PLACEMENT_3D('',#81309,#27075,#27076);
#23294=AXIS2_PLACEMENT_3D('',#81334,#27078,#27079);
#23295=AXIS2_PLACEMENT_3D('',#81358,#27081,#27082);
#23296=AXIS2_PLACEMENT_3D('',#81383,#27084,#27085);
#23297=AXIS2_PLACEMENT_3D('',#81407,#27087,#27088);
#23298=AXIS2_PLACEMENT_3D('',#81432,#27090,#27091);
#23299=AXIS2_PLACEMENT_3D('',#81457,#27093,#27094);
#23300=AXIS2_PLACEMENT_3D('',#81481,#27096,#27097);
#23301=AXIS2_PLACEMENT_3D('',#81506,#27099,#27100);
#23302=AXIS2_PLACEMENT_3D('',#81530,#27102,#27103);
#23303=AXIS2_PLACEMENT_3D('',#81555,#27105,#27106);
#23304=AXIS2_PLACEMENT_3D('',#81580,#27108,#27109);
#23305=AXIS2_PLACEMENT_3D('',#81604,#27111,#27112);
#23306=AXIS2_PLACEMENT_3D('',#81615,#27114,#27115);
#23307=AXIS2_PLACEMENT_3D('',#81621,#27116,#27117);
#23308=AXIS2_PLACEMENT_3D('',#83114,#27118,#27119);
#23309=AXIS2_PLACEMENT_3D('',#84063,#27124,#27125);
#23310=AXIS2_PLACEMENT_3D('',#85368,#27126,#27127);
#23311=AXIS2_PLACEMENT_3D('',#86673,#27128,#27129);
#23312=AXIS2_PLACEMENT_3D('',#87978,#27130,#27131);
#23313=AXIS2_PLACEMENT_3D('',#89283,#27132,#27133);
#23314=AXIS2_PLACEMENT_3D('',#90588,#27134,#27135);
#23315=AXIS2_PLACEMENT_3D('',#90589,#27136,#27137);
#23316=AXIS2_PLACEMENT_3D('',#90590,#27138,#27139);
#23317=AXIS2_PLACEMENT_3D('',#90591,#27140,#27141);
#23318=AXIS2_PLACEMENT_3D('',#90592,#27142,#27143);
#23319=AXIS2_PLACEMENT_3D('',#90593,#27144,#27145);
#23320=AXIS2_PLACEMENT_3D('',#90594,#27146,#27147);
#23321=AXIS2_PLACEMENT_3D('',#90600,#27151,#27152);
#23322=AXIS2_PLACEMENT_3D('',#90604,#27155,#27156);
#23323=AXIS2_PLACEMENT_3D('',#90608,#27159,#27160);
#23324=AXIS2_PLACEMENT_3D('',#90610,#27162,#27163);
#23325=AXIS2_PLACEMENT_3D('',#90611,#27164,#27165);
#23326=AXIS2_PLACEMENT_3D('',#90612,#27166,#27167);
#23327=AXIS2_PLACEMENT_3D('',#90628,#27169,#27170);
#23328=AXIS2_PLACEMENT_3D('',#90636,#27171,#27172);
#23329=AXIS2_PLACEMENT_3D('',#90684,#27174,#27175);
#23330=AXIS2_PLACEMENT_3D('',#90732,#27177,#27178);
#23331=AXIS2_PLACEMENT_3D('',#90780,#27180,#27181);
#23332=AXIS2_PLACEMENT_3D('',#90834,#27183,#27184);
#23333=AXIS2_PLACEMENT_3D('',#90882,#27186,#27187);
#23334=AXIS2_PLACEMENT_3D('',#90930,#27189,#27190);
#23335=AXIS2_PLACEMENT_3D('',#90984,#27192,#27193);
#23336=AXIS2_PLACEMENT_3D('',#91032,#27195,#27196);
#23337=AXIS2_PLACEMENT_3D('',#91080,#27198,#27199);
#23338=AXIS2_PLACEMENT_3D('',#91128,#27201,#27202);
#23339=AXIS2_PLACEMENT_3D('',#91182,#27204,#27205);
#23340=AXIS2_PLACEMENT_3D('',#91230,#27207,#27208);
#23341=AXIS2_PLACEMENT_3D('',#91278,#27210,#27211);
#23342=AXIS2_PLACEMENT_3D('',#91332,#27213,#27214);
#23343=AXIS2_PLACEMENT_3D('',#91380,#27216,#27217);
#23344=AXIS2_PLACEMENT_3D('',#91428,#27219,#27220);
#23345=AXIS2_PLACEMENT_3D('',#91476,#27222,#27223);
#23346=AXIS2_PLACEMENT_3D('',#91530,#27225,#27226);
#23347=AXIS2_PLACEMENT_3D('',#91578,#27228,#27229);
#23348=AXIS2_PLACEMENT_3D('',#91626,#27231,#27232);
#23349=AXIS2_PLACEMENT_3D('',#91680,#27234,#27235);
#23350=AXIS2_PLACEMENT_3D('',#91728,#27237,#27238);
#23351=AXIS2_PLACEMENT_3D('',#91776,#27240,#27241);
#23352=AXIS2_PLACEMENT_3D('',#91824,#27243,#27244);
#23353=AXIS2_PLACEMENT_3D('',#91878,#27246,#27247);
#23354=AXIS2_PLACEMENT_3D('',#91926,#27249,#27250);
#23355=AXIS2_PLACEMENT_3D('',#91974,#27252,#27253);
#23356=AXIS2_PLACEMENT_3D('',#92028,#27255,#27256);
#23357=AXIS2_PLACEMENT_3D('',#92076,#27258,#27259);
#23358=AXIS2_PLACEMENT_3D('',#92124,#27261,#27262);
#23359=AXIS2_PLACEMENT_3D('',#92172,#27264,#27265);
#23360=AXIS2_PLACEMENT_3D('',#92226,#27267,#27268);
#23361=AXIS2_PLACEMENT_3D('',#92274,#27270,#27271);
#23362=AXIS2_PLACEMENT_3D('',#92322,#27273,#27274);
#23363=AXIS2_PLACEMENT_3D('',#92376,#27276,#27277);
#23364=AXIS2_PLACEMENT_3D('',#92424,#27279,#27280);
#23365=AXIS2_PLACEMENT_3D('',#92472,#27282,#27283);
#23366=AXIS2_PLACEMENT_3D('',#92520,#27285,#27286);
#23367=AXIS2_PLACEMENT_3D('',#92574,#27288,#27289);
#23368=AXIS2_PLACEMENT_3D('',#92622,#27291,#27292);
#23369=AXIS2_PLACEMENT_3D('',#92670,#27294,#27295);
#23370=AXIS2_PLACEMENT_3D('',#92724,#27297,#27298);
#23371=AXIS2_PLACEMENT_3D('',#92772,#27300,#27301);
#23372=AXIS2_PLACEMENT_3D('',#92820,#27303,#27304);
#23373=AXIS2_PLACEMENT_3D('',#92868,#27306,#27307);
#23374=AXIS2_PLACEMENT_3D('',#92919,#27309,#27310);
#23375=AXIS2_PLACEMENT_3D('',#92967,#27312,#27313);
#23376=AXIS2_PLACEMENT_3D('',#93015,#27315,#27316);
#23377=AXIS2_PLACEMENT_3D('',#93031,#27318,#27319);
#23378=AXIS2_PLACEMENT_3D('',#93040,#27320,#27321);
#23379=AXIS2_PLACEMENT_3D('',#93065,#27323,#27324);
#23380=AXIS2_PLACEMENT_3D('',#93089,#27326,#27327);
#23381=AXIS2_PLACEMENT_3D('',#93114,#27329,#27330);
#23382=AXIS2_PLACEMENT_3D('',#93139,#27332,#27333);
#23383=AXIS2_PLACEMENT_3D('',#93163,#27335,#27336);
#23384=AXIS2_PLACEMENT_3D('',#93187,#27338,#27339);
#23385=AXIS2_PLACEMENT_3D('',#93212,#27341,#27342);
#23386=AXIS2_PLACEMENT_3D('',#93237,#27344,#27345);
#23387=AXIS2_PLACEMENT_3D('',#93261,#27347,#27348);
#23388=AXIS2_PLACEMENT_3D('',#93286,#27350,#27351);
#23389=AXIS2_PLACEMENT_3D('',#93311,#27353,#27354);
#23390=AXIS2_PLACEMENT_3D('',#93335,#27356,#27357);
#23391=AXIS2_PLACEMENT_3D('',#93359,#27359,#27360);
#23392=AXIS2_PLACEMENT_3D('',#93384,#27362,#27363);
#23393=AXIS2_PLACEMENT_3D('',#93409,#27365,#27366);
#23394=AXIS2_PLACEMENT_3D('',#93433,#27368,#27369);
#23395=AXIS2_PLACEMENT_3D('',#93458,#27371,#27372);
#23396=AXIS2_PLACEMENT_3D('',#93483,#27374,#27375);
#23397=AXIS2_PLACEMENT_3D('',#93507,#27377,#27378);
#23398=AXIS2_PLACEMENT_3D('',#93531,#27380,#27381);
#23399=AXIS2_PLACEMENT_3D('',#93556,#27383,#27384);
#23400=AXIS2_PLACEMENT_3D('',#93581,#27386,#27387);
#23401=AXIS2_PLACEMENT_3D('',#93605,#27389,#27390);
#23402=AXIS2_PLACEMENT_3D('',#93630,#27392,#27393);
#23403=AXIS2_PLACEMENT_3D('',#93655,#27395,#27396);
#23404=AXIS2_PLACEMENT_3D('',#93679,#27398,#27399);
#23405=AXIS2_PLACEMENT_3D('',#93703,#27401,#27402);
#23406=AXIS2_PLACEMENT_3D('',#93728,#27404,#27405);
#23407=AXIS2_PLACEMENT_3D('',#93753,#27407,#27408);
#23408=AXIS2_PLACEMENT_3D('',#93777,#27410,#27411);
#23409=AXIS2_PLACEMENT_3D('',#93802,#27413,#27414);
#23410=AXIS2_PLACEMENT_3D('',#93827,#27416,#27417);
#23411=AXIS2_PLACEMENT_3D('',#93851,#27419,#27420);
#23412=AXIS2_PLACEMENT_3D('',#93875,#27422,#27423);
#23413=AXIS2_PLACEMENT_3D('',#93900,#27425,#27426);
#23414=AXIS2_PLACEMENT_3D('',#93925,#27428,#27429);
#23415=AXIS2_PLACEMENT_3D('',#93949,#27431,#27432);
#23416=AXIS2_PLACEMENT_3D('',#93974,#27434,#27435);
#23417=AXIS2_PLACEMENT_3D('',#93999,#27437,#27438);
#23418=AXIS2_PLACEMENT_3D('',#94023,#27440,#27441);
#23419=AXIS2_PLACEMENT_3D('',#94047,#27443,#27444);
#23420=AXIS2_PLACEMENT_3D('',#94072,#27446,#27447);
#23421=AXIS2_PLACEMENT_3D('',#94097,#27449,#27450);
#23422=AXIS2_PLACEMENT_3D('',#94121,#27452,#27453);
#23423=AXIS2_PLACEMENT_3D('',#94146,#27455,#27456);
#23424=AXIS2_PLACEMENT_3D('',#94171,#27458,#27459);
#23425=AXIS2_PLACEMENT_3D('',#94195,#27461,#27462);
#23426=AXIS2_PLACEMENT_3D('',#94219,#27464,#27465);
#23427=AXIS2_PLACEMENT_3D('',#94507,#27466,#27467);
#23428=AXIS2_PLACEMENT_3D('',#94541,#27469,#27470);
#23429=AXIS2_PLACEMENT_3D('',#95924,#27471,#27472);
#23430=AXIS2_PLACEMENT_3D('',#95935,#27473,#27474);
#23431=AXIS2_PLACEMENT_3D('',#97314,#27475,#27476);
#23432=AXIS2_PLACEMENT_3D('',#97315,#27477,#27478);
#23433=AXIS2_PLACEMENT_3D('',#97324,#27483,#27484);
#23434=AXIS2_PLACEMENT_3D('',#97330,#27488,#27489);
#23435=AXIS2_PLACEMENT_3D('',#97336,#27493,#27494);
#23436=AXIS2_PLACEMENT_3D('',#97342,#27498,#27499);
#23437=AXIS2_PLACEMENT_3D('',#97348,#27503,#27504);
#23438=AXIS2_PLACEMENT_3D('',#97351,#27507,#27508);
#23439=AXIS2_PLACEMENT_3D('',#97352,#27509,#27510);
#23440=AXIS2_PLACEMENT_3D('',#97354,#27511,#27512);
#23441=AXIS2_PLACEMENT_3D('',#97355,#27513,#27514);
#23442=AXIS2_PLACEMENT_3D('',#97358,#27516,#27517);
#23443=AXIS2_PLACEMENT_3D('',#97359,#27518,#27519);
#23444=AXIS2_PLACEMENT_3D('',#97360,#27520,#27521);
#23445=AXIS2_PLACEMENT_3D('',#97361,#27522,#27523);
#23446=AXIS2_PLACEMENT_3D('',#97362,#27524,#27525);
#23447=AXIS2_PLACEMENT_3D('',#97364,#27526,#27527);
#23448=AXIS2_PLACEMENT_3D('',#97367,#27529,#27530);
#23449=AXIS2_PLACEMENT_3D('',#97368,#27531,#27532);
#23450=AXIS2_PLACEMENT_3D('',#97370,#27533,#27534);
#23451=AXIS2_PLACEMENT_3D('',#97373,#27536,#27537);
#23452=AXIS2_PLACEMENT_3D('',#97374,#27538,#27539);
#23453=AXIS2_PLACEMENT_3D('',#97375,#27540,#27541);
#23454=AXIS2_PLACEMENT_3D('',#97376,#27542,#27543);
#23455=AXIS2_PLACEMENT_3D('',#97377,#27544,#27545);
#23456=AXIS2_PLACEMENT_3D('',#97379,#27546,#27547);
#23457=AXIS2_PLACEMENT_3D('',#97382,#27549,#27550);
#23458=AXIS2_PLACEMENT_3D('',#97383,#27551,#27552);
#23459=AXIS2_PLACEMENT_3D('',#97385,#27553,#27554);
#23460=AXIS2_PLACEMENT_3D('',#97388,#27556,#27557);
#23461=AXIS2_PLACEMENT_3D('',#97389,#27558,#27559);
#23462=AXIS2_PLACEMENT_3D('',#97390,#27560,#27561);
#23463=AXIS2_PLACEMENT_3D('',#97391,#27562,#27563);
#23464=AXIS2_PLACEMENT_3D('',#97392,#27564,#27565);
#23465=AXIS2_PLACEMENT_3D('',#97393,#27566,#27567);
#23466=AXIS2_PLACEMENT_3D('',#97394,#27568,#27569);
#23467=AXIS2_PLACEMENT_3D('',#97395,#27570,#27571);
#23468=AXIS2_PLACEMENT_3D('',#97396,#27572,#27573);
#23469=AXIS2_PLACEMENT_3D('',#97397,#27574,#27575);
#23470=AXIS2_PLACEMENT_3D('',#97398,#27576,#27577);
#23471=AXIS2_PLACEMENT_3D('',#97399,#27578,#27579);
#23472=AXIS2_PLACEMENT_3D('',#97400,#27580,#27581);
#23473=AXIS2_PLACEMENT_3D('',#97401,#27582,#27583);
#23474=AXIS2_PLACEMENT_3D('',#97402,#27584,#27585);
#23475=AXIS2_PLACEMENT_3D('',#97403,#27586,#27587);
#23476=AXIS2_PLACEMENT_3D('',#97404,#27588,#27589);
#23477=AXIS2_PLACEMENT_3D('',#97405,#27590,#27591);
#23478=AXIS2_PLACEMENT_3D('',#97406,#27592,#27593);
#23479=AXIS2_PLACEMENT_3D('',#97407,#27594,#27595);
#23480=AXIS2_PLACEMENT_3D('',#97408,#27596,#27597);
#23481=AXIS2_PLACEMENT_3D('',#97409,#27598,#27599);
#23482=AXIS2_PLACEMENT_3D('',#97410,#27600,#27601);
#23483=AXIS2_PLACEMENT_3D('',#97411,#27602,#27603);
#23484=AXIS2_PLACEMENT_3D('',#97412,#27604,#27605);
#23485=AXIS2_PLACEMENT_3D('',#97413,#27606,#27607);
#23486=AXIS2_PLACEMENT_3D('',#97414,#27608,#27609);
#23487=AXIS2_PLACEMENT_3D('',#97415,#27610,#27611);
#23488=AXIS2_PLACEMENT_3D('',#97416,#27612,#27613);
#23489=AXIS2_PLACEMENT_3D('',#97417,#27614,#27615);
#23490=AXIS2_PLACEMENT_3D('',#97418,#27616,#27617);
#23491=AXIS2_PLACEMENT_3D('',#97419,#27618,#27619);
#23492=AXIS2_PLACEMENT_3D('',#97420,#27620,#27621);
#23493=AXIS2_PLACEMENT_3D('',#97421,#27622,#27623);
#23494=AXIS2_PLACEMENT_3D('',#97422,#27624,#27625);
#23495=AXIS2_PLACEMENT_3D('',#97423,#27626,#27627);
#23496=AXIS2_PLACEMENT_3D('',#97424,#27628,#27629);
#23497=AXIS2_PLACEMENT_3D('',#97425,#27630,#27631);
#23498=AXIS2_PLACEMENT_3D('',#97426,#27632,#27633);
#23499=AXIS2_PLACEMENT_3D('',#97427,#27634,#27635);
#23500=AXIS2_PLACEMENT_3D('',#97428,#27636,#27637);
#23501=AXIS2_PLACEMENT_3D('',#97429,#27638,#27639);
#23502=DIRECTION('axis',(0.,0.,1.));
#23503=DIRECTION('refdir',(1.,0.,0.));
#23504=DIRECTION('axis',(0.,0.,1.));
#23505=DIRECTION('refdir',(1.,0.,0.));
#23506=DIRECTION('axis',(0.,0.,1.));
#23507=DIRECTION('refdir',(1.,0.,0.));
#23508=DIRECTION('center_axis',(-1.,0.,0.));
#23509=DIRECTION('ref_axis',(0.,1.,0.));
#23510=DIRECTION('center_axis',(-1.,0.,0.));
#23511=DIRECTION('ref_axis',(0.,1.,0.));
#23512=DIRECTION('',(-1.,0.,0.));
#23513=DIRECTION('center_axis',(1.,0.,0.));
#23514=DIRECTION('ref_axis',(0.,1.,0.));
#23515=DIRECTION('center_axis',(-1.,0.,0.));
#23516=DIRECTION('ref_axis',(0.,1.,0.));
#23517=DIRECTION('center_axis',(-1.,0.,0.));
#23518=DIRECTION('ref_axis',(0.,1.,0.));
#23519=DIRECTION('',(-1.,0.,0.));
#23520=DIRECTION('center_axis',(1.,0.,0.));
#23521=DIRECTION('ref_axis',(0.,1.,0.));
#23522=DIRECTION('center_axis',(-1.,0.,0.));
#23523=DIRECTION('ref_axis',(0.,1.,0.));
#23524=DIRECTION('center_axis',(-1.,0.,0.));
#23525=DIRECTION('ref_axis',(0.,1.,0.));
#23526=DIRECTION('',(-1.,0.,0.));
#23527=DIRECTION('center_axis',(1.,0.,0.));
#23528=DIRECTION('ref_axis',(0.,1.,0.));
#23529=DIRECTION('center_axis',(-1.,0.,0.));
#23530=DIRECTION('ref_axis',(0.,1.,0.));
#23531=DIRECTION('center_axis',(-1.,0.,0.));
#23532=DIRECTION('ref_axis',(0.,1.,0.));
#23533=DIRECTION('',(-1.,0.,0.));
#23534=DIRECTION('center_axis',(1.,0.,0.));
#23535=DIRECTION('ref_axis',(0.,1.,0.));
#23536=DIRECTION('center_axis',(-1.,0.,0.));
#23537=DIRECTION('ref_axis',(0.,1.,0.));
#23538=DIRECTION('center_axis',(-1.,0.,0.));
#23539=DIRECTION('ref_axis',(0.,1.,0.));
#23540=DIRECTION('',(-1.,0.,0.));
#23541=DIRECTION('center_axis',(1.,0.,0.));
#23542=DIRECTION('ref_axis',(0.,1.,0.));
#23543=DIRECTION('center_axis',(-1.,0.,0.));
#23544=DIRECTION('ref_axis',(0.,1.,0.));
#23545=DIRECTION('center_axis',(-1.,0.,0.));
#23546=DIRECTION('ref_axis',(0.,1.,0.));
#23547=DIRECTION('',(-1.,0.,0.));
#23548=DIRECTION('center_axis',(1.,0.,0.));
#23549=DIRECTION('ref_axis',(0.,1.,0.));
#23550=DIRECTION('center_axis',(0.,1.,0.));
#23551=DIRECTION('ref_axis',(-1.,0.,0.));
#23552=DIRECTION('',(-1.,0.,0.));
#23553=DIRECTION('',(0.,0.,1.));
#23554=DIRECTION('',(-1.,0.,0.));
#23555=DIRECTION('',(0.,0.,1.));
#23556=DIRECTION('center_axis',(-1.,0.,0.));
#23557=DIRECTION('ref_axis',(0.,-1.,0.));
#23558=DIRECTION('',(0.,-1.,0.));
#23559=DIRECTION('',(0.,-1.,0.));
#23560=DIRECTION('',(0.,0.,1.));
#23561=DIRECTION('center_axis',(0.,-1.,0.));
#23562=DIRECTION('ref_axis',(1.,0.,0.));
#23563=DIRECTION('',(1.,0.,0.));
#23564=DIRECTION('',(1.,0.,0.));
#23565=DIRECTION('',(0.,0.,1.));
#23566=DIRECTION('center_axis',(1.,0.,0.));
#23567=DIRECTION('ref_axis',(0.,1.,0.));
#23568=DIRECTION('',(0.,1.,0.));
#23569=DIRECTION('',(0.,1.,0.));
#23570=DIRECTION('center_axis',(0.,1.,0.));
#23571=DIRECTION('ref_axis',(-1.,0.,0.));
#23572=DIRECTION('',(-1.,0.,0.));
#23573=DIRECTION('',(0.,0.,1.));
#23574=DIRECTION('',(-1.,0.,0.));
#23575=DIRECTION('',(0.,0.,1.));
#23576=DIRECTION('center_axis',(1.,0.,0.));
#23577=DIRECTION('ref_axis',(0.,1.,0.));
#23578=DIRECTION('',(0.,1.,0.));
#23579=DIRECTION('',(0.,1.,0.));
#23580=DIRECTION('',(0.,0.,1.));
#23581=DIRECTION('center_axis',(0.,-1.,0.));
#23582=DIRECTION('ref_axis',(1.,0.,0.));
#23583=DIRECTION('',(1.,0.,0.));
#23584=DIRECTION('',(1.,0.,0.));
#23585=DIRECTION('',(0.,0.,1.));
#23586=DIRECTION('center_axis',(-1.,0.,0.));
#23587=DIRECTION('ref_axis',(0.,-1.,0.));
#23588=DIRECTION('',(0.,-1.,0.));
#23589=DIRECTION('',(0.,-1.,0.));
#23590=DIRECTION('center_axis',(0.,0.,1.));
#23591=DIRECTION('ref_axis',(1.,0.,0.));
#23592=DIRECTION('center_axis',(0.,0.,1.));
#23593=DIRECTION('ref_axis',(1.,0.,0.));
#23594=DIRECTION('axis',(0.,0.,1.));
#23595=DIRECTION('refdir',(1.,0.,0.));
#23596=DIRECTION('center_axis',(0.,1.,0.));
#23597=DIRECTION('ref_axis',(-1.,0.,0.));
#23598=DIRECTION('',(-1.,0.,0.));
#23599=DIRECTION('',(0.,0.,1.));
#23600=DIRECTION('',(-1.,0.,0.));
#23601=DIRECTION('',(0.,0.,1.));
#23602=DIRECTION('center_axis',(-1.,0.,0.));
#23603=DIRECTION('ref_axis',(0.,-1.,0.));
#23604=DIRECTION('',(0.,-1.,0.));
#23605=DIRECTION('',(0.,-1.,0.));
#23606=DIRECTION('',(0.,0.,1.));
#23607=DIRECTION('center_axis',(0.,-1.,0.));
#23608=DIRECTION('ref_axis',(1.,0.,0.));
#23609=DIRECTION('',(1.,0.,0.));
#23610=DIRECTION('',(1.,0.,0.));
#23611=DIRECTION('',(0.,0.,1.));
#23612=DIRECTION('center_axis',(1.,0.,0.));
#23613=DIRECTION('ref_axis',(0.,1.,0.));
#23614=DIRECTION('',(0.,1.,0.));
#23615=DIRECTION('',(0.,1.,0.));
#23616=DIRECTION('center_axis',(0.,1.,0.));
#23617=DIRECTION('ref_axis',(-1.,0.,0.));
#23618=DIRECTION('',(-1.,0.,0.));
#23619=DIRECTION('',(0.,0.,1.));
#23620=DIRECTION('',(-1.,0.,0.));
#23621=DIRECTION('',(0.,0.,1.));
#23622=DIRECTION('center_axis',(1.,0.,0.));
#23623=DIRECTION('ref_axis',(0.,1.,0.));
#23624=DIRECTION('',(0.,1.,0.));
#23625=DIRECTION('',(0.,1.,0.));
#23626=DIRECTION('',(0.,0.,1.));
#23627=DIRECTION('center_axis',(0.,-1.,0.));
#23628=DIRECTION('ref_axis',(1.,0.,0.));
#23629=DIRECTION('',(1.,0.,0.));
#23630=DIRECTION('',(1.,0.,0.));
#23631=DIRECTION('',(0.,0.,1.));
#23632=DIRECTION('center_axis',(-1.,0.,0.));
#23633=DIRECTION('ref_axis',(0.,-1.,0.));
#23634=DIRECTION('',(0.,-1.,0.));
#23635=DIRECTION('',(0.,-1.,0.));
#23636=DIRECTION('center_axis',(0.,0.,1.));
#23637=DIRECTION('ref_axis',(1.,0.,0.));
#23638=DIRECTION('center_axis',(0.,0.,1.));
#23639=DIRECTION('ref_axis',(1.,0.,0.));
#23640=DIRECTION('axis',(0.,0.,1.));
#23641=DIRECTION('refdir',(1.,0.,0.));
#23642=DIRECTION('center_axis',(0.,0.,-1.));
#23643=DIRECTION('ref_axis',(-0.34687556303371,0.9379111598494,0.));
#23644=DIRECTION('',(0.,0.,-1.));
#23645=DIRECTION('center_axis',(0.,0.,-1.));
#23646=DIRECTION('ref_axis',(1.,0.,0.));
#23647=DIRECTION('center_axis',(0.,0.,-1.));
#23648=DIRECTION('ref_axis',(1.,0.,0.));
#23649=DIRECTION('',(0.,0.,-1.));
#23650=DIRECTION('center_axis',(0.,0.,-1.));
#23651=DIRECTION('ref_axis',(1.,0.,0.));
#23652=DIRECTION('',(0.,0.,-1.));
#23653=DIRECTION('center_axis',(0.,0.,-1.));
#23654=DIRECTION('ref_axis',(1.,0.,0.));
#23655=DIRECTION('',(0.,0.,-1.));
#23656=DIRECTION('center_axis',(0.,0.,-1.));
#23657=DIRECTION('ref_axis',(1.,0.,0.));
#23658=DIRECTION('',(0.,0.,-1.));
#23659=DIRECTION('center_axis',(0.,0.,-1.));
#23660=DIRECTION('ref_axis',(1.,0.,0.));
#23661=DIRECTION('',(0.,0.,-1.));
#23662=DIRECTION('center_axis',(0.,0.,-1.));
#23663=DIRECTION('ref_axis',(1.,0.,0.));
#23664=DIRECTION('',(0.,0.,-1.));
#23665=DIRECTION('center_axis',(0.,0.,-1.));
#23666=DIRECTION('ref_axis',(0.938001830644068,-0.346630301197656,0.));
#23667=DIRECTION('',(0.,0.,-1.));
#23668=DIRECTION('center_axis',(0.,0.,-1.));
#23669=DIRECTION('ref_axis',(1.,0.,0.));
#23670=DIRECTION('center_axis',(0.,0.,-1.));
#23671=DIRECTION('ref_axis',(-0.346875820911814,0.937911064476134,0.));
#23672=DIRECTION('',(0.,0.,-1.));
#23673=DIRECTION('center_axis',(0.,0.,-1.));
#23674=DIRECTION('ref_axis',(1.,0.,0.));
#23675=DIRECTION('center_axis',(0.,0.,-1.));
#23676=DIRECTION('ref_axis',(1.,0.,0.));
#23677=DIRECTION('',(0.,0.,-1.));
#23678=DIRECTION('center_axis',(0.,0.,-1.));
#23679=DIRECTION('ref_axis',(1.,0.,0.));
#23680=DIRECTION('',(0.,0.,-1.));
#23681=DIRECTION('center_axis',(0.,0.,-1.));
#23682=DIRECTION('ref_axis',(1.,0.,0.));
#23683=DIRECTION('',(0.,0.,-1.));
#23684=DIRECTION('center_axis',(0.,0.,-1.));
#23685=DIRECTION('ref_axis',(1.,0.,0.));
#23686=DIRECTION('',(0.,0.,-1.));
#23687=DIRECTION('center_axis',(0.,0.,-1.));
#23688=DIRECTION('ref_axis',(1.,0.,0.));
#23689=DIRECTION('',(0.,0.,-1.));
#23690=DIRECTION('center_axis',(0.,0.,-1.));
#23691=DIRECTION('ref_axis',(1.,0.,0.));
#23692=DIRECTION('',(0.,0.,-1.));
#23693=DIRECTION('center_axis',(0.,0.,-1.));
#23694=DIRECTION('ref_axis',(0.938001844837498,-0.346630262789403,0.));
#23695=DIRECTION('',(0.,0.,-1.));
#23696=DIRECTION('center_axis',(0.,0.,-1.));
#23697=DIRECTION('ref_axis',(1.,0.,0.));
#23698=DIRECTION('center_axis',(0.,0.,-1.));
#23699=DIRECTION('ref_axis',(-0.346875921807931,0.937911027160838,0.));
#23700=DIRECTION('',(0.,0.,-1.));
#23701=DIRECTION('center_axis',(0.,0.,-1.));
#23702=DIRECTION('ref_axis',(1.,0.,0.));
#23703=DIRECTION('center_axis',(0.,0.,-1.));
#23704=DIRECTION('ref_axis',(1.,0.,0.));
#23705=DIRECTION('',(0.,0.,-1.));
#23706=DIRECTION('center_axis',(0.,0.,-1.));
#23707=DIRECTION('ref_axis',(1.,0.,0.));
#23708=DIRECTION('',(0.,0.,-1.));
#23709=DIRECTION('center_axis',(0.,0.,-1.));
#23710=DIRECTION('ref_axis',(1.,0.,0.));
#23711=DIRECTION('',(0.,0.,-1.));
#23712=DIRECTION('center_axis',(0.,0.,-1.));
#23713=DIRECTION('ref_axis',(1.,0.,0.));
#23714=DIRECTION('',(0.,0.,-1.));
#23715=DIRECTION('center_axis',(0.,0.,-1.));
#23716=DIRECTION('ref_axis',(1.,0.,0.));
#23717=DIRECTION('',(0.,0.,-1.));
#23718=DIRECTION('center_axis',(0.,0.,-1.));
#23719=DIRECTION('ref_axis',(1.,0.,0.));
#23720=DIRECTION('',(0.,0.,-1.));
#23721=DIRECTION('center_axis',(0.,0.,-1.));
#23722=DIRECTION('ref_axis',(0.93800185687022,-0.346630230228148,0.));
#23723=DIRECTION('',(0.,0.,-1.));
#23724=DIRECTION('center_axis',(0.,0.,-1.));
#23725=DIRECTION('ref_axis',(1.,0.,0.));
#23726=DIRECTION('center_axis',(0.,0.,-1.));
#23727=DIRECTION('ref_axis',(-0.346875444642522,0.937911203634999,0.));
#23728=DIRECTION('',(0.,0.,-1.));
#23729=DIRECTION('center_axis',(0.,0.,-1.));
#23730=DIRECTION('ref_axis',(1.,0.,0.));
#23731=DIRECTION('center_axis',(0.,0.,-1.));
#23732=DIRECTION('ref_axis',(1.,0.,0.));
#23733=DIRECTION('',(0.,0.,-1.));
#23734=DIRECTION('center_axis',(0.,0.,-1.));
#23735=DIRECTION('ref_axis',(1.,0.,0.));
#23736=DIRECTION('',(0.,0.,-1.));
#23737=DIRECTION('center_axis',(0.,0.,-1.));
#23738=DIRECTION('ref_axis',(1.,0.,0.));
#23739=DIRECTION('',(0.,0.,-1.));
#23740=DIRECTION('center_axis',(0.,0.,-1.));
#23741=DIRECTION('ref_axis',(1.,0.,0.));
#23742=DIRECTION('',(0.,0.,-1.));
#23743=DIRECTION('center_axis',(0.,0.,-1.));
#23744=DIRECTION('ref_axis',(1.,0.,0.));
#23745=DIRECTION('',(0.,0.,-1.));
#23746=DIRECTION('center_axis',(0.,0.,-1.));
#23747=DIRECTION('ref_axis',(1.,0.,0.));
#23748=DIRECTION('',(0.,0.,-1.));
#23749=DIRECTION('center_axis',(0.,0.,-1.));
#23750=DIRECTION('ref_axis',(0.938001817986921,-0.346630335448631,0.));
#23751=DIRECTION('',(0.,0.,-1.));
#23752=DIRECTION('center_axis',(0.,0.,-1.));
#23753=DIRECTION('ref_axis',(1.,0.,0.));
#23754=DIRECTION('center_axis',(0.,0.,-1.));
#23755=DIRECTION('ref_axis',(0.793238775227928,0.608910704023913,0.));
#23756=DIRECTION('',(1.22464679914735E-16,-2.81870473344804E-30,-1.));
#23757=DIRECTION('center_axis',(0.,0.,1.));
#23758=DIRECTION('ref_axis',(1.,-2.28940061540476E-14,0.));
#23759=DIRECTION('center_axis',(0.,0.,-1.));
#23760=DIRECTION('ref_axis',(1.,-2.28940061540476E-14,0.));
#23761=DIRECTION('',(1.22464679914735E-16,-2.81870473344804E-30,-1.));
#23762=DIRECTION('center_axis',(0.,0.,-1.));
#23763=DIRECTION('ref_axis',(1.,-2.28940061540476E-14,0.));
#23764=DIRECTION('',(1.22464679914735E-16,-2.81870473344804E-30,-1.));
#23765=DIRECTION('center_axis',(0.,0.,-1.));
#23766=DIRECTION('ref_axis',(1.,-2.28940061540476E-14,0.));
#23767=DIRECTION('',(1.22464679914735E-16,-2.81870473344804E-30,-1.));
#23768=DIRECTION('center_axis',(0.,0.,-1.));
#23769=DIRECTION('ref_axis',(1.,-2.28940061540476E-14,0.));
#23770=DIRECTION('',(1.22464679914735E-16,-2.81870473344804E-30,-1.));
#23771=DIRECTION('center_axis',(0.,0.,-1.));
#23772=DIRECTION('ref_axis',(1.,-2.28940061540476E-14,0.));
#23773=DIRECTION('',(1.22464679914735E-16,-2.81870473344804E-30,-1.));
#23774=DIRECTION('center_axis',(0.,0.,-1.));
#23775=DIRECTION('ref_axis',(1.,-2.28940061540476E-14,0.));
#23776=DIRECTION('',(1.22464679914735E-16,-2.81870473344804E-30,-1.));
#23777=DIRECTION('center_axis',(0.,0.,-1.));
#23778=DIRECTION('ref_axis',(-0.609093973761813,-0.793098058960582,0.));
#23779=DIRECTION('',(1.22464679914735E-16,-2.81870473344804E-30,-1.));
#23780=DIRECTION('center_axis',(0.,0.,-1.));
#23781=DIRECTION('ref_axis',(1.,-2.28940061540476E-14,0.));
#23782=DIRECTION('center_axis',(0.,0.,-1.));
#23783=DIRECTION('ref_axis',(0.79323871288191,0.608910785243167,0.));
#23784=DIRECTION('',(1.22464679914735E-16,-2.55168500624601E-30,-1.));
#23785=DIRECTION('center_axis',(0.,0.,1.));
#23786=DIRECTION('ref_axis',(1.,-2.0713624615567E-14,0.));
#23787=DIRECTION('center_axis',(0.,0.,-1.));
#23788=DIRECTION('ref_axis',(1.,-2.0713624615567E-14,0.));
#23789=DIRECTION('',(1.22464679914735E-16,-2.55168500624601E-30,-1.));
#23790=DIRECTION('center_axis',(0.,0.,-1.));
#23791=DIRECTION('ref_axis',(1.,-2.0713624615567E-14,0.));
#23792=DIRECTION('',(1.22464679914735E-16,-2.55168500624601E-30,-1.));
#23793=DIRECTION('center_axis',(0.,0.,-1.));
#23794=DIRECTION('ref_axis',(1.,-2.0713624615567E-14,0.));
#23795=DIRECTION('',(1.22464679914735E-16,-2.55168500624601E-30,-1.));
#23796=DIRECTION('center_axis',(0.,0.,-1.));
#23797=DIRECTION('ref_axis',(1.,-2.0713624615567E-14,0.));
#23798=DIRECTION('',(1.22464679914735E-16,-2.55168500624601E-30,-1.));
#23799=DIRECTION('center_axis',(0.,0.,-1.));
#23800=DIRECTION('ref_axis',(1.,-2.0713624615567E-14,0.));
#23801=DIRECTION('',(1.22464679914735E-16,-2.55168500624601E-30,-1.));
#23802=DIRECTION('center_axis',(0.,0.,-1.));
#23803=DIRECTION('ref_axis',(1.,-2.0713624615567E-14,0.));
#23804=DIRECTION('',(1.22464679914735E-16,-2.55168500624601E-30,-1.));
#23805=DIRECTION('center_axis',(0.,0.,-1.));
#23806=DIRECTION('ref_axis',(-0.609093936537935,-0.793098087548269,0.));
#23807=DIRECTION('',(1.22464679914735E-16,-2.55168500624601E-30,-1.));
#23808=DIRECTION('center_axis',(0.,0.,-1.));
#23809=DIRECTION('ref_axis',(1.,-2.0713624615567E-14,0.));
#23810=DIRECTION('center_axis',(0.,0.,-1.));
#23811=DIRECTION('ref_axis',(0.793238788726965,0.608910686438477,0.));
#23812=DIRECTION('',(1.22464679914735E-16,-2.55168500624601E-30,-1.));
#23813=DIRECTION('center_axis',(0.,0.,1.));
#23814=DIRECTION('ref_axis',(1.,-2.0713624615567E-14,0.));
#23815=DIRECTION('center_axis',(0.,0.,-1.));
#23816=DIRECTION('ref_axis',(1.,-2.0713624615567E-14,0.));
#23817=DIRECTION('',(1.22464679914735E-16,-2.55168500624601E-30,-1.));
#23818=DIRECTION('center_axis',(0.,0.,-1.));
#23819=DIRECTION('ref_axis',(1.,-2.0713624615567E-14,0.));
#23820=DIRECTION('',(1.22464679914735E-16,-2.55168500624601E-30,-1.));
#23821=DIRECTION('center_axis',(0.,0.,-1.));
#23822=DIRECTION('ref_axis',(1.,-2.0713624615567E-14,0.));
#23823=DIRECTION('',(1.22464679914735E-16,-2.55168500624601E-30,-1.));
#23824=DIRECTION('center_axis',(0.,0.,-1.));
#23825=DIRECTION('ref_axis',(1.,-2.0713624615567E-14,0.));
#23826=DIRECTION('',(1.22464679914735E-16,-2.55168500624601E-30,-1.));
#23827=DIRECTION('center_axis',(0.,0.,-1.));
#23828=DIRECTION('ref_axis',(1.,-2.0713624615567E-14,0.));
#23829=DIRECTION('',(1.22464679914735E-16,-2.55168500624601E-30,-1.));
#23830=DIRECTION('center_axis',(0.,0.,-1.));
#23831=DIRECTION('ref_axis',(1.,-2.0713624615567E-14,0.));
#23832=DIRECTION('',(1.22464679914735E-16,-2.55168500624601E-30,-1.));
#23833=DIRECTION('center_axis',(0.,0.,-1.));
#23834=DIRECTION('ref_axis',(-0.609093953553475,-0.79309807448045,0.));
#23835=DIRECTION('',(1.22464679914735E-16,-2.55168500624601E-30,-1.));
#23836=DIRECTION('center_axis',(0.,0.,-1.));
#23837=DIRECTION('ref_axis',(1.,-2.0713624615567E-14,0.));
#23838=DIRECTION('center_axis',(0.,0.,-1.));
#23839=DIRECTION('ref_axis',(0.793238729919907,0.608910763047471,0.));
#23840=DIRECTION('',(1.22464679914735E-16,-2.551685006246E-30,-1.));
#23841=DIRECTION('center_axis',(0.,0.,1.));
#23842=DIRECTION('ref_axis',(1.,-2.07136246155669E-14,0.));
#23843=DIRECTION('center_axis',(0.,0.,-1.));
#23844=DIRECTION('ref_axis',(1.,-2.07136246155669E-14,0.));
#23845=DIRECTION('',(1.22464679914735E-16,-2.551685006246E-30,-1.));
#23846=DIRECTION('center_axis',(0.,0.,-1.));
#23847=DIRECTION('ref_axis',(1.,-2.07136246155669E-14,0.));
#23848=DIRECTION('',(1.22464679914735E-16,-2.551685006246E-30,-1.));
#23849=DIRECTION('center_axis',(0.,0.,-1.));
#23850=DIRECTION('ref_axis',(1.,-2.07136246155669E-14,0.));
#23851=DIRECTION('',(1.22464679914735E-16,-2.551685006246E-30,-1.));
#23852=DIRECTION('center_axis',(0.,0.,-1.));
#23853=DIRECTION('ref_axis',(1.,-2.07136246155669E-14,0.));
#23854=DIRECTION('',(1.22464679914735E-16,-2.551685006246E-30,-1.));
#23855=DIRECTION('center_axis',(0.,0.,-1.));
#23856=DIRECTION('ref_axis',(1.,-2.07136246155669E-14,0.));
#23857=DIRECTION('',(1.22464679914735E-16,-2.551685006246E-30,-1.));
#23858=DIRECTION('center_axis',(0.,0.,-1.));
#23859=DIRECTION('ref_axis',(1.,-2.07136246155669E-14,0.));
#23860=DIRECTION('',(1.22464679914735E-16,-2.551685006246E-30,-1.));
#23861=DIRECTION('center_axis',(0.,0.,-1.));
#23862=DIRECTION('ref_axis',(-0.609093922666122,-0.793098098201727,0.));
#23863=DIRECTION('',(1.22464679914735E-16,-2.551685006246E-30,-1.));
#23864=DIRECTION('center_axis',(0.,0.,-1.));
#23865=DIRECTION('ref_axis',(1.,-2.07136246155669E-14,0.));
#23866=DIRECTION('center_axis',(0.,0.,-1.));
#23867=DIRECTION('ref_axis',(1.,-2.07136246155669E-14,0.));
#23868=DIRECTION('center_axis',(0.,0.,1.));
#23869=DIRECTION('ref_axis',(1.,0.,0.));
#23870=DIRECTION('',(0.,-1.,0.));
#23871=DIRECTION('',(1.,0.,0.));
#23872=DIRECTION('',(0.,1.,0.));
#23873=DIRECTION('',(-1.,0.,0.));
#23874=DIRECTION('center_axis',(0.,0.,-1.));
#23875=DIRECTION('ref_axis',(1.,-2.0713624615567E-14,0.));
#23876=DIRECTION('center_axis',(0.,0.,-1.));
#23877=DIRECTION('ref_axis',(1.,-2.0713624615567E-14,0.));
#23878=DIRECTION('center_axis',(0.,0.,-1.));
#23879=DIRECTION('ref_axis',(1.,-2.28940061540476E-14,0.));
#23880=DIRECTION('center_axis',(0.,0.,-1.));
#23881=DIRECTION('ref_axis',(1.,0.,0.));
#23882=DIRECTION('center_axis',(0.,0.,-1.));
#23883=DIRECTION('ref_axis',(1.,0.,0.));
#23884=DIRECTION('center_axis',(0.,0.,-1.));
#23885=DIRECTION('ref_axis',(1.,0.,0.));
#23886=DIRECTION('center_axis',(0.,0.,-1.));
#23887=DIRECTION('ref_axis',(1.,0.,0.));
#23888=DIRECTION('center_axis',(0.,1.,0.));
#23889=DIRECTION('ref_axis',(-1.,0.,0.));
#23890=DIRECTION('',(-1.,0.,0.));
#23891=DIRECTION('',(0.,0.,1.));
#23892=DIRECTION('',(0.,0.,1.));
#23893=DIRECTION('center_axis',(1.,0.,0.));
#23894=DIRECTION('ref_axis',(0.,1.,0.));
#23895=DIRECTION('',(0.,1.,0.));
#23896=DIRECTION('',(0.,0.,1.));
#23897=DIRECTION('center_axis',(0.,-1.,0.));
#23898=DIRECTION('ref_axis',(1.,0.,0.));
#23899=DIRECTION('',(1.,0.,0.));
#23900=DIRECTION('',(0.,0.,1.));
#23901=DIRECTION('center_axis',(-1.,0.,0.));
#23902=DIRECTION('ref_axis',(0.,-1.,0.));
#23903=DIRECTION('',(0.,-1.,0.));
#23904=DIRECTION('center_axis',(0.,0.,1.));
#23905=DIRECTION('ref_axis',(1.,0.,0.));
#23906=DIRECTION('axis',(0.,0.,1.));
#23907=DIRECTION('refdir',(1.,0.,0.));
#23908=DIRECTION('center_axis',(0.,0.,1.));
#23909=DIRECTION('ref_axis',(1.,0.,0.));
#23910=DIRECTION('',(0.,0.,-1.));
#23911=DIRECTION('center_axis',(0.,0.,-1.));
#23912=DIRECTION('ref_axis',(1.,0.,0.));
#23913=DIRECTION('center_axis',(0.,0.,1.));
#23914=DIRECTION('ref_axis',(1.,0.,0.));
#23915=DIRECTION('',(0.,0.,-1.));
#23916=DIRECTION('center_axis',(0.,0.,1.));
#23917=DIRECTION('ref_axis',(1.,0.,0.));
#23918=DIRECTION('',(0.,0.,-1.));
#23919=DIRECTION('center_axis',(0.,0.,1.));
#23920=DIRECTION('ref_axis',(1.,0.,0.));
#23921=DIRECTION('',(0.,0.,-1.));
#23922=DIRECTION('center_axis',(0.,0.,1.));
#23923=DIRECTION('ref_axis',(1.,0.,0.));
#23924=DIRECTION('',(0.,0.,-1.));
#23925=DIRECTION('center_axis',(0.,0.,1.));
#23926=DIRECTION('ref_axis',(1.,0.,0.));
#23927=DIRECTION('',(0.,0.,-1.));
#23928=DIRECTION('center_axis',(0.,0.,1.));
#23929=DIRECTION('ref_axis',(1.,0.,0.));
#23930=DIRECTION('',(0.,0.,-1.));
#23931=DIRECTION('center_axis',(0.,0.,1.));
#23932=DIRECTION('ref_axis',(1.,0.,0.));
#23933=DIRECTION('',(0.,0.,-1.));
#23934=DIRECTION('center_axis',(0.,0.,1.));
#23935=DIRECTION('ref_axis',(1.,0.,0.));
#23936=DIRECTION('',(0.,0.,-1.));
#23937=DIRECTION('center_axis',(0.,0.,1.));
#23938=DIRECTION('ref_axis',(1.,0.,0.));
#23939=DIRECTION('',(0.,0.,-1.));
#23940=DIRECTION('center_axis',(0.,0.,1.));
#23941=DIRECTION('ref_axis',(1.,0.,0.));
#23942=DIRECTION('',(0.,0.,-1.));
#23943=DIRECTION('center_axis',(0.,0.,1.));
#23944=DIRECTION('ref_axis',(1.,0.,0.));
#23945=DIRECTION('',(0.,0.,-1.));
#23946=DIRECTION('center_axis',(0.,0.,1.));
#23947=DIRECTION('ref_axis',(1.,0.,0.));
#23948=DIRECTION('',(0.,0.,-1.));
#23949=DIRECTION('center_axis',(0.,0.,1.));
#23950=DIRECTION('ref_axis',(1.,0.,0.));
#23951=DIRECTION('',(0.,0.,-1.));
#23952=DIRECTION('center_axis',(0.,0.,1.));
#23953=DIRECTION('ref_axis',(1.,0.,0.));
#23954=DIRECTION('',(0.,0.,-1.));
#23955=DIRECTION('center_axis',(0.,0.,1.));
#23956=DIRECTION('ref_axis',(1.,0.,0.));
#23957=DIRECTION('',(0.,0.,-1.));
#23958=DIRECTION('center_axis',(0.,0.,1.));
#23959=DIRECTION('ref_axis',(1.,0.,0.));
#23960=DIRECTION('',(0.,0.,-1.));
#23961=DIRECTION('center_axis',(0.,0.,1.));
#23962=DIRECTION('ref_axis',(1.,0.,0.));
#23963=DIRECTION('',(0.,0.,-1.));
#23964=DIRECTION('center_axis',(0.,0.,1.));
#23965=DIRECTION('ref_axis',(1.,0.,0.));
#23966=DIRECTION('',(0.,0.,-1.));
#23967=DIRECTION('center_axis',(0.,0.,1.));
#23968=DIRECTION('ref_axis',(1.,0.,0.));
#23969=DIRECTION('',(0.,0.,-1.));
#23970=DIRECTION('center_axis',(0.,0.,1.));
#23971=DIRECTION('ref_axis',(1.,0.,0.));
#23972=DIRECTION('',(0.,0.,-1.));
#23973=DIRECTION('center_axis',(0.,0.,1.));
#23974=DIRECTION('ref_axis',(1.,0.,0.));
#23975=DIRECTION('',(0.,0.,-1.));
#23976=DIRECTION('center_axis',(0.,0.,1.));
#23977=DIRECTION('ref_axis',(1.,0.,0.));
#23978=DIRECTION('',(0.,0.,-1.));
#23979=DIRECTION('center_axis',(0.,0.,1.));
#23980=DIRECTION('ref_axis',(1.,0.,0.));
#23981=DIRECTION('',(0.,0.,-1.));
#23982=DIRECTION('center_axis',(0.,0.,1.));
#23983=DIRECTION('ref_axis',(0.997333825498281,-0.0729742455731076,0.));
#23984=DIRECTION('',(0.,0.,1.));
#23985=DIRECTION('center_axis',(0.,0.,-1.));
#23986=DIRECTION('ref_axis',(1.,-6.20171864138877E-14,0.));
#23987=DIRECTION('center_axis',(0.,0.,1.));
#23988=DIRECTION('ref_axis',(1.,-6.20171864138877E-14,0.));
#23989=DIRECTION('',(0.,0.,1.));
#23990=DIRECTION('center_axis',(0.,0.,1.));
#23991=DIRECTION('ref_axis',(1.,-6.20171864138877E-14,0.));
#23992=DIRECTION('',(0.,0.,1.));
#23993=DIRECTION('center_axis',(0.,0.,1.));
#23994=DIRECTION('ref_axis',(1.,-6.20171864138877E-14,0.));
#23995=DIRECTION('',(0.,0.,1.));
#23996=DIRECTION('center_axis',(0.,0.,1.));
#23997=DIRECTION('ref_axis',(1.,-6.20171864138877E-14,0.));
#23998=DIRECTION('',(0.,0.,1.));
#23999=DIRECTION('center_axis',(0.,0.,1.));
#24000=DIRECTION('ref_axis',(1.,-6.20171864138877E-14,0.));
#24001=DIRECTION('',(0.,0.,1.));
#24002=DIRECTION('center_axis',(0.,0.,1.));
#24003=DIRECTION('ref_axis',(1.,-6.20171864138877E-14,0.));
#24004=DIRECTION('',(0.,0.,1.));
#24005=DIRECTION('center_axis',(0.,0.,1.));
#24006=DIRECTION('ref_axis',(1.,-6.20171864138877E-14,0.));
#24007=DIRECTION('',(0.,0.,1.));
#24008=DIRECTION('center_axis',(0.,0.,1.));
#24009=DIRECTION('ref_axis',(1.,-6.20171864138877E-14,0.));
#24010=DIRECTION('',(0.,0.,1.));
#24011=DIRECTION('center_axis',(0.,0.,1.));
#24012=DIRECTION('ref_axis',(1.,-6.20171864138877E-14,0.));
#24013=DIRECTION('',(0.,0.,1.));
#24014=DIRECTION('center_axis',(0.,0.,1.));
#24015=DIRECTION('ref_axis',(1.,-6.20171864138877E-14,0.));
#24016=DIRECTION('',(0.,0.,1.));
#24017=DIRECTION('center_axis',(0.,0.,1.));
#24018=DIRECTION('ref_axis',(1.,-6.20171864138877E-14,0.));
#24019=DIRECTION('',(0.,0.,1.));
#24020=DIRECTION('center_axis',(0.,0.,1.));
#24021=DIRECTION('ref_axis',(1.,-6.20171864138877E-14,0.));
#24022=DIRECTION('',(0.,0.,1.));
#24023=DIRECTION('center_axis',(0.,0.,1.));
#24024=DIRECTION('ref_axis',(1.,-6.20171864138877E-14,0.));
#24025=DIRECTION('',(0.,0.,1.));
#24026=DIRECTION('center_axis',(0.,0.,1.));
#24027=DIRECTION('ref_axis',(1.,-6.20171864138877E-14,0.));
#24028=DIRECTION('',(0.,0.,1.));
#24029=DIRECTION('center_axis',(0.,0.,1.));
#24030=DIRECTION('ref_axis',(1.,-6.20171864138877E-14,0.));
#24031=DIRECTION('',(0.,0.,1.));
#24032=DIRECTION('center_axis',(0.,0.,1.));
#24033=DIRECTION('ref_axis',(1.,-6.20171864138877E-14,0.));
#24034=DIRECTION('',(0.,0.,1.));
#24035=DIRECTION('center_axis',(0.,0.,1.));
#24036=DIRECTION('ref_axis',(1.,-6.20171864138877E-14,0.));
#24037=DIRECTION('',(0.,0.,1.));
#24038=DIRECTION('center_axis',(0.,0.,1.));
#24039=DIRECTION('ref_axis',(1.,-6.20171864138877E-14,0.));
#24040=DIRECTION('',(0.,0.,1.));
#24041=DIRECTION('center_axis',(0.,0.,1.));
#24042=DIRECTION('ref_axis',(1.,-6.20171864138877E-14,0.));
#24043=DIRECTION('',(0.,0.,1.));
#24044=DIRECTION('center_axis',(0.,0.,1.));
#24045=DIRECTION('ref_axis',(1.,-6.20171864138877E-14,0.));
#24046=DIRECTION('',(0.,0.,1.));
#24047=DIRECTION('center_axis',(0.,0.,1.));
#24048=DIRECTION('ref_axis',(1.,-6.20171864138877E-14,0.));
#24049=DIRECTION('',(0.,0.,1.));
#24050=DIRECTION('center_axis',(0.,0.,1.));
#24051=DIRECTION('ref_axis',(1.,-6.20171864138877E-14,0.));
#24052=DIRECTION('',(0.,0.,1.));
#24053=DIRECTION('center_axis',(0.,0.,1.));
#24054=DIRECTION('ref_axis',(1.,-6.20171864138877E-14,0.));
#24055=DIRECTION('',(0.,0.,1.));
#24056=DIRECTION('center_axis',(0.,0.,-1.));
#24057=DIRECTION('ref_axis',(1.,0.,0.));
#24058=DIRECTION('center_axis',(0.,0.,-1.));
#24059=DIRECTION('ref_axis',(1.,0.,0.));
#24060=DIRECTION('',(0.707106781186547,8.65956056235493E-17,0.707106781186548));
#24061=DIRECTION('center_axis',(0.,0.,1.));
#24062=DIRECTION('ref_axis',(1.,0.,0.));
#24063=DIRECTION('center_axis',(0.,0.,1.));
#24064=DIRECTION('ref_axis',(1.,-6.20171864138877E-14,0.));
#24065=DIRECTION('center_axis',(0.,0.,-1.));
#24066=DIRECTION('ref_axis',(1.,-6.20171864138877E-14,0.));
#24067=DIRECTION('center_axis',(0.,0.,1.));
#24068=DIRECTION('ref_axis',(1.,0.,0.));
#24069=DIRECTION('center_axis',(-1.60246890531964E-16,-1.,0.));
#24070=DIRECTION('ref_axis',(1.,-1.60246890531964E-16,0.));
#24071=DIRECTION('',(1.,-1.60246890531964E-16,0.));
#24072=DIRECTION('',(0.,0.,1.));
#24073=DIRECTION('',(1.,-1.60246890531964E-16,0.));
#24074=DIRECTION('',(0.,0.,1.));
#24075=DIRECTION('center_axis',(-0.866025403784439,-0.5,0.));
#24076=DIRECTION('ref_axis',(0.5,-0.866025403784439,0.));
#24077=DIRECTION('',(0.5,-0.866025403784439,0.));
#24078=DIRECTION('',(0.,0.,1.));
#24079=DIRECTION('',(0.5,-0.866025403784439,0.));
#24080=DIRECTION('center_axis',(-0.866025403784439,0.5,0.));
#24081=DIRECTION('ref_axis',(-0.5,-0.866025403784439,0.));
#24082=DIRECTION('',(-0.5,-0.866025403784439,0.));
#24083=DIRECTION('',(0.,0.,1.));
#24084=DIRECTION('',(-0.5,-0.866025403784439,0.));
#24085=DIRECTION('center_axis',(1.60246890531964E-16,1.,0.));
#24086=DIRECTION('ref_axis',(-1.,1.60246890531964E-16,0.));
#24087=DIRECTION('',(-1.,1.60246890531964E-16,0.));
#24088=DIRECTION('',(0.,0.,1.));
#24089=DIRECTION('',(-1.,1.60246890531964E-16,0.));
#24090=DIRECTION('center_axis',(0.866025403784439,0.5,0.));
#24091=DIRECTION('ref_axis',(-0.5,0.866025403784439,0.));
#24092=DIRECTION('',(-0.5,0.866025403784439,0.));
#24093=DIRECTION('',(0.,0.,1.));
#24094=DIRECTION('',(-0.5,0.866025403784439,0.));
#24095=DIRECTION('center_axis',(0.866025403784439,-0.5,0.));
#24096=DIRECTION('ref_axis',(0.5,0.866025403784439,0.));
#24097=DIRECTION('',(0.5,0.866025403784439,0.));
#24098=DIRECTION('',(0.5,0.866025403784439,0.));
#24099=DIRECTION('center_axis',(0.,0.,1.));
#24100=DIRECTION('ref_axis',(1.,0.,0.));
#24101=DIRECTION('center_axis',(0.,0.,1.));
#24102=DIRECTION('ref_axis',(1.,0.,0.));
#24103=DIRECTION('center_axis',(0.,0.,1.));
#24104=DIRECTION('ref_axis',(1.,0.,0.));
#24105=DIRECTION('center_axis',(0.,0.,1.));
#24106=DIRECTION('ref_axis',(1.,0.,0.));
#24107=DIRECTION('',(0.,0.,-1.));
#24108=DIRECTION('center_axis',(0.,0.,1.));
#24109=DIRECTION('ref_axis',(1.,0.,0.));
#24110=DIRECTION('center_axis',(0.,0.,1.));
#24111=DIRECTION('ref_axis',(1.,0.,0.));
#24112=DIRECTION('center_axis',(0.,0.,1.));
#24113=DIRECTION('ref_axis',(1.,0.,0.));
#24114=DIRECTION('axis',(0.,0.,1.));
#24115=DIRECTION('refdir',(1.,0.,0.));
#24116=DIRECTION('center_axis',(0.,0.,1.));
#24117=DIRECTION('ref_axis',(1.,0.,0.));
#24118=DIRECTION('center_axis',(0.,0.,-1.));
#24119=DIRECTION('ref_axis',(1.,0.,0.));
#24120=DIRECTION('',(0.,0.,-1.));
#24121=DIRECTION('center_axis',(0.,0.,-1.));
#24122=DIRECTION('ref_axis',(1.,0.,0.));
#24123=DIRECTION('center_axis',(0.,0.,1.));
#24124=DIRECTION('ref_axis',(1.,0.,0.));
#24125=DIRECTION('center_axis',(0.,0.,1.));
#24126=DIRECTION('ref_axis',(1.,0.,0.));
#24127=DIRECTION('',(0.,0.,-1.));
#24128=DIRECTION('center_axis',(0.,0.,1.));
#24129=DIRECTION('ref_axis',(1.,0.,0.));
#24130=DIRECTION('center_axis',(0.,0.,1.));
#24131=DIRECTION('ref_axis',(1.,0.,0.));
#24132=DIRECTION('center_axis',(0.,0.,1.));
#24133=DIRECTION('ref_axis',(1.,0.,0.));
#24134=DIRECTION('',(1.,0.,2.22044604925031E-16));
#24135=DIRECTION('',(2.22044604925031E-16,0.,-1.));
#24136=DIRECTION('',(0.,1.,0.));
#24137=DIRECTION('',(0.,0.,1.));
#24138=DIRECTION('',(0.,0.,1.));
#24139=DIRECTION('',(1.,0.,0.));
#24140=DIRECTION('',(0.,0.,1.));
#24141=DIRECTION('',(-1.,1.22464679914735E-16,0.));
#24142=DIRECTION('',(0.,0.,1.));
#24143=DIRECTION('',(1.,0.,0.));
#24144=DIRECTION('',(1.,0.,2.22044604925031E-16));
#24145=DIRECTION('',(2.22044604925031E-16,0.,-1.));
#24146=DIRECTION('',(0.,1.,0.));
#24147=DIRECTION('',(0.,0.,1.));
#24148=DIRECTION('',(0.,0.,1.));
#24149=DIRECTION('',(1.,0.,0.));
#24150=DIRECTION('',(0.,0.,1.));
#24151=DIRECTION('',(1.,0.,0.));
#24152=DIRECTION('',(0.,0.,1.));
#24153=DIRECTION('',(1.,0.,0.));
#24154=DIRECTION('',(0.,0.,1.));
#24155=DIRECTION('',(-1.,1.22464679914735E-16,0.));
#24156=DIRECTION('',(0.,0.,1.));
#24157=DIRECTION('',(1.,0.,0.));
#24158=DIRECTION('',(0.,0.,1.));
#24159=DIRECTION('',(-1.,1.22464679914735E-16,0.));
#24160=DIRECTION('',(0.,0.,1.));
#24161=DIRECTION('',(1.,0.,0.));
#24162=DIRECTION('',(0.,0.,1.));
#24163=DIRECTION('',(-1.,1.22464679914735E-16,0.));
#24164=DIRECTION('',(0.,0.,1.));
#24165=DIRECTION('',(1.,0.,0.));
#24166=DIRECTION('',(0.,0.,1.));
#24167=DIRECTION('',(-1.,1.22464679914735E-16,0.));
#24168=DIRECTION('',(0.,0.,1.));
#24169=DIRECTION('',(1.,0.,0.));
#24170=DIRECTION('',(0.,0.,1.));
#24171=DIRECTION('',(-1.,1.22464679914735E-16,0.));
#24172=DIRECTION('',(0.,0.,1.));
#24173=DIRECTION('',(1.,0.,0.));
#24174=DIRECTION('',(0.,0.,1.));
#24175=DIRECTION('',(-1.,1.22464679914735E-16,0.));
#24176=DIRECTION('',(0.,0.,1.));
#24177=DIRECTION('',(1.,0.,0.));
#24178=DIRECTION('',(0.,0.,1.));
#24179=DIRECTION('',(-1.,1.22464679914735E-16,0.));
#24180=DIRECTION('',(0.,0.,1.));
#24181=DIRECTION('',(1.,0.,0.));
#24182=DIRECTION('',(0.,0.,1.));
#24183=DIRECTION('',(-1.,1.22464679914735E-16,0.));
#24184=DIRECTION('',(0.,0.,1.));
#24185=DIRECTION('',(1.,0.,0.));
#24186=DIRECTION('',(0.,0.,1.));
#24187=DIRECTION('',(-1.,1.22464679914735E-16,0.));
#24188=DIRECTION('',(0.,0.,1.));
#24189=DIRECTION('',(1.,0.,0.));
#24190=DIRECTION('',(0.,0.,1.));
#24191=DIRECTION('',(-1.,1.22464679914735E-16,0.));
#24192=DIRECTION('',(0.,0.,1.));
#24193=DIRECTION('',(1.,0.,0.));
#24194=DIRECTION('',(0.,0.,1.));
#24195=DIRECTION('',(-1.,1.22464679914735E-16,0.));
#24196=DIRECTION('',(0.,0.,1.));
#24197=DIRECTION('',(1.,0.,0.));
#24198=DIRECTION('',(0.,0.,1.));
#24199=DIRECTION('',(-1.,1.22464679914735E-16,0.));
#24200=DIRECTION('',(0.,0.,1.));
#24201=DIRECTION('',(1.,0.,0.));
#24202=DIRECTION('',(0.,0.,1.));
#24203=DIRECTION('',(-1.,1.22464679914735E-16,0.));
#24204=DIRECTION('',(0.,0.,1.));
#24205=DIRECTION('',(1.,0.,0.));
#24206=DIRECTION('',(0.,0.,1.));
#24207=DIRECTION('',(-1.,1.22464679914735E-16,0.));
#24208=DIRECTION('',(0.,0.,1.));
#24209=DIRECTION('',(1.,0.,0.));
#24210=DIRECTION('',(0.,0.,1.));
#24211=DIRECTION('',(-1.,1.22464679914735E-16,0.));
#24212=DIRECTION('',(0.,0.,1.));
#24213=DIRECTION('',(1.,0.,0.));
#24214=DIRECTION('axis',(0.,0.,1.));
#24215=DIRECTION('refdir',(1.,0.,0.));
#24216=DIRECTION('axis',(0.,0.,1.));
#24217=DIRECTION('refdir',(1.,0.,0.));
#24218=DIRECTION('center_axis',(0.,0.,-1.));
#24219=DIRECTION('ref_axis',(1.,0.,0.));
#24220=DIRECTION('',(0.,0.,-1.));
#24221=DIRECTION('center_axis',(0.,0.,1.));
#24222=DIRECTION('ref_axis',(1.,0.,0.));
#24223=DIRECTION('',(0.,0.,-1.));
#24224=DIRECTION('center_axis',(0.,0.,1.));
#24225=DIRECTION('ref_axis',(1.,0.,0.));
#24226=DIRECTION('center_axis',(0.,0.,1.));
#24227=DIRECTION('ref_axis',(1.,0.,0.));
#24228=DIRECTION('center_axis',(0.,0.,-1.));
#24229=DIRECTION('ref_axis',(1.,0.,0.));
#24230=DIRECTION('',(0.,0.,-1.));
#24231=DIRECTION('center_axis',(0.,0.,-1.));
#24232=DIRECTION('ref_axis',(1.,0.,0.));
#24233=DIRECTION('',(0.,0.,-1.));
#24234=DIRECTION('center_axis',(0.,0.,-1.));
#24235=DIRECTION('ref_axis',(1.,0.,0.));
#24236=DIRECTION('',(0.,0.,-1.));
#24237=DIRECTION('center_axis',(0.,0.,-1.));
#24238=DIRECTION('ref_axis',(1.,0.,0.));
#24239=DIRECTION('',(0.,0.,-1.));
#24240=DIRECTION('center_axis',(0.,0.,-1.));
#24241=DIRECTION('ref_axis',(1.,0.,0.));
#24242=DIRECTION('',(0.,0.,-1.));
#24243=DIRECTION('center_axis',(0.,0.,-1.));
#24244=DIRECTION('ref_axis',(1.,0.,0.));
#24245=DIRECTION('',(0.,0.,-1.));
#24246=DIRECTION('center_axis',(0.,0.,-1.));
#24247=DIRECTION('ref_axis',(1.,0.,0.));
#24248=DIRECTION('',(0.,0.,-1.));
#24249=DIRECTION('center_axis',(0.,0.,-1.));
#24250=DIRECTION('ref_axis',(1.,0.,0.));
#24251=DIRECTION('',(0.,0.,-1.));
#24252=DIRECTION('center_axis',(0.,0.,-1.));
#24253=DIRECTION('ref_axis',(1.,0.,0.));
#24254=DIRECTION('',(0.,0.,-1.));
#24255=DIRECTION('center_axis',(0.,0.,-1.));
#24256=DIRECTION('ref_axis',(1.,0.,0.));
#24257=DIRECTION('',(0.,0.,-1.));
#24258=DIRECTION('center_axis',(0.,0.,-1.));
#24259=DIRECTION('ref_axis',(1.,0.,0.));
#24260=DIRECTION('',(0.,0.,-1.));
#24261=DIRECTION('center_axis',(0.,0.,-1.));
#24262=DIRECTION('ref_axis',(1.,0.,0.));
#24263=DIRECTION('',(0.,0.,-1.));
#24264=DIRECTION('center_axis',(0.,0.,-1.));
#24265=DIRECTION('ref_axis',(1.,0.,0.));
#24266=DIRECTION('',(0.,0.,-1.));
#24267=DIRECTION('center_axis',(0.,0.,-1.));
#24268=DIRECTION('ref_axis',(1.,0.,0.));
#24269=DIRECTION('',(0.,0.,-1.));
#24270=DIRECTION('center_axis',(0.,0.,-1.));
#24271=DIRECTION('ref_axis',(1.,0.,0.));
#24272=DIRECTION('',(0.,0.,-1.));
#24273=DIRECTION('center_axis',(0.,0.,-1.));
#24274=DIRECTION('ref_axis',(1.,0.,0.));
#24275=DIRECTION('',(0.,0.,-1.));
#24276=DIRECTION('center_axis',(0.,0.,-1.));
#24277=DIRECTION('ref_axis',(1.,0.,0.));
#24278=DIRECTION('',(0.,0.,-1.));
#24279=DIRECTION('center_axis',(0.,0.,-1.));
#24280=DIRECTION('ref_axis',(1.,0.,0.));
#24281=DIRECTION('',(0.,0.,-1.));
#24282=DIRECTION('center_axis',(0.,0.,-1.));
#24283=DIRECTION('ref_axis',(1.,0.,0.));
#24284=DIRECTION('',(0.,0.,-1.));
#24285=DIRECTION('center_axis',(0.,0.,-1.));
#24286=DIRECTION('ref_axis',(1.,0.,0.));
#24287=DIRECTION('',(0.,0.,-1.));
#24288=DIRECTION('center_axis',(0.,0.,-1.));
#24289=DIRECTION('ref_axis',(1.,0.,0.));
#24290=DIRECTION('',(0.,0.,-1.));
#24291=DIRECTION('center_axis',(0.,0.,-1.));
#24292=DIRECTION('ref_axis',(1.,0.,0.));
#24293=DIRECTION('',(0.,0.,-1.));
#24294=DIRECTION('center_axis',(0.,0.,-1.));
#24295=DIRECTION('ref_axis',(1.,0.,0.));
#24296=DIRECTION('',(0.,0.,-1.));
#24297=DIRECTION('center_axis',(0.,0.,-1.));
#24298=DIRECTION('ref_axis',(0.938097899428847,-0.346370222575766,0.));
#24299=DIRECTION('',(0.,0.,-1.));
#24300=DIRECTION('center_axis',(0.,0.,-1.));
#24301=DIRECTION('ref_axis',(1.,0.,0.));
#24302=DIRECTION('center_axis',(0.,0.,-1.));
#24303=DIRECTION('ref_axis',(0.793346897669268,0.608769825105144,0.));
#24304=DIRECTION('',(1.22464679914735E-16,3.85574710022057E-30,-1.));
#24305=DIRECTION('center_axis',(0.,0.,1.));
#24306=DIRECTION('ref_axis',(1.,3.16070290694603E-14,0.));
#24307=DIRECTION('center_axis',(0.,0.,-1.));
#24308=DIRECTION('ref_axis',(1.,3.16070290694603E-14,0.));
#24309=DIRECTION('',(1.22464679914735E-16,3.85574710022057E-30,-1.));
#24310=DIRECTION('center_axis',(0.,0.,-1.));
#24311=DIRECTION('ref_axis',(1.,3.16070290694603E-14,0.));
#24312=DIRECTION('',(1.22464679914735E-16,3.85574710022057E-30,-1.));
#24313=DIRECTION('center_axis',(0.,0.,-1.));
#24314=DIRECTION('ref_axis',(1.,3.16070290694603E-14,0.));
#24315=DIRECTION('',(1.22464679914735E-16,3.85574710022057E-30,-1.));
#24316=DIRECTION('center_axis',(0.,0.,-1.));
#24317=DIRECTION('ref_axis',(1.,3.16070290694603E-14,0.));
#24318=DIRECTION('',(1.22464679914735E-16,3.85574710022057E-30,-1.));
#24319=DIRECTION('center_axis',(0.,0.,-1.));
#24320=DIRECTION('ref_axis',(1.,3.16070290694603E-14,0.));
#24321=DIRECTION('',(1.22464679914735E-16,3.85574710022057E-30,-1.));
#24322=DIRECTION('center_axis',(0.,0.,-1.));
#24323=DIRECTION('ref_axis',(1.,3.16070290694603E-14,0.));
#24324=DIRECTION('',(1.22464679914735E-16,3.85574710022057E-30,-1.));
#24325=DIRECTION('center_axis',(0.,0.,-1.));
#24326=DIRECTION('ref_axis',(1.,3.16070290694603E-14,0.));
#24327=DIRECTION('',(1.22464679914735E-16,3.85574710022057E-30,-1.));
#24328=DIRECTION('center_axis',(0.,0.,-1.));
#24329=DIRECTION('ref_axis',(1.,3.16070290694603E-14,0.));
#24330=DIRECTION('',(1.22464679914735E-16,3.85574710022057E-30,-1.));
#24331=DIRECTION('center_axis',(0.,0.,-1.));
#24332=DIRECTION('ref_axis',(1.,3.16070290694603E-14,0.));
#24333=DIRECTION('',(1.22464679914735E-16,3.85574710022057E-30,-1.));
#24334=DIRECTION('center_axis',(0.,0.,-1.));
#24335=DIRECTION('ref_axis',(1.,3.16070290694603E-14,0.));
#24336=DIRECTION('',(1.22464679914735E-16,3.85574710022057E-30,-1.));
#24337=DIRECTION('center_axis',(0.,0.,-1.));
#24338=DIRECTION('ref_axis',(1.,3.16070290694603E-14,0.));
#24339=DIRECTION('',(1.22464679914735E-16,3.85574710022057E-30,-1.));
#24340=DIRECTION('center_axis',(0.,0.,-1.));
#24341=DIRECTION('ref_axis',(1.,3.16070290694603E-14,0.));
#24342=DIRECTION('',(1.22464679914735E-16,3.85574710022057E-30,-1.));
#24343=DIRECTION('center_axis',(0.,0.,-1.));
#24344=DIRECTION('ref_axis',(1.,3.16070290694603E-14,0.));
#24345=DIRECTION('',(1.22464679914735E-16,3.85574710022057E-30,-1.));
#24346=DIRECTION('center_axis',(0.,0.,-1.));
#24347=DIRECTION('ref_axis',(1.,3.16070290694603E-14,0.));
#24348=DIRECTION('',(1.22464679914735E-16,3.85574710022057E-30,-1.));
#24349=DIRECTION('center_axis',(0.,0.,-1.));
#24350=DIRECTION('ref_axis',(1.,3.16070290694603E-14,0.));
#24351=DIRECTION('',(1.22464679914735E-16,3.85574710022057E-30,-1.));
#24352=DIRECTION('center_axis',(0.,0.,-1.));
#24353=DIRECTION('ref_axis',(1.,3.16070290694603E-14,0.));
#24354=DIRECTION('',(1.22464679914735E-16,3.85574710022057E-30,-1.));
#24355=DIRECTION('center_axis',(0.,0.,-1.));
#24356=DIRECTION('ref_axis',(1.,3.16070290694603E-14,0.));
#24357=DIRECTION('',(1.22464679914735E-16,3.85574710022057E-30,-1.));
#24358=DIRECTION('center_axis',(0.,0.,-1.));
#24359=DIRECTION('ref_axis',(1.,3.16070290694603E-14,0.));
#24360=DIRECTION('',(1.22464679914735E-16,3.85574710022057E-30,-1.));
#24361=DIRECTION('center_axis',(0.,0.,-1.));
#24362=DIRECTION('ref_axis',(1.,3.16070290694603E-14,0.));
#24363=DIRECTION('',(1.22464679914735E-16,3.85574710022057E-30,-1.));
#24364=DIRECTION('center_axis',(0.,0.,-1.));
#24365=DIRECTION('ref_axis',(1.,3.16070290694603E-14,0.));
#24366=DIRECTION('',(1.22464679914735E-16,3.85574710022057E-30,-1.));
#24367=DIRECTION('center_axis',(0.,0.,-1.));
#24368=DIRECTION('ref_axis',(1.,3.16070290694603E-14,0.));
#24369=DIRECTION('',(1.22464679914735E-16,3.85574710022057E-30,-1.));
#24370=DIRECTION('center_axis',(0.,0.,-1.));
#24371=DIRECTION('ref_axis',(1.,3.16070290694603E-14,0.));
#24372=DIRECTION('',(1.22464679914735E-16,3.85574710022057E-30,-1.));
#24373=DIRECTION('center_axis',(0.,0.,-1.));
#24374=DIRECTION('ref_axis',(1.,3.16070290694603E-14,0.));
#24375=DIRECTION('',(1.22464679914735E-16,3.85574710022057E-30,-1.));
#24376=DIRECTION('center_axis',(0.,0.,-1.));
#24377=DIRECTION('ref_axis',(-0.6087766502803,-0.793341660366766,0.));
#24378=DIRECTION('',(1.22464679914735E-16,3.85574710022057E-30,-1.));
#24379=DIRECTION('center_axis',(0.,0.,-1.));
#24380=DIRECTION('ref_axis',(1.,3.16070290694603E-14,0.));
#24381=DIRECTION('center_axis',(0.,0.,1.));
#24382=DIRECTION('ref_axis',(-1.,0.,0.));
#24383=DIRECTION('',(0.,0.,1.));
#24384=DIRECTION('center_axis',(0.,0.,-1.));
#24385=DIRECTION('ref_axis',(-1.,0.,0.));
#24386=DIRECTION('',(0.,0.,1.));
#24387=DIRECTION('center_axis',(0.,0.,-1.));
#24388=DIRECTION('ref_axis',(-1.,0.,0.));
#24389=DIRECTION('center_axis',(0.,0.,-1.));
#24390=DIRECTION('ref_axis',(-1.,0.,0.));
#24391=DIRECTION('center_axis',(0.,0.,1.));
#24392=DIRECTION('ref_axis',(-1.,0.,0.));
#24393=DIRECTION('',(0.,0.,1.));
#24394=DIRECTION('center_axis',(0.,0.,1.));
#24395=DIRECTION('ref_axis',(-1.,0.,0.));
#24396=DIRECTION('',(0.,0.,1.));
#24397=DIRECTION('center_axis',(0.,0.,1.));
#24398=DIRECTION('ref_axis',(-1.,0.,0.));
#24399=DIRECTION('',(0.,0.,1.));
#24400=DIRECTION('center_axis',(0.,0.,1.));
#24401=DIRECTION('ref_axis',(-1.,0.,0.));
#24402=DIRECTION('',(0.,0.,1.));
#24403=DIRECTION('center_axis',(0.,0.,1.));
#24404=DIRECTION('ref_axis',(-1.,0.,0.));
#24405=DIRECTION('',(0.,0.,1.));
#24406=DIRECTION('center_axis',(0.,0.,1.));
#24407=DIRECTION('ref_axis',(-1.,0.,0.));
#24408=DIRECTION('',(0.,0.,1.));
#24409=DIRECTION('center_axis',(0.,0.,1.));
#24410=DIRECTION('ref_axis',(-1.,0.,0.));
#24411=DIRECTION('',(0.,0.,1.));
#24412=DIRECTION('center_axis',(0.,0.,1.));
#24413=DIRECTION('ref_axis',(-1.,0.,0.));
#24414=DIRECTION('',(0.,0.,1.));
#24415=DIRECTION('center_axis',(0.,0.,1.));
#24416=DIRECTION('ref_axis',(-1.,0.,0.));
#24417=DIRECTION('',(0.,0.,1.));
#24418=DIRECTION('center_axis',(0.,0.,1.));
#24419=DIRECTION('ref_axis',(-1.,0.,0.));
#24420=DIRECTION('',(0.,0.,1.));
#24421=DIRECTION('center_axis',(0.,0.,1.));
#24422=DIRECTION('ref_axis',(-1.,0.,0.));
#24423=DIRECTION('',(0.,0.,1.));
#24424=DIRECTION('center_axis',(0.,0.,1.));
#24425=DIRECTION('ref_axis',(-1.,0.,0.));
#24426=DIRECTION('',(0.,0.,1.));
#24427=DIRECTION('center_axis',(0.,0.,1.));
#24428=DIRECTION('ref_axis',(-1.,0.,0.));
#24429=DIRECTION('',(0.,0.,1.));
#24430=DIRECTION('center_axis',(0.,0.,1.));
#24431=DIRECTION('ref_axis',(-1.,0.,0.));
#24432=DIRECTION('',(0.,0.,1.));
#24433=DIRECTION('center_axis',(0.,0.,1.));
#24434=DIRECTION('ref_axis',(-1.,0.,0.));
#24435=DIRECTION('',(0.,0.,1.));
#24436=DIRECTION('center_axis',(0.,0.,1.));
#24437=DIRECTION('ref_axis',(-1.,0.,0.));
#24438=DIRECTION('',(0.,0.,1.));
#24439=DIRECTION('center_axis',(0.,0.,1.));
#24440=DIRECTION('ref_axis',(-1.,0.,0.));
#24441=DIRECTION('',(0.,0.,1.));
#24442=DIRECTION('center_axis',(0.,0.,1.));
#24443=DIRECTION('ref_axis',(-1.,0.,0.));
#24444=DIRECTION('',(0.,0.,1.));
#24445=DIRECTION('center_axis',(0.,0.,1.));
#24446=DIRECTION('ref_axis',(-1.,0.,0.));
#24447=DIRECTION('',(0.,0.,1.));
#24448=DIRECTION('center_axis',(0.,0.,1.));
#24449=DIRECTION('ref_axis',(-1.,0.,0.));
#24450=DIRECTION('',(0.,0.,1.));
#24451=DIRECTION('center_axis',(0.,0.,1.));
#24452=DIRECTION('ref_axis',(-1.,0.,0.));
#24453=DIRECTION('',(0.,0.,1.));
#24454=DIRECTION('center_axis',(0.,0.,1.));
#24455=DIRECTION('ref_axis',(-1.,0.,0.));
#24456=DIRECTION('',(0.,0.,1.));
#24457=DIRECTION('center_axis',(0.,0.,1.));
#24458=DIRECTION('ref_axis',(-1.,0.,0.));
#24459=DIRECTION('',(0.,0.,1.));
#24460=DIRECTION('center_axis',(0.,0.,1.));
#24461=DIRECTION('ref_axis',(-1.,0.,0.));
#24462=DIRECTION('',(0.,0.,1.));
#24463=DIRECTION('center_axis',(0.,0.,1.));
#24464=DIRECTION('ref_axis',(-1.,0.,0.));
#24465=DIRECTION('',(0.,0.,1.));
#24466=DIRECTION('center_axis',(0.,0.,1.));
#24467=DIRECTION('ref_axis',(-1.,0.,0.));
#24468=DIRECTION('',(0.,0.,1.));
#24469=DIRECTION('center_axis',(0.,0.,1.));
#24470=DIRECTION('ref_axis',(-1.,0.,0.));
#24471=DIRECTION('',(0.,0.,1.));
#24472=DIRECTION('center_axis',(0.,0.,1.));
#24473=DIRECTION('ref_axis',(-1.,0.,0.));
#24474=DIRECTION('',(0.,0.,1.));
#24475=DIRECTION('center_axis',(0.,0.,1.));
#24476=DIRECTION('ref_axis',(-1.,0.,0.));
#24477=DIRECTION('',(0.,0.,1.));
#24478=DIRECTION('center_axis',(0.,0.,1.));
#24479=DIRECTION('ref_axis',(-1.,0.,0.));
#24480=DIRECTION('',(0.,0.,1.));
#24481=DIRECTION('center_axis',(0.,0.,1.));
#24482=DIRECTION('ref_axis',(-1.,0.,0.));
#24483=DIRECTION('',(0.,0.,1.));
#24484=DIRECTION('center_axis',(0.,0.,1.));
#24485=DIRECTION('ref_axis',(-1.,0.,0.));
#24486=DIRECTION('',(0.,0.,1.));
#24487=DIRECTION('center_axis',(0.,0.,1.));
#24488=DIRECTION('ref_axis',(-1.,0.,0.));
#24489=DIRECTION('',(0.,0.,1.));
#24490=DIRECTION('center_axis',(0.,0.,1.));
#24491=DIRECTION('ref_axis',(-1.,0.,0.));
#24492=DIRECTION('',(0.,0.,1.));
#24493=DIRECTION('center_axis',(0.,0.,1.));
#24494=DIRECTION('ref_axis',(-1.,0.,0.));
#24495=DIRECTION('',(0.,0.,1.));
#24496=DIRECTION('center_axis',(0.,0.,1.));
#24497=DIRECTION('ref_axis',(-1.,0.,0.));
#24498=DIRECTION('',(0.,0.,1.));
#24499=DIRECTION('center_axis',(0.,0.,1.));
#24500=DIRECTION('ref_axis',(-1.,0.,0.));
#24501=DIRECTION('',(0.,0.,1.));
#24502=DIRECTION('center_axis',(0.,0.,1.));
#24503=DIRECTION('ref_axis',(-1.,0.,0.));
#24504=DIRECTION('',(0.,0.,1.));
#24505=DIRECTION('center_axis',(0.,0.,1.));
#24506=DIRECTION('ref_axis',(-0.938097369934915,-0.346371656636617,0.));
#24507=DIRECTION('',(0.,0.,1.));
#24508=DIRECTION('center_axis',(0.,0.,-1.));
#24509=DIRECTION('ref_axis',(-1.,0.,0.));
#24510=DIRECTION('center_axis',(0.,0.,1.));
#24511=DIRECTION('ref_axis',(-0.793344496203991,0.608772954674266,0.));
#24512=DIRECTION('',(-1.22464679914735E-16,4.47534497895031E-29,1.));
#24513=DIRECTION('center_axis',(0.,0.,-1.));
#24514=DIRECTION('ref_axis',(-1.,3.65562114876707E-13,0.));
#24515=DIRECTION('center_axis',(0.,0.,1.));
#24516=DIRECTION('ref_axis',(-1.,3.65562114876707E-13,0.));
#24517=DIRECTION('',(-1.22464679914735E-16,4.47534497895031E-29,1.));
#24518=DIRECTION('center_axis',(0.,0.,1.));
#24519=DIRECTION('ref_axis',(-1.,3.65562114876707E-13,0.));
#24520=DIRECTION('',(-1.22464679914735E-16,4.47534497895031E-29,1.));
#24521=DIRECTION('center_axis',(0.,0.,1.));
#24522=DIRECTION('ref_axis',(-1.,3.65562114876707E-13,0.));
#24523=DIRECTION('',(-1.22464679914735E-16,4.47534497895031E-29,1.));
#24524=DIRECTION('center_axis',(0.,0.,1.));
#24525=DIRECTION('ref_axis',(-1.,3.65562114876707E-13,0.));
#24526=DIRECTION('',(-1.22464679914735E-16,4.47534497895031E-29,1.));
#24527=DIRECTION('center_axis',(0.,0.,1.));
#24528=DIRECTION('ref_axis',(-1.,3.65562114876707E-13,0.));
#24529=DIRECTION('',(-1.22464679914735E-16,4.47534497895031E-29,1.));
#24530=DIRECTION('center_axis',(0.,0.,1.));
#24531=DIRECTION('ref_axis',(-1.,3.65562114876707E-13,0.));
#24532=DIRECTION('',(-1.22464679914735E-16,4.47534497895031E-29,1.));
#24533=DIRECTION('center_axis',(0.,0.,1.));
#24534=DIRECTION('ref_axis',(-1.,3.65562114876707E-13,0.));
#24535=DIRECTION('',(-1.22464679914735E-16,4.47534497895031E-29,1.));
#24536=DIRECTION('center_axis',(0.,0.,1.));
#24537=DIRECTION('ref_axis',(-1.,3.65562114876707E-13,0.));
#24538=DIRECTION('',(-1.22464679914735E-16,4.47534497895031E-29,1.));
#24539=DIRECTION('center_axis',(0.,0.,1.));
#24540=DIRECTION('ref_axis',(-1.,3.65562114876707E-13,0.));
#24541=DIRECTION('',(-1.22464679914735E-16,4.47534497895031E-29,1.));
#24542=DIRECTION('center_axis',(0.,0.,1.));
#24543=DIRECTION('ref_axis',(-1.,3.65562114876707E-13,0.));
#24544=DIRECTION('',(-1.22464679914735E-16,4.47534497895031E-29,1.));
#24545=DIRECTION('center_axis',(0.,0.,1.));
#24546=DIRECTION('ref_axis',(-1.,3.65562114876707E-13,0.));
#24547=DIRECTION('',(-1.22464679914735E-16,4.47534497895031E-29,1.));
#24548=DIRECTION('center_axis',(0.,0.,1.));
#24549=DIRECTION('ref_axis',(-1.,3.65562114876707E-13,0.));
#24550=DIRECTION('',(-1.22464679914735E-16,4.47534497895031E-29,1.));
#24551=DIRECTION('center_axis',(0.,0.,1.));
#24552=DIRECTION('ref_axis',(-1.,3.65562114876707E-13,0.));
#24553=DIRECTION('',(-1.22464679914735E-16,4.47534497895031E-29,1.));
#24554=DIRECTION('center_axis',(0.,0.,1.));
#24555=DIRECTION('ref_axis',(-1.,3.65562114876707E-13,0.));
#24556=DIRECTION('',(-1.22464679914735E-16,4.47534497895031E-29,1.));
#24557=DIRECTION('center_axis',(0.,0.,1.));
#24558=DIRECTION('ref_axis',(-1.,3.65562114876707E-13,0.));
#24559=DIRECTION('',(-1.22464679914735E-16,4.47534497895031E-29,1.));
#24560=DIRECTION('center_axis',(0.,0.,1.));
#24561=DIRECTION('ref_axis',(-1.,3.65562114876707E-13,0.));
#24562=DIRECTION('',(-1.22464679914735E-16,4.47534497895031E-29,1.));
#24563=DIRECTION('center_axis',(0.,0.,1.));
#24564=DIRECTION('ref_axis',(-1.,3.65562114876707E-13,0.));
#24565=DIRECTION('',(-1.22464679914735E-16,4.47534497895031E-29,1.));
#24566=DIRECTION('center_axis',(0.,0.,1.));
#24567=DIRECTION('ref_axis',(-1.,3.65562114876707E-13,0.));
#24568=DIRECTION('',(-1.22464679914735E-16,4.47534497895031E-29,1.));
#24569=DIRECTION('center_axis',(0.,0.,1.));
#24570=DIRECTION('ref_axis',(-1.,3.65562114876707E-13,0.));
#24571=DIRECTION('',(-1.22464679914735E-16,4.47534497895031E-29,1.));
#24572=DIRECTION('center_axis',(0.,0.,1.));
#24573=DIRECTION('ref_axis',(-1.,3.65562114876707E-13,0.));
#24574=DIRECTION('',(-1.22464679914735E-16,4.47534497895031E-29,1.));
#24575=DIRECTION('center_axis',(0.,0.,1.));
#24576=DIRECTION('ref_axis',(-1.,3.65562114876707E-13,0.));
#24577=DIRECTION('',(-1.22464679914735E-16,4.47534497895031E-29,1.));
#24578=DIRECTION('center_axis',(0.,0.,1.));
#24579=DIRECTION('ref_axis',(-1.,3.65562114876707E-13,0.));
#24580=DIRECTION('',(-1.22464679914735E-16,4.47534497895031E-29,1.));
#24581=DIRECTION('center_axis',(0.,0.,1.));
#24582=DIRECTION('ref_axis',(-1.,3.65562114876707E-13,0.));
#24583=DIRECTION('',(-1.22464679914735E-16,4.47534497895031E-29,1.));
#24584=DIRECTION('center_axis',(0.,0.,1.));
#24585=DIRECTION('ref_axis',(-1.,3.65562114876707E-13,0.));
#24586=DIRECTION('',(-1.22464679914735E-16,4.47534497895031E-29,1.));
#24587=DIRECTION('center_axis',(0.,0.,1.));
#24588=DIRECTION('ref_axis',(-1.,3.65562114876707E-13,0.));
#24589=DIRECTION('',(-1.22464679914735E-16,4.47534497895031E-29,1.));
#24590=DIRECTION('center_axis',(0.,0.,1.));
#24591=DIRECTION('ref_axis',(-1.,3.65562114876707E-13,0.));
#24592=DIRECTION('',(-1.22464679914735E-16,4.47534497895031E-29,1.));
#24593=DIRECTION('center_axis',(0.,0.,1.));
#24594=DIRECTION('ref_axis',(-1.,3.65562114876707E-13,0.));
#24595=DIRECTION('',(-1.22464679914735E-16,4.47534497895031E-29,1.));
#24596=DIRECTION('center_axis',(0.,0.,1.));
#24597=DIRECTION('ref_axis',(-1.,3.65562114876707E-13,0.));
#24598=DIRECTION('',(-1.22464679914735E-16,4.47534497895031E-29,1.));
#24599=DIRECTION('center_axis',(0.,0.,1.));
#24600=DIRECTION('ref_axis',(-1.,3.65562114876707E-13,0.));
#24601=DIRECTION('',(-1.22464679914735E-16,4.47534497895031E-29,1.));
#24602=DIRECTION('center_axis',(0.,0.,1.));
#24603=DIRECTION('ref_axis',(-1.,3.65562114876707E-13,0.));
#24604=DIRECTION('',(-1.22464679914735E-16,4.47534497895031E-29,1.));
#24605=DIRECTION('center_axis',(0.,0.,1.));
#24606=DIRECTION('ref_axis',(-1.,3.65562114876707E-13,0.));
#24607=DIRECTION('',(-1.22464679914735E-16,4.47534497895031E-29,1.));
#24608=DIRECTION('center_axis',(0.,0.,1.));
#24609=DIRECTION('ref_axis',(-1.,3.65562114876707E-13,0.));
#24610=DIRECTION('',(-1.22464679914735E-16,4.47534497895031E-29,1.));
#24611=DIRECTION('center_axis',(0.,0.,1.));
#24612=DIRECTION('ref_axis',(-1.,3.65562114876707E-13,0.));
#24613=DIRECTION('',(-1.22464679914735E-16,4.47534497895031E-29,1.));
#24614=DIRECTION('center_axis',(0.,0.,1.));
#24615=DIRECTION('ref_axis',(-1.,3.65562114876707E-13,0.));
#24616=DIRECTION('',(-1.22464679914735E-16,4.47534497895031E-29,1.));
#24617=DIRECTION('center_axis',(0.,0.,1.));
#24618=DIRECTION('ref_axis',(-1.,3.65562114876707E-13,0.));
#24619=DIRECTION('',(-1.22464679914735E-16,4.47534497895031E-29,1.));
#24620=DIRECTION('center_axis',(0.,0.,1.));
#24621=DIRECTION('ref_axis',(-1.,3.65562114876707E-13,0.));
#24622=DIRECTION('',(-1.22464679914735E-16,4.47534497895031E-29,1.));
#24623=DIRECTION('center_axis',(0.,0.,1.));
#24624=DIRECTION('ref_axis',(-1.,3.65562114876707E-13,0.));
#24625=DIRECTION('',(-1.22464679914735E-16,4.47534497895031E-29,1.));
#24626=DIRECTION('center_axis',(0.,0.,1.));
#24627=DIRECTION('ref_axis',(-1.,3.65562114876707E-13,0.));
#24628=DIRECTION('',(-1.22464679914735E-16,4.47534497895031E-29,1.));
#24629=DIRECTION('center_axis',(0.,0.,1.));
#24630=DIRECTION('ref_axis',(0.608777863132373,-0.793340729674193,0.));
#24631=DIRECTION('',(-1.22464679914735E-16,4.47534497895031E-29,1.));
#24632=DIRECTION('center_axis',(0.,0.,1.));
#24633=DIRECTION('ref_axis',(-1.,3.65562114876707E-13,0.));
#24634=DIRECTION('center_axis',(0.,0.,1.));
#24635=DIRECTION('ref_axis',(1.,0.,0.));
#24636=DIRECTION('center_axis',(0.,0.,1.));
#24637=DIRECTION('ref_axis',(-1.,3.65562114876707E-13,0.));
#24638=DIRECTION('center_axis',(0.,0.,1.));
#24639=DIRECTION('ref_axis',(-1.,0.,0.));
#24640=DIRECTION('center_axis',(0.,0.,1.));
#24641=DIRECTION('ref_axis',(-1.,0.,0.));
#24642=DIRECTION('center_axis',(0.,0.,-1.));
#24643=DIRECTION('ref_axis',(1.,0.,0.));
#24644=DIRECTION('center_axis',(0.,0.,1.));
#24645=DIRECTION('ref_axis',(1.,0.,0.));
#24646=DIRECTION('center_axis',(0.,0.,-1.));
#24647=DIRECTION('ref_axis',(1.,3.16070290694603E-14,0.));
#24648=DIRECTION('center_axis',(0.,0.,-1.));
#24649=DIRECTION('ref_axis',(1.,0.,0.));
#24650=DIRECTION('center_axis',(0.,0.,-1.));
#24651=DIRECTION('ref_axis',(1.,0.,0.));
#24652=DIRECTION('center_axis',(0.,0.,1.));
#24653=DIRECTION('ref_axis',(1.,0.,0.));
#24654=DIRECTION('center_axis',(0.,0.,1.));
#24655=DIRECTION('ref_axis',(0.707106781186548,-0.707106781186547,0.));
#24656=DIRECTION('center_axis',(0.,0.,-1.));
#24657=DIRECTION('ref_axis',(0.707106781186548,-0.707106781186547,0.));
#24658=DIRECTION('',(0.,0.,-1.));
#24659=DIRECTION('center_axis',(0.,0.,1.));
#24660=DIRECTION('ref_axis',(0.707106781186548,-0.707106781186547,0.));
#24661=DIRECTION('',(0.,0.,1.));
#24662=DIRECTION('center_axis',(0.,-1.,0.));
#24663=DIRECTION('ref_axis',(1.,0.,0.));
#24664=DIRECTION('',(1.,0.,0.));
#24665=DIRECTION('',(0.,0.,1.));
#24666=DIRECTION('',(-1.,0.,0.));
#24667=DIRECTION('center_axis',(0.,0.,1.));
#24668=DIRECTION('ref_axis',(1.,0.,0.));
#24669=DIRECTION('',(0.,1.,0.));
#24670=DIRECTION('center_axis',(0.,0.,1.));
#24671=DIRECTION('ref_axis',(-0.707106781186548,0.707106781186547,0.));
#24672=DIRECTION('',(1.,0.,0.));
#24673=DIRECTION('center_axis',(0.,0.,1.));
#24674=DIRECTION('ref_axis',(0.707106781186547,0.707106781186548,0.));
#24675=DIRECTION('',(0.,-1.,0.));
#24676=DIRECTION('center_axis',(0.,0.,1.));
#24677=DIRECTION('ref_axis',(0.707106781186548,-0.707106781186548,0.));
#24678=DIRECTION('',(-1.,0.,0.));
#24679=DIRECTION('center_axis',(0.,0.,1.));
#24680=DIRECTION('ref_axis',(-0.707106781186548,-0.707106781186548,0.));
#24681=DIRECTION('',(0.,1.,0.));
#24682=DIRECTION('center_axis',(0.,0.,-1.));
#24683=DIRECTION('ref_axis',(0.707106781186548,0.707106781186547,0.));
#24684=DIRECTION('',(-1.,0.,0.));
#24685=DIRECTION('center_axis',(0.,0.,-1.));
#24686=DIRECTION('ref_axis',(-0.707106781186548,0.707106781186547,0.));
#24687=DIRECTION('',(0.,-1.,0.));
#24688=DIRECTION('center_axis',(0.,0.,-1.));
#24689=DIRECTION('ref_axis',(-0.707106781186548,-0.707106781186548,0.));
#24690=DIRECTION('',(1.,0.,0.));
#24691=DIRECTION('center_axis',(0.,0.,-1.));
#24692=DIRECTION('ref_axis',(0.707106781186547,-0.707106781186548,0.));
#24693=DIRECTION('',(0.,1.,0.));
#24694=DIRECTION('center_axis',(0.,0.,-1.));
#24695=DIRECTION('ref_axis',(0.707106781186547,0.707106781186548,0.));
#24696=DIRECTION('',(-1.,0.,0.));
#24697=DIRECTION('center_axis',(0.,0.,1.));
#24698=DIRECTION('ref_axis',(-0.707106781186547,-0.707106781186548,0.));
#24699=DIRECTION('',(0.,1.,0.));
#24700=DIRECTION('center_axis',(0.,0.,1.));
#24701=DIRECTION('ref_axis',(-0.707106781186548,0.707106781186547,0.));
#24702=DIRECTION('',(1.,0.,0.));
#24703=DIRECTION('center_axis',(0.,0.,1.));
#24704=DIRECTION('ref_axis',(0.707106781186548,0.707106781186548,0.));
#24705=DIRECTION('',(0.,-1.,0.));
#24706=DIRECTION('center_axis',(0.,0.,1.));
#24707=DIRECTION('ref_axis',(0.707106781186548,-0.707106781186548,0.));
#24708=DIRECTION('',(-1.,0.,0.));
#24709=DIRECTION('center_axis',(0.,0.,-1.));
#24710=DIRECTION('ref_axis',(-0.707106781186547,0.707106781186548,0.));
#24711=DIRECTION('',(0.,-1.,0.));
#24712=DIRECTION('center_axis',(0.,0.,-1.));
#24713=DIRECTION('ref_axis',(-0.707106781186547,-0.707106781186548,0.));
#24714=DIRECTION('',(1.,0.,0.));
#24715=DIRECTION('center_axis',(0.,0.,-1.));
#24716=DIRECTION('ref_axis',(0.707106781186548,-0.707106781186548,0.));
#24717=DIRECTION('',(0.,1.,0.));
#24718=DIRECTION('center_axis',(0.,0.,-1.));
#24719=DIRECTION('ref_axis',(0.707106781186548,0.707106781186547,0.));
#24720=DIRECTION('',(-1.,0.,0.));
#24721=DIRECTION('center_axis',(0.,0.,-1.));
#24722=DIRECTION('ref_axis',(-0.707106781186548,0.707106781186547,0.));
#24723=DIRECTION('',(0.,-1.,0.));
#24724=DIRECTION('center_axis',(0.,0.,1.));
#24725=DIRECTION('ref_axis',(0.707106781186548,-0.707106781186547,0.));
#24726=DIRECTION('',(-1.,0.,0.));
#24727=DIRECTION('center_axis',(0.,0.,1.));
#24728=DIRECTION('ref_axis',(-0.707106781186547,-0.707106781186548,0.));
#24729=DIRECTION('',(0.,1.,0.));
#24730=DIRECTION('center_axis',(0.,0.,1.));
#24731=DIRECTION('ref_axis',(-0.707106781186548,0.707106781186548,0.));
#24732=DIRECTION('',(1.,0.,0.));
#24733=DIRECTION('center_axis',(0.,0.,1.));
#24734=DIRECTION('ref_axis',(0.707106781186548,0.707106781186548,0.));
#24735=DIRECTION('',(0.,-1.,0.));
#24736=DIRECTION('center_axis',(0.,0.,-1.));
#24737=DIRECTION('ref_axis',(-0.707106781186548,-0.707106781186547,0.));
#24738=DIRECTION('',(1.,0.,0.));
#24739=DIRECTION('center_axis',(0.,0.,-1.));
#24740=DIRECTION('ref_axis',(0.707106781186548,-0.707106781186547,0.));
#24741=DIRECTION('',(0.,1.,0.));
#24742=DIRECTION('center_axis',(0.,0.,-1.));
#24743=DIRECTION('ref_axis',(0.707106781186548,0.707106781186548,0.));
#24744=DIRECTION('',(-1.,0.,0.));
#24745=DIRECTION('center_axis',(0.,0.,-1.));
#24746=DIRECTION('ref_axis',(-0.707106781186547,0.707106781186548,0.));
#24747=DIRECTION('',(0.,-1.,0.));
#24748=DIRECTION('center_axis',(0.,0.,-1.));
#24749=DIRECTION('ref_axis',(-0.707106781186547,-0.707106781186548,0.));
#24750=DIRECTION('',(1.,0.,0.));
#24751=DIRECTION('center_axis',(0.,0.,1.));
#24752=DIRECTION('ref_axis',(0.707106781186547,0.707106781186548,0.));
#24753=DIRECTION('',(0.,-1.,0.));
#24754=DIRECTION('center_axis',(0.,0.,1.));
#24755=DIRECTION('ref_axis',(0.707106781186548,-0.707106781186547,0.));
#24756=DIRECTION('',(-1.,0.,0.));
#24757=DIRECTION('center_axis',(0.,0.,1.));
#24758=DIRECTION('ref_axis',(-0.707106781186548,-0.707106781186548,0.));
#24759=DIRECTION('',(0.,1.,0.));
#24760=DIRECTION('center_axis',(0.,0.,1.));
#24761=DIRECTION('ref_axis',(-0.707106781186548,0.707106781186548,0.));
#24762=DIRECTION('',(1.,0.,0.));
#24763=DIRECTION('center_axis',(0.,0.,-1.));
#24764=DIRECTION('ref_axis',(0.707106781186547,-0.707106781186548,0.));
#24765=DIRECTION('',(0.,1.,0.));
#24766=DIRECTION('center_axis',(0.,0.,-1.));
#24767=DIRECTION('ref_axis',(0.707106781186547,0.707106781186548,0.));
#24768=DIRECTION('',(-1.,0.,0.));
#24769=DIRECTION('center_axis',(0.,0.,-1.));
#24770=DIRECTION('ref_axis',(-0.707106781186548,0.707106781186548,0.));
#24771=DIRECTION('',(0.,-1.,0.));
#24772=DIRECTION('center_axis',(0.,0.,-1.));
#24773=DIRECTION('ref_axis',(-0.707106781186548,-0.707106781186547,0.));
#24774=DIRECTION('center_axis',(0.,0.,-1.));
#24775=DIRECTION('ref_axis',(1.,0.,0.));
#24776=DIRECTION('center_axis',(0.,0.,-1.));
#24777=DIRECTION('ref_axis',(1.,0.,0.));
#24778=DIRECTION('center_axis',(0.,0.,-1.));
#24779=DIRECTION('ref_axis',(1.,0.,0.));
#24780=DIRECTION('center_axis',(0.,0.,-1.));
#24781=DIRECTION('ref_axis',(1.,0.,0.));
#24782=DIRECTION('center_axis',(0.,0.,1.));
#24783=DIRECTION('ref_axis',(-0.707106781186548,0.707106781186547,0.));
#24784=DIRECTION('center_axis',(0.,0.,-1.));
#24785=DIRECTION('ref_axis',(-0.707106781186548,0.707106781186547,0.));
#24786=DIRECTION('',(0.,0.,1.));
#24787=DIRECTION('',(0.,0.,-1.));
#24788=DIRECTION('center_axis',(0.,-1.,0.));
#24789=DIRECTION('ref_axis',(1.,0.,0.));
#24790=DIRECTION('',(-1.,0.,0.));
#24791=DIRECTION('',(0.,0.,-1.));
#24792=DIRECTION('center_axis',(0.,0.,1.));
#24793=DIRECTION('ref_axis',(0.707106781186547,0.707106781186548,0.));
#24794=DIRECTION('center_axis',(0.,0.,-1.));
#24795=DIRECTION('ref_axis',(0.707106781186547,0.707106781186548,0.));
#24796=DIRECTION('',(0.,0.,1.));
#24797=DIRECTION('center_axis',(-1.,0.,0.));
#24798=DIRECTION('ref_axis',(0.,-1.,0.));
#24799=DIRECTION('',(0.,1.,0.));
#24800=DIRECTION('',(0.,0.,-1.));
#24801=DIRECTION('center_axis',(0.,0.,1.));
#24802=DIRECTION('ref_axis',(0.707106781186548,-0.707106781186548,0.));
#24803=DIRECTION('center_axis',(0.,0.,-1.));
#24804=DIRECTION('ref_axis',(0.707106781186548,-0.707106781186548,0.));
#24805=DIRECTION('',(0.,0.,1.));
#24806=DIRECTION('center_axis',(0.,1.,0.));
#24807=DIRECTION('ref_axis',(-1.,0.,0.));
#24808=DIRECTION('',(1.,0.,0.));
#24809=DIRECTION('',(0.,0.,-1.));
#24810=DIRECTION('center_axis',(0.,0.,1.));
#24811=DIRECTION('ref_axis',(-0.707106781186548,-0.707106781186548,0.));
#24812=DIRECTION('center_axis',(0.,0.,-1.));
#24813=DIRECTION('ref_axis',(-0.707106781186548,-0.707106781186548,0.));
#24814=DIRECTION('',(0.,0.,1.));
#24815=DIRECTION('center_axis',(1.,0.,0.));
#24816=DIRECTION('ref_axis',(0.,1.,0.));
#24817=DIRECTION('',(0.,-1.,0.));
#24818=DIRECTION('',(0.,0.,-1.));
#24819=DIRECTION('center_axis',(0.,0.,1.));
#24820=DIRECTION('ref_axis',(0.707106781186548,0.707106781186547,0.));
#24821=DIRECTION('center_axis',(0.,0.,1.));
#24822=DIRECTION('ref_axis',(0.707106781186548,0.707106781186547,0.));
#24823=DIRECTION('',(0.,0.,1.));
#24824=DIRECTION('center_axis',(0.,0.,1.));
#24825=DIRECTION('ref_axis',(-0.707106781186548,0.707106781186547,0.));
#24826=DIRECTION('',(0.,0.,-1.));
#24827=DIRECTION('center_axis',(0.,0.,1.));
#24828=DIRECTION('ref_axis',(-0.707106781186548,0.707106781186547,0.));
#24829=DIRECTION('',(0.,0.,1.));
#24830=DIRECTION('center_axis',(-1.,0.,0.));
#24831=DIRECTION('ref_axis',(0.,-1.,0.));
#24832=DIRECTION('',(0.,1.,0.));
#24833=DIRECTION('',(0.,0.,-1.));
#24834=DIRECTION('center_axis',(0.,0.,1.));
#24835=DIRECTION('ref_axis',(-0.707106781186548,-0.707106781186548,0.));
#24836=DIRECTION('center_axis',(0.,0.,1.));
#24837=DIRECTION('ref_axis',(-0.707106781186548,-0.707106781186548,0.));
#24838=DIRECTION('',(0.,0.,1.));
#24839=DIRECTION('center_axis',(0.,0.,1.));
#24840=DIRECTION('ref_axis',(0.707106781186547,-0.707106781186548,0.));
#24841=DIRECTION('',(0.,0.,-1.));
#24842=DIRECTION('center_axis',(0.,0.,1.));
#24843=DIRECTION('ref_axis',(0.707106781186547,-0.707106781186548,0.));
#24844=DIRECTION('',(0.,0.,1.));
#24845=DIRECTION('center_axis',(1.,0.,0.));
#24846=DIRECTION('ref_axis',(0.,1.,0.));
#24847=DIRECTION('',(0.,-1.,0.));
#24848=DIRECTION('',(0.,0.,-1.));
#24849=DIRECTION('center_axis',(0.,0.,1.));
#24850=DIRECTION('ref_axis',(0.707106781186547,0.707106781186548,0.));
#24851=DIRECTION('center_axis',(0.,0.,1.));
#24852=DIRECTION('ref_axis',(0.707106781186547,0.707106781186548,0.));
#24853=DIRECTION('',(0.,0.,1.));
#24854=DIRECTION('center_axis',(0.,0.,1.));
#24855=DIRECTION('ref_axis',(-0.707106781186547,-0.707106781186548,0.));
#24856=DIRECTION('center_axis',(0.,0.,-1.));
#24857=DIRECTION('ref_axis',(-0.707106781186547,-0.707106781186548,0.));
#24858=DIRECTION('',(0.,0.,1.));
#24859=DIRECTION('',(0.,0.,-1.));
#24860=DIRECTION('center_axis',(1.,0.,0.));
#24861=DIRECTION('ref_axis',(0.,1.,0.));
#24862=DIRECTION('',(0.,-1.,0.));
#24863=DIRECTION('',(0.,0.,-1.));
#24864=DIRECTION('center_axis',(0.,0.,1.));
#24865=DIRECTION('ref_axis',(-0.707106781186548,0.707106781186547,0.));
#24866=DIRECTION('center_axis',(0.,0.,-1.));
#24867=DIRECTION('ref_axis',(-0.707106781186548,0.707106781186547,0.));
#24868=DIRECTION('',(0.,0.,1.));
#24869=DIRECTION('center_axis',(0.,-1.,0.));
#24870=DIRECTION('ref_axis',(1.,0.,0.));
#24871=DIRECTION('',(-1.,0.,0.));
#24872=DIRECTION('',(0.,0.,-1.));
#24873=DIRECTION('center_axis',(0.,0.,1.));
#24874=DIRECTION('ref_axis',(0.707106781186548,0.707106781186548,0.));
#24875=DIRECTION('center_axis',(0.,0.,-1.));
#24876=DIRECTION('ref_axis',(0.707106781186548,0.707106781186548,0.));
#24877=DIRECTION('',(0.,0.,1.));
#24878=DIRECTION('center_axis',(-1.,0.,0.));
#24879=DIRECTION('ref_axis',(0.,-1.,0.));
#24880=DIRECTION('',(0.,1.,0.));
#24881=DIRECTION('',(0.,0.,-1.));
#24882=DIRECTION('center_axis',(0.,0.,1.));
#24883=DIRECTION('ref_axis',(0.707106781186548,-0.707106781186548,0.));
#24884=DIRECTION('center_axis',(0.,0.,-1.));
#24885=DIRECTION('ref_axis',(0.707106781186548,-0.707106781186548,0.));
#24886=DIRECTION('',(0.,0.,1.));
#24887=DIRECTION('center_axis',(0.,1.,0.));
#24888=DIRECTION('ref_axis',(-1.,0.,0.));
#24889=DIRECTION('',(1.,0.,0.));
#24890=DIRECTION('',(0.,0.,-1.));
#24891=DIRECTION('center_axis',(0.,0.,1.));
#24892=DIRECTION('ref_axis',(-0.707106781186547,0.707106781186548,0.));
#24893=DIRECTION('center_axis',(0.,0.,1.));
#24894=DIRECTION('ref_axis',(-0.707106781186547,0.707106781186548,0.));
#24895=DIRECTION('',(0.,0.,1.));
#24896=DIRECTION('center_axis',(0.,0.,1.));
#24897=DIRECTION('ref_axis',(-0.707106781186547,-0.707106781186548,0.));
#24898=DIRECTION('',(0.,0.,-1.));
#24899=DIRECTION('center_axis',(0.,0.,1.));
#24900=DIRECTION('ref_axis',(-0.707106781186547,-0.707106781186548,0.));
#24901=DIRECTION('',(0.,0.,1.));
#24902=DIRECTION('center_axis',(0.,-1.,0.));
#24903=DIRECTION('ref_axis',(1.,0.,0.));
#24904=DIRECTION('',(-1.,0.,0.));
#24905=DIRECTION('',(0.,0.,-1.));
#24906=DIRECTION('center_axis',(0.,0.,1.));
#24907=DIRECTION('ref_axis',(0.707106781186548,-0.707106781186548,0.));
#24908=DIRECTION('center_axis',(0.,0.,1.));
#24909=DIRECTION('ref_axis',(0.707106781186548,-0.707106781186548,0.));
#24910=DIRECTION('',(0.,0.,1.));
#24911=DIRECTION('center_axis',(0.,0.,1.));
#24912=DIRECTION('ref_axis',(0.707106781186548,0.707106781186547,0.));
#24913=DIRECTION('',(0.,0.,-1.));
#24914=DIRECTION('center_axis',(0.,0.,1.));
#24915=DIRECTION('ref_axis',(0.707106781186548,0.707106781186547,0.));
#24916=DIRECTION('',(0.,0.,1.));
#24917=DIRECTION('center_axis',(0.,1.,0.));
#24918=DIRECTION('ref_axis',(-1.,0.,0.));
#24919=DIRECTION('',(1.,0.,0.));
#24920=DIRECTION('',(0.,0.,-1.));
#24921=DIRECTION('center_axis',(0.,0.,1.));
#24922=DIRECTION('ref_axis',(-0.707106781186548,0.707106781186547,0.));
#24923=DIRECTION('center_axis',(0.,0.,1.));
#24924=DIRECTION('ref_axis',(-0.707106781186548,0.707106781186547,0.));
#24925=DIRECTION('',(0.,0.,1.));
#24926=DIRECTION('center_axis',(0.,0.,1.));
#24927=DIRECTION('ref_axis',(0.707106781186548,-0.707106781186547,0.));
#24928=DIRECTION('center_axis',(0.,0.,-1.));
#24929=DIRECTION('ref_axis',(0.707106781186548,-0.707106781186547,0.));
#24930=DIRECTION('',(0.,0.,1.));
#24931=DIRECTION('',(0.,0.,-1.));
#24932=DIRECTION('center_axis',(0.,1.,0.));
#24933=DIRECTION('ref_axis',(-1.,0.,0.));
#24934=DIRECTION('',(1.,0.,0.));
#24935=DIRECTION('',(0.,0.,-1.));
#24936=DIRECTION('center_axis',(0.,0.,1.));
#24937=DIRECTION('ref_axis',(-0.707106781186547,-0.707106781186548,0.));
#24938=DIRECTION('center_axis',(0.,0.,-1.));
#24939=DIRECTION('ref_axis',(-0.707106781186547,-0.707106781186548,0.));
#24940=DIRECTION('',(0.,0.,1.));
#24941=DIRECTION('center_axis',(1.,0.,0.));
#24942=DIRECTION('ref_axis',(0.,1.,0.));
#24943=DIRECTION('',(0.,-1.,0.));
#24944=DIRECTION('',(0.,0.,-1.));
#24945=DIRECTION('center_axis',(0.,0.,1.));
#24946=DIRECTION('ref_axis',(-0.707106781186548,0.707106781186548,0.));
#24947=DIRECTION('center_axis',(0.,0.,-1.));
#24948=DIRECTION('ref_axis',(-0.707106781186548,0.707106781186548,0.));
#24949=DIRECTION('',(0.,0.,1.));
#24950=DIRECTION('center_axis',(0.,-1.,0.));
#24951=DIRECTION('ref_axis',(1.,0.,0.));
#24952=DIRECTION('',(-1.,0.,0.));
#24953=DIRECTION('',(0.,0.,-1.));
#24954=DIRECTION('center_axis',(0.,0.,1.));
#24955=DIRECTION('ref_axis',(0.707106781186548,0.707106781186548,0.));
#24956=DIRECTION('center_axis',(0.,0.,-1.));
#24957=DIRECTION('ref_axis',(0.707106781186548,0.707106781186548,0.));
#24958=DIRECTION('',(0.,0.,1.));
#24959=DIRECTION('center_axis',(-1.,0.,0.));
#24960=DIRECTION('ref_axis',(0.,-1.,0.));
#24961=DIRECTION('',(0.,1.,0.));
#24962=DIRECTION('',(0.,0.,-1.));
#24963=DIRECTION('center_axis',(0.,0.,1.));
#24964=DIRECTION('ref_axis',(-0.707106781186548,-0.707106781186547,0.));
#24965=DIRECTION('center_axis',(0.,0.,1.));
#24966=DIRECTION('ref_axis',(-0.707106781186548,-0.707106781186547,0.));
#24967=DIRECTION('',(0.,0.,1.));
#24968=DIRECTION('center_axis',(0.,0.,1.));
#24969=DIRECTION('ref_axis',(0.707106781186548,-0.707106781186547,0.));
#24970=DIRECTION('',(0.,0.,-1.));
#24971=DIRECTION('center_axis',(0.,0.,1.));
#24972=DIRECTION('ref_axis',(0.707106781186548,-0.707106781186547,0.));
#24973=DIRECTION('',(0.,0.,1.));
#24974=DIRECTION('center_axis',(1.,0.,0.));
#24975=DIRECTION('ref_axis',(0.,1.,0.));
#24976=DIRECTION('',(0.,-1.,0.));
#24977=DIRECTION('',(0.,0.,-1.));
#24978=DIRECTION('center_axis',(0.,0.,1.));
#24979=DIRECTION('ref_axis',(0.707106781186548,0.707106781186548,0.));
#24980=DIRECTION('center_axis',(0.,0.,1.));
#24981=DIRECTION('ref_axis',(0.707106781186548,0.707106781186548,0.));
#24982=DIRECTION('',(0.,0.,1.));
#24983=DIRECTION('center_axis',(0.,0.,1.));
#24984=DIRECTION('ref_axis',(-0.707106781186547,0.707106781186548,0.));
#24985=DIRECTION('',(0.,0.,-1.));
#24986=DIRECTION('center_axis',(0.,0.,1.));
#24987=DIRECTION('ref_axis',(-0.707106781186547,0.707106781186548,0.));
#24988=DIRECTION('',(0.,0.,1.));
#24989=DIRECTION('center_axis',(-1.,0.,0.));
#24990=DIRECTION('ref_axis',(0.,-1.,0.));
#24991=DIRECTION('',(0.,1.,0.));
#24992=DIRECTION('',(0.,0.,-1.));
#24993=DIRECTION('center_axis',(0.,0.,1.));
#24994=DIRECTION('ref_axis',(-0.707106781186547,-0.707106781186548,0.));
#24995=DIRECTION('center_axis',(0.,0.,1.));
#24996=DIRECTION('ref_axis',(-0.707106781186547,-0.707106781186548,0.));
#24997=DIRECTION('',(0.,0.,1.));
#24998=DIRECTION('center_axis',(0.,0.,1.));
#24999=DIRECTION('ref_axis',(0.707106781186547,0.707106781186548,0.));
#25000=DIRECTION('center_axis',(0.,0.,-1.));
#25001=DIRECTION('ref_axis',(0.707106781186547,0.707106781186548,0.));
#25002=DIRECTION('',(0.,0.,1.));
#25003=DIRECTION('',(0.,0.,-1.));
#25004=DIRECTION('center_axis',(-1.,0.,0.));
#25005=DIRECTION('ref_axis',(0.,-1.,0.));
#25006=DIRECTION('',(0.,1.,0.));
#25007=DIRECTION('',(0.,0.,-1.));
#25008=DIRECTION('center_axis',(0.,0.,1.));
#25009=DIRECTION('ref_axis',(0.707106781186548,-0.707106781186547,0.));
#25010=DIRECTION('center_axis',(0.,0.,-1.));
#25011=DIRECTION('ref_axis',(0.707106781186548,-0.707106781186547,0.));
#25012=DIRECTION('',(0.,0.,1.));
#25013=DIRECTION('center_axis',(0.,1.,0.));
#25014=DIRECTION('ref_axis',(-1.,0.,0.));
#25015=DIRECTION('',(1.,0.,0.));
#25016=DIRECTION('',(0.,0.,-1.));
#25017=DIRECTION('center_axis',(0.,0.,1.));
#25018=DIRECTION('ref_axis',(-0.707106781186548,-0.707106781186548,0.));
#25019=DIRECTION('center_axis',(0.,0.,-1.));
#25020=DIRECTION('ref_axis',(-0.707106781186548,-0.707106781186548,0.));
#25021=DIRECTION('',(0.,0.,1.));
#25022=DIRECTION('center_axis',(1.,0.,0.));
#25023=DIRECTION('ref_axis',(0.,1.,0.));
#25024=DIRECTION('',(0.,-1.,0.));
#25025=DIRECTION('',(0.,0.,-1.));
#25026=DIRECTION('center_axis',(0.,0.,1.));
#25027=DIRECTION('ref_axis',(-0.707106781186548,0.707106781186548,0.));
#25028=DIRECTION('center_axis',(0.,0.,-1.));
#25029=DIRECTION('ref_axis',(-0.707106781186548,0.707106781186548,0.));
#25030=DIRECTION('',(0.,0.,1.));
#25031=DIRECTION('center_axis',(0.,-1.,0.));
#25032=DIRECTION('ref_axis',(1.,0.,0.));
#25033=DIRECTION('',(-1.,0.,0.));
#25034=DIRECTION('',(0.,0.,-1.));
#25035=DIRECTION('center_axis',(0.,0.,1.));
#25036=DIRECTION('ref_axis',(0.707106781186547,-0.707106781186548,0.));
#25037=DIRECTION('center_axis',(0.,0.,1.));
#25038=DIRECTION('ref_axis',(0.707106781186547,-0.707106781186548,0.));
#25039=DIRECTION('',(0.,0.,1.));
#25040=DIRECTION('center_axis',(0.,0.,1.));
#25041=DIRECTION('ref_axis',(0.707106781186547,0.707106781186548,0.));
#25042=DIRECTION('',(0.,0.,-1.));
#25043=DIRECTION('center_axis',(0.,0.,1.));
#25044=DIRECTION('ref_axis',(0.707106781186547,0.707106781186548,0.));
#25045=DIRECTION('',(0.,0.,1.));
#25046=DIRECTION('center_axis',(0.,1.,0.));
#25047=DIRECTION('ref_axis',(-1.,0.,0.));
#25048=DIRECTION('',(1.,0.,0.));
#25049=DIRECTION('',(0.,0.,-1.));
#25050=DIRECTION('center_axis',(0.,0.,1.));
#25051=DIRECTION('ref_axis',(-0.707106781186548,0.707106781186548,0.));
#25052=DIRECTION('center_axis',(0.,0.,1.));
#25053=DIRECTION('ref_axis',(-0.707106781186548,0.707106781186548,0.));
#25054=DIRECTION('',(0.,0.,1.));
#25055=DIRECTION('center_axis',(0.,0.,1.));
#25056=DIRECTION('ref_axis',(-0.707106781186548,-0.707106781186547,0.));
#25057=DIRECTION('',(0.,0.,-1.));
#25058=DIRECTION('center_axis',(0.,0.,1.));
#25059=DIRECTION('ref_axis',(-0.707106781186548,-0.707106781186547,0.));
#25060=DIRECTION('center_axis',(0.,0.,1.));
#25061=DIRECTION('ref_axis',(1.,0.,0.));
#25062=DIRECTION('',(0.,0.,-1.));
#25063=DIRECTION('center_axis',(0.,0.,-1.));
#25064=DIRECTION('ref_axis',(1.,0.,0.));
#25065=DIRECTION('center_axis',(0.,0.,1.));
#25066=DIRECTION('ref_axis',(1.,0.,0.));
#25067=DIRECTION('',(0.,0.,-1.));
#25068=DIRECTION('center_axis',(0.,0.,-1.));
#25069=DIRECTION('ref_axis',(1.,0.,0.));
#25070=DIRECTION('center_axis',(0.,0.,1.));
#25071=DIRECTION('ref_axis',(1.,0.,0.));
#25072=DIRECTION('',(0.,0.,-1.));
#25073=DIRECTION('center_axis',(0.,0.,1.));
#25074=DIRECTION('ref_axis',(1.,0.,0.));
#25075=DIRECTION('',(0.,0.,-1.));
#25076=DIRECTION('center_axis',(0.,0.,-1.));
#25077=DIRECTION('ref_axis',(1.,0.,0.));
#25078=DIRECTION('center_axis',(0.,0.,1.));
#25079=DIRECTION('ref_axis',(1.,0.,0.));
#25080=DIRECTION('',(0.,0.,-1.));
#25081=DIRECTION('center_axis',(0.,0.,-1.));
#25082=DIRECTION('ref_axis',(1.,0.,0.));
#25083=DIRECTION('center_axis',(-1.,0.,0.));
#25084=DIRECTION('ref_axis',(0.,-1.,0.));
#25085=DIRECTION('',(0.,1.,0.));
#25086=DIRECTION('center_axis',(1.,0.,0.));
#25087=DIRECTION('ref_axis',(0.,1.,0.));
#25088=DIRECTION('',(0.,-1.,0.));
#25089=DIRECTION('center_axis',(0.,-1.,0.));
#25090=DIRECTION('ref_axis',(1.,0.,0.));
#25091=DIRECTION('',(-1.,0.,0.));
#25092=DIRECTION('center_axis',(0.,1.,0.));
#25093=DIRECTION('ref_axis',(-1.,0.,0.));
#25094=DIRECTION('',(1.,0.,0.));
#25095=DIRECTION('center_axis',(0.,-1.,0.));
#25096=DIRECTION('ref_axis',(1.,0.,0.));
#25097=DIRECTION('',(-1.,0.,0.));
#25098=DIRECTION('center_axis',(-1.,0.,0.));
#25099=DIRECTION('ref_axis',(0.,-1.,0.));
#25100=DIRECTION('',(0.,1.,0.));
#25101=DIRECTION('center_axis',(1.,0.,0.));
#25102=DIRECTION('ref_axis',(0.,1.,0.));
#25103=DIRECTION('',(0.,-1.,0.));
#25104=DIRECTION('center_axis',(-1.,0.,0.));
#25105=DIRECTION('ref_axis',(0.,-1.,0.));
#25106=DIRECTION('',(0.,1.,0.));
#25107=DIRECTION('center_axis',(0.,1.,0.));
#25108=DIRECTION('ref_axis',(-1.,0.,0.));
#25109=DIRECTION('',(1.,0.,0.));
#25110=DIRECTION('center_axis',(0.,-1.,0.));
#25111=DIRECTION('ref_axis',(1.,0.,0.));
#25112=DIRECTION('',(-1.,0.,0.));
#25113=DIRECTION('center_axis',(0.,1.,0.));
#25114=DIRECTION('ref_axis',(-1.,0.,0.));
#25115=DIRECTION('',(1.,0.,0.));
#25116=DIRECTION('center_axis',(1.,0.,0.));
#25117=DIRECTION('ref_axis',(0.,1.,0.));
#25118=DIRECTION('',(0.,-1.,0.));
#25119=DIRECTION('center_axis',(0.,0.,1.));
#25120=DIRECTION('ref_axis',(1.,0.,0.));
#25121=DIRECTION('axis',(0.,0.,1.));
#25122=DIRECTION('refdir',(1.,0.,0.));
#25123=DIRECTION('center_axis',(0.,0.,-1.));
#25124=DIRECTION('ref_axis',(1.,0.,0.));
#25125=DIRECTION('center_axis',(0.,0.,-1.));
#25126=DIRECTION('ref_axis',(1.,0.,0.));
#25127=DIRECTION('center_axis',(0.,0.,-1.));
#25128=DIRECTION('ref_axis',(1.,0.,0.));
#25129=DIRECTION('center_axis',(0.,0.,-1.));
#25130=DIRECTION('ref_axis',(1.,0.,0.));
#25131=DIRECTION('center_axis',(0.,0.,-1.));
#25132=DIRECTION('ref_axis',(1.,0.,0.));
#25133=DIRECTION('',(0.,0.,-1.));
#25134=DIRECTION('center_axis',(0.,0.,-1.));
#25135=DIRECTION('ref_axis',(1.,0.,0.));
#25136=DIRECTION('',(0.,0.,-1.));
#25137=DIRECTION('center_axis',(0.,0.,1.));
#25138=DIRECTION('ref_axis',(1.,0.,0.));
#25139=DIRECTION('center_axis',(0.,0.,-1.));
#25140=DIRECTION('ref_axis',(1.,0.,0.));
#25141=DIRECTION('center_axis',(0.,0.,-1.));
#25142=DIRECTION('ref_axis',(1.,0.,0.));
#25143=DIRECTION('',(0.,0.,-1.));
#25144=DIRECTION('center_axis',(0.,0.,1.));
#25145=DIRECTION('ref_axis',(1.,0.,0.));
#25146=DIRECTION('center_axis',(0.,0.,-1.));
#25147=DIRECTION('ref_axis',(1.,0.,0.));
#25148=DIRECTION('center_axis',(0.,0.,-1.));
#25149=DIRECTION('ref_axis',(1.,0.,0.));
#25150=DIRECTION('',(0.,0.,-1.));
#25151=DIRECTION('center_axis',(0.,0.,1.));
#25152=DIRECTION('ref_axis',(1.,0.,0.));
#25153=DIRECTION('center_axis',(0.,0.,-1.));
#25154=DIRECTION('ref_axis',(1.,0.,0.));
#25155=DIRECTION('center_axis',(0.,0.,-1.));
#25156=DIRECTION('ref_axis',(1.,0.,0.));
#25157=DIRECTION('',(0.,0.,-1.));
#25158=DIRECTION('center_axis',(0.,0.,1.));
#25159=DIRECTION('ref_axis',(1.,0.,0.));
#25160=DIRECTION('center_axis',(0.,0.,-1.));
#25161=DIRECTION('ref_axis',(1.,0.,0.));
#25162=DIRECTION('center_axis',(0.,0.,-1.));
#25163=DIRECTION('ref_axis',(1.,0.,0.));
#25164=DIRECTION('',(0.,0.,-1.));
#25165=DIRECTION('center_axis',(0.,0.,1.));
#25166=DIRECTION('ref_axis',(1.,0.,0.));
#25167=DIRECTION('center_axis',(0.,1.,0.));
#25168=DIRECTION('ref_axis',(-1.,0.,0.));
#25169=DIRECTION('',(-1.,0.,0.));
#25170=DIRECTION('',(0.,0.,1.));
#25171=DIRECTION('',(-1.,0.,0.));
#25172=DIRECTION('',(0.,0.,1.));
#25173=DIRECTION('center_axis',(1.,0.,0.));
#25174=DIRECTION('ref_axis',(0.,1.,0.));
#25175=DIRECTION('',(0.,1.,0.));
#25176=DIRECTION('',(0.,1.,0.));
#25177=DIRECTION('',(0.,0.,1.));
#25178=DIRECTION('center_axis',(0.,-1.,0.));
#25179=DIRECTION('ref_axis',(1.,0.,0.));
#25180=DIRECTION('',(1.,0.,0.));
#25181=DIRECTION('',(1.,0.,0.));
#25182=DIRECTION('',(0.,0.,1.));
#25183=DIRECTION('center_axis',(-1.,0.,0.));
#25184=DIRECTION('ref_axis',(0.,-1.,0.));
#25185=DIRECTION('',(0.,-1.,0.));
#25186=DIRECTION('',(0.,-1.,0.));
#25187=DIRECTION('center_axis',(0.,0.,1.));
#25188=DIRECTION('ref_axis',(1.,0.,0.));
#25189=DIRECTION('center_axis',(0.,0.,1.));
#25190=DIRECTION('ref_axis',(1.,0.,0.));
#25191=DIRECTION('axis',(0.,0.,1.));
#25192=DIRECTION('refdir',(1.,0.,0.));
#25193=DIRECTION('center_axis',(0.,0.,1.));
#25194=DIRECTION('ref_axis',(1.,0.,0.));
#25195=DIRECTION('',(0.,0.,-1.));
#25196=DIRECTION('center_axis',(0.,0.,-1.));
#25197=DIRECTION('ref_axis',(1.,0.,0.));
#25198=DIRECTION('center_axis',(0.,0.,1.));
#25199=DIRECTION('ref_axis',(1.,0.,0.));
#25200=DIRECTION('',(0.,0.,-1.));
#25201=DIRECTION('center_axis',(0.,0.,1.));
#25202=DIRECTION('ref_axis',(1.,0.,0.));
#25203=DIRECTION('',(0.,0.,-1.));
#25204=DIRECTION('center_axis',(0.,0.,1.));
#25205=DIRECTION('ref_axis',(1.,0.,0.));
#25206=DIRECTION('',(0.,0.,-1.));
#25207=DIRECTION('center_axis',(0.,0.,1.));
#25208=DIRECTION('ref_axis',(1.,0.,0.));
#25209=DIRECTION('',(0.,0.,-1.));
#25210=DIRECTION('center_axis',(0.,0.,1.));
#25211=DIRECTION('ref_axis',(1.,0.,0.));
#25212=DIRECTION('',(0.,0.,-1.));
#25213=DIRECTION('center_axis',(0.,0.,1.));
#25214=DIRECTION('ref_axis',(1.,0.,0.));
#25215=DIRECTION('',(0.,0.,-1.));
#25216=DIRECTION('center_axis',(0.,0.,1.));
#25217=DIRECTION('ref_axis',(1.,0.,0.));
#25218=DIRECTION('',(0.,0.,-1.));
#25219=DIRECTION('center_axis',(0.,0.,1.));
#25220=DIRECTION('ref_axis',(1.,0.,0.));
#25221=DIRECTION('',(0.,0.,-1.));
#25222=DIRECTION('center_axis',(0.,0.,1.));
#25223=DIRECTION('ref_axis',(1.,0.,0.));
#25224=DIRECTION('',(0.,0.,-1.));
#25225=DIRECTION('center_axis',(0.,0.,1.));
#25226=DIRECTION('ref_axis',(1.,0.,0.));
#25227=DIRECTION('',(0.,0.,-1.));
#25228=DIRECTION('center_axis',(0.,0.,1.));
#25229=DIRECTION('ref_axis',(1.,0.,0.));
#25230=DIRECTION('',(0.,0.,-1.));
#25231=DIRECTION('center_axis',(0.,0.,1.));
#25232=DIRECTION('ref_axis',(1.,0.,0.));
#25233=DIRECTION('',(0.,0.,-1.));
#25234=DIRECTION('center_axis',(0.,0.,1.));
#25235=DIRECTION('ref_axis',(1.,0.,0.));
#25236=DIRECTION('',(0.,0.,-1.));
#25237=DIRECTION('center_axis',(0.,0.,1.));
#25238=DIRECTION('ref_axis',(1.,0.,0.));
#25239=DIRECTION('',(0.,0.,-1.));
#25240=DIRECTION('center_axis',(0.,0.,1.));
#25241=DIRECTION('ref_axis',(1.,0.,0.));
#25242=DIRECTION('',(0.,0.,-1.));
#25243=DIRECTION('center_axis',(0.,0.,1.));
#25244=DIRECTION('ref_axis',(1.,0.,0.));
#25245=DIRECTION('',(0.,0.,-1.));
#25246=DIRECTION('center_axis',(0.,0.,1.));
#25247=DIRECTION('ref_axis',(1.,0.,0.));
#25248=DIRECTION('',(0.,0.,-1.));
#25249=DIRECTION('center_axis',(0.,0.,1.));
#25250=DIRECTION('ref_axis',(1.,0.,0.));
#25251=DIRECTION('',(0.,0.,-1.));
#25252=DIRECTION('center_axis',(0.,0.,1.));
#25253=DIRECTION('ref_axis',(0.997281310794726,-0.0736884464455154,0.));
#25254=DIRECTION('',(0.,0.,1.));
#25255=DIRECTION('center_axis',(0.,0.,-1.));
#25256=DIRECTION('ref_axis',(1.,1.00674340327557E-13,0.));
#25257=DIRECTION('center_axis',(0.,0.,1.));
#25258=DIRECTION('ref_axis',(1.,1.00674340327557E-13,0.));
#25259=DIRECTION('',(0.,0.,1.));
#25260=DIRECTION('center_axis',(0.,0.,1.));
#25261=DIRECTION('ref_axis',(1.,1.00674340327557E-13,0.));
#25262=DIRECTION('',(0.,0.,1.));
#25263=DIRECTION('center_axis',(0.,0.,1.));
#25264=DIRECTION('ref_axis',(1.,1.00674340327557E-13,0.));
#25265=DIRECTION('',(0.,0.,1.));
#25266=DIRECTION('center_axis',(0.,0.,1.));
#25267=DIRECTION('ref_axis',(1.,1.00674340327557E-13,0.));
#25268=DIRECTION('',(0.,0.,1.));
#25269=DIRECTION('center_axis',(0.,0.,1.));
#25270=DIRECTION('ref_axis',(1.,1.00674340327557E-13,0.));
#25271=DIRECTION('',(0.,0.,1.));
#25272=DIRECTION('center_axis',(0.,0.,1.));
#25273=DIRECTION('ref_axis',(1.,1.00674340327557E-13,0.));
#25274=DIRECTION('',(0.,0.,1.));
#25275=DIRECTION('center_axis',(0.,0.,1.));
#25276=DIRECTION('ref_axis',(1.,1.00674340327557E-13,0.));
#25277=DIRECTION('',(0.,0.,1.));
#25278=DIRECTION('center_axis',(0.,0.,1.));
#25279=DIRECTION('ref_axis',(1.,1.00674340327557E-13,0.));
#25280=DIRECTION('',(0.,0.,1.));
#25281=DIRECTION('center_axis',(0.,0.,1.));
#25282=DIRECTION('ref_axis',(1.,1.00674340327557E-13,0.));
#25283=DIRECTION('',(0.,0.,1.));
#25284=DIRECTION('center_axis',(0.,0.,1.));
#25285=DIRECTION('ref_axis',(1.,1.00674340327557E-13,0.));
#25286=DIRECTION('',(0.,0.,1.));
#25287=DIRECTION('center_axis',(0.,0.,1.));
#25288=DIRECTION('ref_axis',(1.,1.00674340327557E-13,0.));
#25289=DIRECTION('',(0.,0.,1.));
#25290=DIRECTION('center_axis',(0.,0.,1.));
#25291=DIRECTION('ref_axis',(1.,1.00674340327557E-13,0.));
#25292=DIRECTION('',(0.,0.,1.));
#25293=DIRECTION('center_axis',(0.,0.,1.));
#25294=DIRECTION('ref_axis',(1.,1.00674340327557E-13,0.));
#25295=DIRECTION('',(0.,0.,1.));
#25296=DIRECTION('center_axis',(0.,0.,1.));
#25297=DIRECTION('ref_axis',(1.,1.00674340327557E-13,0.));
#25298=DIRECTION('',(0.,0.,1.));
#25299=DIRECTION('center_axis',(0.,0.,1.));
#25300=DIRECTION('ref_axis',(1.,1.00674340327557E-13,0.));
#25301=DIRECTION('',(0.,0.,1.));
#25302=DIRECTION('center_axis',(0.,0.,1.));
#25303=DIRECTION('ref_axis',(1.,1.00674340327557E-13,0.));
#25304=DIRECTION('',(0.,0.,1.));
#25305=DIRECTION('center_axis',(0.,0.,1.));
#25306=DIRECTION('ref_axis',(1.,1.00674340327557E-13,0.));
#25307=DIRECTION('',(0.,0.,1.));
#25308=DIRECTION('center_axis',(0.,0.,1.));
#25309=DIRECTION('ref_axis',(1.,1.00674340327557E-13,0.));
#25310=DIRECTION('',(0.,0.,1.));
#25311=DIRECTION('center_axis',(0.,0.,-1.));
#25312=DIRECTION('ref_axis',(1.,0.,0.));
#25313=DIRECTION('center_axis',(0.,0.,-1.));
#25314=DIRECTION('ref_axis',(1.,0.,0.));
#25315=DIRECTION('',(0.707106781186547,8.65956056235493E-17,0.707106781186548));
#25316=DIRECTION('center_axis',(0.,0.,1.));
#25317=DIRECTION('ref_axis',(1.,0.,0.));
#25318=DIRECTION('center_axis',(0.,0.,1.));
#25319=DIRECTION('ref_axis',(1.,1.00674340327557E-13,0.));
#25320=DIRECTION('center_axis',(0.,0.,-1.));
#25321=DIRECTION('ref_axis',(1.,1.00674340327557E-13,0.));
#25322=DIRECTION('center_axis',(0.,0.,1.));
#25323=DIRECTION('ref_axis',(1.,0.,0.));
#25324=DIRECTION('center_axis',(-2.40370335797945E-16,-1.,0.));
#25325=DIRECTION('ref_axis',(1.,-2.40370335797945E-16,0.));
#25326=DIRECTION('',(1.,-2.40370335797945E-16,0.));
#25327=DIRECTION('',(0.,0.,1.));
#25328=DIRECTION('',(1.,-2.40370335797945E-16,0.));
#25329=DIRECTION('',(0.,0.,1.));
#25330=DIRECTION('center_axis',(-0.866025403784439,-0.5,0.));
#25331=DIRECTION('ref_axis',(0.5,-0.866025403784439,0.));
#25332=DIRECTION('',(0.5,-0.866025403784439,0.));
#25333=DIRECTION('',(0.,0.,1.));
#25334=DIRECTION('',(0.5,-0.866025403784439,0.));
#25335=DIRECTION('center_axis',(-0.866025403784439,0.5,0.));
#25336=DIRECTION('ref_axis',(-0.5,-0.866025403784439,0.));
#25337=DIRECTION('',(-0.5,-0.866025403784439,0.));
#25338=DIRECTION('',(0.,0.,1.));
#25339=DIRECTION('',(-0.5,-0.866025403784439,0.));
#25340=DIRECTION('center_axis',(1.20185167898973E-16,1.,0.));
#25341=DIRECTION('ref_axis',(-1.,1.20185167898973E-16,0.));
#25342=DIRECTION('',(-1.,1.20185167898973E-16,0.));
#25343=DIRECTION('',(0.,0.,1.));
#25344=DIRECTION('',(-1.,1.20185167898973E-16,0.));
#25345=DIRECTION('center_axis',(0.866025403784439,0.5,0.));
#25346=DIRECTION('ref_axis',(-0.5,0.866025403784439,0.));
#25347=DIRECTION('',(-0.5,0.866025403784439,0.));
#25348=DIRECTION('',(0.,0.,1.));
#25349=DIRECTION('',(-0.5,0.866025403784439,0.));
#25350=DIRECTION('center_axis',(0.866025403784439,-0.5,0.));
#25351=DIRECTION('ref_axis',(0.5,0.866025403784439,0.));
#25352=DIRECTION('',(0.5,0.866025403784439,0.));
#25353=DIRECTION('',(0.5,0.866025403784439,0.));
#25354=DIRECTION('center_axis',(0.,0.,1.));
#25355=DIRECTION('ref_axis',(1.,0.,0.));
#25356=DIRECTION('center_axis',(0.,0.,1.));
#25357=DIRECTION('ref_axis',(1.,0.,0.));
#25358=DIRECTION('center_axis',(0.,0.,1.));
#25359=DIRECTION('ref_axis',(1.,0.,0.));
#25360=DIRECTION('center_axis',(0.,0.,1.));
#25361=DIRECTION('ref_axis',(1.,0.,0.));
#25362=DIRECTION('',(0.,0.,-1.));
#25363=DIRECTION('center_axis',(0.,0.,1.));
#25364=DIRECTION('ref_axis',(1.,0.,0.));
#25365=DIRECTION('center_axis',(0.,0.,1.));
#25366=DIRECTION('ref_axis',(1.,0.,0.));
#25367=DIRECTION('center_axis',(0.,0.,1.));
#25368=DIRECTION('ref_axis',(1.,0.,0.));
#25369=DIRECTION('axis',(0.,0.,1.));
#25370=DIRECTION('refdir',(1.,0.,0.));
#25371=DIRECTION('center_axis',(0.,0.,1.));
#25372=DIRECTION('ref_axis',(1.,0.,0.));
#25373=DIRECTION('center_axis',(0.,0.,1.));
#25374=DIRECTION('ref_axis',(1.,0.,0.));
#25375=DIRECTION('',(0.,0.,-1.));
#25376=DIRECTION('center_axis',(0.,0.,1.));
#25377=DIRECTION('ref_axis',(1.,0.,0.));
#25378=DIRECTION('center_axis',(0.,0.,1.));
#25379=DIRECTION('ref_axis',(1.,0.,0.));
#25380=DIRECTION('center_axis',(0.,0.,1.));
#25381=DIRECTION('ref_axis',(1.,0.,0.));
#25382=DIRECTION('axis',(0.,0.,1.));
#25383=DIRECTION('refdir',(1.,0.,0.));
#25384=DIRECTION('center_axis',(0.,0.,-1.));
#25385=DIRECTION('ref_axis',(1.,0.,0.));
#25386=DIRECTION('',(0.,0.,-1.));
#25387=DIRECTION('center_axis',(0.,0.,1.));
#25388=DIRECTION('ref_axis',(1.,0.,0.));
#25389=DIRECTION('',(0.,0.,-1.));
#25390=DIRECTION('center_axis',(0.,0.,1.));
#25391=DIRECTION('ref_axis',(1.,0.,0.));
#25392=DIRECTION('center_axis',(0.,0.,1.));
#25393=DIRECTION('ref_axis',(1.,0.,0.));
#25394=DIRECTION('center_axis',(0.,0.,-1.));
#25395=DIRECTION('ref_axis',(1.,0.,0.));
#25396=DIRECTION('',(0.,0.,-1.));
#25397=DIRECTION('center_axis',(0.,0.,-1.));
#25398=DIRECTION('ref_axis',(1.,0.,0.));
#25399=DIRECTION('',(0.,0.,-1.));
#25400=DIRECTION('center_axis',(0.,0.,-1.));
#25401=DIRECTION('ref_axis',(1.,0.,0.));
#25402=DIRECTION('',(0.,0.,-1.));
#25403=DIRECTION('center_axis',(0.,0.,-1.));
#25404=DIRECTION('ref_axis',(1.,0.,0.));
#25405=DIRECTION('',(0.,0.,-1.));
#25406=DIRECTION('center_axis',(0.,0.,-1.));
#25407=DIRECTION('ref_axis',(1.,0.,0.));
#25408=DIRECTION('',(0.,0.,-1.));
#25409=DIRECTION('center_axis',(0.,0.,-1.));
#25410=DIRECTION('ref_axis',(1.,0.,0.));
#25411=DIRECTION('',(0.,0.,-1.));
#25412=DIRECTION('center_axis',(0.,0.,-1.));
#25413=DIRECTION('ref_axis',(0.937997876463511,-0.346641001253376,0.));
#25414=DIRECTION('',(0.,0.,-1.));
#25415=DIRECTION('center_axis',(0.,0.,-1.));
#25416=DIRECTION('ref_axis',(1.,0.,0.));
#25417=DIRECTION('center_axis',(0.,0.,-1.));
#25418=DIRECTION('ref_axis',(0.793233502010203,0.608917573476599,0.));
#25419=DIRECTION('',(1.22464679914735E-16,-2.67208401572961E-30,-1.));
#25420=DIRECTION('center_axis',(0.,0.,1.));
#25421=DIRECTION('ref_axis',(1.,-2.16967571364491E-14,0.));
#25422=DIRECTION('center_axis',(0.,0.,-1.));
#25423=DIRECTION('ref_axis',(1.,-2.16967571364491E-14,0.));
#25424=DIRECTION('',(1.22464679914735E-16,-2.67208401572961E-30,-1.));
#25425=DIRECTION('center_axis',(0.,0.,-1.));
#25426=DIRECTION('ref_axis',(1.,-2.16967571364491E-14,0.));
#25427=DIRECTION('',(1.22464679914735E-16,-2.67208401572961E-30,-1.));
#25428=DIRECTION('center_axis',(0.,0.,-1.));
#25429=DIRECTION('ref_axis',(1.,-2.16967571364491E-14,0.));
#25430=DIRECTION('',(1.22464679914735E-16,-2.67208401572961E-30,-1.));
#25431=DIRECTION('center_axis',(0.,0.,-1.));
#25432=DIRECTION('ref_axis',(1.,-2.16967571364491E-14,0.));
#25433=DIRECTION('',(1.22464679914735E-16,-2.67208401572961E-30,-1.));
#25434=DIRECTION('center_axis',(0.,0.,-1.));
#25435=DIRECTION('ref_axis',(1.,-2.16967571364491E-14,0.));
#25436=DIRECTION('',(1.22464679914735E-16,-2.67208401572961E-30,-1.));
#25437=DIRECTION('center_axis',(0.,0.,-1.));
#25438=DIRECTION('ref_axis',(1.,-2.16967571364491E-14,0.));
#25439=DIRECTION('',(1.22464679914735E-16,-2.67208401572961E-30,-1.));
#25440=DIRECTION('center_axis',(0.,0.,-1.));
#25441=DIRECTION('ref_axis',(-0.609100172155653,-0.793093298597305,0.));
#25442=DIRECTION('',(1.22464679914735E-16,-2.67208401572961E-30,-1.));
#25443=DIRECTION('center_axis',(0.,0.,-1.));
#25444=DIRECTION('ref_axis',(1.,-2.16967571364491E-14,0.));
#25445=DIRECTION('center_axis',(0.,0.,-1.));
#25446=DIRECTION('ref_axis',(1.,0.,0.));
#25447=DIRECTION('',(0.,0.,-1.));
#25448=DIRECTION('center_axis',(0.,0.,1.));
#25449=DIRECTION('ref_axis',(1.,0.,0.));
#25450=DIRECTION('',(0.,0.,-1.));
#25451=DIRECTION('center_axis',(0.,0.,1.));
#25452=DIRECTION('ref_axis',(1.,0.,0.));
#25453=DIRECTION('center_axis',(0.,0.,1.));
#25454=DIRECTION('ref_axis',(1.,0.,0.));
#25455=DIRECTION('center_axis',(0.,0.,-1.));
#25456=DIRECTION('ref_axis',(1.,0.,0.));
#25457=DIRECTION('',(0.,0.,-1.));
#25458=DIRECTION('center_axis',(0.,0.,-1.));
#25459=DIRECTION('ref_axis',(1.,0.,0.));
#25460=DIRECTION('',(0.,0.,-1.));
#25461=DIRECTION('center_axis',(0.,0.,-1.));
#25462=DIRECTION('ref_axis',(1.,0.,0.));
#25463=DIRECTION('',(0.,0.,-1.));
#25464=DIRECTION('center_axis',(0.,0.,-1.));
#25465=DIRECTION('ref_axis',(1.,0.,0.));
#25466=DIRECTION('',(0.,0.,-1.));
#25467=DIRECTION('center_axis',(0.,0.,-1.));
#25468=DIRECTION('ref_axis',(1.,0.,0.));
#25469=DIRECTION('',(0.,0.,-1.));
#25470=DIRECTION('center_axis',(0.,0.,-1.));
#25471=DIRECTION('ref_axis',(1.,0.,0.));
#25472=DIRECTION('',(0.,0.,-1.));
#25473=DIRECTION('center_axis',(0.,0.,-1.));
#25474=DIRECTION('ref_axis',(0.937998514609972,-0.346639274447495,0.));
#25475=DIRECTION('',(0.,0.,-1.));
#25476=DIRECTION('center_axis',(0.,0.,-1.));
#25477=DIRECTION('ref_axis',(1.,0.,0.));
#25478=DIRECTION('center_axis',(0.,0.,-1.));
#25479=DIRECTION('ref_axis',(0.793234421148473,0.608916376118468,0.));
#25480=DIRECTION('',(1.22464679914735E-16,-2.66923102573661E-30,-1.));
#25481=DIRECTION('center_axis',(0.,0.,1.));
#25482=DIRECTION('ref_axis',(1.,-2.16734607052251E-14,0.));
#25483=DIRECTION('center_axis',(0.,0.,-1.));
#25484=DIRECTION('ref_axis',(1.,-2.16734607052251E-14,0.));
#25485=DIRECTION('',(1.22464679914735E-16,-2.66923102573661E-30,-1.));
#25486=DIRECTION('center_axis',(0.,0.,-1.));
#25487=DIRECTION('ref_axis',(1.,-2.16734607052251E-14,0.));
#25488=DIRECTION('',(1.22464679914735E-16,-2.66923102573661E-30,-1.));
#25489=DIRECTION('center_axis',(0.,0.,-1.));
#25490=DIRECTION('ref_axis',(1.,-2.16734607052251E-14,0.));
#25491=DIRECTION('',(1.22464679914735E-16,-2.66923102573661E-30,-1.));
#25492=DIRECTION('center_axis',(0.,0.,-1.));
#25493=DIRECTION('ref_axis',(1.,-2.16734607052251E-14,0.));
#25494=DIRECTION('',(1.22464679914735E-16,-2.66923102573661E-30,-1.));
#25495=DIRECTION('center_axis',(0.,0.,-1.));
#25496=DIRECTION('ref_axis',(1.,-2.16734607052251E-14,0.));
#25497=DIRECTION('',(1.22464679914735E-16,-2.66923102573661E-30,-1.));
#25498=DIRECTION('center_axis',(0.,0.,-1.));
#25499=DIRECTION('ref_axis',(1.,-2.16734607052251E-14,0.));
#25500=DIRECTION('',(1.22464679914735E-16,-2.66923102573661E-30,-1.));
#25501=DIRECTION('center_axis',(0.,0.,-1.));
#25502=DIRECTION('ref_axis',(-0.609099316811134,-0.793093955506036,0.));
#25503=DIRECTION('',(1.22464679914735E-16,-2.66923102573661E-30,-1.));
#25504=DIRECTION('center_axis',(0.,0.,-1.));
#25505=DIRECTION('ref_axis',(1.,-2.16734607052251E-14,0.));
#25506=DIRECTION('center_axis',(0.,0.,-1.));
#25507=DIRECTION('ref_axis',(1.,0.,0.));
#25508=DIRECTION('',(0.,0.,-1.));
#25509=DIRECTION('center_axis',(0.,0.,1.));
#25510=DIRECTION('ref_axis',(1.,0.,0.));
#25511=DIRECTION('',(0.,0.,-1.));
#25512=DIRECTION('center_axis',(0.,0.,1.));
#25513=DIRECTION('ref_axis',(1.,0.,0.));
#25514=DIRECTION('center_axis',(0.,0.,1.));
#25515=DIRECTION('ref_axis',(1.,0.,0.));
#25516=DIRECTION('center_axis',(0.,0.,-1.));
#25517=DIRECTION('ref_axis',(1.,0.,0.));
#25518=DIRECTION('',(0.,0.,-1.));
#25519=DIRECTION('center_axis',(0.,0.,-1.));
#25520=DIRECTION('ref_axis',(1.,0.,0.));
#25521=DIRECTION('',(0.,0.,-1.));
#25522=DIRECTION('center_axis',(0.,0.,-1.));
#25523=DIRECTION('ref_axis',(1.,0.,0.));
#25524=DIRECTION('',(0.,0.,-1.));
#25525=DIRECTION('center_axis',(0.,0.,-1.));
#25526=DIRECTION('ref_axis',(1.,0.,0.));
#25527=DIRECTION('',(0.,0.,-1.));
#25528=DIRECTION('center_axis',(0.,0.,-1.));
#25529=DIRECTION('ref_axis',(1.,0.,0.));
#25530=DIRECTION('',(0.,0.,-1.));
#25531=DIRECTION('center_axis',(0.,0.,-1.));
#25532=DIRECTION('ref_axis',(1.,0.,0.));
#25533=DIRECTION('',(0.,0.,-1.));
#25534=DIRECTION('center_axis',(0.,0.,-1.));
#25535=DIRECTION('ref_axis',(0.937998542404131,-0.346639199237082,0.));
#25536=DIRECTION('',(0.,0.,-1.));
#25537=DIRECTION('center_axis',(0.,0.,-1.));
#25538=DIRECTION('ref_axis',(1.,0.,0.));
#25539=DIRECTION('center_axis',(0.,0.,-1.));
#25540=DIRECTION('ref_axis',(0.793234457633775,0.608916328589118,0.));
#25541=DIRECTION('',(1.22464679914735E-16,-2.66923102573661E-30,-1.));
#25542=DIRECTION('center_axis',(0.,0.,1.));
#25543=DIRECTION('ref_axis',(1.,-2.16734607052251E-14,0.));
#25544=DIRECTION('center_axis',(0.,0.,-1.));
#25545=DIRECTION('ref_axis',(1.,-2.16734607052251E-14,0.));
#25546=DIRECTION('',(1.22464679914735E-16,-2.66923102573661E-30,-1.));
#25547=DIRECTION('center_axis',(0.,0.,-1.));
#25548=DIRECTION('ref_axis',(1.,-2.16734607052251E-14,0.));
#25549=DIRECTION('',(1.22464679914735E-16,-2.66923102573661E-30,-1.));
#25550=DIRECTION('center_axis',(0.,0.,-1.));
#25551=DIRECTION('ref_axis',(1.,-2.16734607052251E-14,0.));
#25552=DIRECTION('',(1.22464679914735E-16,-2.66923102573661E-30,-1.));
#25553=DIRECTION('center_axis',(0.,0.,-1.));
#25554=DIRECTION('ref_axis',(1.,-2.16734607052251E-14,0.));
#25555=DIRECTION('',(1.22464679914735E-16,-2.66923102573661E-30,-1.));
#25556=DIRECTION('center_axis',(0.,0.,-1.));
#25557=DIRECTION('ref_axis',(1.,-2.16734607052251E-14,0.));
#25558=DIRECTION('',(1.22464679914735E-16,-2.66923102573661E-30,-1.));
#25559=DIRECTION('center_axis',(0.,0.,-1.));
#25560=DIRECTION('ref_axis',(1.,-2.16734607052251E-14,0.));
#25561=DIRECTION('',(1.22464679914735E-16,-2.66923102573661E-30,-1.));
#25562=DIRECTION('center_axis',(0.,0.,-1.));
#25563=DIRECTION('ref_axis',(-0.609099265708522,-0.793093994753042,0.));
#25564=DIRECTION('',(1.22464679914735E-16,-2.66923102573661E-30,-1.));
#25565=DIRECTION('center_axis',(0.,0.,-1.));
#25566=DIRECTION('ref_axis',(1.,-2.16734607052251E-14,0.));
#25567=DIRECTION('center_axis',(0.,0.,1.));
#25568=DIRECTION('ref_axis',(1.,0.,0.));
#25569=DIRECTION('center_axis',(0.,0.,-1.));
#25570=DIRECTION('ref_axis',(1.,-2.16734607052251E-14,0.));
#25571=DIRECTION('center_axis',(0.,0.,-1.));
#25572=DIRECTION('ref_axis',(1.,0.,0.));
#25573=DIRECTION('center_axis',(0.,0.,1.));
#25574=DIRECTION('ref_axis',(1.,0.,0.));
#25575=DIRECTION('center_axis',(0.,0.,-1.));
#25576=DIRECTION('ref_axis',(1.,-2.16734607052251E-14,0.));
#25577=DIRECTION('center_axis',(0.,0.,-1.));
#25578=DIRECTION('ref_axis',(1.,0.,0.));
#25579=DIRECTION('center_axis',(0.,0.,1.));
#25580=DIRECTION('ref_axis',(1.,0.,0.));
#25581=DIRECTION('center_axis',(0.,0.,-1.));
#25582=DIRECTION('ref_axis',(1.,-2.16967571364491E-14,0.));
#25583=DIRECTION('center_axis',(0.,0.,-1.));
#25584=DIRECTION('ref_axis',(1.,0.,0.));
#25585=DIRECTION('center_axis',(0.,0.,-1.));
#25586=DIRECTION('ref_axis',(1.,0.,0.));
#25587=DIRECTION('center_axis',(0.,0.,-1.));
#25588=DIRECTION('ref_axis',(1.,0.,0.));
#25589=DIRECTION('center_axis',(0.,0.,-1.));
#25590=DIRECTION('ref_axis',(1.,0.,0.));
#25591=DIRECTION('center_axis',(6.12323399573677E-17,0.,1.));
#25592=DIRECTION('ref_axis',(1.,0.,0.));
#25593=DIRECTION('center_axis',(0.,0.,-1.));
#25594=DIRECTION('ref_axis',(0.,1.,0.));
#25595=DIRECTION('center_axis',(-1.22464679914735E-16,1.,0.));
#25596=DIRECTION('ref_axis',(-1.,-1.22464679914735E-16,0.));
#25597=DIRECTION('center_axis',(0.,0.,1.));
#25598=DIRECTION('ref_axis',(1.,0.,0.));
#25599=DIRECTION('center_axis',(0.,0.,1.));
#25600=DIRECTION('ref_axis',(1.,0.,0.));
#25601=DIRECTION('',(0.,0.,-1.));
#25602=DIRECTION('center_axis',(0.,0.,1.));
#25603=DIRECTION('ref_axis',(1.,0.,0.));
#25604=DIRECTION('center_axis',(0.,0.,1.));
#25605=DIRECTION('ref_axis',(1.,0.,0.));
#25606=DIRECTION('center_axis',(0.,0.,1.));
#25607=DIRECTION('ref_axis',(1.,0.,0.));
#25608=DIRECTION('axis',(0.,0.,1.));
#25609=DIRECTION('refdir',(1.,0.,0.));
#25610=DIRECTION('center_axis',(0.,0.,-1.));
#25611=DIRECTION('ref_axis',(1.,0.,0.));
#25612=DIRECTION('center_axis',(0.,0.,-1.));
#25613=DIRECTION('ref_axis',(1.,0.,0.));
#25614=DIRECTION('',(0.,0.,-1.));
#25615=DIRECTION('center_axis',(0.,0.,1.));
#25616=DIRECTION('ref_axis',(1.,0.,0.));
#25617=DIRECTION('center_axis',(0.,0.,-1.));
#25618=DIRECTION('ref_axis',(1.,0.,0.));
#25619=DIRECTION('center_axis',(0.,0.,-1.));
#25620=DIRECTION('ref_axis',(1.,0.,0.));
#25621=DIRECTION('',(0.,0.,-1.));
#25622=DIRECTION('center_axis',(0.,0.,1.));
#25623=DIRECTION('ref_axis',(1.,0.,0.));
#25624=DIRECTION('center_axis',(0.,0.,-1.));
#25625=DIRECTION('ref_axis',(1.,0.,0.));
#25626=DIRECTION('center_axis',(0.,0.,-1.));
#25627=DIRECTION('ref_axis',(1.,0.,0.));
#25628=DIRECTION('',(0.,0.,-1.));
#25629=DIRECTION('center_axis',(0.,0.,1.));
#25630=DIRECTION('ref_axis',(1.,0.,0.));
#25631=DIRECTION('center_axis',(6.12323399573677E-17,0.,1.));
#25632=DIRECTION('ref_axis',(1.,0.,0.));
#25633=DIRECTION('center_axis',(0.,0.,1.));
#25634=DIRECTION('ref_axis',(0.,-1.,0.));
#25635=DIRECTION('center_axis',(-1.22464679914735E-16,1.,0.));
#25636=DIRECTION('ref_axis',(-1.,-1.22464679914735E-16,0.));
#25637=DIRECTION('center_axis',(0.,0.,-1.));
#25638=DIRECTION('ref_axis',(1.,0.,0.));
#25639=DIRECTION('center_axis',(0.,0.,1.));
#25640=DIRECTION('ref_axis',(1.,0.,0.));
#25641=DIRECTION('center_axis',(0.,0.,-1.));
#25642=DIRECTION('ref_axis',(1.,0.,0.));
#25643=DIRECTION('',(0.,0.,-1.));
#25644=DIRECTION('center_axis',(0.,0.,1.));
#25645=DIRECTION('ref_axis',(1.,0.,0.));
#25646=DIRECTION('center_axis',(0.,0.,1.));
#25647=DIRECTION('ref_axis',(1.,0.,0.));
#25648=DIRECTION('',(0.,0.,-1.));
#25649=DIRECTION('center_axis',(0.,0.,1.));
#25650=DIRECTION('ref_axis',(1.,0.,0.));
#25651=DIRECTION('center_axis',(0.,0.,1.));
#25652=DIRECTION('ref_axis',(1.,0.,0.));
#25653=DIRECTION('center_axis',(0.,0.,1.));
#25654=DIRECTION('ref_axis',(1.,0.,0.));
#25655=DIRECTION('axis',(0.,0.,1.));
#25656=DIRECTION('refdir',(1.,0.,0.));
#25657=DIRECTION('center_axis',(0.,0.,1.));
#25658=DIRECTION('ref_axis',(1.,0.,0.));
#25659=DIRECTION('',(0.,0.,-1.));
#25660=DIRECTION('center_axis',(0.,0.,-1.));
#25661=DIRECTION('ref_axis',(1.,0.,0.));
#25662=DIRECTION('center_axis',(0.,0.,1.));
#25663=DIRECTION('ref_axis',(1.,0.,0.));
#25664=DIRECTION('',(0.,0.,-1.));
#25665=DIRECTION('center_axis',(0.,0.,1.));
#25666=DIRECTION('ref_axis',(1.,0.,0.));
#25667=DIRECTION('',(0.,0.,-1.));
#25668=DIRECTION('center_axis',(0.,0.,1.));
#25669=DIRECTION('ref_axis',(1.,0.,0.));
#25670=DIRECTION('',(0.,0.,-1.));
#25671=DIRECTION('center_axis',(0.,0.,1.));
#25672=DIRECTION('ref_axis',(1.,0.,0.));
#25673=DIRECTION('',(0.,0.,-1.));
#25674=DIRECTION('center_axis',(0.,0.,1.));
#25675=DIRECTION('ref_axis',(1.,0.,0.));
#25676=DIRECTION('',(0.,0.,-1.));
#25677=DIRECTION('center_axis',(0.,0.,1.));
#25678=DIRECTION('ref_axis',(1.,0.,0.));
#25679=DIRECTION('',(0.,0.,-1.));
#25680=DIRECTION('center_axis',(0.,0.,1.));
#25681=DIRECTION('ref_axis',(1.,0.,0.));
#25682=DIRECTION('',(0.,0.,-1.));
#25683=DIRECTION('center_axis',(0.,0.,1.));
#25684=DIRECTION('ref_axis',(1.,0.,0.));
#25685=DIRECTION('',(0.,0.,-1.));
#25686=DIRECTION('center_axis',(0.,0.,1.));
#25687=DIRECTION('ref_axis',(1.,0.,0.));
#25688=DIRECTION('',(0.,0.,-1.));
#25689=DIRECTION('center_axis',(0.,0.,1.));
#25690=DIRECTION('ref_axis',(1.,0.,0.));
#25691=DIRECTION('',(0.,0.,-1.));
#25692=DIRECTION('center_axis',(0.,0.,1.));
#25693=DIRECTION('ref_axis',(1.,0.,0.));
#25694=DIRECTION('',(0.,0.,-1.));
#25695=DIRECTION('center_axis',(0.,0.,1.));
#25696=DIRECTION('ref_axis',(1.,0.,0.));
#25697=DIRECTION('',(0.,0.,-1.));
#25698=DIRECTION('center_axis',(0.,0.,1.));
#25699=DIRECTION('ref_axis',(1.,0.,0.));
#25700=DIRECTION('',(0.,0.,-1.));
#25701=DIRECTION('center_axis',(0.,0.,1.));
#25702=DIRECTION('ref_axis',(1.,0.,0.));
#25703=DIRECTION('',(0.,0.,-1.));
#25704=DIRECTION('center_axis',(0.,0.,1.));
#25705=DIRECTION('ref_axis',(1.,0.,0.));
#25706=DIRECTION('',(0.,0.,-1.));
#25707=DIRECTION('center_axis',(0.,0.,1.));
#25708=DIRECTION('ref_axis',(1.,0.,0.));
#25709=DIRECTION('',(0.,0.,-1.));
#25710=DIRECTION('center_axis',(0.,0.,1.));
#25711=DIRECTION('ref_axis',(1.,0.,0.));
#25712=DIRECTION('',(0.,0.,-1.));
#25713=DIRECTION('center_axis',(0.,0.,1.));
#25714=DIRECTION('ref_axis',(1.,0.,0.));
#25715=DIRECTION('',(0.,0.,-1.));
#25716=DIRECTION('center_axis',(0.,0.,1.));
#25717=DIRECTION('ref_axis',(1.,0.,0.));
#25718=DIRECTION('',(0.,0.,-1.));
#25719=DIRECTION('center_axis',(0.,0.,1.));
#25720=DIRECTION('ref_axis',(1.,0.,0.));
#25721=DIRECTION('',(0.,0.,-1.));
#25722=DIRECTION('center_axis',(0.,0.,1.));
#25723=DIRECTION('ref_axis',(1.,0.,0.));
#25724=DIRECTION('',(0.,0.,-1.));
#25725=DIRECTION('center_axis',(0.,0.,1.));
#25726=DIRECTION('ref_axis',(1.,0.,0.));
#25727=DIRECTION('',(0.,0.,-1.));
#25728=DIRECTION('center_axis',(0.,0.,1.));
#25729=DIRECTION('ref_axis',(1.,0.,0.));
#25730=DIRECTION('',(0.,0.,-1.));
#25731=DIRECTION('center_axis',(0.,0.,1.));
#25732=DIRECTION('ref_axis',(1.,0.,0.));
#25733=DIRECTION('',(0.,0.,-1.));
#25734=DIRECTION('center_axis',(0.,0.,1.));
#25735=DIRECTION('ref_axis',(1.,0.,0.));
#25736=DIRECTION('',(0.,0.,-1.));
#25737=DIRECTION('center_axis',(0.,0.,1.));
#25738=DIRECTION('ref_axis',(1.,0.,0.));
#25739=DIRECTION('',(0.,0.,-1.));
#25740=DIRECTION('center_axis',(0.,0.,1.));
#25741=DIRECTION('ref_axis',(1.,0.,0.));
#25742=DIRECTION('',(0.,0.,-1.));
#25743=DIRECTION('center_axis',(0.,0.,1.));
#25744=DIRECTION('ref_axis',(1.,0.,0.));
#25745=DIRECTION('',(0.,0.,-1.));
#25746=DIRECTION('center_axis',(0.,0.,1.));
#25747=DIRECTION('ref_axis',(1.,0.,0.));
#25748=DIRECTION('',(0.,0.,-1.));
#25749=DIRECTION('center_axis',(0.,0.,1.));
#25750=DIRECTION('ref_axis',(1.,0.,0.));
#25751=DIRECTION('',(0.,0.,-1.));
#25752=DIRECTION('center_axis',(0.,0.,1.));
#25753=DIRECTION('ref_axis',(1.,0.,0.));
#25754=DIRECTION('',(0.,0.,-1.));
#25755=DIRECTION('center_axis',(0.,0.,1.));
#25756=DIRECTION('ref_axis',(1.,0.,0.));
#25757=DIRECTION('',(0.,0.,-1.));
#25758=DIRECTION('center_axis',(0.,0.,1.));
#25759=DIRECTION('ref_axis',(1.,0.,0.));
#25760=DIRECTION('',(0.,0.,-1.));
#25761=DIRECTION('center_axis',(0.,0.,1.));
#25762=DIRECTION('ref_axis',(1.,0.,0.));
#25763=DIRECTION('',(0.,0.,-1.));
#25764=DIRECTION('center_axis',(0.,0.,1.));
#25765=DIRECTION('ref_axis',(1.,0.,0.));
#25766=DIRECTION('',(0.,0.,-1.));
#25767=DIRECTION('center_axis',(0.,0.,1.));
#25768=DIRECTION('ref_axis',(1.,0.,0.));
#25769=DIRECTION('',(0.,0.,-1.));
#25770=DIRECTION('center_axis',(0.,0.,1.));
#25771=DIRECTION('ref_axis',(1.,0.,0.));
#25772=DIRECTION('',(0.,0.,-1.));
#25773=DIRECTION('center_axis',(0.,0.,1.));
#25774=DIRECTION('ref_axis',(1.,0.,0.));
#25775=DIRECTION('',(0.,0.,-1.));
#25776=DIRECTION('center_axis',(0.,0.,1.));
#25777=DIRECTION('ref_axis',(1.,0.,0.));
#25778=DIRECTION('',(0.,0.,-1.));
#25779=DIRECTION('center_axis',(0.,0.,1.));
#25780=DIRECTION('ref_axis',(1.,0.,0.));
#25781=DIRECTION('',(0.,0.,-1.));
#25782=DIRECTION('center_axis',(0.,0.,1.));
#25783=DIRECTION('ref_axis',(1.,0.,0.));
#25784=DIRECTION('',(0.,0.,-1.));
#25785=DIRECTION('center_axis',(0.,0.,1.));
#25786=DIRECTION('ref_axis',(1.,0.,0.));
#25787=DIRECTION('',(0.,0.,-1.));
#25788=DIRECTION('center_axis',(0.,0.,1.));
#25789=DIRECTION('ref_axis',(1.,0.,0.));
#25790=DIRECTION('',(0.,0.,-1.));
#25791=DIRECTION('center_axis',(0.,0.,1.));
#25792=DIRECTION('ref_axis',(1.,0.,0.));
#25793=DIRECTION('',(0.,0.,-1.));
#25794=DIRECTION('center_axis',(0.,0.,1.));
#25795=DIRECTION('ref_axis',(1.,0.,0.));
#25796=DIRECTION('',(0.,0.,-1.));
#25797=DIRECTION('center_axis',(0.,0.,1.));
#25798=DIRECTION('ref_axis',(1.,0.,0.));
#25799=DIRECTION('',(0.,0.,-1.));
#25800=DIRECTION('center_axis',(0.,0.,1.));
#25801=DIRECTION('ref_axis',(1.,0.,0.));
#25802=DIRECTION('',(0.,0.,-1.));
#25803=DIRECTION('center_axis',(0.,0.,1.));
#25804=DIRECTION('ref_axis',(1.,0.,0.));
#25805=DIRECTION('',(0.,0.,-1.));
#25806=DIRECTION('center_axis',(0.,0.,1.));
#25807=DIRECTION('ref_axis',(1.,0.,0.));
#25808=DIRECTION('',(0.,0.,-1.));
#25809=DIRECTION('center_axis',(0.,0.,1.));
#25810=DIRECTION('ref_axis',(1.,0.,0.));
#25811=DIRECTION('',(0.,0.,-1.));
#25812=DIRECTION('center_axis',(0.,0.,1.));
#25813=DIRECTION('ref_axis',(1.,0.,0.));
#25814=DIRECTION('',(0.,0.,-1.));
#25815=DIRECTION('center_axis',(0.,0.,1.));
#25816=DIRECTION('ref_axis',(1.,0.,0.));
#25817=DIRECTION('',(0.,0.,-1.));
#25818=DIRECTION('center_axis',(0.,0.,1.));
#25819=DIRECTION('ref_axis',(1.,0.,0.));
#25820=DIRECTION('',(0.,0.,-1.));
#25821=DIRECTION('center_axis',(0.,0.,1.));
#25822=DIRECTION('ref_axis',(1.,0.,0.));
#25823=DIRECTION('',(0.,0.,-1.));
#25824=DIRECTION('center_axis',(0.,0.,1.));
#25825=DIRECTION('ref_axis',(1.,0.,0.));
#25826=DIRECTION('',(0.,0.,-1.));
#25827=DIRECTION('center_axis',(0.,0.,1.));
#25828=DIRECTION('ref_axis',(1.,0.,0.));
#25829=DIRECTION('',(0.,0.,-1.));
#25830=DIRECTION('center_axis',(0.,0.,1.));
#25831=DIRECTION('ref_axis',(1.,0.,0.));
#25832=DIRECTION('',(0.,0.,-1.));
#25833=DIRECTION('center_axis',(0.,0.,1.));
#25834=DIRECTION('ref_axis',(1.,0.,0.));
#25835=DIRECTION('',(0.,0.,-1.));
#25836=DIRECTION('center_axis',(0.,0.,1.));
#25837=DIRECTION('ref_axis',(1.,0.,0.));
#25838=DIRECTION('',(0.,0.,-1.));
#25839=DIRECTION('center_axis',(0.,0.,1.));
#25840=DIRECTION('ref_axis',(-0.457630590434842,-0.889142419805881,0.));
#25841=DIRECTION('',(0.,0.,1.));
#25842=DIRECTION('center_axis',(0.,0.,1.));
#25843=DIRECTION('ref_axis',(1.,-8.75189148499889E-13,0.));
#25844=DIRECTION('center_axis',(0.,0.,1.));
#25845=DIRECTION('ref_axis',(1.,-8.75189148499889E-13,0.));
#25846=DIRECTION('',(0.,0.,1.));
#25847=DIRECTION('center_axis',(0.,0.,1.));
#25848=DIRECTION('ref_axis',(1.,-8.75189148499889E-13,0.));
#25849=DIRECTION('',(0.,0.,1.));
#25850=DIRECTION('center_axis',(0.,0.,1.));
#25851=DIRECTION('ref_axis',(1.,-8.75189148499889E-13,0.));
#25852=DIRECTION('',(0.,0.,1.));
#25853=DIRECTION('center_axis',(0.,0.,1.));
#25854=DIRECTION('ref_axis',(1.,-8.75189148499889E-13,0.));
#25855=DIRECTION('',(0.,0.,1.));
#25856=DIRECTION('center_axis',(0.,0.,1.));
#25857=DIRECTION('ref_axis',(1.,-8.75189148499889E-13,0.));
#25858=DIRECTION('',(0.,0.,1.));
#25859=DIRECTION('center_axis',(0.,0.,1.));
#25860=DIRECTION('ref_axis',(1.,-8.75189148499889E-13,0.));
#25861=DIRECTION('',(0.,0.,1.));
#25862=DIRECTION('center_axis',(0.,0.,1.));
#25863=DIRECTION('ref_axis',(1.,-8.75189148499889E-13,0.));
#25864=DIRECTION('',(0.,0.,1.));
#25865=DIRECTION('center_axis',(0.,0.,1.));
#25866=DIRECTION('ref_axis',(1.,-8.75189148499889E-13,0.));
#25867=DIRECTION('',(0.,0.,1.));
#25868=DIRECTION('center_axis',(0.,0.,1.));
#25869=DIRECTION('ref_axis',(1.,-8.75189148499889E-13,0.));
#25870=DIRECTION('',(0.,0.,1.));
#25871=DIRECTION('center_axis',(0.,0.,1.));
#25872=DIRECTION('ref_axis',(1.,-8.75189148499889E-13,0.));
#25873=DIRECTION('',(0.,0.,1.));
#25874=DIRECTION('center_axis',(0.,0.,1.));
#25875=DIRECTION('ref_axis',(1.,-8.75189148499889E-13,0.));
#25876=DIRECTION('',(0.,0.,1.));
#25877=DIRECTION('center_axis',(0.,0.,1.));
#25878=DIRECTION('ref_axis',(1.,-8.75189148499889E-13,0.));
#25879=DIRECTION('',(0.,0.,1.));
#25880=DIRECTION('center_axis',(0.,0.,1.));
#25881=DIRECTION('ref_axis',(1.,-8.75189148499889E-13,0.));
#25882=DIRECTION('',(0.,0.,1.));
#25883=DIRECTION('center_axis',(0.,0.,1.));
#25884=DIRECTION('ref_axis',(1.,-8.75189148499889E-13,0.));
#25885=DIRECTION('',(0.,0.,1.));
#25886=DIRECTION('center_axis',(0.,0.,1.));
#25887=DIRECTION('ref_axis',(1.,-8.75189148499889E-13,0.));
#25888=DIRECTION('',(0.,0.,1.));
#25889=DIRECTION('center_axis',(0.,0.,1.));
#25890=DIRECTION('ref_axis',(1.,-8.75189148499889E-13,0.));
#25891=DIRECTION('',(0.,0.,1.));
#25892=DIRECTION('center_axis',(0.,0.,1.));
#25893=DIRECTION('ref_axis',(1.,-8.75189148499889E-13,0.));
#25894=DIRECTION('',(0.,0.,1.));
#25895=DIRECTION('center_axis',(0.,0.,1.));
#25896=DIRECTION('ref_axis',(1.,-8.75189148499889E-13,0.));
#25897=DIRECTION('',(0.,0.,1.));
#25898=DIRECTION('center_axis',(0.,0.,1.));
#25899=DIRECTION('ref_axis',(1.,-8.75189148499889E-13,0.));
#25900=DIRECTION('',(0.,0.,1.));
#25901=DIRECTION('center_axis',(0.,0.,1.));
#25902=DIRECTION('ref_axis',(1.,-8.75189148499889E-13,0.));
#25903=DIRECTION('',(0.,0.,1.));
#25904=DIRECTION('center_axis',(0.,0.,1.));
#25905=DIRECTION('ref_axis',(1.,-8.75189148499889E-13,0.));
#25906=DIRECTION('',(0.,0.,1.));
#25907=DIRECTION('center_axis',(0.,0.,1.));
#25908=DIRECTION('ref_axis',(1.,-8.75189148499889E-13,0.));
#25909=DIRECTION('',(0.,0.,1.));
#25910=DIRECTION('center_axis',(0.,0.,1.));
#25911=DIRECTION('ref_axis',(1.,-8.75189148499889E-13,0.));
#25912=DIRECTION('',(0.,0.,1.));
#25913=DIRECTION('center_axis',(0.,0.,1.));
#25914=DIRECTION('ref_axis',(1.,-8.75189148499889E-13,0.));
#25915=DIRECTION('',(0.,0.,1.));
#25916=DIRECTION('center_axis',(0.,0.,1.));
#25917=DIRECTION('ref_axis',(1.,-8.75189148499889E-13,0.));
#25918=DIRECTION('',(0.,0.,1.));
#25919=DIRECTION('center_axis',(0.,0.,1.));
#25920=DIRECTION('ref_axis',(1.,-8.75189148499889E-13,0.));
#25921=DIRECTION('',(0.,0.,1.));
#25922=DIRECTION('center_axis',(0.,0.,1.));
#25923=DIRECTION('ref_axis',(1.,-8.75189148499889E-13,0.));
#25924=DIRECTION('',(0.,0.,1.));
#25925=DIRECTION('center_axis',(0.,0.,1.));
#25926=DIRECTION('ref_axis',(1.,-8.75189148499889E-13,0.));
#25927=DIRECTION('',(0.,0.,1.));
#25928=DIRECTION('center_axis',(0.,0.,1.));
#25929=DIRECTION('ref_axis',(1.,-8.75189148499889E-13,0.));
#25930=DIRECTION('',(0.,0.,1.));
#25931=DIRECTION('center_axis',(0.,0.,1.));
#25932=DIRECTION('ref_axis',(1.,-8.75189148499889E-13,0.));
#25933=DIRECTION('',(0.,0.,1.));
#25934=DIRECTION('center_axis',(0.,0.,1.));
#25935=DIRECTION('ref_axis',(1.,-8.75189148499889E-13,0.));
#25936=DIRECTION('',(0.,0.,1.));
#25937=DIRECTION('center_axis',(0.,0.,1.));
#25938=DIRECTION('ref_axis',(1.,-8.75189148499889E-13,0.));
#25939=DIRECTION('',(0.,0.,1.));
#25940=DIRECTION('center_axis',(0.,0.,1.));
#25941=DIRECTION('ref_axis',(1.,-8.75189148499889E-13,0.));
#25942=DIRECTION('',(0.,0.,1.));
#25943=DIRECTION('center_axis',(0.,0.,1.));
#25944=DIRECTION('ref_axis',(1.,-8.75189148499889E-13,0.));
#25945=DIRECTION('',(0.,0.,1.));
#25946=DIRECTION('center_axis',(0.,0.,1.));
#25947=DIRECTION('ref_axis',(1.,-8.75189148499889E-13,0.));
#25948=DIRECTION('',(0.,0.,1.));
#25949=DIRECTION('center_axis',(0.,0.,1.));
#25950=DIRECTION('ref_axis',(1.,-8.75189148499889E-13,0.));
#25951=DIRECTION('',(0.,0.,1.));
#25952=DIRECTION('center_axis',(0.,0.,1.));
#25953=DIRECTION('ref_axis',(1.,-8.75189148499889E-13,0.));
#25954=DIRECTION('',(0.,0.,1.));
#25955=DIRECTION('center_axis',(0.,0.,1.));
#25956=DIRECTION('ref_axis',(1.,-8.75189148499889E-13,0.));
#25957=DIRECTION('',(0.,0.,1.));
#25958=DIRECTION('center_axis',(0.,0.,1.));
#25959=DIRECTION('ref_axis',(1.,-8.75189148499889E-13,0.));
#25960=DIRECTION('',(0.,0.,1.));
#25961=DIRECTION('center_axis',(0.,0.,1.));
#25962=DIRECTION('ref_axis',(1.,-8.75189148499889E-13,0.));
#25963=DIRECTION('',(0.,0.,1.));
#25964=DIRECTION('center_axis',(0.,0.,1.));
#25965=DIRECTION('ref_axis',(1.,-8.75189148499889E-13,0.));
#25966=DIRECTION('',(0.,0.,1.));
#25967=DIRECTION('center_axis',(0.,0.,1.));
#25968=DIRECTION('ref_axis',(1.,-8.75189148499889E-13,0.));
#25969=DIRECTION('',(0.,0.,1.));
#25970=DIRECTION('center_axis',(0.,0.,1.));
#25971=DIRECTION('ref_axis',(1.,-8.75189148499889E-13,0.));
#25972=DIRECTION('',(0.,0.,1.));
#25973=DIRECTION('center_axis',(0.,0.,1.));
#25974=DIRECTION('ref_axis',(1.,-8.75189148499889E-13,0.));
#25975=DIRECTION('',(0.,0.,1.));
#25976=DIRECTION('center_axis',(0.,0.,1.));
#25977=DIRECTION('ref_axis',(1.,-8.75189148499889E-13,0.));
#25978=DIRECTION('',(0.,0.,1.));
#25979=DIRECTION('center_axis',(0.,0.,1.));
#25980=DIRECTION('ref_axis',(1.,-8.75189148499889E-13,0.));
#25981=DIRECTION('',(0.,0.,1.));
#25982=DIRECTION('center_axis',(0.,0.,1.));
#25983=DIRECTION('ref_axis',(1.,-8.75189148499889E-13,0.));
#25984=DIRECTION('',(0.,0.,1.));
#25985=DIRECTION('center_axis',(0.,0.,1.));
#25986=DIRECTION('ref_axis',(1.,-8.75189148499889E-13,0.));
#25987=DIRECTION('',(0.,0.,1.));
#25988=DIRECTION('center_axis',(0.,0.,1.));
#25989=DIRECTION('ref_axis',(1.,-8.75189148499889E-13,0.));
#25990=DIRECTION('',(0.,0.,1.));
#25991=DIRECTION('center_axis',(0.,0.,1.));
#25992=DIRECTION('ref_axis',(1.,-8.75189148499889E-13,0.));
#25993=DIRECTION('',(0.,0.,1.));
#25994=DIRECTION('center_axis',(0.,0.,1.));
#25995=DIRECTION('ref_axis',(1.,-8.75189148499889E-13,0.));
#25996=DIRECTION('',(0.,0.,1.));
#25997=DIRECTION('center_axis',(0.,0.,1.));
#25998=DIRECTION('ref_axis',(1.,-8.75189148499889E-13,0.));
#25999=DIRECTION('',(0.,0.,1.));
#26000=DIRECTION('center_axis',(0.,0.,1.));
#26001=DIRECTION('ref_axis',(1.,-8.75189148499889E-13,0.));
#26002=DIRECTION('',(0.,0.,1.));
#26003=DIRECTION('center_axis',(0.,0.,1.));
#26004=DIRECTION('ref_axis',(1.,-8.75189148499889E-13,0.));
#26005=DIRECTION('',(0.,0.,1.));
#26006=DIRECTION('center_axis',(0.,0.,1.));
#26007=DIRECTION('ref_axis',(1.,-8.75189148499889E-13,0.));
#26008=DIRECTION('',(0.,0.,1.));
#26009=DIRECTION('center_axis',(0.,0.,1.));
#26010=DIRECTION('ref_axis',(1.,-8.75189148499889E-13,0.));
#26011=DIRECTION('',(0.,0.,1.));
#26012=DIRECTION('center_axis',(0.,0.,1.));
#26013=DIRECTION('ref_axis',(1.,-8.75189148499889E-13,0.));
#26014=DIRECTION('',(0.,0.,1.));
#26015=DIRECTION('center_axis',(0.,0.,1.));
#26016=DIRECTION('ref_axis',(1.,-8.75189148499889E-13,0.));
#26017=DIRECTION('',(0.,0.,1.));
#26018=DIRECTION('center_axis',(0.,0.,1.));
#26019=DIRECTION('ref_axis',(1.,-8.75189148499889E-13,0.));
#26020=DIRECTION('',(0.,0.,1.));
#26021=DIRECTION('center_axis',(0.,0.,1.));
#26022=DIRECTION('ref_axis',(1.,-8.75189148499889E-13,0.));
#26023=DIRECTION('center_axis',(0.,0.,-1.));
#26024=DIRECTION('ref_axis',(1.,-8.75189148499889E-13,0.));
#26025=DIRECTION('center_axis',(0.,0.,1.));
#26026=DIRECTION('ref_axis',(1.,0.,0.));
#26027=DIRECTION('center_axis',(0.,0.,-1.));
#26028=DIRECTION('ref_axis',(1.,0.,0.));
#26029=DIRECTION('center_axis',(0.,0.,1.));
#26030=DIRECTION('ref_axis',(1.,0.,0.));
#26031=DIRECTION('',(0.5,0.866025403784439,0.));
#26032=DIRECTION('',(-0.5,0.866025403784439,0.));
#26033=DIRECTION('',(-1.,1.20185167898973E-16,0.));
#26034=DIRECTION('',(-0.5,-0.866025403784439,0.));
#26035=DIRECTION('',(0.5,-0.866025403784439,0.));
#26036=DIRECTION('',(1.,-2.40370335797945E-16,0.));
#26037=DIRECTION('center_axis',(0.,0.,1.));
#26038=DIRECTION('ref_axis',(1.,0.,0.));
#26039=DIRECTION('',(0.5,0.866025403784439,0.));
#26040=DIRECTION('',(1.,-2.40370335797945E-16,0.));
#26041=DIRECTION('',(0.5,-0.866025403784439,0.));
#26042=DIRECTION('',(-0.5,-0.866025403784439,0.));
#26043=DIRECTION('',(-1.,1.20185167898973E-16,0.));
#26044=DIRECTION('',(-0.5,0.866025403784439,0.));
#26045=DIRECTION('center_axis',(0.,0.,-1.));
#26046=DIRECTION('ref_axis',(1.,0.,0.));
#26047=DIRECTION('center_axis',(-2.40370335797945E-16,-1.,0.));
#26048=DIRECTION('ref_axis',(1.,-2.40370335797945E-16,0.));
#26049=DIRECTION('',(0.,0.,1.));
#26050=DIRECTION('',(0.,0.,1.));
#26051=DIRECTION('center_axis',(-0.866025403784439,-0.5,0.));
#26052=DIRECTION('ref_axis',(0.5,-0.866025403784439,0.));
#26053=DIRECTION('',(0.,0.,1.));
#26054=DIRECTION('center_axis',(-0.866025403784439,0.5,0.));
#26055=DIRECTION('ref_axis',(-0.5,-0.866025403784439,0.));
#26056=DIRECTION('',(0.,0.,1.));
#26057=DIRECTION('center_axis',(1.20185167898973E-16,1.,0.));
#26058=DIRECTION('ref_axis',(-1.,1.20185167898973E-16,0.));
#26059=DIRECTION('',(0.,0.,1.));
#26060=DIRECTION('center_axis',(0.866025403784439,0.5,0.));
#26061=DIRECTION('ref_axis',(-0.5,0.866025403784439,0.));
#26062=DIRECTION('',(0.,0.,1.));
#26063=DIRECTION('center_axis',(0.866025403784439,-0.5,0.));
#26064=DIRECTION('ref_axis',(0.5,0.866025403784439,0.));
#26065=DIRECTION('center_axis',(0.,0.,1.));
#26066=DIRECTION('ref_axis',(1.,0.,0.));
#26067=DIRECTION('',(0.,0.,-1.));
#26068=DIRECTION('center_axis',(0.,0.,-1.));
#26069=DIRECTION('ref_axis',(1.,0.,0.));
#26070=DIRECTION('center_axis',(0.,0.,1.));
#26071=DIRECTION('ref_axis',(1.,0.,0.));
#26072=DIRECTION('center_axis',(6.12323399573677E-17,0.,1.));
#26073=DIRECTION('ref_axis',(1.,0.,0.));
#26074=DIRECTION('center_axis',(1.22464679914735E-16,-1.,0.));
#26075=DIRECTION('ref_axis',(-1.,-1.22464679914735E-16,0.));
#26076=DIRECTION('axis',(0.,0.,1.));
#26077=DIRECTION('refdir',(1.,0.,0.));
#26078=DIRECTION('center_axis',(0.,0.,-1.));
#26079=DIRECTION('ref_axis',(-0.346147419294793,0.938180134150982,0.));
#26080=DIRECTION('',(0.,0.,-1.));
#26081=DIRECTION('center_axis',(0.,0.,-1.));
#26082=DIRECTION('ref_axis',(1.,0.,0.));
#26083=DIRECTION('center_axis',(0.,0.,-1.));
#26084=DIRECTION('ref_axis',(1.,0.,0.));
#26085=DIRECTION('',(0.,0.,-1.));
#26086=DIRECTION('center_axis',(0.,0.,-1.));
#26087=DIRECTION('ref_axis',(1.,0.,0.));
#26088=DIRECTION('',(0.,0.,-1.));
#26089=DIRECTION('center_axis',(0.,0.,-1.));
#26090=DIRECTION('ref_axis',(1.,0.,0.));
#26091=DIRECTION('',(0.,0.,-1.));
#26092=DIRECTION('center_axis',(0.,0.,-1.));
#26093=DIRECTION('ref_axis',(1.,0.,0.));
#26094=DIRECTION('',(0.,0.,-1.));
#26095=DIRECTION('center_axis',(0.,0.,-1.));
#26096=DIRECTION('ref_axis',(1.,0.,0.));
#26097=DIRECTION('',(0.,0.,-1.));
#26098=DIRECTION('center_axis',(0.,0.,-1.));
#26099=DIRECTION('ref_axis',(1.,0.,0.));
#26100=DIRECTION('',(0.,0.,-1.));
#26101=DIRECTION('center_axis',(0.,0.,-1.));
#26102=DIRECTION('ref_axis',(0.938064160696058,-0.346461585774816,0.));
#26103=DIRECTION('',(0.,0.,-1.));
#26104=DIRECTION('center_axis',(0.,0.,-1.));
#26105=DIRECTION('ref_axis',(1.,0.,0.));
#26106=DIRECTION('center_axis',(0.,0.,-1.));
#26107=DIRECTION('ref_axis',(0.793491609261867,0.608581190993456,0.));
#26108=DIRECTION('',(1.22464679914735E-16,-2.66964461005383E-30,-1.));
#26109=DIRECTION('center_axis',(0.,0.,1.));
#26110=DIRECTION('ref_axis',(1.,-2.16768378774637E-14,0.));
#26111=DIRECTION('center_axis',(0.,0.,-1.));
#26112=DIRECTION('ref_axis',(1.,-2.16768378774637E-14,0.));
#26113=DIRECTION('',(1.22464679914735E-16,-2.66964461005383E-30,-1.));
#26114=DIRECTION('center_axis',(0.,0.,-1.));
#26115=DIRECTION('ref_axis',(1.,-2.16768378774637E-14,0.));
#26116=DIRECTION('',(1.22464679914735E-16,-2.66964461005383E-30,-1.));
#26117=DIRECTION('center_axis',(0.,0.,-1.));
#26118=DIRECTION('ref_axis',(1.,-2.16768378774637E-14,0.));
#26119=DIRECTION('',(1.22464679914735E-16,-2.66964461005383E-30,-1.));
#26120=DIRECTION('center_axis',(0.,0.,-1.));
#26121=DIRECTION('ref_axis',(1.,-2.16768378774637E-14,0.));
#26122=DIRECTION('',(1.22464679914735E-16,-2.66964461005383E-30,-1.));
#26123=DIRECTION('center_axis',(0.,0.,-1.));
#26124=DIRECTION('ref_axis',(1.,-2.16768378774637E-14,0.));
#26125=DIRECTION('',(1.22464679914735E-16,-2.66964461005383E-30,-1.));
#26126=DIRECTION('center_axis',(0.,0.,-1.));
#26127=DIRECTION('ref_axis',(1.,-2.16768378774637E-14,0.));
#26128=DIRECTION('',(1.22464679914735E-16,-2.66964461005383E-30,-1.));
#26129=DIRECTION('center_axis',(0.,0.,-1.));
#26130=DIRECTION('ref_axis',(-0.608751959302999,-0.793360606562211,0.));
#26131=DIRECTION('',(1.22464679914735E-16,-2.66964461005383E-30,-1.));
#26132=DIRECTION('center_axis',(0.,0.,-1.));
#26133=DIRECTION('ref_axis',(1.,-2.16768378774637E-14,0.));
#26134=DIRECTION('center_axis',(0.,0.,-1.));
#26135=DIRECTION('ref_axis',(1.,-2.16768378774637E-14,0.));
#26136=DIRECTION('center_axis',(0.,0.,1.));
#26137=DIRECTION('ref_axis',(1.,0.,0.));
#26138=DIRECTION('',(0.5,0.866025403784439,0.));
#26139=DIRECTION('',(-0.5,0.866025403784439,0.));
#26140=DIRECTION('',(-1.,0.,0.));
#26141=DIRECTION('',(-0.5,-0.866025403784439,0.));
#26142=DIRECTION('',(0.5,-0.866025403784439,0.));
#26143=DIRECTION('',(1.,-3.39346356420629E-16,0.));
#26144=DIRECTION('center_axis',(0.,0.,-1.));
#26145=DIRECTION('ref_axis',(1.,0.,0.));
#26146=DIRECTION('center_axis',(-3.39346356420629E-16,-1.,0.));
#26147=DIRECTION('ref_axis',(1.,-3.39346356420629E-16,0.));
#26148=DIRECTION('',(1.,-3.39346356420629E-16,0.));
#26149=DIRECTION('',(0.,0.,1.));
#26150=DIRECTION('',(0.,0.,1.));
#26151=DIRECTION('center_axis',(-0.866025403784439,-0.5,0.));
#26152=DIRECTION('ref_axis',(0.5,-0.866025403784439,0.));
#26153=DIRECTION('',(0.5,-0.866025403784439,0.));
#26154=DIRECTION('',(0.,0.,1.));
#26155=DIRECTION('center_axis',(-0.866025403784439,0.5,0.));
#26156=DIRECTION('ref_axis',(-0.5,-0.866025403784438,0.));
#26157=DIRECTION('',(-0.5,-0.866025403784439,0.));
#26158=DIRECTION('',(0.,0.,1.));
#26159=DIRECTION('center_axis',(0.,1.,0.));
#26160=DIRECTION('ref_axis',(-1.,0.,0.));
#26161=DIRECTION('',(-1.,0.,0.));
#26162=DIRECTION('',(0.,0.,1.));
#26163=DIRECTION('center_axis',(0.866025403784439,0.5,0.));
#26164=DIRECTION('ref_axis',(-0.5,0.866025403784439,0.));
#26165=DIRECTION('',(-0.5,0.866025403784439,0.));
#26166=DIRECTION('',(0.,0.,1.));
#26167=DIRECTION('center_axis',(0.866025403784439,-0.5,0.));
#26168=DIRECTION('ref_axis',(0.5,0.866025403784439,0.));
#26169=DIRECTION('',(0.5,0.866025403784439,0.));
#26170=DIRECTION('center_axis',(0.,0.,1.));
#26171=DIRECTION('ref_axis',(1.,0.,0.));
#26172=DIRECTION('axis',(0.,0.,1.));
#26173=DIRECTION('refdir',(1.,0.,0.));
#26174=DIRECTION('center_axis',(0.,0.,1.));
#26175=DIRECTION('ref_axis',(1.,0.,0.));
#26176=DIRECTION('center_axis',(0.,0.,-1.));
#26177=DIRECTION('ref_axis',(1.,0.,0.));
#26178=DIRECTION('',(0.,0.,-1.));
#26179=DIRECTION('center_axis',(0.,0.,-1.));
#26180=DIRECTION('ref_axis',(1.,0.,0.));
#26181=DIRECTION('center_axis',(0.,0.,1.));
#26182=DIRECTION('ref_axis',(1.,0.,0.));
#26183=DIRECTION('center_axis',(0.,0.,1.));
#26184=DIRECTION('ref_axis',(1.,0.,0.));
#26185=DIRECTION('',(0.,0.,-1.));
#26186=DIRECTION('center_axis',(0.,0.,1.));
#26187=DIRECTION('ref_axis',(1.,0.,0.));
#26188=DIRECTION('center_axis',(0.,0.,1.));
#26189=DIRECTION('ref_axis',(1.,0.,0.));
#26190=DIRECTION('center_axis',(0.,0.,1.));
#26191=DIRECTION('ref_axis',(1.,0.,0.));
#26192=DIRECTION('axis',(0.,0.,1.));
#26193=DIRECTION('refdir',(1.,0.,0.));
#26194=DIRECTION('center_axis',(0.,0.,1.));
#26195=DIRECTION('ref_axis',(1.,0.,0.));
#26196=DIRECTION('',(0.,0.,-1.));
#26197=DIRECTION('center_axis',(0.,0.,-1.));
#26198=DIRECTION('ref_axis',(1.,0.,0.));
#26199=DIRECTION('center_axis',(0.,0.,1.));
#26200=DIRECTION('ref_axis',(1.,0.,0.));
#26201=DIRECTION('',(0.,0.,-1.));
#26202=DIRECTION('center_axis',(0.,0.,1.));
#26203=DIRECTION('ref_axis',(1.,0.,0.));
#26204=DIRECTION('',(0.,0.,-1.));
#26205=DIRECTION('center_axis',(0.,0.,1.));
#26206=DIRECTION('ref_axis',(1.,0.,0.));
#26207=DIRECTION('',(0.,0.,-1.));
#26208=DIRECTION('center_axis',(0.,0.,1.));
#26209=DIRECTION('ref_axis',(1.,0.,0.));
#26210=DIRECTION('',(0.,0.,-1.));
#26211=DIRECTION('center_axis',(0.,0.,1.));
#26212=DIRECTION('ref_axis',(1.,0.,0.));
#26213=DIRECTION('',(0.,0.,-1.));
#26214=DIRECTION('center_axis',(0.,0.,1.));
#26215=DIRECTION('ref_axis',(1.,0.,0.));
#26216=DIRECTION('',(0.,0.,-1.));
#26217=DIRECTION('center_axis',(0.,0.,1.));
#26218=DIRECTION('ref_axis',(1.,0.,0.));
#26219=DIRECTION('',(0.,0.,-1.));
#26220=DIRECTION('center_axis',(0.,0.,1.));
#26221=DIRECTION('ref_axis',(1.,0.,0.));
#26222=DIRECTION('',(0.,0.,-1.));
#26223=DIRECTION('center_axis',(0.,0.,1.));
#26224=DIRECTION('ref_axis',(1.,0.,0.));
#26225=DIRECTION('',(0.,0.,-1.));
#26226=DIRECTION('center_axis',(0.,0.,1.));
#26227=DIRECTION('ref_axis',(1.,0.,0.));
#26228=DIRECTION('',(0.,0.,-1.));
#26229=DIRECTION('center_axis',(0.,0.,1.));
#26230=DIRECTION('ref_axis',(1.,0.,0.));
#26231=DIRECTION('',(0.,0.,-1.));
#26232=DIRECTION('center_axis',(0.,0.,1.));
#26233=DIRECTION('ref_axis',(1.,0.,0.));
#26234=DIRECTION('',(0.,0.,-1.));
#26235=DIRECTION('center_axis',(0.,0.,1.));
#26236=DIRECTION('ref_axis',(1.,0.,0.));
#26237=DIRECTION('',(0.,0.,-1.));
#26238=DIRECTION('center_axis',(0.,0.,1.));
#26239=DIRECTION('ref_axis',(1.,0.,0.));
#26240=DIRECTION('',(0.,0.,-1.));
#26241=DIRECTION('center_axis',(0.,0.,1.));
#26242=DIRECTION('ref_axis',(0.997339946684471,-0.0728905394918792,0.));
#26243=DIRECTION('',(0.,0.,1.));
#26244=DIRECTION('center_axis',(0.,0.,-1.));
#26245=DIRECTION('ref_axis',(1.,1.10476514494527E-13,0.));
#26246=DIRECTION('center_axis',(0.,0.,1.));
#26247=DIRECTION('ref_axis',(1.,1.10476514494527E-13,0.));
#26248=DIRECTION('',(0.,0.,1.));
#26249=DIRECTION('center_axis',(0.,0.,1.));
#26250=DIRECTION('ref_axis',(1.,1.10476514494527E-13,0.));
#26251=DIRECTION('',(0.,0.,1.));
#26252=DIRECTION('center_axis',(0.,0.,1.));
#26253=DIRECTION('ref_axis',(1.,1.10476514494527E-13,0.));
#26254=DIRECTION('',(0.,0.,1.));
#26255=DIRECTION('center_axis',(0.,0.,1.));
#26256=DIRECTION('ref_axis',(1.,1.10476514494527E-13,0.));
#26257=DIRECTION('',(0.,0.,1.));
#26258=DIRECTION('center_axis',(0.,0.,1.));
#26259=DIRECTION('ref_axis',(1.,1.10476514494527E-13,0.));
#26260=DIRECTION('',(0.,0.,1.));
#26261=DIRECTION('center_axis',(0.,0.,1.));
#26262=DIRECTION('ref_axis',(1.,1.10476514494527E-13,0.));
#26263=DIRECTION('',(0.,0.,1.));
#26264=DIRECTION('center_axis',(0.,0.,1.));
#26265=DIRECTION('ref_axis',(1.,1.10476514494527E-13,0.));
#26266=DIRECTION('',(0.,0.,1.));
#26267=DIRECTION('center_axis',(0.,0.,1.));
#26268=DIRECTION('ref_axis',(1.,1.10476514494527E-13,0.));
#26269=DIRECTION('',(0.,0.,1.));
#26270=DIRECTION('center_axis',(0.,0.,1.));
#26271=DIRECTION('ref_axis',(1.,1.10476514494527E-13,0.));
#26272=DIRECTION('',(0.,0.,1.));
#26273=DIRECTION('center_axis',(0.,0.,1.));
#26274=DIRECTION('ref_axis',(1.,1.10476514494527E-13,0.));
#26275=DIRECTION('',(0.,0.,1.));
#26276=DIRECTION('center_axis',(0.,0.,1.));
#26277=DIRECTION('ref_axis',(1.,1.10476514494527E-13,0.));
#26278=DIRECTION('',(0.,0.,1.));
#26279=DIRECTION('center_axis',(0.,0.,1.));
#26280=DIRECTION('ref_axis',(1.,1.10476514494527E-13,0.));
#26281=DIRECTION('',(0.,0.,1.));
#26282=DIRECTION('center_axis',(0.,0.,1.));
#26283=DIRECTION('ref_axis',(1.,1.10476514494527E-13,0.));
#26284=DIRECTION('',(0.,0.,1.));
#26285=DIRECTION('center_axis',(0.,0.,1.));
#26286=DIRECTION('ref_axis',(1.,1.10476514494527E-13,0.));
#26287=DIRECTION('',(0.,0.,1.));
#26288=DIRECTION('center_axis',(0.,0.,-1.));
#26289=DIRECTION('ref_axis',(1.,0.,0.));
#26290=DIRECTION('center_axis',(0.,0.,-1.));
#26291=DIRECTION('ref_axis',(1.,0.,0.));
#26292=DIRECTION('',(0.707106781186547,8.65956056235493E-17,0.707106781186548));
#26293=DIRECTION('center_axis',(0.,0.,1.));
#26294=DIRECTION('ref_axis',(1.,0.,0.));
#26295=DIRECTION('center_axis',(0.,0.,1.));
#26296=DIRECTION('ref_axis',(1.,1.10476514494527E-13,0.));
#26297=DIRECTION('center_axis',(0.,0.,-1.));
#26298=DIRECTION('ref_axis',(1.,1.10476514494527E-13,0.));
#26299=DIRECTION('center_axis',(0.,0.,1.));
#26300=DIRECTION('ref_axis',(1.,0.,0.));
#26301=DIRECTION('center_axis',(-1.92296268638356E-16,-1.,0.));
#26302=DIRECTION('ref_axis',(1.,-1.92296268638356E-16,0.));
#26303=DIRECTION('',(1.,-1.92296268638356E-16,0.));
#26304=DIRECTION('',(0.,0.,1.));
#26305=DIRECTION('',(1.,-1.92296268638356E-16,0.));
#26306=DIRECTION('',(0.,0.,1.));
#26307=DIRECTION('center_axis',(-0.866025403784439,-0.5,0.));
#26308=DIRECTION('ref_axis',(0.5,-0.866025403784439,0.));
#26309=DIRECTION('',(0.5,-0.866025403784439,0.));
#26310=DIRECTION('',(0.,0.,1.));
#26311=DIRECTION('',(0.5,-0.866025403784439,0.));
#26312=DIRECTION('center_axis',(-0.866025403784439,0.5,0.));
#26313=DIRECTION('ref_axis',(-0.5,-0.866025403784438,0.));
#26314=DIRECTION('',(-0.5,-0.866025403784438,0.));
#26315=DIRECTION('',(0.,0.,1.));
#26316=DIRECTION('',(-0.5,-0.866025403784439,0.));
#26317=DIRECTION('center_axis',(1.92296268638356E-16,1.,0.));
#26318=DIRECTION('ref_axis',(-1.,1.92296268638356E-16,0.));
#26319=DIRECTION('',(-1.,1.92296268638356E-16,0.));
#26320=DIRECTION('',(0.,0.,1.));
#26321=DIRECTION('',(-1.,1.92296268638356E-16,0.));
#26322=DIRECTION('center_axis',(0.866025403784439,0.5,0.));
#26323=DIRECTION('ref_axis',(-0.5,0.866025403784439,0.));
#26324=DIRECTION('',(-0.5,0.866025403784439,0.));
#26325=DIRECTION('',(0.,0.,1.));
#26326=DIRECTION('',(-0.5,0.866025403784439,0.));
#26327=DIRECTION('center_axis',(0.866025403784439,-0.5,0.));
#26328=DIRECTION('ref_axis',(0.5,0.866025403784439,0.));
#26329=DIRECTION('',(0.5,0.866025403784439,0.));
#26330=DIRECTION('',(0.5,0.866025403784439,0.));
#26331=DIRECTION('center_axis',(0.,0.,1.));
#26332=DIRECTION('ref_axis',(1.,0.,0.));
#26333=DIRECTION('center_axis',(0.,0.,1.));
#26334=DIRECTION('ref_axis',(1.,0.,0.));
#26335=DIRECTION('center_axis',(0.,0.,1.));
#26336=DIRECTION('ref_axis',(1.,0.,0.));
#26337=DIRECTION('center_axis',(0.,0.,1.));
#26338=DIRECTION('ref_axis',(1.,0.,0.));
#26339=DIRECTION('',(0.,0.,-1.));
#26340=DIRECTION('center_axis',(0.,0.,1.));
#26341=DIRECTION('ref_axis',(1.,0.,0.));
#26342=DIRECTION('center_axis',(0.,0.,1.));
#26343=DIRECTION('ref_axis',(1.,0.,0.));
#26344=DIRECTION('center_axis',(0.,0.,1.));
#26345=DIRECTION('ref_axis',(1.,0.,0.));
#26346=DIRECTION('axis',(0.,0.,1.));
#26347=DIRECTION('refdir',(1.,0.,0.));
#26348=DIRECTION('center_axis',(0.,0.,-1.));
#26349=DIRECTION('ref_axis',(-0.347005528821294,0.937863083273595,0.));
#26350=DIRECTION('',(0.,0.,-1.));
#26351=DIRECTION('center_axis',(0.,0.,-1.));
#26352=DIRECTION('ref_axis',(1.,0.,0.));
#26353=DIRECTION('center_axis',(0.,0.,-1.));
#26354=DIRECTION('ref_axis',(1.,0.,0.));
#26355=DIRECTION('',(0.,0.,-1.));
#26356=DIRECTION('center_axis',(0.,0.,-1.));
#26357=DIRECTION('ref_axis',(1.,0.,0.));
#26358=DIRECTION('',(0.,0.,-1.));
#26359=DIRECTION('center_axis',(0.,0.,-1.));
#26360=DIRECTION('ref_axis',(1.,0.,0.));
#26361=DIRECTION('',(0.,0.,-1.));
#26362=DIRECTION('center_axis',(0.,0.,-1.));
#26363=DIRECTION('ref_axis',(1.,0.,0.));
#26364=DIRECTION('',(0.,0.,-1.));
#26365=DIRECTION('center_axis',(0.,0.,-1.));
#26366=DIRECTION('ref_axis',(1.,0.,0.));
#26367=DIRECTION('',(0.,0.,-1.));
#26368=DIRECTION('center_axis',(0.,0.,-1.));
#26369=DIRECTION('ref_axis',(1.,0.,0.));
#26370=DIRECTION('',(0.,0.,-1.));
#26371=DIRECTION('center_axis',(0.,0.,-1.));
#26372=DIRECTION('ref_axis',(1.,0.,0.));
#26373=DIRECTION('',(0.,0.,-1.));
#26374=DIRECTION('center_axis',(0.,0.,-1.));
#26375=DIRECTION('ref_axis',(1.,0.,0.));
#26376=DIRECTION('',(0.,0.,-1.));
#26377=DIRECTION('center_axis',(0.,0.,-1.));
#26378=DIRECTION('ref_axis',(1.,0.,0.));
#26379=DIRECTION('',(0.,0.,-1.));
#26380=DIRECTION('center_axis',(0.,0.,-1.));
#26381=DIRECTION('ref_axis',(1.,0.,0.));
#26382=DIRECTION('',(0.,0.,-1.));
#26383=DIRECTION('center_axis',(0.,0.,-1.));
#26384=DIRECTION('ref_axis',(1.,0.,0.));
#26385=DIRECTION('',(0.,0.,-1.));
#26386=DIRECTION('center_axis',(0.,0.,-1.));
#26387=DIRECTION('ref_axis',(1.,0.,0.));
#26388=DIRECTION('',(0.,0.,-1.));
#26389=DIRECTION('center_axis',(0.,0.,-1.));
#26390=DIRECTION('ref_axis',(1.,0.,0.));
#26391=DIRECTION('',(0.,0.,-1.));
#26392=DIRECTION('center_axis',(0.,0.,-1.));
#26393=DIRECTION('ref_axis',(1.,0.,0.));
#26394=DIRECTION('',(0.,0.,-1.));
#26395=DIRECTION('center_axis',(0.,0.,-1.));
#26396=DIRECTION('ref_axis',(1.,0.,0.));
#26397=DIRECTION('',(0.,0.,-1.));
#26398=DIRECTION('center_axis',(0.,0.,-1.));
#26399=DIRECTION('ref_axis',(1.,0.,0.));
#26400=DIRECTION('',(0.,0.,-1.));
#26401=DIRECTION('center_axis',(0.,0.,-1.));
#26402=DIRECTION('ref_axis',(1.,0.,0.));
#26403=DIRECTION('',(0.,0.,-1.));
#26404=DIRECTION('center_axis',(0.,0.,-1.));
#26405=DIRECTION('ref_axis',(1.,0.,0.));
#26406=DIRECTION('',(0.,0.,-1.));
#26407=DIRECTION('center_axis',(0.,0.,-1.));
#26408=DIRECTION('ref_axis',(0.937995430874257,-0.346647618856695,0.));
#26409=DIRECTION('',(0.,0.,-1.));
#26410=DIRECTION('center_axis',(0.,0.,-1.));
#26411=DIRECTION('ref_axis',(1.,0.,0.));
#26412=DIRECTION('center_axis',(0.,0.,-1.));
#26413=DIRECTION('ref_axis',(-0.347005563593634,0.93786307040797,0.));
#26414=DIRECTION('',(0.,0.,-1.));
#26415=DIRECTION('center_axis',(0.,0.,-1.));
#26416=DIRECTION('ref_axis',(1.,0.,0.));
#26417=DIRECTION('center_axis',(0.,0.,-1.));
#26418=DIRECTION('ref_axis',(1.,0.,0.));
#26419=DIRECTION('',(0.,0.,-1.));
#26420=DIRECTION('center_axis',(0.,0.,-1.));
#26421=DIRECTION('ref_axis',(1.,0.,0.));
#26422=DIRECTION('',(0.,0.,-1.));
#26423=DIRECTION('center_axis',(0.,0.,-1.));
#26424=DIRECTION('ref_axis',(1.,0.,0.));
#26425=DIRECTION('',(0.,0.,-1.));
#26426=DIRECTION('center_axis',(0.,0.,-1.));
#26427=DIRECTION('ref_axis',(1.,0.,0.));
#26428=DIRECTION('',(0.,0.,-1.));
#26429=DIRECTION('center_axis',(0.,0.,-1.));
#26430=DIRECTION('ref_axis',(1.,0.,0.));
#26431=DIRECTION('',(0.,0.,-1.));
#26432=DIRECTION('center_axis',(0.,0.,-1.));
#26433=DIRECTION('ref_axis',(1.,0.,0.));
#26434=DIRECTION('',(0.,0.,-1.));
#26435=DIRECTION('center_axis',(0.,0.,-1.));
#26436=DIRECTION('ref_axis',(1.,0.,0.));
#26437=DIRECTION('',(0.,0.,-1.));
#26438=DIRECTION('center_axis',(0.,0.,-1.));
#26439=DIRECTION('ref_axis',(1.,0.,0.));
#26440=DIRECTION('',(0.,0.,-1.));
#26441=DIRECTION('center_axis',(0.,0.,-1.));
#26442=DIRECTION('ref_axis',(1.,0.,0.));
#26443=DIRECTION('',(0.,0.,-1.));
#26444=DIRECTION('center_axis',(0.,0.,-1.));
#26445=DIRECTION('ref_axis',(1.,0.,0.));
#26446=DIRECTION('',(0.,0.,-1.));
#26447=DIRECTION('center_axis',(0.,0.,-1.));
#26448=DIRECTION('ref_axis',(1.,0.,0.));
#26449=DIRECTION('',(0.,0.,-1.));
#26450=DIRECTION('center_axis',(0.,0.,-1.));
#26451=DIRECTION('ref_axis',(1.,0.,0.));
#26452=DIRECTION('',(0.,0.,-1.));
#26453=DIRECTION('center_axis',(0.,0.,-1.));
#26454=DIRECTION('ref_axis',(1.,0.,0.));
#26455=DIRECTION('',(0.,0.,-1.));
#26456=DIRECTION('center_axis',(0.,0.,-1.));
#26457=DIRECTION('ref_axis',(1.,0.,0.));
#26458=DIRECTION('',(0.,0.,-1.));
#26459=DIRECTION('center_axis',(0.,0.,-1.));
#26460=DIRECTION('ref_axis',(1.,0.,0.));
#26461=DIRECTION('',(0.,0.,-1.));
#26462=DIRECTION('center_axis',(0.,0.,-1.));
#26463=DIRECTION('ref_axis',(1.,0.,0.));
#26464=DIRECTION('',(0.,0.,-1.));
#26465=DIRECTION('center_axis',(0.,0.,-1.));
#26466=DIRECTION('ref_axis',(1.,0.,0.));
#26467=DIRECTION('',(0.,0.,-1.));
#26468=DIRECTION('center_axis',(0.,0.,-1.));
#26469=DIRECTION('ref_axis',(1.,0.,0.));
#26470=DIRECTION('',(0.,0.,-1.));
#26471=DIRECTION('center_axis',(0.,0.,-1.));
#26472=DIRECTION('ref_axis',(0.93799543155111,-0.346647617025196,0.));
#26473=DIRECTION('',(0.,0.,-1.));
#26474=DIRECTION('center_axis',(0.,0.,-1.));
#26475=DIRECTION('ref_axis',(1.,0.,0.));
#26476=DIRECTION('center_axis',(0.,0.,-1.));
#26477=DIRECTION('ref_axis',(-0.346979519569086,0.937872706181178,0.));
#26478=DIRECTION('',(0.,0.,-1.));
#26479=DIRECTION('center_axis',(0.,0.,-1.));
#26480=DIRECTION('ref_axis',(1.,0.,0.));
#26481=DIRECTION('center_axis',(0.,0.,-1.));
#26482=DIRECTION('ref_axis',(1.,0.,0.));
#26483=DIRECTION('',(0.,0.,-1.));
#26484=DIRECTION('center_axis',(0.,0.,-1.));
#26485=DIRECTION('ref_axis',(1.,0.,0.));
#26486=DIRECTION('',(0.,0.,-1.));
#26487=DIRECTION('center_axis',(0.,0.,-1.));
#26488=DIRECTION('ref_axis',(1.,0.,0.));
#26489=DIRECTION('',(0.,0.,-1.));
#26490=DIRECTION('center_axis',(0.,0.,-1.));
#26491=DIRECTION('ref_axis',(1.,0.,0.));
#26492=DIRECTION('',(0.,0.,-1.));
#26493=DIRECTION('center_axis',(0.,0.,-1.));
#26494=DIRECTION('ref_axis',(1.,0.,0.));
#26495=DIRECTION('',(0.,0.,-1.));
#26496=DIRECTION('center_axis',(0.,0.,-1.));
#26497=DIRECTION('ref_axis',(1.,0.,0.));
#26498=DIRECTION('',(0.,0.,-1.));
#26499=DIRECTION('center_axis',(0.,0.,-1.));
#26500=DIRECTION('ref_axis',(1.,0.,0.));
#26501=DIRECTION('',(0.,0.,-1.));
#26502=DIRECTION('center_axis',(0.,0.,-1.));
#26503=DIRECTION('ref_axis',(1.,0.,0.));
#26504=DIRECTION('',(0.,0.,-1.));
#26505=DIRECTION('center_axis',(0.,0.,-1.));
#26506=DIRECTION('ref_axis',(1.,0.,0.));
#26507=DIRECTION('',(0.,0.,-1.));
#26508=DIRECTION('center_axis',(0.,0.,-1.));
#26509=DIRECTION('ref_axis',(1.,0.,0.));
#26510=DIRECTION('',(0.,0.,-1.));
#26511=DIRECTION('center_axis',(0.,0.,-1.));
#26512=DIRECTION('ref_axis',(1.,0.,0.));
#26513=DIRECTION('',(0.,0.,-1.));
#26514=DIRECTION('center_axis',(0.,0.,-1.));
#26515=DIRECTION('ref_axis',(1.,0.,0.));
#26516=DIRECTION('',(0.,0.,-1.));
#26517=DIRECTION('center_axis',(0.,0.,-1.));
#26518=DIRECTION('ref_axis',(1.,0.,0.));
#26519=DIRECTION('',(0.,0.,-1.));
#26520=DIRECTION('center_axis',(0.,0.,-1.));
#26521=DIRECTION('ref_axis',(1.,0.,0.));
#26522=DIRECTION('',(0.,0.,-1.));
#26523=DIRECTION('center_axis',(0.,0.,-1.));
#26524=DIRECTION('ref_axis',(1.,0.,0.));
#26525=DIRECTION('',(0.,0.,-1.));
#26526=DIRECTION('center_axis',(0.,0.,-1.));
#26527=DIRECTION('ref_axis',(1.,0.,0.));
#26528=DIRECTION('',(0.,0.,-1.));
#26529=DIRECTION('center_axis',(0.,0.,-1.));
#26530=DIRECTION('ref_axis',(1.,0.,0.));
#26531=DIRECTION('',(0.,0.,-1.));
#26532=DIRECTION('center_axis',(0.,0.,-1.));
#26533=DIRECTION('ref_axis',(1.,0.,0.));
#26534=DIRECTION('',(0.,0.,-1.));
#26535=DIRECTION('center_axis',(0.,0.,-1.));
#26536=DIRECTION('ref_axis',(0.93799553354803,-0.346647341031121,0.));
#26537=DIRECTION('',(0.,0.,-1.));
#26538=DIRECTION('center_axis',(0.,0.,-1.));
#26539=DIRECTION('ref_axis',(1.,0.,0.));
#26540=DIRECTION('center_axis',(0.,0.,-1.));
#26541=DIRECTION('ref_axis',(-0.347005604905985,0.937863055122565,0.));
#26542=DIRECTION('',(0.,0.,-1.));
#26543=DIRECTION('center_axis',(0.,0.,-1.));
#26544=DIRECTION('ref_axis',(1.,0.,0.));
#26545=DIRECTION('center_axis',(0.,0.,-1.));
#26546=DIRECTION('ref_axis',(1.,0.,0.));
#26547=DIRECTION('',(0.,0.,-1.));
#26548=DIRECTION('center_axis',(0.,0.,-1.));
#26549=DIRECTION('ref_axis',(1.,0.,0.));
#26550=DIRECTION('',(0.,0.,-1.));
#26551=DIRECTION('center_axis',(0.,0.,-1.));
#26552=DIRECTION('ref_axis',(1.,0.,0.));
#26553=DIRECTION('',(0.,0.,-1.));
#26554=DIRECTION('center_axis',(0.,0.,-1.));
#26555=DIRECTION('ref_axis',(1.,0.,0.));
#26556=DIRECTION('',(0.,0.,-1.));
#26557=DIRECTION('center_axis',(0.,0.,-1.));
#26558=DIRECTION('ref_axis',(1.,0.,0.));
#26559=DIRECTION('',(0.,0.,-1.));
#26560=DIRECTION('center_axis',(0.,0.,-1.));
#26561=DIRECTION('ref_axis',(1.,0.,0.));
#26562=DIRECTION('',(0.,0.,-1.));
#26563=DIRECTION('center_axis',(0.,0.,-1.));
#26564=DIRECTION('ref_axis',(1.,0.,0.));
#26565=DIRECTION('',(0.,0.,-1.));
#26566=DIRECTION('center_axis',(0.,0.,-1.));
#26567=DIRECTION('ref_axis',(1.,0.,0.));
#26568=DIRECTION('',(0.,0.,-1.));
#26569=DIRECTION('center_axis',(0.,0.,-1.));
#26570=DIRECTION('ref_axis',(1.,0.,0.));
#26571=DIRECTION('',(0.,0.,-1.));
#26572=DIRECTION('center_axis',(0.,0.,-1.));
#26573=DIRECTION('ref_axis',(1.,0.,0.));
#26574=DIRECTION('',(0.,0.,-1.));
#26575=DIRECTION('center_axis',(0.,0.,-1.));
#26576=DIRECTION('ref_axis',(1.,0.,0.));
#26577=DIRECTION('',(0.,0.,-1.));
#26578=DIRECTION('center_axis',(0.,0.,-1.));
#26579=DIRECTION('ref_axis',(1.,0.,0.));
#26580=DIRECTION('',(0.,0.,-1.));
#26581=DIRECTION('center_axis',(0.,0.,-1.));
#26582=DIRECTION('ref_axis',(1.,0.,0.));
#26583=DIRECTION('',(0.,0.,-1.));
#26584=DIRECTION('center_axis',(0.,0.,-1.));
#26585=DIRECTION('ref_axis',(1.,0.,0.));
#26586=DIRECTION('',(0.,0.,-1.));
#26587=DIRECTION('center_axis',(0.,0.,-1.));
#26588=DIRECTION('ref_axis',(1.,0.,0.));
#26589=DIRECTION('',(0.,0.,-1.));
#26590=DIRECTION('center_axis',(0.,0.,-1.));
#26591=DIRECTION('ref_axis',(1.,0.,0.));
#26592=DIRECTION('',(0.,0.,-1.));
#26593=DIRECTION('center_axis',(0.,0.,-1.));
#26594=DIRECTION('ref_axis',(1.,0.,0.));
#26595=DIRECTION('',(0.,0.,-1.));
#26596=DIRECTION('center_axis',(0.,0.,-1.));
#26597=DIRECTION('ref_axis',(1.,0.,0.));
#26598=DIRECTION('',(0.,0.,-1.));
#26599=DIRECTION('center_axis',(0.,0.,-1.));
#26600=DIRECTION('ref_axis',(0.937995429977383,-0.34664762128355,0.));
#26601=DIRECTION('',(0.,0.,-1.));
#26602=DIRECTION('center_axis',(0.,0.,-1.));
#26603=DIRECTION('ref_axis',(1.,0.,0.));
#26604=DIRECTION('center_axis',(0.,0.,-1.));
#26605=DIRECTION('ref_axis',(-0.34700548079112,0.937863101044563,0.));
#26606=DIRECTION('',(0.,0.,-1.));
#26607=DIRECTION('center_axis',(0.,0.,-1.));
#26608=DIRECTION('ref_axis',(1.,0.,0.));
#26609=DIRECTION('center_axis',(0.,0.,-1.));
#26610=DIRECTION('ref_axis',(1.,0.,0.));
#26611=DIRECTION('',(0.,0.,-1.));
#26612=DIRECTION('center_axis',(0.,0.,-1.));
#26613=DIRECTION('ref_axis',(1.,0.,0.));
#26614=DIRECTION('',(0.,0.,-1.));
#26615=DIRECTION('center_axis',(0.,0.,-1.));
#26616=DIRECTION('ref_axis',(1.,0.,0.));
#26617=DIRECTION('',(0.,0.,-1.));
#26618=DIRECTION('center_axis',(0.,0.,-1.));
#26619=DIRECTION('ref_axis',(1.,0.,0.));
#26620=DIRECTION('',(0.,0.,-1.));
#26621=DIRECTION('center_axis',(0.,0.,-1.));
#26622=DIRECTION('ref_axis',(1.,0.,0.));
#26623=DIRECTION('',(0.,0.,-1.));
#26624=DIRECTION('center_axis',(0.,0.,-1.));
#26625=DIRECTION('ref_axis',(1.,0.,0.));
#26626=DIRECTION('',(0.,0.,-1.));
#26627=DIRECTION('center_axis',(0.,0.,-1.));
#26628=DIRECTION('ref_axis',(1.,0.,0.));
#26629=DIRECTION('',(0.,0.,-1.));
#26630=DIRECTION('center_axis',(0.,0.,-1.));
#26631=DIRECTION('ref_axis',(1.,0.,0.));
#26632=DIRECTION('',(0.,0.,-1.));
#26633=DIRECTION('center_axis',(0.,0.,-1.));
#26634=DIRECTION('ref_axis',(1.,0.,0.));
#26635=DIRECTION('',(0.,0.,-1.));
#26636=DIRECTION('center_axis',(0.,0.,-1.));
#26637=DIRECTION('ref_axis',(1.,0.,0.));
#26638=DIRECTION('',(0.,0.,-1.));
#26639=DIRECTION('center_axis',(0.,0.,-1.));
#26640=DIRECTION('ref_axis',(1.,0.,0.));
#26641=DIRECTION('',(0.,0.,-1.));
#26642=DIRECTION('center_axis',(0.,0.,-1.));
#26643=DIRECTION('ref_axis',(1.,0.,0.));
#26644=DIRECTION('',(0.,0.,-1.));
#26645=DIRECTION('center_axis',(0.,0.,-1.));
#26646=DIRECTION('ref_axis',(1.,0.,0.));
#26647=DIRECTION('',(0.,0.,-1.));
#26648=DIRECTION('center_axis',(0.,0.,-1.));
#26649=DIRECTION('ref_axis',(1.,0.,0.));
#26650=DIRECTION('',(0.,0.,-1.));
#26651=DIRECTION('center_axis',(0.,0.,-1.));
#26652=DIRECTION('ref_axis',(1.,0.,0.));
#26653=DIRECTION('',(0.,0.,-1.));
#26654=DIRECTION('center_axis',(0.,0.,-1.));
#26655=DIRECTION('ref_axis',(1.,0.,0.));
#26656=DIRECTION('',(0.,0.,-1.));
#26657=DIRECTION('center_axis',(0.,0.,-1.));
#26658=DIRECTION('ref_axis',(1.,0.,0.));
#26659=DIRECTION('',(0.,0.,-1.));
#26660=DIRECTION('center_axis',(0.,0.,-1.));
#26661=DIRECTION('ref_axis',(1.,0.,0.));
#26662=DIRECTION('',(0.,0.,-1.));
#26663=DIRECTION('center_axis',(0.,0.,-1.));
#26664=DIRECTION('ref_axis',(0.937995432501147,-0.346647614454486,0.));
#26665=DIRECTION('',(0.,0.,-1.));
#26666=DIRECTION('center_axis',(0.,0.,-1.));
#26667=DIRECTION('ref_axis',(1.,0.,0.));
#26668=DIRECTION('center_axis',(0.,0.,-1.));
#26669=DIRECTION('ref_axis',(-0.346979462678664,0.937872727228607,0.));
#26670=DIRECTION('',(0.,0.,-1.));
#26671=DIRECTION('center_axis',(0.,0.,-1.));
#26672=DIRECTION('ref_axis',(1.,0.,0.));
#26673=DIRECTION('center_axis',(0.,0.,-1.));
#26674=DIRECTION('ref_axis',(1.,0.,0.));
#26675=DIRECTION('',(0.,0.,-1.));
#26676=DIRECTION('center_axis',(0.,0.,-1.));
#26677=DIRECTION('ref_axis',(1.,0.,0.));
#26678=DIRECTION('',(0.,0.,-1.));
#26679=DIRECTION('center_axis',(0.,0.,-1.));
#26680=DIRECTION('ref_axis',(1.,0.,0.));
#26681=DIRECTION('',(0.,0.,-1.));
#26682=DIRECTION('center_axis',(0.,0.,-1.));
#26683=DIRECTION('ref_axis',(1.,0.,0.));
#26684=DIRECTION('',(0.,0.,-1.));
#26685=DIRECTION('center_axis',(0.,0.,-1.));
#26686=DIRECTION('ref_axis',(1.,0.,0.));
#26687=DIRECTION('',(0.,0.,-1.));
#26688=DIRECTION('center_axis',(0.,0.,-1.));
#26689=DIRECTION('ref_axis',(1.,0.,0.));
#26690=DIRECTION('',(0.,0.,-1.));
#26691=DIRECTION('center_axis',(0.,0.,-1.));
#26692=DIRECTION('ref_axis',(1.,0.,0.));
#26693=DIRECTION('',(0.,0.,-1.));
#26694=DIRECTION('center_axis',(0.,0.,-1.));
#26695=DIRECTION('ref_axis',(1.,0.,0.));
#26696=DIRECTION('',(0.,0.,-1.));
#26697=DIRECTION('center_axis',(0.,0.,-1.));
#26698=DIRECTION('ref_axis',(1.,0.,0.));
#26699=DIRECTION('',(0.,0.,-1.));
#26700=DIRECTION('center_axis',(0.,0.,-1.));
#26701=DIRECTION('ref_axis',(1.,0.,0.));
#26702=DIRECTION('',(0.,0.,-1.));
#26703=DIRECTION('center_axis',(0.,0.,-1.));
#26704=DIRECTION('ref_axis',(1.,0.,0.));
#26705=DIRECTION('',(0.,0.,-1.));
#26706=DIRECTION('center_axis',(0.,0.,-1.));
#26707=DIRECTION('ref_axis',(1.,0.,0.));
#26708=DIRECTION('',(0.,0.,-1.));
#26709=DIRECTION('center_axis',(0.,0.,-1.));
#26710=DIRECTION('ref_axis',(1.,0.,0.));
#26711=DIRECTION('',(0.,0.,-1.));
#26712=DIRECTION('center_axis',(0.,0.,-1.));
#26713=DIRECTION('ref_axis',(1.,0.,0.));
#26714=DIRECTION('',(0.,0.,-1.));
#26715=DIRECTION('center_axis',(0.,0.,-1.));
#26716=DIRECTION('ref_axis',(1.,0.,0.));
#26717=DIRECTION('',(0.,0.,-1.));
#26718=DIRECTION('center_axis',(0.,0.,-1.));
#26719=DIRECTION('ref_axis',(1.,0.,0.));
#26720=DIRECTION('',(0.,0.,-1.));
#26721=DIRECTION('center_axis',(0.,0.,-1.));
#26722=DIRECTION('ref_axis',(1.,0.,0.));
#26723=DIRECTION('',(0.,0.,-1.));
#26724=DIRECTION('center_axis',(0.,0.,-1.));
#26725=DIRECTION('ref_axis',(1.,0.,0.));
#26726=DIRECTION('',(0.,0.,-1.));
#26727=DIRECTION('center_axis',(0.,0.,-1.));
#26728=DIRECTION('ref_axis',(0.937995529739744,-0.346647351335988,0.));
#26729=DIRECTION('',(0.,0.,-1.));
#26730=DIRECTION('center_axis',(0.,0.,-1.));
#26731=DIRECTION('ref_axis',(1.,0.,0.));
#26732=DIRECTION('center_axis',(0.,0.,-1.));
#26733=DIRECTION('ref_axis',(1.,-9.24734323422938E-14,0.));
#26734=DIRECTION('',(1.22464679914735E-16,-1.13397268902426E-29,-1.));
#26735=DIRECTION('center_axis',(0.,0.,1.));
#26736=DIRECTION('ref_axis',(1.,-9.24734323422938E-14,0.));
#26737=DIRECTION('center_axis',(0.,0.,-1.));
#26738=DIRECTION('ref_axis',(1.,-9.24734323422938E-14,0.));
#26739=DIRECTION('',(1.22464679914735E-16,-1.13397268902426E-29,-1.));
#26740=DIRECTION('center_axis',(0.,0.,-1.));
#26741=DIRECTION('ref_axis',(1.,-9.24734323422938E-14,0.));
#26742=DIRECTION('',(1.22464679914735E-16,-1.13397268902426E-29,-1.));
#26743=DIRECTION('center_axis',(0.,0.,-1.));
#26744=DIRECTION('ref_axis',(1.,-9.24734323422938E-14,0.));
#26745=DIRECTION('',(1.22464679914735E-16,-1.13397268902426E-29,-1.));
#26746=DIRECTION('center_axis',(0.,0.,-1.));
#26747=DIRECTION('ref_axis',(1.,-9.24734323422938E-14,0.));
#26748=DIRECTION('',(1.22464679914735E-16,-1.13397268902426E-29,-1.));
#26749=DIRECTION('center_axis',(0.,0.,-1.));
#26750=DIRECTION('ref_axis',(1.,-9.24734323422938E-14,0.));
#26751=DIRECTION('',(1.22464679914735E-16,-1.13397268902426E-29,-1.));
#26752=DIRECTION('center_axis',(0.,0.,-1.));
#26753=DIRECTION('ref_axis',(1.,-9.24734323422938E-14,0.));
#26754=DIRECTION('',(1.22464679914735E-16,-1.13397268902426E-29,-1.));
#26755=DIRECTION('center_axis',(0.,0.,-1.));
#26756=DIRECTION('ref_axis',(1.,-9.24734323422938E-14,0.));
#26757=DIRECTION('',(1.22464679914735E-16,-1.13397268902426E-29,-1.));
#26758=DIRECTION('center_axis',(0.,0.,-1.));
#26759=DIRECTION('ref_axis',(1.,-9.24734323422938E-14,0.));
#26760=DIRECTION('',(1.22464679914735E-16,-1.13397268902426E-29,-1.));
#26761=DIRECTION('center_axis',(0.,0.,-1.));
#26762=DIRECTION('ref_axis',(1.,-9.24734323422938E-14,0.));
#26763=DIRECTION('',(1.22464679914735E-16,-1.13397268902426E-29,-1.));
#26764=DIRECTION('center_axis',(0.,0.,-1.));
#26765=DIRECTION('ref_axis',(1.,-9.24734323422938E-14,0.));
#26766=DIRECTION('',(1.22464679914735E-16,-1.13397268902426E-29,-1.));
#26767=DIRECTION('center_axis',(0.,0.,-1.));
#26768=DIRECTION('ref_axis',(1.,-9.24734323422938E-14,0.));
#26769=DIRECTION('',(1.22464679914735E-16,-1.13397268902426E-29,-1.));
#26770=DIRECTION('center_axis',(0.,0.,-1.));
#26771=DIRECTION('ref_axis',(1.,-9.24734323422938E-14,0.));
#26772=DIRECTION('',(1.22464679914735E-16,-1.13397268902426E-29,-1.));
#26773=DIRECTION('center_axis',(0.,0.,-1.));
#26774=DIRECTION('ref_axis',(1.,-9.24734323422938E-14,0.));
#26775=DIRECTION('',(1.22464679914735E-16,-1.13397268902426E-29,-1.));
#26776=DIRECTION('center_axis',(0.,0.,-1.));
#26777=DIRECTION('ref_axis',(1.,-9.24734323422938E-14,0.));
#26778=DIRECTION('',(1.22464679914735E-16,-1.13397268902426E-29,-1.));
#26779=DIRECTION('center_axis',(0.,0.,-1.));
#26780=DIRECTION('ref_axis',(1.,-9.24734323422938E-14,0.));
#26781=DIRECTION('',(1.22464679914735E-16,-1.13397268902426E-29,-1.));
#26782=DIRECTION('center_axis',(0.,0.,-1.));
#26783=DIRECTION('ref_axis',(1.,-9.24734323422938E-14,0.));
#26784=DIRECTION('',(1.22464679914735E-16,-1.13397268902426E-29,-1.));
#26785=DIRECTION('center_axis',(0.,0.,-1.));
#26786=DIRECTION('ref_axis',(1.,-9.24734323422938E-14,0.));
#26787=DIRECTION('',(1.22464679914735E-16,-1.13397268902426E-29,-1.));
#26788=DIRECTION('center_axis',(0.,0.,-1.));
#26789=DIRECTION('ref_axis',(1.,-9.24734323422938E-14,0.));
#26790=DIRECTION('',(1.22464679914735E-16,-1.13397268902426E-29,-1.));
#26791=DIRECTION('center_axis',(0.,0.,-1.));
#26792=DIRECTION('ref_axis',(-0.609226759132665,-0.792996063014635,0.));
#26793=DIRECTION('',(1.22464679914735E-16,-1.13397268902426E-29,-1.));
#26794=DIRECTION('center_axis',(0.,0.,-1.));
#26795=DIRECTION('ref_axis',(1.,-9.24734323422938E-14,0.));
#26796=DIRECTION('center_axis',(0.,0.,-1.));
#26797=DIRECTION('ref_axis',(1.,-8.09142532995072E-14,0.));
#26798=DIRECTION('',(1.22464679914735E-16,-9.92413572869059E-30,-1.));
#26799=DIRECTION('center_axis',(0.,0.,1.));
#26800=DIRECTION('ref_axis',(1.,-8.09142532995072E-14,0.));
#26801=DIRECTION('center_axis',(0.,0.,-1.));
#26802=DIRECTION('ref_axis',(1.,-8.09142532995072E-14,0.));
#26803=DIRECTION('',(1.22464679914735E-16,-9.92413572869059E-30,-1.));
#26804=DIRECTION('center_axis',(0.,0.,-1.));
#26805=DIRECTION('ref_axis',(1.,-8.09142532995072E-14,0.));
#26806=DIRECTION('',(1.22464679914735E-16,-9.92413572869059E-30,-1.));
#26807=DIRECTION('center_axis',(0.,0.,-1.));
#26808=DIRECTION('ref_axis',(1.,-8.09142532995072E-14,0.));
#26809=DIRECTION('',(1.22464679914735E-16,-9.92413572869059E-30,-1.));
#26810=DIRECTION('center_axis',(0.,0.,-1.));
#26811=DIRECTION('ref_axis',(1.,-8.09142532995072E-14,0.));
#26812=DIRECTION('',(1.22464679914735E-16,-9.92413572869059E-30,-1.));
#26813=DIRECTION('center_axis',(0.,0.,-1.));
#26814=DIRECTION('ref_axis',(1.,-8.09142532995072E-14,0.));
#26815=DIRECTION('',(1.22464679914735E-16,-9.92413572869059E-30,-1.));
#26816=DIRECTION('center_axis',(0.,0.,-1.));
#26817=DIRECTION('ref_axis',(1.,-8.09142532995072E-14,0.));
#26818=DIRECTION('',(1.22464679914735E-16,-9.92413572869059E-30,-1.));
#26819=DIRECTION('center_axis',(0.,0.,-1.));
#26820=DIRECTION('ref_axis',(1.,-8.09142532995072E-14,0.));
#26821=DIRECTION('',(1.22464679914735E-16,-9.92413572869059E-30,-1.));
#26822=DIRECTION('center_axis',(0.,0.,-1.));
#26823=DIRECTION('ref_axis',(1.,-8.09142532995072E-14,0.));
#26824=DIRECTION('',(1.22464679914735E-16,-9.92413572869059E-30,-1.));
#26825=DIRECTION('center_axis',(0.,0.,-1.));
#26826=DIRECTION('ref_axis',(1.,-8.09142532995072E-14,0.));
#26827=DIRECTION('',(1.22464679914735E-16,-9.92413572869059E-30,-1.));
#26828=DIRECTION('center_axis',(0.,0.,-1.));
#26829=DIRECTION('ref_axis',(1.,-8.09142532995072E-14,0.));
#26830=DIRECTION('',(1.22464679914735E-16,-9.92413572869059E-30,-1.));
#26831=DIRECTION('center_axis',(0.,0.,-1.));
#26832=DIRECTION('ref_axis',(1.,-8.09142532995072E-14,0.));
#26833=DIRECTION('',(1.22464679914735E-16,-9.92413572869059E-30,-1.));
#26834=DIRECTION('center_axis',(0.,0.,-1.));
#26835=DIRECTION('ref_axis',(1.,-8.09142532995072E-14,0.));
#26836=DIRECTION('',(1.22464679914735E-16,-9.92413572869059E-30,-1.));
#26837=DIRECTION('center_axis',(0.,0.,-1.));
#26838=DIRECTION('ref_axis',(1.,-8.09142532995072E-14,0.));
#26839=DIRECTION('',(1.22464679914735E-16,-9.92413572869059E-30,-1.));
#26840=DIRECTION('center_axis',(0.,0.,-1.));
#26841=DIRECTION('ref_axis',(1.,-8.09142532995072E-14,0.));
#26842=DIRECTION('',(1.22464679914735E-16,-9.92413572869059E-30,-1.));
#26843=DIRECTION('center_axis',(0.,0.,-1.));
#26844=DIRECTION('ref_axis',(1.,-8.09142532995072E-14,0.));
#26845=DIRECTION('',(1.22464679914735E-16,-9.92413572869059E-30,-1.));
#26846=DIRECTION('center_axis',(0.,0.,-1.));
#26847=DIRECTION('ref_axis',(1.,-8.09142532995072E-14,0.));
#26848=DIRECTION('',(1.22464679914735E-16,-9.92413572869059E-30,-1.));
#26849=DIRECTION('center_axis',(0.,0.,-1.));
#26850=DIRECTION('ref_axis',(1.,-8.09142532995072E-14,0.));
#26851=DIRECTION('',(1.22464679914735E-16,-9.92413572869059E-30,-1.));
#26852=DIRECTION('center_axis',(0.,0.,-1.));
#26853=DIRECTION('ref_axis',(1.,-8.09142532995072E-14,0.));
#26854=DIRECTION('',(1.22464679914735E-16,-9.92413572869059E-30,-1.));
#26855=DIRECTION('center_axis',(0.,0.,-1.));
#26856=DIRECTION('ref_axis',(-0.60922700896484,-0.79299587107863,0.));
#26857=DIRECTION('',(1.22464679914735E-16,-9.92413572869059E-30,-1.));
#26858=DIRECTION('center_axis',(0.,0.,-1.));
#26859=DIRECTION('ref_axis',(1.,-8.09142532995072E-14,0.));
#26860=DIRECTION('center_axis',(0.,0.,-1.));
#26861=DIRECTION('ref_axis',(1.,-5.77958952139344E-14,0.));
#26862=DIRECTION('',(1.22464679914735E-16,-7.09295340558668E-30,-1.));
#26863=DIRECTION('center_axis',(0.,0.,1.));
#26864=DIRECTION('ref_axis',(1.,-5.77958952139344E-14,0.));
#26865=DIRECTION('center_axis',(0.,0.,-1.));
#26866=DIRECTION('ref_axis',(1.,-5.77958952139344E-14,0.));
#26867=DIRECTION('',(1.22464679914735E-16,-7.09295340558668E-30,-1.));
#26868=DIRECTION('center_axis',(0.,0.,-1.));
#26869=DIRECTION('ref_axis',(1.,-5.77958952139344E-14,0.));
#26870=DIRECTION('',(1.22464679914735E-16,-7.09295340558668E-30,-1.));
#26871=DIRECTION('center_axis',(0.,0.,-1.));
#26872=DIRECTION('ref_axis',(1.,-5.77958952139344E-14,0.));
#26873=DIRECTION('',(1.22464679914735E-16,-7.09295340558668E-30,-1.));
#26874=DIRECTION('center_axis',(0.,0.,-1.));
#26875=DIRECTION('ref_axis',(1.,-5.77958952139344E-14,0.));
#26876=DIRECTION('',(1.22464679914735E-16,-7.09295340558668E-30,-1.));
#26877=DIRECTION('center_axis',(0.,0.,-1.));
#26878=DIRECTION('ref_axis',(1.,-5.77958952139344E-14,0.));
#26879=DIRECTION('',(1.22464679914735E-16,-7.09295340558668E-30,-1.));
#26880=DIRECTION('center_axis',(0.,0.,-1.));
#26881=DIRECTION('ref_axis',(1.,-5.77958952139344E-14,0.));
#26882=DIRECTION('',(1.22464679914735E-16,-7.09295340558668E-30,-1.));
#26883=DIRECTION('center_axis',(0.,0.,-1.));
#26884=DIRECTION('ref_axis',(1.,-5.77958952139344E-14,0.));
#26885=DIRECTION('',(1.22464679914735E-16,-7.09295340558668E-30,-1.));
#26886=DIRECTION('center_axis',(0.,0.,-1.));
#26887=DIRECTION('ref_axis',(1.,-5.77958952139344E-14,0.));
#26888=DIRECTION('',(1.22464679914735E-16,-7.09295340558668E-30,-1.));
#26889=DIRECTION('center_axis',(0.,0.,-1.));
#26890=DIRECTION('ref_axis',(1.,-5.77958952139344E-14,0.));
#26891=DIRECTION('',(1.22464679914735E-16,-7.09295340558668E-30,-1.));
#26892=DIRECTION('center_axis',(0.,0.,-1.));
#26893=DIRECTION('ref_axis',(1.,-5.77958952139344E-14,0.));
#26894=DIRECTION('',(1.22464679914735E-16,-7.09295340558668E-30,-1.));
#26895=DIRECTION('center_axis',(0.,0.,-1.));
#26896=DIRECTION('ref_axis',(1.,-5.77958952139344E-14,0.));
#26897=DIRECTION('',(1.22464679914735E-16,-7.09295340558668E-30,-1.));
#26898=DIRECTION('center_axis',(0.,0.,-1.));
#26899=DIRECTION('ref_axis',(1.,-5.77958952139344E-14,0.));
#26900=DIRECTION('',(1.22464679914735E-16,-7.09295340558668E-30,-1.));
#26901=DIRECTION('center_axis',(0.,0.,-1.));
#26902=DIRECTION('ref_axis',(1.,-5.77958952139344E-14,0.));
#26903=DIRECTION('',(1.22464679914735E-16,-7.09295340558668E-30,-1.));
#26904=DIRECTION('center_axis',(0.,0.,-1.));
#26905=DIRECTION('ref_axis',(1.,-5.77958952139344E-14,0.));
#26906=DIRECTION('',(1.22464679914735E-16,-7.09295340558668E-30,-1.));
#26907=DIRECTION('center_axis',(0.,0.,-1.));
#26908=DIRECTION('ref_axis',(1.,-5.77958952139344E-14,0.));
#26909=DIRECTION('',(1.22464679914735E-16,-7.09295340558668E-30,-1.));
#26910=DIRECTION('center_axis',(0.,0.,-1.));
#26911=DIRECTION('ref_axis',(1.,-5.77958952139344E-14,0.));
#26912=DIRECTION('',(1.22464679914735E-16,-7.09295340558668E-30,-1.));
#26913=DIRECTION('center_axis',(0.,0.,-1.));
#26914=DIRECTION('ref_axis',(1.,-5.77958952139344E-14,0.));
#26915=DIRECTION('',(1.22464679914735E-16,-7.09295340558668E-30,-1.));
#26916=DIRECTION('center_axis',(0.,0.,-1.));
#26917=DIRECTION('ref_axis',(1.,-5.77958952139344E-14,0.));
#26918=DIRECTION('',(1.22464679914735E-16,-7.09295340558668E-30,-1.));
#26919=DIRECTION('center_axis',(0.,0.,-1.));
#26920=DIRECTION('ref_axis',(-0.609226998768103,-0.792995878912375,0.));
#26921=DIRECTION('',(1.22464679914735E-16,-7.09295340558668E-30,-1.));
#26922=DIRECTION('center_axis',(0.,0.,-1.));
#26923=DIRECTION('ref_axis',(1.,-5.77958952139344E-14,0.));
#26924=DIRECTION('center_axis',(0.,0.,-1.));
#26925=DIRECTION('ref_axis',(1.,-8.09142532995081E-14,0.));
#26926=DIRECTION('',(1.22464679914735E-16,-9.9241357286907E-30,-1.));
#26927=DIRECTION('center_axis',(0.,0.,1.));
#26928=DIRECTION('ref_axis',(1.,-8.09142532995081E-14,0.));
#26929=DIRECTION('center_axis',(0.,0.,-1.));
#26930=DIRECTION('ref_axis',(1.,-8.09142532995081E-14,0.));
#26931=DIRECTION('',(1.22464679914735E-16,-9.9241357286907E-30,-1.));
#26932=DIRECTION('center_axis',(0.,0.,-1.));
#26933=DIRECTION('ref_axis',(1.,-8.09142532995081E-14,0.));
#26934=DIRECTION('',(1.22464679914735E-16,-9.9241357286907E-30,-1.));
#26935=DIRECTION('center_axis',(0.,0.,-1.));
#26936=DIRECTION('ref_axis',(1.,-8.09142532995081E-14,0.));
#26937=DIRECTION('',(1.22464679914735E-16,-9.9241357286907E-30,-1.));
#26938=DIRECTION('center_axis',(0.,0.,-1.));
#26939=DIRECTION('ref_axis',(1.,-8.09142532995081E-14,0.));
#26940=DIRECTION('',(1.22464679914735E-16,-9.9241357286907E-30,-1.));
#26941=DIRECTION('center_axis',(0.,0.,-1.));
#26942=DIRECTION('ref_axis',(1.,-8.09142532995081E-14,0.));
#26943=DIRECTION('',(1.22464679914735E-16,-9.9241357286907E-30,-1.));
#26944=DIRECTION('center_axis',(0.,0.,-1.));
#26945=DIRECTION('ref_axis',(1.,-8.09142532995081E-14,0.));
#26946=DIRECTION('',(1.22464679914735E-16,-9.9241357286907E-30,-1.));
#26947=DIRECTION('center_axis',(0.,0.,-1.));
#26948=DIRECTION('ref_axis',(1.,-8.09142532995081E-14,0.));
#26949=DIRECTION('',(1.22464679914735E-16,-9.9241357286907E-30,-1.));
#26950=DIRECTION('center_axis',(0.,0.,-1.));
#26951=DIRECTION('ref_axis',(1.,-8.09142532995081E-14,0.));
#26952=DIRECTION('',(1.22464679914735E-16,-9.9241357286907E-30,-1.));
#26953=DIRECTION('center_axis',(0.,0.,-1.));
#26954=DIRECTION('ref_axis',(1.,-8.09142532995081E-14,0.));
#26955=DIRECTION('',(1.22464679914735E-16,-9.9241357286907E-30,-1.));
#26956=DIRECTION('center_axis',(0.,0.,-1.));
#26957=DIRECTION('ref_axis',(1.,-8.09142532995081E-14,0.));
#26958=DIRECTION('',(1.22464679914735E-16,-9.9241357286907E-30,-1.));
#26959=DIRECTION('center_axis',(0.,0.,-1.));
#26960=DIRECTION('ref_axis',(1.,-8.09142532995081E-14,0.));
#26961=DIRECTION('',(1.22464679914735E-16,-9.9241357286907E-30,-1.));
#26962=DIRECTION('center_axis',(0.,0.,-1.));
#26963=DIRECTION('ref_axis',(1.,-8.09142532995081E-14,0.));
#26964=DIRECTION('',(1.22464679914735E-16,-9.9241357286907E-30,-1.));
#26965=DIRECTION('center_axis',(0.,0.,-1.));
#26966=DIRECTION('ref_axis',(1.,-8.09142532995081E-14,0.));
#26967=DIRECTION('',(1.22464679914735E-16,-9.9241357286907E-30,-1.));
#26968=DIRECTION('center_axis',(0.,0.,-1.));
#26969=DIRECTION('ref_axis',(1.,-8.09142532995081E-14,0.));
#26970=DIRECTION('',(1.22464679914735E-16,-9.9241357286907E-30,-1.));
#26971=DIRECTION('center_axis',(0.,0.,-1.));
#26972=DIRECTION('ref_axis',(1.,-8.09142532995081E-14,0.));
#26973=DIRECTION('',(1.22464679914735E-16,-9.9241357286907E-30,-1.));
#26974=DIRECTION('center_axis',(0.,0.,-1.));
#26975=DIRECTION('ref_axis',(1.,-8.09142532995081E-14,0.));
#26976=DIRECTION('',(1.22464679914735E-16,-9.9241357286907E-30,-1.));
#26977=DIRECTION('center_axis',(0.,0.,-1.));
#26978=DIRECTION('ref_axis',(1.,-8.09142532995081E-14,0.));
#26979=DIRECTION('',(1.22464679914735E-16,-9.9241357286907E-30,-1.));
#26980=DIRECTION('center_axis',(0.,0.,-1.));
#26981=DIRECTION('ref_axis',(1.,-8.09142532995081E-14,0.));
#26982=DIRECTION('',(1.22464679914735E-16,-9.9241357286907E-30,-1.));
#26983=DIRECTION('center_axis',(0.,0.,-1.));
#26984=DIRECTION('ref_axis',(-0.609227002488276,-0.792995876054315,0.));
#26985=DIRECTION('',(1.22464679914735E-16,-9.9241357286907E-30,-1.));
#26986=DIRECTION('center_axis',(0.,0.,-1.));
#26987=DIRECTION('ref_axis',(1.,-8.09142532995081E-14,0.));
#26988=DIRECTION('center_axis',(0.,0.,-1.));
#26989=DIRECTION('ref_axis',(1.,-1.04032611385081E-13,0.));
#26990=DIRECTION('',(1.22464679914735E-16,-1.27553180517946E-29,-1.));
#26991=DIRECTION('center_axis',(0.,0.,1.));
#26992=DIRECTION('ref_axis',(1.,-1.04032611385081E-13,0.));
#26993=DIRECTION('center_axis',(0.,0.,-1.));
#26994=DIRECTION('ref_axis',(1.,-1.04032611385081E-13,0.));
#26995=DIRECTION('',(1.22464679914735E-16,-1.27553180517946E-29,-1.));
#26996=DIRECTION('center_axis',(0.,0.,-1.));
#26997=DIRECTION('ref_axis',(1.,-1.04032611385081E-13,0.));
#26998=DIRECTION('',(1.22464679914735E-16,-1.27553180517946E-29,-1.));
#26999=DIRECTION('center_axis',(0.,0.,-1.));
#27000=DIRECTION('ref_axis',(1.,-1.04032611385081E-13,0.));
#27001=DIRECTION('',(1.22464679914735E-16,-1.27553180517946E-29,-1.));
#27002=DIRECTION('center_axis',(0.,0.,-1.));
#27003=DIRECTION('ref_axis',(1.,-1.04032611385081E-13,0.));
#27004=DIRECTION('',(1.22464679914735E-16,-1.27553180517946E-29,-1.));
#27005=DIRECTION('center_axis',(0.,0.,-1.));
#27006=DIRECTION('ref_axis',(1.,-1.04032611385081E-13,0.));
#27007=DIRECTION('',(1.22464679914735E-16,-1.27553180517946E-29,-1.));
#27008=DIRECTION('center_axis',(0.,0.,-1.));
#27009=DIRECTION('ref_axis',(1.,-1.04032611385081E-13,0.));
#27010=DIRECTION('',(1.22464679914735E-16,-1.27553180517946E-29,-1.));
#27011=DIRECTION('center_axis',(0.,0.,-1.));
#27012=DIRECTION('ref_axis',(1.,-1.04032611385081E-13,0.));
#27013=DIRECTION('',(1.22464679914735E-16,-1.27553180517946E-29,-1.));
#27014=DIRECTION('center_axis',(0.,0.,-1.));
#27015=DIRECTION('ref_axis',(1.,-1.04032611385081E-13,0.));
#27016=DIRECTION('',(1.22464679914735E-16,-1.27553180517946E-29,-1.));
#27017=DIRECTION('center_axis',(0.,0.,-1.));
#27018=DIRECTION('ref_axis',(1.,-1.04032611385081E-13,0.));
#27019=DIRECTION('',(1.22464679914735E-16,-1.27553180517946E-29,-1.));
#27020=DIRECTION('center_axis',(0.,0.,-1.));
#27021=DIRECTION('ref_axis',(1.,-1.04032611385081E-13,0.));
#27022=DIRECTION('',(1.22464679914735E-16,-1.27553180517946E-29,-1.));
#27023=DIRECTION('center_axis',(0.,0.,-1.));
#27024=DIRECTION('ref_axis',(1.,-1.04032611385081E-13,0.));
#27025=DIRECTION('',(1.22464679914735E-16,-1.27553180517946E-29,-1.));
#27026=DIRECTION('center_axis',(0.,0.,-1.));
#27027=DIRECTION('ref_axis',(1.,-1.04032611385081E-13,0.));
#27028=DIRECTION('',(1.22464679914735E-16,-1.27553180517946E-29,-1.));
#27029=DIRECTION('center_axis',(0.,0.,-1.));
#27030=DIRECTION('ref_axis',(1.,-1.04032611385081E-13,0.));
#27031=DIRECTION('',(1.22464679914735E-16,-1.27553180517946E-29,-1.));
#27032=DIRECTION('center_axis',(0.,0.,-1.));
#27033=DIRECTION('ref_axis',(1.,-1.04032611385081E-13,0.));
#27034=DIRECTION('',(1.22464679914735E-16,-1.27553180517946E-29,-1.));
#27035=DIRECTION('center_axis',(0.,0.,-1.));
#27036=DIRECTION('ref_axis',(1.,-1.04032611385081E-13,0.));
#27037=DIRECTION('',(1.22464679914735E-16,-1.27553180517946E-29,-1.));
#27038=DIRECTION('center_axis',(0.,0.,-1.));
#27039=DIRECTION('ref_axis',(1.,-1.04032611385081E-13,0.));
#27040=DIRECTION('',(1.22464679914735E-16,-1.27553180517946E-29,-1.));
#27041=DIRECTION('center_axis',(0.,0.,-1.));
#27042=DIRECTION('ref_axis',(1.,-1.04032611385081E-13,0.));
#27043=DIRECTION('',(1.22464679914735E-16,-1.27553180517946E-29,-1.));
#27044=DIRECTION('center_axis',(0.,0.,-1.));
#27045=DIRECTION('ref_axis',(1.,-1.04032611385081E-13,0.));
#27046=DIRECTION('',(1.22464679914735E-16,-1.27553180517946E-29,-1.));
#27047=DIRECTION('center_axis',(0.,0.,-1.));
#27048=DIRECTION('ref_axis',(-0.60922700588817,-0.792995873442312,0.));
#27049=DIRECTION('',(1.22464679914735E-16,-1.27553180517946E-29,-1.));
#27050=DIRECTION('center_axis',(0.,0.,-1.));
#27051=DIRECTION('ref_axis',(1.,-1.04032611385081E-13,0.));
#27052=DIRECTION('center_axis',(0.,0.,-1.));
#27053=DIRECTION('ref_axis',(1.,-9.24734323422938E-14,0.));
#27054=DIRECTION('',(1.22464679914735E-16,-1.13397268902426E-29,-1.));
#27055=DIRECTION('center_axis',(0.,0.,1.));
#27056=DIRECTION('ref_axis',(1.,-9.24734323422938E-14,0.));
#27057=DIRECTION('center_axis',(0.,0.,-1.));
#27058=DIRECTION('ref_axis',(1.,-9.24734323422938E-14,0.));
#27059=DIRECTION('',(1.22464679914735E-16,-1.13397268902426E-29,-1.));
#27060=DIRECTION('center_axis',(0.,0.,-1.));
#27061=DIRECTION('ref_axis',(1.,-9.24734323422938E-14,0.));
#27062=DIRECTION('',(1.22464679914735E-16,-1.13397268902426E-29,-1.));
#27063=DIRECTION('center_axis',(0.,0.,-1.));
#27064=DIRECTION('ref_axis',(1.,-9.24734323422938E-14,0.));
#27065=DIRECTION('',(1.22464679914735E-16,-1.13397268902426E-29,-1.));
#27066=DIRECTION('center_axis',(0.,0.,-1.));
#27067=DIRECTION('ref_axis',(1.,-9.24734323422938E-14,0.));
#27068=DIRECTION('',(1.22464679914735E-16,-1.13397268902426E-29,-1.));
#27069=DIRECTION('center_axis',(0.,0.,-1.));
#27070=DIRECTION('ref_axis',(1.,-9.24734323422938E-14,0.));
#27071=DIRECTION('',(1.22464679914735E-16,-1.13397268902426E-29,-1.));
#27072=DIRECTION('center_axis',(0.,0.,-1.));
#27073=DIRECTION('ref_axis',(1.,-9.24734323422938E-14,0.));
#27074=DIRECTION('',(1.22464679914735E-16,-1.13397268902426E-29,-1.));
#27075=DIRECTION('center_axis',(0.,0.,-1.));
#27076=DIRECTION('ref_axis',(1.,-9.24734323422938E-14,0.));
#27077=DIRECTION('',(1.22464679914735E-16,-1.13397268902426E-29,-1.));
#27078=DIRECTION('center_axis',(0.,0.,-1.));
#27079=DIRECTION('ref_axis',(1.,-9.24734323422938E-14,0.));
#27080=DIRECTION('',(1.22464679914735E-16,-1.13397268902426E-29,-1.));
#27081=DIRECTION('center_axis',(0.,0.,-1.));
#27082=DIRECTION('ref_axis',(1.,-9.24734323422938E-14,0.));
#27083=DIRECTION('',(1.22464679914735E-16,-1.13397268902426E-29,-1.));
#27084=DIRECTION('center_axis',(0.,0.,-1.));
#27085=DIRECTION('ref_axis',(1.,-9.24734323422938E-14,0.));
#27086=DIRECTION('',(1.22464679914735E-16,-1.13397268902426E-29,-1.));
#27087=DIRECTION('center_axis',(0.,0.,-1.));
#27088=DIRECTION('ref_axis',(1.,-9.24734323422938E-14,0.));
#27089=DIRECTION('',(1.22464679914735E-16,-1.13397268902426E-29,-1.));
#27090=DIRECTION('center_axis',(0.,0.,-1.));
#27091=DIRECTION('ref_axis',(1.,-9.24734323422938E-14,0.));
#27092=DIRECTION('',(1.22464679914735E-16,-1.13397268902426E-29,-1.));
#27093=DIRECTION('center_axis',(0.,0.,-1.));
#27094=DIRECTION('ref_axis',(1.,-9.24734323422938E-14,0.));
#27095=DIRECTION('',(1.22464679914735E-16,-1.13397268902426E-29,-1.));
#27096=DIRECTION('center_axis',(0.,0.,-1.));
#27097=DIRECTION('ref_axis',(1.,-9.24734323422938E-14,0.));
#27098=DIRECTION('',(1.22464679914735E-16,-1.13397268902426E-29,-1.));
#27099=DIRECTION('center_axis',(0.,0.,-1.));
#27100=DIRECTION('ref_axis',(1.,-9.24734323422938E-14,0.));
#27101=DIRECTION('',(1.22464679914735E-16,-1.13397268902426E-29,-1.));
#27102=DIRECTION('center_axis',(0.,0.,-1.));
#27103=DIRECTION('ref_axis',(1.,-9.24734323422938E-14,0.));
#27104=DIRECTION('',(1.22464679914735E-16,-1.13397268902426E-29,-1.));
#27105=DIRECTION('center_axis',(0.,0.,-1.));
#27106=DIRECTION('ref_axis',(1.,-9.24734323422938E-14,0.));
#27107=DIRECTION('',(1.22464679914735E-16,-1.13397268902426E-29,-1.));
#27108=DIRECTION('center_axis',(0.,0.,-1.));
#27109=DIRECTION('ref_axis',(1.,-9.24734323422938E-14,0.));
#27110=DIRECTION('',(1.22464679914735E-16,-1.13397268902426E-29,-1.));
#27111=DIRECTION('center_axis',(0.,0.,-1.));
#27112=DIRECTION('ref_axis',(-0.609226762267633,-0.792996060606165,0.));
#27113=DIRECTION('',(1.22464679914735E-16,-1.13397268902426E-29,-1.));
#27114=DIRECTION('center_axis',(0.,0.,-1.));
#27115=DIRECTION('ref_axis',(1.,-9.24734323422938E-14,0.));
#27116=DIRECTION('center_axis',(0.,0.,-1.));
#27117=DIRECTION('ref_axis',(1.,-9.24734323422938E-14,0.));
#27118=DIRECTION('center_axis',(0.,0.,1.));
#27119=DIRECTION('ref_axis',(1.,0.,0.));
#27120=DIRECTION('',(0.,-1.,0.));
#27121=DIRECTION('',(1.,0.,0.));
#27122=DIRECTION('',(0.,1.,0.));
#27123=DIRECTION('',(-1.,0.,0.));
#27124=DIRECTION('center_axis',(0.,0.,-1.));
#27125=DIRECTION('ref_axis',(1.,-1.04032611385081E-13,0.));
#27126=DIRECTION('center_axis',(0.,0.,-1.));
#27127=DIRECTION('ref_axis',(1.,-8.09142532995081E-14,0.));
#27128=DIRECTION('center_axis',(0.,0.,-1.));
#27129=DIRECTION('ref_axis',(1.,-5.77958952139344E-14,0.));
#27130=DIRECTION('center_axis',(0.,0.,-1.));
#27131=DIRECTION('ref_axis',(1.,-8.09142532995072E-14,0.));
#27132=DIRECTION('center_axis',(0.,0.,-1.));
#27133=DIRECTION('ref_axis',(1.,-9.24734323422938E-14,0.));
#27134=DIRECTION('center_axis',(0.,0.,-1.));
#27135=DIRECTION('ref_axis',(1.,0.,0.));
#27136=DIRECTION('center_axis',(0.,0.,-1.));
#27137=DIRECTION('ref_axis',(1.,0.,0.));
#27138=DIRECTION('center_axis',(0.,0.,-1.));
#27139=DIRECTION('ref_axis',(1.,0.,0.));
#27140=DIRECTION('center_axis',(0.,0.,-1.));
#27141=DIRECTION('ref_axis',(1.,0.,0.));
#27142=DIRECTION('center_axis',(0.,0.,-1.));
#27143=DIRECTION('ref_axis',(1.,0.,0.));
#27144=DIRECTION('center_axis',(0.,0.,-1.));
#27145=DIRECTION('ref_axis',(1.,0.,0.));
#27146=DIRECTION('center_axis',(0.,1.,0.));
#27147=DIRECTION('ref_axis',(-1.,0.,0.));
#27148=DIRECTION('',(-1.,0.,0.));
#27149=DIRECTION('',(0.,0.,1.));
#27150=DIRECTION('',(0.,0.,1.));
#27151=DIRECTION('center_axis',(1.,0.,0.));
#27152=DIRECTION('ref_axis',(0.,1.,0.));
#27153=DIRECTION('',(0.,1.,0.));
#27154=DIRECTION('',(0.,0.,1.));
#27155=DIRECTION('center_axis',(0.,-1.,0.));
#27156=DIRECTION('ref_axis',(1.,0.,0.));
#27157=DIRECTION('',(1.,0.,0.));
#27158=DIRECTION('',(0.,0.,1.));
#27159=DIRECTION('center_axis',(-1.,0.,0.));
#27160=DIRECTION('ref_axis',(0.,-1.,0.));
#27161=DIRECTION('',(0.,-1.,0.));
#27162=DIRECTION('center_axis',(0.,0.,1.));
#27163=DIRECTION('ref_axis',(1.,0.,0.));
#27164=DIRECTION('axis',(0.,0.,1.));
#27165=DIRECTION('refdir',(1.,0.,0.));
#27166=DIRECTION('center_axis',(0.,0.,1.));
#27167=DIRECTION('ref_axis',(1.,0.,0.));
#27168=DIRECTION('',(0.,0.,-1.));
#27169=DIRECTION('center_axis',(0.,0.,-1.));
#27170=DIRECTION('ref_axis',(1.,0.,0.));
#27171=DIRECTION('center_axis',(0.,0.,1.));
#27172=DIRECTION('ref_axis',(1.,0.,0.));
#27173=DIRECTION('',(0.,0.,-1.));
#27174=DIRECTION('center_axis',(0.,0.,1.));
#27175=DIRECTION('ref_axis',(1.,0.,0.));
#27176=DIRECTION('',(0.,0.,-1.));
#27177=DIRECTION('center_axis',(0.,0.,1.));
#27178=DIRECTION('ref_axis',(1.,0.,0.));
#27179=DIRECTION('',(0.,0.,-1.));
#27180=DIRECTION('center_axis',(0.,0.,1.));
#27181=DIRECTION('ref_axis',(1.,0.,0.));
#27182=DIRECTION('',(0.,0.,-1.));
#27183=DIRECTION('center_axis',(0.,0.,1.));
#27184=DIRECTION('ref_axis',(1.,0.,0.));
#27185=DIRECTION('',(0.,0.,-1.));
#27186=DIRECTION('center_axis',(0.,0.,1.));
#27187=DIRECTION('ref_axis',(1.,0.,0.));
#27188=DIRECTION('',(0.,0.,-1.));
#27189=DIRECTION('center_axis',(0.,0.,1.));
#27190=DIRECTION('ref_axis',(1.,0.,0.));
#27191=DIRECTION('',(0.,0.,-1.));
#27192=DIRECTION('center_axis',(0.,0.,1.));
#27193=DIRECTION('ref_axis',(1.,0.,0.));
#27194=DIRECTION('',(0.,0.,-1.));
#27195=DIRECTION('center_axis',(0.,0.,1.));
#27196=DIRECTION('ref_axis',(1.,0.,0.));
#27197=DIRECTION('',(0.,0.,-1.));
#27198=DIRECTION('center_axis',(0.,0.,1.));
#27199=DIRECTION('ref_axis',(1.,0.,0.));
#27200=DIRECTION('',(0.,0.,-1.));
#27201=DIRECTION('center_axis',(0.,0.,1.));
#27202=DIRECTION('ref_axis',(1.,0.,0.));
#27203=DIRECTION('',(0.,0.,-1.));
#27204=DIRECTION('center_axis',(0.,0.,1.));
#27205=DIRECTION('ref_axis',(1.,0.,0.));
#27206=DIRECTION('',(0.,0.,-1.));
#27207=DIRECTION('center_axis',(0.,0.,1.));
#27208=DIRECTION('ref_axis',(1.,0.,0.));
#27209=DIRECTION('',(0.,0.,-1.));
#27210=DIRECTION('center_axis',(0.,0.,1.));
#27211=DIRECTION('ref_axis',(1.,0.,0.));
#27212=DIRECTION('',(0.,0.,-1.));
#27213=DIRECTION('center_axis',(0.,0.,1.));
#27214=DIRECTION('ref_axis',(1.,0.,0.));
#27215=DIRECTION('',(0.,0.,-1.));
#27216=DIRECTION('center_axis',(0.,0.,1.));
#27217=DIRECTION('ref_axis',(1.,0.,0.));
#27218=DIRECTION('',(0.,0.,-1.));
#27219=DIRECTION('center_axis',(0.,0.,1.));
#27220=DIRECTION('ref_axis',(1.,0.,0.));
#27221=DIRECTION('',(0.,0.,-1.));
#27222=DIRECTION('center_axis',(0.,0.,1.));
#27223=DIRECTION('ref_axis',(1.,0.,0.));
#27224=DIRECTION('',(0.,0.,-1.));
#27225=DIRECTION('center_axis',(0.,0.,1.));
#27226=DIRECTION('ref_axis',(1.,0.,0.));
#27227=DIRECTION('',(0.,0.,-1.));
#27228=DIRECTION('center_axis',(0.,0.,1.));
#27229=DIRECTION('ref_axis',(1.,0.,0.));
#27230=DIRECTION('',(0.,0.,-1.));
#27231=DIRECTION('center_axis',(0.,0.,1.));
#27232=DIRECTION('ref_axis',(1.,0.,0.));
#27233=DIRECTION('',(0.,0.,-1.));
#27234=DIRECTION('center_axis',(0.,0.,1.));
#27235=DIRECTION('ref_axis',(1.,0.,0.));
#27236=DIRECTION('',(0.,0.,-1.));
#27237=DIRECTION('center_axis',(0.,0.,1.));
#27238=DIRECTION('ref_axis',(1.,0.,0.));
#27239=DIRECTION('',(0.,0.,-1.));
#27240=DIRECTION('center_axis',(0.,0.,1.));
#27241=DIRECTION('ref_axis',(1.,0.,0.));
#27242=DIRECTION('',(0.,0.,-1.));
#27243=DIRECTION('center_axis',(0.,0.,1.));
#27244=DIRECTION('ref_axis',(1.,0.,0.));
#27245=DIRECTION('',(0.,0.,-1.));
#27246=DIRECTION('center_axis',(0.,0.,1.));
#27247=DIRECTION('ref_axis',(1.,0.,0.));
#27248=DIRECTION('',(0.,0.,-1.));
#27249=DIRECTION('center_axis',(0.,0.,1.));
#27250=DIRECTION('ref_axis',(1.,0.,0.));
#27251=DIRECTION('',(0.,0.,-1.));
#27252=DIRECTION('center_axis',(0.,0.,1.));
#27253=DIRECTION('ref_axis',(1.,0.,0.));
#27254=DIRECTION('',(0.,0.,-1.));
#27255=DIRECTION('center_axis',(0.,0.,1.));
#27256=DIRECTION('ref_axis',(1.,0.,0.));
#27257=DIRECTION('',(0.,0.,-1.));
#27258=DIRECTION('center_axis',(0.,0.,1.));
#27259=DIRECTION('ref_axis',(1.,0.,0.));
#27260=DIRECTION('',(0.,0.,-1.));
#27261=DIRECTION('center_axis',(0.,0.,1.));
#27262=DIRECTION('ref_axis',(1.,0.,0.));
#27263=DIRECTION('',(0.,0.,-1.));
#27264=DIRECTION('center_axis',(0.,0.,1.));
#27265=DIRECTION('ref_axis',(1.,0.,0.));
#27266=DIRECTION('',(0.,0.,-1.));
#27267=DIRECTION('center_axis',(0.,0.,1.));
#27268=DIRECTION('ref_axis',(1.,0.,0.));
#27269=DIRECTION('',(0.,0.,-1.));
#27270=DIRECTION('center_axis',(0.,0.,1.));
#27271=DIRECTION('ref_axis',(1.,0.,0.));
#27272=DIRECTION('',(0.,0.,-1.));
#27273=DIRECTION('center_axis',(0.,0.,1.));
#27274=DIRECTION('ref_axis',(1.,0.,0.));
#27275=DIRECTION('',(0.,0.,-1.));
#27276=DIRECTION('center_axis',(0.,0.,1.));
#27277=DIRECTION('ref_axis',(1.,0.,0.));
#27278=DIRECTION('',(0.,0.,-1.));
#27279=DIRECTION('center_axis',(0.,0.,1.));
#27280=DIRECTION('ref_axis',(1.,0.,0.));
#27281=DIRECTION('',(0.,0.,-1.));
#27282=DIRECTION('center_axis',(0.,0.,1.));
#27283=DIRECTION('ref_axis',(1.,0.,0.));
#27284=DIRECTION('',(0.,0.,-1.));
#27285=DIRECTION('center_axis',(0.,0.,1.));
#27286=DIRECTION('ref_axis',(1.,0.,0.));
#27287=DIRECTION('',(0.,0.,-1.));
#27288=DIRECTION('center_axis',(0.,0.,1.));
#27289=DIRECTION('ref_axis',(1.,0.,0.));
#27290=DIRECTION('',(0.,0.,-1.));
#27291=DIRECTION('center_axis',(0.,0.,1.));
#27292=DIRECTION('ref_axis',(1.,0.,0.));
#27293=DIRECTION('',(0.,0.,-1.));
#27294=DIRECTION('center_axis',(0.,0.,1.));
#27295=DIRECTION('ref_axis',(1.,0.,0.));
#27296=DIRECTION('',(0.,0.,-1.));
#27297=DIRECTION('center_axis',(0.,0.,1.));
#27298=DIRECTION('ref_axis',(1.,0.,0.));
#27299=DIRECTION('',(0.,0.,-1.));
#27300=DIRECTION('center_axis',(0.,0.,1.));
#27301=DIRECTION('ref_axis',(1.,0.,0.));
#27302=DIRECTION('',(0.,0.,-1.));
#27303=DIRECTION('center_axis',(0.,0.,1.));
#27304=DIRECTION('ref_axis',(1.,0.,0.));
#27305=DIRECTION('',(0.,0.,-1.));
#27306=DIRECTION('center_axis',(0.,0.,1.));
#27307=DIRECTION('ref_axis',(1.,0.,0.));
#27308=DIRECTION('',(0.,0.,-1.));
#27309=DIRECTION('center_axis',(0.,0.,1.));
#27310=DIRECTION('ref_axis',(1.,0.,0.));
#27311=DIRECTION('',(0.,0.,-1.));
#27312=DIRECTION('center_axis',(0.,0.,1.));
#27313=DIRECTION('ref_axis',(1.,0.,0.));
#27314=DIRECTION('',(0.,0.,-1.));
#27315=DIRECTION('center_axis',(0.,0.,1.));
#27316=DIRECTION('ref_axis',(0.997333003469248,-0.0729854793161552,0.));
#27317=DIRECTION('',(0.,0.,1.));
#27318=DIRECTION('center_axis',(0.,0.,-1.));
#27319=DIRECTION('ref_axis',(1.,-7.35649788641118E-13,0.));
#27320=DIRECTION('center_axis',(0.,0.,1.));
#27321=DIRECTION('ref_axis',(1.,-7.35649788641118E-13,0.));
#27322=DIRECTION('',(0.,0.,1.));
#27323=DIRECTION('center_axis',(0.,0.,1.));
#27324=DIRECTION('ref_axis',(1.,-7.35649788641118E-13,0.));
#27325=DIRECTION('',(0.,0.,1.));
#27326=DIRECTION('center_axis',(0.,0.,1.));
#27327=DIRECTION('ref_axis',(1.,-7.35649788641118E-13,0.));
#27328=DIRECTION('',(0.,0.,1.));
#27329=DIRECTION('center_axis',(0.,0.,1.));
#27330=DIRECTION('ref_axis',(1.,-7.35649788641118E-13,0.));
#27331=DIRECTION('',(0.,0.,1.));
#27332=DIRECTION('center_axis',(0.,0.,1.));
#27333=DIRECTION('ref_axis',(1.,-7.35649788641118E-13,0.));
#27334=DIRECTION('',(0.,0.,1.));
#27335=DIRECTION('center_axis',(0.,0.,1.));
#27336=DIRECTION('ref_axis',(1.,-7.35649788641118E-13,0.));
#27337=DIRECTION('',(0.,0.,1.));
#27338=DIRECTION('center_axis',(0.,0.,1.));
#27339=DIRECTION('ref_axis',(1.,-7.35649788641118E-13,0.));
#27340=DIRECTION('',(0.,0.,1.));
#27341=DIRECTION('center_axis',(0.,0.,1.));
#27342=DIRECTION('ref_axis',(1.,-7.35649788641118E-13,0.));
#27343=DIRECTION('',(0.,0.,1.));
#27344=DIRECTION('center_axis',(0.,0.,1.));
#27345=DIRECTION('ref_axis',(1.,-7.35649788641118E-13,0.));
#27346=DIRECTION('',(0.,0.,1.));
#27347=DIRECTION('center_axis',(0.,0.,1.));
#27348=DIRECTION('ref_axis',(1.,-7.35649788641118E-13,0.));
#27349=DIRECTION('',(0.,0.,1.));
#27350=DIRECTION('center_axis',(0.,0.,1.));
#27351=DIRECTION('ref_axis',(1.,-7.35649788641118E-13,0.));
#27352=DIRECTION('',(0.,0.,1.));
#27353=DIRECTION('center_axis',(0.,0.,1.));
#27354=DIRECTION('ref_axis',(1.,-7.35649788641118E-13,0.));
#27355=DIRECTION('',(0.,0.,1.));
#27356=DIRECTION('center_axis',(0.,0.,1.));
#27357=DIRECTION('ref_axis',(1.,-7.35649788641118E-13,0.));
#27358=DIRECTION('',(0.,0.,1.));
#27359=DIRECTION('center_axis',(0.,0.,1.));
#27360=DIRECTION('ref_axis',(1.,-7.35649788641118E-13,0.));
#27361=DIRECTION('',(0.,0.,1.));
#27362=DIRECTION('center_axis',(0.,0.,1.));
#27363=DIRECTION('ref_axis',(1.,-7.35649788641118E-13,0.));
#27364=DIRECTION('',(0.,0.,1.));
#27365=DIRECTION('center_axis',(0.,0.,1.));
#27366=DIRECTION('ref_axis',(1.,-7.35649788641118E-13,0.));
#27367=DIRECTION('',(0.,0.,1.));
#27368=DIRECTION('center_axis',(0.,0.,1.));
#27369=DIRECTION('ref_axis',(1.,-7.35649788641118E-13,0.));
#27370=DIRECTION('',(0.,0.,1.));
#27371=DIRECTION('center_axis',(0.,0.,1.));
#27372=DIRECTION('ref_axis',(1.,-7.35649788641118E-13,0.));
#27373=DIRECTION('',(0.,0.,1.));
#27374=DIRECTION('center_axis',(0.,0.,1.));
#27375=DIRECTION('ref_axis',(1.,-7.35649788641118E-13,0.));
#27376=DIRECTION('',(0.,0.,1.));
#27377=DIRECTION('center_axis',(0.,0.,1.));
#27378=DIRECTION('ref_axis',(1.,-7.35649788641118E-13,0.));
#27379=DIRECTION('',(0.,0.,1.));
#27380=DIRECTION('center_axis',(0.,0.,1.));
#27381=DIRECTION('ref_axis',(1.,-7.35649788641118E-13,0.));
#27382=DIRECTION('',(0.,0.,1.));
#27383=DIRECTION('center_axis',(0.,0.,1.));
#27384=DIRECTION('ref_axis',(1.,-7.35649788641118E-13,0.));
#27385=DIRECTION('',(0.,0.,1.));
#27386=DIRECTION('center_axis',(0.,0.,1.));
#27387=DIRECTION('ref_axis',(1.,-7.35649788641118E-13,0.));
#27388=DIRECTION('',(0.,0.,1.));
#27389=DIRECTION('center_axis',(0.,0.,1.));
#27390=DIRECTION('ref_axis',(1.,-7.35649788641118E-13,0.));
#27391=DIRECTION('',(0.,0.,1.));
#27392=DIRECTION('center_axis',(0.,0.,1.));
#27393=DIRECTION('ref_axis',(1.,-7.35649788641118E-13,0.));
#27394=DIRECTION('',(0.,0.,1.));
#27395=DIRECTION('center_axis',(0.,0.,1.));
#27396=DIRECTION('ref_axis',(1.,-7.35649788641118E-13,0.));
#27397=DIRECTION('',(0.,0.,1.));
#27398=DIRECTION('center_axis',(0.,0.,1.));
#27399=DIRECTION('ref_axis',(1.,-7.35649788641118E-13,0.));
#27400=DIRECTION('',(0.,0.,1.));
#27401=DIRECTION('center_axis',(0.,0.,1.));
#27402=DIRECTION('ref_axis',(1.,-7.35649788641118E-13,0.));
#27403=DIRECTION('',(0.,0.,1.));
#27404=DIRECTION('center_axis',(0.,0.,1.));
#27405=DIRECTION('ref_axis',(1.,-7.35649788641118E-13,0.));
#27406=DIRECTION('',(0.,0.,1.));
#27407=DIRECTION('center_axis',(0.,0.,1.));
#27408=DIRECTION('ref_axis',(1.,-7.35649788641118E-13,0.));
#27409=DIRECTION('',(0.,0.,1.));
#27410=DIRECTION('center_axis',(0.,0.,1.));
#27411=DIRECTION('ref_axis',(1.,-7.35649788641118E-13,0.));
#27412=DIRECTION('',(0.,0.,1.));
#27413=DIRECTION('center_axis',(0.,0.,1.));
#27414=DIRECTION('ref_axis',(1.,-7.35649788641118E-13,0.));
#27415=DIRECTION('',(0.,0.,1.));
#27416=DIRECTION('center_axis',(0.,0.,1.));
#27417=DIRECTION('ref_axis',(1.,-7.35649788641118E-13,0.));
#27418=DIRECTION('',(0.,0.,1.));
#27419=DIRECTION('center_axis',(0.,0.,1.));
#27420=DIRECTION('ref_axis',(1.,-7.35649788641118E-13,0.));
#27421=DIRECTION('',(0.,0.,1.));
#27422=DIRECTION('center_axis',(0.,0.,1.));
#27423=DIRECTION('ref_axis',(1.,-7.35649788641118E-13,0.));
#27424=DIRECTION('',(0.,0.,1.));
#27425=DIRECTION('center_axis',(0.,0.,1.));
#27426=DIRECTION('ref_axis',(1.,-7.35649788641118E-13,0.));
#27427=DIRECTION('',(0.,0.,1.));
#27428=DIRECTION('center_axis',(0.,0.,1.));
#27429=DIRECTION('ref_axis',(1.,-7.35649788641118E-13,0.));
#27430=DIRECTION('',(0.,0.,1.));
#27431=DIRECTION('center_axis',(0.,0.,1.));
#27432=DIRECTION('ref_axis',(1.,-7.35649788641118E-13,0.));
#27433=DIRECTION('',(0.,0.,1.));
#27434=DIRECTION('center_axis',(0.,0.,1.));
#27435=DIRECTION('ref_axis',(1.,-7.35649788641118E-13,0.));
#27436=DIRECTION('',(0.,0.,1.));
#27437=DIRECTION('center_axis',(0.,0.,1.));
#27438=DIRECTION('ref_axis',(1.,-7.35649788641118E-13,0.));
#27439=DIRECTION('',(0.,0.,1.));
#27440=DIRECTION('center_axis',(0.,0.,1.));
#27441=DIRECTION('ref_axis',(1.,-7.35649788641118E-13,0.));
#27442=DIRECTION('',(0.,0.,1.));
#27443=DIRECTION('center_axis',(0.,0.,1.));
#27444=DIRECTION('ref_axis',(1.,-7.35649788641118E-13,0.));
#27445=DIRECTION('',(0.,0.,1.));
#27446=DIRECTION('center_axis',(0.,0.,1.));
#27447=DIRECTION('ref_axis',(1.,-7.35649788641118E-13,0.));
#27448=DIRECTION('',(0.,0.,1.));
#27449=DIRECTION('center_axis',(0.,0.,1.));
#27450=DIRECTION('ref_axis',(1.,-7.35649788641118E-13,0.));
#27451=DIRECTION('',(0.,0.,1.));
#27452=DIRECTION('center_axis',(0.,0.,1.));
#27453=DIRECTION('ref_axis',(1.,-7.35649788641118E-13,0.));
#27454=DIRECTION('',(0.,0.,1.));
#27455=DIRECTION('center_axis',(0.,0.,1.));
#27456=DIRECTION('ref_axis',(1.,-7.35649788641118E-13,0.));
#27457=DIRECTION('',(0.,0.,1.));
#27458=DIRECTION('center_axis',(0.,0.,1.));
#27459=DIRECTION('ref_axis',(1.,-7.35649788641118E-13,0.));
#27460=DIRECTION('',(0.,0.,1.));
#27461=DIRECTION('center_axis',(0.,0.,1.));
#27462=DIRECTION('ref_axis',(1.,-7.35649788641118E-13,0.));
#27463=DIRECTION('',(0.,0.,1.));
#27464=DIRECTION('center_axis',(0.,0.,-1.));
#27465=DIRECTION('ref_axis',(1.,0.,0.));
#27466=DIRECTION('center_axis',(0.,0.,-1.));
#27467=DIRECTION('ref_axis',(1.,0.,0.));
#27468=DIRECTION('',(0.707106781186549,8.65956056235495E-17,0.707106781186546));
#27469=DIRECTION('center_axis',(0.,0.,1.));
#27470=DIRECTION('ref_axis',(1.,0.,0.));
#27471=DIRECTION('center_axis',(0.,0.,1.));
#27472=DIRECTION('ref_axis',(1.,-7.35649788641118E-13,0.));
#27473=DIRECTION('center_axis',(0.,0.,-1.));
#27474=DIRECTION('ref_axis',(1.,-7.35649788641118E-13,0.));
#27475=DIRECTION('center_axis',(0.,0.,1.));
#27476=DIRECTION('ref_axis',(1.,0.,0.));
#27477=DIRECTION('center_axis',(-1.92296268638356E-16,-1.,0.));
#27478=DIRECTION('ref_axis',(1.,-1.92296268638356E-16,0.));
#27479=DIRECTION('',(1.,-1.92296268638356E-16,0.));
#27480=DIRECTION('',(0.,0.,1.));
#27481=DIRECTION('',(1.,-1.92296268638356E-16,0.));
#27482=DIRECTION('',(0.,0.,1.));
#27483=DIRECTION('center_axis',(-0.866025403784439,-0.5,0.));
#27484=DIRECTION('ref_axis',(0.5,-0.866025403784439,0.));
#27485=DIRECTION('',(0.5,-0.866025403784439,0.));
#27486=DIRECTION('',(0.,0.,1.));
#27487=DIRECTION('',(0.5,-0.866025403784439,0.));
#27488=DIRECTION('center_axis',(-0.866025403784439,0.5,0.));
#27489=DIRECTION('ref_axis',(-0.5,-0.866025403784438,0.));
#27490=DIRECTION('',(-0.5,-0.866025403784438,0.));
#27491=DIRECTION('',(0.,0.,1.));
#27492=DIRECTION('',(-0.5,-0.866025403784439,0.));
#27493=DIRECTION('center_axis',(1.92296268638356E-16,1.,0.));
#27494=DIRECTION('ref_axis',(-1.,1.92296268638356E-16,0.));
#27495=DIRECTION('',(-1.,1.92296268638356E-16,0.));
#27496=DIRECTION('',(0.,0.,1.));
#27497=DIRECTION('',(-1.,1.92296268638356E-16,0.));
#27498=DIRECTION('center_axis',(0.866025403784439,0.5,0.));
#27499=DIRECTION('ref_axis',(-0.5,0.866025403784439,0.));
#27500=DIRECTION('',(-0.5,0.866025403784439,0.));
#27501=DIRECTION('',(0.,0.,1.));
#27502=DIRECTION('',(-0.5,0.866025403784439,0.));
#27503=DIRECTION('center_axis',(0.866025403784439,-0.5,0.));
#27504=DIRECTION('ref_axis',(0.5,0.866025403784439,0.));
#27505=DIRECTION('',(0.5,0.866025403784439,0.));
#27506=DIRECTION('',(0.5,0.866025403784439,0.));
#27507=DIRECTION('center_axis',(0.,0.,1.));
#27508=DIRECTION('ref_axis',(1.,0.,0.));
#27509=DIRECTION('center_axis',(0.,0.,1.));
#27510=DIRECTION('ref_axis',(1.,0.,0.));
#27511=DIRECTION('center_axis',(0.,0.,1.));
#27512=DIRECTION('ref_axis',(1.,0.,0.));
#27513=DIRECTION('center_axis',(0.,0.,1.));
#27514=DIRECTION('ref_axis',(1.,0.,0.));
#27515=DIRECTION('',(0.,0.,-1.));
#27516=DIRECTION('center_axis',(0.,0.,1.));
#27517=DIRECTION('ref_axis',(1.,0.,0.));
#27518=DIRECTION('center_axis',(0.,0.,1.));
#27519=DIRECTION('ref_axis',(1.,0.,0.));
#27520=DIRECTION('center_axis',(0.,0.,1.));
#27521=DIRECTION('ref_axis',(1.,0.,0.));
#27522=DIRECTION('axis',(0.,0.,1.));
#27523=DIRECTION('refdir',(1.,0.,0.));
#27524=DIRECTION('center_axis',(0.,0.,1.));
#27525=DIRECTION('ref_axis',(1.,0.,0.));
#27526=DIRECTION('center_axis',(0.,0.,-1.));
#27527=DIRECTION('ref_axis',(1.,0.,0.));
#27528=DIRECTION('',(0.,0.,-1.));
#27529=DIRECTION('center_axis',(0.,0.,-1.));
#27530=DIRECTION('ref_axis',(1.,0.,0.));
#27531=DIRECTION('center_axis',(0.,0.,1.));
#27532=DIRECTION('ref_axis',(1.,0.,0.));
#27533=DIRECTION('center_axis',(0.,0.,1.));
#27534=DIRECTION('ref_axis',(1.,0.,0.));
#27535=DIRECTION('',(0.,0.,-1.));
#27536=DIRECTION('center_axis',(0.,0.,1.));
#27537=DIRECTION('ref_axis',(1.,0.,0.));
#27538=DIRECTION('center_axis',(0.,0.,1.));
#27539=DIRECTION('ref_axis',(1.,0.,0.));
#27540=DIRECTION('center_axis',(0.,0.,1.));
#27541=DIRECTION('ref_axis',(1.,0.,0.));
#27542=DIRECTION('axis',(0.,0.,1.));
#27543=DIRECTION('refdir',(1.,0.,0.));
#27544=DIRECTION('center_axis',(0.,0.,1.));
#27545=DIRECTION('ref_axis',(1.,0.,0.));
#27546=DIRECTION('center_axis',(0.,0.,-1.));
#27547=DIRECTION('ref_axis',(1.,0.,0.));
#27548=DIRECTION('',(0.,0.,-1.));
#27549=DIRECTION('center_axis',(0.,0.,-1.));
#27550=DIRECTION('ref_axis',(1.,0.,0.));
#27551=DIRECTION('center_axis',(0.,0.,1.));
#27552=DIRECTION('ref_axis',(1.,0.,0.));
#27553=DIRECTION('center_axis',(0.,0.,1.));
#27554=DIRECTION('ref_axis',(1.,0.,0.));
#27555=DIRECTION('',(0.,0.,-1.));
#27556=DIRECTION('center_axis',(0.,0.,1.));
#27557=DIRECTION('ref_axis',(1.,0.,0.));
#27558=DIRECTION('center_axis',(0.,0.,1.));
#27559=DIRECTION('ref_axis',(1.,0.,0.));
#27560=DIRECTION('center_axis',(0.,0.,1.));
#27561=DIRECTION('ref_axis',(1.,0.,0.));
#27562=DIRECTION('',(0.,0.,1.));
#27563=DIRECTION('',(1.,0.,0.));
#27564=DIRECTION('',(0.,0.,1.));
#27565=DIRECTION('',(1.,0.,0.));
#27566=DIRECTION('',(0.,-1.22464679914735E-16,-1.));
#27567=DIRECTION('',(1.,0.,0.));
#27568=DIRECTION('',(0.,0.,1.));
#27569=DIRECTION('',(1.,0.,0.));
#27570=DIRECTION('',(0.,0.,1.));
#27571=DIRECTION('',(1.,0.,0.));
#27572=DIRECTION('',(0.,0.,1.));
#27573=DIRECTION('',(1.,0.,0.));
#27574=DIRECTION('',(0.,0.,1.));
#27575=DIRECTION('',(-1.,1.22464679914735E-16,0.));
#27576=DIRECTION('',(0.,0.,1.));
#27577=DIRECTION('',(1.,0.,0.));
#27578=DIRECTION('',(0.,0.,1.));
#27579=DIRECTION('',(1.,0.,0.));
#27580=DIRECTION('',(0.,-1.22464679914735E-16,-1.));
#27581=DIRECTION('',(1.,0.,0.));
#27582=DIRECTION('',(0.,0.,1.));
#27583=DIRECTION('',(1.,0.,0.));
#27584=DIRECTION('',(0.,-1.22464679914735E-16,-1.));
#27585=DIRECTION('',(1.,0.,0.));
#27586=DIRECTION('',(0.,0.,1.));
#27587=DIRECTION('',(1.,0.,0.));
#27588=DIRECTION('',(0.,-1.22464679914735E-16,-1.));
#27589=DIRECTION('',(1.,0.,0.));
#27590=DIRECTION('',(0.,0.,1.));
#27591=DIRECTION('',(1.,0.,0.));
#27592=DIRECTION('',(0.,0.,1.));
#27593=DIRECTION('',(1.,0.,0.));
#27594=DIRECTION('',(0.,0.,1.));
#27595=DIRECTION('',(1.,0.,0.));
#27596=DIRECTION('',(0.,0.,1.));
#27597=DIRECTION('',(1.,0.,0.));
#27598=DIRECTION('',(0.,0.,1.));
#27599=DIRECTION('',(1.,0.,0.));
#27600=DIRECTION('',(0.,0.,1.));
#27601=DIRECTION('',(1.,0.,0.));
#27602=DIRECTION('',(0.,0.,1.));
#27603=DIRECTION('',(1.,0.,0.));
#27604=DIRECTION('',(0.,0.,1.));
#27605=DIRECTION('',(-1.,1.22464679914735E-16,0.));
#27606=DIRECTION('',(0.,0.,1.));
#27607=DIRECTION('',(1.,0.,0.));
#27608=DIRECTION('',(0.,0.,1.));
#27609=DIRECTION('',(1.,0.,0.));
#27610=DIRECTION('',(0.,0.,1.));
#27611=DIRECTION('',(-1.,1.22464679914735E-16,0.));
#27612=DIRECTION('',(0.,0.,1.));
#27613=DIRECTION('',(1.,0.,0.));
#27614=DIRECTION('',(0.,0.,1.));
#27615=DIRECTION('',(1.,0.,0.));
#27616=DIRECTION('',(0.,0.,1.));
#27617=DIRECTION('',(-1.,1.22464679914735E-16,0.));
#27618=DIRECTION('',(0.,0.,1.));
#27619=DIRECTION('',(1.,0.,0.));
#27620=DIRECTION('',(0.,0.,1.));
#27621=DIRECTION('',(1.,0.,0.));
#27622=DIRECTION('',(0.,0.,1.));
#27623=DIRECTION('',(-1.,1.22464679914735E-16,0.));
#27624=DIRECTION('',(0.,0.,1.));
#27625=DIRECTION('',(1.,0.,0.));
#27626=DIRECTION('',(0.,0.,1.));
#27627=DIRECTION('',(1.,0.,0.));
#27628=DIRECTION('',(0.,0.,1.));
#27629=DIRECTION('',(-1.,1.22464679914735E-16,0.));
#27630=DIRECTION('',(0.,0.,1.));
#27631=DIRECTION('',(1.,0.,0.));
#27632=DIRECTION('',(0.,0.,1.));
#27633=DIRECTION('',(1.,0.,0.));
#27634=DIRECTION('',(0.,0.,1.));
#27635=DIRECTION('',(-1.,1.22464679914735E-16,0.));
#27636=DIRECTION('',(0.,0.,1.));
#27637=DIRECTION('',(1.,0.,0.));
#27638=DIRECTION('',(0.,0.,1.));
#27639=DIRECTION('',(1.,0.,0.));
#27640=CARTESIAN_POINT('',(0.,0.,0.));
#27641=CARTESIAN_POINT('',(0.,0.,0.));
#27642=CARTESIAN_POINT('',(0.,0.,0.));
#27643=CARTESIAN_POINT('Origin',(0.,0.,300.));
#27644=CARTESIAN_POINT('',(-16.,-3.5,300.));
#27645=CARTESIAN_POINT('Origin',(-16.,0.,300.));
#27646=CARTESIAN_POINT('',(-20.,-3.5,300.));
#27647=CARTESIAN_POINT('',(0.,-3.5,300.));
#27648=CARTESIAN_POINT('Origin',(-20.,0.,300.));
#27649=CARTESIAN_POINT('Origin',(0.,0.,300.));
#27650=CARTESIAN_POINT('',(20.,-3.5,300.));
#27651=CARTESIAN_POINT('Origin',(20.,0.,300.));
#27652=CARTESIAN_POINT('',(16.,-3.5,300.));
#27653=CARTESIAN_POINT('',(0.,-3.5,300.));
#27654=CARTESIAN_POINT('Origin',(16.,0.,300.));
#27655=CARTESIAN_POINT('Origin',(0.,0.,140.));
#27656=CARTESIAN_POINT('',(-16.,-3.5,140.));
#27657=CARTESIAN_POINT('Origin',(-16.,0.,140.));
#27658=CARTESIAN_POINT('',(-20.,-3.5,140.));
#27659=CARTESIAN_POINT('',(0.,-3.5,140.));
#27660=CARTESIAN_POINT('Origin',(-20.,0.,140.));
#27661=CARTESIAN_POINT('Origin',(0.,0.,140.));
#27662=CARTESIAN_POINT('',(20.,-3.5,140.));
#27663=CARTESIAN_POINT('Origin',(20.,0.,140.));
#27664=CARTESIAN_POINT('',(16.,-3.5,140.));
#27665=CARTESIAN_POINT('',(0.,-3.5,140.));
#27666=CARTESIAN_POINT('Origin',(16.,0.,140.));
#27667=CARTESIAN_POINT('Origin',(0.,0.,460.));
#27668=CARTESIAN_POINT('',(-16.,-3.5,460.));
#27669=CARTESIAN_POINT('Origin',(-16.,0.,460.));
#27670=CARTESIAN_POINT('',(-20.,-3.5,460.));
#27671=CARTESIAN_POINT('',(0.,-3.5,460.));
#27672=CARTESIAN_POINT('Origin',(-20.,0.,460.));
#27673=CARTESIAN_POINT('Origin',(0.,0.,460.));
#27674=CARTESIAN_POINT('',(20.,-3.5,460.));
#27675=CARTESIAN_POINT('Origin',(20.,0.,460.));
#27676=CARTESIAN_POINT('',(16.,-3.5,460.));
#27677=CARTESIAN_POINT('',(0.,-3.5,460.));
#27678=CARTESIAN_POINT('Origin',(16.,0.,460.));
#27679=CARTESIAN_POINT('Origin',(16.,-21.,0.));
#27680=CARTESIAN_POINT('',(16.,-21.,0.));
#27681=CARTESIAN_POINT('',(-16.,-21.,0.));
#27682=CARTESIAN_POINT('',(-16.,-21.,0.));
#27683=CARTESIAN_POINT('',(-16.,-21.,600.));
#27684=CARTESIAN_POINT('',(-16.,-21.,0.));
#27685=CARTESIAN_POINT('',(16.,-21.,600.));
#27686=CARTESIAN_POINT('',(-16.,-21.,600.));
#27687=CARTESIAN_POINT('',(16.,-21.,0.));
#27688=CARTESIAN_POINT('Origin',(16.,21.,0.));
#27689=CARTESIAN_POINT('',(16.,21.,0.));
#27690=CARTESIAN_POINT('',(16.,-21.,0.));
#27691=CARTESIAN_POINT('',(16.,21.,600.));
#27692=CARTESIAN_POINT('',(16.,-21.,600.));
#27693=CARTESIAN_POINT('',(16.,21.,0.));
#27694=CARTESIAN_POINT('Origin',(-16.,21.,0.));
#27695=CARTESIAN_POINT('',(-16.,21.,0.));
#27696=CARTESIAN_POINT('',(16.,21.,0.));
#27697=CARTESIAN_POINT('',(-16.,21.,600.));
#27698=CARTESIAN_POINT('',(16.,21.,600.));
#27699=CARTESIAN_POINT('',(-16.,21.,0.));
#27700=CARTESIAN_POINT('Origin',(-16.,-21.,0.));
#27701=CARTESIAN_POINT('',(-16.,21.,0.));
#27702=CARTESIAN_POINT('',(-16.,21.,600.));
#27703=CARTESIAN_POINT('Origin',(20.,25.,0.));
#27704=CARTESIAN_POINT('',(20.,25.,0.));
#27705=CARTESIAN_POINT('',(-20.,25.,0.));
#27706=CARTESIAN_POINT('',(20.,25.,0.));
#27707=CARTESIAN_POINT('',(-20.,25.,600.));
#27708=CARTESIAN_POINT('',(-20.,25.,0.));
#27709=CARTESIAN_POINT('',(20.,25.,600.));
#27710=CARTESIAN_POINT('',(20.,25.,600.));
#27711=CARTESIAN_POINT('',(20.,25.,0.));
#27712=CARTESIAN_POINT('Origin',(20.,-25.,0.));
#27713=CARTESIAN_POINT('',(20.,-25.,0.));
#27714=CARTESIAN_POINT('',(20.,-25.,0.));
#27715=CARTESIAN_POINT('',(20.,-25.,600.));
#27716=CARTESIAN_POINT('',(20.,-25.,600.));
#27717=CARTESIAN_POINT('',(20.,-25.,0.));
#27718=CARTESIAN_POINT('Origin',(-20.,-25.,0.));
#27719=CARTESIAN_POINT('',(-20.,-25.,0.));
#27720=CARTESIAN_POINT('',(-20.,-25.,0.));
#27721=CARTESIAN_POINT('',(-20.,-25.,600.));
#27722=CARTESIAN_POINT('',(-20.,-25.,600.));
#27723=CARTESIAN_POINT('',(-20.,-25.,0.));
#27724=CARTESIAN_POINT('Origin',(-20.,25.,0.));
#27725=CARTESIAN_POINT('',(-20.,25.,0.));
#27726=CARTESIAN_POINT('',(-20.,25.,600.));
#27727=CARTESIAN_POINT('Origin',(0.,0.,600.));
#27728=CARTESIAN_POINT('Origin',(0.,0.,0.));
#27729=CARTESIAN_POINT('',(0.,0.,0.));
#27730=CARTESIAN_POINT('Origin',(16.,-21.,0.));
#27731=CARTESIAN_POINT('',(16.,-21.,0.));
#27732=CARTESIAN_POINT('',(-16.,-21.,0.));
#27733=CARTESIAN_POINT('',(-16.,-21.,0.));
#27734=CARTESIAN_POINT('',(-16.,-21.,400.));
#27735=CARTESIAN_POINT('',(-16.,-21.,0.));
#27736=CARTESIAN_POINT('',(16.,-21.,400.));
#27737=CARTESIAN_POINT('',(-16.,-21.,400.));
#27738=CARTESIAN_POINT('',(16.,-21.,0.));
#27739=CARTESIAN_POINT('Origin',(16.,21.,0.));
#27740=CARTESIAN_POINT('',(16.,21.,0.));
#27741=CARTESIAN_POINT('',(16.,-21.,0.));
#27742=CARTESIAN_POINT('',(16.,21.,400.));
#27743=CARTESIAN_POINT('',(16.,-21.,400.));
#27744=CARTESIAN_POINT('',(16.,21.,0.));
#27745=CARTESIAN_POINT('Origin',(-16.,21.,0.));
#27746=CARTESIAN_POINT('',(-16.,21.,0.));
#27747=CARTESIAN_POINT('',(16.,21.,0.));
#27748=CARTESIAN_POINT('',(-16.,21.,400.));
#27749=CARTESIAN_POINT('',(16.,21.,400.));
#27750=CARTESIAN_POINT('',(-16.,21.,0.));
#27751=CARTESIAN_POINT('Origin',(-16.,-21.,0.));
#27752=CARTESIAN_POINT('',(-16.,21.,0.));
#27753=CARTESIAN_POINT('',(-16.,21.,400.));
#27754=CARTESIAN_POINT('Origin',(20.,25.,0.));
#27755=CARTESIAN_POINT('',(20.,25.,0.));
#27756=CARTESIAN_POINT('',(-20.,25.,0.));
#27757=CARTESIAN_POINT('',(20.,25.,0.));
#27758=CARTESIAN_POINT('',(-20.,25.,400.));
#27759=CARTESIAN_POINT('',(-20.,25.,0.));
#27760=CARTESIAN_POINT('',(20.,25.,400.));
#27761=CARTESIAN_POINT('',(20.,25.,400.));
#27762=CARTESIAN_POINT('',(20.,25.,0.));
#27763=CARTESIAN_POINT('Origin',(20.,-25.,0.));
#27764=CARTESIAN_POINT('',(20.,-25.,0.));
#27765=CARTESIAN_POINT('',(20.,-25.,0.));
#27766=CARTESIAN_POINT('',(20.,-25.,400.));
#27767=CARTESIAN_POINT('',(20.,-25.,400.));
#27768=CARTESIAN_POINT('',(20.,-25.,0.));
#27769=CARTESIAN_POINT('Origin',(-20.,-25.,0.));
#27770=CARTESIAN_POINT('',(-20.,-25.,0.));
#27771=CARTESIAN_POINT('',(-20.,-25.,0.));
#27772=CARTESIAN_POINT('',(-20.,-25.,400.));
#27773=CARTESIAN_POINT('',(-20.,-25.,400.));
#27774=CARTESIAN_POINT('',(-20.,-25.,0.));
#27775=CARTESIAN_POINT('Origin',(-20.,25.,0.));
#27776=CARTESIAN_POINT('',(-20.,25.,0.));
#27777=CARTESIAN_POINT('',(-20.,25.,400.));
#27778=CARTESIAN_POINT('Origin',(0.,0.,400.));
#27779=CARTESIAN_POINT('Origin',(0.,0.,0.));
#27780=CARTESIAN_POINT('',(0.,0.,0.));
#27781=CARTESIAN_POINT('Origin',(35.,35.,4.));
#27782=CARTESIAN_POINT('',(31.4879724201494,34.9998624352662,0.387416697508018));
#27783=CARTESIAN_POINT('',(31.4848003100606,34.9953496614248,0.112583302491981));
#27784=CARTESIAN_POINT('',(31.4825,35.,4.));
#27785=CARTESIAN_POINT('',(32.3264680662286,37.2858331630075,0.));
#27786=CARTESIAN_POINT('Ctrl Pts',(31.4848003100606,34.9953496614248,0.112583302491981));
#27787=CARTESIAN_POINT('Ctrl Pts',(31.491976688325,35.8232723665277,0.0750555349946529));
#27788=CARTESIAN_POINT('Ctrl Pts',(31.7874825103136,36.6554305951821,0.0375277674973252));
#27789=CARTESIAN_POINT('Ctrl Pts',(32.3264680662287,37.2858331630075,-2.22044604925031E-15));
#27790=CARTESIAN_POINT('',(37.6785012740241,37.2890246412443,7.00840805882243E-15));
#27791=CARTESIAN_POINT('Origin',(35.,35.,0.));
#27792=CARTESIAN_POINT('Ctrl Pts',(37.6785244495407,37.2890395253442,4.78783679369599E-15));
#27793=CARTESIAN_POINT('Ctrl Pts',(36.9607517209778,38.1233243316157,0.0499978774624456));
#27794=CARTESIAN_POINT('Ctrl Pts',(35.818670130213,38.598920544762,0.0999957549248864));
#27795=CARTESIAN_POINT('Ctrl Pts',(34.7217021974699,38.5118549254553,0.149993632387327));
#27796=CARTESIAN_POINT('Ctrl Pts',(33.5734927541699,38.4207223013458,0.202327008171411));
#27797=CARTESIAN_POINT('Ctrl Pts',(32.4747101009944,37.7131340510847,0.254660383955495));
#27798=CARTESIAN_POINT('Ctrl Pts',(31.9173289273845,36.7055535968161,0.306993759739579));
#27799=CARTESIAN_POINT('Ctrl Pts',(31.6318117612872,36.1894229315936,0.333801405662392));
#27800=CARTESIAN_POINT('Ctrl Pts',(31.4883570437126,35.5945750322157,0.360609051585205));
#27801=CARTESIAN_POINT('Ctrl Pts',(31.4879724201494,34.9998624352662,0.387416697508018));
#27802=CARTESIAN_POINT('Origin',(35.,35.,4.));
#27803=CARTESIAN_POINT('',(31.4787691259179,34.9978480355345,1.38741669750802));
#27804=CARTESIAN_POINT('',(31.4779837004207,35.0016823853973,1.11258330249198));
#27805=CARTESIAN_POINT('',(31.4825,35.,4.));
#27806=CARTESIAN_POINT('Ctrl Pts',(31.4779837004207,35.0016823853973,1.11258330249198));
#27807=CARTESIAN_POINT('Ctrl Pts',(31.4773936874682,35.1013890235937,1.10805583214991));
#27808=CARTESIAN_POINT('Ctrl Pts',(31.4812693590031,35.201048825548,1.10352836180784));
#27809=CARTESIAN_POINT('Ctrl Pts',(31.4897612702936,35.3003133216161,1.09900089146578));
#27810=CARTESIAN_POINT('Ctrl Pts',(31.5879199220602,36.4477192198909,1.04666751568169));
#27811=CARTESIAN_POINT('Ctrl Pts',(32.3028647460417,37.5423074099748,0.994334139897606));
#27812=CARTESIAN_POINT('Ctrl Pts',(33.3140597553874,38.0934397445863,0.942000764113521));
#27813=CARTESIAN_POINT('Ctrl Pts',(34.3252547647332,38.6445720791978,0.889667388329437));
#27814=CARTESIAN_POINT('Ctrl Pts',(35.632699959443,38.652248558337,0.837334012545353));
#27815=CARTESIAN_POINT('Ctrl Pts',(36.6501699298679,38.1127741860318,0.785000636761269));
#27816=CARTESIAN_POINT('Ctrl Pts',(37.6676399002927,37.5732998137267,0.732667260977184));
#27817=CARTESIAN_POINT('Ctrl Pts',(38.3951346464326,36.4866745899774,0.680333885193099));
#27818=CARTESIAN_POINT('Ctrl Pts',(38.5065308772508,35.3406022936711,0.628000509409014));
#27819=CARTESIAN_POINT('Ctrl Pts',(38.617927108069,34.1945299973649,0.57566713362493));
#27820=CARTESIAN_POINT('Ctrl Pts',(38.1132248235656,32.9890106285018,0.523333757840846));
#27821=CARTESIAN_POINT('Ctrl Pts',(37.2186051779362,32.2635143561234,0.471000382056762));
#27822=CARTESIAN_POINT('Ctrl Pts',(36.3239855323068,31.538018083745,0.418667006272677));
#27823=CARTESIAN_POINT('Ctrl Pts',(35.0394485255514,31.2925449078513,0.366333630488592));
#27824=CARTESIAN_POINT('Ctrl Pts',(33.9411234140671,31.6392615363868,0.314000254704508));
#27825=CARTESIAN_POINT('Ctrl Pts',(32.8427983025828,31.9859781649222,0.261666878920424));
#27826=CARTESIAN_POINT('Ctrl Pts',(31.9306850863697,32.9248845978868,0.20933350313634));
#27827=CARTESIAN_POINT('Ctrl Pts',(31.6136954419349,34.0300704557469,0.157000127352256));
#27828=CARTESIAN_POINT('Ctrl Pts',(31.5240160655112,34.3427380154138,0.142194519065497));
#27829=CARTESIAN_POINT('Ctrl Pts',(31.481969055963,34.6687142103727,0.127388910778739));
#27830=CARTESIAN_POINT('Ctrl Pts',(31.4848003100606,34.9953496614248,0.112583302491981));
#27831=CARTESIAN_POINT('Ctrl Pts',(31.4879724201494,34.9998624352662,0.387416697508018));
#27832=CARTESIAN_POINT('Ctrl Pts',(31.4876061889182,34.4335884275247,0.41294242736929));
#27833=CARTESIAN_POINT('Ctrl Pts',(31.6169542536305,33.8674370915364,0.438468157230561));
#27834=CARTESIAN_POINT('Ctrl Pts',(31.8768865080858,33.3694813094911,0.463993887091832));
#27835=CARTESIAN_POINT('Ctrl Pts',(32.4098049564414,32.3485621347107,0.516327262875917));
#27836=CARTESIAN_POINT('Ctrl Pts',(33.4916215471969,31.6142964434261,0.568660638660002));
#27837=CARTESIAN_POINT('Ctrl Pts',(34.6371338346999,31.4957027110504,0.620994014444087));
#27838=CARTESIAN_POINT('Ctrl Pts',(35.7826461222029,31.3771089786747,0.673327390228171));
#27839=CARTESIAN_POINT('Ctrl Pts',(36.9918541064533,31.8741872052079,0.725660766012256));
#27840=CARTESIAN_POINT('Ctrl Pts',(37.7226853676378,32.7641657941898,0.77799414179634));
#27841=CARTESIAN_POINT('Ctrl Pts',(38.4535166288223,33.6541443831717,0.830327517580425));
#27842=CARTESIAN_POINT('Ctrl Pts',(38.7059711669407,34.9370233346023,0.882660893364508));
#27843=CARTESIAN_POINT('Ctrl Pts',(38.3668191926393,36.0375701678912,0.934994269148593));
#27844=CARTESIAN_POINT('Ctrl Pts',(38.0276672183379,37.13811700118,0.987327644932677));
#27845=CARTESIAN_POINT('Ctrl Pts',(37.0969087316166,38.0563317163271,1.03966102071676));
#27846=CARTESIAN_POINT('Ctrl Pts',(35.9918739069821,38.3805519391724,1.09199439650085));
#27847=CARTESIAN_POINT('Ctrl Pts',(34.8868390823475,38.7047721620176,1.14432777228493));
#27848=CARTESIAN_POINT('Ctrl Pts',(33.6075279197997,38.4349978925611,1.19666114806902));
#27849=CARTESIAN_POINT('Ctrl Pts',(32.727515719297,37.6921720072953,1.2489945238531));
#27850=CARTESIAN_POINT('Ctrl Pts',(31.9516360834601,37.0372453176186,1.29513524840474));
#27851=CARTESIAN_POINT('Ctrl Pts',(31.4861477200874,36.0145964274628,1.34127597295638));
#27852=CARTESIAN_POINT('Ctrl Pts',(31.4787691259179,34.9978480355345,1.38741669750802));
#27853=CARTESIAN_POINT('Origin',(35.,35.,4.));
#27854=CARTESIAN_POINT('',(31.4830373600778,35.0030273041289,2.38741669750802));
#27855=CARTESIAN_POINT('',(31.4877387493273,35.0007919718047,2.11258330249198));
#27856=CARTESIAN_POINT('',(31.4825,35.,4.));
#27857=CARTESIAN_POINT('Ctrl Pts',(31.4877387493273,35.0007919718047,2.11258330249198));
#27858=CARTESIAN_POINT('Ctrl Pts',(31.4866495532798,35.5300199293211,2.08872275352109));
#27859=CARTESIAN_POINT('Ctrl Pts',(31.5990326814287,36.0588086783673,2.06486220455019));
#27860=CARTESIAN_POINT('Ctrl Pts',(31.8273024854561,36.5316518026084,2.0410016555793));
#27861=CARTESIAN_POINT('Ctrl Pts',(32.3279669692824,37.5687392953569,1.98866827979521));
#27862=CARTESIAN_POINT('Ctrl Pts',(33.3861125458452,38.3366963827873,1.93633490401113));
#27863=CARTESIAN_POINT('Ctrl Pts',(34.5273147643209,38.4912077048459,1.88400152822704));
#27864=CARTESIAN_POINT('Ctrl Pts',(35.6685169827965,38.6457190269045,1.83166815244296));
#27865=CARTESIAN_POINT('Ctrl Pts',(36.8927758431849,38.1867845835912,1.77933477665887));
#27866=CARTESIAN_POINT('Ctrl Pts',(37.6511886219643,37.3201660399649,1.72700140087479));
#27867=CARTESIAN_POINT('Ctrl Pts',(38.4096014007438,36.4535474963386,1.6746680250907));
#27868=CARTESIAN_POINT('Ctrl Pts',(38.7021680979142,35.1792448523993,1.62233464930662));
#27869=CARTESIAN_POINT('Ctrl Pts',(38.3977158188189,34.0686054522412,1.57000127352253));
#27870=CARTESIAN_POINT('Ctrl Pts',(38.0932635397237,32.9579660520831,1.51766789773845));
#27871=CARTESIAN_POINT('Ctrl Pts',(37.1917922843629,32.0109898957062,1.46533452195437));
#27872=CARTESIAN_POINT('Ctrl Pts',(36.0974794284194,31.6522428960312,1.41300114617028));
#27873=CARTESIAN_POINT('Ctrl Pts',(35.0031665724759,31.2934958963563,1.3606677703862));
#27874=CARTESIAN_POINT('Ctrl Pts',(33.7160121159498,31.5229780533832,1.30833439460211));
#27875=CARTESIAN_POINT('Ctrl Pts',(32.8131211274626,32.2378309351295,1.25600101881803));
#27876=CARTESIAN_POINT('Ctrl Pts',(31.9883411362357,32.8908403914793,1.20819511337601));
#27877=CARTESIAN_POINT('Ctrl Pts',(31.4842136922894,33.9488723706596,1.160389207934));
#27878=CARTESIAN_POINT('Ctrl Pts',(31.4779837004207,35.0016823853973,1.11258330249198));
#27879=CARTESIAN_POINT('Ctrl Pts',(31.4787691259179,34.9978480355345,1.38741669750802));
#27880=CARTESIAN_POINT('Ctrl Pts',(31.4777788280689,34.86138792912,1.39360934874046));
#27881=CARTESIAN_POINT('Ctrl Pts',(31.4850404305936,34.725034107982,1.39980199997291));
#27882=CARTESIAN_POINT('Ctrl Pts',(31.5009110513053,34.5896898261078,1.40599465120535));
#27883=CARTESIAN_POINT('Ctrl Pts',(31.6350318222736,33.445911031261,1.45832802698944));
#27884=CARTESIAN_POINT('Ctrl Pts',(32.3839866026675,32.3742309426426,1.51066140277352));
#27885=CARTESIAN_POINT('Ctrl Pts',(33.411975462032,31.855139584126,1.56299477855761));
#27886=CARTESIAN_POINT('Ctrl Pts',(34.4399643213965,31.3360482256093,1.61532815434169));
#27887=CARTESIAN_POINT('Ctrl Pts',(35.7469872597314,31.3695455971944,1.66766153012578));
#27888=CARTESIAN_POINT('Ctrl Pts',(36.7470354950296,31.9406144231743,1.71999490590986));
#27889=CARTESIAN_POINT('Ctrl Pts',(37.7470837303277,32.5116832491543,1.77232828169395));
#27890=CARTESIAN_POINT('Ctrl Pts',(38.4401572625891,33.620323529529,1.82466165747803));
#27891=CARTESIAN_POINT('Ctrl Pts',(38.5155126426898,34.7694703662421,1.87699503326212));
#27892=CARTESIAN_POINT('Ctrl Pts',(38.5908680227905,35.9186172029552,1.9293284090462));
#27893=CARTESIAN_POINT('Ctrl Pts',(38.0485052507305,37.1082705960066,1.98166178483028));
#27894=CARTESIAN_POINT('Ctrl Pts',(37.1315955779125,37.8050440926957,2.03399516061437));
#27895=CARTESIAN_POINT('Ctrl Pts',(36.2146859050945,38.5018175893848,2.08632853639845));
#27896=CARTESIAN_POINT('Ctrl Pts',(34.9232293315183,38.7057111897115,2.13866191218254));
#27897=CARTESIAN_POINT('Ctrl Pts',(33.836256457425,38.3253080449544,2.19099528796662));
#27898=CARTESIAN_POINT('Ctrl Pts',(32.7492835833317,37.9449049001973,2.24332866375071));
#27899=CARTESIAN_POINT('Ctrl Pts',(31.8667944087212,36.9802050103563,2.29566203953479));
#27900=CARTESIAN_POINT('Ctrl Pts',(31.5844572622636,35.8637362853384,2.34799541531888));
#27901=CARTESIAN_POINT('Ctrl Pts',(31.5135650119789,35.583401298313,2.36113584271526));
#27902=CARTESIAN_POINT('Ctrl Pts',(31.4805102901148,35.2934978064005,2.37427627011164));
#27903=CARTESIAN_POINT('Ctrl Pts',(31.4830373600778,35.0030273041289,2.38741669750802));
#27904=CARTESIAN_POINT('Origin',(35.,35.,4.));
#27905=CARTESIAN_POINT('',(31.4866348863052,34.9979909502101,3.38741669750802));
#27906=CARTESIAN_POINT('',(31.48047694743,34.9972296622465,3.11258330249198));
#27907=CARTESIAN_POINT('',(31.4825,35.,4.));
#27908=CARTESIAN_POINT('Ctrl Pts',(31.48047694743,34.9972296622465,3.11258330249198));
#27909=CARTESIAN_POINT('Ctrl Pts',(31.4887007318231,35.9502403897084,3.06938967489226));
#27910=CARTESIAN_POINT('Ctrl Pts',(31.8903810058125,36.9093635615769,3.02619604729254));
#27911=CARTESIAN_POINT('Ctrl Pts',(32.5815433671812,37.5618418521763,2.98300241969282));
#27912=CARTESIAN_POINT('Ctrl Pts',(33.4189553095288,38.352384195351,2.93066904390873));
#27913=CARTESIAN_POINT('Ctrl Pts',(34.6813192114488,38.6927800566904,2.87833566812465));
#27914=CARTESIAN_POINT('Ctrl Pts',(35.8026481651385,38.4304113471867,2.82600229234057));
#27915=CARTESIAN_POINT('Ctrl Pts',(36.9239771188282,38.1680426376829,2.77366891655648));
#27916=CARTESIAN_POINT('Ctrl Pts',(37.9042711242876,37.3029093573359,2.7213355407724));
#27917=CARTESIAN_POINT('Ctrl Pts',(38.3040106560533,36.2228981053939,2.66900216498831));
#27918=CARTESIAN_POINT('Ctrl Pts',(38.703750187819,35.1428868534519,2.61666878920423));
#27919=CARTESIAN_POINT('Ctrl Pts',(38.5229352458909,33.8479976299149,2.56433541342014));
#27920=CARTESIAN_POINT('Ctrl Pts',(37.8426350886114,32.9188003439573,2.51200203763606));
#27921=CARTESIAN_POINT('Ctrl Pts',(37.1623349313319,31.9896030579996,2.45966866185197));
#27922=CARTESIAN_POINT('Ctrl Pts',(35.9825495587008,31.4260977096214,2.40733528606789));
#27923=CARTESIAN_POINT('Ctrl Pts',(34.8322413779487,31.4809343941795,2.3550019102838));
#27924=CARTESIAN_POINT('Ctrl Pts',(33.6819331971966,31.5357710787376,2.30266853449972));
#27925=CARTESIAN_POINT('Ctrl Pts',(32.5611022083236,32.208949796232,2.25033515871564));
#27926=CARTESIAN_POINT('Ctrl Pts',(31.9722784094319,33.1986481040126,2.19800178293155));
#27927=CARTESIAN_POINT('Ctrl Pts',(31.6519192161228,33.7371096133752,2.16952895611836));
#27928=CARTESIAN_POINT('Ctrl Pts',(31.4890384885104,34.3692635020513,2.14105612930517));
#27929=CARTESIAN_POINT('Ctrl Pts',(31.4877387493273,35.0007919718047,2.11258330249198));
#27930=CARTESIAN_POINT('Ctrl Pts',(31.4830373600778,35.0030273041289,2.38741669750802));
#27931=CARTESIAN_POINT('Ctrl Pts',(31.4905746584961,34.1366631395343,2.42660964589572));
#27932=CARTESIAN_POINT('Ctrl Pts',(31.8146491184789,33.2652548262212,2.46580259428343));
#27933=CARTESIAN_POINT('Ctrl Pts',(32.3954080438652,32.6276439552295,2.50499554267113));
#27934=CARTESIAN_POINT('Ctrl Pts',(33.1708810902294,31.7762579103332,2.55732891845521));
#27935=CARTESIAN_POINT('Ctrl Pts',(34.4040123012624,31.3417233807355,2.6096622942393));
#27936=CARTESIAN_POINT('Ctrl Pts',(35.5419214016919,31.5188660285384,2.66199567002338));
#27937=CARTESIAN_POINT('Ctrl Pts',(36.6798305021214,31.6960086763413,2.71432904580747));
#27938=CARTESIAN_POINT('Ctrl Pts',(37.7225174919474,32.4848285015448,2.76666242159155));
#27939=CARTESIAN_POINT('Ctrl Pts',(38.2024886486778,33.5316543411059,2.81899579737563));
#27940=CARTESIAN_POINT('Ctrl Pts',(38.6824598054083,34.5784801806669,2.87132917315972));
#27941=CARTESIAN_POINT('Ctrl Pts',(38.5997151290432,35.8833120345855,2.9236625489438));
#27942=CARTESIAN_POINT('Ctrl Pts',(37.9913535966355,36.8611222874319,2.97599592472789));
#27943=CARTESIAN_POINT('Ctrl Pts',(37.3829920642279,37.8389325402782,3.02832930051197));
#27944=CARTESIAN_POINT('Ctrl Pts',(36.2490136757777,38.4897211920522,3.08066267629606));
#27945=CARTESIAN_POINT('Ctrl Pts',(35.0978430789634,38.5217040264218,3.13299605208014));
#27946=CARTESIAN_POINT('Ctrl Pts',(33.946672482149,38.5536868607913,3.18532942786423));
#27947=CARTESIAN_POINT('Ctrl Pts',(32.7783096769706,37.9668638777563,3.23766280364831));
#27948=CARTESIAN_POINT('Ctrl Pts',(32.1165957326192,37.0243399779266,3.2899961794324));
#27949=CARTESIAN_POINT('Ctrl Pts',(31.7059940575521,36.4394922573,3.3224696854576));
#27950=CARTESIAN_POINT('Ctrl Pts',(31.4904702191063,35.7176870288261,3.35494319148281));
#27951=CARTESIAN_POINT('Ctrl Pts',(31.4866348863052,34.9979909502101,3.38741669750802));
#27952=CARTESIAN_POINT('Origin',(35.,35.,4.));
#27953=CARTESIAN_POINT('',(31.4769533103746,34.9997936499005,4.38741669750802));
#27954=CARTESIAN_POINT('',(31.4811433043907,35.0029051520383,4.11258330249198));
#27955=CARTESIAN_POINT('',(31.4825,35.,4.));
#27956=CARTESIAN_POINT('Ctrl Pts',(31.4811433043907,35.0029051520383,4.11258330249198));
#27957=CARTESIAN_POINT('Ctrl Pts',(31.4791554024968,35.227917919132,4.10238997204752));
#27958=CARTESIAN_POINT('Ctrl Pts',(31.4989360215654,35.4525827818457,4.09219664160306));
#27959=CARTESIAN_POINT('Ctrl Pts',(31.5417697834626,35.6727628942377,4.08200331115859));
#27960=CARTESIAN_POINT('Ctrl Pts',(31.761681751374,36.8031852448886,4.02966993537451));
#27961=CARTESIAN_POINT('Ctrl Pts',(32.5892464227109,37.815395051703,3.97733655959042));
#27962=CARTESIAN_POINT('Ctrl Pts',(33.6534212074435,38.2555631921955,3.92500318380634));
#27963=CARTESIAN_POINT('Ctrl Pts',(34.7175959921761,38.6957313326879,3.87266980802225));
#27964=CARTESIAN_POINT('Ctrl Pts',(36.0183808903044,38.5638578068583,3.82033643223817));
#27965=CARTESIAN_POINT('Ctrl Pts',(36.9725627531969,37.9190687430238,3.76800305645409));
#27966=CARTESIAN_POINT('Ctrl Pts',(37.9267446160893,37.2742796791893,3.71566968067));
#27967=CARTESIAN_POINT('Ctrl Pts',(38.5343234437459,36.1165750773498,3.66333630488592));
#27968=CARTESIAN_POINT('Ctrl Pts',(38.5228883542836,34.965017348136,3.61100292910183));
#27969=CARTESIAN_POINT('Ctrl Pts',(38.5114532648213,33.8134596189221,3.55866955331775));
#27970=CARTESIAN_POINT('Ctrl Pts',(37.8810042582401,32.6680487623339,3.50633617753366));
#27971=CARTESIAN_POINT('Ctrl Pts',(36.9142061709404,32.0423352319303,3.45400280174958));
#27972=CARTESIAN_POINT('Ctrl Pts',(35.9474080836407,31.4166217015266,3.40166942596549));
#27973=CARTESIAN_POINT('Ctrl Pts',(34.6442609156224,31.3106054973076,3.34933605018141));
#27974=CARTESIAN_POINT('Ctrl Pts',(33.5890369502264,31.7718194895137,3.29700267439732));
#27975=CARTESIAN_POINT('Ctrl Pts',(32.5338129848304,32.2330334817198,3.24466929861324));
#27976=CARTESIAN_POINT('Ctrl Pts',(31.7265122220568,33.2614776703508,3.19233592282916));
#27977=CARTESIAN_POINT('Ctrl Pts',(31.5290918320576,34.3960441771713,3.14000254704507));
#27978=CARTESIAN_POINT('Ctrl Pts',(31.4946134017248,34.5941902362662,3.13086279886071));
#27979=CARTESIAN_POINT('Ctrl Pts',(31.4787367991106,34.7955731089531,3.12172305067635));
#27980=CARTESIAN_POINT('Ctrl Pts',(31.48047694743,34.9972296622465,3.11258330249198));
#27981=CARTESIAN_POINT('Ctrl Pts',(31.4866348863052,34.9979909502101,3.38741669750802));
#27982=CARTESIAN_POINT('Ctrl Pts',(31.4842893061927,34.5578453627213,3.4072765672669));
#27983=CARTESIAN_POINT('Ctrl Pts',(31.5611193891505,34.1184886387468,3.42713643702577));
#27984=CARTESIAN_POINT('Ctrl Pts',(31.7209246555095,33.7117308512332,3.44699630678465));
#27985=CARTESIAN_POINT('Ctrl Pts',(32.1420326062756,32.6398704409937,3.49932968256873));
#27986=CARTESIAN_POINT('Ctrl Pts',(33.1393135913321,31.7943744371391,3.55166305835282));
#27987=CARTESIAN_POINT('Ctrl Pts',(34.2656318975588,31.5543250290031,3.6039964341369));
#27988=CARTESIAN_POINT('Ctrl Pts',(35.3919502037855,31.3142756208671,3.65632980992098));
#27989=CARTESIAN_POINT('Ctrl Pts',(36.6473058311824,31.6796728084497,3.70866318570507));
#27990=CARTESIAN_POINT('Ctrl Pts',(37.4688540624077,32.4866890097577,3.76099656148916));
#27991=CARTESIAN_POINT('Ctrl Pts',(38.2904022936331,33.2937052110658,3.81332993727324));
#27992=CARTESIAN_POINT('Ctrl Pts',(38.6781431286869,34.5423404260991,3.86566331305732));
#27993=CARTESIAN_POINT('Ctrl Pts',(38.4582311043207,35.6727630669474,3.91799668884141));
#27994=CARTESIAN_POINT('Ctrl Pts',(38.2383190799545,36.8031857077956,3.97033006462549));
#27995=CARTESIAN_POINT('Ctrl Pts',(37.4107541961682,37.8153957744587,4.02266344040958));
#27996=CARTESIAN_POINT('Ctrl Pts',(36.3465791382448,38.2555640279499,4.07499681619366));
#27997=CARTESIAN_POINT('Ctrl Pts',(35.2824040803214,38.6957322814412,4.12733019197775));
#27998=CARTESIAN_POINT('Ctrl Pts',(33.9816188482609,38.5638587217606,4.17966356776183));
#27999=CARTESIAN_POINT('Ctrl Pts',(33.0274367404146,37.9190694923971,4.23199694354592));
#28000=CARTESIAN_POINT('Ctrl Pts',(32.0828594910996,37.2807707529301,4.28380352819995));
#28001=CARTESIAN_POINT('Ctrl Pts',(31.4779426270586,36.1398304565742,4.33561011285398));
#28002=CARTESIAN_POINT('Ctrl Pts',(31.4769533103746,34.9997936499005,4.38741669750802));
#28003=CARTESIAN_POINT('Origin',(35.,35.,4.));
#28004=CARTESIAN_POINT('',(31.4861926565527,35.0022702467704,5.38741669750802));
#28005=CARTESIAN_POINT('',(31.4875431178521,34.9988611670469,5.11258330249198));
#28006=CARTESIAN_POINT('',(31.4825,35.,4.));
#28007=CARTESIAN_POINT('Ctrl Pts',(31.4875431178521,34.9988611670469,5.11258330249198));
#28008=CARTESIAN_POINT('Ctrl Pts',(31.4894883427227,35.6536666001145,5.08305689341869));
#28009=CARTESIAN_POINT('Ctrl Pts',(31.6654106307538,36.3094429302072,5.0535304843454));
#28010=CARTESIAN_POINT('Ctrl Pts',(32.0086471712983,36.8611218096429,5.02400407527211));
#28011=CARTESIAN_POINT('Ctrl Pts',(32.6170085475347,37.8389318114614,4.97167069948803));
#28012=CARTESIAN_POINT('Ctrl Pts',(33.7509866448637,38.4897202961854,4.91933732370394));
#28013=CARTESIAN_POINT('Ctrl Pts',(34.9021569461515,38.5217031223488,4.86700394791986));
#28014=CARTESIAN_POINT('Ctrl Pts',(36.0533272474394,38.5536859485121,4.81467057213577));
#28015=CARTESIAN_POINT('Ctrl Pts',(37.2216897526861,37.9668631161147,4.76233719635169));
#28016=CARTESIAN_POINT('Ctrl Pts',(37.8834035271664,37.0243394582438,4.71000382056761));
#28017=CARTESIAN_POINT('Ctrl Pts',(38.5451173016466,36.0818158003729,4.65767044478352));
#28018=CARTESIAN_POINT('Ctrl Pts',(38.7001823453603,34.7835913170285,4.60533706899944));
#28019=CARTESIAN_POINT('Ctrl Pts',(38.2790745026986,33.7117311819539,4.55300369321535));
#28020=CARTESIAN_POINT('Ctrl Pts',(37.857966660037,32.6398710468792,4.50067031743127));
#28021=CARTESIAN_POINT('Ctrl Pts',(36.860685931,31.7943752600742,4.44833694164718));
#28022=CARTESIAN_POINT('Ctrl Pts',(35.7343679139176,31.5543259135622,4.3960035658631));
#28023=CARTESIAN_POINT('Ctrl Pts',(34.6080498968352,31.3142765670502,4.34367019007902));
#28024=CARTESIAN_POINT('Ctrl Pts',(33.3526945917074,31.6796736608312,4.29133681429493));
#28025=CARTESIAN_POINT('Ctrl Pts',(32.5311465713864,32.4866896549654,4.23900343851085));
#28026=CARTESIAN_POINT('Ctrl Pts',(31.8696170922289,33.1365176103207,4.19686339317123));
#28027=CARTESIAN_POINT('Ctrl Pts',(31.4893614502066,34.0726843317691,4.15472334783161));
#28028=CARTESIAN_POINT('Ctrl Pts',(31.4811433043907,35.0029051520383,4.11258330249198));
#28029=CARTESIAN_POINT('Ctrl Pts',(31.4769533103746,34.9997936499005,4.38741669750802));
#28030=CARTESIAN_POINT('Ctrl Pts',(31.4769432505867,34.9882012764272,4.38794348863807));
#28031=CARTESIAN_POINT('Ctrl Pts',(31.476995634958,34.9766089963718,4.38847027976812));
#28032=CARTESIAN_POINT('Ctrl Pts',(31.4771107413343,34.9650173391525,4.38899707089817));
#28033=CARTESIAN_POINT('Ctrl Pts',(31.4885458337323,33.8134593143178,4.44133044668225));
#28034=CARTESIAN_POINT('Ctrl Pts',(32.1189950021604,32.6680481636951,4.49366382246634));
#28035=CARTESIAN_POINT('Ctrl Pts',(33.0857933376524,32.0423344726558,4.54599719825042));
#28036=CARTESIAN_POINT('Ctrl Pts',(34.0525916731444,31.4166207816165,4.59833057403451));
#28037=CARTESIAN_POINT('Ctrl Pts',(35.3557391757004,31.3106045501606,4.65066394981859));
#28038=CARTESIAN_POINT('Ctrl Pts',(36.4109634119899,31.7718186607773,4.70299732560267));
#28039=CARTESIAN_POINT('Ctrl Pts',(37.4661876482795,32.233032771394,4.75533070138676));
#28040=CARTESIAN_POINT('Ctrl Pts',(38.2734886183026,33.2614772240832,4.80766407717084));
#28041=CARTESIAN_POINT('Ctrl Pts',(38.4709090589814,34.3960440221467,4.85999745295493));
#28042=CARTESIAN_POINT('Ctrl Pts',(38.6683294996601,35.5306108202102,4.91233082873901));
#28043=CARTESIAN_POINT('Ctrl Pts',(38.2558694109946,36.771299963648,4.9646642045231));
#28044=CARTESIAN_POINT('Ctrl Pts',(37.4184572536729,37.5618425098028,5.01699758030718));
#28045=CARTESIAN_POINT('Ctrl Pts',(36.5810450963513,38.3523850559575,5.06933095609127));
#28046=CARTESIAN_POINT('Ctrl Pts',(35.3186808703736,38.6927810048293,5.12166433187535));
#28047=CARTESIAN_POINT('Ctrl Pts',(34.1973516288142,38.4304122279041,5.17399770765944));
#28048=CARTESIAN_POINT('Ctrl Pts',(33.0760223872548,38.168043450979,5.22633108344352));
#28049=CARTESIAN_POINT('Ctrl Pts',(32.0957281301138,37.302909948257,5.2786644592276));
#28050=CARTESIAN_POINT('Ctrl Pts',(31.6959884957425,36.2228984191863,5.33099783501169));
#28051=CARTESIAN_POINT('Ctrl Pts',(31.5523398513352,35.834790313921,5.34980412251047));
#28052=CARTESIAN_POINT('Ctrl Pts',(31.4836619352111,35.4189336360054,5.36861041000924));
#28053=CARTESIAN_POINT('Ctrl Pts',(31.4861926565527,35.0022702467704,5.38741669750802));
#28054=CARTESIAN_POINT('Origin',(35.,35.,4.));
#28055=CARTESIAN_POINT('',(31.4836963557363,34.997016753135,6.38741669750802));
#28056=CARTESIAN_POINT('',(31.4775764275568,34.998690818207,6.11258330249198));
#28057=CARTESIAN_POINT('',(31.4825,35.,4.));
#28058=CARTESIAN_POINT('Ctrl Pts',(31.4775764275568,34.998690818207,6.11258330249198));
#28059=CARTESIAN_POINT('Ctrl Pts',(31.4827872982739,36.074383472183,6.06372381478987));
#28060=CARTESIAN_POINT('Ctrl Pts',(32.0123599558151,37.1545218488605,6.01486432708775));
#28061=CARTESIAN_POINT('Ctrl Pts',(32.8684049695572,37.8050433721304,5.96600483938563));
#28062=CARTESIAN_POINT('Ctrl Pts',(33.7853144071958,38.5018166895356,5.91367146360154));
#28063=CARTESIAN_POINT('Ctrl Pts',(35.0767706487491,38.7057102384231,5.86133808781746));
#28064=CARTESIAN_POINT('Ctrl Pts',(36.1637432436869,38.3253071915374,5.80900471203338));
#28065=CARTESIAN_POINT('Ctrl Pts',(37.2507158386246,37.9449041446517,5.75667133624929));
#28066=CARTESIAN_POINT('Ctrl Pts',(38.1332047869467,36.9802045019929,5.70433796046521));
#28067=CARTESIAN_POINT('Ctrl Pts',(38.4155418609846,35.8637360634774,5.65200458468113));
#28068=CARTESIAN_POINT('Ctrl Pts',(38.6978789350226,34.7472676249618,5.59967120889704));
#28069=CARTESIAN_POINT('Ctrl Pts',(38.3800641347763,33.4790303905896,5.54733783311296));
#28070=CARTESIAN_POINT('Ctrl Pts',(37.604591287456,32.6276445643168,5.49500445732887));
#28071=CARTESIAN_POINT('Ctrl Pts',(36.8291184401356,31.7762587380439,5.44267108154479));
#28072=CARTESIAN_POINT('Ctrl Pts',(35.595987545741,31.3417243198703,5.3903377057607));
#28073=CARTESIAN_POINT('Ctrl Pts',(34.4580787374483,31.5188669221671,5.33800432997662));
#28074=CARTESIAN_POINT('Ctrl Pts',(33.3201699291557,31.6960095244639,5.28567095419254));
#28075=CARTESIAN_POINT('Ctrl Pts',(32.277483206965,32.4848291472311,5.23333757840845));
#28076=CARTESIAN_POINT('Ctrl Pts',(31.7975121734416,33.5316547180712,5.18100420262437));
#28077=CARTESIAN_POINT('Ctrl Pts',(31.5883400491575,33.9878629329714,5.15819723591357));
#28078=CARTESIAN_POINT('Ctrl Pts',(31.4860405755429,34.4930724110572,5.13539026920278));
#28079=CARTESIAN_POINT('Ctrl Pts',(31.4875431178521,34.9988611670469,5.11258330249198));
#28080=CARTESIAN_POINT('Ctrl Pts',(31.4861926565527,35.0022702467704,5.38741669750802));
#28081=CARTESIAN_POINT('Ctrl Pts',(31.4907043241454,34.2594596183014,5.42094378579333));
#28082=CARTESIAN_POINT('Ctrl Pts',(31.7215335296905,33.5140850744687,5.45447087407864));
#28083=CARTESIAN_POINT('Ctrl Pts',(32.1573641816635,32.9187998099572,5.48799796236395));
#28084=CARTESIAN_POINT('Ctrl Pts',(32.8376645135573,31.9896022852182,5.54033133814803));
#28085=CARTESIAN_POINT('Ctrl Pts',(34.0174501889464,31.4260967911598,5.59266471393211));
#28086=CARTESIAN_POINT('Ctrl Pts',(35.1677586650642,31.4809334902507,5.64499808971619));
#28087=CARTESIAN_POINT('Ctrl Pts',(36.318067141182,31.5357701893416,5.69733146550028));
#28088=CARTESIAN_POINT('Ctrl Pts',(37.4388984180285,32.2089490815819,5.74966484128437));
#28089=CARTESIAN_POINT('Ctrl Pts',(38.027722367947,33.1986476425792,5.80199821706845));
#28090=CARTESIAN_POINT('Ctrl Pts',(38.6165463178655,34.1883462035765,5.85433159285254));
#28091=CARTESIAN_POINT('Ctrl Pts',(38.6733629408561,35.4945644333309,5.90666496863662));
#28092=CARTESIAN_POINT('Ctrl Pts',(38.1726983287836,36.5316521939121,5.9589983444207));
#28093=CARTESIAN_POINT('Ctrl Pts',(37.6720337167111,37.5687399544933,6.01133172020479));
#28094=CARTESIAN_POINT('Ctrl Pts',(36.6138878695757,38.3366972459014,6.06366509598887));
#28095=CARTESIAN_POINT('Ctrl Pts',(35.4726853575398,38.491208604665,6.11599847177296));
#28096=CARTESIAN_POINT('Ctrl Pts',(34.3314828455038,38.6457199634287,6.16833184755704));
#28097=CARTESIAN_POINT('Ctrl Pts',(33.1072236685675,38.1867853895479,6.22066522334113));
#28098=CARTESIAN_POINT('Ctrl Pts',(32.3488106963438,37.3201666288988,6.27299859912521));
#28099=CARTESIAN_POINT('Ctrl Pts',(31.7960966856348,36.6885947168973,6.31113796525281));
#28100=CARTESIAN_POINT('Ctrl Pts',(31.490801080199,35.8404951819918,6.34927733138042));
#28101=CARTESIAN_POINT('Ctrl Pts',(31.4836963557363,34.997016753135,6.38741669750802));
#28102=CARTESIAN_POINT('Origin',(35.,35.,4.));
#28103=CARTESIAN_POINT('',(31.47826034488,35.0017653187145,7.38741669750802));
#28104=CARTESIAN_POINT('',(31.4846882532079,35.0028111988253,7.11258330249198));
#28105=CARTESIAN_POINT('',(31.4825,35.,4.));
#28106=CARTESIAN_POINT('',(37.6735319337713,37.2858331630075,8.));
#28107=CARTESIAN_POINT('Ctrl Pts',(31.47826034488,35.0017653187145,7.38741669750802));
#28108=CARTESIAN_POINT('Ctrl Pts',(31.4849539836961,33.9623976729958,7.43461100431976));
#28109=CARTESIAN_POINT('Ctrl Pts',(31.9746240526108,32.9177662403339,7.4818053111315));
#28110=CARTESIAN_POINT('Ctrl Pts',(32.7813938443113,32.2635129435208,7.52899961794324));
#28111=CARTESIAN_POINT('Ctrl Pts',(33.6760141816485,31.5380168836533,7.58133299372733));
#28112=CARTESIAN_POINT('Ctrl Pts',(34.9605532865631,31.292545720314,7.63366636951141));
#28113=CARTESIAN_POINT('Ctrl Pts',(36.0588773921206,31.639261394405,7.68599974529549));
#28114=CARTESIAN_POINT('Ctrl Pts',(37.1572014976782,31.985977068496,7.73833312107957));
#28115=CARTESIAN_POINT('Ctrl Pts',(38.0693106038786,32.9248795800174,7.79066649686366));
#28116=CARTESIAN_POINT('Ctrl Pts',(38.3863002982481,34.0300657119841,7.84299987264775));
#28117=CARTESIAN_POINT('Ctrl Pts',(38.7032899926177,35.1352518439507,7.89533324843183));
#28118=CARTESIAN_POINT('Ctrl Pts',(38.4251602751564,36.4067215963626,7.94766662421592));
#28119=CARTESIAN_POINT('Ctrl Pts',(37.6735319337713,37.2858331630076,8.));
#28120=CARTESIAN_POINT('',(32.321499452735,37.2890251664065,7.99999999999999));
#28121=CARTESIAN_POINT('Origin',(35.,35.,8.));
#28122=CARTESIAN_POINT('Ctrl Pts',(32.321476328717,37.2890400220486,8.));
#28123=CARTESIAN_POINT('Ctrl Pts',(33.0392492598742,38.1233257780545,7.95000212253755));
#28124=CARTESIAN_POINT('Ctrl Pts',(34.1813302937714,38.5989193684354,7.90000424507511));
#28125=CARTESIAN_POINT('Ctrl Pts',(35.278297796919,38.5118532074872,7.85000636761267));
#28126=CARTESIAN_POINT('Ctrl Pts',(36.4265067905564,38.4207200164352,7.79767299182859));
#28127=CARTESIAN_POINT('Ctrl Pts',(37.5252891335093,37.7131334793234,7.74533961604451));
#28128=CARTESIAN_POINT('Ctrl Pts',(38.0826702008662,36.7055536192858,7.69300624026042));
#28129=CARTESIAN_POINT('Ctrl Pts',(38.6400512682231,35.6979737592483,7.64067286447634));
#28130=CARTESIAN_POINT('Ctrl Pts',(38.6560310599838,34.390400576285,7.58833948869225));
#28131=CARTESIAN_POINT('Ctrl Pts',(38.1231127521292,33.3694814726124,7.53600611290816));
#28132=CARTESIAN_POINT('Ctrl Pts',(37.5901944442746,32.3485623689397,7.48367273712408));
#28133=CARTESIAN_POINT('Ctrl Pts',(36.5083780368047,31.6142973445577,7.43133936134));
#28134=CARTESIAN_POINT('Ctrl Pts',(35.3628660305036,31.4957037502949,7.37900598555592));
#28135=CARTESIAN_POINT('Ctrl Pts',(34.2173540242026,31.3771101560321,7.32667260977183));
#28136=CARTESIAN_POINT('Ctrl Pts',(33.0081464190704,31.8741879918886,7.27433923398774));
#28137=CARTESIAN_POINT('Ctrl Pts',(32.2773153573829,32.7641662925145,7.22200585820366));
#28138=CARTESIAN_POINT('Ctrl Pts',(31.7679565185591,33.3844441344804,7.18553167296643));
#28139=CARTESIAN_POINT('Ctrl Pts',(31.4909695616634,34.1955737681155,7.14905748772921));
#28140=CARTESIAN_POINT('Ctrl Pts',(31.4846882532079,35.0028111988253,7.11258330249198));
#28141=CARTESIAN_POINT('Origin',(-35.,35.,4.));
#28142=CARTESIAN_POINT('',(-38.5120268522747,34.9998626667344,0.387416697508021));
#28143=CARTESIAN_POINT('',(-38.5151985683976,34.9953484440209,0.112583302491983));
#28144=CARTESIAN_POINT('',(-38.5175,35.,4.));
#28145=CARTESIAN_POINT('',(-37.6735319337713,37.2858331630075,0.));
#28146=CARTESIAN_POINT('Ctrl Pts',(-38.5151985683976,34.9953484440209,0.112583302491983));
#28147=CARTESIAN_POINT('Ctrl Pts',(-38.508022599206,35.8232716101844,0.0750555349946553));
#28148=CARTESIAN_POINT('Ctrl Pts',(-38.2125174896864,36.6554305951821,0.0375277674973274));
#28149=CARTESIAN_POINT('Ctrl Pts',(-37.6735319337713,37.2858331630075,0.));
#28150=CARTESIAN_POINT('',(-32.3214993158099,37.289025066123,6.74947782880687E-15));
#28151=CARTESIAN_POINT('Origin',(-35.,35.,0.));
#28152=CARTESIAN_POINT('Ctrl Pts',(-32.3214761820288,37.2890399271607,4.52762827229947E-15));
#28153=CARTESIAN_POINT('Ctrl Pts',(-33.0392490750158,38.123325504421,0.0499978774624455));
#28154=CARTESIAN_POINT('Ctrl Pts',(-34.1813302139117,38.5989195898449,0.0999957549248864));
#28155=CARTESIAN_POINT('Ctrl Pts',(-35.2782977979761,38.5118535311589,0.149993632387327));
#28156=CARTESIAN_POINT('Ctrl Pts',(-36.42650687631,38.420720447146,0.202327008171411));
#28157=CARTESIAN_POINT('Ctrl Pts',(-37.5252892775753,37.7131335867401,0.254660383955495));
#28158=CARTESIAN_POINT('Ctrl Pts',(-38.0826703648835,36.7055536147166,0.30699375973958));
#28159=CARTESIAN_POINT('Ctrl Pts',(-38.368187486773,36.189423196523,0.333801405662393));
#28160=CARTESIAN_POINT('Ctrl Pts',(-38.511642203595,35.5945753060192,0.360609051585207));
#28161=CARTESIAN_POINT('Ctrl Pts',(-38.5120268522747,34.9998626667344,0.387416697508021));
#28162=CARTESIAN_POINT('Origin',(-35.,35.,4.));
#28163=CARTESIAN_POINT('',(-38.5212301417031,34.9978480330234,1.38741669750802));
#28164=CARTESIAN_POINT('',(-38.5220165881118,35.0016823567161,1.11258330249198));
#28165=CARTESIAN_POINT('',(-38.5175,35.,4.));
#28166=CARTESIAN_POINT('Ctrl Pts',(-38.5220165881118,35.0016823567161,1.11258330249198));
#28167=CARTESIAN_POINT('Ctrl Pts',(-38.5226066014871,35.1013890040059,1.10805583214991));
#28168=CARTESIAN_POINT('Ctrl Pts',(-38.5187309301454,35.2010488154761,1.10352836180785));
#28169=CARTESIAN_POINT('Ctrl Pts',(-38.5102390188272,35.3003133215195,1.09900089146578));
#28170=CARTESIAN_POINT('Ctrl Pts',(-38.4120803667407,36.4477193350987,1.04666751568169));
#28171=CARTESIAN_POINT('Ctrl Pts',(-37.6971355129363,37.5423077018709,0.994334139897609));
#28172=CARTESIAN_POINT('Ctrl Pts',(-36.6859404016511,38.0934400513324,0.942000764113524));
#28173=CARTESIAN_POINT('Ctrl Pts',(-35.6747452903659,38.6445724007939,0.88966738832944));
#28174=CARTESIAN_POINT('Ctrl Pts',(-34.3672999215998,38.6522487329447,0.837334012545356));
#28175=CARTESIAN_POINT('Ctrl Pts',(-33.3498298999919,38.1127743676805,0.785000636761271));
#28176=CARTESIAN_POINT('Ctrl Pts',(-32.332359878384,37.5733000024162,0.732667260977186));
#28177=CARTESIAN_POINT('Ctrl Pts',(-31.6048652039344,36.4866749397369,0.680333885193101));
#28178=CARTESIAN_POINT('Ctrl Pts',(-31.4934688910568,35.3406024624848,0.628000509409016));
#28179=CARTESIAN_POINT('Ctrl Pts',(-31.3820725781792,34.1945299852327,0.575667133624932));
#28180=CARTESIAN_POINT('Ctrl Pts',(-31.8867746268736,32.9890100934079,0.523333757840848));
#28181=CARTESIAN_POINT('Ctrl Pts',(-32.7813945002955,32.26351389125,0.471000382056763));
#28182=CARTESIAN_POINT('Ctrl Pts',(-33.6760143737173,31.5380176890922,0.418667006272678));
#28183=CARTESIAN_POINT('Ctrl Pts',(-34.9605520718666,31.2925451766014,0.366333630488594));
#28184=CARTESIAN_POINT('Ctrl Pts',(-36.0588768524004,31.6392614911932,0.31400025470451));
#28185=CARTESIAN_POINT('Ctrl Pts',(-37.1572016329341,31.9859778057849,0.261666878920425));
#28186=CARTESIAN_POINT('Ctrl Pts',(-38.0693134958523,32.9248829474593,0.209333503136341));
#28187=CARTESIAN_POINT('Ctrl Pts',(-38.3863031564079,34.0300688951037,0.157000127352256));
#28188=CARTESIAN_POINT('Ctrl Pts',(-38.4759825373922,34.3427364801714,0.142194519065498));
#28189=CARTESIAN_POINT('Ctrl Pts',(-38.5180296611061,34.6687128110693,0.127388910778741));
#28190=CARTESIAN_POINT('Ctrl Pts',(-38.5151985683976,34.9953484440209,0.112583302491983));
#28191=CARTESIAN_POINT('Ctrl Pts',(-38.5120268522747,34.9998626667344,0.387416697508021));
#28192=CARTESIAN_POINT('Ctrl Pts',(-38.5123931074215,34.4335886186821,0.412942427369291));
#28193=CARTESIAN_POINT('Ctrl Pts',(-38.3830450900788,33.8674371959539,0.438468157230563));
#28194=CARTESIAN_POINT('Ctrl Pts',(-38.1231128912653,33.3694814421284,0.463993887091834));
#28195=CARTESIAN_POINT('Ctrl Pts',(-37.5901945569878,32.348562325205,0.516327262875918));
#28196=CARTESIAN_POINT('Ctrl Pts',(-36.5083781150815,31.6142971749993,0.568660638660002));
#28197=CARTESIAN_POINT('Ctrl Pts',(-35.3628660558844,31.4957035546786,0.620994014444087));
#28198=CARTESIAN_POINT('Ctrl Pts',(-34.2173539966873,31.3771099343579,0.673327390228171));
#28199=CARTESIAN_POINT('Ctrl Pts',(-33.0081463201995,31.8741878439222,0.725660766012255));
#28200=CARTESIAN_POINT('Ctrl Pts',(-32.2773152209783,32.7641661988384,0.77799414179634));
#28201=CARTESIAN_POINT('Ctrl Pts',(-31.5464841217571,33.6541445537545,0.830327517580424));
#28202=CARTESIAN_POINT('Ctrl Pts',(-31.2940295998026,34.9370233540225,0.882660893364509));
#28203=CARTESIAN_POINT('Ctrl Pts',(-31.6331814964185,36.0375699846378,0.934994269148593));
#28204=CARTESIAN_POINT('Ctrl Pts',(-31.9723333930344,37.1381166152532,0.987327644932678));
#28205=CARTESIAN_POINT('Ctrl Pts',(-32.9030917082208,38.0563310762161,1.03966102071676));
#28206=CARTESIAN_POINT('Ctrl Pts',(-34.0081263071124,38.3805512169411,1.09199439650085));
#28207=CARTESIAN_POINT('Ctrl Pts',(-35.1131609060039,38.7047713576661,1.14432777228493));
#28208=CARTESIAN_POINT('Ctrl Pts',(-36.3924717886008,38.4349971781534,1.19666114806902));
#28209=CARTESIAN_POINT('Ctrl Pts',(-37.2724838028734,37.6921714555696,1.2489945238531));
#28210=CARTESIAN_POINT('Ctrl Pts',(-38.0483632745171,37.0372449093246,1.29513524840474));
#28211=CARTESIAN_POINT('Ctrl Pts',(-38.5138515465497,36.0145962191428,1.34127597295638));
#28212=CARTESIAN_POINT('Ctrl Pts',(-38.5212301417031,34.9978480330234,1.38741669750802));
#28213=CARTESIAN_POINT('Origin',(-35.,35.,4.));
#28214=CARTESIAN_POINT('',(-38.516961906974,35.0030273033746,2.38741669750802));
#28215=CARTESIAN_POINT('',(-38.512261546942,35.0007919713519,2.11258330249198));
#28216=CARTESIAN_POINT('',(-38.5175,35.,4.));
#28217=CARTESIAN_POINT('Ctrl Pts',(-38.512261546942,35.0007919713519,2.11258330249198));
#28218=CARTESIAN_POINT('Ctrl Pts',(-38.513350743052,35.5300199732952,2.08872275352109));
#28219=CARTESIAN_POINT('Ctrl Pts',(-38.400967605409,36.0588087668393,2.06486220455019));
#28220=CARTESIAN_POINT('Ctrl Pts',(-38.1726977821637,36.5316519312173,2.0410016555793));
#28221=CARTESIAN_POINT('Ctrl Pts',(-37.6720332561867,37.568739511998,1.98866827979521));
#28222=CARTESIAN_POINT('Ctrl Pts',(-36.6138875906958,38.3366966664809,1.93633490401113));
#28223=CARTESIAN_POINT('Ctrl Pts',(-35.472685275733,38.4912080005995,1.88400152822705));
#28224=CARTESIAN_POINT('Ctrl Pts',(-34.3314829607702,38.6457193347182,1.83166815244296));
#28225=CARTESIAN_POINT('Ctrl Pts',(-33.1072239963354,38.1867848484726,1.77933477665888));
#28226=CARTESIAN_POINT('Ctrl Pts',(-32.3488111539779,37.3201662335233,1.72700140087479));
#28227=CARTESIAN_POINT('Ctrl Pts',(-31.5903983116205,36.453547618574,1.67466802509071));
#28228=CARTESIAN_POINT('Ctrl Pts',(-31.2978315913404,35.179244874921,1.62233464930662));
#28229=CARTESIAN_POINT('Ctrl Pts',(-31.6022838952552,34.0686053777681,1.57000127352254));
#28230=CARTESIAN_POINT('Ctrl Pts',(-31.90673619917,32.9579658806151,1.51766789773845));
#28231=CARTESIAN_POINT('Ctrl Pts',(-32.8082075272796,32.0109896299622,1.46533452195437));
#28232=CARTESIAN_POINT('Ctrl Pts',(-33.9025204773781,31.6522426059455,1.41300114617028));
#28233=CARTESIAN_POINT('Ctrl Pts',(-34.9968334274766,31.2934955819288,1.3606677703862));
#28234=CARTESIAN_POINT('Ctrl Pts',(-36.283987999564,31.5229777845482,1.30833439460212));
#28235=CARTESIAN_POINT('Ctrl Pts',(-37.1868790604233,32.2378307160511,1.25600101881803));
#28236=CARTESIAN_POINT('Ctrl Pts',(-38.0116591177612,32.8908402178529,1.20819511337602));
#28237=CARTESIAN_POINT('Ctrl Pts',(-38.5157865917788,33.94887224596,1.160389207934));
#28238=CARTESIAN_POINT('Ctrl Pts',(-38.5220165881118,35.0016823567161,1.11258330249198));
#28239=CARTESIAN_POINT('Ctrl Pts',(-38.5212301417031,34.9978480330234,1.38741669750802));
#28240=CARTESIAN_POINT('Ctrl Pts',(-38.5222204396842,34.8613879542309,1.39360934874046));
#28241=CARTESIAN_POINT('Ctrl Pts',(-38.5149588389545,34.7250341608202,1.39980199997291));
#28242=CARTESIAN_POINT('Ctrl Pts',(-38.499088221748,34.5896899066556,1.40599465120535));
#28243=CARTESIAN_POINT('Ctrl Pts',(-38.3649674804015,33.4459113459803,1.45832802698944));
#28244=CARTESIAN_POINT('Ctrl Pts',(-37.6160128517601,32.3742314902846,1.51066140277352));
#28245=CARTESIAN_POINT('Ctrl Pts',(-36.5880242056904,31.8551402422105,1.56299477855761));
#28246=CARTESIAN_POINT('Ctrl Pts',(-35.5600355596207,31.3360489941365,1.61532815434169));
#28247=CARTESIAN_POINT('Ctrl Pts',(-34.2530128961227,31.3695463536841,1.66766153012578));
#28248=CARTESIAN_POINT('Ctrl Pts',(-33.2529648698024,31.9406150594439,1.71999490590986));
#28249=CARTESIAN_POINT('Ctrl Pts',(-32.2529168434821,32.5116837652037,1.77232828169395));
#28250=CARTESIAN_POINT('Ctrl Pts',(-31.5598434543395,33.6203238171756,1.82466165747803));
#28251=CARTESIAN_POINT('Ctrl Pts',(-31.4844880896413,34.7694704150121,1.87699503326211));
#28252=CARTESIAN_POINT('Ctrl Pts',(-31.4091327249431,35.9186170128485,1.9293284090462));
#28253=CARTESIAN_POINT('Ctrl Pts',(-31.9514953846893,37.1082701565493,1.98166178483028));
#28254=CARTESIAN_POINT('Ctrl Pts',(-32.8684048665688,37.8050435076812,2.03399516061437));
#28255=CARTESIAN_POINT('Ctrl Pts',(-33.7853143484484,38.5018168588132,2.08632853639845));
#28256=CARTESIAN_POINT('Ctrl Pts',(-35.0767706524612,38.7057104173762,2.13866191218254));
#28257=CARTESIAN_POINT('Ctrl Pts',(-36.1637432999128,38.325307352079,2.19099528796662));
#28258=CARTESIAN_POINT('Ctrl Pts',(-37.2507159473644,37.9449042867818,2.24332866375071));
#28259=CARTESIAN_POINT('Ctrl Pts',(-38.1332049382548,36.9802045976245,2.29566203953479));
#28260=CARTESIAN_POINT('Ctrl Pts',(-38.4155420259161,35.8637361052132,2.34799541531887));
#28261=CARTESIAN_POINT('Ctrl Pts',(-38.4864342614375,35.5834011765932,2.36113584271526));
#28262=CARTESIAN_POINT('Ctrl Pts',(-38.5194889764144,35.2934977450987,2.37427627011164));
#28263=CARTESIAN_POINT('Ctrl Pts',(-38.516961906974,35.0030273033746,2.38741669750802));
#28264=CARTESIAN_POINT('Origin',(-35.,35.,4.));
#28265=CARTESIAN_POINT('',(-38.5133643814276,34.9979909506281,3.38741669750802));
#28266=CARTESIAN_POINT('',(-38.5195233495341,34.9972296620149,3.11258330249199));
#28267=CARTESIAN_POINT('',(-38.5175,35.,4.));
#28268=CARTESIAN_POINT('Ctrl Pts',(-38.5195233495341,34.9972296620149,3.11258330249199));
#28269=CARTESIAN_POINT('Ctrl Pts',(-38.5112995644464,35.9502404698791,3.06938967489226));
#28270=CARTESIAN_POINT('Ctrl Pts',(-38.1096192565637,36.9093637226591,3.02619604729254));
#28271=CARTESIAN_POINT('Ctrl Pts',(-37.4184568368782,37.5618420683218,2.98300241969282));
#28272=CARTESIAN_POINT('Ctrl Pts',(-36.581044823874,38.3523844782111,2.93066904390873));
#28273=CARTESIAN_POINT('Ctrl Pts',(-35.3186808154442,38.6927803683205,2.87833566812465));
#28274=CARTESIAN_POINT('Ctrl Pts',(-34.1973517671389,38.4304116366569,2.82600229234057));
#28275=CARTESIAN_POINT('Ctrl Pts',(-33.0760227188335,38.1680429049932,2.77366891655648));
#28276=CARTESIAN_POINT('Ctrl Pts',(-32.0957286306525,37.3029095515566,2.7213355407724));
#28277=CARTESIAN_POINT('Ctrl Pts',(-31.6959890651629,36.2228982085294,2.66900216498831));
#28278=CARTESIAN_POINT('Ctrl Pts',(-31.2962494996734,35.1428868655023,2.61666878920423));
#28279=CARTESIAN_POINT('Ctrl Pts',(-31.4770644568753,33.8479975328846,2.56433541342014));
#28280=CARTESIAN_POINT('Ctrl Pts',(-32.1573646715461,32.9188001684451,2.51200203763606));
#28281=CARTESIAN_POINT('Ctrl Pts',(-32.837664886217,31.9896028040056,2.45966866185197));
#28282=CARTESIAN_POINT('Ctrl Pts',(-34.0174503583568,31.4260974077442,2.40733528606789));
#28283=CARTESIAN_POINT('Ctrl Pts',(-35.1677586361884,31.4809340970796,2.3550019102838));
#28284=CARTESIAN_POINT('Ctrl Pts',(-36.3180669140201,31.535770786415,2.30266853449972));
#28285=CARTESIAN_POINT('Ctrl Pts',(-37.4388979975435,32.2089495613471,2.25033515871564));
#28286=CARTESIAN_POINT('Ctrl Pts',(-38.0277218460737,33.1986479523525,2.19800178293155));
#28287=CARTESIAN_POINT('Ctrl Pts',(-38.3480810663893,33.737109506995,2.16952895611836));
#28288=CARTESIAN_POINT('Ctrl Pts',(-38.5109618076844,34.3692634485841,2.14105612930517));
#28289=CARTESIAN_POINT('Ctrl Pts',(-38.512261546942,35.0007919713519,2.11258330249198));
#28290=CARTESIAN_POINT('Ctrl Pts',(-38.516961906974,35.0030273033746,2.38741669750802));
#28291=CARTESIAN_POINT('Ctrl Pts',(-38.5094246101142,34.1366633193706,2.42660964589572));
#28292=CARTESIAN_POINT('Ctrl Pts',(-38.1853502176079,33.2652551878002,2.46580259428343));
#28293=CARTESIAN_POINT('Ctrl Pts',(-37.6045914132455,32.6276444497373,2.50499554267113));
#28294=CARTESIAN_POINT('Ctrl Pts',(-36.8291185284818,31.7762585823377,2.55732891845521));
#28295=CARTESIAN_POINT('Ctrl Pts',(-35.5959875745222,31.3417241432036,2.6096622942393));
#28296=CARTESIAN_POINT('Ctrl Pts',(-34.4580787112737,31.5188667540608,2.66199567002338));
#28297=CARTESIAN_POINT('Ctrl Pts',(-33.3201698480253,31.6960093649181,2.71432904580747));
#28298=CARTESIAN_POINT('Ctrl Pts',(-32.277483075488,32.4848290257668,2.76666242159155));
#28299=CARTESIAN_POINT('Ctrl Pts',(-31.7975120187873,33.5316546471577,2.81899579737563));
#28300=CARTESIAN_POINT('Ctrl Pts',(-31.3175409620866,34.5784802685486,2.87132917315972));
#28301=CARTESIAN_POINT('Ctrl Pts',(-31.4002856212225,35.8833118504819,2.9236625489438));
#28302=CARTESIAN_POINT('Ctrl Pts',(-32.0086470268372,36.8611218995229,2.97599592472789));
#28303=CARTESIAN_POINT('Ctrl Pts',(-32.617008432452,37.8389319485639,3.02832930051197));
#28304=CARTESIAN_POINT('Ctrl Pts',(-33.7509865845457,38.4897204647128,3.08066267629606));
#28305=CARTESIAN_POINT('Ctrl Pts',(-34.902156941427,38.5217032924198,3.13299605208014));
#28306=CARTESIAN_POINT('Ctrl Pts',(-36.0533272983083,38.5536861201269,3.18532942786423));
#28307=CARTESIAN_POINT('Ctrl Pts',(-37.2216898599771,37.9668632593921,3.23766280364831));
#28308=CARTESIAN_POINT('Ctrl Pts',(-37.8834036664129,37.0243395560048,3.2899961794324));
#28309=CARTESIAN_POINT('Ctrl Pts',(-38.2940052559017,36.439491957273,3.3224696854576));
#28310=CARTESIAN_POINT('Ctrl Pts',(-38.5095290494265,35.7176868792413,3.35494319148281));
#28311=CARTESIAN_POINT('Ctrl Pts',(-38.5133643814276,34.9979909506281,3.38741669750802));
#28312=CARTESIAN_POINT('Origin',(-35.,35.,4.));
#28313=CARTESIAN_POINT('',(-38.5230459553398,34.9997936499459,4.38741669750802));
#28314=CARTESIAN_POINT('',(-38.5188569925171,35.0029051522836,4.11258330249198));
#28315=CARTESIAN_POINT('',(-38.5175,35.,4.));
#28316=CARTESIAN_POINT('Ctrl Pts',(-38.5188569925171,35.0029051522836,4.11258330249198));
#28317=CARTESIAN_POINT('Ctrl Pts',(-38.5208448945788,35.2279179383631,4.10238997204752));
#28318=CARTESIAN_POINT('Ctrl Pts',(-38.5010642738412,35.4525828200332,4.09219664160306));
#28319=CARTESIAN_POINT('Ctrl Pts',(-38.4582305083298,35.6727629510031,4.08200331115859));
#28320=CARTESIAN_POINT('Ctrl Pts',(-38.2383185218631,36.8031853970347,4.02966993537451));
#28321=CARTESIAN_POINT('Ctrl Pts',(-37.4107537806994,37.8153952892549,3.97733655959042));
#28322=CARTESIAN_POINT('Ctrl Pts',(-36.3465789061757,38.2555634668873,3.92500318380634));
#28323=CARTESIAN_POINT('Ctrl Pts',(-35.282404031652,38.6957316445196,3.87266980802226));
#28324=CARTESIAN_POINT('Ctrl Pts',(-33.9816190237685,38.5638581075641,3.82033643223817));
#28325=CARTESIAN_POINT('Ctrl Pts',(-33.0274370803658,37.9190689893243,3.76800305645409));
#28326=CARTESIAN_POINT('Ctrl Pts',(-32.0732551369631,37.2742798710845,3.71566968067));
#28327=CARTESIAN_POINT('Ctrl Pts',(-31.4656762580412,36.1165751715604,3.66333630488592));
#28328=CARTESIAN_POINT('Ctrl Pts',(-31.4771113484684,34.9650173451833,3.61100292910183));
#28329=CARTESIAN_POINT('Ctrl Pts',(-31.4885464388956,33.8134595188062,3.55866955331775));
#28330=CARTESIAN_POINT('Ctrl Pts',(-32.1189954986718,32.6680485655762,3.50633617753366));
#28331=CARTESIAN_POINT('Ctrl Pts',(-33.0857936675462,32.0423349823756,3.45400280174958));
#28332=CARTESIAN_POINT('Ctrl Pts',(-34.0525918364206,31.4166213991749,3.40166942596549));
#28333=CARTESIAN_POINT('Ctrl Pts',(-35.3557391143932,31.3106051860038,3.34933605018141));
#28334=CARTESIAN_POINT('Ctrl Pts',(-36.4109631688252,31.7718192171285,3.29700267439732));
#28335=CARTESIAN_POINT('Ctrl Pts',(-37.4661872232571,32.2330332482532,3.24466929861324));
#28336=CARTESIAN_POINT('Ctrl Pts',(-38.2734880541485,33.2614775236738,3.19233592282916));
#28337=CARTESIAN_POINT('Ctrl Pts',(-38.4709084608049,34.3960441262186,3.14000254704507));
#28338=CARTESIAN_POINT('Ctrl Pts',(-38.5053868940467,34.5941902020313,3.13086279886071));
#28339=CARTESIAN_POINT('Ctrl Pts',(-38.5212634980004,34.7955730917084,3.12172305067635));
#28340=CARTESIAN_POINT('Ctrl Pts',(-38.5195233495341,34.9972296620149,3.11258330249199));
#28341=CARTESIAN_POINT('Ctrl Pts',(-38.5133643814276,34.9979909506281,3.38741669750802));
#28342=CARTESIAN_POINT('Ctrl Pts',(-38.5157099610507,34.5578454548766,3.4072765672669));
#28343=CARTESIAN_POINT('Ctrl Pts',(-38.4388798941057,34.1184888224752,3.42713643702577));
#28344=CARTESIAN_POINT('Ctrl Pts',(-38.2790746610536,33.7117311197398,3.44699630678465));
#28345=CARTESIAN_POINT('Ctrl Pts',(-37.8579667980557,32.6398709329021,3.49932968256873));
#28346=CARTESIAN_POINT('Ctrl Pts',(-36.8606860208572,31.7943751052665,3.55166305835282));
#28347=CARTESIAN_POINT('Ctrl Pts',(-35.734367949382,31.554325747162,3.6039964341369));
#28348=CARTESIAN_POINT('Ctrl Pts',(-34.6080498779068,31.3142763890575,3.65632980992099));
#28349=CARTESIAN_POINT('Ctrl Pts',(-33.3526945121549,31.6796735004841,3.70866318570507));
#28350=CARTESIAN_POINT('Ctrl Pts',(-32.5311464521593,32.4866895335911,3.76099656148916));
#28351=CARTESIAN_POINT('Ctrl Pts',(-31.7095983921637,33.2937055666981,3.81332993727324));
#28352=CARTESIAN_POINT('Ctrl Pts',(-31.3218576379244,34.5423405214855,3.86566331305732));
#28353=CARTESIAN_POINT('Ctrl Pts',(-31.5417696164559,35.6727629267273,3.91799668884141));
#28354=CARTESIAN_POINT('Ctrl Pts',(-31.7616815949873,36.8031853319691,3.97033006462549));
#28355=CARTESIAN_POINT('Ctrl Pts',(-32.5892463062895,37.8153951876653,4.02266344040958));
#28356=CARTESIAN_POINT('Ctrl Pts',(-33.6534211424138,38.2555633494147,4.07499681619366));
#28357=CARTESIAN_POINT('Ctrl Pts',(-34.7175959785381,38.6957315111641,4.12733019197775));
#28358=CARTESIAN_POINT('Ctrl Pts',(-36.0183809394846,38.5638579789666,4.17966356776183));
#28359=CARTESIAN_POINT('Ctrl Pts',(-36.9725628484569,37.9190688839933,4.23199694354592));
#28360=CARTESIAN_POINT('Ctrl Pts',(-37.9171399008999,37.2807702775639,4.28380352819995));
#28361=CARTESIAN_POINT('Ctrl Pts',(-38.5220566388619,36.1398302190111,4.33561011285399));
#28362=CARTESIAN_POINT('Ctrl Pts',(-38.5230459553398,34.9997936499459,4.38741669750802));
#28363=CARTESIAN_POINT('Origin',(-35.,35.,4.));
#28364=CARTESIAN_POINT('',(-38.5138066110977,35.0022702462197,5.38741669750802));
#28365=CARTESIAN_POINT('',(-38.5124571785126,34.9988611669454,5.11258330249198));
#28366=CARTESIAN_POINT('',(-38.5175,35.,4.));
#28367=CARTESIAN_POINT('Ctrl Pts',(-38.5124571785126,34.9988611669454,5.11258330249198));
#28368=CARTESIAN_POINT('Ctrl Pts',(-38.5105119534794,35.6536666552656,5.08305689341869));
#28369=CARTESIAN_POINT('Ctrl Pts',(-38.3345896506072,36.3094430406945,5.0535304843454));
#28370=CARTESIAN_POINT('Ctrl Pts',(-37.9913530811025,36.8611219666803,5.02400407527211));
#28371=CARTESIAN_POINT('Ctrl Pts',(-37.3829916535365,37.8389320510055,4.97167069948803));
#28372=CARTESIAN_POINT('Ctrl Pts',(-36.2490134605232,38.4897205906347,4.91933732370395));
#28373=CARTESIAN_POINT('Ctrl Pts',(-35.0978430621031,38.5217034194952,4.86700394791986));
#28374=CARTESIAN_POINT('Ctrl Pts',(-33.946672663683,38.5536862483557,4.81467057213578));
#28375=CARTESIAN_POINT('Ctrl Pts',(-32.7783100598561,37.9668633664475,4.76233719635169));
#28376=CARTESIAN_POINT('Ctrl Pts',(-32.1165962295435,37.0243396290507,4.71000382056761));
#28377=CARTESIAN_POINT('Ctrl Pts',(-31.4548823992308,36.081815891654,4.65767044478352));
#28378=CARTESIAN_POINT('Ctrl Pts',(-31.2998173424323,34.7835912987687,4.60533706899944));
#28379=CARTESIAN_POINT('Ctrl Pts',(-31.7209252206252,33.7117310732541,4.55300369321535));
#28380=CARTESIAN_POINT('Ctrl Pts',(-32.1420330988181,32.6398708477396,4.50067031743127));
#28381=CARTESIAN_POINT('Ctrl Pts',(-33.1393139120024,31.7943749895958,4.44833694164718));
#28382=CARTESIAN_POINT('Ctrl Pts',(-34.2656320241194,31.5543256228295,4.3960035658631));
#28383=CARTESIAN_POINT('Ctrl Pts',(-35.3919501362363,31.3142762560632,4.34367019007901));
#28384=CARTESIAN_POINT('Ctrl Pts',(-36.647305547286,31.6796733806745,4.29133681429493));
#28385=CARTESIAN_POINT('Ctrl Pts',(-37.4688536369261,32.4866894429016,4.23900343851085));
#28386=CARTESIAN_POINT('Ctrl Pts',(-38.1303831719009,33.1365174530869,4.19686339317123));
#28387=CARTESIAN_POINT('Ctrl Pts',(-38.5106388460078,34.0726842535258,4.15472334783161));
#28388=CARTESIAN_POINT('Ctrl Pts',(-38.5188569925171,35.0029051522836,4.11258330249198));
#28389=CARTESIAN_POINT('Ctrl Pts',(-38.5230459553398,34.9997936499459,4.38741669750802));
#28390=CARTESIAN_POINT('Ctrl Pts',(-38.5230560151256,34.9882012788887,4.38794348863807));
#28391=CARTESIAN_POINT('Ctrl Pts',(-38.5230036307651,34.9766090012494,4.38847027976812));
#28392=CARTESIAN_POINT('Ctrl Pts',(-38.5228885244128,34.9650173464461,4.38899707089817));
#28393=CARTESIAN_POINT('Ctrl Pts',(-38.5114534343983,33.813459561621,4.44133044668225));
#28394=CARTESIAN_POINT('Ctrl Pts',(-37.881004397371,32.66804864972,4.49366382246634));
#28395=CARTESIAN_POINT('Ctrl Pts',(-36.9142062633822,32.0423350890982,4.54599719825042));
#28396=CARTESIAN_POINT('Ctrl Pts',(-35.9474081293934,31.4166215284763,4.59833057403451));
#28397=CARTESIAN_POINT('Ctrl Pts',(-34.6442608984431,31.3106053191336,4.65066394981859));
#28398=CARTESIAN_POINT('Ctrl Pts',(-33.5890368820876,31.7718193336147,4.70299732560267));
#28399=CARTESIAN_POINT('Ctrl Pts',(-32.533812865732,32.2330333480957,4.75533070138676));
#28400=CARTESIAN_POINT('Ctrl Pts',(-31.7265120639713,33.2614775864005,4.80766407717084));
#28401=CARTESIAN_POINT('Ctrl Pts',(-31.5290916644384,34.3960441480086,4.85999745295493));
#28402=CARTESIAN_POINT('Ctrl Pts',(-31.3316712649055,35.5306107096167,4.91233082873901));
#28403=CARTESIAN_POINT('Ctrl Pts',(-31.7441312676005,36.771299594528,4.9646642045231));
#28404=CARTESIAN_POINT('Ctrl Pts',(-32.5815432503882,37.5618419758867,5.01699758030718));
#28405=CARTESIAN_POINT('Ctrl Pts',(-33.418955233176,38.3523843572453,5.06933095609127));
#28406=CARTESIAN_POINT('Ctrl Pts',(-34.6813191960565,38.6927802350512,5.12166433187535));
#28407=CARTESIAN_POINT('Ctrl Pts',(-35.8026482038993,38.4304115128643,5.17399770765944));
#28408=CARTESIAN_POINT('Ctrl Pts',(-36.9239772117421,38.1680427906774,5.22633108344352));
#28409=CARTESIAN_POINT('Ctrl Pts',(-37.9042712645471,37.3029094684976,5.2786644592276));
#28410=CARTESIAN_POINT('Ctrl Pts',(-38.3040108156146,36.2228981644233,5.33099783501169));
#28411=CARTESIAN_POINT('Ctrl Pts',(-38.4476594300862,35.8347901400117,5.34980412251047));
#28412=CARTESIAN_POINT('Ctrl Pts',(-38.5163373319043,35.4189335486904,5.36861041000924));
#28413=CARTESIAN_POINT('Ctrl Pts',(-38.5138066110977,35.0022702462197,5.38741669750802));
#28414=CARTESIAN_POINT('Origin',(-35.,35.,4.));
#28415=CARTESIAN_POINT('',(-38.5163029138352,34.997016742257,6.38741669750802));
#28416=CARTESIAN_POINT('',(-38.5224238694764,34.9986908177615,6.11258330249199));
#28417=CARTESIAN_POINT('',(-38.5175,35.,4.));
#28418=CARTESIAN_POINT('Ctrl Pts',(-38.5224238694764,34.9986908177615,6.11258330249199));
#28419=CARTESIAN_POINT('Ctrl Pts',(-38.5172129982537,36.0743835623573,6.06372381478987));
#28420=CARTESIAN_POINT('Ctrl Pts',(-37.9876402962914,37.154522030678,6.01486432708775));
#28421=CARTESIAN_POINT('Ctrl Pts',(-37.1315952103829,37.8050436089632,5.96600483938563));
#28422=CARTESIAN_POINT('Ctrl Pts',(-36.2146856954469,38.5018169852953,5.91367146360155));
#28423=CARTESIAN_POINT('Ctrl Pts',(-34.9232293447652,38.705710551088,5.86133808781746));
#28424=CARTESIAN_POINT('Ctrl Pts',(-33.8362566580758,38.325307472034,5.80900471203338));
#28425=CARTESIAN_POINT('Ctrl Pts',(-32.7492839713864,37.9449043929801,5.75667133624929));
#28426=CARTESIAN_POINT('Ctrl Pts',(-31.8667949486893,36.9802046690794,5.70433796046521));
#28427=CARTESIAN_POINT('Ctrl Pts',(-31.5844578508488,35.8637361363978,5.65200458468113));
#28428=CARTESIAN_POINT('Ctrl Pts',(-31.3021207530084,34.7472676037162,5.59967120889704));
#28429=CARTESIAN_POINT('Ctrl Pts',(-31.6199355800247,33.4790302622538,5.54733783311296));
#28430=CARTESIAN_POINT('Ctrl Pts',(-32.3954084927658,32.6276443641247,5.49500445732887));
#28431=CARTESIAN_POINT('Ctrl Pts',(-33.1708814055069,31.7762584659956,5.44267108154479));
#28432=CARTESIAN_POINT('Ctrl Pts',(-34.4040124039728,31.3417240112,5.39033770576071));
#28433=CARTESIAN_POINT('Ctrl Pts',(-35.5419213082836,31.5188666284535,5.33800432997662));
#28434=CARTESIAN_POINT('Ctrl Pts',(-36.6798302125945,31.6960092457071,5.28567095419254));
#28435=CARTESIAN_POINT('Ctrl Pts',(-37.7225170227502,32.4848289350099,5.23333757840845));
#28436=CARTESIAN_POINT('Ctrl Pts',(-38.2024880967687,33.5316545941719,5.18100420262437));
#28437=CARTESIAN_POINT('Ctrl Pts',(-38.4116602387006,33.987862847563,5.15819723591357));
#28438=CARTESIAN_POINT('Ctrl Pts',(-38.5139597209473,34.4930723682773,5.13539026920278));
#28439=CARTESIAN_POINT('Ctrl Pts',(-38.5124571785126,34.9988611669454,5.11258330249198));
#28440=CARTESIAN_POINT('Ctrl Pts',(-38.5138066110977,35.0022702462197,5.38741669750802));
#28441=CARTESIAN_POINT('Ctrl Pts',(-38.5092949444589,34.2594597724306,5.42094378579333));
#28442=CARTESIAN_POINT('Ctrl Pts',(-38.2784657870358,33.5140853838181,5.45447087407863));
#28443=CARTESIAN_POINT('Ctrl Pts',(-37.8426352258847,32.9188002435034,5.48799796236394));
#28444=CARTESIAN_POINT('Ctrl Pts',(-37.1623350357574,31.9896029126267,5.54033133814803));
#28445=CARTESIAN_POINT('Ctrl Pts',(-35.9825496061728,31.4260975368425,5.59266471393211));
#28446=CARTESIAN_POINT('Ctrl Pts',(-34.8322413698574,31.4809342241349,5.6449980897162));
#28447=CARTESIAN_POINT('Ctrl Pts',(-33.681933133542,31.5357709114273,5.69733146550028));
#28448=CARTESIAN_POINT('Ctrl Pts',(-32.5611020904959,32.2089496617965,5.74966484128436));
#28449=CARTESIAN_POINT('Ctrl Pts',(-31.9722782631938,33.1986480172104,5.80199821706845));
#28450=CARTESIAN_POINT('Ctrl Pts',(-31.3834544358917,34.1883463726244,5.85433159285253));
#28451=CARTESIAN_POINT('Ctrl Pts',(-31.3266378243335,35.4945643330831,5.90666496863662));
#28452=CARTESIAN_POINT('Ctrl Pts',(-31.8273023322845,36.531651876217,5.95899834442071));
#28453=CARTESIAN_POINT('Ctrl Pts',(-32.3279668402356,37.5687394193509,6.01133172020479));
#28454=CARTESIAN_POINT('Ctrl Pts',(-33.3861124676959,38.3366965451598,6.06366509598887));
#28455=CARTESIAN_POINT('Ctrl Pts',(-34.5273147413959,38.4912078741205,6.11599847177296));
#28456=CARTESIAN_POINT('Ctrl Pts',(-35.668517015096,38.6457192030811,6.16833184755704));
#28457=CARTESIAN_POINT('Ctrl Pts',(-36.8927759350357,38.1867847351935,6.22066522334113));
#28458=CARTESIAN_POINT('Ctrl Pts',(-37.6511887502036,37.3201661507465,6.27299859912521));
#28459=CARTESIAN_POINT('Ctrl Pts',(-38.2039026464539,36.688594367157,6.31113796525282));
#28460=CARTESIAN_POINT('Ctrl Pts',(-38.5091981905113,35.8404949979527,6.34927733138042));
#28461=CARTESIAN_POINT('Ctrl Pts',(-38.5163029138352,34.997016742257,6.38741669750802));
#28462=CARTESIAN_POINT('Origin',(-35.,35.,4.));
#28463=CARTESIAN_POINT('',(-38.521739013009,35.0017650567249,7.38741669750802));
#28464=CARTESIAN_POINT('',(-38.5153120432796,35.002811202661,7.11258330249199));
#28465=CARTESIAN_POINT('',(-38.5175,35.,4.));
#28466=CARTESIAN_POINT('',(-32.3264680662287,37.2858331630075,8.));
#28467=CARTESIAN_POINT('Ctrl Pts',(-38.521739013009,35.0017650567249,7.38741669750802));
#28468=CARTESIAN_POINT('Ctrl Pts',(-38.515045138314,33.9623979425516,7.43461100431976));
#28469=CARTESIAN_POINT('Ctrl Pts',(-38.025374647688,32.917767542155,7.4818053111315));
#28470=CARTESIAN_POINT('Ctrl Pts',(-37.2186053621485,32.2635140899837,7.52899961794324));
#28471=CARTESIAN_POINT('Ctrl Pts',(-36.3239855860891,31.5380178578407,7.58133299372732));
#28472=CARTESIAN_POINT('Ctrl Pts',(-35.039448183402,31.2925450618756,7.63366636951141));
#28473=CARTESIAN_POINT('Ctrl Pts',(-33.9411232613757,31.6392615106971,7.68599974529549));
#28474=CARTESIAN_POINT('Ctrl Pts',(-32.8427983393495,31.9859779595187,7.73833312107958));
#28475=CARTESIAN_POINT('Ctrl Pts',(-31.9306858979841,32.9248836531268,7.79066649686366));
#28476=CARTESIAN_POINT('Ctrl Pts',(-31.6136962443577,34.0300695623378,7.84299987264775));
#28477=CARTESIAN_POINT('Ctrl Pts',(-31.2967065907312,35.1352554715487,7.89533324843183));
#28478=CARTESIAN_POINT('Ctrl Pts',(-31.5748397248436,36.4067215963625,7.94766662421592));
#28479=CARTESIAN_POINT('Ctrl Pts',(-32.3264680662287,37.2858331630075,8.));
#28480=CARTESIAN_POINT('',(-37.6785007864356,37.2890249916441,8.));
#28481=CARTESIAN_POINT('Origin',(-35.,35.,8.));
#28482=CARTESIAN_POINT('Ctrl Pts',(-37.6785239274887,37.2890398567007,8.));
#28483=CARTESIAN_POINT('Ctrl Pts',(-36.9607510630042,38.1233253004298,7.95000212253756));
#28484=CARTESIAN_POINT('Ctrl Pts',(-35.8186698457281,38.5989197552422,7.90000424507511));
#28485=CARTESIAN_POINT('Ctrl Pts',(-34.7217022012346,38.5118537728532,7.85000636761267));
#28486=CARTESIAN_POINT('Ctrl Pts',(-33.5734930596489,38.4207207687012,7.79767299182859));
#28487=CARTESIAN_POINT('Ctrl Pts',(-32.4747106147993,37.7131336670436,7.7453396160445));
#28488=CARTESIAN_POINT('Ctrl Pts',(-31.9173295125726,36.7055536114064,7.69300624026042));
#28489=CARTESIAN_POINT('Ctrl Pts',(-31.3599484103458,35.6979735557692,7.64067286447633));
#28490=CARTESIAN_POINT('Ctrl Pts',(-31.3439686507417,34.3904005461523,7.58833948869225));
#28491=CARTESIAN_POINT('Ctrl Pts',(-31.8768870047646,33.3694814192899,7.53600611290817));
#28492=CARTESIAN_POINT('Ctrl Pts',(-32.4098053587874,32.3485622924274,7.48367273712408));
#28493=CARTESIAN_POINT('Ctrl Pts',(-33.4916218264372,31.6142970483194,7.43133936134));
#28494=CARTESIAN_POINT('Ctrl Pts',(-34.6371339251584,31.4957034085517,7.37900598555591));
#28495=CARTESIAN_POINT('Ctrl Pts',(-35.7826460238797,31.3771097687841,7.32667260977183));
#28496=CARTESIAN_POINT('Ctrl Pts',(-36.9918537536724,31.8741877333568,7.27433923398774));
#28497=CARTESIAN_POINT('Ctrl Pts',(-37.7226848809369,32.7641661288242,7.22200585820366));
#28498=CARTESIAN_POINT('Ctrl Pts',(-38.232043765465,33.3844440368906,7.18553167296644));
#28499=CARTESIAN_POINT('Ctrl Pts',(-38.5090307393652,34.1955737201714,7.14905748772921));
#28500=CARTESIAN_POINT('Ctrl Pts',(-38.5153120432796,35.002811202661,7.11258330249199));
#28501=CARTESIAN_POINT('Origin',(-35.,-35.,4.));
#28502=CARTESIAN_POINT('',(-38.5120271382808,-35.0001374244476,0.387416697508025));
#28503=CARTESIAN_POINT('',(-38.5151976130935,-35.0046525930694,0.112583302491978));
#28504=CARTESIAN_POINT('',(-38.5175,-35.,4.));
#28505=CARTESIAN_POINT('',(-37.6735319337713,-32.7141668369925,0.));
#28506=CARTESIAN_POINT('Ctrl Pts',(-38.5151976130935,-35.0046525930694,
0.112583302491978));
#28507=CARTESIAN_POINT('Ctrl Pts',(-38.5080219923978,-34.1767290340604,
0.075055534994651));
#28508=CARTESIAN_POINT('Ctrl Pts',(-38.2125174896864,-33.3445694048179,
0.0375277674973242));
#28509=CARTESIAN_POINT('Ctrl Pts',(-37.6735319337713,-32.7141668369925,
-2.28983498828939E-15));
#28510=CARTESIAN_POINT('',(-32.3214990837181,-32.7109751024398,8.09549783939668E-17));
#28511=CARTESIAN_POINT('Origin',(-35.,-35.,0.));
#28512=CARTESIAN_POINT('Ctrl Pts',(-32.3214759334524,-32.7109602322923,
3.12480707463443E-17));
#28513=CARTESIAN_POINT('Ctrl Pts',(-33.0392487617403,-31.8766749582113,
0.0499978774624439));
#28514=CARTESIAN_POINT('Ctrl Pts',(-34.1813300785248,-31.4010800346315,
0.099995754924887));
#28515=CARTESIAN_POINT('Ctrl Pts',(-35.2782977997678,-31.4881459202074,
0.149993632387331));
#28516=CARTESIAN_POINT('Ctrl Pts',(-36.4265070216881,-31.5792788230239,
0.202327008171415));
#28517=CARTESIAN_POINT('Ctrl Pts',(-37.5252895219377,-32.2868662308611,
0.254660383955499));
#28518=CARTESIAN_POINT('Ctrl Pts',(-38.0826706431354,-33.2944463926721,
0.306993759739583));
#28519=CARTESIAN_POINT('Ctrl Pts',(-38.3681877823846,-33.8105769080839,
0.333801405662397));
#28520=CARTESIAN_POINT('Ctrl Pts',(-38.5116424994856,-34.4054248019609,
0.360609051585211));
#28521=CARTESIAN_POINT('Ctrl Pts',(-38.5120271382808,-35.0001374244476,
0.387416697508025));
#28522=CARTESIAN_POINT('Origin',(-35.,-35.,4.));
#28523=CARTESIAN_POINT('',(-38.5212304296149,-35.0021519659852,1.38741669750803));
#28524=CARTESIAN_POINT('',(-38.5220168341852,-34.9983176676613,1.11258330249198));
#28525=CARTESIAN_POINT('',(-38.5175,-35.,4.));
#28526=CARTESIAN_POINT('Ctrl Pts',(-38.5220168341852,-34.9983176676613,
1.11258330249198));
#28527=CARTESIAN_POINT('Ctrl Pts',(-38.52260684792,-34.8986110126186,1.10805583214991));
#28528=CARTESIAN_POINT('Ctrl Pts',(-38.5187311767415,-34.7989511930367,
1.10352836180784));
#28529=CARTESIAN_POINT('Ctrl Pts',(-38.5102392653976,-34.699686678491,1.09900089146577));
#28530=CARTESIAN_POINT('Ctrl Pts',(-38.4120806130139,-33.5522805666331,
1.04666751568169));
#28531=CARTESIAN_POINT('Ctrl Pts',(-37.6971357336766,-32.4576920494149,
0.994334139897603));
#28532=CARTESIAN_POINT('Ctrl Pts',(-36.6859405355102,-31.906559687218,0.942000764113519));
#28533=CARTESIAN_POINT('Ctrl Pts',(-35.6747453373438,-31.355427325021,0.889667388329434));
#28534=CARTESIAN_POINT('Ctrl Pts',(-34.3672998203483,-31.3477511178455,
0.83733401254535));
#28535=CARTESIAN_POINT('Ctrl Pts',(-33.3498297550083,-31.8872254772169,
0.785000636761265));
#28536=CARTESIAN_POINT('Ctrl Pts',(-32.3323596896683,-32.4266998365882,
0.732667260977181));
#28537=CARTESIAN_POINT('Ctrl Pts',(-31.6048650759839,-33.5133247625066,
0.680333885193095));
#28538=CARTESIAN_POINT('Ctrl Pts',(-31.4934686932928,-34.6593973938948,
0.628000509409011));
#28539=CARTESIAN_POINT('Ctrl Pts',(-31.3820723106017,-35.8054700252831,
0.575667133624927));
#28540=CARTESIAN_POINT('Ctrl Pts',(-31.8867741589039,-37.0109903621411,
0.523333757840844));
#28541=CARTESIAN_POINT('Ctrl Pts',(-32.7813942262272,-37.7364865047087,
0.47100038205676));
#28542=CARTESIAN_POINT('Ctrl Pts',(-33.6760142935505,-38.4619826472763,
0.418667006272675));
#28543=CARTESIAN_POINT('Ctrl Pts',(-34.9605525798949,-38.7074545955534,
0.366333630488589));
#28544=CARTESIAN_POINT('Ctrl Pts',(-36.0588770784695,-38.3607385484851,
0.314000254704505));
#28545=CARTESIAN_POINT('Ctrl Pts',(-37.157201577044,-38.0140225014167,0.26166687892042));
#28546=CARTESIAN_POINT('Ctrl Pts',(-38.0693122878488,-37.0751184590028,
0.209333503136336));
#28547=CARTESIAN_POINT('Ctrl Pts',(-38.3863019623769,-35.9699324345579,
0.157000127352251));
#28548=CARTESIAN_POINT('Ctrl Pts',(-38.4759813473142,-35.6572648277626,
0.142194519065493));
#28549=CARTESIAN_POINT('Ctrl Pts',(-38.518028568312,-35.3312883810079,0.127388910778735));
#28550=CARTESIAN_POINT('Ctrl Pts',(-38.5151976130935,-35.0046525930694,
0.112583302491978));
#28551=CARTESIAN_POINT('Ctrl Pts',(-38.5120271382808,-35.0001374244476,
0.387416697508025));
#28552=CARTESIAN_POINT('Ctrl Pts',(-38.5123933840156,-35.5664114565052,
0.412942427369296));
#28553=CARTESIAN_POINT('Ctrl Pts',(-38.3830453480461,-36.1325628449505,
0.438468157230567));
#28554=CARTESIAN_POINT('Ctrl Pts',(-38.1231131273625,-36.6305186098067,
0.463993887091838));
#28555=CARTESIAN_POINT('Ctrl Pts',(-37.5901947482463,-37.6514377493457,
0.516327262875923));
#28556=CARTESIAN_POINT('Ctrl Pts',(-36.5083782478681,-38.3857031126391,
0.568660638660007));
#28557=CARTESIAN_POINT('Ctrl Pts',(-35.362866098922,-38.5042967770896,0.620994014444091));
#28558=CARTESIAN_POINT('Ctrl Pts',(-34.2173539499758,-38.6228904415402,
0.673327390228176));
#28559=CARTESIAN_POINT('Ctrl Pts',(-33.0081461524618,-38.1258124071479,
0.72566076601226));
#28560=CARTESIAN_POINT('Ctrl Pts',(-32.2773149895643,-37.2358339601687,
0.777994141796345));
#28561=CARTESIAN_POINT('Ctrl Pts',(-31.5464838266669,-36.3458555131895,
0.83032751758043));
#28562=CARTESIAN_POINT('Ctrl Pts',(-31.294029298386,-35.0629766536234,0.882660893364515));
#28563=CARTESIAN_POINT('Ctrl Pts',(-31.6331812255463,-33.9624299433603,
0.934994269148599));
#28564=CARTESIAN_POINT('Ctrl Pts',(-31.9723331527066,-32.8618832330971,
0.987327644932684));
#28565=CARTESIAN_POINT('Ctrl Pts',(-32.9030915353081,-31.9436686721369,
1.03966102071677));
#28566=CARTESIAN_POINT('Ctrl Pts',(-34.0081262229406,-31.6194484991129,
1.09199439650085));
#28567=CARTESIAN_POINT('Ctrl Pts',(-35.1131609105731,-31.2952283260889,
1.14432777228494));
#28568=CARTESIAN_POINT('Ctrl Pts',(-36.3924719032364,-31.5650025410011,
1.19666114806902));
#28569=CARTESIAN_POINT('Ctrl Pts',(-37.2724839907223,-32.3078283275476,
1.24899452385311));
#28570=CARTESIAN_POINT('Ctrl Pts',(-38.0483635269158,-32.9627549301865,
1.29513524840475));
#28571=CARTESIAN_POINT('Ctrl Pts',(-38.5138518348506,-33.9854036989656,
1.34127597295639));
#28572=CARTESIAN_POINT('Ctrl Pts',(-38.5212304296149,-35.0021519659852,
1.38741669750803));
#28573=CARTESIAN_POINT('Origin',(-35.,-35.,4.));
#28574=CARTESIAN_POINT('',(-38.5169621951111,-34.9969726963287,2.38741669750803));
#28575=CARTESIAN_POINT('',(-38.5122617995812,-34.9992080290324,2.11258330249198));
#28576=CARTESIAN_POINT('',(-38.5175,-35.,4.));
#28577=CARTESIAN_POINT('Ctrl Pts',(-38.5122617995812,-34.9992080290324,
2.11258330249198));
#28578=CARTESIAN_POINT('Ctrl Pts',(-38.5133509957446,-34.4699799892041,
2.08872275352108));
#28579=CARTESIAN_POINT('Ctrl Pts',(-38.4009678500058,-33.9411911577145,
2.06486220455019));
#28580=CARTESIAN_POINT('Ctrl Pts',(-38.1726980103725,-33.4683479591114,
2.04100165557929));
#28581=CARTESIAN_POINT('Ctrl Pts',(-37.6720334484517,-32.4312603032644,
1.98866827979521));
#28582=CARTESIAN_POINT('Ctrl Pts',(-36.613887707127,-31.6633030916115,1.93633490401112));
#28583=CARTESIAN_POINT('Ctrl Pts',(-35.4726853098873,-31.5087917472057,
1.88400152822704));
#28584=CARTESIAN_POINT('Ctrl Pts',(-34.3314829126475,-31.3542804028,1.83166815244296));
#28585=CARTESIAN_POINT('Ctrl Pts',(-33.1072238594927,-31.8132149256414,
1.77933477665887));
#28586=CARTESIAN_POINT('Ctrl Pts',(-32.3488109629184,-32.6798336014156,
1.72700140087479));
#28587=CARTESIAN_POINT('Ctrl Pts',(-31.5903980663441,-33.5464522771898,
1.6746680250907));
#28588=CARTESIAN_POINT('Ctrl Pts',(-31.2978313263503,-34.8207551058968,
1.62233464930662));
#28589=CARTESIAN_POINT('Ctrl Pts',(-31.602283651433,-35.931394685751,1.57000127352253));
#28590=CARTESIAN_POINT('Ctrl Pts',(-31.9067359765157,-37.0420342656052,
1.51766789773845));
#28591=CARTESIAN_POINT('Ctrl Pts',(-32.808207366675,-37.9890105966065,1.46533452195436));
#28592=CARTESIAN_POINT('Ctrl Pts',(-33.9025203970559,-38.3477576413965,
1.41300114617028));
#28593=CARTESIAN_POINT('Ctrl Pts',(-34.9968334274368,-38.7065046861866,
1.36066777038619));
#28594=CARTESIAN_POINT('Ctrl Pts',(-36.2839880980393,-38.4770224447653,
1.30833439460211));
#28595=CARTESIAN_POINT('Ctrl Pts',(-37.1868792206255,-37.7621694708059,
1.25600101881803));
#28596=CARTESIAN_POINT('Ctrl Pts',(-38.0116593343501,-37.1091599302205,
1.20819511337601));
#28597=CARTESIAN_POINT('Ctrl Pts',(-38.515786834056,-36.0511278602802,1.16038920793399));
#28598=CARTESIAN_POINT('Ctrl Pts',(-38.5220168341852,-34.9983176676613,
1.11258330249198));
#28599=CARTESIAN_POINT('Ctrl Pts',(-38.5212304296149,-35.0021519659852,
1.38741669750803));
#28600=CARTESIAN_POINT('Ctrl Pts',(-38.5222207275437,-35.1386120556355,
1.39360934874047));
#28601=CARTESIAN_POINT('Ctrl Pts',(-38.5149591261082,-35.2749658599455,
1.39980199997291));
#28602=CARTESIAN_POINT('Ctrl Pts',(-38.4990885075235,-35.4103101250027,
1.40599465120536));
#28603=CARTESIAN_POINT('Ctrl Pts',(-38.3649677545306,-36.5540887777307,
1.45832802698944));
#28604=CARTESIAN_POINT('Ctrl Pts',(-37.6160130662365,-37.6257687250057,
1.51066140277353));
#28605=CARTESIAN_POINT('Ctrl Pts',(-36.5880243363171,-38.1448600164999,
1.56299477855761));
#28606=CARTESIAN_POINT('Ctrl Pts',(-35.5600356063977,-38.6639513079941,
1.6153281543417));
#28607=CARTESIAN_POINT('Ctrl Pts',(-34.2530128348529,-38.6304539437074,
1.66766153012578));
#28608=CARTESIAN_POINT('Ctrl Pts',(-33.2529647263785,-38.059385190685,1.71999490590987));
#28609=CARTESIAN_POINT('Ctrl Pts',(-32.2529166179041,-37.4883164376626,
1.77232828169395));
#28610=CARTESIAN_POINT('Ctrl Pts',(-31.5598431725,-36.3796762959045,1.82466165747803));
#28611=CARTESIAN_POINT('Ctrl Pts',(-31.4844878017471,-35.2305296041615,
1.87699503326212));
#28612=CARTESIAN_POINT('Ctrl Pts',(-31.4091324309942,-34.0813829124186,
1.9293284090462));
#28613=CARTESIAN_POINT('Ctrl Pts',(-31.9514951348924,-32.8917296706907,
1.98166178483029));
#28614=CARTESIAN_POINT('Ctrl Pts',(-32.8684046918336,-32.1949562623368,
2.03399516061437));
#28615=CARTESIAN_POINT('Ctrl Pts',(-33.7853142487749,-31.4981828539828,
2.08632853639846));
#28616=CARTESIAN_POINT('Ctrl Pts',(-35.0767706587592,-31.2942892790027,
2.13866191218254));
#28617=CARTESIAN_POINT('Ctrl Pts',(-36.1637433953085,-31.6746923755375,
2.19099528796663));
#28618=CARTESIAN_POINT('Ctrl Pts',(-37.2507161318578,-32.0550954720723,
2.24332866375071));
#28619=CARTESIAN_POINT('Ctrl Pts',(-38.1332051949721,-33.019795240122,2.29566203953479));
#28620=CARTESIAN_POINT('Ctrl Pts',(-38.4155423057474,-34.1362638239756,
2.34799541531888));
#28621=CARTESIAN_POINT('Ctrl Pts',(-38.4864345470726,-34.416598775556,2.36113584271526));
#28622=CARTESIAN_POINT('Ctrl Pts',(-38.519489264757,-34.7065022308021,2.37427627011164));
#28623=CARTESIAN_POINT('Ctrl Pts',(-38.5169621951111,-34.9969726963287,
2.38741669750803));
#28624=CARTESIAN_POINT('Origin',(-35.,-35.,4.));
#28625=CARTESIAN_POINT('',(-38.5133646692972,-35.0020090495363,3.38741669750803));
#28626=CARTESIAN_POINT('',(-38.5195236027652,-35.0027703381826,3.11258330249198));
#28627=CARTESIAN_POINT('',(-38.5175,-35.,4.));
#28628=CARTESIAN_POINT('Ctrl Pts',(-38.5195236027652,-35.0027703381826,
3.11258330249198));
#28629=CARTESIAN_POINT('Ctrl Pts',(-38.5112998170852,-34.0497594617567,
3.06938967489226));
#28630=CARTESIAN_POINT('Ctrl Pts',(-38.1096194803006,-33.0906361399806,
3.02619604729253));
#28631=CARTESIAN_POINT('Ctrl Pts',(-37.4184570108864,-32.4381577473637,
2.98300241969281));
#28632=CARTESIAN_POINT('Ctrl Pts',(-36.5810449376309,-31.6476152805848,
2.93066904390873));
#28633=CARTESIAN_POINT('Ctrl Pts',(-35.3186808383768,-31.3072193659425,
2.87833566812464));
#28634=CARTESIAN_POINT('Ctrl Pts',(-34.1973517093896,-31.5695881165025,
2.82600229234056));
#28635=CARTESIAN_POINT('Ctrl Pts',(-33.0760225804023,-31.8319568670625,
2.77366891655648));
#28636=CARTESIAN_POINT('Ctrl Pts',(-32.0957284216819,-32.6970902828246,
2.72133554077239));
#28637=CARTESIAN_POINT('Ctrl Pts',(-31.6959888274348,-33.7771017035233,
2.66900216498831));
#28638=CARTESIAN_POINT('Ctrl Pts',(-31.2962492331877,-34.8571131242219,
2.61666878920422));
#28639=CARTESIAN_POINT('Ctrl Pts',(-31.477064203414,-36.1520025498569,2.56433541342014));
#28640=CARTESIAN_POINT('Ctrl Pts',(-32.1573644670244,-37.0811999812203,
2.51200203763605));
#28641=CARTESIAN_POINT('Ctrl Pts',(-32.8376647306348,-38.0103974125836,
2.45966866185197));
#28642=CARTESIAN_POINT('Ctrl Pts',(-34.0174502876292,-38.5739028496752,
2.40733528606788));
#28643=CARTESIAN_POINT('Ctrl Pts',(-35.1677586482437,-38.5190661562666,
2.3550019102838));
#28644=CARTESIAN_POINT('Ctrl Pts',(-36.3180670088582,-38.4642294628581,
2.30266853449971));
#28645=CARTESIAN_POINT('Ctrl Pts',(-37.4388981730927,-37.7910506389493,
2.25033515871563));
#28646=CARTESIAN_POINT('Ctrl Pts',(-38.0277220639514,-36.8013521769744,
2.19800178293155));
#28647=CARTESIAN_POINT('Ctrl Pts',(-38.3480813072967,-36.2628905837198,
2.16952895611836));
#28648=CARTESIAN_POINT('Ctrl Pts',(-38.5109620602598,-35.6307365970085,
2.14105612930517));
#28649=CARTESIAN_POINT('Ctrl Pts',(-38.5122617995812,-34.9992080290324,
2.11258330249198));
#28650=CARTESIAN_POINT('Ctrl Pts',(-38.5169621951111,-34.9969726963287,
2.38741669750803));
#28651=CARTESIAN_POINT('Ctrl Pts',(-38.5094248976387,-35.8633367513267,
2.42660964589573));
#28652=CARTESIAN_POINT('Ctrl Pts',(-38.1853504786061,-36.7347449543441,
2.46580259428343));
#28653=CARTESIAN_POINT('Ctrl Pts',(-37.6045916266667,-37.3723557446642,
2.50499554267113));
#28654=CARTESIAN_POINT('Ctrl Pts',(-36.8291186783745,-38.2237416818415,
2.55732891845522));
#28655=CARTESIAN_POINT('Ctrl Pts',(-35.5959876233539,-38.6582761565386,
2.6096622942393));
#28656=CARTESIAN_POINT('Ctrl Pts',(-34.4580786668646,-38.4811335311572,
2.66199567002338));
#28657=CARTESIAN_POINT('Ctrl Pts',(-33.3201697103753,-38.3039909057758,
2.71432904580747));
#28658=CARTESIAN_POINT('Ctrl Pts',(-32.2774828524173,-37.5151711803159,
2.76666242159156));
#28659=CARTESIAN_POINT('Ctrl Pts',(-31.7975117563928,-36.4683454731577,
2.81899579737564));
#28660=CARTESIAN_POINT('Ctrl Pts',(-31.3175406603683,-35.4215197659996,
2.87132917315973));
#28661=CARTESIAN_POINT('Ctrl Pts',(-31.4002853262773,-34.1166880771431,
2.92366254894381));
#28662=CARTESIAN_POINT('Ctrl Pts',(-32.008646781737,-33.138877947982,2.97599592472789));
#28663=CARTESIAN_POINT('Ctrl Pts',(-32.6170082371967,-32.1610678188208,
3.02832930051198));
#28664=CARTESIAN_POINT('Ctrl Pts',(-33.7509864822071,-31.5102792493549,
3.08066267629606));
#28665=CARTESIAN_POINT('Ctrl Pts',(-34.9021569334111,-31.4782964190287,
3.13299605208015));
#28666=CARTESIAN_POINT('Ctrl Pts',(-36.0533273846151,-31.4463135887025,
3.18532942786423));
#28667=CARTESIAN_POINT('Ctrl Pts',(-37.2216900420126,-32.033136497516,3.23766280364832));
#28668=CARTESIAN_POINT('Ctrl Pts',(-37.883403902666,-32.9756602781289,3.2899961794324));
#28669=CARTESIAN_POINT('Ctrl Pts',(-38.2940055257973,-33.5605079247801,
3.32246968545761));
#28670=CARTESIAN_POINT('Ctrl Pts',(-38.5095293369816,-34.2823130619538,
3.35494319148282));
#28671=CARTESIAN_POINT('Ctrl Pts',(-38.5133646692972,-35.0020090495363,
3.38741669750803));
#28672=CARTESIAN_POINT('Origin',(-35.,-35.,4.));
#28673=CARTESIAN_POINT('',(-38.5230462440028,-35.0002063500719,4.38741669750802));
#28674=CARTESIAN_POINT('',(-38.5188572457002,-34.9970948475072,4.11258330249198));
#28675=CARTESIAN_POINT('',(-38.5175,-35.,4.));
#28676=CARTESIAN_POINT('Ctrl Pts',(-38.5188572457002,-34.9970948475072,
4.11258330249198));
#28677=CARTESIAN_POINT('Ctrl Pts',(-38.5208451479049,-34.772082045238,4.10238997204752));
#28678=CARTESIAN_POINT('Ctrl Pts',(-38.5010645257441,-34.5474171474031,
4.09219664160305));
#28679=CARTESIAN_POINT('Ctrl Pts',(-38.4582307571508,-34.3272370005912,
4.08200331115859));
#28680=CARTESIAN_POINT('Ctrl Pts',(-38.2383187548614,-33.1968144732253,
4.0296699353745));
#28681=CARTESIAN_POINT('Ctrl Pts',(-37.410753954154,-32.1846045081767,3.97733655959042));
#28682=CARTESIAN_POINT('Ctrl Pts',(-36.3465790030625,-31.7444362988739,
3.92500318380633));
#28683=CARTESIAN_POINT('Ctrl Pts',(-35.2824040519711,-31.3042680895711,
3.87266980802225));
#28684=CARTESIAN_POINT('Ctrl Pts',(-33.9816189504956,-31.4361416360142,
3.82033643223816));
#28685=CARTESIAN_POINT('Ctrl Pts',(-33.0274369384391,-32.0809308006472,
3.76800305645408));
#28686=CARTESIAN_POINT('Ctrl Pts',(-32.0732549263827,-32.7257199652802,
3.71566968067));
#28687=CARTESIAN_POINT('Ctrl Pts',(-31.4656760037452,-33.8834247481031,
3.66333630488591));
#28688=CARTESIAN_POINT('Ctrl Pts',(-31.4771110949952,-35.0349826573345,
3.61100292910183));
#28689=CARTESIAN_POINT('Ctrl Pts',(-31.4885461862452,-36.1865405665659,
3.55866955331774));
#28690=CARTESIAN_POINT('Ctrl Pts',(-32.1189952913826,-37.3319516022057,
3.50633617753366));
#28691=CARTESIAN_POINT('Ctrl Pts',(-33.0857935298184,-37.957665230428,3.45400280174958));
#28692=CARTESIAN_POINT('Ctrl Pts',(-34.0525917682542,-38.5833788586504,
3.40166942596549));
#28693=CARTESIAN_POINT('Ctrl Pts',(-35.3557391399884,-38.6893950794552,
3.3493360501814));
#28694=CARTESIAN_POINT('Ctrl Pts',(-36.4109632703443,-38.2281810151433,
3.29700267439732));
#28695=CARTESIAN_POINT('Ctrl Pts',(-37.4661874007003,-37.7669669508313,
3.24466929861323));
#28696=CARTESIAN_POINT('Ctrl Pts',(-38.273488289678,-36.7385226014027,3.19233592282915));
#28697=CARTESIAN_POINT('Ctrl Pts',(-38.4709087105384,-35.6039559172305,
3.14000254704507));
#28698=CARTESIAN_POINT('Ctrl Pts',(-38.5053871462609,-35.4058098271621,
3.1308627988607));
#28699=CARTESIAN_POINT('Ctrl Pts',(-38.5212637513569,-35.2044269229967,
3.12172305067634));
#28700=CARTESIAN_POINT('Ctrl Pts',(-38.5195236027652,-35.0027703381826,
3.11258330249198));
#28701=CARTESIAN_POINT('Ctrl Pts',(-38.5133646692972,-35.0020090495363,
3.38741669750803));
#28702=CARTESIAN_POINT('Ctrl Pts',(-38.5157102491126,-35.4421545813516,
3.4072765672669));
#28703=CARTESIAN_POINT('Ctrl Pts',(-38.4388801758726,-35.8815112497523,
3.42713643702578));
#28704=CARTESIAN_POINT('Ctrl Pts',(-38.2790749297269,-36.2882689858157,
3.44699630678465));
#28705=CARTESIAN_POINT('Ctrl Pts',(-37.8579670322255,-37.3601292604774,
3.49932968256874));
#28706=CARTESIAN_POINT('Ctrl Pts',(-36.8606861733137,-38.2056251573884,
3.55166305835282));
#28707=CARTESIAN_POINT('Ctrl Pts',(-35.7343680095528,-38.4456745351613,
3.60399643413691));
#28708=CARTESIAN_POINT('Ctrl Pts',(-34.6080498457918,-38.6857239129342,
3.65632980992099));
#28709=CARTESIAN_POINT('Ctrl Pts',(-33.3526943771818,-38.3203267715691,
3.70866318570508));
#28710=CARTESIAN_POINT('Ctrl Pts',(-32.5311462498722,-37.5133106723387,
3.76099656148916));
#28711=CARTESIAN_POINT('Ctrl Pts',(-31.7095981225626,-36.7062945731084,
3.81332993727325));
#28712=CARTESIAN_POINT('Ctrl Pts',(-31.3218573365535,-35.4576595160129,
3.86566331305733));
#28713=CARTESIAN_POINT('Ctrl Pts',(-31.5417693331035,-34.3272370181493,
3.91799668884141));
#28714=CARTESIAN_POINT('Ctrl Pts',(-31.7616813296536,-33.1968145202857,
3.9703300646255));
#28715=CARTESIAN_POINT('Ctrl Pts',(-32.5892461087628,-32.184604581654,4.02266344040958));
#28716=CARTESIAN_POINT('Ctrl Pts',(-33.653421032081,-31.7444363838389,4.07499681619367));
#28717=CARTESIAN_POINT('Ctrl Pts',(-34.7175959553992,-31.3042681860239,
4.12733019197775));
#28718=CARTESIAN_POINT('Ctrl Pts',(-36.0183810229263,-31.4361417290255,
4.17966356776184));
#28719=CARTESIAN_POINT('Ctrl Pts',(-36.9725630100801,-32.0809308768304,
4.23199694354592));
#28720=CARTESIAN_POINT('Ctrl Pts',(-37.9171401399176,-32.7192295355597,
4.28380352819995));
#28721=CARTESIAN_POINT('Ctrl Pts',(-38.5220569274439,-33.8601696875978,
4.33561011285399));
#28722=CARTESIAN_POINT('Ctrl Pts',(-38.5230462440028,-35.0002063500719,
4.38741669750802));
#28723=CARTESIAN_POINT('Origin',(-35.,-35.,4.));
#28724=CARTESIAN_POINT('',(-38.5138068989996,-34.9977297535637,5.38741669750802));
#28725=CARTESIAN_POINT('',(-38.5124574312326,-35.001138833141,5.11258330249198));
#28726=CARTESIAN_POINT('',(-38.5175,-35.,4.));
#28727=CARTESIAN_POINT('Ctrl Pts',(-38.5124574312326,-35.001138833141,5.11258330249198));
#28728=CARTESIAN_POINT('Ctrl Pts',(-38.5105122060607,-34.3463332977053,
5.08305689341869));
#28729=CARTESIAN_POINT('Ctrl Pts',(-38.3345898905329,-33.6905568650893,
5.0535304843454));
#28730=CARTESIAN_POINT('Ctrl Pts',(-37.9913532963331,-33.1388778994087,
5.02400407527211));
#28731=CARTESIAN_POINT('Ctrl Pts',(-37.3829918249966,-32.1610677447274,
4.97167069948802));
#28732=CARTESIAN_POINT('Ctrl Pts',(-36.2490135503901,-31.5102791582787,
4.91933732370394));
#28733=CARTESIAN_POINT('Ctrl Pts',(-35.0978430691422,-31.4782963271182,
4.86700394791986));
#28734=CARTESIAN_POINT('Ctrl Pts',(-33.9466725878942,-31.4463134959578,
4.81467057213577));
#28735=CARTESIAN_POINT('Ctrl Pts',(-32.7783099000047,-32.0331364200855,
4.76233719635169));
#28736=CARTESIAN_POINT('Ctrl Pts',(-32.1165960220819,-32.9756602252966,
4.7100038205676));
#28737=CARTESIAN_POINT('Ctrl Pts',(-31.454882144159,-33.9181840305077,4.65767044478352));
#28738=CARTESIAN_POINT('Ctrl Pts',(-31.2998170762027,-35.216408716802,4.60533706899943));
#28739=CARTESIAN_POINT('Ctrl Pts',(-31.7209249846943,-36.2882690194377,
4.55300369321535));
#28740=CARTESIAN_POINT('Ctrl Pts',(-32.1420328931859,-37.3601293220733,
4.50067031743126));
#28741=CARTESIAN_POINT('Ctrl Pts',(-33.1393137781253,-38.2056252410501,
4.44833694164718));
#28742=CARTESIAN_POINT('Ctrl Pts',(-34.2656319712814,-38.4456746250879,
4.39600356586309));
#28743=CARTESIAN_POINT('Ctrl Pts',(-35.3919501644375,-38.6857240091257,
4.34367019007901));
#28744=CARTESIAN_POINT('Ctrl Pts',(-36.6473056658103,-38.3203268582244,
4.29133681429492));
#28745=CARTESIAN_POINT('Ctrl Pts',(-37.468853814561,-37.5133107379322,4.23900343851084));
#28746=CARTESIAN_POINT('Ctrl Pts',(-38.1303833971331,-36.8634826809916,
4.19686339317122));
#28747=CARTESIAN_POINT('Ctrl Pts',(-38.5106390985996,-35.9273158131948,
4.1547233478316));
#28748=CARTESIAN_POINT('Ctrl Pts',(-38.5188572457002,-34.9970948475072,
4.11258330249198));
#28749=CARTESIAN_POINT('Ctrl Pts',(-38.5230462440028,-35.0002063500719,
4.38741669750802));
#28750=CARTESIAN_POINT('Ctrl Pts',(-38.5230563037894,-35.0117987220789,
4.38794348863807));
#28751=CARTESIAN_POINT('Ctrl Pts',(-38.5230039194247,-35.023391000668,4.38847027976812));
#28752=CARTESIAN_POINT('Ctrl Pts',(-38.5228888130629,-35.0349826564212,
4.38899707089817));
#28753=CARTESIAN_POINT('Ctrl Pts',(-38.5114537221114,-36.186540535599,4.44133044668226));
#28754=CARTESIAN_POINT('Ctrl Pts',(-37.8810046334278,-37.3319515413465,
4.49366382246634));
#28755=CARTESIAN_POINT('Ctrl Pts',(-36.9142064202239,-37.9576651532382,
4.54599719825043));
#28756=CARTESIAN_POINT('Ctrl Pts',(-35.94740820702,-38.5833787651299,4.59833057403451));
#28757=CARTESIAN_POINT('Ctrl Pts',(-34.6442608692957,-38.6893949831658,
4.6506639498186));
#28758=CARTESIAN_POINT('Ctrl Pts',(-33.5890367664795,-38.2281809308918,
4.70299732560268));
#28759=CARTESIAN_POINT('Ctrl Pts',(-32.5338126636633,-37.7669668786178,
4.75533070138677));
#28760=CARTESIAN_POINT('Ctrl Pts',(-31.7265117957552,-36.7385225560339,
4.80766407717085));
#28761=CARTESIAN_POINT('Ctrl Pts',(-31.529091380047,-35.6039559014703,4.85999745295494));
#28762=CARTESIAN_POINT('Ctrl Pts',(-31.3316709643388,-34.4693892469067,
4.91233082873902));
#28763=CARTESIAN_POINT('Ctrl Pts',(-31.7441310008306,-33.2287002603633,
4.9646642045231));
#28764=CARTESIAN_POINT('Ctrl Pts',(-32.5815430522312,-32.4381578142198,
5.01699758030719));
#28765=CARTESIAN_POINT('Ctrl Pts',(-33.4189551036319,-31.6476153680763,
5.06933095609127));
#28766=CARTESIAN_POINT('Ctrl Pts',(-34.6813191699414,-31.3072194623328,
5.12166433187536));
#28767=CARTESIAN_POINT('Ctrl Pts',(-35.8026482696631,-31.5695882060385,
5.17399770765944));
#28768=CARTESIAN_POINT('Ctrl Pts',(-36.9239773693848,-31.8319569497442,
5.22633108344353));
#28769=CARTESIAN_POINT('Ctrl Pts',(-37.9042715025186,-32.6970903428993,
5.27866445922761));
#28770=CARTESIAN_POINT('Ctrl Pts',(-38.3040110863345,-33.7771017354242,
5.33099783501169));
#28771=CARTESIAN_POINT('Ctrl Pts',(-38.4476597125745,-34.1652097916211,
5.34980412251047));
#28772=CARTESIAN_POINT('Ctrl Pts',(-38.5163376200166,-34.5810664169843,
5.36861041000925));
#28773=CARTESIAN_POINT('Ctrl Pts',(-38.5138068989996,-34.9977297535637,
5.38741669750802));
#28774=CARTESIAN_POINT('Origin',(-35.,-35.,4.));
#28775=CARTESIAN_POINT('',(-38.5163032009778,-35.0029832534533,6.38741669750803));
#28776=CARTESIAN_POINT('',(-38.522424122767,-35.0013091826171,6.11258330249198));
#28777=CARTESIAN_POINT('',(-38.5175,-35.,4.));
#28778=CARTESIAN_POINT('Ctrl Pts',(-38.522424122767,-35.0013091826171,6.11258330249198));
#28779=CARTESIAN_POINT('Ctrl Pts',(-38.5172132511134,-33.9256163607463,
6.06372381478986));
#28780=CARTESIAN_POINT('Ctrl Pts',(-37.9876405112709,-32.8454778142804,
6.01486432708775));
#28781=CARTESIAN_POINT('Ctrl Pts',(-37.1315953638235,-32.1949561890823,
5.96600483938563));
#28782=CARTESIAN_POINT('Ctrl Pts',(-36.2146857829733,-31.4981827625019,
5.91367146360154));
#28783=CARTESIAN_POINT('Ctrl Pts',(-34.9232293392347,-31.2942891822923,
5.86133808781746));
#28784=CARTESIAN_POINT('Ctrl Pts',(-33.8362565743057,-31.6746922887769,
5.80900471203338));
#28785=CARTESIAN_POINT('Ctrl Pts',(-32.7492838093767,-32.0550953952615,
5.75667133624929));
#28786=CARTESIAN_POINT('Ctrl Pts',(-31.8667947232573,-33.0197951884404,
5.7043379604652));
#28787=CARTESIAN_POINT('Ctrl Pts',(-31.5844576051196,-34.1362638014206,
5.65200458468112));
#28788=CARTESIAN_POINT('Ctrl Pts',(-31.302120486982,-35.2527324144008,5.59967120889704));
#28789=CARTESIAN_POINT('Ctrl Pts',(-31.6199353368261,-36.5209698471824,
5.54733783311296));
#28790=CARTESIAN_POINT('Ctrl Pts',(-32.3954083053537,-37.3723558065856,
5.49500445732887));
#28791=CARTESIAN_POINT('Ctrl Pts',(-33.1708812738812,-38.2237417659887,
5.44267108154479));
#28792=CARTESIAN_POINT('Ctrl Pts',(-34.4040123610921,-38.6582762520135,
5.3903377057607));
#28793=CARTESIAN_POINT('Ctrl Pts',(-35.5419213472807,-38.4811336220058,
5.33800432997661));
#28794=CARTESIAN_POINT('Ctrl Pts',(-36.6798303334694,-38.3039909919981,
5.28567095419253));
#28795=CARTESIAN_POINT('Ctrl Pts',(-37.722517218636,-37.515171245958,5.23333757840845));
#28796=CARTESIAN_POINT('Ctrl Pts',(-38.202488327186,-36.468345511481,5.18100420262436));
#28797=CARTESIAN_POINT('Ctrl Pts',(-38.4116604841668,-36.0121372252676,
5.15819723591357));
#28798=CARTESIAN_POINT('Ctrl Pts',(-38.5139599737744,-35.5069276682025,
5.13539026920277));
#28799=CARTESIAN_POINT('Ctrl Pts',(-38.5124574312326,-35.001138833141,5.11258330249198));
#28800=CARTESIAN_POINT('Ctrl Pts',(-38.5138068989996,-34.9977297535637,
5.38741669750802));
#28801=CARTESIAN_POINT('Ctrl Pts',(-38.5092952319858,-35.7405402881605,
5.42094378579333));
#28802=CARTESIAN_POINT('Ctrl Pts',(-38.2784660556449,-36.4859147377931,
5.45447087407864));
#28803=CARTESIAN_POINT('Ctrl Pts',(-37.8426354587898,-37.0811999269324,
5.48799796236395));
#28804=CARTESIAN_POINT('Ctrl Pts',(-37.1623352129312,-38.0103973340206,
5.54033133814803));
#28805=CARTESIAN_POINT('Ctrl Pts',(-35.982549686716,-38.5739027563021,5.59266471393212));
#28806=CARTESIAN_POINT('Ctrl Pts',(-34.8322413561292,-38.5190660643709,
5.6449980897162));
#28807=CARTESIAN_POINT('Ctrl Pts',(-33.6819330255423,-38.4642293724398,
5.69733146550029));
#28808=CARTESIAN_POINT('Ctrl Pts',(-32.5611018905839,-37.791050566296,5.74966484128437));
#28809=CARTESIAN_POINT('Ctrl Pts',(-31.9722780150789,-36.8013521300638,
5.80199821706845));
#28810=CARTESIAN_POINT('Ctrl Pts',(-31.3834541395739,-35.8116536938316,
5.85433159285254));
#28811=CARTESIAN_POINT('Ctrl Pts',(-31.3266375235224,-34.5054356275111,
5.90666496863662));
#28812=CARTESIAN_POINT('Ctrl Pts',(-31.8273020724053,-33.4683479988925,
5.95899834442071));
#28813=CARTESIAN_POINT('Ctrl Pts',(-32.3279666212882,-32.431260370274,6.01133172020479));
#28814=CARTESIAN_POINT('Ctrl Pts',(-33.3861123351056,-31.6633031793574,
6.06366509598888));
#28815=CARTESIAN_POINT('Ctrl Pts',(-34.5273147025013,-31.5087918386834,
6.11599847177296));
#28816=CARTESIAN_POINT('Ctrl Pts',(-35.668517069897,-31.3542804980094,6.16833184755705));
#28817=CARTESIAN_POINT('Ctrl Pts',(-36.892776090871,-31.8132150075779,6.22066522334113));
#28818=CARTESIAN_POINT('Ctrl Pts',(-37.6511889677791,-32.6798336612887,
6.27299859912521));
#28819=CARTESIAN_POINT('Ctrl Pts',(-38.2039029090244,-33.3114054953559,
6.31113796525282));
#28820=CARTESIAN_POINT('Ctrl Pts',(-38.509198477207,-34.1595049296877,6.34927733138042));
#28821=CARTESIAN_POINT('Ctrl Pts',(-38.5163032009778,-35.0029832534533,
6.38741669750803));
#28822=CARTESIAN_POINT('Origin',(-35.,-35.,4.));
#28823=CARTESIAN_POINT('',(-38.5217392653161,-34.9982348400382,7.38741669750802));
#28824=CARTESIAN_POINT('',(-38.5153122961063,-34.9971887940747,7.11258330249198));
#28825=CARTESIAN_POINT('',(-38.5175,-35.,4.));
#28826=CARTESIAN_POINT('',(-32.3264680662287,-32.7141668369925,8.));
#28827=CARTESIAN_POINT('Ctrl Pts',(-38.5217392653161,-34.9982348400382,
7.38741669750802));
#28828=CARTESIAN_POINT('Ctrl Pts',(-38.5150454835571,-36.0376021634142,
7.43461100431976));
#28829=CARTESIAN_POINT('Ctrl Pts',(-38.0253751592018,-37.0822329702746,
7.48180531113151));
#28830=CARTESIAN_POINT('Ctrl Pts',(-37.2186056743939,-37.7364863611315,
7.52899961794325));
#28831=CARTESIAN_POINT('Ctrl Pts',(-36.3239856773675,-38.4619825252834,
7.58133299372733));
#28832=CARTESIAN_POINT('Ctrl Pts',(-35.0394476042314,-38.7074546780583,
7.63366636951141));
#28833=CARTESIAN_POINT('Ctrl Pts',(-33.9411230034093,-38.3607385339716,
7.68599974529549));
#28834=CARTESIAN_POINT('Ctrl Pts',(-32.8427984025871,-38.0140223898848,
7.73833312107958));
#28835=CARTESIAN_POINT('Ctrl Pts',(-31.9306872740789,-37.0751179489365,
7.79066649686366));
#28836=CARTESIAN_POINT('Ctrl Pts',(-31.613697604643,-35.9699319523746,7.84299987264775));
#28837=CARTESIAN_POINT('Ctrl Pts',(-31.2967079352071,-34.8647459558128,
7.89533324843184));
#28838=CARTESIAN_POINT('Ctrl Pts',(-31.5748397248436,-33.5932784036375,
7.94766662421592));
#28839=CARTESIAN_POINT('Ctrl Pts',(-32.3264680662287,-32.7141668369925,
8.));
#28840=CARTESIAN_POINT('',(-37.6785009901498,-32.7109751557132,8.));
#28841=CARTESIAN_POINT('Origin',(-35.,-35.,8.));
#28842=CARTESIAN_POINT('Ctrl Pts',(-37.6785241456451,-32.7109602826759,
8.));
#28843=CARTESIAN_POINT('Ctrl Pts',(-36.9607513379489,-31.8766751051408,
7.95000212253756));
#28844=CARTESIAN_POINT('Ctrl Pts',(-35.8186699645707,-31.4010799150529,
7.90000424507511));
#28845=CARTESIAN_POINT('Ctrl Pts',(-34.7217021996619,-31.4881457455928,
7.85000636761267));
#28846=CARTESIAN_POINT('Ctrl Pts',(-33.573492932036,-31.5792785908026,7.79767299182859));
#28847=CARTESIAN_POINT('Ctrl Pts',(-32.4747104002448,-32.2868661727234,
7.7453396160445));
#28848=CARTESIAN_POINT('Ctrl Pts',(-31.9173292682424,-33.2944463949298,
7.69300624026042));
#28849=CARTESIAN_POINT('Ctrl Pts',(-31.3599481362399,-34.3020266171361,
7.64067286447633));
#28850=CARTESIAN_POINT('Ctrl Pts',(-31.3439684040262,-35.609599479628,7.58833948869224));
#28851=CARTESIAN_POINT('Ctrl Pts',(-31.8768867974267,-36.6305186264058,
7.53600611290816));
#28852=CARTESIAN_POINT('Ctrl Pts',(-32.4098051908272,-37.6514377731836,
7.48367273712407));
#28853=CARTESIAN_POINT('Ctrl Pts',(-33.491621709842,-38.3857032042473,7.43133936134));
#28854=CARTESIAN_POINT('Ctrl Pts',(-34.6371338873761,-38.5042968827328,
7.37900598555591));
#28855=CARTESIAN_POINT('Ctrl Pts',(-35.7826460649101,-38.6228905612183,
7.32667260977183));
#28856=CARTESIAN_POINT('Ctrl Pts',(-36.9918539009634,-38.1258124871256,
7.27433923398775));
#28857=CARTESIAN_POINT('Ctrl Pts',(-37.7226850841419,-37.2358340108349,
7.22200585820366));
#28858=CARTESIAN_POINT('Ctrl Pts',(-38.2320440076398,-36.615556046438,7.18553167296643));
#28859=CARTESIAN_POINT('Ctrl Pts',(-38.5090309960538,-35.8044263207662,
7.14905748772921));
#28860=CARTESIAN_POINT('Ctrl Pts',(-38.5153122961063,-34.9971887940747,
7.11258330249198));
#28861=CARTESIAN_POINT('Origin',(35.,-35.,4.));
#28862=CARTESIAN_POINT('',(31.4879726191333,-35.0001375015905,0.387416697508024));
#28863=CARTESIAN_POINT('',(31.4847993146864,-35.0046492582639,0.112583302491975));
#28864=CARTESIAN_POINT('',(31.4825,-35.,4.));
#28865=CARTESIAN_POINT('',(32.3264680662287,-32.7141668369925,0.));
#28866=CARTESIAN_POINT('Ctrl Pts',(31.4847993146864,-35.0046492582639,0.112583302491975));
#28867=CARTESIAN_POINT('Ctrl Pts',(31.4919760559448,-34.1767269622227,0.0750555349946493));
#28868=CARTESIAN_POINT('Ctrl Pts',(31.7874825103136,-33.3445694048179,0.037527767497323));
#28869=CARTESIAN_POINT('Ctrl Pts',(32.3264680662287,-32.7141668369925,-2.98372437868011E-15));
#28870=CARTESIAN_POINT('',(37.6785011129036,-32.7109752438421,-5.55678203018928E-16));
#28871=CARTESIAN_POINT('Origin',(35.,-35.,0.));
#28872=CARTESIAN_POINT('Ctrl Pts',(37.6785242770714,-32.7109603660127,-2.86292032689789E-16));
#28873=CARTESIAN_POINT('Ctrl Pts',(36.9607515035944,-31.8766753489742,0.0499978774624439));
#28874=CARTESIAN_POINT('Ctrl Pts',(35.8186700361932,-31.4010797162719,0.099995754924888));
#28875=CARTESIAN_POINT('Ctrl Pts',(34.7217021987141,-31.4881454554173,0.149993632387332));
#28876=CARTESIAN_POINT('Ctrl Pts',(33.5734928551282,-31.5792782049632,0.202327008171416));
#28877=CARTESIAN_POINT('Ctrl Pts',(32.4747102708807,-32.2868660760186,0.2546603839555));
#28878=CARTESIAN_POINT('Ctrl Pts',(31.9173291209027,-33.2944463985812,0.306993759739584));
#28879=CARTESIAN_POINT('Ctrl Pts',(31.6318119669108,-33.8105769963377,0.333801405662397));
#28880=CARTESIAN_POINT('Ctrl Pts',(31.488357249556,-34.4054248931928,0.360609051585211));
#28881=CARTESIAN_POINT('Ctrl Pts',(31.4879726191333,-35.0001375015905,0.387416697508024));
#28882=CARTESIAN_POINT('Origin',(35.,-35.,4.));
#28883=CARTESIAN_POINT('',(31.4787693262007,-35.0021519651487,1.38741669750802));
#28884=CARTESIAN_POINT('',(31.4779839561681,-34.998317589092,1.11258330249197));
#28885=CARTESIAN_POINT('',(31.4825,-35.,4.));
#28886=CARTESIAN_POINT('Ctrl Pts',(31.4779839561681,-34.998317589092,1.11258330249197));
#28887=CARTESIAN_POINT('Ctrl Pts',(31.4773939435915,-34.8986109589584,1.10805583214991));
#28888=CARTESIAN_POINT('Ctrl Pts',(31.4812696152992,-34.7989511654426,1.10352836180784));
#28889=CARTESIAN_POINT('Ctrl Pts',(31.4897615265674,-34.6996866782215,1.09900089146577));
#28890=CARTESIAN_POINT('Ctrl Pts',(31.5879201780762,-33.5522808822113,1.04666751568169));
#28891=CARTESIAN_POINT('Ctrl Pts',(32.3028649757287,-32.457692848996,0.994334139897601));
#28892=CARTESIAN_POINT('Ctrl Pts',(33.314059894657,-31.906560527472,0.942000764113516));
#28893=CARTESIAN_POINT('Ctrl Pts',(34.3252548135852,-31.3554282059481,0.889667388329432));
#28894=CARTESIAN_POINT('Ctrl Pts',(35.6326998537893,-31.3477515961155,0.837334012545348));
#28895=CARTESIAN_POINT('Ctrl Pts',(36.650169778933,-31.8872259747803,0.785000636761264));
#28896=CARTESIAN_POINT('Ctrl Pts',(37.6676397040767,-32.4267003534451,0.732667260977179));
#28897=CARTESIAN_POINT('Ctrl Pts',(38.39513451416,-33.5133257206073,0.680333885193094));
#28898=CARTESIAN_POINT('Ctrl Pts',(38.5065306720619,-34.6593978563341,0.628000509409009));
#28899=CARTESIAN_POINT('Ctrl Pts',(38.6179268299637,-35.8054699920609,0.575667133624925));
#28900=CARTESIAN_POINT('Ctrl Pts',(38.1132243356843,-37.0109888963523,0.523333757840841));
#28901=CARTESIAN_POINT('Ctrl Pts',(37.2186048923566,-37.7364852312874,0.471000382056757));
#28902=CARTESIAN_POINT('Ctrl Pts',(36.3239854490289,-38.4619815662224,0.418667006272672));
#28903=CARTESIAN_POINT('Ctrl Pts',(35.0394490566529,-38.7074553318012,0.366333630488587));
#28904=CARTESIAN_POINT('Ctrl Pts',(33.9411236515154,-38.3607384247595,0.314000254704503));
#28905=CARTESIAN_POINT('Ctrl Pts',(32.842798246378,-38.0140215177178,0.261666878920419));
#28906=CARTESIAN_POINT('Ctrl Pts',(31.930683828479,-37.0751139380558,0.209333503136335));
#28907=CARTESIAN_POINT('Ctrl Pts',(31.6136941980954,-35.9699281595357,0.157000127352251));
#28908=CARTESIAN_POINT('Ctrl Pts',(31.524014825647,-35.6572606223148,0.142194519065492));
#28909=CARTESIAN_POINT('Ctrl Pts',(31.4819679173789,-35.3312845479312,0.127388910778734));
#28910=CARTESIAN_POINT('Ctrl Pts',(31.4847993146864,-35.0046492582639,0.112583302491975));
#28911=CARTESIAN_POINT('Ctrl Pts',(31.4879726191333,-35.0001375015905,0.387416697508024));
#28912=CARTESIAN_POINT('Ctrl Pts',(31.4876063813705,-35.5664115202329,0.412942427369295));
#28913=CARTESIAN_POINT('Ctrl Pts',(31.6169544331328,-36.1325628797889,0.438468157230566));
#28914=CARTESIAN_POINT('Ctrl Pts',(31.8768866723687,-36.6305186540646,0.463993887091838));
#28915=CARTESIAN_POINT('Ctrl Pts',(32.4098050895213,-37.6514378129155,0.516327262875923));
#28916=CARTESIAN_POINT('Ctrl Pts',(33.491621639535,-38.3857033565476,0.568660638660007));
#28917=CARTESIAN_POINT('Ctrl Pts',(34.6371338646016,-38.5042970583454,0.620994014444092));
#28918=CARTESIAN_POINT('Ctrl Pts',(35.7826460896681,-38.6228907601432,0.673327390228177));
#28919=CARTESIAN_POINT('Ctrl Pts',(36.9918539897876,-38.1258126201067,0.725660766012261));
#28920=CARTESIAN_POINT('Ctrl Pts',(37.7226852066847,-37.235834095095,0.777994141796346));
#28921=CARTESIAN_POINT('Ctrl Pts',(38.4535164235819,-36.3458555700833,0.83032751758043));
#28922=CARTESIAN_POINT('Ctrl Pts',(38.7059709572567,-35.0629766600964,0.882660893364514));
#28923=CARTESIAN_POINT('Ctrl Pts',(38.3668190041959,-33.9624298822548,0.934994269148598));
#28924=CARTESIAN_POINT('Ctrl Pts',(38.027667051135,-32.8618831044132,0.987327644932683));
#28925=CARTESIAN_POINT('Ctrl Pts',(37.0969086113384,-31.9436684587171,1.03966102071677));
#28926=CARTESIAN_POINT('Ctrl Pts',(35.9918738484399,-31.6194482583158,1.09199439650085));
#28927=CARTESIAN_POINT('Ctrl Pts',(34.8868390855414,-31.2952280579146,1.14432777228494));
#28928=CARTESIAN_POINT('Ctrl Pts',(33.607527999541,-31.5650023028083,1.19666114806902));
#28929=CARTESIAN_POINT('Ctrl Pts',(32.7275158499642,-32.3078281435934,1.24899452385311));
#28930=CARTESIAN_POINT('Ctrl Pts',(31.9516362590269,-32.9627547940529,1.29513524840474));
#28931=CARTESIAN_POINT('Ctrl Pts',(31.4861479206373,-33.9854036295086,1.34127597295638));
#28932=CARTESIAN_POINT('Ctrl Pts',(31.4787693262007,-35.0021519651487,1.38741669750802));
#28933=CARTESIAN_POINT('Origin',(35.,-35.,4.));
#28934=CARTESIAN_POINT('',(31.4830375605149,-34.9969726960772,2.38741669750802));
#28935=CARTESIAN_POINT('',(31.4877390119671,-34.9992080277921,2.11258330249198));
#28936=CARTESIAN_POINT('',(31.4825,-35.,4.));
#28937=CARTESIAN_POINT('Ctrl Pts',(31.4877390119671,-34.9992080277921,2.11258330249198));
#28938=CARTESIAN_POINT('Ctrl Pts',(31.4866498159747,-34.4699801096587,2.08872275352108));
#28939=CARTESIAN_POINT('Ctrl Pts',(31.5990329357071,-33.9411914000592,2.06486220455019));
#28940=CARTESIAN_POINT('Ctrl Pts',(31.8273027226982,-33.4683483113999,2.04100165557929));
#28941=CARTESIAN_POINT('Ctrl Pts',(32.3279671691587,-32.431260896693,1.98866827979521));
#28942=CARTESIAN_POINT('Ctrl Pts',(33.3861126668897,-31.6633038687123,1.93633490401112));
#28943=CARTESIAN_POINT('Ctrl Pts',(34.5273147998293,-31.5087925573416,1.88400152822704));
#28944=CARTESIAN_POINT('Ctrl Pts',(35.6685169327689,-31.3542812459709,1.83166815244295));
#28945=CARTESIAN_POINT('Ctrl Pts',(36.892775700917,-31.8132156512101,1.77933477665887));
#28946=CARTESIAN_POINT('Ctrl Pts',(37.651188423337,-32.679834131615,1.72700140087478));
#28947=CARTESIAN_POINT('Ctrl Pts',(38.409601145757,-33.5464526120198,1.6746680250907));
#28948=CARTESIAN_POINT('Ctrl Pts',(38.7021678224488,-34.8207551675903,1.62233464930661));
#28949=CARTESIAN_POINT('Ctrl Pts',(38.3977155653522,-35.9313944817532,1.57000127352253));
#28950=CARTESIAN_POINT('Ctrl Pts',(38.0932633082556,-37.0420337959161,1.51766789773845));
#28951=CARTESIAN_POINT('Ctrl Pts',(37.1917921173706,-37.9890098686715,1.46533452195436));
#28952=CARTESIAN_POINT('Ctrl Pts',(36.0974793449018,-38.347756846785,1.41300114617028));
#28953=CARTESIAN_POINT('Ctrl Pts',(35.0031665724331,-38.7065038248986,1.36066777038619));
#28954=CARTESIAN_POINT('Ctrl Pts',(33.7160122183805,-38.4770217083703,1.30833439460211));
#28955=CARTESIAN_POINT('Ctrl Pts',(32.8131212940369,-37.7621688707036,1.25600101881802));
#28956=CARTESIAN_POINT('Ctrl Pts',(31.9883413614044,-37.10915945462,1.20819511337601));
#28957=CARTESIAN_POINT('Ctrl Pts',(31.4842139440677,-36.051127518694,1.16038920793399));
#28958=CARTESIAN_POINT('Ctrl Pts',(31.4779839561681,-34.998317589092,1.11258330249197));
#28959=CARTESIAN_POINT('Ctrl Pts',(31.4787693262007,-35.0021519651487,1.38741669750802));
#28960=CARTESIAN_POINT('Ctrl Pts',(31.4777790283158,-35.1386120640087,1.39360934874047));
#28961=CARTESIAN_POINT('Ctrl Pts',(31.4850406303498,-35.2749658775635,1.39980199997291));
#28962=CARTESIAN_POINT('Ctrl Pts',(31.5009112501032,-35.4103101518596,1.40599465120536));
#28963=CARTESIAN_POINT('Ctrl Pts',(31.6350320129721,-36.554088882664,1.45832802698944));
#28964=CARTESIAN_POINT('Ctrl Pts',(32.3839867518631,-37.6257689075961,1.51066140277353));
#28965=CARTESIAN_POINT('Ctrl Pts',(33.4119755528977,-38.1448602359127,1.56299477855761));
#28966=CARTESIAN_POINT('Ctrl Pts',(34.4399643539324,-38.6639515642293,1.6153281543417));
#28967=CARTESIAN_POINT('Ctrl Pts',(35.7469872171107,-38.6304541959304,1.66766153012578));
#28968=CARTESIAN_POINT('Ctrl Pts',(36.7470353952608,-38.0593854028254,1.71999490590987));
#28969=CARTESIAN_POINT('Ctrl Pts',(37.7470835734109,-37.4883166097203,1.77232828169395));
#28970=CARTESIAN_POINT('Ctrl Pts',(38.4401570665328,-36.3796763918093,1.82466165747804));
#28971=CARTESIAN_POINT('Ctrl Pts',(38.5155124424211,-35.2305296204218,1.87699503326212));
#28972=CARTESIAN_POINT('Ctrl Pts',(38.5908678183095,-34.0813828490343,1.9293284090462));
#28973=CARTESIAN_POINT('Ctrl Pts',(38.0485050769643,-32.8917295241703,1.98166178483029));
#28974=CARTESIAN_POINT('Ctrl Pts',(37.1315954563618,-32.1949560672859,2.03399516061437));
#28975=CARTESIAN_POINT('Ctrl Pts',(36.2146858357593,-31.4981826104015,2.08632853639846));
#28976=CARTESIAN_POINT('Ctrl Pts',(34.9232293358993,-31.2942890214966,2.13866191218254));
#28977=CARTESIAN_POINT('Ctrl Pts',(33.8362565237849,-31.6746921445243,2.19099528796663));
#28978=CARTESIAN_POINT('Ctrl Pts',(32.7492837116705,-32.055095267552,2.24332866375071));
#28979=CARTESIAN_POINT('Ctrl Pts',(31.8667945873017,-33.0197951025121,2.2956620395348));
#28980=CARTESIAN_POINT('Ctrl Pts',(31.5844574569229,-34.1362637639197,2.34799541531888));
#28981=CARTESIAN_POINT('Ctrl Pts',(31.5135652106755,-34.4165987349732,2.36113584271526));
#28982=CARTESIAN_POINT('Ctrl Pts',(31.4805104906949,-34.7065022103634,2.37427627011164));
#28983=CARTESIAN_POINT('Ctrl Pts',(31.4830375605149,-34.9969726960772,2.38741669750802));
#28984=CARTESIAN_POINT('Origin',(35.,-35.,4.));
#28985=CARTESIAN_POINT('',(31.486635086556,-35.0020090496756,3.38741669750802));
#28986=CARTESIAN_POINT('',(31.4804772106861,-35.0027703375482,3.11258330249198));
#28987=CARTESIAN_POINT('',(31.4825,-35.,4.));
#28988=CARTESIAN_POINT('Ctrl Pts',(31.4804772106861,-35.0027703375482,3.11258330249198));
#28989=CARTESIAN_POINT('Ctrl Pts',(31.4887009944635,-34.0497596813621,3.06938967489225));
#28990=CARTESIAN_POINT('Ctrl Pts',(31.8903812384068,-33.090636581221,3.02619604729253));
#28991=CARTESIAN_POINT('Ctrl Pts',(32.5815435480781,-32.4381583394347,2.98300241969281));
#28992=CARTESIAN_POINT('Ctrl Pts',(33.4189554277892,-31.647616055402,2.93066904390873));
#28993=CARTESIAN_POINT('Ctrl Pts',(34.6813192352892,-31.3072202195671,2.87833566812464));
#28994=CARTESIAN_POINT('Ctrl Pts',(35.8026481051029,-31.5695889094262,2.82600229234056));
#28995=CARTESIAN_POINT('Ctrl Pts',(36.9239769749167,-31.8319575992854,2.77366891655647));
#28996=CARTESIAN_POINT('Ctrl Pts',(37.904270907044,-32.6970908148387,2.72133554077239));
#28997=CARTESIAN_POINT('Ctrl Pts',(38.3040104089138,-33.7771019860347,2.66900216498831));
#28998=CARTESIAN_POINT('Ctrl Pts',(38.7037499107836,-34.8571131572306,2.61666878920422));
#28999=CARTESIAN_POINT('Ctrl Pts',(38.5229349823959,-36.1520022840693,2.56433541342014));
#29000=CARTESIAN_POINT('Ctrl Pts',(37.8426348759932,-37.0811995004531,2.51200203763605));
#29001=CARTESIAN_POINT('Ctrl Pts',(37.1623347695905,-38.0103967168369,2.45966866185197));
#29002=CARTESIAN_POINT('Ctrl Pts',(35.9825494851727,-38.5739020227658,2.40733528606788));
#29003=CARTESIAN_POINT('Ctrl Pts',(34.832241390481,-38.5190653424433,2.3550019102838));
#29004=CARTESIAN_POINT('Ctrl Pts',(33.6819332957892,-38.4642286621207,2.30266853449971));
#29005=CARTESIAN_POINT('Ctrl Pts',(32.5611023908235,-37.7910499955468,2.25033515871563));
#29006=CARTESIAN_POINT('Ctrl Pts',(31.9722786359356,-36.8013517615434,2.19800178293155));
#29007=CARTESIAN_POINT('Ctrl Pts',(31.6519194665675,-36.2628902923203,2.16952895611836));
#29008=CARTESIAN_POINT('Ctrl Pts',(31.4890387510844,-35.6307364505496,2.14105612930517));
#29009=CARTESIAN_POINT('Ctrl Pts',(31.4877390119671,-34.9992080277921,2.11258330249198));
#29010=CARTESIAN_POINT('Ctrl Pts',(31.4830375605149,-34.9969726960772,2.38741669750802));
#29011=CARTESIAN_POINT('Ctrl Pts',(31.490574858507,-35.8633368112863,2.42660964589573));
#29012=CARTESIAN_POINT('Ctrl Pts',(31.8146493000371,-36.734745074899,2.46580259428343));
#29013=CARTESIAN_POINT('Ctrl Pts',(32.3954081923274,-37.3723559095391,2.50499554267113));
#29014=CARTESIAN_POINT('Ctrl Pts',(33.1708811944992,-38.223741905896,2.55732891845522));
#29015=CARTESIAN_POINT('Ctrl Pts',(34.4040123352312,-38.6582764107548,2.60966229423931));
#29016=CARTESIAN_POINT('Ctrl Pts',(35.5419213707996,-38.4811337730552,2.66199567002339));
#29017=CARTESIAN_POINT('Ctrl Pts',(36.679830406368,-38.3039911353557,2.71432904580747));
#29018=CARTESIAN_POINT('Ctrl Pts',(37.7225173367726,-37.5151713550979,2.76666242159156));
#29019=CARTESIAN_POINT('Ctrl Pts',(38.2024884661482,-36.4683455751991,2.81899579737564));
#29020=CARTESIAN_POINT('Ctrl Pts',(38.6824595955238,-35.4215197953004,2.87132917315972));
#29021=CARTESIAN_POINT('Ctrl Pts',(38.5997149238704,-34.1166880157607,2.92366254894381));
#29022=CARTESIAN_POINT('Ctrl Pts',(37.9913534261364,-33.1388778186484,2.97599592472789));
#29023=CARTESIAN_POINT('Ctrl Pts',(37.3829919284024,-32.161067621536,3.02832930051198));
#29024=CARTESIAN_POINT('Ctrl Pts',(36.2490136045879,-31.510279006851,3.08066267629606));
#29025=CARTESIAN_POINT('Ctrl Pts',(35.0978430733873,-31.4782961743034,3.13299605208015));
#29026=CARTESIAN_POINT('Ctrl Pts',(33.9466725421867,-31.4463133417559,3.18532942786423));
#29027=CARTESIAN_POINT('Ctrl Pts',(32.7783098036,-32.0331362913458,3.23766280364832));
#29028=CARTESIAN_POINT('Ctrl Pts',(32.116595896964,-32.975660137455,3.2899961794324));
#29029=CARTESIAN_POINT('Ctrl Pts',(31.7059942452997,-33.5605078247475,3.32246968545761));
#29030=CARTESIAN_POINT('Ctrl Pts',(31.4904704191383,-34.2823130120804,3.35494319148282));
#29031=CARTESIAN_POINT('Ctrl Pts',(31.486635086556,-35.0020090496756,3.38741669750802));
#29032=CARTESIAN_POINT('Origin',(35.,-35.,4.));
#29033=CARTESIAN_POINT('',(31.4769535111774,-35.000206350087,4.38741669750802));
#29034=CARTESIAN_POINT('',(31.481143567597,-34.9970948481792,4.11258330249198));
#29035=CARTESIAN_POINT('',(31.4825,-35.,4.));
#29036=CARTESIAN_POINT('Ctrl Pts',(31.481143567597,-34.9970948481792,4.11258330249198));
#29037=CARTESIAN_POINT('Ctrl Pts',(31.4791556658517,-34.7720820979161,4.10238997204751));
#29038=CARTESIAN_POINT('Ctrl Pts',(31.4989362834408,-34.5474172520071,4.09219664160305));
#29039=CARTESIAN_POINT('Ctrl Pts',(31.5417700421341,-34.3272371560843,4.08200331115859));
#29040=CARTESIAN_POINT('Ctrl Pts',(31.7616819935963,-33.1968148899876,4.0296699353745));
#29041=CARTESIAN_POINT('Ctrl Pts',(32.5892466030323,-32.1846051588847,3.97733655959042));
#29042=CARTESIAN_POINT('Ctrl Pts',(33.6534213081659,-31.7444370513165,3.92500318380633));
#29043=CARTESIAN_POINT('Ctrl Pts',(34.7175960132996,-31.3042689437483,3.87266980802225));
#29044=CARTESIAN_POINT('Ctrl Pts',(36.0183808141308,-31.4361424597148,3.82033643223816));
#29045=CARTESIAN_POINT('Ctrl Pts',(36.9725626056516,-32.0809314753194,3.76800305645408));
#29046=CARTESIAN_POINT('Ctrl Pts',(37.9267443971724,-32.7257204909241,3.71566968066999));
#29047=CARTESIAN_POINT('Ctrl Pts',(38.5343231793827,-33.883425006167,3.66333630488591));
#29048=CARTESIAN_POINT('Ctrl Pts',(38.5228880907758,-35.0349826492465,3.61100292910183));
#29049=CARTESIAN_POINT('Ctrl Pts',(38.5114530021688,-36.186540292326,3.55866955331774));
#29050=CARTESIAN_POINT('Ctrl Pts',(37.8810040427447,-37.3319510632421,3.50633617753366));
#29051=CARTESIAN_POINT('Ctrl Pts',(36.9142060277602,-37.9576645468416,3.45400280174957));
#29052=CARTESIAN_POINT('Ctrl Pts',(35.9474080127757,-38.5833780304411,3.40166942596549));
#29053=CARTESIAN_POINT('Ctrl Pts',(34.6442609422309,-38.6893942267241,3.3493360501814));
#29054=CARTESIAN_POINT('Ctrl Pts',(33.5890370557646,-38.2281802690192,3.29700267439732));
#29055=CARTESIAN_POINT('Ctrl Pts',(32.5338131692983,-37.7669663113142,3.24466929861323));
#29056=CARTESIAN_POINT('Ctrl Pts',(31.7265124669105,-36.7385221996213,3.19233592282915));
#29057=CARTESIAN_POINT('Ctrl Pts',(31.5290920916777,-35.6039557776596,3.14000254704507));
#29058=CARTESIAN_POINT('Ctrl Pts',(31.4946136639238,-35.4058097333848,3.1308627988607));
#29059=CARTESIAN_POINT('Ctrl Pts',(31.478737062497,-35.2044268757596,3.12172305067634));
#29060=CARTESIAN_POINT('Ctrl Pts',(31.4804772106861,-35.0027703375482,3.11258330249198));
#29061=CARTESIAN_POINT('Ctrl Pts',(31.486635086556,-35.0020090496756,3.38741669750802));
#29062=CARTESIAN_POINT('Ctrl Pts',(31.4842895065774,-35.4421546120773,3.4072765672669));
#29063=CARTESIAN_POINT('Ctrl Pts',(31.5611195851562,-35.8815113110096,3.42713643702578));
#29064=CARTESIAN_POINT('Ctrl Pts',(31.7209248424069,-36.2882690753391,3.44699630678465));
#29065=CARTESIAN_POINT('Ctrl Pts',(32.1420327691713,-37.3601294244856,3.49932968256874));
#29066=CARTESIAN_POINT('Ctrl Pts',(33.1393136973855,-38.2056253801502,3.55166305835282));
#29067=CARTESIAN_POINT('Ctrl Pts',(34.2656319394155,-38.4456747746043,3.60399643413691));
#29068=CARTESIAN_POINT('Ctrl Pts',(35.3919501814454,-38.6857241690583,3.65632980992099));
#29069=CARTESIAN_POINT('Ctrl Pts',(36.647305737291,-38.3203270023018,3.70866318570508));
#29070=CARTESIAN_POINT('Ctrl Pts',(37.4688539216907,-37.5133108469912,3.76099656148916));
#29071=CARTESIAN_POINT('Ctrl Pts',(38.2904021060904,-36.7062946916805,3.81332993727324));
#29072=CARTESIAN_POINT('Ctrl Pts',(38.6781429190441,-35.4576595478158,3.86566331305733));
#29073=CARTESIAN_POINT('Ctrl Pts',(38.4582309072122,-34.3272369713982,3.91799668884141));
#29074=CARTESIAN_POINT('Ctrl Pts',(38.2383188953802,-33.1968143949805,3.9703300646255));
#29075=CARTESIAN_POINT('Ctrl Pts',(37.4107540587627,-32.1846043860099,4.02266344040958));
#29076=CARTESIAN_POINT('Ctrl Pts',(36.346579061494,-31.744436157607,4.07499681619367));
#29077=CARTESIAN_POINT('Ctrl Pts',(35.2824040642253,-31.3042679292041,4.12733019197775));
#29078=CARTESIAN_POINT('Ctrl Pts',(33.9816189063054,-31.4361414813689,4.17966356776183));
#29079=CARTESIAN_POINT('Ctrl Pts',(33.0274368528446,-32.0809306739812,4.23199694354592));
#29080=CARTESIAN_POINT('Ctrl Pts',(32.0828596573675,-32.7192293770668,4.28380352819995));
#29081=CARTESIAN_POINT('Ctrl Pts',(31.477942827805,-33.8601696083914,4.33561011285399));
#29082=CARTESIAN_POINT('Ctrl Pts',(31.4769535111774,-35.000206350087,4.38741669750802));
#29083=CARTESIAN_POINT('Origin',(35.,-35.,4.));
#29084=CARTESIAN_POINT('',(31.4861928568261,-34.9977297533801,5.38741669750802));
#29085=CARTESIAN_POINT('',(31.4875433805768,-35.0011388328632,5.11258330249198));
#29086=CARTESIAN_POINT('',(31.4825,-35.,4.));
#29087=CARTESIAN_POINT('Ctrl Pts',(31.4875433805768,-35.0011388328632,5.11258330249198));
#29088=CARTESIAN_POINT('Ctrl Pts',(31.4894886053032,-34.3463334487764,5.08305689341869));
#29089=CARTESIAN_POINT('Ctrl Pts',(31.6654108801779,-33.6905571677388,5.0535304843454));
#29090=CARTESIAN_POINT('Ctrl Pts',(32.0086473950495,-33.1388783295694,5.02400407527211));
#29091=CARTESIAN_POINT('Ctrl Pts',(32.6170087257827,-32.1610684008923,4.97167069948802));
#29092=CARTESIAN_POINT('Ctrl Pts',(33.7509867382882,-31.5102799648413,4.91933732370394));
#29093=CARTESIAN_POINT('Ctrl Pts',(34.9021569534692,-31.478297141069,4.86700394791986));
#29094=CARTESIAN_POINT('Ctrl Pts',(36.0533271686501,-31.4463143172967,4.81467057213577));
#29095=CARTESIAN_POINT('Ctrl Pts',(37.2216895865065,-32.0331371058031,4.76233719635168));
#29096=CARTESIAN_POINT('Ctrl Pts',(37.8834033114917,-32.975660693175,4.7100038205676));
#29097=CARTESIAN_POINT('Ctrl Pts',(38.5451170364769,-33.9181842805469,4.65767044478351));
#29098=CARTESIAN_POINT('Ctrl Pts',(38.7001820685911,-35.2164086667843,4.60533706899943));
#29099=CARTESIAN_POINT('Ctrl Pts',(38.2790742574276,-36.2882687216848,4.55300369321535));
#29100=CARTESIAN_POINT('Ctrl Pts',(37.8579664462641,-37.3601287765853,4.50067031743126));
#29101=CARTESIAN_POINT('Ctrl Pts',(36.8606857918229,-38.205624500149,4.44833694164718));
#29102=CARTESIAN_POINT('Ctrl Pts',(35.7343678589879,-38.4456738287057,4.39600356586309));
#29103=CARTESIAN_POINT('Ctrl Pts',(34.6080499261528,-38.6857231572625,4.34367019007901));
#29104=CARTESIAN_POINT('Ctrl Pts',(33.3526947149239,-38.3203260908123,4.29133681429492));
#29105=CARTESIAN_POINT('Ctrl Pts',(32.5311467560536,-37.5133101570419,4.23900343851084));
#29106=CARTESIAN_POINT('Ctrl Pts',(31.8696173263776,-36.863482250293,4.19686339317122));
#29107=CARTESIAN_POINT('Ctrl Pts',(31.489361712798,-35.9273155988689,4.1547233478316));
#29108=CARTESIAN_POINT('Ctrl Pts',(31.481143567597,-34.9970948481792,4.11258330249198));
#29109=CARTESIAN_POINT('Ctrl Pts',(31.4769535111774,-35.000206350087,4.38741669750802));
#29110=CARTESIAN_POINT('Ctrl Pts',(31.47694345139,-35.0117987228996,4.38794348863807));
#29111=CARTESIAN_POINT('Ctrl Pts',(31.4769958357584,-35.0233910022943,4.38847027976812));
#29112=CARTESIAN_POINT('Ctrl Pts',(31.4771109421281,-35.034982658853,4.38899707089817));
#29113=CARTESIAN_POINT('Ctrl Pts',(31.4885460338743,-36.1865406180529,4.44133044668226));
#29114=CARTESIAN_POINT('Ctrl Pts',(32.1189951663686,-37.3319517033932,4.49366382246634));
#29115=CARTESIAN_POINT('Ctrl Pts',(33.0857934467562,-37.9576653587677,4.54599719825043));
#29116=CARTESIAN_POINT('Ctrl Pts',(34.0525917271438,-38.5833790141421,4.59833057403451));
#29117=CARTESIAN_POINT('Ctrl Pts',(35.3557391554246,-38.6893952395508,4.6506639498186));
#29118=CARTESIAN_POINT('Ctrl Pts',(36.4109633315695,-38.228181155224,4.70299732560268));
#29119=CARTESIAN_POINT('Ctrl Pts',(37.4661875077144,-37.7669670708972,4.75533070138676));
#29120=CARTESIAN_POINT('Ctrl Pts',(38.2734884317233,-36.738522676835,4.80766407717085));
#29121=CARTESIAN_POINT('Ctrl Pts',(38.47090886115,-35.6039559434342,4.85999745295493));
#29122=CARTESIAN_POINT('Ctrl Pts',(38.6683292905767,-34.4693892100334,4.91233082873902));
#29123=CARTESIAN_POINT('Ctrl Pts',(38.2558692254213,-33.2287001372941,4.9646642045231));
#29124=CARTESIAN_POINT('Ctrl Pts',(37.4184571158289,-32.4381576362056,5.01699758030719));
#29125=CARTESIAN_POINT('Ctrl Pts',(36.5810450062365,-31.6476151351171,5.06933095609127));
#29126=CARTESIAN_POINT('Ctrl Pts',(35.3186808522071,-31.3072192056794,5.12166433187536));
#29127=CARTESIAN_POINT('Ctrl Pts',(34.1973516745615,-31.5695879676355,5.17399770765944));
#29128=CARTESIAN_POINT('Ctrl Pts',(33.0760224969158,-31.8319567295916,5.22633108344352));
#29129=CARTESIAN_POINT('Ctrl Pts',(32.0957282956539,-32.6970901829416,5.27866445922761));
#29130=CARTESIAN_POINT('Ctrl Pts',(31.6959886840635,-33.7771016504831,5.33099783501169));
#29131=CARTESIAN_POINT('Ctrl Pts',(31.5523400478426,-34.1652097336376,5.34980412251047));
#29132=CARTESIAN_POINT('Ctrl Pts',(31.4836621356307,-34.5810663878724,5.36861041000924));
#29133=CARTESIAN_POINT('Ctrl Pts',(31.4861928568261,-34.9977297533801,5.38741669750802));
#29134=CARTESIAN_POINT('Origin',(35.,-35.,4.));
#29135=CARTESIAN_POINT('',(31.4836965554877,-35.0029832498286,6.38741669750802));
#29136=CARTESIAN_POINT('',(31.4775766908735,-35.0013091813966,6.11258330249198));
#29137=CARTESIAN_POINT('',(31.4825,-35.,4.));
#29138=CARTESIAN_POINT('Ctrl Pts',(31.4775766908735,-35.0013091813966,6.11258330249198));
#29139=CARTESIAN_POINT('Ctrl Pts',(31.4827875611424,-33.9256166077537,6.06372381478986));
#29140=CARTESIAN_POINT('Ctrl Pts',(32.0123601793055,-32.8454783123193,6.01486432708774));
#29141=CARTESIAN_POINT('Ctrl Pts',(32.8684051290729,-32.1949568378204,5.96600483938563));
#29142=CARTESIAN_POINT('Ctrl Pts',(33.7853144981881,-31.4981835726539,5.91367146360154));
#29143=CARTESIAN_POINT('Ctrl Pts',(35.0767706429996,-31.2942900387516,5.86133808781746));
#29144=CARTESIAN_POINT('Ctrl Pts',(36.1637431566001,-31.6746930571201,5.80900471203337));
#29145=CARTESIAN_POINT('Ctrl Pts',(37.2507156702007,-32.0550960754886,5.75667133624929));
#29146=CARTESIAN_POINT('Ctrl Pts',(38.1332045525903,-33.0197956461279,5.70433796046521));
#29147=CARTESIAN_POINT('Ctrl Pts',(38.4155416055276,-34.1362640011663,5.65200458468112));
#29148=CARTESIAN_POINT('Ctrl Pts',(38.6978786584649,-35.2527323562045,5.59967120889703));
#29149=CARTESIAN_POINT('Ctrl Pts',(38.3800638819499,-36.5209694956418,5.54733783311295));
#29150=CARTESIAN_POINT('Ctrl Pts',(37.6045910926243,-37.3723552582146,5.49500445732887));
#29151=CARTESIAN_POINT('Ctrl Pts',(36.8291183032988,-38.2237410207875,5.44267108154478));
#29152=CARTESIAN_POINT('Ctrl Pts',(35.5959875011627,-38.658275406496,5.3903377057607));
#29153=CARTESIAN_POINT('Ctrl Pts',(34.4580787779894,-38.4811328174583,5.33800432997662));
#29154=CARTESIAN_POINT('Ctrl Pts',(33.3201700548161,-38.3039902284206,5.28567095419253));
#29155=CARTESIAN_POINT('Ctrl Pts',(32.2774834106055,-37.5151706646368,5.23333757840844));
#29156=CARTESIAN_POINT('Ctrl Pts',(31.7975124129806,-36.4683451720932,5.18100420262436));
#29157=CARTESIAN_POINT('Ctrl Pts',(31.5883403043411,-36.0121369913148,5.15819723591357));
#29158=CARTESIAN_POINT('Ctrl Pts',(31.486040838379,-35.5069275510188,5.13539026920277));
#29159=CARTESIAN_POINT('Ctrl Pts',(31.4875433805768,-35.0011388328632,5.11258330249198));
#29160=CARTESIAN_POINT('Ctrl Pts',(31.4861928568261,-34.9977297533801,5.38741669750802));
#29161=CARTESIAN_POINT('Ctrl Pts',(31.4907045241579,-35.7405403395491,5.42094378579333));
#29162=CARTESIAN_POINT('Ctrl Pts',(31.7215337165433,-36.4859148409341,5.45447087407864));
#29163=CARTESIAN_POINT('Ctrl Pts',(32.1573643436795,-37.081200071482,5.48799796236395));
#29164=CARTESIAN_POINT('Ctrl Pts',(32.8376646368048,-38.0103975432063,5.54033133814803));
#29165=CARTESIAN_POINT('Ctrl Pts',(34.0174502449743,-38.5739030049216,5.59266471393212));
#29166=CARTESIAN_POINT('Ctrl Pts',(35.1677586555142,-38.5190663090568,5.6449980897162));
#29167=CARTESIAN_POINT('Ctrl Pts',(36.318067066054,-38.464229613192,5.69733146550028));
#29168=CARTESIAN_POINT('Ctrl Pts',(37.4388982789643,-37.7910507597469,5.74966484128437));
#29169=CARTESIAN_POINT('Ctrl Pts',(38.0277221953511,-36.8013522549706,5.80199821706845));
#29170=CARTESIAN_POINT('Ctrl Pts',(38.6165461117379,-35.8116537501943,5.85433159285254));
#29171=CARTESIAN_POINT('Ctrl Pts',(38.6733627316013,-34.5054355940866,5.90666496863662));
#29172=CARTESIAN_POINT('Ctrl Pts',(38.172698148003,-33.4683478929687,5.9589983444207));
#29173=CARTESIAN_POINT('Ctrl Pts',(37.6720335644046,-32.4312601918508,6.01133172020479));
#29174=CARTESIAN_POINT('Ctrl Pts',(36.6138877773445,-31.6633029457227,6.06366509598888));
#29175=CARTESIAN_POINT('Ctrl Pts',(35.4726853304849,-31.5087915951115,6.11599847177296));
#29176=CARTESIAN_POINT('Ctrl Pts',(34.3314828836252,-31.3542802445004,6.16833184755705));
#29177=CARTESIAN_POINT('Ctrl Pts',(33.107223776966,-31.8132147894062,6.22066522334113));
#29178=CARTESIAN_POINT('Ctrl Pts',(32.3488108476933,-32.6798335018657,6.27299859912521));
#29179=CARTESIAN_POINT('Ctrl Pts',(31.7960968682859,-33.3114053787477,6.31113796525282));
#29180=CARTESIAN_POINT('Ctrl Pts',(31.4908012796383,-34.1595048683285,6.34927733138042));
#29181=CARTESIAN_POINT('Ctrl Pts',(31.4836965554877,-35.0029832498286,6.38741669750802));
#29182=CARTESIAN_POINT('Origin',(35.,-35.,4.));
#29183=CARTESIAN_POINT('',(31.478260520576,-34.9982347527286,7.38741669750802));
#29184=CARTESIAN_POINT('',(31.4846885160394,-34.9971888045819,7.11258330249198));
#29185=CARTESIAN_POINT('',(31.4825,-35.,4.));
#29186=CARTESIAN_POINT('',(37.6735319337713,-32.7141668369925,8.));
#29187=CARTESIAN_POINT('Ctrl Pts',(31.478260520576,-34.9982347527286,7.38741669750802));
#29188=CARTESIAN_POINT('Ctrl Pts',(31.4849542237249,-36.0376022532878,7.43461100431976));
#29189=CARTESIAN_POINT('Ctrl Pts',(31.9746244075585,-37.0822334042073,7.4818053111315));
#29190=CARTESIAN_POINT('Ctrl Pts',(32.7813940610787,-37.7364867433061,7.52899961794324));
#29191=CARTESIAN_POINT('Ctrl Pts',(33.6760142451889,-38.4619828500639,7.58133299372733));
#29192=CARTESIAN_POINT('Ctrl Pts',(34.9605528856554,-38.7074544587316,7.63366636951141));
#29193=CARTESIAN_POINT('Ctrl Pts',(36.0588772142959,-38.3607385729207,7.6859997452955));
#29194=CARTESIAN_POINT('Ctrl Pts',(37.1572015429365,-38.0140226871098,7.73833312107958));
#29195=CARTESIAN_POINT('Ctrl Pts',(38.069311559751,-37.0751193068202,7.79066649686367));
#29196=CARTESIAN_POINT('Ctrl Pts',(38.386301242806,-35.9699332359521,7.84299987264775));
#29197=CARTESIAN_POINT('Ctrl Pts',(38.703290925861,-34.864747165084,7.89533324843183));
#29198=CARTESIAN_POINT('Ctrl Pts',(38.4251602751564,-33.5932784036374,7.94766662421592));
#29199=CARTESIAN_POINT('Ctrl Pts',(37.6735319337713,-32.7141668369925,8.));
#29200=CARTESIAN_POINT('',(32.3214996650065,-32.7109746768979,8.));
#29201=CARTESIAN_POINT('Origin',(35.,-35.,8.));
#29202=CARTESIAN_POINT('Ctrl Pts',(32.3214765561793,-32.7109598296518,8.));
#29203=CARTESIAN_POINT('Ctrl Pts',(33.0392495465109,-31.8766737967152,7.95000212253756));
#29204=CARTESIAN_POINT('Ctrl Pts',(34.181330417556,-31.4010809746138,7.90000424507511));
#29205=CARTESIAN_POINT('Ctrl Pts',(35.2782977952799,-31.4881472942925,7.85000636761267));
#29206=CARTESIAN_POINT('Ctrl Pts',(36.4265066576347,-31.5792806514897,7.79767299182859));
#29207=CARTESIAN_POINT('Ctrl Pts',(37.5252889103119,-32.2868666869212,7.74533961604451));
#29208=CARTESIAN_POINT('Ctrl Pts',(38.0826699468004,-33.2944463733222,7.69300624026042));
#29209=CARTESIAN_POINT('Ctrl Pts',(38.6400509832889,-34.302026059723,7.64067286447634));
#29210=CARTESIAN_POINT('Ctrl Pts',(38.6560308035887,-35.6095993970933,7.58833948869224));
#29211=CARTESIAN_POINT('Ctrl Pts',(38.1231125366528,-36.6305184803578,7.53600611290816));
#29212=CARTESIAN_POINT('Ctrl Pts',(37.5901942697169,-37.6514375636223,7.48367273712407));
#29213=CARTESIAN_POINT('Ctrl Pts',(36.5083779155453,-38.3857023927811,7.43133936133999));
#29214=CARTESIAN_POINT('Ctrl Pts',(35.3628659911708,-38.5042959466132,7.37900598555591));
#29215=CARTESIAN_POINT('Ctrl Pts',(34.2173540667963,-38.6228895004453,7.32667260977183));
#29216=CARTESIAN_POINT('Ctrl Pts',(33.0081465722189,-38.1258117789507,7.27433923398774));
#29217=CARTESIAN_POINT('Ctrl Pts',(32.2773155686706,-37.2358335624551,7.22200585820366));
#29218=CARTESIAN_POINT('Ctrl Pts',(31.7679567703675,-36.6155557791246,7.18553167296643));
#29219=CARTESIAN_POINT('Ctrl Pts',(31.4909698285316,-35.80442618944,7.1490574877292));
#29220=CARTESIAN_POINT('Ctrl Pts',(31.4846885160394,-34.9971888045819,7.11258330249198));
#29221=CARTESIAN_POINT('Origin',(-35.,35.,10.2084234471775));
#29222=CARTESIAN_POINT('',(-39.0787305107814,35.0019482814736,0.791576552822544));
#29223=CARTESIAN_POINT('',(-39.0671617292797,34.9998409589035,0.708423447177453));
#29224=CARTESIAN_POINT('',(-39.0735,35.0000000000001,10.2084234471775));
#29225=CARTESIAN_POINT('',(-33.9479286229388,31.0647048309474,0.));
#29226=CARTESIAN_POINT('Ctrl Pts',(-39.0671617292797,34.9998409589035,0.708423447177453));
#29227=CARTESIAN_POINT('Ctrl Pts',(-39.0667162804106,35.6885579272407,0.68161580125464));
#29228=CARTESIAN_POINT('Ctrl Pts',(-38.5762700272017,37.7222374436051,0.602474779547742));
#29229=CARTESIAN_POINT('Ctrl Pts',(-35.379526836985,39.7808556694562,0.471000382056761));
#29230=CARTESIAN_POINT('Ctrl Pts',(-31.2187001848465,37.9557862959725,0.314000254704507));
#29231=CARTESIAN_POINT('Ctrl Pts',(-30.4549372314006,33.4726351387477,0.157000127352253));
#29232=CARTESIAN_POINT('Ctrl Pts',(-32.6539236935135,31.4106472544613,0.0523333757840845));
#29233=CARTESIAN_POINT('Ctrl Pts',(-33.9479286229388,31.0647048309474,0.));
#29234=CARTESIAN_POINT('',(-36.0547197101746,31.058399207452,2.73005324693302E-15));
#29235=CARTESIAN_POINT('Origin',(-35.,35.,0.));
#29236=CARTESIAN_POINT('Ctrl Pts',(-39.0787305107814,35.0019482814736,0.791576552822544));
#29237=CARTESIAN_POINT('Ctrl Pts',(-39.0794137856881,35.117415240318,0.787049082480477));
#29238=CARTESIAN_POINT('Ctrl Pts',(-39.0230450544057,36.5668924114048,0.730188236354325));
#29239=CARTESIAN_POINT('Ctrl Pts',(-37.2955092110801,39.2117686241983,0.620994014444089));
#29240=CARTESIAN_POINT('Ctrl Pts',(-32.7531819533668,39.2384377406302,0.463993887091835));
#29241=CARTESIAN_POINT('Ctrl Pts',(-30.2257196451616,35.46328448449,0.306993759739582));
#29242=CARTESIAN_POINT('Ctrl Pts',(-31.9530720002325,31.3373697401077,0.152329130708971));
#29243=CARTESIAN_POINT('Ctrl Pts',(-34.822442511108,30.7329994872565,0.0499978774624443));
#29244=CARTESIAN_POINT('Ctrl Pts',(-36.0547320440515,31.0583698407595,2.40774197454718E-15));
#29245=CARTESIAN_POINT('Origin',(-35.,35.,10.2084234471775));
#29246=CARTESIAN_POINT('',(-39.0674335213841,35.0009171557363,1.79157655282254));
#29247=CARTESIAN_POINT('',(-39.0778197532985,34.9975078784707,1.70842344717745));
#29248=CARTESIAN_POINT('',(-39.0735,35.0000000000001,10.2084234471775));
#29249=CARTESIAN_POINT('Ctrl Pts',(-39.0778197532985,34.9975078784707,1.70842344717745));
#29250=CARTESIAN_POINT('Ctrl Pts',(-39.0692748471557,36.1749702057365,1.66228272262582));
#29251=CARTESIAN_POINT('Ctrl Pts',(-37.9187924724061,38.702508200362,1.56380862229009));
#29252=CARTESIAN_POINT('Ctrl Pts',(-33.6495204180096,39.602789266723,1.41300114617028));
#29253=CARTESIAN_POINT('Ctrl Pts',(-30.4158794824773,36.4127281948833,1.25600101881803));
#29254=CARTESIAN_POINT('Ctrl Pts',(-31.2929570903083,31.9557501199225,1.09900089146578));
#29255=CARTESIAN_POINT('Ctrl Pts',(-35.4939869156159,30.2288018345407,0.942000764113521));
#29256=CARTESIAN_POINT('Ctrl Pts',(-38.6106822216958,32.3442076080298,0.811808282684081));
#29257=CARTESIAN_POINT('Ctrl Pts',(-39.0675858772087,34.3440577791618,0.733949177038725));
#29258=CARTESIAN_POINT('Ctrl Pts',(-39.0671617292797,34.9998409589035,0.708423447177453));
#29259=CARTESIAN_POINT('Ctrl Pts',(-39.0674335213841,35.0009171557363,1.79157655282255));
#29260=CARTESIAN_POINT('Ctrl Pts',(-39.0686948832473,35.6137985390812,1.76771600385165));
#29261=CARTESIAN_POINT('Ctrl Pts',(-38.6530957043657,37.569289309386,1.69152207909667));
#29262=CARTESIAN_POINT('Ctrl Pts',(-35.6435862778458,39.7534633517259,1.56299477855761));
#29263=CARTESIAN_POINT('Ctrl Pts',(-31.3902652615342,38.1590329639038,1.40599465120536));
#29264=CARTESIAN_POINT('Ctrl Pts',(-30.3738298371754,33.7318498284919,1.2489945238531));
#29265=CARTESIAN_POINT('Ctrl Pts',(-33.5057219097166,30.4418645346457,1.09199439650085));
#29266=CARTESIAN_POINT('Ctrl Pts',(-37.8485989831919,31.216140614721,0.939521739490665));
#29267=CARTESIAN_POINT('Ctrl Pts',(-39.0715157588091,33.7827238362241,0.839382458264561));
#29268=CARTESIAN_POINT('Ctrl Pts',(-39.0787305107814,35.0019482814736,0.791576552822544));
#29269=CARTESIAN_POINT('Origin',(-35.,35.,10.2084234471775));
#29270=CARTESIAN_POINT('',(-39.0758431739381,34.9967917635303,2.79157655282255));
#29271=CARTESIAN_POINT('',(-39.0728768523265,35.0035058195583,2.70842344717746));
#29272=CARTESIAN_POINT('',(-39.0735,35.0000000000001,10.2084234471775));
#29273=CARTESIAN_POINT('Ctrl Pts',(-39.0728768523265,35.0035058195583,2.70842344717746));
#29274=CARTESIAN_POINT('Ctrl Pts',(-39.075803367569,35.3398899970603,2.69528301978107));
#29275=CARTESIAN_POINT('Ctrl Pts',(-38.8850706886071,37.0126939576436,2.62980921660061));
#29276=CARTESIAN_POINT('Ctrl Pts',(-36.5844982252159,39.5275826001387,2.51200203763606));
#29277=CARTESIAN_POINT('Ctrl Pts',(-32.0977201830868,38.819215512031,2.3550019102838));
#29278=CARTESIAN_POINT('Ctrl Pts',(-30.2134435993119,34.6861220528707,2.19800178293155));
#29279=CARTESIAN_POINT('Ctrl Pts',(-32.6213194634248,30.8344843115421,2.04100165557929));
#29280=CARTESIAN_POINT('Ctrl Pts',(-37.1621781583154,30.7181077707172,1.88400152822704));
#29281=CARTESIAN_POINT('Ctrl Pts',(-38.9994901450348,33.3471191547144,1.77314212542643));
#29282=CARTESIAN_POINT('Ctrl Pts',(-39.0789665845212,34.8394779904932,1.7146160984099));
#29283=CARTESIAN_POINT('Ctrl Pts',(-39.0778197532985,34.9975078784707,1.70842344717745));
#29284=CARTESIAN_POINT('Ctrl Pts',(-39.0758431739381,34.9967917635303,2.79157655282255));
#29285=CARTESIAN_POINT('Ctrl Pts',(-39.0663194813852,36.100441948558,2.74838292522283));
#29286=CARTESIAN_POINT('Ctrl Pts',(-38.0375439399374,38.5569291706849,2.65285592183902));
#29287=CARTESIAN_POINT('Ctrl Pts',(-33.9071518161688,39.6706875589806,2.50499554267113));
#29288=CARTESIAN_POINT('Ctrl Pts',(-30.5014136769744,36.6650408935442,2.34799541531887));
#29289=CARTESIAN_POINT('Ctrl Pts',(-31.1296010783918,32.1663358219723,2.19099528796663));
#29290=CARTESIAN_POINT('Ctrl Pts',(-35.2284122688067,30.2086051339802,2.03399516061437));
#29291=CARTESIAN_POINT('Ctrl Pts',(-38.5306034134223,32.1919236036427,1.90085558223301));
#29292=CARTESIAN_POINT('Ctrl Pts',(-39.0659283364897,34.2695649347001,1.82004937963574));
#29293=CARTESIAN_POINT('Ctrl Pts',(-39.0674335213841,35.0009171557363,1.79157655282255));
#29294=CARTESIAN_POINT('Origin',(-35.,35.,10.2084234471775));
#29295=CARTESIAN_POINT('',(-39.0750714879939,35.0033643604342,3.79157655282255));
#29296=CARTESIAN_POINT('',(-39.0687106773974,34.997673386605,3.70842344717746));
#29297=CARTESIAN_POINT('',(-39.0735,35.0000000000001,10.2084234471775));
#29298=CARTESIAN_POINT('Ctrl Pts',(-39.0687106773974,34.997673386605,3.70842344717746));
#29299=CARTESIAN_POINT('Ctrl Pts',(-39.0642691067062,35.8311293539699,3.67594994115225));
#29300=CARTESIAN_POINT('Ctrl Pts',(-38.4124444982778,38.0141380355395,3.59114305934295));
#29301=CARTESIAN_POINT('Ctrl Pts',(-34.866781479659,39.7949860223284,3.45400280174958));
#29302=CARTESIAN_POINT('Ctrl Pts',(-30.9271141000824,37.5340162820022,3.29700267439732));
#29303=CARTESIAN_POINT('Ctrl Pts',(-30.6396425700269,33.0007698436185,3.14000254704507));
#29304=CARTESIAN_POINT('Ctrl Pts',(-34.2621453998186,30.2602522415144,2.98300241969281));
#29305=CARTESIAN_POINT('Ctrl Pts',(-38.1877198129624,31.6435581024348,2.83914271973695));
#29306=CARTESIAN_POINT('Ctrl Pts',(-39.064148159005,34.0001984453322,2.74761639556516));
#29307=CARTESIAN_POINT('Ctrl Pts',(-39.0728768523265,35.0035058195583,2.70842344717746));
#29308=CARTESIAN_POINT('Ctrl Pts',(-39.0750714879939,35.0033643604342,3.79157655282255));
#29309=CARTESIAN_POINT('Ctrl Pts',(-39.0773736113907,35.2639441995514,3.78138322237809));
#29310=CARTESIAN_POINT('Ctrl Pts',(-38.9368585171591,36.8598904257655,3.71885651614954));
#29311=CARTESIAN_POINT('Ctrl Pts',(-36.8334386787628,39.4326225179073,3.6039964341369));
#29312=CARTESIAN_POINT('Ctrl Pts',(-32.314250849668,38.9744674195804,3.44699630678465));
#29313=CARTESIAN_POINT('Ctrl Pts',(-30.2034000494222,34.9523692588031,3.2899961794324));
#29314=CARTESIAN_POINT('Ctrl Pts',(-32.3937064417451,30.9729820366429,3.13299605208014));
#29315=CARTESIAN_POINT('Ctrl Pts',(-36.9211012705904,30.6046604636344,2.97599592472789));
#29316=CARTESIAN_POINT('Ctrl Pts',(-38.9541946698804,33.1946779489209,2.86218942497536));
#29317=CARTESIAN_POINT('Ctrl Pts',(-39.0778583821194,34.7632599826793,2.80071630100691));
#29318=CARTESIAN_POINT('Ctrl Pts',(-39.0758431739381,34.9967917635303,2.79157655282255));
#29319=CARTESIAN_POINT('Origin',(-35.,35.,10.2084234471775));
#29320=CARTESIAN_POINT('',(-39.0676600758127,34.9986811552388,4.79157655282255));
#29321=CARTESIAN_POINT('',(-39.0799225868021,34.9997610328513,4.70842344717746));
#29322=CARTESIAN_POINT('',(-39.0735,35.0000000000001,10.2084234471775));
#29323=CARTESIAN_POINT('Ctrl Pts',(-39.0799225868021,34.9997610328513,4.70842344717746));
#29324=CARTESIAN_POINT('Ctrl Pts',(-39.0787768922257,36.3199995443189,4.65661686252342));
#29325=CARTESIAN_POINT('Ctrl Pts',(-37.6705855754179,38.9760045490164,4.5524769020853));
#29326=CARTESIAN_POINT('Ctrl Pts',(-33.1665613873943,39.4326223579625,4.3960035658631));
#29327=CARTESIAN_POINT('Ctrl Pts',(-30.2914357144823,35.9160024456566,4.23900343851084));
#29328=CARTESIAN_POINT('Ctrl Pts',(-31.6385248082081,31.5779943532675,4.08200331115859));
#29329=CARTESIAN_POINT('Ctrl Pts',(-35.9998809552364,30.3085315529294,3.92500318380634));
#29330=CARTESIAN_POINT('Ctrl Pts',(-38.7479935181635,32.6383846484188,3.80047656247929));
#29331=CARTESIAN_POINT('Ctrl Pts',(-39.0714270153063,34.4879554969268,3.72828331693633));
#29332=CARTESIAN_POINT('Ctrl Pts',(-39.0687106773974,34.997673386605,3.70842344717746));
#29333=CARTESIAN_POINT('Ctrl Pts',(-39.0676600758127,34.9986811552388,4.79157655282255));
#29334=CARTESIAN_POINT('Ctrl Pts',(-39.065407375266,35.756989657491,4.76205014374926));
#29335=CARTESIAN_POINT('Ctrl Pts',(-38.500581632009,37.8624610972284,4.68019035889188));
#29336=CARTESIAN_POINT('Ctrl Pts',(-35.1332185251462,39.7949861953461,4.54599719825043));
#29337=CARTESIAN_POINT('Ctrl Pts',(-31.0740926686951,37.7562458887763,4.38899707089817));
#29338=CARTESIAN_POINT('Ctrl Pts',(-30.5353655822401,33.2459534545604,4.23199694354592));
#29339=CARTESIAN_POINT('Ctrl Pts',(-34.0001190086845,30.3085313836444,4.07499681619366));
#29340=CARTESIAN_POINT('Ctrl Pts',(-38.0783115555367,31.4955735687615,3.92819001928588));
#29341=CARTESIAN_POINT('Ctrl Pts',(-39.0655543252915,33.9261064127185,3.83371659816217));
#29342=CARTESIAN_POINT('Ctrl Pts',(-39.0750714879939,35.0033643604342,3.79157655282255));
#29343=CARTESIAN_POINT('Origin',(-35.,35.,10.2084234471775));
#29344=CARTESIAN_POINT('',(-39.0792021698116,34.998483879503,5.79157655282255));
#29345=CARTESIAN_POINT('',(-39.0692228089002,35.0026290967949,5.70842344717746));
#29346=CARTESIAN_POINT('',(-39.0735,35.0000000000001,10.2084234471775));
#29347=CARTESIAN_POINT('Ctrl Pts',(-39.0692228089002,35.0026290967949,5.70842344717746));
#29348=CARTESIAN_POINT('Ctrl Pts',(-39.0721535526687,35.4851530378365,5.68961715967868));
#29349=CARTESIAN_POINT('Ctrl Pts',(-38.7712970745332,37.3068911247937,5.61847749639582));
#29350=CARTESIAN_POINT('Ctrl Pts',(-36.092848144401,39.6706873903976,5.49500445732886));
#29351=CARTESIAN_POINT('Ctrl Pts',(-31.7071427262397,38.4880838865661,5.33800432997662));
#29352=CARTESIAN_POINT('Ctrl Pts',(-30.2741740089879,34.1776820335287,5.18100420262436));
#29353=CARTESIAN_POINT('Ctrl Pts',(-33.0788987987297,30.6046606222411,5.02400407527212));
#29354=CARTESIAN_POINT('Ctrl Pts',(-37.6062934642105,30.9729821819491,4.86700394791985));
#29355=CARTESIAN_POINT('Ctrl Pts',(-39.073846927859,33.6392591565121,4.76181040522164));
#29356=CARTESIAN_POINT('Ctrl Pts',(-39.0799342367062,34.9863362926946,4.70895023830751));
#29357=CARTESIAN_POINT('Ctrl Pts',(-39.0799225868021,34.9997610328513,4.70842344717746));
#29358=CARTESIAN_POINT('Ctrl Pts',(-39.0792021698116,34.998483879503,5.79157655282255));
#29359=CARTESIAN_POINT('Ctrl Pts',(-39.0731676328035,36.2442079435004,5.74271706512043));
#29360=CARTESIAN_POINT('Ctrl Pts',(-37.8030025161425,38.8348894467969,5.64152420163423));
#29361=CARTESIAN_POINT('Ctrl Pts',(-33.4155017175264,39.5275827633586,5.48799796236395));
#29362=CARTESIAN_POINT('Ctrl Pts',(-30.3495579785441,36.176022571197,5.33099783501169));
#29363=CARTESIAN_POINT('Ctrl Pts',(-31.4537103860929,31.7699118586619,5.17399770765944));
#29364=CARTESIAN_POINT('Ctrl Pts',(-35.7378546268185,30.2602520705083,5.01699758030719));
#29365=CARTESIAN_POINT('Ctrl Pts',(-38.6790874120226,32.4853711659013,4.88952386202822));
#29366=CARTESIAN_POINT('Ctrl Pts',(-39.0694001203352,34.4129439352318,4.81438351953334));
#29367=CARTESIAN_POINT('Ctrl Pts',(-39.0676600758127,34.9986811552388,4.79157655282255));
#29368=CARTESIAN_POINT('Origin',(-35.,35.,10.2084234471775));
#29369=CARTESIAN_POINT('',(-39.070966199943,35.0032555604945,6.79157655282255));
#29370=CARTESIAN_POINT('',(-39.0721136942453,34.9965451882256,6.70842344717746));
#29371=CARTESIAN_POINT('',(-39.0735,35.0000000000001,10.2084234471775));
#29372=CARTESIAN_POINT('Ctrl Pts',(-39.0721136942453,34.9965451882256,6.70842344717746));
#29373=CARTESIAN_POINT('Ctrl Pts',(-39.0638859499781,35.9733493601025,6.67028408104985));
#29374=CARTESIAN_POINT('Ctrl Pts',(-38.2252019424137,38.3031815231405,6.57981133913817));
#29375=CARTESIAN_POINT('Ctrl Pts',(-34.3564137457339,39.7534631780217,6.4370052214424));
#29376=CARTESIAN_POINT('Ctrl Pts',(-30.6802037555765,37.0854262040492,6.28000509409013));
#29377=CARTESIAN_POINT('Ctrl Pts',(-30.8775960516807,32.5473632088007,6.12300496673789));
#29378=CARTESIAN_POINT('Ctrl Pts',(-34.7715877393978,30.2086053071985,5.96600483938563));
#29379=CARTESIAN_POINT('Ctrl Pts',(-38.3794219899756,31.9318288223888,5.82781099953215));
#29380=CARTESIAN_POINT('Ctrl Pts',(-39.0639979975134,34.142404941861,5.74195053546276));
#29381=CARTESIAN_POINT('Ctrl Pts',(-39.0692228089002,35.0026290967949,5.70842344717746));
#29382=CARTESIAN_POINT('Ctrl Pts',(-39.070966199943,35.0032555604945,6.79157655282255));
#29383=CARTESIAN_POINT('Ctrl Pts',(-39.0741290517156,35.409727295843,6.77571736227569));
#29384=CARTESIAN_POINT('Ctrl Pts',(-38.8328829256554,37.1538415310843,6.70752479594475));
#29385=CARTESIAN_POINT('Ctrl Pts',(-36.3504796357983,39.6027894460767,6.58699885382972));
#29386=CARTESIAN_POINT('Ctrl Pts',(-31.905897053523,38.6655398223873,6.42999872647746));
#29387=CARTESIAN_POINT('Ctrl Pts',(-30.2358031812474,34.4413383659989,6.27299859912522));
#29388=CARTESIAN_POINT('Ctrl Pts',(-32.8378217627235,30.7181076142107,6.11599847177296));
#29389=CARTESIAN_POINT('Ctrl Pts',(-37.3786806229274,30.8344841622903,5.95899834442071));
#29390=CARTESIAN_POINT('Ctrl Pts',(-39.0372095034026,33.4874666211437,5.85085770477057));
#29391=CARTESIAN_POINT('Ctrl Pts',(-39.0796312227382,34.9099134465561,5.79505044090451));
#29392=CARTESIAN_POINT('Ctrl Pts',(-39.0792021698116,34.998483879503,5.79157655282255));
#29393=CARTESIAN_POINT('Origin',(-35.,35.,10.2084234471775));
#29394=CARTESIAN_POINT('',(-39.0691248821302,34.9959228837483,7.79157655282255));
#29395=CARTESIAN_POINT('',(-39.0784090602678,35.0020440536087,7.70842344717746));
#29396=CARTESIAN_POINT('',(-39.0735,35.0000000000001,10.2084234471775));
#29397=CARTESIAN_POINT('',(-36.0520713770612,31.0647048309474,8.));
#29398=CARTESIAN_POINT('Ctrl Pts',(-36.0520713770612,31.0647048309474,8.));
#29399=CARTESIAN_POINT('Ctrl Pts',(-37.3460763064866,31.4106472544613,7.94766662421592));
#29400=CARTESIAN_POINT('Ctrl Pts',(-38.8056938328118,32.7793309690615,7.87819214182344));
#29401=CARTESIAN_POINT('Ctrl Pts',(-39.0721267560147,34.5563414191054,7.80871765943095));
#29402=CARTESIAN_POINT('Ctrl Pts',(-39.0691248821302,34.9959228837483,7.79157655282255));
#29403=CARTESIAN_POINT('',(-33.9452804362612,31.0583992034428,8.));
#29404=CARTESIAN_POINT('Origin',(-35.,35.,8.));
#29405=CARTESIAN_POINT('Ctrl Pts',(-33.9452681066883,31.058369845356,8.));
#29406=CARTESIAN_POINT('Ctrl Pts',(-35.1775577544271,30.7329993831125,7.95000212253756));
#29407=CARTESIAN_POINT('Ctrl Pts',(-37.9028280459028,31.3070187859893,7.85280993826337));
#29408=CARTESIAN_POINT('Ctrl Pts',(-39.0706571061612,33.7983874965128,7.7556177539892));
#29409=CARTESIAN_POINT('Ctrl Pts',(-39.0784090602678,35.0020440536087,7.70842344717747));
#29410=CARTESIAN_POINT('Origin',(35.,-35.,10.2084234471775));
#29411=CARTESIAN_POINT('',(30.9212701195312,-34.9980516557686,0.791576552822542));
#29412=CARTESIAN_POINT('',(30.9328376585755,-35.000159236028,0.708423447177449));
#29413=CARTESIAN_POINT('',(30.9265,-34.9999999999999,10.2084234471775));
#29414=CARTESIAN_POINT('',(36.0520713770612,-38.9352951690526,0.));
#29415=CARTESIAN_POINT('Ctrl Pts',(30.9328376585755,-35.000159236028,0.708423447177449));
#29416=CARTESIAN_POINT('Ctrl Pts',(30.9332830863018,-34.31144230346,0.681615801254637));
#29417=CARTESIAN_POINT('Ctrl Pts',(31.423729341332,-32.2777627653814,0.602474779547741));
#29418=CARTESIAN_POINT('Ctrl Pts',(34.6204730639081,-30.2191415991965,0.471000382056761));
#29419=CARTESIAN_POINT('Ctrl Pts',(38.7813009234074,-32.0442168078902,0.314000254704507));
#29420=CARTESIAN_POINT('Ctrl Pts',(39.5450614875854,-36.5273565705141,0.157000127352254));
#29421=CARTESIAN_POINT('Ctrl Pts',(37.3460763064866,-38.5893527455387,0.0523333757840845));
#29422=CARTESIAN_POINT('Ctrl Pts',(36.0520713770612,-38.9352951690526,0.));
#29423=CARTESIAN_POINT('',(33.9452809380949,-38.9416008127442,2.82508323912273E-15));
#29424=CARTESIAN_POINT('Origin',(35.,-35.,0.));
#29425=CARTESIAN_POINT('Ctrl Pts',(30.9212701195312,-34.9980516557686,0.791576552822542));
#29426=CARTESIAN_POINT('Ctrl Pts',(30.9205868455494,-34.8825847167923,0.787049082480475));
#29427=CARTESIAN_POINT('Ctrl Pts',(30.9769555821544,-33.4331078068366,0.730188236354323));
#29428=CARTESIAN_POINT('Ctrl Pts',(32.704491289799,-30.7882324000235,0.620994014444087));
#29429=CARTESIAN_POINT('Ctrl Pts',(37.2468174060219,-30.7615623188695,0.463993887091833));
#29430=CARTESIAN_POINT('Ctrl Pts',(39.7742801854456,-34.536716632844,0.306993759739581));
#29431=CARTESIAN_POINT('Ctrl Pts',(38.0469263053514,-38.6626279973746,0.152329130708969));
#29432=CARTESIAN_POINT('Ctrl Pts',(35.1775586628442,-39.2670009745688,0.0499978774624438));
#29433=CARTESIAN_POINT('Ctrl Pts',(33.94526862329,-38.9416301412996,2.47469145869816E-15));
#29434=CARTESIAN_POINT('Origin',(35.,-35.,10.2084234471775));
#29435=CARTESIAN_POINT('',(30.9325671258701,-34.9990828432724,1.79157655282254));
#29436=CARTESIAN_POINT('',(30.9221796304986,-35.0024921194124,1.70842344717745));
#29437=CARTESIAN_POINT('',(30.9265,-34.9999999999999,10.2084234471775));
#29438=CARTESIAN_POINT('Ctrl Pts',(30.9221796304986,-35.0024921194124,1.70842344717745));
#29439=CARTESIAN_POINT('Ctrl Pts',(30.9307245358113,-33.8250296189916,1.66228272262581));
#29440=CARTESIAN_POINT('Ctrl Pts',(32.0812070745664,-31.2974912653129,1.56380862229009));
#29441=CARTESIAN_POINT('Ctrl Pts',(36.3504798077544,-30.397209980765,1.41300114617028));
#29442=CARTESIAN_POINT('Ctrl Pts',(39.5841211762074,-33.5872716944053,1.25600101881803));
#29443=CARTESIAN_POINT('Ctrl Pts',(38.7070435276578,-38.0442501505519,1.09900089146578));
#29444=CARTESIAN_POINT('Ctrl Pts',(34.5060129254091,-39.7711992366401,0.942000764113522));
#29445=CARTESIAN_POINT('Ctrl Pts',(31.3893173078737,-37.6557923296961,0.811808282684079));
#29446=CARTESIAN_POINT('Ctrl Pts',(30.9324135307783,-35.6559423817109,0.733949177038721));
#29447=CARTESIAN_POINT('Ctrl Pts',(30.9328376585755,-35.000159236028,0.708423447177449));
#29448=CARTESIAN_POINT('Ctrl Pts',(30.9325671258701,-34.9990828432724,1.79157655282254));
#29449=CARTESIAN_POINT('Ctrl Pts',(30.931305764143,-34.3862015569849,1.76771600385165));
#29450=CARTESIAN_POINT('Ctrl Pts',(31.3469048767902,-32.4307110971121,1.69152207909667));
#29451=CARTESIAN_POINT('Ctrl Pts',(34.3564138261785,-30.2465374145616,1.56299477855761));
#29452=CARTESIAN_POINT('Ctrl Pts',(38.6097341605507,-31.8409675209513,1.40599465120535));
#29453=CARTESIAN_POINT('Ctrl Pts',(39.6261694334752,-36.2681500029269,1.2489945238531));
#29454=CARTESIAN_POINT('Ctrl Pts',(36.4942778376799,-39.5581346787212,1.09199439650085));
#29455=CARTESIAN_POINT('Ctrl Pts',(32.1514014998571,-38.7838588891191,0.939521739490662));
#29456=CARTESIAN_POINT('Ctrl Pts',(30.928484861737,-36.2172758912295,0.839382458264559));
#29457=CARTESIAN_POINT('Ctrl Pts',(30.9212701195312,-34.9980516557686,0.791576552822542));
#29458=CARTESIAN_POINT('Origin',(35.,-35.,10.2084234471775));
#29459=CARTESIAN_POINT('',(30.9241574748343,-35.0032082359637,2.79157655282255));
#29460=CARTESIAN_POINT('',(30.9271225309901,-34.9964941798068,2.70842344717745));
#29461=CARTESIAN_POINT('',(30.9265,-34.9999999999999,10.2084234471775));
#29462=CARTESIAN_POINT('Ctrl Pts',(30.9271225309901,-34.9964941798068,2.70842344717745));
#29463=CARTESIAN_POINT('Ctrl Pts',(30.9241960153079,-34.6601099513618,2.69528301978107));
#29464=CARTESIAN_POINT('Ctrl Pts',(31.1149287231428,-32.9873057374911,2.62980921660061));
#29465=CARTESIAN_POINT('Ctrl Pts',(33.4155015345008,-30.4724167149005,2.51200203763606));
#29466=CARTESIAN_POINT('Ctrl Pts',(37.9022802570419,-31.180783908422,2.3550019102838));
#29467=CARTESIAN_POINT('Ctrl Pts',(39.7865571243079,-35.3138779969793,2.19800178293155));
#29468=CARTESIAN_POINT('Ctrl Pts',(37.3786808989502,-39.1655163148135,2.04100165557929));
#29469=CARTESIAN_POINT('Ctrl Pts',(32.8378215103303,-39.2818928860424,1.88400152822704));
#29470=CARTESIAN_POINT('Ctrl Pts',(31.0005092531499,-36.6528810868796,1.77314212542643));
#29471=CARTESIAN_POINT('Ctrl Pts',(30.9210327993872,-35.1605220306295,1.7146160984099));
#29472=CARTESIAN_POINT('Ctrl Pts',(30.9221796304986,-35.0024921194124,1.70842344717745));
#29473=CARTESIAN_POINT('Ctrl Pts',(30.9241574748343,-35.0032082359637,2.79157655282255));
#29474=CARTESIAN_POINT('Ctrl Pts',(30.9336811658698,-33.8995582265895,2.74838292522282));
#29475=CARTESIAN_POINT('Ctrl Pts',(31.9624565435572,-31.4430713953983,2.65285592183902));
#29476=CARTESIAN_POINT('Ctrl Pts',(36.092848009894,-30.329313184686,2.50499554267113));
#29477=CARTESIAN_POINT('Ctrl Pts',(39.4985856069267,-33.3349593710879,2.34799541531888));
#29478=CARTESIAN_POINT('Ctrl Pts',(38.8703983056154,-37.8336637277424,2.19099528796662));
#29479=CARTESIAN_POINT('Ctrl Pts',(34.7715877673847,-39.7913941019012,2.03399516061437));
#29480=CARTESIAN_POINT('Ctrl Pts',(31.4693971488356,-37.8080759514836,1.90085558223301));
#29481=CARTESIAN_POINT('Ctrl Pts',(30.9340723106019,-35.73043494849,1.82004937963573));
#29482=CARTESIAN_POINT('Ctrl Pts',(30.9325671258701,-34.9990828432724,1.79157655282254));
#29483=CARTESIAN_POINT('Origin',(35.,-35.,10.2084234471775));
#29484=CARTESIAN_POINT('',(30.9249291606556,-34.9966356401017,3.79157655282255));
#29485=CARTESIAN_POINT('',(30.9312887064921,-35.0023266137465,3.70842344717745));
#29486=CARTESIAN_POINT('',(30.9265,-34.9999999999999,10.2084234471775));
#29487=CARTESIAN_POINT('Ctrl Pts',(30.9312887064921,-35.0023266137465,3.70842344717745));
#29488=CARTESIAN_POINT('Ctrl Pts',(30.9357302778565,-34.1688705201733,3.67594994115225));
#29489=CARTESIAN_POINT('Ctrl Pts',(31.5875549849899,-31.9858615080358,3.59114305934295));
#29490=CARTESIAN_POINT('Ctrl Pts',(35.1332185405061,-30.2050132515957,3.45400280174957));
#29491=CARTESIAN_POINT('Ctrl Pts',(39.0728865166754,-32.4659833342563,3.29700267439732));
#29492=CARTESIAN_POINT('Ctrl Pts',(39.3603580902194,-36.9992304591644,3.14000254704507));
#29493=CARTESIAN_POINT('Ctrl Pts',(35.7378547119649,-39.73974847612,2.98300241969282));
#29494=CARTESIAN_POINT('Ctrl Pts',(31.8122797042457,-38.3564424059702,2.83914271973694));
#29495=CARTESIAN_POINT('Ctrl Pts',(30.9358512256228,-35.9998017059771,2.74761639556516));
#29496=CARTESIAN_POINT('Ctrl Pts',(30.9271225309901,-34.9964941798068,2.70842344717745));
#29497=CARTESIAN_POINT('Ctrl Pts',(30.9249291606557,-34.9966356401017,3.79157655282255));
#29498=CARTESIAN_POINT('Ctrl Pts',(30.9226270376253,-34.7360558424623,3.78138322237808));
#29499=CARTESIAN_POINT('Ctrl Pts',(31.0631421094905,-33.1401098702831,3.71885651614953));
#29500=CARTESIAN_POINT('Ctrl Pts',(33.1665616130745,-30.567378187653,3.6039964341369));
#29501=CARTESIAN_POINT('Ctrl Pts',(37.6857487228281,-31.0255332130596,3.44699630678465));
#29502=CARTESIAN_POINT('Ctrl Pts',(39.7965991870786,-35.0476307336073,3.28999617943239));
#29503=CARTESIAN_POINT('Ctrl Pts',(37.606293143399,-39.0270173223719,3.13299605208014));
#29504=CARTESIAN_POINT('Ctrl Pts',(33.0788990351993,-39.3953388367078,2.97599592472789));
#29505=CARTESIAN_POINT('Ctrl Pts',(31.0458059595307,-36.8053217637502,2.86218942497536));
#29506=CARTESIAN_POINT('Ctrl Pts',(30.9221422669741,-35.2367399796465,2.80071630100691));
#29507=CARTESIAN_POINT('Ctrl Pts',(30.9241574748343,-35.0032082359637,2.79157655282255));
#29508=CARTESIAN_POINT('Origin',(35.,-35.,10.2084234471775));
#29509=CARTESIAN_POINT('',(30.9323405716502,-35.0013188445396,4.79157655282255));
#29510=CARTESIAN_POINT('',(30.9200767953891,-35.0002389671868,4.70842344717745));
#29511=CARTESIAN_POINT('',(30.9265,-34.9999999999999,10.2084234471775));
#29512=CARTESIAN_POINT('Ctrl Pts',(30.9200767953891,-35.0002389671868,4.70842344717745));
#29513=CARTESIAN_POINT('Ctrl Pts',(30.9212224901389,-33.6800002558017,4.65661686252342));
#29514=CARTESIAN_POINT('Ctrl Pts',(32.3294140201846,-31.0239948489069,4.5524769020853));
#29515=CARTESIAN_POINT('Ctrl Pts',(36.8334388902368,-30.5673769708228,4.39600356586309));
#29516=CARTESIAN_POINT('Ctrl Pts',(39.7085649985197,-34.0839974156347,4.23900343851085));
#29517=CARTESIAN_POINT('Ctrl Pts',(38.3614757008081,-38.4220061649164,4.08200331115859));
#29518=CARTESIAN_POINT('Ctrl Pts',(34.0001188933562,-39.6914691574817,3.92500318380634));
#29519=CARTESIAN_POINT('Ctrl Pts',(31.2520059142893,-37.3616157091949,3.80047656247929));
#29520=CARTESIAN_POINT('Ctrl Pts',(30.9285723681714,-35.5120445806103,3.72828331693633));
#29521=CARTESIAN_POINT('Ctrl Pts',(30.9312887064921,-35.0023266137465,3.70842344717745));
#29522=CARTESIAN_POINT('Ctrl Pts',(30.9323405716502,-35.0013188445396,4.79157655282255));
#29523=CARTESIAN_POINT('Ctrl Pts',(30.9345932718416,-34.2430104629966,4.76205014374926));
#29524=CARTESIAN_POINT('Ctrl Pts',(31.4994189252081,-32.1375393584237,4.68019035889188));
#29525=CARTESIAN_POINT('Ctrl Pts',(34.8667814960507,-30.2050145678827,4.54599719825042));
#29526=CARTESIAN_POINT('Ctrl Pts',(38.9259067064028,-32.2437545499559,4.38899707089817));
#29527=CARTESIAN_POINT('Ctrl Pts',(39.4646337070995,-36.7540462662356,4.23199694354592));
#29528=CARTESIAN_POINT('Ctrl Pts',(35.9998808321606,-39.6914678695931,4.07499681619366));
#29529=CARTESIAN_POINT('Ctrl Pts',(31.921688934453,-38.5044258734202,3.92819001928587));
#29530=CARTESIAN_POINT('Ctrl Pts',(30.934446321843,-36.0738934163447,3.83371659816217));
#29531=CARTESIAN_POINT('Ctrl Pts',(30.9249291606557,-34.9966356401017,3.79157655282255));
#29532=CARTESIAN_POINT('Origin',(35.,-35.,10.2084234471775));
#29533=CARTESIAN_POINT('',(30.9207984791111,-35.0015161195221,5.79157655282255));
#29534=CARTESIAN_POINT('',(30.93077657492,-34.9973709027416,5.70842344717745));
#29535=CARTESIAN_POINT('',(30.9265,-34.9999999999999,10.2084234471775));
#29536=CARTESIAN_POINT('Ctrl Pts',(30.93077657492,-34.9973709027416,5.70842344717745));
#29537=CARTESIAN_POINT('Ctrl Pts',(30.9278458307013,-34.5148468886989,5.68961715967867));
#29538=CARTESIAN_POINT('Ctrl Pts',(31.2287023543687,-32.6931085261371,5.61847749639581));
#29539=CARTESIAN_POINT('Ctrl Pts',(33.9071516901285,-30.3293119021379,5.49500445732887));
#29540=CARTESIAN_POINT('Ctrl Pts',(38.292857772379,-31.5119155853487,5.33800432997662));
#29541=CARTESIAN_POINT('Ctrl Pts',(39.7258267066312,-35.8223180909381,5.18100420262436));
#29542=CARTESIAN_POINT('Ctrl Pts',(36.9211014921746,-39.3953400433581,5.02400407527211));
#29543=CARTESIAN_POINT('Ctrl Pts',(32.3937061411281,-39.0270184278339,4.86700394791986));
#29544=CARTESIAN_POINT('Ctrl Pts',(30.9261524552523,-36.3607410495406,4.76181040522164));
#29545=CARTESIAN_POINT('Ctrl Pts',(30.9200651454832,-35.0136637093765,4.7089502383075));
#29546=CARTESIAN_POINT('Ctrl Pts',(30.9200767953891,-35.0002389671868,4.70842344717745));
#29547=CARTESIAN_POINT('Ctrl Pts',(30.9207984791111,-35.0015161195221,5.79157655282254));
#29548=CARTESIAN_POINT('Ctrl Pts',(30.9268330150145,-33.7557922534996,5.74271706512043));
#29549=CARTESIAN_POINT('Ctrl Pts',(32.1969979306855,-31.1651111648659,5.64152420163423));
#29550=CARTESIAN_POINT('Ctrl Pts',(36.584498029893,-30.4724179566463,5.48799796236395));
#29551=CARTESIAN_POINT('Ctrl Pts',(39.6504412814188,-33.8239776163473,5.33099783501169));
#29552=CARTESIAN_POINT('Ctrl Pts',(38.5462890493217,-38.2300876270061,5.17399770765944));
#29553=CARTESIAN_POINT('Ctrl Pts',(34.2621454906851,-39.7397471751372,5.01699758030718));
#29554=CARTESIAN_POINT('Ctrl Pts',(31.3209131735827,-37.5146284338107,4.88952386202822));
#29555=CARTESIAN_POINT('Ctrl Pts',(30.9306005274021,-35.5870559713077,4.81438351953334));
#29556=CARTESIAN_POINT('Ctrl Pts',(30.9323405716502,-35.0013188445396,4.79157655282255));
#29557=CARTESIAN_POINT('Origin',(35.,-35.,10.2084234471775));
#29558=CARTESIAN_POINT('',(30.9290344477858,-34.9967444478932,6.79157655282255));
#29559=CARTESIAN_POINT('',(30.9278856911952,-35.003454802609,6.70842344717745));
#29560=CARTESIAN_POINT('',(30.9265,-34.9999999999999,10.2084234471775));
#29561=CARTESIAN_POINT('Ctrl Pts',(30.9278856911952,-35.003454802609,6.70842344717745));
#29562=CARTESIAN_POINT('Ctrl Pts',(30.9361134364198,-34.0266504850423,6.67028408104985));
#29563=CARTESIAN_POINT('Ctrl Pts',(31.7747975664789,-31.6968179913154,6.57981133913816));
#29564=CARTESIAN_POINT('Ctrl Pts',(35.6435863532121,-30.2465360930486,6.43700522144239));
#29565=CARTESIAN_POINT('Ctrl Pts',(39.3197968978512,-32.9145734850341,6.28000509409014));
#29566=CARTESIAN_POINT('Ctrl Pts',(39.1224045728929,-37.4526371600059,6.12300496673789));
#29567=CARTESIAN_POINT('Ctrl Pts',(35.2284122950338,-39.7913954197145,5.96600483938562));
#29568=CARTESIAN_POINT('Ctrl Pts',(31.6205774983358,-38.0681716417432,5.82781099953216));
#29569=CARTESIAN_POINT('Ctrl Pts',(30.9360013871094,-35.857595187819,5.74195053546276));
#29570=CARTESIAN_POINT('Ctrl Pts',(30.93077657492,-34.9973709027416,5.70842344717745));
#29571=CARTESIAN_POINT('Ctrl Pts',(30.9290344477858,-34.9967444478932,6.79157655282255));
#29572=CARTESIAN_POINT('Ctrl Pts',(30.9258715916941,-34.5902727617055,6.77571736227569));
#29573=CARTESIAN_POINT('Ctrl Pts',(31.1671176609215,-32.8461587416485,6.70752479594475));
#29574=CARTESIAN_POINT('Ctrl Pts',(33.6495206016122,-30.3972113452741,6.58699885382972));
#29575=CARTESIAN_POINT('Ctrl Pts',(38.09410244091,-31.3344607296745,6.42999872647747));
#29576=CARTESIAN_POINT('Ctrl Pts',(39.7641960678496,-35.558661561786,6.27299859912521));
#29577=CARTESIAN_POINT('Ctrl Pts',(37.1621778889461,-39.2818916953666,6.11599847177296));
#29578=CARTESIAN_POINT('Ctrl Pts',(32.6213197580022,-39.1655151793351,5.95899834442071));
#29579=CARTESIAN_POINT('Ctrl Pts',(30.962791139069,-36.5125331378606,5.85085770477057));
#29580=CARTESIAN_POINT('Ctrl Pts',(30.920369426263,-35.0900865383931,5.79505044090451));
#29581=CARTESIAN_POINT('Ctrl Pts',(30.9207984791111,-35.0015161195221,5.79157655282254));
#29582=CARTESIAN_POINT('Origin',(35.,-35.,10.2084234471775));
#29583=CARTESIAN_POINT('',(30.9308748007386,-35.0040807474719,7.79157655282254));
#29584=CARTESIAN_POINT('',(30.9215903995924,-34.9979557257256,7.70842344717745));
#29585=CARTESIAN_POINT('',(30.9265,-34.9999999999999,10.2084234471775));
#29586=CARTESIAN_POINT('',(33.9479286229388,-38.9352951690526,8.));
#29587=CARTESIAN_POINT('Ctrl Pts',(33.9479286229388,-38.9352951690526,8.));
#29588=CARTESIAN_POINT('Ctrl Pts',(32.6539236935135,-38.5893527455387,7.94766662421592));
#29589=CARTESIAN_POINT('Ctrl Pts',(31.1943052713303,-37.2206748258175,7.87819214182343));
#29590=CARTESIAN_POINT('Ctrl Pts',(30.9278727863252,-35.4436627970733,7.80871765943094));
#29591=CARTESIAN_POINT('Ctrl Pts',(30.9308748007386,-35.0040807474719,7.79157655282254));
#29592=CARTESIAN_POINT('',(36.0547201762178,-38.9416007819636,8.));
#29593=CARTESIAN_POINT('Origin',(35.,-35.,8.));
#29594=CARTESIAN_POINT('Ctrl Pts',(36.0547325237759,-38.9416301760088,8.));
#29595=CARTESIAN_POINT('Ctrl Pts',(34.822443357586,-39.2670001819919,7.95000212253756));
#29596=CARTESIAN_POINT('Ctrl Pts',(32.0971704836176,-38.6929832307492,7.85280993826338));
#29597=CARTESIAN_POINT('Ctrl Pts',(30.9293421550372,-36.2016127302822,7.75561775398919));
#29598=CARTESIAN_POINT('Ctrl Pts',(30.9215903995924,-34.9979557257256,7.70842344717745));
#29599=CARTESIAN_POINT('Origin',(-35.,-35.,10.2084234471775));
#29600=CARTESIAN_POINT('',(-39.0787307957508,-34.998051746757,0.791576552822544));
#29601=CARTESIAN_POINT('',(-39.0671620604938,-35.0001591466914,0.708423447177451));
#29602=CARTESIAN_POINT('',(-39.0735,-34.9999999999999,10.2084234471775));
#29603=CARTESIAN_POINT('',(-33.9479286229388,-38.9352951690526,0.));
#29604=CARTESIAN_POINT('Ctrl Pts',(-39.0671620604938,-35.0001591466914,
0.708423447177451));
#29605=CARTESIAN_POINT('Ctrl Pts',(-39.0667166230717,-34.3114421978074,
0.681615801254639));
#29606=CARTESIAN_POINT('Ctrl Pts',(-38.5762703689089,-32.2777626699106,
0.602474779547742));
#29607=CARTESIAN_POINT('Ctrl Pts',(-35.3795268907121,-30.2191428513895,
0.471000382056761));
#29608=CARTESIAN_POINT('Ctrl Pts',(-31.2186995847689,-32.0442153857854,
0.314000254704507));
#29609=CARTESIAN_POINT('Ctrl Pts',(-30.4549379250093,-36.5273603729133,
0.157000127352253));
#29610=CARTESIAN_POINT('Ctrl Pts',(-32.6539236935135,-38.5893527455387,
0.0523333757840845));
#29611=CARTESIAN_POINT('Ctrl Pts',(-33.9479286229388,-38.9352951690526,
0.));
#29612=CARTESIAN_POINT('',(-36.0547200012553,-38.9416007855471,4.26113251110999E-15));
#29613=CARTESIAN_POINT('Origin',(-35.,-35.,0.));
#29614=CARTESIAN_POINT('Ctrl Pts',(-39.0787307957508,-34.9980517467571,
0.791576552822544));
#29615=CARTESIAN_POINT('Ctrl Pts',(-39.0794140710738,-34.8825847789344,
0.787049082480477));
#29616=CARTESIAN_POINT('Ctrl Pts',(-39.0230453421645,-33.4331074898667,
0.730188236354326));
#29617=CARTESIAN_POINT('Ctrl Pts',(-37.2955094371433,-30.7882309135474,
0.620994014444089));
#29618=CARTESIAN_POINT('Ctrl Pts',(-32.7531816644513,-30.7615622313046,
0.463993887091836));
#29619=CARTESIAN_POINT('Ctrl Pts',(-30.2257195673566,-34.5367150123096,
0.306993759739581));
#29620=CARTESIAN_POINT('Ctrl Pts',(-31.9530712365814,-38.6626312798268,
0.152329130708972));
#29621=CARTESIAN_POINT('Ctrl Pts',(-34.8224430395506,-39.2670003060384,
0.0499978774624443));
#29622=CARTESIAN_POINT('Ctrl Pts',(-36.0547323436802,-38.9416301693299,
2.36437388764776E-15));
#29623=CARTESIAN_POINT('Origin',(-35.,-35.,10.2084234471775));
#29624=CARTESIAN_POINT('',(-39.0674338139571,-34.9990828447087,1.79157655282254));
#29625=CARTESIAN_POINT('',(-39.0778200867196,-35.0024921203811,1.70842344717745));
#29626=CARTESIAN_POINT('',(-39.0735,-34.9999999999999,10.2084234471775));
#29627=CARTESIAN_POINT('Ctrl Pts',(-39.0778200867196,-35.0024921203811,
1.70842344717745));
#29628=CARTESIAN_POINT('Ctrl Pts',(-39.0692751810275,-33.8250296994275,
1.66228272262581));
#29629=CARTESIAN_POINT('Ctrl Pts',(-37.9187927175433,-31.297491510544,1.56380862229009));
#29630=CARTESIAN_POINT('Ctrl Pts',(-33.6495202958365,-30.3972103260493,
1.41300114617028));
#29631=CARTESIAN_POINT('Ctrl Pts',(-30.4158791260905,-33.5872717453,1.25600101881803));
#29632=CARTESIAN_POINT('Ctrl Pts',(-31.2929567559004,-38.0442500262742,
1.09900089146578));
#29633=CARTESIAN_POINT('Ctrl Pts',(-35.4939870016774,-39.7711987453336,
0.942000764113521));
#29634=CARTESIAN_POINT('Ctrl Pts',(-38.6106824762136,-37.6557923579424,
0.81180828268408));
#29635=CARTESIAN_POINT('Ctrl Pts',(-39.0675861975231,-35.6559423079101,
0.733949177038723));
#29636=CARTESIAN_POINT('Ctrl Pts',(-39.0671620604938,-35.0001591466914,
0.708423447177451));
#29637=CARTESIAN_POINT('Ctrl Pts',(-39.0674338139571,-34.9990828447087,
1.79157655282254));
#29638=CARTESIAN_POINT('Ctrl Pts',(-39.0686951758822,-34.3862014174905,
1.76771600385165));
#29639=CARTESIAN_POINT('Ctrl Pts',(-38.6530959670617,-32.4307105068614,
1.69152207909667));
#29640=CARTESIAN_POINT('Ctrl Pts',(-35.6435863248602,-30.2465363019221,
1.56299477855761));
#29641=CARTESIAN_POINT('Ctrl Pts',(-31.3902650003177,-31.8409668168855,
1.40599465120536));
#29642=CARTESIAN_POINT('Ctrl Pts',(-30.3738295074692,-36.2681502477922,
1.2489945238531));
#29643=CARTESIAN_POINT('Ctrl Pts',(-33.5057217955833,-39.5581358207848,
1.09199439650085));
#29644=CARTESIAN_POINT('Ctrl Pts',(-37.8485992014502,-38.7838596097918,
0.939521739490664));
#29645=CARTESIAN_POINT('Ctrl Pts',(-39.0715160393823,-36.2172762868091,
0.839382458264562));
#29646=CARTESIAN_POINT('Ctrl Pts',(-39.0787307957508,-34.9980517467571,
0.791576552822544));
#29647=CARTESIAN_POINT('Origin',(-35.,-35.,10.2084234471775));
#29648=CARTESIAN_POINT('',(-39.0758434671966,-35.0032082366984,2.79157655282255));
#29649=CARTESIAN_POINT('',(-39.0728771860086,-34.996494180098,2.70842344717745));
#29650=CARTESIAN_POINT('',(-39.0735,-34.9999999999999,10.2084234471775));
#29651=CARTESIAN_POINT('Ctrl Pts',(-39.0728771860086,-34.996494180098,2.70842344717745));
#29652=CARTESIAN_POINT('Ctrl Pts',(-39.075803701489,-34.6601099750312,2.69528301978107));
#29653=CARTESIAN_POINT('Ctrl Pts',(-38.8850710069041,-32.9873058773963,
2.62980921660061));
#29654=CARTESIAN_POINT('Ctrl Pts',(-36.5844983552314,-30.4724170292356,
2.51200203763606));
#29655=CARTESIAN_POINT('Ctrl Pts',(-32.0977199449364,-31.1807841743797,
2.3550019102838));
#29656=CARTESIAN_POINT('Ctrl Pts',(-30.2134432077683,-35.3138779741053,
2.19800178293155));
#29657=CARTESIAN_POINT('Ctrl Pts',(-32.621319267345,-39.1655160273689,2.04100165557929));
#29658=CARTESIAN_POINT('Ctrl Pts',(-37.1621783376115,-39.2818925846584,
1.88400152822705));
#29659=CARTESIAN_POINT('Ctrl Pts',(-38.9994904706692,-36.6528809760016,
1.77314212542643));
#29660=CARTESIAN_POINT('Ctrl Pts',(-39.0789669178819,-35.1605220209328,
1.7146160984099));
#29661=CARTESIAN_POINT('Ctrl Pts',(-39.0778200867196,-35.0024921203811,
1.70842344717745));
#29662=CARTESIAN_POINT('Ctrl Pts',(-39.0758434671966,-35.0032082366984,
2.79157655282255));
#29663=CARTESIAN_POINT('Ctrl Pts',(-39.0663197739578,-33.8995579722718,
2.74838292522283));
#29664=CARTESIAN_POINT('Ctrl Pts',(-38.037544158487,-31.4430705734335,2.65285592183902));
#29665=CARTESIAN_POINT('Ctrl Pts',(-33.9071517375455,-30.3293121048675,
2.50499554267113));
#29666=CARTESIAN_POINT('Ctrl Pts',(-30.5014133532831,-33.3349589868354,
2.34799541531887));
#29667=CARTESIAN_POINT('Ctrl Pts',(-31.12960079995,-37.8336643815683,2.19099528796663));
#29668=CARTESIAN_POINT('Ctrl Pts',(-35.2284122851668,-39.7913952114128,
2.03399516061437));
#29669=CARTESIAN_POINT('Ctrl Pts',(-38.5306036675732,-37.8080765974554,
1.90085558223301));
#29670=CARTESIAN_POINT('Ctrl Pts',(-39.0659286289889,-35.7304351180991,
1.82004937963574));
#29671=CARTESIAN_POINT('Ctrl Pts',(-39.0674338139571,-34.9990828447087,
1.79157655282254));
#29672=CARTESIAN_POINT('Origin',(-35.,-35.,10.2084234471775));
#29673=CARTESIAN_POINT('',(-39.0750717811968,-34.9966356393236,3.79157655282255));
#29674=CARTESIAN_POINT('',(-39.0687110107696,-35.0023266135852,3.70842344717746));
#29675=CARTESIAN_POINT('',(-39.0735,-34.9999999999999,10.2084234471775));
#29676=CARTESIAN_POINT('Ctrl Pts',(-39.0687110107696,-35.0023266135852,
3.70842344717746));
#29677=CARTESIAN_POINT('Ctrl Pts',(-39.0642694397141,-34.16887057793,3.67594994115225));
#29678=CARTESIAN_POINT('Ctrl Pts',(-38.4124447778773,-31.9858617174929,
3.59114305934296));
#29679=CARTESIAN_POINT('Ctrl Pts',(-34.8667814687478,-30.2050135847982,
3.45400280174957));
#29680=CARTESIAN_POINT('Ctrl Pts',(-30.9271137663599,-32.4659835103585,
3.29700267439732));
#29681=CARTESIAN_POINT('Ctrl Pts',(-30.6396422127733,-36.9992303202149,
3.14000254704507));
#29682=CARTESIAN_POINT('Ctrl Pts',(-34.2621453393335,-39.7397481467912,
2.98300241969281));
#29683=CARTESIAN_POINT('Ctrl Pts',(-38.1877200741971,-38.356442172659,2.83914271973695));
#29684=CARTESIAN_POINT('Ctrl Pts',(-39.0641484919776,-35.9998016365399,
2.74761639556516));
#29685=CARTESIAN_POINT('Ctrl Pts',(-39.0728771860086,-34.996494180098,2.70842344717745));
#29686=CARTESIAN_POINT('Ctrl Pts',(-39.0750717811968,-34.9966356393236,
3.79157655282255));
#29687=CARTESIAN_POINT('Ctrl Pts',(-39.0773739047593,-34.7360557814575,
3.78138322237809));
#29688=CARTESIAN_POINT('Ctrl Pts',(-38.9368588004177,-33.1401094404144,
3.71885651614954));
#29689=CARTESIAN_POINT('Ctrl Pts',(-36.8334388106793,-30.5673771631648,
3.6039964341369));
#29690=CARTESIAN_POINT('Ctrl Pts',(-32.3142506564274,-31.0255322944533,
3.44699630678465));
#29691=CARTESIAN_POINT('Ctrl Pts',(-30.2033997043049,-35.0476307446275,
3.28999617943239));
#29692=CARTESIAN_POINT('Ctrl Pts',(-32.3937062542216,-39.0270182530956,
3.13299605208014));
#29693=CARTESIAN_POINT('Ctrl Pts',(-36.9211014088136,-39.3953398526252,
2.97599592472789));
#29694=CARTESIAN_POINT('Ctrl Pts',(-38.9541949543872,-36.8053221809578,
2.86218942497536));
#29695=CARTESIAN_POINT('Ctrl Pts',(-39.077858675523,-35.2367400343503,2.80071630100691));
#29696=CARTESIAN_POINT('Ctrl Pts',(-39.0758434671966,-35.0032082366984,
2.79157655282255));
#29697=CARTESIAN_POINT('Origin',(-35.,-35.,10.2084234471775));
#29698=CARTESIAN_POINT('',(-39.0676603684793,-35.0013188448613,4.79157655282255));
#29699=CARTESIAN_POINT('',(-39.0799229210932,-35.0002389671693,4.70842344717745));
#29700=CARTESIAN_POINT('',(-39.0735,-34.9999999999999,10.2084234471775));
#29701=CARTESIAN_POINT('Ctrl Pts',(-39.0799229210932,-35.0002389671693,
4.70842344717745));
#29702=CARTESIAN_POINT('Ctrl Pts',(-39.0787772264229,-33.680000347528,4.65661686252342));
#29703=CARTESIAN_POINT('Ctrl Pts',(-37.6705857942339,-31.023995125205,4.5524769020853));
#29704=CARTESIAN_POINT('Ctrl Pts',(-33.1665612371704,-30.5673772788489,
4.39600356586309));
#29705=CARTESIAN_POINT('Ctrl Pts',(-30.291435328683,-34.0839974792893,4.23900343851084));
#29706=CARTESIAN_POINT('Ctrl Pts',(-31.6385245327839,-38.4220059271175,
4.08200331115859));
#29707=CARTESIAN_POINT('Ctrl Pts',(-35.9998810371616,-39.6914688314679,
3.92500318380634));
#29708=CARTESIAN_POINT('Ctrl Pts',(-38.7479938252585,-37.361615545083,3.80047656247929));
#29709=CARTESIAN_POINT('Ctrl Pts',(-39.0714273489013,-35.5120445450279,
3.72828331693633));
#29710=CARTESIAN_POINT('Ctrl Pts',(-39.0687110107696,-35.0023266135852,
3.70842344717746));
#29711=CARTESIAN_POINT('Ctrl Pts',(-39.0676603684793,-35.0013188448613,
4.79157655282255));
#29712=CARTESIAN_POINT('Ctrl Pts',(-39.065407667772,-34.2430102880461,4.76205014374926));
#29713=CARTESIAN_POINT('Ctrl Pts',(-38.5005818838826,-32.1375386968076,
4.68019035889189));
#29714=CARTESIAN_POINT('Ctrl Pts',(-35.1332185347277,-30.2050134596587,
4.54599719825043));
#29715=CARTESIAN_POINT('Ctrl Pts',(-31.0740923862265,-32.2437539129077,
4.38899707089817));
#29716=CARTESIAN_POINT('Ctrl Pts',(-30.535365261007,-36.7540466716456,4.23199694354592));
#29717=CARTESIAN_POINT('Ctrl Pts',(-34.0001189367432,-39.6914689539076,
4.07499681619366));
#29718=CARTESIAN_POINT('Ctrl Pts',(-38.0783117770221,-38.5044266833838,
3.92819001928587));
#29719=CARTESIAN_POINT('Ctrl Pts',(-39.0655546178097,-36.0738936645484,
3.83371659816217));
#29720=CARTESIAN_POINT('Ctrl Pts',(-39.0750717811968,-34.9966356393236,
3.79157655282255));
#29721=CARTESIAN_POINT('Origin',(-35.,-35.,10.2084234471775));
#29722=CARTESIAN_POINT('',(-39.0792024631389,-35.0015161209354,5.79157655282255));
#29723=CARTESIAN_POINT('',(-39.0692231423099,-34.9973709029543,5.70842344717745));
#29724=CARTESIAN_POINT('',(-39.0735,-34.9999999999999,10.2084234471775));
#29725=CARTESIAN_POINT('Ctrl Pts',(-39.0692231423099,-34.9973709029543,
5.70842344717745));
#29726=CARTESIAN_POINT('Ctrl Pts',(-39.072153886322,-34.5148469224124,5.68961715967868));
#29727=CARTESIAN_POINT('Ctrl Pts',(-38.7712973835496,-32.6931086863282,
5.61847749639582));
#29728=CARTESIAN_POINT('Ctrl Pts',(-36.0928482339355,-30.3293122267992,
5.49500445732888));
#29729=CARTESIAN_POINT('Ctrl Pts',(-31.7071424564414,-31.5119158276916,
5.33800432997661));
#29730=CARTESIAN_POINT('Ctrl Pts',(-30.2741736217725,-35.8223180338192,
5.18100420262437));
#29731=CARTESIAN_POINT('Ctrl Pts',(-33.0788986413239,-39.395339737909,5.02400407527211));
#29732=CARTESIAN_POINT('Ctrl Pts',(-37.6062936777584,-39.0270181479993,
4.86700394791986));
#29733=CARTESIAN_POINT('Ctrl Pts',(-39.0738472616523,-36.3607409549812,
4.76181040522164));
#29734=CARTESIAN_POINT('Ctrl Pts',(-39.0799345709982,-35.013663708426,4.7089502383075));
#29735=CARTESIAN_POINT('Ctrl Pts',(-39.0799229210932,-35.0002389671693,
4.70842344717745));
#29736=CARTESIAN_POINT('Ctrl Pts',(-39.0792024631389,-35.0015161209354,
5.79157655282255));
#29737=CARTESIAN_POINT('Ctrl Pts',(-39.0731679256319,-33.7557919674485,
5.74271706512043));
#29738=CARTESIAN_POINT('Ctrl Pts',(-37.8030027181165,-31.1651102767228,
5.64152420163424));
#29739=CARTESIAN_POINT('Ctrl Pts',(-33.4155016033557,-30.4724169111822,
5.48799796236394));
#29740=CARTESIAN_POINT('Ctrl Pts',(-30.3495576440316,-33.8239773440302,
5.3309978350117));
#29741=CARTESIAN_POINT('Ctrl Pts',(-31.4537101308888,-38.230088373826,5.17399770765944));
#29742=CARTESIAN_POINT('Ctrl Pts',(-35.7378546799324,-39.7397482704758,
5.01699758030718));
#29743=CARTESIAN_POINT('Ctrl Pts',(-38.6790876767283,-37.5146290150371,
4.88952386202822));
#29744=CARTESIAN_POINT('Ctrl Pts',(-39.0694004131258,-35.5870561070142,
4.81438351953334));
#29745=CARTESIAN_POINT('Ctrl Pts',(-39.0676603684793,-35.0013188448613,
4.79157655282255));
#29746=CARTESIAN_POINT('Origin',(-35.,-35.,10.2084234471775));
#29747=CARTESIAN_POINT('',(-39.0709664927331,-34.9967444357251,6.79157655282255));
#29748=CARTESIAN_POINT('',(-39.0721140267755,-35.0034548068065,6.70842344717746));
#29749=CARTESIAN_POINT('',(-39.0735,-34.9999999999999,10.2084234471775));
#29750=CARTESIAN_POINT('Ctrl Pts',(-39.0721140267755,-35.0034548068065,
6.70842344717746));
#29751=CARTESIAN_POINT('Ctrl Pts',(-39.0638862819908,-34.0266505561004,
6.67028408104986));
#29752=CARTESIAN_POINT('Ctrl Pts',(-38.2252022081515,-31.6968182141492,
6.57981133913816));
#29753=CARTESIAN_POINT('Ctrl Pts',(-34.3564136921927,-30.2465364275518,
6.4370052214424));
#29754=CARTESIAN_POINT('Ctrl Pts',(-30.6802034020135,-32.9145736277213,
6.28000509409013));
#29755=CARTESIAN_POINT('Ctrl Pts',(-30.8775957137286,-37.4526369907548,
6.12300496673789));
#29756=CARTESIAN_POINT('Ctrl Pts',(-34.7715877207675,-39.7913950861294,
5.96600483938563));
#29757=CARTESIAN_POINT('Ctrl Pts',(-38.3794222668459,-38.0681714287485,
5.82781099953215));
#29758=CARTESIAN_POINT('Ctrl Pts',(-39.0639983304887,-35.8575951283075,
5.74195053546276));
#29759=CARTESIAN_POINT('Ctrl Pts',(-39.0692231423099,-34.9973709029543,
5.70842344717745));
#29760=CARTESIAN_POINT('Ctrl Pts',(-39.0709664927331,-34.9967444357251,
6.79157655282255));
#29761=CARTESIAN_POINT('Ctrl Pts',(-39.074129342561,-34.5902726781194,6.77571736227569));
#29762=CARTESIAN_POINT('Ctrl Pts',(-38.8328831908397,-32.8461583454701,
6.70752479594475));
#29763=CARTESIAN_POINT('Ctrl Pts',(-36.3504797430715,-30.3972101963624,
6.58699885382972));
#29764=CARTESIAN_POINT('Ctrl Pts',(-31.905896825022,-31.3344599279876,6.42999872647746));
#29765=CARTESIAN_POINT('Ctrl Pts',(-30.2358028418083,-35.5586616666892,
6.27299859912522));
#29766=CARTESIAN_POINT('Ctrl Pts',(-32.83782160528,-39.2818926978495,6.11599847177295));
#29767=CARTESIAN_POINT('Ctrl Pts',(-37.3786807951101,-39.1655161353224,
5.95899834442071));
#29768=CARTESIAN_POINT('Ctrl Pts',(-39.0372097938135,-36.5125334877904,
5.85085770477057));
#29769=CARTESIAN_POINT('Ctrl Pts',(-39.0796315161011,-35.090086560245,5.79505044090452));
#29770=CARTESIAN_POINT('Ctrl Pts',(-39.0792024631389,-35.0015161209354,
5.79157655282255));
#29771=CARTESIAN_POINT('Origin',(-35.,-35.,10.2084234471775));
#29772=CARTESIAN_POINT('',(-39.0691247390887,-35.0040754761348,7.79157655282255));
#29773=CARTESIAN_POINT('',(-39.0784093524563,-34.997955826836,7.70842344717746));
#29774=CARTESIAN_POINT('',(-39.0735,-34.9999999999999,10.2084234471775));
#29775=CARTESIAN_POINT('',(-36.0520713770612,-38.9352951690526,8.));
#29776=CARTESIAN_POINT('Ctrl Pts',(-36.0520713770612,-38.9352951690526,
8.));
#29777=CARTESIAN_POINT('Ctrl Pts',(-37.3460763064865,-38.5893527455387,
7.94766662421592));
#29778=CARTESIAN_POINT('Ctrl Pts',(-38.8056934287649,-37.2206664159851,
7.87819214182344));
#29779=CARTESIAN_POINT('Ctrl Pts',(-39.0721265495934,-35.4436566771087,
7.80871765943095));
#29780=CARTESIAN_POINT('Ctrl Pts',(-39.0691247390887,-35.0040754761348,
7.79157655282255));
#29781=CARTESIAN_POINT('',(-33.9452801041878,-38.9416007879337,8.));
#29782=CARTESIAN_POINT('Origin',(-35.,-35.,8.));
#29783=CARTESIAN_POINT('Ctrl Pts',(-33.9452677648582,-38.941630165528,8.));
#29784=CARTESIAN_POINT('Ctrl Pts',(-35.1775571519718,-39.2670003808689,
7.95000212253756));
#29785=CARTESIAN_POINT('Ctrl Pts',(-37.9028288422611,-38.6929823061133,
7.85280993826337));
#29786=CARTESIAN_POINT('Ctrl Pts',(-39.0706575059758,-36.2016126262027,
7.75561775398919));
#29787=CARTESIAN_POINT('Ctrl Pts',(-39.0784093524563,-34.997955826836,7.70842344717745));
#29788=CARTESIAN_POINT('Origin',(35.,35.,10.2084234471775));
#29789=CARTESIAN_POINT('',(30.9212698233586,35.0019483146883,0.791576552822542));
#29790=CARTESIAN_POINT('',(30.9328374281389,34.9998406908479,0.708423447177449));
#29791=CARTESIAN_POINT('',(30.9265,35.0000000000001,10.2084234471775));
#29792=CARTESIAN_POINT('',(36.0520713770613,31.0647048309474,0.));
#29793=CARTESIAN_POINT('Ctrl Pts',(30.9328374281389,34.9998406908479,0.708423447177449));
#29794=CARTESIAN_POINT('Ctrl Pts',(30.9332828479214,35.688557610158,0.681615801254637));
#29795=CARTESIAN_POINT('Ctrl Pts',(31.423729103703,37.7222371568615,0.602474779547742));
#29796=CARTESIAN_POINT('Ctrl Pts',(34.620473026815,39.7808594262888,0.47100038205676));
#29797=CARTESIAN_POINT('Ctrl Pts',(38.7813013396977,37.9557820285754,0.314000254704507));
#29798=CARTESIAN_POINT('Ctrl Pts',(39.5450610063768,33.4726465453437,0.157000127352254));
#29799=CARTESIAN_POINT('Ctrl Pts',(37.3460763064866,31.4106472544613,0.0523333757840845));
#29800=CARTESIAN_POINT('Ctrl Pts',(36.0520713770613,31.0647048309474,0.));
#29801=CARTESIAN_POINT('',(33.9452806327216,31.0583991975554,1.9516645121422E-15));
#29802=CARTESIAN_POINT('Origin',(35.,35.,0.));
#29803=CARTESIAN_POINT('Ctrl Pts',(30.9212698233586,35.0019483146883,0.791576552822542));
#29804=CARTESIAN_POINT('Ctrl Pts',(30.9205865489415,35.1174152630019,0.787049082480475));
#29805=CARTESIAN_POINT('Ctrl Pts',(30.9769552830328,36.5668922956884,0.730188236354323));
#29806=CARTESIAN_POINT('Ctrl Pts',(32.7044910542971,39.2117680815463,0.620994014444087));
#29807=CARTESIAN_POINT('Ctrl Pts',(37.246817707304,39.2384377086451,0.463993887091833));
#29808=CARTESIAN_POINT('Ctrl Pts',(39.7742802645754,35.4632838929154,0.30699375973958));
#29809=CARTESIAN_POINT('Ctrl Pts',(38.0469271024438,31.3373709383794,0.152329130708969));
#29810=CARTESIAN_POINT('Ctrl Pts',(35.1775581103468,30.7329992432291,0.0499978774624438));
#29811=CARTESIAN_POINT('Ctrl Pts',(33.9452683089267,31.0583698510224,2.42915496745377E-15));
#29812=CARTESIAN_POINT('Origin',(35.,35.,10.2084234471775));
#29813=CARTESIAN_POINT('',(30.9325668217157,35.0009171562606,1.79157655282254));
#29814=CARTESIAN_POINT('',(30.9221793985577,34.9975078813789,1.70842344717745));
#29815=CARTESIAN_POINT('',(30.9265,35.0000000000001,10.2084234471775));
#29816=CARTESIAN_POINT('Ctrl Pts',(30.9221793985577,34.9975078813789,1.70842344717745));
#29817=CARTESIAN_POINT('Ctrl Pts',(30.9307243035611,36.174970446985,1.66228272262581));
#29818=CARTESIAN_POINT('Ctrl Pts',(32.0812069040633,38.7025089358584,1.56380862229009));
#29819=CARTESIAN_POINT('Ctrl Pts',(36.3504798927025,39.6027903023767,1.41300114617028));
#29820=CARTESIAN_POINT('Ctrl Pts',(39.5841214241815,36.41272834745,1.25600101881803));
#29821=CARTESIAN_POINT('Ctrl Pts',(38.7070437601939,31.9557497473198,1.09900089146578));
#29822=CARTESIAN_POINT('Ctrl Pts',(34.5060128656572,30.2288003607244,0.942000764113522));
#29823=CARTESIAN_POINT('Ctrl Pts',(31.3893171307454,32.344207693053,0.811808282684079));
#29824=CARTESIAN_POINT('Ctrl Pts',(30.9324133079056,34.3440575577889,0.733949177038721));
#29825=CARTESIAN_POINT('Ctrl Pts',(30.9328374281389,34.9998406908479,0.708423447177449));
#29826=CARTESIAN_POINT('Ctrl Pts',(30.9325668217157,35.0009171562606,1.79157655282254));
#29827=CARTESIAN_POINT('Ctrl Pts',(30.9313054599248,35.6137984881563,1.76771600385165));
#29828=CARTESIAN_POINT('Ctrl Pts',(31.3469046036967,37.5692890939049,1.69152207909667));
#29829=CARTESIAN_POINT('Ctrl Pts',(34.3564137772933,39.7534629455386,1.56299477855761));
#29830=CARTESIAN_POINT('Ctrl Pts',(38.6097344321268,38.159032706872,1.40599465120535));
#29831=CARTESIAN_POINT('Ctrl Pts',(39.6261697761982,33.7318499178854,1.2489945238531));
#29832=CARTESIAN_POINT('Ctrl Pts',(36.4942779564007,30.441864951573,1.09199439650085));
#29833=CARTESIAN_POINT('Ctrl Pts',(32.1514012728307,31.2161408778184,0.939521739490661));
#29834=CARTESIAN_POINT('Ctrl Pts',(30.9284845701608,33.7827239806345,0.839382458264559));
#29835=CARTESIAN_POINT('Ctrl Pts',(30.9212698233586,35.0019483146883,0.791576552822542));
#29836=CARTESIAN_POINT('Origin',(35.,35.,10.2084234471775));
#29837=CARTESIAN_POINT('',(30.9241571699662,34.9967917637985,2.79157655282254));
#29838=CARTESIAN_POINT('',(30.9271222988705,35.0035058204319,2.70842344717745));
#29839=CARTESIAN_POINT('',(30.9265,35.0000000000001,10.2084234471775));
#29840=CARTESIAN_POINT('Ctrl Pts',(30.9271222988705,35.0035058204319,2.70842344717745));
#29841=CARTESIAN_POINT('Ctrl Pts',(30.9241957830228,35.3398900680519,2.69528301978107));
#29842=CARTESIAN_POINT('Ctrl Pts',(31.1149285017256,37.0126943772598,2.62980921660061));
#29843=CARTESIAN_POINT('Ctrl Pts',(33.415501444059,39.52758354292,2.51200203763605));
#29844=CARTESIAN_POINT('Ctrl Pts',(37.902280422705,38.8192163097165,2.3550019102838));
#29845=CARTESIAN_POINT('Ctrl Pts',(39.7865573966804,34.6861219842625,2.19800178293155));
#29846=CARTESIAN_POINT('Ctrl Pts',(37.3786810353442,30.8344834494167,2.0410016555793));
#29847=CARTESIAN_POINT('Ctrl Pts',(32.8378213856151,30.7181068667712,1.88400152822704));
#29848=CARTESIAN_POINT('Ctrl Pts',(31.0005090266209,33.347118822167,1.77314212542643));
#29849=CARTESIAN_POINT('Ctrl Pts',(30.9210325674879,34.839477961413,1.7146160984099));
#29850=CARTESIAN_POINT('Ctrl Pts',(30.9221793985577,34.9975078813789,1.70842344717745));
#29851=CARTESIAN_POINT('Ctrl Pts',(30.9241571699662,34.9967917637985,2.79157655282254));
#29852=CARTESIAN_POINT('Ctrl Pts',(30.9336808617147,36.100441855715,2.74838292522282));
#29853=CARTESIAN_POINT('Ctrl Pts',(31.9624563163556,38.5569288706128,2.65285592183902));
#29854=CARTESIAN_POINT('Ctrl Pts',(36.0928480916297,39.6706871647746,2.50499554267113));
#29855=CARTESIAN_POINT('Ctrl Pts',(39.4985859434327,36.6650407532663,2.34799541531887));
#29856=CARTESIAN_POINT('Ctrl Pts',(38.8703985950797,32.1663360606625,2.19099528796662));
#29857=CARTESIAN_POINT('Ctrl Pts',(34.7715877503781,30.208605539026,2.03399516061437));
#29858=CARTESIAN_POINT('Ctrl Pts',(31.4693968846214,32.1919238394657,1.90085558223301));
#29859=CARTESIAN_POINT('Ctrl Pts',(30.9340720065237,34.2695649966187,1.82004937963573));
#29860=CARTESIAN_POINT('Ctrl Pts',(30.9325668217157,35.0009171562606,1.79157655282254));
#29861=CARTESIAN_POINT('Origin',(35.,35.,10.2084234471775));
#29862=CARTESIAN_POINT('',(30.9249288558452,35.0033643601501,3.79157655282254));
#29863=CARTESIAN_POINT('',(30.9312884745882,34.9976733861211,3.70842344717745));
#29864=CARTESIAN_POINT('',(30.9265,35.0000000000001,10.2084234471775));
#29865=CARTESIAN_POINT('Ctrl Pts',(30.9312884745882,34.9976733861211,3.70842344717745));
#29866=CARTESIAN_POINT('Ctrl Pts',(30.935730046206,35.8311295271992,3.67594994115225));
#29867=CARTESIAN_POINT('Ctrl Pts',(31.587554790492,38.0141386637623,3.59114305934295));
#29868=CARTESIAN_POINT('Ctrl Pts',(35.1332185480963,39.7949870216991,3.45400280174957));
#29869=CARTESIAN_POINT('Ctrl Pts',(39.0728867488228,37.5340168101838,3.29700267439732));
#29870=CARTESIAN_POINT('Ctrl Pts',(39.360358338736,33.0007694268683,3.14000254704507));
#29871=CARTESIAN_POINT('Ctrl Pts',(35.7378547540399,30.2602512537625,2.98300241969282));
#29872=CARTESIAN_POINT('Ctrl Pts',(31.8122795225231,31.6435574026667,2.83914271973694));
#29873=CARTESIAN_POINT('Ctrl Pts',(30.9358509939969,34.0001982370698,2.74761639556516));
#29874=CARTESIAN_POINT('Ctrl Pts',(30.9271222988705,35.0035058204319,2.70842344717745));
#29875=CARTESIAN_POINT('Ctrl Pts',(30.9249288558452,35.0033643601501,3.79157655282255));
#29876=CARTESIAN_POINT('Ctrl Pts',(30.9226267326427,35.2639441772806,3.78138322237808));
#29877=CARTESIAN_POINT('Ctrl Pts',(31.0631418150181,36.8598902688347,3.71885651614953));
#29878=CARTESIAN_POINT('Ctrl Pts',(33.1665614759356,39.4326221439007,3.60399643413691));
#29879=CARTESIAN_POINT('Ctrl Pts',(37.6857489237188,38.9744670842276,3.44699630678464));
#29880=CARTESIAN_POINT('Ctrl Pts',(39.7965995458586,34.9523692628263,3.2899961794324));
#29881=CARTESIAN_POINT('Ctrl Pts',(37.6062933383462,30.9729823764193,3.13299605208014));
#29882=CARTESIAN_POINT('Ctrl Pts',(33.078898891504,30.6046608345122,2.97599592472789));
#29883=CARTESIAN_POINT('Ctrl Pts',(31.0458056637607,33.1946781012295,2.86218942497536));
#29884=CARTESIAN_POINT('Ctrl Pts',(30.9221419619551,34.7632600026498,2.80071630100691));
#29885=CARTESIAN_POINT('Ctrl Pts',(30.9241571699662,34.9967917637985,2.79157655282254));
#29886=CARTESIAN_POINT('Origin',(35.,35.,10.2084234471775));
#29887=CARTESIAN_POINT('',(30.9323402673974,34.9986811553562,4.79157655282255));
#29888=CARTESIAN_POINT('',(30.920076562846,34.9997610327988,4.70842344717745));
#29889=CARTESIAN_POINT('',(30.9265,35.0000000000001,10.2084234471775));
#29890=CARTESIAN_POINT('Ctrl Pts',(30.920076562846,34.9997610327988,4.70842344717745));
#29891=CARTESIAN_POINT('Ctrl Pts',(30.9212222576611,36.3199998194329,4.65661686252342));
#29892=CARTESIAN_POINT('Ctrl Pts',(32.3294138679696,38.9760053777146,4.5524769020853));
#29893=CARTESIAN_POINT('Ctrl Pts',(36.833438994737,39.4326232818222,4.39600356586309));
#29894=CARTESIAN_POINT('Ctrl Pts',(39.7085652668935,35.9160026365752,4.23900343851085));
#29895=CARTESIAN_POINT('Ctrl Pts',(38.3614758924016,31.5779936400392,4.08200331115859));
#29896=CARTESIAN_POINT('Ctrl Pts',(34.0001188363665,30.3085305751198,3.92500318380634));
#29897=CARTESIAN_POINT('Ctrl Pts',(31.2520057006646,32.6383841561994,3.80047656247929));
#29898=CARTESIAN_POINT('Ctrl Pts',(30.9285721361126,34.4879553902047,3.72828331693633));
#29899=CARTESIAN_POINT('Ctrl Pts',(30.9312884745882,34.9976733861211,3.70842344717745));
#29900=CARTESIAN_POINT('Ctrl Pts',(30.9323402673974,34.9986811553562,4.79157655282255));
#29901=CARTESIAN_POINT('Ctrl Pts',(30.9345929677557,35.7569895936223,4.76205014374926));
#29902=CARTESIAN_POINT('Ctrl Pts',(31.4994186633631,37.8624608556942,4.68019035889188));
#29903=CARTESIAN_POINT('Ctrl Pts',(34.86678148609,39.7949857907703,4.54599719825042));
#29904=CARTESIAN_POINT('Ctrl Pts',(38.9259070000539,37.7562456562111,4.38899707089817));
#29905=CARTESIAN_POINT('Ctrl Pts',(39.4646340410498,33.2459536025622,4.23199694354592));
#29906=CARTESIAN_POINT('Ctrl Pts',(35.9998809069499,30.3085317794917,4.07499681619366));
#29907=CARTESIAN_POINT('Ctrl Pts',(31.9216887041993,31.4955738644524,3.92819001928588));
#29908=CARTESIAN_POINT('Ctrl Pts',(30.9344460177445,33.9261065033295,3.83371659816217));
#29909=CARTESIAN_POINT('Ctrl Pts',(30.9249288558452,35.0033643601501,3.79157655282255));
#29910=CARTESIAN_POINT('Origin',(35.,35.,10.2084234471775));
#29911=CARTESIAN_POINT('',(30.9207981741727,34.9984838800189,5.79157655282254));
#29912=CARTESIAN_POINT('',(30.93077634299,35.0026290974327,5.70842344717745));
#29913=CARTESIAN_POINT('',(30.9265,35.0000000000001,10.2084234471775));
#29914=CARTESIAN_POINT('Ctrl Pts',(30.93077634299,35.0026290974327,5.70842344717745));
#29915=CARTESIAN_POINT('Ctrl Pts',(30.9278455986019,35.4851531389532,5.68961715967867));
#29916=CARTESIAN_POINT('Ctrl Pts',(31.2287021394076,37.3068916052531,5.61847749639582));
#29917=CARTESIAN_POINT('Ctrl Pts',(33.9071516278456,39.6706883641509,5.49500445732887));
#29918=CARTESIAN_POINT('Ctrl Pts',(38.2928579600589,38.4880846134226,5.33800432997661));
#29919=CARTESIAN_POINT('Ctrl Pts',(39.72582697599,34.1776818622125,5.18100420262437));
#29920=CARTESIAN_POINT('Ctrl Pts',(36.9211016016709,30.6046597061106,5.0240040752721));
#29921=CARTESIAN_POINT('Ctrl Pts',(32.3937059925777,30.9729813426439,4.86700394791986));
#29922=CARTESIAN_POINT('Ctrl Pts',(30.9261522230555,33.6392588729013,4.76181040522164));
#29923=CARTESIAN_POINT('Ctrl Pts',(30.9200649129395,34.986336289844,4.7089502383075));
#29924=CARTESIAN_POINT('Ctrl Pts',(30.920076562846,34.9997610327988,4.70842344717745));
#29925=CARTESIAN_POINT('Ctrl Pts',(30.9207981741727,34.9984838800189,5.79157655282254));
#29926=CARTESIAN_POINT('Ctrl Pts',(30.9268327105953,36.2442078390725,5.74271706512043));
#29927=CARTESIAN_POINT('Ctrl Pts',(32.1969977207135,38.8348891225654,5.64152420163423));
#29928=CARTESIAN_POINT('Ctrl Pts',(36.5844981485848,39.5275823816942,5.48799796236394));
#29929=CARTESIAN_POINT('Ctrl Pts',(39.6504416291735,36.1760224717832,5.33099783501169));
#29930=CARTESIAN_POINT('Ctrl Pts',(38.5462893146292,31.7699121313011,5.17399770765944));
#29931=CARTESIAN_POINT('Ctrl Pts',(34.2621454354683,30.2602524703801,5.01699758030718));
#29932=CARTESIAN_POINT('Ctrl Pts',(31.3209128983978,32.4853713780877,4.88952386202822));
#29933=CARTESIAN_POINT('Ctrl Pts',(30.9306002230203,34.4129439847737,4.81438351953334));
#29934=CARTESIAN_POINT('Ctrl Pts',(30.9323402673974,34.9986811553562,4.79157655282255));
#29935=CARTESIAN_POINT('Origin',(35.,35.,10.2084234471775));
#29936=CARTESIAN_POINT('',(30.9290341434093,35.0032555560525,6.79157655282255));
#29937=CARTESIAN_POINT('',(30.9278854598697,34.9965452008231,6.70842344717745));
#29938=CARTESIAN_POINT('',(30.9265,35.0000000000001,10.2084234471775));
#29939=CARTESIAN_POINT('Ctrl Pts',(30.9278854598697,34.9965452008231,6.70842344717745));
#29940=CARTESIAN_POINT('Ctrl Pts',(30.9361132054557,35.973349573232,6.67028408104985));
#29941=CARTESIAN_POINT('Ctrl Pts',(31.7747973816342,38.3031821914714,6.57981133913817));
#29942=CARTESIAN_POINT('Ctrl Pts',(35.6435863904507,39.7534641813021,6.43700522144238));
#29943=CARTESIAN_POINT('Ctrl Pts',(39.3197971438036,37.085426632005,6.28000509409014));
#29944=CARTESIAN_POINT('Ctrl Pts',(39.122404807981,32.5473627011697,6.12300496673788));
#29945=CARTESIAN_POINT('Ctrl Pts',(35.2284123079944,30.2086043066787,5.96600483938564));
#29946=CARTESIAN_POINT('Ctrl Pts',(31.6205773057362,31.9318281835565,5.82781099953215));
#29947=CARTESIAN_POINT('Ctrl Pts',(30.9360011554815,34.1424047633691,5.74195053546276));
#29948=CARTESIAN_POINT('Ctrl Pts',(30.93077634299,35.0026290974327,5.70842344717745));
#29949=CARTESIAN_POINT('Ctrl Pts',(30.9290341434093,35.0032555560525,6.79157655282255));
#29950=CARTESIAN_POINT('Ctrl Pts',(30.9258712893501,35.4097272653281,6.77571736227569));
#29951=CARTESIAN_POINT('Ctrl Pts',(31.167117385295,37.1538413864501,6.70752479594475));
#29952=CARTESIAN_POINT('Ctrl Pts',(33.6495204900336,39.6027890266495,6.58699885382972));
#29953=CARTESIAN_POINT('Ctrl Pts',(38.0941026784935,38.6655395297167,6.42999872647747));
#29954=CARTESIAN_POINT('Ctrl Pts',(39.7641964207046,34.4413384042963,6.27299859912521));
#29955=CARTESIAN_POINT('Ctrl Pts',(37.1621780526355,30.7181079801836,6.11599847177296));
#29956=CARTESIAN_POINT('Ctrl Pts',(32.6213195789955,30.8344845112897,5.95899834442071));
#29957=CARTESIAN_POINT('Ctrl Pts',(30.9627908371619,33.4874667488915,5.85085770477057));
#29958=CARTESIAN_POINT('Ctrl Pts',(30.9203691212877,34.9099134545334,5.79505044090451));
#29959=CARTESIAN_POINT('Ctrl Pts',(30.9207981741727,34.9984838800189,5.79157655282254));
#29960=CARTESIAN_POINT('Origin',(35.,35.,10.2084234471775));
#29961=CARTESIAN_POINT('',(30.9308749498806,34.995920959377,7.79157655282255));
#29962=CARTESIAN_POINT('',(30.9215901961247,35.0020443570103,7.70842344717745));
#29963=CARTESIAN_POINT('',(30.9265,35.0000000000001,10.2084234471775));
#29964=CARTESIAN_POINT('',(33.9479286229388,31.0647048309474,8.));
#29965=CARTESIAN_POINT('Ctrl Pts',(33.9479286229388,31.0647048309474,8.));
#29966=CARTESIAN_POINT('Ctrl Pts',(32.6539236935135,31.4106472544613,7.94766662421592));
#29967=CARTESIAN_POINT('Ctrl Pts',(31.1943056926496,32.7793278989778,7.87819214182343));
#29968=CARTESIAN_POINT('Ctrl Pts',(30.927873001558,34.5563391849396,7.80871765943095));
#29969=CARTESIAN_POINT('Ctrl Pts',(30.9308749498806,34.995920959377,7.79157655282255));
#29970=CARTESIAN_POINT('',(36.0547204053665,31.0583992220146,8.));
#29971=CARTESIAN_POINT('Origin',(35.,35.,8.));
#29972=CARTESIAN_POINT('Ctrl Pts',(36.0547327596422,31.0583698145405,8.));
#29973=CARTESIAN_POINT('Ctrl Pts',(34.8224437745751,30.7329999802434,7.95000212253756));
#29974=CARTESIAN_POINT('Ctrl Pts',(32.0971699315749,31.3070160119469,7.85280993826337));
#29975=CARTESIAN_POINT('Ctrl Pts',(30.9293418770678,33.7983871843493,7.75561775398919));
#29976=CARTESIAN_POINT('Ctrl Pts',(30.9215901961247,35.0020443570103,7.70842344717745));
#29977=CARTESIAN_POINT('Origin',(35.,35.,10.2084234471775));
#29978=CARTESIAN_POINT('Ctrl Pts',(30.9215901961247,35.0020443570103,7.70842344717745));
#29979=CARTESIAN_POINT('Ctrl Pts',(30.9207461022984,35.1331126499304,7.70328437820511));
#29980=CARTESIAN_POINT('Ctrl Pts',(30.985475579174,36.5980980633283,7.64581193344868));
#29981=CARTESIAN_POINT('Ctrl Pts',(32.753181262015,39.238437809064,7.53600611290817));
#29982=CARTESIAN_POINT('Ctrl Pts',(37.2955097522044,39.2117697306779,7.37900598555592));
#29983=CARTESIAN_POINT('Ctrl Pts',(39.7793716811886,35.4089491092894,7.22200585820366));
#29984=CARTESIAN_POINT('Ctrl Pts',(37.9775554192851,31.2391311721338,7.06500573085141));
#29985=CARTESIAN_POINT('Ctrl Pts',(33.5057216363881,30.441863683446,6.90800560349916));
#29986=CARTESIAN_POINT('Ctrl Pts',(31.1346462527125,32.9326274967327,6.7891448422745));
#29987=CARTESIAN_POINT('Ctrl Pts',(30.9248234084473,34.6330160680086,6.72261745683393));
#29988=CARTESIAN_POINT('Ctrl Pts',(30.9278854598697,34.9965452008231,6.70842344717745));
#29989=CARTESIAN_POINT('Ctrl Pts',(30.9308749498806,34.995920959377,7.79157655282255));
#29990=CARTESIAN_POINT('Ctrl Pts',(30.9370382260235,35.8984227922016,7.75638428364686));
#29991=CARTESIAN_POINT('Ctrl Pts',(31.6729751170447,38.1550462153353,7.66885863868709));
#29992=CARTESIAN_POINT('Ctrl Pts',(35.3795268052061,39.7808547962683,7.52899961794324));
#29993=CARTESIAN_POINT('Ctrl Pts',(39.1969168896572,37.3225573472918,7.37199949059099));
#29994=CARTESIAN_POINT('Ctrl Pts',(39.2524338890068,32.7797860374403,7.21499936323873));
#29995=CARTESIAN_POINT('Ctrl Pts',(35.4939868648458,30.2288021766129,7.05799923588648));
#29996=CARTESIAN_POINT('Ctrl Pts',(31.7173195455156,31.7813045011721,6.91685829908108));
#29997=CARTESIAN_POINT('Ctrl Pts',(30.9363083182476,34.0684206807159,6.82805073805977));
#29998=CARTESIAN_POINT('Ctrl Pts',(30.9290341434093,35.0032555560525,6.79157655282255));
#29999=CARTESIAN_POINT('Ctrl Pts',(37.6735319337713,37.2858331630076,8.));
#30000=CARTESIAN_POINT('Ctrl Pts',(38.4251602751564,36.4067215963626,7.94766662421592));
#30001=CARTESIAN_POINT('Ctrl Pts',(38.981419710079,33.8637820915388,7.84299987264775));
#30002=CARTESIAN_POINT('Ctrl Pts',(36.2450923914777,31.0470745569746,7.68599974529549));
#30003=CARTESIAN_POINT('Ctrl Pts',(32.3914750767338,31.7834880469926,7.52899961794325));
#30004=CARTESIAN_POINT('Ctrl Pts',(30.877370367455,35.4000509161799,7.37199949059098));
#30005=CARTESIAN_POINT('Ctrl Pts',(33.0598539558457,38.6599251241887,7.21499936323874));
#30006=CARTESIAN_POINT('Ctrl Pts',(36.9821911263972,38.6368970240971,7.05799923588648));
#30007=CARTESIAN_POINT('Ctrl Pts',(39.1270258717517,35.3531308437279,6.90099910853422));
#30008=CARTESIAN_POINT('Ctrl Pts',(37.5711430434112,31.75245953062,6.74399898118198));
#30009=CARTESIAN_POINT('Ctrl Pts',(33.7096786193679,31.0640126442915,6.58699885382972));
#30010=CARTESIAN_POINT('Ctrl Pts',(31.0052641890983,33.9049419734146,6.42999872647747));
#30011=CARTESIAN_POINT('Ctrl Pts',(31.882964491631,37.7278508156672,6.27299859912521));
#30012=CARTESIAN_POINT('Ctrl Pts',(35.5557420224402,39.1046545373095,6.11599847177296));
#30013=CARTESIAN_POINT('Ctrl Pts',(38.7301795638466,36.8007826630852,5.9589983444207));
#30014=CARTESIAN_POINT('Ctrl Pts',(38.559729694875,32.8821279738221,5.80199821706846));
#30015=CARTESIAN_POINT('Ctrl Pts',(35.1972358643355,30.8625912971014,5.64499808971619));
#30016=CARTESIAN_POINT('Ctrl Pts',(31.6578788381682,32.5531077792767,5.48799796236396));
#30017=CARTESIAN_POINT('Ctrl Pts',(31.1154338729727,36.437776445535,5.33099783501168));
#30018=CARTESIAN_POINT('Ctrl Pts',(34.0563166443959,39.033176953701,5.17399770765944));
#30019=CARTESIAN_POINT('Ctrl Pts',(37.843409322329,38.0119891070858,5.01699758030718));
#30020=CARTESIAN_POINT('Ctrl Pts',(39.0807895883257,34.2899216767724,4.85999745295493));
#30021=CARTESIAN_POINT('Ctrl Pts',(36.6588866782563,31.2045883187048,4.70299732560268));
#30022=CARTESIAN_POINT('Ctrl Pts',(32.7494441705885,31.5226370130723,4.54599719825042));
#30023=CARTESIAN_POINT('Ctrl Pts',(30.8580966653042,34.9588704649406,4.38899707089817));
#30024=CARTESIAN_POINT('Ctrl Pts',(32.6808336162004,38.4319851620801,4.23199694354592));
#30025=CARTESIAN_POINT('Ctrl Pts',(36.5831893123819,38.8276058411217,4.07499681619366));
#30026=CARTESIAN_POINT('Ctrl Pts',(39.0658839637408,35.7909756411325,3.91799668884141));
#30027=CARTESIAN_POINT('Ctrl Pts',(37.9026614585792,32.0450699960324,3.76099656148916));
#30028=CARTESIAN_POINT('Ctrl Pts',(34.1365945763887,30.9488784332844,3.6039964341369));
#30029=CARTESIAN_POINT('Ctrl Pts',(31.1447516212191,33.4853664448484,3.44699630678465));
#30030=CARTESIAN_POINT('Ctrl Pts',(31.6099468717921,37.3800408947213,3.2899961794324));
#30031=CARTESIAN_POINT('Ctrl Pts',(35.1150352873275,39.1405098438263,3.13299605208014));
#30032=CARTESIAN_POINT('Ctrl Pts',(38.5169704526781,37.1881438885041,2.97599592472789));
#30033=CARTESIAN_POINT('Ctrl Pts',(38.7652044817734,33.2736483267483,2.81899579737564));
#30034=CARTESIAN_POINT('Ctrl Pts',(35.6371435122955,30.9071888511377,2.66199567002338));
#30035=CARTESIAN_POINT('Ctrl Pts',(31.9377498791963,32.2107924399309,2.50499554267113));
#30036=CARTESIAN_POINT('Ctrl Pts',(30.9843052341107,36.0155051205153,2.34799541531888));
#30037=CARTESIAN_POINT('Ctrl Pts',(33.6317727579422,38.9096047900383,2.19099528796662));
#30038=CARTESIAN_POINT('Ctrl Pts',(37.5061424786706,38.297923989058,2.03399516061437));
#30039=CARTESIAN_POINT('Ctrl Pts',(39.1332307948504,34.7289638099038,1.87699503326212));
#30040=CARTESIAN_POINT('Ctrl Pts',(37.0540101980664,31.4030429687795,1.71999490590986));
#30041=CARTESIAN_POINT('Ctrl Pts',(33.1329413830615,31.3025508540242,1.56299477855761));
#30042=CARTESIAN_POINT('Ctrl Pts',(30.8860770418796,34.5175911198794,1.40599465120536));
#30043=CARTESIAN_POINT('Ctrl Pts',(32.3282167572518,38.1652236231046,1.2489945238531));
#30044=CARTESIAN_POINT('Ctrl Pts',(36.1661502448953,38.9745464314742,1.09199439650085));
#30045=CARTESIAN_POINT('Ctrl Pts',(38.9584257050592,36.219902286033,0.934994269148596));
#30046=CARTESIAN_POINT('Ctrl Pts',(38.2010620907038,32.3712654317411,0.777994141796343));
#30047=CARTESIAN_POINT('Ctrl Pts',(34.5734381379524,30.8800307521414,0.620994014444089));
#30048=CARTESIAN_POINT('Ctrl Pts',(31.3279883656859,33.0828278259953,0.463993887091835));
#30049=CARTESIAN_POINT('Ctrl Pts',(31.3759274478189,37.0055458008236,0.306993759739581));
#30050=CARTESIAN_POINT('Ctrl Pts',(34.6722754073454,39.1283105516069,0.149993632387328));
#30051=CARTESIAN_POINT('Ctrl Pts',(38.2651841076192,37.5523415454803,-0.007006494964925));
#30052=CARTESIAN_POINT('Ctrl Pts',(38.9246967202481,33.681118012335,-0.164006622317179));
#30053=CARTESIAN_POINT('Ctrl Pts',(37.0258557525633,31.9005650466596,-0.268673373885348));
#30054=CARTESIAN_POINT('Ctrl Pts',(35.9084720925035,31.6018409826581,-0.321006749669432));
#30055=CARTESIAN_POINT('Ctrl Pts',(37.8143974874483,37.4062712808594,8.10700224988981));
#30056=CARTESIAN_POINT('Ctrl Pts',(38.6056283266121,36.4808402609044,8.05466887410573));
#30057=CARTESIAN_POINT('Ctrl Pts',(39.1911964794515,33.80391597857,7.95000212253756));
#30058=CARTESIAN_POINT('Ctrl Pts',(36.3106949851439,30.8387991202229,7.7930019951853));
#30059=CARTESIAN_POINT('Ctrl Pts',(32.2540346732905,31.6140134536857,7.63600186783305));
#30060=CARTESIAN_POINT('Ctrl Pts',(30.6601533974768,35.4211291734076,7.4790017404808));
#30061=CARTESIAN_POINT('Ctrl Pts',(32.9576297245688,38.8527626858139,7.32200161312855));
#30062=CARTESIAN_POINT('Ctrl Pts',(37.0866306683329,38.828521259624,7.16500148577629));
#30063=CARTESIAN_POINT('Ctrl Pts',(39.3444744748973,35.3717369322484,7.00800135842404));
#30064=CARTESIAN_POINT('Ctrl Pts',(37.7066138353691,31.5813500777913,6.85100123107178));
#30065=CARTESIAN_POINT('Ctrl Pts',(33.6416929583746,30.856629657343,6.69400110371953));
#30066=CARTESIAN_POINT('Ctrl Pts',(30.7947858085381,33.8472445308389,6.53700097636727));
#30067=CARTESIAN_POINT('Ctrl Pts',(31.7187312063761,37.8715783734507,6.38000084901503));
#30068=CARTESIAN_POINT('Ctrl Pts',(35.5850234784437,39.3209244186404,6.22300072166276));
#30069=CARTESIAN_POINT('Ctrl Pts',(38.9267187571656,36.8956639860585,6.06600059431053));
#30070=CARTESIAN_POINT('Ctrl Pts',(38.7472880659103,32.7705395496047,5.90900046695826));
#30071=CARTESIAN_POINT('Ctrl Pts',(35.2076280122218,30.6445956336272,5.75200033960601));
#30072=CARTESIAN_POINT('Ctrl Pts',(31.4817860292625,32.4241836309969,5.59500021225375));
#30073=CARTESIAN_POINT('Ctrl Pts',(30.9107602158652,36.5135313570458,5.4380000849015));
#30074=CARTESIAN_POINT('Ctrl Pts',(34.0065949722125,39.2456807571843,5.28099995754925));
#30075=CARTESIAN_POINT('Ctrl Pts',(37.9932255349056,38.1706876091981,5.12399983019699));
#30076=CARTESIAN_POINT('Ctrl Pts',(39.2958020508805,34.2525084052524,4.96699970284474));
#30077=CARTESIAN_POINT('Ctrl Pts',(36.7462916527279,31.0046121145067,4.80999957549249));
#30078=CARTESIAN_POINT('Ctrl Pts',(32.6308647779182,31.3394184562628,4.65299944814024));
#30079=CARTESIAN_POINT('Ctrl Pts',(30.6398641844617,34.956703393489,4.49599932078798));
#30080=CARTESIAN_POINT('Ctrl Pts',(32.5586392064025,38.612812809568,4.33899919343573));
#30081=CARTESIAN_POINT('Ctrl Pts',(36.6666058731669,39.0292783213552,4.18199906608348));
#30082=CARTESIAN_POINT('Ctrl Pts',(39.2801110647917,35.8326513062801,4.02499893873122));
#30083=CARTESIAN_POINT('Ctrl Pts',(38.0555996031866,31.889377877368,3.86799881137897));
#30084=CARTESIAN_POINT('Ctrl Pts',(34.0911026630479,30.7354291472295,3.71099868402672));
#30085=CARTESIAN_POINT('Ctrl Pts',(30.9416226850806,33.4055620139871,3.55399855667446));
#30086=CARTESIAN_POINT('Ctrl Pts',(31.4313285785645,37.5054427177457,3.39699842932221));
#30087=CARTESIAN_POINT('Ctrl Pts',(35.1210963742505,39.3586689031172,3.23999830196995));
#30088=CARTESIAN_POINT('Ctrl Pts',(38.7022758847263,37.3034348623974,3.0829981746177));
#30089=CARTESIAN_POINT('Ctrl Pts',(38.9635891007609,33.1826886934549,2.92599804726545));
#30090=CARTESIAN_POINT('Ctrl Pts',(35.6707139262103,30.691542985346,2.76899791991319));
#30091=CARTESIAN_POINT('Ctrl Pts',(31.7764031777353,32.0638320605518,2.61199779256094));
#30092=CARTESIAN_POINT('Ctrl Pts',(30.7727225485069,36.0690110050931,2.45499766520869));
#30093=CARTESIAN_POINT('Ctrl Pts',(33.5596823199811,39.1155977076656,2.29799753785643));
#30094=CARTESIAN_POINT('Ctrl Pts',(37.6381884600154,38.4716880959441,2.14099741050418));
#30095=CARTESIAN_POINT('Ctrl Pts',(39.3510063287937,34.7146832013567,1.98399728315193));
#30096=CARTESIAN_POINT('Ctrl Pts',(37.1622338104923,31.2135231289919,1.82699715579967));
#30097=CARTESIAN_POINT('Ctrl Pts',(33.0345680505794,31.1077361916065,1.66999702844742));
#30098=CARTESIAN_POINT('Ctrl Pts',(30.6693188173153,34.4921735091382,1.51299690109517));
#30099=CARTESIAN_POINT('Ctrl Pts',(32.1874433402447,38.3319958888659,1.35599677374292));
#30100=CARTESIAN_POINT('Ctrl Pts',(36.227593460831,39.1839610551084,1.19899664639066));
#30101=CARTESIAN_POINT('Ctrl Pts',(39.1669909447667,36.2841776398386,1.04199651903841));
#30102=CARTESIAN_POINT('Ctrl Pts',(38.3697226472005,32.2327602036007,0.884996391686153));
#30103=CARTESIAN_POINT('Ctrl Pts',(34.5509630471873,30.6629539550025,0.727996264333901));
#30104=CARTESIAN_POINT('Ctrl Pts',(31.1345139786991,32.9818140634986,0.570996136981646));
#30105=CARTESIAN_POINT('Ctrl Pts',(31.1849789200754,37.1112158757118,0.413996009629392));
#30106=CARTESIAN_POINT('Ctrl Pts',(34.6550079471686,39.3458268431676,0.256995882277139));
#30107=CARTESIAN_POINT('Ctrl Pts',(38.4372231849787,37.6868217065119,0.0999957549248859));
#30108=CARTESIAN_POINT('Ctrl Pts',(39.1314848156243,33.611627523338,-0.0570043724273679));
#30109=CARTESIAN_POINT('Ctrl Pts',(37.1325959372044,31.7372591159268,-0.161671123995537));
#30110=CARTESIAN_POINT('Ctrl Pts',(35.9563385206894,31.4227955987545,-0.214004499779622));
#30111=CARTESIAN_POINT('Ctrl Pts',(37.9552630411254,37.5267093987114,8.21400449977962));
#30112=CARTESIAN_POINT('Ctrl Pts',(38.7860963780679,36.5549589254462,8.16167112399554));
#30113=CARTESIAN_POINT('Ctrl Pts',(39.4009732488241,33.744049865601,8.05700437242737));
#30114=CARTESIAN_POINT('Ctrl Pts',(36.37629757881,30.6305236834712,7.90000424507512));
#30115=CARTESIAN_POINT('Ctrl Pts',(32.1165942698471,31.4445388603786,7.74300411772287));
#30116=CARTESIAN_POINT('Ctrl Pts',(30.4429364274986,35.4422074306354,7.58600399037061));
#30117=CARTESIAN_POINT('Ctrl Pts',(32.8554054932919,39.0456002474389,7.42900386301836));
#30118=CARTESIAN_POINT('Ctrl Pts',(37.1910702102687,39.020145495151,7.2720037356661));
#30119=CARTESIAN_POINT('Ctrl Pts',(39.561923078043,35.3903430207689,7.11500360831385));
#30120=CARTESIAN_POINT('Ctrl Pts',(37.8420846273271,31.4102406249626,6.95800348096159));
#30121=CARTESIAN_POINT('Ctrl Pts',(33.5737072973814,30.6492466703945,6.80100335360934));
#30122=CARTESIAN_POINT('Ctrl Pts',(30.5843074279779,33.789547088263,6.64400322625708));
#30123=CARTESIAN_POINT('Ctrl Pts',(31.5544979211211,38.0153059312343,6.48700309890484));
#30124=CARTESIAN_POINT('Ctrl Pts',(35.6143049344472,39.5371942999712,6.33000297155258));
#30125=CARTESIAN_POINT('Ctrl Pts',(39.1232579504846,36.9905453090318,6.17300284420033));
#30126=CARTESIAN_POINT('Ctrl Pts',(38.9348464369457,32.6589511253872,6.01600271684807));
#30127=CARTESIAN_POINT('Ctrl Pts',(35.2180201601081,30.4265999701529,5.85900258949582));
#30128=CARTESIAN_POINT('Ctrl Pts',(31.3056932203567,32.2952594827172,5.70200246214357));
#30129=CARTESIAN_POINT('Ctrl Pts',(30.7060865587576,36.5892862685565,5.54500233479131));
#30130=CARTESIAN_POINT('Ctrl Pts',(33.956873300029,39.4581845606676,5.38800220743906));
#30131=CARTESIAN_POINT('Ctrl Pts',(38.1430417474823,38.3293861113103,5.2310020800868));
#30132=CARTESIAN_POINT('Ctrl Pts',(39.5108145134353,34.2150951337324,5.07400195273456));
#30133=CARTESIAN_POINT('Ctrl Pts',(36.8336966271993,30.8046359103087,4.9170018253823));
#30134=CARTESIAN_POINT('Ctrl Pts',(32.512285385248,31.1561998994534,4.76000169803005));
#30135=CARTESIAN_POINT('Ctrl Pts',(30.4216317036192,34.9545363220374,4.60300157067779));
#30136=CARTESIAN_POINT('Ctrl Pts',(32.4364447966046,38.7936404570559,4.44600144332554));
#30137=CARTESIAN_POINT('Ctrl Pts',(36.750022433952,39.2309508015887,4.28900131597329));
#30138=CARTESIAN_POINT('Ctrl Pts',(39.4943381658426,35.8743269714277,4.13200118862103));
#30139=CARTESIAN_POINT('Ctrl Pts',(38.2085377477941,31.7336857587036,3.97500106126878));
#30140=CARTESIAN_POINT('Ctrl Pts',(34.0456107497072,30.5219798611747,3.81800093391652));
#30141=CARTESIAN_POINT('Ctrl Pts',(30.738493748942,33.3257575831257,3.66100080656427));
#30142=CARTESIAN_POINT('Ctrl Pts',(31.252710285337,37.6308445407701,3.50400067921202));
#30143=CARTESIAN_POINT('Ctrl Pts',(35.1271574611734,39.5768279624082,3.34700055185977));
#30144=CARTESIAN_POINT('Ctrl Pts',(38.8875813167745,37.4187258362905,3.19000042450751));
#30145=CARTESIAN_POINT('Ctrl Pts',(39.1619737197485,33.0917290601617,3.03300029715526));
#30146=CARTESIAN_POINT('Ctrl Pts',(35.7042843401251,30.4758971195542,2.876000169803));
#30147=CARTESIAN_POINT('Ctrl Pts',(31.6150564762743,31.9168716811727,2.71900004245075));
#30148=CARTESIAN_POINT('Ctrl Pts',(30.5611398629031,36.1225168896708,2.5619999150985));
#30149=CARTESIAN_POINT('Ctrl Pts',(33.48759188202,39.3215906252928,2.40499978774624));
#30150=CARTESIAN_POINT('Ctrl Pts',(37.7702344413602,38.6454522028303,2.24799966039399));
#30151=CARTESIAN_POINT('Ctrl Pts',(39.568781862737,34.7004025928096,2.09099953304174));
#30152=CARTESIAN_POINT('Ctrl Pts',(37.2704574229183,31.0240032892043,1.93399940568949));
#30153=CARTESIAN_POINT('Ctrl Pts',(32.9361947180972,30.9129215291889,1.77699927833723));
#30154=CARTESIAN_POINT('Ctrl Pts',(30.4525605927511,34.4667558983969,1.61999915098498));
#30155=CARTESIAN_POINT('Ctrl Pts',(32.0466699232375,38.4987681546272,1.46299902363272));
#30156=CARTESIAN_POINT('Ctrl Pts',(36.2890366767668,39.3933756787425,1.30599889628047));
#30157=CARTESIAN_POINT('Ctrl Pts',(39.3755561844741,36.3484529936443,1.14899876892822));
#30158=CARTESIAN_POINT('Ctrl Pts',(38.5383832036972,32.0942549754603,0.991998641575964));
#30159=CARTESIAN_POINT('Ctrl Pts',(34.5284879564222,30.4458771578634,0.834998514223711));
#30160=CARTESIAN_POINT('Ctrl Pts',(30.9410395917123,32.8808003010019,0.677998386871457));
#30161=CARTESIAN_POINT('Ctrl Pts',(30.9940303923319,37.2168859506,0.520998259519203));
#30162=CARTESIAN_POINT('Ctrl Pts',(34.6377404869918,39.5633431347282,0.36399813216695));
#30163=CARTESIAN_POINT('Ctrl Pts',(38.6092622623382,37.8213018675437,0.206998004814697));
#30164=CARTESIAN_POINT('Ctrl Pts',(39.3382729110006,33.5421370343408,0.0499978774624429));
#30165=CARTESIAN_POINT('Ctrl Pts',(37.2393361218455,31.5739531851941,-0.0546688741057264));
#30166=CARTESIAN_POINT('Ctrl Pts',(36.0042049488753,31.243750214851,-0.107002249889811));
#30167=CARTESIAN_POINT('Ctrl Pts',(38.0961285948024,37.6471475165633,8.32100674966943));
#30168=CARTESIAN_POINT('Ctrl Pts',(38.9665644295237,36.6290775899881,8.26867337388535));
#30169=CARTESIAN_POINT('Ctrl Pts',(39.6107500181967,33.6841837526321,8.16400662231718));
#30170=CARTESIAN_POINT('Ctrl Pts',(36.441900172476,30.4222482467195,8.00700649496493));
#30171=CARTESIAN_POINT('Ctrl Pts',(31.9791538664038,31.2750642670716,7.85000636761267));
#30172=CARTESIAN_POINT('Ctrl Pts',(30.2257194575204,35.4632856878632,7.69300624026042));
#30173=CARTESIAN_POINT('Ctrl Pts',(32.753181262015,39.238437809064,7.53600611290817));
#30174=CARTESIAN_POINT('Ctrl Pts',(37.2955097522044,39.2117697306779,7.37900598555592));
#30175=CARTESIAN_POINT('Ctrl Pts',(39.7793716811886,35.4089491092894,7.22200585820366));
#30176=CARTESIAN_POINT('Ctrl Pts',(37.9775554192851,31.2391311721338,7.06500573085141));
#30177=CARTESIAN_POINT('Ctrl Pts',(33.5057216363881,30.441863683446,6.90800560349916));
#30178=CARTESIAN_POINT('Ctrl Pts',(30.3738290474178,33.7318496456872,6.75100547614689));
#30179=CARTESIAN_POINT('Ctrl Pts',(31.3902646358661,38.1590334890178,6.59400534879465));
#30180=CARTESIAN_POINT('Ctrl Pts',(35.6435863904507,39.7534641813021,6.43700522144238));
#30181=CARTESIAN_POINT('Ctrl Pts',(39.3197971438036,37.085426632005,6.28000509409014));
#30182=CARTESIAN_POINT('Ctrl Pts',(39.122404807981,32.5473627011697,6.12300496673788));
#30183=CARTESIAN_POINT('Ctrl Pts',(35.2284123079944,30.2086043066787,5.96600483938564));
#30184=CARTESIAN_POINT('Ctrl Pts',(31.1296004114509,32.1663353344374,5.80900471203338));
#30185=CARTESIAN_POINT('Ctrl Pts',(30.5014129016501,36.6650411800673,5.65200458468112));
#30186=CARTESIAN_POINT('Ctrl Pts',(33.9071516278456,39.6706883641509,5.49500445732887));
#30187=CARTESIAN_POINT('Ctrl Pts',(38.2928579600589,38.4880846134226,5.33800432997661));
#30188=CARTESIAN_POINT('Ctrl Pts',(39.72582697599,34.1776818622125,5.18100420262437));
#30189=CARTESIAN_POINT('Ctrl Pts',(36.9211016016709,30.6046597061106,5.0240040752721));
#30190=CARTESIAN_POINT('Ctrl Pts',(32.3937059925777,30.9729813426439,4.86700394791986));
#30191=CARTESIAN_POINT('Ctrl Pts',(30.2033992227766,34.9523692505858,4.7100038205676));
#30192=CARTESIAN_POINT('Ctrl Pts',(32.3142503868067,38.9744681045439,4.55300369321535));
#30193=CARTESIAN_POINT('Ctrl Pts',(36.833438994737,39.4326232818222,4.39600356586309));
#30194=CARTESIAN_POINT('Ctrl Pts',(39.7085652668935,35.9160026365752,4.23900343851085));
#30195=CARTESIAN_POINT('Ctrl Pts',(38.3614758924016,31.5779936400392,4.08200331115859));
#30196=CARTESIAN_POINT('Ctrl Pts',(34.0001188363665,30.3085305751198,3.92500318380634));
#30197=CARTESIAN_POINT('Ctrl Pts',(30.5353648128034,33.2459531522644,3.76800305645408));
#30198=CARTESIAN_POINT('Ctrl Pts',(31.0740919921095,37.7562463637945,3.61100292910183));
#30199=CARTESIAN_POINT('Ctrl Pts',(35.1332185480963,39.7949870216991,3.45400280174957));
#30200=CARTESIAN_POINT('Ctrl Pts',(39.0728867488228,37.5340168101838,3.29700267439732));
#30201=CARTESIAN_POINT('Ctrl Pts',(39.360358338736,33.0007694268683,3.14000254704507));
#30202=CARTESIAN_POINT('Ctrl Pts',(35.7378547540399,30.2602512537625,2.98300241969282));
#30203=CARTESIAN_POINT('Ctrl Pts',(31.4537097748133,31.7699113017935,2.82600229234056));
#30204=CARTESIAN_POINT('Ctrl Pts',(30.3495571772993,36.1760227742485,2.66900216498831));
#30205=CARTESIAN_POINT('Ctrl Pts',(33.415501444059,39.52758354292,2.51200203763605));
#30206=CARTESIAN_POINT('Ctrl Pts',(37.902280422705,38.8192163097165,2.3550019102838));
#30207=CARTESIAN_POINT('Ctrl Pts',(39.7865573966804,34.6861219842625,2.19800178293155));
#30208=CARTESIAN_POINT('Ctrl Pts',(37.3786810353442,30.8344834494167,2.0410016555793));
#30209=CARTESIAN_POINT('Ctrl Pts',(32.8378213856151,30.7181068667712,1.88400152822704));
#30210=CARTESIAN_POINT('Ctrl Pts',(30.2358023681867,34.4413382876556,1.72700140087479));
#30211=CARTESIAN_POINT('Ctrl Pts',(31.9058965062304,38.6655404203885,1.57000127352254));
#30212=CARTESIAN_POINT('Ctrl Pts',(36.3504798927025,39.6027903023767,1.41300114617028));
#30213=CARTESIAN_POINT('Ctrl Pts',(39.5841214241815,36.41272834745,1.25600101881803));
#30214=CARTESIAN_POINT('Ctrl Pts',(38.7070437601939,31.9557497473198,1.09900089146578));
#30215=CARTESIAN_POINT('Ctrl Pts',(34.5060128656572,30.2288003607244,0.942000764113522));
#30216=CARTESIAN_POINT('Ctrl Pts',(30.7475652047255,32.7797865385051,0.785000636761267));
#30217=CARTESIAN_POINT('Ctrl Pts',(30.8030818645885,37.3225560254883,0.628000509409015));
#30218=CARTESIAN_POINT('Ctrl Pts',(34.620473026815,39.7808594262888,0.47100038205676));
#30219=CARTESIAN_POINT('Ctrl Pts',(38.7813013396977,37.9557820285754,0.314000254704507));
#30220=CARTESIAN_POINT('Ctrl Pts',(39.5450610063768,33.4726465453437,0.157000127352254));
#30221=CARTESIAN_POINT('Ctrl Pts',(37.3460763064866,31.4106472544613,0.0523333757840845));
#30222=CARTESIAN_POINT('Ctrl Pts',(36.0520713770613,31.0647048309474,0.));
#30223=CARTESIAN_POINT('Ctrl Pts',(36.0520713770613,31.0647048309474,0.));
#30224=CARTESIAN_POINT('Ctrl Pts',(36.1681792227746,31.1043194052127,-1.93406836379874E-16));
#30225=CARTESIAN_POINT('Ctrl Pts',(36.2820220087194,31.1494844117486,-1.00024874895392E-15));
#30226=CARTESIAN_POINT('Ctrl Pts',(36.3933738437048,31.1998422365254,-1.16573417585641E-15));
#30227=CARTESIAN_POINT('Ctrl Pts',(36.5072229375308,31.2513294232309,-1.33493090168249E-15));
#30228=CARTESIAN_POINT('Ctrl Pts',(36.6184687230184,31.3082454542348,-1.64395861563978E-15));
#30229=CARTESIAN_POINT('Ctrl Pts',(36.7268454950609,31.3702566870239,-9.99200722162641E-16));
#30230=CARTESIAN_POINT('Ctrl Pts',(36.8407839045068,31.435450188349,-3.21355391692774E-16));
#30231=CARTESIAN_POINT('Ctrl Pts',(36.9515522547681,31.5062756815887,8.02288849704332E-16));
#30232=CARTESIAN_POINT('Ctrl Pts',(37.058802639455,31.5823916741173,9.99200722162641E-16));
#30233=CARTESIAN_POINT('Ctrl Pts',(37.1526467260561,31.6489931675798,1.17149861056366E-15));
#30234=CARTESIAN_POINT('Ctrl Pts',(37.2437970657742,31.7196462572752,8.48680262035355E-16));
#30235=CARTESIAN_POINT('Ctrl Pts',(37.3319890907744,31.7941443117117,9.99200722162641E-16));
#30236=CARTESIAN_POINT('Ctrl Pts',(37.3493641971328,31.8088215075162,1.02885543304851E-15));
#30237=CARTESIAN_POINT('Ctrl Pts',(37.3666243754182,31.8236479962496,-1.0299785826125E-15));
#30238=CARTESIAN_POINT('Ctrl Pts',(37.3837674478979,31.8386222687341,-1.0547118733939E-15));
#30239=CARTESIAN_POINT('Ctrl Pts',(37.3963017832026,31.8495708634207,-1.07279587555905E-15));
#30240=CARTESIAN_POINT('Ctrl Pts',(37.4087723034701,31.8605974704649,-2.60456824673694E-15));
#30241=CARTESIAN_POINT('Ctrl Pts',(37.4211693573137,31.8716933759855,-2.4980018054066E-15));
#30242=CARTESIAN_POINT('Ctrl Pts',(37.5137485970205,31.954555845562,-1.70218045614906E-15));
#30243=CARTESIAN_POINT('Ctrl Pts',(37.6023719888639,32.0414000295362,-2.33877871405102E-15));
#30244=CARTESIAN_POINT('Ctrl Pts',(37.6867781087441,32.1319050017937,-1.99840144432528E-15));
#30245=CARTESIAN_POINT('Ctrl Pts',(37.7709925191637,32.2222044124232,-1.65879726478403E-15));
#30246=CARTESIAN_POINT('Ctrl Pts',(37.8510093104121,32.3161487056446,-9.47721428060247E-16));
#30247=CARTESIAN_POINT('Ctrl Pts',(37.9265284067741,32.4134511741487,-1.30451205393456E-15));
#30248=CARTESIAN_POINT('Ctrl Pts',(38.0010152019123,32.5094235756611,-1.65642556372184E-15));
#30249=CARTESIAN_POINT('Ctrl Pts',(38.0711268225993,32.6086636566059,-6.10757404334397E-16));
#30250=CARTESIAN_POINT('Ctrl Pts',(38.1365292929227,32.710917134839,-5.27355936696949E-16));
#30251=CARTESIAN_POINT('Ctrl Pts',(38.1898350382321,32.7942579909372,-4.59380256721482E-16));
#30252=CARTESIAN_POINT('Ctrl Pts',(38.2400117946351,32.8796011515617,-1.29327937900734E-15));
#30253=CARTESIAN_POINT('Ctrl Pts',(38.28685279593,32.9668147810226,-1.63757896132211E-15));
#30254=CARTESIAN_POINT('Ctrl Pts',(38.298752249944,32.9889704682297,-1.72504457763057E-15));
#30255=CARTESIAN_POINT('Ctrl Pts',(38.3104363019817,33.0112468837781,3.54805112116964E-15));
#30256=CARTESIAN_POINT('Ctrl Pts',(38.3219012991264,33.0336418915139,3.66373598126302E-15));
#30257=CARTESIAN_POINT('Ctrl Pts',(38.3300587509266,33.0495761472196,3.74604683213415E-15));
#30258=CARTESIAN_POINT('Ctrl Pts',(38.3381015974855,33.0655632618739,-7.08373702740619E-16));
#30259=CARTESIAN_POINT('Ctrl Pts',(38.3460261690062,33.0815968043693,-6.93889390390723E-16));
#30260=CARTESIAN_POINT('Ctrl Pts',(38.3989870883303,33.1887510080204,-5.97088888833881E-16));
#30261=CARTESIAN_POINT('Ctrl Pts',(38.4467091567301,33.2980550637735,1.26900815615077E-15));
#30262=CARTESIAN_POINT('Ctrl Pts',(38.4889135757351,33.409246351529,1.0547118733939E-15));
#30263=CARTESIAN_POINT('Ctrl Pts',(38.5302818373033,33.5182347083035,8.44661246299018E-16));
#30264=CARTESIAN_POINT('Ctrl Pts',(38.5663491876186,33.6290368908256,3.13106813660632E-16));
#30265=CARTESIAN_POINT('Ctrl Pts',(38.5968048600256,33.7414193655312,4.9960036108132E-16));
#30266=CARTESIAN_POINT('Ctrl Pts',(38.6012591757497,33.7578559431745,5.26876105632901E-16));
#30267=CARTESIAN_POINT('Ctrl Pts',(38.6055933637529,33.7743263394091,3.42924457172855E-16));
#30268=CARTESIAN_POINT('Ctrl Pts',(38.6098063577125,33.7908298367184,3.33066907387547E-16));
#30269=CARTESIAN_POINT('Ctrl Pts',(38.6394749188516,33.9070500410733,3.19833619294622E-16));
#30270=CARTESIAN_POINT('Ctrl Pts',(38.6631375043611,34.0249121336904,2.13657224701249E-16));
#30271=CARTESIAN_POINT('Ctrl Pts',(38.6808849682855,34.1439802784308,6.10622663543836E-16));
#30272=CARTESIAN_POINT('Ctrl Pts',(38.6908685193634,34.2109601528418,8.33929201973265E-16));
#30273=CARTESIAN_POINT('Ctrl Pts',(38.6989793099884,34.2783216258907,1.0776972087123E-15));
#30274=CARTESIAN_POINT('Ctrl Pts',(38.705226464765,34.3459856591442,1.13797860024079E-15));
#30275=CARTESIAN_POINT('Ctrl Pts',(38.7081089504882,34.3772063695005,1.1657929023787E-15));
#30276=CARTESIAN_POINT('Ctrl Pts',(38.7105946047039,34.4084914721069,9.83922849187538E-16));
#30277=CARTESIAN_POINT('Ctrl Pts',(38.7126839762627,34.4398330679179,1.02695629777827E-15));
#30278=CARTESIAN_POINT('Ctrl Pts',(38.7138850693151,34.4578500514573,1.05169444256127E-15));
#30279=CARTESIAN_POINT('Ctrl Pts',(38.7149546915907,34.4758786502346,-4.64302084245928E-16));
#30280=CARTESIAN_POINT('Ctrl Pts',(38.715892912359,34.4939090237972,-4.44089209850063E-16));
#30281=CARTESIAN_POINT('Ctrl Pts',(38.7222038666684,34.6151905681615,-3.08127044991787E-16));
#30282=CARTESIAN_POINT('Ctrl Pts',(38.7225822971166,34.7366693867671,-2.99144274726584E-15));
#30283=CARTESIAN_POINT('Ctrl Pts',(38.7171864105867,34.8578982328034,-2.05391259555654E-15));
#30284=CARTESIAN_POINT('Ctrl Pts',(38.71190245704,34.9766122916381,-1.13583069320137E-15));
#30285=CARTESIAN_POINT('Ctrl Pts',(38.7010807679502,35.0950875649844,1.78168855748587E-15));
#30286=CARTESIAN_POINT('Ctrl Pts',(38.6848165352731,35.2128980770419,1.76247905159244E-15));
#30287=CARTESIAN_POINT('Ctrl Pts',(38.6687112067838,35.3295575613132,1.74345722568323E-15));
#30288=CARTESIAN_POINT('Ctrl Pts',(38.6472688142291,35.4455660470931,1.26625388930718E-16));
#30289=CARTESIAN_POINT('Ctrl Pts',(38.62053500354,35.5604910223212,1.80411241501588E-16));
#30290=CARTESIAN_POINT('Ctrl Pts',(38.6031281268642,35.6353207910372,2.15432201045671E-16));
#30291=CARTESIAN_POINT('Ctrl Pts',(38.5834769893052,35.7096907862118,1.51379352364637E-15));
#30292=CARTESIAN_POINT('Ctrl Pts',(38.5615843902035,35.7834747121961,1.2490009027033E-15));
#30293=CARTESIAN_POINT('Ctrl Pts',(38.5541960332861,35.8083754550181,1.15963817406959E-15));
#30294=CARTESIAN_POINT('Ctrl Pts',(38.5465523248095,35.8332093935643,2.32778305945499E-15));
#30295=CARTESIAN_POINT('Ctrl Pts',(38.5386531847276,35.8579714965102,2.3037127760972E-15));
#30296=CARTESIAN_POINT('Ctrl Pts',(38.5335667575399,35.8739163502969,2.28821339990993E-15));
#30297=CARTESIAN_POINT('Ctrl Pts',(38.528375210839,35.8898288067619,1.8799349255917E-16));
#30298=CARTESIAN_POINT('Ctrl Pts',(38.5230814037796,35.9056994997334,2.77555756156289E-16));
#30299=CARTESIAN_POINT('Ctrl Pts',(38.4861837480683,36.016317691632,9.0180169672523E-16));
#30300=CARTESIAN_POINT('Ctrl Pts',(38.4442853792632,36.1250244064477,1.67610385059537E-15));
#30301=CARTESIAN_POINT('Ctrl Pts',(38.3974510894444,36.2314004501635,1.54737334057131E-15));
#30302=CARTESIAN_POINT('Ctrl Pts',(38.3593370450265,36.3179699544917,1.44261162867242E-15));
#30303=CARTESIAN_POINT('Ctrl Pts',(38.3179530965748,36.4029957144323,1.09861093914672E-15));
#30304=CARTESIAN_POINT('Ctrl Pts',(38.27331318169,36.4862361414904,1.49186218934005E-15));
#30305=CARTESIAN_POINT('Ctrl Pts',(38.2516982037212,36.526541773829,1.68227736219745E-15));
#30306=CARTESIAN_POINT('Ctrl Pts',(38.2293195714479,36.5664285801089,1.70359564472489E-15));
#30307=CARTESIAN_POINT('Ctrl Pts',(38.2061773939932,36.6058676078699,1.76247905159244E-15));
#30308=CARTESIAN_POINT('Ctrl Pts',(38.1925910511184,36.629021529097,1.79704840691352E-15));
#30309=CARTESIAN_POINT('Ctrl Pts',(38.1787394785284,36.652024183054,3.81993764399042E-15));
#30310=CARTESIAN_POINT('Ctrl Pts',(38.1646367510805,36.6748472188681,3.75394160201381E-15));
#30311=CARTESIAN_POINT('Ctrl Pts',(38.1062052960737,36.7694092952617,3.48050195910614E-15));
#30312=CARTESIAN_POINT('Ctrl Pts',(38.0434225704545,36.8609661715359,-8.52927663010733E-16));
#30313=CARTESIAN_POINT('Ctrl Pts',(37.9763226192313,36.9491271397218,-6.21031004399697E-16));
#30314=CARTESIAN_POINT('Ctrl Pts',(37.9162919198372,37.0279999925776,-4.13565598690696E-16));
#30315=CARTESIAN_POINT('Ctrl Pts',(37.8528051248739,37.1041547391556,2.13873726282784E-15));
#30316=CARTESIAN_POINT('Ctrl Pts',(37.7858631238401,37.1772850733286,2.38004060904018E-15));
#30317=CARTESIAN_POINT('Ctrl Pts',(37.7510082002317,37.215362097793,2.52360662668101E-15));
#30318=CARTESIAN_POINT('Ctrl Pts',(37.71521617243,37.2526187144799,1.78459625189646E-16));
#30319=CARTESIAN_POINT('Ctrl Pts',(37.6785244495408,37.2890395253442,2.4980018054066E-16));
#30320=CARTESIAN_POINT('Ctrl Pts',(37.6735319337713,37.2858331630076,8.));
#30321=CARTESIAN_POINT('Ctrl Pts',(37.7506743707736,37.2087205217211,8.));
#30322=CARTESIAN_POINT('Ctrl Pts',(37.8237044431802,37.1279857045437,8.));
#30323=CARTESIAN_POINT('Ctrl Pts',(37.8926298478593,37.044047215584,8.));
#30324=CARTESIAN_POINT('Ctrl Pts',(37.9633151675467,36.957965473245,8.));
#30325=CARTESIAN_POINT('Ctrl Pts',(38.0296839050274,36.8685139150261,8.));
#30326=CARTESIAN_POINT('Ctrl Pts',(38.0917144885261,36.7760977905708,8.));
#30327=CARTESIAN_POINT('Ctrl Pts',(38.1550361362519,36.681758176998,8.));
#30328=CARTESIAN_POINT('Ctrl Pts',(38.213837583624,36.5843287225808,8.));
#30329=CARTESIAN_POINT('Ctrl Pts',(38.2680590919843,36.4842010613249,8.));
#30330=CARTESIAN_POINT('Ctrl Pts',(38.3198483094818,36.3885649681376,8.));
#30331=CARTESIAN_POINT('Ctrl Pts',(38.367459260449,36.2904664802624,8.));
#30332=CARTESIAN_POINT('Ctrl Pts',(38.4108043761726,36.1902222494829,8.));
#30333=CARTESIAN_POINT('Ctrl Pts',(38.4178413961439,36.1739477363751,8.));
#30334=CARTESIAN_POINT('Ctrl Pts',(38.4247659020623,36.1576166279166,8.));
#30335=CARTESIAN_POINT('Ctrl Pts',(38.4315774256463,36.1412302363951,8.));
#30336=CARTESIAN_POINT('Ctrl Pts',(38.4380879567714,36.1255679384209,8.));
#30337=CARTESIAN_POINT('Ctrl Pts',(38.444492253249,36.1098623247479,8.));
#30338=CARTESIAN_POINT('Ctrl Pts',(38.4507880993566,36.0941200527897,8.));
#30339=CARTESIAN_POINT('Ctrl Pts',(38.4941733303702,35.9856386677758,8.));
#30340=CARTESIAN_POINT('Ctrl Pts',(38.5324447107219,35.8753402935035,8.));
#30341=CARTESIAN_POINT('Ctrl Pts',(38.5655736281431,35.7636567372894,8.));
#30342=CARTESIAN_POINT('Ctrl Pts',(38.5991370998293,35.6505082202659,8.));
#30343=CARTESIAN_POINT('Ctrl Pts',(38.6274227108421,35.5359371924552,8.));
#30344=CARTESIAN_POINT('Ctrl Pts',(38.6503580685478,35.4203601525596,8.));
#30345=CARTESIAN_POINT('Ctrl Pts',(38.6743329744418,35.2995445677074,8.));
#30346=CARTESIAN_POINT('Ctrl Pts',(38.6924624153241,35.1776288913195,8.));
#30347=CARTESIAN_POINT('Ctrl Pts',(38.7046079739425,35.0550654857614,8.));
#30348=CARTESIAN_POINT('Ctrl Pts',(38.7137171429063,34.9631429315928,8.));
#30349=CARTESIAN_POINT('Ctrl Pts',(38.7194592548969,34.8708554330634,8.));
#30350=CARTESIAN_POINT('Ctrl Pts',(38.7217527860176,34.7783903770868,8.));
#30351=CARTESIAN_POINT('Ctrl Pts',(38.7223003505608,34.7563149905001,8.));
#30352=CARTESIAN_POINT('Ctrl Pts',(38.7226511975219,34.7342249565511,8.));
#30353=CARTESIAN_POINT('Ctrl Pts',(38.7228041151383,34.7121518890107,8.));
#30354=CARTESIAN_POINT('Ctrl Pts',(38.7236388754478,34.5916574611757,8.));
#30355=CARTESIAN_POINT('Ctrl Pts',(38.7185854897377,34.4715178604479,8.));
#30356=CARTESIAN_POINT('Ctrl Pts',(38.7075750014661,34.3521591261975,8.));
#30357=CARTESIAN_POINT('Ctrl Pts',(38.6966351615249,34.2335662521979,8.));
#30358=CARTESIAN_POINT('Ctrl Pts',(38.6798146688512,34.1157433795803,8.));
#30359=CARTESIAN_POINT('Ctrl Pts',(38.6569964506754,33.9990955538343,8.));
#30360=CARTESIAN_POINT('Ctrl Pts',(38.6541228094095,33.9844053618549,8.));
#30361=CARTESIAN_POINT('Ctrl Pts',(38.6511539769623,33.9697337993248,8.));
#30362=CARTESIAN_POINT('Ctrl Pts',(38.6480896603102,33.9550816715453,8.));
#30363=CARTESIAN_POINT('Ctrl Pts',(38.6241791602958,33.840752853322,8.));
#30364=CARTESIAN_POINT('Ctrl Pts',(38.5944594648021,33.7276067766126,8.));
#30365=CARTESIAN_POINT('Ctrl Pts',(38.5592367168361,33.6159099315205,8.));
#30366=CARTESIAN_POINT('Ctrl Pts',(38.5372714828272,33.5462547375853,8.));
#30367=CARTESIAN_POINT('Ctrl Pts',(38.5131650961288,33.4771632221397,8.));
#30368=CARTESIAN_POINT('Ctrl Pts',(38.4869819486326,33.4087021985955,8.));
#30369=CARTESIAN_POINT('Ctrl Pts',(38.4780327050517,33.385302629251,8.));
#30370=CARTESIAN_POINT('Ctrl Pts',(38.4688407862625,33.3619767358619,8.));
#30371=CARTESIAN_POINT('Ctrl Pts',(38.4594085763077,33.3387272549231,8.));
#30372=CARTESIAN_POINT('Ctrl Pts',(38.4526591454727,33.3220905638083,8.));
#30373=CARTESIAN_POINT('Ctrl Pts',(38.4457861267366,33.3054918782784,8.));
#30374=CARTESIAN_POINT('Ctrl Pts',(38.438797464252,33.2889485050412,8.));
#30375=CARTESIAN_POINT('Ctrl Pts',(38.3928761431039,33.180244792853,8.));
#30376=CARTESIAN_POINT('Ctrl Pts',(38.3419017974374,33.073767495779,8.));
#30377=CARTESIAN_POINT('Ctrl Pts',(38.2862328647479,32.9697709587171,8.));
#30378=CARTESIAN_POINT('Ctrl Pts',(38.2286487527766,32.8621966269402,8.));
#30379=CARTESIAN_POINT('Ctrl Pts',(38.1660413106006,32.757275993628,8.));
#30380=CARTESIAN_POINT('Ctrl Pts',(38.0987518751312,32.6552979021095,8.));
#30381=CARTESIAN_POINT('Ctrl Pts',(38.0308292899206,32.5523602632,8.));
#30382=CARTESIAN_POINT('Ctrl Pts',(37.9581357532083,32.4524200570822,8.));
#30383=CARTESIAN_POINT('Ctrl Pts',(37.8809718147757,32.3557926317859,8.));
#30384=CARTESIAN_POINT('Ctrl Pts',(37.8265588287192,32.2876547573834,8.));
#30385=CARTESIAN_POINT('Ctrl Pts',(37.7699218575833,32.221164530513,8.));
#30386=CARTESIAN_POINT('Ctrl Pts',(37.7111532334385,32.156441009698,8.));
#30387=CARTESIAN_POINT('Ctrl Pts',(37.6849201407301,32.1275497748485,8.));
#30388=CARTESIAN_POINT('Ctrl Pts',(37.6582621737227,32.0990106723795,8.));
#30389=CARTESIAN_POINT('Ctrl Pts',(37.6311869343715,32.0708348649218,8.));
#30390=CARTESIAN_POINT('Ctrl Pts',(37.6195644247842,32.0587399176506,8.));
#30391=CARTESIAN_POINT('Ctrl Pts',(37.6078664443942,32.0467134553255,8.));
#30392=CARTESIAN_POINT('Ctrl Pts',(37.5961000985213,32.0347627427216,8.));
#30393=CARTESIAN_POINT('Ctrl Pts',(37.5076578370054,31.9449346804806,8.));
#30394=CARTESIAN_POINT('Ctrl Pts',(37.4152562466455,31.8592792534028,8.));
#30395=CARTESIAN_POINT('Ctrl Pts',(37.3192240628069,31.7781146097001,8.));
#30396=CARTESIAN_POINT('Ctrl Pts',(37.2371844701374,31.7087762478888,8.));
#30397=CARTESIAN_POINT('Ctrl Pts',(37.1524942030697,31.6427153977926,8.));
#30398=CARTESIAN_POINT('Ctrl Pts',(37.0653339993003,31.5801479843188,8.));
#30399=CARTESIAN_POINT('Ctrl Pts',(37.026223350155,31.552072646602,8.));
#30400=CARTESIAN_POINT('Ctrl Pts',(36.9866151034059,31.5247009668187,8.));
#30401=CARTESIAN_POINT('Ctrl Pts',(36.9465243462331,31.4980538108418,8.));
#30402=CARTESIAN_POINT('Ctrl Pts',(36.9192915198287,31.4799529461023,8.));
#30403=CARTESIAN_POINT('Ctrl Pts',(36.891830409748,31.4621830185383,8.));
#30404=CARTESIAN_POINT('Ctrl Pts',(36.8641757039143,31.4447693408987,8.));
#30405=CARTESIAN_POINT('Ctrl Pts',(36.7573714959831,31.3775166259847,8.));
#30406=CARTESIAN_POINT('Ctrl Pts',(36.6476205511297,31.3155307102762,8.));
#30407=CARTESIAN_POINT('Ctrl Pts',(36.53522484258,31.2591452484686,8.));
#30408=CARTESIAN_POINT('Ctrl Pts',(36.4331310435836,31.2079279370747,8.));
#30409=CARTESIAN_POINT('Ctrl Pts',(36.328854296794,31.161331443821,8.));
#30410=CARTESIAN_POINT('Ctrl Pts',(36.2225975660985,31.1196349359533,8.));
#30411=CARTESIAN_POINT('Ctrl Pts',(36.1671670804927,31.0978833004188,8.));
#30412=CARTESIAN_POINT('Ctrl Pts',(36.1111974373468,31.0774656305418,8.));
#30413=CARTESIAN_POINT('Ctrl Pts',(36.0547327596422,31.0583698145405,8.));
#30414=CARTESIAN_POINT('Ctrl Pts',(31.4836963557363,34.997016753135,6.38741669750802));
#30415=CARTESIAN_POINT('Ctrl Pts',(31.4810522497149,34.6831064242593,6.4016107071645));
#30416=CARTESIAN_POINT('Ctrl Pts',(31.5197088623892,34.3698361384337,6.41580471682098));
#30417=CARTESIAN_POINT('Ctrl Pts',(31.602283311232,34.0686052256029,6.42999872647746));
#30418=CARTESIAN_POINT('Ctrl Pts',(31.9067356658548,32.9579655303736,6.48233210226155));
#30419=CARTESIAN_POINT('Ctrl Pts',(32.8082071426114,32.0109890873326,6.53466547804563));
#30420=CARTESIAN_POINT('Ctrl Pts',(33.9025202849968,31.6522420135335,6.58699885382972));
#30421=CARTESIAN_POINT('Ctrl Pts',(34.9968334273823,31.2934949397344,6.6393322296138));
#30422=CARTESIAN_POINT('Ctrl Pts',(36.2839882353967,31.5229772351772,6.69166560539789));
#30423=CARTESIAN_POINT('Ctrl Pts',(37.1868794441274,32.2378302684166,6.74399898118197));
#30424=CARTESIAN_POINT('Ctrl Pts',(38.089770652858,32.952683301656,6.79633235696606));
#30425=CARTESIAN_POINT('Ctrl Pts',(38.6083982623049,34.1529070726919,6.84866573275014));
#30426=CARTESIAN_POINT('Ctrl Pts',(38.5102396094692,35.3003133216048,6.90099910853422));
#30427=CARTESIAN_POINT('Ctrl Pts',(38.4120809566336,36.4477195705176,6.95333248431831));
#30428=CARTESIAN_POINT('Ctrl Pts',(37.6971360415154,37.5423082973073,7.00566586010239));
#30429=CARTESIAN_POINT('Ctrl Pts',(36.6859407221977,38.0934406773841,7.05799923588648));
#30430=CARTESIAN_POINT('Ctrl Pts',(35.67474540288,38.6445730574609,7.11033261167056));
#30431=CARTESIAN_POINT('Ctrl Pts',(34.3672996793629,38.6522490908248,7.16266598745465));
#30432=CARTESIAN_POINT('Ctrl Pts',(33.3498295528725,38.1127747395053,7.21499936323873));
#30433=CARTESIAN_POINT('Ctrl Pts',(32.3323594263822,37.5733003881858,7.26733273902282));
#30434=CARTESIAN_POINT('Ctrl Pts',(31.6048648969186,36.4866756521828,7.3196661148069));
#30435=CARTESIAN_POINT('Ctrl Pts',(31.4934684170666,35.3406028059835,7.37199949059098));
#30436=CARTESIAN_POINT('Ctrl Pts',(31.4825294286169,35.2280599532493,7.37713855956333));
#30437=CARTESIAN_POINT('Ctrl Pts',(31.4775314630746,35.1149438434099,7.38227762853567));
#30438=CARTESIAN_POINT('Ctrl Pts',(31.47826034488,35.0017653187145,7.38741669750802));
#30439=CARTESIAN_POINT('Ctrl Pts',(33.9479286229388,31.0647048309474,8.));
#30440=CARTESIAN_POINT('Ctrl Pts',(32.6539236935135,31.4106472544613,7.94766662421592));
#30441=CARTESIAN_POINT('Ctrl Pts',(30.454936822078,33.4726324908028,7.84299987264775));
#30442=CARTESIAN_POINT('Ctrl Pts',(31.2187005389846,37.9557872897229,7.6859997452955));
#30443=CARTESIAN_POINT('Ctrl Pts',(35.3795268052061,39.7808547962683,7.52899961794324));
#30444=CARTESIAN_POINT('Ctrl Pts',(39.1969168896572,37.3225573472918,7.37199949059099));
#30445=CARTESIAN_POINT('Ctrl Pts',(39.2524338890068,32.7797860374403,7.21499936323873));
#30446=CARTESIAN_POINT('Ctrl Pts',(35.4939868648458,30.2288021766129,7.05799923588648));
#30447=CARTESIAN_POINT('Ctrl Pts',(31.2929572874421,31.9557502059188,6.90099910853422));
#30448=CARTESIAN_POINT('Ctrl Pts',(30.4158796925061,36.4127281597254,6.74399898118197));
#30449=CARTESIAN_POINT('Ctrl Pts',(33.6495204900336,39.6027890266495,6.58699885382972));
#30450=CARTESIAN_POINT('Ctrl Pts',(38.0941026784935,38.6655395297167,6.42999872647747));
#30451=CARTESIAN_POINT('Ctrl Pts',(39.7641964207046,34.4413384042963,6.27299859912521));
#30452=CARTESIAN_POINT('Ctrl Pts',(37.1621780526355,30.7181079801836,6.11599847177296));
#30453=CARTESIAN_POINT('Ctrl Pts',(32.6213195789955,30.8344845112897,5.95899834442071));
#30454=CARTESIAN_POINT('Ctrl Pts',(30.2134438300848,34.686122068773,5.80199821706845));
#30455=CARTESIAN_POINT('Ctrl Pts',(32.0977203234525,38.8192153272012,5.6449980897162));
#30456=CARTESIAN_POINT('Ctrl Pts',(36.5844981485848,39.5275823816942,5.48799796236394));
#30457=CARTESIAN_POINT('Ctrl Pts',(39.6504416291735,36.1760224717832,5.33099783501169));
#30458=CARTESIAN_POINT('Ctrl Pts',(38.5462893146292,31.7699121313011,5.17399770765944));
#30459=CARTESIAN_POINT('Ctrl Pts',(34.2621454354683,30.2602524703801,5.01699758030718));
#30460=CARTESIAN_POINT('Ctrl Pts',(30.6396427805907,33.0007699401812,4.85999745295493));
#30461=CARTESIAN_POINT('Ctrl Pts',(30.927114296777,37.5340161596205,4.70299732560268));
#30462=CARTESIAN_POINT('Ctrl Pts',(34.86678148609,39.7949857907703,4.54599719825042));
#30463=CARTESIAN_POINT('Ctrl Pts',(38.9259070000539,37.7562456562111,4.38899707089817));
#30464=CARTESIAN_POINT('Ctrl Pts',(39.4646340410498,33.2459536025622,4.23199694354592));
#30465=CARTESIAN_POINT('Ctrl Pts',(35.9998809069499,30.3085317794917,4.07499681619366));
#30466=CARTESIAN_POINT('Ctrl Pts',(31.6385249705421,31.5779945185253,3.91799668884141));
#30467=CARTESIAN_POINT('Ctrl Pts',(30.291435941871,35.9160024014201,3.76099656148915));
#30468=CARTESIAN_POINT('Ctrl Pts',(33.1665614759356,39.4326221439007,3.60399643413691));
#30469=CARTESIAN_POINT('Ctrl Pts',(37.6857489237188,38.9744670842276,3.44699630678464));
#30470=CARTESIAN_POINT('Ctrl Pts',(39.7965995458586,34.9523692628263,3.2899961794324));
#30471=CARTESIAN_POINT('Ctrl Pts',(37.6062933383462,30.9729823764193,3.13299605208014));
#30472=CARTESIAN_POINT('Ctrl Pts',(33.078898891504,30.6046608345122,2.97599592472789));
#30473=CARTESIAN_POINT('Ctrl Pts',(30.2741742372111,34.1776820732232,2.81899579737563));
#30474=CARTESIAN_POINT('Ctrl Pts',(31.7071428852578,38.4880837181509,2.66199567002338));
#30475=CARTESIAN_POINT('Ctrl Pts',(36.0928480916297,39.6706871647746,2.50499554267113));
#30476=CARTESIAN_POINT('Ctrl Pts',(39.4985859434327,36.6650407532663,2.34799541531887));
#30477=CARTESIAN_POINT('Ctrl Pts',(38.8703985950797,32.1663360606625,2.19099528796662));
#30478=CARTESIAN_POINT('Ctrl Pts',(34.7715877503781,30.208605539026,2.03399516061437));
#30479=CARTESIAN_POINT('Ctrl Pts',(30.8775962508689,32.547363326415,1.87699503326212));
#30480=CARTESIAN_POINT('Ctrl Pts',(30.6802039639638,37.0854261049008,1.71999490590986));
#30481=CARTESIAN_POINT('Ctrl Pts',(34.3564137772933,39.7534629455386,1.56299477855761));
#30482=CARTESIAN_POINT('Ctrl Pts',(38.6097344321268,38.159032706872,1.40599465120535));
#30483=CARTESIAN_POINT('Ctrl Pts',(39.6261697761982,33.7318499178854,1.2489945238531));
#30484=CARTESIAN_POINT('Ctrl Pts',(36.4942779564007,30.441864951573,1.09199439650085));
#30485=CARTESIAN_POINT('Ctrl Pts',(32.0224453946446,31.2391319593762,0.934994269148593));
#30486=CARTESIAN_POINT('Ctrl Pts',(30.2206294419397,35.4089493247815,0.77799414179634));
#30487=CARTESIAN_POINT('Ctrl Pts',(32.7044910542971,39.2117680815463,0.620994014444087));
#30488=CARTESIAN_POINT('Ctrl Pts',(37.246817707304,39.2384377086451,0.463993887091833));
#30489=CARTESIAN_POINT('Ctrl Pts',(39.7742802645754,35.4632838929154,0.30699375973958));
#30490=CARTESIAN_POINT('Ctrl Pts',(38.0208433725288,31.2750679875305,0.149993632387326));
#30491=CARTESIAN_POINT('Ctrl Pts',(33.5581043558821,30.4222449751611,-0.00700649496492684));
#30492=CARTESIAN_POINT('Ctrl Pts',(30.3892402311535,33.6841941049532,-0.164006622317179));
#30493=CARTESIAN_POINT('Ctrl Pts',(31.0334355704763,36.629077589988,-0.26867337388535));
#30494=CARTESIAN_POINT('Ctrl Pts',(31.9038714051976,37.6471475165632,-0.321006749669435));
#30495=CARTESIAN_POINT('Ctrl Pts',(33.9957950511247,31.243750214851,8.10700224988981));
#30496=CARTESIAN_POINT('Ctrl Pts',(32.7606638781546,31.573953185194,8.05466887410573));
#30497=CARTESIAN_POINT('Ctrl Pts',(30.6617250162538,33.5421236192438,7.95000212253755));
#30498=CARTESIAN_POINT('Ctrl Pts',(31.3907395308691,37.8213068893232,7.79300199518531));
#30499=CARTESIAN_POINT('Ctrl Pts',(35.3622593526719,39.5633387153612,7.63600186783305));
#30500=CARTESIAN_POINT('Ctrl Pts',(39.0059684185923,37.2168872122651,7.4790017404808));
#30501=CARTESIAN_POINT('Ctrl Pts',(39.0589595432527,32.8807998227341,7.32200161312854));
#30502=CARTESIAN_POINT('Ctrl Pts',(35.4715117863422,30.4458788911338,7.16500148577629));
#30503=CARTESIAN_POINT('Ctrl Pts',(31.4616177962741,32.0942554131942,7.00800135842404));
#30504=CARTESIAN_POINT('Ctrl Pts',(30.6244448814073,36.3484528144607,6.85100123107178));
#30505=CARTESIAN_POINT('Ctrl Pts',(33.7109636885558,39.3933744610575,6.69400110371954));
#30506=CARTESIAN_POINT('Ctrl Pts',(37.9533292985792,38.4987673044786,6.53700097636727));
#30507=CARTESIAN_POINT('Ctrl Pts',(39.5474382512424,34.4667560097307,6.38000084901502));
#30508=CARTESIAN_POINT('Ctrl Pts',(37.0638047457115,30.9129225919439,6.22300072166277));
#30509=CARTESIAN_POINT('Ctrl Pts',(32.7295431634706,31.0240043027649,6.06600059431052));
#30510=CARTESIAN_POINT('Ctrl Pts',(30.4312193082136,34.7004026734751,5.90900046695826));
#30511=CARTESIAN_POINT('Ctrl Pts',(32.2297662708491,38.6454512650169,5.75200033960601));
#30512=CARTESIAN_POINT('Ctrl Pts',(36.5124077291574,39.3215895168996,5.59500021225375));
#30513=CARTESIAN_POINT('Ctrl Pts',(39.4388589978718,36.1225166009669,5.4380000849015));
#30514=CARTESIAN_POINT('Ctrl Pts',(38.3849426545962,31.9168724729398,5.28099995754925));
#30515=CARTESIAN_POINT('Ctrl Pts',(34.295715840761,30.4758982808191,5.12399983019699));
#30516=CARTESIAN_POINT('Ctrl Pts',(30.8380273486519,33.0917295501202,4.96699970284475));
#30517=CARTESIAN_POINT('Ctrl Pts',(31.1124196812533,37.4187252153261,4.80999957549248));
#30518=CARTESIAN_POINT('Ctrl Pts',(34.8728425714575,39.5768267874833,4.65299944814023));
#30519=CARTESIAN_POINT('Ctrl Pts',(38.7472887526802,37.6308438653799,4.49599932078798));
#30520=CARTESIAN_POINT('Ctrl Pts',(39.2615051570579,33.3257580129361,4.33899919343573));
#30521=CARTESIAN_POINT('Ctrl Pts',(35.9543890052876,30.5219810107509,4.18199906608348));
#30522=CARTESIAN_POINT('Ctrl Pts',(31.7914630758879,31.7336865972209,4.02499893873122));
#30523=CARTESIAN_POINT('Ctrl Pts',(30.5056629879263,35.8743267469715,3.86799881137897));
#30524=CARTESIAN_POINT('Ctrl Pts',(33.2499780153063,39.2309497154396,3.71099868402671));
#30525=CARTESIAN_POINT('Ctrl Pts',(37.5635545452901,38.7936394831613,3.55399855667446));
#30526=CARTESIAN_POINT('Ctrl Pts',(39.5783671210399,34.954536333721,3.39699842932221));
#30527=CARTESIAN_POINT('Ctrl Pts',(37.4877139761171,31.1562008861948,3.23999830196995));
#30528=CARTESIAN_POINT('Ctrl Pts',(33.1663038435374,30.804636987371,3.0829981746177));
#30529=CARTESIAN_POINT('Ctrl Pts',(30.4891866445685,34.2150953351428,2.92599804726545));
#30530=CARTESIAN_POINT('Ctrl Pts',(31.8569590593748,38.3293852567711,2.76899791991319));
#30531=CARTESIAN_POINT('Ctrl Pts',(36.0431264322094,39.4581834158598,2.61199779256094));
#30532=CARTESIAN_POINT('Ctrl Pts',(39.2939123388708,36.5892858611738,2.45499766520869));
#30533=CARTESIAN_POINT('Ctrl Pts',(38.6943058313741,32.295260175901,2.29799753785643));
#30534=CARTESIAN_POINT('Ctrl Pts',(34.7819798956087,30.4266011464317,2.14099741050418));
#30535=CARTESIAN_POINT('Ctrl Pts',(31.0651545737294,32.6589517221855,1.98399728315193));
#30536=CARTESIAN_POINT('Ctrl Pts',(30.8767431068824,36.9905448059094,1.82699715579967));
#30537=CARTESIAN_POINT('Ctrl Pts',(34.3856952256649,39.5371931204316,1.66999702844742));
#30538=CARTESIAN_POINT('Ctrl Pts',(38.4455011892756,38.015305184674,1.51299690109516));
#30539=CARTESIAN_POINT('Ctrl Pts',(39.4156914491603,33.789547348077,1.35599677374291));
#30540=CARTESIAN_POINT('Ctrl Pts',(36.4262923139345,30.6492478808251,1.19899664639066));
#30541=CARTESIAN_POINT('Ctrl Pts',(32.1579161495709,31.4102413763875,1.0419965190384));
#30542=CARTESIAN_POINT('Ctrl Pts',(30.438077993986,35.3903432264567,0.884996391686151));
#30543=CARTESIAN_POINT('Ctrl Pts',(32.8089305595391,39.0201439210504,0.727996264333897));
#30544=CARTESIAN_POINT('Ctrl Pts',(37.1445935229203,39.0456001515887,0.570996136981644));
#30545=CARTESIAN_POINT('Ctrl Pts',(39.5570633072411,35.4422057173529,0.413996009629391));
#30546=CARTESIAN_POINT('Ctrl Pts',(37.8834030947066,31.4445424115665,0.256995882277137));
#30547=CARTESIAN_POINT('Ctrl Pts',(33.6237067435201,30.63052056076,0.0999957549248841));
#30548=CARTESIAN_POINT('Ctrl Pts',(30.5990174441545,33.7440597469193,-0.0570043724273687));
#30549=CARTESIAN_POINT('Ctrl Pts',(31.2139036219321,36.5549589254462,-0.161671123995539));
#30550=CARTESIAN_POINT('Ctrl Pts',(32.0447369588746,37.5267093987113,-0.214004499779624));
#30551=CARTESIAN_POINT('Ctrl Pts',(34.0436614793107,31.4227955987545,8.21400449977962));
#30552=CARTESIAN_POINT('Ctrl Pts',(32.8674040627957,31.7372591159268,8.16167112399554));
#30553=CARTESIAN_POINT('Ctrl Pts',(30.8685132104295,33.6116147476849,8.05700437242736));
#30554=CARTESIAN_POINT('Ctrl Pts',(31.5627785227536,37.6868264889233,7.90000424507513));
#30555=CARTESIAN_POINT('Ctrl Pts',(35.3449919001376,39.3458226344541,7.74300411772285));
#30556=CARTESIAN_POINT('Ctrl Pts',(38.8150199475273,37.1112170772383,7.58600399037062));
#30557=CARTESIAN_POINT('Ctrl Pts',(38.8654851974986,32.9818136080279,7.42900386301834));
#30558=CARTESIAN_POINT('Ctrl Pts',(35.4490367078385,30.6629556056548,7.27200373566611));
#30559=CARTESIAN_POINT('Ctrl Pts',(31.6302783051062,32.2327606204696,7.11500360831384));
#30560=CARTESIAN_POINT('Ctrl Pts',(30.8330100703084,36.284177469196,6.9580034809616));
#30561=CARTESIAN_POINT('Ctrl Pts',(33.7724068870781,39.1839598954654,6.80100335360933));
#30562=CARTESIAN_POINT('Ctrl Pts',(37.812555918665,38.3319950792405,6.64400322625709));
#30563=CARTESIAN_POINT('Ctrl Pts',(39.3306800817804,34.4921736151651,6.48700309890483));
#30564=CARTESIAN_POINT('Ctrl Pts',(36.9654314387874,31.1077372037044,6.33000297155258));
#30565=CARTESIAN_POINT('Ctrl Pts',(32.8377667479458,31.2135240942401,6.17300284420033));
#30566=CARTESIAN_POINT('Ctrl Pts',(30.6489947863424,34.7146832781773,6.01600271684807));
#30567=CARTESIAN_POINT('Ctrl Pts',(32.3618122182458,38.4716872028325,5.85900258949582));
#30568=CARTESIAN_POINT('Ctrl Pts',(36.4403173097299,39.1155966521051,5.70200246214356));
#30569=CARTESIAN_POINT('Ctrl Pts',(39.2272763665704,36.0690107301504,5.54500233479131));
#30570=CARTESIAN_POINT('Ctrl Pts',(38.2235959945632,32.0638328145787,5.38800220743906));
#30571=CARTESIAN_POINT('Ctrl Pts',(34.3292862460537,30.6915440912579,5.2310020800868));
#30572=CARTESIAN_POINT('Ctrl Pts',(31.0364119167131,33.1826891600592,5.07400195273456));
#30573=CARTESIAN_POINT('Ctrl Pts',(31.2977250657295,37.3034342710318,4.9170018253823));
#30574=CARTESIAN_POINT('Ctrl Pts',(34.8789036568251,39.3586677841964,4.76000169803004));
#30575=CARTESIAN_POINT('Ctrl Pts',(38.5686705053066,37.5054420745486,4.60300157067779));
#30576=CARTESIAN_POINT('Ctrl Pts',(39.0583762730659,33.4055624233101,4.44600144332554));
#30577=CARTESIAN_POINT('Ctrl Pts',(35.9088971036253,30.7354302420101,4.28900131597329));
#30578=CARTESIAN_POINT('Ctrl Pts',(31.9444011812337,31.8893786759165,4.13200118862103));
#30579=CARTESIAN_POINT('Ctrl Pts',(30.7198900339817,35.8326510925229,3.97500106126878));
#30580=CARTESIAN_POINT('Ctrl Pts',(33.333394554677,39.0292772869785,3.81800093391652));
#30581=CARTESIAN_POINT('Ctrl Pts',(37.4413601668615,38.6128118820951,3.66100080656427));
#30582=CARTESIAN_POINT('Ctrl Pts',(39.3601346962212,34.9567034046157,3.50400067921202));
#30583=CARTESIAN_POINT('Ctrl Pts',(37.3691346138881,31.3394193959702,3.34700055185976));
#30584=CARTESIAN_POINT('Ctrl Pts',(33.2537087955707,31.0046131402298,3.19000042450751));
#30585=CARTESIAN_POINT('Ctrl Pts',(30.7041990519258,34.2525085970623,3.03300029715526));
#30586=CARTESIAN_POINT('Ctrl Pts',(32.0067752334918,38.1706867953913,2.876000169803));
#30587=CARTESIAN_POINT('Ctrl Pts',(35.9934047727891,39.2456796669448,2.71900004245075));
#30588=CARTESIAN_POINT('Ctrl Pts',(39.0892387343089,36.5135309690814,2.5619999150985));
#30589=CARTESIAN_POINT('Ctrl Pts',(38.5182130676685,32.4241842911394,2.40499978774624));
#30590=CARTESIAN_POINT('Ctrl Pts',(34.7923720408392,30.6445967538374,2.24799966039399));
#30591=CARTESIAN_POINT('Ctrl Pts',(31.25271289659,32.770540117956,2.09099953304174));
#30592=CARTESIAN_POINT('Ctrl Pts',(31.0732822498009,36.8956635069179,1.93399940568948));
#30593=CARTESIAN_POINT('Ctrl Pts',(34.4149766740365,39.3209232953247,1.77699927833723));
#30594=CARTESIAN_POINT('Ctrl Pts',(38.2812679464245,37.8715776624759,1.61999915098497));
#30595=CARTESIAN_POINT('Ctrl Pts',(39.2052131221224,33.8472447782685,1.46299902363272));
#30596=CARTESIAN_POINT('Ctrl Pts',(36.3583066714682,30.8566308100772,1.30599889628047));
#30597=CARTESIAN_POINT('Ctrl Pts',(32.2933869044973,31.5813507933988,1.14899876892822));
#30598=CARTESIAN_POINT('Ctrl Pts',(30.6555265460323,35.3717371281319,0.991998641575962));
#30599=CARTESIAN_POINT('Ctrl Pts',(32.9133700647812,38.8285197605545,0.834998514223708));
#30600=CARTESIAN_POINT('Ctrl Pts',(37.0423693385366,38.8527625945324,0.677998386871455));
#30601=CARTESIAN_POINT('Ctrl Pts',(39.3398463499068,35.4211275417905,0.520998259519202));
#30602=CARTESIAN_POINT('Ctrl Pts',(37.7459628168843,31.6140168356026,0.363998132166948));
#30603=CARTESIAN_POINT('Ctrl Pts',(33.6893091311581,30.8387961463588,0.206998004814695));
#30604=CARTESIAN_POINT('Ctrl Pts',(30.8087946571555,33.8039253888853,0.0499978774624422));
#30605=CARTESIAN_POINT('Ctrl Pts',(31.3943716733878,36.4808402609044,-0.0546688741057282));
#30606=CARTESIAN_POINT('Ctrl Pts',(32.1856025125517,37.4062712808594,-0.107002249889813));
#30607=CARTESIAN_POINT('Ctrl Pts',(34.0915279074966,31.601840982658,8.32100674966943));
#30608=CARTESIAN_POINT('Ctrl Pts',(32.9741442474368,31.9005650466595,8.26867337388535));
#30609=CARTESIAN_POINT('Ctrl Pts',(31.0753014046052,33.6811058761259,8.16400662231717));
#30610=CARTESIAN_POINT('Ctrl Pts',(31.7348175146381,37.5523460885235,8.00700649496493));
#30611=CARTESIAN_POINT('Ctrl Pts',(35.3277244476034,39.128306553547,7.85000636761267));
#30612=CARTESIAN_POINT('Ctrl Pts',(38.6240714764623,37.0055469422116,7.69300624026043));
#30613=CARTESIAN_POINT('Ctrl Pts',(38.6720108517446,33.0828273933217,7.53600611290816));
#30614=CARTESIAN_POINT('Ctrl Pts',(35.4265616293347,30.8800323201757,7.37900598555592));
#30615=CARTESIAN_POINT('Ctrl Pts',(31.7989388139383,32.371265827745,7.22200585820365));
#30616=CARTESIAN_POINT('Ctrl Pts',(31.0415752592096,36.2199021239313,7.06500573085141));
#30617=CARTESIAN_POINT('Ctrl Pts',(33.8338500856003,38.9745453298735,6.90800560349915));
#30618=CARTESIAN_POINT('Ctrl Pts',(37.6717825387507,38.1652228540024,6.75100547614691));
#30619=CARTESIAN_POINT('Ctrl Pts',(39.1139219123182,34.5175912205995,6.59400534879464));
#30620=CARTESIAN_POINT('Ctrl Pts',(36.8670581318634,31.3025518154648,6.4370052214424));
#30621=CARTESIAN_POINT('Ctrl Pts',(32.9459903324209,31.4030438857154,6.28000509409014));
#30622=CARTESIAN_POINT('Ctrl Pts',(30.8667702644712,34.7289638828794,6.12300496673789));
#30623=CARTESIAN_POINT('Ctrl Pts',(32.4938581656424,38.2979231406482,5.96600483938563));
#30624=CARTESIAN_POINT('Ctrl Pts',(36.3682268903025,38.9096037873106,5.80900471203337));
#30625=CARTESIAN_POINT('Ctrl Pts',(39.0156937352688,36.0155048593341,5.65200458468113));
#30626=CARTESIAN_POINT('Ctrl Pts',(38.0622493345301,32.2107931562174,5.49500445732887));
#30627=CARTESIAN_POINT('Ctrl Pts',(34.3628566513464,30.9071899016968,5.33800432997662));
#30628=CARTESIAN_POINT('Ctrl Pts',(31.2347964847743,33.2736487699982,5.18100420262436));
#30629=CARTESIAN_POINT('Ctrl Pts',(31.4830304502057,37.1881433267374,5.02400407527211));
#30630=CARTESIAN_POINT('Ctrl Pts',(34.8849647421926,39.1405087809095,4.86700394791985));
#30631=CARTESIAN_POINT('Ctrl Pts',(38.3900522579329,37.3800402837173,4.71000382056761));
#30632=CARTESIAN_POINT('Ctrl Pts',(38.855247389074,33.4853668336842,4.55300369321535));
#30633=CARTESIAN_POINT('Ctrl Pts',(35.863405201963,30.9488794732692,4.3960035658631));
#30634=CARTESIAN_POINT('Ctrl Pts',(32.0973392865795,32.0450707546122,4.23900343851084));
#30635=CARTESIAN_POINT('Ctrl Pts',(30.9341170800371,35.7909754380742,4.08200331115859));
#30636=CARTESIAN_POINT('Ctrl Pts',(33.4168110940477,38.8276048585174,3.92500318380633));
#30637=CARTESIAN_POINT('Ctrl Pts',(37.3191657884328,38.4319842810288,3.76800305645409));
#30638=CARTESIAN_POINT('Ctrl Pts',(39.1419022714024,34.9588704755104,3.61100292910183));
#30639=CARTESIAN_POINT('Ctrl Pts',(37.250555251659,31.5226379057457,3.45400280174958));
#30640=CARTESIAN_POINT('Ctrl Pts',(33.3411137476041,31.2045892930886,3.29700267439732));
#30641=CARTESIAN_POINT('Ctrl Pts',(30.9192114592832,34.2899218589819,3.14000254704507));
#30642=CARTESIAN_POINT('Ctrl Pts',(32.1565914076088,38.0119883340115,2.98300241969281));
#30643=CARTESIAN_POINT('Ctrl Pts',(35.9436831133688,39.0331759180299,2.82600229234056));
#30644=CARTESIAN_POINT('Ctrl Pts',(38.884565129747,36.4377760769889,2.66900216498831));
#30645=CARTESIAN_POINT('Ctrl Pts',(38.3421203039629,32.5531084063779,2.51200203763606));
#30646=CARTESIAN_POINT('Ctrl Pts',(34.8027641860698,30.8625923612432,2.3550019102838));
#30647=CARTESIAN_POINT('Ctrl Pts',(31.4402712194505,32.8821285137264,2.19800178293155));
#30648=CARTESIAN_POINT('Ctrl Pts',(31.2698213927195,36.8007822079265,2.04100165557929));
#30649=CARTESIAN_POINT('Ctrl Pts',(34.4442581224081,39.1046534702177,1.88400152822704));
#30650=CARTESIAN_POINT('Ctrl Pts',(38.1170347035733,37.7278501402779,1.72700140087479));
#30651=CARTESIAN_POINT('Ctrl Pts',(38.9947347950846,33.90494220846,1.57000127352253));
#30652=CARTESIAN_POINT('Ctrl Pts',(36.290321029002,31.0640137393293,1.41300114617028));
#30653=CARTESIAN_POINT('Ctrl Pts',(32.4288576594237,31.7524602104101,1.25600101881803));
#30654=CARTESIAN_POINT('Ctrl Pts',(30.8729750980786,35.353131029807,1.09900089146577));
#30655=CARTESIAN_POINT('Ctrl Pts',(33.0178095700233,38.6368956000587,0.94200076411352));
#30656=CARTESIAN_POINT('Ctrl Pts',(36.9401451541529,38.6599250374761,0.785000636761265));
#30657=CARTESIAN_POINT('Ctrl Pts',(39.1226293925725,35.400049366228,0.628000509409013));
#30658=CARTESIAN_POINT('Ctrl Pts',(37.6085225390622,31.7834912596387,0.471000382056759));
#30659=CARTESIAN_POINT('Ctrl Pts',(33.754911518796,31.0470717319576,0.314000254704506));
#30660=CARTESIAN_POINT('Ctrl Pts',(31.0185718701565,33.8637910308514,0.157000127352253));
#30661=CARTESIAN_POINT('Ctrl Pts',(31.5748397248436,36.4067215963626,0.0523333757840826));
#30662=CARTESIAN_POINT('Ctrl Pts',(32.3264680662287,37.2858331630075,-2.22044604925031E-15));
#30663=CARTESIAN_POINT('Ctrl Pts',(32.3264680662287,37.2858331630075,-2.16493489801906E-15));
#30664=CARTESIAN_POINT('Ctrl Pts',(32.2493253814486,37.208720274039,-2.02930540817935E-15));
#30665=CARTESIAN_POINT('Ctrl Pts',(32.1762950504991,37.1279852253981,-2.22088175559797E-15));
#30666=CARTESIAN_POINT('Ctrl Pts',(32.1073693836416,37.0440465177293,-2.44249065417534E-15));
#30667=CARTESIAN_POINT('Ctrl Pts',(32.0366838276613,36.957964590773,-2.66975792514024E-15));
#30668=CARTESIAN_POINT('Ctrl Pts',(31.9703148460741,36.8685128644539,-1.62037951577862E-15));
#30669=CARTESIAN_POINT('Ctrl Pts',(31.9082840182324,36.7760965840633,-1.60982338570648E-15));
#30670=CARTESIAN_POINT('Ctrl Pts',(31.8449621738338,36.681756889908,-1.59904755618531E-15));
#30671=CARTESIAN_POINT('Ctrl Pts',(31.7861605220008,36.5843273727301,-2.0500807145436E-15));
#30672=CARTESIAN_POINT('Ctrl Pts',(31.7319388093681,36.4841996609406,-1.27675647831893E-15));
#30673=CARTESIAN_POINT('Ctrl Pts',(31.6801495481474,36.3885637990409,-5.38124499843711E-16));
#30674=CARTESIAN_POINT('Ctrl Pts',(31.6325385292086,36.2904655679991,-4.81778164441647E-15));
#30675=CARTESIAN_POINT('Ctrl Pts',(31.5891933275412,36.1902216120283,-5.77315972805081E-15));
#30676=CARTESIAN_POINT('Ctrl Pts',(31.5821551531175,36.1739445059149,-5.92828918493564E-15));
#30677=CARTESIAN_POINT('Ctrl Pts',(31.5752295287451,36.1576107865788,-2.14687895786075E-15));
#30678=CARTESIAN_POINT('Ctrl Pts',(31.5684169229622,36.1412217669136,-2.1094237467878E-15));
#30679=CARTESIAN_POINT('Ctrl Pts',(31.5619076362096,36.1255624388982,-2.07363616168158E-15));
#30680=CARTESIAN_POINT('Ctrl Pts',(31.5555045468442,36.1098598194457,-5.01667023260332E-15));
#30681=CARTESIAN_POINT('Ctrl Pts',(31.5492098653947,36.0941205526839,-4.94049245958195E-15));
#30682=CARTESIAN_POINT('Ctrl Pts',(31.5058243818098,35.9856391775398,-4.41544452070402E-15));
#30683=CARTESIAN_POINT('Ctrl Pts',(31.4675527596774,35.875340817696,2.70422581427715E-15));
#30684=CARTESIAN_POINT('Ctrl Pts',(31.4344236193294,35.7636572747171,2.16493489801906E-15));
#30685=CARTESIAN_POINT('Ctrl Pts',(31.4008599589415,35.6505088963383,1.61857067083336E-15));
#30686=CARTESIAN_POINT('Ctrl Pts',(31.3725741668882,35.5359380090966,1.5704555898309E-16));
#30687=CARTESIAN_POINT('Ctrl Pts',(31.3496386440377,35.4203611044154,3.88578058618805E-16));
#30688=CARTESIAN_POINT('Ctrl Pts',(31.3256636190246,35.2995459305591,6.30604259909078E-16));
#30689=CARTESIAN_POINT('Ctrl Pts',(31.3075340503036,35.1776306642325,-4.77206768499493E-16));
#30690=CARTESIAN_POINT('Ctrl Pts',(31.2953883637021,35.0550676565495,-7.49400541621981E-16));
#30691=CARTESIAN_POINT('Ctrl Pts',(31.2862790987509,34.9631454007872,-9.53545871463847E-16));
#30692=CARTESIAN_POINT('Ctrl Pts',(31.2805368906832,34.8708581938176,-1.66063273915206E-15));
#30693=CARTESIAN_POINT('Ctrl Pts',(31.2782432669551,34.7783934177904,-1.83186799063151E-15));
#30694=CARTESIAN_POINT('Ctrl Pts',(31.2776956893352,34.7563184621811,-1.87274853712248E-15));
#30695=CARTESIAN_POINT('Ctrl Pts',(31.2773448230031,34.7342288592592,-1.15850189636716E-15));
#30696=CARTESIAN_POINT('Ctrl Pts',(31.2771918797387,34.7121562214804,-1.19348975147204E-15));
#30697=CARTESIAN_POINT('Ctrl Pts',(31.2763569642807,34.5916619548496,-1.38448803559665E-15));
#30698=CARTESIAN_POINT('Ctrl Pts',(31.2814102215213,34.471522491006,-2.99090776565717E-15));
#30699=CARTESIAN_POINT('Ctrl Pts',(31.2924206159431,34.3521638613563,-2.66453525910038E-15));
#30700=CARTESIAN_POINT('Ctrl Pts',(31.3033603504718,34.2335712231593,-2.34025726846702E-15));
#30701=CARTESIAN_POINT('Ctrl Pts',(31.3201807588279,34.1157485527733,3.70943136885229E-16));
#30702=CARTESIAN_POINT('Ctrl Pts',(31.342998921253,33.9991008864625,6.93889390390723E-16));
#30703=CARTESIAN_POINT('Ctrl Pts',(31.3458725738232,33.9844106208813,7.34560296054722E-16));
#30704=CARTESIAN_POINT('Ctrl Pts',(31.348841419242,33.9697389843081,-2.36384243829245E-16));
#30705=CARTESIAN_POINT('Ctrl Pts',(31.3519057505532,33.9550867820407,-2.22044604925031E-16));
#30706=CARTESIAN_POINT('Ctrl Pts',(31.3758162053254,33.8407581458576,-1.09500521307372E-16));
#30707=CARTESIAN_POINT('Ctrl Pts',(31.405535880703,33.7276122083523,-1.31284998081472E-15));
#30708=CARTESIAN_POINT('Ctrl Pts',(31.4407586285186,33.6159154648327,-2.41473507855972E-15));
#30709=CARTESIAN_POINT('Ctrl Pts',(31.4627238926124,33.5462602385377,-3.10188184234126E-15));
#30710=CARTESIAN_POINT('Ctrl Pts',(31.4868303230444,33.4771686776378,-2.63257088976062E-16));
#30711=CARTESIAN_POINT('Ctrl Pts',(31.5130135264214,33.4087075970126,-2.22044604925031E-16));
#30712=CARTESIAN_POINT('Ctrl Pts',(31.5219635139129,33.385306112999,-2.0795728293307E-16));
#30713=CARTESIAN_POINT('Ctrl Pts',(31.5311562173418,33.361978315516,-2.32755725796262E-15));
#30714=CARTESIAN_POINT('Ctrl Pts',(31.5405892520308,33.3387269417829,-2.58126853225349E-15));
#30715=CARTESIAN_POINT('Ctrl Pts',(31.5473379087033,33.3220922591317,-2.76278066918334E-15));
#30716=CARTESIAN_POINT('Ctrl Pts',(31.5542101234624,33.3054955734371,-8.17270399285879E-16));
#30717=CARTESIAN_POINT('Ctrl Pts',(31.5611979545174,33.288954186216,-7.7715611723761E-16));
#30718=CARTESIAN_POINT('Ctrl Pts',(31.6071192859873,33.1802505670847,-5.13540522049862E-16));
#30719=CARTESIAN_POINT('Ctrl Pts',(31.6580936513602,33.0737733268919,-1.22043518676627E-15));
#30720=CARTESIAN_POINT('Ctrl Pts',(31.713762608453,32.9697768155529,-8.60422844084496E-16));
#30721=CARTESIAN_POINT('Ctrl Pts',(31.7713468082815,32.8622023934125,-4.88024585443386E-16));
#30722=CARTESIAN_POINT('Ctrl Pts',(31.8339543542604,32.7572816421653,-1.6844387016455E-15));
#30723=CARTESIAN_POINT('Ctrl Pts',(31.9012439032021,32.6553034111749,-1.60982338570648E-15));
#30724=CARTESIAN_POINT('Ctrl Pts',(31.9691666425039,32.5523655715406,-1.53450594440749E-15));
#30725=CARTESIAN_POINT('Ctrl Pts',(32.0418603487199,32.4524251462352,-2.14412608245669E-16));
#30726=CARTESIAN_POINT('Ctrl Pts',(32.119024465224,32.3557974897081,-1.11022302462516E-16));
#30727=CARTESIAN_POINT('Ctrl Pts',(32.1734376325243,32.2876593825328,-3.81154351168831E-17));
#30728=CARTESIAN_POINT('Ctrl Pts',(32.2300747937192,32.2211689202647,2.3957932567246E-15));
#30729=CARTESIAN_POINT('Ctrl Pts',(32.2888436140898,32.1564451639975,2.85882428840978E-15));
#30730=CARTESIAN_POINT('Ctrl Pts',(32.3150756619651,32.1275550712175,3.06550279776831E-15));
#30731=CARTESIAN_POINT('Ctrl Pts',(32.3417325486905,32.0990170804093,1.33832078810492E-15));
#30732=CARTESIAN_POINT('Ctrl Pts',(32.3688066730543,32.0708423529797,1.58206781009085E-15));
#30733=CARTESIAN_POINT('Ctrl Pts',(32.3804284156068,32.0587481694606,1.68669779181855E-15));
#30734=CARTESIAN_POINT('Ctrl Pts',(32.3921256212299,32.0467224591722,5.62787663488911E-16));
#30735=CARTESIAN_POINT('Ctrl Pts',(32.4038911827787,32.0347724888588,5.27355936696949E-16));
#30736=CARTESIAN_POINT('Ctrl Pts',(32.4923334498706,31.9449440126051,2.61014017404201E-16));
#30737=CARTESIAN_POINT('Ctrl Pts',(32.584735051869,31.8592881592603,-7.81291389151021E-17));
#30738=CARTESIAN_POINT('Ctrl Pts',(32.6807672456031,31.778123082898,1.11022302462516E-16));
#30739=CARTESIAN_POINT('Ctrl Pts',(32.7628075187761,31.7087837834614,2.72614319871455E-16));
#30740=CARTESIAN_POINT('Ctrl Pts',(32.8474985084852,31.6427220447333,9.36044375735486E-16));
#30741=CARTESIAN_POINT('Ctrl Pts',(32.9346594679295,31.5801538004245,1.38777878078145E-16));
#30742=CARTESIAN_POINT('Ctrl Pts',(32.9737706916096,31.5520779208788,-2.18974819016821E-16));
#30743=CARTESIAN_POINT('Ctrl Pts',(33.0133795255453,31.5247057193814,-1.25086984652678E-15));
#30744=CARTESIAN_POINT('Ctrl Pts',(33.0534708815057,31.4980580630162,-1.7277845820729E-15));
#30745=CARTESIAN_POINT('Ctrl Pts',(33.0807055590029,31.479955898353,-2.0517601300469E-15));
#30746=CARTESIAN_POINT('Ctrl Pts',(33.1081685502538,31.462184715489,8.66601268491E-16));
#30747=CARTESIAN_POINT('Ctrl Pts',(33.1358251623594,31.4447698310871,9.5062846483529E-16));
#30748=CARTESIAN_POINT('Ctrl Pts',(33.2426295858021,31.377516955689,1.27512505265964E-15));
#30749=CARTESIAN_POINT('Ctrl Pts',(33.3523807267505,31.315530896685,3.7726686237795E-15));
#30750=CARTESIAN_POINT('Ctrl Pts',(33.4647766052556,31.2591453155976,2.97331603782425E-15));
#30751=CARTESIAN_POINT('Ctrl Pts',(33.5668702670808,31.2079280421183,2.24723218426034E-15));
#30752=CARTESIAN_POINT('Ctrl Pts',(33.6711468426795,31.1613315802118,-1.73124610826904E-15));
#30753=CARTESIAN_POINT('Ctrl Pts',(33.7774033647392,31.1196350998879,-2.12763834328555E-15));
#30754=CARTESIAN_POINT('Ctrl Pts',(33.8328339031569,31.0978834152884,-2.36077539403599E-15));
#30755=CARTESIAN_POINT('Ctrl Pts',(33.8888035920626,31.0774657030867,3.31895026664625E-16));
#30756=CARTESIAN_POINT('Ctrl Pts',(33.9452683089267,31.0583698510224,1.66533453693773E-16));
#30757=CARTESIAN_POINT('Ctrl Pts',(31.4846882532079,35.0028111988253,7.11258330249198));
#30758=CARTESIAN_POINT('Ctrl Pts',(31.4819571032991,35.3538027877235,7.09672411194513));
#30759=CARTESIAN_POINT('Ctrl Pts',(31.5304045241347,35.7040585316776,7.08086492139827));
#30760=CARTESIAN_POINT('Ctrl Pts',(31.6331816560628,36.037569942224,7.06500573085141));
#30761=CARTESIAN_POINT('Ctrl Pts',(31.9723335346732,37.138116525912,7.01267235506733));
#30762=CARTESIAN_POINT('Ctrl Pts',(32.9030918101368,38.0563309278927,6.96033897928324));
#30763=CARTESIAN_POINT('Ctrl Pts',(34.008126356727,38.3805510495713,6.90800560349915));
#30764=CARTESIAN_POINT('Ctrl Pts',(35.1131609033171,38.7047711712498,6.85567222771507));
#30765=CARTESIAN_POINT('Ctrl Pts',(36.3924717210339,38.4349970126261,6.80333885193099));
#30766=CARTESIAN_POINT('Ctrl Pts',(37.2724836921536,37.6921713277471,6.75100547614691));
#30767=CARTESIAN_POINT('Ctrl Pts',(38.1524956632732,36.9493456428681,6.69867210036282));
#30768=CARTESIAN_POINT('Ctrl Pts',(38.6332087877957,35.7334684317338,6.64633872457873));
#30769=CARTESIAN_POINT('Ctrl Pts',(38.4990880533145,34.5896899253109,6.59400534879465));
#30770=CARTESIAN_POINT('Ctrl Pts',(38.3649673188333,33.4459114188879,6.54167197301056));
#30771=CARTESIAN_POINT('Ctrl Pts',(37.6160127253483,32.3742316171763,6.48933859722648));
#30772=CARTESIAN_POINT('Ctrl Pts',(36.5880241286988,31.8551403946957,6.4370052214424));
#30773=CARTESIAN_POINT('Ctrl Pts',(35.5600355320492,31.336049172215,6.38467184565831));
#30774=CARTESIAN_POINT('Ctrl Pts',(34.2530129322351,31.3695465289652,6.33233846987422));
#30775=CARTESIAN_POINT('Ctrl Pts',(33.2529649543364,31.9406152068676,6.28000509409014));
#30776=CARTESIAN_POINT('Ctrl Pts',(32.2529169764377,32.51168388477,6.22767171830605));
#30777=CARTESIAN_POINT('Ctrl Pts',(31.5598436204544,33.6203238838247,6.17533834252197));
#30778=CARTESIAN_POINT('Ctrl Pts',(31.4844882593247,34.7694704263135,6.12300496673789));
#30779=CARTESIAN_POINT('Ctrl Pts',(31.4794861724725,34.8457507430058,6.11953107865592));
#30780=CARTESIAN_POINT('Ctrl Pts',(31.4772059369411,34.9222095437145,6.11605719057395));
#30781=CARTESIAN_POINT('Ctrl Pts',(31.4775764275568,34.998690818207,6.11258330249198));
#30782=CARTESIAN_POINT('Ctrl Pts',(33.9479286229388,31.0647048309474,8.));
#30783=CARTESIAN_POINT('Ctrl Pts',(33.8318204903556,31.1043195030892,8.));
#30784=CARTESIAN_POINT('Ctrl Pts',(33.7179774196666,31.1494845762766,8.));
#30785=CARTESIAN_POINT('Ctrl Pts',(33.6066253055996,31.1998424449166,8.));
#30786=CARTESIAN_POINT('Ctrl Pts',(33.4927760432216,31.2513296236524,8.));
#30787=CARTESIAN_POINT('Ctrl Pts',(33.3815300897553,31.3082456117247,8.));
#30788=CARTESIAN_POINT('Ctrl Pts',(33.2731531534421,31.3702567766217,8.));
#30789=CARTESIAN_POINT('Ctrl Pts',(33.1592147882362,31.4354500824416,8.));
#30790=CARTESIAN_POINT('Ctrl Pts',(33.0484464742462,31.5062753311388,8.));
#30791=CARTESIAN_POINT('Ctrl Pts',(32.9411961197039,31.5823910435948,8.));
#30792=CARTESIAN_POINT('Ctrl Pts',(32.8473520594793,31.6489922919938,8.));
#30793=CARTESIAN_POINT('Ctrl Pts',(32.7562017414451,31.719645109407,8.));
#30794=CARTESIAN_POINT('Ctrl Pts',(32.6680097346461,31.7941428733673,8.));
#30795=CARTESIAN_POINT('Ctrl Pts',(32.6506331562116,31.8088212584686,8.));
#30796=CARTESIAN_POINT('Ctrl Pts',(32.6333715252365,31.8236489611523,8.));
#30797=CARTESIAN_POINT('Ctrl Pts',(32.6162270200198,31.8386244719266,8.));
#30798=CARTESIAN_POINT('Ctrl Pts',(32.6036927426372,31.8495730063766,8.));
#30799=CARTESIAN_POINT('Ctrl Pts',(32.5912222824502,31.8605995500244,8.));
#30800=CARTESIAN_POINT('Ctrl Pts',(32.5788252877513,31.8716953917,8.));
#30801=CARTESIAN_POINT('Ctrl Pts',(32.4862461171128,31.9545577179984,8.));
#30802=CARTESIAN_POINT('Ctrl Pts',(32.397622799937,32.0414017436923,8.));
#30803=CARTESIAN_POINT('Ctrl Pts',(32.3132167630922,32.1319065542212,8.));
#30804=CARTESIAN_POINT('Ctrl Pts',(32.2290025191065,32.2222057138629,8.));
#30805=CARTESIAN_POINT('Ctrl Pts',(32.1489858942929,32.3161497454154,8.));
#30806=CARTESIAN_POINT('Ctrl Pts',(32.0734669664008,32.4134519537301,8.));
#30807=CARTESIAN_POINT('Ctrl Pts',(31.9989803737659,32.5094240517922,8.));
#30808=CARTESIAN_POINT('Ctrl Pts',(31.9288689532965,32.6086638275202,8.));
#30809=CARTESIAN_POINT('Ctrl Pts',(31.8634666824091,32.7109170108275,8.));
#30810=CARTESIAN_POINT('Ctrl Pts',(31.8101613092083,32.7942572989124,8.));
#30811=CARTESIAN_POINT('Ctrl Pts',(31.7599848998086,32.8795998826136,8.));
#30812=CARTESIAN_POINT('Ctrl Pts',(31.7131442187192,32.9668129344489,8.));
#30813=CARTESIAN_POINT('Ctrl Pts',(31.7012430571606,32.9889718056646,8.));
#30814=CARTESIAN_POINT('Ctrl Pts',(31.6895573606131,33.0112514414787,8.));
#30815=CARTESIAN_POINT('Ctrl Pts',(31.6780907836173,33.033649704911,8.));
#30816=CARTESIAN_POINT('Ctrl Pts',(31.6699353210994,33.0495801955843,8.));
#30817=CARTESIAN_POINT('Ctrl Pts',(31.6618944152098,33.0655635106099,8.));
#30818=CARTESIAN_POINT('Ctrl Pts',(31.6539717264445,33.0815932364824,8.));
#30819=CARTESIAN_POINT('Ctrl Pts',(31.6010109140258,33.1887471750268,8.));
#30820=CARTESIAN_POINT('Ctrl Pts',(31.5532889518817,33.2980509944504,8.));
#30821=CARTESIAN_POINT('Ctrl Pts',(31.5110846398564,33.4092420858783,8.));
#30822=CARTESIAN_POINT('Ctrl Pts',(31.469716484976,33.5182302453998,8.));
#30823=CARTESIAN_POINT('Ctrl Pts',(31.4336492415757,33.6290322689246,8.));
#30824=CARTESIAN_POINT('Ctrl Pts',(31.4031936775095,33.7414146337669,8.));
#30825=CARTESIAN_POINT('Ctrl Pts',(31.39873956261,33.7578505127609,8.));
#30826=CARTESIAN_POINT('Ctrl Pts',(31.3944055654848,33.7743202085893,8.));
#30827=CARTESIAN_POINT('Ctrl Pts',(31.3901927523269,33.7908230038594,8.));
#30828=CARTESIAN_POINT('Ctrl Pts',(31.3605242058421,33.9070431945601,8.));
#30829=CARTESIAN_POINT('Ctrl Pts',(31.3368616451868,34.0249053317963,8.));
#30830=CARTESIAN_POINT('Ctrl Pts',(31.3191142145135,34.1439735700009,8.));
#30831=CARTESIAN_POINT('Ctrl Pts',(31.3091306818643,34.210953498841,8.));
#30832=CARTESIAN_POINT('Ctrl Pts',(31.3010199124296,34.2783150418024,8.));
#30833=CARTESIAN_POINT('Ctrl Pts',(31.294772781286,34.3459791587903,8.));
#30834=CARTESIAN_POINT('Ctrl Pts',(31.2918903120279,34.3771998475526,8.));
#30835=CARTESIAN_POINT('Ctrl Pts',(31.2894046732663,34.4084849312592,8.));
#30836=CARTESIAN_POINT('Ctrl Pts',(31.2873153161224,34.4398265107474,8.));
#30837=CARTESIAN_POINT('Ctrl Pts',(31.2861142259533,34.4578435659536,8.));
#30838=CARTESIAN_POINT('Ctrl Pts',(31.2850446073883,34.4758722375043,8.));
#30839=CARTESIAN_POINT('Ctrl Pts',(31.2841063911591,34.4939026846615,8.));
#30840=CARTESIAN_POINT('Ctrl Pts',(31.2777954835053,34.6151844142158,8.));
#30841=CARTESIAN_POINT('Ctrl Pts',(31.2774171066952,34.7366634572185,8.));
#30842=CARTESIAN_POINT('Ctrl Pts',(31.2828130518753,34.8578925565699,8.));
#30843=CARTESIAN_POINT('Ctrl Pts',(31.2880970630825,34.976606868563,8.));
#30844=CARTESIAN_POINT('Ctrl Pts',(31.2989188151177,35.0950824227959,8.));
#30845=CARTESIAN_POINT('Ctrl Pts',(31.3151831142098,35.2128932340069,8.));
#30846=CARTESIAN_POINT('Ctrl Pts',(31.3312885029229,35.3295529743629,8.));
#30847=CARTESIAN_POINT('Ctrl Pts',(31.3527309554357,35.4455617346014,8.));
#30848=CARTESIAN_POINT('Ctrl Pts',(31.3794648241005,35.5604869939325,8.));
#30849=CARTESIAN_POINT('Ctrl Pts',(31.3968717446295,35.6353169738744,8.));
#30850=CARTESIAN_POINT('Ctrl Pts',(31.4165229267736,35.7096871840419,8.));
#30851=CARTESIAN_POINT('Ctrl Pts',(31.438415570696,35.7834713262069,8.));
#30852=CARTESIAN_POINT('Ctrl Pts',(31.4458039136858,35.8083720440668,8.));
#30853=CARTESIAN_POINT('Ctrl Pts',(31.4534476062533,35.833205958311,8.));
#30854=CARTESIAN_POINT('Ctrl Pts',(31.4613467284242,35.8579680375739,8.));
#30855=CARTESIAN_POINT('Ctrl Pts',(31.4664331210497,35.8739128039203,8.));
#30856=CARTESIAN_POINT('Ctrl Pts',(31.4716246314855,35.8898251737367,8.));
#30857=CARTESIAN_POINT('Ctrl Pts',(31.4769184005249,35.9056957806736,8.));
#30858=CARTESIAN_POINT('Ctrl Pts',(31.5138160950465,36.0163142837243,8.));
#30859=CARTESIAN_POINT('Ctrl Pts',(31.5557145002446,36.1250213095504,8.));
#30860=CARTESIAN_POINT('Ctrl Pts',(31.6025488222259,36.2313976553429,8.));
#30861=CARTESIAN_POINT('Ctrl Pts',(31.6406629285514,36.3179674866662,8.));
#30862=CARTESIAN_POINT('Ctrl Pts',(31.6820469422375,36.4029935647969,8.));
#30863=CARTESIAN_POINT('Ctrl Pts',(31.7266869246432,36.4862342957322,8.));
#30864=CARTESIAN_POINT('Ctrl Pts',(31.7483019214948,36.5265400494563,8.));
#30865=CARTESIAN_POINT('Ctrl Pts',(31.7706805722115,36.5664269742985,8.));
#30866=CARTESIAN_POINT('Ctrl Pts',(31.7938227675543,36.605866117211,8.));
#30867=CARTESIAN_POINT('Ctrl Pts',(31.8074092117442,36.6290202608064,8.));
#30868=CARTESIAN_POINT('Ctrl Pts',(31.8212608890592,36.6520231340321,8.));
#30869=CARTESIAN_POINT('Ctrl Pts',(31.8353637243995,36.6748463853764,8.));
#30870=CARTESIAN_POINT('Ctrl Pts',(31.8937951632988,36.7694086052589,8.));
#30871=CARTESIAN_POINT('Ctrl Pts',(31.9565778581775,36.8609656088156,8.));
#30872=CARTESIAN_POINT('Ctrl Pts',(32.0236777625255,36.9491266811452,8.));
#30873=CARTESIAN_POINT('Ctrl Pts',(32.0837085788304,37.0279998358789,8.));
#30874=CARTESIAN_POINT('Ctrl Pts',(32.1471954960693,37.1041548514456,8.));
#30875=CARTESIAN_POINT('Ctrl Pts',(32.2141376235347,37.177285414151,8.));
#30876=CARTESIAN_POINT('Ctrl Pts',(32.248992559173,37.2153624988329,8.));
#30877=CARTESIAN_POINT('Ctrl Pts',(32.2847845972398,37.2526191672925,8.));
#30878=CARTESIAN_POINT('Ctrl Pts',(32.321476328717,37.2890400220485,8.));
#30879=CARTESIAN_POINT('Origin',(0.,0.,8.));
#30880=CARTESIAN_POINT('',(-50.,50.,8.));
#30881=CARTESIAN_POINT('',(-50.,-50.,8.));
#30882=CARTESIAN_POINT('',(-50.,50.,8.));
#30883=CARTESIAN_POINT('',(50.,-50.,8.));
#30884=CARTESIAN_POINT('',(-50.,-50.,8.));
#30885=CARTESIAN_POINT('',(50.,50.,8.));
#30886=CARTESIAN_POINT('',(50.,-50.,8.));
#30887=CARTESIAN_POINT('',(50.,50.,8.));
#30888=CARTESIAN_POINT('Ctrl Pts',(37.6735319337713,-32.7141668369925,8.));
#30889=CARTESIAN_POINT('Ctrl Pts',(37.7506744257016,-32.7912795331857,8.));
#30890=CARTESIAN_POINT('Ctrl Pts',(37.8237045554225,-32.8720144016735,8.));
#30891=CARTESIAN_POINT('Ctrl Pts',(37.8926300182219,-32.9559529391151,8.));
#30892=CARTESIAN_POINT('Ctrl Pts',(37.9633153902931,-33.0420347223805,8.));
#30893=CARTESIAN_POINT('Ctrl Pts',(38.0296841818896,-33.1314863178634,8.));
#30894=CARTESIAN_POINT('Ctrl Pts',(38.0917148195566,-33.2239024768849,8.));
#30895=CARTESIAN_POINT('Ctrl Pts',(38.1550365108844,-33.3182421083212,8.));
#30896=CARTESIAN_POINT('Ctrl Pts',(38.2138380035849,-33.4156715766502,8.));
#30897=CARTESIAN_POINT('Ctrl Pts',(38.268059557232,-33.515799249106,8.));
#30898=CARTESIAN_POINT('Ctrl Pts',(38.3198487844224,-33.6114352910132,8.));
#30899=CARTESIAN_POINT('Ctrl Pts',(38.3674597504585,-33.7095337219438,8.));
#30900=CARTESIAN_POINT('Ctrl Pts',(38.410804885236,-33.8097778917925,8.));
#30901=CARTESIAN_POINT('Ctrl Pts',(38.4178421610283,-33.8260529794907,8.));
#30902=CARTESIAN_POINT('Ctrl Pts',(38.4247669147912,-33.8423846664997,8.));
#30903=CARTESIAN_POINT('Ctrl Pts',(38.4315786781863,-33.8587716403974,8.));
#30904=CARTESIAN_POINT('Ctrl Pts',(38.4380889335058,-33.8744332800934,8.));
#30905=CARTESIAN_POINT('Ctrl Pts',(38.4444929624372,-33.8901382301107,8.));
#30906=CARTESIAN_POINT('Ctrl Pts',(38.4507885504088,-33.9058798359799,8.));
#30907=CARTESIAN_POINT('Ctrl Pts',(38.4941738374283,-34.014361218793,8.));
#30908=CARTESIAN_POINT('Ctrl Pts',(38.5324452713943,-34.124659589853,8.));
#30909=CARTESIAN_POINT('Ctrl Pts',(38.5655742382515,-34.2363431431182,8.));
#30910=CARTESIAN_POINT('Ctrl Pts',(38.5991377517882,-34.3494916293961,8.));
#30911=CARTESIAN_POINT('Ctrl Pts',(38.6274234029538,-34.4640626260336,8.));
#30912=CARTESIAN_POINT('Ctrl Pts',(38.6503587972893,-34.5796396359417,8.));
#30913=CARTESIAN_POINT('Ctrl Pts',(38.6743337296149,-34.7004551296896,8.));
#30914=CARTESIAN_POINT('Ctrl Pts',(38.692463198861,-34.8223707151795,8.));
#30915=CARTESIAN_POINT('Ctrl Pts',(38.7046087858744,-34.9449340325394,8.));
#30916=CARTESIAN_POINT('Ctrl Pts',(38.7137179761345,-35.0368565205594,8.));
#30917=CARTESIAN_POINT('Ctrl Pts',(38.7194601094409,-35.1291439544571,8.));
#30918=CARTESIAN_POINT('Ctrl Pts',(38.721753661108,-35.2216089483748,8.));
#30919=CARTESIAN_POINT('Ctrl Pts',(38.7223012285573,-35.2436842395473,8.));
#30920=CARTESIAN_POINT('Ctrl Pts',(38.7226520798176,-35.2657741780712,8.));
#30921=CARTESIAN_POINT('Ctrl Pts',(38.7228050031224,-35.2878471504668,8.));
#30922=CARTESIAN_POINT('Ctrl Pts',(38.723639797835,-35.4083415425535,8.));
#30923=CARTESIAN_POINT('Ctrl Pts',(38.7185864406144,-35.528481112922,8.));
#30924=CARTESIAN_POINT('Ctrl Pts',(38.7075759731584,-35.6478398239672,8.));
#30925=CARTESIAN_POINT('Ctrl Pts',(38.6966361565965,-35.766432645673,8.));
#30926=CARTESIAN_POINT('Ctrl Pts',(38.6798156826268,-35.8842554734363,8.));
#30927=CARTESIAN_POINT('Ctrl Pts',(38.6569974768235,-36.0009032638125,8.));
#30928=CARTESIAN_POINT('Ctrl Pts',(38.6541238330716,-36.0155934720123,8.));
#30929=CARTESIAN_POINT('Ctrl Pts',(38.6511549977698,-36.0302650508608,8.));
#30930=CARTESIAN_POINT('Ctrl Pts',(38.6480906778903,-36.0449171950576,8.));
#30931=CARTESIAN_POINT('Ctrl Pts',(38.6241801879288,-36.1592459728997,8.));
#30932=CARTESIAN_POINT('Ctrl Pts',(38.5944604969197,-36.2723920187216,8.));
#30933=CARTESIAN_POINT('Ctrl Pts',(38.5592377490131,-36.3840888412668,8.));
#30934=CARTESIAN_POINT('Ctrl Pts',(38.5372725083531,-36.4537440423509,8.));
#30935=CARTESIAN_POINT('Ctrl Pts',(38.5131661119788,-36.5228355678477,8.));
#30936=CARTESIAN_POINT('Ctrl Pts',(38.4869829521143,-36.5912966040202,8.));
#30937=CARTESIAN_POINT('Ctrl Pts',(38.4780335436947,-36.614696597631,8.));
#30938=CARTESIAN_POINT('Ctrl Pts',(38.4688414510417,-36.6380229129432,8.));
#30939=CARTESIAN_POINT('Ctrl Pts',(38.4594090583389,-36.6612728133014,8.));
#30940=CARTESIAN_POINT('Ctrl Pts',(38.4526597990907,-36.677909059263,8.));
#30941=CARTESIAN_POINT('Ctrl Pts',(38.4457869585498,-36.6945073015523,8.));
#30942=CARTESIAN_POINT('Ctrl Pts',(38.4387984803451,-36.7110502346119,8.));
#30943=CARTESIAN_POINT('Ctrl Pts',(38.3928771569434,-36.8197539261443,8.));
#30944=CARTESIAN_POINT('Ctrl Pts',(38.3419028069428,-36.9262312105814,8.));
#30945=CARTESIAN_POINT('Ctrl Pts',(38.286233868877,-37.0302277419135,8.));
#30946=CARTESIAN_POINT('Ctrl Pts',(38.2286497374683,-37.1378020936858,8.));
#30947=CARTESIAN_POINT('Ctrl Pts',(38.1660422723199,-37.2427227531059,8.));
#30948=CARTESIAN_POINT('Ctrl Pts',(38.0987528117336,-37.3447008755076,8.));
#30949=CARTESIAN_POINT('Ctrl Pts',(38.0308301924039,-37.447638558876,8.));
#30950=CARTESIAN_POINT('Ctrl Pts',(37.9581366181552,-37.5475788135467,8.));
#30951=CARTESIAN_POINT('Ctrl Pts',(37.8809726402855,-37.6442062900679,8.));
#30952=CARTESIAN_POINT('Ctrl Pts',(37.8265596140724,-37.7123442160536,8.));
#30953=CARTESIAN_POINT('Ctrl Pts',(37.7699226008246,-37.7788344950898,8.));
#30954=CARTESIAN_POINT('Ctrl Pts',(37.7111539331996,-37.8435580680838,8.));
#30955=CARTESIAN_POINT('Ctrl Pts',(37.6849210722466,-37.8724490496109,8.));
#30956=CARTESIAN_POINT('Ctrl Pts',(37.6582633448569,-37.9009879055023,8.));
#30957=CARTESIAN_POINT('Ctrl Pts',(37.6311883528209,-37.9291634733987,8.));
#30958=CARTESIAN_POINT('Ctrl Pts',(37.6195660136439,-37.9412582509764,8.));
#30959=CARTESIAN_POINT('Ctrl Pts',(37.6078682053827,-37.9532845462101,8.));
#30960=CARTESIAN_POINT('Ctrl Pts',(37.5961020337617,-37.9652350938879,8.));
#30961=CARTESIAN_POINT('Ctrl Pts',(37.507659771091,-38.055063247923,8.));
#30962=CARTESIAN_POINT('Ctrl Pts',(37.415258178228,-38.1407187695167,8.));
#30963=CARTESIAN_POINT('Ctrl Pts',(37.3192259922681,-38.2218835091588,8.));
#30964=CARTESIAN_POINT('Ctrl Pts',(37.2371862486548,-38.2912220789739,8.));
#30965=CARTESIAN_POINT('Ctrl Pts',(37.152495821289,-38.3572831262055,8.));
#30966=CARTESIAN_POINT('Ctrl Pts',(37.0653354498859,-38.4198507239943,8.));
#30967=CARTESIAN_POINT('Ctrl Pts',(37.0262246732672,-38.4479261819266,8.));
#30968=CARTESIAN_POINT('Ctrl Pts',(36.9866162962358,-38.4752979774627,8.));
#30969=CARTESIAN_POINT('Ctrl Pts',(36.9465254062051,-38.5019452444609,8.));
#30970=CARTESIAN_POINT('Ctrl Pts',(36.9192921690604,-38.5200463976374,8.));
#30971=CARTESIAN_POINT('Ctrl Pts',(36.8918306415648,-38.5378166037371,8.));
#30972=CARTESIAN_POINT('Ctrl Pts',(36.8641755127457,-38.555230549143,8.));
#30973=CARTESIAN_POINT('Ctrl Pts',(36.7573712570443,-38.6224832996203,8.));
#30974=CARTESIAN_POINT('Ctrl Pts',(36.6476202687202,-38.6844692470865,8.));
#30975=CARTESIAN_POINT('Ctrl Pts',(36.5352245224892,-38.7408547353335,8.));
#30976=CARTESIAN_POINT('Ctrl Pts',(36.4331307539574,-38.7920720382892,8.));
#30977=CARTESIAN_POINT('Ctrl Pts',(36.3288540451722,-38.8386685245707,8.));
#30978=CARTESIAN_POINT('Ctrl Pts',(36.2225973607791,-38.8803650263204,8.));
#30979=CARTESIAN_POINT('Ctrl Pts',(36.1671668634624,-38.9021166727374,8.));
#30980=CARTESIAN_POINT('Ctrl Pts',(36.1111972101676,-38.9225343520043,8.));
#30981=CARTESIAN_POINT('Ctrl Pts',(36.054732523776,-38.9416301760088,8.));
#30982=CARTESIAN_POINT('Ctrl Pts',(33.9479286229388,-38.9352951690526,8.));
#30983=CARTESIAN_POINT('Ctrl Pts',(33.8318204065611,-38.8956804683211,8.));
#30984=CARTESIAN_POINT('Ctrl Pts',(33.7179772526967,-38.8505153756638,8.));
#30985=CARTESIAN_POINT('Ctrl Pts',(33.6066250571068,-38.8001574942087,8.));
#30986=CARTESIAN_POINT('Ctrl Pts',(33.4927757454994,-38.7486703178014,8.));
#30987=CARTESIAN_POINT('Ctrl Pts',(33.3815297429693,-38.6917543422691,8.));
#30988=CARTESIAN_POINT('Ctrl Pts',(33.2731527586738,-38.6297431972011,8.));
#30989=CARTESIAN_POINT('Ctrl Pts',(33.1592144063828,-38.5645499484809,8.));
#30990=CARTESIAN_POINT('Ctrl Pts',(33.0484461029789,-38.4937247712042,8.));
#30991=CARTESIAN_POINT('Ctrl Pts',(32.9411957572322,-38.4176091405434,8.));
#30992=CARTESIAN_POINT('Ctrl Pts',(32.8473517047039,-38.3510079637152,8.));
#30993=CARTESIAN_POINT('Ctrl Pts',(32.7562013929947,-38.2803552258207,8.));
#30994=CARTESIAN_POINT('Ctrl Pts',(32.668009391503,-38.2058575466902,8.));
#30995=CARTESIAN_POINT('Ctrl Pts',(32.6506323829748,-38.1911788141103,8.));
#30996=CARTESIAN_POINT('Ctrl Pts',(32.6333703275703,-38.1763507567444,8.));
#30997=CARTESIAN_POINT('Ctrl Pts',(32.6162254037543,-38.1613748841763,8.));
#30998=CARTESIAN_POINT('Ctrl Pts',(32.603691142847,-38.1504263669302,8.));
#30999=CARTESIAN_POINT('Ctrl Pts',(32.5912206997708,-38.139399841404,8.));
#31000=CARTESIAN_POINT('Ctrl Pts',(32.5788237219142,-38.1283040179759,8.));
#31001=CARTESIAN_POINT('Ctrl Pts',(32.4862445714949,-38.0454417334689,8.));
#31002=CARTESIAN_POINT('Ctrl Pts',(32.3976212761744,-37.9585977539474,8.));
#31003=CARTESIAN_POINT('Ctrl Pts',(32.3132152636303,-37.8680929905958,8.));
#31004=CARTESIAN_POINT('Ctrl Pts',(32.2290010683149,-37.7777939042141,8.));
#31005=CARTESIAN_POINT('Ctrl Pts',(32.1489844921721,-37.6838499490402,8.));
#31006=CARTESIAN_POINT('Ctrl Pts',(32.0734656135458,-37.5865478166696,8.));
#31007=CARTESIAN_POINT('Ctrl Pts',(31.9989790801238,-37.4905758071975,8.));
#31008=CARTESIAN_POINT('Ctrl Pts',(31.9288677181994,-37.3913361205739,8.));
#31009=CARTESIAN_POINT('Ctrl Pts',(31.8634655056288,-37.2890830233624,8.));
#31010=CARTESIAN_POINT('Ctrl Pts',(31.8101602412414,-37.2057429012617,8.));
#31011=CARTESIAN_POINT('Ctrl Pts',(31.7599839333137,-37.1204004861509,8.));
#31012=CARTESIAN_POINT('Ctrl Pts',(31.7131433458597,-37.0331876031136,8.));
#31013=CARTESIAN_POINT('Ctrl Pts',(31.7012416847729,-37.011027800414,8.));
#31014=CARTESIAN_POINT('Ctrl Pts',(31.6895555071392,-36.9887472225083,8.));
#31015=CARTESIAN_POINT('Ctrl Pts',(31.6780884679743,-36.9663480066189,8.));
#31016=CARTESIAN_POINT('Ctrl Pts',(31.6699335871488,-36.9504186168665,8.));
#31017=CARTESIAN_POINT('Ctrl Pts',(31.6618932487394,-36.9344364128785,8.));
#31018=CARTESIAN_POINT('Ctrl Pts',(31.6539711105215,-36.918407803011,8.));
#31019=CARTESIAN_POINT('Ctrl Pts',(31.6010103294039,-36.8112539418358,8.));
#31020=CARTESIAN_POINT('Ctrl Pts',(31.553288398372,-36.7019501913722,8.));
#31021=CARTESIAN_POINT('Ctrl Pts',(31.5110841176717,-36.5907591572156,8.));
#31022=CARTESIAN_POINT('Ctrl Pts',(31.4697159940302,-36.4817710552385,8.));
#31023=CARTESIAN_POINT('Ctrl Pts',(31.433648781936,-36.3709690780795,8.));
#31024=CARTESIAN_POINT('Ctrl Pts',(31.4031932495943,-36.2585867452464,8.));
#31025=CARTESIAN_POINT('Ctrl Pts',(31.3987391935523,-36.2421510709998,8.));
#31026=CARTESIAN_POINT('Ctrl Pts',(31.3944052523692,-36.2256815804349,8.));
#31027=CARTESIAN_POINT('Ctrl Pts',(31.3901924922002,-36.2091789909079,8.));
#31028=CARTESIAN_POINT('Ctrl Pts',(31.3605239499998,-36.0929588041061,8.));
#31029=CARTESIAN_POINT('Ctrl Pts',(31.3368613966103,-35.9750966537399,8.));
#31030=CARTESIAN_POINT('Ctrl Pts',(31.319113975657,-35.8560283881328,8.));
#31031=CARTESIAN_POINT('Ctrl Pts',(31.3091304483948,-35.7890484433355,8.));
#31032=CARTESIAN_POINT('Ctrl Pts',(31.3010196851544,-35.7216868798927,8.));
#31033=CARTESIAN_POINT('Ctrl Pts',(31.2947725609189,-35.6540227383851,8.));
#31034=CARTESIAN_POINT('Ctrl Pts',(31.2918900964785,-35.6228020559662,8.));
#31035=CARTESIAN_POINT('Ctrl Pts',(31.2894044622378,-35.591516977816,8.));
#31036=CARTESIAN_POINT('Ctrl Pts',(31.2873151093096,-35.5601754031315,8.));
#31037=CARTESIAN_POINT('Ctrl Pts',(31.2861140199798,-35.542158326923,8.));
#31038=CARTESIAN_POINT('Ctrl Pts',(31.2850444024964,-35.5241296340464,8.));
#31039=CARTESIAN_POINT('Ctrl Pts',(31.2841061875917,-35.5060991653233,8.));
#31040=CARTESIAN_POINT('Ctrl Pts',(31.2777952935748,-35.3848173815625,8.));
#31041=CARTESIAN_POINT('Ctrl Pts',(31.2774169324427,-35.2633382728991,8.));
#31042=CARTESIAN_POINT('Ctrl Pts',(31.2828128947659,-35.142109099441,8.));
#31043=CARTESIAN_POINT('Ctrl Pts',(31.2880969228261,-35.0233947134034,8.));
#31044=CARTESIAN_POINT('Ctrl Pts',(31.2989186932579,-34.9049190770275,8.));
#31045=CARTESIAN_POINT('Ctrl Pts',(31.3151830117592,-34.7871081783408,8.));
#31046=CARTESIAN_POINT('Ctrl Pts',(31.3312884180702,-34.67044836311,8.));
#31047=CARTESIAN_POINT('Ctrl Pts',(31.3527308881008,-34.5544395226326,8.));
#31048=CARTESIAN_POINT('Ctrl Pts',(31.3794647737014,-34.4395141802506,8.));
#31049=CARTESIAN_POINT('Ctrl Pts',(31.396871707047,-34.3646841385402,8.));
#31050=CARTESIAN_POINT('Ctrl Pts',(31.416522902222,-34.2903138655065,8.));
#31051=CARTESIAN_POINT('Ctrl Pts',(31.4384155592443,-34.2165296601315,8.));
#31052=CARTESIAN_POINT('Ctrl Pts',(31.4458038981696,-34.1916289495378,8.));
#31053=CARTESIAN_POINT('Ctrl Pts',(31.4534475860939,-34.1667950423673,8.));
#31054=CARTESIAN_POINT('Ctrl Pts',(31.461346703037,-34.1420329699976,8.));
#31055=CARTESIAN_POINT('Ctrl Pts',(31.46643308557,-34.1260882291753,8.));
#31056=CARTESIAN_POINT('Ctrl Pts',(31.471624585416,-34.1101758846519,8.));
#31057=CARTESIAN_POINT('Ctrl Pts',(31.476918343353,-34.0943053028287,8.));
#31058=CARTESIAN_POINT('Ctrl Pts',(31.513816049212,-33.9836867088362,8.));
#31059=CARTESIAN_POINT('Ctrl Pts',(31.5557144650388,-33.8749795921173,8.));
#31060=CARTESIAN_POINT('Ctrl Pts',(31.6025487964097,-33.7686031580514,8.));
#31061=CARTESIAN_POINT('Ctrl Pts',(31.6406629208299,-33.6820332311479,8.));
#31062=CARTESIAN_POINT('Ctrl Pts',(31.682046953583,-33.5970070600165,8.));
#31063=CARTESIAN_POINT('Ctrl Pts',(31.7266869557237,-33.5137662402706,8.));
#31064=CARTESIAN_POINT('Ctrl Pts',(31.7483019580961,-33.4734604510681,8.));
#31065=CARTESIAN_POINT('Ctrl Pts',(31.7706806142055,-33.4335734915742,8.));
#31066=CARTESIAN_POINT('Ctrl Pts',(31.7938228147784,-33.3941343150086,8.));
#31067=CARTESIAN_POINT('Ctrl Pts',(31.8074092885987,-33.3709801063925,8.));
#31068=CARTESIAN_POINT('Ctrl Pts',(31.8212609965416,-33.347977169053,8.));
#31069=CARTESIAN_POINT('Ctrl Pts',(31.8353638634359,-33.3251538546887,8.));
#31070=CARTESIAN_POINT('Ctrl Pts',(31.8937952976074,-33.2305915929272,8.));
#31071=CARTESIAN_POINT('Ctrl Pts',(31.9565779834776,-33.1390345522359,8.));
#31072=CARTESIAN_POINT('Ctrl Pts',(32.0236778740976,-33.0508734495428,8.));
#31073=CARTESIAN_POINT('Ctrl Pts',(32.0837087245751,-32.972000206609,8.));
#31074=CARTESIAN_POINT('Ctrl Pts',(32.1471956775548,-32.8958451124639,8.));
#31075=CARTESIAN_POINT('Ctrl Pts',(32.2141378419758,-32.8227144830143,8.));
#31076=CARTESIAN_POINT('Ctrl Pts',(32.2489927811285,-32.7846373807617,8.));
#31077=CARTESIAN_POINT('Ctrl Pts',(32.2847848221939,-32.7473806972021,8.));
#31078=CARTESIAN_POINT('Ctrl Pts',(32.3214765561793,-32.7109598296518,8.));
#31079=CARTESIAN_POINT('Ctrl Pts',(-32.3264680662287,-32.7141668369925,
8.));
#31080=CARTESIAN_POINT('Ctrl Pts',(-32.2493255072635,-32.7912796001948,
8.));
#31081=CARTESIAN_POINT('Ctrl Pts',(-32.1762953075955,-32.8720145313034,
8.));
#31082=CARTESIAN_POINT('Ctrl Pts',(-32.1073697738656,-32.9559531279149,
8.));
#31083=CARTESIAN_POINT('Ctrl Pts',(-32.0366843378685,-33.0420349611253,
8.));
#31084=CARTESIAN_POINT('Ctrl Pts',(-31.9703154802321,-33.1314866020839,
8.));
#31085=CARTESIAN_POINT('Ctrl Pts',(-31.9082847764611,-33.2239028032894,
8.));
#31086=CARTESIAN_POINT('Ctrl Pts',(-31.8449630319238,-33.3182424565268,
8.));
#31087=CARTESIAN_POINT('Ctrl Pts',(-31.786161483907,-33.415671941835,8.));
#31088=CARTESIAN_POINT('Ctrl Pts',(-31.7319398749946,-33.5157996279616,
8.));
#31089=CARTESIAN_POINT('Ctrl Pts',(-31.6801506359753,-33.6114356072929,
8.));
#31090=CARTESIAN_POINT('Ctrl Pts',(-31.6325396515499,-33.709533968736,8.));
#31091=CARTESIAN_POINT('Ctrl Pts',(-31.5891944935205,-33.8097780642334,
8.));
#31092=CARTESIAN_POINT('Ctrl Pts',(-31.582156905406,-33.8260538534356,8.));
#31093=CARTESIAN_POINT('Ctrl Pts',(-31.5752318490596,-33.8423862467834,
8.));
#31094=CARTESIAN_POINT('Ctrl Pts',(-31.568419792889,-33.8587739316911,8.));
#31095=CARTESIAN_POINT('Ctrl Pts',(-31.5619098742369,-33.8744347678579,
8.));
#31096=CARTESIAN_POINT('Ctrl Pts',(-31.5555061718916,-33.8901389077819,
8.));
#31097=CARTESIAN_POINT('Ctrl Pts',(-31.5492108990198,-33.9058797005882,
8.));
#31098=CARTESIAN_POINT('Ctrl Pts',(-31.5058255436634,-34.0143610807278,
8.));
#31099=CARTESIAN_POINT('Ctrl Pts',(-31.4675540442795,-34.1246594478804,
8.));
#31100=CARTESIAN_POINT('Ctrl Pts',(-31.434425017105,-34.2363429975606,8.));
#31101=CARTESIAN_POINT('Ctrl Pts',(-31.4008614525105,-34.3494914463237,
8.));
#31102=CARTESIAN_POINT('Ctrl Pts',(-31.3725757523594,-34.4640624049253,
8.));
#31103=CARTESIAN_POINT('Ctrl Pts',(-31.3496403133382,-34.5796393782454,
8.));
#31104=CARTESIAN_POINT('Ctrl Pts',(-31.3256653487767,-34.7004547608028,
8.));
#31105=CARTESIAN_POINT('Ctrl Pts',(-31.307535844936,-34.8223702353544,8.));
#31106=CARTESIAN_POINT('Ctrl Pts',(-31.2953902232888,-34.9449334450722,
8.));
#31107=CARTESIAN_POINT('Ctrl Pts',(-31.2862810070535,-35.0368558523606,
8.));
#31108=CARTESIAN_POINT('Ctrl Pts',(-31.2805388477475,-35.1291432073786,
8.));
#31109=CARTESIAN_POINT('Ctrl Pts',(-31.2782452710195,-35.2216081255571,
8.));
#31110=CARTESIAN_POINT('Ctrl Pts',(-31.2776977000309,-35.243683300125,8.));
#31111=CARTESIAN_POINT('Ctrl Pts',(-31.2773468435284,-35.2657731220308,
8.));
#31112=CARTESIAN_POINT('Ctrl Pts',(-31.277193913283,-35.2878459781507,8.));
#31113=CARTESIAN_POINT('Ctrl Pts',(-31.2763590765867,-35.4083403266138,
8.));
#31114=CARTESIAN_POINT('Ctrl Pts',(-31.2814123990406,-35.5284798599375,
8.));
#31115=CARTESIAN_POINT('Ctrl Pts',(-31.2924228410947,-35.6478385426709,
8.));
#31116=CARTESIAN_POINT('Ctrl Pts',(-31.303362629127,-35.7664313005734,8.));
#31117=CARTESIAN_POINT('Ctrl Pts',(-31.3201830802735,-35.8842540736147,
8.));
#31118=CARTESIAN_POINT('Ctrl Pts',(-31.3430012709811,-36.000901820846,8.));
#31119=CARTESIAN_POINT('Ctrl Pts',(-31.3458749177941,-36.0155920489787,
8.));
#31120=CARTESIAN_POINT('Ctrl Pts',(-31.3488437566082,-36.0302636478795,
8.));
#31121=CARTESIAN_POINT('Ctrl Pts',(-31.3519080804568,-36.0449158122488,
8.));
#31122=CARTESIAN_POINT('Ctrl Pts',(-31.3758185581684,-36.1592445408324,
8.));
#31123=CARTESIAN_POINT('Ctrl Pts',(-31.4055382437248,-36.2723905489836,
8.));
#31124=CARTESIAN_POINT('Ctrl Pts',(-31.4407609915798,-36.3840873440382,
8.));
#31125=CARTESIAN_POINT('Ctrl Pts',(-31.4627262403709,-36.4537425538657,
8.));
#31126=CARTESIAN_POINT('Ctrl Pts',(-31.4868326485685,-36.5228340916482,
8.));
#31127=CARTESIAN_POINT('Ctrl Pts',(-31.5130158235422,-36.5912951432516,
8.));
#31128=CARTESIAN_POINT('Ctrl Pts',(-31.5219654331702,-36.6146956547323,
8.));
#31129=CARTESIAN_POINT('Ctrl Pts',(-31.5311577380477,-36.638022485054,8.));
#31130=CARTESIAN_POINT('Ctrl Pts',(-31.5405903538195,-36.6612728973655,
8.));
#31131=CARTESIAN_POINT('Ctrl Pts',(-31.5473394036631,-36.677908600056,8.));
#31132=CARTESIAN_POINT('Ctrl Pts',(-31.5542120267349,-36.6945063014083,
8.));
#31133=CARTESIAN_POINT('Ctrl Pts',(-31.5612002800447,-36.7110486972688,
8.));
#31134=CARTESIAN_POINT('Ctrl Pts',(-31.6071216062265,-36.8197523636167,
8.));
#31135=CARTESIAN_POINT('Ctrl Pts',(-31.6580959615467,-36.9262296326556,
8.));
#31136=CARTESIAN_POINT('Ctrl Pts',(-31.7137649062032,-37.0302261570189,
8.));
#31137=CARTESIAN_POINT('Ctrl Pts',(-31.7713490613653,-37.1378005332208,
8.));
#31138=CARTESIAN_POINT('Ctrl Pts',(-31.833956554581,-37.2427212245297,8.));
#31139=CARTESIAN_POINT('Ctrl Pts',(-31.9012460458509,-37.3446993846474,
8.));
#31140=CARTESIAN_POINT('Ctrl Pts',(-31.9691687068521,-37.4476371223012,
8.));
#31141=CARTESIAN_POINT('Ctrl Pts',(-32.0418623269422,-37.547577436253,8.));
#31142=CARTESIAN_POINT('Ctrl Pts',(-32.1190263529718,-37.6442049753141,
8.));
#31143=CARTESIAN_POINT('Ctrl Pts',(-32.1734394282079,-37.7123429642625,
8.));
#31144=CARTESIAN_POINT('Ctrl Pts',(-32.230076492864,-37.7788333069719,8.));
#31145=CARTESIAN_POINT('Ctrl Pts',(-32.288845213566,-37.8435569436544,8.));
#31146=CARTESIAN_POINT('Ctrl Pts',(-32.3150777918285,-37.8724476161826,
8.));
#31147=CARTESIAN_POINT('Ctrl Pts',(-32.3417352269367,-37.9009861713024,
8.));
#31148=CARTESIAN_POINT('Ctrl Pts',(-32.3688099173017,-37.9291614469859,
8.));
#31149=CARTESIAN_POINT('Ctrl Pts',(-32.3804320487223,-37.941256017686,8.));
#31150=CARTESIAN_POINT('Ctrl Pts',(-32.3921296471323,-37.9532821092146,
8.));
#31151=CARTESIAN_POINT('Ctrl Pts',(-32.4038956063136,-37.9652324558272,
8.));
#31152=CARTESIAN_POINT('Ctrl Pts',(-32.4923378704609,-38.0550607218847,
8.));
#31153=CARTESIAN_POINT('Ctrl Pts',(-32.5847394664431,-38.1407163588179,
8.));
#31154=CARTESIAN_POINT('Ctrl Pts',(-32.6807716550536,-38.2218812155311,
8.));
#31155=CARTESIAN_POINT('Ctrl Pts',(-32.7628115828128,-38.2912200390828,
8.));
#31156=CARTESIAN_POINT('Ctrl Pts',(-32.8475022057307,-38.3572813267927,
8.));
#31157=CARTESIAN_POINT('Ctrl Pts',(-32.9346627816287,-38.4198491494197,
8.));
#31158=CARTESIAN_POINT('Ctrl Pts',(-32.9737737137373,-38.447924753989,8.));
#31159=CARTESIAN_POINT('Ctrl Pts',(-33.0133822496832,-38.4752966907185,
8.));
#31160=CARTESIAN_POINT('Ctrl Pts',(-33.0534733017689,-38.5019440931387,
8.));
#31161=CARTESIAN_POINT('Ctrl Pts',(-33.0807070399686,-38.5200455981744,
8.));
#31162=CARTESIAN_POINT('Ctrl Pts',(-33.1081690766608,-38.5378161440549,
8.));
#31163=CARTESIAN_POINT('Ctrl Pts',(-33.1358247214715,-38.5552304161034,
8.));
#31164=CARTESIAN_POINT('Ctrl Pts',(-33.2426290354803,-38.6224832099845,
8.));
#31165=CARTESIAN_POINT('Ctrl Pts',(-33.3523800768607,-38.684469196206,8.));
#31166=CARTESIAN_POINT('Ctrl Pts',(-33.4647758690787,-38.7408547167133,
8.));
#31167=CARTESIAN_POINT('Ctrl Pts',(-33.5668696003918,-38.7920720093452,
8.));
#31168=CARTESIAN_POINT('Ctrl Pts',(-33.6711462627517,-38.8386684870918,
8.));
#31169=CARTESIAN_POINT('Ctrl Pts',(-33.777402890587,-38.880364981349,8.));
#31170=CARTESIAN_POINT('Ctrl Pts',(-33.8328334021929,-38.9021166410425,
8.));
#31171=CARTESIAN_POINT('Ctrl Pts',(-33.8888030678697,-38.9225343317631,
8.));
#31172=CARTESIAN_POINT('Ctrl Pts',(-33.9452677648582,-38.941630165528,8.));
#31173=CARTESIAN_POINT('Ctrl Pts',(-36.0520713770612,-38.9352951690526,
8.));
#31174=CARTESIAN_POINT('Ctrl Pts',(-36.1681793348248,-38.8956805565571,
8.));
#31175=CARTESIAN_POINT('Ctrl Pts',(-36.2820222319885,-38.8505155239877,
8.));
#31176=CARTESIAN_POINT('Ctrl Pts',(-36.39337417598,-38.8001576820793,8.));
#31177=CARTESIAN_POINT('Ctrl Pts',(-36.507223335641,-38.7486704984873,8.));
#31178=CARTESIAN_POINT('Ctrl Pts',(-36.6184691867386,-38.6917544842536,
8.));
#31179=CARTESIAN_POINT('Ctrl Pts',(-36.726846022942,-38.6297432779853,8.));
#31180=CARTESIAN_POINT('Ctrl Pts',(-36.8407844151035,-38.5645498530274,
8.));
#31181=CARTESIAN_POINT('Ctrl Pts',(-36.9515527511922,-38.4937244553102,
8.));
#31182=CARTESIAN_POINT('Ctrl Pts',(-37.0588031240991,-38.417608572184,8.));
#31183=CARTESIAN_POINT('Ctrl Pts',(-37.1526472003926,-38.3510071744486,
8.));
#31184=CARTESIAN_POINT('Ctrl Pts',(-37.2437975316357,-38.2803541911134,
8.));
#31185=CARTESIAN_POINT('Ctrl Pts',(-37.3319895495211,-38.2058562501456,
8.));
#31186=CARTESIAN_POINT('Ctrl Pts',(-37.3493652308069,-38.1911785898568,
8.));
#31187=CARTESIAN_POINT('Ctrl Pts',(-37.3666259764485,-38.1763516270108,
8.));
#31188=CARTESIAN_POINT('Ctrl Pts',(-37.3837696084918,-38.1613768709081,
8.));
#31189=CARTESIAN_POINT('Ctrl Pts',(-37.3963039208792,-38.1504283000079,
8.));
#31190=CARTESIAN_POINT('Ctrl Pts',(-37.4087744173897,-38.1394017179875,
8.));
#31191=CARTESIAN_POINT('Ctrl Pts',(-37.421171447845,-38.1283058376695,8.));
#31192=CARTESIAN_POINT('Ctrl Pts',(-37.5137506606012,-38.0454434240953,
8.));
#31193=CARTESIAN_POINT('Ctrl Pts',(-37.6023740233075,-37.9585993019841,
8.));
#31194=CARTESIAN_POINT('Ctrl Pts',(-37.686780110783,-37.8680943929378,8.));
#31195=CARTESIAN_POINT('Ctrl Pts',(-37.7709944562299,-37.7777950803761,
8.));
#31196=CARTESIAN_POINT('Ctrl Pts',(-37.8510111825053,-37.6838508893952,
8.));
#31197=CARTESIAN_POINT('Ctrl Pts',(-37.9265302130999,-37.5865485225552,
8.));
#31198=CARTESIAN_POINT('Ctrl Pts',(-38.0010169291866,-37.4905762395914,
8.));
#31199=CARTESIAN_POINT('Ctrl Pts',(-38.0711284717142,-37.3913362778857,
8.));
#31200=CARTESIAN_POINT('Ctrl Pts',(-38.1365308641829,-37.2890829148734,
8.));
#31201=CARTESIAN_POINT('Ctrl Pts',(-38.1898364642257,-37.2057422805937,
8.));
#31202=CARTESIAN_POINT('Ctrl Pts',(-38.2400130851628,-37.1203993452656,
8.));
#31203=CARTESIAN_POINT('Ctrl Pts',(-38.2868539614533,-37.0331859413737,
8.));
#31204=CARTESIAN_POINT('Ctrl Pts',(-38.2987540819478,-37.0110290114177,
8.));
#31205=CARTESIAN_POINT('Ctrl Pts',(-38.3104387758635,-36.9887513389692,
8.));
#31206=CARTESIAN_POINT('Ctrl Pts',(-38.3219043896502,-36.9663550605045,
8.));
#31207=CARTESIAN_POINT('Ctrl Pts',(-38.3300610648434,-36.9504222746659,
8.));
#31208=CARTESIAN_POINT('Ctrl Pts',(-38.3381031537755,-36.9344366433847,
8.));
#31209=CARTESIAN_POINT('Ctrl Pts',(-38.3460269902799,-36.918404590898,8.));
#31210=CARTESIAN_POINT('Ctrl Pts',(-38.3989878678949,-36.8112504908368,
8.));
#31211=CARTESIAN_POINT('Ctrl Pts',(-38.4467098948397,-36.7019465274356,
8.));
#31212=CARTESIAN_POINT('Ctrl Pts',(-38.4889142721076,-36.5907553164102,
8.));
#31213=CARTESIAN_POINT('Ctrl Pts',(-38.5302824920512,-36.4817670367281,
8.));
#31214=CARTESIAN_POINT('Ctrl Pts',(-38.566349800654,-36.3709649163585,8.));
#31215=CARTESIAN_POINT('Ctrl Pts',(-38.5968054307926,-36.2585824846173,
8.));
#31216=CARTESIAN_POINT('Ctrl Pts',(-38.6012596681997,-36.2421461794391,
8.));
#31217=CARTESIAN_POINT('Ctrl Pts',(-38.6055937817646,-36.225676056354,8.));
#31218=CARTESIAN_POINT('Ctrl Pts',(-38.6098067052154,-36.2091728328306,
8.));
#31219=CARTESIAN_POINT('Ctrl Pts',(-38.6394752606328,-36.0929526338671,
8.));
#31220=CARTESIAN_POINT('Ctrl Pts',(-38.6631378364378,-35.9750905238851,
8.));
#31221=CARTESIAN_POINT('Ctrl Pts',(-38.6808852873793,-35.8560223427045,
8.));
#31222=CARTESIAN_POINT('Ctrl Pts',(-38.6908688312617,-35.7890424470708,
8.));
#31223=CARTESIAN_POINT('Ctrl Pts',(-38.6989796136129,-35.7216809467524,
8.));
#31224=CARTESIAN_POINT('Ctrl Pts',(-38.705226759162,-35.6540168808315,8.));
#31225=CARTESIAN_POINT('Ctrl Pts',(-38.7081092384591,-35.6227961788899,
8.));
#31226=CARTESIAN_POINT('Ctrl Pts',(-38.7105948866426,-35.5915110836458,
8.));
#31227=CARTESIAN_POINT('Ctrl Pts',(-38.7126842525742,-35.5601694941906,
8.));
#31228=CARTESIAN_POINT('Ctrl Pts',(-38.713885344499,-35.542152482698,8.));
#31229=CARTESIAN_POINT('Ctrl Pts',(-38.7149549653242,-35.5241238555354,
8.));
#31230=CARTESIAN_POINT('Ctrl Pts',(-38.7158931843189,-35.5060934532667,
8.));
#31231=CARTESIAN_POINT('Ctrl Pts',(-38.7222041204107,-35.3848118366399,
8.));
#31232=CARTESIAN_POINT('Ctrl Pts',(-38.7225825299149,-35.2633329304591,
8.));
#31233=CARTESIAN_POINT('Ctrl Pts',(-38.717186620484,-35.142103985552,8.));
#31234=CARTESIAN_POINT('Ctrl Pts',(-38.7119026444224,-35.0233898278976,
8.));
#31235=CARTESIAN_POINT('Ctrl Pts',(-38.7010809307532,-34.9049144449008,
8.));
#31236=CARTESIAN_POINT('Ctrl Pts',(-38.684816672141,-34.7871038160559,8.));
#31237=CARTESIAN_POINT('Ctrl Pts',(-38.668711320133,-34.6704442318052,8.));
#31238=CARTESIAN_POINT('Ctrl Pts',(-38.6472689041617,-34.5544356388673,
8.));
#31239=CARTESIAN_POINT('Ctrl Pts',(-38.6205350708283,-34.439510552711,8.));
#31240=CARTESIAN_POINT('Ctrl Pts',(-38.6031281770284,-34.364680701536,8.));
#31241=CARTESIAN_POINT('Ctrl Pts',(-38.5834770220596,-34.2903106224296,
8.));
#31242=CARTESIAN_POINT('Ctrl Pts',(-38.5615844054563,-34.2165266120474,
8.));
#31243=CARTESIAN_POINT('Ctrl Pts',(-38.5541960539989,-34.1916258790507,
8.));
#31244=CARTESIAN_POINT('Ctrl Pts',(-38.5465523517576,-34.1667919500715,
8.));
#31245=CARTESIAN_POINT('Ctrl Pts',(-38.5386532186941,-34.1420298564502,
8.));
#31246=CARTESIAN_POINT('Ctrl Pts',(-38.5335668050111,-34.1260850368347,
8.));
#31247=CARTESIAN_POINT('Ctrl Pts',(-38.5283752724802,-34.1101726142316,
8.));
#31248=CARTESIAN_POINT('Ctrl Pts',(-38.5230814802764,-34.094301954882,8.));
#31249=CARTESIAN_POINT('Ctrl Pts',(-38.4861838094094,-33.9836836414723,
8.));
#31250=CARTESIAN_POINT('Ctrl Pts',(-38.4442854263901,-33.8749768051962,
8.));
#31251=CARTESIAN_POINT('Ctrl Pts',(-38.3974511240065,-33.7686006435033,
8.));
#31252=CARTESIAN_POINT('Ctrl Pts',(-38.3593370554135,-33.6820310114798,
8.));
#31253=CARTESIAN_POINT('Ctrl Pts',(-38.3179530814865,-33.5970051272784,
8.));
#31254=CARTESIAN_POINT('Ctrl Pts',(-38.2733131402326,-33.5137645815446,
8.));
#31255=CARTESIAN_POINT('Ctrl Pts',(-38.2516981548861,-33.4734589017939,
8.));
#31256=CARTESIAN_POINT('Ctrl Pts',(-38.2293195154062,-33.4335720492035,
8.));
#31257=CARTESIAN_POINT('Ctrl Pts',(-38.2061773309613,-33.3941329764629,
8.));
#31258=CARTESIAN_POINT('Ctrl Pts',(-38.1925909485316,-33.3709789684133,
8.));
#31259=CARTESIAN_POINT('Ctrl Pts',(-38.1787393350554,-33.3479762288434,
8.));
#31260=CARTESIAN_POINT('Ctrl Pts',(-38.1646365654847,-33.3251531088758,
8.));
#31261=CARTESIAN_POINT('Ctrl Pts',(-38.1062051167558,-33.2305909764135,
8.));
#31262=CARTESIAN_POINT('Ctrl Pts',(-38.0434224031259,-33.139034050394,8.));
#31263=CARTESIAN_POINT('Ctrl Pts',(-37.9763224701899,-33.050873041493,8.));
#31264=CARTESIAN_POINT('Ctrl Pts',(-37.9162917251371,-32.972000070726,8.));
#31265=CARTESIAN_POINT('Ctrl Pts',(-37.8528048824192,-32.8958452190746,
8.));
#31266=CARTESIAN_POINT('Ctrl Pts',(-37.7858628320068,-32.8227147956203,
8.));
#31267=CARTESIAN_POINT('Ctrl Pts',(-37.7510079037,-32.7846377476237,8.));
#31268=CARTESIAN_POINT('Ctrl Pts',(-37.7152158718889,-32.7473811107005,
8.));
#31269=CARTESIAN_POINT('Ctrl Pts',(-37.6785241456451,-32.7109602826758,
8.));
#31270=CARTESIAN_POINT('Ctrl Pts',(-32.3264680662287,37.2858331630075,8.));
#31271=CARTESIAN_POINT('Ctrl Pts',(-32.2493254281347,37.208720320707,8.));
#31272=CARTESIAN_POINT('Ctrl Pts',(-32.1762951458997,37.1279853156793,8.));
#31273=CARTESIAN_POINT('Ctrl Pts',(-32.1073695284417,37.0440466492215,8.));
#31274=CARTESIAN_POINT('Ctrl Pts',(-32.036684016981,36.9579647570495,8.));
#31275=CARTESIAN_POINT('Ctrl Pts',(-31.9703150813857,36.8685130624034,8.));
#31276=CARTESIAN_POINT('Ctrl Pts',(-31.9082842995806,36.7760968113946,8.));
#31277=CARTESIAN_POINT('Ctrl Pts',(-31.8449624922372,36.6817571324243,8.));
#31278=CARTESIAN_POINT('Ctrl Pts',(-31.7861608789268,36.5843276270745,8.));
#31279=CARTESIAN_POINT('Ctrl Pts',(-31.7319392047808,36.4841999248104,8.));
#31280=CARTESIAN_POINT('Ctrl Pts',(-31.680149951798,36.3885640193387,8.));
#31281=CARTESIAN_POINT('Ctrl Pts',(-31.6325389456654,36.2904657399127,8.));
#31282=CARTESIAN_POINT('Ctrl Pts',(-31.5891937601898,36.1902217321721,8.));
#31283=CARTESIAN_POINT('Ctrl Pts',(-31.5821558034642,36.1739451150407,8.));
#31284=CARTESIAN_POINT('Ctrl Pts',(-31.575230390001,36.1576118880571,8.));
#31285=CARTESIAN_POINT('Ctrl Pts',(-31.56841798829,36.1412233640005,8.));
#31286=CARTESIAN_POINT('Ctrl Pts',(-31.5619084669515,36.125563476111,8.));
#31287=CARTESIAN_POINT('Ctrl Pts',(-31.5555051500235,36.1098602922108,8.));
#31288=CARTESIAN_POINT('Ctrl Pts',(-31.5492102490141,36.0941204589327,8.));
#31289=CARTESIAN_POINT('Ctrl Pts',(-31.5058248130015,35.9856390819387,8.));
#31290=CARTESIAN_POINT('Ctrl Pts',(-31.467553236408,35.8753407193868,8.));
#31291=CARTESIAN_POINT('Ctrl Pts',(-31.4344241380457,35.7636571739254,8.));
#31292=CARTESIAN_POINT('Ctrl Pts',(-31.4008605131946,35.650508769435,8.));
#31293=CARTESIAN_POINT('Ctrl Pts',(-31.3725747552338,35.5359378557202,8.));
#31294=CARTESIAN_POINT('Ctrl Pts',(-31.3496392634799,35.4203609255757,8.));
#31295=CARTESIAN_POINT('Ctrl Pts',(-31.3256642608852,35.2995456742689,8.));
#31296=CARTESIAN_POINT('Ctrl Pts',(-31.3075347162269,35.1776303306686,8.));
#31297=CARTESIAN_POINT('Ctrl Pts',(-31.2953890537165,35.0550672480091,8.));
#31298=CARTESIAN_POINT('Ctrl Pts',(-31.2862798068337,34.9631449360145,8.));
#31299=CARTESIAN_POINT('Ctrl Pts',(-31.2805376168519,34.8708576741034,8.));
#31300=CARTESIAN_POINT('Ctrl Pts',(-31.2782440105566,34.778392845323,8.));
#31301=CARTESIAN_POINT('Ctrl Pts',(-31.2776964353943,34.7563178084142,8.));
#31302=CARTESIAN_POINT('Ctrl Pts',(-31.2773455727076,34.7342281241833,8.));
#31303=CARTESIAN_POINT('Ctrl Pts',(-31.2771926342729,34.7121554053342,8.));
#31304=CARTESIAN_POINT('Ctrl Pts',(-31.2763577480363,34.5916611083402,8.));
#31305=CARTESIAN_POINT('Ctrl Pts',(-31.2814110294711,34.4715216187175,8.));
#31306=CARTESIAN_POINT('Ctrl Pts',(-31.2924214415633,34.3521629693739,8.));
#31307=CARTESIAN_POINT('Ctrl Pts',(-31.3033611959409,34.2335702867641,8.));
#31308=CARTESIAN_POINT('Ctrl Pts',(-31.3201816201703,34.115747578293,8.));
#31309=CARTESIAN_POINT('Ctrl Pts',(-31.3429997930851,33.999099881963,8.));
#31310=CARTESIAN_POINT('Ctrl Pts',(-31.345873443513,33.984409630306,8.));
#31311=CARTESIAN_POINT('Ctrl Pts',(-31.3488422864746,33.96973800774,8.));
#31312=CARTESIAN_POINT('Ctrl Pts',(-31.35190661501,33.9550858195635,8.));
#31313=CARTESIAN_POINT('Ctrl Pts',(-31.3758170782861,33.8407571491025,8.));
#31314=CARTESIAN_POINT('Ctrl Pts',(-31.4055367574321,33.7276111853924,8.));
#31315=CARTESIAN_POINT('Ctrl Pts',(-31.4407595052535,33.6159144227599,8.));
#31316=CARTESIAN_POINT('Ctrl Pts',(-31.4627247636627,33.5462592025841,8.));
#31317=CARTESIAN_POINT('Ctrl Pts',(-31.4868311858377,33.4771676502711,8.));
#31318=CARTESIAN_POINT('Ctrl Pts',(-31.5130143786684,33.4087065804238,8.));
#31319=CARTESIAN_POINT('Ctrl Pts',(-31.5219642258836,33.3853054574484,8.));
#31320=CARTESIAN_POINT('Ctrl Pts',(-31.5311567813561,33.3619780190094,8.));
#31321=CARTESIAN_POINT('Ctrl Pts',(-31.5405896605283,33.3387270021894,8.));
#31322=CARTESIAN_POINT('Ctrl Pts',(-31.5473384631411,33.3220919409105,8.));
#31323=CARTESIAN_POINT('Ctrl Pts',(-31.5542108294608,33.3054948782145,8.));
#31324=CARTESIAN_POINT('Ctrl Pts',(-31.5611988172515,33.288953116597,8.));
#31325=CARTESIAN_POINT('Ctrl Pts',(-31.6071201467481,33.1802494799514,8.));
#31326=CARTESIAN_POINT('Ctrl Pts',(-31.6580945083799,33.0737722290612,8.));
#31327=CARTESIAN_POINT('Ctrl Pts',(-31.7137634608477,32.9697757128959,8.));
#31328=CARTESIAN_POINT('Ctrl Pts',(-31.7713476440883,32.8622013078145,8.));
#31329=CARTESIAN_POINT('Ctrl Pts',(-31.8339551704749,32.7572805788209,8.));
#31330=CARTESIAN_POINT('Ctrl Pts',(-31.9012446980031,32.6553023741411,8.));
#31331=CARTESIAN_POINT('Ctrl Pts',(-31.9691674082359,32.552364572362,8.));
#31332=CARTESIAN_POINT('Ctrl Pts',(-32.0418610824791,32.4524241883893,8.));
#31333=CARTESIAN_POINT('Ctrl Pts',(-32.1190251653974,32.3557965754622,8.));
#31334=CARTESIAN_POINT('Ctrl Pts',(-32.1734382985285,32.2876585121627,8.));
#31335=CARTESIAN_POINT('Ctrl Pts',(-32.2300754238941,32.2211680942644,8.));
#31336=CARTESIAN_POINT('Ctrl Pts',(-32.2888442072745,32.1564443823762,8.));
#31337=CARTESIAN_POINT('Ctrl Pts',(-32.3150764518969,32.1275540745384,8.));
#31338=CARTESIAN_POINT('Ctrl Pts',(-32.341733542045,32.0990158743987,8.));
#31339=CARTESIAN_POINT('Ctrl Pts',(-32.3688078763672,32.0708409435943,8.));
#31340=CARTESIAN_POINT('Ctrl Pts',(-32.3804297629888,32.0587466166393,8.));
#31341=CARTESIAN_POINT('Ctrl Pts',(-32.3921271141324,32.0467207651166,8.));
#31342=CARTESIAN_POINT('Ctrl Pts',(-32.4038928229971,32.0347706553995,8.));
#31343=CARTESIAN_POINT('Ctrl Pts',(-32.4923350889694,31.9449422571145,8.));
#31344=CARTESIAN_POINT('Ctrl Pts',(-32.5847366887113,31.8592864840437,8.));
#31345=CARTESIAN_POINT('Ctrl Pts',(-32.6807688805232,31.7781214891551,8.));
#31346=CARTESIAN_POINT('Ctrl Pts',(-32.7628090255767,31.7087823662183,8.));
#31347=CARTESIAN_POINT('Ctrl Pts',(-32.8474998792406,31.6427207947673,8.));
#31348=CARTESIAN_POINT('Ctrl Pts',(-32.9346606964287,31.5801527068548,8.));
#31349=CARTESIAN_POINT('Ctrl Pts',(-32.9737718119822,31.5520769292834,8.));
#31350=CARTESIAN_POINT('Ctrl Pts',(-33.0133805354119,31.5247048259746,8.));
#31351=CARTESIAN_POINT('Ctrl Pts',(-33.0534717786847,31.4980572637843,8.));
#31352=CARTESIAN_POINT('Ctrl Pts',(-33.0807061080661,31.4799553435978,8.));
#31353=CARTESIAN_POINT('Ctrl Pts',(-33.1081687455454,31.4621843968183,8.));
#31354=CARTESIAN_POINT('Ctrl Pts',(-33.1358249991596,31.4447697393726,8.));
#31355=CARTESIAN_POINT('Ctrl Pts',(-33.2426293820058,31.3775168942506,8.));
#31356=CARTESIAN_POINT('Ctrl Pts',(-33.3523804860194,31.3155308622806,8.));
#31357=CARTESIAN_POINT('Ctrl Pts',(-33.464776332519,31.2591453036981,8.));
#31358=CARTESIAN_POINT('Ctrl Pts',(-33.5668700198747,31.2079280232686,8.));
#31359=CARTESIAN_POINT('Ctrl Pts',(-33.671146627403,31.161331555616,8.));
#31360=CARTESIAN_POINT('Ctrl Pts',(-33.7774031884393,31.1196350702262,8.));
#31361=CARTESIAN_POINT('Ctrl Pts',(-33.8328337169093,31.0978833948665,8.));
#31362=CARTESIAN_POINT('Ctrl Pts',(-33.8888033971972,31.0774656906331,8.));
#31363=CARTESIAN_POINT('Ctrl Pts',(-33.9452681066883,31.058369845356,8.));
#31364=CARTESIAN_POINT('Ctrl Pts',(-36.0520713770612,31.0647048309474,8.));
#31365=CARTESIAN_POINT('Ctrl Pts',(-36.168179415234,31.1043194708775,8.));
#31366=CARTESIAN_POINT('Ctrl Pts',(-36.2820223922111,31.1494845221288,8.));
#31367=CARTESIAN_POINT('Ctrl Pts',(-36.3933744144291,31.1998423763314,8.));
#31368=CARTESIAN_POINT('Ctrl Pts',(-36.5072236213378,31.25132955769,8.));
#31369=CARTESIAN_POINT('Ctrl Pts',(-36.6184695195224,31.3082455598905,8.));
#31370=CARTESIAN_POINT('Ctrl Pts',(-36.7268464017735,31.3702567471293,8.));
#31371=CARTESIAN_POINT('Ctrl Pts',(-36.8407847815347,31.4354501172862,8.));
#31372=CARTESIAN_POINT('Ctrl Pts',(-36.9515531074568,31.5062754464572,8.));
#31373=CARTESIAN_POINT('Ctrl Pts',(-37.0588034719145,31.5823912510781,8.));
#31374=CARTESIAN_POINT('Ctrl Pts',(-37.152647540815,31.6489925801213,8.));
#31375=CARTESIAN_POINT('Ctrl Pts',(-37.2437978659804,31.7196454871349,8.));
#31376=CARTESIAN_POINT('Ctrl Pts',(-37.3319898787643,31.7941433466814,8.));
#31377=CARTESIAN_POINT('Ctrl Pts',(-37.3493659727369,31.8088213403836,8.));
#31378=CARTESIAN_POINT('Ctrl Pts',(-37.3666271256303,31.8236486435546,8.));
#31379=CARTESIAN_POINT('Ctrl Pts',(-37.3837711593319,31.8386237468057,8.));
#31380=CARTESIAN_POINT('Ctrl Pts',(-37.3963054555396,31.8495723008716,8.));
#31381=CARTESIAN_POINT('Ctrl Pts',(-37.4087759352647,31.8605988651726,8.));
#31382=CARTESIAN_POINT('Ctrl Pts',(-37.4211729491963,31.8716947276461,8.));
#31383=CARTESIAN_POINT('Ctrl Pts',(-37.5137521425834,31.9545571010691,8.));
#31384=CARTESIAN_POINT('Ctrl Pts',(-37.6023754843508,32.0414011788236,8.));
#31385=CARTESIAN_POINT('Ctrl Pts',(-37.6867815485414,32.1319060425465,8.));
#31386=CARTESIAN_POINT('Ctrl Pts',(-37.7709958473242,32.2222052847627,8.));
#31387=CARTESIAN_POINT('Ctrl Pts',(-37.8510125269352,32.3161494024035,8.));
#31388=CARTESIAN_POINT('Ctrl Pts',(-37.9265315102947,32.413451696318,8.));
#31389=CARTESIAN_POINT('Ctrl Pts',(-38.0010181696068,32.5094238942302,8.));
#31390=CARTESIAN_POINT('Ctrl Pts',(-38.0711296560004,32.6086637703888,8.));
#31391=CARTESIAN_POINT('Ctrl Pts',(-38.1365319925539,32.7109170507384,8.));
#31392=CARTESIAN_POINT('Ctrl Pts',(-38.189837488265,32.7942575257788,8.));
#31393=CARTESIAN_POINT('Ctrl Pts',(-38.2400140119095,32.8796002993686,8.));
#31394=CARTESIAN_POINT('Ctrl Pts',(-38.2868547984211,32.966813541324,8.));
#31395=CARTESIAN_POINT('Ctrl Pts',(-38.2987553976748,32.9889713640128,8.));
#31396=CARTESIAN_POINT('Ctrl Pts',(-38.3104405526761,33.0112499393599,8.));
#31397=CARTESIAN_POINT('Ctrl Pts',(-38.3219066094193,33.0336471306571,8.));
#31398=CARTESIAN_POINT('Ctrl Pts',(-38.3300627268695,33.0495788608817,8.));
#31399=CARTESIAN_POINT('Ctrl Pts',(-38.3381042716881,33.0655634268488,8.));
#31400=CARTESIAN_POINT('Ctrl Pts',(-38.3460275803167,33.0815944092568,8.));
#31401=CARTESIAN_POINT('Ctrl Pts',(-38.3989884279579,33.1887484350122,8.));
#31402=CARTESIAN_POINT('Ctrl Pts',(-38.4467104251109,33.2980523321741,8.));
#31403=CARTESIAN_POINT('Ctrl Pts',(-38.4889147723839,33.409243488173,8.));
#31404=CARTESIAN_POINT('Ctrl Pts',(-38.5302829624144,33.5182317125689,8.));
#31405=CARTESIAN_POINT('Ctrl Pts',(-38.5663502410402,33.6290337883757,8.));
#31406=CARTESIAN_POINT('Ctrl Pts',(-38.596805840802,33.7414161893267,8.));
#31407=CARTESIAN_POINT('Ctrl Pts',(-38.6012600218942,33.7578522985917,8.));
#31408=CARTESIAN_POINT('Ctrl Pts',(-38.6055940819337,33.7743222252706,8.));
#31409=CARTESIAN_POINT('Ctrl Pts',(-38.6098069546845,33.7908252519299,8.));
#31410=CARTESIAN_POINT('Ctrl Pts',(-38.6394755059943,33.9070454470715,8.));
#31411=CARTESIAN_POINT('Ctrl Pts',(-38.6631380748325,34.0249075695662,8.));
#31412=CARTESIAN_POINT('Ctrl Pts',(-38.6808855164532,34.1439757769513,8.));
#31413=CARTESIAN_POINT('Ctrl Pts',(-38.6908690551697,34.2109556878445,8.));
#31414=CARTESIAN_POINT('Ctrl Pts',(-38.6989798315808,34.2783172077624,8.));
#31415=CARTESIAN_POINT('Ctrl Pts',(-38.7052269705051,34.3459812971573,8.));
#31416=CARTESIAN_POINT('Ctrl Pts',(-38.7081094451816,34.3772019929916,8.));
#31417=CARTESIAN_POINT('Ctrl Pts',(-38.7105950890294,34.4084870828833,8.));
#31418=CARTESIAN_POINT('Ctrl Pts',(-38.712684450918,34.4398286677084,8.));
#31419=CARTESIAN_POINT('Ctrl Pts',(-38.7138855420385,34.457845699339,8.));
#31420=CARTESIAN_POINT('Ctrl Pts',(-38.7149551618269,34.47587434695,8.));
#31421=CARTESIAN_POINT('Ctrl Pts',(-38.7158933795518,34.4939047698972,8.));
#31422=CARTESIAN_POINT('Ctrl Pts',(-38.722204302566,34.6151864384397,8.));
#31423=CARTESIAN_POINT('Ctrl Pts',(-38.7225826970351,34.7366654075262,8.));
#31424=CARTESIAN_POINT('Ctrl Pts',(-38.7171867711641,34.8578944234449,8.));
#31425=CARTESIAN_POINT('Ctrl Pts',(-38.7119027789398,34.9766086520668,8.));
#31426=CARTESIAN_POINT('Ctrl Pts',(-38.7010810476264,35.0950841138035,8.));
#31427=CARTESIAN_POINT('Ctrl Pts',(-38.6848167703974,35.2128948265086,8.));
#31428=CARTESIAN_POINT('Ctrl Pts',(-38.6687114015083,35.3295544825446,8.));
#31429=CARTESIAN_POINT('Ctrl Pts',(-38.6472689687305,35.445563152418,8.));
#31430=CARTESIAN_POINT('Ctrl Pts',(-38.6205351191465,35.5604883182129,8.));
#31431=CARTESIAN_POINT('Ctrl Pts',(-38.603128213054,35.6353182285994,8.));
#31432=CARTESIAN_POINT('Ctrl Pts',(-38.5834770455875,35.7096883679731,8.));
#31433=CARTESIAN_POINT('Ctrl Pts',(-38.5615844164204,35.7834724389555,8.));
#31434=CARTESIAN_POINT('Ctrl Pts',(-38.5541960688544,35.8083731649983,8.));
#31435=CARTESIAN_POINT('Ctrl Pts',(-38.546552371059,35.8332070872086,8.));
#31436=CARTESIAN_POINT('Ctrl Pts',(-38.5386532430018,35.8579691742342,8.));
#31437=CARTESIAN_POINT('Ctrl Pts',(-38.533566838996,35.8739139693719,8.));
#31438=CARTESIAN_POINT('Ctrl Pts',(-38.5283753166192,35.8898263677189,8.));
#31439=CARTESIAN_POINT('Ctrl Pts',(-38.5230815350611,35.9056970029845,8.));
#31440=CARTESIAN_POINT('Ctrl Pts',(-38.4861838533105,36.0163154036073,8.));
#31441=CARTESIAN_POINT('Ctrl Pts',(-38.4442854600859,36.1250223270562,8.));
#31442=CARTESIAN_POINT('Ctrl Pts',(-38.3974511486834,36.2313985734173,8.));
#31443=CARTESIAN_POINT('Ctrl Pts',(-38.3593370627389,36.3179682970844,8.));
#31444=CARTESIAN_POINT('Ctrl Pts',(-38.3179530705292,36.4029942704614,8.));
#31445=CARTESIAN_POINT('Ctrl Pts',(-38.2733131103528,36.4862349013589,8.));
#31446=CARTESIAN_POINT('Ctrl Pts',(-38.2516981197193,36.52654061512,8.));
#31447=CARTESIAN_POINT('Ctrl Pts',(-38.2293194750761,36.5664275009295,8.));
#31448=CARTESIAN_POINT('Ctrl Pts',(-38.2061772856241,36.6058666059334,8.));
#31449=CARTESIAN_POINT('Ctrl Pts',(-38.1925908747914,36.6290206763194,8.));
#31450=CARTESIAN_POINT('Ctrl Pts',(-38.1787392319563,36.6520234773565,8.));
#31451=CARTESIAN_POINT('Ctrl Pts',(-38.1646364321387,36.6748466577435,8.));
#31452=CARTESIAN_POINT('Ctrl Pts',(-38.1062049879234,36.7694088304221,8.));
#31453=CARTESIAN_POINT('Ctrl Pts',(-38.0434222829092,36.8609657921147,8.));
#31454=CARTESIAN_POINT('Ctrl Pts',(-37.9763223631119,36.9491268302023,8.));
#31455=CARTESIAN_POINT('Ctrl Pts',(-37.9162915853069,37.0279998855573,8.));
#31456=CARTESIAN_POINT('Ctrl Pts',(-37.8528047083354,37.1041548125789,8.));
#31457=CARTESIAN_POINT('Ctrl Pts',(-37.7858626225071,37.1772853000647,8.));
#31458=CARTESIAN_POINT('Ctrl Pts',(-37.7510076908282,37.2153623649398,8.));
#31459=CARTESIAN_POINT('Ctrl Pts',(-37.7152156561398,37.2526190163742,8.));
#31460=CARTESIAN_POINT('Ctrl Pts',(-37.6785239274887,37.2890398567007,8.));
#31461=CARTESIAN_POINT('Origin',(-35.,-35.,10.2084234471775));
#31462=CARTESIAN_POINT('Ctrl Pts',(-39.0784093524563,-34.997955826836,7.70842344717746));
#31463=CARTESIAN_POINT('Ctrl Pts',(-39.0792534643083,-34.8668875745646,
7.70328437820511));
#31464=CARTESIAN_POINT('Ctrl Pts',(-39.0145241717454,-33.401902569157,7.64581193344868));
#31465=CARTESIAN_POINT('Ctrl Pts',(-37.2468182307978,-30.7615622415685,
7.53600611290816));
#31466=CARTESIAN_POINT('Ctrl Pts',(-32.7044906448315,-30.7882310811688,
7.37900598555592));
#31467=CARTESIAN_POINT('Ctrl Pts',(-30.2206288723714,-34.591050784955,7.22200585820366));
#31468=CARTESIAN_POINT('Ctrl Pts',(-32.0224449816578,-38.760868439734,7.06500573085141));
#31469=CARTESIAN_POINT('Ctrl Pts',(-36.4942781630208,-39.5581356918704,
6.90800560349915));
#31470=CARTESIAN_POINT('Ctrl Pts',(-38.8653532597229,-37.0673722499186,
6.78914484227451));
#31471=CARTESIAN_POINT('Ctrl Pts',(-39.0751760778997,-35.366983894328,6.72261745683394));
#31472=CARTESIAN_POINT('Ctrl Pts',(-39.0721140267755,-35.0034548068065,
6.70842344717746));
#31473=CARTESIAN_POINT('Ctrl Pts',(-39.0691247390887,-35.0040754761348,
7.79157655282255));
#31474=CARTESIAN_POINT('Ctrl Pts',(-39.0629617458988,-34.1015748206833,
7.75638428364687));
#31475=CARTESIAN_POINT('Ctrl Pts',(-38.3270258918815,-31.8449563360523,
7.6688586386871));
#31476=CARTESIAN_POINT('Ctrl Pts',(-34.6204730922247,-30.2191423808613,
7.52899961794324));
#31477=CARTESIAN_POINT('Ctrl Pts',(-30.8030823517117,-32.6774434597138,
7.37199949059099));
#31478=CARTESIAN_POINT('Ctrl Pts',(-30.7475655592404,-37.2202136561835,
7.21499936323873));
#31479=CARTESIAN_POINT('Ctrl Pts',(-34.5060129709306,-39.7711989299046,
7.05799923588648));
#31480=CARTESIAN_POINT('Ctrl Pts',(-38.2826810114871,-38.2186958612719,
6.91685829908109));
#31481=CARTESIAN_POINT('Ctrl Pts',(-39.0636923276262,-35.9315794222149,
6.82805073805978));
#31482=CARTESIAN_POINT('Ctrl Pts',(-39.0709664927331,-34.9967444357251,
6.79157655282255));
#31483=CARTESIAN_POINT('Ctrl Pts',(-32.3264680662287,-32.7141668369925,
8.));
#31484=CARTESIAN_POINT('Ctrl Pts',(-31.5748397248436,-33.5932784036375,
7.94766662421592));
#31485=CARTESIAN_POINT('Ctrl Pts',(-31.0185761455706,-36.1362135079881,
7.84299987264775));
#31486=CARTESIAN_POINT('Ctrl Pts',(-33.7549095310954,-38.9529268308332,
7.68599974529549));
#31487=CARTESIAN_POINT('Ctrl Pts',(-37.6085237505035,-38.2165103725086,
7.52899961794325));
#31488=CARTESIAN_POINT('Ctrl Pts',(-39.122629513254,-34.5999498459216,7.37199949059098));
#31489=CARTESIAN_POINT('Ctrl Pts',(-36.940145606194,-31.3400749195329,7.21499936323873));
#31490=CARTESIAN_POINT('Ctrl Pts',(-33.0178092164465,-31.3631036769391,
7.05799923588649));
#31491=CARTESIAN_POINT('Ctrl Pts',(-30.8729746062518,-34.6468690649513,
6.90099910853422));
#31492=CARTESIAN_POINT('Ctrl Pts',(-32.4288573028063,-38.2475401342247,
6.74399898118198));
#31493=CARTESIAN_POINT('Ctrl Pts',(-36.2903212074201,-38.9359868162892,
6.58699885382972));
#31494=CARTESIAN_POINT('Ctrl Pts',(-38.9947353103719,-36.0950579107052,
6.42999872647747));
#31495=CARTESIAN_POINT('Ctrl Pts',(-38.117035111845,-32.2721495171465,6.27299859912521));
#31496=CARTESIAN_POINT('Ctrl Pts',(-34.444258048923,-30.8953459884408,6.11599847177297));
#31497=CARTESIAN_POINT('Ctrl Pts',(-31.2698209074708,-33.1992175611906,
5.9589983444207));
#31498=CARTESIAN_POINT('Ctrl Pts',(-31.4402707556255,-37.1178717601522,
5.80199821706845));
#31499=CARTESIAN_POINT('Ctrl Pts',(-34.8027641605008,-39.1374081785836,
5.6449980897162));
#31500=CARTESIAN_POINT('Ctrl Pts',(-38.3421207391464,-37.4468919117391,
5.48799796236395));
#31501=CARTESIAN_POINT('Ctrl Pts',(-38.8845656356524,-33.5622237360543,
5.33099783501169));
#31502=CARTESIAN_POINT('Ctrl Pts',(-35.943683236251,-30.9668235565892,5.17399770765944));
#31503=CARTESIAN_POINT('Ctrl Pts',(-32.1565910373224,-31.9880112738199,
5.01699758030718));
#31504=CARTESIAN_POINT('Ctrl Pts',(-30.919210927847,-35.7100782334501,4.85999745295493));
#31505=CARTESIAN_POINT('Ctrl Pts',(-33.3411135315715,-38.7954112012017,
4.70299732560268));
#31506=CARTESIAN_POINT('Ctrl Pts',(-37.2505555447442,-38.477362547094,4.54599719825042));
#31507=CARTESIAN_POINT('Ctrl Pts',(-39.141902810795,-35.0411295298515,4.38899707089817));
#31508=CARTESIAN_POINT('Ctrl Pts',(-37.3191660904533,-31.5680152720272,
4.23199694354592));
#31509=CARTESIAN_POINT('Ctrl Pts',(-33.4168108878721,-31.1723946430222,
4.07499681619366));
#31510=CARTESIAN_POINT('Ctrl Pts',(-30.9341165505443,-34.2090244589174,
3.91799668884141));
#31511=CARTESIAN_POINT('Ctrl Pts',(-32.0973389085718,-37.9549296302039,
3.76099656148916));
#31512=CARTESIAN_POINT('Ctrl Pts',(-35.8634053144019,-39.0511210542994,
3.6039964341369));
#31513=CARTESIAN_POINT('Ctrl Pts',(-38.8552478911374,-36.5146333635664,
3.44699630678465));
#31514=CARTESIAN_POINT('Ctrl Pts',(-38.3900526994102,-32.6199594063295,
3.2899961794324));
#31515=CARTESIAN_POINT('Ctrl Pts',(-34.8849647272175,-30.8594906798889,
3.13299605208015));
#31516=CARTESIAN_POINT('Ctrl Pts',(-31.4830299921864,-32.8118563882867,
2.97599592472789));
#31517=CARTESIAN_POINT('Ctrl Pts',(-31.2347959944593,-36.726351454856,2.81899579737564));
#31518=CARTESIAN_POINT('Ctrl Pts',(-34.3628565683332,-39.0928106312356,
2.66199567002338));
#31519=CARTESIAN_POINT('Ctrl Pts',(-38.0622497333952,-37.7892072071444,
2.50499554267113));
#31520=CARTESIAN_POINT('Ctrl Pts',(-39.0156942580864,-33.9844950081716,
2.34799541531887));
#31521=CARTESIAN_POINT('Ctrl Pts',(-36.3682270687435,-31.0903957040226,
2.19099528796663));
#31522=CARTESIAN_POINT('Ctrl Pts',(-32.4938578387906,-31.7020764289629,
2.03399516061437));
#31523=CARTESIAN_POINT('Ctrl Pts',(-30.866769727096,-35.2710361541464,1.87699503326212));
#31524=CARTESIAN_POINT('Ctrl Pts',(-32.9459900633082,-38.5969565794207,
1.71999490590986));
#31525=CARTESIAN_POINT('Ctrl Pts',(-36.8670583779424,-38.6974486722808,
1.56299477855761));
#31526=CARTESIAN_POINT('Ctrl Pts',(-39.1139224428247,-35.4824088304557,
1.40599465120536));
#31527=CARTESIAN_POINT('Ctrl Pts',(-37.6717828958998,-31.8347767559132,
1.2489945238531));
#31528=CARTESIAN_POINT('Ctrl Pts',(-33.8338499179097,-31.0254541111767,
1.09199439650085));
#31529=CARTESIAN_POINT('Ctrl Pts',(-31.0415747701051,-33.7800977940573,
0.934994269148597));
#31530=CARTESIAN_POINT('Ctrl Pts',(-31.7989383549478,-37.6287343727556,
0.777994141796342));
#31531=CARTESIAN_POINT('Ctrl Pts',(-35.4265617474899,-39.1199684759325,
0.620994014444089));
#31532=CARTESIAN_POINT('Ctrl Pts',(-38.6720112486245,-36.9171723860524,
0.463993887091836));
#31533=CARTESIAN_POINT('Ctrl Pts',(-38.6240720221873,-32.9944536386984,
0.306993759739581));
#31534=CARTESIAN_POINT('Ctrl Pts',(-35.3277245214386,-30.8716914151866,
0.149993632387329));
#31535=CARTESIAN_POINT('Ctrl Pts',(-31.7348166906651,-32.4476562217995,
-0.00700649496492554));
#31536=CARTESIAN_POINT('Ctrl Pts',(-31.0753023569953,-36.3188879616356,
-0.164006622317179));
#31537=CARTESIAN_POINT('Ctrl Pts',(-32.9741442474368,-38.0994349533405,
-0.268673373885348));
#31538=CARTESIAN_POINT('Ctrl Pts',(-34.0915279074966,-38.3981590173419,
-0.321006749669432));
#31539=CARTESIAN_POINT('Ctrl Pts',(-32.1856025125516,-32.5937287191406,
8.10700224988981));
#31540=CARTESIAN_POINT('Ctrl Pts',(-31.3943716733878,-33.5191597390956,
8.05466887410573));
#31541=CARTESIAN_POINT('Ctrl Pts',(-30.8087991578366,-36.1960793891008,
7.95000212253755));
#31542=CARTESIAN_POINT('Ctrl Pts',(-33.6893070387277,-39.1612023407069,
7.79300199518531));
#31543=CARTESIAN_POINT('Ctrl Pts',(-37.7459640921552,-38.3859848825408,
7.63600186783305));
#31544=CARTESIAN_POINT('Ctrl Pts',(-39.3398464769469,-34.5788716288481,
7.4790017404808));
#31545=CARTESIAN_POINT('Ctrl Pts',(-37.0423698143953,-31.1472373602114,
7.32200161312854));
#31546=CARTESIAN_POINT('Ctrl Pts',(-32.9133696925748,-31.171479478349,7.1650014857763));
#31547=CARTESIAN_POINT('Ctrl Pts',(-30.6555260282916,-34.6282629716192,
7.00800135842403));
#31548=CARTESIAN_POINT('Ctrl Pts',(-32.2933865290902,-38.4186495693944,
6.85100123107179));
#31549=CARTESIAN_POINT('Ctrl Pts',(-36.358306859287,-39.1433697748163,6.69400110371953));
#31550=CARTESIAN_POINT('Ctrl Pts',(-39.2052136645597,-36.1527553471755,
6.53700097636729));
#31551=CARTESIAN_POINT('Ctrl Pts',(-38.2812683762075,-32.1284219768986,
6.38000084901502));
#31552=CARTESIAN_POINT('Ctrl Pts',(-34.4149765966796,-30.6790761348112,
6.22300072166278));
#31553=CARTESIAN_POINT('Ctrl Pts',(-31.073281738985,-33.1043362500341,6.06600059431052));
#31554=CARTESIAN_POINT('Ctrl Pts',(-31.2527124083266,-37.2294601703531,
5.90900046695826));
#31555=CARTESIAN_POINT('Ctrl Pts',(-34.792372013923,-39.3554038144322,5.75200033960602));
#31556=CARTESIAN_POINT('Ctrl Pts',(-38.5182135257814,-37.5758160437388,
5.59500021225375));
#31557=CARTESIAN_POINT('Ctrl Pts',(-39.0892392668699,-33.4864688341112,
5.43800008490151));
#31558=CARTESIAN_POINT('Ctrl Pts',(-35.9934049021458,-30.7543197799925,
5.28099995754925));
#31559=CARTESIAN_POINT('Ctrl Pts',(-32.0067748436954,-31.8293127917771,
5.12399983019699));
#31560=CARTESIAN_POINT('Ctrl Pts',(-30.7041984924888,-35.7474915002398,
4.96699970284474));
#31561=CARTESIAN_POINT('Ctrl Pts',(-33.2537085681557,-38.9953873801041,
4.80999957549249));
#31562=CARTESIAN_POINT('Ctrl Pts',(-37.3691349224156,-38.6605810807291,
4.65299944814024));
#31563=CARTESIAN_POINT('Ctrl Pts',(-39.3601352640338,-35.0432966010287,
4.49599932078798));
#31564=CARTESIAN_POINT('Ctrl Pts',(-37.4413604847951,-31.3871876474119,
4.33899919343573));
#31565=CARTESIAN_POINT('Ctrl Pts',(-33.3333943376382,-30.9707221882978,
4.18199906608348));
#31566=CARTESIAN_POINT('Ctrl Pts',(-30.7198894765905,-34.1673487990413,
4.02499893873122));
#31567=CARTESIAN_POINT('Ctrl Pts',(-31.9444007833091,-38.1106217291751,
3.86799881137897));
#31568=CARTESIAN_POINT('Ctrl Pts',(-35.9088972219885,-39.2645703133555,
3.71099868402671));
#31569=CARTESIAN_POINT('Ctrl Pts',(-39.0583768015825,-36.5944377843333,
3.55399855667446));
#31570=CARTESIAN_POINT('Ctrl Pts',(-38.5686709700449,-32.4945575991672,
3.39699842932221));
#31571=CARTESIAN_POINT('Ctrl Pts',(-34.8789036410609,-30.641331648192,3.23999830196996));
#31572=CARTESIAN_POINT('Ctrl Pts',(-31.2977245835776,-32.6965654289773,
3.0829981746177));
#31573=CARTESIAN_POINT('Ctrl Pts',(-31.0364114005639,-36.8173110766423,
2.92599804726545));
#31574=CARTESIAN_POINT('Ctrl Pts',(-34.3292861586667,-39.3084564697542,
2.76899791991319));
#31575=CARTESIAN_POINT('Ctrl Pts',(-38.2235964144439,-37.9361675679284,
2.61199779256094));
#31576=CARTESIAN_POINT('Ctrl Pts',(-39.2272769169348,-33.9309891303743,
2.45499766520869));
#31577=CARTESIAN_POINT('Ctrl Pts',(-36.4403174975728,-30.8844028124269,
2.29799753785644));
#31578=CARTESIAN_POINT('Ctrl Pts',(-32.3618118741726,-31.5283123441018,
2.14099741050418));
#31579=CARTESIAN_POINT('Ctrl Pts',(-30.6489942206534,-35.2853167607994,
1.98399728315193));
#31580=CARTESIAN_POINT('Ctrl Pts',(-32.8377664646538,-38.7864763954034,
1.82699715579967));
#31581=CARTESIAN_POINT('Ctrl Pts',(-36.9654316978321,-38.89226330974,1.66999702844742));
#31582=CARTESIAN_POINT('Ctrl Pts',(-39.3306806402386,-35.5078264385801,
1.51299690109516));
#31583=CARTESIAN_POINT('Ctrl Pts',(-37.8125562946319,-31.668004510122,1.35599677374291));
#31584=CARTESIAN_POINT('Ctrl Pts',(-33.7724067105519,-30.8160395161343,
1.19899664639066));
#31585=CARTESIAN_POINT('Ctrl Pts',(-30.8330095554335,-33.7158224444716,
1.04199651903841));
#31586=CARTESIAN_POINT('Ctrl Pts',(-31.630277821932,-37.7672395905951,0.884996391686153));
#31587=CARTESIAN_POINT('Ctrl Pts',(-35.4490368322191,-39.3370452323995,
0.727996264333899));
#31588=CARTESIAN_POINT('Ctrl Pts',(-38.8654856152897,-37.0181861597217,
0.570996136981647));
#31589=CARTESIAN_POINT('Ctrl Pts',(-38.815020522006,-32.8887835342792,0.413996009629392));
#31590=CARTESIAN_POINT('Ctrl Pts',(-35.3449919778631,-30.6541752272542,
0.256995882277139));
#31591=CARTESIAN_POINT('Ctrl Pts',(-31.5627776553664,-32.3131759431282,
0.0999957549248853));
#31592=CARTESIAN_POINT('Ctrl Pts',(-30.8685142129999,-36.3883787653949,
-0.0570043724273683));
#31593=CARTESIAN_POINT('Ctrl Pts',(-32.8674040627957,-38.2627408840732,
-0.161671123995537));
#31594=CARTESIAN_POINT('Ctrl Pts',(-34.0436614793107,-38.5772044012455,
-0.214004499779622));
#31595=CARTESIAN_POINT('Ctrl Pts',(-32.0447369588746,-32.4732906012887,
8.21400449977962));
#31596=CARTESIAN_POINT('Ctrl Pts',(-31.2139036219321,-33.4450410745538,
8.16167112399554));
#31597=CARTESIAN_POINT('Ctrl Pts',(-30.5990221701027,-36.2559452702134,
8.05700437242737));
#31598=CARTESIAN_POINT('Ctrl Pts',(-33.6237045463599,-39.3694778505807,
7.90000424507512));
#31599=CARTESIAN_POINT('Ctrl Pts',(-37.883404433807,-38.555459392573,7.74300411772286));
#31600=CARTESIAN_POINT('Ctrl Pts',(-39.5570634406398,-34.5577934117747,
7.58600399037061));
#31601=CARTESIAN_POINT('Ctrl Pts',(-37.1445940225965,-30.95439980089,7.42900386301835));
#31602=CARTESIAN_POINT('Ctrl Pts',(-32.8089301687032,-30.9798552797588,
7.2720037356661));
#31603=CARTESIAN_POINT('Ctrl Pts',(-30.4380774503315,-34.6096568782872,
7.11500360831385));
#31604=CARTESIAN_POINT('Ctrl Pts',(-32.157915755374,-38.5897590045642,6.9580034809616));
#31605=CARTESIAN_POINT('Ctrl Pts',(-36.4262925111539,-39.3507527333434,
6.80100335360934));
#31606=CARTESIAN_POINT('Ctrl Pts',(-39.4156920187475,-36.2104527836457,
6.64400322625709));
#31607=CARTESIAN_POINT('Ctrl Pts',(-38.4455016405701,-31.9846944366506,
6.48700309890483));
#31608=CARTESIAN_POINT('Ctrl Pts',(-34.3856951444362,-30.4628062811815,
6.33000297155259));
#31609=CARTESIAN_POINT('Ctrl Pts',(-30.8767425704992,-33.0094549388777,
6.17300284420032));
#31610=CARTESIAN_POINT('Ctrl Pts',(-31.0651540610276,-37.3410485805539,
6.01600271684808));
#31611=CARTESIAN_POINT('Ctrl Pts',(-34.7819798673453,-39.5733994502808,
5.85900258949582));
#31612=CARTESIAN_POINT('Ctrl Pts',(-38.6943063124164,-37.7047401757385,
5.70200246214356));
#31613=CARTESIAN_POINT('Ctrl Pts',(-39.2939128980875,-33.4107139321682,
5.54500233479131));
#31614=CARTESIAN_POINT('Ctrl Pts',(-36.0431265680407,-30.5418160033959,
5.38800220743906));
#31615=CARTESIAN_POINT('Ctrl Pts',(-31.8569586500684,-31.6706143097344,
5.2310020800868));
#31616=CARTESIAN_POINT('Ctrl Pts',(-30.4891860571307,-35.7849047670295,
5.07400195273456));
#31617=CARTESIAN_POINT('Ctrl Pts',(-33.1663036047398,-39.1953635590066,
4.9170018253823));
#31618=CARTESIAN_POINT('Ctrl Pts',(-37.487714300087,-38.8437996143642,4.76000169803005));
#31619=CARTESIAN_POINT('Ctrl Pts',(-39.5783677172726,-35.0454636722059,
4.60300157067779));
#31620=CARTESIAN_POINT('Ctrl Pts',(-37.563554879137,-31.2063600227966,4.44600144332554));
#31621=CARTESIAN_POINT('Ctrl Pts',(-33.2499777874043,-30.7690497335734,
4.28900131597329));
#31622=CARTESIAN_POINT('Ctrl Pts',(-30.5056624026368,-34.1256731391653,
4.13200118862103));
#31623=CARTESIAN_POINT('Ctrl Pts',(-31.7914626580464,-38.2663138281463,
3.97500106126878));
#31624=CARTESIAN_POINT('Ctrl Pts',(-35.9543891295751,-39.4780195724117,
3.81800093391652));
#31625=CARTESIAN_POINT('Ctrl Pts',(-39.2615057120276,-36.6742422051002,
3.66100080656427));
#31626=CARTESIAN_POINT('Ctrl Pts',(-38.7472892406796,-32.3691557920048,
3.50400067921202));
#31627=CARTESIAN_POINT('Ctrl Pts',(-34.8728425549044,-30.4231726164951,
3.34700055185977));
#31628=CARTESIAN_POINT('Ctrl Pts',(-31.1124191749688,-32.5812744696679,
3.19000042450751));
#31629=CARTESIAN_POINT('Ctrl Pts',(-30.8380268066686,-36.9082706984286,
3.03300029715526));
#31630=CARTESIAN_POINT('Ctrl Pts',(-34.295715749,-39.5241023082727,2.876000169803));
#31631=CARTESIAN_POINT('Ctrl Pts',(-38.3849430954928,-38.0831279287123,
2.71900004245075));
#31632=CARTESIAN_POINT('Ctrl Pts',(-39.438859575783,-33.8774832525769,2.5619999150985));
#31633=CARTESIAN_POINT('Ctrl Pts',(-36.5124079264021,-30.6784099208313,
2.40499978774625));
#31634=CARTESIAN_POINT('Ctrl Pts',(-32.2297659095544,-31.3545482592407,
2.24799966039399));
#31635=CARTESIAN_POINT('Ctrl Pts',(-30.4312187142109,-35.2995973674523,
2.09099953304174));
#31636=CARTESIAN_POINT('Ctrl Pts',(-32.7295428659994,-38.9759962113862,
1.93399940568948));
#31637=CARTESIAN_POINT('Ctrl Pts',(-37.0638050177218,-39.0870779471991,
1.77699927833723));
#31638=CARTESIAN_POINT('Ctrl Pts',(-39.5474388376525,-35.5332440467046,
1.61999915098498));
#31639=CARTESIAN_POINT('Ctrl Pts',(-37.953329693364,-31.5012322643307,1.46299902363272));
#31640=CARTESIAN_POINT('Ctrl Pts',(-33.7109635031942,-30.6066249210918,
1.30599889628047));
#31641=CARTESIAN_POINT('Ctrl Pts',(-30.624444340762,-33.6515470948858,1.14899876892822));
#31642=CARTESIAN_POINT('Ctrl Pts',(-31.4616172889162,-37.9057448084347,
0.991998641575964));
#31643=CARTESIAN_POINT('Ctrl Pts',(-35.4715119169482,-39.5541219888666,
0.83499851422371));
#31644=CARTESIAN_POINT('Ctrl Pts',(-39.0589599819549,-37.1191999333909,
0.677998386871458));
#31645=CARTESIAN_POINT('Ctrl Pts',(-39.0059690218246,-32.78311342986,0.520998259519202));
#31646=CARTESIAN_POINT('Ctrl Pts',(-35.3622594342876,-30.4366590393219,
0.36399813216695));
#31647=CARTESIAN_POINT('Ctrl Pts',(-31.3907386200676,-32.1786956644568,
0.206998004814696));
#31648=CARTESIAN_POINT('Ctrl Pts',(-30.6617260690046,-36.4578695691541,
0.0499978774624427));
#31649=CARTESIAN_POINT('Ctrl Pts',(-32.7606638781546,-38.426046814806,-0.0546688741057264));
#31650=CARTESIAN_POINT('Ctrl Pts',(-33.9957950511247,-38.756249785149,-0.107002249889811));
#31651=CARTESIAN_POINT('Ctrl Pts',(-31.9038714051976,-32.3528524834368,
8.32100674966943));
#31652=CARTESIAN_POINT('Ctrl Pts',(-31.0334355704763,-33.370922410012,8.26867337388535));
#31653=CARTESIAN_POINT('Ctrl Pts',(-30.3892451823686,-36.3158111513261,
8.16400662231718));
#31654=CARTESIAN_POINT('Ctrl Pts',(-33.5581020539921,-39.5777533604545,
8.00700649496493));
#31655=CARTESIAN_POINT('Ctrl Pts',(-38.0208447754587,-38.7249339026052,
7.85000636761267));
#31656=CARTESIAN_POINT('Ctrl Pts',(-39.7742804043327,-34.5367151947012,
7.69300624026042));
#31657=CARTESIAN_POINT('Ctrl Pts',(-37.2468182307978,-30.7615622415685,
7.53600611290816));
#31658=CARTESIAN_POINT('Ctrl Pts',(-32.7044906448315,-30.7882310811688,
7.37900598555592));
#31659=CARTESIAN_POINT('Ctrl Pts',(-30.2206288723714,-34.591050784955,7.22200585820366));
#31660=CARTESIAN_POINT('Ctrl Pts',(-32.0224449816578,-38.760868439734,7.06500573085141));
#31661=CARTESIAN_POINT('Ctrl Pts',(-36.4942781630208,-39.5581356918704,
6.90800560349915));
#31662=CARTESIAN_POINT('Ctrl Pts',(-39.6261703729353,-36.2681502201159,
6.75100547614691));
#31663=CARTESIAN_POINT('Ctrl Pts',(-38.6097349049326,-31.8409668964026,
6.59400534879464));
#31664=CARTESIAN_POINT('Ctrl Pts',(-34.3564136921927,-30.2465364275518,
6.4370052214424));
#31665=CARTESIAN_POINT('Ctrl Pts',(-30.6802034020135,-32.9145736277213,
6.28000509409013));
#31666=CARTESIAN_POINT('Ctrl Pts',(-30.8775957137286,-37.4526369907548,
6.12300496673789));
#31667=CARTESIAN_POINT('Ctrl Pts',(-34.7715877207675,-39.7913950861294,
5.96600483938563));
#31668=CARTESIAN_POINT('Ctrl Pts',(-38.8703990990513,-37.8336643077382,
5.80900471203337));
#31669=CARTESIAN_POINT('Ctrl Pts',(-39.498586529305,-33.3349590302252,5.65200458468112));
#31670=CARTESIAN_POINT('Ctrl Pts',(-36.0928482339355,-30.3293122267992,
5.49500445732888));
#31671=CARTESIAN_POINT('Ctrl Pts',(-31.7071424564414,-31.5119158276916,
5.33800432997661));
#31672=CARTESIAN_POINT('Ctrl Pts',(-30.2741736217725,-35.8223180338192,
5.18100420262437));
#31673=CARTESIAN_POINT('Ctrl Pts',(-33.0788986413239,-39.395339737909,5.02400407527211));
#31674=CARTESIAN_POINT('Ctrl Pts',(-37.6062936777584,-39.0270181479993,
4.86700394791986));
#31675=CARTESIAN_POINT('Ctrl Pts',(-39.7966001705114,-35.0476307433831,
4.7100038205676));
#31676=CARTESIAN_POINT('Ctrl Pts',(-37.6857492734788,-31.0255323981813,
4.55300369321535));
#31677=CARTESIAN_POINT('Ctrl Pts',(-33.1665612371704,-30.5673772788489,
4.39600356586309));
#31678=CARTESIAN_POINT('Ctrl Pts',(-30.291435328683,-34.0839974792893,4.23900343851084));
#31679=CARTESIAN_POINT('Ctrl Pts',(-31.6385245327839,-38.4220059271175,
4.08200331115859));
#31680=CARTESIAN_POINT('Ctrl Pts',(-35.9998810371616,-39.6914688314679,
3.92500318380634));
#31681=CARTESIAN_POINT('Ctrl Pts',(-39.4646346224728,-36.7540466258671,
3.76800305645408));
#31682=CARTESIAN_POINT('Ctrl Pts',(-38.9259075113142,-32.2437539848424,
3.61100292910183));
#31683=CARTESIAN_POINT('Ctrl Pts',(-34.8667814687478,-30.2050135847982,
3.45400280174957));
#31684=CARTESIAN_POINT('Ctrl Pts',(-30.9271137663599,-32.4659835103585,
3.29700267439732));
#31685=CARTESIAN_POINT('Ctrl Pts',(-30.6396422127733,-36.9992303202149,
3.14000254704507));
#31686=CARTESIAN_POINT('Ctrl Pts',(-34.2621453393335,-39.7397481467912,
2.98300241969281));
#31687=CARTESIAN_POINT('Ctrl Pts',(-38.5462897765416,-38.2300882894962,
2.82600229234056));
#31688=CARTESIAN_POINT('Ctrl Pts',(-39.6504422346313,-33.8239773747795,
2.66900216498831));
#31689=CARTESIAN_POINT('Ctrl Pts',(-36.5844983552314,-30.4724170292356,
2.51200203763606));
#31690=CARTESIAN_POINT('Ctrl Pts',(-32.0977199449364,-31.1807841743797,
2.3550019102838));
#31691=CARTESIAN_POINT('Ctrl Pts',(-30.2134432077683,-35.3138779741053,
2.19800178293155));
#31692=CARTESIAN_POINT('Ctrl Pts',(-32.621319267345,-39.1655160273689,2.04100165557929));
#31693=CARTESIAN_POINT('Ctrl Pts',(-37.1621783376115,-39.2818925846584,
1.88400152822705));
#31694=CARTESIAN_POINT('Ctrl Pts',(-39.7641970350665,-35.558661654829,1.72700140087479));
#31695=CARTESIAN_POINT('Ctrl Pts',(-38.0941030920961,-31.3344600185395,
1.57000127352254));
#31696=CARTESIAN_POINT('Ctrl Pts',(-33.6495202958365,-30.3972103260493,
1.41300114617028));
#31697=CARTESIAN_POINT('Ctrl Pts',(-30.4158791260905,-33.5872717453,1.25600101881803));
#31698=CARTESIAN_POINT('Ctrl Pts',(-31.2929567559004,-38.0442500262742,
1.09900089146578));
#31699=CARTESIAN_POINT('Ctrl Pts',(-35.4939870016774,-39.7711987453336,
0.942000764113521));
#31700=CARTESIAN_POINT('Ctrl Pts',(-39.2524343486202,-37.2202137070602,
0.785000636761268));
#31701=CARTESIAN_POINT('Ctrl Pts',(-39.1969175216432,-32.6774433254408,
0.628000509409014));
#31702=CARTESIAN_POINT('Ctrl Pts',(-35.3795268907121,-30.2191428513895,
0.471000382056761));
#31703=CARTESIAN_POINT('Ctrl Pts',(-31.2186995847689,-32.0442153857854,
0.314000254704507));
#31704=CARTESIAN_POINT('Ctrl Pts',(-30.4549379250093,-36.5273603729133,
0.157000127352253));
#31705=CARTESIAN_POINT('Ctrl Pts',(-32.6539236935135,-38.5893527455387,
0.0523333757840845));
#31706=CARTESIAN_POINT('Ctrl Pts',(-33.9479286229388,-38.9352951690526,
0.));
#31707=CARTESIAN_POINT('Ctrl Pts',(-33.9479286229388,-38.9352951690526,
5.55111512312578E-17));
#31708=CARTESIAN_POINT('Ctrl Pts',(-33.8318206360164,-38.8956805466085,
1.21569200333733E-16));
#31709=CARTESIAN_POINT('Ctrl Pts',(-33.7179777099102,-38.8505155072641,
1.50554103324791E-15));
#31710=CARTESIAN_POINT('Ctrl Pts',(-33.6066257375518,-38.8001576608968,
1.0547118733939E-15));
#31711=CARTESIAN_POINT('Ctrl Pts',(-33.492776560763,-38.7486704781164,5.93772317186044E-16));
#31712=CARTESIAN_POINT('Ctrl Pts',(-33.3815306925957,-38.6917544682482,
3.73522748729697E-15));
#31713=CARTESIAN_POINT('Ctrl Pts',(-33.2731538396993,-38.6297432688828,
2.72004641033163E-15));
#31714=CARTESIAN_POINT('Ctrl Pts',(-33.1592154520342,-38.5645498637963,
1.65276966251693E-15));
#31715=CARTESIAN_POINT('Ctrl Pts',(-33.048447119632,-38.4937244909346,-6.09647221355942E-16));
#31716=CARTESIAN_POINT('Ctrl Pts',(-32.9411967497889,-38.4176086362753,
-1.0547118733939E-15));
#31717=CARTESIAN_POINT('Ctrl Pts',(-32.8473526761762,-38.3510072634485,
-1.44414344392711E-15));
#31718=CARTESIAN_POINT('Ctrl Pts',(-32.7562023471369,-38.2803543077884,
-2.56653707031024E-15));
#31719=CARTESIAN_POINT('Ctrl Pts',(-32.6680103311015,-38.2058563963449,
-2.83106871279415E-15));
#31720=CARTESIAN_POINT('Ctrl Pts',(-32.6506345001076,-38.1911786151031,
-2.88318745685931E-15));
#31721=CARTESIAN_POINT('Ctrl Pts',(-32.6333736067294,-38.1763515287969,
-1.26352082166837E-15));
#31722=CARTESIAN_POINT('Ctrl Pts',(-32.6162298289787,-38.1613766467586,
-1.22124532708767E-15));
#31723=CARTESIAN_POINT('Ctrl Pts',(-32.6036955222168,-38.1504280817505,
-1.1903365025982E-15));
#31724=CARTESIAN_POINT('Ctrl Pts',(-32.5912250315541,-38.1394015059403,
9.6075348530294E-17));
#31725=CARTESIAN_POINT('Ctrl Pts',(-32.5788280068545,-38.1283056318751,
1.11022302462516E-16));
#31726=CARTESIAN_POINT('Ctrl Pts',(-32.4862488011484,-38.0454432328352,
2.22644014631185E-16));
#31727=CARTESIAN_POINT('Ctrl Pts',(-32.3976254460622,-37.9585991267844,
2.93313669984113E-16));
#31728=CARTESIAN_POINT('Ctrl Pts',(-32.3132193670584,-37.8680942341505,
1.66533453693773E-16));
#31729=CARTESIAN_POINT('Ctrl Pts',(-32.2290050385629,-37.7777949470768,
4.00412518592805E-17));
#31730=CARTESIAN_POINT('Ctrl Pts',(-32.1489883292395,-37.6838507826712,
-7.67367206503618E-16));
#31731=CARTESIAN_POINT('Ctrl Pts',(-32.0734693158047,-37.5865484422576,
-3.88578058618805E-16));
#31732=CARTESIAN_POINT('Ctrl Pts',(-31.9989826203281,-37.4905761901068,
-1.49668231824771E-17));
#31733=CARTESIAN_POINT('Ctrl Pts',(-31.9288710981801,-37.3913362593944,
6.39667558614738E-17));
#31734=CARTESIAN_POINT('Ctrl Pts',(-31.8634687260135,-37.2890829263301,
2.77555756156289E-16));
#31735=CARTESIAN_POINT('Ctrl Pts',(-31.8101631638829,-37.2057423498624,
4.51639376496992E-16));
#31736=CARTESIAN_POINT('Ctrl Pts',(-31.7599865782998,-37.1203994732574,
-1.91642689345195E-15));
#31737=CARTESIAN_POINT('Ctrl Pts',(-31.7131457346326,-37.0331861281649,
-2.08166817117217E-15));
#31738=CARTESIAN_POINT('Ctrl Pts',(-31.7012454402134,-37.0110288738836,
-2.12364905155618E-15));
#31739=CARTESIAN_POINT('Ctrl Pts',(-31.6895605787933,-36.988750873417,8.89729854294519E-16));
#31740=CARTESIAN_POINT('Ctrl Pts',(-31.6780948040882,-36.9663542633258,
9.71445146547012E-16));
#31741=CARTESIAN_POINT('Ctrl Pts',(-31.6699383315321,-36.9504218610016,
1.0295754129979E-15));
#31742=CARTESIAN_POINT('Ctrl Pts',(-31.661896440285,-36.9344366167593,-7.00903233658188E-16));
#31743=CARTESIAN_POINT('Ctrl Pts',(-31.6539727955662,-36.9184049530428,
-6.38378239159465E-16));
#31744=CARTESIAN_POINT('Ctrl Pts',(-31.6010119288307,-36.8112508799156,
-2.20467287978913E-16));
#31745=CARTESIAN_POINT('Ctrl Pts',(-31.5532899127003,-36.7019469405238,
-5.43579179869397E-17));
#31746=CARTESIAN_POINT('Ctrl Pts',(-31.5110855463215,-36.5907557494425,
2.77555756156289E-17));
#31747=CARTESIAN_POINT('Ctrl Pts',(-31.4697173372396,-36.4817674898051,
1.08242228141372E-16));
#31748=CARTESIAN_POINT('Ctrl Pts',(-31.433650039522,-36.3709653855926,-1.8533573671039E-16));
#31749=CARTESIAN_POINT('Ctrl Pts',(-31.4031944204139,-36.2585829650152,
-1.08246744900953E-15));
#31750=CARTESIAN_POINT('Ctrl Pts',(-31.3987402034729,-36.2421467310371,
-1.21367539645156E-15));
#31751=CARTESIAN_POINT('Ctrl Pts',(-31.3944061093602,-36.2256766793315,
1.54092145767103E-16));
#31752=CARTESIAN_POINT('Ctrl Pts',(-31.3901932043347,-36.2091735273543,
1.66533453693773E-16));
#31753=CARTESIAN_POINT('Ctrl Pts',(-31.3605246504064,-36.0929533297801,
3.08986100652746E-16));
#31754=CARTESIAN_POINT('Ctrl Pts',(-31.3368620771271,-35.9750912152647,
2.82593330474131E-15));
#31755=CARTESIAN_POINT('Ctrl Pts',(-31.319114629565,-35.8560230245863,3.49720252756924E-15));
#31756=CARTESIAN_POINT('Ctrl Pts',(-31.3091310875555,-35.7890431234222,
3.87481426369542E-15));
#31757=CARTESIAN_POINT('Ctrl Pts',(-31.3010203073581,-35.7216816160001,
-1.45794491220195E-16));
#31758=CARTESIAN_POINT('Ctrl Pts',(-31.294773164211,-35.6540175415704,-4.71844785465692E-16));
#31759=CARTESIAN_POINT('Ctrl Pts',(-31.2918906865937,-35.6227968418935,
-6.22286780009977E-16));
#31760=CARTESIAN_POINT('Ctrl Pts',(-31.2894050399855,-35.5915117486406,
3.58433295205778E-16));
#31761=CARTESIAN_POINT('Ctrl Pts',(-31.2873156755218,-35.5601701609149,
2.4980018054066E-16));
#31762=CARTESIAN_POINT('Ctrl Pts',(-31.286114583885,-35.5421531420771,1.87351370019253E-16));
#31763=CARTESIAN_POINT('Ctrl Pts',(-31.2850449634327,-35.5241245074566,
-4.29409397736477E-17));
#31764=CARTESIAN_POINT('Ctrl Pts',(-31.284106744896,-35.5060940976467,-5.55111512312578E-17));
#31765=CARTESIAN_POINT('Ctrl Pts',(-31.2777958135452,-35.3848124622,-1.40064737065375E-16));
#31766=CARTESIAN_POINT('Ctrl Pts',(-31.2774174094918,-35.2633335332142,
2.82866543587948E-15));
#31767=CARTESIAN_POINT('Ctrl Pts',(-31.282813324883,-35.142104562563,2.35922392732846E-15));
#31768=CARTESIAN_POINT('Ctrl Pts',(-31.2880973068045,-35.0233903791791,
1.89952056570822E-15));
#31769=CARTESIAN_POINT('Ctrl Pts',(-31.2989190268708,-34.9049149676345,
7.28996419448176E-16));
#31770=CARTESIAN_POINT('Ctrl Pts',(-31.3151832922329,-34.7871043083849,
6.93889390390723E-16));
#31771=CARTESIAN_POINT('Ctrl Pts',(-31.3312886503615,-34.670444698108,6.59125368578839E-16));
#31772=CARTESIAN_POINT('Ctrl Pts',(-31.3527310724264,-34.5544360772762,
1.70606179182567E-15));
#31773=CARTESIAN_POINT('Ctrl Pts',(-31.379464911652,-34.4395109622456,2.28983498828939E-15));
#31774=CARTESIAN_POINT('Ctrl Pts',(-31.3968718099089,-34.3646810896034,
2.66994053729605E-15));
#31775=CARTESIAN_POINT('Ctrl Pts',(-31.4165229694089,-34.2903109886468,
-2.96848706176688E-17));
#31776=CARTESIAN_POINT('Ctrl Pts',(-31.4384155905674,-34.2165269562934,
1.38777878078145E-17));
#31777=CARTESIAN_POINT('Ctrl Pts',(-31.4458039406444,-34.1916262257156,
2.85793700622958E-17));
#31778=CARTESIAN_POINT('Ctrl Pts',(-31.4534476413064,-34.1667922990885,
3.06223347651583E-15));
#31779=CARTESIAN_POINT('Ctrl Pts',(-31.4613467725894,-34.1420302077573,
3.1641356201817E-15));
#31780=CARTESIAN_POINT('Ctrl Pts',(-31.4664331829338,-34.1260853964884,
3.22975247083094E-15));
#31781=CARTESIAN_POINT('Ctrl Pts',(-31.4716247119601,-34.1101729821539,
1.52985938675526E-15));
#31782=CARTESIAN_POINT('Ctrl Pts',(-31.4769185004878,-34.0943023310132,
1.56819002228303E-15));
#31783=CARTESIAN_POINT('Ctrl Pts',(-31.5138161753674,-33.9836839859762,
1.8353543263008E-15));
#31784=CARTESIAN_POINT('Ctrl Pts',(-31.5557145621555,-33.8749771180903,
2.68190903327311E-15));
#31785=CARTESIAN_POINT('Ctrl Pts',(-31.60254886788,-33.7686009256992,2.26207941267376E-15));
#31786=CARTESIAN_POINT('Ctrl Pts',(-31.6406629427424,-33.6820312606289,
1.92041922701669E-15));
#31787=CARTESIAN_POINT('Ctrl Pts',(-31.6820469232643,-33.5970053442715,
1.26636124083292E-15));
#31788=CARTESIAN_POINT('Ctrl Pts',(-31.7266868713332,-33.5137647678308,
1.40165656858926E-15));
#31789=CARTESIAN_POINT('Ctrl Pts',(-31.7483018585373,-33.473459075901,1.46716754933025E-15));
#31790=CARTESIAN_POINT('Ctrl Pts',(-31.7706804998245,-33.4335722114158,
1.17298588323861E-16));
#31791=CARTESIAN_POINT('Ctrl Pts',(-31.7938226860146,-33.3941331271239,
-4.02455846426619E-16));
#31792=CARTESIAN_POINT('Ctrl Pts',(-31.8074090785167,-33.3709790968731,
-7.07595028060502E-16));
#31793=CARTESIAN_POINT('Ctrl Pts',(-31.8212607024029,-33.3479763354121,
-4.73580047421181E-16));
#31794=CARTESIAN_POINT('Ctrl Pts',(-31.8353634826968,-33.3251531939272,
-3.88578058618805E-16));
#31795=CARTESIAN_POINT('Ctrl Pts',(-31.8937949297824,-33.2305910468749,
-3.63929499130585E-17));
#31796=CARTESIAN_POINT('Ctrl Pts',(-31.9565776402818,-33.1390341079118,
1.65098064735663E-15));
#31797=CARTESIAN_POINT('Ctrl Pts',(-32.0236775684477,-33.0508730884183,
2.24126273096203E-15));
#31798=CARTESIAN_POINT('Ctrl Pts',(-32.0837083254303,-32.9720000868933,
2.76935689262062E-15));
#31799=CARTESIAN_POINT('Ctrl Pts',(-32.1471951806296,-32.895845207831,1.97196154581884E-15));
#31800=CARTESIAN_POINT('Ctrl Pts',(-32.2141372439519,-32.8227147610826,
2.21437451708439E-15));
#31801=CARTESIAN_POINT('Ctrl Pts',(-32.2489921734814,-32.7846377069649,
2.36892565463969E-15));
#31802=CARTESIAN_POINT('Ctrl Pts',(-32.2847842063358,-32.7473810647789,
1.32299506859179E-17));
#31803=CARTESIAN_POINT('Ctrl Pts',(-32.3214759334524,-32.7109602322923,
-5.55111512312578E-17));
#31804=CARTESIAN_POINT('Ctrl Pts',(-38.5163032009778,-35.0029832534533,
6.38741669750803));
#31805=CARTESIAN_POINT('Ctrl Pts',(-38.5189473067417,-35.316893543218,6.40161070716451));
#31806=CARTESIAN_POINT('Ctrl Pts',(-38.4802906988737,-35.6301637893069,
6.41580471682099));
#31807=CARTESIAN_POINT('Ctrl Pts',(-38.3977162601254,-35.9313946627094,
6.42999872647747));
#31808=CARTESIAN_POINT('Ctrl Pts',(-38.0932639427213,-37.0420342125665,
6.48233210226156));
#31809=CARTESIAN_POINT('Ctrl Pts',(-37.1917925750707,-37.9890105144279,
6.53466547804564));
#31810=CARTESIAN_POINT('Ctrl Pts',(-36.0974795738098,-38.3477575516811,
6.58699885382972));
#31811=CARTESIAN_POINT('Ctrl Pts',(-35.0031665725488,-38.7065045889344,
6.63933222961381));
#31812=CARTESIAN_POINT('Ctrl Pts',(-33.7160119376775,-38.4770223615795,
6.69166560539789));
#31813=CARTESIAN_POINT('Ctrl Pts',(-32.8131208374828,-37.7621694030232,
6.74399898118198));
#31814=CARTESIAN_POINT('Ctrl Pts',(-31.9102297372881,-37.0473164444669,
6.79633235696606));
#31815=CARTESIAN_POINT('Ctrl Pts',(-31.3916021717699,-35.8470927547091,
6.84866573275014));
#31816=CARTESIAN_POINT('Ctrl Pts',(-31.4897608240433,-34.6996866784948,
6.90099910853423));
#31817=CARTESIAN_POINT('Ctrl Pts',(-31.5879194763167,-33.5522806022806,
6.95333248431831));
#31818=CARTESIAN_POINT('Ctrl Pts',(-32.3028643463816,-32.4576921396098,
7.0056658601024));
#31819=CARTESIAN_POINT('Ctrl Pts',(-33.3140595130386,-31.9065597820401,
7.05799923588649));
#31820=CARTESIAN_POINT('Ctrl Pts',(-34.3252546796956,-31.3554274244703,
7.11033261167057));
#31821=CARTESIAN_POINT('Ctrl Pts',(-35.6327001429448,-31.3477511720016,
7.16266598745465));
#31822=CARTESIAN_POINT('Ctrl Pts',(-36.6501701924127,-31.8872255334987,
7.21499936323874));
#31823=CARTESIAN_POINT('Ctrl Pts',(-37.6676402418807,-32.4266998949958,
7.26733273902282));
#31824=CARTESIAN_POINT('Ctrl Pts',(-38.3951348775673,-33.5133248704587,
7.3196661148069));
#31825=CARTESIAN_POINT('Ctrl Pts',(-38.5065312349523,-34.6593974459546,
7.37199949059099));
#31826=CARTESIAN_POINT('Ctrl Pts',(-38.5174702113759,-34.7719402721061,
7.37713855956333));
#31827=CARTESIAN_POINT('Ctrl Pts',(-38.5224681626868,-34.8850563504433,
7.38227762853568));
#31828=CARTESIAN_POINT('Ctrl Pts',(-38.5217392653161,-34.9982348400382,
7.38741669750802));
#31829=CARTESIAN_POINT('Ctrl Pts',(-36.0520713770612,-38.9352951690526,
8.));
#31830=CARTESIAN_POINT('Ctrl Pts',(-37.3460763064865,-38.5893527455387,
7.94766662421592));
#31831=CARTESIAN_POINT('Ctrl Pts',(-39.5450618542894,-36.527358944407,7.84299987264775));
#31832=CARTESIAN_POINT('Ctrl Pts',(-38.7813006061664,-32.0442159203332,
7.6859997452955));
#31833=CARTESIAN_POINT('Ctrl Pts',(-34.6204730922247,-30.2191423808613,
7.52899961794324));
#31834=CARTESIAN_POINT('Ctrl Pts',(-30.8030823517117,-32.6774434597138,
7.37199949059099));
#31835=CARTESIAN_POINT('Ctrl Pts',(-30.7475655592404,-37.2202136561835,
7.21499936323873));
#31836=CARTESIAN_POINT('Ctrl Pts',(-34.5060129709306,-39.7711989299046,
7.05799923588648));
#31837=CARTESIAN_POINT('Ctrl Pts',(-38.7070433506006,-38.044250072918,6.90099910853423));
#31838=CARTESIAN_POINT('Ctrl Pts',(-39.584120987438,-33.5872717262032,6.74399898118198));
#31839=CARTESIAN_POINT('Ctrl Pts',(-36.3504797430715,-30.3972101963624,
6.58699885382972));
#31840=CARTESIAN_POINT('Ctrl Pts',(-31.905896825022,-31.3344599279876,6.42999872647746));
#31841=CARTESIAN_POINT('Ctrl Pts',(-30.2358028418083,-35.5586616666892,
6.27299859912522));
#31842=CARTESIAN_POINT('Ctrl Pts',(-32.83782160528,-39.2818926978495,6.11599847177295));
#31843=CARTESIAN_POINT('Ctrl Pts',(-37.3786807951101,-39.1655161353224,
5.95899834442071));
#31844=CARTESIAN_POINT('Ctrl Pts',(-39.7865569169479,-35.3138779826965,
5.80199821706845));
#31845=CARTESIAN_POINT('Ctrl Pts',(-37.9022801309199,-31.1807840744948,
5.64499808971621));
#31846=CARTESIAN_POINT('Ctrl Pts',(-33.4155016033557,-30.4724169111822,
5.48799796236394));
#31847=CARTESIAN_POINT('Ctrl Pts',(-30.3495576440316,-33.8239773440302,
5.3309978350117));
#31848=CARTESIAN_POINT('Ctrl Pts',(-31.4537101308888,-38.230088373826,5.17399770765944));
#31849=CARTESIAN_POINT('Ctrl Pts',(-35.7378546799324,-39.7397482704758,
5.01699758030718));
#31850=CARTESIAN_POINT('Ctrl Pts',(-39.3603579010204,-36.9992303723996,
4.85999745295493));
#31851=CARTESIAN_POINT('Ctrl Pts',(-39.0728863399384,-32.4659834442205,
4.70299732560268));
#31852=CARTESIAN_POINT('Ctrl Pts',(-35.1332185347277,-30.2050134596587,
4.54599719825043));
#31853=CARTESIAN_POINT('Ctrl Pts',(-31.0740923862265,-32.2437539129077,
4.38899707089817));
#31854=CARTESIAN_POINT('Ctrl Pts',(-30.535365261007,-36.7540466716456,4.23199694354592));
#31855=CARTESIAN_POINT('Ctrl Pts',(-34.0001189367432,-39.6914689539076,
4.07499681619366));
#31856=CARTESIAN_POINT('Ctrl Pts',(-38.3614755549453,-38.4220060164266,
3.91799668884141));
#31857=CARTESIAN_POINT('Ctrl Pts',(-39.7085647942032,-34.0839974553828,
3.76099656148916));
#31858=CARTESIAN_POINT('Ctrl Pts',(-36.8334388106793,-30.5673771631648,
3.6039964341369));
#31859=CARTESIAN_POINT('Ctrl Pts',(-32.3142506564274,-31.0255322944533,
3.44699630678465));
#31860=CARTESIAN_POINT('Ctrl Pts',(-30.2033997043049,-35.0476307446275,
3.28999617943239));
#31861=CARTESIAN_POINT('Ctrl Pts',(-32.3937062542216,-39.0270182530956,
3.13299605208014));
#31862=CARTESIAN_POINT('Ctrl Pts',(-36.9211014088136,-39.3953398526252,
2.97599592472789));
#31863=CARTESIAN_POINT('Ctrl Pts',(-39.7258265015647,-35.8223180552711,
2.81899579737564));
#31864=CARTESIAN_POINT('Ctrl Pts',(-38.2928576294957,-31.5119157366759,
2.66199567002338));
#31865=CARTESIAN_POINT('Ctrl Pts',(-33.9071517375455,-30.3293121048675,
2.50499554267113));
#31866=CARTESIAN_POINT('Ctrl Pts',(-30.5014133532831,-33.3349589868354,
2.34799541531887));
#31867=CARTESIAN_POINT('Ctrl Pts',(-31.12960079995,-37.8336643815683,2.19099528796663));
#31868=CARTESIAN_POINT('Ctrl Pts',(-35.2284122851668,-39.7913952114128,
2.03399516061437));
#31869=CARTESIAN_POINT('Ctrl Pts',(-39.1224043939168,-37.4526370543192,
1.87699503326212));
#31870=CARTESIAN_POINT('Ctrl Pts',(-39.3197967106052,-32.9145735741338,
1.71999490590986));
#31871=CARTESIAN_POINT('Ctrl Pts',(-35.6435863248602,-30.2465363019221,
1.56299477855761));
#31872=CARTESIAN_POINT('Ctrl Pts',(-31.3902650003177,-31.8409668168855,
1.40599465120536));
#31873=CARTESIAN_POINT('Ctrl Pts',(-30.3738295074692,-36.2681502477922,
1.2489945238531));
#31874=CARTESIAN_POINT('Ctrl Pts',(-33.5057217955833,-39.5581358207848,
1.09199439650085));
#31875=CARTESIAN_POINT('Ctrl Pts',(-37.977555101084,-38.7608685197788,0.934994269148597));
#31876=CARTESIAN_POINT('Ctrl Pts',(-39.7793712418172,-34.5910508068424,
0.777994141796343));
#31877=CARTESIAN_POINT('Ctrl Pts',(-37.2955094371433,-30.7882309135474,
0.620994014444089));
#31878=CARTESIAN_POINT('Ctrl Pts',(-32.7531816644513,-30.7615622313046,
0.463993887091836));
#31879=CARTESIAN_POINT('Ctrl Pts',(-30.2257195673566,-34.5367150123096,
0.306993759739581));
#31880=CARTESIAN_POINT('Ctrl Pts',(-31.9791549439529,-38.7249342807031,
0.149993632387329));
#31881=CARTESIAN_POINT('Ctrl Pts',(-36.441898406148,-39.5777530280863,-0.00700649496492615));
#31882=CARTESIAN_POINT('Ctrl Pts',(-39.6107538265857,-36.3158122035465,
-0.164006622317178));
#31883=CARTESIAN_POINT('Ctrl Pts',(-38.9665644295237,-33.3709224100119,
-0.268673373885348));
#31884=CARTESIAN_POINT('Ctrl Pts',(-38.0961285948024,-32.3528524834368,
-0.321006749669432));
#31885=CARTESIAN_POINT('Ctrl Pts',(-36.0042049488753,-38.756249785149,8.10700224988981));
#31886=CARTESIAN_POINT('Ctrl Pts',(-37.2393361218454,-38.4260468148059,
8.05466887410573));
#31887=CARTESIAN_POINT('Ctrl Pts',(-39.3382737203354,-36.457868205641,7.95000212253756));
#31888=CARTESIAN_POINT('Ctrl Pts',(-38.6092615621806,-32.178696174684,7.7930019951853));
#31889=CARTESIAN_POINT('Ctrl Pts',(-34.6377405494255,-30.4366585902015,
7.63600186783305));
#31890=CARTESIAN_POINT('Ctrl Pts',(-30.9940308572923,-32.7831135580239,
7.4790017404808));
#31891=CARTESIAN_POINT('Ctrl Pts',(-30.9410399300978,-37.119199884829,7.32200161312854));
#31892=CARTESIAN_POINT('Ctrl Pts',(-34.528488056906,-39.5541221650401,7.16500148577629));
#31893=CARTESIAN_POINT('Ctrl Pts',(-38.5383828127393,-37.9057448529564,
7.00800135842404));
#31894=CARTESIAN_POINT('Ctrl Pts',(-39.3755557676012,-33.6515470766578,
6.85100123107178));
#31895=CARTESIAN_POINT('Ctrl Pts',(-36.2890365339436,-30.6066247973054,
6.69400110371953));
#31896=CARTESIAN_POINT('Ctrl Pts',(-32.046670227525,-31.5012321778987,6.53700097636728));
#31897=CARTESIAN_POINT('Ctrl Pts',(-30.4525610448241,-35.5332440580251,
6.38000084901503));
#31898=CARTESIAN_POINT('Ctrl Pts',(-32.936194927768,-39.0870780552405,6.22300072166276));
#31899=CARTESIAN_POINT('Ctrl Pts',(-37.2704571936142,-38.975996314428,6.06600059431052));
#31900=CARTESIAN_POINT('Ctrl Pts',(-39.5687814048312,-35.2995973756527,
5.90900046695826));
#31901=CARTESIAN_POINT('Ctrl Pts',(-37.7702341628505,-31.3545481639004,
5.75200033960601));
#31902=CARTESIAN_POINT('Ctrl Pts',(-33.4875920340692,-30.678409808149,5.59500021225376));
#31903=CARTESIAN_POINT('Ctrl Pts',(-30.5611403084004,-33.8774832232266,
5.4380000849015));
#31904=CARTESIAN_POINT('Ctrl Pts',(-31.6150568161493,-38.0831280092054,
5.28099995754926));
#31905=CARTESIAN_POINT('Ctrl Pts',(-35.7042842693892,-39.5241024263299,
5.12399983019699));
#31906=CARTESIAN_POINT('Ctrl Pts',(-39.1619733019478,-36.908270748239,4.96699970284474));
#31907=CARTESIAN_POINT('Ctrl Pts',(-38.8875809264933,-32.581274406539,4.80999957549249));
#31908=CARTESIAN_POINT('Ctrl Pts',(-35.127157448413,-30.4231724970492,4.65299944814023));
#31909=CARTESIAN_POINT('Ctrl Pts',(-31.2527106615227,-32.3691557233429,
4.49599932078798));
#31910=CARTESIAN_POINT('Ctrl Pts',(-30.7384941767535,-36.6742422487958,
4.33899919343573));
#31911=CARTESIAN_POINT('Ctrl Pts',(-34.045610845517,-39.4780196892807,4.18199906608348));
#31912=CARTESIAN_POINT('Ctrl Pts',(-38.2085374256912,-38.2663139133921,
4.02499893873122));
#31913=CARTESIAN_POINT('Ctrl Pts',(-39.4943377146584,-34.1256731163465,
3.86799881137897));
#31914=CARTESIAN_POINT('Ctrl Pts',(-36.7500222582684,-30.7690496231526,
3.71099868402672));
#31915=CARTESIAN_POINT('Ctrl Pts',(-32.4364450539584,-31.206359923788,3.55399855667446));
#31916=CARTESIAN_POINT('Ctrl Pts',(-30.4216321632391,-35.0454636733936,
3.39699842932221));
#31917=CARTESIAN_POINT('Ctrl Pts',(-32.5122856349878,-38.843799714679,3.23999830196996));
#31918=CARTESIAN_POINT('Ctrl Pts',(-36.8336964431165,-39.1953636685035,
3.0829981746177));
#31919=CARTESIAN_POINT('Ctrl Pts',(-39.510814060595,-35.7849047875054,2.92599804726545));
#31920=CARTESIAN_POINT('Ctrl Pts',(-38.1430414319588,-31.6706142228596,
2.76899791991319));
#31921=CARTESIAN_POINT('Ctrl Pts',(-33.9568734047379,-30.5418158870118,
2.61199779256094));
#31922=CARTESIAN_POINT('Ctrl Pts',(-30.7060869898426,-33.4107138907526,
2.45499766520869));
#31923=CARTESIAN_POINT('Ctrl Pts',(-31.3056935911801,-37.7047402462095,
2.29799753785644));
#31924=CARTESIAN_POINT('Ctrl Pts',(-35.2180201383191,-39.5733995698641,
2.14099741050418));
#31925=CARTESIAN_POINT('Ctrl Pts',(-38.9348460417202,-37.3410486412263,
1.98399728315193));
#31926=CARTESIAN_POINT('Ctrl Pts',(-39.1232575369955,-33.0094548877283,
1.82699715579967));
#31927=CARTESIAN_POINT('Ctrl Pts',(-35.614304871841,-30.4628061612676,1.66999702844742));
#31928=CARTESIAN_POINT('Ctrl Pts',(-31.5544982689911,-31.9846943607513,
1.51299690109517));
#31929=CARTESIAN_POINT('Ctrl Pts',(-30.5843078670984,-36.2104528100627,
1.35599677374291));
#31930=CARTESIAN_POINT('Ctrl Pts',(-33.5737074493336,-39.3507528563925,
1.19899664639066));
#31931=CARTESIAN_POINT('Ctrl Pts',(-37.8420843236033,-38.5897590809672,
1.04199651903841));
#31932=CARTESIAN_POINT('Ctrl Pts',(-39.5619226586618,-34.6096568991787,
0.884996391686153));
#31933=CARTESIAN_POINT('Ctrl Pts',(-37.191069909542,-30.9798551197638,0.7279962643339));
#31934=CARTESIAN_POINT('Ctrl Pts',(-32.8554058774184,-30.954399791093,0.570996136981647));
#31935=CARTESIAN_POINT('Ctrl Pts',(-30.4429365323376,-34.5577932376814,
0.413996009629392));
#31936=CARTESIAN_POINT('Ctrl Pts',(-32.1165952983707,-38.5554597534685,
0.25699588227714));
#31937=CARTESIAN_POINT('Ctrl Pts',(-36.3762958928451,-39.3694775333344,
0.0999957549248847));
#31938=CARTESIAN_POINT('Ctrl Pts',(-39.4009768839417,-36.2559462745606,
-0.0570043724273669));
#31939=CARTESIAN_POINT('Ctrl Pts',(-38.7860963780679,-33.4450410745538,
-0.161671123995537));
#31940=CARTESIAN_POINT('Ctrl Pts',(-37.9552630411254,-32.4732906012887,
-0.214004499779622));
#31941=CARTESIAN_POINT('Ctrl Pts',(-35.9563385206894,-38.5772044012455,
8.21400449977962));
#31942=CARTESIAN_POINT('Ctrl Pts',(-37.1325959372043,-38.2627408840732,
8.16167112399554));
#31943=CARTESIAN_POINT('Ctrl Pts',(-39.1314855863814,-36.388377466875,8.05700437242737));
#31944=CARTESIAN_POINT('Ctrl Pts',(-38.4372225181948,-32.3131764290349,
7.90000424507512));
#31945=CARTESIAN_POINT('Ctrl Pts',(-34.6550080066264,-30.6541747995416,
7.74300411772286));
#31946=CARTESIAN_POINT('Ctrl Pts',(-31.184979362873,-32.8887836563341,7.58600399037061));
#31947=CARTESIAN_POINT('Ctrl Pts',(-31.1345143009551,-37.0181861134745,
7.42900386301835));
#31948=CARTESIAN_POINT('Ctrl Pts',(-34.5509631428814,-39.3370454001755,
7.2720037356661));
#31949=CARTESIAN_POINT('Ctrl Pts',(-38.3697222748781,-37.7672396329946,
7.11500360831385));
#31950=CARTESIAN_POINT('Ctrl Pts',(-39.1669905477644,-33.7158224271125,
6.95800348096159));
#31951=CARTESIAN_POINT('Ctrl Pts',(-36.2275933248156,-30.8160393982482,
6.80100335360935));
#31952=CARTESIAN_POINT('Ctrl Pts',(-32.187443630028,-31.6680044278098,6.64400322625708));
#31953=CARTESIAN_POINT('Ctrl Pts',(-30.6693192478399,-35.5078264493611,
6.48700309890484));
#31954=CARTESIAN_POINT('Ctrl Pts',(-33.0345682502559,-38.8922634126314,
6.33000297155257));
#31955=CARTESIAN_POINT('Ctrl Pts',(-37.1622335921182,-38.7864764935337,
6.17300284420033));
#31956=CARTESIAN_POINT('Ctrl Pts',(-39.3510058927144,-35.2853167686088,
6.01600271684807));
#31957=CARTESIAN_POINT('Ctrl Pts',(-37.6381881947812,-31.5283122533059,
5.85900258949583));
#31958=CARTESIAN_POINT('Ctrl Pts',(-33.5596824647827,-30.8844027051158,
5.70200246214357));
#31959=CARTESIAN_POINT('Ctrl Pts',(-30.7727229727691,-33.9309891024229,
5.54500233479131));
#31960=CARTESIAN_POINT('Ctrl Pts',(-31.7764035014098,-37.9361676445846,
5.38800220743907));
#31961=CARTESIAN_POINT('Ctrl Pts',(-35.6707138588461,-39.3084565821841,
5.2310020800868));
#31962=CARTESIAN_POINT('Ctrl Pts',(-38.9635887028751,-36.8173111240784,
5.07400195273455));
#31963=CARTESIAN_POINT('Ctrl Pts',(-38.7022755130482,-32.6965653688576,
4.9170018253823));
#31964=CARTESIAN_POINT('Ctrl Pts',(-35.1210963620983,-30.6413315344396,
4.76000169803004));
#31965=CARTESIAN_POINT('Ctrl Pts',(-31.431328936819,-32.4945575337781,4.6030015706778));
#31966=CARTESIAN_POINT('Ctrl Pts',(-30.9416230925,-36.5944378259461,4.44600144332554));
#31967=CARTESIAN_POINT('Ctrl Pts',(-34.0911027542909,-39.2645704246538,
4.28900131597328));
#31968=CARTESIAN_POINT('Ctrl Pts',(-38.0555992964371,-38.1106218103576,
4.13200118862104));
#31969=CARTESIAN_POINT('Ctrl Pts',(-39.2801106351136,-34.1673487773102,
3.97500106126878));
#31970=CARTESIAN_POINT('Ctrl Pts',(-36.6666057058575,-30.9707220831404,
3.81800093391653));
#31971=CARTESIAN_POINT('Ctrl Pts',(-32.5586394514893,-31.3871875531226,
3.66100080656427));
#31972=CARTESIAN_POINT('Ctrl Pts',(-30.6398646221734,-35.0432966021599,
3.50400067921202));
#31973=CARTESIAN_POINT('Ctrl Pts',(-32.6308650157539,-38.6605811762622,
3.34700055185977));
#31974=CARTESIAN_POINT('Ctrl Pts',(-36.7462914774195,-38.9953874843817,
3.19000042450751));
#31975=CARTESIAN_POINT('Ctrl Pts',(-39.2958016196254,-35.7474915197397,
3.03300029715526));
#31976=CARTESIAN_POINT('Ctrl Pts',(-37.9932252344219,-31.8293127090433,
2.876000169803));
#31977=CARTESIAN_POINT('Ctrl Pts',(-34.0065950719303,-30.754319669156,2.71900004245075));
#31978=CARTESIAN_POINT('Ctrl Pts',(-30.910760626402,-33.4864687946697,2.5619999150985));
#31979=CARTESIAN_POINT('Ctrl Pts',(-31.4817863824102,-37.5758161108508,
2.40499978774625));
#31980=CARTESIAN_POINT('Ctrl Pts',(-35.2076279914714,-39.3554039283154,
2.24799966039399));
#31981=CARTESIAN_POINT('Ctrl Pts',(-38.7472876895237,-37.2294602281335,
2.09099953304174));
#31982=CARTESIAN_POINT('Ctrl Pts',(-38.9267183633859,-33.1043362013228,
1.93399940568948));
#31983=CARTESIAN_POINT('Ctrl Pts',(-35.5850234188216,-30.6790760206131,
1.77699927833723));
#31984=CARTESIAN_POINT('Ctrl Pts',(-31.7187315376645,-32.128421904617,1.61999915098498));
#31985=CARTESIAN_POINT('Ctrl Pts',(-30.7947862267274,-36.1527553723333,
1.46299902363272));
#31986=CARTESIAN_POINT('Ctrl Pts',(-33.6416931030839,-39.1433698920001,
1.30599889628047));
#31987=CARTESIAN_POINT('Ctrl Pts',(-37.7066135461226,-38.4186496421557,
1.14899876892822));
#31988=CARTESIAN_POINT('Ctrl Pts',(-39.3444740755065,-34.628262991515,0.991998641575964));
#31989=CARTESIAN_POINT('Ctrl Pts',(-37.0866303819407,-31.1714793259802,
0.83499851422371));
#31990=CARTESIAN_POINT('Ctrl Pts',(-32.9576300903856,-31.1472373508815,
0.677998386871457));
#31991=CARTESIAN_POINT('Ctrl Pts',(-30.6601534973185,-34.5788714630532,
0.520998259519203));
#31992=CARTESIAN_POINT('Ctrl Pts',(-32.2540356527884,-38.3859852262338,
0.363998132166951));
#31993=CARTESIAN_POINT('Ctrl Pts',(-36.3106933795422,-39.1612020385825,
0.206998004814695));
#31994=CARTESIAN_POINT('Ctrl Pts',(-39.1911999412976,-36.1960803455747,
0.049997877462444));
#31995=CARTESIAN_POINT('Ctrl Pts',(-38.6056283266121,-33.5191597390956,
-0.0546688741057268));
#31996=CARTESIAN_POINT('Ctrl Pts',(-37.8143974874483,-32.5937287191406,
-0.107002249889811));
#31997=CARTESIAN_POINT('Ctrl Pts',(-35.9084720925035,-38.3981590173419,
8.32100674966943));
#31998=CARTESIAN_POINT('Ctrl Pts',(-37.0258557525633,-38.0994349533404,
8.26867337388535));
#31999=CARTESIAN_POINT('Ctrl Pts',(-38.9246974524274,-36.318886728109,8.16400662231718));
#32000=CARTESIAN_POINT('Ctrl Pts',(-38.265183474209,-32.4476566833857,8.00700649496493));
#32001=CARTESIAN_POINT('Ctrl Pts',(-34.6722754638272,-30.8716910088818,
7.85000636761267));
#32002=CARTESIAN_POINT('Ctrl Pts',(-31.3759278684536,-32.9944537546442,
7.69300624026043));
#32003=CARTESIAN_POINT('Ctrl Pts',(-31.3279886718125,-36.9171723421199,
7.53600611290816));
#32004=CARTESIAN_POINT('Ctrl Pts',(-34.5734382288568,-39.119968635311,7.37900598555592));
#32005=CARTESIAN_POINT('Ctrl Pts',(-38.2010617370167,-37.6287344130329,
7.22200585820366));
#32006=CARTESIAN_POINT('Ctrl Pts',(-38.9584253279276,-33.7800977775671,
7.0650057308514));
#32007=CARTESIAN_POINT('Ctrl Pts',(-36.1661501156877,-31.0254539991911,
6.90800560349916));
#32008=CARTESIAN_POINT('Ctrl Pts',(-32.328217032531,-31.834776677721,6.75100547614689));
#32009=CARTESIAN_POINT('Ctrl Pts',(-30.8860774508557,-35.482408840697,6.59400534879465));
#32010=CARTESIAN_POINT('Ctrl Pts',(-33.1329415727439,-38.6974487700223,
6.43700522144238));
#32011=CARTESIAN_POINT('Ctrl Pts',(-37.0540099906223,-38.5969566726394,
6.28000509409015));
#32012=CARTESIAN_POINT('Ctrl Pts',(-39.1332303805976,-35.271036161565,6.12300496673788));
#32013=CARTESIAN_POINT('Ctrl Pts',(-37.5061422267118,-31.7020763427115,
5.96600483938563));
#32014=CARTESIAN_POINT('Ctrl Pts',(-33.6317728954962,-31.0903956020826,
5.80900471203338));
#32015=CARTESIAN_POINT('Ctrl Pts',(-30.9843056371378,-33.9844949816193,
5.65200458468112));
#32016=CARTESIAN_POINT('Ctrl Pts',(-31.9377501866703,-37.7892072799639,
5.49500445732888));
#32017=CARTESIAN_POINT('Ctrl Pts',(-35.6371434483029,-39.0928107380382,
5.33800432997661));
#32018=CARTESIAN_POINT('Ctrl Pts',(-38.7652041038025,-36.7263514999179,
5.18100420262437));
#32019=CARTESIAN_POINT('Ctrl Pts',(-38.5169700996031,-32.8118563311761,
5.02400407527211));
#32020=CARTESIAN_POINT('Ctrl Pts',(-35.1150352757837,-30.85949057183,4.86700394791986));
#32021=CARTESIAN_POINT('Ctrl Pts',(-31.6099472121153,-32.6199593442133,
4.7100038205676));
#32022=CARTESIAN_POINT('Ctrl Pts',(-31.1447520082465,-36.5146334030964,
4.55300369321535));
#32023=CARTESIAN_POINT('Ctrl Pts',(-34.1365946630648,-39.0511211600269,
4.3960035658631));
#32024=CARTESIAN_POINT('Ctrl Pts',(-37.902661167183,-37.9549297073231,4.23900343851084));
#32025=CARTESIAN_POINT('Ctrl Pts',(-39.0658835555688,-34.2090244382739,
4.08200331115859));
#32026=CARTESIAN_POINT('Ctrl Pts',(-36.5831891534466,-31.1723945431281,
3.92500318380633));
#32027=CARTESIAN_POINT('Ctrl Pts',(-32.6808338490201,-31.5680151824572,
3.76800305645409));
#32028=CARTESIAN_POINT('Ctrl Pts',(-30.8580970811077,-35.041129530926,3.61100292910183));
#32029=CARTESIAN_POINT('Ctrl Pts',(-32.74944439652,-38.4773626378456,3.45400280174958));
#32030=CARTESIAN_POINT('Ctrl Pts',(-36.6588865117225,-38.79541130026,3.29700267439732));
#32031=CARTESIAN_POINT('Ctrl Pts',(-39.0807891786557,-35.710078251974,3.14000254704507));
#32032=CARTESIAN_POINT('Ctrl Pts',(-37.8434090368849,-31.988011195227,2.98300241969281));
#32033=CARTESIAN_POINT('Ctrl Pts',(-34.0563167391228,-30.9668234513003,
2.82600229234056));
#32034=CARTESIAN_POINT('Ctrl Pts',(-31.1154342629614,-33.5622236985868,
2.66900216498831));
#32035=CARTESIAN_POINT('Ctrl Pts',(-31.6578791736403,-37.446891975492,2.51200203763606));
#32036=CARTESIAN_POINT('Ctrl Pts',(-35.1972358446236,-39.1374082867668,
2.3550019102838));
#32037=CARTESIAN_POINT('Ctrl Pts',(-38.5597293373271,-37.1178718150406,
2.19800178293155));
#32038=CARTESIAN_POINT('Ctrl Pts',(-38.7301791897763,-33.1992175149173,
2.04100165557929));
#32039=CARTESIAN_POINT('Ctrl Pts',(-35.5557419658023,-30.8953458799586,
1.88400152822704));
#32040=CARTESIAN_POINT('Ctrl Pts',(-31.8829648063379,-32.2721494484828,
1.72700140087479));
#32041=CARTESIAN_POINT('Ctrl Pts',(-31.0052645863564,-36.0950579346039,
1.57000127352254));
#32042=CARTESIAN_POINT('Ctrl Pts',(-33.7096787568343,-38.9359869276078,
1.41300114617028));
#32043=CARTESIAN_POINT('Ctrl Pts',(-37.5711427686419,-38.247540203344,1.25600101881803));
#32044=CARTESIAN_POINT('Ctrl Pts',(-39.1270254923511,-34.6468690838513,
1.09900089146578));
#32045=CARTESIAN_POINT('Ctrl Pts',(-36.9821908543394,-31.3631035321966,
0.94200076411352));
#32046=CARTESIAN_POINT('Ctrl Pts',(-33.0598543033527,-31.3400749106699,
0.785000636761268));
#32047=CARTESIAN_POINT('Ctrl Pts',(-30.8773704622995,-34.599949688425,0.628000509409013));
#32048=CARTESIAN_POINT('Ctrl Pts',(-32.3914760072062,-38.2165106989991,
0.471000382056762));
#32049=CARTESIAN_POINT('Ctrl Pts',(-36.2450908662393,-38.9529265438306,
0.314000254704506));
#32050=CARTESIAN_POINT('Ctrl Pts',(-38.9814229986536,-36.1362144165888,
0.157000127352255));
#32051=CARTESIAN_POINT('Ctrl Pts',(-38.4251602751564,-33.5932784036374,
0.0523333757840841));
#32052=CARTESIAN_POINT('Ctrl Pts',(-37.6735319337713,-32.7141668369925,
0.));
#32053=CARTESIAN_POINT('Ctrl Pts',(-37.6735319337713,-32.7141668369925,
0.));
#32054=CARTESIAN_POINT('Ctrl Pts',(-37.7506744675535,-32.7912795750214,
1.11409720010452E-16));
#32055=CARTESIAN_POINT('Ctrl Pts',(-37.8237046409441,-32.8720144826054,
2.54111086902063E-16));
#32056=CARTESIAN_POINT('Ctrl Pts',(-37.8926301480271,-32.9559530569886,
5.55111512312578E-17));
#32057=CARTESIAN_POINT('Ctrl Pts',(-37.9633155600031,-33.0420348714294,
-1.48159722809431E-16));
#32058=CARTESIAN_POINT('Ctrl Pts',(-38.0296843928246,-33.1314864952968,
-2.01877327443104E-15));
#32059=CARTESIAN_POINT('Ctrl Pts',(-38.0917150717573,-33.2239026806474,
-1.83186799063151E-15));
#32060=CARTESIAN_POINT('Ctrl Pts',(-38.155036796301,-33.318242325688,-1.64107264387499E-15));
#32061=CARTESIAN_POINT('Ctrl Pts',(-38.2138383235334,-33.4156718046105,
-8.85373385211783E-16));
#32062=CARTESIAN_POINT('Ctrl Pts',(-38.268059911681,-33.515799485594,-9.43689570931383E-16));
#32063=CARTESIAN_POINT('Ctrl Pts',(-38.319849146258,-33.6114354884346,-9.99389721462685E-16));
#32064=CARTESIAN_POINT('Ctrl Pts',(-38.3674601237765,-33.7095338759835,
-7.11957983305256E-16));
#32065=CARTESIAN_POINT('Ctrl Pts',(-38.4108052730721,-33.809777999414,-7.21644966006352E-16));
#32066=CARTESIAN_POINT('Ctrl Pts',(-38.4178427440334,-33.8260535254913,
-7.23217733907022E-16));
#32067=CARTESIAN_POINT('Ctrl Pts',(-38.4247676868796,-33.8423856539009,
2.30001299369943E-15));
#32068=CARTESIAN_POINT('Ctrl Pts',(-38.4315796332288,-33.8587730721181,
2.33146835171283E-15));
#32069=CARTESIAN_POINT('Ctrl Pts',(-38.4380896782009,-33.8744342097871,
2.3615296271221E-15));
#32070=CARTESIAN_POINT('Ctrl Pts',(-38.4444935030833,-33.8901386536763,
1.24943603957411E-15));
#32071=CARTESIAN_POINT('Ctrl Pts',(-38.4507888941826,-33.9058797515619,
1.16573417585641E-15));
#32072=CARTESIAN_POINT('Ctrl Pts',(-38.4941742238636,-34.0143611327099,
5.88894247237743E-16));
#32073=CARTESIAN_POINT('Ctrl Pts',(-38.5324456986686,-34.1246595013341,
-1.81750747552515E-15));
#32074=CARTESIAN_POINT('Ctrl Pts',(-38.5655747031801,-34.2363430523647,
-1.22124532708767E-15));
#32075=CARTESIAN_POINT('Ctrl Pts',(-38.5991382485882,-34.3494915152183,
-6.17162228628305E-16));
#32076=CARTESIAN_POINT('Ctrl Pts',(-38.6274239303319,-34.4640624881056,
-2.28097715513866E-15));
#32077=CARTESIAN_POINT('Ctrl Pts',(-38.6503593525615,-34.5796394751672,
-2.85882428840978E-15));
#32078=CARTESIAN_POINT('Ctrl Pts',(-38.6743343050071,-34.7004548994865,
-3.46286189462104E-15));
#32079=CARTESIAN_POINT('Ctrl Pts',(-38.6924637958468,-34.8223704157046,
7.50012201101083E-16));
#32080=CARTESIAN_POINT('Ctrl Pts',(-38.7046094044796,-34.9449336658503,
9.15933995315754E-16));
#32081=CARTESIAN_POINT('Ctrl Pts',(-38.7137186109542,-35.0368561034595,
1.04037534097676E-15));
#32082=CARTESIAN_POINT('Ctrl Pts',(-38.7194607604909,-35.1291434881023,
1.55226768069038E-15));
#32083=CARTESIAN_POINT('Ctrl Pts',(-38.7217543278029,-35.2216084347256,
1.52655665885959E-15));
#32084=CARTESIAN_POINT('Ctrl Pts',(-38.7223018974601,-35.2436836530358,
1.52041837142613E-15));
#32085=CARTESIAN_POINT('Ctrl Pts',(-38.7226527519925,-35.2657735186889,
2.89381252678048E-15));
#32086=CARTESIAN_POINT('Ctrl Pts',(-38.722805679631,-35.2878464184275,2.85882428840978E-15));
#32087=CARTESIAN_POINT('Ctrl Pts',(-38.7236405005601,-35.4083407832928,
2.66782602310891E-15));
#32088=CARTESIAN_POINT('Ctrl Pts',(-38.7185871650491,-35.5284803305467,
-1.0113839359997E-15));
#32089=CARTESIAN_POINT('Ctrl Pts',(-38.7075767134548,-35.6478390239293,
-6.10622663543836E-16));
#32090=CARTESIAN_POINT('Ctrl Pts',(-38.696636914708,-35.766431805807,-2.12433031749896E-16));
#32091=CARTESIAN_POINT('Ctrl Pts',(-38.6798164549903,-35.8842545994116,
4.47017550934916E-16));
#32092=CARTESIAN_POINT('Ctrl Pts',(-38.6569982586142,-36.0009023628565,
1.11022302462516E-15));
#32093=CARTESIAN_POINT('Ctrl Pts',(-38.6541246129484,-36.0155925835174,
1.19374485534308E-15));
#32094=CARTESIAN_POINT('Ctrl Pts',(-38.6511557754508,-36.0302641749016,
1.91345521755541E-15));
#32095=CARTESIAN_POINT('Ctrl Pts',(-38.6480914530901,-36.044916331709,1.97064586870965E-15));
#32096=CARTESIAN_POINT('Ctrl Pts',(-38.6241809707793,-36.1592450787926,
2.44399783547239E-15));
#32097=CARTESIAN_POINT('Ctrl Pts',(-38.594461283178,-36.2723911010901,-8.48644965904397E-16));
#32098=CARTESIAN_POINT('Ctrl Pts',(-38.5592385353076,-36.3840879064664,
-8.60422844084496E-16));
#32099=CARTESIAN_POINT('Ctrl Pts',(-38.5372732895732,-36.4537431130068,
-8.67767642662035E-16));
#32100=CARTESIAN_POINT('Ctrl Pts',(-38.5131668858195,-36.5228346461715,
9.22437028861002E-17));
#32101=CARTESIAN_POINT('Ctrl Pts',(-38.4869837165243,-36.5912956919754,
8.32667268468867E-17));
#32102=CARTESIAN_POINT('Ctrl Pts',(-38.4780341824549,-36.6146960089858,
8.01983529614736E-17));
#32103=CARTESIAN_POINT('Ctrl Pts',(-38.4688419572729,-36.6380226459113,
-1.61456985271483E-15));
#32104=CARTESIAN_POINT('Ctrl Pts',(-38.4594094252689,-36.6612728659742,
-1.77635683940025E-15));
#32105=CARTESIAN_POINT('Ctrl Pts',(-38.4526602969819,-36.6779087722017,
-1.89211802927477E-15));
#32106=CARTESIAN_POINT('Ctrl Pts',(-38.4457875924452,-36.6945066762169,
2.33562128204704E-15));
#32107=CARTESIAN_POINT('Ctrl Pts',(-38.4387992548886,-36.7110492733397,
2.24820162486594E-15));
#32108=CARTESIAN_POINT('Ctrl Pts',(-38.3928779298073,-36.8197529491441,
1.67375506108868E-15));
#32109=CARTESIAN_POINT('Ctrl Pts',(-38.341903576542,-36.9262302239648,1.3366443388947E-15));
#32110=CARTESIAN_POINT('Ctrl Pts',(-38.2862346344182,-37.0302267509451,
1.30451205393456E-15));
#32111=CARTESIAN_POINT('Ctrl Pts',(-38.2286504882323,-37.1378011179799,
1.2712743072873E-15));
#32112=CARTESIAN_POINT('Ctrl Pts',(-38.1660430056126,-37.2427217973211,
4.33181580130382E-15));
#32113=CARTESIAN_POINT('Ctrl Pts',(-38.098753525921,-37.3446999432836,3.3584246494911E-15));
#32114=CARTESIAN_POINT('Ctrl Pts',(-38.030830880622,-37.4476376605642,2.37587429771653E-15));
#32115=CARTESIAN_POINT('Ctrl Pts',(-37.9581372777995,-37.5475779522675,
-1.61807423508707E-16));
#32116=CARTESIAN_POINT('Ctrl Pts',(-37.8809732699071,-37.6442054678576,
-4.30211422042248E-16));
#32117=CARTESIAN_POINT('Ctrl Pts',(-37.826560213076,-37.7123434332233,-6.19479481397997E-16));
#32118=CARTESIAN_POINT('Ctrl Pts',(-37.769923167717,-37.7788337520814,-1.16007728999665E-15));
#32119=CARTESIAN_POINT('Ctrl Pts',(-37.7111544669349,-37.8435573649047,
-1.58206781009085E-15));
#32120=CARTESIAN_POINT('Ctrl Pts',(-37.6849217834628,-37.8724481524459,
-1.77043242585642E-15));
#32121=CARTESIAN_POINT('Ctrl Pts',(-37.6582642395734,-37.9009868195143,
-1.55320898075906E-15));
#32122=CARTESIAN_POINT('Ctrl Pts',(-37.6311894369306,-37.9291622039588,
-1.76247905159244E-15));
#32123=CARTESIAN_POINT('Ctrl Pts',(-37.6195672281553,-37.9412568516894,
-1.85231093276087E-15));
#32124=CARTESIAN_POINT('Ctrl Pts',(-37.6078695516101,-37.9532830190668,
-1.32384934798458E-15));
#32125=CARTESIAN_POINT('Ctrl Pts',(-37.5961035133295,-37.9652334405448,
-1.346145417358E-15));
#32126=CARTESIAN_POINT('Ctrl Pts',(-37.5076612499423,-38.0550616646887,
-1.51373919811968E-15));
#32127=CARTESIAN_POINT('Ctrl Pts',(-37.4152596553304,-38.1407172584711,
9.39449970766038E-16));
#32128=CARTESIAN_POINT('Ctrl Pts',(-37.3192274679083,-38.221882071393,-9.29811783123569E-16));
#32129=CARTESIAN_POINT('Ctrl Pts',(-37.2371876089162,-38.2912208002711,
-2.52671355975721E-15));
#32130=CARTESIAN_POINT('Ctrl Pts',(-37.1524970590086,-38.3572819982496,
-3.43309726072543E-16));
#32131=CARTESIAN_POINT('Ctrl Pts',(-37.0653365594432,-38.419849736978,-1.11022302462516E-16));
#32132=CARTESIAN_POINT('Ctrl Pts',(-37.0262256852631,-38.4479252869043,
-6.78971724635936E-18));
#32133=CARTESIAN_POINT('Ctrl Pts',(-36.9866172085179,-38.4752971710175,
-3.75915299087743E-16));
#32134=CARTESIAN_POINT('Ctrl Pts',(-36.9465262167991,-38.5019445229708,
-5.06539254985228E-16));
#32135=CARTESIAN_POINT('Ctrl Pts',(-36.9192926653871,-38.5200458968282,
-5.95271263500483E-16));
#32136=CARTESIAN_POINT('Ctrl Pts',(-36.8918308185162,-38.5378163160328,
-1.49578843933597E-15));
#32137=CARTESIAN_POINT('Ctrl Pts',(-36.8641753660581,-38.555230466303,-1.48492329543615E-15));
#32138=CARTESIAN_POINT('Ctrl Pts',(-36.7573710739483,-38.6224832438564,
-1.44296252821847E-15));
#32139=CARTESIAN_POINT('Ctrl Pts',(-36.6476200524945,-38.6844692154967,
-2.67652767243929E-15));
#32140=CARTESIAN_POINT('Ctrl Pts',(-36.5352242775472,-38.7408547238633,
-3.18495230189342E-15));
#32141=CARTESIAN_POINT('Ctrl Pts',(-36.4331305324386,-38.792072020258,-3.64677548475584E-15));
#32142=CARTESIAN_POINT('Ctrl Pts',(-36.3288538528326,-38.8386685011131,
8.48923205726707E-17));
#32143=CARTESIAN_POINT('Ctrl Pts',(-36.2225972039516,-38.8803649981066,
1.52308721190764E-15));
#32144=CARTESIAN_POINT('Ctrl Pts',(-36.1671666977136,-38.9021166528128,
2.30316661476457E-15));
#32145=CARTESIAN_POINT('Ctrl Pts',(-36.1111970366882,-38.922534339231,-1.9802954995054E-18));
#32146=CARTESIAN_POINT('Ctrl Pts',(-36.0547323436802,-38.9416301693299,
1.11022302462516E-16));
#32147=CARTESIAN_POINT('Ctrl Pts',(-38.5153122961063,-34.9971887940747,
7.11258330249198));
#32148=CARTESIAN_POINT('Ctrl Pts',(-38.5180434423612,-34.646197163443,7.09672411194512));
#32149=CARTESIAN_POINT('Ctrl Pts',(-38.4695960103246,-34.2959413770096,
7.08086492139826));
#32150=CARTESIAN_POINT('Ctrl Pts',(-38.3668188607358,-33.9624299204154,
7.0650057308514));
#32151=CARTESIAN_POINT('Ctrl Pts',(-38.0276669238477,-32.8618831847751,
7.01267235506732));
#32152=CARTESIAN_POINT('Ctrl Pts',(-37.0969085197677,-31.9436685919831,
6.96033897928324));
#32153=CARTESIAN_POINT('Ctrl Pts',(-35.9918738038683,-31.6194484086754,
6.90800560349915));
#32154=CARTESIAN_POINT('Ctrl Pts',(-34.8868390879688,-31.2952282253677,
6.85567222771507));
#32155=CARTESIAN_POINT('Ctrl Pts',(-33.6075280602499,-31.5650024515443,
6.80333885193098));
#32156=CARTESIAN_POINT('Ctrl Pts',(-32.7275159494446,-32.307828258462,6.75100547614689));
#32157=CARTESIAN_POINT('Ctrl Pts',(-31.8475038386392,-33.0506540653796,
6.69867210036281));
#32158=CARTESIAN_POINT('Ctrl Pts',(-31.3667906447475,-34.2665314530383,
6.64633872457873));
#32159=CARTESIAN_POINT('Ctrl Pts',(-31.5009114014496,-35.4103101350885,
6.59400534879465));
#32160=CARTESIAN_POINT('Ctrl Pts',(-31.6350321581518,-36.5540888171387,
6.54167197301056));
#32161=CARTESIAN_POINT('Ctrl Pts',(-32.3839868654478,-37.6257687935805,
6.48933859722647));
#32162=CARTESIAN_POINT('Ctrl Pts',(-33.4119756220756,-38.1448600989042,
6.43700522144239));
#32163=CARTESIAN_POINT('Ctrl Pts',(-34.4399643787034,-38.663951404228,6.3846718456583));
#32164=CARTESIAN_POINT('Ctrl Pts',(-35.7469871846628,-38.6304540384337,
6.33233846987422));
#32165=CARTESIAN_POINT('Ctrl Pts',(-36.7470353193051,-38.0593852703575,
6.28000509409014));
#32166=CARTESIAN_POINT('Ctrl Pts',(-37.7470834539474,-37.4883165022812,
6.22767171830606));
#32167=CARTESIAN_POINT('Ctrl Pts',(-38.4401569172725,-36.3796763319231,
6.17533834252197));
#32168=CARTESIAN_POINT('Ctrl Pts',(-38.5155122899541,-35.2305296102685,
6.12300496673788));
#32169=CARTESIAN_POINT('Ctrl Pts',(-38.5205143775731,-35.1542492816832,
6.11953107865591));
#32170=CARTESIAN_POINT('Ctrl Pts',(-38.5227946134492,-35.0777904690468,
6.11605719057395));
#32171=CARTESIAN_POINT('Ctrl Pts',(-38.522424122767,-35.0013091826171,6.11258330249198));
#32172=CARTESIAN_POINT('Origin',(35.,-35.,10.2084234471775));
#32173=CARTESIAN_POINT('Ctrl Pts',(30.9215903995924,-34.9979557257256,7.70842344717745));
#32174=CARTESIAN_POINT('Ctrl Pts',(30.9207462976534,-34.8668874511107,7.70328437820511));
#32175=CARTESIAN_POINT('Ctrl Pts',(30.9854756915705,-33.4019022214529,7.64581193344868));
#32176=CARTESIAN_POINT('Ctrl Pts',(32.753181490405,-30.7615622140283,7.53600611290817));
#32177=CARTESIAN_POINT('Ctrl Pts',(37.2955095733766,-30.7882306349807,7.3790059855559));
#32178=CARTESIAN_POINT('Ctrl Pts',(39.7793714317054,-34.5910508431566,7.22200585820367));
#32179=CARTESIAN_POINT('Ctrl Pts',(37.9775552386376,-38.7608686529102,7.0650057308514));
#32180=CARTESIAN_POINT('Ctrl Pts',(33.5057217267653,-39.5581360350982,6.90800560349915));
#32181=CARTESIAN_POINT('Ctrl Pts',(31.1346464724166,-37.067372389099,6.7891448422745));
#32182=CARTESIAN_POINT('Ctrl Pts',(30.9248236399074,-35.3669839150134,6.72261745683393));
#32183=CARTESIAN_POINT('Ctrl Pts',(30.9278856911952,-35.003454802609,6.70842344717745));
#32184=CARTESIAN_POINT('Ctrl Pts',(30.9308748007386,-35.0040807474719,7.79157655282254));
#32185=CARTESIAN_POINT('Ctrl Pts',(30.9370382125719,-34.10157834971,7.75638428364686));
#32186=CARTESIAN_POINT('Ctrl Pts',(31.6729756008745,-31.8449525580975,7.66885863868709));
#32187=CARTESIAN_POINT('Ctrl Pts',(35.3795267558193,-30.2191465582126,7.52899961794324));
#32188=CARTESIAN_POINT('Ctrl Pts',(39.1969165266342,-32.6774422642514,7.37199949059099));
#32189=CARTESIAN_POINT('Ctrl Pts',(39.2524336251343,-37.2202141105436,7.21499936323873));
#32190=CARTESIAN_POINT('Ctrl Pts',(35.4939867861423,-39.7711972931265,7.05799923588648));
#32191=CARTESIAN_POINT('Ctrl Pts',(31.7173198121032,-38.2186953257486,6.91685829908109));
#32192=CARTESIAN_POINT('Ctrl Pts',(30.9363086272988,-35.9315792701304,6.82805073805977));
#32193=CARTESIAN_POINT('Ctrl Pts',(30.9290344477858,-34.9967444478932,6.79157655282255));
#32194=CARTESIAN_POINT('Ctrl Pts',(37.6735319337713,-32.7141668369925,8.));
#32195=CARTESIAN_POINT('Ctrl Pts',(38.4251602751564,-33.5932784036374,7.94766662421592));
#32196=CARTESIAN_POINT('Ctrl Pts',(38.9814215765655,-36.1362159265307,7.84299987264775));
#32197=CARTESIAN_POINT('Ctrl Pts',(36.2450915261219,-38.9529260673994,7.6859997452955));
#32198=CARTESIAN_POINT('Ctrl Pts',(32.3914756047223,-38.2165112413961,7.52899961794324));
#32199=CARTESIAN_POINT('Ctrl Pts',(30.8773704214612,-34.5999494268526,7.37199949059098));
#32200=CARTESIAN_POINT('Ctrl Pts',(33.0598541530624,-31.3400748957517,7.21499936323873));
#32201=CARTESIAN_POINT('Ctrl Pts',(36.9821909719779,-31.3631032916521,7.05799923588648));
#32202=CARTESIAN_POINT('Ctrl Pts',(39.127025656321,-34.6468691152089,6.90099910853422));
#32203=CARTESIAN_POINT('Ctrl Pts',(37.5711428874206,-38.2475403183041,6.74399898118197));
#32204=CARTESIAN_POINT('Ctrl Pts',(33.7096786974094,-38.9359871126692,6.58699885382972));
#32205=CARTESIAN_POINT('Ctrl Pts',(31.005264414648,-36.0950579743517,6.42999872647747));
#32206=CARTESIAN_POINT('Ctrl Pts',(31.8829646703068,-32.272149334312,6.27299859912521));
#32207=CARTESIAN_POINT('Ctrl Pts',(35.5557419902844,-30.8953456995945,6.11599847177296));
#32208=CARTESIAN_POINT('Ctrl Pts',(38.7301793514647,-33.1992174379789,5.9589983444207));
#32209=CARTESIAN_POINT('Ctrl Pts',(38.5597294918745,-37.1178719063019,5.80199821706845));
#32210=CARTESIAN_POINT('Ctrl Pts',(35.1972358531438,-39.137408466637,5.6449980897162));
#32211=CARTESIAN_POINT('Ctrl Pts',(31.6578790286353,-37.4468920814909,5.48799796236395));
#32212=CARTESIAN_POINT('Ctrl Pts',(31.115434094392,-33.5622236362915,5.33099783501169));
#32213=CARTESIAN_POINT('Ctrl Pts',(34.0563166981778,-30.9668232762417,5.17399770765944));
#32214=CARTESIAN_POINT('Ctrl Pts',(37.8434091602659,-31.9880110645548,5.01699758030718));
#32215=CARTESIAN_POINT('Ctrl Pts',(39.0807893557322,-35.7100782827727,4.85999745295493));
#32216=CARTESIAN_POINT('Ctrl Pts',(36.6588865837055,-38.7954114649594,4.70299732560268));
#32217=CARTESIAN_POINT('Ctrl Pts',(32.7494442988629,-38.4773627887335,4.54599719825042));
#32218=CARTESIAN_POINT('Ctrl Pts',(30.8580969013801,-35.0411295327127,4.38899707089817));
#32219=CARTESIAN_POINT('Ctrl Pts',(32.6808337483856,-31.5680150335338,4.23199694354591));
#32220=CARTESIAN_POINT('Ctrl Pts',(36.5831892221451,-31.1723943770392,4.07499681619367));
#32221=CARTESIAN_POINT('Ctrl Pts',(39.0658837319978,-34.2090244039511,3.91799668884141));
#32222=CARTESIAN_POINT('Ctrl Pts',(37.9026612931367,-37.9549298355453,3.76099656148916));
#32223=CARTESIAN_POINT('Ctrl Pts',(34.1365946255998,-39.0511213358148,3.6039964341369));
#32224=CARTESIAN_POINT('Ctrl Pts',(31.144751840957,-36.5146334688211,3.44699630678465));
#32225=CARTESIAN_POINT('Ctrl Pts',(31.6099470650134,-32.6199592409358,3.2899961794324));
#32226=CARTESIAN_POINT('Ctrl Pts',(35.1150352807734,-30.8594903921659,3.13299605208014));
#32227=CARTESIAN_POINT('Ctrl Pts',(38.5169702522169,-32.811856236221,2.97599592472789));
#32228=CARTESIAN_POINT('Ctrl Pts',(38.7652042671773,-36.72635157484,2.81899579737563));
#32229=CARTESIAN_POINT('Ctrl Pts',(35.6371434759633,-39.0928109156136,2.66199567002339));
#32230=CARTESIAN_POINT('Ctrl Pts',(31.9377500537671,-37.7892074010372,2.50499554267113));
#32231=CARTESIAN_POINT('Ctrl Pts',(30.9843054629328,-33.9844949374723,2.34799541531888));
#32232=CARTESIAN_POINT('Ctrl Pts',(33.6317728360394,-31.0903954325918,2.19099528796662));
#32233=CARTESIAN_POINT('Ctrl Pts',(37.5061423356192,-31.7020761993063,2.03399516061437));
#32234=CARTESIAN_POINT('Ctrl Pts',(39.1332305596546,-35.2710361738983,1.87699503326212));
#32235=CARTESIAN_POINT('Ctrl Pts',(37.054010080289,-38.5969568276314,1.71999490590986));
#32236=CARTESIAN_POINT('Ctrl Pts',(33.1329414907541,-38.6974489325283,1.56299477855761));
#32237=CARTESIAN_POINT('Ctrl Pts',(30.8860772740811,-35.4824088577318,1.40599465120536));
#32238=CARTESIAN_POINT('Ctrl Pts',(32.3282169135405,-31.8347765477019,1.2489945238531));
#32239=CARTESIAN_POINT('Ctrl Pts',(36.1661501715419,-31.025453813021,1.09199439650085));
#32240=CARTESIAN_POINT('Ctrl Pts',(38.9584254909315,-33.7800977501094,0.934994269148596));
#32241=CARTESIAN_POINT('Ctrl Pts',(38.201061889907,-37.6287344800703,0.777994141796343));
#32242=CARTESIAN_POINT('Ctrl Pts',(34.5734381895487,-39.1199689001796,0.620994014444089));
#32243=CARTESIAN_POINT('Ctrl Pts',(31.3279885395076,-36.9171722692834,0.463993887091836));
#32244=CARTESIAN_POINT('Ctrl Pts',(31.3759276866332,-32.994453947074,0.306993759739581));
#32245=CARTESIAN_POINT('Ctrl Pts',(34.6722754393756,-30.8716903339078,0.149993632387328));
#32246=CARTESIAN_POINT('Ctrl Pts',(38.2651837481491,-32.4476574497985,-0.00700649496492499));
#32247=CARTESIAN_POINT('Ctrl Pts',(38.9246971357756,-36.3188846782332,-0.164006622317179));
#32248=CARTESIAN_POINT('Ctrl Pts',(37.0258557525633,-38.0994349533404,-0.268673373885348));
#32249=CARTESIAN_POINT('Ctrl Pts',(35.9084720925035,-38.3981590173419,-0.321006749669432));
#32250=CARTESIAN_POINT('Ctrl Pts',(37.8143974874483,-32.5937287191406,8.10700224988981));
#32251=CARTESIAN_POINT('Ctrl Pts',(38.6056283266121,-33.5191597390956,8.05466887410573));
#32252=CARTESIAN_POINT('Ctrl Pts',(39.1911984442813,-36.1960819350737,7.95000212253756));
#32253=CARTESIAN_POINT('Ctrl Pts',(36.3106940741934,-39.1612015370487,7.7930019951853));
#32254=CARTESIAN_POINT('Ctrl Pts',(32.2540352290981,-38.3859857972091,7.63600186783306));
#32255=CARTESIAN_POINT('Ctrl Pts',(30.6601534543285,-34.5788711876989,7.47900174048079));
#32256=CARTESIAN_POINT('Ctrl Pts',(32.9576299321766,-31.1472373351772,7.32200161312855));
#32257=CARTESIAN_POINT('Ctrl Pts',(37.0866305057775,-31.1714790727616,7.16500148577629));
#32258=CARTESIAN_POINT('Ctrl Pts',(39.3444742481158,-34.6282630245248,7.00800135842403));
#32259=CARTESIAN_POINT('Ctrl Pts',(37.7066136711597,-38.4186497631728,6.85100123107179));
#32260=CARTESIAN_POINT('Ctrl Pts',(33.641693040528,-39.1433700868122,6.69400110371952));
#32261=CARTESIAN_POINT('Ctrl Pts',(30.7947860459719,-36.1527554141754,6.53700097636728));
#32262=CARTESIAN_POINT('Ctrl Pts',(31.718731394466,-32.1284217844307,6.38000084901502));
#32263=CARTESIAN_POINT('Ctrl Pts',(35.5850234445937,-30.6790758307459,6.22300072166277));
#32264=CARTESIAN_POINT('Ctrl Pts',(38.9267185335935,-33.1043361203307,6.06600059431051));
#32265=CARTESIAN_POINT('Ctrl Pts',(38.747287852214,-37.2294603242033,5.90900046695826));
#32266=CARTESIAN_POINT('Ctrl Pts',(35.2076280004405,-39.3554041176628,5.75200033960601));
#32267=CARTESIAN_POINT('Ctrl Pts',(31.481786229765,-37.5758162224347,5.59500021225375));
#32268=CARTESIAN_POINT('Ctrl Pts',(30.9107604489508,-33.4864687290921,5.4380000849015));
#32269=CARTESIAN_POINT('Ctrl Pts',(34.0065950288281,-30.7543194848738,5.28099995754925));
#32270=CARTESIAN_POINT('Ctrl Pts',(37.9932253643036,-31.8293125714861,5.123999830197));
#32271=CARTESIAN_POINT('Ctrl Pts',(39.2958018060318,-35.7474915521612,4.96699970284474));
#32272=CARTESIAN_POINT('Ctrl Pts',(36.7462915531952,-38.995387657759,4.80999957549249));
#32273=CARTESIAN_POINT('Ctrl Pts',(32.6308649129514,-38.6605813351003,4.65299944814023));
#32274=CARTESIAN_POINT('Ctrl Pts',(30.6398644329761,-35.0432966040406,4.49599932078798));
#32275=CARTESIAN_POINT('Ctrl Pts',(32.5586393455524,-31.3871873963525,4.33899919343573));
#32276=CARTESIAN_POINT('Ctrl Pts',(36.6666057781757,-30.9707219083004,4.18199906608348));
#32277=CARTESIAN_POINT('Ctrl Pts',(39.2801108208385,-34.167348741179,4.02499893873122));
#32278=CARTESIAN_POINT('Ctrl Pts',(38.0555994290271,-38.1106219453356,3.86799881137897));
#32279=CARTESIAN_POINT('Ctrl Pts',(34.0911027148519,-39.2645706097038,3.71099868402672));
#32280=CARTESIAN_POINT('Ctrl Pts',(30.9416229163962,-36.5944378951337,3.55399855667446));
#32281=CARTESIAN_POINT('Ctrl Pts',(31.4313287819664,-32.494557425059,3.39699842932221));
#32282=CARTESIAN_POINT('Ctrl Pts',(35.1210963673509,-30.6413313453092,3.23999830196996));
#32283=CARTESIAN_POINT('Ctrl Pts',(38.7022756737031,-32.6965652688994,3.0829981746177));
#32284=CARTESIAN_POINT('Ctrl Pts',(38.963588874858,-36.8173112029482,2.92599804726545));
#32285=CARTESIAN_POINT('Ctrl Pts',(35.6707138879638,-39.3084567691156,2.76899791991319));
#32286=CARTESIAN_POINT('Ctrl Pts',(31.7764033615041,-37.9361677720372,2.61199779256094));
#32287=CARTESIAN_POINT('Ctrl Pts',(30.7727227893853,-33.9309890559499,2.45499766520869));
#32288=CARTESIAN_POINT('Ctrl Pts',(33.5596824021932,-30.8844025266947,2.29799753785643));
#32289=CARTESIAN_POINT('Ctrl Pts',(37.6381883094267,-31.5283121023449,2.14099741050418));
#32290=CARTESIAN_POINT('Ctrl Pts',(39.3510060812057,-35.2853167815919,1.98399728315193));
#32291=CARTESIAN_POINT('Ctrl Pts',(37.1622336865094,-38.7864766566921,1.82699715579967));
#32292=CARTESIAN_POINT('Ctrl Pts',(33.0345681639462,-38.8922635836996,1.66999702844742));
#32293=CARTESIAN_POINT('Ctrl Pts',(30.6693190617512,-35.5078264672934,1.51299690109517));
#32294=CARTESIAN_POINT('Ctrl Pts',(32.187443504768,-31.6680042909403,1.35599677374291));
#32295=CARTESIAN_POINT('Ctrl Pts',(36.2275933836127,-30.8160392022689,1.19899664639066));
#32296=CARTESIAN_POINT('Ctrl Pts',(39.1669907193568,-33.715822398208,1.04199651903841));
#32297=CARTESIAN_POINT('Ctrl Pts',(38.3697224358239,-37.7672397035641,0.884996391686155));
#32298=CARTESIAN_POINT('Ctrl Pts',(34.5509631015021,-39.3370456789998,0.7279962643339));
#32299=CARTESIAN_POINT('Ctrl Pts',(31.1345141616793,-37.0181860368003,0.570996136981647));
#32300=CARTESIAN_POINT('Ctrl Pts',(31.1849791714726,-32.8887838589028,0.413996009629392));
#32301=CARTESIAN_POINT('Ctrl Pts',(34.6550079808865,-30.6541740890041,0.256995882277139));
#32302=CARTESIAN_POINT('Ctrl Pts',(38.4372228065685,-32.313177235829,0.0999957549248859));
#32303=CARTESIAN_POINT('Ctrl Pts',(39.1314852530455,-36.3883753089936,-0.0570043724273679));
#32304=CARTESIAN_POINT('Ctrl Pts',(37.1325959372044,-38.2627408840732,-0.161671123995537));
#32305=CARTESIAN_POINT('Ctrl Pts',(35.9563385206894,-38.5772044012455,-0.214004499779622));
#32306=CARTESIAN_POINT('Ctrl Pts',(37.9552630411254,-32.4732906012887,8.21400449977962));
#32307=CARTESIAN_POINT('Ctrl Pts',(38.7860963780679,-33.4450410745538,8.16167112399554));
#32308=CARTESIAN_POINT('Ctrl Pts',(39.400975311997,-36.2559479436168,8.05700437242737));
#32309=CARTESIAN_POINT('Ctrl Pts',(36.3762966222648,-39.369477006698,7.90000424507512));
#32310=CARTESIAN_POINT('Ctrl Pts',(32.1165948534739,-38.5554603530221,7.74300411772285));
#32311=CARTESIAN_POINT('Ctrl Pts',(30.4429364871958,-34.5577929485451,7.58600399037062));
#32312=CARTESIAN_POINT('Ctrl Pts',(32.8554057112908,-30.9543997746027,7.42900386301835));
#32313=CARTESIAN_POINT('Ctrl Pts',(37.191070039577,-30.9798548538712,7.2720037356661));
#32314=CARTESIAN_POINT('Ctrl Pts',(39.5619228399106,-34.6096569338406,7.11500360831384));
#32315=CARTESIAN_POINT('Ctrl Pts',(37.8420844548986,-38.5897592080416,6.9580034809616));
#32316=CARTESIAN_POINT('Ctrl Pts',(33.5737073836467,-39.3507530609551,6.80100335360933));
#32317=CARTESIAN_POINT('Ctrl Pts',(30.5843076772956,-36.2104528539991,6.64400322625709));
#32318=CARTESIAN_POINT('Ctrl Pts',(31.5544981186253,-31.9846942345494,6.48700309890483));
#32319=CARTESIAN_POINT('Ctrl Pts',(35.6143048989029,-30.4628059618972,6.33000297155259));
#32320=CARTESIAN_POINT('Ctrl Pts',(39.1232577157224,-33.0094548026823,6.17300284420032));
#32321=CARTESIAN_POINT('Ctrl Pts',(38.9348462125535,-37.3410487421046,6.01600271684808));
#32322=CARTESIAN_POINT('Ctrl Pts',(35.2180201477371,-39.5733997686886,5.85900258949581));
#32323=CARTESIAN_POINT('Ctrl Pts',(31.3056934308947,-37.7047403633785,5.70200246214358));
#32324=CARTESIAN_POINT('Ctrl Pts',(30.7060868035096,-33.4107138218927,5.54500233479131));
#32325=CARTESIAN_POINT('Ctrl Pts',(33.9568733594783,-30.5418156935059,5.38800220743906));
#32326=CARTESIAN_POINT('Ctrl Pts',(38.1430415683413,-31.6706140784174,5.2310020800868));
#32327=CARTESIAN_POINT('Ctrl Pts',(39.5108142563315,-35.7849048215497,5.07400195273456));
#32328=CARTESIAN_POINT('Ctrl Pts',(36.8336965226849,-39.1953638505585,4.9170018253823));
#32329=CARTESIAN_POINT('Ctrl Pts',(32.5122855270398,-38.8437998814671,4.76000169803005));
#32330=CARTESIAN_POINT('Ctrl Pts',(30.4216319645722,-35.0454636753686,4.60300157067779));
#32331=CARTESIAN_POINT('Ctrl Pts',(32.4364449427192,-31.2063597591713,4.44600144332554));
#32332=CARTESIAN_POINT('Ctrl Pts',(36.7500223342062,-30.7690494395616,4.28900131597329));
#32333=CARTESIAN_POINT('Ctrl Pts',(39.4943379096791,-34.1256730784068,4.13200118862103));
#32334=CARTESIAN_POINT('Ctrl Pts',(38.2085375649176,-38.266314055126,3.97500106126878));
#32335=CARTESIAN_POINT('Ctrl Pts',(34.0456108041041,-39.4780198835927,3.81800093391653));
#32336=CARTESIAN_POINT('Ctrl Pts',(30.7384939918355,-36.6742423214464,3.66100080656427));
#32337=CARTESIAN_POINT('Ctrl Pts',(31.2527104989195,-32.3691556091822,3.50400067921202));
#32338=CARTESIAN_POINT('Ctrl Pts',(35.1271574539286,-30.4231722984524,3.34700055185977));
#32339=CARTESIAN_POINT('Ctrl Pts',(38.8875810951892,-32.5812743015779,3.19000042450751));
#32340=CARTESIAN_POINT('Ctrl Pts',(39.1619734825387,-36.9082708310562,3.03300029715526));
#32341=CARTESIAN_POINT('Ctrl Pts',(35.7042842999643,-39.5241026226178,2.876000169803));
#32342=CARTESIAN_POINT('Ctrl Pts',(31.6150566692411,-38.083128143037,2.71900004245075));
#32343=CARTESIAN_POINT('Ctrl Pts',(30.5611401158378,-33.8774831744275,2.5619999150985));
#32344=CARTESIAN_POINT('Ctrl Pts',(33.487591968347,-30.6784096207976,2.40499978774624));
#32345=CARTESIAN_POINT('Ctrl Pts',(37.7702342832343,-31.3545480053834,2.24799966039399));
#32346=CARTESIAN_POINT('Ctrl Pts',(39.5687816027568,-35.2995973892856,2.09099953304174));
#32347=CARTESIAN_POINT('Ctrl Pts',(37.2704572927298,-38.9759964857528,1.93399940568948));
#32348=CARTESIAN_POINT('Ctrl Pts',(32.9361948371383,-39.087078234871,1.77699927833723));
#32349=CARTESIAN_POINT('Ctrl Pts',(30.4525608494213,-35.533244076855,1.61999915098498));
#32350=CARTESIAN_POINT('Ctrl Pts',(32.0466700959956,-31.5012320341786,1.46299902363273));
#32351=CARTESIAN_POINT('Ctrl Pts',(36.2890365956835,-30.606624591517,1.30599889628047));
#32352=CARTESIAN_POINT('Ctrl Pts',(39.3755559477821,-33.6515470463066,1.14899876892822));
#32353=CARTESIAN_POINT('Ctrl Pts',(38.5383829817409,-37.905744927058,0.991998641575965));
#32354=CARTESIAN_POINT('Ctrl Pts',(34.5284880134556,-39.55412245782,0.83499851422371));
#32355=CARTESIAN_POINT('Ctrl Pts',(30.9410397838509,-37.1191998043172,0.677998386871458));
#32356=CARTESIAN_POINT('Ctrl Pts',(30.9940306563121,-32.7831137707316,0.520998259519202));
#32357=CARTESIAN_POINT('Ctrl Pts',(34.6377405223973,-30.4366578441002,0.36399813216695));
#32358=CARTESIAN_POINT('Ctrl Pts',(38.6092618649879,-32.1786970218597,0.206998004814696));
#32359=CARTESIAN_POINT('Ctrl Pts',(39.3382733703155,-36.4578659397538,0.0499978774624431));
#32360=CARTESIAN_POINT('Ctrl Pts',(37.2393361218455,-38.4260468148059,-0.0546688741057264));
#32361=CARTESIAN_POINT('Ctrl Pts',(36.0042049488753,-38.756249785149,-0.107002249889811));
#32362=CARTESIAN_POINT('Ctrl Pts',(38.0961285948024,-32.3528524834367,8.32100674966943));
#32363=CARTESIAN_POINT('Ctrl Pts',(38.9665644295237,-33.3709224100119,8.26867337388535));
#32364=CARTESIAN_POINT('Ctrl Pts',(39.6107521797128,-36.3158139521599,8.16400662231718));
#32365=CARTESIAN_POINT('Ctrl Pts',(36.4418991703362,-39.5777524763472,8.00700649496493));
#32366=CARTESIAN_POINT('Ctrl Pts',(31.9791544778497,-38.724934908835,7.85000636761268));
#32367=CARTESIAN_POINT('Ctrl Pts',(30.2257195200631,-34.5367147093914,7.69300624026041));
#32368=CARTESIAN_POINT('Ctrl Pts',(32.753181490405,-30.7615622140283,7.53600611290817));
#32369=CARTESIAN_POINT('Ctrl Pts',(37.2955095733766,-30.7882306349807,7.3790059855559));
#32370=CARTESIAN_POINT('Ctrl Pts',(39.7793714317054,-34.5910508431566,7.22200585820367));
#32371=CARTESIAN_POINT('Ctrl Pts',(37.9775552386376,-38.7608686529102,7.0650057308514));
#32372=CARTESIAN_POINT('Ctrl Pts',(33.5057217267653,-39.5581360350982,6.90800560349915));
#32373=CARTESIAN_POINT('Ctrl Pts',(30.3738293086194,-36.2681502938228,6.7510054761469));
#32374=CARTESIAN_POINT('Ctrl Pts',(31.3902648427845,-31.8409666846681,6.59400534879465));
#32375=CARTESIAN_POINT('Ctrl Pts',(35.6435863532121,-30.2465360930486,6.43700522144239));
#32376=CARTESIAN_POINT('Ctrl Pts',(39.3197968978512,-32.9145734850341,6.28000509409014));
#32377=CARTESIAN_POINT('Ctrl Pts',(39.1224045728929,-37.4526371600059,6.12300496673789));
#32378=CARTESIAN_POINT('Ctrl Pts',(35.2284122950338,-39.7913954197145,5.96600483938562));
#32379=CARTESIAN_POINT('Ctrl Pts',(31.1296006320244,-37.8336645043222,5.80900471203338));
#32380=CARTESIAN_POINT('Ctrl Pts',(30.5014131580684,-33.3349589146933,5.65200458468112));
#32381=CARTESIAN_POINT('Ctrl Pts',(33.9071516901285,-30.3293119021379,5.49500445732887));
#32382=CARTESIAN_POINT('Ctrl Pts',(38.292857772379,-31.5119155853487,5.33800432997662));
#32383=CARTESIAN_POINT('Ctrl Pts',(39.7258267066312,-35.8223180909381,5.18100420262436));
#32384=CARTESIAN_POINT('Ctrl Pts',(36.9211014921746,-39.3953400433581,5.02400407527211));
#32385=CARTESIAN_POINT('Ctrl Pts',(32.3937061411281,-39.0270184278339,4.86700394791986));
#32386=CARTESIAN_POINT('Ctrl Pts',(30.2033994961682,-35.0476307466965,4.7100038205676));
#32387=CARTESIAN_POINT('Ctrl Pts',(32.314250539886,-31.02553212199,4.55300369321535));
#32388=CARTESIAN_POINT('Ctrl Pts',(36.8334388902368,-30.5673769708228,4.39600356586309));
#32389=CARTESIAN_POINT('Ctrl Pts',(39.7085649985197,-34.0839974156347,4.23900343851085));
#32390=CARTESIAN_POINT('Ctrl Pts',(38.3614757008081,-38.4220061649164,4.08200331115859));
#32391=CARTESIAN_POINT('Ctrl Pts',(34.0001188933562,-39.6914691574817,3.92500318380634));
#32392=CARTESIAN_POINT('Ctrl Pts',(30.5353650672746,-36.754046747759,3.76800305645408));
#32393=CARTESIAN_POINT('Ctrl Pts',(31.0740922158726,-32.2437537933055,3.61100292910183));
#32394=CARTESIAN_POINT('Ctrl Pts',(35.1332185405061,-30.2050132515957,3.45400280174957));
#32395=CARTESIAN_POINT('Ctrl Pts',(39.0728865166754,-32.4659833342563,3.29700267439732));
#32396=CARTESIAN_POINT('Ctrl Pts',(39.3603580902194,-36.9992304591644,3.14000254704507));
#32397=CARTESIAN_POINT('Ctrl Pts',(35.7378547119649,-39.73974847612,2.98300241969282));
#32398=CARTESIAN_POINT('Ctrl Pts',(31.453709976978,-38.2300885140369,2.82600229234056));
#32399=CARTESIAN_POINT('Ctrl Pts',(30.3495574422904,-33.8239772929051,2.66900216498831));
#32400=CARTESIAN_POINT('Ctrl Pts',(33.4155015345008,-30.4724167149005,2.51200203763606));
#32401=CARTESIAN_POINT('Ctrl Pts',(37.9022802570419,-31.180783908422,2.3550019102838));
#32402=CARTESIAN_POINT('Ctrl Pts',(39.7865571243079,-35.3138779969793,2.19800178293155));
#32403=CARTESIAN_POINT('Ctrl Pts',(37.3786808989502,-39.1655163148135,2.04100165557929));
#32404=CARTESIAN_POINT('Ctrl Pts',(32.8378215103303,-39.2818928860424,1.88400152822704));
#32405=CARTESIAN_POINT('Ctrl Pts',(30.2358026370915,-35.5586616864166,1.72700140087479));
#32406=CARTESIAN_POINT('Ctrl Pts',(31.9058966872231,-31.3344597774169,1.57000127352254));
#32407=CARTESIAN_POINT('Ctrl Pts',(36.3504798077544,-30.397209980765,1.41300114617028));
#32408=CARTESIAN_POINT('Ctrl Pts',(39.5841211762074,-33.5872716944053,1.25600101881803));
#32409=CARTESIAN_POINT('Ctrl Pts',(38.7070435276578,-38.0442501505519,1.09900089146578));
#32410=CARTESIAN_POINT('Ctrl Pts',(34.5060129254091,-39.7711992366401,0.942000764113522));
#32411=CARTESIAN_POINT('Ctrl Pts',(30.7475654060226,-37.220213571834,0.785000636761267));
#32412=CARTESIAN_POINT('Ctrl Pts',(30.8030821411515,-32.6774436825603,0.628000509409014));
#32413=CARTESIAN_POINT('Ctrl Pts',(34.6204730639081,-30.2191415991965,0.471000382056761));
#32414=CARTESIAN_POINT('Ctrl Pts',(38.7813009234074,-32.0442168078902,0.314000254704507));
#32415=CARTESIAN_POINT('Ctrl Pts',(39.5450614875854,-36.5273565705141,0.157000127352254));
#32416=CARTESIAN_POINT('Ctrl Pts',(37.3460763064866,-38.5893527455387,0.0523333757840845));
#32417=CARTESIAN_POINT('Ctrl Pts',(36.0520713770612,-38.9352951690526,0.));
#32418=CARTESIAN_POINT('Ctrl Pts',(36.0520713770612,-38.9352951690526,0.));
#32419=CARTESIAN_POINT('Ctrl Pts',(36.1681792863691,-38.8956805730896,-1.36202072051053E-17));
#32420=CARTESIAN_POINT('Ctrl Pts',(36.2820221354364,-38.8505155517789,2.68655360649277E-15));
#32421=CARTESIAN_POINT('Ctrl Pts',(36.3933740322884,-38.80015771728,1.94289029309402E-15));
#32422=CARTESIAN_POINT('Ctrl Pts',(36.5072231634749,-38.7486705323445,1.18254920758684E-15));
#32423=CARTESIAN_POINT('Ctrl Pts',(36.6184689861953,-38.6917545108625,4.54098351417643E-16));
#32424=CARTESIAN_POINT('Ctrl Pts',(36.7268457946485,-38.6297432931302,1.66533453693773E-16));
#32425=CARTESIAN_POINT('Ctrl Pts',(36.8407841942848,-38.56454983515,-1.35788460984399E-16));
#32426=CARTESIAN_POINT('Ctrl Pts',(36.9515525365026,-38.4937243961273,-1.82271800722416E-15));
#32427=CARTESIAN_POINT('Ctrl Pts',(37.0588029145039,-38.4176084656939,-1.99840144432528E-15));
#32428=CARTESIAN_POINT('Ctrl Pts',(37.1526469952551,-38.3510070265646,-2.15212445178876E-15));
#32429=CARTESIAN_POINT('Ctrl Pts',(37.2437973301633,-38.2803539972376,-9.7785017405382E-16));
#32430=CARTESIAN_POINT('Ctrl Pts',(37.3319893511255,-38.2058560072044,-8.88178419700125E-16));
#32431=CARTESIAN_POINT('Ctrl Pts',(37.3493647837374,-38.1911785478217,-8.70511452689226E-16));
#32432=CARTESIAN_POINT('Ctrl Pts',(37.3666252839799,-38.1763517900465,-1.48427532953915E-15));
#32433=CARTESIAN_POINT('Ctrl Pts',(37.3837686739948,-38.1613772431262,-1.55431223447522E-15));
#32434=CARTESIAN_POINT('Ctrl Pts',(37.3963029962073,-38.1504286620158,-1.60551944217877E-15));
#32435=CARTESIAN_POINT('Ctrl Pts',(37.4087735029071,-38.139402069251,-1.97641509759958E-15));
#32436=CARTESIAN_POINT('Ctrl Pts',(37.4211705433933,-38.1283061781123,-1.88737914186277E-15));
#32437=CARTESIAN_POINT('Ctrl Pts',(37.5137497678178,-38.0454437403337,-1.22247208301798E-15));
#32438=CARTESIAN_POINT('Ctrl Pts',(37.6023731431382,-37.9585995914834,-1.41571360075421E-15));
#32439=CARTESIAN_POINT('Ctrl Pts',(37.6867792446409,-37.8680946551148,-1.63757896132211E-15));
#32440=CARTESIAN_POINT('Ctrl Pts',(37.7709936181979,-37.7777953001582,-1.85894035607411E-15));
#32441=CARTESIAN_POINT('Ctrl Pts',(37.8510103725839,-37.6838510649778,4.27670315709133E-16));
#32442=CARTESIAN_POINT('Ctrl Pts',(37.9265294316329,-37.5865486541875,7.49400541621981E-16));
#32443=CARTESIAN_POINT('Ctrl Pts',(38.0010161819357,-37.4905763199493,1.06673287208574E-15));
#32444=CARTESIAN_POINT('Ctrl Pts',(38.0711277582919,-37.3913363066692,-2.10142620498032E-15));
#32445=CARTESIAN_POINT('Ctrl Pts',(38.1365301844556,-37.2890828938187,-2.44249065417534E-15));
#32446=CARTESIAN_POINT('Ctrl Pts',(38.1898358473465,-37.2057421635956,-2.72047218512562E-15));
#32447=CARTESIAN_POINT('Ctrl Pts',(38.2400125268915,-37.1203991308186,-6.32482117348439E-16));
#32448=CARTESIAN_POINT('Ctrl Pts',(38.2868534572638,-37.0331856293588,-5.55111512312578E-16));
#32449=CARTESIAN_POINT('Ctrl Pts',(38.2987532893997,-37.0110292370944,-5.35455685563087E-16));
#32450=CARTESIAN_POINT('Ctrl Pts',(38.3104377056016,-36.9887521084602,-5.70989169773688E-17));
#32451=CARTESIAN_POINT('Ctrl Pts',(38.3219030525931,-36.9663563797929,-2.77555756156289E-17));
#32452=CARTESIAN_POINT('Ctrl Pts',(38.3300600637675,-36.9504229580542,-6.87928085047562E-18));
#32453=CARTESIAN_POINT('Ctrl Pts',(38.3381024804697,-36.9344366850298,-1.37102362174578E-15));
#32454=CARTESIAN_POINT('Ctrl Pts',(38.3460266349626,-36.9184039879293,-1.33226762955019E-15));
#32455=CARTESIAN_POINT('Ctrl Pts',(38.3989875306322,-36.8112498430667,-1.07324288929609E-15));
#32456=CARTESIAN_POINT('Ctrl Pts',(38.4467095755205,-36.7019458397232,2.38645293041498E-15));
#32457=CARTESIAN_POINT('Ctrl Pts',(38.4889139708526,-36.5907545955107,1.9151347174784E-15));
#32458=CARTESIAN_POINT('Ctrl Pts',(38.5302822088046,-36.4817662825029,1.45315430452751E-15));
#32459=CARTESIAN_POINT('Ctrl Pts',(38.5663495354543,-36.3709641352684,1.27266374069395E-15));
#32460=CARTESIAN_POINT('Ctrl Pts',(38.5968051838807,-36.2585816849604,1.52655665885959E-15));
#32461=CARTESIAN_POINT('Ctrl Pts',(38.6012594551821,-36.2421452618648,1.56368960455097E-15));
#32462=CARTESIAN_POINT('Ctrl Pts',(38.6055936009628,-36.2256750205659,1.48568813827467E-15));
#32463=CARTESIAN_POINT('Ctrl Pts',(38.6098065549286,-36.2091716785531,1.47104550762833E-15));
#32464=CARTESIAN_POINT('Ctrl Pts',(38.6394751128162,-36.092951477284,1.34152120378576E-15));
#32465=CARTESIAN_POINT('Ctrl Pts',(38.6631376928158,-35.9750893748381,9.72065328759131E-16));
#32466=CARTESIAN_POINT('Ctrl Pts',(38.6808851493713,-35.856021209443,1.41553435639707E-15));
#32467=CARTESIAN_POINT('Ctrl Pts',(38.6908686963668,-35.7890413229915,1.66500074413739E-15));
#32468=CARTESIAN_POINT('Ctrl Pts',(38.6989794822973,-35.7216798344703,1.48644827793188E-15));
#32469=CARTESIAN_POINT('Ctrl Pts',(38.7052266318381,-35.6540157826807,1.55431223447522E-15));
#32470=CARTESIAN_POINT('Ctrl Pts',(38.7081091139172,-35.6227950770761,1.58562517764618E-15));
#32471=CARTESIAN_POINT('Ctrl Pts',(38.7105947647117,-35.591509978624,7.00070747597251E-16));
#32472=CARTESIAN_POINT('Ctrl Pts',(38.7126841330784,-35.5601683863959,6.66133814775094E-16));
#32473=CARTESIAN_POINT('Ctrl Pts',(38.7138852254902,-35.5421513870013,6.46624860231182E-16));
#32474=CARTESIAN_POINT('Ctrl Pts',(38.7149548469422,-35.5241227721236,2.63074882680395E-16));
#32475=CARTESIAN_POINT('Ctrl Pts',(38.7158930667035,-35.5060923822785,2.77555756156289E-16));
#32476=CARTESIAN_POINT('Ctrl Pts',(38.7222040106739,-35.3848107969113,3.74961486578641E-16));
#32477=CARTESIAN_POINT('Ctrl Pts',(38.7225824292358,-35.263331928612,-1.41858650592555E-15));
#32478=CARTESIAN_POINT('Ctrl Pts',(38.717186529709,-35.1421030264707,-9.99200722162641E-16));
#32479=CARTESIAN_POINT('Ctrl Pts',(38.7119025633842,-35.0233889115555,-5.88514728574682E-16));
#32480=CARTESIAN_POINT('Ctrl Pts',(38.7010808603444,-34.9049135759813,2.80055440532142E-15));
#32481=CARTESIAN_POINT('Ctrl Pts',(38.6848166129475,-34.7871029976449,2.56739074444567E-15));
#32482=CARTESIAN_POINT('Ctrl Pts',(38.6687112711112,-34.6704434566446,2.3365051479245E-15));
#32483=CARTESIAN_POINT('Ctrl Pts',(38.6472688652681,-34.5544349100609,2.77413847088875E-15));
#32484=CARTESIAN_POINT('Ctrl Pts',(38.6205350417295,-34.4395098718885,3.02535774210355E-15));
#32485=CARTESIAN_POINT('Ctrl Pts',(38.6031281553353,-34.3646800563773,3.18893125068641E-15));
#32486=CARTESIAN_POINT('Ctrl Pts',(38.583477007896,-34.2903100135713,5.83132516188889E-16));
#32487=CARTESIAN_POINT('Ctrl Pts',(38.5615843988617,-34.2165260396906,2.91433543964104E-16));
#32488=CARTESIAN_POINT('Ctrl Pts',(38.5541960449916,-34.1916253022719,1.92990492842735E-16));
#32489=CARTESIAN_POINT('Ctrl Pts',(38.5465523399986,-34.1667913689833,-1.55624678416612E-15));
#32490=CARTESIAN_POINT('Ctrl Pts',(38.5386532038413,-34.1420292711584,-1.62370117351429E-15));
#32491=CARTESIAN_POINT('Ctrl Pts',(38.5335667843701,-34.1260844369365,-1.66713646980058E-15));
#32492=CARTESIAN_POINT('Ctrl Pts',(38.5283752457655,-34.1101719998602,9.92420310992954E-16));
#32493=CARTESIAN_POINT('Ctrl Pts',(38.5230814471938,-34.0943013261403,9.71445146547012E-16));
#32494=CARTESIAN_POINT('Ctrl Pts',(38.4861837828756,-33.9836830652666,8.25248693044116E-16));
#32495=CARTESIAN_POINT('Ctrl Pts',(38.4442854059965,-33.8749762815042,4.28212832527473E-15));
#32496=CARTESIAN_POINT('Ctrl Pts',(38.3974511090383,-33.7686001708186,3.23352455922077E-15));
#32497=CARTESIAN_POINT('Ctrl Pts',(38.359337050901,-33.6820305940251,2.38016393467622E-15));
#32498=CARTESIAN_POINT('Ctrl Pts',(38.3179530879923,-33.5970047635678,1.69064823388315E-15));
#32499=CARTESIAN_POINT('Ctrl Pts',(38.2733131581435,-33.5137642691618,1.70696790036118E-15));
#32500=CARTESIAN_POINT('Ctrl Pts',(38.251698175988,-33.473458609917,1.71487000282641E-15));
#32501=CARTESIAN_POINT('Ctrl Pts',(38.2293195396252,-33.4335717773559,1.04902033086069E-15));
#32502=CARTESIAN_POINT('Ctrl Pts',(38.2061773582038,-33.3941327240688,1.01307850997046E-15));
#32503=CARTESIAN_POINT('Ctrl Pts',(38.1925909929398,-33.3709787536688,9.91977702834968E-16));
#32504=CARTESIAN_POINT('Ctrl Pts',(38.1787393972074,-33.347976051224,-1.47665884113671E-16));
#32505=CARTESIAN_POINT('Ctrl Pts',(38.1646366459175,-33.3251529677485,-1.38777878078145E-17));
#32506=CARTESIAN_POINT('Ctrl Pts',(38.1062051944783,-33.230590859521,5.40441897174675E-16));
#32507=CARTESIAN_POINT('Ctrl Pts',(38.0434224756675,-33.1390339550006,1.08623518571526E-16));
#32508=CARTESIAN_POINT('Ctrl Pts',(37.9763225348264,-33.0508729636923,6.24500451351651E-16));
#32509=CARTESIAN_POINT('Ctrl Pts',(37.9162918094667,-32.9720000438309,1.08602792936337E-15));
#32510=CARTESIAN_POINT('Ctrl Pts',(37.8528049873413,-32.8958452375375,9.00746847309969E-16));
#32511=CARTESIAN_POINT('Ctrl Pts',(37.7858629582169,-32.8227148526165,3.72098185597025E-16));
#32512=CARTESIAN_POINT('Ctrl Pts',(37.7510080319419,-32.784637814794,1.2084137301326E-16));
#32513=CARTESIAN_POINT('Ctrl Pts',(37.7152160018646,-32.7473811866193,3.2434591796547E-16));
#32514=CARTESIAN_POINT('Ctrl Pts',(37.6785242770714,-32.7109603660126,2.77555756156289E-16));
#32515=CARTESIAN_POINT('Ctrl Pts',(31.4836965554877,-35.0029832498286,6.38741669750802));
#32516=CARTESIAN_POINT('Ctrl Pts',(31.4810524495825,-35.31689356108,6.4016107071645));
#32517=CARTESIAN_POINT('Ctrl Pts',(31.519709060091,-35.6301638289998,6.41580471682099));
#32518=CARTESIAN_POINT('Ctrl Pts',(31.6022835043847,-35.9313947240647,6.42999872647747));
#32519=CARTESIAN_POINT('Ctrl Pts',(31.9067358422351,-37.0420343537909,6.48233210226155));
#32520=CARTESIAN_POINT('Ctrl Pts',(32.8082072698223,-37.98901073323,6.53466547804564));
#32521=CARTESIAN_POINT('Ctrl Pts',(33.9025203486177,-38.3477577905554,6.58699885382972));
#32522=CARTESIAN_POINT('Ctrl Pts',(34.9968334274131,-38.7065048478808,6.6393322296138));
#32523=CARTESIAN_POINT('Ctrl Pts',(36.2839881574169,-38.4770225830925,6.69166560539789));
#32524=CARTESIAN_POINT('Ctrl Pts',(37.1868793172355,-37.7621695835158,6.74399898118197));
#32525=CARTESIAN_POINT('Ctrl Pts',(38.0897704770541,-37.0473165839391,6.79633235696606));
#32526=CARTESIAN_POINT('Ctrl Pts',(38.6083980666875,-35.847092849574,6.84866573275014));
#32527=CARTESIAN_POINT('Ctrl Pts',(38.5102394141138,-34.6996866784653,6.90099910853423));
#32528=CARTESIAN_POINT('Ctrl Pts',(38.41208076154,-33.5522805073566,6.95333248431831));
#32529=CARTESIAN_POINT('Ctrl Pts',(37.697135866759,-32.4576918995043,7.0056658601024));
#32530=CARTESIAN_POINT('Ctrl Pts',(36.6859406162159,-31.9065595295948,7.05799923588648));
#32531=CARTESIAN_POINT('Ctrl Pts',(35.6747453656728,-31.3554271596853,7.11033261167057));
#32532=CARTESIAN_POINT('Ctrl Pts',(34.3672997593676,-31.3477510277185,7.16266598745465));
#32533=CARTESIAN_POINT('Ctrl Pts',(33.3498296676148,-31.8872253835852,7.21499936323873));
#32534=CARTESIAN_POINT('Ctrl Pts',(32.332359575862,-32.426699739452,7.26733273902282));
#32535=CARTESIAN_POINT('Ctrl Pts',(31.6048649986616,-33.5133245831523,7.3196661148069));
#32536=CARTESIAN_POINT('Ctrl Pts',(31.4934685739382,-34.6593973074264,7.37199949059099));
#32537=CARTESIAN_POINT('Ctrl Pts',(31.4825295909021,-34.7719401481876,7.37713855956333));
#32538=CARTESIAN_POINT('Ctrl Pts',(31.4775316317653,-34.8850562438399,7.38227762853568));
#32539=CARTESIAN_POINT('Ctrl Pts',(31.478260520576,-34.9982347527286,7.38741669750802));
#32540=CARTESIAN_POINT('Ctrl Pts',(33.9479286229388,-38.9352951690526,8.));
#32541=CARTESIAN_POINT('Ctrl Pts',(32.6539236935135,-38.5893527455387,7.94766662421592));
#32542=CARTESIAN_POINT('Ctrl Pts',(30.4549361873396,-36.5273716142364,7.84299987264774));
#32543=CARTESIAN_POINT('Ctrl Pts',(31.2187010881653,-32.044211167377,7.68599974529549));
#32544=CARTESIAN_POINT('Ctrl Pts',(35.3795267558193,-30.2191465582126,7.52899961794324));
#32545=CARTESIAN_POINT('Ctrl Pts',(39.1969165266342,-32.6774422642514,7.37199949059099));
#32546=CARTESIAN_POINT('Ctrl Pts',(39.2524336251343,-37.2202141105436,7.21499936323873));
#32547=CARTESIAN_POINT('Ctrl Pts',(35.4939867861423,-39.7711972931265,7.05799923588648));
#32548=CARTESIAN_POINT('Ctrl Pts',(31.292957592828,-38.0442496611363,6.90099910853423));
#32549=CARTESIAN_POINT('Ctrl Pts',(30.4158800177777,-33.5872718945856,6.74399898118197));
#32550=CARTESIAN_POINT('Ctrl Pts',(33.6495206016122,-30.3972113452741,6.58699885382972));
#32551=CARTESIAN_POINT('Ctrl Pts',(38.09410244091,-31.3344607296745,6.42999872647747));
#32552=CARTESIAN_POINT('Ctrl Pts',(39.7641960678496,-35.558661561786,6.27299859912521));
#32553=CARTESIAN_POINT('Ctrl Pts',(37.1621778889461,-39.2818916953666,6.11599847177296));
#32554=CARTESIAN_POINT('Ctrl Pts',(32.6213197580022,-39.1655151793351,5.95899834442071));
#32555=CARTESIAN_POINT('Ctrl Pts',(30.2134441875202,-35.3138779065921,5.80199821706845));
#32556=CARTESIAN_POINT('Ctrl Pts',(32.0977205408613,-31.1807849590781,5.6449980897162));
#32557=CARTESIAN_POINT('Ctrl Pts',(36.584498029893,-30.4724179566463,5.48799796236395));
#32558=CARTESIAN_POINT('Ctrl Pts',(39.6504412814188,-33.8239776163473,5.33099783501169));
#32559=CARTESIAN_POINT('Ctrl Pts',(38.5462890493217,-38.2300876270061,5.17399770765944));
#32560=CARTESIAN_POINT('Ctrl Pts',(34.2621454906851,-39.7397471751372,5.01699758030718));
#32561=CARTESIAN_POINT('Ctrl Pts',(30.6396431067263,-36.9992299102556,4.85999745295493));
#32562=CARTESIAN_POINT('Ctrl Pts',(30.9271146014312,-32.4659840299328,4.70299732560268));
#32563=CARTESIAN_POINT('Ctrl Pts',(34.8667814960507,-30.2050145678827,4.54599719825042));
#32564=CARTESIAN_POINT('Ctrl Pts',(38.9259067064028,-32.2437545499559,4.38899707089817));
#32565=CARTESIAN_POINT('Ctrl Pts',(39.4646337070995,-36.7540462662356,4.23199694354592));
#32566=CARTESIAN_POINT('Ctrl Pts',(35.9998808321606,-39.6914678695931,4.07499681619366));
#32567=CARTESIAN_POINT('Ctrl Pts',(31.6385252219761,-38.4220052255121,3.91799668884141));
#32568=CARTESIAN_POINT('Ctrl Pts',(30.291436294066,-34.0839976670965,3.76099656148916));
#32569=CARTESIAN_POINT('Ctrl Pts',(33.1665616130745,-30.567378187653,3.6039964341369));
#32570=CARTESIAN_POINT('Ctrl Pts',(37.6857487228281,-31.0255332130596,3.44699630678465));
#32571=CARTESIAN_POINT('Ctrl Pts',(39.7965991870786,-35.0476307336073,3.28999617943239));
#32572=CARTESIAN_POINT('Ctrl Pts',(37.606293143399,-39.0270173223719,3.13299605208014));
#32573=CARTESIAN_POINT('Ctrl Pts',(33.0788990351993,-39.3953388367078,2.97599592472789));
#32574=CARTESIAN_POINT('Ctrl Pts',(30.2741745906988,-35.8223178652953,2.81899579737564));
#32575=CARTESIAN_POINT('Ctrl Pts',(31.7071431315558,-31.5119165427019,2.66199567002338));
#32576=CARTESIAN_POINT('Ctrl Pts',(36.092848009894,-30.329313184686,2.50499554267113));
#32577=CARTESIAN_POINT('Ctrl Pts',(39.4985856069267,-33.3349593710879,2.34799541531888));
#32578=CARTESIAN_POINT('Ctrl Pts',(38.8703983056154,-37.8336637277424,2.19099528796662));
#32579=CARTESIAN_POINT('Ctrl Pts',(34.7715877673847,-39.7913941019012,2.03399516061437));
#32580=CARTESIAN_POINT('Ctrl Pts',(30.8775965593863,-37.4526364914204,1.87699503326212));
#32581=CARTESIAN_POINT('Ctrl Pts',(30.6802042867265,-32.914574048659,1.71999490590986));
#32582=CARTESIAN_POINT('Ctrl Pts',(34.3564138261785,-30.2465374145616,1.56299477855761));
#32583=CARTESIAN_POINT('Ctrl Pts',(38.6097341605507,-31.8409675209513,1.40599465120535));
#32584=CARTESIAN_POINT('Ctrl Pts',(39.6261694334752,-36.2681500029269,1.2489945238531));
#32585=CARTESIAN_POINT('Ctrl Pts',(36.4942778376799,-39.5581346787212,1.09199439650085));
#32586=CARTESIAN_POINT('Ctrl Pts',(32.0224456319375,-38.7608678116187,0.934994269148595));
#32587=CARTESIAN_POINT('Ctrl Pts',(30.2206297689144,-34.5910506117954,0.777994141796339));
#32588=CARTESIAN_POINT('Ctrl Pts',(32.704491289799,-30.7882324000235,0.620994014444087));
#32589=CARTESIAN_POINT('Ctrl Pts',(37.2468174060219,-30.7615623188695,0.463993887091833));
#32590=CARTESIAN_POINT('Ctrl Pts',(39.7742801854456,-34.536716632844,0.306993759739581));
#32591=CARTESIAN_POINT('Ctrl Pts',(38.0208425645948,-38.7249309242138,0.149993632387326));
#32592=CARTESIAN_POINT('Ctrl Pts',(33.5581056824257,-39.5777559852671,-0.00700649496492666));
#32593=CARTESIAN_POINT('Ctrl Pts',(30.3892373827997,-36.3158028716181,-0.16400662231718));
#32594=CARTESIAN_POINT('Ctrl Pts',(31.0334355704763,-33.370922410012,-0.26867337388535));
#32595=CARTESIAN_POINT('Ctrl Pts',(31.9038714051976,-32.3528524834368,-0.321006749669435));
#32596=CARTESIAN_POINT('Ctrl Pts',(33.9957950511247,-38.756249785149,8.10700224988981));
#32597=CARTESIAN_POINT('Ctrl Pts',(32.7606638781546,-38.426046814806,8.05466887410573));
#32598=CARTESIAN_POINT('Ctrl Pts',(30.6617244103942,-36.4578802990271,7.95000212253756));
#32599=CARTESIAN_POINT('Ctrl Pts',(31.3907400550635,-32.1786916379746,7.79300199518531));
#32600=CARTESIAN_POINT('Ctrl Pts',(35.3622593055321,-30.4366625774945,7.63600186783305));
#32601=CARTESIAN_POINT('Ctrl Pts',(39.0059680720859,-32.7831124169518,7.4790017404808));
#32602=CARTESIAN_POINT('Ctrl Pts',(39.0589592913856,-37.1192003185169,7.32200161312853));
#32603=CARTESIAN_POINT('Ctrl Pts',(35.4715117112195,-39.554120602731,7.16500148577629));
#32604=CARTESIAN_POINT('Ctrl Pts',(31.4616180877658,-37.9057444599095,7.00800135842404));
#32605=CARTESIAN_POINT('Ctrl Pts',(30.6244451918799,-33.6515472373793,6.85100123107178));
#32606=CARTESIAN_POINT('Ctrl Pts',(33.7109637950579,-30.6066258939446,6.69400110371953));
#32607=CARTESIAN_POINT('Ctrl Pts',(37.9533290718052,-31.5012329431111,6.53700097636728));
#32608=CARTESIAN_POINT('Ctrl Pts',(39.5474379144414,-35.5332439578948,6.38000084901502));
#32609=CARTESIAN_POINT('Ctrl Pts',(37.0638045894695,-39.0870770983678,6.22300072166277));
#32610=CARTESIAN_POINT('Ctrl Pts',(32.729543334333,-38.9759954019356,6.06600059431052));
#32611=CARTESIAN_POINT('Ctrl Pts',(30.4312196493866,-35.2995973030108,5.90900046695826));
#32612=CARTESIAN_POINT('Ctrl Pts',(32.2297664783665,-31.3545490082375,5.752000339606));
#32613=CARTESIAN_POINT('Ctrl Pts',(36.5124076158656,-30.6784108060473,5.59500021225375));
#32614=CARTESIAN_POINT('Ctrl Pts',(39.4388586659392,-33.8774834831539,5.4380000849015));
#32615=CARTESIAN_POINT('Ctrl Pts',(38.3849424013594,-38.0831272963638,5.28099995754925));
#32616=CARTESIAN_POINT('Ctrl Pts',(34.2957158934656,-39.5241013808263,5.123999830197));
#32617=CARTESIAN_POINT('Ctrl Pts',(30.8380276599492,-36.9082703071214,4.96699970284474));
#32618=CARTESIAN_POINT('Ctrl Pts',(31.1124199720466,-32.581274965603,4.80999957549249));
#32619=CARTESIAN_POINT('Ctrl Pts',(34.8728425809651,-30.4231735548519,4.65299944814024));
#32620=CARTESIAN_POINT('Ctrl Pts',(38.7472884723895,-32.3691563314071,4.49599932078798));
#32621=CARTESIAN_POINT('Ctrl Pts',(39.2615048383014,-36.674241861831,4.33899919343573));
#32622=CARTESIAN_POINT('Ctrl Pts',(35.954388933901,-39.4780186542996,4.18199906608348));
#32623=CARTESIAN_POINT('Ctrl Pts',(31.7914633158823,-38.2663131584621,4.02499893873122));
#32624=CARTESIAN_POINT('Ctrl Pts',(30.5056633240975,-34.1256733184278,3.86799881137897));
#32625=CARTESIAN_POINT('Ctrl Pts',(33.2499781462058,-30.7690506010293,3.71099868402671));
#32626=CARTESIAN_POINT('Ctrl Pts',(37.5635543535394,-31.2063608006002,3.55399855667446));
#32627=CARTESIAN_POINT('Ctrl Pts',(39.5783667785835,-35.0454636628748,3.39699842932221));
#32628=CARTESIAN_POINT('Ctrl Pts',(37.4877137900394,-38.8437988263006,3.23999830196995));
#32629=CARTESIAN_POINT('Ctrl Pts',(33.1663039806949,-39.1953626988076,3.0829981746177));
#32630=CARTESIAN_POINT('Ctrl Pts',(30.4891869819735,-35.784904606173,2.92599804726545));
#32631=CARTESIAN_POINT('Ctrl Pts',(31.856959294467,-31.6706149922136,2.76899791991319));
#32632=CARTESIAN_POINT('Ctrl Pts',(36.0431263541924,-30.5418169177014,2.61199779256094));
#32633=CARTESIAN_POINT('Ctrl Pts',(39.2939120176749,-33.4107142575226,2.45499766520869));
#32634=CARTESIAN_POINT('Ctrl Pts',(38.6943055550796,-37.704739622131,2.29799753785643));
#32635=CARTESIAN_POINT('Ctrl Pts',(34.7819799118415,-39.5733985108324,2.14099741050418));
#32636=CARTESIAN_POINT('Ctrl Pts',(31.0651548682101,-37.3410481039379,1.98399728315193));
#32637=CARTESIAN_POINT('Ctrl Pts',(30.8767434149602,-33.0094553406639,1.82699715579967));
#32638=CARTESIAN_POINT('Ctrl Pts',(34.3856952723259,-30.4628072232849,1.66999702844742));
#32639=CARTESIAN_POINT('Ctrl Pts',(38.4455009300555,-31.9846950327841,1.51299690109516));
#32640=CARTESIAN_POINT('Ctrl Pts',(39.4156911220303,-36.2104525763381,1.35599677374291));
#32641=CARTESIAN_POINT('Ctrl Pts',(36.4262922006151,-39.3507517662898,1.19899664639066));
#32642=CARTESIAN_POINT('Ctrl Pts',(32.1579163760677,-38.5897584050265,1.04199651903841));
#32643=CARTESIAN_POINT('Ctrl Pts',(30.4380783060842,-34.6096567130058,0.884996391686151));
#32644=CARTESIAN_POINT('Ctrl Pts',(32.8089307843264,-30.9798565386092,0.727996264333898));
#32645=CARTESIAN_POINT('Ctrl Pts',(37.1445932353457,-30.9543998746739,0.570996136981644));
#32646=CARTESIAN_POINT('Ctrl Pts',(39.5570632317115,-34.5577947844858,0.413996009629391));
#32647=CARTESIAN_POINT('Ctrl Pts',(37.8834023235315,-38.5554565496905,0.256995882277137));
#32648=CARTESIAN_POINT('Ctrl Pts',(33.6237080097094,-39.3694803559713,0.0999957549248841));
#32649=CARTESIAN_POINT('Ctrl Pts',(30.5990147253931,-36.25593736721,-0.0570043724273687));
#32650=CARTESIAN_POINT('Ctrl Pts',(31.2139036219321,-33.4450410745538,-0.161671123995539));
#32651=CARTESIAN_POINT('Ctrl Pts',(32.0447369588746,-32.4732906012887,-0.214004499779624));
#32652=CARTESIAN_POINT('Ctrl Pts',(34.0436614793107,-38.5772044012455,8.21400449977962));
#32653=CARTESIAN_POINT('Ctrl Pts',(32.8674040627957,-38.2627408840732,8.16167112399554));
#32654=CARTESIAN_POINT('Ctrl Pts',(30.8685126334489,-36.3883889838178,8.05700437242737));
#32655=CARTESIAN_POINT('Ctrl Pts',(31.5627790219617,-32.3131721085722,7.90000424507511));
#32656=CARTESIAN_POINT('Ctrl Pts',(35.3449918552448,-30.6541785967763,7.74300411772285));
#32657=CARTESIAN_POINT('Ctrl Pts',(38.8150196175374,-32.8887825696523,7.58600399037061));
#32658=CARTESIAN_POINT('Ctrl Pts',(38.8654849576371,-37.0181865264902,7.42900386301835));
#32659=CARTESIAN_POINT('Ctrl Pts',(35.4490366362965,-39.3370439123355,7.2720037356661));
#32660=CARTESIAN_POINT('Ctrl Pts',(31.6302785827036,-37.7672392586828,7.11500360831385));
#32661=CARTESIAN_POINT('Ctrl Pts',(30.833010365982,-33.715822580173,6.95800348096159));
#32662=CARTESIAN_POINT('Ctrl Pts',(33.7724069885036,-30.8160404426151,6.80100335360934));
#32663=CARTESIAN_POINT('Ctrl Pts',(37.8125557027003,-31.6680051565476,6.64400322625708));
#32664=CARTESIAN_POINT('Ctrl Pts',(39.3306797610333,-35.5078263540035,6.48700309890484));
#32665=CARTESIAN_POINT('Ctrl Pts',(36.9654312899929,-38.892262501369,6.33000297155257));
#32666=CARTESIAN_POINT('Ctrl Pts',(32.8377669106638,-38.7864756245362,6.17300284420034));
#32667=CARTESIAN_POINT('Ctrl Pts',(30.6489951112531,-35.2853166994296,6.01600271684807));
#32668=CARTESIAN_POINT('Ctrl Pts',(32.3618124158715,-31.5283130573969,5.85900258949582));
#32669=CARTESIAN_POINT('Ctrl Pts',(36.4403172018384,-30.8844036554483,5.70200246214356));
#32670=CARTESIAN_POINT('Ctrl Pts',(39.2272760504595,-33.9309893499606,5.54500233479132));
#32671=CARTESIAN_POINT('Ctrl Pts',(38.2235957533972,-37.9361669657214,5.38800220743906));
#32672=CARTESIAN_POINT('Ctrl Pts',(34.3292862962461,-39.3084555865154,5.23100208008681));
#32673=CARTESIAN_POINT('Ctrl Pts',(31.0364122131721,-36.8173107039871,5.07400195273455));
#32674=CARTESIAN_POINT('Ctrl Pts',(31.2977253426618,-32.6965659012732,4.9170018253823));
#32675=CARTESIAN_POINT('Ctrl Pts',(34.8789036658794,-30.6413325418211,4.76000169803005));
#32676=CARTESIAN_POINT('Ctrl Pts',(38.5686702383762,-32.4945581128583,4.60300157067779));
#32677=CARTESIAN_POINT('Ctrl Pts',(39.0583759695033,-36.5944374574263,4.44600144332554));
#32678=CARTESIAN_POINT('Ctrl Pts',(35.9088970356414,-39.2645694390062,4.28900131597328));
#32679=CARTESIAN_POINT('Ctrl Pts',(31.9444014097886,-38.1106210914121,4.13200118862103));
#32680=CARTESIAN_POINT('Ctrl Pts',(30.7198903541289,-34.1673489697591,3.97500106126878));
#32681=CARTESIAN_POINT('Ctrl Pts',(33.333394679337,-30.9707230144056,3.81800093391652));
#32682=CARTESIAN_POINT('Ctrl Pts',(37.4413599842507,-31.3871883881407,3.66100080656427));
#32683=CARTESIAN_POINT('Ctrl Pts',(39.3601343700882,-35.0432965921423,3.50400067921202));
#32684=CARTESIAN_POINT('Ctrl Pts',(37.36913443668,-38.6605803302294,3.34700055185977));
#32685=CARTESIAN_POINT('Ctrl Pts',(33.2537089261905,-38.9953865609073,3.19000042450751));
#32686=CARTESIAN_POINT('Ctrl Pts',(30.7041993732481,-35.7474913470507,3.03300029715526));
#32687=CARTESIAN_POINT('Ctrl Pts',(32.006775457378,-31.8293134417253,2.876000169803));
#32688=CARTESIAN_POINT('Ctrl Pts',(35.9934046984909,-30.7543206507168,2.71900004245075));
#32689=CARTESIAN_POINT('Ctrl Pts',(39.0892384284232,-33.4864691439573,2.5619999150985));
#32690=CARTESIAN_POINT('Ctrl Pts',(38.5182128045439,-37.5758155165195,2.40499978774624));
#32691=CARTESIAN_POINT('Ctrl Pts',(34.7923720562983,-39.3554029197635,2.24799966039399));
#32692=CARTESIAN_POINT('Ctrl Pts',(31.2527131770338,-37.2294597164554,2.09099953304174));
#32693=CARTESIAN_POINT('Ctrl Pts',(31.073282543194,-33.1043366326688,1.93399940568948));
#32694=CARTESIAN_POINT('Ctrl Pts',(34.4149767184733,-30.6790770320082,1.77699927833723));
#32695=CARTESIAN_POINT('Ctrl Pts',(38.2812676995604,-32.1284225446167,1.61999915098497));
#32696=CARTESIAN_POINT('Ctrl Pts',(39.2052128105854,-36.1527551497494,1.46299902363272));
#32697=CARTESIAN_POINT('Ctrl Pts',(36.3583065635504,-39.1433688538583,1.30599889628047));
#32698=CARTESIAN_POINT('Ctrl Pts',(32.2933871201978,-38.4186489984343,1.14899876892821));
#32699=CARTESIAN_POINT('Ctrl Pts',(30.655526843254,-34.6282628142162,0.991998641575962));
#32700=CARTESIAN_POINT('Ctrl Pts',(32.9133702788538,-31.1714806771949,0.834998514223709));
#32701=CARTESIAN_POINT('Ctrl Pts',(37.0423690646695,-31.1472374304784,0.677998386871454));
#32702=CARTESIAN_POINT('Ctrl Pts',(39.3398462779774,-34.5788729361276,0.520998259519202));
#32703=CARTESIAN_POINT('Ctrl Pts',(37.7459620824681,-38.385982175167,0.363998132166948));
#32704=CARTESIAN_POINT('Ctrl Pts',(33.6893103369932,-39.1612047266757,0.206998004814695));
#32705=CARTESIAN_POINT('Ctrl Pts',(30.8087920679866,-36.1960718628018,0.0499978774624421));
#32706=CARTESIAN_POINT('Ctrl Pts',(31.3943716733879,-33.5191597390956,-0.0546688741057282));
#32707=CARTESIAN_POINT('Ctrl Pts',(32.1856025125517,-32.5937287191406,-0.107002249889813));
#32708=CARTESIAN_POINT('Ctrl Pts',(34.0915279074966,-38.398159017342,8.32100674966943));
#32709=CARTESIAN_POINT('Ctrl Pts',(32.9741442474368,-38.0994349533405,8.26867337388535));
#32710=CARTESIAN_POINT('Ctrl Pts',(31.0753008565035,-36.3188976686085,8.16400662231718));
#32711=CARTESIAN_POINT('Ctrl Pts',(31.73481798886,-32.4476525791699,8.00700649496493));
#32712=CARTESIAN_POINT('Ctrl Pts',(35.3277244049576,-30.8716946160581,7.85000636761267));
#32713=CARTESIAN_POINT('Ctrl Pts',(38.6240711629891,-32.9944527223528,7.69300624026043));
#32714=CARTESIAN_POINT('Ctrl Pts',(38.6720106238885,-36.9171727344635,7.53600611290815));
#32715=CARTESIAN_POINT('Ctrl Pts',(35.4265615613737,-39.1199672219399,7.37900598555592));
#32716=CARTESIAN_POINT('Ctrl Pts',(31.7989390776415,-37.628734057456,7.22200585820365));
#32717=CARTESIAN_POINT('Ctrl Pts',(31.0415755400842,-33.7800979229667,7.06500573085141));
#32718=CARTESIAN_POINT('Ctrl Pts',(33.8338501819494,-31.0254549912856,6.90800560349915));
#32719=CARTESIAN_POINT('Ctrl Pts',(37.6717823335954,-31.8347773699841,6.75100547614689));
#32720=CARTESIAN_POINT('Ctrl Pts',(39.1139216076251,-35.4824087501123,6.59400534879465));
#32721=CARTESIAN_POINT('Ctrl Pts',(36.8670579905162,-38.6974479043702,6.43700522144239));
#32722=CARTESIAN_POINT('Ctrl Pts',(32.9459904869947,-38.5969558471367,6.28000509409014));
#32723=CARTESIAN_POINT('Ctrl Pts',(30.8667705731195,-35.2710360958482,6.12300496673788));
#32724=CARTESIAN_POINT('Ctrl Pts',(32.4938583533767,-31.7020771065563,5.96600483938563));
#32725=CARTESIAN_POINT('Ctrl Pts',(36.3682267878111,-31.0903965048492,5.80900471203338));
#32726=CARTESIAN_POINT('Ctrl Pts',(39.0156934349799,-33.9844952167673,5.65200458468112));
#32727=CARTESIAN_POINT('Ctrl Pts',(38.0622491054349,-37.789206635079,5.49500445732887));
#32728=CARTESIAN_POINT('Ctrl Pts',(34.3628566990267,-39.0928097922045,5.33800432997662));
#32729=CARTESIAN_POINT('Ctrl Pts',(31.234796766395,-36.7263511008529,5.18100420262436));
#32730=CARTESIAN_POINT('Ctrl Pts',(31.4830307132771,-32.8118568369433,5.02400407527211));
#32731=CARTESIAN_POINT('Ctrl Pts',(34.8849647507938,-30.8594915287904,4.86700394791986));
#32732=CARTESIAN_POINT('Ctrl Pts',(38.3900520043628,-32.6199598943095,4.7100038205676));
#32733=CARTESIAN_POINT('Ctrl Pts',(38.8552471007052,-36.5146330530217,4.55300369321535));
#32734=CARTESIAN_POINT('Ctrl Pts',(35.8634051373818,-39.0511202237127,4.39600356586309));
#32735=CARTESIAN_POINT('Ctrl Pts',(32.0973395036949,-37.9549290243621,4.23900343851084));
#32736=CARTESIAN_POINT('Ctrl Pts',(30.9341173841603,-34.2090246210904,4.08200331115859));
#32737=CARTESIAN_POINT('Ctrl Pts',(33.4168112124683,-31.1723954277819,3.92500318380634));
#32738=CARTESIAN_POINT('Ctrl Pts',(37.319165614962,-31.5680159756812,3.76800305645408));
#32739=CARTESIAN_POINT('Ctrl Pts',(39.141901961593,-35.0411295214099,3.61100292910183));
#32740=CARTESIAN_POINT('Ctrl Pts',(37.2505550833205,-38.4773618341581,3.45400280174957));
#32741=CARTESIAN_POINT('Ctrl Pts',(33.3411138716861,-38.7954104230071,3.29700267439732));
#32742=CARTESIAN_POINT('Ctrl Pts',(30.9192117645227,-35.7100780879284,3.14000254704507));
#32743=CARTESIAN_POINT('Ctrl Pts',(32.1565916202891,-31.988011891237,2.98300241969282));
#32744=CARTESIAN_POINT('Ctrl Pts',(35.9436830427893,-30.9668243837322,2.82600229234056));
#32745=CARTESIAN_POINT('Ctrl Pts',(38.8845648391714,-33.5622240303919,2.66900216498831));
#32746=CARTESIAN_POINT('Ctrl Pts',(38.3421200540082,-37.4468914109081,2.51200203763606));
#32747=CARTESIAN_POINT('Ctrl Pts',(34.802764200755,-39.1374073286946,2.3550019102838));
#32748=CARTESIAN_POINT('Ctrl Pts',(31.4402714858577,-37.1178713289729,2.19800178293155));
#32749=CARTESIAN_POINT('Ctrl Pts',(31.2698216714276,-33.1992179246737,2.04100165557929));
#32750=CARTESIAN_POINT('Ctrl Pts',(34.4442581646208,-30.8953468407316,1.88400152822704));
#32751=CARTESIAN_POINT('Ctrl Pts',(38.1170344690652,-32.2721500564494,1.72700140087478));
#32752=CARTESIAN_POINT('Ctrl Pts',(38.9947344991405,-36.0950577231607,1.57000127352253));
#32753=CARTESIAN_POINT('Ctrl Pts',(36.2903209264856,-38.9359859414268,1.41300114617028));
#32754=CARTESIAN_POINT('Ctrl Pts',(32.428857864328,-38.247539591842,1.25600101881803));
#32755=CARTESIAN_POINT('Ctrl Pts',(30.8729753804238,-34.6468689154266,1.09900089146577));
#32756=CARTESIAN_POINT('Ctrl Pts',(33.0178097733811,-31.3631048157807,0.942000764113519));
#32757=CARTESIAN_POINT('Ctrl Pts',(36.9401448939934,-31.3400749862829,0.785000636761266));
#32758=CARTESIAN_POINT('Ctrl Pts',(39.1226293242432,-34.5999510877694,0.628000509409013));
#32759=CARTESIAN_POINT('Ctrl Pts',(37.6085218414048,-38.2165078006437,0.471000382056759));
#32760=CARTESIAN_POINT('Ctrl Pts',(33.754912664277,-38.9529290973799,0.314000254704506));
#32761=CARTESIAN_POINT('Ctrl Pts',(31.0185694105801,-36.1362063583937,0.157000127352253));
#32762=CARTESIAN_POINT('Ctrl Pts',(31.5748397248436,-33.5932784036374,0.0523333757840826));
#32763=CARTESIAN_POINT('Ctrl Pts',(32.3264680662287,-32.7141668369925,-2.22044604925031E-15));
#32764=CARTESIAN_POINT('Ctrl Pts',(32.3264680662287,-32.7141668369925,-2.27595720048157E-15));
#32765=CARTESIAN_POINT('Ctrl Pts',(32.2493253090815,-32.7912797983002,-2.16394166852401E-15));
#32766=CARTESIAN_POINT('Ctrl Pts',(32.1762949026186,-32.8720149145437,3.46363794187806E-16));
#32767=CARTESIAN_POINT('Ctrl Pts',(32.1073691591848,-32.9559536860909,1.66533453693773E-16));
#32768=CARTESIAN_POINT('Ctrl Pts',(32.0366835341849,-33.0420356669728,-1.78884963425382E-17));
#32769=CARTESIAN_POINT('Ctrl Pts',(31.9703144812951,-33.1314874423946,-2.24888209125886E-15));
#32770=CARTESIAN_POINT('Ctrl Pts',(31.9082835820817,-33.2239037683368,-2.33146835171283E-15));
#32771=CARTESIAN_POINT('Ctrl Pts',(31.8449616802408,-33.3182434860262,-2.41577341812641E-15));
#32772=CARTESIAN_POINT('Ctrl Pts',(31.7861599686898,-33.4156730215343,-2.34515801197777E-15));
#32773=CARTESIAN_POINT('Ctrl Pts',(31.7319381963941,-33.5158007480848,-2.77555756156289E-15));
#32774=CARTESIAN_POINT('Ctrl Pts',(31.6801489223982,-33.611436542441,-3.18664851741706E-15));
#32775=CARTESIAN_POINT('Ctrl Pts',(31.6325378836028,-33.7095346984804,-3.69832300465041E-15));
#32776=CARTESIAN_POINT('Ctrl Pts',(31.5891926568309,-33.8097785742014,-3.99680288865056E-15));
#32777=CARTESIAN_POINT('Ctrl Pts',(31.5821541452564,-33.8260564375806,-4.04527083482939E-15));
#32778=CARTESIAN_POINT('Ctrl Pts',(31.5752281942475,-33.8423909194022,-5.19848407519141E-15));
#32779=CARTESIAN_POINT('Ctrl Pts',(31.568415272417,-33.8587807065962,-5.21804821573824E-15));
#32780=CARTESIAN_POINT('Ctrl Pts',(31.561906348996,-33.8744391674425,-5.23673938757109E-15));
#32781=CARTESIAN_POINT('Ctrl Pts',(31.5555036120846,-33.8901409126424,-5.57046258471252E-15));
#32782=CARTESIAN_POINT('Ctrl Pts',(31.5492092706946,-33.9058793019477,-5.49560397189452E-15));
#32783=CARTESIAN_POINT('Ctrl Pts',(31.5058237133564,-34.0143606742329,-4.97961946494936E-15));
#32784=CARTESIAN_POINT('Ctrl Pts',(31.4675520206245,-34.1246590298884,-6.38605598306829E-15));
#32785=CARTESIAN_POINT('Ctrl Pts',(31.4344228151864,-34.2363425690307,-5.19029264012261E-15));
#32786=CARTESIAN_POINT('Ctrl Pts',(31.4008590997118,-34.3494909069217,-3.9788461207494E-15));
#32787=CARTESIAN_POINT('Ctrl Pts',(31.3725732548101,-34.4640617531158,-1.67269218670119E-15));
#32788=CARTESIAN_POINT('Ctrl Pts',(31.3496376837557,-34.5796386183165,-1.85962356624714E-15));
#32789=CARTESIAN_POINT('Ctrl Pts',(31.3256626239872,-34.7004536721242,-2.05502707229468E-15));
#32790=CARTESIAN_POINT('Ctrl Pts',(31.3075330179638,-34.8223688186784,-6.90474885500916E-16));
#32791=CARTESIAN_POINT('Ctrl Pts',(31.2953872940185,-34.9449317101526,1.11022302462516E-16));
#32792=CARTESIAN_POINT('Ctrl Pts',(31.2862780010595,-35.0368538787582,7.12145193435089E-16));
#32793=CARTESIAN_POINT('Ctrl Pts',(31.2805357649583,-35.1291410005731,-7.33619512718545E-16));
#32794=CARTESIAN_POINT('Ctrl Pts',(31.2782421142109,-35.2216056948398,-3.88578058618805E-16));
#32795=CARTESIAN_POINT('Ctrl Pts',(31.2776945327762,-35.2436805246709,-3.0620357564075E-16));
#32796=CARTESIAN_POINT('Ctrl Pts',(31.2773436607928,-35.2657700018002,-4.90649572448904E-16));
#32797=CARTESIAN_POINT('Ctrl Pts',(31.2771907100455,-35.287842514156,-5.27355936696949E-16));
#32798=CARTESIAN_POINT('Ctrl Pts',(31.2763557493203,-35.4083367336975,-7.27736602069211E-16));
#32799=CARTESIAN_POINT('Ctrl Pts',(31.2814089690861,-35.5284761575602,-1.32546033095374E-15));
#32800=CARTESIAN_POINT('Ctrl Pts',(31.2924193361456,-35.6478347566642,-1.0547118733939E-15));
#32801=CARTESIAN_POINT('Ctrl Pts',(31.3033590399359,-35.7664273260093,-7.85701048289603E-16));
#32802=CARTESIAN_POINT('Ctrl Pts',(31.3201794237171,-35.8842499373544,-3.19095490877261E-16));
#32803=CARTESIAN_POINT('Ctrl Pts',(31.3429975699143,-36.0008975571309,1.94289029309402E-16));
#32804=CARTESIAN_POINT('Ctrl Pts',(31.3458712257766,-36.0155878441288,2.58943292776536E-16));
#32805=CARTESIAN_POINT('Ctrl Pts',(31.3488400749734,-36.030259502248,-2.41414676176044E-15));
#32806=CARTESIAN_POINT('Ctrl Pts',(31.3519044105546,-36.0449117261916,-2.44249065417534E-15));
#32807=CARTESIAN_POINT('Ctrl Pts',(31.375814852164,-36.1592403092631,-2.71916393553799E-15));
#32808=CARTESIAN_POINT('Ctrl Pts',(31.4055345217229,-36.272386206175,5.65793814005205E-16));
#32809=CARTESIAN_POINT('Ctrl Pts',(31.4407572695548,-36.384082920097,4.44089209850063E-16));
#32810=CARTESIAN_POINT('Ctrl Pts',(31.4627225424769,-36.453738155898,3.68192949317207E-16));
#32811=CARTESIAN_POINT('Ctrl Pts',(31.4868289857256,-36.52282973013,-1.13814971295829E-15));
#32812=CARTESIAN_POINT('Ctrl Pts',(31.513012205469,-36.5912908274846,-1.69309011255336E-15));
#32813=CARTESIAN_POINT('Ctrl Pts',(31.5219624105717,-36.6146928715758,-1.88278528544959E-15));
#32814=CARTESIAN_POINT('Ctrl Pts',(31.531155343526,-36.6380212260425,4.03667916851762E-15));
#32815=CARTESIAN_POINT('Ctrl Pts',(31.5405886194687,-36.6612731534534,4.32986979603811E-15));
#32816=CARTESIAN_POINT('Ctrl Pts',(31.5473370498667,-36.6779072490427,4.53961416853196E-15));
#32817=CARTESIAN_POINT('Ctrl Pts',(31.5542090296369,-36.6945033501966,3.07759665647771E-15));
#32818=CARTESIAN_POINT('Ctrl Pts',(31.561196617679,-36.7110441569158,2.94209101525666E-15));
#32819=CARTESIAN_POINT('Ctrl Pts',(31.6071179522689,-36.8197477489354,2.0515691568155E-15));
#32820=CARTESIAN_POINT('Ctrl Pts',(31.6580923235038,-36.9262249725842,4.21341387307547E-15));
#32821=CARTESIAN_POINT('Ctrl Pts',(31.7137612878297,-37.0302214764794,3.42781358853017E-15));
#32822=CARTESIAN_POINT('Ctrl Pts',(31.7713455134326,-37.1377959250922,2.61518514166327E-15));
#32823=CARTESIAN_POINT('Ctrl Pts',(31.8339530898433,-37.2427167108642,9.07249106506457E-16));
#32824=CARTESIAN_POINT('Ctrl Pts',(31.9012426720394,-37.3446949826671,6.80011602582908E-16));
#32825=CARTESIAN_POINT('Ctrl Pts',(31.9691654564611,-37.4476328810058,4.50635769240332E-16));
#32826=CARTESIAN_POINT('Ctrl Pts',(32.0418592122967,-37.5475733704053,-1.57902851375934E-15));
#32827=CARTESIAN_POINT('Ctrl Pts',(32.1190233809196,-37.6442010945393,-1.81799020282369E-15));
#32828=CARTESIAN_POINT('Ctrl Pts',(32.1734366012044,-37.712339269715,-1.98649684598102E-15));
#32829=CARTESIAN_POINT('Ctrl Pts',(32.2300738179544,-37.7788298007494,1.23701449661782E-16));
#32830=CARTESIAN_POINT('Ctrl Pts',(32.2888426956766,-37.8435536257978,-3.88578058618805E-16));
#32831=CARTESIAN_POINT('Ctrl Pts',(32.3150744390812,-37.8724433857632,-6.17236238483284E-16));
#32832=CARTESIAN_POINT('Ctrl Pts',(32.3417310110036,-37.9009810526196,1.30430196317008E-16));
#32833=CARTESIAN_POINT('Ctrl Pts',(32.3688048104485,-37.9291554653168,-2.77555756156289E-17));
#32834=CARTESIAN_POINT('Ctrl Pts',(32.3804263297313,-37.9412494265322,-9.56573491554205E-17));
#32835=CARTESIAN_POINT('Ctrl Pts',(32.392123309834,-37.9532749179279,-6.28475541027777E-16));
#32836=CARTESIAN_POINT('Ctrl Pts',(32.4038886430803,-37.9652246721857,-5.96744875736022E-16));
#32837=CARTESIAN_POINT('Ctrl Pts',(32.4923309120516,-38.05505326931,-3.5821937240873E-16));
#32838=CARTESIAN_POINT('Ctrl Pts',(32.5847325176906,-38.1407092470896,2.11600168392725E-15));
#32839=CARTESIAN_POINT('Ctrl Pts',(32.6807647145451,-38.221874449736,1.96370697480575E-15));
#32840=CARTESIAN_POINT('Ctrl Pts',(32.7628051861864,-38.2912140225467,1.8336013417573E-15));
#32841=CARTESIAN_POINT('Ctrl Pts',(32.8474963866317,-38.3572760203649,1.20960812321559E-15));
#32842=CARTESIAN_POINT('Ctrl Pts',(32.9346575664231,-38.4198445069104,5.62050406216485E-16));
#32843=CARTESIAN_POINT('Ctrl Pts',(32.973768957553,-38.4479205443796,2.71475138541893E-16));
#32844=CARTESIAN_POINT('Ctrl Pts',(33.0133779626213,-38.4752928979382,3.47992543175087E-15));
#32845=CARTESIAN_POINT('Ctrl Pts',(33.0534694930906,-38.5019407001488,3.78169717762944E-15));
#32846=CARTESIAN_POINT('Ctrl Pts',(33.0807047104967,-38.5200432439556,3.98669855846499E-15));
#32847=CARTESIAN_POINT('Ctrl Pts',(33.108168250427,-38.5378147929466,1.27528005472796E-15));
#32848=CARTESIAN_POINT('Ctrl Pts',(33.1358254185318,-38.5552300293176,1.47104550762833E-15));
#32849=CARTESIAN_POINT('Ctrl Pts',(33.2426299049644,-38.6224829515854,2.22703862229035E-15));
#32850=CARTESIAN_POINT('Ctrl Pts',(33.3523811032195,-38.6844690524263,5.56024339803508E-15));
#32851=CARTESIAN_POINT('Ctrl Pts',(33.4647770313827,-38.7408546683214,3.76781938982163E-15));
#32852=CARTESIAN_POINT('Ctrl Pts',(33.5668706528472,-38.7920719305417,2.13969049592827E-15));
#32853=CARTESIAN_POINT('Ctrl Pts',(33.6711471781243,-38.8386683831236,1.86420798495096E-15));
#32854=CARTESIAN_POINT('Ctrl Pts',(33.7774036389012,-38.880364855251,2.14498557804532E-15));
#32855=CARTESIAN_POINT('Ctrl Pts',(33.8328341927383,-38.9021165541705,2.26717202503918E-15));
#32856=CARTESIAN_POINT('Ctrl Pts',(33.8888038950002,-38.9225342787199,1.50877474080585E-16));
#32857=CARTESIAN_POINT('Ctrl Pts',(33.94526862329,-38.9416301412996,1.94289029309402E-16));
#32858=CARTESIAN_POINT('Ctrl Pts',(31.4846885160394,-34.9971888045819,7.11258330249198));
#32859=CARTESIAN_POINT('Ctrl Pts',(31.4819573643756,-34.6461972356202,7.09672411194512));
#32860=CARTESIAN_POINT('Ctrl Pts',(31.5304047798457,-34.2959415119622,7.08086492139826));
#32861=CARTESIAN_POINT('Ctrl Pts',(31.6331819033213,-33.9624301234347,7.0650057308514));
#32862=CARTESIAN_POINT('Ctrl Pts',(31.9723337540393,-32.8618836124063,7.01267235506732));
#32863=CARTESIAN_POINT('Ctrl Pts',(32.9030919679943,-31.943669301846,6.96033897928324));
#32864=CARTESIAN_POINT('Ctrl Pts',(34.0081264335795,-31.6194492096822,6.90800560349915));
#32865=CARTESIAN_POINT('Ctrl Pts',(35.1131608991647,-31.2952291175184,6.85567222771506));
#32866=CARTESIAN_POINT('Ctrl Pts',(36.3924716163801,-31.5650032437512,6.80333885193098));
#32867=CARTESIAN_POINT('Ctrl Pts',(37.2724835206594,-32.3078288702224,6.75100547614689));
#32868=CARTESIAN_POINT('Ctrl Pts',(38.1524954249387,-33.0506544966935,6.69867210036281));
#32869=CARTESIAN_POINT('Ctrl Pts',(38.6332085162819,-34.2665316234029,6.64633872457873));
#32870=CARTESIAN_POINT('Ctrl Pts',(38.4990877924354,-35.4103100458006,6.59400534879464));
#32871=CARTESIAN_POINT('Ctrl Pts',(38.3649670685888,-36.5540884681983,6.54167197301056));
#32872=CARTESIAN_POINT('Ctrl Pts',(37.6160125295525,-37.6257681862843,6.48933859722647));
#32873=CARTESIAN_POINT('Ctrl Pts',(36.5880240094475,-38.1448593691216,6.43700522144239));
#32874=CARTESIAN_POINT('Ctrl Pts',(35.5600354893424,-38.663950551959,6.3846718456583));
#32875=CARTESIAN_POINT('Ctrl Pts',(34.2530129881685,-38.6304531995479,6.33233846987422));
#32876=CARTESIAN_POINT('Ctrl Pts',(33.2529650852691,-38.0593845647942,6.28000509409014));
#32877=CARTESIAN_POINT('Ctrl Pts',(32.2529171823696,-37.4883159300405,6.22767171830605));
#32878=CARTESIAN_POINT('Ctrl Pts',(31.5598438777445,-36.3796760129444,6.17533834252196));
#32879=CARTESIAN_POINT('Ctrl Pts',(31.4844885221415,-35.230529556181,6.12300496673788));
#32880=CARTESIAN_POINT('Ctrl Pts',(31.4794864356562,-35.1542492451791,6.11953107865591));
#32881=CARTESIAN_POINT('Ctrl Pts',(31.4772062002897,-35.0777904501775,6.11605719057394));
#32882=CARTESIAN_POINT('Ctrl Pts',(31.4775766908735,-35.0013091813966,6.11258330249198));
#32883=CARTESIAN_POINT('Origin',(-35.,35.,10.2084234471775));
#32884=CARTESIAN_POINT('Ctrl Pts',(-39.0784090602678,35.0020440536088,7.70842344717747));
#32885=CARTESIAN_POINT('Ctrl Pts',(-39.0792531838394,35.133112279499,7.70328437820512));
#32886=CARTESIAN_POINT('Ctrl Pts',(-39.0145240110799,36.5980970201662,7.64581193344869));
#32887=CARTESIAN_POINT('Ctrl Pts',(-37.2468179015868,39.238437726829,7.53600611290815));
#32888=CARTESIAN_POINT('Ctrl Pts',(-32.7044909023729,39.2117683922069,7.37900598555592));
#32889=CARTESIAN_POINT('Ctrl Pts',(-30.2206292307696,35.4089492839864,7.22200585820365));
#32890=CARTESIAN_POINT('Ctrl Pts',(-32.0224452414743,31.2391318114334,7.0650057308514));
#32891=CARTESIAN_POINT('Ctrl Pts',(-36.4942780330333,30.4418647129305,6.90800560349915));
#32892=CARTESIAN_POINT('Ctrl Pts',(-38.8653529438983,32.9326279141667,6.7891448422745));
#32893=CARTESIAN_POINT('Ctrl Pts',(-39.0751757451768,34.6330161300415,6.72261745683394));
#32894=CARTESIAN_POINT('Ctrl Pts',(-39.0721136942453,34.9965451882256,6.70842344717746));
#32895=CARTESIAN_POINT('Ctrl Pts',(-39.0691248821302,34.9959228837483,7.79157655282255));
#32896=CARTESIAN_POINT('Ctrl Pts',(-39.0629617588157,35.8984240805364,7.75638428364687));
#32897=CARTESIAN_POINT('Ctrl Pts',(-38.3270254278953,38.1550448362135,7.6688586386871));
#32898=CARTESIAN_POINT('Ctrl Pts',(-34.6204731393245,39.7808563212243,7.52899961794324));
#32899=CARTESIAN_POINT('Ctrl Pts',(-30.8030827008644,37.3225569109026,7.37199949059099));
#32900=CARTESIAN_POINT('Ctrl Pts',(-30.7475658132336,32.7797862032913,7.21499936323873));
#32901=CARTESIAN_POINT('Ctrl Pts',(-34.5060130464714,30.2288015790917,7.05799923588648));
#32902=CARTESIAN_POINT('Ctrl Pts',(-38.2826807551488,31.7813043056651,6.91685829908108));
#32903=CARTESIAN_POINT('Ctrl Pts',(-39.0636920303636,34.0684206251935,6.82805073805977));
#32904=CARTESIAN_POINT('Ctrl Pts',(-39.070966199943,35.0032555604945,6.79157655282255));
#32905=CARTESIAN_POINT('Ctrl Pts',(-32.3264680662287,37.2858331630075,8.));
#32906=CARTESIAN_POINT('Ctrl Pts',(-31.5748397248436,36.4067215963625,7.94766662421592));
#32907=CARTESIAN_POINT('Ctrl Pts',(-31.0185734566188,33.863789346735,7.84299987264775));
#32908=CARTESIAN_POINT('Ctrl Pts',(-33.7549107807148,31.0470722659105,7.68599974529549));
#32909=CARTESIAN_POINT('Ctrl Pts',(-37.6085229887763,31.7834906538058,7.52899961794324));
#32910=CARTESIAN_POINT('Ctrl Pts',(-39.122629437071,35.4000496587684,7.37199949059099));
#32911=CARTESIAN_POINT('Ctrl Pts',(-36.9401453219176,38.6599250531781,7.21499936323873));
#32912=CARTESIAN_POINT('Ctrl Pts',(-33.0178094388356,38.6368958683166,7.05799923588648));
#32913=CARTESIAN_POINT('Ctrl Pts',(-30.8729749157314,35.3531309945801,6.90099910853423));
#32914=CARTESIAN_POINT('Ctrl Pts',(-32.4288575271599,31.7524600826604,6.74399898118197));
#32915=CARTESIAN_POINT('Ctrl Pts',(-36.2903210951748,31.0640135332596,6.58699885382972));
#32916=CARTESIAN_POINT('Ctrl Pts',(-38.9947349861635,33.9049421642868,6.42999872647747));
#32917=CARTESIAN_POINT('Ctrl Pts',(-38.1170348549754,37.7278502673058,6.27299859912521));
#32918=CARTESIAN_POINT('Ctrl Pts',(-34.4442580951562,39.1046536709688,6.11599847177296));
#32919=CARTESIAN_POINT('Ctrl Pts',(-31.2698212127753,36.8007822935419,5.95899834442071));
#32920=CARTESIAN_POINT('Ctrl Pts',(-31.4402710474498,32.8821284121656,5.80199821706844));
#32921=CARTESIAN_POINT('Ctrl Pts',(-34.8027641765881,30.8625921610582,5.6449980897162));
#32922=CARTESIAN_POINT('Ctrl Pts',(-38.3421204653421,32.553108288411,5.48799796236394));
#32923=CARTESIAN_POINT('Ctrl Pts',(-38.884565317352,36.4377761463179,5.33099783501169));
#32924=CARTESIAN_POINT('Ctrl Pts',(-35.9436831589371,39.0331761128571,5.17399770765944));
#32925=CARTESIAN_POINT('Ctrl Pts',(-32.1565912702954,38.0119884794394,5.01699758030718));
#32926=CARTESIAN_POINT('Ctrl Pts',(-30.9192112622106,34.2899218247053,4.85999745295493));
#32927=CARTESIAN_POINT('Ctrl Pts',(-33.3411136674927,31.2045891097909,4.70299732560268));
#32928=CARTESIAN_POINT('Ctrl Pts',(-37.2505553603438,31.522637737819,4.54599719825043));
#32929=CARTESIAN_POINT('Ctrl Pts',(-39.1419024714255,34.9588704735221,4.38899707089817));
#32930=CARTESIAN_POINT('Ctrl Pts',(-37.3191659004311,38.4319844467691,4.23199694354592));
#32931=CARTESIAN_POINT('Ctrl Pts',(-33.4168110175916,38.8276050433616,4.07499681619367));
#32932=CARTESIAN_POINT('Ctrl Pts',(-30.9341168836852,35.7909754762728,3.91799668884141));
#32933=CARTESIAN_POINT('Ctrl Pts',(-32.0973391464029,32.0450706119108,3.76099656148916));
#32934=CARTESIAN_POINT('Ctrl Pts',(-35.8634052436587,30.9488792776308,3.6039964341369));
#32935=CARTESIAN_POINT('Ctrl Pts',(-38.8552475752543,33.4853667605377,3.44699630678465));
#32936=CARTESIAN_POINT('Ctrl Pts',(-38.390052421646,37.3800403986573,3.2899961794324));
#32937=CARTESIAN_POINT('Ctrl Pts',(-34.8849647366394,39.1405089808617,3.13299605208014));
#32938=CARTESIAN_POINT('Ctrl Pts',(-31.4830302803583,37.1881434324151,2.97599592472789));
#32939=CARTESIAN_POINT('Ctrl Pts',(-31.2347963029507,33.2736486866154,2.81899579737564));
#32940=CARTESIAN_POINT('Ctrl Pts',(-34.3628566205626,30.9071897040694,2.66199567002338));
#32941=CARTESIAN_POINT('Ctrl Pts',(-38.0622494824414,32.2107930214718,2.50499554267113));
#32942=CARTESIAN_POINT('Ctrl Pts',(-39.0156939291453,36.0155049084671,2.34799541531888));
#32943=CARTESIAN_POINT('Ctrl Pts',(-36.368226956474,38.9096039759392,2.19099528796663));
#32944=CARTESIAN_POINT('Ctrl Pts',(-32.4938580444355,38.2979233002502,2.03399516061437));
#32945=CARTESIAN_POINT('Ctrl Pts',(-30.8667700651969,34.7289638691476,1.87699503326212));
#32946=CARTESIAN_POINT('Ctrl Pts',(-32.9459902326247,31.4030437132317,1.71999490590986));
#32947=CARTESIAN_POINT('Ctrl Pts',(-36.8670582231188,31.3025516345889,1.56299477855761));
#32948=CARTESIAN_POINT('Ctrl Pts',(-39.1139221090429,34.517591201676,1.40599465120536));
#32949=CARTESIAN_POINT('Ctrl Pts',(-37.6717826711976,38.1652229986406,1.2489945238531));
#32950=CARTESIAN_POINT('Ctrl Pts',(-33.8338500234071,38.9745455371789,1.09199439650085));
#32951=CARTESIAN_POINT('Ctrl Pts',(-31.041575077848,36.2199021542904,0.934994269148598));
#32952=CARTESIAN_POINT('Ctrl Pts',(-31.7989386437116,32.3712657534865,0.777994141796342));
#32953=CARTESIAN_POINT('Ctrl Pts',(-35.4265616731752,30.8800320247936,0.620994014444089));
#32954=CARTESIAN_POINT('Ctrl Pts',(-38.6720109988941,33.0828274754107,0.463993887091835));
#32955=CARTESIAN_POINT('Ctrl Pts',(-38.6240716788406,37.0055467263343,0.306993759739582));
#32956=CARTESIAN_POINT('Ctrl Pts',(-35.3277244750448,39.1283073075518,0.149993632387328));
#32957=CARTESIAN_POINT('Ctrl Pts',(-31.734817208837,37.552345230412,-0.00700649496492534));
#32958=CARTESIAN_POINT('Ctrl Pts',(-31.0753017580586,33.6811081626476,-0.164006622317179));
#32959=CARTESIAN_POINT('Ctrl Pts',(-32.9741442474368,31.9005650466595,-0.268673373885348));
#32960=CARTESIAN_POINT('Ctrl Pts',(-34.0915279074966,31.601840982658,-0.321006749669432));
#32961=CARTESIAN_POINT('Ctrl Pts',(-32.1856025125516,37.4062712808594,8.10700224988981));
#32962=CARTESIAN_POINT('Ctrl Pts',(-31.3943716733878,36.4808402609044,8.05466887410573));
#32963=CARTESIAN_POINT('Ctrl Pts',(-30.8087963272068,33.8039236160346,7.95000212253756));
#32964=CARTESIAN_POINT('Ctrl Pts',(-33.6893083541881,30.8387967084451,7.79300199518531));
#32965=CARTESIAN_POINT('Ctrl Pts',(-37.7459632902934,31.614016197849,7.63600186783304));
#32966=CARTESIAN_POINT('Ctrl Pts',(-39.3398463967498,35.4211278497445,7.47900174048081));
#32967=CARTESIAN_POINT('Ctrl Pts',(-37.0423695151407,38.8527626110617,7.32200161312853));
#32968=CARTESIAN_POINT('Ctrl Pts',(-32.9133699266814,38.8285200429468,7.1650014857763));
#32969=CARTESIAN_POINT('Ctrl Pts',(-30.6555263540774,35.3717370910488,7.00800135842403));
#32970=CARTESIAN_POINT('Ctrl Pts',(-32.2933867652647,31.5813506589181,6.85100123107178));
#32971=CARTESIAN_POINT('Ctrl Pts',(-36.3583067411276,30.8566305931499,6.69400110371953));
#32972=CARTESIAN_POINT('Ctrl Pts',(-39.2052133232691,33.8472447317679,6.53700097636727));
#32973=CARTESIAN_POINT('Ctrl Pts',(-38.2812681058037,37.8715777961968,6.38000084901503));
#32974=CARTESIAN_POINT('Ctrl Pts',(-34.4149766453488,39.3209235066531,6.22300072166276));
#32975=CARTESIAN_POINT('Ctrl Pts',(-31.0732820603757,36.8956635970443,6.06600059431052));
#32976=CARTESIAN_POINT('Ctrl Pts',(-31.2527127155268,32.770540011044,5.90900046695826));
#32977=CARTESIAN_POINT('Ctrl Pts',(-34.7923720308581,30.644596543105,5.75200033960601));
#32978=CARTESIAN_POINT('Ctrl Pts',(-38.5182132375505,32.424184166957,5.59500021225375));
#32979=CARTESIAN_POINT('Ctrl Pts',(-39.0892389317987,36.5135310420632,5.43800008490151));
#32980=CARTESIAN_POINT('Ctrl Pts',(-35.9934048207584,39.2456798720372,5.28099995754924));
#32981=CARTESIAN_POINT('Ctrl Pts',(-32.0067750889435,38.1706869484817,5.12399983019699));
#32982=CARTESIAN_POINT('Ctrl Pts',(-30.7041988444697,34.2525085609798,4.96699970284475));
#32983=CARTESIAN_POINT('Ctrl Pts',(-33.2537087112384,31.0046129472743,4.80999957549248));
#32984=CARTESIAN_POINT('Ctrl Pts',(-37.3691347282993,31.3394192191957,4.65299944814024));
#32985=CARTESIAN_POINT('Ctrl Pts',(-39.3601349067833,34.9567034025226,4.49599932078798));
#32986=CARTESIAN_POINT('Ctrl Pts',(-37.4413602847608,38.6128120565681,4.33899919343573));
#32987=CARTESIAN_POINT('Ctrl Pts',(-33.3333944741925,39.0292774815619,4.18199906608348));
#32988=CARTESIAN_POINT('Ctrl Pts',(-30.7198898272843,35.8326511327341,4.02499893873122));
#32989=CARTESIAN_POINT('Ctrl Pts',(-31.9444010336713,31.8893785256963,3.86799881137897));
#32990=CARTESIAN_POINT('Ctrl Pts',(-35.9088971475179,30.7354300360637,3.71099868402671));
#32991=CARTESIAN_POINT('Ctrl Pts',(-39.0583764690558,33.4055623463097,3.55399855667446));
#32992=CARTESIAN_POINT('Ctrl Pts',(-38.5686706776456,37.5054421955447,3.39699842932221));
#32993=CARTESIAN_POINT('Ctrl Pts',(-34.8789036509792,39.3586679946839,3.23999830196995));
#32994=CARTESIAN_POINT('Ctrl Pts',(-31.297724886933,37.3034343822775,3.0829981746177));
#32995=CARTESIAN_POINT('Ctrl Pts',(-31.0364117253094,33.1826890722831,2.92599804726545));
#32996=CARTESIAN_POINT('Ctrl Pts',(-34.3292862136479,30.6915438832177,2.76899791991319));
#32997=CARTESIAN_POINT('Ctrl Pts',(-38.2235961502677,32.0638326727334,2.61199779256094));
#32998=CARTESIAN_POINT('Ctrl Pts',(-39.2272765706619,36.0690107818723,2.45499766520869));
#32999=CARTESIAN_POINT('Ctrl Pts',(-36.440317379388,39.1155968506723,2.29799753785644));
#33000=CARTESIAN_POINT('Ctrl Pts',(-32.3618120906526,38.4716873708438,2.14099741050418));
#33001=CARTESIAN_POINT('Ctrl Pts',(-30.6489945765686,34.714683263722,1.98399728315193));
#33002=CARTESIAN_POINT('Ctrl Pts',(-32.8377666428914,31.2135239126685,1.82699715579967));
#33003=CARTESIAN_POINT('Ctrl Pts',(-36.965431534851,31.1077370132983,1.66999702844742));
#33004=CARTESIAN_POINT('Ctrl Pts',(-39.3306802888702,34.4921735952445,1.51299690109517));
#33005=CARTESIAN_POINT('Ctrl Pts',(-37.8125560580904,38.3319952314996,1.35599677374291));
#33006=CARTESIAN_POINT('Ctrl Pts',(-33.7724068216079,39.1839601136936,1.19899664639066));
#33007=CARTESIAN_POINT('Ctrl Pts',(-30.8330098793911,36.2841775011547,1.04199651903841));
#33008=CARTESIAN_POINT('Ctrl Pts',(-31.6302781259105,32.2327605422985,0.884996391686154));
#33009=CARTESIAN_POINT('Ctrl Pts',(-35.4490367539887,30.6629552947093,0.7279962643339));
#33010=CARTESIAN_POINT('Ctrl Pts',(-38.8654853524014,32.981813694442,0.570996136981647));
#33011=CARTESIAN_POINT('Ctrl Pts',(-38.8150201605686,37.1112168499867,0.413996009629392));
#33012=CARTESIAN_POINT('Ctrl Pts',(-35.3449919290248,39.3458234281866,0.256995882277139));
#33013=CARTESIAN_POINT('Ctrl Pts',(-31.5627782008402,37.6868255855989,0.0999957549248854));
#33014=CARTESIAN_POINT('Ctrl Pts',(-30.8685135825059,33.611617154681,-0.0570043724273683));
#33015=CARTESIAN_POINT('Ctrl Pts',(-32.8674040627957,31.7372591159268,-0.161671123995537));
#33016=CARTESIAN_POINT('Ctrl Pts',(-34.0436614793107,31.4227955987545,-0.214004499779622));
#33017=CARTESIAN_POINT('Ctrl Pts',(-32.0447369588746,37.5267093987113,8.21400449977962));
#33018=CARTESIAN_POINT('Ctrl Pts',(-31.2139036219321,36.5549589254462,8.16167112399554));
#33019=CARTESIAN_POINT('Ctrl Pts',(-30.5990191977949,33.7440578853343,8.05700437242737));
#33020=CARTESIAN_POINT('Ctrl Pts',(-33.6237059276614,30.6305211509797,7.90000424507511));
#33021=CARTESIAN_POINT('Ctrl Pts',(-37.8834035918105,31.4445417418923,7.74300411772286));
#33022=CARTESIAN_POINT('Ctrl Pts',(-39.5570633564287,35.4422060407206,7.58600399037061));
#33023=CARTESIAN_POINT('Ctrl Pts',(-37.1445937083637,39.0456001689453,7.42900386301835));
#33024=CARTESIAN_POINT('Ctrl Pts',(-32.8089304145272,39.0201442175769,7.27200373566611));
#33025=CARTESIAN_POINT('Ctrl Pts',(-30.4380777924235,35.3903431875176,7.11500360831384));
#33026=CARTESIAN_POINT('Ctrl Pts',(-32.1579160033695,31.4102412351758,6.9580034809616));
#33027=CARTESIAN_POINT('Ctrl Pts',(-36.4262923870805,30.6492476530402,6.80100335360934));
#33028=CARTESIAN_POINT('Ctrl Pts',(-39.4156916603747,33.7895472992489,6.64400322625709));
#33029=CARTESIAN_POINT('Ctrl Pts',(-38.4455013566321,38.0153053250877,6.48700309890483));
#33030=CARTESIAN_POINT('Ctrl Pts',(-34.3856951955414,39.5371933423375,6.33000297155258));
#33031=CARTESIAN_POINT('Ctrl Pts',(-30.876742907976,36.9905449005467,6.17300284420033));
#33032=CARTESIAN_POINT('Ctrl Pts',(-31.0651543836038,32.6589516099224,6.01600271684807));
#33033=CARTESIAN_POINT('Ctrl Pts',(-34.781979885128,30.4266009251517,5.85900258949583));
#33034=CARTESIAN_POINT('Ctrl Pts',(-38.694306009759,32.295260045503,5.70200246214356));
#33035=CARTESIAN_POINT('Ctrl Pts',(-39.2939125462453,36.5892859378086,5.54500233479132));
#33036=CARTESIAN_POINT('Ctrl Pts',(-36.0431264825797,39.4581836312174,5.38800220743905));
#33037=CARTESIAN_POINT('Ctrl Pts',(-31.8569589075916,38.3293854175239,5.23100208008681));
#33038=CARTESIAN_POINT('Ctrl Pts',(-30.4891864267288,34.2150952972543,5.07400195273455));
#33039=CARTESIAN_POINT('Ctrl Pts',(-33.166303754984,30.8046367847576,4.9170018253823));
#33040=CARTESIAN_POINT('Ctrl Pts',(-37.487714096255,31.1562007005724,4.76000169803004));
#33041=CARTESIAN_POINT('Ctrl Pts',(-39.578367342141,34.9545363315231,4.60300157067779));
#33042=CARTESIAN_POINT('Ctrl Pts',(-37.5635546690906,38.7936396663671,4.44600144332554));
#33043=CARTESIAN_POINT('Ctrl Pts',(-33.2499779307934,39.2309499197622,4.28900131597329));
#33044=CARTESIAN_POINT('Ctrl Pts',(-30.5056627708833,35.8743267891954,4.13200118862103));
#33045=CARTESIAN_POINT('Ctrl Pts',(-31.7914629209398,31.7336864394819,3.97500106126878));
#33046=CARTESIAN_POINT('Ctrl Pts',(-35.9543890513771,30.5219807944966,3.81800093391652));
#33047=CARTESIAN_POINT('Ctrl Pts',(-39.2615053628575,33.3257579320817,3.66100080656427));
#33048=CARTESIAN_POINT('Ctrl Pts',(-38.747288933645,37.630843992432,3.50400067921202));
#33049=CARTESIAN_POINT('Ctrl Pts',(-34.8728425653191,39.5768270085061,3.34700055185976));
#33050=CARTESIAN_POINT('Ctrl Pts',(-31.1124194935077,37.4187253321399,3.19000042450751));
#33051=CARTESIAN_POINT('Ctrl Pts',(-30.8380271476682,33.0917294579507,3.03300029715526));
#33052=CARTESIAN_POINT('Ctrl Pts',(-34.2957158067332,30.4758980623661,2.87600016980301));
#33053=CARTESIAN_POINT('Ctrl Pts',(-38.3849428180941,31.916872323995,2.71900004245075));
#33054=CARTESIAN_POINT('Ctrl Pts',(-39.4388592121786,36.1225166552775,2.5619999150985));
#33055=CARTESIAN_POINT('Ctrl Pts',(-36.5124078023019,39.3215897254055,2.40499978774625));
#33056=CARTESIAN_POINT('Ctrl Pts',(-32.2297661368697,38.6454514414374,2.24799966039399));
#33057=CARTESIAN_POINT('Ctrl Pts',(-30.4312190879402,34.7004026582963,2.09099953304174));
#33058=CARTESIAN_POINT('Ctrl Pts',(-32.7295430531581,31.0240041121053,1.93399940568948));
#33059=CARTESIAN_POINT('Ctrl Pts',(-37.0638048465832,30.9129223920078,1.77699927833723));
#33060=CARTESIAN_POINT('Ctrl Pts',(-39.5474384686975,34.466755988813,1.61999915098498));
#33061=CARTESIAN_POINT('Ctrl Pts',(-37.9533294449832,38.4987674643586,1.46299902363273));
#33062=CARTESIAN_POINT('Ctrl Pts',(-33.7109636198088,39.3933746902084,1.30599889628047));
#33063=CARTESIAN_POINT('Ctrl Pts',(-30.6244446809342,36.348452848019,1.14899876892822));
#33064=CARTESIAN_POINT('Ctrl Pts',(-31.4616176081094,32.0942553311105,0.991998641575964));
#33065=CARTESIAN_POINT('Ctrl Pts',(-35.4715118348024,30.445878564625,0.834998514223711));
#33066=CARTESIAN_POINT('Ctrl Pts',(-39.0589597059086,32.8807999134734,0.677998386871457));
#33067=CARTESIAN_POINT('Ctrl Pts',(-39.0059686422967,37.2168869736391,0.520998259519203));
#33068=CARTESIAN_POINT('Ctrl Pts',(-35.3622593830049,39.5633395488214,0.36399813216695));
#33069=CARTESIAN_POINT('Ctrl Pts',(-31.3907391928433,37.8213059407857,0.206998004814696));
#33070=CARTESIAN_POINT('Ctrl Pts',(-30.6617254069532,33.5421261467143,0.0499978774624425));
#33071=CARTESIAN_POINT('Ctrl Pts',(-32.7606638781546,31.573953185194,-0.0546688741057264));
#33072=CARTESIAN_POINT('Ctrl Pts',(-33.9957950511247,31.243750214851,-0.107002249889811));
#33073=CARTESIAN_POINT('Ctrl Pts',(-31.9038714051976,37.6471475165632,8.32100674966943));
#33074=CARTESIAN_POINT('Ctrl Pts',(-31.0334355704763,36.629077589988,8.26867337388535));
#33075=CARTESIAN_POINT('Ctrl Pts',(-30.3892420683829,33.6841921546339,8.16400662231718));
#33076=CARTESIAN_POINT('Ctrl Pts',(-33.5581035011348,30.4222455935143,8.00700649496493));
#33077=CARTESIAN_POINT('Ctrl Pts',(-38.0208438933277,31.2750672859355,7.85000636761266));
#33078=CARTESIAN_POINT('Ctrl Pts',(-39.7742803161076,35.4632842316967,7.69300624026044));
#33079=CARTESIAN_POINT('Ctrl Pts',(-37.2468179015868,39.238437726829,7.53600611290815));
#33080=CARTESIAN_POINT('Ctrl Pts',(-32.7044909023729,39.2117683922069,7.37900598555592));
#33081=CARTESIAN_POINT('Ctrl Pts',(-30.2206292307696,35.4089492839864,7.22200585820365));
#33082=CARTESIAN_POINT('Ctrl Pts',(-32.0224452414743,31.2391318114334,7.0650057308514));
#33083=CARTESIAN_POINT('Ctrl Pts',(-36.4942780330333,30.4418647129305,6.90800560349915));
#33084=CARTESIAN_POINT('Ctrl Pts',(-39.6261699974803,33.7318498667299,6.7510054761469));
#33085=CARTESIAN_POINT('Ctrl Pts',(-38.6097346074605,38.1590328539788,6.59400534879465));
#33086=CARTESIAN_POINT('Ctrl Pts',(-34.3564137457339,39.7534631780217,6.4370052214424));
#33087=CARTESIAN_POINT('Ctrl Pts',(-30.6802037555765,37.0854262040492,6.28000509409013));
#33088=CARTESIAN_POINT('Ctrl Pts',(-30.8775960516807,32.5473632088007,6.12300496673789));
#33089=CARTESIAN_POINT('Ctrl Pts',(-34.7715877393978,30.2086053071985,5.96600483938563));
#33090=CARTESIAN_POINT('Ctrl Pts',(-38.8703987819675,32.166335924049,5.80900471203337));
#33091=CARTESIAN_POINT('Ctrl Pts',(-39.4985861606919,36.6650408335539,5.65200458468113));
#33092=CARTESIAN_POINT('Ctrl Pts',(-36.092848144401,39.6706873903976,5.49500445732886));
#33093=CARTESIAN_POINT('Ctrl Pts',(-31.7071427262397,38.4880838865661,5.33800432997662));
#33094=CARTESIAN_POINT('Ctrl Pts',(-30.2741740089879,34.1776820335287,5.18100420262436));
#33095=CARTESIAN_POINT('Ctrl Pts',(-33.0788987987297,30.6046606222411,5.02400407527212));
#33096=CARTESIAN_POINT('Ctrl Pts',(-37.6062934642105,30.9729821819491,4.86700394791985));
#33097=CARTESIAN_POINT('Ctrl Pts',(-39.7965997774987,34.9523692605237,4.7100038205676));
#33098=CARTESIAN_POINT('Ctrl Pts',(-37.6857490534203,38.974467276166,4.55300369321535));
#33099=CARTESIAN_POINT('Ctrl Pts',(-33.1665613873943,39.4326223579625,4.3960035658631));
#33100=CARTESIAN_POINT('Ctrl Pts',(-30.2914357144823,35.9160024456566,4.23900343851084));
#33101=CARTESIAN_POINT('Ctrl Pts',(-31.6385248082081,31.5779943532675,4.08200331115859));
#33102=CARTESIAN_POINT('Ctrl Pts',(-35.9998809552364,30.3085315529294,3.92500318380634));
#33103=CARTESIAN_POINT('Ctrl Pts',(-39.464634256659,33.2459535178537,3.76800305645409));
#33104=CARTESIAN_POINT('Ctrl Pts',(-38.9259071896446,37.7562457893193,3.61100292910183));
#33105=CARTESIAN_POINT('Ctrl Pts',(-34.866781479659,39.7949860223284,3.45400280174958));
#33106=CARTESIAN_POINT('Ctrl Pts',(-30.9271141000824,37.5340162820022,3.29700267439732));
#33107=CARTESIAN_POINT('Ctrl Pts',(-30.6396425700269,33.0007698436185,3.14000254704507));
#33108=CARTESIAN_POINT('Ctrl Pts',(-34.2621453998186,30.2602522415144,2.98300241969281));
#33109=CARTESIAN_POINT('Ctrl Pts',(-38.5462894859204,31.7699119752566,2.82600229234057));
#33110=CARTESIAN_POINT('Ctrl Pts',(-39.6504418536953,36.1760225286826,2.66900216498831));
#33111=CARTESIAN_POINT('Ctrl Pts',(-36.5844982252159,39.5275826001387,2.51200203763606));
#33112=CARTESIAN_POINT('Ctrl Pts',(-32.0977201830868,38.819215512031,2.3550019102838));
#33113=CARTESIAN_POINT('Ctrl Pts',(-30.2134435993119,34.6861220528707,2.19800178293155));
#33114=CARTESIAN_POINT('Ctrl Pts',(-32.6213194634248,30.8344843115421,2.04100165557929));
#33115=CARTESIAN_POINT('Ctrl Pts',(-37.1621781583154,30.7181077707172,1.88400152822704));
#33116=CARTESIAN_POINT('Ctrl Pts',(-39.7641966485248,34.4413383823816,1.72700140087479));
#33117=CARTESIAN_POINT('Ctrl Pts',(-38.0941028318759,38.6655396972175,1.57000127352254));
#33118=CARTESIAN_POINT('Ctrl Pts',(-33.6495204180096,39.602789266723,1.41300114617028));
#33119=CARTESIAN_POINT('Ctrl Pts',(-30.4158794824773,36.4127281948833,1.25600101881803));
#33120=CARTESIAN_POINT('Ctrl Pts',(-31.2929570903083,31.9557501199225,1.09900089146578));
#33121=CARTESIAN_POINT('Ctrl Pts',(-35.4939869156159,30.2288018345407,0.942000764113521));
#33122=CARTESIAN_POINT('Ctrl Pts',(-39.2524340594159,32.7797861325047,0.785000636761268));
#33123=CARTESIAN_POINT('Ctrl Pts',(-39.1969171240247,37.3225570972915,0.628000509409013));
#33124=CARTESIAN_POINT('Ctrl Pts',(-35.379526836985,39.7808556694562,0.471000382056761));
#33125=CARTESIAN_POINT('Ctrl Pts',(-31.2187001848465,37.9557862959725,0.314000254704507));
#33126=CARTESIAN_POINT('Ctrl Pts',(-30.4549372314006,33.4726351387477,0.157000127352253));
#33127=CARTESIAN_POINT('Ctrl Pts',(-32.6539236935135,31.4106472544613,0.0523333757840845));
#33128=CARTESIAN_POINT('Ctrl Pts',(-33.9479286229388,31.0647048309474,0.));
#33129=CARTESIAN_POINT('Ctrl Pts',(-33.9479286229388,31.0647048309474,0.));
#33130=CARTESIAN_POINT('Ctrl Pts',(-33.8318205444026,31.104319484649,-6.12910217551102E-18));
#33131=CARTESIAN_POINT('Ctrl Pts',(-33.7179775273608,31.1494845452793,-1.6976040424202E-15));
#33132=CARTESIAN_POINT('Ctrl Pts',(-33.6066254658749,31.1998424056554,-1.16573417585641E-15));
#33133=CARTESIAN_POINT('Ctrl Pts',(-33.4927762352539,31.2513295858929,-6.21936653918048E-16));
#33134=CARTESIAN_POINT('Ctrl Pts',(-33.3815303134372,31.3082455820535,1.45039252013455E-15));
#33135=CARTESIAN_POINT('Ctrl Pts',(-33.2731534080755,31.3702567597409,9.99200722162641E-16));
#33136=CARTESIAN_POINT('Ctrl Pts',(-33.1592150345376,31.4354501023936,5.24855570462807E-16));
#33137=CARTESIAN_POINT('Ctrl Pts',(-33.0484467137175,31.5062753971616,-4.62145718692395E-16));
#33138=CARTESIAN_POINT('Ctrl Pts',(-32.9411963534997,31.5823911623814,-5.55111512312578E-16));
#33139=CARTESIAN_POINT('Ctrl Pts',(-32.8473522883091,31.6489924569487,-6.36456581730239E-16));
#33140=CARTESIAN_POINT('Ctrl Pts',(-32.7562019661932,31.7196453256574,-1.95036301750383E-15));
#33141=CARTESIAN_POINT('Ctrl Pts',(-32.6680099559688,31.7941431443398,-1.99840144432528E-15));
#33142=CARTESIAN_POINT('Ctrl Pts',(-32.6506336549248,31.8088213053349,-2.00786636256454E-15));
#33143=CARTESIAN_POINT('Ctrl Pts',(-32.6333722976869,31.8236487792666,-7.57847684029515E-16));
#33144=CARTESIAN_POINT('Ctrl Pts',(-32.6162280624477,31.8386240567023,-7.7715611723761E-16));
#33145=CARTESIAN_POINT('Ctrl Pts',(-32.6036937742642,31.8495726024021,-7.91272667951259E-16));
#33146=CARTESIAN_POINT('Ctrl Pts',(-32.5912233028683,31.8605991578939,4.81364284937086E-16));
#33147=CARTESIAN_POINT('Ctrl Pts',(-32.5788262971356,31.8716950114967,4.44089209850063E-16));
#33148=CARTESIAN_POINT('Ctrl Pts',(-32.4862471134748,31.9545573647705,1.6572392577578E-16));
#33149=CARTESIAN_POINT('Ctrl Pts',(-32.3976237822216,32.0414014202655,8.13390076176465E-16));
#33150=CARTESIAN_POINT('Ctrl Pts',(-32.3132177297223,32.1319062612438,6.38378239159465E-16));
#33151=CARTESIAN_POINT('Ctrl Pts',(-32.2290034543674,32.222205468154,4.63764042706654E-16));
#33152=CARTESIAN_POINT('Ctrl Pts',(-32.1489867981842,32.3161495489862,3.17588722629917E-16));
#33153=CARTESIAN_POINT('Ctrl Pts',(-32.0734678385385,32.4134518063003,8.88178419700125E-16));
#33154=CARTESIAN_POINT('Ctrl Pts',(-31.9989812077255,32.5094239615292,1.4509682715575E-15));
#33155=CARTESIAN_POINT('Ctrl Pts',(-31.9288697495096,32.6086637947563,-1.05272258015246E-15));
#33156=CARTESIAN_POINT('Ctrl Pts',(-31.8634674410238,32.710917033623,-1.02695629777827E-15));
#33157=CARTESIAN_POINT('Ctrl Pts',(-31.8101619976839,32.7942574287394,-1.00595576833249E-15));
#33158=CARTESIAN_POINT('Ctrl Pts',(-31.7599855228772,32.8796001211512,6.44886685271164E-16));
#33159=CARTESIAN_POINT('Ctrl Pts',(-31.7131447814318,32.9668132818295,6.10622663543836E-16));
#33160=CARTESIAN_POINT('Ctrl Pts',(-31.7012439418187,32.9889715527142,6.01917194448022E-16));
#33161=CARTESIAN_POINT('Ctrl Pts',(-31.6895585553312,33.0112505813609,1.19774783640231E-15));
#33162=CARTESIAN_POINT('Ctrl Pts',(-31.6780922762038,33.0336482309453,1.16573417585641E-15));
#33163=CARTESIAN_POINT('Ctrl Pts',(-31.6699364387253,33.0495794312833,1.14296321331454E-15));
#33164=CARTESIAN_POINT('Ctrl Pts',(-31.661895167037,33.0655634624947,-2.51368181031482E-15));
#33165=CARTESIAN_POINT('Ctrl Pts',(-31.6539721233883,33.0815939077556,-2.4980018054066E-15));
#33166=CARTESIAN_POINT('Ctrl Pts',(-31.6010112907938,33.1887478962384,-2.3931903021702E-15));
#33167=CARTESIAN_POINT('Ctrl Pts',(-31.5532893085976,33.2980517601776,-1.33576692347369E-15));
#33168=CARTESIAN_POINT('Ctrl Pts',(-31.5110849763849,33.409242888583,-1.0547118733939E-15));
#33169=CARTESIAN_POINT('Ctrl Pts',(-31.469716801377,33.5182310852453,-7.79225119096594E-16));
#33170=CARTESIAN_POINT('Ctrl Pts',(-31.4336495378063,33.6290331387016,-1.04560375035282E-15));
#33171=CARTESIAN_POINT('Ctrl Pts',(-31.4031939533011,33.7414155242157,-1.19348975147204E-15));
#33172=CARTESIAN_POINT('Ctrl Pts',(-31.3987398005021,33.7578515350533,-1.2151181935629E-15));
#33173=CARTESIAN_POINT('Ctrl Pts',(-31.3944057673546,33.7743213630571,-1.05328088726205E-15));
#33174=CARTESIAN_POINT('Ctrl Pts',(-31.390192920076,33.7908242908111,-1.11022302462516E-15));
#33175=CARTESIAN_POINT('Ctrl Pts',(-31.3605243708329,33.9070444840312,-1.45504712955035E-15));
#33176=CARTESIAN_POINT('Ctrl Pts',(-31.336861805495,34.0249066128039,2.32711961845814E-15));
#33177=CARTESIAN_POINT('Ctrl Pts',(-31.3191143685546,34.1439748333396,2.41473507855972E-15));
#33178=CARTESIAN_POINT('Ctrl Pts',(-31.3091308324304,34.2109547519018,2.46402175098999E-15));
#33179=CARTESIAN_POINT('Ctrl Pts',(-31.3010200590003,34.2783162816674,1.31577829093223E-15));
#33180=CARTESIAN_POINT('Ctrl Pts',(-31.2947729234008,34.3459803828548,1.66533453693773E-15));
#33181=CARTESIAN_POINT('Ctrl Pts',(-31.2918904510582,34.3772010754682,1.82662224956662E-15));
#33182=CARTESIAN_POINT('Ctrl Pts',(-31.2894048093972,34.4084861625173,5.36743605776751E-16));
#33183=CARTESIAN_POINT('Ctrl Pts',(-31.2873154495445,34.4398277448617,5.55111512312578E-16));
#33184=CARTESIAN_POINT('Ctrl Pts',(-31.2861143588149,34.4578447867584,5.6567049870877E-16));
#33185=CARTESIAN_POINT('Ctrl Pts',(-31.2850447395365,34.4758734447918,-4.83710549279582E-16));
#33186=CARTESIAN_POINT('Ctrl Pts',(-31.2841065224407,34.4939038782769,-4.44089209850063E-16));
#33187=CARTESIAN_POINT('Ctrl Pts',(-31.2777956059898,34.6151855728967,-1.77576305814986E-16));
#33188=CARTESIAN_POINT('Ctrl Pts',(-31.2774172190669,34.7366645735772,1.74591754833025E-15));
#33189=CARTESIAN_POINT('Ctrl Pts',(-31.2828131531898,34.8578936251582,1.77635683940025E-15));
#33190=CARTESIAN_POINT('Ctrl Pts',(-31.2880971535264,34.9766078894115,1.80616469483294E-15));
#33191=CARTESIAN_POINT('Ctrl Pts',(-31.2989188936952,35.0950833906807,2.23513941723243E-15));
#33192=CARTESIAN_POINT('Ctrl Pts',(-31.3151831802674,35.2128941454877,2.73392419813945E-15));
#33193=CARTESIAN_POINT('Ctrl Pts',(-31.3312885576294,35.3295538375714,3.22783563306706E-15));
#33194=CARTESIAN_POINT('Ctrl Pts',(-31.3527309988427,35.445562546077,2.65572620552751E-15));
#33195=CARTESIAN_POINT('Ctrl Pts',(-31.3794648565834,35.5604877518601,3.06699110552699E-15));
#33196=CARTESIAN_POINT('Ctrl Pts',(-31.3968717688464,35.6353176919788,3.33477333511016E-15));
#33197=CARTESIAN_POINT('Ctrl Pts',(-31.4165229425865,35.7096878616141,5.4636862845821E-16));
#33198=CARTESIAN_POINT('Ctrl Pts',(-31.4384155780607,35.7834719630247,4.85722573273506E-16));
#33199=CARTESIAN_POINT('Ctrl Pts',(-31.4458039236167,35.8083726853891,4.65255690113341E-16));
#33200=CARTESIAN_POINT('Ctrl Pts',(-31.45344761912,35.8332066040146,2.20922363074103E-15));
#33201=CARTESIAN_POINT('Ctrl Pts',(-31.4613467446,35.8579686875435,2.27595720048157E-15));
#33202=CARTESIAN_POINT('Ctrl Pts',(-31.4664331437066,35.8739134702743,2.31892823194254E-15));
#33203=CARTESIAN_POINT('Ctrl Pts',(-31.4716246609433,35.8898258563265,-1.15821499265833E-16));
#33204=CARTESIAN_POINT('Ctrl Pts',(-31.4769184371132,35.9056964793841,2.77555756156289E-17));
#33205=CARTESIAN_POINT('Ctrl Pts',(-31.5138161242914,36.0163149237837,1.02848961215397E-15));
#33206=CARTESIAN_POINT('Ctrl Pts',(-31.5557145226016,36.1250218909898,1.27042107846669E-15));
#33207=CARTESIAN_POINT('Ctrl Pts',(-31.6025488384922,36.2313981798515,1.95676808090184E-15));
#33208=CARTESIAN_POINT('Ctrl Pts',(-31.6406629331589,36.3179679496208,2.51532208404033E-15));
#33209=CARTESIAN_POINT('Ctrl Pts',(-31.6820469345646,36.4029939678578,-2.48735046316874E-16));
#33210=CARTESIAN_POINT('Ctrl Pts',(-31.7266869042645,36.4862346415976,-4.02455846426619E-16));
#33211=CARTESIAN_POINT('Ctrl Pts',(-31.748301897583,36.5265403725114,-4.76888559747074E-16));
#33212=CARTESIAN_POINT('Ctrl Pts',(-31.7706805448521,36.566427275075,1.22980137611631E-15));
#33213=CARTESIAN_POINT('Ctrl Pts',(-31.7938227368542,36.6058663963511,1.14491749414469E-15));
#33214=CARTESIAN_POINT('Ctrl Pts',(-31.8074091619825,36.6290204981016,1.09508347207335E-15));
#33215=CARTESIAN_POINT('Ctrl Pts',(-31.8212608195948,36.6520233300662,-7.62339319688486E-16));
#33216=CARTESIAN_POINT('Ctrl Pts',(-31.8353636346369,36.6748465408533,-5.68989300120393E-16));
#33217=CARTESIAN_POINT('Ctrl Pts',(-31.8937950765752,36.7694087337193,2.32107531151829E-16));
#33218=CARTESIAN_POINT('Ctrl Pts',(-31.9565777772527,36.8609657133175,3.78686475409805E-16));
#33219=CARTESIAN_POINT('Ctrl Pts',(-32.0236776904421,36.9491267660533,4.5102810375397E-17));
#33220=CARTESIAN_POINT('Ctrl Pts',(-32.0837084847486,37.0279998639616,-2.53337104489111E-16));
#33221=CARTESIAN_POINT('Ctrl Pts',(-32.1471953789829,37.1041548289018,-7.94184032652028E-16));
#33222=CARTESIAN_POINT('Ctrl Pts',(-32.2141374826654,37.1772853486058,-1.07986536379556E-15));
#33223=CARTESIAN_POINT('Ctrl Pts',(-32.2489924160368,37.2153624219495,-1.21791469682805E-15));
#33224=CARTESIAN_POINT('Ctrl Pts',(-32.2847844521695,37.2526190806637,6.40917790468134E-17));
#33225=CARTESIAN_POINT('Ctrl Pts',(-32.3214761820288,37.2890399271606,-2.77555756156289E-17));
#33226=CARTESIAN_POINT('Ctrl Pts',(-38.5163029138352,34.997016742257,6.38741669750802));
#33227=CARTESIAN_POINT('Ctrl Pts',(-38.5189470194328,34.6831064778252,6.4016107071645));
#33228=CARTESIAN_POINT('Ctrl Pts',(-38.4802904146781,34.3698362574768,6.41580471682098));
#33229=CARTESIAN_POINT('Ctrl Pts',(-38.3977159824674,34.0686054096188,6.42999872647747));
#33230=CARTESIAN_POINT('Ctrl Pts',(-38.0932636891673,32.9579659539444,6.48233210226155));
#33231=CARTESIAN_POINT('Ctrl Pts',(-37.1917923921711,32.010989743602,6.53466547804563));
#33232=CARTESIAN_POINT('Ctrl Pts',(-36.0974794823371,31.6522427299976,6.58699885382972));
#33233=CARTESIAN_POINT('Ctrl Pts',(-35.0031665725032,31.2934957163932,6.6393322296138));
#33234=CARTESIAN_POINT('Ctrl Pts',(-33.7160120498315,31.5229778995268,6.69166560539789));
#33235=CARTESIAN_POINT('Ctrl Pts',(-32.8131210199243,32.2378308097469,6.74399898118197));
#33236=CARTESIAN_POINT('Ctrl Pts',(-31.9102299900171,32.952683719967,6.79633235696605));
#33237=CARTESIAN_POINT('Ctrl Pts',(-31.3916024528742,34.1529073572735,6.84866573275014));
#33238=CARTESIAN_POINT('Ctrl Pts',(-31.4897611048202,35.3003133215496,6.90099910853422));
#33239=CARTESIAN_POINT('Ctrl Pts',(-31.5879197567661,36.4477192858256,6.95333248431831));
#33240=CARTESIAN_POINT('Ctrl Pts',(-32.3028645978009,37.5423075770711,7.00566586010239));
#33241=CARTESIAN_POINT('Ctrl Pts',(-33.3140596654986,38.0934399201708,7.05799923588648));
#33242=CARTESIAN_POINT('Ctrl Pts',(-34.3252547331963,38.6445722632704,7.11033261167056));
#33243=CARTESIAN_POINT('Ctrl Pts',(-35.6327000275569,38.6522486582243,7.16266598745464));
#33244=CARTESIAN_POINT('Ctrl Pts',(-36.6501700272628,38.1127742899662,7.21499936323873));
#33245=CARTESIAN_POINT('Ctrl Pts',(-37.6676400269687,37.5732999217082,7.26733273902281));
#33246=CARTESIAN_POINT('Ctrl Pts',(-38.3951347320199,36.4866747902383,7.3196661148069));
#33247=CARTESIAN_POINT('Ctrl Pts',(-38.5065310098296,35.3406023903429,7.37199949059099));
#33248=CARTESIAN_POINT('Ctrl Pts',(-38.5174699784391,35.2280595814352,7.37713855956333));
#33249=CARTESIAN_POINT('Ctrl Pts',(-38.5224679204996,35.1149435235394,7.38227762853568));
#33250=CARTESIAN_POINT('Ctrl Pts',(-38.521739013009,35.0017650567249,7.38741669750802));
#33251=CARTESIAN_POINT('Ctrl Pts',(-36.0520713770612,31.0647048309474,8.));
#33252=CARTESIAN_POINT('Ctrl Pts',(-37.3460763064866,31.4106472544613,7.94766662421592));
#33253=CARTESIAN_POINT('Ctrl Pts',(-39.5450624630061,33.4726371160361,7.84299987264775));
#33254=CARTESIAN_POINT('Ctrl Pts',(-38.7813000795415,37.9557855546777,7.6859997452955));
#33255=CARTESIAN_POINT('Ctrl Pts',(-34.6204731393245,39.7808563212243,7.52899961794324));
#33256=CARTESIAN_POINT('Ctrl Pts',(-30.8030827008644,37.3225569109026,7.37199949059099));
#33257=CARTESIAN_POINT('Ctrl Pts',(-30.7475658132336,32.7797862032913,7.21499936323873));
#33258=CARTESIAN_POINT('Ctrl Pts',(-34.5060130464714,30.2288015790917,7.05799923588648));
#33259=CARTESIAN_POINT('Ctrl Pts',(-38.707043056971,31.9557500555838,6.90099910853422));
#33260=CARTESIAN_POINT('Ctrl Pts',(-39.5841206744658,36.4127282212004,6.74399898118198));
#33261=CARTESIAN_POINT('Ctrl Pts',(-36.3504796357983,39.6027894460767,6.58699885382972));
#33262=CARTESIAN_POINT('Ctrl Pts',(-31.905897053523,38.6655398223873,6.42999872647746));
#33263=CARTESIAN_POINT('Ctrl Pts',(-30.2358031812474,34.4413383659989,6.27299859912522));
#33264=CARTESIAN_POINT('Ctrl Pts',(-32.8378217627235,30.7181076142107,6.11599847177296));
#33265=CARTESIAN_POINT('Ctrl Pts',(-37.3786806229274,30.8344841622903,5.95899834442071));
#33266=CARTESIAN_POINT('Ctrl Pts',(-39.7865565731199,34.68612204099,5.80199821706845));
#33267=CARTESIAN_POINT('Ctrl Pts',(-37.9022799217924,38.8192156501332,5.6449980897162));
#33268=CARTESIAN_POINT('Ctrl Pts',(-33.4155017175264,39.5275827633586,5.48799796236395));
#33269=CARTESIAN_POINT('Ctrl Pts',(-30.3495579785441,36.176022571197,5.33099783501169));
#33270=CARTESIAN_POINT('Ctrl Pts',(-31.4537103860929,31.7699118586619,5.17399770765944));
#33271=CARTESIAN_POINT('Ctrl Pts',(-35.7378546268185,30.2602520705083,5.01699758030719));
#33272=CARTESIAN_POINT('Ctrl Pts',(-39.3603575873042,33.0007697714678,4.85999745295493));
#33273=CARTESIAN_POINT('Ctrl Pts',(-39.0728860468858,37.5340163734447,4.70299732560268));
#33274=CARTESIAN_POINT('Ctrl Pts',(-35.1332185251462,39.7949861953461,4.54599719825043));
#33275=CARTESIAN_POINT('Ctrl Pts',(-31.0740926686951,37.7562458887763,4.38899707089817));
#33276=CARTESIAN_POINT('Ctrl Pts',(-30.5353655822401,33.2459534545604,4.23199694354592));
#33277=CARTESIAN_POINT('Ctrl Pts',(-34.0001190086845,30.3085313836444,4.07499681619366));
#33278=CARTESIAN_POINT('Ctrl Pts',(-38.3614753130862,31.5779942297887,3.91799668884141));
#33279=CARTESIAN_POINT('Ctrl Pts',(-39.70856445542,35.9160024787098,3.76099656148916));
#33280=CARTESIAN_POINT('Ctrl Pts',(-36.8334386787628,39.4326225179073,3.6039964341369));
#33281=CARTESIAN_POINT('Ctrl Pts',(-32.314250849668,38.9744674195804,3.44699630678465));
#33282=CARTESIAN_POINT('Ctrl Pts',(-30.2034000494222,34.9523692588031,3.2899961794324));
#33283=CARTESIAN_POINT('Ctrl Pts',(-32.3937064417451,30.9729820366429,3.13299605208014));
#33284=CARTESIAN_POINT('Ctrl Pts',(-36.9211012705904,30.6046604636344,2.97599592472789));
#33285=CARTESIAN_POINT('Ctrl Pts',(-39.7258261615381,34.1776820038694,2.81899579737564));
#33286=CARTESIAN_POINT('Ctrl Pts',(-38.2928573925768,38.4880840124043,2.66199567002338));
#33287=CARTESIAN_POINT('Ctrl Pts',(-33.9071518161688,39.6706875589806,2.50499554267113));
#33288=CARTESIAN_POINT('Ctrl Pts',(-30.5014136769744,36.6650408935442,2.34799541531887));
#33289=CARTESIAN_POINT('Ctrl Pts',(-31.1296010783918,32.1663358219723,2.19099528796663));
#33290=CARTESIAN_POINT('Ctrl Pts',(-35.2284122688067,30.2086051339802,2.03399516061437));
#33291=CARTESIAN_POINT('Ctrl Pts',(-39.1224040971504,32.5473631209192,1.87699503326212));
#33292=CARTESIAN_POINT('Ctrl Pts',(-39.319796400129,37.0854262781345,1.71999490590986));
#33293=CARTESIAN_POINT('Ctrl Pts',(-35.6435862778458,39.7534633517259,1.56299477855761));
#33294=CARTESIAN_POINT('Ctrl Pts',(-31.3902652615342,38.1590329639038,1.40599465120536));
#33295=CARTESIAN_POINT('Ctrl Pts',(-30.3738298371754,33.7318498284919,1.2489945238531));
#33296=CARTESIAN_POINT('Ctrl Pts',(-33.5057219097166,30.4418645346457,1.09199439650085));
#33297=CARTESIAN_POINT('Ctrl Pts',(-37.9775548729557,31.2391317008465,0.934994269148598));
#33298=CARTESIAN_POINT('Ctrl Pts',(-39.7793709270477,35.4089492535829,0.777994141796342));
#33299=CARTESIAN_POINT('Ctrl Pts',(-37.2955092110801,39.2117686241983,0.620994014444089));
#33300=CARTESIAN_POINT('Ctrl Pts',(-32.7531819533668,39.2384377406302,0.463993887091835));
#33301=CARTESIAN_POINT('Ctrl Pts',(-30.2257196451616,35.46328448449,0.306993759739582));
#33302=CARTESIAN_POINT('Ctrl Pts',(-31.9791557179606,31.2750667622313,0.149993632387329));
#33303=CARTESIAN_POINT('Ctrl Pts',(-36.4418971366481,30.4222460546565,-0.00700649496492604));
#33304=CARTESIAN_POINT('Ctrl Pts',(-39.6107565597589,33.6841906982476,-0.164006622317178));
#33305=CARTESIAN_POINT('Ctrl Pts',(-38.9665644295237,36.6290775899881,-0.268673373885348));
#33306=CARTESIAN_POINT('Ctrl Pts',(-38.0961285948024,37.6471475165632,-0.321006749669432));
#33307=CARTESIAN_POINT('Ctrl Pts',(-36.0042049488753,31.243750214851,8.10700224988981));
#33308=CARTESIAN_POINT('Ctrl Pts',(-37.2393361218455,31.5739531851941,8.05466887410573));
#33309=CARTESIAN_POINT('Ctrl Pts',(-39.3382743013571,33.5421280340415,7.95000212253756));
#33310=CARTESIAN_POINT('Ctrl Pts',(-38.6092610595157,37.8213052332178,7.79300199518531));
#33311=CARTESIAN_POINT('Ctrl Pts',(-34.6377405943825,39.5633401709358,7.63600186783305));
#33312=CARTESIAN_POINT('Ctrl Pts',(-30.9940311905596,37.2168867957304,7.4790017404808));
#33313=CARTESIAN_POINT('Ctrl Pts',(-30.941040172535,32.8807999810394,7.32200161312854));
#33314=CARTESIAN_POINT('Ctrl Pts',(-34.5284881290099,30.4458783207982,7.16500148577629));
#33315=CARTESIAN_POINT('Ctrl Pts',(-38.5383825324691,32.0942552696991,7.00800135842404));
#33316=CARTESIAN_POINT('Ctrl Pts',(-39.3755554688683,36.3484528731387,6.85100123107178));
#33317=CARTESIAN_POINT('Ctrl Pts',(-36.2890364315511,39.3933748614019,6.69400110371953));
#33318=CARTESIAN_POINT('Ctrl Pts',(-32.0466704456298,38.4987675838335,6.53700097636727));
#33319=CARTESIAN_POINT('Ctrl Pts',(-30.4525613688197,34.4667559731757,6.38000084901503));
#33320=CARTESIAN_POINT('Ctrl Pts',(-32.9361950780481,30.9129222426219,6.22300072166277));
#33321=CARTESIAN_POINT('Ctrl Pts',(-37.2704570292653,31.024003969644,6.06600059431052));
#33322=CARTESIAN_POINT('Ctrl Pts',(-39.5687810766463,34.7004026469562,5.90900046695827));
#33323=CARTESIAN_POINT('Ctrl Pts',(-37.7702339632379,38.6454515732563,5.752000339606));
#33324=CARTESIAN_POINT('Ctrl Pts',(-33.4875921430454,39.3215898811993,5.59500021225376));
#33325=CARTESIAN_POINT('Ctrl Pts',(-30.5611406276935,36.1225166958576,5.4380000849015));
#33326=CARTESIAN_POINT('Ctrl Pts',(-31.6150570597422,31.916872212705,5.28099995754925));
#33327=CARTESIAN_POINT('Ctrl Pts',(-35.7042842186919,30.4758978991403,5.123999830197));
#33328=CARTESIAN_POINT('Ctrl Pts',(-39.1619730025048,33.0917293890828,4.96699970284474));
#33329=CARTESIAN_POINT('Ctrl Pts',(-38.8875806467738,37.4187254194219,4.80999957549249));
#33330=CARTESIAN_POINT('Ctrl Pts',(-35.1271574392675,39.576827173652,4.65299944814024));
#33331=CARTESIAN_POINT('Ctrl Pts',(-31.2527109311398,37.6308440873639,4.49599932078798));
#33332=CARTESIAN_POINT('Ctrl Pts',(-30.7384944833714,33.3257578716681,4.33899919343573));
#33333=CARTESIAN_POINT('Ctrl Pts',(-34.0456109141852,30.5219806329136,4.18199906608347));
#33334=CARTESIAN_POINT('Ctrl Pts',(-38.208537194836,31.7336863216211,4.02499893873123));
#33335=CARTESIAN_POINT('Ctrl Pts',(-39.4943373912889,35.8743268207447,3.86799881137897));
#33336=CARTESIAN_POINT('Ctrl Pts',(-36.7500221323538,39.23095007243,3.71099868402672));
#33337=CARTESIAN_POINT('Ctrl Pts',(-32.4364452384069,38.7936398032564,3.55399855667446));
#33338=CARTESIAN_POINT('Ctrl Pts',(-30.4216324926546,34.9545363298808,3.39699842932221));
#33339=CARTESIAN_POINT('Ctrl Pts',(-32.5122858139794,31.1562005618773,3.23999830196995));
#33340=CARTESIAN_POINT('Ctrl Pts',(-36.8336963111821,30.8046366333671,3.0829981746177));
#33341=CARTESIAN_POINT('Ctrl Pts',(-39.5108137360388,34.2150952689444,2.92599804726545));
#33342=CARTESIAN_POINT('Ctrl Pts',(-38.1430412058191,38.3293855376367,2.7689979199132));
#33343=CARTESIAN_POINT('Ctrl Pts',(-33.9568734797841,39.4581837921304,2.61199779256094));
#33344=CARTESIAN_POINT('Ctrl Pts',(-30.7060872988067,36.5892859950694,2.45499766520869));
#33345=CARTESIAN_POINT('Ctrl Pts',(-31.3056938569536,32.2952599480705,2.29799753785643));
#33346=CARTESIAN_POINT('Ctrl Pts',(-35.2180201227033,30.4266007598144,2.14099741050418));
#33347=CARTESIAN_POINT('Ctrl Pts',(-38.9348457584559,32.6589515260392,1.98399728315193));
#33348=CARTESIAN_POINT('Ctrl Pts',(-39.1232572406452,36.9905449712614,1.82699715579967));
#33349=CARTESIAN_POINT('Ctrl Pts',(-35.6143048269655,39.5371935081385,1.66999702844742));
#33350=CARTESIAN_POINT('Ctrl Pts',(-31.554498518323,38.0153054300115,1.51299690109517));
#33351=CARTESIAN_POINT('Ctrl Pts',(-30.5843081818037,33.7895472627506,1.35599677374291));
#33352=CARTESIAN_POINT('Ctrl Pts',(-33.5737075582741,30.6492474828669,1.19899664639066));
#33353=CARTESIAN_POINT('Ctrl Pts',(-37.8420841058543,31.4102411296202,1.04199651903841));
#33354=CARTESIAN_POINT('Ctrl Pts',(-39.5619223582134,35.3903431584975,0.884996391686153));
#33355=CARTESIAN_POINT('Ctrl Pts',(-37.1910696937641,39.0201444390132,0.7279962643339));
#33356=CARTESIAN_POINT('Ctrl Pts',(-32.8554061531891,39.0456001821187,0.570996136981647));
#33357=CARTESIAN_POINT('Ctrl Pts',(-30.4429366066027,35.4422062820125,0.413996009629392));
#33358=CARTESIAN_POINT('Ctrl Pts',(-32.116596037163,31.4445412420153,0.25699588227714));
#33359=CARTESIAN_POINT('Ctrl Pts',(-36.3762946811041,30.6305215911411,0.0999957549248848));
#33360=CARTESIAN_POINT('Ctrl Pts',(-39.4009794927627,33.7440564952096,-0.057004372427367));
#33361=CARTESIAN_POINT('Ctrl Pts',(-38.7860963780679,36.5549589254462,-0.161671123995537));
#33362=CARTESIAN_POINT('Ctrl Pts',(-37.9552630411254,37.5267093987113,-0.214004499779622));
#33363=CARTESIAN_POINT('Ctrl Pts',(-35.9563385206894,31.4227955987545,8.21400449977962));
#33364=CARTESIAN_POINT('Ctrl Pts',(-37.1325959372044,31.7372591159268,8.16167112399554));
#33365=CARTESIAN_POINT('Ctrl Pts',(-39.1314861397082,33.6116189520467,8.05700437242738));
#33366=CARTESIAN_POINT('Ctrl Pts',(-38.4372220394899,37.6868249117579,7.90000424507511));
#33367=CARTESIAN_POINT('Ctrl Pts',(-34.6550080494404,39.3458240206473,7.74300411772287));
#33368=CARTESIAN_POINT('Ctrl Pts',(-31.1849796802547,37.1112166805582,7.5860039903706));
#33369=CARTESIAN_POINT('Ctrl Pts',(-31.1345145318363,32.9818137587874,7.42900386301836));
#33370=CARTESIAN_POINT('Ctrl Pts',(-34.5509632115484,30.6629550625048,7.2720037356661));
#33371=CARTESIAN_POINT('Ctrl Pts',(-38.3697220079671,32.2327604838143,7.11500360831385));
#33372=CARTESIAN_POINT('Ctrl Pts',(-39.166990263271,36.2841775250771,6.95800348096159));
#33373=CARTESIAN_POINT('Ctrl Pts',(-36.2275932273038,39.1839602767271,6.80100335360935));
#33374=CARTESIAN_POINT('Ctrl Pts',(-32.1874438377366,38.3319953452796,6.64400322625709));
#33375=CARTESIAN_POINT('Ctrl Pts',(-30.6693195563919,34.4921735803525,6.48700309890483));
#33376=CARTESIAN_POINT('Ctrl Pts',(-33.0345683933729,31.1077368710331,6.33000297155259));
#33377=CARTESIAN_POINT('Ctrl Pts',(-37.1622334356032,31.2135237769978,6.17300284420032));
#33378=CARTESIAN_POINT('Ctrl Pts',(-39.3510055801728,34.7146832529224,6.01600271684808));
#33379=CARTESIAN_POINT('Ctrl Pts',(-37.6381880046832,38.4716874963794,5.85900258949581));
#33380=CARTESIAN_POINT('Ctrl Pts',(-33.5596825685645,39.11559699904,5.70200246214357));
#33381=CARTESIAN_POINT('Ctrl Pts',(-30.7727232768428,36.0690108205182,5.54500233479131));
#33382=CARTESIAN_POINT('Ctrl Pts',(-31.7764037333916,32.0638325667482,5.38800220743906));
#33383=CARTESIAN_POINT('Ctrl Pts',(-35.6707138105653,30.6915437277723,5.23100208008681));
#33384=CARTESIAN_POINT('Ctrl Pts',(-38.9635884177054,33.1826890066978,5.07400195273455));
#33385=CARTESIAN_POINT('Ctrl Pts',(-38.7022752466618,37.3034344653991,4.9170018253823));
#33386=CARTESIAN_POINT('Ctrl Pts',(-35.1210963533887,39.3586681519579,4.76000169803004));
#33387=CARTESIAN_POINT('Ctrl Pts',(-31.4313291935845,37.5054422859516,4.6030015706778));
#33388=CARTESIAN_POINT('Ctrl Pts',(-30.9416233845026,33.4055622887757,4.44600144332554));
#33389=CARTESIAN_POINT('Ctrl Pts',(-34.091102819686,30.7354298821828,4.28900131597329));
#33390=CARTESIAN_POINT('Ctrl Pts',(-38.0555990765859,31.8893784134534,4.13200118862103));
#33391=CARTESIAN_POINT('Ctrl Pts',(-39.2801103271579,35.8326511627796,3.97500106126878));
#33392=CARTESIAN_POINT('Ctrl Pts',(-36.6666055859447,39.0292776269525,3.81800093391652));
#33393=CARTESIAN_POINT('Ctrl Pts',(-32.5586396271459,38.6128121869325,3.66100080656428));
#33394=CARTESIAN_POINT('Ctrl Pts',(-30.639864935887,34.9567034009586,3.50400067921202));
#33395=CARTESIAN_POINT('Ctrl Pts',(-32.6308651862137,31.3394190871117,3.34700055185977));
#33396=CARTESIAN_POINT('Ctrl Pts',(-36.7462913517739,31.0046128030999,3.19000042450751));
#33397=CARTESIAN_POINT('Ctrl Pts',(-39.2958013105393,34.2525085340193,3.03300029715526));
#33398=CARTESIAN_POINT('Ctrl Pts',(-37.9932250190614,38.1706870628692,2.876000169803));
#33399=CARTESIAN_POINT('Ctrl Pts',(-34.0065951433993,39.2456800252801,2.71900004245075));
#33400=CARTESIAN_POINT('Ctrl Pts',(-30.9107609206391,36.5135310965947,2.5619999150985));
#33401=CARTESIAN_POINT('Ctrl Pts',(-31.4817866355154,32.4241840741688,2.40499978774625));
#33402=CARTESIAN_POINT('Ctrl Pts',(-35.2076279765999,30.6445963856486,2.24799966039399));
#33403=CARTESIAN_POINT('Ctrl Pts',(-38.7472874197615,32.7705399311592,2.09099953304174));
#33404=CARTESIAN_POINT('Ctrl Pts',(-38.9267180811614,36.8956636643883,1.93399940568948));
#33405=CARTESIAN_POINT('Ctrl Pts',(-35.5850233760853,39.3209236645512,1.77699927833723));
#33406=CARTESIAN_POINT('Ctrl Pts',(-31.7187317751118,37.8715778961193,1.61999915098498));
#33407=CARTESIAN_POINT('Ctrl Pts',(-30.7947865264321,33.8472446970093,1.46299902363273));
#33408=CARTESIAN_POINT('Ctrl Pts',(-33.6416932068317,30.8566304310881,1.30599889628047));
#33409=CARTESIAN_POINT('Ctrl Pts',(-37.7066133387528,31.581350558394,1.14899876892822));
#33410=CARTESIAN_POINT('Ctrl Pts',(-39.3444737893792,35.371737063412,0.991998641575963));
#33411=CARTESIAN_POINT('Ctrl Pts',(-37.086630176448,38.8285202538281,0.834998514223711));
#33412=CARTESIAN_POINT('Ctrl Pts',(-32.9576303530114,38.8527626236071,0.677998386871457));
#33413=CARTESIAN_POINT('Ctrl Pts',(-30.6601535680437,35.421128079535,0.520998259519203));
#33414=CARTESIAN_POINT('Ctrl Pts',(-32.2540363563655,31.6140157217992,0.36399813216695));
#33415=CARTESIAN_POINT('Ctrl Pts',(-36.31069222556,30.8387971276259,0.206998004814696));
#33416=CARTESIAN_POINT('Ctrl Pts',(-39.1912024257666,33.8039222921716,0.0499978774624438));
#33417=CARTESIAN_POINT('Ctrl Pts',(-38.6056283266121,36.4808402609044,-0.0546688741057268));
#33418=CARTESIAN_POINT('Ctrl Pts',(-37.8143974874483,37.4062712808594,-0.107002249889811));
#33419=CARTESIAN_POINT('Ctrl Pts',(-35.9084720925035,31.6018409826581,8.32100674966943));
#33420=CARTESIAN_POINT('Ctrl Pts',(-37.0258557525633,31.9005650466595,8.26867337388535));
#33421=CARTESIAN_POINT('Ctrl Pts',(-38.9246979780591,33.681109870052,8.16400662231719));
#33422=CARTESIAN_POINT('Ctrl Pts',(-38.2651830194642,37.552344590298,8.00700649496492));
#33423=CARTESIAN_POINT('Ctrl Pts',(-34.6722755044984,39.1283078703588,7.85000636761267));
#33424=CARTESIAN_POINT('Ctrl Pts',(-31.3759281699498,37.005546565386,7.69300624026042));
#33425=CARTESIAN_POINT('Ctrl Pts',(-31.3279888911377,33.0828275365354,7.53600611290817));
#33426=CARTESIAN_POINT('Ctrl Pts',(-34.5734382940869,30.8800318042114,7.37900598555591));
#33427=CARTESIAN_POINT('Ctrl Pts',(-38.2010614834652,32.3712656979296,7.22200585820366));
#33428=CARTESIAN_POINT('Ctrl Pts',(-38.9584250576736,36.2199021770154,7.06500573085141));
#33429=CARTESIAN_POINT('Ctrl Pts',(-36.1661500230565,38.9745456920523,6.90800560349915));
#33430=CARTESIAN_POINT('Ctrl Pts',(-32.3282172298434,38.1652231067258,6.7510054761469));
#33431=CARTESIAN_POINT('Ctrl Pts',(-30.8860777439641,34.5175911875294,6.59400534879464));
#33432=CARTESIAN_POINT('Ctrl Pts',(-33.1329417086976,31.3025514994443,6.43700522144239));
#33433=CARTESIAN_POINT('Ctrl Pts',(-37.0540098419411,31.4030435843515,6.28000509409013));
#33434=CARTESIAN_POINT('Ctrl Pts',(-39.1332300836993,34.7289638588885,6.12300496673789));
#33435=CARTESIAN_POINT('Ctrl Pts',(-37.5061420461286,38.2979234195025,5.96600483938563));
#33436=CARTESIAN_POINT('Ctrl Pts',(-33.6317729940835,38.9096041168808,5.80900471203338));
#33437=CARTESIAN_POINT('Ctrl Pts',(-30.9843059259921,36.0155049451787,5.65200458468113));
#33438=CARTESIAN_POINT('Ctrl Pts',(-31.937750407041,32.2107929207913,5.49500445732887));
#33439=CARTESIAN_POINT('Ctrl Pts',(-35.6371434024388,30.9071895564043,5.33800432997662));
#33440=CARTESIAN_POINT('Ctrl Pts',(-38.765203832906,33.2736486243128,5.18100420262436));
#33441=CARTESIAN_POINT('Ctrl Pts',(-38.5169698465499,37.1881435113763,5.02400407527211));
#33442=CARTESIAN_POINT('Ctrl Pts',(-35.1150352675099,39.1405091302639,4.86700394791986));
#33443=CARTESIAN_POINT('Ctrl Pts',(-31.6099474560293,37.3800404845393,4.7100038205676));
#33444=CARTESIAN_POINT('Ctrl Pts',(-31.1447522856339,33.4853667058834,4.55300369321536));
#33445=CARTESIAN_POINT('Ctrl Pts',(-34.1365947251866,30.9488791314519,4.39600356586309));
#33446=CARTESIAN_POINT('Ctrl Pts',(-37.9026609583357,32.0450705052858,4.23900343851085));
#33447=CARTESIAN_POINT('Ctrl Pts',(-39.0658832630269,35.7909755048144,4.08200331115859));
#33448=CARTESIAN_POINT('Ctrl Pts',(-36.5831890395356,38.8276051814752,3.92500318380634));
#33449=CARTESIAN_POINT('Ctrl Pts',(-32.6808340158849,38.4319845706085,3.76800305645408));
#33450=CARTESIAN_POINT('Ctrl Pts',(-30.8580973791193,34.9588704720363,3.61100292910183));
#33451=CARTESIAN_POINT('Ctrl Pts',(-32.7494445584481,31.522637612346,3.45400280174958));
#33452=CARTESIAN_POINT('Ctrl Pts',(-36.6588863923657,31.2045889728327,3.29700267439732));
#33453=CARTESIAN_POINT('Ctrl Pts',(-39.0807888850399,34.2899217990943,3.14000254704507));
#33454=CARTESIAN_POINT('Ctrl Pts',(-37.8434088323037,38.0119885881016,2.98300241969281));
#33455=CARTESIAN_POINT('Ctrl Pts',(-34.0563168070145,39.0331762584299,2.82600229234057));
#33456=CARTESIAN_POINT('Ctrl Pts',(-31.1154345424715,36.4377761981199,2.66900216498831));
#33457=CARTESIAN_POINT('Ctrl Pts',(-31.6578794140771,32.553108200267,2.51200203763606));
#33458=CARTESIAN_POINT('Ctrl Pts',(-35.1972358304966,30.8625920114828,2.3550019102838));
#33459=CARTESIAN_POINT('Ctrl Pts',(-38.559729081067,32.8821283362792,2.19800178293155));
#33460=CARTESIAN_POINT('Ctrl Pts',(-38.7301789216776,36.8007823575152,2.04100165557929));
#33461=CARTESIAN_POINT('Ctrl Pts',(-35.555741925205,39.1046538209638,1.88400152822704));
#33462=CARTESIAN_POINT('Ctrl Pts',(-31.8829650319005,37.727850362227,1.72700140087479));
#33463=CARTESIAN_POINT('Ctrl Pts',(-31.0052648710604,33.904942131268,1.57000127352254));
#33464=CARTESIAN_POINT('Ctrl Pts',(-33.7096788553892,31.0640133793093,1.41300114617028));
#33465=CARTESIAN_POINT('Ctrl Pts',(-37.5711425716514,31.7524599871677,1.25600101881803));
#33466=CARTESIAN_POINT('Ctrl Pts',(-39.127025220545,35.3531309683265,1.09900089146578));
#33467=CARTESIAN_POINT('Ctrl Pts',(-36.982190659132,38.6368960686431,0.942000764113521));
#33468=CARTESIAN_POINT('Ctrl Pts',(-33.0598545528336,38.6599250650956,0.785000636761268));
#33469=CARTESIAN_POINT('Ctrl Pts',(-30.8773705294847,35.4000498770575,0.628000509409013));
#33470=CARTESIAN_POINT('Ctrl Pts',(-32.391476675568,31.7834902015831,0.471000382056762));
#33471=CARTESIAN_POINT('Ctrl Pts',(-36.2450897700159,31.0470726641105,0.314000254704506));
#33472=CARTESIAN_POINT('Ctrl Pts',(-38.9814253587705,33.8637880891336,0.157000127352255));
#33473=CARTESIAN_POINT('Ctrl Pts',(-38.4251602751564,36.4067215963626,0.0523333757840841));
#33474=CARTESIAN_POINT('Ctrl Pts',(-37.6735319337713,37.2858331630075,0.));
#33475=CARTESIAN_POINT('Ctrl Pts',(-37.6735319337713,37.2858331630075,0.));
#33476=CARTESIAN_POINT('Ctrl Pts',(-37.7506745369995,37.2087203555594,1.28363488612132E-16));
#33477=CARTESIAN_POINT('Ctrl Pts',(-37.8237047828546,37.1279853831031,-1.45961390077584E-15));
#33478=CARTESIAN_POINT('Ctrl Pts',(-37.8926303634218,37.044046747423,-1.27675647831893E-15));
#33479=CARTESIAN_POINT('Ctrl Pts',(-37.9633158416367,36.9579648812288,-1.08923010211539E-15));
#33480=CARTESIAN_POINT('Ctrl Pts',(-38.0296847428869,36.8685132102372,2.69373606469353E-15));
#33481=CARTESIAN_POINT('Ctrl Pts',(-38.0917154903142,36.776096981172,2.1094237467878E-15));
#33482=CARTESIAN_POINT('Ctrl Pts',(-38.1550372699928,36.6817573135345,1.51295026561079E-15));
#33483=CARTESIAN_POINT('Ctrl Pts',(-38.2138388545422,36.5843278170101,-6.22870230136456E-16));
#33484=CARTESIAN_POINT('Ctrl Pts',(-38.2680604999532,36.4842001218513,-1.22124532708767E-15));
#33485=CARTESIAN_POINT('Ctrl Pts',(-38.3198497467852,36.3885641838418,-1.7927771454093E-15));
#33486=CARTESIAN_POINT('Ctrl Pts',(-38.3674607433557,36.2904658682844,-1.21061342909026E-15));
#33487=CARTESIAN_POINT('Ctrl Pts',(-38.4108059167409,36.1902218218841,-1.49880108324396E-15));
#33488=CARTESIAN_POINT('Ctrl Pts',(-38.4178437109143,36.1739455698685,-1.54559303803029E-15));
#33489=CARTESIAN_POINT('Ctrl Pts',(-38.4247689668943,36.1576127105175,5.76904931418396E-16));
#33490=CARTESIAN_POINT('Ctrl Pts',(-38.4315812162273,36.1412245565248,6.10622663543836E-16));
#33491=CARTESIAN_POINT('Ctrl Pts',(-38.4380909127403,36.1255642505548,6.42842888099819E-16));
#33492=CARTESIAN_POINT('Ctrl Pts',(-38.4444943995979,36.1098606451587,1.94214412995646E-15));
#33493=CARTESIAN_POINT('Ctrl Pts',(-38.4507894645608,36.0941203888398,1.88737914186277E-15));
#33494=CARTESIAN_POINT('Ctrl Pts',(-38.4941748650482,35.9856390104596,1.50994047282167E-15));
#33495=CARTESIAN_POINT('Ctrl Pts',(-38.5324464076346,35.8753406458803,4.14672721999528E-16));
#33496=CARTESIAN_POINT('Ctrl Pts',(-38.5655754746426,35.7636570985597,-1.11022302462516E-16));
#33497=CARTESIAN_POINT('Ctrl Pts',(-38.599139072954,35.6505086745683,-6.43612508853869E-16));
#33498=CARTESIAN_POINT('Ctrl Pts',(-38.6274248054533,35.535937741082,5.81275891054099E-16));
#33499=CARTESIAN_POINT('Ctrl Pts',(-38.6503602739825,35.4203607919199,1.85962356624714E-15));
#33500=CARTESIAN_POINT('Ctrl Pts',(-38.6743352598313,35.2995454827809,3.19591052212541E-15));
#33501=CARTESIAN_POINT('Ctrl Pts',(-38.692464786516,35.1776300814803,-8.4407659709162E-16));
#33502=CARTESIAN_POINT('Ctrl Pts',(-38.7046104310317,35.0550669428354,-1.38777878078145E-15));
#33503=CARTESIAN_POINT('Ctrl Pts',(-38.7137196644185,34.9631445888517,-1.79555541854881E-15));
#33504=CARTESIAN_POINT('Ctrl Pts',(-38.7194618408911,34.8708572859148,2.82896256593911E-15));
#33505=CARTESIAN_POINT('Ctrl Pts',(-38.721755434165,34.7783924177428,2.94209101525666E-15));
#33506=CARTESIAN_POINT('Ctrl Pts',(-38.7223030074901,34.7563173201712,2.96909934400004E-15));
#33507=CARTESIAN_POINT('Ctrl Pts',(-38.7226538674535,34.7342275752707,-2.60000342473094E-16));
#33508=CARTESIAN_POINT('Ctrl Pts',(-38.7228068022813,34.7121547959299,-2.77555756156289E-16));
#33509=CARTESIAN_POINT('Ctrl Pts',(-38.7236416666969,34.5916604762348,-3.73389977849103E-16));
#33510=CARTESIAN_POINT('Ctrl Pts',(-38.7185883671926,34.4715209673338,1.72146304164403E-15));
#33511=CARTESIAN_POINT('Ctrl Pts',(-38.7075779418993,34.3521623032552,1.58206781009085E-15));
#33512=CARTESIAN_POINT('Ctrl Pts',(-38.6966381726954,34.2335695874665,1.44356710546673E-15));
#33513=CARTESIAN_POINT('Ctrl Pts',(-38.6798177366068,34.1157468505408,1.14312909921041E-17));
#33514=CARTESIAN_POINT('Ctrl Pts',(-38.6569995558515,33.9990991317786,-2.77555756156289E-16));
#33515=CARTESIAN_POINT('Ctrl Pts',(-38.654125907022,33.9844088905153,-3.13949862184534E-16));
#33516=CARTESIAN_POINT('Ctrl Pts',(-38.6511570658937,33.9697372784049,2.13659354022824E-15));
#33517=CARTESIAN_POINT('Ctrl Pts',(-38.6480927394297,33.9550851007466,2.1094237467878E-15));
#33518=CARTESIAN_POINT('Ctrl Pts',(-38.6241822697972,33.8407564046822,1.89676768741005E-15));
#33519=CARTESIAN_POINT('Ctrl Pts',(-38.5944625878303,33.7276104213963,7.3858195394121E-16));
#33520=CARTESIAN_POINT('Ctrl Pts',(-38.5592398399973,33.6159136444833,2.4980018054066E-16));
#33521=CARTESIAN_POINT('Ctrl Pts',(-38.5372745858279,33.5462584288701,-5.50089711192647E-17));
#33522=CARTESIAN_POINT('Ctrl Pts',(-38.5131681698132,33.4771668829623,6.13912691963219E-16));
#33523=CARTESIAN_POINT('Ctrl Pts',(-38.4869849848521,33.408705821156,6.93889390390723E-16));
#33524=CARTESIAN_POINT('Ctrl Pts',(-38.478035242453,33.3853049679579,7.21226433226402E-16));
#33525=CARTESIAN_POINT('Ctrl Pts',(-38.4688427975352,33.3619777978058,1.17968218996551E-15));
#33526=CARTESIAN_POINT('Ctrl Pts',(-38.4594100345669,33.3387270476804,1.30451205393456E-15));
#33527=CARTESIAN_POINT('Ctrl Pts',(-38.4526611227965,33.3220917032197,1.39382477610025E-15));
#33528=CARTESIAN_POINT('Ctrl Pts',(-38.4457886431155,33.3054943585584,8.23245697379087E-16));
#33529=CARTESIAN_POINT('Ctrl Pts',(-38.4388005380928,33.2889523169239,7.49400541621981E-16));
#33530=CARTESIAN_POINT('Ctrl Pts',(-38.3928792100309,33.1802486671866,2.64137711097381E-16));
#33531=CARTESIAN_POINT('Ctrl Pts',(-38.3419048511529,33.0737714082961,1.17255001397609E-15));
#33532=CARTESIAN_POINT('Ctrl Pts',(-38.2862359020984,32.9697748885158,9.43689570931383E-16));
#33533=CARTESIAN_POINT('Ctrl Pts',(-38.2286517312081,32.8622004961707,7.06955465363536E-16));
#33534=CARTESIAN_POINT('Ctrl Pts',(-38.1660442194156,32.7572797837933,2.65690729149937E-16));
#33535=CARTESIAN_POINT('Ctrl Pts',(-38.0987547078419,32.6553015987604,4.44089209850063E-16));
#33536=CARTESIAN_POINT('Ctrl Pts',(-38.0308320192805,32.5523638252493,6.24166374344619E-16));
#33537=CARTESIAN_POINT('Ctrl Pts',(-37.9581383688774,32.4524234721426,-1.26765506881022E-15));
#33538=CARTESIAN_POINT('Ctrl Pts',(-37.8809743110047,32.3557958917759,-1.62370117351429E-15));
#33539=CARTESIAN_POINT('Ctrl Pts',(-37.82656120339,32.2876578612733,-1.87477110872936E-15));
#33540=CARTESIAN_POINT('Ctrl Pts',(-37.7699241047827,32.2211674765398,1.39931090156461E-15));
#33541=CARTESIAN_POINT('Ctrl Pts',(-37.7111553490298,32.1564437978227,1.60982338570648E-15));
#33542=CARTESIAN_POINT('Ctrl Pts',(-37.6849229569216,32.1275533287794,1.70378906452554E-15));
#33543=CARTESIAN_POINT('Ctrl Pts',(-37.6582657142846,32.0990149717255,2.33543966985802E-16));
#33544=CARTESIAN_POINT('Ctrl Pts',(-37.6311912225754,32.0708398884709,3.05311331771918E-16));
#33545=CARTESIAN_POINT('Ctrl Pts',(-37.6195692277271,32.0587454537553,3.36118186902312E-16));
#33546=CARTESIAN_POINT('Ctrl Pts',(-37.6078717672662,32.0467194961249,-1.14899013469077E-15));
#33547=CARTESIAN_POINT('Ctrl Pts',(-37.5961059477358,32.034769281675,-1.17961196366423E-15));
#33548=CARTESIAN_POINT('Ctrl Pts',(-37.5076636824121,31.9449409416833,-1.40979260818075E-15));
#33549=CARTESIAN_POINT('Ctrl Pts',(-37.4152620841693,31.8592852286376,-2.45663089159861E-15));
#33550=CARTESIAN_POINT('Ctrl Pts',(-37.3192298936088,31.778120294682,-2.019218126037E-15));
#33551=CARTESIAN_POINT('Ctrl Pts',(-37.2371898445147,31.7087813040001,-1.64553754506066E-15));
#33552=CARTESIAN_POINT('Ctrl Pts',(-37.1524990927587,31.6427198578901,-2.42654488972963E-15));
#33553=CARTESIAN_POINT('Ctrl Pts',(-37.0653383821438,31.5801518871639,-2.52575738102223E-15));
#33554=CARTESIAN_POINT('Ctrl Pts',(-37.0262273476737,31.5520761860535,-2.57027632928952E-15));
#33555=CARTESIAN_POINT('Ctrl Pts',(-36.9866187071144,31.524704156366,-1.17712968719052E-15));
#33556=CARTESIAN_POINT('Ctrl Pts',(-36.946527548351,31.4980566647868,-6.31439345255558E-16));
#33557=CARTESIAN_POINT('Ctrl Pts',(-36.9192934800282,31.479954927928,-2.60749933581654E-16));
#33558=CARTESIAN_POINT('Ctrl Pts',(-36.89183110785,31.4621841581827,-1.11508673223599E-15));
#33559=CARTESIAN_POINT('Ctrl Pts',(-36.8641751230777,31.4447696709256,-1.17267306976032E-15));
#33560=CARTESIAN_POINT('Ctrl Pts',(-36.757370770553,31.3775168483861,-1.39506513224507E-15));
#33561=CARTESIAN_POINT('Ctrl Pts',(-36.6476196941272,31.3155308365787,-2.17833836995006E-15));
#33562=CARTESIAN_POINT('Ctrl Pts',(-36.5352238715355,31.2591452947779,-6.38378239159465E-16));
#33563=CARTESIAN_POINT('Ctrl Pts',(-36.4331301648989,31.2079280090246,7.60430312613923E-16));
#33564=CARTESIAN_POINT('Ctrl Pts',(-36.3288535333025,31.1613315369686,5.40797342115576E-17));
#33565=CARTESIAN_POINT('Ctrl Pts',(-36.2225969429285,31.1196350477066,-1.58727198051878E-16));
#33566=CARTESIAN_POINT('Ctrl Pts',(-36.1671664218874,31.0978833792477,-2.38185072021888E-16));
#33567=CARTESIAN_POINT('Ctrl Pts',(-36.1111967480356,31.0774656809663,2.2162435752245E-16));
#33568=CARTESIAN_POINT('Ctrl Pts',(-36.0547320440516,31.0583698407596,1.38777878078145E-16));
#33569=CARTESIAN_POINT('Ctrl Pts',(-38.5153120432796,35.002811202661,7.11258330249199));
#33570=CARTESIAN_POINT('Ctrl Pts',(-38.5180431912138,35.3538028140734,7.09672411194513));
#33571=CARTESIAN_POINT('Ctrl Pts',(-38.4695957643305,35.7040585809451,7.08086492139827));
#33572=CARTESIAN_POINT('Ctrl Pts',(-38.3668186228693,36.0375700163406,7.06500573085141));
#33573=CARTESIAN_POINT('Ctrl Pts',(-38.0276667128012,37.1381166820277,7.01267235506732));
#33574=CARTESIAN_POINT('Ctrl Pts',(-37.0969083679288,38.05633118704,6.96033897928324));
#33575=CARTESIAN_POINT('Ctrl Pts',(-35.9918737299572,38.3805513419917,6.90800560349915));
#33576=CARTESIAN_POINT('Ctrl Pts',(-34.8868390919855,38.7047714969434,6.85567222771507));
#33577=CARTESIAN_POINT('Ctrl Pts',(-33.6075281609145,38.4349973018346,6.80333885193099));
#33578=CARTESIAN_POINT('Ctrl Pts',(-32.7275161143991,37.6921715510808,6.7510054761469));
#33579=CARTESIAN_POINT('Ctrl Pts',(-31.8475040678837,36.949345800327,6.69867210036282));
#33580=CARTESIAN_POINT('Ctrl Pts',(-31.3667909059239,35.7334684939282,6.64633872457873));
#33581=CARTESIAN_POINT('Ctrl Pts',(-31.5009116523996,34.5896898927146,6.59400534879465));
#33582=CARTESIAN_POINT('Ctrl Pts',(-31.6350323988753,33.445911291501,6.54167197301056));
#33583=CARTESIAN_POINT('Ctrl Pts',(-32.3839870537864,32.3742313954726,6.48933859722648));
#33584=CARTESIAN_POINT('Ctrl Pts',(-33.4119757367826,31.8551401282763,6.43700522144239));
#33585=CARTESIAN_POINT('Ctrl Pts',(-34.4399644197788,31.33604886108,6.38467184565831));
#33586=CARTESIAN_POINT('Ctrl Pts',(-35.74698713086,31.3695462227158,6.33233846987422));
#33587=CARTESIAN_POINT('Ctrl Pts',(-36.7470351933603,31.9406149492898,6.28000509409014));
#33588=CARTESIAN_POINT('Ctrl Pts',(-37.7470832558605,32.5116836758639,6.22767171830605));
#33589=CARTESIAN_POINT('Ctrl Pts',(-38.4401566697799,33.6203237673762,6.17533834252197));
#33590=CARTESIAN_POINT('Ctrl Pts',(-38.5155120371445,34.769470406568,6.12300496673789));
#33591=CARTESIAN_POINT('Ctrl Pts',(-38.5205141244106,34.8457507296795,6.11953107865592));
#33592=CARTESIAN_POINT('Ctrl Pts',(-38.5227943601281,34.922209536826,6.11605719057395));
#33593=CARTESIAN_POINT('Ctrl Pts',(-38.5224238694764,34.9986908177615,6.11258330249199));
#33594=CARTESIAN_POINT('Origin',(35.,-35.,4.));
#33595=CARTESIAN_POINT('Origin',(-35.,-35.,4.));
#33596=CARTESIAN_POINT('Origin',(-35.,35.,4.));
#33597=CARTESIAN_POINT('Origin',(35.,35.,4.));
#33598=CARTESIAN_POINT('Origin',(50.,50.,0.));
#33599=CARTESIAN_POINT('',(50.,50.,0.));
#33600=CARTESIAN_POINT('',(-50.,50.,0.));
#33601=CARTESIAN_POINT('',(50.,50.,0.));
#33602=CARTESIAN_POINT('',(-50.,50.,0.));
#33603=CARTESIAN_POINT('',(50.,50.,0.));
#33604=CARTESIAN_POINT('Origin',(50.,-50.,0.));
#33605=CARTESIAN_POINT('',(50.,-50.,0.));
#33606=CARTESIAN_POINT('',(50.,-50.,0.));
#33607=CARTESIAN_POINT('',(50.,-50.,0.));
#33608=CARTESIAN_POINT('Origin',(-50.,-50.,0.));
#33609=CARTESIAN_POINT('',(-50.,-50.,0.));
#33610=CARTESIAN_POINT('',(-50.,-50.,0.));
#33611=CARTESIAN_POINT('',(-50.,-50.,0.));
#33612=CARTESIAN_POINT('Origin',(-50.,50.,0.));
#33613=CARTESIAN_POINT('',(-50.,50.,0.));
#33614=CARTESIAN_POINT('Origin',(0.,0.,0.));
#33615=CARTESIAN_POINT('',(0.,0.,0.));
#33616=CARTESIAN_POINT('Origin',(0.,0.,0.));
#33617=CARTESIAN_POINT('',(-3.94684541635378,0.00250618816942501,0.322176117089595));
#33618=CARTESIAN_POINT('',(-3.94571229786942,0.00420644411048898,0.1778238829104));
#33619=CARTESIAN_POINT('',(-3.942,-4.82755768223887E-16,0.));
#33620=CARTESIAN_POINT('',(1.7270326134187,3.54354657824448,0.));
#33621=CARTESIAN_POINT('Ctrl Pts',(-3.94684541635378,0.00250618816942501,
0.322176117089595));
#33622=CARTESIAN_POINT('Ctrl Pts',(-3.94773112778461,0.132835587750837,
0.316895328369763));
#33623=CARTESIAN_POINT('Ctrl Pts',(-3.94183789351545,0.26307859818693,0.311614539649932));
#33624=CARTESIAN_POINT('Ctrl Pts',(-3.92890301514817,0.39261184999977,0.3063337509301));
#33625=CARTESIAN_POINT('Ctrl Pts',(-3.79917189807037,1.69177315474756,0.253369772435476));
#33626=CARTESIAN_POINT('Ctrl Pts',(-2.96110743411295,2.91953839146377,0.200405793940852));
#33627=CARTESIAN_POINT('Ctrl Pts',(-1.79852789548214,3.51470668248002,0.147441815446229));
#33628=CARTESIAN_POINT('Ctrl Pts',(-0.719726524887938,4.06698577113378,
0.098294543630819));
#33629=CARTESIAN_POINT('Ctrl Pts',(0.638504507243322,4.07455564834572,0.0491472718154096));
#33630=CARTESIAN_POINT('Ctrl Pts',(1.73118107496479,3.54876586530513,-4.77048955893622E-17));
#33631=CARTESIAN_POINT('',(-1.72703261341866,3.5435465782445,0.));
#33632=CARTESIAN_POINT('Origin',(0.,0.,0.));
#33633=CARTESIAN_POINT('Ctrl Pts',(-1.72703261341866,3.5435465782445,-1.38777878078145E-15));
#33634=CARTESIAN_POINT('Ctrl Pts',(-2.90680413394004,2.96855656546122,0.0529882887282479));
#33635=CARTESIAN_POINT('Ctrl Pts',(-3.76655616656995,1.76297958901422,0.105976577456497));
#33636=CARTESIAN_POINT('Ctrl Pts',(-3.92036033233788,0.467860933696955,
0.158964866184747));
#33637=CARTESIAN_POINT('Ctrl Pts',(-3.93860710223307,0.314212741058287,
0.165251205093298));
#33638=CARTESIAN_POINT('Ctrl Pts',(-3.94691794439651,0.159304285881835,
0.171537544001849));
#33639=CARTESIAN_POINT('Ctrl Pts',(-3.94571229786942,0.00420644411048898,
0.1778238829104));
#33640=CARTESIAN_POINT('Origin',(0.,0.,0.));
#33641=CARTESIAN_POINT('',(-3.93670753965503,0.00216852164164449,1.32217611708959));
#33642=CARTESIAN_POINT('',(-3.93636006504333,0.00190811380198534,1.1778238829104));
#33643=CARTESIAN_POINT('',(-3.942,-4.82755768223887E-16,0.));
#33644=CARTESIAN_POINT('Ctrl Pts',(-3.93670753965503,0.00216852164164449,
1.32217611708959));
#33645=CARTESIAN_POINT('Ctrl Pts',(-3.93928378279248,0.519701728735777,
1.30134586600417));
#33646=CARTESIAN_POINT('Ctrl Pts',(-3.8445230015698,1.03632804611489,1.28051561491875));
#33647=CARTESIAN_POINT('Ctrl Pts',(-3.6480161981814,1.51081450660005,1.25968536383333));
#33648=CARTESIAN_POINT('Ctrl Pts',(-3.14836873517057,2.71726615166507,1.2067213853387));
#33649=CARTESIAN_POINT('Ctrl Pts',(-1.9909276922364,3.6512813246822,1.15375740684408));
#33650=CARTESIAN_POINT('Ctrl Pts',(-0.706151782787128,3.88482400643261,
1.10079342834945));
#33651=CARTESIAN_POINT('Ctrl Pts',(0.57862412666215,4.11836668818302,1.04782944985483));
#33652=CARTESIAN_POINT('Ctrl Pts',(1.99073490262654,3.65143687866671,0.994865471360208));
#33653=CARTESIAN_POINT('Ctrl Pts',(2.88298828242626,2.69797395029701,0.941901492865584));
#33654=CARTESIAN_POINT('Ctrl Pts',(3.77524166222597,1.74451102192732,0.88893751437096));
#33655=CARTESIAN_POINT('Ctrl Pts',(4.14763764586101,0.304514974704242,0.835973535876336));
#33656=CARTESIAN_POINT('Ctrl Pts',(3.82952478082154,-0.96194142997557,0.783009557381713));
#33657=CARTESIAN_POINT('Ctrl Pts',(3.51141191578207,-2.22839783465538,0.730045578887089));
#33658=CARTESIAN_POINT('Ctrl Pts',(2.50279020206811,-3.32131459679193,0.677081600392466));
#33659=CARTESIAN_POINT('Ctrl Pts',(1.26587965171505,-3.74001178475658,0.624117621897842));
#33660=CARTESIAN_POINT('Ctrl Pts',(0.0289691013620001,-4.15870897272123,
0.571153643403219));
#33661=CARTESIAN_POINT('Ctrl Pts',(-1.43623028563014,-3.90318658651399,
0.518189664908595));
#33662=CARTESIAN_POINT('Ctrl Pts',(-2.45813109402713,-3.09014670702069,
0.465225686413971));
#33663=CARTESIAN_POINT('Ctrl Pts',(-3.37814298820071,-2.35817120272038,
0.417542496639179));
#33664=CARTESIAN_POINT('Ctrl Pts',(-3.9388478333255,-1.17431072748125,0.369859306864387));
#33665=CARTESIAN_POINT('Ctrl Pts',(-3.94684541635378,0.00250618816942501,
0.322176117089595));
#33666=CARTESIAN_POINT('Ctrl Pts',(-3.94571229786942,0.00420644411048898,
0.1778238829104));
#33667=CARTESIAN_POINT('Ctrl Pts',(-3.93675540826681,-1.14803363217555,
0.224525832730098));
#33668=CARTESIAN_POINT('Ctrl Pts',(-3.40256651647006,-2.31072629277711,
0.271227782549796));
#33669=CARTESIAN_POINT('Ctrl Pts',(-2.51512664140724,-3.04478428612434,
0.317929732369494));
#33670=CARTESIAN_POINT('Ctrl Pts',(-1.50823248580272,-3.87765051644084,
0.370918021097743));
#33671=CARTESIAN_POINT('Ctrl Pts',(-0.0465878756876988,-4.1587226428863,
0.423906309825993));
#33672=CARTESIAN_POINT('Ctrl Pts',(1.1983574972874,-3.76190237425103,0.476894598554242));
#33673=CARTESIAN_POINT('Ctrl Pts',(2.44330287026249,-3.36508210561577,0.529882887282491));
#33674=CARTESIAN_POINT('Ctrl Pts',(3.47154900609766,-2.29036944189979,0.58287117601074));
#33675=CARTESIAN_POINT('Ctrl Pts',(3.81196419489399,-1.02929753659268,0.635859464738989));
#33676=CARTESIAN_POINT('Ctrl Pts',(4.15237938369031,0.231774368714438,0.688847753467239));
#33677=CARTESIAN_POINT('Ctrl Pts',(3.80496362544778,1.67920551561269,0.741836042195488));
#33678=CARTESIAN_POINT('Ctrl Pts',(2.92880392464218,2.64832610367255,0.794824330923737));
#33679=CARTESIAN_POINT('Ctrl Pts',(2.05264422383658,3.61744669173242,0.847812619651987));
#33680=CARTESIAN_POINT('Ctrl Pts',(0.647740580467906,4.1082567209539,0.900800908380236));
#33681=CARTESIAN_POINT('Ctrl Pts',(-0.641345987445116,3.89601342814375,
0.953789197108486));
#33682=CARTESIAN_POINT('Ctrl Pts',(-1.93043255535814,3.68377013533359,1.00677748583673));
#33683=CARTESIAN_POINT('Ctrl Pts',(-3.10370204781551,2.7684735204918,1.05976577456498));
#33684=CARTESIAN_POINT('Ctrl Pts',(-3.6230578333699,1.56976054866973,1.11275406329323));
#33685=CARTESIAN_POINT('Ctrl Pts',(-3.83564812513838,1.0790858560709,1.13444400316562));
#33686=CARTESIAN_POINT('Ctrl Pts',(-3.9386720278785,0.540923388712033,1.15613394303801));
#33687=CARTESIAN_POINT('Ctrl Pts',(-3.93636006504333,0.00190811380198534,
1.1778238829104));
#33688=CARTESIAN_POINT('Origin',(0.,0.,0.));
#33689=CARTESIAN_POINT('',(-3.93898402517327,-0.0032694952000395,2.32217611708959));
#33690=CARTESIAN_POINT('',(-3.93943713807335,-0.00339197931643889,2.1778238829104));
#33691=CARTESIAN_POINT('',(-3.942,-4.82755768223887E-16,0.));
#33692=CARTESIAN_POINT('Ctrl Pts',(-3.93898402517327,-0.0032694952000395,
2.32217611708959));
#33693=CARTESIAN_POINT('Ctrl Pts',(-3.93192709039827,0.89928000152811,2.28579640363858));
#33694=CARTESIAN_POINT('Ctrl Pts',(-3.6239186993101,1.80618191912708,2.24941669018756));
#33695=CARTESIAN_POINT('Ctrl Pts',(-3.05593295732034,2.50036976841156,2.21303697673655));
#33696=CARTESIAN_POINT('Ctrl Pts',(-2.22902197396405,3.51101407626844,2.16007299824193));
#33697=CARTESIAN_POINT('Ctrl Pts',(-0.851077281590667,4.07080133208995,
2.1071090197473));
#33698=CARTESIAN_POINT('Ctrl Pts',(0.446378324979883,3.92317725380663,2.05414504125268));
#33699=CARTESIAN_POINT('Ctrl Pts',(1.74383393155043,3.77555317552331,2.00118106275806));
#33700=CARTESIAN_POINT('Ctrl Pts',(2.96080045231815,2.92051776313515,1.94821708426343));
#33701=CARTESIAN_POINT('Ctrl Pts',(3.53953231896037,1.74993928366879,1.89525310576881));
#33702=CARTESIAN_POINT('Ctrl Pts',(4.11826418560259,0.57936080420243,1.84228912727419));
#33703=CARTESIAN_POINT('Ctrl Pts',(4.05876139811932,-0.906760742342139,
1.78932514877956));
#33704=CARTESIAN_POINT('Ctrl Pts',(3.38829497669137,-2.0273218478537,1.73636117028494));
#33705=CARTESIAN_POINT('Ctrl Pts',(2.71782855526341,-3.14788295336526,1.68339719179031));
#33706=CARTESIAN_POINT('Ctrl Pts',(1.43639849989078,-3.90288361784382,1.63043321329569));
#33707=CARTESIAN_POINT('Ctrl Pts',(0.131293493556904,-3.9463054651445,1.57746923480107));
#33708=CARTESIAN_POINT('Ctrl Pts',(-1.17381151277698,-3.98972731244518,
1.52450525630644));
#33709=CARTESIAN_POINT('Ctrl Pts',(-2.50259147007212,-3.32157034256797,
1.47154127781182));
#33710=CARTESIAN_POINT('Ctrl Pts',(-3.24605450717593,-2.24804779907291,
1.4185772993172));
#33711=CARTESIAN_POINT('Ctrl Pts',(-3.69712029286904,-1.59673190927805,
1.386443571908));
#33712=CARTESIAN_POINT('Ctrl Pts',(-3.93273330552895,-0.796202603784206,
1.3543098444988));
#33713=CARTESIAN_POINT('Ctrl Pts',(-3.93670753965503,0.00216852164164449,
1.32217611708959));
#33714=CARTESIAN_POINT('Ctrl Pts',(-3.93636006504333,0.00190811380198534,
1.1778238829104));
#33715=CARTESIAN_POINT('Ctrl Pts',(-3.93302392765509,-0.775885103331329,
1.20912223176626));
#33716=CARTESIAN_POINT('Ctrl Pts',(-3.71035557449182,-1.55545405153981,
1.24042058062212));
#33717=CARTESIAN_POINT('Ctrl Pts',(-3.28106611164764,-2.19667847798475,
1.27171892947798));
#33718=CARTESIAN_POINT('Ctrl Pts',(-2.5542765257196,-3.28227520401484,1.32470721820623));
#33719=CARTESIAN_POINT('Ctrl Pts',(-1.23525527521213,-3.97133932727269,
1.37769550693448));
#33720=CARTESIAN_POINT('Ctrl Pts',(0.0709513775297463,-3.94785759961686,
1.43068379566273));
#33721=CARTESIAN_POINT('Ctrl Pts',(1.37715803027162,-3.92437587196102,1.48367208439098));
#33722=CARTESIAN_POINT('Ctrl Pts',(2.67055008524789,-3.1883482933915,1.53666037311923));
#33723=CARTESIAN_POINT('Ctrl Pts',(3.3578681272901,-2.07735647460328,1.58964866184748));
#33724=CARTESIAN_POINT('Ctrl Pts',(4.0451861693323,-0.966364655815065,1.64263695057573));
#33725=CARTESIAN_POINT('Ctrl Pts',(4.12643019844044,0.519591403191845,1.69562523930397));
#33726=CARTESIAN_POINT('Ctrl Pts',(3.56432857554823,1.69889860460012,1.74861352803222));
#33727=CARTESIAN_POINT('Ctrl Pts',(3.00222695265603,2.87820580600839,1.80160181676047));
#33728=CARTESIAN_POINT('Ctrl Pts',(1.7967796777635,3.75086414981802,1.85459010548872));
#33729=CARTESIAN_POINT('Ctrl Pts',(0.500920035194316,3.91659925522552,1.90757839421697));
#33730=CARTESIAN_POINT('Ctrl Pts',(-0.794939607374858,4.08233436063301,
1.96056668294522));
#33731=CARTESIAN_POINT('Ctrl Pts',(-2.18121161762068,3.54114622763838,2.01355497167347));
#33732=CARTESIAN_POINT('Ctrl Pts',(-3.02202408579975,2.54126994215436,2.06654326040172));
#33733=CARTESIAN_POINT('Ctrl Pts',(-3.61062040344951,1.84132373296486,2.10363680123794));
#33734=CARTESIAN_POINT('Ctrl Pts',(-3.93191648715648,0.916599256990189,
2.14073034207417));
#33735=CARTESIAN_POINT('Ctrl Pts',(-3.93943713807335,-0.00339197931643889,
2.1778238829104));
#33736=CARTESIAN_POINT('Origin',(0.,0.,0.));
#33737=CARTESIAN_POINT('',(-3.94841909008794,-0.000476659622032916,3.3221761170896));
#33738=CARTESIAN_POINT('',(-3.94848727448062,-0.000227313299713517,3.1778238829104));
#33739=CARTESIAN_POINT('',(-3.942,-4.82755768223887E-16,0.));
#33740=CARTESIAN_POINT('Ctrl Pts',(-3.94841909008794,-0.000476659622032916,
3.3221761170896));
#33741=CARTESIAN_POINT('Ctrl Pts',(-3.94623626626659,1.27989932784314,3.27024694127299));
#33742=CARTESIAN_POINT('Ctrl Pts',(-3.2656648832367,2.56226681984272,3.21831776545638));
#33743=CARTESIAN_POINT('Ctrl Pts',(-2.20319423243154,3.27666141545475,3.16638858963978));
#33744=CARTESIAN_POINT('Ctrl Pts',(-1.11955152454134,4.00529188962783,3.11342461114515));
#33745=CARTESIAN_POINT('Ctrl Pts',(0.361362461026873,4.14308771897741,3.06046063265053));
#33746=CARTESIAN_POINT('Ctrl Pts',(1.56083317716561,3.62689600200629,3.00749665415591));
#33747=CARTESIAN_POINT('Ctrl Pts',(2.76030389330435,3.11070428503517,2.95453267566128));
#33748=CARTESIAN_POINT('Ctrl Pts',(3.67833134001362,1.94052502174336,2.90156869716666));
#33749=CARTESIAN_POINT('Ctrl Pts',(3.89417629964206,0.652660565018754,2.84860471867204));
#33750=CARTESIAN_POINT('Ctrl Pts',(4.11002125927051,-0.635203891705856,
2.79564074017741));
#33751=CARTESIAN_POINT('Ctrl Pts',(3.62368373181814,-2.04075354186327,2.74267676168279));
#33752=CARTESIAN_POINT('Ctrl Pts',(2.65805604729365,-2.91981385750971,2.68971278318817));
#33753=CARTESIAN_POINT('Ctrl Pts',(1.69242836276915,-3.79887417315615,2.63674880469354));
#33754=CARTESIAN_POINT('Ctrl Pts',(0.247510521172539,-4.15144515429161,
2.58378482619892));
#33755=CARTESIAN_POINT('Ctrl Pts',(-1.01448026111426,-3.8159408321598,2.53082084770429));
#33756=CARTESIAN_POINT('Ctrl Pts',(-2.27647104340105,-3.48043651002799,
2.47785686920967));
#33757=CARTESIAN_POINT('Ctrl Pts',(-3.35553476637803,-2.45685688462891,
2.42489289071505));
#33758=CARTESIAN_POINT('Ctrl Pts',(-3.75712799069693,-1.21431639198325,
2.37192891222042));
#33759=CARTESIAN_POINT('Ctrl Pts',(-3.88287625699264,-0.825247793982355,
2.35534464717681));
#33760=CARTESIAN_POINT('Ctrl Pts',(-3.94220103997636,-0.414710890659917,
2.3387603821332));
#33761=CARTESIAN_POINT('Ctrl Pts',(-3.93898402517327,-0.0032694952000395,
2.32217611708959));
#33762=CARTESIAN_POINT('Ctrl Pts',(-3.93943713807335,-0.00339197931643889,
2.1778238829104));
#33763=CARTESIAN_POINT('Ctrl Pts',(-3.9426597705752,-0.397612332356497,
2.19371863080242));
#33764=CARTESIAN_POINT('Ctrl Pts',(-3.8882681890457,-0.790963586497156,
2.20961337869445));
#33765=CARTESIAN_POINT('Ctrl Pts',(-3.77260571048107,-1.16538770550329,
2.22550812658647));
#33766=CARTESIAN_POINT('Ctrl Pts',(-3.387021940871,-2.41360462970351,2.27849641531472));
#33767=CARTESIAN_POINT('Ctrl Pts',(-2.32050147553854,-3.45147404013054,
2.33148470404296));
#33768=CARTESIAN_POINT('Ctrl Pts',(-1.06225033291184,-3.80293352608456,
2.38447299277121));
#33769=CARTESIAN_POINT('Ctrl Pts',(0.19600080971487,-4.15439301203859,2.43746128149946));
#33770=CARTESIAN_POINT('Ctrl Pts',(1.64598262963581,-3.81944257351961,2.49044957022771));
#33771=CARTESIAN_POINT('Ctrl Pts',(2.62259865984893,-2.95172107137353,2.54343785895596));
#33772=CARTESIAN_POINT('Ctrl Pts',(3.59921469006204,-2.08399956922746,2.59642614768421));
#33773=CARTESIAN_POINT('Ctrl Pts',(4.10246493056733,-0.683507003454308,
2.64941443641246));
#33774=CARTESIAN_POINT('Ctrl Pts',(3.90151184350976,0.607360005829592,2.70240272514071));
#33775=CARTESIAN_POINT('Ctrl Pts',(3.70055875645219,1.89822701511349,2.75539101386896));
#33776=CARTESIAN_POINT('Ctrl Pts',(2.79540234183177,3.07946846790813,2.80837930259721));
#33777=CARTESIAN_POINT('Ctrl Pts',(1.60123168012205,3.60925720078016,2.86136759132546));
#33778=CARTESIAN_POINT('Ctrl Pts',(0.407061018412325,4.1390459336522,2.91435588005371));
#33779=CARTESIAN_POINT('Ctrl Pts',(-1.0761238903867,4.01738194660163,2.96734416878196));
#33780=CARTESIAN_POINT('Ctrl Pts',(-2.16799636339283,3.30007158724765,3.0203324575102));
#33781=CARTESIAN_POINT('Ctrl Pts',(-3.24974830176843,2.58940995703755,3.07282959931027));
#33782=CARTESIAN_POINT('Ctrl Pts',(-3.94740831268547,1.29409283853931,3.12532674111033));
#33783=CARTESIAN_POINT('Ctrl Pts',(-3.94848727448062,-0.000227313299713517,
3.1778238829104));
#33784=CARTESIAN_POINT('Origin',(0.,0.,0.));
#33785=CARTESIAN_POINT('',(-3.94039517343639,0.00354505425716481,4.32217611708959));
#33786=CARTESIAN_POINT('',(-3.94011414712863,0.00351656949004968,4.1778238829104));
#33787=CARTESIAN_POINT('',(-3.942,-4.82755768223887E-16,0.));
#33788=CARTESIAN_POINT('Ctrl Pts',(-3.94039517343639,0.00354505425716481,
4.32217611708959));
#33789=CARTESIAN_POINT('Ctrl Pts',(-3.94353004938676,0.363314892612021,
4.30766145740202));
#33790=CARTESIAN_POINT('Ctrl Pts',(-3.89832073254977,0.722311104007169,
4.29314679771445));
#33791=CARTESIAN_POINT('Ctrl Pts',(-3.80162926767229,1.06685976451013,4.27863213802688));
#33792=CARTESIAN_POINT('Ctrl Pts',(-3.44880221029601,2.32411747761066,4.22566815953225));
#33793=CARTESIAN_POINT('Ctrl Pts',(-2.41048038450093,3.38900325344725,4.17270418103763));
#33794=CARTESIAN_POINT('Ctrl Pts',(-1.16253486527102,3.7734715492884,4.119740202543));
#33795=CARTESIAN_POINT('Ctrl Pts',(0.0854106539588831,4.15793984512954,
4.06677622404838));
#33796=CARTESIAN_POINT('Ctrl Pts',(1.54297986662362,3.86199066097525,4.01381224555376));
#33797=CARTESIAN_POINT('Ctrl Pts',(2.54215731665373,3.02125984033277,3.96084826705914));
#33798=CARTESIAN_POINT('Ctrl Pts',(3.54133476668386,2.18052901969028,3.90788428856451));
#33799=CARTESIAN_POINT('Ctrl Pts',(4.08212045407936,0.795016562559593,3.85492031006988));
#33800=CARTESIAN_POINT('Ctrl Pts',(3.91666803670668,-0.500286254334146,
3.80195633157526));
#33801=CARTESIAN_POINT('Ctrl Pts',(3.75121561933401,-1.79558907122787,3.74899235308063));
#33802=CARTESIAN_POINT('Ctrl Pts',(2.87952509719318,-3.00068224788464,3.69602837458601));
#33803=CARTESIAN_POINT('Ctrl Pts',(1.70109910586756,-3.56326208407903,3.64306439609139));
#33804=CARTESIAN_POINT('Ctrl Pts',(0.522673114541947,-4.12584192027342,
3.59010041759677));
#33805=CARTESIAN_POINT('Ctrl Pts',(-0.962488345968457,-4.04590841600543,
3.53713643910214));
#33806=CARTESIAN_POINT('Ctrl Pts',(-2.07372407526821,-3.36009572803379,
3.48417246060752));
#33807=CARTESIAN_POINT('Ctrl Pts',(-3.18495980456796,-2.67428304006214,
3.4312084821129));
#33808=CARTESIAN_POINT('Ctrl Pts',(-3.92226980265706,-1.38259116838684,
3.37824450361827));
#33809=CARTESIAN_POINT('Ctrl Pts',(-3.94773908659551,-0.0770126730508915,
3.32528052512365));
#33810=CARTESIAN_POINT('Ctrl Pts',(-3.94823670184224,-0.0515044661197667,
3.32424572244563));
#33811=CARTESIAN_POINT('Ctrl Pts',(-3.94846258763822,-0.025990958277152,
3.32321091976761));
#33812=CARTESIAN_POINT('Ctrl Pts',(-3.94841909008794,-0.000476659622032916,
3.3221761170896));
#33813=CARTESIAN_POINT('Ctrl Pts',(-3.94848727448062,-0.000227313299713517,
3.1778238829104));
#33814=CARTESIAN_POINT('Ctrl Pts',(-3.94849736891154,-0.0123365700109349,
3.17831502983858));
#33815=CARTESIAN_POINT('Ctrl Pts',(-3.94844649235883,-0.0244457394587464,
3.17880617676677));
#33816=CARTESIAN_POINT('Ctrl Pts',(-3.94833438892723,-0.0365543420562738,
3.17929732369495));
#33817=CARTESIAN_POINT('Ctrl Pts',(-3.9362399042423,-1.34291318034886,3.2322856124232));
#33818=CARTESIAN_POINT('Ctrl Pts',(-3.21149089765924,-2.64267412527665,
3.28527390115145));
#33819=CARTESIAN_POINT('Ctrl Pts',(-2.1065247612934,-3.33964579658387,3.3382621898797));
#33820=CARTESIAN_POINT('Ctrl Pts',(-1.00155862492758,-4.03661746789108,
3.39125047860795));
#33821=CARTESIAN_POINT('Ctrl Pts',(0.483624641221001,-4.13079986557773,
3.4442387673362));
#33822=CARTESIAN_POINT('Ctrl Pts',(1.66778169459976,-3.57899215935798,3.49722705606445));
#33823=CARTESIAN_POINT('Ctrl Pts',(2.85193874797851,-3.02718445313824,3.5502153447927));
#33824=CARTESIAN_POINT('Ctrl Pts',(3.73506958858744,-1.82938664301209,3.60320363352094));
#33825=CARTESIAN_POINT('Ctrl Pts',(3.91208817286041,-0.535020350876169,
3.65619192224919));
#33826=CARTESIAN_POINT('Ctrl Pts',(4.08910675713339,0.759345941259773,3.70918021097745));
#33827=CARTESIAN_POINT('Ctrl Pts',(3.56001308507038,2.1502807154055,3.7621684997057));
#33828=CARTESIAN_POINT('Ctrl Pts',(2.56749878545275,2.99977176280624,3.81515678843395));
#33829=CARTESIAN_POINT('Ctrl Pts',(1.57498448583515,3.84926281020697,3.86814507716219));
#33830=CARTESIAN_POINT('Ctrl Pts',(0.11904955866294,4.15731013086274,3.92113336589044));
#33831=CARTESIAN_POINT('Ctrl Pts',(-1.13247866152849,3.78261453618225,3.97412165461869));
#33832=CARTESIAN_POINT('Ctrl Pts',(-2.38400688171994,3.40791894150175,4.02710994334694));
#33833=CARTESIAN_POINT('Ctrl Pts',(-3.43112839493061,2.35048043148498,4.08009823207519));
#33834=CARTESIAN_POINT('Ctrl Pts',(-3.79353576624568,1.09533877709901,4.13308652080344));
#33835=CARTESIAN_POINT('Ctrl Pts',(-3.89552779876129,0.742105210239426,
4.14799897483909));
#33836=CARTESIAN_POINT('Ctrl Pts',(-3.94328881467064,0.373213076031263,
4.16291142887475));
#33837=CARTESIAN_POINT('Ctrl Pts',(-3.94011414712863,0.00351656949004968,
4.1778238829104));
#33838=CARTESIAN_POINT('Origin',(0.,0.,0.));
#33839=CARTESIAN_POINT('',(-3.93600110646763,-0.0014281919745418,5.32217611708959));
#33840=CARTESIAN_POINT('',(-3.93605515638862,-0.00152114337219748,5.1778238829104));
#33841=CARTESIAN_POINT('',(-3.942,-4.82755768223887E-16,0.));
#33842=CARTESIAN_POINT('Ctrl Pts',(-3.93600110646763,-0.0014281919745418,
5.32217611708959));
#33843=CARTESIAN_POINT('Ctrl Pts',(-3.93357236454694,0.74585693902175,5.29211199503643));
#33844=CARTESIAN_POINT('Ctrl Pts',(-3.72918845072319,1.49437332783476,5.26204787298327));
#33845=CARTESIAN_POINT('Ctrl Pts',(-3.33126090733014,2.11973479786067,5.2319837509301));
#33846=CARTESIAN_POINT('Ctrl Pts',(-2.63023175991589,3.22143440482896,5.17901977243548));
#33847=CARTESIAN_POINT('Ctrl Pts',(-1.32852280829314,3.94091180862283,5.12605579394085));
#33848=CARTESIAN_POINT('Ctrl Pts',(-0.0227175227337642,3.94842484544612,
5.07309181544622));
#33849=CARTESIAN_POINT('Ctrl Pts',(1.28308776282561,3.95593788226941,5.0201278369516));
#33850=CARTESIAN_POINT('Ctrl Pts',(2.59298938232161,3.25148655212212,4.96716385845699));
#33851=CARTESIAN_POINT('Ctrl Pts',(3.30664910123763,2.15792645084216,4.91419987996236));
#33852=CARTESIAN_POINT('Ctrl Pts',(4.02030882015365,1.06436634956219,4.86123590146774));
#33853=CARTESIAN_POINT('Ctrl Pts',(4.13772663848969,-0.418302522850447,
4.80827192297311));
#33854=CARTESIAN_POINT('Ctrl Pts',(3.60508904482309,-1.61056133843436,4.75530794447848));
#33855=CARTESIAN_POINT('Ctrl Pts',(3.07245145115649,-2.80282015401828,4.70234396598386));
#33856=CARTESIAN_POINT('Ctrl Pts',(1.88975844548724,-3.70466891277347,4.64937998748924));
#33857=CARTESIAN_POINT('Ctrl Pts',(0.599047552189011,-3.90278322178284,
4.59641600899462));
#33858=CARTESIAN_POINT('Ctrl Pts',(-0.691663341109217,-4.10089753079221,
4.54345203049999));
#33859=CARTESIAN_POINT('Ctrl Pts',(-2.09039212203642,-3.59527739005576,
4.49048805200536));
#33860=CARTESIAN_POINT('Ctrl Pts',(-2.95609036802126,-2.61765249450529,
4.43752407351074));
#33861=CARTESIAN_POINT('Ctrl Pts',(-3.58454594852404,-1.90794351207784,
4.39907475470369));
#33862=CARTESIAN_POINT('Ctrl Pts',(-3.93209089021995,-0.949484883048943,
4.36062543589664));
#33863=CARTESIAN_POINT('Ctrl Pts',(-3.94039517343639,0.00354505425716481,
4.32217611708959));
#33864=CARTESIAN_POINT('Ctrl Pts',(-3.94011414712863,0.00351656949004968,
4.1778238829104));
#33865=CARTESIAN_POINT('Ctrl Pts',(-3.93200829706235,-0.94042619377602,
4.215899717603));
#33866=CARTESIAN_POINT('Ctrl Pts',(-3.59183770381144,-1.88961289751958,
4.25397555229559));
#33867=CARTESIAN_POINT('Ctrl Pts',(-2.97445535308007,-2.59678570511794,
4.29205138698818));
#33868=CARTESIAN_POINT('Ctrl Pts',(-2.1152743391799,-3.5809237341938,4.34503967571643));
#33869=CARTESIAN_POINT('Ctrl Pts',(-0.719219081960083,-4.09635499359035,
4.39802796444469));
#33870=CARTESIAN_POINT('Ctrl Pts',(0.573349476162703,-3.90665471020838,
4.45101625317294));
#33871=CARTESIAN_POINT('Ctrl Pts',(1.86591803428548,-3.7169544268264,4.50400454190118));
#33872=CARTESIAN_POINT('Ctrl Pts',(3.05499989331122,-2.82212260066591,4.55699283062943));
#33873=CARTESIAN_POINT('Ctrl Pts',(3.59517138458731,-1.63261243464328,4.60998111935768));
#33874=CARTESIAN_POINT('Ctrl Pts',(4.13534287586339,-0.443102268620652,
4.66296940808593));
#33875=CARTESIAN_POINT('Ctrl Pts',(4.02660399938981,1.04108623726411,4.71595769681418));
#33876=CARTESIAN_POINT('Ctrl Pts',(3.31883252977577,2.13916602570979,4.76894598554243));
#33877=CARTESIAN_POINT('Ctrl Pts',(2.61106106016173,3.23724581415546,4.82193427427068));
#33878=CARTESIAN_POINT('Ctrl Pts',(1.3042569974072,3.94921688516205,4.87492256299893));
#33879=CARTESIAN_POINT('Ctrl Pts',(-0.00215762490102876,3.94850300633285,
4.92791085172718));
#33880=CARTESIAN_POINT('Ctrl Pts',(-1.30857224720925,3.94778912750366,4.98089914045543));
#33881=CARTESIAN_POINT('Ctrl Pts',(-2.61459742907118,3.23439029883869,5.03388742918367));
#33882=CARTESIAN_POINT('Ctrl Pts',(-3.32116840418697,2.13553765533301,5.08687571791192));
#33883=CARTESIAN_POINT('Ctrl Pts',(-3.72541706095167,1.50685388432656,5.11719177291141));
#33884=CARTESIAN_POINT('Ctrl Pts',(-3.93344647436031,0.751999581783958,
5.14750782791091));
#33885=CARTESIAN_POINT('Ctrl Pts',(-3.93605515638862,-0.00152114337219748,
5.1778238829104));
#33886=CARTESIAN_POINT('Origin',(0.,0.,0.));
#33887=CARTESIAN_POINT('',(-3.94563673384516,-0.00288256983268176,6.3221761170896));
#33888=CARTESIAN_POINT('',(-3.94570073178844,-0.00286656758253237,6.1778238829104));
#33889=CARTESIAN_POINT('',(-3.942,-4.82755768223887E-16,0.));
#33890=CARTESIAN_POINT('Ctrl Pts',(-3.94563673384516,-0.00288256983268176,
6.3221761170896));
#33891=CARTESIAN_POINT('Ctrl Pts',(-3.93638288024859,1.12386902299333,6.27656253267084));
#33892=CARTESIAN_POINT('Ctrl Pts',(-3.42887602753453,2.25790074792199,6.23094894825208));
#33893=CARTESIAN_POINT('Ctrl Pts',(-2.57675389815072,2.99180784716095,6.18533536383333));
#33894=CARTESIAN_POINT('Ctrl Pts',(-1.58731667872186,3.84398029351578,6.1323713853387));
#33895=CARTESIAN_POINT('Ctrl Pts',(-0.133249377743896,4.15668177021255,
6.07940740684408));
#33896=CARTESIAN_POINT('Ctrl Pts',(1.1190375023862,3.78659872632712,6.02644342834946));
#33897=CARTESIAN_POINT('Ctrl Pts',(2.37132438251632,3.41651568244167,5.97347944985483));
#33898=CARTESIAN_POINT('Ctrl Pts',(3.42183084179856,2.363648117974,5.92051547136021));
#33899=CARTESIAN_POINT('Ctrl Pts',(3.78910149173018,1.11053353453949,5.86755149286558));
#33900=CARTESIAN_POINT('Ctrl Pts',(4.15637214166179,-0.142581048895014,
5.81458751437096));
#33901=CARTESIAN_POINT('Ctrl Pts',(3.84040698224279,-1.59594265129635,5.76162353587634));
#33902=CARTESIAN_POINT('Ctrl Pts',(2.98601533590735,-2.58346419748652,5.70865955738171));
#33903=CARTESIAN_POINT('Ctrl Pts',(2.1316236895719,-3.57098574367668,5.65569557888709));
#33904=CARTESIAN_POINT('Ctrl Pts',(0.738805556320001,-4.09266723365567,
5.60273160039247));
#33905=CARTESIAN_POINT('Ctrl Pts',(-0.554099537676607,-3.9094179296049,
5.54976762189784));
#33906=CARTESIAN_POINT('Ctrl Pts',(-1.84700463167322,-3.72616862555414,
5.49680364340322));
#33907=CARTESIAN_POINT('Ctrl Pts',(-3.03999668641454,-2.83798852747363,
5.44383966490859));
#33908=CARTESIAN_POINT('Ctrl Pts',(-3.58631804218233,-1.65193757336201,
5.39087568641397));
#33909=CARTESIAN_POINT('Ctrl Pts',(-3.8225291610139,-1.1391287294386,5.36797582997251));
#33910=CARTESIAN_POINT('Ctrl Pts',(-3.93785108037402,-0.570635640986049,
5.34507597353105));
#33911=CARTESIAN_POINT('Ctrl Pts',(-3.93600110646763,-0.0014281919745418,
5.32217611708959));
#33912=CARTESIAN_POINT('Ctrl Pts',(-3.93605515638862,-0.00152114337219748,
5.1778238829104));
#33913=CARTESIAN_POINT('Ctrl Pts',(-3.93800609125369,-0.565050863861574,
5.20049611663916));
#33914=CARTESIAN_POINT('Ctrl Pts',(-3.82506562686086,-1.12783471721807,
5.22316835036792));
#33915=CARTESIAN_POINT('Ctrl Pts',(-3.59338498454405,-1.63654055836231,
5.24584058409668));
#33916=CARTESIAN_POINT('Ctrl Pts',(-3.05191382141567,-2.82545967020557,
5.29882887282492));
#33917=CARTESIAN_POINT('Ctrl Pts',(-1.86185472678928,-3.71899143554569,
5.35181716155317));
#33918=CARTESIAN_POINT('Ctrl Pts',(-0.569079620514193,-3.90727898054932,
5.40480545028142));
#33919=CARTESIAN_POINT('Ctrl Pts',(0.723695485760891,-4.09556652555295,
5.45779373900967));
#33920=CARTESIAN_POINT('Ctrl Pts',(2.11918660368467,-3.57860985022007,5.51078202773792));
#33921=CARTESIAN_POINT('Ctrl Pts',(2.97729155756073,-2.59353342519368,5.56377031646617));
#33922=CARTESIAN_POINT('Ctrl Pts',(3.83539651143679,-1.60845700016728,5.61675860519442));
#33923=CARTESIAN_POINT('Ctrl Pts',(4.15611530126515,-0.155260825447382,
5.66974689392266));
#33924=CARTESIAN_POINT('Ctrl Pts',(3.79233642449449,1.09948401069401,5.72273518265091));
#33925=CARTESIAN_POINT('Ctrl Pts',(3.42855754772383,2.35422884683541,5.77572347137916));
#33926=CARTESIAN_POINT('Ctrl Pts',(2.38028100435414,3.41052234439828,5.82871176010741));
#33927=CARTESIAN_POINT('Ctrl Pts',(1.12834403334923,3.78384994268096,5.88170004883566));
#33928=CARTESIAN_POINT('Ctrl Pts',(-0.12359293765566,4.15717754096363,5.93468833756392));
#33929=CARTESIAN_POINT('Ctrl Pts',(-1.57919033629578,3.8475392399661,5.98767662629216));
#33930=CARTESIAN_POINT('Ctrl Pts',(-2.57077564940419,2.99696399824068,6.04066491502041));
#33931=CARTESIAN_POINT('Ctrl Pts',(-3.4263409160258,2.26306584157345,6.08638457098374));
#33932=CARTESIAN_POINT('Ctrl Pts',(-3.93646396625886,1.126457364296,6.13210422694707));
#33933=CARTESIAN_POINT('Ctrl Pts',(-3.94570073178844,-0.00286656758253237,
6.1778238829104));
#33934=CARTESIAN_POINT('Origin',(0.,0.,0.));
#33935=CARTESIAN_POINT('',(-3.94505905468816,0.00309284708018512,7.32217611708959));
#33936=CARTESIAN_POINT('',(-3.94511280640764,0.00308469250234145,7.1778238829104));
#33937=CARTESIAN_POINT('',(-3.942,-4.82755768223887E-16,0.));
#33938=CARTESIAN_POINT('Ctrl Pts',(-3.94505905468816,0.00309284708018512,
7.32217611708959));
#33939=CARTESIAN_POINT('Ctrl Pts',(-3.9468047458557,0.205704294057958,7.31397704879987));
#33940=CARTESIAN_POINT('Ctrl Pts',(-3.93254600075262,0.408069386251045,
7.30577798051015));
#33941=CARTESIAN_POINT('Ctrl Pts',(-3.90142848745745,0.607808031556218,
7.29757891222042));
#33942=CARTESIAN_POINT('Ctrl Pts',(-3.7004169521544,1.89807089322147,7.2446149337258));
#33943=CARTESIAN_POINT('Ctrl Pts',(-2.79591524746178,3.0787362122301,7.19165095523118));
#33944=CARTESIAN_POINT('Ctrl Pts',(-1.60246363230549,3.60869576898733,7.13868697673655));
#33945=CARTESIAN_POINT('Ctrl Pts',(-0.409012017149199,4.13865532574456,
7.08572299824193));
#33946=CARTESIAN_POINT('Ctrl Pts',(1.07338950847076,4.01790912025038,7.03275901974731));
#33947=CARTESIAN_POINT('Ctrl Pts',(2.16534464372431,3.30179608998848,6.97979504125268));
#33948=CARTESIAN_POINT('Ctrl Pts',(3.25729977897786,2.58568305972658,6.92683106275806));
#33949=CARTESIAN_POINT('Ctrl Pts',(3.95880852386501,1.27420320469696,6.87386708426343));
#33950=CARTESIAN_POINT('Ctrl Pts',(3.94836389256626,-0.0315819228008631,
6.82090310576881));
#33951=CARTESIAN_POINT('Ctrl Pts',(3.93791926126751,-1.33736705029871,6.76793912727419));
#33952=CARTESIAN_POINT('Ctrl Pts',(3.21552125378285,-2.63745745026476,6.71497514877956));
#33953=CARTESIAN_POINT('Ctrl Pts',(2.11225056959203,-3.33601144740646,6.66201117028494));
#33954=CARTESIAN_POINT('Ctrl Pts',(1.00897988540122,-4.03456544454814,6.60904719179032));
#33955=CARTESIAN_POINT('Ctrl Pts',(-0.475163475495736,-4.1315830388655,
6.55608321329569));
#33956=CARTESIAN_POINT('Ctrl Pts',(-1.65998491543528,-3.58260030236365,
6.50311923480107));
#33957=CARTESIAN_POINT('Ctrl Pts',(-2.84480635537483,-3.0336175658618,6.45015525630644));
#33958=CARTESIAN_POINT('Ctrl Pts',(-3.73030587435696,-1.83863449854073,
6.39719127781182));
#33959=CARTESIAN_POINT('Ctrl Pts',(-3.91065206490815,-0.545321256873756,
6.3442272993172));
#33960=CARTESIAN_POINT('Ctrl Pts',(-3.93568069017971,-0.365833947574368,
6.33687690524133));
#33961=CARTESIAN_POINT('Ctrl Pts',(-3.94712794466584,-0.1844527827072,6.32952651116546));
#33962=CARTESIAN_POINT('Ctrl Pts',(-3.94563673384516,-0.00288256983268176,
6.3221761170896));
#33963=CARTESIAN_POINT('Ctrl Pts',(-3.94570073178844,-0.00286656758253237,
6.1778238829104));
#33964=CARTESIAN_POINT('Ctrl Pts',(-3.94716921739174,-0.182409496340425,
6.18509251567532));
#33965=CARTESIAN_POINT('Ctrl Pts',(-3.93597755777244,-0.361768304659314,
6.19236114844024));
#33966=CARTESIAN_POINT('Ctrl Pts',(-3.91150112201508,-0.539295483751872,
6.19962978120516));
#33967=CARTESIAN_POINT('Ctrl Pts',(-3.73306805394085,-1.83346754156567,
6.25261806993341));
#33968=CARTESIAN_POINT('Ctrl Pts',(-2.84862869021566,-3.03029947473994,
6.30560635866166));
#33969=CARTESIAN_POINT('Ctrl Pts',(-1.66386928259682,-3.58081270897423,
6.35859464738991));
#33970=CARTESIAN_POINT('Ctrl Pts',(-0.479109874977974,-4.13132594320853,
6.41158293611816));
#33971=CARTESIAN_POINT('Ctrl Pts',(1.00596957653452,-4.03552047850286,6.4645712248464));
#33972=CARTESIAN_POINT('Ctrl Pts',(2.11017334393921,-3.33734162243677,6.51755951357465));
#33973=CARTESIAN_POINT('Ctrl Pts',(3.21437711134392,-2.63916276637067,6.5705478023029));
#33974=CARTESIAN_POINT('Ctrl Pts',(3.9377051946408,-1.33861051894414,6.62353609103116));
#33975=CARTESIAN_POINT('Ctrl Pts',(3.94837197806129,-0.0322392490748367,
6.6765243797594));
#33976=CARTESIAN_POINT('Ctrl Pts',(3.95903876148178,1.27413202079445,6.72951266848765));
#33977=CARTESIAN_POINT('Ctrl Pts',(3.25704424502592,2.58632231310649,6.7825009572159));
#33978=CARTESIAN_POINT('Ctrl Pts',(2.16438848411372,3.30243896781703,6.83548924594415));
#33979=CARTESIAN_POINT('Ctrl Pts',(1.07173272320153,4.01855562252758,6.8884775346724));
#33980=CARTESIAN_POINT('Ctrl Pts',(-0.411584282167038,4.13859863963661,
6.94146582340065));
#33981=CARTESIAN_POINT('Ctrl Pts',(-1.60517522591216,3.60750511301625,6.9944541121289));
#33982=CARTESIAN_POINT('Ctrl Pts',(-2.7987661696573,3.07641158639588,7.04744240085715));
#33983=CARTESIAN_POINT('Ctrl Pts',(-3.70263105177901,1.89418151604613,7.1004306895854));
#33984=CARTESIAN_POINT('Ctrl Pts',(-3.9021732688668,0.603095702241273,7.15341897831364));
#33985=CARTESIAN_POINT('Ctrl Pts',(-3.9328077662116,0.404883186052253,7.16155394651256));
#33986=CARTESIAN_POINT('Ctrl Pts',(-3.94684167082104,0.204104985193814,
7.16968891471148));
#33987=CARTESIAN_POINT('Ctrl Pts',(-3.94511280640764,0.00308469250234145,
7.1778238829104));
#33988=CARTESIAN_POINT('Origin',(0.,0.,0.));
#33989=CARTESIAN_POINT('',(-3.93579878224384,0.00110209819909501,8.3221761170896));
#33990=CARTESIAN_POINT('',(-3.93583379497513,0.00119086740244391,8.17782388291041));
#33991=CARTESIAN_POINT('',(-3.942,-4.82755768223887E-16,0.));
#33992=CARTESIAN_POINT('Ctrl Pts',(-3.93579878224384,0.00110209819909501,
8.3221761170896));
#33993=CARTESIAN_POINT('Ctrl Pts',(-3.93727495532409,0.591480280077664,
8.29842758643428));
#33994=CARTESIAN_POINT('Ctrl Pts',(-3.81287497830763,1.18126751761344,8.27467905577897));
#33995=CARTESIAN_POINT('Ctrl Pts',(-3.55943403140727,1.70909456204991,8.25093052512365));
#33996=CARTESIAN_POINT('Ctrl Pts',(-2.9942099737124,2.88625455717395,8.19796654662903));
#33997=CARTESIAN_POINT('Ctrl Pts',(-1.78716283564177,3.75523737390689,8.1450025681344));
#33998=CARTESIAN_POINT('Ctrl Pts',(-0.491491832360601,3.91778133957111,
8.09203858963978));
#33999=CARTESIAN_POINT('Ctrl Pts',(0.804179170920576,4.08032530523533,8.03907461114515));
#34000=CARTESIAN_POINT('Ctrl Pts',(2.18847403941229,3.53643041983081,7.98611063265053));
#34001=CARTESIAN_POINT('Ctrl Pts',(3.02695952634759,2.53536799534552,7.93314665415591));
#34002=CARTESIAN_POINT('Ctrl Pts',(3.86544501328289,1.53430557086022,7.88018267566129));
#34003=CARTESIAN_POINT('Ctrl Pts',(4.15812111866178,0.0760756072941503,
7.82721869716666));
#34004=CARTESIAN_POINT('Ctrl Pts',(3.77085207703933,-1.17100361188895,7.77425471867203));
#34005=CARTESIAN_POINT('Ctrl Pts',(3.38358303541687,-2.41808283107204,7.72129074017741));
#34006=CARTESIAN_POINT('Ctrl Pts',(2.31636884679309,-3.45401130587216,7.66832676168279));
#34007=CARTESIAN_POINT('Ctrl Pts',(1.05832218368842,-3.8040148529523,7.61536278318817));
#34008=CARTESIAN_POINT('Ctrl Pts',(-0.199724479416271,-4.15401840003245,
7.56239880469355));
#34009=CARTESIAN_POINT('Ctrl Pts',(-1.64860361700185,-3.81809701939261,
7.50943482619892));
#34010=CARTESIAN_POINT('Ctrl Pts',(-2.62428250283791,-2.95020612691174,
7.45647084770429));
#34011=CARTESIAN_POINT('Ctrl Pts',(-3.44892179457277,-2.21666874973946,
7.41170593749939));
#34012=CARTESIAN_POINT('Ctrl Pts',(-3.93552800730583,-1.10311616471836,
7.36694102729449));
#34013=CARTESIAN_POINT('Ctrl Pts',(-3.94505905468816,0.00309284708018512,
7.32217611708959));
#34014=CARTESIAN_POINT('Ctrl Pts',(-3.94511280640764,0.00308469250234145,
7.1778238829104));
#34015=CARTESIAN_POINT('Ctrl Pts',(-3.93558046309789,-1.10526968584544,
7.22267720343973));
#34016=CARTESIAN_POINT('Ctrl Pts',(-3.44685564182305,-2.22098372195378,
7.26753052396906));
#34017=CARTESIAN_POINT('Ctrl Pts',(-2.61937124393104,-2.95458540793588,
7.31238384449839));
#34018=CARTESIAN_POINT('Ctrl Pts',(-1.64180744985364,-3.82123914704826,
7.36537213322664));
#34019=CARTESIAN_POINT('Ctrl Pts',(-0.191460309644946,-4.15460506801304,
7.41836042195489));
#34020=CARTESIAN_POINT('Ctrl Pts',(1.06640592095225,-3.80177051623037,7.47134871068314));
#34021=CARTESIAN_POINT('Ctrl Pts',(2.32427215154943,-3.44893596444769,7.52433699941139));
#34022=CARTESIAN_POINT('Ctrl Pts',(3.38965747253514,-2.40990093991759,7.57732528813964));
#34023=CARTESIAN_POINT('Ctrl Pts',(3.77387696635039,-1.16126366048821,7.63031357686789));
#34024=CARTESIAN_POINT('Ctrl Pts',(4.15809646016565,0.0873736189411645,
7.68330186559614));
#34025=CARTESIAN_POINT('Ctrl Pts',(3.86115012681045,1.5456131532698,7.73629015432439));
#34026=CARTESIAN_POINT('Ctrl Pts',(3.01924520659187,2.54457049986684,7.78927844305264));
#34027=CARTESIAN_POINT('Ctrl Pts',(2.17734028637328,3.54352784646387,7.84226673178089));
#34028=CARTESIAN_POINT('Ctrl Pts',(0.79047677929132,4.08320300532929,7.89525502050913));
#34029=CARTESIAN_POINT('Ctrl Pts',(-0.505200564699283,3.91605069371529,
7.94824330923738));
#34030=CARTESIAN_POINT('Ctrl Pts',(-1.80087790868988,3.74889838210129,8.00123159796563));
#34031=CARTESIAN_POINT('Ctrl Pts',(-3.00536908958914,2.87491860000785,8.05421988669388));
#34032=CARTESIAN_POINT('Ctrl Pts',(-3.56618228885602,1.69499986105314,8.10720817542213));
#34033=CARTESIAN_POINT('Ctrl Pts',(-3.81530790878367,1.17085387502675,8.13074674458489));
#34034=CARTESIAN_POINT('Ctrl Pts',(-3.93741444221381,0.586335951582262,
8.15428531374765));
#34035=CARTESIAN_POINT('Ctrl Pts',(-3.93583379497513,0.00119086740244391,
8.17782388291041));
#34036=CARTESIAN_POINT('Origin',(0.,0.,0.));
#34037=CARTESIAN_POINT('',(-3.94101045068862,-0.00360005201630542,9.3221761170896));
#34038=CARTESIAN_POINT('',(-3.94073510056759,-0.00358878591061127,9.1778238829104));
#34039=CARTESIAN_POINT('',(-3.942,-4.82755768223887E-16,0.));
#34040=CARTESIAN_POINT('Ctrl Pts',(-3.94101045068862,-0.00360005201630542,
9.3221761170896));
#34041=CARTESIAN_POINT('Ctrl Pts',(-3.93228175108165,0.970079126201241,
9.28287812406869));
#34042=CARTESIAN_POINT('Ctrl Pts',(-3.56768740150403,1.94959821666609,9.24358013104778));
#34043=CARTESIAN_POINT('Ctrl Pts',(-2.91383898553304,2.66460451331084,9.20428213802687));
#34044=CARTESIAN_POINT('Ctrl Pts',(-2.03261297931419,3.6282562219074,9.15131815953225));
#34045=CARTESIAN_POINT('Ctrl Pts',(-0.625975040492547,4.11143697314778,
9.09835418103763));
#34046=CARTESIAN_POINT('Ctrl Pts',(0.661401578964616,3.89270122117173,9.04539020254301));
#34047=CARTESIAN_POINT('Ctrl Pts',(1.9487781984218,3.67396546919568,8.99242622404838));
#34048=CARTESIAN_POINT('Ctrl Pts',(3.11689349851449,2.75331321400316,8.93946224555376));
#34049=CARTESIAN_POINT('Ctrl Pts',(3.63039103221387,1.55268663908397,8.88649826705913));
#34050=CARTESIAN_POINT('Ctrl Pts',(4.14388856591324,0.352060064164805,8.83353428856451));
#34051=CARTESIAN_POINT('Ctrl Pts',(4.00276833321932,-1.12854083048104,8.78057031006989));
#34052=CARTESIAN_POINT('Ctrl Pts',(3.2717068488331,-2.21054498738825,8.72760633157527));
#34053=CARTESIAN_POINT('Ctrl Pts',(2.54064536444688,-3.29254914429547,8.67464235308064));
#34054=CARTESIAN_POINT('Ctrl Pts',(1.21964262836836,-3.97595656346406,8.62167837458601));
#34055=CARTESIAN_POINT('Ctrl Pts',(-0.0858753956759256,-3.94755623929365,
8.56871439609139));
#34056=CARTESIAN_POINT('Ctrl Pts',(-1.39139341972021,-3.91915591512325,
8.51575041759677));
#34057=CARTESIAN_POINT('Ctrl Pts',(-2.68142673173026,-3.17894784761384,
8.46278643910214));
#34058=CARTESIAN_POINT('Ctrl Pts',(-3.36474289907574,-2.06617522710156,
8.40982246060752));
#34059=CARTESIAN_POINT('Ctrl Pts',(-3.74166677096472,-1.45235898112435,
8.38060701276821));
#34060=CARTESIAN_POINT('Ctrl Pts',(-3.93398279378317,-0.725181276064265,
8.35139156492891));
#34061=CARTESIAN_POINT('Ctrl Pts',(-3.93579878224384,0.00110209819909501,
8.3221761170896));
#34062=CARTESIAN_POINT('Ctrl Pts',(-3.93583379497513,0.00119086740244391,
8.17782388291041));
#34063=CARTESIAN_POINT('Ctrl Pts',(-3.93385620587065,-0.730899452746949,
8.2072736024759));
#34064=CARTESIAN_POINT('Ctrl Pts',(-3.73826901230947,-1.46397147804348,
8.23672332204139));
#34065=CARTESIAN_POINT('Ctrl Pts',(-3.35559744737338,-2.0810205230852,8.26617304160688));
#34066=CARTESIAN_POINT('Ctrl Pts',(-2.66706418898931,-3.19126447245286,
8.31916133033513));
#34067=CARTESIAN_POINT('Ctrl Pts',(-1.37286245458661,-3.92589467537216,
8.37214961906338));
#34068=CARTESIAN_POINT('Ctrl Pts',(-0.0666336764464662,-3.94794131155515,
8.42513790779163));
#34069=CARTESIAN_POINT('Ctrl Pts',(1.23959510169366,-3.96998794773813,8.47812619651988));
#34070=CARTESIAN_POINT('Ctrl Pts',(2.55785092357125,-3.27945101718484,8.53111448524812));
#34071=CARTESIAN_POINT('Ctrl Pts',(3.28345891245731,-2.19307505948273,8.58410277397638));
#34072=CARTESIAN_POINT('Ctrl Pts',(4.00906690134337,-1.10669910178063,8.63709106270462));
#34073=CARTESIAN_POINT('Ctrl Pts',(4.14202705723791,0.375515883070263,8.69007935143287));
#34074=CARTESIAN_POINT('Ctrl Pts',(3.62135147131388,1.57368807822049,8.74306764016112));
#34075=CARTESIAN_POINT('Ctrl Pts',(3.10067588538986,2.77186027337072,8.79605592888937));
#34076=CARTESIAN_POINT('Ctrl Pts',(1.92636455764724,3.68598967882027,8.84904421761762));
#34077=CARTESIAN_POINT('Ctrl Pts',(0.637066015602396,3.89677142492153,8.90203250634587));
#34078=CARTESIAN_POINT('Ctrl Pts',(-0.652232526442438,4.1075531710228,8.95502079507412));
#34079=CARTESIAN_POINT('Ctrl Pts',(-2.05651828278951,3.61498725777581,9.00800908380237));
#34080=CARTESIAN_POINT('Ctrl Pts',(-2.93165503760022,2.64501028104501,9.06099737253062));
#34081=CARTESIAN_POINT('Ctrl Pts',(-3.57481082178969,1.93215449058061,9.09993954265721));
#34082=CARTESIAN_POINT('Ctrl Pts',(-3.93216906200874,0.9614452240408,9.13888171278381));
#34083=CARTESIAN_POINT('Ctrl Pts',(-3.94073510056759,-0.00358878591061127,
9.1778238829104));
#34084=CARTESIAN_POINT('Origin',(0.,0.,0.));
#34085=CARTESIAN_POINT('',(-3.94826120782986,0.000860587304522282,10.3221761170896));
#34086=CARTESIAN_POINT('',(-3.94838239458768,0.000624922565347272,10.1778238829104));
#34087=CARTESIAN_POINT('',(-3.942,-4.82755768223887E-16,0.));
#34088=CARTESIAN_POINT('Ctrl Pts',(-3.94826120782986,0.000860587304522282,
10.3221761170896));
#34089=CARTESIAN_POINT('Ctrl Pts',(-3.94839882197096,0.0473049479418113,
10.3202926401977));
#34090=CARTESIAN_POINT('Ctrl Pts',(-3.94765033544244,0.0937447675908473,
10.3184091633059));
#34091=CARTESIAN_POINT('Ctrl Pts',(-3.94600203836796,0.140152628104641,
10.316525686414));
#34092=CARTESIAN_POINT('Ctrl Pts',(-3.89965139229318,1.4451566538172,10.2635617079194));
#34093=CARTESIAN_POINT('Ctrl Pts',(-3.14177325024928,2.72488891140618,10.2105977294247));
#34094=CARTESIAN_POINT('Ctrl Pts',(-2.0197091369755,3.39283802265691,10.1576337509301));
#34095=CARTESIAN_POINT('Ctrl Pts',(-0.897645023701731,4.06078713390763,
10.1046697724355));
#34096=CARTESIAN_POINT('Ctrl Pts',(0.588605060801912,4.11695309882012,10.0517057939409));
#34097=CARTESIAN_POINT('Ctrl Pts',(1.75788099084149,3.53559461307527,9.99874181544624));
#34098=CARTESIAN_POINT('Ctrl Pts',(2.92715692088108,2.95423612733042,9.94577783695161));
#34099=CARTESIAN_POINT('Ctrl Pts',(3.7794586964566,1.73535319092823,9.89281385845698));
#34100=CARTESIAN_POINT('Ctrl Pts',(3.92416969750304,0.437569458677891,9.83984987996236));
#34101=CARTESIAN_POINT('Ctrl Pts',(4.06888069854947,-0.860214273572448,
9.78688590146773));
#34102=CARTESIAN_POINT('Ctrl Pts',(3.50600092506682,-2.23689880167093,9.73392192297312));
#34103=CARTESIAN_POINT('Ctrl Pts',(2.49350261285418,-3.06153875782394,9.68095794447849));
#34104=CARTESIAN_POINT('Ctrl Pts',(1.48100430064151,-3.88617871397697,9.62799396598387));
#34105=CARTESIAN_POINT('Ctrl Pts',(0.0188874496988303,-4.15877409818449,
9.57502998748924));
#34106=CARTESIAN_POINT('Ctrl Pts',(-1.22274826539589,-3.75439229775474,
9.52206600899461));
#34107=CARTESIAN_POINT('Ctrl Pts',(-2.46438398049055,-3.350010497325,9.46910203049999));
#34108=CARTESIAN_POINT('Ctrl Pts',(-3.48553855973727,-2.26865151225807,
9.41613805200537));
#34109=CARTESIAN_POINT('Ctrl Pts',(-3.81820881255261,-1.00591068674825,
9.36317407351075));
#34110=CARTESIAN_POINT('Ctrl Pts',(-3.90404577140141,-0.680093059958056,
9.34950808803704));
#34111=CARTESIAN_POINT('Ctrl Pts',(-3.94404588005443,-0.342199672065631,
9.33584210256332));
#34112=CARTESIAN_POINT('Ctrl Pts',(-3.94101045068862,-0.00360005201630542,
9.3221761170896));
#34113=CARTESIAN_POINT('Ctrl Pts',(-3.94073510056759,-0.00358878591061127,
9.1778238829104));
#34114=CARTESIAN_POINT('Ctrl Pts',(-3.94382479981015,-0.351668569711599,
9.19187000151206));
#34115=CARTESIAN_POINT('Ctrl Pts',(-3.90153714912137,-0.6990100110183,9.20591612011371));
#34116=CARTESIAN_POINT('Ctrl Pts',(-3.81091609517323,-1.03324690266663,
9.21996223871536));
#34117=CARTESIAN_POINT('Ctrl Pts',(-3.46905264466117,-2.29413906943288,
9.27295052744361));
#34118=CARTESIAN_POINT('Ctrl Pts',(-2.4393379903627,-3.36853536275074,9.32593881617186));
#34119=CARTESIAN_POINT('Ctrl Pts',(-1.194095160419,-3.76361759404226,9.37892710490011));
#34120=CARTESIAN_POINT('Ctrl Pts',(0.0511476695246889,-4.15869982533377,
9.43191539362836));
#34121=CARTESIAN_POINT('Ctrl Pts',(1.5119186751136,-3.87446799459896,9.48490368235661));
#34122=CARTESIAN_POINT('Ctrl Pts',(2.5181722452647,-3.04129728726066,9.53789197108486));
#34123=CARTESIAN_POINT('Ctrl Pts',(3.5244258154158,-2.20812657992236,9.59088025981311));
#34124=CARTESIAN_POINT('Ctrl Pts',(4.07616195012909,-0.826016995980571,
9.64386854854136));
#34125=CARTESIAN_POINT('Ctrl Pts',(3.92030308000722,0.471067306450377,9.69685683726961));
#34126=CARTESIAN_POINT('Ctrl Pts',(3.76444420988535,1.76815160888132,9.74984512599786));
#34127=CARTESIAN_POINT('Ctrl Pts',(2.90099033492832,2.98021062980143,9.8028334147261));
#34128=CARTESIAN_POINT('Ctrl Pts',(1.72600180756239,3.55128123451409,9.85582170345435));
#34129=CARTESIAN_POINT('Ctrl Pts',(0.551013280196442,4.12235183922675,9.90880999218261));
#34130=CARTESIAN_POINT('Ctrl Pts',(-0.935509899578419,4.05243402773195,
9.96179828091086));
#34131=CARTESIAN_POINT('Ctrl Pts',(-2.05170977553871,3.37359861917203,10.0147865696391));
#34132=CARTESIAN_POINT('Ctrl Pts',(-3.16790965149901,2.69476321061211,10.0677748583674));
#34133=CARTESIAN_POINT('Ctrl Pts',(-3.91378622364473,1.40701020498706,10.1207631470956));
#34134=CARTESIAN_POINT('Ctrl Pts',(-3.94721103949169,0.101023047050935,
10.1737514358238));
#34135=CARTESIAN_POINT('Ctrl Pts',(-3.94806733432703,0.0675655685271688,
10.175108918186));
#34136=CARTESIAN_POINT('Ctrl Pts',(-3.94845604040098,0.0340961227584357,
10.1764664005482));
#34137=CARTESIAN_POINT('Ctrl Pts',(-3.94838239458768,0.000624922565347272,
10.1778238829104));
#34138=CARTESIAN_POINT('Origin',(0.,0.,0.));
#34139=CARTESIAN_POINT('',(-3.93845364011251,0.00310220437029302,11.3221761170896));
#34140=CARTESIAN_POINT('',(-3.93886953396072,0.00324640498314072,11.1778238829104));
#34141=CARTESIAN_POINT('',(-3.942,-4.82755768223887E-16,0.));
#34142=CARTESIAN_POINT('Ctrl Pts',(-3.93845364011251,0.00310220437029302,
11.3221761170896));
#34143=CARTESIAN_POINT('Ctrl Pts',(-3.94163276156383,0.435745363096063,
11.3047431778321));
#34144=CARTESIAN_POINT('Ctrl Pts',(-3.87593103620607,0.867449899692147,
11.2873102385747));
#34145=CARTESIAN_POINT('Ctrl Pts',(-3.73722250128773,1.27426167714383,11.2698772993172));
#34146=CARTESIAN_POINT('Ctrl Pts',(-3.31580441728399,2.51021907446466,11.2169133208226));
#34147=CARTESIAN_POINT('Ctrl Pts',(-2.2205051385,3.51640664107286,11.163949342328));
#34148=CARTESIAN_POINT('Ctrl Pts',(-0.953308955593125,3.83168068622044,
11.1109853638333));
#34149=CARTESIAN_POINT('Ctrl Pts',(0.313887227313751,4.14695473136801,11.0580213853387));
#34150=CARTESIAN_POINT('Ctrl Pts',(1.75298031434354,3.77131525505496,11.0050574068441));
#34151=CARTESIAN_POINT('Ctrl Pts',(2.70442260335169,2.87692078939432,10.9520934283495));
#34152=CARTESIAN_POINT('Ctrl Pts',(3.65586489235987,1.98252632373365,10.8991294498548));
#34153=CARTESIAN_POINT('Ctrl Pts',(4.11965638334642,0.569376868725343,10.8461654713602));
#34154=CARTESIAN_POINT('Ctrl Pts',(3.88323778121684,-0.714870044482812,
10.7932014928656));
#34155=CARTESIAN_POINT('Ctrl Pts',(3.64681917908728,-1.99911695769091,10.740237514371));
#34156=CARTESIAN_POINT('Ctrl Pts',(2.71019048384171,-3.15446132909884,10.6872735358763));
#34157=CARTESIAN_POINT('Ctrl Pts',(1.5026160073439,-3.65139972893172,10.6343095573817));
#34158=CARTESIAN_POINT('Ctrl Pts',(0.295041530846062,-4.14833812876461,
10.5813455788871));
#34159=CARTESIAN_POINT('Ctrl Pts',(-1.18347872690403,-3.98687055702237,
10.5283816003925));
#34160=CARTESIAN_POINT('Ctrl Pts',(-2.25532728072623,-3.24099887423319,
10.4754176218978));
#34161=CARTESIAN_POINT('Ctrl Pts',(-3.28905932517556,-2.52165148434584,
10.4243371202951));
#34162=CARTESIAN_POINT('Ctrl Pts',(-3.94452906787893,-1.25872547303165,
10.3732566186924));
#34163=CARTESIAN_POINT('Ctrl Pts',(-3.94826120782986,0.000860587304522282,
10.3221761170896));
#34164=CARTESIAN_POINT('Ctrl Pts',(-3.94838239458768,0.000624922565347272,
10.1778238829104));
#34165=CARTESIAN_POINT('Ctrl Pts',(-3.94558133224467,-1.27242665007483,
10.2294546892765));
#34166=CARTESIAN_POINT('Ctrl Pts',(-3.27394054517676,-2.548016178621,10.2810854956425));
#34167=CARTESIAN_POINT('Ctrl Pts',(-2.22159520444575,-3.26422967848529,
10.3327163020086));
#34168=CARTESIAN_POINT('Ctrl Pts',(-1.14158149400459,-3.99927393583826,
10.3857045907369));
#34169=CARTESIAN_POINT('Ctrl Pts',(0.339418986425944,-4.14514114029698,
10.4386928794651));
#34170=CARTESIAN_POINT('Ctrl Pts',(1.54208150481898,-3.63492300865035,10.4916811681933));
#34171=CARTESIAN_POINT('Ctrl Pts',(2.744744023212,-3.12470487700374,10.5446694569216));
#34172=CARTESIAN_POINT('Ctrl Pts',(3.66906857956751,-1.95840140925179,10.5976577456498));
#34173=CARTESIAN_POINT('Ctrl Pts',(3.89107385865357,-0.670987982622134,
10.6506460343781));
#34174=CARTESIAN_POINT('Ctrl Pts',(4.11307913773965,0.616425444007545,10.7036343231063));
#34175=CARTESIAN_POINT('Ctrl Pts',(3.63276513955622,2.02494882951498,10.7566226118346));
#34176=CARTESIAN_POINT('Ctrl Pts',(2.67044859081355,2.90850218671784,10.8096109005628));
#34177=CARTESIAN_POINT('Ctrl Pts',(1.70813204207087,3.79205554392072,10.8625991892911));
#34178=CARTESIAN_POINT('Ctrl Pts',(0.263812942768934,4.15063887281905,10.9155874780193));
#34179=CARTESIAN_POINT('Ctrl Pts',(-1.00000947224434,3.81977246727369,10.9685757667476));
#34180=CARTESIAN_POINT('Ctrl Pts',(-2.2638318872576,3.48890606172833,11.0215640554758));
#34181=CARTESIAN_POINT('Ctrl Pts',(-3.34715761798219,2.46858992173929,11.0745523442041));
#34182=CARTESIAN_POINT('Ctrl Pts',(-3.75307260433058,1.22683604158983,11.1275406329323));
#34183=CARTESIAN_POINT('Ctrl Pts',(-3.88147031395203,0.834048488809281,
11.1443017162584));
#34184=CARTESIAN_POINT('Ctrl Pts',(-3.94208881978707,0.419104697969423,
11.1610627995844));
#34185=CARTESIAN_POINT('Ctrl Pts',(-3.93886953396072,0.00324640498314072,
11.1778238829104));
#34186=CARTESIAN_POINT('Origin',(0.,0.,0.));
#34187=CARTESIAN_POINT('',(-3.93708098219134,-0.00243404615490106,12.3221761170896));
#34188=CARTESIAN_POINT('',(-3.93670434321626,-0.00217448122624482,12.1778238829104));
#34189=CARTESIAN_POINT('',(-3.942,-4.82755768223887E-16,0.));
#34190=CARTESIAN_POINT('Ctrl Pts',(-3.93708098219134,-0.00243404615490106,
12.3221761170896));
#34191=CARTESIAN_POINT('Ctrl Pts',(-3.93246581499902,0.816826384091263,
12.2891937154665));
#34192=CARTESIAN_POINT('Ctrl Pts',(-3.68329161894405,1.63865836153011,12.2562113138435));
#34193=CARTESIAN_POINT('Ctrl Pts',(-3.20967797357049,2.29968305467193,12.2232289122204));
#34194=CARTESIAN_POINT('Ctrl Pts',(-2.4491371489512,3.36117330126154,12.1702649337258));
#34195=CARTESIAN_POINT('Ctrl Pts',(-1.10983987433617,4.00799378602558,12.1173009552312));
#34196=CARTESIAN_POINT('Ctrl Pts',(0.194403355371928,3.94370158371407,12.0643369767366));
#34197=CARTESIAN_POINT('Ctrl Pts',(1.49864658508003,3.87940938140256,12.0113729982419));
#34198=CARTESIAN_POINT('Ctrl Pts',(2.7678357698812,3.1040044920155,11.9584090197473));
#34199=CARTESIAN_POINT('Ctrl Pts',(3.42029150490108,1.97286108671397,11.9054450412527));
#34200=CARTESIAN_POINT('Ctrl Pts',(4.07274723992097,0.841717681412442,11.8524810627581));
#34201=CARTESIAN_POINT('Ctrl Pts',(4.10846952515958,-0.645164239803552,
11.7995170842634));
#34202=CARTESIAN_POINT('Ctrl Pts',(3.51108655579286,-1.8063349754958,11.7465531057688));
#34203=CARTESIAN_POINT('Ctrl Pts',(2.91370358642613,-2.96750571118807,11.6935891272742));
#34204=CARTESIAN_POINT('Ctrl Pts',(1.68321536245406,-3.80296526135658,11.6406251487796));
#34205=CARTESIAN_POINT('Ctrl Pts',(0.383564333431266,-3.92981593056064,
11.5876611702849));
#34206=CARTESIAN_POINT('Ctrl Pts',(-0.91608669559151,-4.0566665997647,11.5346971917903));
#34207=CARTESIAN_POINT('Ctrl Pts',(-2.28490052966501,-3.47490838800432,
11.4817332132957));
#34208=CARTESIAN_POINT('Ctrl Pts',(-3.09553900209,-2.4511656681074,11.4287692348011));
#34209=CARTESIAN_POINT('Ctrl Pts',(-3.6393581823996,-1.76438488268918,11.3932381955639));
#34210=CARTESIAN_POINT('Ctrl Pts',(-3.93197409656805,-0.878691784660489,
11.3577071563268));
#34211=CARTESIAN_POINT('Ctrl Pts',(-3.93845364011251,0.00310220437029302,
11.3221761170896));
#34212=CARTESIAN_POINT('Ctrl Pts',(-3.93886953396072,0.00324640498314072,
11.1778238829104));
#34213=CARTESIAN_POINT('Ctrl Pts',(-3.9319114080084,-0.895584744841287,
11.2140510883126));
#34214=CARTESIAN_POINT('Ctrl Pts',(-3.62672875965172,-1.79868808138705,
11.2502782937149));
#34215=CARTESIAN_POINT('Ctrl Pts',(-3.06311856673542,-2.49158288893653,
11.2865054991171));
#34216=CARTESIAN_POINT('Ctrl Pts',(-2.23874530081967,-3.50505631900356,
11.3394937878453));
#34217=CARTESIAN_POINT('Ctrl Pts',(-0.861494527015975,-4.06881155882777,
11.3924820765736));
#34218=CARTESIAN_POINT('Ctrl Pts',(0.436898299346125,-3.92425795818127,
11.4454703653018));
#34219=CARTESIAN_POINT('Ctrl Pts',(1.73529112570822,-3.77970435753476,11.4984586540301));
#34220=CARTESIAN_POINT('Ctrl Pts',(2.95482600462875,-2.92684191641753,11.5514469427583));
#34221=CARTESIAN_POINT('Ctrl Pts',(3.53611067677546,-1.75687276941591,11.6044352314866));
#34222=CARTESIAN_POINT('Ctrl Pts',(4.11739534892219,-0.586903622414244,
11.6574235202148));
#34223=CARTESIAN_POINT('Ctrl Pts',(4.06042981429509,0.900172230471804,11.7104118089431));
#34224=CARTESIAN_POINT('Ctrl Pts',(3.39134377174076,2.02224332566476,11.7634000976713));
#34225=CARTESIAN_POINT('Ctrl Pts',(2.72225772918646,3.14431442085768,11.8163883863996));
#34226=CARTESIAN_POINT('Ctrl Pts',(1.44105117870494,3.90138075835749,11.8693766751278));
#34227=CARTESIAN_POINT('Ctrl Pts',(0.135404751111381,3.94618121729058,11.9223649638561));
#34228=CARTESIAN_POINT('Ctrl Pts',(-1.17024167648218,3.99098167622367,11.9753532525843));
#34229=CARTESIAN_POINT('Ctrl Pts',(-2.50032798118779,3.32351625659005,12.0283415413126));
#34230=CARTESIAN_POINT('Ctrl Pts',(-3.24475272518949,2.24994675463574,12.0813298300408));
#34231=CARTESIAN_POINT('Ctrl Pts',(-3.69662968598688,1.59827399972424,12.1134945143307));
#34232=CARTESIAN_POINT('Ctrl Pts',(-3.93270958942814,0.796965223217272,
12.1456591986205));
#34233=CARTESIAN_POINT('Ctrl Pts',(-3.93670434321626,-0.00217448122624482,
12.1778238829104));
#34234=CARTESIAN_POINT('Origin',(0.,0.,0.));
#34235=CARTESIAN_POINT('',(-3.94733077553239,-0.00192598462593618,13.3221761170896));
#34236=CARTESIAN_POINT('',(-3.94682996399265,-0.00229165249276323,13.1778238829104));
#34237=CARTESIAN_POINT('',(-3.942,-4.82755768223887E-16,0.));
#34238=CARTESIAN_POINT('Ctrl Pts',(-3.94733077553239,-0.00192598462593618,
13.3221761170896));
#34239=CARTESIAN_POINT('Ctrl Pts',(-3.94013816129704,1.1955636687552,13.273644253101));
#34240=CARTESIAN_POINT('Ctrl Pts',(-3.356565432248,2.39912123530496,13.2251123891123));
#34241=CARTESIAN_POINT('Ctrl Pts',(-2.40836516771617,3.12895382914166,13.1765805251237));
#34242=CARTESIAN_POINT('Ctrl Pts',(-1.37357164668001,3.92543751280327,13.123616546629));
#34243=CARTESIAN_POINT('Ctrl Pts',(0.0954887653771007,4.15772060523228,
13.0706525681344));
#34244=CARTESIAN_POINT('Ctrl Pts',(1.32553410510171,3.71934593472844,13.0176885896398));
#34245=CARTESIAN_POINT('Ctrl Pts',(2.55557944482628,3.28097126422461,12.9647246111452));
#34246=CARTESIAN_POINT('Ctrl Pts',(3.54660971221836,2.17193883078797,12.9117606326505));
#34247=CARTESIAN_POINT('Ctrl Pts',(3.84442792620346,0.900526938073336,12.8587966541559));
#34248=CARTESIAN_POINT('Ctrl Pts',(4.14224614018855,-0.370884954641299,
12.8058326756613));
#34249=CARTESIAN_POINT('Ctrl Pts',(3.74685230076666,-1.80467630663392,12.7528686971667));
#34250=CARTESIAN_POINT('Ctrl Pts',(2.83945852033214,-2.74372924270635,12.699904718672));
#34251=CARTESIAN_POINT('Ctrl Pts',(1.93206473989763,-3.68278217877878,12.6469407401774));
#34252=CARTESIAN_POINT('Ctrl Pts',(0.512671018450501,-4.127096698931,12.5939767616828));
#34253=CARTESIAN_POINT('Ctrl Pts',(-0.768203316346435,-3.8730399572846,
12.5410127831882));
#34254=CARTESIAN_POINT('Ctrl Pts',(-2.04907765114337,-3.6189832156382,12.4880488046935));
#34255=CARTESIAN_POINT('Ctrl Pts',(-3.19143259929011,-2.66655521219318,
12.4350848261989));
#34256=CARTESIAN_POINT('Ctrl Pts',(-3.67171788605172,-1.45226120626306,
12.3821208477043));
#34257=CARTESIAN_POINT('Ctrl Pts',(-3.85291381676684,-0.994147791942479,
12.3621392708327));
#34258=CARTESIAN_POINT('Ctrl Pts',(-3.93987696773182,-0.498762829361246,
12.3421576939612));
#34259=CARTESIAN_POINT('Ctrl Pts',(-3.93708098219134,-0.00243404615490106,
12.3221761170896));
#34260=CARTESIAN_POINT('Ctrl Pts',(-3.93670434321626,-0.00217448122624482,
12.1778238829104));
#34261=CARTESIAN_POINT('Ctrl Pts',(-3.93929057014649,-0.519542192545187,
12.1986474873488));
#34262=CARTESIAN_POINT('Ctrl Pts',(-3.84460194542603,-1.03600077131728,
12.2194710917872));
#34263=CARTESIAN_POINT('Ctrl Pts',(-3.64821869509448,-1.51035790430073,
12.2402946962256));
#34264=CARTESIAN_POINT('Ctrl Pts',(-3.14849673769996,-2.71741947700787,
12.2932829849538));
#34265=CARTESIAN_POINT('Ctrl Pts',(-1.99028963961311,-3.65186903814713,
12.3462712736821));
#34266=CARTESIAN_POINT('Ctrl Pts',(-0.704859028994106,-3.8850810024459,
12.3992595624103));
#34267=CARTESIAN_POINT('Ctrl Pts',(0.580571581624919,-4.11829296674466,
12.4522478511386));
#34268=CARTESIAN_POINT('Ctrl Pts',(1.99322570477611,-3.6502673342029,12.5052361398668));
#34269=CARTESIAN_POINT('Ctrl Pts',(2.88512861233689,-2.6956842427472,12.5582244285951));
#34270=CARTESIAN_POINT('Ctrl Pts',(3.77703151989765,-1.74110115129151,12.6112127173233));
#34271=CARTESIAN_POINT('Ctrl Pts',(4.148183211868,-0.299960600921891,12.6642010060516));
#34272=CARTESIAN_POINT('Ctrl Pts',(3.82833896043004,0.966696152042594,12.7171892947798));
#34273=CARTESIAN_POINT('Ctrl Pts',(3.50849470899208,2.23335290500708,12.7701775835081));
#34274=CARTESIAN_POINT('Ctrl Pts',(2.4976545141458,3.32552586056643,12.8231658722363));
#34275=CARTESIAN_POINT('Ctrl Pts',(1.259483819326,3.74224279746471,12.8761541609646));
#34276=CARTESIAN_POINT('Ctrl Pts',(0.0213131245061955,4.158959734363,12.9291424496928));
#34277=CARTESIAN_POINT('Ctrl Pts',(-1.44418807028713,3.90022065260022,12.9821307384211));
#34278=CARTESIAN_POINT('Ctrl Pts',(-2.46480444872359,3.08470738901973,13.0351190271493));
#34279=CARTESIAN_POINT('Ctrl Pts',(-3.38102522484729,2.35261038265819,13.082687312403));
#34280=CARTESIAN_POINT('Ctrl Pts',(-3.93871824071251,1.17181521210322,13.1302555976567));
#34281=CARTESIAN_POINT('Ctrl Pts',(-3.94682996399265,-0.00229165249276323,
13.1778238829104));
#34282=CARTESIAN_POINT('Origin',(0.,0.,0.));
#34283=CARTESIAN_POINT('',(-3.9429197498326,0.0035503728418125,14.3221761170896));
#34284=CARTESIAN_POINT('',(-3.94377660893062,0.00343048778150908,14.1778238829104));
#34285=CARTESIAN_POINT('',(-3.942,-4.82755768223887E-16,0.));
#34286=CARTESIAN_POINT('Ctrl Pts',(-3.9429197498326,0.0035503728418125,
14.3221761170896));
#34287=CARTESIAN_POINT('Ctrl Pts',(-3.94546599449794,0.278662013094457,
14.31105876923));
#34288=CARTESIAN_POINT('Ctrl Pts',(-3.91912941936741,0.553289499978031,
14.2999414213704));
#34289=CARTESIAN_POINT('Ctrl Pts',(-3.86210967795079,0.821391308358944,
14.2888240735108));
#34290=CARTESIAN_POINT('Ctrl Pts',(-3.59046284308573,2.09865083039248,14.2358600950161));
#34291=CARTESIAN_POINT('Ctrl Pts',(-2.62241565120338,3.22780031721448,14.1828961165215));
#34292=CARTESIAN_POINT('Ctrl Pts',(-1.40163175876062,3.69134166107696,14.1299321380269));
#34293=CARTESIAN_POINT('Ctrl Pts',(-0.18084786631787,4.15488300493943,14.0769681595322));
#34294=CARTESIAN_POINT('Ctrl Pts',(1.29267272668526,3.95281620584241,14.0240041810376));
#34295=CARTESIAN_POINT('Ctrl Pts',(2.34360392082064,3.17775007014128,13.971040202543));
#34296=CARTESIAN_POINT('Ctrl Pts',(3.39453511495603,2.40268393444014,13.9180762240484));
#34297=CARTESIAN_POINT('Ctrl Pts',(4.02287691022366,1.05461846213484,13.8651122455537));
#34298=CARTESIAN_POINT('Ctrl Pts',(3.9406553103857,-0.24861731777516,13.8121482670591));
#34299=CARTESIAN_POINT('Ctrl Pts',(3.85843371054775,-1.55185309768514,13.7591842885645));
#34300=CARTESIAN_POINT('Ctrl Pts',(3.06564871560427,-2.81025918519985,13.7062203100699));
#34301=CARTESIAN_POINT('Ctrl Pts',(1.92563993605177,-3.44709815390442,13.6532563315753));
#34302=CARTESIAN_POINT('Ctrl Pts',(0.7856311564993,-4.08393712260898,13.6002923530807));
#34303=CARTESIAN_POINT('Ctrl Pts',(-0.701601407662154,-4.09920897250343,
13.547328374586));
#34304=CARTESIAN_POINT('Ctrl Pts',(-1.85444735256939,-3.48591449443573,
13.4943643960914));
#34305=CARTESIAN_POINT('Ctrl Pts',(-3.00729329747666,-2.87262001636802,
13.4414004175968));
#34306=CARTESIAN_POINT('Ctrl Pts',(-3.82575262312968,-1.63075921033812,
13.3884364391021));
#34307=CARTESIAN_POINT('Ctrl Pts',(-3.93471897094859,-0.329486669876098,
13.3354724606075));
#34308=CARTESIAN_POINT('Ctrl Pts',(-3.94383745759853,-0.22059400231727,
13.3310403461016));
#34309=CARTESIAN_POINT('Ctrl Pts',(-3.94798763243564,-0.111285296783124,
13.3266082315956));
#34310=CARTESIAN_POINT('Ctrl Pts',(-3.94733077553239,-0.00192598462593618,
13.3221761170896));
#34311=CARTESIAN_POINT('Ctrl Pts',(-3.94682996399265,-0.00229165249276323,
13.1778238829104));
#34312=CARTESIAN_POINT('Ctrl Pts',(-3.94775422620073,-0.13607119177326,
13.183243886385));
#34313=CARTESIAN_POINT('Ctrl Pts',(-3.94154345388817,-0.269763898960769,
13.1886638898595));
#34314=CARTESIAN_POINT('Ctrl Pts',(-3.92791502810543,-0.402696136440426,
13.1940838933341));
#34315=CARTESIAN_POINT('Ctrl Pts',(-3.79467766697122,-1.70229895292184,
13.2470721820623));
#34316=CARTESIAN_POINT('Ctrl Pts',(-2.95247138262324,-2.92921714048647,
13.3000604707906));
#34317=CARTESIAN_POINT('Ctrl Pts',(-1.78761040384536,-3.52067176691954,
13.3530487595188));
#34318=CARTESIAN_POINT('Ctrl Pts',(-0.622749425067479,-4.1121263933526,
13.4060370482471));
#34319=CARTESIAN_POINT('Ctrl Pts',(0.864766248140306,-4.0681174586541,13.4590253369753));
#34320=CARTESIAN_POINT('Ctrl Pts',(1.99262340964458,-3.4088315584166,13.5120136257036));
#34321=CARTESIAN_POINT('Ctrl Pts',(3.12048057114885,-2.7495456581791,13.5650019144318));
#34322=CARTESIAN_POINT('Ctrl Pts',(3.8886792209496,-1.4749827924026,13.6179902031601));
#34323=CARTESIAN_POINT('Ctrl Pts',(3.94485192310407,-0.169776179432411,
13.6709784918883));
#34324=CARTESIAN_POINT('Ctrl Pts',(4.00102462525853,1.13543043353777,13.7239667806165));
#34325=CARTESIAN_POINT('Ctrl Pts',(3.34517137976671,2.47128079370165,13.7769550693448));
#34326=CARTESIAN_POINT('Ctrl Pts',(2.27812755848019,3.2250295306576,13.829943358073));
#34327=CARTESIAN_POINT('Ctrl Pts',(1.21108373719365,3.97877826761357,13.8829316468013));
#34328=CARTESIAN_POINT('Ctrl Pts',(-0.267150659887593,4.15042538136161,
13.9359199355295));
#34329=CARTESIAN_POINT('Ctrl Pts',(-1.47851968414005,3.66123752164906,13.9889082242578));
#34330=CARTESIAN_POINT('Ctrl Pts',(-2.68988870839249,3.17204966193652,14.041896512986));
#34331=CARTESIAN_POINT('Ctrl Pts',(-3.63439235981614,2.02202682876341,14.0948848017143));
#34332=CARTESIAN_POINT('Ctrl Pts',(-3.87879331109071,0.738676584276535,
14.1478730904425));
#34333=CARTESIAN_POINT('Ctrl Pts',(-3.92484123568096,0.496878772227051,
14.1578566879318));
#34334=CARTESIAN_POINT('Ctrl Pts',(-3.9460363164428,0.250347989813759,14.1678402854211));
#34335=CARTESIAN_POINT('Ctrl Pts',(-3.94377660893062,0.00343048778150908,
14.1778238829104));
#34336=CARTESIAN_POINT('Origin',(0.,0.,0.));
#34337=CARTESIAN_POINT('',(-3.935515150562,-7.56757525427476E-5,15.3221761170896));
#34338=CARTESIAN_POINT('',(-3.93554762371472,0.000453016733568931,15.1778238829104));
#34339=CARTESIAN_POINT('',(-3.942,-4.82755768223887E-16,0.));
#34340=CARTESIAN_POINT('Ctrl Pts',(-3.935515150562,-7.56757525427476E-5,
15.3221761170896));
#34341=CARTESIAN_POINT('Ctrl Pts',(-3.93540179088204,0.662968867054025,
15.2955093068644));
#34342=CARTESIAN_POINT('Ctrl Pts',(-3.77682343808938,1.32606434282809,15.2688424966392));
#34343=CARTESIAN_POINT('Ctrl Pts',(-3.46008318945363,1.90220902322252,15.242175686414));
#34344=CARTESIAN_POINT('Ctrl Pts',(-2.83099318673311,3.04651215526165,15.1892117079193));
#34345=CARTESIAN_POINT('Ctrl Pts',(-1.57799465489921,3.84781647231203,15.1362477294247));
#34346=CARTESIAN_POINT('Ctrl Pts',(-0.275346694985541,3.93887789142153,
15.0832837509301));
#34347=CARTESIAN_POINT('Ctrl Pts',(1.02730126492813,4.02993931053103,15.0303197724355));
#34348=CARTESIAN_POINT('Ctrl Pts',(2.37959865292158,3.41075783169958,14.9773557939409));
#34349=CARTESIAN_POINT('Ctrl Pts',(3.16177691968707,2.36510920595707,14.9243918154462));
#34350=CARTESIAN_POINT('Ctrl Pts',(3.94395518645256,1.31946058021456,14.8714278369516));
#34351=CARTESIAN_POINT('Ctrl Pts',(4.15601433199016,-0.152655192438981,
14.818463858457));
#34352=CARTESIAN_POINT('Ctrl Pts',(3.70076597882895,-1.37655585281198,14.7654998799624));
#34353=CARTESIAN_POINT('Ctrl Pts',(3.24551762566774,-2.60045651318499,14.7125359014677));
#34354=CARTESIAN_POINT('Ctrl Pts',(2.1229617738077,-3.57614206127742,14.6595719229731));
#34355=CARTESIAN_POINT('Ctrl Pts',(0.847574616134508,-3.85644812178943,
14.6066079444785));
#34356=CARTESIAN_POINT('Ctrl Pts',(-0.427812541538684,-4.13675418230144,
14.5536439659839));
#34357=CARTESIAN_POINT('Ctrl Pts',(-1.85603100502504,-3.72168075523303,
14.5006799874892));
#34358=CARTESIAN_POINT('Ctrl Pts',(-2.78251699784433,-2.80145926307632,
14.4477160089946));
#34359=CARTESIAN_POINT('Ctrl Pts',(-3.5145299287451,-2.07439588945562,14.4058693783596));
#34360=CARTESIAN_POINT('Ctrl Pts',(-3.93333547115731,-1.0319929364451,14.3640227477246));
#34361=CARTESIAN_POINT('Ctrl Pts',(-3.9429197498326,0.0035503728418125,
14.3221761170896));
#34362=CARTESIAN_POINT('Ctrl Pts',(-3.94377660893062,0.00343048778150908,
14.1778238829104));
#34363=CARTESIAN_POINT('Ctrl Pts',(-3.93404284072175,-1.06017518620376,
14.2208285741494));
#34364=CARTESIAN_POINT('Ctrl Pts',(-3.48910890040614,-2.13095638625906,
14.2638332653883));
#34365=CARTESIAN_POINT('Ctrl Pts',(-2.72071532173612,-2.86153608825589,
14.3068379566273));
#34366=CARTESIAN_POINT('Ctrl Pts',(-1.77393812998146,-3.7617208605008,14.3598262453555));
#34367=CARTESIAN_POINT('Ctrl Pts',(-0.336085495346666,-4.14541274918995,
14.4128145340838));
#34368=CARTESIAN_POINT('Ctrl Pts',(0.933309470178012,-3.83661492453915,
14.465802822812));
#34369=CARTESIAN_POINT('Ctrl Pts',(2.20270443570267,-3.52781709988836,14.5187911115403));
#34370=CARTESIAN_POINT('Ctrl Pts',(3.30364173211722,-2.5265295618976,14.5717794002685));
#34371=CARTESIAN_POINT('Ctrl Pts',(3.73112899530853,-1.29203601601831,14.6247676889968));
#34372=CARTESIAN_POINT('Ctrl Pts',(4.15861625849985,-0.0575424701390118,
14.677755977725));
#34373=CARTESIAN_POINT('Ctrl Pts',(3.91265348846795,1.41015708362883,14.7307442664533));
#34374=CARTESIAN_POINT('Ctrl Pts',(3.10606211575817,2.43783895681654,14.7837325551815));
#34375=CARTESIAN_POINT('Ctrl Pts',(2.29947074304839,3.46552083000428,14.8367208439098));
#34376=CARTESIAN_POINT('Ctrl Pts',(0.932250767660721,4.05318502261185,14.889709132638));
#34377=CARTESIAN_POINT('Ctrl Pts',(-0.368463413303181,3.93127401224813,
14.9426974213663));
#34378=CARTESIAN_POINT('Ctrl Pts',(-1.66917759426705,3.80936300188441,14.9956857100945));
#34379=CARTESIAN_POINT('Ctrl Pts',(-2.90338598080718,2.9778767885494,15.0486739988228));
#34380=CARTESIAN_POINT('Ctrl Pts',(-3.50496567659063,1.81821237820066,15.101662287551));
#34381=CARTESIAN_POINT('Ctrl Pts',(-3.79318829122445,1.26260601250841,15.1270494860042));
#34382=CARTESIAN_POINT('Ctrl Pts',(-3.93619350756073,0.631667647738924,
15.1524366844573));
#34383=CARTESIAN_POINT('Ctrl Pts',(-3.93554762371472,0.000453016733568931,
15.1778238829104));
#34384=CARTESIAN_POINT('Origin',(0.,0.,0.));
#34385=CARTESIAN_POINT('',(-3.94319808732824,-0.00351593218956836,16.3221761170896));
#34386=CARTESIAN_POINT('',(-3.94210945089404,-0.00361990150021516,16.1778238829104));
#34387=CARTESIAN_POINT('',(-3.942,-4.82755768223887E-16,0.));
#34388=CARTESIAN_POINT('Ctrl Pts',(-3.94319808732824,-0.00351593218956836,
16.3221761170896));
#34389=CARTESIAN_POINT('Ctrl Pts',(-3.93355225073649,1.04098512265698,16.2799598444988));
#34390=CARTESIAN_POINT('Ctrl Pts',(-3.50650185007344,2.09245600266764,16.237743571908));
#34391=CARTESIAN_POINT('Ctrl Pts',(-2.76293020390983,2.82077853336478,16.1955272993172));
#34392=CARTESIAN_POINT('Ctrl Pts',(-1.83005502901329,3.73452236922869,16.1425633208226));
#34393=CARTESIAN_POINT('Ctrl Pts',(-0.398979196739877,4.13963456552086,
16.089599342328));
#34394=CARTESIAN_POINT('Ctrl Pts',(0.87442396179839,3.85044901031056,16.0366353638333));
#34395=CARTESIAN_POINT('Ctrl Pts',(2.14782712033666,3.56126345510026,15.9836713853387));
#34396=CARTESIAN_POINT('Ctrl Pts',(3.26355760513978,2.57778014838748,15.9307074068441));
#34397=CARTESIAN_POINT('Ctrl Pts',(3.7102673428296,1.35073723969577,15.8777434283495));
#34398=CARTESIAN_POINT('Ctrl Pts',(4.15697708051941,0.123694331004073,15.8247794498548));
#34399=CARTESIAN_POINT('Ctrl Pts',(3.93466607109594,-1.34690817966655,15.7718154713602));
#34400=CARTESIAN_POINT('Ctrl Pts',(3.14522120203587,-2.38708157301605,15.7188514928656));
#34401=CARTESIAN_POINT('Ctrl Pts',(2.3557763329758,-3.42725496636555,15.665887514371));
#34402=CARTESIAN_POINT('Ctrl Pts',(0.999197604279134,-4.03699924239392,
15.6129235358763));
#34403=CARTESIAN_POINT('Ctrl Pts',(-0.302784262564327,-3.93686379448313,
15.5599595573817));
#34404=CARTESIAN_POINT('Ctrl Pts',(-1.60476612940779,-3.83672834657235,
15.5069955788871));
#34405=CARTESIAN_POINT('Ctrl Pts',(-2.85215113439804,-3.02671317472241,
15.4540316003925));
#34406=CARTESIAN_POINT('Ctrl Pts',(-3.47325290008964,-1.8780546152835,15.4010676218978));
#34407=CARTESIAN_POINT('Ctrl Pts',(-3.78163641109193,-1.30773364846388,
15.3747704536284));
#34408=CARTESIAN_POINT('Ctrl Pts',(-3.9356269389069,-0.653929427477854,
15.348473285359));
#34409=CARTESIAN_POINT('Ctrl Pts',(-3.935515150562,-7.56757525427476E-5,
15.3221761170896));
#34410=CARTESIAN_POINT('Ctrl Pts',(-3.93554762371472,0.000453016733568931,
15.1778238829104));
#34411=CARTESIAN_POINT('Ctrl Pts',(-3.93484541553788,-0.685806715529583,
15.2054249731855));
#34412=CARTESIAN_POINT('Ctrl Pts',(-3.76434547901772,-1.37239299857592,
15.2330260634607));
#34413=CARTESIAN_POINT('Ctrl Pts',(-3.42606065206783,-1.96285227530577,
15.2606271537358));
#34414=CARTESIAN_POINT('Ctrl Pts',(-2.77662492673475,-3.09640991110095,
15.313615442464));
#34415=CARTESIAN_POINT('Ctrl Pts',(-1.5088024710418,-3.87568257532879,15.3666037311923));
#34416=CARTESIAN_POINT('Ctrl Pts',(-0.204134723598678,-3.94322325781103,
15.4195920199205));
#34417=CARTESIAN_POINT('Ctrl Pts',(1.10053302384446,-4.01076394029327,15.4725803086488));
#34418=CARTESIAN_POINT('Ctrl Pts',(2.44204606303776,-3.36657264102987,15.525568597377));
#34419=CARTESIAN_POINT('Ctrl Pts',(3.2050615916644,-2.30613547736428,15.5785568861053));
#34420=CARTESIAN_POINT('Ctrl Pts',(3.96807712029102,-1.24569831369873,15.6315451748335));
#34421=CARTESIAN_POINT('Ctrl Pts',(4.15259513835105,0.230984714368973,15.6845334635618));
#34422=CARTESIAN_POINT('Ctrl Pts',(3.67397850032763,1.44656926050946,15.73752175229));
#34423=CARTESIAN_POINT('Ctrl Pts',(3.1953618623042,2.66215380664994,15.7905100410183));
#34424=CARTESIAN_POINT('Ctrl Pts',(2.05361056819728,3.6166398708632,15.8434983297465));
#34425=CARTESIAN_POINT('Ctrl Pts',(0.772438082086977,3.87221126175501,15.8964866184748));
#34426=CARTESIAN_POINT('Ctrl Pts',(-0.508734404023323,4.12778265264681,
15.949474907203));
#34427=CARTESIAN_POINT('Ctrl Pts',(-1.92932808213704,3.68443937021718,16.0024631959313));
#34428=CARTESIAN_POINT('Ctrl Pts',(-2.83772640488938,2.74553992819521,16.0554514846595));
#34429=CARTESIAN_POINT('Ctrl Pts',(-3.53701854402849,2.02276778870165,16.0962422840765));
#34430=CARTESIAN_POINT('Ctrl Pts',(-3.93278162022236,1.00632704174549,16.1370330834934));
#34431=CARTESIAN_POINT('Ctrl Pts',(-3.94210945089404,-0.00361990150021516,
16.1778238829104));
#34432=CARTESIAN_POINT('Origin',(0.,0.,0.));
#34433=CARTESIAN_POINT('',(-3.94714763575412,0.00206509481356407,17.3221761170896));
#34434=CARTESIAN_POINT('',(-3.94786894067556,0.00143683566665543,17.1778238829104));
#34435=CARTESIAN_POINT('',(-3.942,-4.82755768223887E-16,0.));
#34436=CARTESIAN_POINT('Ctrl Pts',(-3.94714763575412,0.00206509481356407,
17.3221761170896));
#34437=CARTESIAN_POINT('Ctrl Pts',(-3.94790115726501,0.120559580499713,
17.3173743606278));
#34438=CARTESIAN_POINT('Ctrl Pts',(-3.94302847934562,0.238991236972465,
17.3125726041661));
#34439=CARTESIAN_POINT('Ctrl Pts',(-3.93232775304421,0.356893945881719,
17.3077708477043));
#34440=CARTESIAN_POINT('Ctrl Pts',(-3.81429739431669,1.6573756735258,17.2548068692097));
#34441=CARTESIAN_POINT('Ctrl Pts',(-2.98720523271932,2.89350369502107,17.201842890715));
#34442=CARTESIAN_POINT('Ctrl Pts',(-1.83011412357382,3.49875079716524,17.1488789122204));
#34443=CARTESIAN_POINT('Ctrl Pts',(-0.67302301442832,4.10399789930941,17.0959149337258));
#34444=CARTESIAN_POINT('Ctrl Pts',(0.814067042265299,4.07836408210249,17.0429509552312));
#34445=CARTESIAN_POINT('Ctrl Pts',(1.94961095493928,3.43359752597032,16.9899869767366));
#34446=CARTESIAN_POINT('Ctrl Pts',(3.08515486761327,2.78883096983815,16.9370229982419));
#34447=CARTESIAN_POINT('Ctrl Pts',(3.86915263626762,1.52493167478073,16.8840590197473));
#34448=CARTESIAN_POINT('Ctrl Pts',(3.94229190545934,0.221154647517415,16.8310950412527));
#34449=CARTESIAN_POINT('Ctrl Pts',(4.01543117465106,-1.08262237974594,16.7781310627581));
#34450=CARTESIAN_POINT('Ctrl Pts',(3.37771194438013,-2.42627713921516,16.7251670842634));
#34451=CARTESIAN_POINT('Ctrl Pts',(2.32140596324251,-3.19400206634104,16.6722031057688));
#34452=CARTESIAN_POINT('Ctrl Pts',(1.26509998210492,-3.96172699346691,16.6192391272742));
#34453=CARTESIAN_POINT('Ctrl Pts',(-0.209792749899407,-4.15352208824943,
16.5662751487796));
#34454=CARTESIAN_POINT('Ctrl Pts',(-1.42731727122521,-3.68148614736372,
16.5133111702849));
#34455=CARTESIAN_POINT('Ctrl Pts',(-2.64484179255099,-3.20945020647802,
16.4603471917903));
#34456=CARTESIAN_POINT('Ctrl Pts',(-3.60499810319833,-2.07358322992414,
16.4073832132957));
#34457=CARTESIAN_POINT('Ctrl Pts',(-3.86773899976216,-0.794462003929412,
16.3544192348011));
#34458=CARTESIAN_POINT('Ctrl Pts',(-3.92105564940663,-0.534896556939351,
16.3436715288973));
#34459=CARTESIAN_POINT('Ctrl Pts',(-3.94565379003534,-0.269432117224103,
16.3329238229934));
#34460=CARTESIAN_POINT('Ctrl Pts',(-3.94319808732824,-0.00351593218956836,
16.3221761170896));
#34461=CARTESIAN_POINT('Ctrl Pts',(-3.94210945089404,-0.00361990150021516,
16.1778238829104));
#34462=CARTESIAN_POINT('Ctrl Pts',(-3.94489871015204,-0.305619794154464,
16.1900213722217));
#34463=CARTESIAN_POINT('Ctrl Pts',(-3.91313437834161,-0.607039035223508,
16.202218861533));
#34464=CARTESIAN_POINT('Ctrl Pts',(-3.84459973154587,-0.899851960334574,
16.2144163508443));
#34465=CARTESIAN_POINT('Ctrl Pts',(-3.54687176805904,-2.17188880522799,
16.2674046395725));
#34466=CARTESIAN_POINT('Ctrl Pts',(-2.55521287369446,-3.2815068934005,16.3203929283008));
#34467=CARTESIAN_POINT('Ctrl Pts',(-1.32449016131116,-3.71973204127804,
16.373381217029));
#34468=CARTESIAN_POINT('Ctrl Pts',(-0.0937674489278181,-4.15795718915558,
16.4263695057573));
#34469=CARTESIAN_POINT('Ctrl Pts',(1.37601908147424,-3.9247893967381,16.4793577944855));
#34470=CARTESIAN_POINT('Ctrl Pts',(2.4106884596013,-3.12718112636055,16.5323460832138));
#34471=CARTESIAN_POINT('Ctrl Pts',(3.44535783772833,-2.32957285598302,16.585334371942));
#34472=CARTESIAN_POINT('Ctrl Pts',(4.04491006358037,-0.967524107645474,
16.6383226606703));
#34473=CARTESIAN_POINT('Ctrl Pts',(3.93433465569921,0.334202727823592,16.6913109493985));
#34474=CARTESIAN_POINT('Ctrl Pts',(3.82375924781804,1.63592956329268,16.7442992381268));
#34475=CARTESIAN_POINT('Ctrl Pts',(3.00305620620361,2.87733448589332,16.797287526855));
#34476=CARTESIAN_POINT('Ctrl Pts',(1.84867637012666,3.48899359770921,16.8502758155833));
#34477=CARTESIAN_POINT('Ctrl Pts',(0.694296534049695,4.10065270952511,16.9032641043115));
#34478=CARTESIAN_POINT('Ctrl Pts',(-0.793760096489806,4.08256601055629,
16.9562523930398));
#34479=CARTESIAN_POINT('Ctrl Pts',(-1.93293218195181,3.44302974519471,17.009240681768));
#34480=CARTESIAN_POINT('Ctrl Pts',(-3.0721042674138,2.80349347983313,17.0622289704962));
#34481=CARTESIAN_POINT('Ctrl Pts',(-3.86239180779829,1.54250764807881,17.1152172592245));
#34482=CARTESIAN_POINT('Ctrl Pts',(-3.94129534500935,0.238477776172487,
17.1682055479527));
#34483=CARTESIAN_POINT('Ctrl Pts',(-3.94606948578935,0.159576089253736,
17.1714116596053));
#34484=CARTESIAN_POINT('Ctrl Pts',(-3.9482392631182,0.0805168189138495,
17.1746177712579));
#34485=CARTESIAN_POINT('Ctrl Pts',(-3.94786894067556,0.00143683566665543,
17.1778238829104));
#34486=CARTESIAN_POINT('Origin',(0.,0.,0.));
#34487=CARTESIAN_POINT('',(-3.93691309430117,0.00231896033839218,18.3221761170896));
#34488=CARTESIAN_POINT('',(-3.93777174659584,0.00283174072808758,18.1778238829104));
#34489=CARTESIAN_POINT('',(-3.942,-4.82755768223887E-16,0.));
#34490=CARTESIAN_POINT('Ctrl Pts',(-3.93691309430117,0.00231896033839218,
18.3221761170896));
#34491=CARTESIAN_POINT('Ctrl Pts',(-3.93961914157867,0.507883428428715,
18.3018248982623));
#34492=CARTESIAN_POINT('Ctrl Pts',(-3.84930447301574,1.01251781158405,18.2814736794349));
#34493=CARTESIAN_POINT('Ctrl Pts',(-3.66151008646525,1.47780876052409,18.2611224606075));
#34494=CARTESIAN_POINT('Ctrl Pts',(-3.17277582759625,2.68872688893964,18.2081584821129));
#34495=CARTESIAN_POINT('Ctrl Pts',(-2.02381253743022,3.63317238083008,18.1551945036183));
#34496=CARTESIAN_POINT('Ctrl Pts',(-0.741199145924524,3.87829842483136,
18.1022305251237));
#34497=CARTESIAN_POINT('Ctrl Pts',(0.541414245581171,4.12342446883263,18.049266546629));
#34498=CARTESIAN_POINT('Ctrl Pts',(1.95767773842654,3.66923106494473,17.9963025681344));
#34499=CARTESIAN_POINT('Ctrl Pts',(2.8585066133837,2.72387862930978,17.9433385896398));
#34500=CARTESIAN_POINT('Ctrl Pts',(3.75933548834084,1.77852619367486,17.8903746111452));
#34501=CARTESIAN_POINT('Ctrl Pts',(4.14472974540982,0.342014726292911,17.8374106326505));
#34502=CARTESIAN_POINT('Ctrl Pts',(3.83806015958749,-0.927291247319836,
17.7844466541559));
#34503=CARTESIAN_POINT('Ctrl Pts',(3.53139057376515,-2.19659722093258,17.7314826756613));
#34504=CARTESIAN_POINT('Ctrl Pts',(2.53265714505146,-3.29869770077617,17.6785186971667));
#34505=CARTESIAN_POINT('Ctrl Pts',(1.29958727405717,-3.72849135215269,17.625554718672));
#34506=CARTESIAN_POINT('Ctrl Pts',(0.0665174030628353,-4.15828500352923,
17.5725907401774));
#34507=CARTESIAN_POINT('Ctrl Pts',(-1.40088891021208,-3.91577182643871,
17.5196267616828));
#34508=CARTESIAN_POINT('Ctrl Pts',(-2.43010778892075,-3.11209752099697,
17.4666627831882));
#34509=CARTESIAN_POINT('Ctrl Pts',(-3.36601686459191,-2.38128496799525,
17.4185005611553));
#34510=CARTESIAN_POINT('Ctrl Pts',(-3.93958972010326,-1.18644951952042,
17.3703383391225));
#34511=CARTESIAN_POINT('Ctrl Pts',(-3.94714763575412,0.00206509481356407,
17.3221761170896));
#34512=CARTESIAN_POINT('Ctrl Pts',(-3.94786894067556,0.00143683566665543,
17.1778238829104));
#34513=CARTESIAN_POINT('Ctrl Pts',(-3.94211884229706,-1.22645980543112,
17.2276060599861));
#34514=CARTESIAN_POINT('Ctrl Pts',(-3.32396017207549,-2.45935025115224,
17.2773882370618));
#34515=CARTESIAN_POINT('Ctrl Pts',(-2.33396838579359,-3.18485042355784,
17.3271704141375));
#34516=CARTESIAN_POINT('Ctrl Pts',(-1.28021835532917,-3.95707483932351,
17.3801587028657));
#34517=CARTESIAN_POINT('Ctrl Pts',(0.194801239637294,-4.15444975879655,
17.433146991594));
#34518=CARTESIAN_POINT('Ctrl Pts',(1.41450905809659,-3.68644066422928,17.4861352803222));
#34519=CARTESIAN_POINT('Ctrl Pts',(2.63421687655591,-3.21843156966201,17.5391235690505));
#34520=CARTESIAN_POINT('Ctrl Pts',(3.59861291850804,-2.08503846105438,17.5921118577787));
#34521=CARTESIAN_POINT('Ctrl Pts',(3.86533535394433,-0.806140960297021,
17.645100146507));
#34522=CARTESIAN_POINT('Ctrl Pts',(4.13205778938061,0.472756540460342,17.6980884352352));
#34523=CARTESIAN_POINT('Ctrl Pts',(3.70110661830104,1.89715843336744,17.7510767239635));
#34524=CARTESIAN_POINT('Ctrl Pts',(2.77015617820835,2.81370136913189,17.8040650126917));
#34525=CARTESIAN_POINT('Ctrl Pts',(1.83920573811566,3.73024430489631,17.85705330142));
#34526=CARTESIAN_POINT('Ctrl Pts',(0.408256029009864,4.13892828351809,17.9100415901482));
#34527=CARTESIAN_POINT('Ctrl Pts',(-0.866326161571161,3.85229277549071,
17.9630298788765));
#34528=CARTESIAN_POINT('Ctrl Pts',(-2.14090835215219,3.56565726746332,18.0160181676047));
#34529=CARTESIAN_POINT('Ctrl Pts',(-3.25912302420844,2.58370227278676,18.069006456333));
#34530=CARTESIAN_POINT('Ctrl Pts',(-3.70805280027739,1.35684379228987,18.1219947450612));
#34531=CARTESIAN_POINT('Ctrl Pts',(-3.86571884909867,0.925965870186712,
18.1406044576776));
#34532=CARTESIAN_POINT('Ctrl Pts',(-3.94083233343714,0.464880467044514,
18.159214170294));
#34533=CARTESIAN_POINT('Ctrl Pts',(-3.93777174659584,0.00283174072808758,
18.1778238829104));
#34534=CARTESIAN_POINT('Origin',(0.,0.,0.));
#34535=CARTESIAN_POINT('',(-3.93868067607543,-0.00317875339515938,19.3221761170896));
#34536=CARTESIAN_POINT('',(-3.93757571821786,-0.00273443803236162,19.1778238829104));
#34537=CARTESIAN_POINT('',(-3.942,-4.82755768223887E-16,0.));
#34538=CARTESIAN_POINT('Ctrl Pts',(-3.93868067607543,-0.00317875339515938,
19.3221761170896));
#34539=CARTESIAN_POINT('Ctrl Pts',(-3.93194593082782,0.887659399123926,
19.2862754358966));
#34540=CARTESIAN_POINT('Ctrl Pts',(-3.63268362464169,1.78259416274328,19.2503747547037));
#34541=CARTESIAN_POINT('Ctrl Pts',(-3.07838529125365,2.47267443157326,19.2144740735107));
#34542=CARTESIAN_POINT('Ctrl Pts',(-2.26063353742526,3.4907441534662,19.1615100950161));
#34543=CARTESIAN_POINT('Ctrl Pts',(-0.887799511314515,4.06295099197559,
19.1085461165215));
#34544=CARTESIAN_POINT('Ctrl Pts',(0.410936134697139,3.92704804390779,19.0555821380269));
#34545=CARTESIAN_POINT('Ctrl Pts',(1.70967178070872,3.79114509584001,19.0026181595322));
#34546=CARTESIAN_POINT('Ctrl Pts',(2.93430904662124,2.94713236119515,18.9496541810376));
#34547=CARTESIAN_POINT('Ctrl Pts',(3.52358702306116,1.78182752725689,18.896690202543));
#34548=CARTESIAN_POINT('Ctrl Pts',(4.11286499950109,0.616522693318613,18.8437262240484));
#34549=CARTESIAN_POINT('Ctrl Pts',(4.06678368646841,-0.870074239913033,
18.7907622455538));
#34550=CARTESIAN_POINT('Ctrl Pts',(3.40646251285886,-1.99664418323714,18.7377982670591));
#34551=CARTESIAN_POINT('Ctrl Pts',(2.74614133924929,-3.1232141265613,18.6848342885645));
#34552=CARTESIAN_POINT('Ctrl Pts',(1.47158030506274,-3.88975707997784,18.6318703100699));
#34553=CARTESIAN_POINT('Ctrl Pts',(0.166920776077049,-3.94496036741581,
18.5789063315753));
#34554=CARTESIAN_POINT('Ctrl Pts',(-1.1377387529086,-4.00016365485379,18.5259423530806));
#34555=CARTESIAN_POINT('Ctrl Pts',(-2.47249677669342,-3.34402727631325,
18.472978374586));
#34556=CARTESIAN_POINT('Ctrl Pts',(-3.22562317479983,-2.27726370457266,
18.4200143960914));
#34557=CARTESIAN_POINT('Ctrl Pts',(-3.689363454866,-1.62040021025458,18.3874016364241));
#34558=CARTESIAN_POINT('Ctrl Pts',(-3.93257666264772,-0.807846398012042,
18.3547888767569));
#34559=CARTESIAN_POINT('Ctrl Pts',(-3.93691309430117,0.00231896033839218,
18.3221761170896));
#34560=CARTESIAN_POINT('Ctrl Pts',(-3.93777174659584,0.00283174072808758,
18.1778238829104));
#34561=CARTESIAN_POINT('Ctrl Pts',(-3.93211778407426,-0.850732074710112,
18.2122024590223));
#34562=CARTESIAN_POINT('Ctrl Pts',(-3.65968019788323,-1.70758341046428,
18.2465810351341));
#34563=CARTESIAN_POINT('Ctrl Pts',(-3.14806281812505,-2.38335501750349,
18.280959611246));
#34564=CARTESIAN_POINT('Ctrl Pts',(-2.3594981798221,-3.42493338048278,18.3339478999742));
#34565=CARTESIAN_POINT('Ctrl Pts',(-1.00272402313454,-4.03632814012413,
18.3869361887025));
#34566=CARTESIAN_POINT('Ctrl Pts',(0.299916680013111,-3.93709672618929,
18.4399244774307));
#34567=CARTESIAN_POINT('Ctrl Pts',(1.60255738316074,-3.83786531225445,18.492912766159));
#34568=CARTESIAN_POINT('Ctrl Pts',(2.85106463276846,-3.02800772474346,18.5459010548872));
#34569=CARTESIAN_POINT('Ctrl Pts',(3.47275674238136,-1.8790000677396,18.5988893436155));
#34570=CARTESIAN_POINT('Ctrl Pts',(4.09444885199426,-0.729992410735758,
18.6518776323437));
#34571=CARTESIAN_POINT('Ctrl Pts',(4.08932582161236,0.758165315760947,18.704865921072));
#34572=CARTESIAN_POINT('Ctrl Pts',(3.45973755002874,1.90286540019034,18.7578542098002));
#34573=CARTESIAN_POINT('Ctrl Pts',(2.83014927844509,3.04756548461977,18.8108424985285));
#34574=CARTESIAN_POINT('Ctrl Pts',(1.57609576565968,3.84880792698187,18.8638307872567));
#34575=CARTESIAN_POINT('Ctrl Pts',(0.272802730892003,3.93906833100647,18.916819075985));
#34576=CARTESIAN_POINT('Ctrl Pts',(-1.03049030387567,4.02932873503108,18.9698073647132));
#34577=CARTESIAN_POINT('Ctrl Pts',(-2.3830228606256,3.4086071007182,19.0227956534415));
#34578=CARTESIAN_POINT('Ctrl Pts',(-3.16439756014476,2.36162417155469,19.0757839421697));
#34579=CARTESIAN_POINT('Ctrl Pts',(-3.66596391218726,1.68956324002662,19.10979725575));
#34580=CARTESIAN_POINT('Ctrl Pts',(-3.93219107470607,0.841866122485371,
19.1438105693302));
#34581=CARTESIAN_POINT('Ctrl Pts',(-3.93757571821786,-0.00273443803236162,
19.1778238829104));
#34582=CARTESIAN_POINT('Origin',(0.,0.,0.));
#34583=CARTESIAN_POINT('',(-3.94834041879863,-0.000694519400761262,20.3221761170896));
#34584=CARTESIAN_POINT('',(-3.94772619292891,-0.00158826883248112,20.1778238829104));
#34585=CARTESIAN_POINT('',(-3.942,-4.82755768223887E-16,0.));
#34586=CARTESIAN_POINT('Ctrl Pts',(-3.94834041879863,-0.000694519400761262,
20.3221761170896));
#34587=CARTESIAN_POINT('Ctrl Pts',(-3.94525718695861,1.26793825937276,20.270725973531));
#34588=CARTESIAN_POINT('Ctrl Pts',(-3.27892645249503,2.53935361509062,20.2192758299725));
#34589=CARTESIAN_POINT('Ctrl Pts',(-2.23269077785256,3.25663426508529,20.167825686414));
#34590=CARTESIAN_POINT('Ctrl Pts',(-1.15567135789659,3.9950197056954,20.1148617079193));
#34591=CARTESIAN_POINT('Ctrl Pts',(0.323938040913112,4.14618172311401,20.0618977294247));
#34592=CARTESIAN_POINT('Ctrl Pts',(1.52802077187684,3.64084157388599,20.0089337509301));
#34593=CARTESIAN_POINT('Ctrl Pts',(2.73210350284056,3.13550142465798,19.9559697724355));
#34594=CARTESIAN_POINT('Ctrl Pts',(3.66065956595831,1.97365910878334,19.9030057939409));
#34595=CARTESIAN_POINT('Ctrl Pts',(3.88812440006945,0.687796115025536,19.8500418154462));
#34596=CARTESIAN_POINT('Ctrl Pts',(4.11558923418059,-0.598066878732264,
19.7970778369516));
#34597=CARTESIAN_POINT('Ctrl Pts',(3.64196283928513,-2.00795055037323,19.744113858457));
#34598=CARTESIAN_POINT('Ctrl Pts',(2.68431192455269,-2.89569410291512,19.6911498799624));
#34599=CARTESIAN_POINT('Ctrl Pts',(1.72666100982023,-3.78343765545704,19.6381859014677));
#34600=CARTESIAN_POINT('Ctrl Pts',(0.284985575250775,-4.14904108889985,
19.5852219229731));
#34601=CARTESIAN_POINT('Ctrl Pts',(-0.979983166843207,-3.82494546870956,
19.5322579444785));
#34602=CARTESIAN_POINT('Ctrl Pts',(-2.24495190893719,-3.50084984851927,
19.4792939659839));
#34603=CARTESIAN_POINT('Ctrl Pts',(-3.3332139585557,-2.48705517469588,19.4263299874892));
#34604=CARTESIAN_POINT('Ctrl Pts',(-3.74601024259189,-1.24819153514592,
19.3733660089946));
#34605=CARTESIAN_POINT('Ctrl Pts',(-3.87899998240626,-0.849069354397836,
19.3563027116929));
#34606=CARTESIAN_POINT('Ctrl Pts',(-3.94188164487581,-0.426586770708422,
19.3392394143913));
#34607=CARTESIAN_POINT('Ctrl Pts',(-3.93868067607543,-0.00317875339515938,
19.3221761170896));
#34608=CARTESIAN_POINT('Ctrl Pts',(-3.93757571821786,-0.00273443803236162,
19.1778238829104));
#34609=CARTESIAN_POINT('Ctrl Pts',(-3.9405796442122,-0.473910955663478,
19.1967988580584));
#34610=CARTESIAN_POINT('Ctrl Pts',(-3.86240471339523,-0.944123769370189,
19.2157738332064));
#34611=CARTESIAN_POINT('Ctrl Pts',(-3.69862306761181,-1.38234150992047,
19.2347488083545));
#34612=CARTESIAN_POINT('Ctrl Pts',(-3.24125703327134,-2.60608003821792,
19.2877370970827));
#34613=CARTESIAN_POINT('Ctrl Pts',(-2.11630812230202,-3.58031287079873,
19.340725385811));
#34614=CARTESIAN_POINT('Ctrl Pts',(-0.839782661227222,-3.85816610946462,
19.3937136745392));
#34615=CARTESIAN_POINT('Ctrl Pts',(0.436742799847613,-4.13601934813052,
19.4467019632675));
#34616=CARTESIAN_POINT('Ctrl Pts',(1.86484481102796,-3.71749299288145,19.4996902519957));
#34617=CARTESIAN_POINT('Ctrl Pts',(2.78946280422149,-2.79456220367197,19.552678540724));
#34618=CARTESIAN_POINT('Ctrl Pts',(3.714080797415,-1.8716314144625,19.6056668294522));
#34619=CARTESIAN_POINT('Ctrl Pts',(4.13521477262173,-0.444296191292658,
19.6586551181805));
#34620=CARTESIAN_POINT('Ctrl Pts',(3.85969347255442,0.832734618130101,19.7116434069087));
#34621=CARTESIAN_POINT('Ctrl Pts',(3.5841721724871,2.10976542755288,19.764631695637));
#34622=CARTESIAN_POINT('Ctrl Pts',(2.6119955971457,3.23649182322855,19.8176199843652));
#34623=CARTESIAN_POINT('Ctrl Pts',(1.38909445367046,3.69609215863147,19.8706082730935));
#34624=CARTESIAN_POINT('Ctrl Pts',(0.166193310195227,4.1556924940344,19.9235965618217));
#34625=CARTESIAN_POINT('Ctrl Pts',(-1.30743240141386,3.94816676916459,19.97658485055));
#34626=CARTESIAN_POINT('Ctrl Pts',(-2.35584070483748,3.16870560636289,20.0295731392782));
#34627=CARTESIAN_POINT('Ctrl Pts',(-3.33358701031412,2.44177958936821,20.0789900538223));
#34628=CARTESIAN_POINT('Ctrl Pts',(-3.94150300763008,1.21741613169822,20.1284069683663));
#34629=CARTESIAN_POINT('Ctrl Pts',(-3.94772619292891,-0.00158826883248112,
20.1778238829104));
#34630=CARTESIAN_POINT('Origin',(0.,0.,0.));
#34631=CARTESIAN_POINT('',(-3.94074044801927,0.00358039056613663,21.3221761170896));
#34632=CARTESIAN_POINT('',(-3.94238528018782,0.00360576479228953,21.1778238829104));
#34633=CARTESIAN_POINT('',(-3.942,-4.82755768223887E-16,0.));
#34634=CARTESIAN_POINT('Ctrl Pts',(-3.94074044801927,0.00358039056613663,
21.3221761170896));
#34635=CARTESIAN_POINT('Ctrl Pts',(-3.94382356658785,0.35139917714199,21.3081404896601));
#34636=CARTESIAN_POINT('Ctrl Pts',(-3.90159553870986,0.69848167363253,21.2941048622306));
#34637=CARTESIAN_POINT('Ctrl Pts',(-3.81110742902655,1.03248974691214,21.2800692348011));
#34638=CARTESIAN_POINT('Ctrl Pts',(-3.46964707612424,2.29288202357064,21.2271052563065));
#34639=CARTESIAN_POINT('Ctrl Pts',(-2.44098286072968,3.36709985140295,21.1741412778118));
#34640=CARTESIAN_POINT('Ctrl Pts',(-1.19655973690358,3.76282070551412,21.1211772993172));
#34641=CARTESIAN_POINT('Ctrl Pts',(0.0478633869225303,4.15854155962529,
21.0682133208226));
#34642=CARTESIAN_POINT('Ctrl Pts',(1.50804541918014,3.87576544001532,21.0152493423279));
#34643=CARTESIAN_POINT('Ctrl Pts',(2.51477344786687,3.04409088599763,20.9622853638333));
#34644=CARTESIAN_POINT('Ctrl Pts',(3.52150147655357,2.21241633197998,20.9093213853387));
#34645=CARTESIAN_POINT('Ctrl Pts',(4.07477550166942,0.831843343554564,20.8563574068441));
#34646=CARTESIAN_POINT('Ctrl Pts',(3.92102566715379,-0.464900607518139,
20.8033934283495));
#34647=CARTESIAN_POINT('Ctrl Pts',(3.76727583263815,-1.76164455859092,20.7504294498548));
#34648=CARTESIAN_POINT('Ctrl Pts',(2.90650213849103,-2.97455947231102,20.6974654713602));
#34649=CARTESIAN_POINT('Ctrl Pts',(1.73320395728241,-3.54775688148229,20.6445014928656));
#34650=CARTESIAN_POINT('Ctrl Pts',(0.559905776073817,-4.12095429065355,
20.5915375143709));
#34651=CARTESIAN_POINT('Ctrl Pts',(-0.925916892196226,-4.05443419527599,
20.5385735358763));
#34652=CARTESIAN_POINT('Ctrl Pts',(-2.04329981292238,-3.37868328145881,
20.4856095573817));
#34653=CARTESIAN_POINT('Ctrl Pts',(-3.16068273364853,-2.70293236764162,
20.4326455788871));
#34654=CARTESIAN_POINT('Ctrl Pts',(-3.90962590683076,-1.41795063538484,
20.3796816003925));
#34655=CARTESIAN_POINT('Ctrl Pts',(-3.94688277287076,-0.11265533735563,
20.3267176218978));
#34656=CARTESIAN_POINT('Ctrl Pts',(-3.94794766163145,-0.0753469311478099,
20.3252037869617));
#34657=CARTESIAN_POINT('Ctrl Pts',(-3.94843113776951,-0.0380219297583325,
20.3236899520257));
#34658=CARTESIAN_POINT('Ctrl Pts',(-3.94834041879863,-0.000694519400761262,
20.3221761170896));
#34659=CARTESIAN_POINT('Ctrl Pts',(-3.94772619292891,-0.00158826883248112,
20.1778238829104));
#34660=CARTESIAN_POINT('Ctrl Pts',(-3.94817594426456,-0.0896860565358013,
20.1813952570946));
#34661=CARTESIAN_POINT('Ctrl Pts',(-3.9454830581488,-0.177755853920253,
20.1849666312788));
#34662=CARTESIAN_POINT('Ctrl Pts',(-3.93956001409796,-0.265607871813588,
20.188538005463));
#34663=CARTESIAN_POINT('Ctrl Pts',(-3.85168012469672,-1.56906358645505,
20.2415262941912));
#34664=CARTESIAN_POINT('Ctrl Pts',(-3.05272945065598,-2.82457841500438,
20.2945145829195));
#34665=CARTESIAN_POINT('Ctrl Pts',(-1.90918116982076,-3.45625634279478,
20.3475028716477));
#34666=CARTESIAN_POINT('Ctrl Pts',(-0.765632888985623,-4.08793427058512,
20.4004911603759));
#34667=CARTESIAN_POINT('Ctrl Pts',(0.722512998643886,-4.09577529761664,
20.4534794491042));
#34668=CARTESIAN_POINT('Ctrl Pts',(1.87265421179595,-3.47618279865318,20.5064677378324));
#34669=CARTESIAN_POINT('Ctrl Pts',(3.0227954249481,-2.85659029968967,20.5594560265607));
#34670=CARTESIAN_POINT('Ctrl Pts',(3.8349319636227,-1.60956427473106,20.6124443152889));
#34671=CARTESIAN_POINT('Ctrl Pts',(3.9365423847422,-0.307106982824769,20.6654326040172));
#34672=CARTESIAN_POINT('Ctrl Pts',(4.03815280586171,0.995350309081448,20.7184208927454));
#34673=CARTESIAN_POINT('Ctrl Pts',(3.4292371094262,2.35323886793535,20.7714091814737));
#34674=CARTESIAN_POINT('Ctrl Pts',(2.38910073600262,3.14370455348999,20.8243974702019));
#34675=CARTESIAN_POINT('Ctrl Pts',(1.348964362579,3.93417023904466,20.8773857589302));
#34676=CARTESIAN_POINT('Ctrl Pts',(-0.12239268783275,4.15721305130006,20.9303740476584));
#34677=CARTESIAN_POINT('Ctrl Pts',(-1.35006905738725,3.71052478612394,20.9833623363867));
#34678=CARTESIAN_POINT('Ctrl Pts',(-2.57774542694174,3.26383652094782,21.0363506251149));
#34679=CARTESIAN_POINT('Ctrl Pts',(-3.56174111563901,2.14741717834018,21.0893389138432));
#34680=CARTESIAN_POINT('Ctrl Pts',(-3.85070407192177,0.873360631535526,
21.1423272025715));
#34681=CARTESIAN_POINT('Ctrl Pts',(-3.91522918325707,0.588865201437585,
21.1541594293511));
#34682=CARTESIAN_POINT('Ctrl Pts',(-3.94509829421553,0.296509601950098,
21.1659916561308));
#34683=CARTESIAN_POINT('Ctrl Pts',(-3.94238528018782,0.00360576479228953,
21.1778238829104));
#34684=CARTESIAN_POINT('Origin',(0.,0.,0.));
#34685=CARTESIAN_POINT('',(-3.93587951376728,-0.00124481178566893,22.3221761170896));
#34686=CARTESIAN_POINT('',(-3.93552176014147,-0.00030393483444853,22.1778238829104));
#34687=CARTESIAN_POINT('',(-3.942,-4.82755768223887E-16,0.));
#34688=CARTESIAN_POINT('Ctrl Pts',(-3.93587951376728,-0.00124481178566893,
22.3221761170896));
#34689=CARTESIAN_POINT('Ctrl Pts',(-3.9337992464037,0.734189273701127,22.2925910272945));
#34690=CARTESIAN_POINT('Ctrl Pts',(-3.73627980596971,1.47066093628887,22.2630059374994));
#34691=CARTESIAN_POINT('Ctrl Pts',(-3.35026562609245,2.08956860583238,22.2334208477043));
#34692=CARTESIAN_POINT('Ctrl Pts',(-2.65921324588212,3.19755282108702,22.1804568692097));
#34693=CARTESIAN_POINT('Ctrl Pts',(-1.36405277538343,3.92875538432108,22.1274928907151));
#34694=CARTESIAN_POINT('Ctrl Pts',(-0.0583683106578484,3.94805897547177,
22.0745289122204));
#34695=CARTESIAN_POINT('Ctrl Pts',(1.2473161540677,3.96736256662245,22.0215649337258));
#34696=CARTESIAN_POINT('Ctrl Pts',(2.56352461302015,3.27476718568979,21.9686009552312));
#34697=CARTESIAN_POINT('Ctrl Pts',(3.28702932421304,2.18769549882087,21.9156369767366));
#34698=CARTESIAN_POINT('Ctrl Pts',(4.01053403540591,1.10062381195199,21.8626729982419));
#34699=CARTESIAN_POINT('Ctrl Pts',(4.14133499883926,-0.380924180853135,
21.8097090197473));
#34700=CARTESIAN_POINT('Ctrl Pts',(3.6194845960222,-1.57794374981529,21.7567450412527));
#34701=CARTESIAN_POINT('Ctrl Pts',(3.09763419320511,-2.77496331877751,21.7037810627581));
#34702=CARTESIAN_POINT('Ctrl Pts',(1.92313242413752,-3.68745446389673,21.6508170842634));
#34703=CARTESIAN_POINT('Ctrl Pts',(0.634262969967227,-3.89721509840628,
21.5978531057688));
#34704=CARTESIAN_POINT('Ctrl Pts',(-0.654606484203027,-4.10697573291583,
21.5448891272742));
#34705=CARTESIAN_POINT('Ctrl Pts',(-2.05784362347597,-3.61400585681575,
21.4919251487796));
#34706=CARTESIAN_POINT('Ctrl Pts',(-2.93233394790743,-2.64423755602338,
21.4389611702849));
#34707=CARTESIAN_POINT('Ctrl Pts',(-3.57508147783416,-1.93146102491564,
21.4000328192198));
#34708=CARTESIAN_POINT('Ctrl Pts',(-3.93218930040467,-0.961108355901809,
21.3611044681547));
#34709=CARTESIAN_POINT('Ctrl Pts',(-3.94074044801927,0.00358039056613663,
21.3221761170896));
#34710=CARTESIAN_POINT('Ctrl Pts',(-3.94238528018782,0.00360576479228953,
21.1778238829104));
#34711=CARTESIAN_POINT('Ctrl Pts',(-3.93294859718036,-1.0152023337623,21.218979944859));
#34712=CARTESIAN_POINT('Ctrl Pts',(-3.52931423770067,-2.04064333351309,
21.2601360068076));
#34713=CARTESIAN_POINT('Ctrl Pts',(-2.81875615331693,-2.76501254901743,
21.3012920687562));
#34714=CARTESIAN_POINT('Ctrl Pts',(-1.90391505456104,-3.69763543176414,
21.3542803574844));
#34715=CARTESIAN_POINT('Ctrl Pts',(-0.480302633180845,-4.13118744625593,
21.4072686462127));
#34716=CARTESIAN_POINT('Ctrl Pts',(0.799079880925017,-3.86680126221775,
21.4602569349409));
#34717=CARTESIAN_POINT('Ctrl Pts',(2.07846239503088,-3.60241507817958,21.5132452236692));
#34718=CARTESIAN_POINT('Ctrl Pts',(3.21361500186243,-2.64009069561159,21.5662335123974));
#34719=CARTESIAN_POINT('Ctrl Pts',(3.68385102080785,-1.42123969585553,21.6192218011257));
#34720=CARTESIAN_POINT('Ctrl Pts',(4.15408703975328,-0.202388696099407,
21.6722100898539));
#34721=CARTESIAN_POINT('Ctrl Pts',(3.95940647081237,1.27298892084472,21.7251983785822));
#34722=CARTESIAN_POINT('Ctrl Pts',(3.18910793065139,2.32814760557936,21.7781866673104));
#34723=CARTESIAN_POINT('Ctrl Pts',(2.41880939049046,3.38330629031394,21.8311749560387));
#34724=CARTESIAN_POINT('Ctrl Pts',(1.07289287910942,4.01824604283911,21.8841632447669));
#34725=CARTESIAN_POINT('Ctrl Pts',(-0.231278918613751,3.94172434024104,
21.9371515334952));
#34726=CARTESIAN_POINT('Ctrl Pts',(-1.53545071633696,3.86520263764296,21.9901398222234));
#34727=CARTESIAN_POINT('Ctrl Pts',(-2.79787780040235,3.07721947992169,22.0431281109517));
#34728=CARTESIAN_POINT('Ctrl Pts',(-3.43949362875525,1.93921737114795,22.0961163996799));
#34729=CARTESIAN_POINT('Ctrl Pts',(-3.76928231599023,1.35428756589898,22.1233522274234));
#34730=CARTESIAN_POINT('Ctrl Pts',(-3.93505699138564,0.676885190519015,
22.1505880551669));
#34731=CARTESIAN_POINT('Ctrl Pts',(-3.93552176014147,-0.00030393483444853,
22.1778238829104));
#34732=CARTESIAN_POINT('Origin',(0.,0.,0.));
#34733=CARTESIAN_POINT('',(-3.94525314071248,-0.00295827654940184,23.3221761170896));
#34734=CARTESIAN_POINT('',(-3.94350653563855,-0.00347714007584369,23.1778238829104));
#34735=CARTESIAN_POINT('',(-3.942,-4.82755768223887E-16,0.));
#34736=CARTESIAN_POINT('Ctrl Pts',(-3.94525314071248,-0.00295827654940184,
23.3221761170896));
#34737=CARTESIAN_POINT('Ctrl Pts',(-3.93582062597525,1.11220231279806,23.2770415649289));
#34738=CARTESIAN_POINT('Ctrl Pts',(-3.44025122786987,2.23463092251658,23.2319070127682));
#34739=CARTESIAN_POINT('Ctrl Pts',(-2.60368934111206,2.9683990932166,23.1867724606075));
#34740=CARTESIAN_POINT('Ctrl Pts',(-1.62201025804696,3.82945298103697,23.1338084821129));
#34741=CARTESIAN_POINT('Ctrl Pts',(-0.170774803008089,4.15531037113838,
23.0808445036183));
#34742=CARTESIAN_POINT('Ctrl Pts',(1.08481479710351,3.79655919604497,23.0278805251236));
#34743=CARTESIAN_POINT('Ctrl Pts',(2.34040439721512,3.43780802095157,22.974916546629));
#34744=CARTESIAN_POINT('Ctrl Pts',(3.40034814239945,2.39444828066336,22.9219525681344));
#34745=CARTESIAN_POINT('Ctrl Pts',(3.77891236751962,1.14469612557038,22.8689885896398));
#34746=CARTESIAN_POINT('Ctrl Pts',(4.15747659263979,-0.105056029522605,
22.8160246111452));
#34747=CARTESIAN_POINT('Ctrl Pts',(3.85466129769578,-1.56120059942036,22.7630606326505));
#34748=CARTESIAN_POINT('Ctrl Pts',(3.00922455792002,-2.55639398676302,22.7100966541559));
#34749=CARTESIAN_POINT('Ctrl Pts',(2.16378781814425,-3.55158737410568,22.6571326756613));
#34750=CARTESIAN_POINT('Ctrl Pts',(0.77572963353673,-4.08582957889326,22.6041686971666));
#34751=CARTESIAN_POINT('Ctrl Pts',(-0.518779131279689,-3.91426327466899,
22.551204718672));
#34752=CARTESIAN_POINT('Ctrl Pts',(-1.81328789609611,-3.74269697044473,
22.4982407401774));
#34753=CARTESIAN_POINT('Ctrl Pts',(-3.01424724112142,-2.86532215720863,
22.4452767616828));
#34754=CARTESIAN_POINT('Ctrl Pts',(-3.57125476867308,-1.684251816953,22.3923127831882));
#34755=CARTESIAN_POINT('Ctrl Pts',(-3.81712408139379,-1.16291424345579,
22.3689338944886));
#34756=CARTESIAN_POINT('Ctrl Pts',(-3.9375233938263,-0.582403488318747,
22.3455550057891));
#34757=CARTESIAN_POINT('Ctrl Pts',(-3.93587951376728,-0.00124481178566893,
22.3221761170896));
#34758=CARTESIAN_POINT('Ctrl Pts',(-3.93552176014147,-0.00030393483444853,
22.1778238829104));
#34759=CARTESIAN_POINT('Ctrl Pts',(-3.93596121582331,-0.640610765021898,
22.2035763438952));
#34760=CARTESIAN_POINT('Ctrl Pts',(-3.78860721752551,-1.28072694143294,
22.2293288048799));
#34761=CARTESIAN_POINT('Ctrl Pts',(-3.49236428582461,-1.84230088118771,
22.2550812658647));
#34762=CARTESIAN_POINT('Ctrl Pts',(-2.88281454190065,-2.99779596492355,
22.3080695545929));
#34763=CARTESIAN_POINT('Ctrl Pts',(-1.64291048141232,-3.82076507256913,
22.3610578433212));
#34764=CARTESIAN_POINT('Ctrl Pts',(-0.341387846963322,-3.93371775192091,
22.4140461320494));
#34765=CARTESIAN_POINT('Ctrl Pts',(0.96013478748571,-4.04667043127269,22.4670344207777));
#34766=CARTESIAN_POINT('Ctrl Pts',(2.3232759958954,-3.44960668233064,22.5200227095059));
#34767=CARTESIAN_POINT('Ctrl Pts',(3.12277281794346,-2.41639589080571,22.5730109982342));
#34768=CARTESIAN_POINT('Ctrl Pts',(3.92226963999152,-1.38318509928078,22.6259992869624));
#34769=CARTESIAN_POINT('Ctrl Pts',(4.15812207567794,0.0861727348270178,
22.6789875756907));
#34770=CARTESIAN_POINT('Ctrl Pts',(3.72214521454942,1.31769395259273,22.7319758644189));
#34771=CARTESIAN_POINT('Ctrl Pts',(3.28616835342092,2.5492151703584,22.7849641531472));
#34772=CARTESIAN_POINT('Ctrl Pts',(2.17836219547751,3.54289977178199,22.8379524418754));
#34773=CARTESIAN_POINT('Ctrl Pts',(0.906871753871591,3.84295018391872,22.8909407306037));
#34774=CARTESIAN_POINT('Ctrl Pts',(-0.364618687734369,4.14300059605545,
22.9439290193319));
#34775=CARTESIAN_POINT('Ctrl Pts',(-1.79979341300285,3.74941681890528,22.9969173080602));
#34776=CARTESIAN_POINT('Ctrl Pts',(-2.74035137198678,2.84273547234742,23.0499055967884));
#34777=CARTESIAN_POINT('Ctrl Pts',(-3.49721397313409,2.11313322315816,23.0925450254957));
#34778=CARTESIAN_POINT('Ctrl Pts',(-3.9337951138205,1.05128255440302,23.1351844542031));
#34779=CARTESIAN_POINT('Ctrl Pts',(-3.94350653563855,-0.00347714007584369,
23.1778238829104));
#34780=CARTESIAN_POINT('Origin',(0.,0.,-1.84858989190503));
#34781=CARTESIAN_POINT('',(-3.37453254114594,-0.00253033205341837,23.651410108095));
#34782=CARTESIAN_POINT('',(-3.37610896110192,0.00188753811008129,23.848589891905));
#34783=CARTESIAN_POINT('',(-3.37175,2.08693528006523E-13,-1.84858989190503));
#34784=CARTESIAN_POINT('',(-3.33611311329475,0.488924695431507,24.62825));
#34785=CARTESIAN_POINT('Ctrl Pts',(-3.37453254114594,-0.00253033205341877,
23.651410108095));
#34786=CARTESIAN_POINT('Ctrl Pts',(-3.37593208671392,-0.167991834513083,
23.6592395344289));
#34787=CARTESIAN_POINT('Ctrl Pts',(-3.28964411790747,-1.45130369571974,
23.7200329392575));
#34788=CARTESIAN_POINT('Ctrl Pts',(-1.64345961820725,-3.63211696072943,
23.8337903225806));
#34789=CARTESIAN_POINT('Ctrl Pts',(2.163389782855,-3.34808861530533,23.9926822580645));
#34790=CARTESIAN_POINT('Ctrl Pts',(3.98513370400483,0.0032270738820094,
24.1515741935484));
#34791=CARTESIAN_POINT('Ctrl Pts',(2.15811323746268,3.35470758430291,24.3104661290323));
#34792=CARTESIAN_POINT('Ctrl Pts',(-1.65524532662936,3.62504834974875,24.4693580645161));
#34793=CARTESIAN_POINT('Ctrl Pts',(-3.1734075349997,1.59912472915632,24.5752860215054));
#34794=CARTESIAN_POINT('Ctrl Pts',(-3.33611311329483,0.488924695430968,
24.62825));
#34795=CARTESIAN_POINT('',(-0.624728334461187,3.31336876465952,24.62825));
#34796=CARTESIAN_POINT('Origin',(0.,0.,24.62825));
#34797=CARTESIAN_POINT('Ctrl Pts',(-3.37610896110192,0.00188753811008135,
23.848589891905));
#34798=CARTESIAN_POINT('Ctrl Pts',(-3.36932955763165,-1.01002015324007,
23.8965234396903));
#34799=CARTESIAN_POINT('Ctrl Pts',(-2.34697770975975,-3.15243101165571,
23.997445276204));
#34800=CARTESIAN_POINT('Ctrl Pts',(1.29650641132588,-3.76899081084458,24.1513554014457));
#34801=CARTESIAN_POINT('Ctrl Pts',(3.87454091099827,-0.951014904317504,
24.3103202676305));
#34802=CARTESIAN_POINT('Ctrl Pts',(2.88961752940844,2.74513957150359,24.4692851338152));
#34803=CARTESIAN_POINT('Ctrl Pts',(0.478408881098333,3.52136284087264,24.5752617112718));
#34804=CARTESIAN_POINT('Ctrl Pts',(-0.624728334461281,3.3133687646595,24.62825));
#34805=CARTESIAN_POINT('Origin',(0.,0.,-1.84858989190503));
#34806=CARTESIAN_POINT('',(-3.36651490374044,-0.00106473722420811,22.651410108095));
#34807=CARTESIAN_POINT('',(-3.37303860008607,-0.00297413674536479,22.848589891905));
#34808=CARTESIAN_POINT('',(-3.37175,2.08693528006523E-13,-1.84858989190503));
#34809=CARTESIAN_POINT('Ctrl Pts',(-3.36651490374044,-0.00106473722420751,
22.651410108095));
#34810=CARTESIAN_POINT('Ctrl Pts',(-3.36792097999337,-0.498152958330381,
22.6747889967945));
#34811=CARTESIAN_POINT('Ctrl Pts',(-3.03163608822923,-2.11956584279889,
22.7511318639887));
#34812=CARTESIAN_POINT('Ctrl Pts',(-0.52374905937927,-3.95173187129016,
22.8804387096774));
#34813=CARTESIAN_POINT('Ctrl Pts',(3.03803570770629,-2.58085580280275,23.0393306451613));
#34814=CARTESIAN_POINT('Ctrl Pts',(3.81506574631169,1.15563997615671,23.1982225806452));
#34815=CARTESIAN_POINT('Ctrl Pts',(1.095229123157,3.83292171460177,23.357114516129));
#34816=CARTESIAN_POINT('Ctrl Pts',(-2.44517403763626,3.03796695389969,23.508177025279));
#34817=CARTESIAN_POINT('Ctrl Pts',(-3.36646453466052,0.951311047229191,
23.6062755559343));
#34818=CARTESIAN_POINT('Ctrl Pts',(-3.37453254114594,-0.00253033205341877,
23.651410108095));
#34819=CARTESIAN_POINT('Ctrl Pts',(-3.37303860008607,-0.00297413674536527,
22.848589891905));
#34820=CARTESIAN_POINT('Ctrl Pts',(-3.3750546565899,-0.221938484280555,
22.8589387519259));
#34821=CARTESIAN_POINT('Ctrl Pts',(-3.25576106932785,-1.5598586434856,22.9222759006751));
#34822=CARTESIAN_POINT('Ctrl Pts',(-1.46739644894177,-3.70704069007233,
23.0386013381526));
#34823=CARTESIAN_POINT('Ctrl Pts',(2.32262200499063,-3.24046036848089,23.1975662043372));
#34824=CARTESIAN_POINT('Ctrl Pts',(3.98198637087808,0.198816238648098,23.3565310705221));
#34825=CARTESIAN_POINT('Ctrl Pts',(1.98816433058814,3.45581133218519,23.5154959367067));
#34826=CARTESIAN_POINT('Ctrl Pts',(-1.82925354411967,3.5422830008711,23.6744608028915));
#34827=CARTESIAN_POINT('Ctrl Pts',(-3.3238940749889,1.33320070540347,23.7854921212909));
#34828=CARTESIAN_POINT('Ctrl Pts',(-3.37682387017652,0.108596335481547,
23.8435351509621));
#34829=CARTESIAN_POINT('Ctrl Pts',(-3.37610896110192,0.00188753811008135,
23.848589891905));
#34830=CARTESIAN_POINT('Origin',(0.,0.,-1.84858989190503));
#34831=CARTESIAN_POINT('',(-3.37067265489827,0.00306245101284196,21.651410108095));
#34832=CARTESIAN_POINT('',(-3.36620890277955,-0.000259967599581801,21.848589891905));
#34833=CARTESIAN_POINT('',(-3.37175,2.08693528006523E-13,-1.84858989190503));
#34834=CARTESIAN_POINT('Ctrl Pts',(-3.37067265489827,0.00306245101284172,
21.651410108095));
#34835=CARTESIAN_POINT('Ctrl Pts',(-3.36335851690506,-0.822074352869367,
21.6903384591601));
#34836=CARTESIAN_POINT('Ctrl Pts',(-2.64233179033033,-2.78128712935246,
21.7822307887199));
#34837=CARTESIAN_POINT('Ctrl Pts',(0.640333691332285,-3.93451715048184,
21.9270870967742));
#34838=CARTESIAN_POINT('Ctrl Pts',(3.6541284705207,-1.59304681672573,22.0859790322581));
#34839=CARTESIAN_POINT('Ctrl Pts',(3.31849061020388,2.20863464806944,22.2448709677419));
#34840=CARTESIAN_POINT('Ctrl Pts',(-0.058926339166703,3.98584809986529,
22.4037629032258));
#34841=CARTESIAN_POINT('Ctrl Pts',(-2.89333741463138,2.3856381715614,22.5392759500101));
#34842=CARTESIAN_POINT('Ctrl Pts',(-3.36473556800141,0.627981401218202,
22.6218250182999));
#34843=CARTESIAN_POINT('Ctrl Pts',(-3.36651490374044,-0.00106473722420751,
22.651410108095));
#34844=CARTESIAN_POINT('Ctrl Pts',(-3.36620890277955,-0.00025996759958187,
21.848589891905));
#34845=CARTESIAN_POINT('Ctrl Pts',(-3.36658478677126,-0.547939966251195,
21.8743423528898));
#34846=CARTESIAN_POINT('Ctrl Pts',(-2.98121161418831,-2.22202824736231,
21.9530831026028));
#34847=CARTESIAN_POINT('Ctrl Pts',(-0.344707483447601,-3.97197126386073,
22.0848121410441));
#34848=CARTESIAN_POINT('Ctrl Pts',(3.15313982968432,-2.43989387002868,22.2437770072288));
#34849=CARTESIAN_POINT('Ctrl Pts',(3.75834184644668,1.33050740634341,22.4027418734136));
#34850=CARTESIAN_POINT('Ctrl Pts',(0.915689325102905,3.88032175554439,22.5617067395983));
#34851=CARTESIAN_POINT('Ctrl Pts',(-2.52724878310966,2.93612690507347,22.7103227457621));
#34852=CARTESIAN_POINT('Ctrl Pts',(-3.36473203323799,0.899203945410642,
22.8059504631977));
#34853=CARTESIAN_POINT('Ctrl Pts',(-3.37303860008607,-0.00297413674536527,
22.848589891905));
#34854=CARTESIAN_POINT('Origin',(0.,0.,-1.84858989190503));
#34855=CARTESIAN_POINT('',(-3.37717321336486,-0.000594050174885632,20.651410108095));
#34856=CARTESIAN_POINT('',(-3.37207954552848,0.0030841546013495,20.848589891905));
#34857=CARTESIAN_POINT('',(-3.37175,2.08693528006523E-13,-1.84858989190503));
#34858=CARTESIAN_POINT('Ctrl Pts',(-3.37717321336486,-0.000594050174885286,
20.651410108095));
#34859=CARTESIAN_POINT('Ctrl Pts',(-3.37725080892297,-0.0325216746987667,
20.6529239430311));
#34860=CARTESIAN_POINT('Ctrl Pts',(-3.36236902703727,-1.18141504466881,
20.7074017564618));
#34861=CARTESIAN_POINT('Ctrl Pts',(-2.06285714434356,-3.41102216294582,
20.8148435483871));
#34862=CARTESIAN_POINT('Ctrl Pts',(1.74979322227715,-3.58171404391184,20.9737354838709));
#34863=CARTESIAN_POINT('Ctrl Pts',(3.95855555351044,-0.46935037546761,21.1326274193549));
#34864=CARTESIAN_POINT('Ctrl Pts',(2.53884345747981,3.07322723010567,21.2915193548387));
#34865=CARTESIAN_POINT('Ctrl Pts',(-1.20801252978399,3.79883634829061,21.4504112903226));
#34866=CARTESIAN_POINT('Ctrl Pts',(-3.20089281760442,1.71770287259066,21.5703748747413));
#34867=CARTESIAN_POINT('Ctrl Pts',(-3.3733097693157,0.300565747216989,21.6373744806655));
#34868=CARTESIAN_POINT('Ctrl Pts',(-3.37067265489827,0.00306245101284172,
21.651410108095));
#34869=CARTESIAN_POINT('Ctrl Pts',(-3.37207954552848,0.00308415460134954,
20.848589891905));
#34870=CARTESIAN_POINT('Ctrl Pts',(-3.36400797375518,-0.868343092050458,
20.8897459538536));
#34871=CARTESIAN_POINT('Ctrl Pts',(-2.57426217007386,-2.87470778191459,
20.9838903045305));
#34872=CARTESIAN_POINT('Ctrl Pts',(0.806850527235046,-3.9044039261228,21.1310229439355));
#34873=CARTESIAN_POINT('Ctrl Pts',(3.71967457752779,-1.43506051902692,21.2899878101203));
#34874=CARTESIAN_POINT('Ctrl Pts',(3.22012038549849,2.35078763921597,21.448952676305));
#34875=CARTESIAN_POINT('Ctrl Pts',(-0.233528014234224,3.98005560769136,
21.6079175424898));
#34876=CARTESIAN_POINT('Ctrl Pts',(-2.94815289437509,2.2856379957105,21.7411299476898));
#34877=CARTESIAN_POINT('Ctrl Pts',(-3.36581136750493,0.578966930779549,
21.8213540641615));
#34878=CARTESIAN_POINT('Ctrl Pts',(-3.36620890277955,-0.00025996759958187,
21.848589891905));
#34879=CARTESIAN_POINT('Origin',(0.,0.,-1.84858989190503));
#34880=CARTESIAN_POINT('',(-3.36891084971013,-0.00271891470300727,19.651410108095));
#34881=CARTESIAN_POINT('',(-3.37664784145308,-0.00135850975013785,19.848589891905));
#34882=CARTESIAN_POINT('',(-3.37175,2.08693528006523E-13,-1.84858989190503));
#34883=CARTESIAN_POINT('Ctrl Pts',(-3.36891084971013,-0.00271891470300756,
19.651410108095));
#34884=CARTESIAN_POINT('Ctrl Pts',(-3.3716487661365,-0.364876698157186,
19.6684734053967));
#34885=CARTESIAN_POINT('Ctrl Pts',(-3.15091588331813,-1.84791316659487,
19.738500681193));
#34886=CARTESIAN_POINT('Ctrl Pts',(-0.989363022110038,-3.86155572506565,
19.8614919354839));
#34887=CARTESIAN_POINT('Ctrl Pts',(2.71000466929749,-2.92341008068914,20.0203838709678));
#34888=CARTESIAN_POINT('Ctrl Pts',(3.92533937020224,0.694379317983201,20.1792758064516));
#34889=CARTESIAN_POINT('Ctrl Pts',(1.54264613898669,3.6756896897871,20.3381677419355));
#34890=CARTESIAN_POINT('Ctrl Pts',(-2.21788792003282,3.29150051432633,20.4955458424833));
#34891=CARTESIAN_POINT('Ctrl Pts',(-3.37453600206181,1.08451822071036,20.5999599645364));
#34892=CARTESIAN_POINT('Ctrl Pts',(-3.37717321336486,-0.000594050174885286,
20.651410108095));
#34893=CARTESIAN_POINT('Ctrl Pts',(-3.37664784145308,-0.0013585097501378,
19.848589891905));
#34894=CARTESIAN_POINT('Ctrl Pts',(-3.37703253172857,-0.0767120652268113,
19.8521612660892));
#34895=CARTESIAN_POINT('Ctrl Pts',(-3.3405547692736,-1.26970315744226,19.9087209290016));
#34896=CARTESIAN_POINT('Ctrl Pts',(-1.92774697870435,-3.4898666651324,20.0182688806423));
#34897=CARTESIAN_POINT('Ctrl Pts',(1.89086481476229,-3.50998689564495,20.1772337468271));
#34898=CARTESIAN_POINT('Ctrl Pts',(3.97482324267393,-0.310093440809367,
20.3361986130118));
#34899=CARTESIAN_POINT('Ctrl Pts',(2.41233351706024,3.17427546962878,20.4951634791965));
#34900=CARTESIAN_POINT('Ctrl Pts',(-1.36319778790607,3.74660773920425,20.6541283453813));
#34901=CARTESIAN_POINT('Ctrl Pts',(-3.23443909431523,1.62353950510727,20.7719371496175));
#34902=CARTESIAN_POINT('Ctrl Pts',(-3.37440009475423,0.25361650187097,20.8367576651254));
#34903=CARTESIAN_POINT('Ctrl Pts',(-3.37207954552848,0.00308415460134954,
20.848589891905));
#34904=CARTESIAN_POINT('Origin',(0.,0.,-1.84858989190503));
#34905=CARTESIAN_POINT('',(-3.36739896644089,0.00198349937115513,18.651410108095));
#34906=CARTESIAN_POINT('',(-3.36796573513472,-0.00233887403243982,18.848589891905));
#34907=CARTESIAN_POINT('',(-3.37175,2.08693528006523E-13,-1.84858989190503));
#34908=CARTESIAN_POINT('Ctrl Pts',(-3.36739896644089,0.00198349937115483,
18.651410108095));
#34909=CARTESIAN_POINT('Ctrl Pts',(-3.36368984329845,-0.690983280694315,
18.6840228677623));
#34910=CARTESIAN_POINT('Ctrl Pts',(-2.81781374229535,-2.51470704523694,
18.7695996059241));
#34911=CARTESIAN_POINT('Ctrl Pts',(0.168518449156949,-3.98271933982683,
18.9081403225806));
#34912=CARTESIAN_POINT('Ctrl Pts',(3.43906728250426,-2.01575495384355,19.0670322580645));
#34913=CARTESIAN_POINT('Ctrl Pts',(3.55731284355299,1.79888219198906,19.2259241935484));
#34914=CARTESIAN_POINT('Ctrl Pts',(0.41486938743375,3.96463556949202,19.3848161290323));
#34915=CARTESIAN_POINT('Ctrl Pts',(-2.72954745140897,2.65402060505441,19.5266447672144));
#34916=CARTESIAN_POINT('Ctrl Pts',(-3.36315035318836,0.75925052739643,19.615509426902));
#34917=CARTESIAN_POINT('Ctrl Pts',(-3.36891084971013,-0.00271891470300756,
19.651410108095));
#34918=CARTESIAN_POINT('Ctrl Pts',(-3.36796573513472,-0.00233887403243996,
18.848589891905));
#34919=CARTESIAN_POINT('Ctrl Pts',(-3.37053511298134,-0.405354963155371,
18.867564867053));
#34920=CARTESIAN_POINT('Ctrl Pts',(-3.11694291466331,-1.93068155902232,
18.9395281309293));
#34921=CARTESIAN_POINT('Ctrl Pts',(-0.847949117405149,-3.89568479841959,
19.0644796835338));
#34922=CARTESIAN_POINT('Ctrl Pts',(2.81658890100978,-2.82173788950715,19.2234445497186));
#34923=CARTESIAN_POINT('Ctrl Pts',(3.89722701433046,0.840832535700663,19.3824094159033));
#34924=CARTESIAN_POINT('Ctrl Pts',(1.40260268563389,3.73203476143841,19.5413742820881));
#34925=CARTESIAN_POINT('Ctrl Pts',(-2.29379652508948,3.21148336255172,19.6967677740886));
#34926=CARTESIAN_POINT('Ctrl Pts',(-3.37132490258154,1.04130462761393,19.799172977361));
#34927=CARTESIAN_POINT('Ctrl Pts',(-3.37664784145308,-0.0013585097501378,
19.848589891905));
#34928=CARTESIAN_POINT('Origin',(0.,0.,-1.84858989190503));
#34929=CARTESIAN_POINT('',(-3.3761529784003,0.00176635805113218,17.651410108095));
#34930=CARTESIAN_POINT('',(-3.36813340603362,0.00242210091315795,17.848589891905));
#34931=CARTESIAN_POINT('',(-3.37175,2.08693528006523E-13,-1.84858989190503));
#34932=CARTESIAN_POINT('Ctrl Pts',(-3.3761529784003,0.00176635805113214,
17.651410108095));
#34933=CARTESIAN_POINT('Ctrl Pts',(-3.36968839136432,-1.01481764775316,
17.6995723301278));
#34934=CARTESIAN_POINT('Ctrl Pts',(-2.33957623769215,-3.16069067030928,
17.8006985306553));
#34935=CARTESIAN_POINT('Ctrl Pts',(1.31202620257783,-3.7641784032229,17.9547887096774));
#34936=CARTESIAN_POINT('Ctrl Pts',(3.87479594250582,-0.936166764781103,
18.1136806451613));
#34937=CARTESIAN_POINT('Ctrl Pts',(2.88586665310525,2.74995008464444,18.2725725806452));
#34938=CARTESIAN_POINT('Ctrl Pts',(-0.748293493014444,3.91541934610488,
18.431464516129));
#34939=CARTESIAN_POINT('Ctrl Pts',(-3.09142162050251,1.98937278233,18.5577436919457));
#34940=CARTESIAN_POINT('Ctrl Pts',(-3.36971355672701,0.434412975597321,
18.6310588892676));
#34941=CARTESIAN_POINT('Ctrl Pts',(-3.36739896644089,0.00198349937115483,
18.651410108095));
#34942=CARTESIAN_POINT('Ctrl Pts',(-3.36813340603362,0.00242210091315778,
17.848589891905));
#34943=CARTESIAN_POINT('Ctrl Pts',(-3.36329734613199,-0.727665112355139,
17.8829684680169));
#34944=CARTESIAN_POINT('Ctrl Pts',(-2.77110248260437,-2.59019431375764,
17.970335332857));
#34945=CARTESIAN_POINT('Ctrl Pts',(0.302833216085013,-3.97538297495793,
18.1106904864254));
#34946=CARTESIAN_POINT('Ctrl Pts',(3.5065275226793,-1.89727238082542,18.2696553526101));
#34947=CARTESIAN_POINT('Ctrl Pts',(3.49338172535042,1.92136979140851,18.4286202187948));
#34948=CARTESIAN_POINT('Ctrl Pts',(0.275455597698851,3.97737375262188,18.5875850849796));
#34949=CARTESIAN_POINT('Ctrl Pts',(-2.78089559275923,2.57471376007135,18.7275749760163));
#34950=CARTESIAN_POINT('Ctrl Pts',(-3.36336003453583,0.720081709408907,
18.8145765783248));
#34951=CARTESIAN_POINT('Ctrl Pts',(-3.36796573513472,-0.00233887403243996,
18.848589891905));
#34952=CARTESIAN_POINT('Origin',(0.,0.,-1.84858989190503));
#34953=CARTESIAN_POINT('',(-3.37277477193024,-0.0030073171892592,16.651410108095));
#34954=CARTESIAN_POINT('',(-3.37676993930056,0.00122898291704077,16.848589891905));
#34955=CARTESIAN_POINT('',(-3.37175,2.08693528006523E-13,-1.84858989190503));
#34956=CARTESIAN_POINT('Ctrl Pts',(-3.37277477193024,-0.0030073171892591,
16.651410108095));
#34957=CARTESIAN_POINT('Ctrl Pts',(-3.3748752325093,-0.230456048008689,
16.6621578139988));
#34958=CARTESIAN_POINT('Ctrl Pts',(-3.25015286697033,-1.5764664391,16.7258694983973));
#34959=CARTESIAN_POINT('Ctrl Pts',(-1.44097876042837,-3.71672329068694,
16.8425451612903));
#34960=CARTESIAN_POINT('Ctrl Pts',(2.34362517346463,-3.22457328244272,17.0014370967742));
#34961=CARTESIAN_POINT('Ctrl Pts',(3.980025336833,0.223271417131382,17.1603290322581));
#34962=CARTESIAN_POINT('Ctrl Pts',(1.96827154957251,3.46646201691059,17.3192209677419));
#34963=CARTESIAN_POINT('Ctrl Pts',(-1.84763096082072,3.53223889907763,17.4781129032258));
#34964=CARTESIAN_POINT('Ctrl Pts',(-3.32665838484882,1.32176305576882,17.5888426166768));
#34965=CARTESIAN_POINT('Ctrl Pts',(-3.3767974954359,0.103119423021283,17.6466083516332));
#34966=CARTESIAN_POINT('Ctrl Pts',(-3.3761529784003,0.00176635805113214,
17.651410108095));
#34967=CARTESIAN_POINT('Ctrl Pts',(-3.37676993930056,0.00122898291704094,
16.848589891905));
#34968=CARTESIAN_POINT('Ctrl Pts',(-3.37185165056191,-1.0490400428621,16.8983720689807));
#34969=CARTESIAN_POINT('Ctrl Pts',(-2.28032799824397,-3.22603625281427,
17.0011425347847));
#34970=CARTESIAN_POINT('Ctrl Pts',(1.42826443406275,-3.7222894112013,17.1569012893169));
#34971=CARTESIAN_POINT('Ctrl Pts',(3.90292376012977,-0.813980268166524,
17.3158661555016));
#34972=CARTESIAN_POINT('Ctrl Pts',(2.79709452794753,2.84106317354542,17.4748310216864));
#34973=CARTESIAN_POINT('Ctrl Pts',(-0.87475073969136,3.88975434928213,17.6337958878711));
#34974=CARTESIAN_POINT('Ctrl Pts',(-3.12356865319579,1.91496539554474,17.758382177944));
#34975=CARTESIAN_POINT('Ctrl Pts',(-3.37075124816507,0.397630825661392,
17.8299801792886));
#34976=CARTESIAN_POINT('Ctrl Pts',(-3.36813340603362,0.00242210091315778,
17.848589891905));
#34977=CARTESIAN_POINT('Origin',(0.,0.,-1.84858989190503));
#34978=CARTESIAN_POINT('',(-3.36620324934232,-6.47284927745773E-5,15.651410108095));
#34979=CARTESIAN_POINT('',(-3.37184361771993,-0.00309624629213801,15.848589891905));
#34980=CARTESIAN_POINT('',(-3.37175,2.08693528006523E-13,-1.84858989190503));
#34981=CARTESIAN_POINT('Ctrl Pts',(-3.36620324934232,-6.47284927745434E-5,
15.651410108095));
#34982=CARTESIAN_POINT('Ctrl Pts',(-3.36629886637731,-0.559331950050314,
15.6777072763644));
#34983=CARTESIAN_POINT('Ctrl Pts',(-2.969304704679,-2.24486717295088,15.7569684231284));
#34984=CARTESIAN_POINT('Ctrl Pts',(-0.30568234557457,-3.97454527098943,
15.8891935483871));
#34985=CARTESIAN_POINT('Ctrl Pts',(3.17532551476257,-2.40992939374543,16.048085483871));
#34986=CARTESIAN_POINT('Ctrl Pts',(3.74577996379122,1.36366574731522,16.2069774193548));
#34987=CARTESIAN_POINT('Ctrl Pts',(0.882793462927545,3.88730337243608,16.3658693548387));
#34988=CARTESIAN_POINT('Ctrl Pts',(-2.54098403241842,2.91809266432718,16.5140135844188));
#34989=CARTESIAN_POINT('Ctrl Pts',(-3.36452430274498,0.890396140872364,
16.6091938355042));
#34990=CARTESIAN_POINT('Ctrl Pts',(-3.37277477193024,-0.0030073171892591,
16.651410108095));
#34991=CARTESIAN_POINT('Ctrl Pts',(-3.37184361771993,-0.00309624629213769,
15.848589891905));
#34992=CARTESIAN_POINT('Ctrl Pts',(-3.37422938253555,-0.261408813023958,
15.8607873812163));
#34993=CARTESIAN_POINT('Ctrl Pts',(-3.22903130121081,-1.63922767409008,
15.9259731592558));
#34994=CARTESIAN_POINT('Ctrl Pts',(-1.33737014962086,-3.75590452983738,
16.0441472260236));
#34995=CARTESIAN_POINT('Ctrl Pts',(2.43413116992486,-3.15759136082396,16.2031120922084));
#34996=CARTESIAN_POINT('Ctrl Pts',(3.97259404474729,0.337452678146523,16.3620769583931));
#34997=CARTESIAN_POINT('Ctrl Pts',(1.86665380078734,3.52292227310739,16.5210418245779));
#34998=CARTESIAN_POINT('Ctrl Pts',(-1.95172895721992,3.47651144567355,16.6800066907626));
#34999=CARTESIAN_POINT('Ctrl Pts',(-3.34455787065121,1.25410828714709,16.7891893798717));
#35000=CARTESIAN_POINT('Ctrl Pts',(-3.37708669087234,0.0688692501706657,
16.8453837802525));
#35001=CARTESIAN_POINT('Ctrl Pts',(-3.37676993930056,0.00122898291704094,
16.848589891905));
#35002=CARTESIAN_POINT('Origin',(0.,0.,-1.84858989190503));
#35003=CARTESIAN_POINT('',(-3.37253669875649,0.00303677565441225,14.651410108095));
#35004=CARTESIAN_POINT('',(-3.36623102492646,0.000387483300791081,14.848589891905));
#35005=CARTESIAN_POINT('',(-3.37175,2.08693528006523E-13,-1.84858989190503));
#35006=CARTESIAN_POINT('Ctrl Pts',(-3.37253669875649,0.00303677565441206,
14.651410108095));
#35007=CARTESIAN_POINT('Ctrl Pts',(-3.36433888251516,-0.882704764956481,
14.69325673873));
#35008=CARTESIAN_POINT('Ctrl Pts',(-2.55272847437535,-2.90279523765218,
14.7880673478596));
#35009=CARTESIAN_POINT('Ctrl Pts',(0.8556871302199,-3.8933599040824,14.9358419354839));
#35010=CARTESIAN_POINT('Ctrl Pts',(3.73618765800463,-1.38973148187494,15.0947338709677));
#35011=CARTESIAN_POINT('Ctrl Pts',(3.19203969455987,2.38774671937678,15.2536258064516));
#35012=CARTESIAN_POINT('Ctrl Pts',(-0.277982160818163,3.97657864574653,
15.4125177419355));
#35013=CARTESIAN_POINT('Ctrl Pts',(-2.9610712487067,2.26071800063538,15.54511250915));
#35014=CARTESIAN_POINT('Ctrl Pts',(-3.3661062882817,0.567063743655371,15.6247432978698));
#35015=CARTESIAN_POINT('Ctrl Pts',(-3.36620324934232,-6.47284927745434E-5,
15.651410108095));
#35016=CARTESIAN_POINT('Ctrl Pts',(-3.36623102492646,0.000387483300790976,
14.848589891905));
#35017=CARTESIAN_POINT('Ctrl Pts',(-3.36563039823437,-0.58659786734821,
14.8761909821801));
#35018=CARTESIAN_POINT('Ctrl Pts',(-2.93982168940875,-2.30128717837213,
14.9567803611835));
#35019=CARTESIAN_POINT('Ctrl Pts',(-0.206119829211681,-3.98156908396121,
15.0903580289152));
#35020=CARTESIAN_POINT('Ctrl Pts',(3.23622917375625,-2.32856146349605,15.2493228950999));
#35021=CARTESIAN_POINT('Ctrl Pts',(3.70970605913983,1.46063640552025,15.4082877612846));
#35022=CARTESIAN_POINT('Ctrl Pts',(0.779949646731194,3.90986653262151,15.5672526274694));
#35023=CARTESIAN_POINT('Ctrl Pts',(-2.58561751919903,2.85952988987219,15.7140200043429));
#35024=CARTESIAN_POINT('Ctrl Pts',(-3.36386515169579,0.8607517004072,15.8077990924881));
#35025=CARTESIAN_POINT('Ctrl Pts',(-3.37184361771993,-0.00309624629213769,
15.848589891905));
#35026=CARTESIAN_POINT('Origin',(0.,0.,-1.84858989190503));
#35027=CARTESIAN_POINT('',(-3.37630962516523,-0.00164737155311467,13.651410108095));
#35028=CARTESIAN_POINT('',(-3.37326960455653,0.00293423317535069,13.848589891905));
#35029=CARTESIAN_POINT('',(-3.37175,2.08693528006523E-13,-1.84858989190503));
#35030=CARTESIAN_POINT('Ctrl Pts',(-3.37630962516523,-0.00164737155311456,
13.651410108095));
#35031=CARTESIAN_POINT('Ctrl Pts',(-3.3768714611022,-0.0951867578458431,
13.6558422226009));
#35032=CARTESIAN_POINT('Ctrl Pts',(-3.33090125004588,-1.30596569148795,
13.7132383156015));
#35033=CARTESIAN_POINT('Ctrl Pts',(-1.87219709398698,-3.51927973437849,
13.8235983870968));
#35034=CARTESIAN_POINT('Ctrl Pts',(1.94407109338865,-3.48009186536664,13.9824903225806));
#35035=CARTESIAN_POINT('Ctrl Pts',(3.97837307717912,-0.25099694483561,14.1413822580645));
#35036=CARTESIAN_POINT('Ctrl Pts',(2.36603559757979,3.20816573115008,14.3002741935484));
#35037=CARTESIAN_POINT('Ctrl Pts',(-1.41504740048591,3.7266731359107,14.4591661290323));
#35038=CARTESIAN_POINT('Ctrl Pts',(-3.24486867351568,1.59233323105557,14.5762114338811));
#35039=CARTESIAN_POINT('Ctrl Pts',(-3.37471460348768,0.238350746486947,
14.6402927602354));
#35040=CARTESIAN_POINT('Ctrl Pts',(-3.37253669875649,0.00303677565441206,
14.651410108095));
#35041=CARTESIAN_POINT('Ctrl Pts',(-3.37326960455653,0.00293423317535065,
13.848589891905));
#35042=CARTESIAN_POINT('Ctrl Pts',(-3.36494392394814,-0.906810168463347,
13.891594583144));
#35043=CARTESIAN_POINT('Ctrl Pts',(-2.51545460624217,-2.95119723051152,
13.9875875631112));
#35044=CARTESIAN_POINT('Ctrl Pts',(0.942385426660244,-3.87392403926152,
14.1365688318067));
#35045=CARTESIAN_POINT('Ctrl Pts',(3.76741231340739,-1.30460040439068,14.2955336979914));
#35046=CARTESIAN_POINT('Ctrl Pts',(3.1362669786623,2.46154569181692,14.4544985641762));
#35047=CARTESIAN_POINT('Ctrl Pts',(-0.372046531241306,3.96950363810656,
14.6134634303609));
#35048=CARTESIAN_POINT('Ctrl Pts',(-2.98916250729706,2.20635255558199,14.7448272062705));
#35049=CARTESIAN_POINT('Ctrl Pts',(-3.36678347516941,0.540290560949759,
14.8232026934519));
#35050=CARTESIAN_POINT('Ctrl Pts',(-3.36623102492646,0.000387483300790976,
14.848589891905));
#35051=CARTESIAN_POINT('Origin',(0.,0.,-1.84858989190503));
#35052=CARTESIAN_POINT('',(-3.36754256765694,-0.00208193686516585,12.651410108095));
#35053=CARTESIAN_POINT('',(-3.3758812610584,-0.00196014188030613,12.848589891905));
#35054=CARTESIAN_POINT('',(-3.37175,2.08693528006523E-13,-1.84858989190503));
#35055=CARTESIAN_POINT('Ctrl Pts',(-3.36754256765694,-0.00208193686516537,
12.651410108095));
#35056=CARTESIAN_POINT('Ctrl Pts',(-3.36993408573054,-0.426611763038696,
12.6713916849665));
#35057=CARTESIAN_POINT('Ctrl Pts',(-3.09838828538505,-1.97347045721629,
12.7443372403327));
#35058=CARTESIAN_POINT('Ctrl Pts',(-0.775556132376715,-3.9101105474236,
12.8702467741936));
#35059=CARTESIAN_POINT('Ctrl Pts',(2.86663624227273,-2.76999069710151,13.0291387096774));
#35060=CARTESIAN_POINT('Ctrl Pts',(3.88122465785174,0.909146282412278,13.1880306451613));
#35061=CARTESIAN_POINT('Ctrl Pts',(1.33822138229676,3.75494545093591,13.3469225806451));
#35062=CARTESIAN_POINT('Ctrl Pts',(-2.32626682514693,3.17552839905125,13.5013824016231));
#35063=CARTESIAN_POINT('Ctrl Pts',(-3.37015749501604,1.02261334351231,13.6028782441063));
#35064=CARTESIAN_POINT('Ctrl Pts',(-3.37630962516523,-0.00164737155311456,
13.651410108095));
#35065=CARTESIAN_POINT('Ctrl Pts',(-3.3758812610584,-0.00196014188030577,
12.848589891905));
#35066=CARTESIAN_POINT('Ctrl Pts',(-3.37667181942981,-0.11638712350615,
12.8540098953796));
#35067=CARTESIAN_POINT('Ctrl Pts',(-3.31942395404611,-1.34870119310656,
12.9124181875824));
#35068=CARTESIAN_POINT('Ctrl Pts',(-1.80499399926681,-3.5549084962852,13.0238147685134));
#35069=CARTESIAN_POINT('Ctrl Pts',(2.01200065152342,-3.44198069904803,13.1827796346982));
#35070=CARTESIAN_POINT('Ctrl Pts',(3.98321358718988,-0.171427165804589,
13.3417445008829));
#35071=CARTESIAN_POINT('Ctrl Pts',(2.30028118194861,3.25639129072706,13.5007093670677));
#35072=CARTESIAN_POINT('Ctrl Pts',(-1.49289753065309,3.69684118097057,13.6596742332524));
#35073=CARTESIAN_POINT('Ctrl Pts',(-3.26085313565002,1.54418744509758,13.7756344081982));
#35074=CARTESIAN_POINT('Ctrl Pts',(-3.37520242261949,0.214132631825097,
13.8386062944157));
#35075=CARTESIAN_POINT('Ctrl Pts',(-3.37326960455653,0.00293423317535065,
13.848589891905));
#35076=CARTESIAN_POINT('Origin',(0.,0.,-1.84858989190503));
#35077=CARTESIAN_POINT('',(-3.36871665678573,0.00265343926576773,11.651410108095));
#35078=CARTESIAN_POINT('',(-3.36722041330275,-0.00185992061757206,11.848589891905));
#35079=CARTESIAN_POINT('',(-3.37175,2.08693528006523E-13,-1.84858989190503));
#35080=CARTESIAN_POINT('Ctrl Pts',(-3.36871665678573,0.00265343926576761,
11.651410108095));
#35081=CARTESIAN_POINT('Ctrl Pts',(-3.36317444447066,-0.751580168678052,
11.6869411473321));
#35082=CARTESIAN_POINT('Ctrl Pts',(-2.7398020033052,-2.63841079513441,11.7754361650639));
#35083=CARTESIAN_POINT('Ctrl Pts',(0.38723559847199,-3.96742994882286,11.9168951612903));
#35084=CARTESIAN_POINT('Ctrl Pts',(3.54469272874429,-1.82362421192741,12.0757870967742));
#35085=CARTESIAN_POINT('Ctrl Pts',(3.45302863798842,1.9917442187119,12.2346790322581));
#35086=CARTESIAN_POINT('Ctrl Pts',(0.196264076456207,3.98144850774605,12.3935709677419));
#35087=CARTESIAN_POINT('Ctrl Pts',(-2.80821900811,2.53041799939006,12.5324813263542));
#35088=CARTESIAN_POINT('Ctrl Pts',(-3.36359503087846,0.698664221349558,
12.6184277064719));
#35089=CARTESIAN_POINT('Ctrl Pts',(-3.36754256765694,-0.00208193686516537,
12.651410108095));
#35090=CARTESIAN_POINT('Ctrl Pts',(-3.36722041330275,-0.00185992061757217,
11.848589891905));
#35091=CARTESIAN_POINT('Ctrl Pts',(-3.36943251646156,-0.444385182068521,
11.8694134963434));
#35092=CARTESIAN_POINT('Ctrl Pts',(-3.08234983495276,-2.01021544013623,
11.9432253895101));
#35093=CARTESIAN_POINT('Ctrl Pts',(-0.711713421966334,-3.92286142494773,
12.0700255714049));
#35094=CARTESIAN_POINT('Ctrl Pts',(2.91318501009988,-2.72189839106446,12.2289904375897));
#35095=CARTESIAN_POINT('Ctrl Pts',(3.86556759564105,0.976096776902648,12.3879553037744));
#35096=CARTESIAN_POINT('Ctrl Pts',(1.27173165426137,3.77863419159615,12.5469201699592));
#35097=CARTESIAN_POINT('Ctrl Pts',(-2.36055670961755,3.13734167043916,12.7004650326694));
#35098=CARTESIAN_POINT('Ctrl Pts',(-3.36894298024411,1.00230034028648,12.8010216066513));
#35099=CARTESIAN_POINT('Ctrl Pts',(-3.3758812610584,-0.00196014188030577,
12.848589891905));
#35100=CARTESIAN_POINT('Origin',(0.,0.,-1.84858989190503));
#35101=CARTESIAN_POINT('',(-3.37710546106046,0.000736094683953019,10.651410108095));
#35102=CARTESIAN_POINT('',(-3.36907238740032,0.00277677980771746,10.848589891905));
#35103=CARTESIAN_POINT('',(-3.37175,2.08693528006523E-13,-1.84858989190503));
#35104=CARTESIAN_POINT('Ctrl Pts',(-3.37710546106046,0.000736094683952996,
10.651410108095));
#35105=CARTESIAN_POINT('Ctrl Pts',(-3.37391321273993,-1.07663815669567,
10.7024906096977));
#35106=CARTESIAN_POINT('Ctrl Pts',(-2.23194165802167,-3.27693130018453,
10.8065350897951));
#35107=CARTESIAN_POINT('Ctrl Pts',(1.51699821428175,-3.68634890174633,10.9635435483871));
#35108=CARTESIAN_POINT('Ctrl Pts',(3.92040597926993,-0.721712384018116,
11.122435483871));
#35109=CARTESIAN_POINT('Ctrl Pts',(2.73030783639792,2.90445707939446,11.2813274193548));
#35110=CARTESIAN_POINT('Ctrl Pts',(-0.962433500126168,3.86835540835836,
11.4402193548387));
#35111=CARTESIAN_POINT('Ctrl Pts',(-3.1445024192473,1.86381595651157,11.5635802510854));
#35112=CARTESIAN_POINT('Ctrl Pts',(-3.37143588630209,0.372710407919653,
11.6339771688375));
#35113=CARTESIAN_POINT('Ctrl Pts',(-3.36871665678573,0.00265343926576761,
11.651410108095));
#35114=CARTESIAN_POINT('Ctrl Pts',(-3.36907238740032,0.00277677980771742,
10.848589891905));
#35115=CARTESIAN_POINT('Ctrl Pts',(-3.36312082444251,-0.766029392039194,
10.8848170973072));
#35116=CARTESIAN_POINT('Ctrl Pts',(-2.72027913252513,-2.66834094208117,
10.9740325914377));
#35117=CARTESIAN_POINT('Ctrl Pts',(0.441146911493231,-3.96241935650807,
11.1162363742964));
#35118=CARTESIAN_POINT('Ctrl Pts',(3.57049754163045,-1.77395745708877,11.2752012404812));
#35119=CARTESIAN_POINT('Ctrl Pts',(3.42432285260543,2.04190860605321,11.4341661066659));
#35120=CARTESIAN_POINT('Ctrl Pts',(0.136721492950909,3.98455580808139,11.5931309728507));
#35121=CARTESIAN_POINT('Ctrl Pts',(-2.82921667119627,2.49618535096433,11.7312722345971));
#35122=CARTESIAN_POINT('Ctrl Pts',(-3.36380354088135,0.681676177418306,
11.8164252076152));
#35123=CARTESIAN_POINT('Ctrl Pts',(-3.36722041330275,-0.00185992061757217,
11.848589891905));
#35124=CARTESIAN_POINT('Origin',(0.,0.,-1.84858989190503));
#35125=CARTESIAN_POINT('',(-3.37090359896229,-0.00307926823583696,9.65141010809498));
#35126=CARTESIAN_POINT('',(-3.37720911693329,0.000534521222638907,9.84858989190502));
#35127=CARTESIAN_POINT('',(-3.37175,2.08693528006523E-13,-1.84858989190503));
#35128=CARTESIAN_POINT('Ctrl Pts',(-3.37090359896229,-0.0030792682358368,
9.65141010809498));
#35129=CARTESIAN_POINT('Ctrl Pts',(-3.37349992290045,-0.292697043198134,
9.6650760935687));
#35130=CARTESIAN_POINT('Ctrl Pts',(-3.20668744219234,-1.70181407180786,
9.73170605753704));
#35131=CARTESIAN_POINT('Ctrl Pts',(-1.23445173354738,-3.79032725830928,
9.85129999999999));
#35132=CARTESIAN_POINT('Ctrl Pts',(2.51736903674626,-3.09084210861242,10.0101919354839));
#35133=CARTESIAN_POINT('Ctrl Pts',(3.96172967315432,0.441757630821415,10.1690838709677));
#35134=CARTESIAN_POINT('Ctrl Pts',(1.77470645260886,3.56943536355667,10.3279758064516));
#35135=CARTESIAN_POINT('Ctrl Pts',(-2.03904067252446,3.42531238624034,10.4868677419355));
#35136=CARTESIAN_POINT('Ctrl Pts',(-3.35858003390563,1.1971743885357,10.5946791758166));
#35137=CARTESIAN_POINT('Ctrl Pts',(-3.37722316793013,0.0404618108125119,
10.6495266312031));
#35138=CARTESIAN_POINT('Ctrl Pts',(-3.37710546106046,0.000736094683952996,
10.651410108095));
#35139=CARTESIAN_POINT('Ctrl Pts',(-3.37720911693329,0.000534521222638742,
9.84858989190502));
#35140=CARTESIAN_POINT('Ctrl Pts',(-3.37481325646777,-1.08835732049462,
9.90022069827108));
#35141=CARTESIAN_POINT('Ctrl Pts',(-2.21074657312113,-3.29916896326091,
10.0048397933654));
#35142=CARTESIAN_POINT('Ctrl Pts',(1.55707745747673,-3.67027077281332,10.1624471771879));
#35143=CARTESIAN_POINT('Ctrl Pts',(3.928912558612,-0.677512997019795,10.3214120433727));
#35144=CARTESIAN_POINT('Ctrl Pts',(2.69641733534343,2.93678588051791,10.4803769095574));
#35145=CARTESIAN_POINT('Ctrl Pts',(-1.00973405207762,3.8569177977272,10.6393417757422));
#35146=CARTESIAN_POINT('Ctrl Pts',(-3.15606037844699,1.83542847981608,10.7620794365247));
#35147=CARTESIAN_POINT('Ctrl Pts',(-3.37182597111036,0.358476982592217,
10.831828808579));
#35148=CARTESIAN_POINT('Ctrl Pts',(-3.36907238740032,0.00277677980771742,
10.848589891905));
#35149=CARTESIAN_POINT('Origin',(0.,0.,-1.84858989190503));
#35150=CARTESIAN_POINT('',(-3.36644585084492,0.000942668595409863,8.65141010809498));
#35151=CARTESIAN_POINT('',(-3.37066808100933,-0.00306963188584058,8.84858989190501));
#35152=CARTESIAN_POINT('',(-3.37175,2.08693528006523E-13,-1.84858989190503));
#35153=CARTESIAN_POINT('Ctrl Pts',(-3.36644585084492,0.000942668595410034,
8.65141010809498));
#35154=CARTESIAN_POINT('Ctrl Pts',(-3.36489256340397,-0.620276501159167,
8.68062555593429));
#35155=CARTESIAN_POINT('Ctrl Pts',(-2.90218694538986,-2.36984060140867,
8.76280498226821));
#35156=CARTESIAN_POINT('Ctrl Pts',(-0.086697347329244,-3.9853400579507,
8.89794838709678));
#35157=CARTESIAN_POINT('Ctrl Pts',(3.30302181201077,-2.23170309784288,9.05684032258065));
#35158=CARTESIAN_POINT('Ctrl Pts',(3.66513912143678,1.56754809433529,9.21573225806451));
#35159=CARTESIAN_POINT('Ctrl Pts',(0.667732148006428,3.92995999802278,9.3746241935484));
#35160=CARTESIAN_POINT('Ctrl Pts',(-2.63128595375923,2.79674582771393,9.51985014355854));
#35161=CARTESIAN_POINT('Ctrl Pts',(-3.36343759366045,0.829747410900375,
9.61211211507407));
#35162=CARTESIAN_POINT('Ctrl Pts',(-3.37090359896229,-0.0030792682358368,
9.65141010809498));
#35163=CARTESIAN_POINT('Ctrl Pts',(-3.37066808100933,-0.0030696318858409,
8.84858989190502));
#35164=CARTESIAN_POINT('Ctrl Pts',(-3.37331082414,-0.300796169438093,8.86263601050667));
#35165=CARTESIAN_POINT('Ctrl Pts',(-3.20068977672434,-1.71866740211794,
8.92967041783657));
#35166=CARTESIAN_POINT('Ctrl Pts',(-1.20570712414377,-3.80021684712055,
9.04969311389473));
#35167=CARTESIAN_POINT('Ctrl Pts',(2.54266018034211,-3.07087234538534,9.20865798007948));
#35168=CARTESIAN_POINT('Ctrl Pts',(3.95842601916979,0.47564819468749,9.36762284626423));
#35169=CARTESIAN_POINT('Ctrl Pts',(1.74278629094578,3.58581562527152,9.52658771244896));
#35170=CARTESIAN_POINT('Ctrl Pts',(-2.07166160205713,3.40640513751843,9.68555257863373));
#35171=CARTESIAN_POINT('Ctrl Pts',(-3.36396169301834,1.17525404838138,9.7928866384524));
#35172=CARTESIAN_POINT('Ctrl Pts',(-3.377272109138,0.0291637752183697,9.84723240954283));
#35173=CARTESIAN_POINT('Ctrl Pts',(-3.37720911693329,0.000534521222638742,
9.84858989190502));
#35174=CARTESIAN_POINT('Origin',(0.,0.,-1.84858989190503));
#35175=CARTESIAN_POINT('',(-3.37436653161969,0.00264543560195785,7.65141010809498));
#35176=CARTESIAN_POINT('',(-3.36647579863201,0.00101859643942465,7.84858989190502));
#35177=CARTESIAN_POINT('',(-3.37175,2.08693528006523E-13,-1.84858989190503));
#35178=CARTESIAN_POINT('Ctrl Pts',(-3.37436653161969,0.00264543560195811,
7.65141010809498));
#35179=CARTESIAN_POINT('Ctrl Pts',(-3.36621424622869,-0.943539301975876,
7.69617501829988));
#35180=CARTESIAN_POINT('Ctrl Pts',(-2.45755376938072,-3.02292340440546,
7.7939039069994));
#35181=CARTESIAN_POINT('Ctrl Pts',(1.06845185659111,-3.84042477308012,7.94459677419355));
#35182=CARTESIAN_POINT('Ctrl Pts',(3.80694458147109,-1.18221180891932,8.10348870967742));
#35183=CARTESIAN_POINT('Ctrl Pts',(3.0559319039131,2.55963513145653,8.2623806451613));
#35184=CARTESIAN_POINT('Ctrl Pts',(-0.49619611955484,3.95528016940384,8.42127258064515));
#35185=CARTESIAN_POINT('Ctrl Pts',(-3.02400139141134,2.13545120331948,8.55094906828973));
#35186=CARTESIAN_POINT('Ctrl Pts',(-3.36770848062251,0.505916700748885,
8.62766157743967));
#35187=CARTESIAN_POINT('Ctrl Pts',(-3.36644585084492,0.000942668595410034,
8.65141010809498));
#35188=CARTESIAN_POINT('Ctrl Pts',(-3.36647579863201,0.00101859643942433,
7.84858989190502));
#35189=CARTESIAN_POINT('Ctrl Pts',(-3.36478428770786,-0.625167485996831,
7.87803961147051));
#35190=CARTESIAN_POINT('Ctrl Pts',(-2.8964828528491,-2.38038813746449,7.96047761976425));
#35191=CARTESIAN_POINT('Ctrl Pts',(-0.0672816548149041,-3.98633301836102,
8.09590391678625));
#35192=CARTESIAN_POINT('Ctrl Pts',(3.31538886833258,-2.21440159096907,8.25486878297098));
#35193=CARTESIAN_POINT('Ctrl Pts',(3.65656725922866,1.58899138861319,8.41383364915575));
#35194=CARTESIAN_POINT('Ctrl Pts',(0.643261156248369,3.93466553079316,8.57279851534047));
#35195=CARTESIAN_POINT('Ctrl Pts',(-2.64176562949924,2.78241271369441,8.71771726292358));
#35196=CARTESIAN_POINT('Ctrl Pts',(-3.36334120619684,0.822362489639698,
8.80964772177842));
#35197=CARTESIAN_POINT('Ctrl Pts',(-3.37066808100933,-0.0030696318858409,
8.84858989190502));
#35198=CARTESIAN_POINT('Origin',(0.,0.,-1.84858989190503));
#35199=CARTESIAN_POINT('',(-3.3748606436688,-0.00246557707590639,6.65141010809498));
#35200=CARTESIAN_POINT('',(-3.37441250761161,0.00263846066578283,6.84858989190502));
#35201=CARTESIAN_POINT('',(-3.37175,2.08693528006523E-13,-1.84858989190503));
#35202=CARTESIAN_POINT('Ctrl Pts',(-3.3748606436688,-0.00246557707590626,
6.65141010809497));
#35203=CARTESIAN_POINT('Ctrl Pts',(-3.37613613582624,-0.157769830059076,
6.65876050217084));
#35204=CARTESIAN_POINT('Ctrl Pts',(-3.29579272315184,-1.43080711580639,
6.71907487474133));
#35205=CARTESIAN_POINT('Ctrl Pts',(-1.67587337027072,-3.61689096522939,
6.83235322580646));
#35206=CARTESIAN_POINT('Ctrl Pts',(2.13246786040229,-3.36794189853266,6.99124516129032));
#35207=CARTESIAN_POINT('Ctrl Pts',(3.98615544163244,-0.0318842074478251,
7.15013709677419));
#35208=CARTESIAN_POINT('Ctrl Pts',(2.18607012156152,3.33339905069232,7.30902903225807));
#35209=CARTESIAN_POINT('Ctrl Pts',(-1.61780152532516,3.64323620318475,7.46792096774193));
#35210=CARTESIAN_POINT('Ctrl Pts',(-3.28487995770484,1.46716325720085,7.58204799302091));
#35211=CARTESIAN_POINT('Ctrl Pts',(-3.37585969097893,0.175947096268433,
7.64321103980526));
#35212=CARTESIAN_POINT('Ctrl Pts',(-3.37436653161969,0.00264543560195811,
7.65141010809498));
#35213=CARTESIAN_POINT('Ctrl Pts',(-3.37441250761161,0.00263846066578258,
6.84858989190502));
#35214=CARTESIAN_POINT('Ctrl Pts',(-3.36625911376211,-0.945381294583835,
6.89344321243435));
#35215=CARTESIAN_POINT('Ctrl Pts',(-2.45439078883877,-3.02709322103295,
6.99128482169193));
#35216=CARTESIAN_POINT('Ctrl Pts',(1.07677617223565,-3.83874078693202,7.14211471967776));
#35217=CARTESIAN_POINT('Ctrl Pts',(3.81057598656871,-1.17255635469506,7.3010795858625));
#35218=CARTESIAN_POINT('Ctrl Pts',(3.04860581952888,2.56931514444696,7.46004445204726));
#35219=CARTESIAN_POINT('Ctrl Pts',(-0.510113381387115,3.95413228059959,
7.619009318232));
#35220=CARTESIAN_POINT('Ctrl Pts',(-3.02827174132543,2.12695452322279,7.74852446485126));
#35221=CARTESIAN_POINT('Ctrl Pts',(-3.36782778932888,0.501516551178981,
7.82505132274226));
#35222=CARTESIAN_POINT('Ctrl Pts',(-3.36647579863201,0.00101859643942433,
7.84858989190502));
#35223=CARTESIAN_POINT('Origin',(0.,0.,-1.84858989190503));
#35224=CARTESIAN_POINT('',(-3.36661890683212,-0.00122158962200572,5.65141010809498));
#35225=CARTESIAN_POINT('',(-3.37491538366506,-0.00245188971244759,5.84858989190502));
#35226=CARTESIAN_POINT('',(-3.37175,2.08693528006523E-13,-1.84858989190503));
#35227=CARTESIAN_POINT('Ctrl Pts',(-3.36661890683212,-0.00122158962200539,
5.65141010809498));
#35228=CARTESIAN_POINT('Ctrl Pts',(-3.36820126338182,-0.488087448628749,
5.67430996453643));
#35229=CARTESIAN_POINT('Ctrl Pts',(-3.04142339082007,-2.09897775501084,
5.75017379947252));
#35230=CARTESIAN_POINT('Ctrl Pts',(-0.559403071098495,-3.94683670951677,
5.87900161290323));
#35231=CARTESIAN_POINT('Ctrl Pts',(3.01459581839321,-2.60819168376593,6.03789354838709));
#35232=CARTESIAN_POINT('Ctrl Pts',(3.82536866943663,1.12116294553142,6.19678548387097));
#35233=CARTESIAN_POINT('Ctrl Pts',(1.12974830864147,3.82284194895142,6.35567741935484));
#35234=CARTESIAN_POINT('Ctrl Pts',(-2.42881219485455,3.0575629803579,6.50721896076285));
#35235=CARTESIAN_POINT('Ctrl Pts',(-3.3669454531908,0.961290050298803,6.60579652367622));
#35236=CARTESIAN_POINT('Ctrl Pts',(-3.3748606436688,-0.00246557707590626,
6.65141010809497));
#35237=CARTESIAN_POINT('Ctrl Pts',(-3.37491538366506,-0.00245188971244781,
5.84858989190502));
#35238=CARTESIAN_POINT('Ctrl Pts',(-3.37617143803668,-0.156022125643285,
5.85585852466994));
#35239=CARTESIAN_POINT('Ctrl Pts',(-3.29681403413222,-1.42781289481916,
5.91611544616311));
#35240=CARTESIAN_POINT('Ctrl Pts',(-1.68004955900417,-3.61563427819245,
6.02936065638453));
#35241=CARTESIAN_POINT('Ctrl Pts',(2.13069369871068,-3.3697955600636,6.18832552256926));
#35242=CARTESIAN_POINT('Ctrl Pts',(3.98676787287831,-0.032552759256669,
6.34729038875402));
#35243=CARTESIAN_POINT('Ctrl Pts',(2.18543605335013,3.3345534950076,6.50625525493876));
#35244=CARTESIAN_POINT('Ctrl Pts',(-1.62078473268592,3.64258625218979,6.66522012112352));
#35245=CARTESIAN_POINT('Ctrl Pts',(-3.2856992999535,1.4649244081245,6.77933166677893));
#35246=CARTESIAN_POINT('Ctrl Pts',(-3.37589127437617,0.174579143538081,
6.8404549237061));
#35247=CARTESIAN_POINT('Ctrl Pts',(-3.37441250761161,0.00263846066578258,
6.84858989190502));
#35248=CARTESIAN_POINT('Origin',(0.,0.,-1.84858989190503));
#35249=CARTESIAN_POINT('',(-3.37037732776107,0.00303222645661923,4.65141010809497));
#35250=CARTESIAN_POINT('',(-3.36666513788771,-0.00130109466394523,4.84858989190502));
#35251=CARTESIAN_POINT('',(-3.37175,2.08693528006523E-13,-1.84858989190503));
#35252=CARTESIAN_POINT('Ctrl Pts',(-3.37037732776107,0.00303222645661912,
4.65141010809497));
#35253=CARTESIAN_POINT('Ctrl Pts',(-3.36327434274459,-0.812132332425157,
4.68985942690203));
#35254=CARTESIAN_POINT('Ctrl Pts',(-2.65651681547025,-2.76122659154967,
4.7812727242037));
#35255=CARTESIAN_POINT('Ctrl Pts',(0.604781303071069,-3.94013849796468,
4.92565));
#35256=CARTESIAN_POINT('Ctrl Pts',(3.63959495745868,-1.6259767381985,5.08454193548388));
#35257=CARTESIAN_POINT('Ctrl Pts',(3.3382985122726,2.17858092584818,5.24343387096774));
#35258=CARTESIAN_POINT('Ctrl Pts',(-0.0229349622598251,3.98621697792136,
5.40232580645161));
#35259=CARTESIAN_POINT('Ctrl Pts',(-2.88174731779988,2.40610117021057,5.53831788549402));
#35260=CARTESIAN_POINT('Ctrl Pts',(-3.36454150689018,0.637961221244742,
5.62134598604181));
#35261=CARTESIAN_POINT('Ctrl Pts',(-3.36661890683212,-0.00122158962200539,
5.65141010809498));
#35262=CARTESIAN_POINT('Ctrl Pts',(-3.36666513788771,-0.00130109466394548,
4.84858989190502));
#35263=CARTESIAN_POINT('Ctrl Pts',(-3.36833385037662,-0.483310565759833,
4.87126212563378));
#35264=CARTESIAN_POINT('Ctrl Pts',(-3.04595737613669,-2.0897168735396,4.94692264809078));
#35265=CARTESIAN_POINT('Ctrl Pts',(-0.574613628296617,-3.94527526701846,
5.07557145927603));
#35266=CARTESIAN_POINT('Ctrl Pts',(3.0062441927532,-2.61875420913902,5.2345363254608));
#35267=CARTESIAN_POINT('Ctrl Pts',(3.8292149534867,1.11017592945447,5.39350119164552));
#35268=CARTESIAN_POINT('Ctrl Pts',(1.13931660104628,3.82064594498541,5.55246605783029));
#35269=CARTESIAN_POINT('Ctrl Pts',(-2.42498889622798,3.06243800957472,5.7041622912501));
#35270=CARTESIAN_POINT('Ctrl Pts',(-3.36701480929308,0.963503961964746,
5.80287023594169));
#35271=CARTESIAN_POINT('Ctrl Pts',(-3.37491538366506,-0.00245188971244781,
5.84858989190502));
#35272=CARTESIAN_POINT('Origin',(0.,0.,-1.84858989190503));
#35273=CARTESIAN_POINT('',(-3.37724050405987,-0.000407706007126927,3.65141010809498));
#35274=CARTESIAN_POINT('',(-3.37013695473896,0.00300786229786701,3.84858989190502));
#35275=CARTESIAN_POINT('',(-3.37175,2.08693528006523E-13,-1.84858989190503));
#35276=CARTESIAN_POINT('Ctrl Pts',(-3.37724050405987,-0.000407706007126926,
3.65141010809498));
#35277=CARTESIAN_POINT('Ctrl Pts',(-3.37727770925144,-0.0222311044065494,
3.652444910773));
#35278=CARTESIAN_POINT('Ctrl Pts',(-3.36719553771294,-1.16099931030625,
3.70644369194564));
#35279=CARTESIAN_POINT('Ctrl Pts',(-2.09357261161725,-3.39225669930255,
3.8134064516129));
#35280=CARTESIAN_POINT('Ctrl Pts',(1.71738108280889,-3.59736765289132,3.97229838709678));
#35281=CARTESIAN_POINT('Ctrl Pts',(3.95415621068438,-0.505074716519562,
4.13119032258065));
#35282=CARTESIAN_POINT('Ctrl Pts',(2.56648943634972,3.05017766348832,4.29008225806451));
#35283=CARTESIAN_POINT('Ctrl Pts',(-1.17366200413909,3.8095891259482,4.44897419354839));
#35284=CARTESIAN_POINT('Ctrl Pts',(-3.19328501843251,1.73829700144105,4.56941681022521));
#35285=CARTESIAN_POINT('Ctrl Pts',(-3.37305871233378,0.310757734440618,
4.6368954484074));
#35286=CARTESIAN_POINT('Ctrl Pts',(-3.37037732776107,0.00303222645661912,
4.65141010809497));
#35287=CARTESIAN_POINT('Ctrl Pts',(-3.37013695473896,0.00300786229786694,
3.84858989190502));
#35288=CARTESIAN_POINT('Ctrl Pts',(-3.36320369751902,-0.804384073785939,
3.88666572659761));
#35289=CARTESIAN_POINT('Ctrl Pts',(-2.66732523950674,-2.7461115272218,3.97772985001845));
#35290=CARTESIAN_POINT('Ctrl Pts',(0.57892500607099,-3.94464492605495,4.12178226216755));
#35291=CARTESIAN_POINT('Ctrl Pts',(3.63013258458704,-1.64848875417016,4.2807471283523));
#35292=CARTESIAN_POINT('Ctrl Pts',(3.35110647594949,2.15996831943484,4.43971199453705));
#35293=CARTESIAN_POINT('Ctrl Pts',(-0.00217860669321579,3.9869001753454,
4.59867686072179));
#35294=CARTESIAN_POINT('Ctrl Pts',(-2.87549058156321,2.41739184906724,4.73496949317778));
#35295=CARTESIAN_POINT('Ctrl Pts',(-3.36443382798691,0.643215268868607,
4.81827383690552));
#35296=CARTESIAN_POINT('Ctrl Pts',(-3.36666513788771,-0.00130109466394548,
4.84858989190502));
#35297=CARTESIAN_POINT('Origin',(0.,0.,-1.84858989190503));
#35298=CARTESIAN_POINT('',(-3.36917031630593,-0.00279652979204336,2.65141010809498));
#35299=CARTESIAN_POINT('',(-3.37729882489346,-0.000194430141600699,2.84858989190502));
#35300=CARTESIAN_POINT('',(-3.37175,2.08693528006523E-13,-1.84858989190503));
#35301=CARTESIAN_POINT('Ctrl Pts',(-3.36917031630593,-0.00279652979204365,
2.65141010809498));
#35302=CARTESIAN_POINT('Ctrl Pts',(-3.37192195751912,-0.354718783760072,
2.66799437313859));
#35303=CARTESIAN_POINT('Ctrl Pts',(-3.15912528101716,-1.82730552094877,
2.73754261667682));
#35304=CARTESIAN_POINT('Ctrl Pts',(-1.02419029239979,-3.85246484135621,
2.86005483870968));
#35305=CARTESIAN_POINT('Ctrl Pts',(2.68349747959669,-2.94776072747231,3.01894677419354));
#35306=CARTESIAN_POINT('Ctrl Pts',(3.9314491981565,0.658907486316316,3.17783870967743));
#35307=CARTESIAN_POINT('Ctrl Pts',(1.57577260497388,3.66161063015511,3.33673064516129));
#35308=CARTESIAN_POINT('Ctrl Pts',(-2.19953367602677,3.310326581852,3.49458777796714));
#35309=CARTESIAN_POINT('Ctrl Pts',(-3.37537344768752,1.09474900016628,3.59948093227837));
#35310=CARTESIAN_POINT('Ctrl Pts',(-3.37724050405987,-0.000407706007126926,
3.65141010809498));
#35311=CARTESIAN_POINT('Ctrl Pts',(-3.37729882489346,-0.000194430141600942,
2.84858989190502));
#35312=CARTESIAN_POINT('Ctrl Pts',(-3.37730745906329,-0.0105519609168573,
2.8490810388332));
#35313=CARTESIAN_POINT('Ctrl Pts',(-3.3725690581147,-1.13834260190552,2.90256047448963));
#35314=CARTESIAN_POINT('Ctrl Pts',(-2.12700963248002,-3.37212213291773,
3.00902819887431));
#35315=CARTESIAN_POINT('Ctrl Pts',(1.68400001564517,-3.61379602896036,3.16799306505907));
#35316=CARTESIAN_POINT('Ctrl Pts',(3.95013122707835,-0.540223147458982,
3.32695793124381));
#35317=CARTESIAN_POINT('Ctrl Pts',(2.59246639543577,3.02894300530038,3.48592279742856));
#35318=CARTESIAN_POINT('Ctrl Pts',(-1.14349143614182,3.81939852540782,3.6448876636133));
#35319=CARTESIAN_POINT('Ctrl Pts',(-3.18684176799334,1.75591563149786,3.76577669510546));
#35320=CARTESIAN_POINT('Ctrl Pts',(-3.37285237464884,0.31922404594331,3.83367743786936));
#35321=CARTESIAN_POINT('Ctrl Pts',(-3.37013695473896,0.00300786229786694,
3.84858989190502));
#35322=CARTESIAN_POINT('Origin',(0.,0.,-1.84858989190503));
#35323=CARTESIAN_POINT('',(-3.36722314734446,0.00185482314707379,1.65141010809497));
#35324=CARTESIAN_POINT('',(-3.3695578818617,-0.00290129534754852,1.84858989190502));
#35325=CARTESIAN_POINT('',(-3.37175,2.08693528006523E-13,-1.84858989190503));
#35326=CARTESIAN_POINT('Ctrl Pts',(-3.36722314734446,0.00185482314707382,
1.65141010809497));
#35327=CARTESIAN_POINT('Ctrl Pts',(-3.36382382620938,-0.68102387856646,
1.68354383550418));
#35328=CARTESIAN_POINT('Ctrl Pts',(-2.83012682104856,-2.49433668358649,
1.768641541408));
#35329=CARTESIAN_POINT('Ctrl Pts',(0.13255069832671,-3.98407441119242,1.90670322580645));
#35330=CARTESIAN_POINT('Ctrl Pts',(3.42072557595435,-2.04672776701011,2.06559516129032));
#35331=CARTESIAN_POINT('Ctrl Pts',(3.57341090601276,1.76668952717683,2.2244870967742));
#35332=CARTESIAN_POINT('Ctrl Pts',(0.45065073371557,3.96072731387378,2.38337903225806));
#35333=CARTESIAN_POINT('Ctrl Pts',(-2.71613180302817,2.67422828685271,2.52568670269832));
#35334=CARTESIAN_POINT('Ctrl Pts',(-3.36313423821671,0.769190092631348,
2.61503039464396));
#35335=CARTESIAN_POINT('Ctrl Pts',(-3.36917031630593,-0.00279652979204365,
2.65141010809498));
#35336=CARTESIAN_POINT('Ctrl Pts',(-3.3695578818617,-0.00290129534754862,
1.84858989190502));
#35337=CARTESIAN_POINT('Ctrl Pts',(-3.37231432811694,-0.34009370411539,
1.86448463979704));
#35338=CARTESIAN_POINT('Ctrl Pts',(-3.1706964344189,-1.79816219768021,1.93336767641731));
#35339=CARTESIAN_POINT('Ctrl Pts',(-1.07258002819951,-3.83991470812214,
2.05523900176583));
#35340=CARTESIAN_POINT('Ctrl Pts',(2.6481020123777,-2.98042525524821,2.21420386795058));
#35341=CARTESIAN_POINT('Ctrl Pts',(3.9394520872816,0.613266379946328,2.37316873413532));
#35342=CARTESIAN_POINT('Ctrl Pts',(1.61680281711694,3.64435532093595,2.53213360032008));
#35343=CARTESIAN_POINT('Ctrl Pts',(-2.17732013669245,3.33312768965276,2.69060731957663));
#35344=CARTESIAN_POINT('Ctrl Pts',(-3.37637594578823,1.10688927659692,2.79609275010495));
#35345=CARTESIAN_POINT('Ctrl Pts',(-3.37729882489346,-0.000194430141600942,
2.84858989190502));
#35346=CARTESIAN_POINT('Origin',(0.,0.,-1.84858989190503));
#35347=CARTESIAN_POINT('',(-3.37589447807987,0.00214364281095937,0.651410108094974));
#35348=CARTESIAN_POINT('',(-3.36692593843476,0.00163208592380837,0.848589891905015));
#35349=CARTESIAN_POINT('',(-3.37175,2.08693528006523E-13,-1.84858989190503));
#35350=CARTESIAN_POINT('Ctrl Pts',(-3.37589447807987,0.0021436428109594,
0.651410108094974));
#35351=CARTESIAN_POINT('Ctrl Pts',(-3.36905382598057,-1.00443485423249,
0.699093297869767));
#35352=CARTESIAN_POINT('Ctrl Pts',(-2.35675364226999,-3.1417842761117,0.799740466139185));
#35353=CARTESIAN_POINT('Ctrl Pts',(1.27802196869812,-3.77566833700333,0.953351612903227));
#35354=CARTESIAN_POINT('Ctrl Pts',(3.86616524359544,-0.97122229991515,1.1122435483871));
#35355=CARTESIAN_POINT('Ctrl Pts',(2.91058978102209,2.72383605033175,1.27113548387097));
#35356=CARTESIAN_POINT('Ctrl Pts',(-0.71291441141164,3.92198718064885,1.43002741935484));
#35357=CARTESIAN_POINT('Ctrl Pts',(-3.08228566582866,2.00998594685298,1.55678562742951));
#35358=CARTESIAN_POINT('Ctrl Pts',(-3.36942671096663,0.444521639742584,
1.63057985700955));
#35359=CARTESIAN_POINT('Ctrl Pts',(-3.36722314734446,0.00185482314707382,
1.65141010809497));
#35360=CARTESIAN_POINT('Ctrl Pts',(-3.36692593843476,0.00163208592380858,
0.848589891905015));
#35361=CARTESIAN_POINT('Ctrl Pts',(-3.36407240691806,-0.663645509172373,
0.879888240760876));
#35362=CARTESIAN_POINT('Ctrl Pts',(-2.85117022634889,-2.45933226824664,
0.964174878344985));
#35363=CARTESIAN_POINT('Ctrl Pts',(0.0716483833591926,-3.98622915634864,
1.10144980465734));
#35364=CARTESIAN_POINT('Ctrl Pts',(3.39051798866077,-2.09756782602768,1.26041467084209));
#35365=CARTESIAN_POINT('Ctrl Pts',(3.59899177492058,1.71542482386315,1.41937953702684));
#35366=CARTESIAN_POINT('Ctrl Pts',(0.505790215469384,3.95468340129096,1.57834440321159));
#35367=CARTESIAN_POINT('Ctrl Pts',(-2.69572995999776,2.70483870003466,1.72141452150431));
#35368=CARTESIAN_POINT('Ctrl Pts',(-3.36312516884065,0.784003943368042,
1.81149635106879));
#35369=CARTESIAN_POINT('Ctrl Pts',(-3.3695578818617,-0.00290129534754862,
1.84858989190502));
#35370=CARTESIAN_POINT('Origin',(0.,0.,24.5));
#35371=CARTESIAN_POINT('',(-3.87097280197699,0.00213832761144025,24.1339652975667));
#35372=CARTESIAN_POINT('Ctrl Pts',(-0.624728334461281,3.3133687646595,24.62825));
#35373=CARTESIAN_POINT('Ctrl Pts',(-0.520138250042208,3.33634852849099,
24.625046902956));
#35374=CARTESIAN_POINT('Ctrl Pts',(-0.414648098080521,3.35389705620374,
24.6218539025135));
#35375=CARTESIAN_POINT('Ctrl Pts',(-0.308613703672553,3.36622114122732,
24.6186673709615));
#35376=CARTESIAN_POINT('Ctrl Pts',(-0.199986616426575,3.37884656778403,
24.6154029241484));
#35377=CARTESIAN_POINT('Ctrl Pts',(-0.0907876447210383,3.38598894312879,
24.6121452664408));
#35378=CARTESIAN_POINT('Ctrl Pts',(0.018614620750679,3.38781780937344,24.6088904974597));
#35379=CARTESIAN_POINT('Ctrl Pts',(0.0805633655032933,3.38885340006882,
24.6070474930945));
#35380=CARTESIAN_POINT('Ctrl Pts',(0.142577487054791,3.38818433590453,24.6052054149592));
#35381=CARTESIAN_POINT('Ctrl Pts',(0.204590631758452,3.38583417858992,24.6033635549037));
#35382=CARTESIAN_POINT('Ctrl Pts',(0.254638036250335,3.38393749564785,24.6018770907733));
#35383=CARTESIAN_POINT('Ctrl Pts',(0.304684819171919,3.38094577981049,24.600390768683));
#35384=CARTESIAN_POINT('Ctrl Pts',(0.354695913393206,3.3768690300029,24.5989042163964));
#35385=CARTESIAN_POINT('Ctrl Pts',(0.372494580510141,3.37541813767843,24.5983751607996));
#35386=CARTESIAN_POINT('Ctrl Pts',(0.39028796136771,3.37382978973891,24.5978460986132));
#35387=CARTESIAN_POINT('Ctrl Pts',(0.408061433233138,3.37210587416845,24.5973174010591));
#35388=CARTESIAN_POINT('Ctrl Pts',(0.519404457290808,3.36130629745725,24.5940053422263));
#35389=CARTESIAN_POINT('Ctrl Pts',(0.630100011901245,3.34518038635334,24.5907036020021));
#35390=CARTESIAN_POINT('Ctrl Pts',(0.739763436768937,3.32391000487198,24.5874081616821));
#35391=CARTESIAN_POINT('Ctrl Pts',(0.850257666159321,3.3024784800636,24.5840877552741));
#35392=CARTESIAN_POINT('Ctrl Pts',(0.95970493776685,3.27582407416606,24.5807737445874));
#35393=CARTESIAN_POINT('Ctrl Pts',(1.06770973553523,3.24407969544398,24.5774620188875));
#35394=CARTESIAN_POINT('Ctrl Pts',(1.1361584697924,3.22396149154746,24.5753631914553));
#35395=CARTESIAN_POINT('Ctrl Pts',(1.20402775637168,3.20179785912252,24.5732652817816));
#35396=CARTESIAN_POINT('Ctrl Pts',(1.27121405220256,3.17761217468148,24.5711672434934));
#35397=CARTESIAN_POINT('Ctrl Pts',(1.29774075436021,3.16806310757318,24.5703388894951));
#35398=CARTESIAN_POINT('Ctrl Pts',(1.32416095392457,3.15819874582631,24.5695105154476));
#35399=CARTESIAN_POINT('Ctrl Pts',(1.35046812449935,3.14802019412801,24.5686820569498));
#35400=CARTESIAN_POINT('Ctrl Pts',(1.36653976589062,3.14180188827438,24.5681759330454));
#35401=CARTESIAN_POINT('Ctrl Pts',(1.38256076287534,3.13546957145725,24.5676700437565));
#35402=CARTESIAN_POINT('Ctrl Pts',(1.39852700263983,3.12902498441374,24.5671644619047));
#35403=CARTESIAN_POINT('Ctrl Pts',(1.5038400459978,3.08651659892363,24.5638296526902));
#35404=CARTESIAN_POINT('Ctrl Pts',(1.60681042310701,3.03911282071154,24.5605069879339));
#35405=CARTESIAN_POINT('Ctrl Pts',(1.70704837153172,2.98697613057657,24.5571923886324));
#35406=CARTESIAN_POINT('Ctrl Pts',(1.80670371564138,2.935142469994,24.5538970544882));
#35407=CARTESIAN_POINT('Ctrl Pts',(1.90365915425284,2.87863046313165,24.5506096923149));
#35408=CARTESIAN_POINT('Ctrl Pts',(1.99751737945406,2.81755070396422,24.5473262938205));
#35409=CARTESIAN_POINT('Ctrl Pts',(2.09219867451912,2.7559353187613,24.5440141022572));
#35410=CARTESIAN_POINT('Ctrl Pts',(2.18372913512715,2.68967155408011,24.5407059441949));
#35411=CARTESIAN_POINT('Ctrl Pts',(2.271672791588,2.61882611527755,24.5373977049647));
#35412=CARTESIAN_POINT('Ctrl Pts',(2.31564461981842,2.58340339587627,24.5357435853496));
#35413=CARTESIAN_POINT('Ctrl Pts',(2.3587192214935,2.54683454512376,24.5340894454425));
#35414=CARTESIAN_POINT('Ctrl Pts',(2.40083835867941,2.50912376524234,24.5324347709098));
#35415=CARTESIAN_POINT('Ctrl Pts',(2.4199270309962,2.49203298969322,24.5316848614374));
#35416=CARTESIAN_POINT('Ctrl Pts',(2.43881941610424,2.47470762973993,24.5309348421549));
#35417=CARTESIAN_POINT('Ctrl Pts',(2.45750989027674,2.45714789797131,24.5301846651845));
#35418=CARTESIAN_POINT('Ctrl Pts',(2.47259728190695,2.4429732682819,24.5295791046386));
#35419=CARTESIAN_POINT('Ctrl Pts',(2.48755582869293,2.42864311414144,24.5289733271752));
#35420=CARTESIAN_POINT('Ctrl Pts',(2.50236326380812,2.41417672018039,24.528368102554));
#35421=CARTESIAN_POINT('Ctrl Pts',(2.5096874370137,2.40702123550619,24.5280687414615));
#35422=CARTESIAN_POINT('Ctrl Pts',(2.51697555679688,2.39983158202503,24.5277694793085));
#35423=CARTESIAN_POINT('Ctrl Pts',(2.52422733942721,2.39260786015533,24.5274703131481));
#35424=CARTESIAN_POINT('Ctrl Pts',(2.60073745914298,2.31639379621843,24.5243139528543));
#35425=CARTESIAN_POINT('Ctrl Pts',(2.67320522179129,2.23639118372509,24.5211682778273));
#35426=CARTESIAN_POINT('Ctrl Pts',(2.74161153441807,2.15302978874429,24.5180298269183));
#35427=CARTESIAN_POINT('Ctrl Pts',(2.81186762190031,2.06741421857952,24.5148065091695));
#35428=CARTESIAN_POINT('Ctrl Pts',(2.87784002551868,1.97825519814193,24.511590811516));
#35429=CARTESIAN_POINT('Ctrl Pts',(2.93947332195402,1.88597569204873,24.5083789843694));
#35430=CARTESIAN_POINT('Ctrl Pts',(3.00543439044467,1.78721649574186,24.5049416288708));
#35431=CARTESIAN_POINT('Ctrl Pts',(3.06642646008642,1.68488265861663,24.5015087065221));
#35432=CARTESIAN_POINT('Ctrl Pts',(3.12233208000985,1.57945276379857,24.4980756211074));
#35433=CARTESIAN_POINT('Ctrl Pts',(3.14679078872635,1.53332718481566,24.4965736462384));
#35434=CARTESIAN_POINT('Ctrl Pts',(3.1702752276744,1.48660856181708,24.4950716401576));
#35435=CARTESIAN_POINT('Ctrl Pts',(3.19277220676191,1.43933527974668,24.4935692179767));
#35436=CARTESIAN_POINT('Ctrl Pts',(3.20843753613705,1.40641745858516,24.4925230358101));
#35437=CARTESIAN_POINT('Ctrl Pts',(3.2236240268298,1.3732306769969,24.4914766518865));
#35438=CARTESIAN_POINT('Ctrl Pts',(3.23832660560595,1.33978769663366,24.4904299362547));
#35439=CARTESIAN_POINT('Ctrl Pts',(3.24466706730076,1.32536546913318,24.489978541947));
#35440=CARTESIAN_POINT('Ctrl Pts',(3.25091694288974,1.31089679039211,24.489527124135));
#35441=CARTESIAN_POINT('Ctrl Pts',(3.25707117071328,1.29639411279135,24.4890760252508));
#35442=CARTESIAN_POINT('Ctrl Pts',(3.30189883440903,1.19075597705509,24.4857902013176));
#35443=CARTESIAN_POINT('Ctrl Pts',(3.34172661274634,1.08315538243838,24.4825162404531));
#35444=CARTESIAN_POINT('Ctrl Pts',(3.37649898345667,0.974036565393082,24.4792502460069));
#35445=CARTESIAN_POINT('Ctrl Pts',(3.41163056334322,0.863790517745426,24.4759505128437));
#35446=CARTESIAN_POINT('Ctrl Pts',(3.44160210056879,0.751993878752548,24.47265891154));
#35447=CARTESIAN_POINT('Ctrl Pts',(3.46631080319639,0.639077130310462,24.4693714234329));
#35448=CARTESIAN_POINT('Ctrl Pts',(3.4909156460234,0.526635012655473,24.4660977538522));
#35449=CARTESIAN_POINT('Ctrl Pts',(3.51030206328578,0.41308129028903,24.4628281629622));
#35450=CARTESIAN_POINT('Ctrl Pts',(3.5243192195213,0.298826837120347,24.4595586825629));
#35451=CARTESIAN_POINT('Ctrl Pts',(3.5361116521245,0.202706203521802,24.4568081155714));
#35452=CARTESIAN_POINT('Ctrl Pts',(3.54410317841348,0.106089103613188,24.4540576267811));
#35453=CARTESIAN_POINT('Ctrl Pts',(3.54817462918724,0.00921931232785102,
24.451304853408));
#35454=CARTESIAN_POINT('Ctrl Pts',(3.54887956636703,-0.00755287067786807,
24.4508282340391));
#35455=CARTESIAN_POINT('Ctrl Pts',(3.54946687335721,-0.0243333324170402,
24.4503515260614));
#35456=CARTESIAN_POINT('Ctrl Pts',(3.5499355914206,-0.0411046474494315,
24.4498751757144));
#35457=CARTESIAN_POINT('Ctrl Pts',(3.55318741783251,-0.157459039234995,
24.4465703987905));
#35458=CARTESIAN_POINT('Ctrl Pts',(3.55074422185484,-0.273556149324447,
24.4432776009626));
#35459=CARTESIAN_POINT('Ctrl Pts',(3.54250561679224,-0.388968852721143,
24.4399928190226));
#35460=CARTESIAN_POINT('Ctrl Pts',(3.53438980253945,-0.502661408204027,
24.4367569945253));
#35461=CARTESIAN_POINT('Ctrl Pts',(3.52065018301948,-0.615690678667281,
24.4335289487538));
#35462=CARTESIAN_POINT('Ctrl Pts',(3.50114108221864,-0.727654569046081,
24.430304893079));
#35463=CARTESIAN_POINT('Ctrl Pts',(3.49384800416623,-0.769509977961124,
24.42909964585));
#35464=CARTESIAN_POINT('Ctrl Pts',(3.48574813528587,-0.811216498584334,
24.427894956231));
#35465=CARTESIAN_POINT('Ctrl Pts',(3.47683197850714,-0.852752977896645,
24.4266906262961));
#35466=CARTESIAN_POINT('Ctrl Pts',(3.4529871352566,-0.963835685722627,24.4234698374258));
#35467=CARTESIAN_POINT('Ctrl Pts',(3.42330774908946,-1.07370337125384,24.4202516210517));
#35468=CARTESIAN_POINT('Ctrl Pts',(3.38809113649622,-1.1820724034292,24.4170321914123));
#35469=CARTESIAN_POINT('Ctrl Pts',(3.37495661955853,-1.22249011495268,24.4158314611315));
#35470=CARTESIAN_POINT('Ctrl Pts',(3.36105136220375,-1.26269920199182,24.4146305620831));
#35471=CARTESIAN_POINT('Ctrl Pts',(3.34638908048464,-1.30268427759558,24.4134292978622));
#35472=CARTESIAN_POINT('Ctrl Pts',(3.33893812623189,-1.32300355496479,24.4128188495754));
#35473=CARTESIAN_POINT('Ctrl Pts',(3.33129166525305,-1.3432649771586,24.412208306987));
#35474=CARTESIAN_POINT('Ctrl Pts',(3.32345141301749,-1.36346647925837,24.411597644323));
#35475=CARTESIAN_POINT('Ctrl Pts',(3.31733644758331,-1.37922253956704,24.4111213610389));
#35476=CARTESIAN_POINT('Ctrl Pts',(3.31110676245958,-1.39493393196613,24.4106452528772));
#35477=CARTESIAN_POINT('Ctrl Pts',(3.30476515852903,-1.41059588192003,24.4101694268982));
#35478=CARTESIAN_POINT('Ctrl Pts',(3.26241982156158,-1.51517676644526,24.4069921531923));
#35479=CARTESIAN_POINT('Ctrl Pts',(3.21506671129281,-1.61761018296196,24.4038257550006));
#35480=CARTESIAN_POINT('Ctrl Pts',(3.16305493267433,-1.71764249367417,24.4006667076014));
#35481=CARTESIAN_POINT('Ctrl Pts',(3.10936292149889,-1.82090633289145,24.3974056076588));
#35482=CARTESIAN_POINT('Ctrl Pts',(3.05070610897566,-1.92161214375833,24.3941523411125));
#35483=CARTESIAN_POINT('Ctrl Pts',(2.98741482167415,-2.01946701686137,24.3909030304897));
#35484=CARTESIAN_POINT('Ctrl Pts',(2.92378476042904,-2.11784566950304,24.3876363275557));
#35485=CARTESIAN_POINT('Ctrl Pts',(2.85546994313465,-2.2133435033276,24.3843736230076));
#35486=CARTESIAN_POINT('Ctrl Pts',(2.78275913579883,-2.30563818528626,24.3811109767752));
#35487=CARTESIAN_POINT('Ctrl Pts',(2.73115118701869,-2.37114618050358,24.3787952484011));
#35488=CARTESIAN_POINT('Ctrl Pts',(2.67732765960473,-2.4350400215934,24.3764795494049));
#35489=CARTESIAN_POINT('Ctrl Pts',(2.62137984513178,-2.49719390809692,24.3741624709621));
#35490=CARTESIAN_POINT('Ctrl Pts',(2.60733587761121,-2.51279571795411,24.3735808401209));
#35491=CARTESIAN_POINT('Ctrl Pts',(2.59315801395097,-2.52828784255011,24.3729991223601));
#35492=CARTESIAN_POINT('Ctrl Pts',(2.5788476135988,-2.54366818796195,24.3724172953964));
#35493=CARTESIAN_POINT('Ctrl Pts',(2.56780240058981,-2.55553921791534,24.3719682232117));
#35494=CARTESIAN_POINT('Ctrl Pts',(2.55668178857907,-2.56733978704972,24.3715192315499));
#35495=CARTESIAN_POINT('Ctrl Pts',(2.54549189058683,-2.5790635828598,24.3710705218887));
#35496=CARTESIAN_POINT('Ctrl Pts',(2.46377857881438,-2.6646756396319,24.367793856412));
#35497=CARTESIAN_POINT('Ctrl Pts',(2.37828958660479,-2.74628708545935,24.3645287774285));
#35498=CARTESIAN_POINT('Ctrl Pts',(2.28935576945552,-2.82360475294287,24.3612714210233));
#35499=CARTESIAN_POINT('Ctrl Pts',(2.2004312170102,-2.9009143658379,24.358014403954));
#35500=CARTESIAN_POINT('Ctrl Pts',(2.10806196086699,-2.97393178300944,24.354765107854));
#35501=CARTESIAN_POINT('Ctrl Pts',(2.01253765634337,-3.04233309530011,24.3515196700154));
#35502=CARTESIAN_POINT('Ctrl Pts',(1.91831994223422,-3.10979880801304,24.3483186235807));
#35503=CARTESIAN_POINT('Ctrl Pts',(1.82103227216761,-3.17277441103138,24.345121330582));
#35504=CARTESIAN_POINT('Ctrl Pts',(1.72092180235263,-3.23090982550694,24.3419240846569));
#35505=CARTESIAN_POINT('Ctrl Pts',(1.63731823238491,-3.27945947471638,24.3392540225356));
#35506=CARTESIAN_POINT('Ctrl Pts',(1.55174530961941,-3.32463302100756,24.3365839932441));
#35507=CARTESIAN_POINT('Ctrl Pts',(1.46433480530475,-3.3662006160568,24.3339118381243));
#35508=CARTESIAN_POINT('Ctrl Pts',(1.44360953039847,-3.37605640903435,24.3332782626761));
#35509=CARTESIAN_POINT('Ctrl Pts',(1.42277595537401,-3.38571149112601,24.3326444189594));
#35510=CARTESIAN_POINT('Ctrl Pts',(1.40186473452666,-3.39514984035219,24.3320111514667));
#35511=CARTESIAN_POINT('Ctrl Pts',(1.33458120918284,-3.42551848377093,24.3299735626666));
#35512=CARTESIAN_POINT('Ctrl Pts',(1.2664465713012,-3.45366766831798,24.3279404681835));
#35513=CARTESIAN_POINT('Ctrl Pts',(1.19753254997869,-3.47952152342011,24.3259109394442));
#35514=CARTESIAN_POINT('Ctrl Pts',(1.09102290473056,-3.51947979145293,24.3227742136821));
#35515=CARTESIAN_POINT('Ctrl Pts',(0.982652679880705,-3.55395790982246,
24.3196460054332));
#35516=CARTESIAN_POINT('Ctrl Pts',(0.872822247400536,-3.58310705179026,
24.3165228865437));
#35517=CARTESIAN_POINT('Ctrl Pts',(0.760371906501168,-3.61295152091583,
24.3133252683986));
#35518=CARTESIAN_POINT('Ctrl Pts',(0.646390155341705,-3.6372098459968,24.3101329853132));
#35519=CARTESIAN_POINT('Ctrl Pts',(0.53128616178814,-3.6559936831665,24.3069423579087));
#35520=CARTESIAN_POINT('Ctrl Pts',(0.41453738712084,-3.67504593240137,24.3037061379619));
#35521=CARTESIAN_POINT('Ctrl Pts',(0.296633230443278,-3.68846615738096,
24.3004716213517));
#35522=CARTESIAN_POINT('Ctrl Pts',(0.177991630975357,-3.69631848981734,
24.2972349687049));
#35523=CARTESIAN_POINT('Ctrl Pts',(0.142360760405031,-3.69867673045107,
24.2962629255763));
#35524=CARTESIAN_POINT('Ctrl Pts',(0.1066633636693,-3.70053242315808,24.2952906897893));
#35525=CARTESIAN_POINT('Ctrl Pts',(0.0709107847277581,-3.70188639298558,
24.2943181573453));
#35526=CARTESIAN_POINT('Ctrl Pts',(0.0511417931589634,-3.70263505556873,
24.2937804063283));
#35527=CARTESIAN_POINT('Ctrl Pts',(0.0313540742527653,-3.70323026849973,
24.2932425143369));
#35528=CARTESIAN_POINT('Ctrl Pts',(0.0115717980804544,-3.70367187863094,
24.2927050676203));
#35529=CARTESIAN_POINT('Ctrl Pts',(-0.107433551546183,-3.70632849749549,
24.2894719192276));
#35530=CARTESIAN_POINT('Ctrl Pts',(-0.226418918411982,-3.7034386910525,
24.2862500321799));
#35531=CARTESIAN_POINT('Ctrl Pts',(-0.344959013740293,-3.6951464558983,
24.2830356970017));
#35532=CARTESIAN_POINT('Ctrl Pts',(-0.464907323931171,-3.68675571189142,
24.2797831766461));
#35533=CARTESIAN_POINT('Ctrl Pts',(-0.584400592051045,-3.67283340149898,
24.2765383886529));
#35534=CARTESIAN_POINT('Ctrl Pts',(-0.703006950795025,-3.65347561626452,
24.2732974897681));
#35535=CARTESIAN_POINT('Ctrl Pts',(-0.821420460393264,-3.63414930600648,
24.2700618604539));
#35536=CARTESIAN_POINT('Ctrl Pts',(-0.938950841911184,-3.6094050645999,
24.2668301076113));
#35537=CARTESIAN_POINT('Ctrl Pts',(-1.05516365811085,-3.57928709699041,
24.2635984067028));
#35538=CARTESIAN_POINT('Ctrl Pts',(-1.11307514573956,-3.56427862920126,
24.261987976689));
#35539=CARTESIAN_POINT('Ctrl Pts',(-1.17065929149193,-3.5479349386455,24.2603775595719));
#35540=CARTESIAN_POINT('Ctrl Pts',(-1.22786083460473,-3.53025684653982,
24.258766682079));
#35541=CARTESIAN_POINT('Ctrl Pts',(-1.27025654792723,-3.5171544845367,24.2575727579877));
#35542=CARTESIAN_POINT('Ctrl Pts',(-1.31244206756123,-3.50331904033182,
24.256378581001));
#35543=CARTESIAN_POINT('Ctrl Pts',(-1.35439435742328,-3.48874976896511,
24.2551839584315));
#35544=CARTESIAN_POINT('Ctrl Pts',(-1.37450122726203,-3.48176701679641,
24.2546114003997));
#35545=CARTESIAN_POINT('Ctrl Pts',(-1.39455787836581,-3.47461436152618,
24.2540386428268));
#35546=CARTESIAN_POINT('Ctrl Pts',(-1.4145370881139,-3.46730094250551,24.2534663728415));
#35547=CARTESIAN_POINT('Ctrl Pts',(-1.52840519986039,-3.42561935325375,
24.2502048172814));
#35548=CARTESIAN_POINT('Ctrl Pts',(-1.63991365982444,-3.37866812586214,
24.2469546926609));
#35549=CARTESIAN_POINT('Ctrl Pts',(-1.74863318528068,-3.32654324532194,
24.2437121916767));
#35550=CARTESIAN_POINT('Ctrl Pts',(-1.85558872732241,-3.27526409533814,
24.2405223005429));
#35551=CARTESIAN_POINT('Ctrl Pts',(-1.95984592910298,-3.2189775652086,24.2373397876639));
#35552=CARTESIAN_POINT('Ctrl Pts',(-2.06098377301333,-3.15772709883281,
24.2341610280672));
#35553=CARTESIAN_POINT('Ctrl Pts',(-2.15682437201784,-3.09968471667599,
24.2311487607293));
#35554=CARTESIAN_POINT('Ctrl Pts',(-2.24986433245661,-3.03718433413316,
24.2281398638026));
#35555=CARTESIAN_POINT('Ctrl Pts',(-2.33972491633012,-2.97022484402709,
24.2251312525923));
#35556=CARTESIAN_POINT('Ctrl Pts',(-2.39708388099203,-2.9274838906389,24.2232108241167));
#35557=CARTESIAN_POINT('Ctrl Pts',(-2.45314695486067,-2.88292530873872,
24.2212905120536));
#35558=CARTESIAN_POINT('Ctrl Pts',(-2.50788173230019,-2.8366336564438,24.2193695141552));
#35559=CARTESIAN_POINT('Ctrl Pts',(-2.53563831690701,-2.81315866990653,
24.2183953558013));
#35560=CARTESIAN_POINT('Ctrl Pts',(-2.56305323963533,-2.78923792330051,
24.2174210210771));
#35561=CARTESIAN_POINT('Ctrl Pts',(-2.59012178635459,-2.76488197889541,
24.2164464053624));
#35562=CARTESIAN_POINT('Ctrl Pts',(-2.60345465688749,-2.75288522647173,
24.2159663491083));
#35563=CARTESIAN_POINT('Ctrl Pts',(-2.61670472847459,-2.74078173073675,
24.2154861793416));
#35564=CARTESIAN_POINT('Ctrl Pts',(-2.62986751863965,-2.72857633888938,
24.2150060254729));
#35565=CARTESIAN_POINT('Ctrl Pts',(-2.71508215755265,-2.6495598047031,24.2118975554583));
#35566=CARTESIAN_POINT('Ctrl Pts',(-2.79636860051037,-2.56653035928709,
24.2087997059384));
#35567=CARTESIAN_POINT('Ctrl Pts',(-2.87364584295152,-2.47991615691849,
24.2057091871955));
#35568=CARTESIAN_POINT('Ctrl Pts',(-2.95372207710542,-2.39016477694134,
24.2025067294641));
#35569=CARTESIAN_POINT('Ctrl Pts',(-3.02949395217132,-2.29656378485085,
24.1993121431703));
#35570=CARTESIAN_POINT('Ctrl Pts',(-3.10083927390671,-2.19954365518354,
24.1961217680305));
#35571=CARTESIAN_POINT('Ctrl Pts',(-3.1729388167544,-2.1014978853154,24.1928976661062));
#35572=CARTESIAN_POINT('Ctrl Pts',(-3.24051817780072,-1.99995957525359,
24.1896778648424));
#35573=CARTESIAN_POINT('Ctrl Pts',(-3.30341172612255,-1.89533643715524,
24.1864585866407));
#35574=CARTESIAN_POINT('Ctrl Pts',(-3.34638934220069,-1.82384336382643,
24.1842587282087));
#35575=CARTESIAN_POINT('Ctrl Pts',(-3.38717808530971,-1.7509090628703,24.1820591140217));
#35576=CARTESIAN_POINT('Ctrl Pts',(-3.42571297641979,-1.67665668248674,
24.1798585386985));
#35577=CARTESIAN_POINT('Ctrl Pts',(-3.445014281687,-1.63946524845605,24.1787563174426));
#35578=CARTESIAN_POINT('Ctrl Pts',(-3.46374997985981,-1.60194306216562,
24.1776538550573));
#35579=CARTESIAN_POINT('Ctrl Pts',(-3.48191088985649,-1.56410523444394,
24.1765510000744));
#35580=CARTESIAN_POINT('Ctrl Pts',(-3.49096642636183,-1.54523823767566,
24.1760010858047));
#35581=CARTESIAN_POINT('Ctrl Pts',(-3.4998801459806,-1.52629016625364,24.1754509999921));
#35582=CARTESIAN_POINT('Ctrl Pts',(-3.50864077925426,-1.5072853111527,24.174901369431));
#35583=CARTESIAN_POINT('Ctrl Pts',(-3.56003841051657,-1.39578600463474,
24.171676749928));
#35584=CARTESIAN_POINT('Ctrl Pts',(-3.60624692934267,-1.28217850112835,
24.1684632179365));
#35585=CARTESIAN_POINT('Ctrl Pts',(-3.6471387300781,-1.1668916502069,24.1652570948759));
#35586=CARTESIAN_POINT('Ctrl Pts',(-3.6882879122029,-1.05087916017607,24.1620307918185));
#35587=CARTESIAN_POINT('Ctrl Pts',(-3.72405366249247,-0.933165324275529,
24.1588119912523));
#35588=CARTESIAN_POINT('Ctrl Pts',(-3.75426180619985,-0.814159485558989,
24.1555969446976));
#35589=CARTESIAN_POINT('Ctrl Pts',(-3.7841716362032,-0.696328862138458,
24.1524136476093));
#35590=CARTESIAN_POINT('Ctrl Pts',(-3.80863339059432,-0.577230809008665,
24.1492340307549));
#35591=CARTESIAN_POINT('Ctrl Pts',(-3.8274295805391,-0.457247749762826,
24.1460544556133));
#35592=CARTESIAN_POINT('Ctrl Pts',(-3.83933667583213,-0.381240339527709,
24.1440402439932));
#35593=CARTESIAN_POINT('Ctrl Pts',(-3.84896918346273,-0.304877515113294,
24.1420260491124));
#35594=CARTESIAN_POINT('Ctrl Pts',(-3.85626072121049,-0.2282555949368,24.14001094599));
#35595=CARTESIAN_POINT('Ctrl Pts',(-3.85942265273046,-0.195028959773208,
24.1391371086324));
#35596=CARTESIAN_POINT('Ctrl Pts',(-3.86214425712046,-0.161753603333563,
24.1382631004825));
#35597=CARTESIAN_POINT('Ctrl Pts',(-3.86441958153066,-0.128437410079632,
24.1373888461123));
#35598=CARTESIAN_POINT('Ctrl Pts',(-3.86591347492261,-0.106563236566722,
24.1368148432051));
#35599=CARTESIAN_POINT('Ctrl Pts',(-3.86721509040623,-0.0846675012688186,
24.1362406305225));
#35600=CARTESIAN_POINT('Ctrl Pts',(-3.86832155925171,-0.0627797067798542,
24.1356669009074));
#35601=CARTESIAN_POINT('Ctrl Pts',(-3.86941608558997,-0.0411281549512009,
24.1350993637576));
#35602=CARTESIAN_POINT('Ctrl Pts',(-3.87032006240666,-0.0194794249965481,
24.1345321693282));
#35603=CARTESIAN_POINT('Ctrl Pts',(-3.87103266938659,0.00216425178203038,
24.1339652975667));
#35604=CARTESIAN_POINT('',(0.349572399382967,3.92005776261121,24.058));
#35605=CARTESIAN_POINT('Ctrl Pts',(0.349418900843753,3.91916189049795,24.058));
#35606=CARTESIAN_POINT('Ctrl Pts',(0.226012228632792,3.91828850060595,24.0696807256992));
#35607=CARTESIAN_POINT('Ctrl Pts',(0.102952431902507,3.91191927543051,24.0813859465783));
#35608=CARTESIAN_POINT('Ctrl Pts',(-0.0193397180673949,3.90006603014558,
24.0931306202039));
#35609=CARTESIAN_POINT('Ctrl Pts',(-0.140580622517234,3.88831467750876,
24.1047743344831));
#35610=CARTESIAN_POINT('Ctrl Pts',(-0.261067870571708,3.87117297838718,
24.1164568261384));
#35611=CARTESIAN_POINT('Ctrl Pts',(-0.380377476123202,3.84860347157658,
24.1281926703091));
#35612=CARTESIAN_POINT('Ctrl Pts',(-0.496161715673067,3.82670084964599,
24.1395817431879));
#35613=CARTESIAN_POINT('Ctrl Pts',(-0.610837511562959,3.79968611836398,
24.1510210622381));
#35614=CARTESIAN_POINT('Ctrl Pts',(-0.723993462162786,3.76748283972913,
24.1625239483983));
#35615=CARTESIAN_POINT('Ctrl Pts',(-0.796757989013667,3.74677463728383,
24.1699208379514));
#35616=CARTESIAN_POINT('Ctrl Pts',(-0.868893538246561,3.72392009045816,
24.177344013056));
#35617=CARTESIAN_POINT('Ctrl Pts',(-0.940283456718533,3.69889010045098,
24.1847970158196));
#35618=CARTESIAN_POINT('Ctrl Pts',(-0.958852956027486,3.69237945592175,
24.1867356443071));
#35619=CARTESIAN_POINT('Ctrl Pts',(-0.977371972215163,3.6857215872702,24.188676290909));
#35620=CARTESIAN_POINT('Ctrl Pts',(-0.995838377017294,3.67891590798256,
24.1906190179632));
#35621=CARTESIAN_POINT('Ctrl Pts',(-1.01171569758055,3.67306441967942,24.1922893647652));
#35622=CARTESIAN_POINT('Ctrl Pts',(-1.0275456693922,3.66710676559807,24.1939603606721));
#35623=CARTESIAN_POINT('Ctrl Pts',(-1.04332469128769,3.6610438482036,24.1956317888384));
#35624=CARTESIAN_POINT('Ctrl Pts',(-1.15165978098886,3.619417269311,24.2071074253844));
#35625=CARTESIAN_POINT('Ctrl Pts',(-1.25763328276278,3.57281828211811,24.2186074516257));
#35626=CARTESIAN_POINT('Ctrl Pts',(-1.36087067794145,3.52121736057027,24.2301462409952));
#35627=CARTESIAN_POINT('Ctrl Pts',(-1.42681061365643,3.48825874665126,24.2375163129341));
#35628=CARTESIAN_POINT('Ctrl Pts',(-1.49163388388109,3.45325861360399,24.2449021988746));
#35629=CARTESIAN_POINT('Ctrl Pts',(-1.55523660610354,3.41620000588947,24.2523076441887));
#35630=CARTESIAN_POINT('Ctrl Pts',(-1.65681419035516,3.35701505726094,24.2641346103786));
#35631=CARTESIAN_POINT('Ctrl Pts',(-1.75528075449242,3.2925810923405,24.276011464936));
#35632=CARTESIAN_POINT('Ctrl Pts',(-1.8504118158475,3.22325698482629,24.2879534645915));
#35633=CARTESIAN_POINT('Ctrl Pts',(-1.94589009699015,3.15367985057672,24.2999390514679));
#35634=CARTESIAN_POINT('Ctrl Pts',(-2.03800893445419,3.07917596454707,24.3119902598576));
#35635=CARTESIAN_POINT('Ctrl Pts',(-2.12649675572721,3.00008130698686,24.3241225141588));
#35636=CARTESIAN_POINT('Ctrl Pts',(-2.15464819134299,2.97491820399908,24.3279822585951));
#35637=CARTESIAN_POINT('Ctrl Pts',(-2.18243175770649,2.94929030687597,24.3318502058895));
#35638=CARTESIAN_POINT('Ctrl Pts',(-2.20983765373967,2.92320808164845,24.3357268527022));
#35639=CARTESIAN_POINT('Ctrl Pts',(-2.22035441337321,2.91319926846847,24.3372144801333));
#35640=CARTESIAN_POINT('Ctrl Pts',(-2.23081386252428,2.90312511161636,24.3387031532638));
#35641=CARTESIAN_POINT('Ctrl Pts',(-2.24120927897093,2.89299245114185,24.3401919995702));
#35642=CARTESIAN_POINT('Ctrl Pts',(-2.32385350748897,2.81243714948096,24.3520284233442));
#35643=CARTESIAN_POINT('Ctrl Pts',(-2.40257000364209,2.72807711715171,24.3638921677319));
#35644=CARTESIAN_POINT('Ctrl Pts',(-2.47717616028223,2.64027648475023,24.3757991858546));
#35645=CARTESIAN_POINT('Ctrl Pts',(-2.55187618325755,2.55236538527792,24.3877211848877));
#35646=CARTESIAN_POINT('Ctrl Pts',(-2.62245590857137,2.46100416174114,24.3996865666148));
#35647=CARTESIAN_POINT('Ctrl Pts',(-2.68868744355177,2.36653097722017,24.4117113444476));
#35648=CARTESIAN_POINT('Ctrl Pts',(-2.75414075468922,2.27316785733437,24.4235948305405));
#35649=CARTESIAN_POINT('Ctrl Pts',(-2.81534772258566,2.17676464445494,24.4355363251252));
#35650=CARTESIAN_POINT('Ctrl Pts',(-2.8720401475082,2.07763370148774,24.4475512837449));
#35651=CARTESIAN_POINT('Ctrl Pts',(-2.90668546327039,2.01705377699881,24.4548937467957));
#35652=CARTESIAN_POINT('Ctrl Pts',(-2.93964383947717,1.95545494636204,24.462263645402));
#35653=CARTESIAN_POINT('Ctrl Pts',(-2.97084438937695,1.89290785453322,24.4696645068668));
#35654=CARTESIAN_POINT('Ctrl Pts',(-2.98845779797902,1.85759862156167,24.4738424587748));
#35655=CARTESIAN_POINT('Ctrl Pts',(-3.00551087593063,1.82198719162217,24.4780302780973));
#35656=CARTESIAN_POINT('Ctrl Pts',(-3.02198977071177,1.78608635326393,24.4822285994141));
#35657=CARTESIAN_POINT('Ctrl Pts',(-3.02877383007556,1.77130663521446,24.4839569714572));
#35658=CARTESIAN_POINT('Ctrl Pts',(-3.03545687173813,1.75648588102819,24.4856861859929));
#35659=CARTESIAN_POINT('Ctrl Pts',(-3.04203688563128,1.74162824455868,24.4874159221199));
#35660=CARTESIAN_POINT('Ctrl Pts',(-3.08710741956134,1.63985921800425,24.4992639412984));
#35661=CARTESIAN_POINT('Ctrl Pts',(-3.12737033179139,1.53631268431983,24.5111420689289));
#35662=CARTESIAN_POINT('Ctrl Pts',(-3.16262066493997,1.43129464400087,24.5230664886917));
#35663=CARTESIAN_POINT('Ctrl Pts',(-3.19738804194613,1.32771543001649,24.534827534913));
#35664=CARTESIAN_POINT('Ctrl Pts',(-3.22727942618041,1.22270400117247,24.5466336134818));
#35665=CARTESIAN_POINT('Ctrl Pts',(-3.2520488351859,1.1165476391786,24.5585002519648));
#35666=CARTESIAN_POINT('Ctrl Pts',(-3.27606482816892,1.01362025628536,24.5700059405533));
#35667=CARTESIAN_POINT('Ctrl Pts',(-3.29526569753493,0.909615922196257,
24.5815685609605));
#35668=CARTESIAN_POINT('Ctrl Pts',(-3.3093795070715,0.804800410213191,24.5932022664991));
#35669=CARTESIAN_POINT('Ctrl Pts',(-3.32346107752391,0.700224320202117,
24.6048093980635));
#35670=CARTESIAN_POINT('Ctrl Pts',(-3.33247901104835,0.594840172393064,
24.6164872903817));
#35671=CARTESIAN_POINT('Ctrl Pts',(-3.33611311329483,0.488924695430968,
24.62825));
#35672=CARTESIAN_POINT('',(-2.87185821835411,2.69480181882395,24.058));
#35673=CARTESIAN_POINT('Origin',(0.,0.,24.058));
#35674=CARTESIAN_POINT('Ctrl Pts',(-3.87103266938659,0.00216425178203038,
24.1339652975667));
#35675=CARTESIAN_POINT('Ctrl Pts',(-3.87507260628243,0.124867355795072,
24.1307515679672));
#35676=CARTESIAN_POINT('Ctrl Pts',(-3.87296594485587,0.247407050622043,
24.1275482085216));
#35677=CARTESIAN_POINT('Ctrl Pts',(-3.86453408452217,0.369385378863034,
24.1243515657403));
#35678=CARTESIAN_POINT('Ctrl Pts',(-3.85627040623579,0.488930725038259,
24.1212186832571));
#35679=CARTESIAN_POINT('Ctrl Pts',(-3.84193179212873,0.607937675272044,
24.1180922521689));
#35680=CARTESIAN_POINT('Ctrl Pts',(-3.82181791447054,0.726086832854309,
24.1149688332722));
#35681=CARTESIAN_POINT('Ctrl Pts',(-3.80134858411548,0.846323923823187,
24.1117902172779));
#35682=CARTESIAN_POINT('Ctrl Pts',(-3.77489779988944,0.965673358591756,
24.1086147208788));
#35683=CARTESIAN_POINT('Ctrl Pts',(-3.74272692791689,1.08379247292844,24.1054387192973));
#35684=CARTESIAN_POINT('Ctrl Pts',(-3.72259049299425,1.15772574589009,24.1034507921682));
#35685=CARTESIAN_POINT('Ctrl Pts',(-3.70021198877918,1.23117684933353,24.1014626671201));
#35686=CARTESIAN_POINT('Ctrl Pts',(-3.67564568396927,1.30405861901184,24.099473455278));
#35687=CARTESIAN_POINT('Ctrl Pts',(-3.66863540268018,1.32485628110409,24.0989058105034));
#35688=CARTESIAN_POINT('Ctrl Pts',(-3.66144692163609,1.3456075617141,24.0983380772297));
#35689=CARTESIAN_POINT('Ctrl Pts',(-3.65408139767167,1.36631038395308,24.097770234802));
#35690=CARTESIAN_POINT('Ctrl Pts',(-3.64822216373193,1.38277936556212,24.0973185192633));
#35691=CARTESIAN_POINT('Ctrl Pts',(-3.64225062386782,1.39921823302553,24.0968667189574));
#35692=CARTESIAN_POINT('Ctrl Pts',(-3.63617302699739,1.41561112341376,24.0964152327823));
#35693=CARTESIAN_POINT('Ctrl Pts',(-3.59274946073352,1.53273599648544,24.0931894281991));
#35694=CARTESIAN_POINT('Ctrl Pts',(-3.54385270980084,1.6476965516567,24.0899746657265));
#35695=CARTESIAN_POINT('Ctrl Pts',(-3.48981414813695,1.76015005122282,24.0867672641288));
#35696=CARTESIAN_POINT('Ctrl Pts',(-3.43581118825365,1.87252946397587,24.0835619756371));
#35697=CARTESIAN_POINT('Ctrl Pts',(-3.37667270383973,1.98240587688454,24.0803640383244));
#35698=CARTESIAN_POINT('Ctrl Pts',(-3.31267597495322,2.08942561654219,24.0771697782258));
#35699=CARTESIAN_POINT('Ctrl Pts',(-3.24861596071611,2.19655118632369,24.0739723593741));
#35700=CARTESIAN_POINT('Ctrl Pts',(-3.17968763174453,2.30081519811777,24.0707786250127));
#35701=CARTESIAN_POINT('Ctrl Pts',(-3.10612258128374,2.40183988004365,24.0675848902668));
#35702=CARTESIAN_POINT('Ctrl Pts',(-3.03255753082295,2.50286456196954,24.0643911555208));
#35703=CARTESIAN_POINT('Ctrl Pts',(-2.95435530373159,2.60065069905013,24.0611974203902));
#35704=CARTESIAN_POINT('Ctrl Pts',(-2.87170785494336,2.69478584831407,24.058));
#35705=CARTESIAN_POINT('',(-3.,-3.67394039744206E-16,25.));
#35706=CARTESIAN_POINT('',(-3.5,-4.28626379701574E-16,24.5));
#35707=CARTESIAN_POINT('Origin',(0.,0.,25.));
#35708=CARTESIAN_POINT('Ctrl Pts',(2.28870316125076,-3.20954854141214,-0.329233991005384));
#35709=CARTESIAN_POINT('Ctrl Pts',(3.35678472141098,-2.44790820113649,-0.27627001251076));
#35710=CARTESIAN_POINT('Ctrl Pts',(4.65420965805454,0.212376298523761,-0.170342055521513));
#35711=CARTESIAN_POINT('Ctrl Pts',(2.33824086975704,4.03501766412881,-0.011450120037642));
#35712=CARTESIAN_POINT('Ctrl Pts',(-2.12304297015552,4.14730362817999,0.147441815446229));
#35713=CARTESIAN_POINT('Ctrl Pts',(-4.6372363620278,0.464007918031343,0.3063337509301));
#35714=CARTESIAN_POINT('Ctrl Pts',(-2.9014296726223,-3.64766420030675,0.46522568641397));
#35715=CARTESIAN_POINT('Ctrl Pts',(1.49416848835415,-4.41423135892847,0.624117621897843));
#35716=CARTESIAN_POINT('Ctrl Pts',(4.52003362949604,-1.13548107251883,0.783009557381712));
#35717=CARTESIAN_POINT('Ctrl Pts',(3.40284567859094,3.18450706915039,0.941901492865584));
#35718=CARTESIAN_POINT('Ctrl Pts',(-0.833486649302243,4.58529649769934,
1.10079342834945));
#35719=CARTESIAN_POINT('Ctrl Pts',(-4.30580977810473,1.78325097864793,1.25968536383333));
#35720=CARTESIAN_POINT('Ctrl Pts',(-3.83137142736725,-2.65341337269076,
1.4185772993172));
#35721=CARTESIAN_POINT('Ctrl Pts',(0.154968444518143,-4.65788428232239,
1.57746923480107));
#35722=CARTESIAN_POINT('Ctrl Pts',(3.99925861063605,-2.3928822888867,1.73636117028494));
#35723=CARTESIAN_POINT('Ctrl Pts',(4.17776697308586,2.065482350747,1.89525310576881));
#35724=CARTESIAN_POINT('Ctrl Pts',(0.526867410782717,4.63058858791146,2.05414504125268));
#35725=CARTESIAN_POINT('Ctrl Pts',(-3.60696666633743,2.95122682044694,2.21303697673655));
#35726=CARTESIAN_POINT('Ctrl Pts',(-4.43459848935502,-1.43327725922984,
2.37192891222043));
#35727=CARTESIAN_POINT('Ctrl Pts',(-1.19740732042406,-4.50401613542707,
2.53082084770429));
#35728=CARTESIAN_POINT('Ctrl Pts',(3.13734620436576,-3.44630319202068,2.68971278318817));
#35729=CARTESIAN_POINT('Ctrl Pts',(4.59635878672289,0.770345758451563,2.84860471867204));
#35730=CARTESIAN_POINT('Ctrl Pts',(1.84227644659507,4.28088354832699,3.00749665415591));
#35731=CARTESIAN_POINT('Ctrl Pts',(-2.60046551010954,3.86749606027826,3.16638858963978));
#35732=CARTESIAN_POINT('Ctrl Pts',(-4.65957980074616,-0.0908992967115246,
3.32528052512365));
#35733=CARTESIAN_POINT('Ctrl Pts',(-2.44764980647886,-3.96597491173744,
3.48417246060752));
#35734=CARTESIAN_POINT('Ctrl Pts',(2.00783457505236,-4.20577542454142,3.64306439609139));
#35735=CARTESIAN_POINT('Ctrl Pts',(4.62290614147485,-0.590495894571063,
3.80195633157526));
#35736=CARTESIAN_POINT('Ctrl Pts',(3.00054907928836,3.56604147682096,3.96084826705914));
#35737=CARTESIAN_POINT('Ctrl Pts',(-1.37215855870585,4.45388902928383,4.119740202543));
#35738=CARTESIAN_POINT('Ctrl Pts',(-4.48712403609106,1.2592317017741,4.27863213802688));
#35739=CARTESIAN_POINT('Ctrl Pts',(-3.48912090296361,-3.08965724931931,
4.43752407351074));
#35740=CARTESIAN_POINT('Ctrl Pts',(0.707065439817984,-4.60651767152865,
4.59641600899462));
#35741=CARTESIAN_POINT('Ctrl Pts',(4.25514445682574,-1.9009713952631,4.75530794447848));
#35742=CARTESIAN_POINT('Ctrl Pts',(3.90289100181761,2.54703522197484,4.91419987996237));
#35743=CARTESIAN_POINT('Ctrl Pts',(-0.0268138566703869,4.6603892124167,
5.07309181544622));
#35744=CARTESIAN_POINT('Ctrl Pts',(-3.93194071153866,2.50195700103508,5.23198375093011));
#35745=CARTESIAN_POINT('Ctrl Pts',(-4.23298874115587,-1.9498084293931,5.39087568641397));
#35746=CARTESIAN_POINT('Ctrl Pts',(-0.654012576931896,-4.61434872363465,
5.54976762189785));
#35747=CARTESIAN_POINT('Ctrl Pts',(3.52444182282379,-3.04930425369769,5.70865955738171));
#35748=CARTESIAN_POINT('Ctrl Pts',(4.47233730108079,1.31078055350635,5.86755149286558));
#35749=CARTESIAN_POINT('Ctrl Pts',(1.32081792323409,4.46938324690933,6.02644342834946));
#35750=CARTESIAN_POINT('Ctrl Pts',(-3.04138397969982,3.531278816819,6.18533536383333));
#35751=CARTESIAN_POINT('Ctrl Pts',(-4.61580539333909,-0.643651431219671,
6.3442272993172));
#35752=CARTESIAN_POINT('Ctrl Pts',(-1.95930683639269,-4.22860063318286,
6.50311923480107));
#35753=CARTESIAN_POINT('Ctrl Pts',(2.4931232462982,-3.93754785023079,6.66201117028494));
#35754=CARTESIAN_POINT('Ctrl Pts',(4.66031726875216,-0.037276650332675,
6.82090310576881));
#35755=CARTESIAN_POINT('Ctrl Pts',(2.55579103409072,3.8971629147562,6.97979504125268));
#35756=CARTESIAN_POINT('Ctrl Pts',(-1.89141354276916,4.25940153123874,7.13868697673655));
#35757=CARTESIAN_POINT('Ctrl Pts',(-4.60491865684703,0.717405574212831,
7.29757891222042));
#35758=CARTESIAN_POINT('Ctrl Pts',(-3.09748275458741,-3.48217563875277,
7.45647084770429));
#35759=CARTESIAN_POINT('Ctrl Pts',(1.24915465816929,-4.48993978067229,7.61536278318817));
#35760=CARTESIAN_POINT('Ctrl Pts',(4.45079722404066,-1.38215435627192,7.77425471867203));
#35761=CARTESIAN_POINT('Ctrl Pts',(3.57276890790401,2.99253553442627,7.93314665415592));
#35762=CARTESIAN_POINT('Ctrl Pts',(-0.580115697571088,4.62422019063984,
8.09203858963977));
#35763=CARTESIAN_POINT('Ctrl Pts',(-4.20125711178304,2.01727174044104,8.25093052512366));
#35764=CARTESIAN_POINT('Ctrl Pts',(-3.97146004374031,-2.43873978010442,
8.40982246060752));
#35765=CARTESIAN_POINT('Ctrl Pts',(-0.101360107710164,-4.65936398263266,
8.56871439609139));
#35766=CARTESIAN_POINT('Ctrl Pts',(3.86164810052541,-2.60914172512687,8.72760633157527));
#35767=CARTESIAN_POINT('Ctrl Pts',(4.28500879860717,1.83266095881065,8.88649826705913));
#35768=CARTESIAN_POINT('Ctrl Pts',(0.78066289832912,4.59461772438818,9.04539020254301));
#35769=CARTESIAN_POINT('Ctrl Pts',(-3.43925091813584,3.14507547066701,9.20428213802687));
#35770=CARTESIAN_POINT('Ctrl Pts',(-4.50669313898401,-1.18729252719113,
9.36317407351076));
#35771=CARTESIAN_POINT('Ctrl Pts',(-1.44322940124376,-4.431369482392,9.52206600899461));
#35772=CARTESIAN_POINT('Ctrl Pts',(2.94312115158416,-3.61358332976944,9.6809579444785));
#35773=CARTESIAN_POINT('Ctrl Pts',(4.63176047203213,0.516470254526036,9.83984987996235));
#35774=CARTESIAN_POINT('Ctrl Pts',(2.07485514530555,4.17311906373262,9.99874181544625));
#35775=CARTESIAN_POINT('Ctrl Pts',(-2.3838951082054,4.00462116899514,10.1576337509301));
#35776=CARTESIAN_POINT('Ctrl Pts',(-4.65752953433707,0.165424396228235,
10.316525686414));
#35777=CARTESIAN_POINT('Ctrl Pts',(-2.6619989846541,-3.82540298528012,10.4754176218978));
#35778=CARTESIAN_POINT('Ctrl Pts',(1.77356178859607,-4.30980570050686,10.6343095573817));
#35779=CARTESIAN_POINT('Ctrl Pts',(4.58344787433293,-0.843772586282874,
10.7932014928656));
#35780=CARTESIAN_POINT('Ctrl Pts',(3.19207340137333,3.39567577874192,10.9520934283495));
#35781=CARTESIAN_POINT('Ctrl Pts',(-1.12520585971602,4.52259420768106,11.1109853638333));
#35782=CARTESIAN_POINT('Ctrl Pts',(-4.41110369606797,1.50403150785647,11.2698772993172));
#35783=CARTESIAN_POINT('Ctrl Pts',(-3.65371436373851,-2.89315017624395,
11.4287692348011));
#35784=CARTESIAN_POINT('Ctrl Pts',(0.452727138482009,-4.63842481152508,
11.5876611702849));
#35785=CARTESIAN_POINT('Ctrl Pts',(4.14419181039819,-2.13204616101957,11.7465531057688));
#35786=CARTESIAN_POINT('Ctrl Pts',(4.03702495468236,2.32859960262844,11.9054450412527));
#35787=CARTESIAN_POINT('Ctrl Pts',(0.229457400278859,4.65481427078963,12.0643369767365));
#35788=CARTESIAN_POINT('Ctrl Pts',(-3.78843442356625,2.7143528164975,12.2232289122204));
#35789=CARTESIAN_POINT('Ctrl Pts',(-4.33378754743687,-1.71412720874813,
12.3821208477043));
#35790=CARTESIAN_POINT('Ctrl Pts',(-0.906722702996628,-4.57141121908323,
12.5410127831882));
#35791=CARTESIAN_POINT('Ctrl Pts',(3.35145846134476,-3.23846765862655,12.699904718672));
#35792=CARTESIAN_POINT('Ctrl Pts',(4.53763997961045,1.06290639735133,12.8587966541559));
#35793=CARTESIAN_POINT('Ctrl Pts',(1.56454917743418,4.39000369766127,13.0176885896398));
#35794=CARTESIAN_POINT('Ctrl Pts',(-2.84263205873703,3.69315442037428,13.1765805251236));
#35795=CARTESIAN_POINT('Ctrl Pts',(-4.6442119487827,-0.388898404308158,
13.3354724606075));
#35796=CARTESIAN_POINT('Ctrl Pts',(-2.1888339718237,-4.11448082239789,13.4943643960914));
#35797=CARTESIAN_POINT('Ctrl Pts',(2.27286372066084,-4.06866527271454,13.6532563315753));
#35798=CARTESIAN_POINT('Ctrl Pts',(4.65121870549125,-0.293447010170337,
13.8121482670591));
#35799=CARTESIAN_POINT('Ctrl Pts',(2.76619331968842,3.75074940674537,13.971040202543));
#35800=CARTESIAN_POINT('Ctrl Pts',(-1.65436845932101,4.35694980403646,14.1299321380269));
#35801=CARTESIAN_POINT('Ctrl Pts',(-4.55851003496805,0.969501343570532,
14.2888240735108));
#35802=CARTESIAN_POINT('Ctrl Pts',(-3.28424946851144,-3.30660732816461,
14.4477160089946));
#35803=CARTESIAN_POINT('Ctrl Pts',(1.00040592194765,-4.55182760936985,14.6066079444785));
#35804=CARTESIAN_POINT('Ctrl Pts',(4.36807347752778,-1.62477096509257,14.7654998799624));
#35805=CARTESIAN_POINT('Ctrl Pts',(3.73189604091493,2.79157635286821,14.9243918154462));
#35806=CARTESIAN_POINT('Ctrl Pts',(-0.324996123065272,4.64912078936244,
15.0832837509301));
#35807=CARTESIAN_POINT('Ctrl Pts',(-4.08399171856711,2.24520783821119,15.242175686414));
#35808=CARTESIAN_POINT('Ctrl Pts',(-4.09953613938831,-2.21669800287246,
15.4010676218978));
#35809=CARTESIAN_POINT('Ctrl Pts',(-0.357381124417536,-4.64674351842229,
15.5599595573817));
#35810=CARTESIAN_POINT('Ctrl Pts',(3.71235506167248,-2.81751069033718,15.7188514928656));
#35811=CARTESIAN_POINT('Ctrl Pts',(4.37928808994288,1.59429684167472,15.8777434283495));
#35812=CARTESIAN_POINT('Ctrl Pts',(1.03209663553355,4.54474676181302,16.0366353638333));
#35813=CARTESIAN_POINT('Ctrl Pts',(-3.26113086128664,3.32941017293654,16.1955272993172));
#35814=CARTESIAN_POINT('Ctrl Pts',(-4.56515441384568,-0.937716253370267,
16.3544192348011));
#35815=CARTESIAN_POINT('Ctrl Pts',(-1.68468548190361,-4.34531718303195,
16.5133111702849));
#35816=CARTESIAN_POINT('Ctrl Pts',(2.7399927141092,-3.76993189868439,16.6722031057688));
#35817=CARTESIAN_POINT('Ctrl Pts',(4.65315040492198,0.261032379723303,16.8310950412527));
#35818=CARTESIAN_POINT('Ctrl Pts',(2.30115709895892,4.05273026489556,16.9899869767366));
#35819=CARTESIAN_POINT('Ctrl Pts',(-2.16011307112194,4.12963171651633,17.1488789122204));
#35820=CARTESIAN_POINT('Ctrl Pts',(-4.64138955591407,0.421247652030533,
17.3077708477043));
#35821=CARTESIAN_POINT('Ctrl Pts',(-2.86829522348703,-3.67325864934817,
17.4666627831881));
#35822=CARTESIAN_POINT('Ctrl Pts',(1.53392371633779,-4.40079818061975,17.6255547186721));
#35823=CARTESIAN_POINT('Ctrl Pts',(4.53012400247882,-1.09449674108904,17.7844466541559));
#35824=CARTESIAN_POINT('Ctrl Pts',(3.37394123127184,3.21503766105686,17.9433385896398));
#35825=CARTESIAN_POINT('Ctrl Pts',(-0.874849247264209,4.57761787272052,
18.1022305251236));
#35826=CARTESIAN_POINT('Ctrl Pts',(-4.32173911776226,1.7442813970492,18.2611224606075));
#35827=CARTESIAN_POINT('Ctrl Pts',(-3.80725480047823,-2.68789089777271,
18.4200143960914));
#35828=CARTESIAN_POINT('Ctrl Pts',(0.197019270876202,-4.65630003339433,
18.5789063315753));
#35829=CARTESIAN_POINT('Ctrl Pts',(4.02070237343572,-2.35667117314485,18.7377982670591));
#35830=CARTESIAN_POINT('Ctrl Pts',(4.15894631253379,2.10311962655031,18.896690202543));
#35831=CARTESIAN_POINT('Ctrl Pts',(0.485034514796087,4.63515783048493,19.0555821380269));
#35832=CARTESIAN_POINT('Ctrl Pts',(-3.63346756353596,2.9185373149568,19.2144740735107));
#35833=CARTESIAN_POINT('Ctrl Pts',(-4.42147600817412,-1.47326050087259,
19.3733660089946));
#35834=CARTESIAN_POINT('Ctrl Pts',(-1.15668985931864,-4.51464452234266,
19.5322579444785));
#35835=CARTESIAN_POINT('Ctrl Pts',(3.16833644438965,-3.41783422201423,19.6911498799624));
#35836=CARTESIAN_POINT('Ctrl Pts',(4.58921562907606,0.811816792908698,19.8500418154462));
#35837=CARTESIAN_POINT('Ctrl Pts',(1.80354743972281,4.29734374053261,20.0089337509301));
#35838=CARTESIAN_POINT('Ctrl Pts',(-2.63528075670629,3.84385768827679,20.167825686414));
#35839=CARTESIAN_POINT('Ctrl Pts',(-4.65856908001299,-0.132968903128038,
20.3267176218978));
#35840=CARTESIAN_POINT('Ctrl Pts',(-2.41173956046629,-3.98791409989842,
20.4856095573818));
#35841=CARTESIAN_POINT('Ctrl Pts',(2.04572844434392,-4.18747438603111,20.6445014928655));
#35842=CARTESIAN_POINT('Ctrl Pts',(4.62804952678526,-0.548729644870818,
20.8033934283495));
#35843=CARTESIAN_POINT('Ctrl Pts',(2.96822745143777,3.59298932040533,20.9622853638333));
#35844=CARTESIAN_POINT('Ctrl Pts',(-1.4123186453351,4.44131767923527,21.1211772993172));
#35845=CARTESIAN_POINT('Ctrl Pts',(-4.49831129151882,1.21866419573831,21.2800692348011));
#35846=CARTESIAN_POINT('Ctrl Pts',(-3.46108076274892,-3.12103598071567,
21.438961170285));
#35847=CARTESIAN_POINT('Ctrl Pts',(0.748630655069918,-4.59994560901591,
21.5978531057688));
#35848=CARTESIAN_POINT('Ctrl Pts',(4.2721359622726,-1.86247217365839,21.7567450412527));
#35849=CARTESIAN_POINT('Ctrl Pts',(3.8797330719726,2.58217180475713,21.9156369767366));
#35850=CARTESIAN_POINT('Ctrl Pts',(-0.0688923048847857,4.65995794755513,
22.0745289122204));
#35851=CARTESIAN_POINT('Ctrl Pts',(-3.95437371638077,2.46635025785298,22.2334208477043));
#35852=CARTESIAN_POINT('Ctrl Pts',(-4.21520658614674,-1.98794734397253,
22.3923127831882));
#35853=CARTESIAN_POINT('Ctrl Pts',(-0.612328551070793,-4.62007178368083,
22.551204718672));
#35854=CARTESIAN_POINT('Ctrl Pts',(3.55184600275178,-3.01734516931811,22.7100966541559));
#35855=CARTESIAN_POINT('Ctrl Pts',(4.46029188758379,1.35108854037515,22.8689885896398));
#35856=CARTESIAN_POINT('Ctrl Pts',(1.28046065203078,4.48116776123978,23.0278805251236));
#35857=CARTESIAN_POINT('Ctrl Pts',(-3.07324571308582,3.50359559093557,23.1867724606075));
#35858=CARTESIAN_POINT('Ctrl Pts',(-4.60961384635985,-0.685155565682453,
23.3456643960914));
#35859=CARTESIAN_POINT('Ctrl Pts',(-1.9214110817744,-4.24640173773129,23.5045563315753));
#35860=CARTESIAN_POINT('Ctrl Pts',(2.52927486439223,-3.91433686410129,23.6634482670591));
#35861=CARTESIAN_POINT('Ctrl Pts',(4.65912272890548,0.00377285541425606,
23.822340202543));
#35862=CARTESIAN_POINT('Ctrl Pts',(2.52310591890791,3.92207527169042,23.9812321380269));
#35863=CARTESIAN_POINT('Ctrl Pts',(-1.93519005785514,4.23813764208779,24.1401240735107));
#35864=CARTESIAN_POINT('Ctrl Pts',(-3.71011270200011,1.86957801804229,24.2460520305));
#35865=CARTESIAN_POINT('Ctrl Pts',(-3.90033599543508,0.571614487844223,
24.2990160089946));
#35866=CARTESIAN_POINT('Ctrl Pts',(2.17834184062643,-3.05478403475391,-0.219489327336923));
#35867=CARTESIAN_POINT('Ctrl Pts',(3.19492048266714,-2.32987000971945,-0.166525348842299));
#35868=CARTESIAN_POINT('Ctrl Pts',(4.42978355814708,0.202135508380576,-0.0605973918530519));
#35869=CARTESIAN_POINT('Ctrl Pts',(2.22549083965568,3.84044901682883,0.0982945436308193));
#35870=CARTESIAN_POINT('Ctrl Pts',(-2.02066978786809,3.94732054903492,0.25718647911469));
#35871=CARTESIAN_POINT('Ctrl Pts',(-4.41362871485661,0.441633445237732,
0.416078414598561));
#35872=CARTESIAN_POINT('Ctrl Pts',(-2.76152266511234,-3.4717737462035,0.574970350082432));
#35873=CARTESIAN_POINT('Ctrl Pts',(1.42211964846881,-4.20137701828676,0.733862285566304));
#35874=CARTESIAN_POINT('Ctrl Pts',(4.30207750086251,-1.08072814831761,0.892754221050174));
#35875=CARTESIAN_POINT('Ctrl Pts',(3.23876037940132,3.03095006287751,1.05164615653404));
#35876=CARTESIAN_POINT('Ctrl Pts',(-0.793295903338713,4.36419339201584,
1.21053809201792));
#35877=CARTESIAN_POINT('Ctrl Pts',(-4.09818352865738,1.69726257423614,1.36943002750179));
#35878=CARTESIAN_POINT('Ctrl Pts',(-3.64662260642559,-2.52546571703568,
1.52832196298566));
#35879=CARTESIAN_POINT('Ctrl Pts',(0.147495862454333,-4.43328099194573,
1.68721389846953));
#35880=CARTESIAN_POINT('Ctrl Pts',(3.80641426574215,-2.27749744826117,1.8461058339534));
#35881=CARTESIAN_POINT('Ctrl Pts',(3.97631495072816,1.96588474289028,2.00499776943727));
#35882=CARTESIAN_POINT('Ctrl Pts',(0.501461851760338,4.40730149656556,2.16388970492114));
#35883=CARTESIAN_POINT('Ctrl Pts',(-3.43303864828577,2.80891859328985,2.32278164040501));
#35884=CARTESIAN_POINT('Ctrl Pts',(-4.22076204520191,-1.36416459585457,
2.48167357588889));
#35885=CARTESIAN_POINT('Ctrl Pts',(-1.13966831108264,-4.28683237073678,
2.64056551137275));
#35886=CARTESIAN_POINT('Ctrl Pts',(2.98606329610941,-3.28012237050456,2.79945744685663));
#35887=CARTESIAN_POINT('Ctrl Pts',(4.37472225720076,0.733199667739815,2.9583493823405));
#35888=CARTESIAN_POINT('Ctrl Pts',(1.75344183272134,4.07445924226969,3.11724131782437));
#35889=CARTESIAN_POINT('Ctrl Pts',(-2.47507100164175,3.68100530868232,3.27613325330824));
#35890=CARTESIAN_POINT('Ctrl Pts',(-4.43489475243097,-0.0865161304718975,
3.43502518879211));
#35891=CARTESIAN_POINT('Ctrl Pts',(-2.32962407485832,-3.77473550759247,
3.59391712427598));
#35892=CARTESIAN_POINT('Ctrl Pts',(1.91101674430454,-4.00297283399139,3.75280905975985));
#35893=CARTESIAN_POINT('Ctrl Pts',(4.39998949787803,-0.562022168553895,
3.91170099524372));
#35894=CARTESIAN_POINT('Ctrl Pts',(2.85586253164215,3.39408687237674,4.07059293072759));
#35895=CARTESIAN_POINT('Ctrl Pts',(-1.30599304051693,4.23912239483862,4.22948486621146));
#35896=CARTESIAN_POINT('Ctrl Pts',(-4.27075480883071,1.19851151930018,4.38837680169534));
#35897=CARTESIAN_POINT('Ctrl Pts',(-3.32087541041203,-2.94067390360441,
4.5472687371792));
#35898=CARTESIAN_POINT('Ctrl Pts',(0.672970727569009,-4.38439128034066,
4.70616067266308));
#35899=CARTESIAN_POINT('Ctrl Pts',(4.04996129037005,-1.8093065095749,4.86505260814695));
#35900=CARTESIAN_POINT('Ctrl Pts',(3.7146935053026,2.42421712326595,5.02394454363082));
#35901=CARTESIAN_POINT('Ctrl Pts',(-0.0255208918668632,4.43566513425159,
5.18283647911469));
#35902=CARTESIAN_POINT('Ctrl Pts',(-3.7423424373331,2.38131257520723,5.34172841459856));
#35903=CARTESIAN_POINT('Ctrl Pts',(-4.02887392383437,-1.85578862076283,
5.50062035008243));
#35904=CARTESIAN_POINT('Ctrl Pts',(-0.622476074987428,-4.39184471892869,
5.6595122855663));
#35905=CARTESIAN_POINT('Ctrl Pts',(3.35449315468027,-2.90226673038711,5.81840422105018));
#35906=CARTESIAN_POINT('Ctrl Pts',(4.25668109053274,1.24757468418137,5.97729615653404));
#35907=CARTESIAN_POINT('Ctrl Pts',(1.25712805170321,4.25386948092336,6.13618809201792));
#35908=CARTESIAN_POINT('Ctrl Pts',(-2.89472837218891,3.36100046866316,6.29508002750178));
#35909=CARTESIAN_POINT('Ctrl Pts',(-4.3932311479855,-0.61261454396674,6.45397196298565));
#35910=CARTESIAN_POINT('Ctrl Pts',(-1.86482901435204,-4.0246974105317,6.61286389846953));
#35911=CARTESIAN_POINT('Ctrl Pts',(2.37290478433289,-3.74767919966474,6.77175583395341));
#35912=CARTESIAN_POINT('Ctrl Pts',(4.43559665971225,-0.0354791693710577,
6.93064776943726));
#35913=CARTESIAN_POINT('Ctrl Pts',(2.43255072991432,3.7092416267349,7.08953970492115));
#35914=CARTESIAN_POINT('Ctrl Pts',(-1.80020953695449,4.05401308855407,7.248431640405));
#35915=CARTESIAN_POINT('Ctrl Pts',(-4.38286937018484,0.682812260438543,
7.40732357588889));
#35916=CARTESIAN_POINT('Ctrl Pts',(-2.94812206282321,-3.31426504700587,
7.56621551137276));
#35917=CARTESIAN_POINT('Ctrl Pts',(1.18892039097656,-4.27343477814157,7.72510744685661));
#35918=CARTESIAN_POINT('Ctrl Pts',(4.23617967651747,-1.31550684048772,7.88399938234051));
#35919=CARTESIAN_POINT('Ctrl Pts',(3.40048990657371,2.84823540010302,8.04289131782437));
#35920=CARTESIAN_POINT('Ctrl Pts',(-0.552142504899003,4.40124018356118,
8.20178325330824));
#35921=CARTESIAN_POINT('Ctrl Pts',(-3.99867239438119,1.91999884935475,8.36067518879212));
#35922=CARTESIAN_POINT('Ctrl Pts',(-3.7799561464003,-2.3211436901666,8.51956712427598));
#35923=CARTESIAN_POINT('Ctrl Pts',(-0.0964725209165242,-4.43468934107201,
8.67845905975986));
#35924=CARTESIAN_POINT('Ctrl Pts',(3.67543933768719,-2.48332884936554,8.83735099524372));
#35925=CARTESIAN_POINT('Ctrl Pts',(4.0783855728837,1.74429000398553,8.9962429307276));
#35926=CARTESIAN_POINT('Ctrl Pts',(0.743019314888223,4.37306514893305,9.15513486621146));
#35927=CARTESIAN_POINT('Ctrl Pts',(-3.2734101574334,2.99341985700662,9.31402680169534));
#35928=CARTESIAN_POINT('Ctrl Pts',(-4.28938028911884,-1.13004125341886,
9.4729187371792));
#35929=CARTESIAN_POINT('Ctrl Pts',(-1.37363684534497,-4.2176887410311,9.63181067266308));
#35930=CARTESIAN_POINT('Ctrl Pts',(2.80120377997153,-3.43933625605043,9.79070260814695));
#35931=CARTESIAN_POINT('Ctrl Pts',(4.40841687240619,0.491566046624494,9.94959454363082));
#35932=CARTESIAN_POINT('Ctrl Pts',(1.97480558107332,3.97189116367397,10.1084864791147));
#35933=CARTESIAN_POINT('Ctrl Pts',(-2.26894362964508,3.81151824141021,10.2673784145986));
#35934=CARTESIAN_POINT('Ctrl Pts',(-4.43294334991667,0.157447627925427,
10.4262703500824));
#35935=CARTESIAN_POINT('Ctrl Pts',(-2.53363733058688,-3.6409419627572,10.5851622855663));
#35936=CARTESIAN_POINT('Ctrl Pts',(1.68804059715796,-4.10198676758668,10.7440542210502));
#35937=CARTESIAN_POINT('Ctrl Pts',(4.36243390931193,-0.803085852194621,
10.902946156534));
#35938=CARTESIAN_POINT('Ctrl Pts',(3.03815154638153,3.23193621229276,11.0618380920179));
#35939=CARTESIAN_POINT('Ctrl Pts',(-1.07094840651941,4.30451460790682,11.2207300275018));
#35940=CARTESIAN_POINT('Ctrl Pts',(-4.19840017140343,1.43150707293723,11.3796219629857));
#35941=CARTESIAN_POINT('Ctrl Pts',(-3.47753217061135,-2.75364240624537,
11.5385138984695));
#35942=CARTESIAN_POINT('Ctrl Pts',(0.430896625145342,-4.41475985729101,
11.6974058339534));
#35943=CARTESIAN_POINT('Ctrl Pts',(3.94435878318021,-2.02923884465551,11.8562977694373));
#35944=CARTESIAN_POINT('Ctrl Pts',(3.84235951578439,2.21631447465625,12.0151897049212));
#35945=CARTESIAN_POINT('Ctrl Pts',(0.218392959004639,4.43035901644177,12.174081640405));
#35946=CARTESIAN_POINT('Ctrl Pts',(-3.60575602596446,2.58346665941922,12.3329735758889));
#35947=CARTESIAN_POINT('Ctrl Pts',(-4.12481220928992,-1.63147195415751,
12.4918655113728));
#35948=CARTESIAN_POINT('Ctrl Pts',(-0.86300051278999,-4.35097766186335,
12.6507574468566));
#35949=CARTESIAN_POINT('Ctrl Pts',(3.18985105498742,-3.08230867145154,12.8096493823405));
#35950=CARTESIAN_POINT('Ctrl Pts',(4.31883487235755,1.01165302570498,12.9685413178244));
#35951=CARTESIAN_POINT('Ctrl Pts',(1.48910657905504,4.17831761541948,13.1274332533082));
#35952=CARTESIAN_POINT('Ctrl Pts',(-2.70556027356073,3.51507042678234,13.2863251887921));
#35953=CARTESIAN_POINT('Ctrl Pts',(-4.42026793865305,-0.3701457140446,13.445217124276));
#35954=CARTESIAN_POINT('Ctrl Pts',(-2.08328834587812,-3.91608045972475,
13.6041090597598));
#35955=CARTESIAN_POINT('Ctrl Pts',(2.16326617823678,-3.87247413693191,13.7630009952437));
#35956=CARTESIAN_POINT('Ctrl Pts',(4.4269368293872,-0.279296988392094,13.9218929307276));
#35957=CARTESIAN_POINT('Ctrl Pts',(2.63280741231888,3.56988818154694,14.0807848662115));
#35958=CARTESIAN_POINT('Ctrl Pts',(-1.57459477304264,4.14685758132787,14.2396768016953));
#35959=CARTESIAN_POINT('Ctrl Pts',(-4.33869857315167,0.922751965829036,
14.3985687371792));
#35960=CARTESIAN_POINT('Ctrl Pts',(-3.12588288137982,-3.14716264451114,
14.5574606726631));
#35961=CARTESIAN_POINT('Ctrl Pts',(0.952166324705068,-4.33233837427404,
14.716352608147));
#35962=CARTESIAN_POINT('Ctrl Pts',(4.15744487102007,-1.54642447068669,14.8752445436308));
#35963=CARTESIAN_POINT('Ctrl Pts',(3.55194392546324,2.65696647503773,15.0341364791147));
#35964=CARTESIAN_POINT('Ctrl Pts',(-0.309324802316237,4.4249400748238,15.1930284145986));
#35965=CARTESIAN_POINT('Ctrl Pts',(-3.88706154120257,2.13694386309366,15.3519203500824));
#35966=CARTESIAN_POINT('Ctrl Pts',(-3.90185640968376,-2.10980877268997,
15.5108122855663));
#35967=CARTESIAN_POINT('Ctrl Pts',(-0.340148198136544,-4.42267743594467,
15.6697042210502));
#35968=CARTESIAN_POINT('Ctrl Pts',(3.53334521270251,-2.68165025813993,15.8285961565341));
#35969=CARTESIAN_POINT('Ctrl Pts',(4.168118714559,1.51741981022156,15.9874880920179));
#35970=CARTESIAN_POINT('Ctrl Pts',(0.982328911331549,4.32559896535404,16.1463800275018));
#35971=CARTESIAN_POINT('Ctrl Pts',(-3.10387905394275,3.16886593556829,16.3052719629857));
#35972=CARTESIAN_POINT('Ctrl Pts',(-4.3450225599225,-0.892499553430768,
16.4641638984695));
#35973=CARTESIAN_POINT('Ctrl Pts',(-1.60344990807853,-4.13578588558361,
16.6230558339534));
#35974=CARTESIAN_POINT('Ctrl Pts',(2.60787020056101,-3.5881456932705,16.7819477694373));
#35975=CARTESIAN_POINT('Ctrl Pts',(4.42877538222566,0.248445392192659,16.9408397049211));
#35976=CARTESIAN_POINT('Ctrl Pts',(2.19019524916345,3.85730751556724,17.099731640405));
#35977=CARTESIAN_POINT('Ctrl Pts',(-2.0559523676882,3.9305007773701,17.2586235758889));
#35978=CARTESIAN_POINT('Ctrl Pts',(-4.41758164163537,0.400935080275903,
17.4175155113728));
#35979=CARTESIAN_POINT('Ctrl Pts',(-2.72998595989888,-3.49613403030616,
17.5764074468566));
#35980=CARTESIAN_POINT('Ctrl Pts',(1.4599578784178,-4.18859158815413,17.7352993823405));
#35981=CARTESIAN_POINT('Ctrl Pts',(4.31168131582116,-1.04172008231973,17.8941913178244));
#35982=CARTESIAN_POINT('Ctrl Pts',(3.2112497052163,3.06000846891939,18.0530832533082));
#35983=CARTESIAN_POINT('Ctrl Pts',(-0.832663995847618,4.35688503051531,
18.2119751887921));
#35984=CARTESIAN_POINT('Ctrl Pts',(-4.11334475517948,1.66017210678477,18.370867124276));
#35985=CARTESIAN_POINT('Ctrl Pts',(-3.62366888385615,-2.55828073504186,
18.5297590597599));
#35986=CARTESIAN_POINT('Ctrl Pts',(0.187518996969786,-4.4317731355385,18.6886509952437));
#35987=CARTESIAN_POINT('Ctrl Pts',(3.82682400979189,-2.24303243337775,18.8475429307276));
#35988=CARTESIAN_POINT('Ctrl Pts',(3.95840182287352,2.00170714836323,19.0064348662115));
#35989=CARTESIAN_POINT('Ctrl Pts',(0.461646139008639,4.41165041015396,19.1653268016953));
#35990=CARTESIAN_POINT('Ctrl Pts',(-3.45826167159393,2.77780537652842,19.3242187371792));
#35991=CARTESIAN_POINT('Ctrl Pts',(-4.20827233037425,-1.40221984463863,
19.4831106726631));
#35992=CARTESIAN_POINT('Ctrl Pts',(-1.10091424691577,-4.29694825658366,
19.6420026081469));
#35993=CARTESIAN_POINT('Ctrl Pts',(3.01555918602559,-3.25302617490586,19.8008945436308));
#35994=CARTESIAN_POINT('Ctrl Pts',(4.36792354278479,0.772670967933531,19.9597864791147));
#35995=CARTESIAN_POINT('Ctrl Pts',(1.71658033947744,4.09012572361745,20.1186784145985));
#35996=CARTESIAN_POINT('Ctrl Pts',(-2.5082074562233,3.65850677953844,20.2775703500824));
#35997=CARTESIAN_POINT('Ctrl Pts',(-4.43393276867548,-0.126557139470934,
20.4364622855663));
#35998=CARTESIAN_POINT('Ctrl Pts',(-2.29544542175872,-3.79561678758089,
20.5953542210502));
#35999=CARTESIAN_POINT('Ctrl Pts',(1.94708337032167,-3.98555427199136,20.7542461565341));
#36000=CARTESIAN_POINT('Ctrl Pts',(4.40488486902698,-0.52226988840308,20.9131380920179));
#36001=CARTESIAN_POINT('Ctrl Pts',(2.82509945345179,3.41973529030544,21.0720300275018));
#36002=CARTESIAN_POINT('Ctrl Pts',(-1.34421660681807,4.22715723558706,21.2309219629857));
#36003=CARTESIAN_POINT('Ctrl Pts',(-4.28140261453686,1.15990017936594,21.3898138984695));
#36004=CARTESIAN_POINT('Ctrl Pts',(-3.29418736642239,-2.97053955182989,
21.5487058339534));
#36005=CARTESIAN_POINT('Ctrl Pts',(0.712531667157375,-4.37813612283788,
21.7075977694373));
#36006=CARTESIAN_POINT('Ctrl Pts',(4.06613346502197,-1.7726637213475,21.8664897049211));
#36007=CARTESIAN_POINT('Ctrl Pts',(3.69265225138302,2.45765941919457,22.025381640405));
#36008=CARTESIAN_POINT('Ctrl Pts',(-0.0655703163120924,4.43525466499184,
22.1842735758889));
#36009=CARTESIAN_POINT('Ctrl Pts',(-3.76369372215058,2.34742279002442,22.3431655113728));
#36010=CARTESIAN_POINT('Ctrl Pts',(-4.0119492247608,-1.89208847597824,22.5020574468566));
#36011=CARTESIAN_POINT('Ctrl Pts',(-0.582802053840284,-4.39729181288394,
22.6609493823405));
#36012=CARTESIAN_POINT('Ctrl Pts',(3.38057590440328,-2.87184871381299,22.8198413178244));
#36013=CARTESIAN_POINT('Ctrl Pts',(4.24521650715976,1.285939018969,22.9787332533082));
#36014=CARTESIAN_POINT('Ctrl Pts',(1.21871680907285,4.26508574569377,23.1376251887921));
#36015=CARTESIAN_POINT('Ctrl Pts',(-2.92505373203667,3.33465212858728,23.296517124276));
#36016=CARTESIAN_POINT('Ctrl Pts',(-4.38733815754819,-0.652117348083053,
23.4554090597599));
#36017=CARTESIAN_POINT('Ctrl Pts',(-1.82876059391868,-4.04164014539733,
23.6143009952437));
#36018=CARTESIAN_POINT('Ctrl Pts',(2.40731317054649,-3.72558744783597,23.7731929307276));
#36019=CARTESIAN_POINT('Ctrl Pts',(4.43445972060527,0.00359092823684341,
23.9320848662115));
#36020=CARTESIAN_POINT('Ctrl Pts',(2.4014416917595,3.73295270922791,24.0909768016953));
#36021=CARTESIAN_POINT('Ctrl Pts',(-1.84187514744654,4.03377454464145,24.2498687371792));
#36022=CARTESIAN_POINT('Ctrl Pts',(-3.53121097966664,1.77942692174697,24.3557966941685));
#36023=CARTESIAN_POINT('Ctrl Pts',(-3.71226170138833,0.544051223706471,
24.4087606726631));
#36024=CARTESIAN_POINT('Ctrl Pts',(2.06798052000209,-2.90001952809568,-0.109744663668461));
#36025=CARTESIAN_POINT('Ctrl Pts',(3.0330562439233,-2.2118318183024,-0.0567806851738377));
#36026=CARTESIAN_POINT('Ctrl Pts',(4.20535745823963,0.191894718237391,0.0491472718154096));
#36027=CARTESIAN_POINT('Ctrl Pts',(2.1127408095543,3.64588036952885,0.20803920729928));
#36028=CARTESIAN_POINT('Ctrl Pts',(-1.91829660558064,3.74733746988985,0.366931142783152));
#36029=CARTESIAN_POINT('Ctrl Pts',(-4.19002106768543,0.419258972444119,
0.525823078267022));
#36030=CARTESIAN_POINT('Ctrl Pts',(-2.62161565760238,-3.29588329210025,
0.684715013750895));
#36031=CARTESIAN_POINT('Ctrl Pts',(1.35007080858346,-3.98852267764505,0.843606949234764));
#36032=CARTESIAN_POINT('Ctrl Pts',(4.08412137222898,-1.02597522411638,1.00249888471864));
#36033=CARTESIAN_POINT('Ctrl Pts',(3.07467508021171,2.87739305660463,1.16139082020251));
#36034=CARTESIAN_POINT('Ctrl Pts',(-0.753105157375175,4.14309028633234,
1.32028275568638));
#36035=CARTESIAN_POINT('Ctrl Pts',(-3.89055727921005,1.61127416982435,1.47917469117025));
#36036=CARTESIAN_POINT('Ctrl Pts',(-3.46187378548392,-2.39751806138059,
1.63806662665412));
#36037=CARTESIAN_POINT('Ctrl Pts',(0.14002328039052,-4.20867770156907,1.79695856213799));
#36038=CARTESIAN_POINT('Ctrl Pts',(3.61356992084825,-2.16211260763564,1.95585049762186));
#36039=CARTESIAN_POINT('Ctrl Pts',(3.77486292837046,1.86628713503355,2.11474243310573));
#36040=CARTESIAN_POINT('Ctrl Pts',(0.476056292737952,4.18401440521967,2.27363436858961));
#36041=CARTESIAN_POINT('Ctrl Pts',(-3.2591106302341,2.66661036613276,2.43252630407347));
#36042=CARTESIAN_POINT('Ctrl Pts',(-4.0069256010488,-1.2950519324793,2.59141823955734));
#36043=CARTESIAN_POINT('Ctrl Pts',(-1.08192930174121,-4.0696486060465,2.75031017504122));
#36044=CARTESIAN_POINT('Ctrl Pts',(2.83478038785305,-3.11394154898843,2.90920211052509));
#36045=CARTESIAN_POINT('Ctrl Pts',(4.15308572767863,0.696053577028067,3.06809404600896));
#36046=CARTESIAN_POINT('Ctrl Pts',(1.66460721884761,3.8680349362124,3.22698598149283));
#36047=CARTESIAN_POINT('Ctrl Pts',(-2.34967649317396,3.49451455708637,3.3858779169767));
#36048=CARTESIAN_POINT('Ctrl Pts',(-4.21020970411577,-0.0821329642322605,
3.54476985246057));
#36049=CARTESIAN_POINT('Ctrl Pts',(-2.21159834323779,-3.58349610344751,
3.70366178794445));
#36050=CARTESIAN_POINT('Ctrl Pts',(1.81419891355671,-3.80017024344135,3.86255372342831));
#36051=CARTESIAN_POINT('Ctrl Pts',(4.1770728542812,-0.53354844253673,4.02144565891219));
#36052=CARTESIAN_POINT('Ctrl Pts',(2.71117598399594,3.22213226793253,4.18033759439605));
#36053=CARTESIAN_POINT('Ctrl Pts',(-1.23982752232801,4.02435576039341,4.33922952987993));
#36054=CARTESIAN_POINT('Ctrl Pts',(-4.05438558157035,1.13779133682627,4.4981214653638));
#36055=CARTESIAN_POINT('Ctrl Pts',(-3.15262991786046,-2.79169055788951,
4.65701340084767));
#36056=CARTESIAN_POINT('Ctrl Pts',(0.638876015320037,-4.16226488915267,
4.81590533633154));
#36057=CARTESIAN_POINT('Ctrl Pts',(3.84477812391437,-1.7176416238867,4.97479727181542));
#36058=CARTESIAN_POINT('Ctrl Pts',(3.5264960087876,2.30139902455706,5.13368920729927));
#36059=CARTESIAN_POINT('Ctrl Pts',(-0.0242279270633424,4.21094105608648,
5.29258114278316));
#36060=CARTESIAN_POINT('Ctrl Pts',(-3.55274416312754,2.26066814937938,5.45147307826701));
#36061=CARTESIAN_POINT('Ctrl Pts',(-3.82475910651287,-1.76176881213256,
5.61036501375091));
#36062=CARTESIAN_POINT('Ctrl Pts',(-0.590939573042961,-4.16934071422273,
5.76925694923476));
#36063=CARTESIAN_POINT('Ctrl Pts',(3.18454448653674,-2.75522920707652,5.92814888471864));
#36064=CARTESIAN_POINT('Ctrl Pts',(4.04102487998468,1.1843688148564,6.0870408202025));
#36065=CARTESIAN_POINT('Ctrl Pts',(1.19343818017234,4.03835571493739,6.24593275568638));
#36066=CARTESIAN_POINT('Ctrl Pts',(-2.74807276467801,3.19072212050733,6.40482469117025));
#36067=CARTESIAN_POINT('Ctrl Pts',(-4.17065690263191,-0.581577656713809,
6.56371662665412));
#36068=CARTESIAN_POINT('Ctrl Pts',(-1.77035119231138,-3.82079418788054,
6.72260856213799));
#36069=CARTESIAN_POINT('Ctrl Pts',(2.25268632236759,-3.5578105490987,6.88150049762186));
#36070=CARTESIAN_POINT('Ctrl Pts',(4.21087605067235,-0.033681688409442,
7.04039243310573));
#36071=CARTESIAN_POINT('Ctrl Pts',(2.30931042573792,3.52132033871361,7.19928436858961));
#36072=CARTESIAN_POINT('Ctrl Pts',(-1.70900553113983,3.84862464586941,7.35817630407347));
#36073=CARTESIAN_POINT('Ctrl Pts',(-4.16082008352265,0.648218946664257,
7.51706823955734));
#36074=CARTESIAN_POINT('Ctrl Pts',(-2.79876137105901,-3.14635445525897,
7.67596017504123));
#36075=CARTESIAN_POINT('Ctrl Pts',(1.12868612378383,-4.05692977561084,7.83485211052507));
#36076=CARTESIAN_POINT('Ctrl Pts',(4.02156212899428,-1.24885932470353,7.99374404600897));
#36077=CARTESIAN_POINT('Ctrl Pts',(3.2282109052434,2.70393526577978,8.15263598149282));
#36078=CARTESIAN_POINT('Ctrl Pts',(-0.524169312226923,4.1782601764825,8.3115279169767));
#36079=CARTESIAN_POINT('Ctrl Pts',(-3.79608767697933,1.82272595826847,8.47041985246058));
#36080=CARTESIAN_POINT('Ctrl Pts',(-3.5884522490603,-2.20354760022878,8.62931178794444));
#36081=CARTESIAN_POINT('Ctrl Pts',(-0.0915849341228856,-4.21001469951135,
8.78820372342831));
#36082=CARTESIAN_POINT('Ctrl Pts',(3.48923057484898,-2.35751597360421,8.94709565891219));
#36083=CARTESIAN_POINT('Ctrl Pts',(3.87176234716024,1.65591904916041,9.10598759439605));
#36084=CARTESIAN_POINT('Ctrl Pts',(0.705375731447328,4.15151257347791,9.26487952987993));
#36085=CARTESIAN_POINT('Ctrl Pts',(-3.10756939673095,2.84176424334623,9.42377146536379));
#36086=CARTESIAN_POINT('Ctrl Pts',(-4.07206743925366,-1.07278997964659,
9.58266340084768));
#36087=CARTESIAN_POINT('Ctrl Pts',(-1.30404428944617,-4.00400799967019,
9.74155533633153));
#36088=CARTESIAN_POINT('Ctrl Pts',(2.65928640835889,-3.26508918233143,9.90044727181542));
#36089=CARTESIAN_POINT('Ctrl Pts',(4.18507327278026,0.466661838722957,10.0593392072993));
#36090=CARTESIAN_POINT('Ctrl Pts',(1.87475601684109,3.77066326361532,10.2182311427832));
#36091=CARTESIAN_POINT('Ctrl Pts',(-2.15399215108477,3.61841531382528,10.377123078267));
#36092=CARTESIAN_POINT('Ctrl Pts',(-4.20835716549627,0.149470859622617,
10.5360150137509));
#36093=CARTESIAN_POINT('Ctrl Pts',(-2.40527567651967,-3.45648094023428,
10.6949069492348));
#36094=CARTESIAN_POINT('Ctrl Pts',(1.60251940571986,-3.89416783466651,10.8537988847186));
#36095=CARTESIAN_POINT('Ctrl Pts',(4.14141994429093,-0.762399118106369,
11.0126908202025));
#36096=CARTESIAN_POINT('Ctrl Pts',(2.88422969138973,3.06819664584361,11.1715827556864));
#36097=CARTESIAN_POINT('Ctrl Pts',(-1.01669095332279,4.08643500813259,11.3304746911703));
#36098=CARTESIAN_POINT('Ctrl Pts',(-3.98569664673889,1.35898263801798,11.4893666266541));
#36099=CARTESIAN_POINT('Ctrl Pts',(-3.30134997748419,-2.61413463624678,
11.648258562138));
#36100=CARTESIAN_POINT('Ctrl Pts',(0.409066111808665,-4.19109490305693,
11.8071504976218));
#36101=CARTESIAN_POINT('Ctrl Pts',(3.74452575596225,-1.92643152829146,11.9660424331058));
#36102=CARTESIAN_POINT('Ctrl Pts',(3.6476940768864,2.10402934668408,12.1249343685896));
#36103=CARTESIAN_POINT('Ctrl Pts',(0.207328517730425,4.20590376209391,12.2838263040735));
#36104=CARTESIAN_POINT('Ctrl Pts',(-3.42307762836267,2.45258050234096,12.4427182395573));
#36105=CARTESIAN_POINT('Ctrl Pts',(-3.91583687114297,-1.54881669956688,
12.6016101750412));
#36106=CARTESIAN_POINT('Ctrl Pts',(-0.819278322583353,-4.13054410464348,
12.7605021105251));
#36107=CARTESIAN_POINT('Ctrl Pts',(3.02824364863007,-2.92614968427652,12.919394046009));
#36108=CARTESIAN_POINT('Ctrl Pts',(4.10002976510464,0.960399654058624,13.0782859814928));
#36109=CARTESIAN_POINT('Ctrl Pts',(1.4136639806759,3.9666315331777,13.2371779169767));
#36110=CARTESIAN_POINT('Ctrl Pts',(-2.56848848838443,3.33698643319039,13.3960698524606));
#36111=CARTESIAN_POINT('Ctrl Pts',(-4.19632392852339,-0.351393023781037,
13.5549617879445));
#36112=CARTESIAN_POINT('Ctrl Pts',(-1.97774271993255,-3.71768009705162,
13.7138537234283));
#36113=CARTESIAN_POINT('Ctrl Pts',(2.05366863581272,-3.67628300114927,13.8727456589122));
#36114=CARTESIAN_POINT('Ctrl Pts',(4.20265495328316,-0.265146966613851,
14.0316375943961));
#36115=CARTESIAN_POINT('Ctrl Pts',(2.49942150494934,3.38902695634851,14.1905295298799));
#36116=CARTESIAN_POINT('Ctrl Pts',(-1.49482108676428,3.93676535861929,14.3494214653638));
#36117=CARTESIAN_POINT('Ctrl Pts',(-4.11888711133529,0.876002588087538,
14.5083134008477));
#36118=CARTESIAN_POINT('Ctrl Pts',(-2.96751629424819,-2.98771796085767,
14.6672053363315));
#36119=CARTESIAN_POINT('Ctrl Pts',(0.903926727462482,-4.11284913917822,
14.8260972718154));
#36120=CARTESIAN_POINT('Ctrl Pts',(3.94681626451235,-1.46807797628081,14.9849892072993));
#36121=CARTESIAN_POINT('Ctrl Pts',(3.37199181001155,2.52235659720725,15.1438811427832));
#36122=CARTESIAN_POINT('Ctrl Pts',(-0.293653481567197,4.20075936028517,
15.302773078267));
#36123=CARTESIAN_POINT('Ctrl Pts',(-3.69013136383804,2.02867988797614,15.4616650137509));
#36124=CARTESIAN_POINT('Ctrl Pts',(-3.7041766799792,-2.00291954250747,15.6205569492348));
#36125=CARTESIAN_POINT('Ctrl Pts',(-0.322915271855557,-4.19861135346705,
15.7794488847186));
#36126=CARTESIAN_POINT('Ctrl Pts',(3.35433536373254,-2.54578982594268,15.9383408202025));
#36127=CARTESIAN_POINT('Ctrl Pts',(3.95694933917511,1.44054277876839,16.0972327556863));
#36128=CARTESIAN_POINT('Ctrl Pts',(0.932561187129547,4.10645116889506,16.2561246911703));
#36129=CARTESIAN_POINT('Ctrl Pts',(-2.94662724659887,3.00832169820004,16.4150166266541));
#36130=CARTESIAN_POINT('Ctrl Pts',(-4.12489070599933,-0.847282853491266,
16.573908562138));
#36131=CARTESIAN_POINT('Ctrl Pts',(-1.52221433425345,-3.92625458813528,
16.7328004976219));
#36132=CARTESIAN_POINT('Ctrl Pts',(2.47574768701282,-3.40635948785661,16.8916924331057));
#36133=CARTESIAN_POINT('Ctrl Pts',(4.20440035952933,0.235858404662022,17.0505843685896));
#36134=CARTESIAN_POINT('Ctrl Pts',(2.07923339936798,3.66188476623891,17.2094763040735));
#36135=CARTESIAN_POINT('Ctrl Pts',(-1.95179166425446,3.73136983822386,17.3683682395573));
#36136=CARTESIAN_POINT('Ctrl Pts',(-4.19377372735666,0.380622508521273,
17.5272601750413));
#36137=CARTESIAN_POINT('Ctrl Pts',(-2.59167669631074,-3.31900941126415,
17.6861521105251));
#36138=CARTESIAN_POINT('Ctrl Pts',(1.38599204049781,-3.97638499568851,17.845044046009));
#36139=CARTESIAN_POINT('Ctrl Pts',(4.09323862916349,-0.988943423550422,
18.0039359814928));
#36140=CARTESIAN_POINT('Ctrl Pts',(3.04855817916078,2.90497927678192,18.1628279169767));
#36141=CARTESIAN_POINT('Ctrl Pts',(-0.79047874443103,4.13615218831009,18.3217198524606));
#36142=CARTESIAN_POINT('Ctrl Pts',(-3.9049503925967,1.57606281652034,18.4806117879444));
#36143=CARTESIAN_POINT('Ctrl Pts',(-3.44008296723408,-2.42867057231101,
18.6395037234283));
#36144=CARTESIAN_POINT('Ctrl Pts',(0.178018723063364,-4.20724623768266,
18.7983956589122));
#36145=CARTESIAN_POINT('Ctrl Pts',(3.63294564614808,-2.12939369361065,18.9572875943961));
#36146=CARTESIAN_POINT('Ctrl Pts',(3.75785733321325,1.90029467017615,19.1161795298799));
#36147=CARTESIAN_POINT('Ctrl Pts',(0.438257763221198,4.18814298982299,19.2750714653638));
#36148=CARTESIAN_POINT('Ctrl Pts',(-3.2830557796519,2.63707343810004,19.4339634008477));
#36149=CARTESIAN_POINT('Ctrl Pts',(-3.99506865257438,-1.33117918840468,
19.5928553363316));
#36150=CARTESIAN_POINT('Ctrl Pts',(-1.04513863451291,-4.07925199082465,
19.7517472718154));
#36151=CARTESIAN_POINT('Ctrl Pts',(2.86278192766154,-3.08821812779751,19.9106392072993));
#36152=CARTESIAN_POINT('Ctrl Pts',(4.14663145649351,0.733525142958367,20.0695311427831));
#36153=CARTESIAN_POINT('Ctrl Pts',(1.62961323923206,3.88290770670228,20.228423078267));
#36154=CARTESIAN_POINT('Ctrl Pts',(-2.3811341557403,3.47315587080009,20.3873150137509));
#36155=CARTESIAN_POINT('Ctrl Pts',(-4.20929645733797,-0.120145375813829,
20.5462069492348));
#36156=CARTESIAN_POINT('Ctrl Pts',(-2.17915128305114,-3.60331947526336,
20.7050988847187));
#36157=CARTESIAN_POINT('Ctrl Pts',(1.8484382962994,-3.78363415795159,20.8639908202025));
#36158=CARTESIAN_POINT('Ctrl Pts',(4.18172021126871,-0.495810131935346,
21.0228827556864));
#36159=CARTESIAN_POINT('Ctrl Pts',(2.6819714554658,3.24648126020556,21.1817746911702));
#36160=CARTESIAN_POINT('Ctrl Pts',(-1.27611456830103,4.01299679193883,21.3406666266541));
#36161=CARTESIAN_POINT('Ctrl Pts',(-4.0644939375549,1.10113616299357,21.499558562138));
#36162=CARTESIAN_POINT('Ctrl Pts',(-3.12729397009587,-2.82004312294412,
21.6584504976218));
#36163=CARTESIAN_POINT('Ctrl Pts',(0.676432679244829,-4.15632663665986,
21.8173424331058));
#36164=CARTESIAN_POINT('Ctrl Pts',(3.86013096777133,-1.68285526903662,21.9762343685896));
#36165=CARTESIAN_POINT('Ctrl Pts',(3.50557143079345,2.33314703363201,22.1351263040735));
#36166=CARTESIAN_POINT('Ctrl Pts',(-0.062248327739398,4.21055138242857,
22.2940182395573));
#36167=CARTESIAN_POINT('Ctrl Pts',(-3.57301372792039,2.22849532219585,22.4529101750413));
#36168=CARTESIAN_POINT('Ctrl Pts',(-3.80869186337486,-1.79622960798394,
22.6118021105251));
#36169=CARTESIAN_POINT('Ctrl Pts',(-0.553275556609776,-4.17451184208706,
22.770694046009));
#36170=CARTESIAN_POINT('Ctrl Pts',(3.20930580605478,-2.72635225830787,22.9295859814928));
#36171=CARTESIAN_POINT('Ctrl Pts',(4.03014112673573,1.22078949756286,23.0884779169767));
#36172=CARTESIAN_POINT('Ctrl Pts',(1.15697296611493,4.04900373014777,23.2473698524606));
#36173=CARTESIAN_POINT('Ctrl Pts',(-2.77686175098751,3.16570866623898,23.4062617879444));
#36174=CARTESIAN_POINT('Ctrl Pts',(-4.16506246873653,-0.619079130483647,
23.5651537234284));
#36175=CARTESIAN_POINT('Ctrl Pts',(-1.73611010606296,-3.83687855306338,
23.7240456589121));
#36176=CARTESIAN_POINT('Ctrl Pts',(2.28535147670074,-3.53683803157065,23.8829375943961));
#36177=CARTESIAN_POINT('Ctrl Pts',(4.20979671230505,0.00340900105942339,
24.0418295298799));
#36178=CARTESIAN_POINT('Ctrl Pts',(2.27977746461109,3.54383014676541,24.2007214653638));
#36179=CARTESIAN_POINT('Ctrl Pts',(-1.74856023703795,3.82941144719509,24.3596134008477));
#36180=CARTESIAN_POINT('Ctrl Pts',(-3.35230925733317,1.68927582545165,24.4655413578369));
#36181=CARTESIAN_POINT('Ctrl Pts',(-3.52418740734158,0.51648795956872,24.5185053363315));
#36182=CARTESIAN_POINT('Ctrl Pts',(1.95761919937776,-2.74525502143746,0.));
#36183=CARTESIAN_POINT('Ctrl Pts',(2.87119200517945,-2.09379362688536,0.0529639784946237));
#36184=CARTESIAN_POINT('Ctrl Pts',(3.98093135833217,0.181653928094203,0.158891935483871));
#36185=CARTESIAN_POINT('Ctrl Pts',(1.99999077945293,3.45131172222888,0.317783870967742));
#36186=CARTESIAN_POINT('Ctrl Pts',(-1.81592342329319,3.54735439074478,0.476675806451613));
#36187=CARTESIAN_POINT('Ctrl Pts',(-3.96641342051426,0.396884499650513,
0.635567741935484));
#36188=CARTESIAN_POINT('Ctrl Pts',(-2.48170865009243,-3.119992837997,0.794459677419355));
#36189=CARTESIAN_POINT('Ctrl Pts',(1.27802196869812,-3.77566833700333,0.953351612903227));
#36190=CARTESIAN_POINT('Ctrl Pts',(3.86616524359544,-0.97122229991515,1.1122435483871));
#36191=CARTESIAN_POINT('Ctrl Pts',(2.91058978102209,2.72383605033175,1.27113548387097));
#36192=CARTESIAN_POINT('Ctrl Pts',(-0.71291441141164,3.92198718064885,1.43002741935484));
#36193=CARTESIAN_POINT('Ctrl Pts',(-3.6829310297627,1.52528576541256,1.58891935483871));
#36194=CARTESIAN_POINT('Ctrl Pts',(-3.27712496454226,-2.26957040572551,
1.74781129032258));
#36195=CARTESIAN_POINT('Ctrl Pts',(0.13255069832671,-3.98407441119242,1.90670322580645));
#36196=CARTESIAN_POINT('Ctrl Pts',(3.42072557595435,-2.04672776701011,2.06559516129032));
#36197=CARTESIAN_POINT('Ctrl Pts',(3.57341090601276,1.76668952717683,2.2244870967742));
#36198=CARTESIAN_POINT('Ctrl Pts',(0.45065073371557,3.96072731387378,2.38337903225806));
#36199=CARTESIAN_POINT('Ctrl Pts',(-3.08518261218244,2.52430213897566,2.54227096774194));
#36200=CARTESIAN_POINT('Ctrl Pts',(-3.79308915689569,-1.22593926910403,
2.70116290322581));
#36201=CARTESIAN_POINT('Ctrl Pts',(-1.02419029239979,-3.85246484135621,
2.86005483870968));
#36202=CARTESIAN_POINT('Ctrl Pts',(2.68349747959669,-2.94776072747231,3.01894677419354));
#36203=CARTESIAN_POINT('Ctrl Pts',(3.9314491981565,0.658907486316316,3.17783870967743));
#36204=CARTESIAN_POINT('Ctrl Pts',(1.57577260497388,3.66161063015511,3.33673064516129));
#36205=CARTESIAN_POINT('Ctrl Pts',(-2.22428198470617,3.30802380549044,3.49562258064516));
#36206=CARTESIAN_POINT('Ctrl Pts',(-3.98552465580058,-0.07774979799263,
3.65451451612903));
#36207=CARTESIAN_POINT('Ctrl Pts',(-2.09357261161725,-3.39225669930255,
3.8134064516129));
#36208=CARTESIAN_POINT('Ctrl Pts',(1.71738108280889,-3.59736765289132,3.97229838709678));
#36209=CARTESIAN_POINT('Ctrl Pts',(3.95415621068438,-0.505074716519562,
4.13119032258065));
#36210=CARTESIAN_POINT('Ctrl Pts',(2.56648943634972,3.05017766348832,4.29008225806451));
#36211=CARTESIAN_POINT('Ctrl Pts',(-1.17366200413909,3.8095891259482,4.44897419354839));
#36212=CARTESIAN_POINT('Ctrl Pts',(-3.83801635431,1.07707115435234,4.60786612903225));
#36213=CARTESIAN_POINT('Ctrl Pts',(-2.98438442530889,-2.6427072121746,4.76675806451613));
#36214=CARTESIAN_POINT('Ctrl Pts',(0.604781303071069,-3.94013849796468,
4.92565));
#36215=CARTESIAN_POINT('Ctrl Pts',(3.63959495745868,-1.6259767381985,5.08454193548388));
#36216=CARTESIAN_POINT('Ctrl Pts',(3.3382985122726,2.17858092584818,5.24343387096774));
#36217=CARTESIAN_POINT('Ctrl Pts',(-0.0229349622598251,3.98621697792136,
5.40232580645161));
#36218=CARTESIAN_POINT('Ctrl Pts',(-3.36314588892197,2.14002372355154,5.56121774193549));
#36219=CARTESIAN_POINT('Ctrl Pts',(-3.62064428919136,-1.6677490035023,5.72010967741935));
#36220=CARTESIAN_POINT('Ctrl Pts',(-0.559403071098495,-3.94683670951677,
5.87900161290323));
#36221=CARTESIAN_POINT('Ctrl Pts',(3.01459581839321,-2.60819168376593,6.03789354838709));
#36222=CARTESIAN_POINT('Ctrl Pts',(3.82536866943663,1.12116294553142,6.19678548387097));
#36223=CARTESIAN_POINT('Ctrl Pts',(1.12974830864147,3.82284194895142,6.35567741935484));
#36224=CARTESIAN_POINT('Ctrl Pts',(-2.60141715716711,3.02044377235149,6.51456935483871));
#36225=CARTESIAN_POINT('Ctrl Pts',(-3.94808265727831,-0.550540769460877,
6.67346129032257));
#36226=CARTESIAN_POINT('Ctrl Pts',(-1.67587337027072,-3.61689096522939,
6.83235322580646));
#36227=CARTESIAN_POINT('Ctrl Pts',(2.13246786040229,-3.36794189853266,6.99124516129032));
#36228=CARTESIAN_POINT('Ctrl Pts',(3.98615544163244,-0.0318842074478251,
7.15013709677419));
#36229=CARTESIAN_POINT('Ctrl Pts',(2.18607012156152,3.33339905069232,7.30902903225807));
#36230=CARTESIAN_POINT('Ctrl Pts',(-1.61780152532516,3.64323620318475,7.46792096774193));
#36231=CARTESIAN_POINT('Ctrl Pts',(-3.93877079686046,0.613625632889965,
7.62681290322582));
#36232=CARTESIAN_POINT('Ctrl Pts',(-2.64940067929482,-2.97844386351206,
7.78570483870967));
#36233=CARTESIAN_POINT('Ctrl Pts',(1.06845185659111,-3.84042477308012,7.94459677419355));
#36234=CARTESIAN_POINT('Ctrl Pts',(3.80694458147109,-1.18221180891932,8.10348870967742));
#36235=CARTESIAN_POINT('Ctrl Pts',(3.0559319039131,2.55963513145653,8.2623806451613));
#36236=CARTESIAN_POINT('Ctrl Pts',(-0.49619611955484,3.95528016940384,8.42127258064515));
#36237=CARTESIAN_POINT('Ctrl Pts',(-3.59350295957747,1.72545306718219,8.58016451612905));
#36238=CARTESIAN_POINT('Ctrl Pts',(-3.39694835172031,-2.08595151029096,
8.7390564516129));
#36239=CARTESIAN_POINT('Ctrl Pts',(-0.086697347329244,-3.9853400579507,
8.89794838709678));
#36240=CARTESIAN_POINT('Ctrl Pts',(3.30302181201077,-2.23170309784288,9.05684032258065));
#36241=CARTESIAN_POINT('Ctrl Pts',(3.66513912143678,1.56754809433529,9.21573225806451));
#36242=CARTESIAN_POINT('Ctrl Pts',(0.667732148006428,3.92995999802278,9.3746241935484));
#36243=CARTESIAN_POINT('Ctrl Pts',(-2.94172863602851,2.69010862968584,9.53351612903225));
#36244=CARTESIAN_POINT('Ctrl Pts',(-3.85475458938848,-1.01553870587432,
9.69240806451614));
#36245=CARTESIAN_POINT('Ctrl Pts',(-1.23445173354738,-3.79032725830928,
9.85129999999999));
#36246=CARTESIAN_POINT('Ctrl Pts',(2.51736903674626,-3.09084210861242,10.0101919354839));
#36247=CARTESIAN_POINT('Ctrl Pts',(3.96172967315432,0.441757630821415,10.1690838709677));
#36248=CARTESIAN_POINT('Ctrl Pts',(1.77470645260886,3.56943536355667,10.3279758064516));
#36249=CARTESIAN_POINT('Ctrl Pts',(-2.03904067252446,3.42531238624034,10.4868677419355));
#36250=CARTESIAN_POINT('Ctrl Pts',(-3.98377098107586,0.14149409131981,10.6457596774194));
#36251=CARTESIAN_POINT('Ctrl Pts',(-2.27691402245245,-3.27201991771136,
10.8046516129032));
#36252=CARTESIAN_POINT('Ctrl Pts',(1.51699821428175,-3.68634890174633,10.9635435483871));
#36253=CARTESIAN_POINT('Ctrl Pts',(3.92040597926993,-0.721712384018116,
11.122435483871));
#36254=CARTESIAN_POINT('Ctrl Pts',(2.73030783639792,2.90445707939446,11.2813274193548));
#36255=CARTESIAN_POINT('Ctrl Pts',(-0.962433500126168,3.86835540835836,
11.4402193548387));
#36256=CARTESIAN_POINT('Ctrl Pts',(-3.77299312207436,1.28645820309873,11.5991112903226));
#36257=CARTESIAN_POINT('Ctrl Pts',(-3.12516778435703,-2.4746268662482,11.7580032258064));
#36258=CARTESIAN_POINT('Ctrl Pts',(0.38723559847199,-3.96742994882286,11.9168951612903));
#36259=CARTESIAN_POINT('Ctrl Pts',(3.54469272874429,-1.82362421192741,12.0757870967742));
#36260=CARTESIAN_POINT('Ctrl Pts',(3.45302863798842,1.9917442187119,12.2346790322581));
#36261=CARTESIAN_POINT('Ctrl Pts',(0.196264076456207,3.98144850774605,12.3935709677419));
#36262=CARTESIAN_POINT('Ctrl Pts',(-3.24039923076088,2.32169434526269,12.5524629032258));
#36263=CARTESIAN_POINT('Ctrl Pts',(-3.70686153299603,-1.46616144497625,
12.7113548387097));
#36264=CARTESIAN_POINT('Ctrl Pts',(-0.775556132376715,-3.9101105474236,
12.8702467741936));
#36265=CARTESIAN_POINT('Ctrl Pts',(2.86663624227273,-2.76999069710151,13.0291387096774));
#36266=CARTESIAN_POINT('Ctrl Pts',(3.88122465785174,0.909146282412278,13.1880306451613));
#36267=CARTESIAN_POINT('Ctrl Pts',(1.33822138229676,3.75494545093591,13.3469225806451));
#36268=CARTESIAN_POINT('Ctrl Pts',(-2.43141670320813,3.15890243959844,13.5058145161291));
#36269=CARTESIAN_POINT('Ctrl Pts',(-3.97237991839373,-0.332640333517474,
13.6647064516129));
#36270=CARTESIAN_POINT('Ctrl Pts',(-1.87219709398698,-3.51927973437849,
13.8235983870968));
#36271=CARTESIAN_POINT('Ctrl Pts',(1.94407109338865,-3.48009186536664,13.9824903225806));
#36272=CARTESIAN_POINT('Ctrl Pts',(3.97837307717912,-0.25099694483561,14.1413822580645));
#36273=CARTESIAN_POINT('Ctrl Pts',(2.36603559757979,3.20816573115008,14.3002741935484));
#36274=CARTESIAN_POINT('Ctrl Pts',(-1.41504740048591,3.7266731359107,14.4591661290323));
#36275=CARTESIAN_POINT('Ctrl Pts',(-3.8990756495189,0.82925321034604,14.6180580645161));
#36276=CARTESIAN_POINT('Ctrl Pts',(-2.80914970711657,-2.8282732772042,14.77695));
#36277=CARTESIAN_POINT('Ctrl Pts',(0.8556871302199,-3.8933599040824,14.9358419354839));
#36278=CARTESIAN_POINT('Ctrl Pts',(3.73618765800463,-1.38973148187494,15.0947338709677));
#36279=CARTESIAN_POINT('Ctrl Pts',(3.19203969455987,2.38774671937678,15.2536258064516));
#36280=CARTESIAN_POINT('Ctrl Pts',(-0.277982160818163,3.97657864574653,
15.4125177419355));
#36281=CARTESIAN_POINT('Ctrl Pts',(-3.4932011864735,1.92041591285862,15.5714096774194));
#36282=CARTESIAN_POINT('Ctrl Pts',(-3.50649695027464,-1.89603031232498,
15.7303016129032));
#36283=CARTESIAN_POINT('Ctrl Pts',(-0.30568234557457,-3.97454527098943,
15.8891935483871));
#36284=CARTESIAN_POINT('Ctrl Pts',(3.17532551476257,-2.40992939374543,16.048085483871));
#36285=CARTESIAN_POINT('Ctrl Pts',(3.74577996379122,1.36366574731522,16.2069774193548));
#36286=CARTESIAN_POINT('Ctrl Pts',(0.882793462927545,3.88730337243608,16.3658693548387));
#36287=CARTESIAN_POINT('Ctrl Pts',(-2.78937543925498,2.84777746083178,16.5247612903226));
#36288=CARTESIAN_POINT('Ctrl Pts',(-3.90475885207616,-0.802066153551767,
16.6836532258065));
#36289=CARTESIAN_POINT('Ctrl Pts',(-1.44097876042837,-3.71672329068694,
16.8425451612903));
#36290=CARTESIAN_POINT('Ctrl Pts',(2.34362517346463,-3.22457328244272,17.0014370967742));
#36291=CARTESIAN_POINT('Ctrl Pts',(3.980025336833,0.223271417131382,17.1603290322581));
#36292=CARTESIAN_POINT('Ctrl Pts',(1.96827154957251,3.46646201691059,17.3192209677419));
#36293=CARTESIAN_POINT('Ctrl Pts',(-1.84763096082072,3.53223889907763,17.4781129032258));
#36294=CARTESIAN_POINT('Ctrl Pts',(-3.96996581307795,0.360309936766638,
17.6370048387097));
#36295=CARTESIAN_POINT('Ctrl Pts',(-2.4533674327226,-3.14188479222213,17.7958967741935));
#36296=CARTESIAN_POINT('Ctrl Pts',(1.31202620257783,-3.7641784032229,17.9547887096774));
#36297=CARTESIAN_POINT('Ctrl Pts',(3.87479594250582,-0.936166764781103,
18.1136806451613));
#36298=CARTESIAN_POINT('Ctrl Pts',(2.88586665310525,2.74995008464444,18.2725725806452));
#36299=CARTESIAN_POINT('Ctrl Pts',(-0.748293493014444,3.91541934610488,
18.431464516129));
#36300=CARTESIAN_POINT('Ctrl Pts',(-3.69655603001392,1.49195352625591,18.5903564516129));
#36301=CARTESIAN_POINT('Ctrl Pts',(-3.25649705061201,-2.29906040958017,
18.7492483870968));
#36302=CARTESIAN_POINT('Ctrl Pts',(0.168518449156949,-3.98271933982683,
18.9081403225806));
#36303=CARTESIAN_POINT('Ctrl Pts',(3.43906728250426,-2.01575495384355,19.0670322580645));
#36304=CARTESIAN_POINT('Ctrl Pts',(3.55731284355299,1.79888219198906,19.2259241935484));
#36305=CARTESIAN_POINT('Ctrl Pts',(0.41486938743375,3.96463556949202,19.3848161290323));
#36306=CARTESIAN_POINT('Ctrl Pts',(-3.10784988770987,2.49634149967166,19.5437080645161));
#36307=CARTESIAN_POINT('Ctrl Pts',(-3.78186497477451,-1.26013853217073,
19.7026));
#36308=CARTESIAN_POINT('Ctrl Pts',(-0.989363022110038,-3.86155572506565,
19.8614919354839));
#36309=CARTESIAN_POINT('Ctrl Pts',(2.71000466929749,-2.92341008068914,20.0203838709678));
#36310=CARTESIAN_POINT('Ctrl Pts',(3.92533937020224,0.694379317983201,20.1792758064516));
#36311=CARTESIAN_POINT('Ctrl Pts',(1.54264613898669,3.6756896897871,20.3381677419355));
#36312=CARTESIAN_POINT('Ctrl Pts',(-2.25406085525731,3.28780496206174,20.4970596774194));
#36313=CARTESIAN_POINT('Ctrl Pts',(-3.98466014600046,-0.113733612156729,
20.6559516129032));
#36314=CARTESIAN_POINT('Ctrl Pts',(-2.06285714434356,-3.41102216294582,
20.8148435483871));
#36315=CARTESIAN_POINT('Ctrl Pts',(1.74979322227715,-3.58171404391184,20.9737354838709));
#36316=CARTESIAN_POINT('Ctrl Pts',(3.95855555351044,-0.46935037546761,21.1326274193549));
#36317=CARTESIAN_POINT('Ctrl Pts',(2.53884345747981,3.07322723010567,21.2915193548387));
#36318=CARTESIAN_POINT('Ctrl Pts',(-1.20801252978399,3.79883634829061,21.4504112903226));
#36319=CARTESIAN_POINT('Ctrl Pts',(-3.84758526057294,1.0423721466212,21.6093032258064));
#36320=CARTESIAN_POINT('Ctrl Pts',(-2.96040057376934,-2.66954669405833,
21.7681951612904));
#36321=CARTESIAN_POINT('Ctrl Pts',(0.640333691332285,-3.93451715048184,
21.9270870967742));
#36322=CARTESIAN_POINT('Ctrl Pts',(3.6541284705207,-1.59304681672573,22.0859790322581));
#36323=CARTESIAN_POINT('Ctrl Pts',(3.31849061020388,2.20863464806944,22.2448709677419));
#36324=CARTESIAN_POINT('Ctrl Pts',(-0.058926339166703,3.98584809986529,
22.4037629032258));
#36325=CARTESIAN_POINT('Ctrl Pts',(-3.3823337336902,2.1095678543673,22.5626548387097));
#36326=CARTESIAN_POINT('Ctrl Pts',(-3.60543450198892,-1.70037073998966,
22.7215467741936));
#36327=CARTESIAN_POINT('Ctrl Pts',(-0.52374905937927,-3.95173187129016,
22.8804387096774));
#36328=CARTESIAN_POINT('Ctrl Pts',(3.03803570770629,-2.58085580280275,23.0393306451613));
#36329=CARTESIAN_POINT('Ctrl Pts',(3.81506574631169,1.15563997615671,23.1982225806452));
#36330=CARTESIAN_POINT('Ctrl Pts',(1.095229123157,3.83292171460177,23.357114516129));
#36331=CARTESIAN_POINT('Ctrl Pts',(-2.62866976993836,2.99676520389069,23.5160064516129));
#36332=CARTESIAN_POINT('Ctrl Pts',(-3.94278677992486,-0.586040912884242,
23.6748983870968));
#36333=CARTESIAN_POINT('Ctrl Pts',(-1.64345961820725,-3.63211696072943,
23.8337903225806));
#36334=CARTESIAN_POINT('Ctrl Pts',(2.163389782855,-3.34808861530533,23.9926822580645));
#36335=CARTESIAN_POINT('Ctrl Pts',(3.98513370400483,0.0032270738820094,
24.1515741935484));
#36336=CARTESIAN_POINT('Ctrl Pts',(2.15811323746268,3.35470758430291,24.3104661290323));
#36337=CARTESIAN_POINT('Ctrl Pts',(-1.65524532662936,3.62504834974875,24.4693580645161));
#36338=CARTESIAN_POINT('Ctrl Pts',(-3.1734075349997,1.59912472915632,24.5752860215054));
#36339=CARTESIAN_POINT('Ctrl Pts',(-3.33611311329483,0.488924695430968,
24.62825));
#36340=CARTESIAN_POINT('',(1.95761919937778,-2.74525502143744,0.));
#36341=CARTESIAN_POINT('Ctrl Pts',(1.95761919937776,-2.74525502143746,0.));
#36342=CARTESIAN_POINT('Ctrl Pts',(2.87119200517945,-2.09379362688536,0.0529639784946237));
#36343=CARTESIAN_POINT('Ctrl Pts',(3.98093135833217,0.181653928094203,0.158891935483871));
#36344=CARTESIAN_POINT('Ctrl Pts',(1.99999077945293,3.45131172222888,0.317783870967742));
#36345=CARTESIAN_POINT('Ctrl Pts',(-1.81592342329319,3.54735439074478,0.476675806451613));
#36346=CARTESIAN_POINT('Ctrl Pts',(-3.32105516281529,1.34233496093003,0.58788455216069));
#36347=CARTESIAN_POINT('Ctrl Pts',(-3.3766520624322,0.1136195821916,0.646129319375144));
#36348=CARTESIAN_POINT('Ctrl Pts',(-3.37589447807987,0.0021436428109594,
0.651410108094974));
#36349=CARTESIAN_POINT('Ctrl Pts',(1.73118107496478,3.54876586530513,2.39391839684799E-16));
#36350=CARTESIAN_POINT('Ctrl Pts',(1.81301063452785,3.50205269354806,2.06920727311338E-16));
#36351=CARTESIAN_POINT('Ctrl Pts',(1.89292240658196,3.4522795469799,5.6760153975772E-16));
#36352=CARTESIAN_POINT('Ctrl Pts',(1.97072352421092,3.39943606703627,2.9316826744008E-16));
#36353=CARTESIAN_POINT('Ctrl Pts',(2.07158749034463,3.33092801556019,-4.87384004076243E-17));
#36354=CARTESIAN_POINT('Ctrl Pts',(2.16890551010069,3.25726040082769,-6.1331688516479E-17));
#36355=CARTESIAN_POINT('Ctrl Pts',(2.26249391432527,3.17884397520376,-1.04083408558608E-17));
#36356=CARTESIAN_POINT('Ctrl Pts',(2.31703211703773,3.13314717171513,1.92670006623856E-17));
#36357=CARTESIAN_POINT('Ctrl Pts',(2.37030307443948,3.08583698417059,-9.57318163015451E-16));
#36358=CARTESIAN_POINT('Ctrl Pts',(2.42226407127706,3.03698980450436,-1.02695629777827E-15));
#36359=CARTESIAN_POINT('Ctrl Pts',(2.45441149625484,3.00676884764696,-1.07004028094122E-15));
#36360=CARTESIAN_POINT('Ctrl Pts',(2.48605741280453,2.97595951290433,-8.19532942944583E-16));
#36361=CARTESIAN_POINT('Ctrl Pts',(2.51719072732778,2.9445793777147,-8.39606162372775E-16));
#36362=CARTESIAN_POINT('Ctrl Pts',(2.53181221876951,2.92984196908534,-8.49033375972473E-16));
#36363=CARTESIAN_POINT('Ctrl Pts',(2.54632072268487,2.91497845934833,-6.96615474306211E-16));
#36364=CARTESIAN_POINT('Ctrl Pts',(2.56070494112922,2.90000148244637,-7.07767178198537E-16));
#36365=CARTESIAN_POINT('Ctrl Pts',(2.64790074151672,2.80921243517189,-7.75367774667319E-16));
#36366=CARTESIAN_POINT('Ctrl Pts',(2.73062866917384,2.71416182380689,-8.593918943852E-16));
#36367=CARTESIAN_POINT('Ctrl Pts',(2.80868748257388,2.61529981528879,-7.7715611723761E-16));
#36368=CARTESIAN_POINT('Ctrl Pts',(2.87698894429891,2.52879555783546,-7.05199812233468E-16));
#36369=CARTESIAN_POINT('Ctrl Pts',(2.94171511816388,2.43937213712426,-7.20848724153807E-16));
#36370=CARTESIAN_POINT('Ctrl Pts',(3.00269897791456,2.3473133317077,-6.24500451351651E-16));
#36371=CARTESIAN_POINT('Ctrl Pts',(3.02937941655548,2.30703760433796,-5.82348082000707E-16));
#36372=CARTESIAN_POINT('Ctrl Pts',(3.05534314365639,2.26625728440317,-1.08606649764317E-16));
#36373=CARTESIAN_POINT('Ctrl Pts',(3.08057418911428,2.22499554197223,-6.93889390390723E-17));
#36374=CARTESIAN_POINT('Ctrl Pts',(3.09523937783659,2.20101273710704,-4.6594198725879E-17));
#36375=CARTESIAN_POINT('Ctrl Pts',(3.10965701779078,2.17686728558595,-1.5350788780052E-16));
#36376=CARTESIAN_POINT('Ctrl Pts',(3.12382377516257,2.1525637049523,-1.66533453693773E-16));
#36377=CARTESIAN_POINT('Ctrl Pts',(3.1333468514065,2.13622652592816,-1.75289406369904E-16));
#36378=CARTESIAN_POINT('Ctrl Pts',(3.14275743380374,2.11981622896702,-6.17919290773945E-16));
#36379=CARTESIAN_POINT('Ctrl Pts',(3.15204614385832,2.10334928089744,-6.10622663543836E-16));
#36380=CARTESIAN_POINT('Ctrl Pts',(3.21133027918083,1.99825085797653,-5.64052770246931E-16));
#36381=CARTESIAN_POINT('Ctrl Pts',(3.26572921710173,1.89071971149897,-2.93721959998899E-16));
#36382=CARTESIAN_POINT('Ctrl Pts',(3.3150665440347,1.78114320161924,-3.46944695195361E-16));
#36383=CARTESIAN_POINT('Ctrl Pts',(3.36416434269629,1.67209867580975,-3.99909038813826E-16));
#36384=CARTESIAN_POINT('Ctrl Pts',(3.40824985101865,1.5610277430108,-6.74639111044964E-16));
#36385=CARTESIAN_POINT('Ctrl Pts',(3.44710068203266,1.44829560050515,-7.21644966006352E-16));
#36386=CARTESIAN_POINT('Ctrl Pts',(3.48485757303191,1.33873770674576,-7.67327256340457E-16));
#36387=CARTESIAN_POINT('Ctrl Pts',(3.51767049623361,1.22761008128266,-7.45739296926402E-16));
#36388=CARTESIAN_POINT('Ctrl Pts',(3.54528704260767,1.11524410687019,-6.10622663543836E-16));
#36389=CARTESIAN_POINT('Ctrl Pts',(3.56429882714017,1.03788911593903,-5.17605662582399E-16));
#36390=CARTESIAN_POINT('Ctrl Pts',(3.58084694549942,0.959947166702576,1.01128139593754E-16));
#36391=CARTESIAN_POINT('Ctrl Pts',(3.59483483174014,0.881527990398642,1.38777878078145E-16));
#36392=CARTESIAN_POINT('Ctrl Pts',(3.60174616248926,0.842781545425996,1.5738038819335E-16));
#36393=CARTESIAN_POINT('Ctrl Pts',(3.60803228263339,0.803918629301433,-8.2431208915498E-16));
#36394=CARTESIAN_POINT('Ctrl Pts',(3.6136804381616,0.764952740225288,-8.60422844084496E-16));
#36395=CARTESIAN_POINT('Ctrl Pts',(3.61598402562173,0.749060590478247,-8.75150533826084E-16));
#36396=CARTESIAN_POINT('Ctrl Pts',(3.6181800809526,0.733160977259198,-9.56453568707426E-16));
#36397=CARTESIAN_POINT('Ctrl Pts',(3.62026800126996,0.71725566677106,-9.43689570931383E-16));
#36398=CARTESIAN_POINT('Ctrl Pts',(3.63517124652415,0.603726074153541,-8.52582172005361E-16));
#36399=CARTESIAN_POINT('Ctrl Pts',(3.64457137343043,0.489891978911761,1.54068630345449E-16));
#36400=CARTESIAN_POINT('Ctrl Pts',(3.64826597516095,0.3760806489335,1.38777878078145E-16));
#36401=CARTESIAN_POINT('Ctrl Pts',(3.65049038519446,0.307558225463841,1.29571770019922E-16));
#36402=CARTESIAN_POINT('Ctrl Pts',(3.65064564728474,0.239043959798587,2.28153843810054E-16));
#36403=CARTESIAN_POINT('Ctrl Pts',(3.64867842117138,0.170609648189261,1.38777878078145E-16));
#36404=CARTESIAN_POINT('Ctrl Pts',(3.64536397368567,0.0553092612588858,
-9.22057312926959E-18));
#36405=CARTESIAN_POINT('Ctrl Pts',(3.63602703897368,-0.0597651999246838,
-3.71059406415836E-16));
#36406=CARTESIAN_POINT('Ctrl Pts',(3.62088618085986,-0.174255990612961,
-4.44089209850063E-16));
#36407=CARTESIAN_POINT('Ctrl Pts',(3.60564019443288,-0.289541731204713,
-5.17626084943432E-16));
#36408=CARTESIAN_POINT('Ctrl Pts',(3.58450894234823,-0.404236478340693,
2.06881119674206E-16));
#36409=CARTESIAN_POINT('Ctrl Pts',(3.55766829556208,-0.517952337059044,
1.66533453693773E-16));
#36410=CARTESIAN_POINT('Ctrl Pts',(3.55209090522836,-0.541582085487224,
1.58149353116006E-16));
#36411=CARTESIAN_POINT('Ctrl Pts',(3.54626683911464,-0.565169464342046,
2.72822796152711E-16));
#36412=CARTESIAN_POINT('Ctrl Pts',(3.54019745029697,-0.588710821151176,
2.77555756156289E-16));
#36413=CARTESIAN_POINT('Ctrl Pts',(3.53607649256559,-0.604694792398417,
2.80769313353732E-16));
#36414=CARTESIAN_POINT('Ctrl Pts',(3.53184170988113,-0.62066020100356,-1.61867697048363E-17));
#36415=CARTESIAN_POINT('Ctrl Pts',(3.52749592285427,-0.636597072708719,
-2.77555756156289E-17));
#36416=CARTESIAN_POINT('Ctrl Pts',(3.49747618222011,-0.7466854760641,-1.07670341512578E-16));
#36417=CARTESIAN_POINT('Ctrl Pts',(3.46222700262188,-0.855189606000695,
-1.99543722780696E-16));
#36418=CARTESIAN_POINT('Ctrl Pts',(3.42199607778626,-0.961778490999782,
-2.77555756156289E-16));
#36419=CARTESIAN_POINT('Ctrl Pts',(3.38156991618782,-1.0688846414842,-3.55946374337476E-16));
#36420=CARTESIAN_POINT('Ctrl Pts',(3.33611303054141,-1.17405769074672,1.35240542225809E-16));
#36421=CARTESIAN_POINT('Ctrl Pts',(3.28582849960376,-1.27693996092432,1.11022302462516E-16));
#36422=CARTESIAN_POINT('Ctrl Pts',(3.23598893769955,-1.3789118233987,8.70183704900679E-17));
#36423=CARTESIAN_POINT('Ctrl Pts',(3.18140622212873,-1.47863395215989,2.26466381867324E-16));
#36424=CARTESIAN_POINT('Ctrl Pts',(3.1222390297712,-1.57572584500942,2.22044604925031E-16));
#36425=CARTESIAN_POINT('Ctrl Pts',(3.08604888850041,-1.6351129678129,2.19339985594059E-16));
#36426=CARTESIAN_POINT('Ctrl Pts',(3.04814284654775,-1.69351537716898,-1.98475779326559E-16));
#36427=CARTESIAN_POINT('Ctrl Pts',(3.00855126708734,-1.75083831899302,-2.22044604925031E-16));
#36428=CARTESIAN_POINT('Ctrl Pts',(2.9875142347103,-1.78129693164588,-2.34567928166019E-16));
#36429=CARTESIAN_POINT('Ctrl Pts',(2.96600124729196,-1.81145066683922,-9.64459754115302E-17));
#36430=CARTESIAN_POINT('Ctrl Pts',(2.94401641708542,-1.8412845286552,-1.11022302462516E-16));
#36431=CARTESIAN_POINT('Ctrl Pts',(2.93430327275808,-1.85446546309672,-1.17462287082754E-16));
#36432=CARTESIAN_POINT('Ctrl Pts',(2.92449763119146,-1.86758436264681,1.18006511135168E-16));
#36433=CARTESIAN_POINT('Ctrl Pts',(2.91460943608169,-1.8806275411502,1.11022302462516E-16));
#36434=CARTESIAN_POINT('Ctrl Pts',(2.8471863415804,-1.96956302907997,6.34001675707856E-17));
#36435=CARTESIAN_POINT('Ctrl Pts',(2.77582498992288,-2.05512251526362,-2.18484873575661E-16));
#36436=CARTESIAN_POINT('Ctrl Pts',(2.70071126790977,-2.13697549169768,-1.66533453693773E-16));
#36437=CARTESIAN_POINT('Ctrl Pts',(2.6265626894838,-2.21777673120304,-1.1524956270538E-16));
#36438=CARTESIAN_POINT('Ctrl Pts',(2.54875698937316,-2.29496666804747,3.16111469076589E-16));
#36439=CARTESIAN_POINT('Ctrl Pts',(2.46744030034225,-2.36818969290806,1.66533453693773E-16));
#36440=CARTESIAN_POINT('Ctrl Pts',(2.38865944095536,-2.43912928592605,2.1619971139621E-17));
#36441=CARTESIAN_POINT('Ctrl Pts',(2.30658261909198,-2.50634586230322,1.27495535944492E-16));
#36442=CARTESIAN_POINT('Ctrl Pts',(2.22131994895062,-2.56947408053004,1.66533453693773E-16));
#36443=CARTESIAN_POINT('Ctrl Pts',(2.13653932671254,-2.63224539197476,2.05350663525179E-16));
#36444=CARTESIAN_POINT('Ctrl Pts',(2.04860838319626,-2.69097492590926,9.78571983200637E-17));
#36445=CARTESIAN_POINT('Ctrl Pts',(1.95761919937776,-2.74525502143746,5.55111512312578E-17));
#36446=CARTESIAN_POINT('Ctrl Pts',(0.349418900843865,3.91916189049794,24.058));
#36447=CARTESIAN_POINT('Ctrl Pts',(0.983708099956935,3.86349481221817,24.0324107126756));
#36448=CARTESIAN_POINT('Ctrl Pts',(1.60505772607221,3.66267070559658,24.0068214253513));
#36449=CARTESIAN_POINT('Ctrl Pts',(2.13605939111367,3.32170193071062,23.9812321380269));
#36450=CARTESIAN_POINT('Ctrl Pts',(3.23511152224044,2.61597446626503,23.9282681595323));
#36451=CARTESIAN_POINT('Ctrl Pts',(3.94711712557296,1.30987366083964,23.8753041810376));
#36452=CARTESIAN_POINT('Ctrl Pts',(3.94814528315368,0.00380497154103099,
23.822340202543));
#36453=CARTESIAN_POINT('Ctrl Pts',(3.94917344073441,-1.30226371775762,23.7693762240484));
#36454=CARTESIAN_POINT('Ctrl Pts',(3.23922415256329,-2.60830029092949,23.7164122455538));
#36455=CARTESIAN_POINT('Ctrl Pts',(2.14246851744994,-3.3166627231204,23.6634482670591));
#36456=CARTESIAN_POINT('Ctrl Pts',(1.04571288233662,-4.0250251553113,23.6104842885645));
#36457=CARTESIAN_POINT('Ctrl Pts',(-0.437849099718904,-4.13571344652128,
23.5575203100699));
#36458=CARTESIAN_POINT('Ctrl Pts',(-1.62766388484424,-3.59751656345146,
23.5045563315753));
#36459=CARTESIAN_POINT('Ctrl Pts',(-2.81747866996957,-3.05931968038165,
23.4515923530806));
#36460=CARTESIAN_POINT('Ctrl Pts',(-3.71354625816471,-1.87223762303205,
23.398628374586));
#36461=CARTESIAN_POINT('Ctrl Pts',(-3.90551869671661,-0.580571401587583,
23.3456643960914));
#36462=CARTESIAN_POINT('Ctrl Pts',(-3.93389711745665,-0.389630203130338,
23.3378349697575));
#36463=CARTESIAN_POINT('Ctrl Pts',(-3.94688938557907,-0.196403592096446,
23.3300055434235));
#36464=CARTESIAN_POINT('Ctrl Pts',(-3.94525314071248,-0.00295827654940184,
23.3221761170896));
#36465=CARTESIAN_POINT('Origin',(0.,0.,-1.84858989190503));
#36466=CARTESIAN_POINT('',(-1.95761919937781,-2.74525502143742,0.));
#36467=CARTESIAN_POINT('Ctrl Pts',(-1.96186193197216,-2.74910310536277,
-1.68972908581866E-15));
#36468=CARTESIAN_POINT('Ctrl Pts',(-1.11318069597017,-3.34796943221813,
0.0492202025162847));
#36469=CARTESIAN_POINT('Ctrl Pts',(1.27289724729396,-3.73216471134832,0.15142869376082));
#36470=CARTESIAN_POINT('Ctrl Pts',(3.84885445708067,-1.03979978230375,0.306625473733605));
#36471=CARTESIAN_POINT('Ctrl Pts',(2.95737874714596,2.67433718082728,0.465590339918353));
#36472=CARTESIAN_POINT('Ctrl Pts',(-0.647631800440264,3.93376542742361,
0.624555206103101));
#36473=CARTESIAN_POINT('Ctrl Pts',(-3.06550566908991,2.04752208664245,0.752221723431987));
#36474=CARTESIAN_POINT('Ctrl Pts',(-3.36890345256199,0.462673372879177,
0.826899952032626));
#36475=CARTESIAN_POINT('Ctrl Pts',(-3.36692593843476,0.00163208592380858,
0.848589891905015));
#36476=CARTESIAN_POINT('Origin',(0.,0.,0.));
#36477=CARTESIAN_POINT('Ctrl Pts',(-1.47719995289048,3.03093687853778,-0.329233991005386));
#36478=CARTESIAN_POINT('Ctrl Pts',(-2.48630564145415,2.53912496184525,-0.276245702277136));
#36479=CARTESIAN_POINT('Ctrl Pts',(-3.95706612649723,0.476768711041013,
-0.170269124820638));
#36480=CARTESIAN_POINT('Ctrl Pts',(-2.54025446427213,-3.07629710463389,
-0.0113042586358904));
#36481=CARTESIAN_POINT('Ctrl Pts',(1.21035452671364,-3.79753374264191,0.147660607548857));
#36482=CARTESIAN_POINT('Ctrl Pts',(3.84885445708067,-1.03979978230375,0.306625473733605));
#36483=CARTESIAN_POINT('Ctrl Pts',(2.95737874714596,2.67433718082728,0.465590339918353));
#36484=CARTESIAN_POINT('Ctrl Pts',(-0.647631800440264,3.93376542742361,
0.624555206103101));
#36485=CARTESIAN_POINT('Ctrl Pts',(-3.65826453346399,1.58509620284767,0.783520072287847));
#36486=CARTESIAN_POINT('Ctrl Pts',(-3.31298624479799,-2.21807698161905,
0.942484938472596));
#36487=CARTESIAN_POINT('Ctrl Pts',(0.0716483833591926,-3.98622915634864,
1.10144980465734));
#36488=CARTESIAN_POINT('Ctrl Pts',(3.39051798866077,-2.09756782602768,1.26041467084209));
#36489=CARTESIAN_POINT('Ctrl Pts',(3.59899177492058,1.71542482386315,1.41937953702684));
#36490=CARTESIAN_POINT('Ctrl Pts',(0.505790215469384,3.95468340129096,1.57834440321159));
#36491=CARTESIAN_POINT('Ctrl Pts',(-3.05141119286119,2.56598394358578,1.73730926939633));
#36492=CARTESIAN_POINT('Ctrl Pts',(-3.80929264538726,-1.17672126473752,
1.89627413558108));
#36493=CARTESIAN_POINT('Ctrl Pts',(-1.07258002819951,-3.83991470812214,
2.05523900176583));
#36494=CARTESIAN_POINT('Ctrl Pts',(2.6481020123777,-2.98042525524821,2.21420386795058));
#36495=CARTESIAN_POINT('Ctrl Pts',(3.9394520872816,0.613266379946328,2.37316873413532));
#36496=CARTESIAN_POINT('Ctrl Pts',(1.61680281711694,3.64435532093595,2.53213360032008));
#36497=CARTESIAN_POINT('Ctrl Pts',(-2.18907900650795,3.33216312280983,2.69109846650482));
#36498=CARTESIAN_POINT('Ctrl Pts',(-3.98672992391563,-0.0369098299799313,
2.85006333268957));
#36499=CARTESIAN_POINT('Ctrl Pts',(-2.12700963248002,-3.37212213291773,
3.00902819887431));
#36500=CARTESIAN_POINT('Ctrl Pts',(1.68400001564517,-3.61379602896036,3.16799306505907));
#36501=CARTESIAN_POINT('Ctrl Pts',(3.95013122707835,-0.540223147458982,
3.32695793124381));
#36502=CARTESIAN_POINT('Ctrl Pts',(2.59246639543577,3.02894300530038,3.48592279742856));
#36503=CARTESIAN_POINT('Ctrl Pts',(-1.14349143614182,3.81939852540782,3.6448876636133));
#36504=CARTESIAN_POINT('Ctrl Pts',(-3.83042595833975,1.10599038526397,3.80385252979806));
#36505=CARTESIAN_POINT('Ctrl Pts',(-3.00338040757504,-2.62203811565132,
3.9628173959828));
#36506=CARTESIAN_POINT('Ctrl Pts',(0.57892500607099,-3.94464492605495,4.12178226216755));
#36507=CARTESIAN_POINT('Ctrl Pts',(3.63013258458704,-1.64848875417016,4.2807471283523));
#36508=CARTESIAN_POINT('Ctrl Pts',(3.35110647594949,2.15996831943484,4.43971199453705));
#36509=CARTESIAN_POINT('Ctrl Pts',(-0.00217860669321579,3.9869001753454,
4.59867686072179));
#36510=CARTESIAN_POINT('Ctrl Pts',(-3.35346506555395,2.15630466503255,4.75764172690654));
#36511=CARTESIAN_POINT('Ctrl Pts',(-3.6283288127004,-1.65245507692285,4.91660659309129));
#36512=CARTESIAN_POINT('Ctrl Pts',(-0.574613628296617,-3.94527526701846,
5.07557145927603));
#36513=CARTESIAN_POINT('Ctrl Pts',(3.0062441927532,-2.61875420913902,5.2345363254608));
#36514=CARTESIAN_POINT('Ctrl Pts',(3.8292149534867,1.11017592945447,5.39350119164552));
#36515=CARTESIAN_POINT('Ctrl Pts',(1.13931660104628,3.82064594498541,5.55246605783029));
#36516=CARTESIAN_POINT('Ctrl Pts',(-2.59577512563926,3.02610793784054,5.71143092401502));
#36517=CARTESIAN_POINT('Ctrl Pts',(-3.94953846664522,-0.544539856061292,
5.87039579019978));
#36518=CARTESIAN_POINT('Ctrl Pts',(-1.68004955900417,-3.61563427819245,
6.02936065638453));
#36519=CARTESIAN_POINT('Ctrl Pts',(2.13069369871068,-3.3697955600636,6.18832552256926));
#36520=CARTESIAN_POINT('Ctrl Pts',(3.98676787287831,-0.032552759256669,
6.34729038875402));
#36521=CARTESIAN_POINT('Ctrl Pts',(2.18543605335013,3.3345534950076,6.50625525493876));
#36522=CARTESIAN_POINT('Ctrl Pts',(-1.62078473268592,3.64258625218979,6.66522012112352));
#36523=CARTESIAN_POINT('Ctrl Pts',(-3.94011990490355,0.608960498992104,
6.82418498730826));
#36524=CARTESIAN_POINT('Ctrl Pts',(-2.64484328742837,-2.98331723745481,
6.98314985349301));
#36525=CARTESIAN_POINT('Ctrl Pts',(1.07677617223565,-3.83874078693202,7.14211471967776));
#36526=CARTESIAN_POINT('Ctrl Pts',(3.81057598656871,-1.17255635469506,7.3010795858625));
#36527=CARTESIAN_POINT('Ctrl Pts',(3.04860581952888,2.56931514444696,7.46004445204726));
#36528=CARTESIAN_POINT('Ctrl Pts',(-0.510113381387115,3.95413228059959,
7.619009318232));
#36529=CARTESIAN_POINT('Ctrl Pts',(-3.60086158473341,1.71148286638841,7.77797418441675));
#36530=CARTESIAN_POINT('Ctrl Pts',(-3.38822891354565,-2.10125738160825,
7.93693905060149));
#36531=CARTESIAN_POINT('Ctrl Pts',(-0.0672816548149041,-3.98633301836102,
8.09590391678625));
#36532=CARTESIAN_POINT('Ctrl Pts',(3.31538886833258,-2.21440159096907,8.25486878297098));
#36533=CARTESIAN_POINT('Ctrl Pts',(3.65656725922866,1.58899138861319,8.41383364915575));
#36534=CARTESIAN_POINT('Ctrl Pts',(0.643261156248369,3.93466553079316,8.57279851534047));
#36535=CARTESIAN_POINT('Ctrl Pts',(-2.96016388101437,2.67073165104392,8.73176338152524));
#36536=CARTESIAN_POINT('Ctrl Pts',(-3.84797530194499,-1.04329469948394,
8.89072824770997));
#36537=CARTESIAN_POINT('Ctrl Pts',(-1.20570712414377,-3.80021684712055,
9.04969311389473));
#36538=CARTESIAN_POINT('Ctrl Pts',(2.54266018034211,-3.07087234538534,9.20865798007948));
#36539=CARTESIAN_POINT('Ctrl Pts',(3.95842601916979,0.47564819468749,9.36762284626423));
#36540=CARTESIAN_POINT('Ctrl Pts',(1.74278629094578,3.58581562527152,9.52658771244896));
#36541=CARTESIAN_POINT('Ctrl Pts',(-2.07166160205713,3.40640513751843,9.68555257863373));
#36542=CARTESIAN_POINT('Ctrl Pts',(-3.98559564477585,0.102005444431573,
9.84451744481845));
#36543=CARTESIAN_POINT('Ctrl Pts',(-2.24319907973156,-3.29597263991092,
10.0034823110032));
#36544=CARTESIAN_POINT('Ctrl Pts',(1.55707745747673,-3.67027077281332,10.1624471771879));
#36545=CARTESIAN_POINT('Ctrl Pts',(3.928912558612,-0.677512997019795,10.3214120433727));
#36546=CARTESIAN_POINT('Ctrl Pts',(2.69641733534343,2.93678588051791,10.4803769095574));
#36547=CARTESIAN_POINT('Ctrl Pts',(-1.00973405207762,3.8569177977272,10.6393417757422));
#36548=CARTESIAN_POINT('Ctrl Pts',(-3.7895693127859,1.2387663936115,10.7983066419269));
#36549=CARTESIAN_POINT('Ctrl Pts',(-3.0929058256244,-2.51581225614482,10.9572715081117));
#36550=CARTESIAN_POINT('Ctrl Pts',(0.441146911493231,-3.96241935650807,
11.1162363742964));
#36551=CARTESIAN_POINT('Ctrl Pts',(3.57049754163045,-1.77395745708877,11.2752012404812));
#36552=CARTESIAN_POINT('Ctrl Pts',(3.42432285260543,2.04190860605321,11.4341661066659));
#36553=CARTESIAN_POINT('Ctrl Pts',(0.136721492950909,3.98455580808139,11.5931309728507));
#36554=CARTESIAN_POINT('Ctrl Pts',(-3.27630628322196,2.27182633422323,11.7520958390354));
#36555=CARTESIAN_POINT('Ctrl Pts',(-3.683695752997,-1.52504536119478,11.9110607052202));
#36556=CARTESIAN_POINT('Ctrl Pts',(-0.711713421966334,-3.92286142494773,
12.0700255714049));
#36557=CARTESIAN_POINT('Ctrl Pts',(2.91318501009988,-2.72189839106446,12.2289904375897));
#36558=CARTESIAN_POINT('Ctrl Pts',(3.86556759564105,0.976096776902648,12.3879553037744));
#36559=CARTESIAN_POINT('Ctrl Pts',(1.27173165426137,3.77863419159615,12.5469201699592));
#36560=CARTESIAN_POINT('Ctrl Pts',(-2.48877340931887,3.11470458814592,12.7058850361439));
#36561=CARTESIAN_POINT('Ctrl Pts',(-3.96611198956382,-0.406612150074322,
12.8648499023287));
#36562=CARTESIAN_POINT('Ctrl Pts',(-1.80499399926681,-3.5549084962852,13.0238147685134));
#36563=CARTESIAN_POINT('Ctrl Pts',(2.01200065152342,-3.44198069904803,13.1827796346982));
#36564=CARTESIAN_POINT('Ctrl Pts',(3.98321358718988,-0.171427165804589,
13.3417445008829));
#36565=CARTESIAN_POINT('Ctrl Pts',(2.30028118194861,3.25639129072706,13.5007093670677));
#36566=CARTESIAN_POINT('Ctrl Pts',(-1.49289753065309,3.69684118097057,13.6596742332524));
#36567=CARTESIAN_POINT('Ctrl Pts',(-3.91651258901516,0.74585983564986,13.8186390994372));
#36568=CARTESIAN_POINT('Ctrl Pts',(-2.74717288447362,-2.88936306080816,
13.9776039656219));
#36569=CARTESIAN_POINT('Ctrl Pts',(0.942385426660244,-3.87392403926152,
14.1365688318067));
#36570=CARTESIAN_POINT('Ctrl Pts',(3.76741231340739,-1.30460040439068,14.2955336979914));
#36571=CARTESIAN_POINT('Ctrl Pts',(3.1362669786623,2.46154569181692,14.4544985641762));
#36572=CARTESIAN_POINT('Ctrl Pts',(-0.372046531241306,3.96950363810656,
14.6134634303609));
#36573=CARTESIAN_POINT('Ctrl Pts',(-3.53904967227374,1.83589356214594,14.7724282965457));
#36574=CARTESIAN_POINT('Ctrl Pts',(-3.45937733680892,-1.98194000815431,
14.9313931627304));
#36575=CARTESIAN_POINT('Ctrl Pts',(-0.206119829211681,-3.98156908396121,
15.0903580289152));
#36576=CARTESIAN_POINT('Ctrl Pts',(3.23622917375625,-2.32856146349605,15.2493228950999));
#36577=CARTESIAN_POINT('Ctrl Pts',(3.70970605913983,1.46063640552025,15.4082877612846));
#36578=CARTESIAN_POINT('Ctrl Pts',(0.779949646731194,3.90986653262151,15.5672526274694));
#36579=CARTESIAN_POINT('Ctrl Pts',(-2.86532184046814,2.77223889751338,15.7262174936541));
#36580=CARTESIAN_POINT('Ctrl Pts',(-3.88198649442593,-0.908602559673156,
15.8851823598389));
#36581=CARTESIAN_POINT('Ctrl Pts',(-1.33737014962086,-3.75590452983738,
16.0441472260236));
#36582=CARTESIAN_POINT('Ctrl Pts',(2.43413116992486,-3.15759136082396,16.2031120922084));
#36583=CARTESIAN_POINT('Ctrl Pts',(3.97259404474729,0.337452678146523,16.3620769583931));
#36584=CARTESIAN_POINT('Ctrl Pts',(1.86665380078734,3.52292227310739,16.5210418245779));
#36585=CARTESIAN_POINT('Ctrl Pts',(-1.95172895721992,3.47651144567355,16.6800066907626));
#36586=CARTESIAN_POINT('Ctrl Pts',(-3.97962242319515,0.240796850378547,
16.8389715569474));
#36587=CARTESIAN_POINT('Ctrl Pts',(-2.35666503270154,-3.21582146239366,
16.9979364231321));
#36588=CARTESIAN_POINT('Ctrl Pts',(1.42826443406275,-3.7222894112013,17.1569012893169));
#36589=CARTESIAN_POINT('Ctrl Pts',(3.90292376012977,-0.813980268166524,
17.3158661555016));
#36590=CARTESIAN_POINT('Ctrl Pts',(2.79709452794753,2.84106317354542,17.4748310216864));
#36591=CARTESIAN_POINT('Ctrl Pts',(-0.87475073969136,3.88975434928213,17.6337958878711));
#36592=CARTESIAN_POINT('Ctrl Pts',(-3.74411171420101,1.37003840308681,17.7927607540559));
#36593=CARTESIAN_POINT('Ctrl Pts',(-3.1786761163436,-2.40653192410502,17.9517256202406));
#36594=CARTESIAN_POINT('Ctrl Pts',(0.302833216085013,-3.97538297495793,
18.1106904864254));
#36595=CARTESIAN_POINT('Ctrl Pts',(3.5065275226793,-1.89727238082542,18.2696553526101));
#36596=CARTESIAN_POINT('Ctrl Pts',(3.49338172535042,1.92136979140851,18.4286202187948));
#36597=CARTESIAN_POINT('Ctrl Pts',(0.275455597698851,3.97737375262188,18.5875850849796));
#36598=CARTESIAN_POINT('Ctrl Pts',(-3.19516970536172,2.38458975681184,18.7465499511644));
#36599=CARTESIAN_POINT('Ctrl Pts',(-3.73459028221552,-1.3957840729596,18.9055148173491));
#36600=CARTESIAN_POINT('Ctrl Pts',(-0.847949117405149,-3.89568479841959,
19.0644796835338));
#36601=CARTESIAN_POINT('Ctrl Pts',(2.81658890100978,-2.82173788950715,19.2234445497186));
#36602=CARTESIAN_POINT('Ctrl Pts',(3.89722701433046,0.840832535700663,19.3824094159033));
#36603=CARTESIAN_POINT('Ctrl Pts',(1.40260268563389,3.73203476143841,19.5413742820881));
#36604=CARTESIAN_POINT('Ctrl Pts',(-2.3787500488546,3.19951964512964,19.7003391482728));
#36605=CARTESIAN_POINT('Ctrl Pts',(-3.97787021705804,-0.268190772315832,
19.8593040144576));
#36606=CARTESIAN_POINT('Ctrl Pts',(-1.92774697870435,-3.4898666651324,20.0182688806423));
#36607=CARTESIAN_POINT('Ctrl Pts',(1.89086481476229,-3.50998689564495,20.1772337468271));
#36608=CARTESIAN_POINT('Ctrl Pts',(3.97482324267393,-0.310093440809367,
20.3361986130118));
#36609=CARTESIAN_POINT('Ctrl Pts',(2.41233351706024,3.17427546962878,20.4951634791965));
#36610=CARTESIAN_POINT('Ctrl Pts',(-1.36319778790607,3.74660773920425,20.6541283453813));
#36611=CARTESIAN_POINT('Ctrl Pts',(-3.88815019533756,0.881853615583829,
20.813093211566));
#36612=CARTESIAN_POINT('Ctrl Pts',(-2.84616711491744,-2.79190087828212,
20.9720580777508));
#36613=CARTESIAN_POINT('Ctrl Pts',(0.806850527235046,-3.9044039261228,21.1310229439355));
#36614=CARTESIAN_POINT('Ctrl Pts',(3.71967457752779,-1.43506051902692,21.2899878101203));
#36615=CARTESIAN_POINT('Ctrl Pts',(3.22012038549849,2.35078763921597,21.448952676305));
#36616=CARTESIAN_POINT('Ctrl Pts',(-0.233528014234224,3.98005560769136,
21.6079175424898));
#36617=CARTESIAN_POINT('Ctrl Pts',(-3.47294089147738,1.95807523322667,21.7668824086745));
#36618=CARTESIAN_POINT('Ctrl Pts',(-3.52632583653101,-1.86021624962628,
21.9258472748593));
#36619=CARTESIAN_POINT('Ctrl Pts',(-0.344707483447601,-3.97197126386073,
22.0848121410441));
#36620=CARTESIAN_POINT('Ctrl Pts',(3.15313982968432,-2.43989387002868,22.2437770072288));
#36621=CARTESIAN_POINT('Ctrl Pts',(3.75834184644668,1.33050740634341,22.4027418734136));
#36622=CARTESIAN_POINT('Ctrl Pts',(0.915689325102905,3.88032175554439,22.5617067395983));
#36623=CARTESIAN_POINT('Ctrl Pts',(-2.76699741760937,2.87037799557025,22.720671605783));
#36624=CARTESIAN_POINT('Ctrl Pts',(-3.91129134187434,-0.7728027958352,22.8796364719677));
#36625=CARTESIAN_POINT('Ctrl Pts',(-1.46739644894177,-3.70704069007233,
23.0386013381526));
#36626=CARTESIAN_POINT('Ctrl Pts',(2.32262200499063,-3.24046036848089,23.1975662043372));
#36627=CARTESIAN_POINT('Ctrl Pts',(3.98198637087808,0.198816238648098,23.3565310705221));
#36628=CARTESIAN_POINT('Ctrl Pts',(1.98816433058814,3.45581133218519,23.5154959367067));
#36629=CARTESIAN_POINT('Ctrl Pts',(-1.82925354411967,3.5422830008711,23.6744608028915));
#36630=CARTESIAN_POINT('Ctrl Pts',(-3.96914826399699,0.379513463839679,
23.8334256690762));
#36631=CARTESIAN_POINT('Ctrl Pts',(-2.46663759784563,-3.13218185614485,
23.992390535261));
#36632=CARTESIAN_POINT('Ctrl Pts',(1.29650641132588,-3.76899081084458,24.1513554014457));
#36633=CARTESIAN_POINT('Ctrl Pts',(3.87454091099827,-0.951014904317504,
24.3103202676305));
#36634=CARTESIAN_POINT('Ctrl Pts',(2.88961752940844,2.74513957150359,24.4692851338152));
#36635=CARTESIAN_POINT('Ctrl Pts',(0.478408881098333,3.52136284087264,24.5752617112718));
#36636=CARTESIAN_POINT('Ctrl Pts',(-0.624728334461281,3.3133687646595,24.62825));
#36637=CARTESIAN_POINT('Ctrl Pts',(-1.56047750639987,3.20180677844002,-0.219489327336924));
#36638=CARTESIAN_POINT('Ctrl Pts',(-2.62647180561611,2.68226882971724,-0.166501038608675));
#36639=CARTESIAN_POINT('Ctrl Pts',(-4.1801468173981,0.503646678216414,-0.0605244611521764));
#36640=CARTESIAN_POINT('Ctrl Pts',(-2.683462008154,-3.24972419975438,0.0984404050325707));
#36641=CARTESIAN_POINT('Ctrl Pts',(1.27858859595154,-4.01162075153852,0.257405271217319));
#36642=CARTESIAN_POINT('Ctrl Pts',(4.06583468536472,-1.09841878093043,0.416370137402066));
#36643=CARTESIAN_POINT('Ctrl Pts',(3.12410178716573,2.82510367472183,0.575335003586814));
#36644=CARTESIAN_POINT('Ctrl Pts',(-0.684142221260432,4.15553253500754,
0.734299869771561));
#36645=CARTESIAN_POINT('Ctrl Pts',(-3.86450020240029,1.67445643711512,0.89326473595631));
#36646=CARTESIAN_POINT('Ctrl Pts',(-3.49975675527435,-2.3431216813317,1.05222960214106));
#36647=CARTESIAN_POINT('Ctrl Pts',(0.0756875806712427,-4.21095392107594,
1.2111944683258));
#36648=CARTESIAN_POINT('Ctrl Pts',(3.58165937251524,-2.21581878895911,1.37015933451055));
#36649=CARTESIAN_POINT('Ctrl Pts',(3.80188592579657,1.81213236997502,1.5291242006953));
#36650=CARTESIAN_POINT('Ctrl Pts',(0.534304277936582,4.17762976540319,1.68808906688005));
#36651=CARTESIAN_POINT('Ctrl Pts',(-3.22343533786296,2.71064199393843,1.8470539330648));
#36652=CARTESIAN_POINT('Ctrl Pts',(-4.02404256565933,-1.24305924958384,
2.00601879924955));
#36653=CARTESIAN_POINT('Ctrl Pts',(-1.1330470222017,-4.05639095560061,2.16498366543429));
#36654=CARTESIAN_POINT('Ctrl Pts',(2.79738949143739,-3.14844754849901,2.32394853161904));
#36655=CARTESIAN_POINT('Ctrl Pts',(4.1615397818786,0.647839440737169,2.48291339780379));
#36656=CARTESIAN_POINT('Ctrl Pts',(1.70795052048174,3.84980685419155,2.64187826398853));
#36657=CARTESIAN_POINT('Ctrl Pts',(-2.31248893740054,3.52001473505691,2.80084313017328));
#36658=CARTESIAN_POINT('Ctrl Pts',(-4.21148291955221,-0.0389906317936465,
2.95980799635803));
#36659=CARTESIAN_POINT('Ctrl Pts',(-2.2469203853454,-3.56222644534663,3.11877286254278));
#36660=CARTESIAN_POINT('Ctrl Pts',(1.77893597955331,-3.81752477372836,3.27773772872752));
#36661=CARTESIAN_POINT('Ctrl Pts',(4.17282096111768,-0.570678375934639,
3.43670259491227));
#36662=CARTESIAN_POINT('Ctrl Pts',(2.73861740129298,3.19970050005065,3.59566746109702));
#36663=CARTESIAN_POINT('Ctrl Pts',(-1.20795608026431,4.03471816744471,3.75463232728177));
#36664=CARTESIAN_POINT('Ctrl Pts',(-4.04636727494025,1.16834089733205,3.91359719346651));
#36665=CARTESIAN_POINT('Ctrl Pts',(-3.17269680384994,-2.76985623536663,
4.07256205965127));
#36666=CARTESIAN_POINT('Ctrl Pts',(0.611562062467236,-4.1670253683656,4.23152692583601));
#36667=CARTESIAN_POINT('Ctrl Pts',(3.83478230717035,-1.74142276094858,4.39049179202076));
#36668=CARTESIAN_POINT('Ctrl Pts',(3.5400260249384,2.28173712733952,4.54945665820551));
#36669=CARTESIAN_POINT('Ctrl Pts',(-0.00230142624457838,4.21166276895315,
4.70842152439025));
#36670=CARTESIAN_POINT('Ctrl Pts',(-3.54251758068034,2.27786693341294,4.867386390575));
#36671=CARTESIAN_POINT('Ctrl Pts',(-3.83287684714762,-1.74561268623704,
5.02635125675975));
#36672=CARTESIAN_POINT('Ctrl Pts',(-0.607007629585367,-4.16769124497425,
5.18531612294449));
#36673=CARTESIAN_POINT('Ctrl Pts',(3.17572203570494,-2.76638719772175,5.34428098912925));
#36674=CARTESIAN_POINT('Ctrl Pts',(4.04508799935564,1.17276240272716,5.50324585531399));
#36675=CARTESIAN_POINT('Ctrl Pts',(1.20354588769234,4.03603591064399,5.66221072149874));
#36676=CARTESIAN_POINT('Ctrl Pts',(-2.74211266207147,3.19670560488322,5.82117558768349));
#36677=CARTESIAN_POINT('Ctrl Pts',(-4.17219478365215,-0.575238440171331,
5.98014045386823));
#36678=CARTESIAN_POINT('Ctrl Pts',(-1.77476281483295,-3.81946665476637,
6.13910532005299));
#36679=CARTESIAN_POINT('Ctrl Pts',(2.2508121418228,-3.55976871130813,6.29807018623772));
#36680=CARTESIAN_POINT('Ctrl Pts',(4.21152300789809,-0.0343879300103317,
6.45703505242249));
#36681=CARTESIAN_POINT('Ctrl Pts',(2.30864061175677,3.52253986514459,6.61599991860723));
#36682=CARTESIAN_POINT('Ctrl Pts',(-1.71215691763581,3.84793805370841,6.77496478479197));
#36683=CARTESIAN_POINT('Ctrl Pts',(-4.16224524790261,0.643290814560192,
6.93392965097673));
#36684=CARTESIAN_POINT('Ctrl Pts',(-2.79394705497301,-3.1515025669977,7.09289451716147));
#36685=CARTESIAN_POINT('Ctrl Pts',(1.13747972501166,-4.05515085428062,7.25185938334622));
#36686=CARTESIAN_POINT('Ctrl Pts',(4.02539825555276,-1.23865954159255,7.41082424953096));
#36687=CARTESIAN_POINT('Ctrl Pts',(3.22047181083767,2.71416099216412,7.56978911571571));
#36688=CARTESIAN_POINT('Ctrl Pts',(-0.538871163521626,4.1770475751313,7.72875398190046));
#36689=CARTESIAN_POINT('Ctrl Pts',(-3.80386114665173,1.80796818356375,7.8877188480852));
#36690=CARTESIAN_POINT('Ctrl Pts',(-3.57924125016108,-2.21971634425003,
8.04668371426996));
#36691=CARTESIAN_POINT('Ctrl Pts',(-0.0710746766045851,-4.21106363833782,
8.2056485804547));
#36692=CARTESIAN_POINT('Ctrl Pts',(3.50229482737133,-2.33923908952323,8.36461344663945));
#36693=CARTESIAN_POINT('Ctrl Pts',(3.86270724386325,1.6785712150492,8.5235783128242));
#36694=CARTESIAN_POINT('Ctrl Pts',(0.679525180800456,4.15648338195204,8.68254317900894));
#36695=CARTESIAN_POINT('Ctrl Pts',(-3.12704393372178,2.82129488220555,8.8415080451937));
#36696=CARTESIAN_POINT('Ctrl Pts',(-4.06490596761654,-1.10211072502764,
9.00047291137844));
#36697=CARTESIAN_POINT('Ctrl Pts',(-1.27367919478393,-4.0144551167699,9.15943777756319));
#36698=CARTESIAN_POINT('Ctrl Pts',(2.68600334712891,-3.24399361821161,9.31840264374794));
#36699=CARTESIAN_POINT('Ctrl Pts',(4.18158337439399,0.502462992445402,9.47736750993269));
#36700=CARTESIAN_POINT('Ctrl Pts',(1.84103634728762,3.7879669670882,9.63633237611743));
#36701=CARTESIAN_POINT('Ctrl Pts',(-2.18845209448917,3.59844216375801,9.79529724230219));
#36702=CARTESIAN_POINT('Ctrl Pts',(-4.21028469511404,0.107756029408409,
9.95426210848692));
#36703=CARTESIAN_POINT('Ctrl Pts',(-2.36966004463275,-3.48178400373378,
10.1132269746717));
#36704=CARTESIAN_POINT('Ctrl Pts',(1.64485812726998,-3.87718329679412,10.2721918408564));
#36705=CARTESIAN_POINT('Ctrl Pts',(4.15040608438235,-0.71570797851312,10.4311567070412));
#36706=CARTESIAN_POINT('Ctrl Pts',(2.84842860401989,3.1023479920194,10.5901215732259));
#36707=CARTESIAN_POINT('Ctrl Pts',(-1.06665808689608,4.07435259905726,10.7490864394107));
#36708=CARTESIAN_POINT('Ctrl Pts',(-4.00320732475952,1.30860218965774,10.9080513055954));
#36709=CARTESIAN_POINT('Ctrl Pts',(-3.26726924195739,-2.657641863823,11.0670161717801));
#36710=CARTESIAN_POINT('Ctrl Pts',(0.466016689924724,-4.18580183722271,
11.2259810379649));
#36711=CARTESIAN_POINT('Ctrl Pts',(3.77178532227006,-1.87396479649261,11.3849459041496));
#36712=CARTESIAN_POINT('Ctrl Pts',(3.61736999495961,2.15702176515476,11.5439107703344));
#36713=CARTESIAN_POINT('Ctrl Pts',(0.144429204708414,4.20918623734002,11.7028756365191));
#36714=CARTESIAN_POINT('Ctrl Pts',(-3.4610089507791,2.39990116846763,11.8618405027039));
#36715=CARTESIAN_POINT('Ctrl Pts',(-3.89136511392694,-1.61102021275272,
12.0208053688886));
#36716=CARTESIAN_POINT('Ctrl Pts',(-0.751836461819641,-4.14401381639395,
12.1797702350734));
#36717=CARTESIAN_POINT('Ctrl Pts',(3.07741661604235,-2.87534616126336,12.3387351012581));
#36718=CARTESIAN_POINT('Ctrl Pts',(4.08349003170681,1.03112450108435,12.4976999674429));
#36719=CARTESIAN_POINT('Ctrl Pts',(1.34342587594075,3.99165573310602,12.6566648336276));
#36720=CARTESIAN_POINT('Ctrl Pts',(-2.62907869457274,3.29029691570976,12.8156296998124));
#36721=CARTESIAN_POINT('Ctrl Pts',(-4.18970264348228,-0.429535021835278,
12.9745945659971));
#36722=CARTESIAN_POINT('Ctrl Pts',(-1.90675103226963,-3.75531744020717,
13.1335594321819));
#36723=CARTESIAN_POINT('Ctrl Pts',(2.12542774146498,-3.63602330735055,13.2925242983666));
#36724=CARTESIAN_POINT('Ctrl Pts',(4.2077683483767,-0.181091419411761,13.4514891645514));
#36725=CARTESIAN_POINT('Ctrl Pts',(2.42996016605737,3.43997124510655,13.6104540307361));
#36726=CARTESIAN_POINT('Ctrl Pts',(-1.577060039425,3.90525161901692,13.7694188969209));
#36727=CARTESIAN_POINT('Ctrl Pts',(-4.13730706309004,0.787907888963343,
13.9283837631056));
#36728=CARTESIAN_POINT('Ctrl Pts',(-2.90204551118784,-3.05225169780932,
14.0873486292903));
#36729=CARTESIAN_POINT('Ctrl Pts',(0.995512664202879,-4.09231757213405,
14.2463134954751));
#36730=CARTESIAN_POINT('Ctrl Pts',(3.97980121844884,-1.37814761089607,14.4052783616599));
#36731=CARTESIAN_POINT('Ctrl Pts',(3.3130748919202,2.60031600701019,14.5642432278446));
#36732=CARTESIAN_POINT('Ctrl Pts',(-0.393020756736522,4.19328549714417,
14.7232080940294));
#36733=CARTESIAN_POINT('Ctrl Pts',(-3.73856457063159,1.9393925665021,14.8821729602141));
#36734=CARTESIAN_POINT('Ctrl Pts',(-3.65440068534852,-2.09367242106057,
15.0411378263989));
#36735=CARTESIAN_POINT('Ctrl Pts',(-0.217739891257386,-4.20603113582635,
15.2001026925836));
#36736=CARTESIAN_POINT('Ctrl Pts',(3.41867248324782,-2.45983475625287,15.3590675587684));
#36737=CARTESIAN_POINT('Ctrl Pts',(3.91884175823025,1.5429801844924,15.5180324249531));
#36738=CARTESIAN_POINT('Ctrl Pts',(0.823919522517587,4.13028633343982,15.6769972911379));
#36739=CARTESIAN_POINT('Ctrl Pts',(-3.02685514706235,2.92852462760477,15.8359621573226));
#36740=CARTESIAN_POINT('Ctrl Pts',(-4.10083455042517,-0.95982527880059,
15.9949270235073));
#36741=CARTESIAN_POINT('Ctrl Pts',(-1.41276475952385,-3.96764468041594,
16.1538918896921));
#36742=CARTESIAN_POINT('Ctrl Pts',(2.57135598390867,-3.3356014419895,16.3128567558768));
#36743=CARTESIAN_POINT('Ctrl Pts',(4.196550126309,0.356476665661734,16.4718216220616));
#36744=CARTESIAN_POINT('Ctrl Pts',(1.97188692205462,3.72152798490289,16.6307864882463));
#36745=CARTESIAN_POINT('Ctrl Pts',(-2.06175821382304,3.67250073431153,16.7897513544311));
#36746=CARTESIAN_POINT('Ctrl Pts',(-4.20397473152436,0.254371839027192,
16.9487162206158));
#36747=CARTESIAN_POINT('Ctrl Pts',(-2.48952267189958,-3.39711428154593,
17.1076810868006));
#36748=CARTESIAN_POINT('Ctrl Pts',(1.50878323424311,-3.93213450022406,17.2666459529853));
#36749=CARTESIAN_POINT('Ctrl Pts',(4.1229521602399,-0.859868629593263,17.4256108191701));
#36750=CARTESIAN_POINT('Ctrl Pts',(2.95478150103885,3.00122889112179,17.5845756853548));
#36751=CARTESIAN_POINT('Ctrl Pts',(-0.924065053159552,4.10904032023471,
17.7435405515396));
#36752=CARTESIAN_POINT('Ctrl Pts',(-3.95518704155557,1.44727469476127,17.9025054177243));
#36753=CARTESIAN_POINT('Ctrl Pts',(-3.35787485639895,-2.54220082301716,
18.0614702839091));
#36754=CARTESIAN_POINT('Ctrl Pts',(0.319905521907667,-4.1994962832271,18.2204351500938));
#36755=CARTESIAN_POINT('Ctrl Pts',(3.70420897591159,-2.00423163296111,18.3794000162786));
#36756=CARTESIAN_POINT('Ctrl Pts',(3.69032208064376,2.02968754169158,18.5383648824633));
#36757=CARTESIAN_POINT('Ctrl Pts',(0.290984482757316,4.20159929152924,18.6973297486481));
#36758=CARTESIAN_POINT('Ctrl Pts',(-3.37529827603299,2.51902166000967,18.8562946148328));
#36759=CARTESIAN_POINT('Ctrl Pts',(-3.94512883622391,-1.47447178385209,
19.0152594810176));
#36760=CARTESIAN_POINT('Ctrl Pts',(-0.895752482047657,-4.11530510007291,
19.1742243472023));
#36761=CARTESIAN_POINT('Ctrl Pts',(2.9753748747426,-2.98081413888224,19.333189213387));
#36762=CARTESIAN_POINT('Ctrl Pts',(4.1169342588298,0.888234701092859,19.4921540795718));
#36763=CARTESIAN_POINT('Ctrl Pts',(1.48167479769069,3.94242924726034,19.6511189457566));
#36764=CARTESIAN_POINT('Ctrl Pts',(-2.5128527369107,3.37989344485135,19.8100838119413));
#36765=CARTESIAN_POINT('Ctrl Pts',(-4.20212374428449,-0.283310100845846,
19.9690486781261));
#36766=CARTESIAN_POINT('Ctrl Pts',(-2.03642424467465,-3.68660885793949,
20.1280135443108));
#36767=CARTESIAN_POINT('Ctrl Pts',(1.9974628385994,-3.70786337197934,20.2869784104955));
#36768=CARTESIAN_POINT('Ctrl Pts',(4.1989049958817,-0.327575043797077,20.4459432766802));
#36769=CARTESIAN_POINT('Ctrl Pts',(2.54832948237039,3.35322612201562,20.6049081428651));
#36770=CARTESIAN_POINT('Ctrl Pts',(-1.44004843801888,3.95782378065465,20.7638730090497));
#36771=CARTESIAN_POINT('Ctrl Pts',(-4.10734573167046,0.931568355633416,
20.9228378752345));
#36772=CARTESIAN_POINT('Ctrl Pts',(-3.00662056859199,-2.94929505794555,
21.0818027414192));
#36773=CARTESIAN_POINT('Ctrl Pts',(0.852336947556435,-4.12451577099776,
21.240767607604));
#36774=CARTESIAN_POINT('Ctrl Pts',(3.92937225458326,-1.51596245036574,21.3997324737888));
#36775=CARTESIAN_POINT('Ctrl Pts',(3.4016555576228,2.48331393874026,21.5586973399735));
#36776=CARTESIAN_POINT('Ctrl Pts',(-0.246693220246651,4.20443233691565,
21.7176622061583));
#36777=CARTESIAN_POINT('Ctrl Pts',(-3.66872888914082,2.0684622628846,21.876627072343));
#36778=CARTESIAN_POINT('Ctrl Pts',(-3.72512342515035,-1.96508645217684,
22.0355919385278));
#36779=CARTESIAN_POINT('Ctrl Pts',(-0.364140462606384,-4.19589223597873,
22.1945568047125));
#36780=CARTESIAN_POINT('Ctrl Pts',(3.33089895455792,-2.57744355781532,22.3535216708973));
#36781=CARTESIAN_POINT('Ctrl Pts',(3.97021940141924,1.4055151272072,22.512486537082));
#36782=CARTESIAN_POINT('Ctrl Pts',(0.967311562579962,4.09907596143147,22.6714514032667));
#36783=CARTESIAN_POINT('Ctrl Pts',(-2.92298765783001,3.03219634429854,22.8304162694515));
#36784=CARTESIAN_POINT('Ctrl Pts',(-4.13179146670604,-0.816369765937287,
22.9893811356362));
#36785=CARTESIAN_POINT('Ctrl Pts',(-1.5501213272205,-3.91602612824874,23.148346001821));
#36786=CARTESIAN_POINT('Ctrl Pts',(2.45356045914115,-3.42314221273843,23.3073108680058));
#36787=CARTESIAN_POINT('Ctrl Pts',(4.20647194740789,0.210024558767638,23.4662757341905));
#36788=CARTESIAN_POINT('Ctrl Pts',(2.10024764138301,3.65063364623366,23.6252406003752));
#36789=CARTESIAN_POINT('Ctrl Pts',(-1.93237821563391,3.74198017901762,23.78420546656));
#36790=CARTESIAN_POINT('Ctrl Pts',(-4.19291008872147,0.400908639713182,
23.9431703327447));
#36791=CARTESIAN_POINT('Ctrl Pts',(-2.60569497064129,-3.30875946949763,
24.1021351989295));
#36792=CARTESIAN_POINT('Ctrl Pts',(1.36959731674678,-3.98146870411307,24.2611000651142));
#36793=CARTESIAN_POINT('Ctrl Pts',(4.09296922018457,-1.00462863103577,24.420064931299));
#36794=CARTESIAN_POINT('Ctrl Pts',(3.05252051214689,2.89989756964007,24.5790297974837));
#36795=CARTESIAN_POINT('Ctrl Pts',(0.505379313311694,3.71988063924714,24.6850063749402));
#36796=CARTESIAN_POINT('Ctrl Pts',(-0.659947566089433,3.50016083979823,
24.7379946636685));
#36797=CARTESIAN_POINT('Ctrl Pts',(-1.64375505990927,3.37267667834226,-0.109744663668463));
#36798=CARTESIAN_POINT('Ctrl Pts',(-2.76663796977808,2.82541269758923,-0.0567563749402136));
#36799=CARTESIAN_POINT('Ctrl Pts',(-4.40322750829897,0.530524645391819,
0.0492202025162849));
#36800=CARTESIAN_POINT('Ctrl Pts',(-2.82666955203587,-3.42315129487488,
0.208185068701033));
#36801=CARTESIAN_POINT('Ctrl Pts',(1.34682266518943,-4.22570776043514,0.36714993488578));
#36802=CARTESIAN_POINT('Ctrl Pts',(4.28281491364878,-1.15703777955712,0.526114801070528));
#36803=CARTESIAN_POINT('Ctrl Pts',(3.29082482718549,2.97587016861638,0.685079667255276));
#36804=CARTESIAN_POINT('Ctrl Pts',(-0.720652642080601,4.37729964259146,
0.844044533440024));
#36805=CARTESIAN_POINT('Ctrl Pts',(-4.07073587133658,1.76381667138256,1.00300939962477));
#36806=CARTESIAN_POINT('Ctrl Pts',(-3.68652726575071,-2.46816638104435,
1.16197426580952));
#36807=CARTESIAN_POINT('Ctrl Pts',(0.0797267779832985,-4.43567868580324,
1.32093913199426));
#36808=CARTESIAN_POINT('Ctrl Pts',(3.7728007563697,-2.33406975189055,1.47990399817901));
#36809=CARTESIAN_POINT('Ctrl Pts',(4.00478007667258,1.90883991608689,1.63886886436376));
#36810=CARTESIAN_POINT('Ctrl Pts',(0.562818340403771,4.40057612951542,1.79783373054851));
#36811=CARTESIAN_POINT('Ctrl Pts',(-3.39545948286473,2.85530004429109,1.95679859673326));
#36812=CARTESIAN_POINT('Ctrl Pts',(-4.23879248593139,-1.30939723443016,
2.11576346291801));
#36813=CARTESIAN_POINT('Ctrl Pts',(-1.19351401620389,-4.27286720307909,
2.27472832910275));
#36814=CARTESIAN_POINT('Ctrl Pts',(2.94667697049707,-3.31646984174982,2.4336931952875));
#36815=CARTESIAN_POINT('Ctrl Pts',(4.3836274764756,0.682412501528009,2.59265806147225));
#36816=CARTESIAN_POINT('Ctrl Pts',(1.79909822384654,4.05525838744716,2.751622927657));
#36817=CARTESIAN_POINT('Ctrl Pts',(-2.43589886829313,3.70786634730399,2.91058779384175));
#36818=CARTESIAN_POINT('Ctrl Pts',(-4.43623591518879,-0.041071433607366,
3.06955266002649));
#36819=CARTESIAN_POINT('Ctrl Pts',(-2.36683113821078,-3.75233075777553,
3.22851752621124));
#36820=CARTESIAN_POINT('Ctrl Pts',(1.87387194346144,-4.02125351849637,3.38748239239599));
#36821=CARTESIAN_POINT('Ctrl Pts',(4.39551069515703,-0.601133604410289,
3.54644725858073));
#36822=CARTESIAN_POINT('Ctrl Pts',(2.88476840715019,3.37045799480092,3.70541212476548));
#36823=CARTESIAN_POINT('Ctrl Pts',(-1.27242072438679,4.25003780948162,3.86437699095023));
#36824=CARTESIAN_POINT('Ctrl Pts',(-4.26230859154076,1.23069140940013,4.02334185713497));
#36825=CARTESIAN_POINT('Ctrl Pts',(-3.34201320012482,-2.91767435508194,
4.18230672331973));
#36826=CARTESIAN_POINT('Ctrl Pts',(0.64419911886348,-4.38940581067625,4.34127158950447));
#36827=CARTESIAN_POINT('Ctrl Pts',(4.03943202975366,-1.834356767727,4.50023645568922));
#36828=CARTESIAN_POINT('Ctrl Pts',(3.72894557392732,2.40350593524421,4.65920132187397));
#36829=CARTESIAN_POINT('Ctrl Pts',(-0.00242424579594498,4.43642536256088,
4.81816618805872));
#36830=CARTESIAN_POINT('Ctrl Pts',(-3.73157009580673,2.39942920179332,4.97713105424346));
#36831=CARTESIAN_POINT('Ctrl Pts',(-4.03742488159485,-1.83877029555123,
5.13609592042822));
#36832=CARTESIAN_POINT('Ctrl Pts',(-0.639401630874114,-4.39010722293004,
5.29506078661295));
#36833=CARTESIAN_POINT('Ctrl Pts',(3.34519987865668,-2.91402018630447,5.45402565279771));
#36834=CARTESIAN_POINT('Ctrl Pts',(4.26096104522458,1.23534887599985,5.61299051898245));
#36835=CARTESIAN_POINT('Ctrl Pts',(1.26777517433839,4.25142587630257,5.77195538516721));
#36836=CARTESIAN_POINT('Ctrl Pts',(-2.88845019850368,3.3673032719259,5.93092025135195));
#36837=CARTESIAN_POINT('Ctrl Pts',(-4.39485110065909,-0.605937024281373,
6.0898851175367));
#36838=CARTESIAN_POINT('Ctrl Pts',(-1.86947607066172,-4.02329903134028,
6.24884998372145));
#36839=CARTESIAN_POINT('Ctrl Pts',(2.37093058493492,-3.74974186255266,6.40781484990618));
#36840=CARTESIAN_POINT('Ctrl Pts',(4.43627814291787,-0.0362231007639915,
6.56677971609095));
#36841=CARTESIAN_POINT('Ctrl Pts',(2.43184517016341,3.71052623528157,6.72574458227568));
#36842=CARTESIAN_POINT('Ctrl Pts',(-1.80352910258568,4.05328985522703,6.88470944846044));
#36843=CARTESIAN_POINT('Ctrl Pts',(-4.38437059090167,0.677621130128278,
7.04367431464518));
#36844=CARTESIAN_POINT('Ctrl Pts',(-2.94305082251765,-3.31968789654059,
7.20263918082993));
#36845=CARTESIAN_POINT('Ctrl Pts',(1.19818327778767,-4.27156092162922,7.36160404701468));
#36846=CARTESIAN_POINT('Ctrl Pts',(4.2402205245368,-1.30476272849002,7.52056891319943));
#36847=CARTESIAN_POINT('Ctrl Pts',(3.39233780214647,2.85900683988128,7.67953377938417));
#36848=CARTESIAN_POINT('Ctrl Pts',(-0.567628945656141,4.39996286966301,
7.83849864556892));
#36849=CARTESIAN_POINT('Ctrl Pts',(-4.00686070857005,1.90445350073909,7.99746351175367));
#36850=CARTESIAN_POINT('Ctrl Pts',(-3.77025358677652,-2.33817530689181,
8.15642837793842));
#36851=CARTESIAN_POINT('Ctrl Pts',(-0.0748676983942658,-4.43579425831462,
8.31539324412316));
#36852=CARTESIAN_POINT('Ctrl Pts',(3.68920078641008,-2.4640765880774,8.47435811030792));
#36853=CARTESIAN_POINT('Ctrl Pts',(4.06884722849785,1.76815104148521,8.63332297649266));
#36854=CARTESIAN_POINT('Ctrl Pts',(0.715789205352545,4.37830123311092,8.79228784267741));
#36855=CARTESIAN_POINT('Ctrl Pts',(-3.29392398642918,2.97185811336718,8.95125270886215));
#36856=CARTESIAN_POINT('Ctrl Pts',(-4.28183663328808,-1.16092675057133,
9.1102175750469));
#36857=CARTESIAN_POINT('Ctrl Pts',(-1.34165126542409,-4.22869338641924,
9.26918244123165));
#36858=CARTESIAN_POINT('Ctrl Pts',(2.82934651391571,-3.41711489103788,9.42814730741641));
#36859=CARTESIAN_POINT('Ctrl Pts',(4.40474072961818,0.529277790203311,9.58711217360113));
#36860=CARTESIAN_POINT('Ctrl Pts',(1.93928640362945,3.99011830890487,9.74607703978591));
#36861=CARTESIAN_POINT('Ctrl Pts',(-2.30524258692121,3.79047918999758,9.90504190597063));
#36862=CARTESIAN_POINT('Ctrl Pts',(-4.43497374545224,0.113506614385248,
10.0640067721554));
#36863=CARTESIAN_POINT('Ctrl Pts',(-2.49612100953394,-3.66759536755666,
10.2229716383401));
#36864=CARTESIAN_POINT('Ctrl Pts',(1.73263879706324,-4.08409582077491,10.3819365045249));
#36865=CARTESIAN_POINT('Ctrl Pts',(4.3718996101527,-0.753902960006452,10.5409013707096));
#36866=CARTESIAN_POINT('Ctrl Pts',(3.00043987269634,3.26791010352089,10.6998662368944));
#36867=CARTESIAN_POINT('Ctrl Pts',(-1.12358212171453,4.29178740038732,10.8588311030791));
#36868=CARTESIAN_POINT('Ctrl Pts',(-4.21684533673315,1.37843798570399,11.0177959692639));
#36869=CARTESIAN_POINT('Ctrl Pts',(-3.44163265829037,-2.79947147150118,
11.1767608354486));
#36870=CARTESIAN_POINT('Ctrl Pts',(0.490886468356214,-4.40918431793734,
11.3357257016334));
#36871=CARTESIAN_POINT('Ctrl Pts',(3.97307310290967,-1.97397213589646,11.4946905678181));
#36872=CARTESIAN_POINT('Ctrl Pts',(3.8104171373138,2.27213492425632,11.6536554340029));
#36873=CARTESIAN_POINT('Ctrl Pts',(0.152136916465922,4.43381666659865,11.8126203001876));
#36874=CARTESIAN_POINT('Ctrl Pts',(-3.64571161833625,2.52797600271203,11.9715851663724));
#36875=CARTESIAN_POINT('Ctrl Pts',(-4.09903447485687,-1.69699506431066,
12.1305500325571));
#36876=CARTESIAN_POINT('Ctrl Pts',(-0.791959501672948,-4.36516620784018,
12.2895148987418));
#36877=CARTESIAN_POINT('Ctrl Pts',(3.24164822198482,-3.02879393146226,12.4484797649266));
#36878=CARTESIAN_POINT('Ctrl Pts',(4.30141246777259,1.08615222526604,12.6074446311113));
#36879=CARTESIAN_POINT('Ctrl Pts',(1.41512009762014,4.2046772746159,12.7664094972961));
#36880=CARTESIAN_POINT('Ctrl Pts',(-2.76938397982661,3.4658892432736,12.9253743634808));
#36881=CARTESIAN_POINT('Ctrl Pts',(-4.41329329740075,-0.452457893596237,
13.0843392296656));
#36882=CARTESIAN_POINT('Ctrl Pts',(-2.00850806527244,-3.95572638412914,
13.2433040958503));
#36883=CARTESIAN_POINT('Ctrl Pts',(2.23885483140653,-3.83006591565308,13.4022689620351));
#36884=CARTESIAN_POINT('Ctrl Pts',(4.43232310956353,-0.19075567301893,13.5612338282198));
#36885=CARTESIAN_POINT('Ctrl Pts',(2.55963915016612,3.62355119948605,13.7201986944046));
#36886=CARTESIAN_POINT('Ctrl Pts',(-1.66122254819691,4.11366205706328,13.8791635605893));
#36887=CARTESIAN_POINT('Ctrl Pts',(-4.35810153716492,0.829955942276827,
14.0381284267741));
#36888=CARTESIAN_POINT('Ctrl Pts',(-3.05691813790205,-3.21514033481048,
14.1970932929588));
#36889=CARTESIAN_POINT('Ctrl Pts',(1.04863990174551,-4.31071110500657,14.3560581591436));
#36890=CARTESIAN_POINT('Ctrl Pts',(4.19219012349031,-1.45169481740146,14.5150230253283));
#36891=CARTESIAN_POINT('Ctrl Pts',(3.48988280517811,2.73908632220345,14.6739878915131));
#36892=CARTESIAN_POINT('Ctrl Pts',(-0.413994982231739,4.41706735618179,
14.8329527576978));
#36893=CARTESIAN_POINT('Ctrl Pts',(-3.93807946898943,2.04289157085825,14.9919176238826));
#36894=CARTESIAN_POINT('Ctrl Pts',(-3.84942403388813,-2.20540483396684,
15.1508824900673));
#36895=CARTESIAN_POINT('Ctrl Pts',(-0.229359953303091,-4.4304931876915,
15.3098473562521));
#36896=CARTESIAN_POINT('Ctrl Pts',(3.60111579273939,-2.5911080490097,15.4688122224368));
#36897=CARTESIAN_POINT('Ctrl Pts',(4.12797745732068,1.62532396346455,15.6277770886216));
#36898=CARTESIAN_POINT('Ctrl Pts',(0.867889398303981,4.35070613425814,15.7867419548063));
#36899=CARTESIAN_POINT('Ctrl Pts',(-3.18838845365656,3.08481035769615,15.9457068209911));
#36900=CARTESIAN_POINT('Ctrl Pts',(-4.31968260642442,-1.01104799792802,
16.1046716871758));
#36901=CARTESIAN_POINT('Ctrl Pts',(-1.48815936942683,-4.1793848309945,16.2636365533605));
#36902=CARTESIAN_POINT('Ctrl Pts',(2.70858079789248,-3.51361152315505,16.4226014195453));
#36903=CARTESIAN_POINT('Ctrl Pts',(4.42050620787071,0.375500653176939,16.5815662857301));
#36904=CARTESIAN_POINT('Ctrl Pts',(2.07712004332191,3.92013369669841,16.7405311519148));
#36905=CARTESIAN_POINT('Ctrl Pts',(-2.17178747042617,3.8684900229495,16.8994960180995));
#36906=CARTESIAN_POINT('Ctrl Pts',(-4.42832703985357,0.267946827675841,
17.0584608842843));
#36907=CARTESIAN_POINT('Ctrl Pts',(-2.62238031109761,-3.57840710069821,
17.217425750469));
#36908=CARTESIAN_POINT('Ctrl Pts',(1.58930203442347,-4.14197958924682,17.3763906166538));
#36909=CARTESIAN_POINT('Ctrl Pts',(4.34298056035004,-0.905756991020003,
17.5353554828385));
#36910=CARTESIAN_POINT('Ctrl Pts',(3.11246847413016,3.16139460869816,17.6943203490233));
#36911=CARTESIAN_POINT('Ctrl Pts',(-0.973379366627741,4.32832629118729,
17.853285215208));
#36912=CARTESIAN_POINT('Ctrl Pts',(-4.16626236891013,1.52451098643573,18.0122500813928));
#36913=CARTESIAN_POINT('Ctrl Pts',(-3.53707359645429,-2.67786972192929,
18.1712149475776));
#36914=CARTESIAN_POINT('Ctrl Pts',(0.336977827730321,-4.42360959149628,
18.3301798137622));
#36915=CARTESIAN_POINT('Ctrl Pts',(3.90189042914389,-2.11119088509681,18.489144679947));
#36916=CARTESIAN_POINT('Ctrl Pts',(3.88726243593711,2.13800529197465,18.6481095461317));
#36917=CARTESIAN_POINT('Ctrl Pts',(0.306513367815784,4.42582483043659,18.8070744123165));
#36918=CARTESIAN_POINT('Ctrl Pts',(-3.55542684670427,2.6534535632075,18.9660392785013));
#36919=CARTESIAN_POINT('Ctrl Pts',(-4.15566739023229,-1.5531594947446,19.125004144686));
#36920=CARTESIAN_POINT('Ctrl Pts',(-0.943555846690173,-4.33492540172624,
19.2839690108708));
#36921=CARTESIAN_POINT('Ctrl Pts',(3.13416084847543,-3.13989038825732,19.4429338770555));
#36922=CARTESIAN_POINT('Ctrl Pts',(4.33664150332913,0.935636866485059,19.6018987432403));
#36923=CARTESIAN_POINT('Ctrl Pts',(1.5607469097475,4.15282373308227,19.760863609425));
#36924=CARTESIAN_POINT('Ctrl Pts',(-2.6469554249668,3.56026724457307,19.9198284756097));
#36925=CARTESIAN_POINT('Ctrl Pts',(-4.42637727151094,-0.298429429375862,
20.0787933417945));
#36926=CARTESIAN_POINT('Ctrl Pts',(-2.14510151064494,-3.88335105074656,
20.2377582079792));
#36927=CARTESIAN_POINT('Ctrl Pts',(2.10406086243651,-3.90573984831374,20.396723074164));
#36928=CARTESIAN_POINT('Ctrl Pts',(4.42298674908946,-0.345056646784782,
20.5556879403487));
#36929=CARTESIAN_POINT('Ctrl Pts',(2.68432544768054,3.53217677440245,20.7146528065335));
#36930=CARTESIAN_POINT('Ctrl Pts',(-1.51689908813168,4.16903982210505,20.8736176727182));
#36931=CARTESIAN_POINT('Ctrl Pts',(-4.32654126800335,0.981283095682997,
21.032582538903));
#36932=CARTESIAN_POINT('Ctrl Pts',(-3.16707402226655,-3.10668923760898,
21.1915474050877));
#36933=CARTESIAN_POINT('Ctrl Pts',(0.897823367877824,-4.34462761587273,
21.3505122712725));
#36934=CARTESIAN_POINT('Ctrl Pts',(4.13906993163872,-1.59686438170456,21.5094771374572));
#36935=CARTESIAN_POINT('Ctrl Pts',(3.58319072974711,2.61584023826454,21.668442003642));
#36936=CARTESIAN_POINT('Ctrl Pts',(-0.25985842625908,4.42880906613994,21.8274068698267));
#36937=CARTESIAN_POINT('Ctrl Pts',(-3.86451688680425,2.17884929254253,21.9863717360115));
#36938=CARTESIAN_POINT('Ctrl Pts',(-3.92392101376968,-2.0699566547274,22.1453366021962));
#36939=CARTESIAN_POINT('Ctrl Pts',(-0.383573441765164,-4.41981320809673,
22.304301468381));
#36940=CARTESIAN_POINT('Ctrl Pts',(3.50865807943151,-2.71499324560195,22.4632663345657));
#36941=CARTESIAN_POINT('Ctrl Pts',(4.1820969563918,1.48052284807099,22.6222312007505));
#36942=CARTESIAN_POINT('Ctrl Pts',(1.01893380005702,4.31783016731854,22.7811960669352));
#36943=CARTESIAN_POINT('Ctrl Pts',(-3.07897789805066,3.19401469302683,22.9401609331199));
#36944=CARTESIAN_POINT('Ctrl Pts',(-4.35229159153774,-0.859936736039379,
23.0991257993047));
#36945=CARTESIAN_POINT('Ctrl Pts',(-1.63284620549922,-4.12501156642513,
23.2580906654894));
#36946=CARTESIAN_POINT('Ctrl Pts',(2.58449891329166,-3.60582405699598,23.4170555316742));
#36947=CARTESIAN_POINT('Ctrl Pts',(4.43095752393771,0.221232878887186,23.5760203978589));
#36948=CARTESIAN_POINT('Ctrl Pts',(2.21233095217787,3.84545596028211,23.7349852640437));
#36949=CARTESIAN_POINT('Ctrl Pts',(-2.03550288714815,3.94167735716416,23.8939501302284));
#36950=CARTESIAN_POINT('Ctrl Pts',(-4.41667191344595,0.422303815586678,
24.0529149964132));
#36951=CARTESIAN_POINT('Ctrl Pts',(-2.74475234343696,-3.48533708285041,
24.2118798625979));
#36952=CARTESIAN_POINT('Ctrl Pts',(1.44268822216767,-4.19394659738156,24.3708447287827));
#36953=CARTESIAN_POINT('Ctrl Pts',(4.31139752937088,-1.05824235775403,24.5298095949674));
#36954=CARTESIAN_POINT('Ctrl Pts',(3.21542349488533,3.05465556777655,24.6887744611522));
#36955=CARTESIAN_POINT('Ctrl Pts',(0.532349745525053,3.91839843762163,24.7947510386087));
#36956=CARTESIAN_POINT('Ctrl Pts',(-0.695166797717585,3.68695291493697,
24.8477393273369));
#36957=CARTESIAN_POINT('Ctrl Pts',(-1.72703261341866,3.5435465782445,-1.38777878078145E-15));
#36958=CARTESIAN_POINT('Ctrl Pts',(-2.90680413394004,2.96855656546122,0.0529882887282479));
#36959=CARTESIAN_POINT('Ctrl Pts',(-4.62630819919985,0.557402612567225,
0.158964866184747));
#36960=CARTESIAN_POINT('Ctrl Pts',(-2.96987709591773,-3.59657838999538,
0.317929732369494));
#36961=CARTESIAN_POINT('Ctrl Pts',(1.41505673442732,-4.43979476933175,0.476894598554242));
#36962=CARTESIAN_POINT('Ctrl Pts',(4.49979514193284,-1.21565677818381,0.635859464738989));
#36963=CARTESIAN_POINT('Ctrl Pts',(3.45754786720525,3.12663666251093,0.794824330923737));
#36964=CARTESIAN_POINT('Ctrl Pts',(-0.757163062900767,4.59906675017539,
0.953789197108486));
#36965=CARTESIAN_POINT('Ctrl Pts',(-4.27697154027288,1.85317690565,1.11275406329323));
#36966=CARTESIAN_POINT('Ctrl Pts',(-3.87329777622707,-2.593211080757,1.27171892947798));
#36967=CARTESIAN_POINT('Ctrl Pts',(0.0837659752953463,-4.66040345053054,
1.43068379566273));
#36968=CARTESIAN_POINT('Ctrl Pts',(3.96394214022417,-2.45232071482198,1.58964866184748));
#36969=CARTESIAN_POINT('Ctrl Pts',(4.20767422754857,2.00554746219876,1.74861352803222));
#36970=CARTESIAN_POINT('Ctrl Pts',(0.591332402870964,4.62352249362764,1.90757839421698));
#36971=CARTESIAN_POINT('Ctrl Pts',(-3.5674836278665,2.99995809464374,2.06654326040171));
#36972=CARTESIAN_POINT('Ctrl Pts',(-4.45354240620347,-1.37573521927647,
2.22550812658647));
#36973=CARTESIAN_POINT('Ctrl Pts',(-1.25398101020607,-4.48934345055757,
2.38447299277121));
#36974=CARTESIAN_POINT('Ctrl Pts',(3.09596444955676,-3.48449213500062,2.54343785895597));
#36975=CARTESIAN_POINT('Ctrl Pts',(4.60571517107261,0.716985562318844,2.70240272514071));
#36976=CARTESIAN_POINT('Ctrl Pts',(1.89024592721134,4.26070992070277,2.86136759132546));
#36977=CARTESIAN_POINT('Ctrl Pts',(-2.55930879918572,3.89571795955106,3.0203324575102));
#36978=CARTESIAN_POINT('Ctrl Pts',(-4.66098891082537,-0.0431522354210798,
3.17929732369495));
#36979=CARTESIAN_POINT('Ctrl Pts',(-2.48674189107617,-3.94243507020443,
3.3382621898797));
#36980=CARTESIAN_POINT('Ctrl Pts',(1.96880790736958,-4.22498226326438,3.49722705606445));
#36981=CARTESIAN_POINT('Ctrl Pts',(4.61820042919637,-0.631588832885941,
3.65619192224919));
#36982=CARTESIAN_POINT('Ctrl Pts',(3.0309194130074,3.54121548955118,3.81515678843395));
#36983=CARTESIAN_POINT('Ctrl Pts',(-1.33688536850928,4.46535745151852,3.97412165461869));
#36984=CARTESIAN_POINT('Ctrl Pts',(-4.47824990814127,1.29304192146821,4.13308652080344));
#36985=CARTESIAN_POINT('Ctrl Pts',(-3.51132959639971,-3.06549247479725,
4.29205138698818));
#36986=CARTESIAN_POINT('Ctrl Pts',(0.676836175259727,-4.61178625298691,
4.45101625317294));
#36987=CARTESIAN_POINT('Ctrl Pts',(4.24408175233697,-1.92729077450542,4.60998111935768));
#36988=CARTESIAN_POINT('Ctrl Pts',(3.91786512291623,2.52527474314889,4.76894598554243));
#36989=CARTESIAN_POINT('Ctrl Pts',(-0.00254706534730991,4.66118795616863,
4.92791085172718));
#36990=CARTESIAN_POINT('Ctrl Pts',(-3.92062261093312,2.52099147017371,5.08687571791192));
#36991=CARTESIAN_POINT('Ctrl Pts',(-4.24197291604209,-1.93192790486543,
5.24584058409668));
#36992=CARTESIAN_POINT('Ctrl Pts',(-0.671795632162863,-4.61252320088583,
5.40480545028142));
#36993=CARTESIAN_POINT('Ctrl Pts',(3.51467772160843,-3.0616531748872,5.56377031646618));
#36994=CARTESIAN_POINT('Ctrl Pts',(4.47683409109351,1.29793534927254,5.72273518265091));
#36995=CARTESIAN_POINT('Ctrl Pts',(1.33200446098445,4.46681584196115,5.88170004883567));
#36996=CARTESIAN_POINT('Ctrl Pts',(-3.03478773493588,3.53790093896858,6.04066491502041));
#36997=CARTESIAN_POINT('Ctrl Pts',(-4.61750741766603,-0.636635608391419,
6.19962978120516));
#36998=CARTESIAN_POINT('Ctrl Pts',(-1.96418932649049,-4.22713140791419,
6.35859464738991));
#36999=CARTESIAN_POINT('Ctrl Pts',(2.49104902804703,-3.93971501379719,6.51755951357465));
#37000=CARTESIAN_POINT('Ctrl Pts',(4.66103327793766,-0.0380582715176506,
6.6765243797594));
#37001=CARTESIAN_POINT('Ctrl Pts',(2.55504972857005,3.89851260541856,6.83548924594414));
#37002=CARTESIAN_POINT('Ctrl Pts',(-1.89490128753556,4.25864165674564,6.9944541121289));
#37003=CARTESIAN_POINT('Ctrl Pts',(-4.60649593390074,0.711951445696367,
7.15341897831364));
#37004=CARTESIAN_POINT('Ctrl Pts',(-3.09215459006229,-3.48787322608348,
7.3123838444984));
#37005=CARTESIAN_POINT('Ctrl Pts',(1.25888683056368,-4.48797098897782,7.47134871068314));
#37006=CARTESIAN_POINT('Ctrl Pts',(4.45504279352084,-1.3708659153875,7.63031357686789));
#37007=CARTESIAN_POINT('Ctrl Pts',(3.56420379345526,3.00385268759844,7.78927844305264));
#37008=CARTESIAN_POINT('Ctrl Pts',(-0.596386727790659,4.62287816419472,
7.94824330923738));
#37009=CARTESIAN_POINT('Ctrl Pts',(-4.20986027048837,2.00093881791443,8.10720817542214));
#37010=CARTESIAN_POINT('Ctrl Pts',(-3.96126592339197,-2.45663426953358,
8.26617304160689));
#37011=CARTESIAN_POINT('Ctrl Pts',(-0.0786607201839425,-4.66052487829143,
8.42513790779162));
#37012=CARTESIAN_POINT('Ctrl Pts',(3.87610674544883,-2.58891408663156,8.58410277397638));
#37013=CARTESIAN_POINT('Ctrl Pts',(4.27498721313245,1.85773086792121,8.74306764016112));
#37014=CARTESIAN_POINT('Ctrl Pts',(0.752053229904626,4.60011908426979,8.90203250634587));
#37015=CARTESIAN_POINT('Ctrl Pts',(-3.46080403913657,3.12242134452881,9.06099737253062));
#37016=CARTESIAN_POINT('Ctrl Pts',(-4.49876729895963,-1.21974277611503,
9.21996223871536));
#37017=CARTESIAN_POINT('Ctrl Pts',(-1.40962333606424,-4.44293165606859,
9.37892710490011));
#37018=CARTESIAN_POINT('Ctrl Pts',(2.97268968070251,-3.59023616386415,9.53789197108486));
#37019=CARTESIAN_POINT('Ctrl Pts',(4.62789808484238,0.556092587961218,9.69685683726961));
#37020=CARTESIAN_POINT('Ctrl Pts',(2.03753645997128,4.19226965072155,9.85582170345435));
#37021=CARTESIAN_POINT('Ctrl Pts',(-2.42203307935326,3.98251621623715,10.0147865696391));
#37022=CARTESIAN_POINT('Ctrl Pts',(-4.65966279579043,0.119257199362087,
10.1737514358238));
#37023=CARTESIAN_POINT('Ctrl Pts',(-2.62258197443514,-3.85340673137953,
10.3327163020086));
#37024=CARTESIAN_POINT('Ctrl Pts',(1.82041946685649,-4.2910083447557,10.4916811681933));
#37025=CARTESIAN_POINT('Ctrl Pts',(4.59339313592305,-0.792097941499782,
10.6506460343781));
#37026=CARTESIAN_POINT('Ctrl Pts',(3.15245114137279,3.43347221502238,10.8096109005628));
#37027=CARTESIAN_POINT('Ctrl Pts',(-1.18050615653299,4.50922220171738,10.9685757667476));
#37028=CARTESIAN_POINT('Ctrl Pts',(-4.43048334870678,1.44827378175024,11.1275406329323));
#37029=CARTESIAN_POINT('Ctrl Pts',(-3.61599607462336,-2.94130107917936,
11.2865054991171));
#37030=CARTESIAN_POINT('Ctrl Pts',(0.515756246787712,-4.63256679865198,
11.4454703653018));
#37031=CARTESIAN_POINT('Ctrl Pts',(4.17436088354928,-2.07397947530031,11.6044352314866));
#37032=CARTESIAN_POINT('Ctrl Pts',(4.00346427966798,2.38724808335786,11.7634000976713));
#37033=CARTESIAN_POINT('Ctrl Pts',(0.159844628223428,4.6584470958573,11.9223649638561));
#37034=CARTESIAN_POINT('Ctrl Pts',(-3.83041428589339,2.65605083695643,12.0813298300408));
#37035=CARTESIAN_POINT('Ctrl Pts',(-4.3067038357868,-1.7829699158686,12.2402946962256));
#37036=CARTESIAN_POINT('Ctrl Pts',(-0.832082541526254,-4.58631859928641,
12.3992595624103));
#37037=CARTESIAN_POINT('Ctrl Pts',(3.40587982792729,-3.18224170166115,12.5582244285951));
#37038=CARTESIAN_POINT('Ctrl Pts',(4.51933490383836,1.14117994944773,12.7171892947798));
#37039=CARTESIAN_POINT('Ctrl Pts',(1.48681431929952,4.41769881612578,12.8761541609645));
#37040=CARTESIAN_POINT('Ctrl Pts',(-2.90968926508048,3.64148157083744,13.0351190271493));
#37041=CARTESIAN_POINT('Ctrl Pts',(-4.63688395131922,-0.475380765357195,
13.1940838933341));
#37042=CARTESIAN_POINT('Ctrl Pts',(-2.11026509827526,-4.1561353280511,13.3530487595188));
#37043=CARTESIAN_POINT('Ctrl Pts',(2.35228192134809,-4.0241085239556,13.5120136257036));
#37044=CARTESIAN_POINT('Ctrl Pts',(4.65687787075036,-0.200419926626097,
13.6709784918883));
#37045=CARTESIAN_POINT('Ctrl Pts',(2.68931813427488,3.80713115386554,13.829943358073));
#37046=CARTESIAN_POINT('Ctrl Pts',(-1.74538505696882,4.32207249510964,13.9889082242578));
#37047=CARTESIAN_POINT('Ctrl Pts',(-4.57889601123979,0.872003995590307,
14.1478730904425));
#37048=CARTESIAN_POINT('Ctrl Pts',(-3.21179076461628,-3.37802897181164,
14.3068379566273));
#37049=CARTESIAN_POINT('Ctrl Pts',(1.10176713928815,-4.5291046378791,14.465802822812));
#37050=CARTESIAN_POINT('Ctrl Pts',(4.40457902853176,-1.52524202390685,14.6247676889968));
#37051=CARTESIAN_POINT('Ctrl Pts',(3.66669071843603,2.87785663739672,14.7837325551815));
#37052=CARTESIAN_POINT('Ctrl Pts',(-0.434969207726955,4.6408492152194,14.9426974213663));
#37053=CARTESIAN_POINT('Ctrl Pts',(-4.13759436734728,2.14639057521441,15.101662287551));
#37054=CARTESIAN_POINT('Ctrl Pts',(-4.04444738242773,-2.3171372468731,15.2606271537358));
#37055=CARTESIAN_POINT('Ctrl Pts',(-0.240980015348797,-4.65495523955664,
15.4195920199205));
#37056=CARTESIAN_POINT('Ctrl Pts',(3.78355910223096,-2.72238134176653,15.5785568861053));
#37057=CARTESIAN_POINT('Ctrl Pts',(4.33711315641111,1.7076677424367,15.73752175229));
#37058=CARTESIAN_POINT('Ctrl Pts',(0.911859274090375,4.57112593507645,15.8964866184748));
#37059=CARTESIAN_POINT('Ctrl Pts',(-3.34992176025076,3.24109608778754,16.0554514846595));
#37060=CARTESIAN_POINT('Ctrl Pts',(-4.53853066242366,-1.06227071705545,
16.2144163508443));
#37061=CARTESIAN_POINT('Ctrl Pts',(-1.56355397932982,-4.39112498157307,
16.373381217029));
#37062=CARTESIAN_POINT('Ctrl Pts',(2.8458056118763,-3.69162160432059,16.5323460832138));
#37063=CARTESIAN_POINT('Ctrl Pts',(4.64446228943243,0.394524640692141,16.6913109493985));
#37064=CARTESIAN_POINT('Ctrl Pts',(2.18235316458919,4.11873940849393,16.8502758155833));
#37065=CARTESIAN_POINT('Ctrl Pts',(-2.2818167270293,4.06447931158747,17.009240681768));
#37066=CARTESIAN_POINT('Ctrl Pts',(-4.65267934818278,0.281521816324489,
17.1682055479527));
#37067=CARTESIAN_POINT('Ctrl Pts',(-2.75523795029565,-3.75969991985049,
17.3271704141375));
#37068=CARTESIAN_POINT('Ctrl Pts',(1.66982083460383,-4.35182467826958,17.4861352803222));
#37069=CARTESIAN_POINT('Ctrl Pts',(4.56300896046017,-0.95164535244674,17.645100146507));
#37070=CARTESIAN_POINT('Ctrl Pts',(3.27015544722148,3.32156032627453,17.8040650126917));
#37071=CARTESIAN_POINT('Ctrl Pts',(-1.02269368009593,4.54761226213988,17.9630298788765));
#37072=CARTESIAN_POINT('Ctrl Pts',(-4.37733769626469,1.6017472781102,18.1219947450612));
#37073=CARTESIAN_POINT('Ctrl Pts',(-3.71627233650965,-2.81353862084143,
18.280959611246));
#37074=CARTESIAN_POINT('Ctrl Pts',(0.354050133552978,-4.64772289976546,
18.4399244774307));
#37075=CARTESIAN_POINT('Ctrl Pts',(4.09957188237618,-2.21815013723249,18.5988893436155));
#37076=CARTESIAN_POINT('Ctrl Pts',(4.08420279123045,2.24632304225772,18.7578542098002));
#37077=CARTESIAN_POINT('Ctrl Pts',(0.322042252874243,4.65005036934395,18.916819075985));
#37078=CARTESIAN_POINT('Ctrl Pts',(-3.73555541737554,2.78788546640533,19.0757839421697));
#37079=CARTESIAN_POINT('Ctrl Pts',(-4.36620594424068,-1.63184720563709,
19.2347488083544));
#37080=CARTESIAN_POINT('Ctrl Pts',(-0.991359211332678,-4.55454570337957,
19.3937136745392));
#37081=CARTESIAN_POINT('Ctrl Pts',(3.29294682220825,-3.29896663763241,19.5526785407239));
#37082=CARTESIAN_POINT('Ctrl Pts',(4.55634874782847,0.983039031877256,19.7116434069087));
#37083=CARTESIAN_POINT('Ctrl Pts',(1.63981902180431,4.3632182189042,19.8706082730935));
#37084=CARTESIAN_POINT('Ctrl Pts',(-2.7810581130229,3.74064104429479,20.0295731392782));
#37085=CARTESIAN_POINT('Ctrl Pts',(-4.65063079873739,-0.313548757905883,
20.188538005463));
#37086=CARTESIAN_POINT('Ctrl Pts',(-2.25377877661524,-4.08009324355364,
20.3475028716477));
#37087=CARTESIAN_POINT('Ctrl Pts',(2.21065888627362,-4.10361632464813,20.5064677378324));
#37088=CARTESIAN_POINT('Ctrl Pts',(4.64706850229723,-0.362538249772487,
20.6654326040172));
#37089=CARTESIAN_POINT('Ctrl Pts',(2.82032141299069,3.71112742678928,20.824397470202));
#37090=CARTESIAN_POINT('Ctrl Pts',(-1.59374973824449,4.38025586355546,20.9833623363867));
#37091=CARTESIAN_POINT('Ctrl Pts',(-4.54573680433624,1.03099783573258,21.1423272025715));
#37092=CARTESIAN_POINT('Ctrl Pts',(-3.32752747594111,-3.2640834172724,21.3012920687562));
#37093=CARTESIAN_POINT('Ctrl Pts',(0.943309788199209,-4.5647394607477,21.4602569349409));
#37094=CARTESIAN_POINT('Ctrl Pts',(4.34876760869419,-1.67776631304337,21.6192218011257));
#37095=CARTESIAN_POINT('Ctrl Pts',(3.76472590187142,2.74836653778883,21.7781866673104));
#37096=CARTESIAN_POINT('Ctrl Pts',(-0.273023632271506,4.65318579536423,
21.9371515334952));
#37097=CARTESIAN_POINT('Ctrl Pts',(-4.06030488446768,2.28923632220046,22.0961163996799));
#37098=CARTESIAN_POINT('Ctrl Pts',(-4.12271860238902,-2.17482685727795,
22.2550812658647));
#37099=CARTESIAN_POINT('Ctrl Pts',(-0.403006420923942,-4.64373418021473,
22.4140461320495));
#37100=CARTESIAN_POINT('Ctrl Pts',(3.68641720430509,-2.85254293338859,22.5730109982341));
#37101=CARTESIAN_POINT('Ctrl Pts',(4.39397451136436,1.55553056893478,22.7319758644189));
#37102=CARTESIAN_POINT('Ctrl Pts',(1.07055603753408,4.53658437320562,22.8909407306037));
#37103=CARTESIAN_POINT('Ctrl Pts',(-3.2349681382713,3.35583304175512,23.0499055967884));
#37104=CARTESIAN_POINT('Ctrl Pts',(-4.57279171636944,-0.903503706141469,
23.2088704629732));
#37105=CARTESIAN_POINT('Ctrl Pts',(-1.71557108377795,-4.33399700460152,
23.3678353291579));
#37106=CARTESIAN_POINT('Ctrl Pts',(2.71543736744218,-3.78850590125353,23.5268001953427));
#37107=CARTESIAN_POINT('Ctrl Pts',(4.65544310046753,0.232441199006727,23.6857650615274));
#37108=CARTESIAN_POINT('Ctrl Pts',(2.32441426297274,4.04027827433057,23.8447299277122));
#37109=CARTESIAN_POINT('Ctrl Pts',(-2.13862755866238,4.14137453531068,24.0036947938969));
#37110=CARTESIAN_POINT('Ctrl Pts',(-4.64043373817043,0.443698991460186,
24.1626596600816));
#37111=CARTESIAN_POINT('Ctrl Pts',(-2.88380971623262,-3.66191469620319,
24.3216245262664));
#37112=CARTESIAN_POINT('Ctrl Pts',(1.51577912758857,-4.40642449065004,24.4805893924511));
#37113=CARTESIAN_POINT('Ctrl Pts',(4.52982583855719,-1.1118560844723,24.6395542586359));
#37114=CARTESIAN_POINT('Ctrl Pts',(3.37832647762378,3.20941356591303,24.7985191248206));
#37115=CARTESIAN_POINT('Ctrl Pts',(0.559320177738415,4.11691623599613,24.9044957022771));
#37116=CARTESIAN_POINT('Ctrl Pts',(-0.730386029345736,3.8737449900757,24.9574839910054));
#37117=CARTESIAN_POINT('Ctrl Pts',(-3.94350653563855,-0.00347714007584369,
23.1778238829104));
#37118=CARTESIAN_POINT('Ctrl Pts',(-3.94586355936157,-0.259474013504655,
23.1881727429313));
#37119=CARTESIAN_POINT('Ctrl Pts',(-3.92307523690983,-0.515053183369563,
23.1985216029522));
#37120=CARTESIAN_POINT('Ctrl Pts',(-3.87361768125451,-0.765363131235343,
23.2088704629732));
#37121=CARTESIAN_POINT('Ctrl Pts',(-3.62038483883896,-2.0470014722948,23.2618587517014));
#37122=CARTESIAN_POINT('Ctrl Pts',(-2.66797796130846,-3.19049923844816,
23.3148470404297));
#37123=CARTESIAN_POINT('Ctrl Pts',(-1.45327311400651,-3.67133293763351,
23.3678353291579));
#37124=CARTESIAN_POINT('Ctrl Pts',(-0.238568266704596,-4.15216663681884,
23.4208236178862));
#37125=CARTESIAN_POINT('Ctrl Pts',(1.23843455036875,-3.9703362690362,23.4738119066144));
#37126=CARTESIAN_POINT('Ctrl Pts',(2.30027024774299,-3.20926323510153,23.5268001953427));
#37127=CARTESIAN_POINT('Ctrl Pts',(3.36210594511727,-2.44819020116684,23.5797884840709));
#37128=CARTESIAN_POINT('Ctrl Pts',(4.00877452279241,-1.10787450108007,23.6327767727992));
#37129=CARTESIAN_POINT('Ctrl Pts',(3.94360400538084,0.196922861517294,23.6857650615274));
#37130=CARTESIAN_POINT('Ctrl Pts',(3.87843348796927,1.50172022411466,23.7387533502557));
#37131=CARTESIAN_POINT('Ctrl Pts',(3.10142387547099,2.77099924922264,23.7917416389839));
#37132=CARTESIAN_POINT('Ctrl Pts',(1.96907876561599,3.42248813860663,23.8447299277122));
#37133=CARTESIAN_POINT('Ctrl Pts',(0.836733655761017,4.07397702799061,23.8977182164404));
#37134=CARTESIAN_POINT('Ctrl Pts',(-0.650946951450773,4.10767578165063,
23.9507065051686));
#37135=CARTESIAN_POINT('Ctrl Pts',(-1.81175495164127,3.50824590117222,24.0036947938969));
#37136=CARTESIAN_POINT('Ctrl Pts',(-2.20830746798924,3.30347006620307,24.0217965292646));
#37137=CARTESIAN_POINT('Ctrl Pts',(-2.56671309215799,3.02480645592577,24.0398982646323));
#37138=CARTESIAN_POINT('Ctrl Pts',(-2.87170785494343,2.69478584831398,24.058));
#37139=CARTESIAN_POINT('Ctrl Pts',(-1.96186193197213,-2.74910310536279,
1.04083408558608E-17));
#37140=CARTESIAN_POINT('Ctrl Pts',(-2.03089214936932,-2.70842374984998,
4.0844089957036E-17));
#37141=CARTESIAN_POINT('Ctrl Pts',(-2.0982520786512,-2.66519645821488,9.07751022854637E-17));
#37142=CARTESIAN_POINT('Ctrl Pts',(-2.16378064478676,-2.619448737651,1.42247325030098E-16));
#37143=CARTESIAN_POINT('Ctrl Pts',(-2.25130095090051,-2.55834783549675,
1.98311708005797E-16));
#37144=CARTESIAN_POINT('Ctrl Pts',(-2.33555581159229,-2.49275291176235,
1.14301651927622E-16));
#37145=CARTESIAN_POINT('Ctrl Pts',(-2.41645347142118,-2.4230636931251,1.90819582357449E-16));
#37146=CARTESIAN_POINT('Ctrl Pts',(-2.46698855966785,-2.37953028534638,
2.38618744594068E-16));
#37147=CARTESIAN_POINT('Ctrl Pts',(-2.51621317497323,-2.33439817262585,
-8.87118969308996E-17));
#37148=CARTESIAN_POINT('Ctrl Pts',(-2.56410004332752,-2.28775595645186,
-9.0205620750794E-17));
#37149=CARTESIAN_POINT('Ctrl Pts',(-2.58450501257648,-2.26788134323446,
-9.08421081566083E-17));
#37150=CARTESIAN_POINT('Ctrl Pts',(-2.60466703883067,-2.24773246660606,
1.20223089018126E-16));
#37151=CARTESIAN_POINT('Ctrl Pts',(-2.62458377340069,-2.22731585490721,
1.31838984174237E-16));
#37152=CARTESIAN_POINT('Ctrl Pts',(-2.6428539078105,-2.20858717031188,1.42494544454281E-16));
#37153=CARTESIAN_POINT('Ctrl Pts',(-2.66092072754138,-2.18962968712113,
4.62480998826576E-16));
#37154=CARTESIAN_POINT('Ctrl Pts',(-2.67876242915531,-2.17047018454057,
4.44089209850063E-16));
#37155=CARTESIAN_POINT('Ctrl Pts',(-2.75353668750271,-2.09017304546908,
3.67009545019966E-16));
#37156=CARTESIAN_POINT('Ctrl Pts',(-2.82442308955658,-2.00626812836577,
4.38199731939201E-16));
#37157=CARTESIAN_POINT('Ctrl Pts',(-2.89132427090349,-1.91917015947591,
2.28983498828939E-16));
#37158=CARTESIAN_POINT('Ctrl Pts',(-2.9553640840902,-1.83579737674842,2.87154585004375E-17));
#37159=CARTESIAN_POINT('Ctrl Pts',(-3.01575243661163,-1.74949800545801,
1.64657856526806E-16));
#37160=CARTESIAN_POINT('Ctrl Pts',(-3.07237914628982,-1.6606009570442,2.22044604925031E-16));
#37161=CARTESIAN_POINT('Ctrl Pts',(-3.09715333177403,-1.62170849836315,
2.47151307349255E-16));
#37162=CARTESIAN_POINT('Ctrl Pts',(-3.12120717339458,-1.58231843772374,
3.74830717982145E-16));
#37163=CARTESIAN_POINT('Ctrl Pts',(-3.14452974084395,-1.54245667505035,
4.16333634234434E-16));
#37164=CARTESIAN_POINT('Ctrl Pts',(-3.1552141693008,-1.52419538574881,4.35346761344512E-16));
#37165=CARTESIAN_POINT('Ctrl Pts',(-3.1657451101877,-1.50583508811633,6.65859873947159E-18));
#37166=CARTESIAN_POINT('Ctrl Pts',(-3.17612143314624,-1.48737821330264,
4.16333634234434E-17));
#37167=CARTESIAN_POINT('Ctrl Pts',(-3.1851701035806,-1.47128289918176,7.21331002193362E-17));
#37168=CARTESIAN_POINT('Ctrl Pts',(-3.19410146294443,-1.45511349134961,
1.2766348924177E-16));
#37169=CARTESIAN_POINT('Ctrl Pts',(-3.20290718418031,-1.4388859283946,1.2490009027033E-16));
#37170=CARTESIAN_POINT('Ctrl Pts',(-3.25753999780039,-1.33820622270319,
1.07755298047126E-16));
#37171=CARTESIAN_POINT('Ctrl Pts',(-3.30741231186542,-1.23516335787123,
5.68363615759287E-16));
#37172=CARTESIAN_POINT('Ctrl Pts',(-3.35241796906181,-1.13019103593447,
4.71844785465692E-16));
#37173=CARTESIAN_POINT('Ctrl Pts',(-3.39804200535616,-1.0237763911033,3.73999783509847E-16));
#37174=CARTESIAN_POINT('Ctrl Pts',(-3.43866526602443,-0.915378183946712,
-6.22512805566231E-17));
#37175=CARTESIAN_POINT('Ctrl Pts',(-3.47413966247048,-0.805410191460158,
-1.66533453693773E-16));
#37176=CARTESIAN_POINT('Ctrl Pts',(-3.50939387582959,-0.696124750178875,
-2.70168366465852E-16));
#37177=CARTESIAN_POINT('Ctrl Pts',(-3.53956336356882,-0.585288114116654,
-7.73645964354313E-17));
#37178=CARTESIAN_POINT('Ctrl Pts',(-3.56445901023683,-0.473280938901883,
-1.38777878078145E-16));
#37179=CARTESIAN_POINT('Ctrl Pts',(-3.58104437402115,-0.39866228078212,
-1.79691120092537E-16));
#37180=CARTESIAN_POINT('Ctrl Pts',(-3.59528821670414,-0.323523611696084,
-9.85603223433227E-18));
#37181=CARTESIAN_POINT('Ctrl Pts',(-3.60712230450606,-0.24797391740747,
-2.77555756156289E-17));
#37182=CARTESIAN_POINT('Ctrl Pts',(-3.61048639425725,-0.226497318913744,
-3.28438994009322E-17));
#37183=CARTESIAN_POINT('Ctrl Pts',(-3.613655686349,-0.204987494839638,2.70286722177284E-16));
#37184=CARTESIAN_POINT('Ctrl Pts',(-3.61662845468875,-0.183446929103701,
2.77555756156289E-16));
#37185=CARTESIAN_POINT('Ctrl Pts',(-3.61934694140478,-0.163748878291719,
2.84203018926811E-16));
#37186=CARTESIAN_POINT('Ctrl Pts',(-3.62190130092961,-0.144022588989176,
-9.4234710418247E-17));
#37187=CARTESIAN_POINT('Ctrl Pts',(-3.62428757941211,-0.124293547804644,
-8.32667268468867E-17));
#37188=CARTESIAN_POINT('Ctrl Pts',(-3.63845233765523,-0.007183537050793,
-1.81616534692129E-17));
#37189=CARTESIAN_POINT('Ctrl Pts',(-3.64672404198312,0.110194833970378,
2.72159498670366E-16));
#37190=CARTESIAN_POINT('Ctrl Pts',(-3.64895596115005,0.227419084314086,
2.4980018054066E-16));
#37191=CARTESIAN_POINT('Ctrl Pts',(-3.6502760977502,0.296754939123098,2.36575080521473E-16));
#37192=CARTESIAN_POINT('Ctrl Pts',(-3.64948239134564,0.366037414325706,
-3.91023963353986E-16));
#37193=CARTESIAN_POINT('Ctrl Pts',(-3.64653656430167,0.435182446792325,
-3.33066907387547E-16));
#37194=CARTESIAN_POINT('Ctrl Pts',(-3.64171075252927,0.548454851010284,
-2.38122486414389E-16));
#37195=CARTESIAN_POINT('Ctrl Pts',(-3.63111244226456,0.661358405661847,
1.01745842338307E-16));
#37196=CARTESIAN_POINT('Ctrl Pts',(-3.61501201454962,0.773605457518614,
8.32667268468867E-17));
#37197=CARTESIAN_POINT('Ctrl Pts',(-3.5986111375463,0.887947146080084,6.44427734916789E-17));
#37198=CARTESIAN_POINT('Ctrl Pts',(-3.57650072189919,1.00160829055033,1.76269981291295E-16));
#37199=CARTESIAN_POINT('Ctrl Pts',(-3.5489124899874,1.11428362811214,1.66533453693773E-16));
#37200=CARTESIAN_POINT('Ctrl Pts',(-3.53981806230419,1.1514269184982,1.63323819005896E-16));
#37201=CARTESIAN_POINT('Ctrl Pts',(-3.53012795001213,1.18846302772386,5.91487372108521E-17));
#37202=CARTESIAN_POINT('Ctrl Pts',(-3.51984924725713,1.22538078979166,5.55111512312578E-17));
#37203=CARTESIAN_POINT('Ctrl Pts',(-3.51512490385872,1.24234909694735,5.38392276706252E-17));
#37204=CARTESIAN_POINT('Ctrl Pts',(-3.51027554782375,1.25929445386572,-8.56270895207211E-17));
#37205=CARTESIAN_POINT('Ctrl Pts',(-3.5053071420154,1.27619828084334,-8.32667268468867E-17));
#37206=CARTESIAN_POINT('Ctrl Pts',(-3.4726474677456,1.38731510670219,-6.77509499438615E-17));
#37207=CARTESIAN_POINT('Ctrl Pts',(-3.43480620738079,1.4967920748245,-3.16991689118145E-16));
#37208=CARTESIAN_POINT('Ctrl Pts',(-3.3920889732967,1.60433756714027,-2.77555756156289E-16));
#37209=CARTESIAN_POINT('Ctrl Pts',(-3.34803513046651,1.71524812390167,-2.36885885322814E-16));
#37210=CARTESIAN_POINT('Ctrl Pts',(-3.29879531544834,1.82410515487266,-4.90905898233538E-17));
#37211=CARTESIAN_POINT('Ctrl Pts',(-3.2446494755425,1.93058787890887,-2.77555756156289E-17));
#37212=CARTESIAN_POINT('Ctrl Pts',(-3.19007975249465,2.03790420773747,-6.25353928999361E-18));
#37213=CARTESIAN_POINT('Ctrl Pts',(-3.13052656738101,2.14280969706861,3.27691398306138E-16));
#37214=CARTESIAN_POINT('Ctrl Pts',(-3.06622468325314,2.24496360523417,3.33066907387547E-16));
#37215=CARTESIAN_POINT('Ctrl Pts',(-3.02442954901331,2.31136191319685,3.36560897131582E-16));
#37216=CARTESIAN_POINT('Ctrl Pts',(-2.98062715064349,2.37659746123392,-1.92345692100733E-16));
#37217=CARTESIAN_POINT('Ctrl Pts',(-2.93487136195522,2.44057147262401,-2.22044604925031E-16));
#37218=CARTESIAN_POINT('Ctrl Pts',(-2.91011088425382,2.47519063509293,-2.38115998071626E-16));
#37219=CARTESIAN_POINT('Ctrl Pts',(-2.88477824351069,2.50944029002795,-9.06967170124101E-17));
#37220=CARTESIAN_POINT('Ctrl Pts',(-2.85888104291211,2.54330410738954,-1.11022302462516E-16));
#37221=CARTESIAN_POINT('Ctrl Pts',(-2.84939469288667,2.55570869233558,-1.1846772565866E-16));
#37222=CARTESIAN_POINT('Ctrl Pts',(-2.83983467756884,2.56805870725536,-6.92597506618051E-18));
#37223=CARTESIAN_POINT('Ctrl Pts',(-2.83020669950388,2.58034686246535,0.));
#37224=CARTESIAN_POINT('Ctrl Pts',(-2.75399123609851,2.67762039564213,5.48262984856848E-17));
#37225=CARTESIAN_POINT('Ctrl Pts',(-2.67342730379929,2.77114184208896,-1.37750122974287E-16));
#37226=CARTESIAN_POINT('Ctrl Pts',(-2.58880471591903,2.86057864451344,-1.11022302462516E-16));
#37227=CARTESIAN_POINT('Ctrl Pts',(-2.5041872730583,2.95001000921607,-8.42961069915503E-17));
#37228=CARTESIAN_POINT('Ctrl Pts',(-2.41551123635495,3.03535802102991,-2.67279349305171E-16));
#37229=CARTESIAN_POINT('Ctrl Pts',(-2.3230183042847,3.11627005080055,-3.33066907387547E-16));
#37230=CARTESIAN_POINT('Ctrl Pts',(-2.23098883090374,3.19677665085427,-3.98524820655353E-16));
#37231=CARTESIAN_POINT('Ctrl Pts',(-2.13518016460462,3.27289238327565,-7.81735663884996E-17));
#37232=CARTESIAN_POINT('Ctrl Pts',(-2.0357894675403,3.34423830723631,-2.22044604925031E-16));
#37233=CARTESIAN_POINT('Ctrl Pts',(-1.93639877047599,3.41558423119697,-3.65915643461563E-16));
#37234=CARTESIAN_POINT('Ctrl Pts',(-1.83342562767619,3.48216116641753,-4.77297284244418E-18));
#37235=CARTESIAN_POINT('Ctrl Pts',(-1.72703261341869,3.54354657824449,0.));
#37236=CARTESIAN_POINT('Origin',(0.,0.,0.));
#37237=CARTESIAN_POINT('Origin',(-1.73205080756888,-3.,-8.));
#37238=CARTESIAN_POINT('',(-1.73205080756888,-3.,-8.));
#37239=CARTESIAN_POINT('',(1.73205080756888,-3.,-8.));
#37240=CARTESIAN_POINT('',(-0.86602540378444,-3.,-8.));
#37241=CARTESIAN_POINT('',(-1.73205080756888,-3.,-4.));
#37242=CARTESIAN_POINT('',(-1.73205080756888,-3.,-8.));
#37243=CARTESIAN_POINT('',(1.73205080756888,-3.,-4.));
#37244=CARTESIAN_POINT('',(-1.73205080756888,-3.,-4.));
#37245=CARTESIAN_POINT('',(1.73205080756888,-3.,-8.));
#37246=CARTESIAN_POINT('Origin',(-3.46410161513775,4.24230095489963E-16,
-8.));
#37247=CARTESIAN_POINT('',(-3.46410161513775,4.24230095489963E-16,-8.));
#37248=CARTESIAN_POINT('',(-3.03108891324554,-0.749999999999999,-8.));
#37249=CARTESIAN_POINT('',(-3.46410161513775,5.55111512312578E-16,-4.));
#37250=CARTESIAN_POINT('',(-3.46410161513775,4.24230095489963E-16,-8.));
#37251=CARTESIAN_POINT('',(-3.46410161513775,4.24230095489963E-16,-4.));
#37252=CARTESIAN_POINT('Origin',(-1.73205080756888,3.,-8.));
#37253=CARTESIAN_POINT('',(-1.73205080756888,3.,-8.));
#37254=CARTESIAN_POINT('',(-2.1650635094611,2.25,-8.));
#37255=CARTESIAN_POINT('',(-1.73205080756888,3.,-4.));
#37256=CARTESIAN_POINT('',(-1.73205080756888,3.,-8.));
#37257=CARTESIAN_POINT('',(-1.73205080756888,3.,-4.));
#37258=CARTESIAN_POINT('Origin',(1.73205080756888,3.,-8.));
#37259=CARTESIAN_POINT('',(1.73205080756888,3.,-8.));
#37260=CARTESIAN_POINT('',(0.866025403784439,3.,-8.));
#37261=CARTESIAN_POINT('',(1.73205080756888,3.,-4.));
#37262=CARTESIAN_POINT('',(1.73205080756888,3.,-8.));
#37263=CARTESIAN_POINT('',(1.73205080756888,3.,-4.));
#37264=CARTESIAN_POINT('Origin',(3.46410161513775,0.,-8.));
#37265=CARTESIAN_POINT('',(3.46410161513775,0.,-8.));
#37266=CARTESIAN_POINT('',(3.03108891324554,0.75,-8.));
#37267=CARTESIAN_POINT('',(3.46410161513775,0.,-4.));
#37268=CARTESIAN_POINT('',(3.46410161513775,0.,-8.));
#37269=CARTESIAN_POINT('',(3.46410161513775,0.,-4.));
#37270=CARTESIAN_POINT('Origin',(1.73205080756888,-3.,-8.));
#37271=CARTESIAN_POINT('',(2.1650635094611,-2.25,-8.));
#37272=CARTESIAN_POINT('',(1.73205080756888,-3.,-4.));
#37273=CARTESIAN_POINT('Origin',(0.,5.55111512312578E-16,-4.));
#37274=CARTESIAN_POINT('Origin',(0.,0.,0.));
#37275=CARTESIAN_POINT('',(-6.5,-7.9602041944578E-16,0.));
#37276=CARTESIAN_POINT('Origin',(0.,0.,0.));
#37277=CARTESIAN_POINT('Origin',(0.,0.,-8.));
#37278=CARTESIAN_POINT('',(-6.5,-7.9602041944578E-16,-8.));
#37279=CARTESIAN_POINT('',(-6.5,-7.9602041944578E-16,-8.));
#37280=CARTESIAN_POINT('Origin',(0.,0.,-8.));
#37281=CARTESIAN_POINT('Origin',(0.,0.,-8.));
#37282=CARTESIAN_POINT('Origin',(0.,0.,25.));
#37283=CARTESIAN_POINT('',(0.,0.,0.));
#37284=CARTESIAN_POINT('Origin',(0.,0.,0.));
#37285=CARTESIAN_POINT('',(-4.5,-5.51091059616309E-16,2.));
#37286=CARTESIAN_POINT('Origin',(0.,0.,2.));
#37287=CARTESIAN_POINT('',(-4.5,-5.51091059616309E-16,0.));
#37288=CARTESIAN_POINT('',(-4.5,-5.51091059616309E-16,0.));
#37289=CARTESIAN_POINT('Origin',(0.,0.,0.));
#37290=CARTESIAN_POINT('Origin',(0.,0.,0.));
#37291=CARTESIAN_POINT('',(-9.,-1.10218211923262E-15,2.));
#37292=CARTESIAN_POINT('Origin',(0.,0.,2.));
#37293=CARTESIAN_POINT('',(-9.,-1.10218211923262E-15,0.));
#37294=CARTESIAN_POINT('',(-9.,-1.10218211923262E-15,0.));
#37295=CARTESIAN_POINT('Origin',(0.,0.,0.));
#37296=CARTESIAN_POINT('Origin',(0.,0.,2.));
#37297=CARTESIAN_POINT('Origin',(0.,0.,0.));
#37298=CARTESIAN_POINT('',(-300.,-225.,494.));
#37299=CARTESIAN_POINT('',(-275.,-200.,494.));
#37300=CARTESIAN_POINT('',(-250.,-200.,466.));
#37301=CARTESIAN_POINT('',(-285.,-235.,448.));
#37302=CARTESIAN_POINT('',(-285.,-235.,448.));
#37303=CARTESIAN_POINT('',(-300.,225.,494.));
#37304=CARTESIAN_POINT('',(275.,-200.,494.));
#37305=CARTESIAN_POINT('',(250.,-200.,466.));
#37306=CARTESIAN_POINT('',(-250.,200.,466.));
#37307=CARTESIAN_POINT('',(250.,200.,466.));
#37308=CARTESIAN_POINT('',(-285.,-165.,448.));
#37309=CARTESIAN_POINT('',(-285.,-165.,448.));
#37310=CARTESIAN_POINT('',(-215.,-235.,448.));
#37311=CARTESIAN_POINT('',(-215.,-235.,448.));
#37312=CARTESIAN_POINT('',(-215.,-165.,448.));
#37313=CARTESIAN_POINT('',(-215.,-165.,448.));
#37314=CARTESIAN_POINT('',(215.,-235.,448.));
#37315=CARTESIAN_POINT('',(215.,-235.,448.));
#37316=CARTESIAN_POINT('',(215.,-165.,448.));
#37317=CARTESIAN_POINT('',(215.,-165.,448.));
#37318=CARTESIAN_POINT('',(285.,-235.,448.));
#37319=CARTESIAN_POINT('',(285.,-235.,448.));
#37320=CARTESIAN_POINT('',(285.,-165.,448.));
#37321=CARTESIAN_POINT('',(285.,-165.,448.));
#37322=CARTESIAN_POINT('',(-285.,165.,448.));
#37323=CARTESIAN_POINT('',(-285.,165.,448.));
#37324=CARTESIAN_POINT('',(-285.,235.,448.));
#37325=CARTESIAN_POINT('',(-285.,235.,448.));
#37326=CARTESIAN_POINT('',(-215.,165.,448.));
#37327=CARTESIAN_POINT('',(-215.,165.,448.));
#37328=CARTESIAN_POINT('',(-215.,235.,448.));
#37329=CARTESIAN_POINT('',(-215.,235.,448.));
#37330=CARTESIAN_POINT('',(215.,165.,448.));
#37331=CARTESIAN_POINT('',(215.,165.,448.));
#37332=CARTESIAN_POINT('',(215.,235.,448.));
#37333=CARTESIAN_POINT('',(215.,235.,448.));
#37334=CARTESIAN_POINT('',(285.,165.,448.));
#37335=CARTESIAN_POINT('',(285.,165.,448.));
#37336=CARTESIAN_POINT('',(285.,235.,448.));
#37337=CARTESIAN_POINT('',(285.,235.,448.));
#37338=CARTESIAN_POINT('',(0.,0.,0.));
#37339=CARTESIAN_POINT('',(0.,0.,0.));
#37340=CARTESIAN_POINT('Origin',(0.,0.,387.));
#37341=CARTESIAN_POINT('',(-4.51811257745934,-3.71096681342671E-5,375.387416697508));
#37342=CARTESIAN_POINT('',(-4.51738402494857,7.56118822245166E-5,375.112583302492));
#37343=CARTESIAN_POINT('',(-4.51775,5.53264807684796E-16,387.));
#37344=CARTESIAN_POINT('',(-3.43378788736318,2.93584158412846,375.));
#37345=CARTESIAN_POINT('Ctrl Pts',(-4.51738402494857,7.56118822245166E-5,
375.112583302492));
#37346=CARTESIAN_POINT('Ctrl Pts',(-4.51750331650906,0.316697913039608,
375.101431493481));
#37347=CARTESIAN_POINT('Ctrl Pts',(-4.4846735281982,0.633280120229468,375.09027968447));
#37348=CARTESIAN_POINT('Ctrl Pts',(-4.41862189351514,0.942742403897512,
375.07912787546));
#37349=CARTESIAN_POINT('Ctrl Pts',(-4.26239834514751,1.67467426709133,375.052751916973));
#37350=CARTESIAN_POINT('Ctrl Pts',(-3.92033033613571,2.36677696691102,375.026375958487));
#37351=CARTESIAN_POINT('Ctrl Pts',(-3.43378788736318,2.93584158412846,375.));
#37352=CARTESIAN_POINT('',(-4.51775,5.53264807684796E-16,375.));
#37353=CARTESIAN_POINT('Origin',(0.,0.,375.));
#37354=CARTESIAN_POINT('',(-4.51775,-5.53264807684796E-16,374.));
#37355=CARTESIAN_POINT('',(-4.51775,5.53264807684796E-16,387.));
#37356=CARTESIAN_POINT('Origin',(0.,0.,374.));
#37357=CARTESIAN_POINT('',(3.43408816985915,2.93604417002329,375.));
#37358=CARTESIAN_POINT('Origin',(0.,0.,375.));
#37359=CARTESIAN_POINT('Ctrl Pts',(3.43408816985915,2.93604417002329,375.));
#37360=CARTESIAN_POINT('Ctrl Pts',(2.97450239048794,3.47304931219374,375.024906410057));
#37361=CARTESIAN_POINT('Ctrl Pts',(2.38685944123298,3.90077491345638,375.049812820113));
#37362=CARTESIAN_POINT('Ctrl Pts',(1.73419289985632,4.17206490566361,375.07471923017));
#37363=CARTESIAN_POINT('Ctrl Pts',(1.04301719200363,4.45936177245515,375.101095188656));
#37364=CARTESIAN_POINT('Ctrl Pts',(0.278918372660684,4.57121814160633,375.127471147143));
#37365=CARTESIAN_POINT('Ctrl Pts',(-0.465602633695269,4.49408396451439,
375.153847105629));
#37366=CARTESIAN_POINT('Ctrl Pts',(-1.21012364005122,4.41694978742245,375.180223064116));
#37367=CARTESIAN_POINT('Ctrl Pts',(-1.93506683342019,4.15082506408738,375.206599022603));
#37368=CARTESIAN_POINT('Ctrl Pts',(-2.55266299064051,3.7279323762134,375.232974981089));
#37369=CARTESIAN_POINT('Ctrl Pts',(-3.17025914786083,3.30503968833942,375.259350939576));
#37370=CARTESIAN_POINT('Ctrl Pts',(-3.68050826893252,2.72537903592653,375.285726898063));
#37371=CARTESIAN_POINT('Ctrl Pts',(-4.02163754569994,2.05912619262106,375.312102856549));
#37372=CARTESIAN_POINT('Ctrl Pts',(-4.346324085653,1.4249873333691,375.337207470202));
#37373=CARTESIAN_POINT('Ctrl Pts',(-4.51780131678173,0.712402743689628,
375.362312083855));
#37374=CARTESIAN_POINT('Ctrl Pts',(-4.51811257745934,-3.71096681342671E-5,
375.387416697508));
#37375=CARTESIAN_POINT('Origin',(0.,0.,387.));
#37376=CARTESIAN_POINT('',(-4.51742232703027,-5.89235854892012E-5,376.387416697508));
#37377=CARTESIAN_POINT('',(-4.51809885152616,4.59828434581654E-5,376.112583302492));
#37378=CARTESIAN_POINT('',(-4.51775,5.53264807684796E-16,387.));
#37379=CARTESIAN_POINT('Ctrl Pts',(-4.51809885152616,4.59828434581654E-5,
376.112583302492));
#37380=CARTESIAN_POINT('Ctrl Pts',(-4.51812276106344,0.0453867389231147,
376.110985620474));
#37381=CARTESIAN_POINT('Ctrl Pts',(-4.51745435602182,0.090726788718723,
376.109387938455));
#37382=CARTESIAN_POINT('Ctrl Pts',(-4.51608913278767,0.136045847103087,
376.107790256437));
#37383=CARTESIAN_POINT('Ctrl Pts',(-4.49355081105947,0.884213247670103,
376.08141429795));
#37384=CARTESIAN_POINT('Ctrl Pts',(-4.28109923000243,1.62665957583979,376.055038339464));
#37385=CARTESIAN_POINT('Ctrl Pts',(-3.90445518421615,2.27349934356334,376.028662380977));
#37386=CARTESIAN_POINT('Ctrl Pts',(-3.52781113842983,2.92033911128693,376.002286422491));
#37387=CARTESIAN_POINT('Ctrl Pts',(-2.98697462791424,3.47157231856439,375.975910464004));
#37388=CARTESIAN_POINT('Ctrl Pts',(-2.3474228959368,3.86046307951571,375.949534505517));
#37389=CARTESIAN_POINT('Ctrl Pts',(-1.70787116395944,4.24935384046699,375.923158547031));
#37390=CARTESIAN_POINT('Ctrl Pts',(-0.969604210520236,4.47590215509218,
375.896782588544));
#37391=CARTESIAN_POINT('Ctrl Pts',(-0.222001520476049,4.51268047531198,
375.870406630058));
#37392=CARTESIAN_POINT('Ctrl Pts',(0.525601169568224,4.54945879553177,375.844030671571));
#37393=CARTESIAN_POINT('Ctrl Pts',(1.28253959621751,4.39646712134613,375.817654713084));
#37394=CARTESIAN_POINT('Ctrl Pts',(1.95717379585807,4.07222787085974,375.791278754598));
#37395=CARTESIAN_POINT('Ctrl Pts',(2.63180799549863,3.74798862037335,375.764902796111));
#37396=CARTESIAN_POINT('Ctrl Pts',(3.2241379681305,3.25250179358621,375.738526837624));
#37397=CARTESIAN_POINT('Ctrl Pts',(3.66245231025333,2.64575380780901,375.712150879138));
#37398=CARTESIAN_POINT('Ctrl Pts',(4.10076665237614,2.03900582203184,375.685774920651));
#37399=CARTESIAN_POINT('Ctrl Pts',(4.38506536398996,1.3209966772646,375.659398962165));
#37400=CARTESIAN_POINT('Ctrl Pts',(4.48092940302618,0.578654357786939,375.633023003678));
#37401=CARTESIAN_POINT('Ctrl Pts',(4.57679344206242,-0.163687961690764,
375.606647045192));
#37402=CARTESIAN_POINT('Ctrl Pts',(4.48422280852107,-0.930363455878798,
375.580271086705));
#37403=CARTESIAN_POINT('Ctrl Pts',(4.21442463026058,-1.62855553605874,375.553895128218));
#37404=CARTESIAN_POINT('Ctrl Pts',(3.9446264520001,-2.32674761623864,375.527519169732));
#37405=CARTESIAN_POINT('Ctrl Pts',(3.49760072902049,-2.95645628241037,375.501143211245));
#37406=CARTESIAN_POINT('Ctrl Pts',(2.92746753425598,-3.44144014717816,375.474767252759));
#37407=CARTESIAN_POINT('Ctrl Pts',(2.35733433949146,-3.92642401194595,375.448391294272));
#37408=CARTESIAN_POINT('Ctrl Pts',(1.66409367294202,-4.26668307530983,375.422015335785));
#37409=CARTESIAN_POINT('Ctrl Pts',(0.931673460847324,-4.42103326145621,
375.395639377299));
#37410=CARTESIAN_POINT('Ctrl Pts',(0.199253248752631,-4.57538344760259,
375.369263418812));
#37411=CARTESIAN_POINT('Ctrl Pts',(-0.572346508887337,-4.54382475653147,
375.342887460326));
#37412=CARTESIAN_POINT('Ctrl Pts',(-1.28970997066769,-4.33015694226547,
375.316511501839));
#37413=CARTESIAN_POINT('Ctrl Pts',(-2.00707343244804,-4.11648912799948,
375.290135543353));
#37414=CARTESIAN_POINT('Ctrl Pts',(-2.67020059836879,-3.72071219053859,
375.263759584866));
#37415=CARTESIAN_POINT('Ctrl Pts',(-3.19881015683584,-3.19078643170059,
375.237383626379));
#37416=CARTESIAN_POINT('Ctrl Pts',(-3.72741971530293,-2.66086067286256,
375.211007667893));
#37417=CARTESIAN_POINT('Ctrl Pts',(-4.12151166631632,-1.99678609264739,
375.184631709406));
#37418=CARTESIAN_POINT('Ctrl Pts',(-4.33336809796127,-1.27886828925581,
375.158255750919));
#37419=CARTESIAN_POINT('Ctrl Pts',(-4.45565119847602,-0.864487596482785,
375.143031601444));
#37420=CARTESIAN_POINT('Ctrl Pts',(-4.51722117132128,-0.432168630785926,
375.127807451968));
#37421=CARTESIAN_POINT('Ctrl Pts',(-4.51738402494857,7.56118822245166E-5,
375.112583302492));
#37422=CARTESIAN_POINT('Ctrl Pts',(-4.51811257745934,-3.71096681342671E-5,
375.387416697508));
#37423=CARTESIAN_POINT('Ctrl Pts',(-4.51812834028524,-0.0361164032740072,
375.388688042342));
#37424=CARTESIAN_POINT('Ctrl Pts',(-4.51770513086054,-0.072195325689107,
375.389959387175));
#37425=CARTESIAN_POINT('Ctrl Pts',(-4.51684061704284,-0.108263669884894,
375.391230732009));
#37426=CARTESIAN_POINT('Ctrl Pts',(-4.49890497915514,-0.856555654887204,
375.417606690495));
#37427=CARTESIAN_POINT('Ctrl Pts',(-4.29102427091659,-1.60029459069377,
375.443982648982));
#37428=CARTESIAN_POINT('Ctrl Pts',(-3.91836620190419,-2.24943891961304,
375.470358607469));
#37429=CARTESIAN_POINT('Ctrl Pts',(-3.54570813289175,-2.89858324853235,
375.496734565955));
#37430=CARTESIAN_POINT('Ctrl Pts',(-3.00827270310544,-3.45313297056435,
375.523110524442));
#37431=CARTESIAN_POINT('Ctrl Pts',(-2.37112526060116,-3.84595044058964,
375.549486482929));
#37432=CARTESIAN_POINT('Ctrl Pts',(-1.73397781809692,-4.2387679106149,375.575862441415));
#37433=CARTESIAN_POINT('Ctrl Pts',(-0.997118362874728,-4.46985312863346,
375.602238399902));
#37434=CARTESIAN_POINT('Ctrl Pts',(-0.249756040595646,-4.5112294783827,
375.628614358388));
#37435=CARTESIAN_POINT('Ctrl Pts',(0.497606281683436,-4.55260582813195,
375.654990316875));
#37436=CARTESIAN_POINT('Ctrl Pts',(1.25547147101941,-4.40427330961188,375.681366275361));
#37437=CARTESIAN_POINT('Ctrl Pts',(1.93208738599618,-4.08418999671804,375.707742233848));
#37438=CARTESIAN_POINT('Ctrl Pts',(2.60870330097296,-3.76410668382419,375.734118192335));
#37439=CARTESIAN_POINT('Ctrl Pts',(3.20406994159053,-3.27227257655657,375.760494150821));
#37440=CARTESIAN_POINT('Ctrl Pts',(3.64610826956487,-2.66823238495421,375.786870109308));
#37441=CARTESIAN_POINT('Ctrl Pts',(4.0881465975392,-2.06419219335185,375.813246067794));
#37442=CARTESIAN_POINT('Ctrl Pts',(4.37685661287028,-1.34794591741475,375.839622026281));
#37443=CARTESIAN_POINT('Ctrl Pts',(4.47728517843054,-0.606207059497561,
375.865997984767));
#37444=CARTESIAN_POINT('Ctrl Pts',(4.57771374399081,0.135531798419669,375.892373943254));
#37445=CARTESIAN_POINT('Ctrl Pts',(4.48986085978024,0.902763238316989,375.918749901741));
#37446=CARTESIAN_POINT('Ctrl Pts',(4.22436257375966,1.6026011428634,375.945125860228));
#37447=CARTESIAN_POINT('Ctrl Pts',(3.95886428773907,2.30243904740981,375.971501818714));
#37448=CARTESIAN_POINT('Ctrl Pts',(3.51572059990846,2.93488341660531,375.9978777772));
#37449=CARTESIAN_POINT('Ctrl Pts',(2.9485814178138,3.42336635395337,376.024253735687));
#37450=CARTESIAN_POINT('Ctrl Pts',(2.38144223571922,3.91184929130138,376.050629694174));
#37451=CARTESIAN_POINT('Ctrl Pts',(1.69030755936062,4.25637079680199,376.07700565266));
#37452=CARTESIAN_POINT('Ctrl Pts',(0.958850723376994,4.41522081720076,376.103381611147));
#37453=CARTESIAN_POINT('Ctrl Pts',(0.227393887393287,4.57407083759954,376.129757569634));
#37454=CARTESIAN_POINT('Ctrl Pts',(-0.544385108215453,4.54724937289643,
376.15613352812));
#37455=CARTESIAN_POINT('Ctrl Pts',(-1.26304959302181,4.33800360748393,376.182509486607));
#37456=CARTESIAN_POINT('Ctrl Pts',(-1.98171407782812,4.12875784207144,376.208885445093));
#37457=CARTESIAN_POINT('Ctrl Pts',(-2.64726405183205,3.73708777594958,376.23526140358));
#37458=CARTESIAN_POINT('Ctrl Pts',(-3.17912363311765,3.21041157777291,376.261637362067));
#37459=CARTESIAN_POINT('Ctrl Pts',(-3.71098321440328,2.68373537959622,376.288013320553));
#37460=CARTESIAN_POINT('Ctrl Pts',(-4.10915240297055,2.0220530493647,376.31438927904));
#37461=CARTESIAN_POINT('Ctrl Pts',(-4.32542620311525,1.30547222672582,376.340765237526));
#37462=CARTESIAN_POINT('Ctrl Pts',(-4.45293485255022,0.882997322948535,
376.356315724187));
#37463=CARTESIAN_POINT('Ctrl Pts',(-4.51721787315074,0.44144006785591,376.371866210847));
#37464=CARTESIAN_POINT('Ctrl Pts',(-4.51742232703027,-5.89235854892012E-5,
376.387416697508));
#37465=CARTESIAN_POINT('Origin',(0.,0.,387.));
#37466=CARTESIAN_POINT('',(-4.51776278108284,0.000115059314115817,377.387416697508));
#37467=CARTESIAN_POINT('',(-4.51759690135649,-0.00010734614409786,377.112583302492));
#37468=CARTESIAN_POINT('',(-4.51775,5.53264807684796E-16,387.));
#37469=CARTESIAN_POINT('Ctrl Pts',(-4.51759690135649,-0.00010734614409786,
377.112583302492));
#37470=CARTESIAN_POINT('Ctrl Pts',(-4.51713109747156,0.522789201244633,
377.094163788979));
#37471=CARTESIAN_POINT('Ctrl Pts',(-4.42639959069602,1.04584321668838,377.075744275467));
#37472=CARTESIAN_POINT('Ctrl Pts',(-4.24853722021895,1.53736821094173,377.057324761954));
#37473=CARTESIAN_POINT('Ctrl Pts',(-3.99384588448772,2.24121105862155,377.030948803468));
#37474=CARTESIAN_POINT('Ctrl Pts',(-3.56049254147675,2.88040358637871,377.004572844981));
#37475=CARTESIAN_POINT('Ctrl Pts',(-3.00094181327236,3.37756091891157,376.978196886494));
#37476=CARTESIAN_POINT('Ctrl Pts',(-2.44139108506791,3.87471825144449,376.951820928008));
#37477=CARTESIAN_POINT('Ctrl Pts',(-1.75564297167002,4.22984038875309,376.925444969521));
#37478=CARTESIAN_POINT('Ctrl Pts',(-1.02671867551292,4.39993389597404,376.899069011035));
#37479=CARTESIAN_POINT('Ctrl Pts',(-0.297794379355856,4.57002740319499,
376.872693052548));
#37480=CARTESIAN_POINT('Ctrl Pts',(0.474306099560417,4.55509228032832,376.846317094061));
#37481=CARTESIAN_POINT('Ctrl Pts',(1.19610717026038,4.35693667212173,376.819941135575));
#37482=CARTESIAN_POINT('Ctrl Pts',(1.91790824096034,4.15878106391514,376.793565177088));
#37483=CARTESIAN_POINT('Ctrl Pts',(2.58940990344398,3.77740497036863,376.767189218602));
#37484=CARTESIAN_POINT('Ctrl Pts',(3.12931572485767,3.25898030397792,376.740813260115));
#37485=CARTESIAN_POINT('Ctrl Pts',(3.66922154627136,2.74055563758721,376.714437301628));
#37486=CARTESIAN_POINT('Ctrl Pts',(4.07753152661508,2.0850823983523,376.688061343142));
#37487=CARTESIAN_POINT('Ctrl Pts',(4.30481295893208,1.37191651212926,376.661685384655));
#37488=CARTESIAN_POINT('Ctrl Pts',(4.53209439124908,0.658750625906209,376.635309426169));
#37489=CARTESIAN_POINT('Ctrl Pts',(4.57834727553935,-0.112107907304984,
376.608933467682));
#37490=CARTESIAN_POINT('Ctrl Pts',(4.4379719316997,-0.847333854561028,376.582557509196));
#37491=CARTESIAN_POINT('Ctrl Pts',(4.29759658786004,-1.58255980181707,376.556181550709));
#37492=CARTESIAN_POINT('Ctrl Pts',(3.97059301589046,-2.28215316311797,376.529805592222));
#37493=CARTESIAN_POINT('Ctrl Pts',(3.49655043114217,-2.86141653901512,376.503429633736));
#37494=CARTESIAN_POINT('Ctrl Pts',(3.02250784639385,-3.4406799149123,376.477053675249));
#37495=CARTESIAN_POINT('Ctrl Pts',(2.40142624886681,-3.89961330540572,376.450677716762));
#37496=CARTESIAN_POINT('Ctrl Pts',(1.7084978848751,-4.18265519808121,376.424301758276));
#37497=CARTESIAN_POINT('Ctrl Pts',(1.01556952088344,-4.46569709075668,376.397925799789));
#37498=CARTESIAN_POINT('Ctrl Pts',(0.250794390427128,-4.57284748561423,
376.371549841303));
#37499=CARTESIAN_POINT('Ctrl Pts',(-0.493238770703864,-4.4911340483472,
376.345173882816));
#37500=CARTESIAN_POINT('Ctrl Pts',(-1.2372719318349,-4.40942061108017,376.31879792433));
#37501=CARTESIAN_POINT('Ctrl Pts',(-1.96056312364061,-4.13884334168854,
376.292421965843));
#37502=CARTESIAN_POINT('Ctrl Pts',(-2.5755459301882,-3.71216011150867,376.266046007356));
#37503=CARTESIAN_POINT('Ctrl Pts',(-3.19052873673575,-3.28547688132881,
376.23967004887));
#37504=CARTESIAN_POINT('Ctrl Pts',(-3.69720315802519,-2.70268769036073,
376.213294090383));
#37505=CARTESIAN_POINT('Ctrl Pts',(-4.03422783747023,-2.03434885839451,
376.186918131897));
#37506=CARTESIAN_POINT('Ctrl Pts',(-4.350837779367,-1.40649359537751,376.162139855428));
#37507=CARTESIAN_POINT('Ctrl Pts',(-4.51772804111577,-0.703138866533066,
376.13736157896));
#37508=CARTESIAN_POINT('Ctrl Pts',(-4.51809885152616,4.59828434581654E-5,
376.112583302492));
#37509=CARTESIAN_POINT('Ctrl Pts',(-4.51742232703027,-5.89235854892012E-5,
376.387416697508));
#37510=CARTESIAN_POINT('Ctrl Pts',(-4.51756465760558,-0.307408461731671,
376.398242169334));
#37511=CARTESIAN_POINT('Ctrl Pts',(-4.48665292107515,-0.614729763863418,
376.40906764116));
#37512=CARTESIAN_POINT('Ctrl Pts',(-4.42439936040209,-0.915565329693696,
376.419893112986));
#37513=CARTESIAN_POINT('Ctrl Pts',(-4.27272030582208,-1.64854274842831,
376.446269071473));
#37514=CARTESIAN_POINT('Ctrl Pts',(-3.9349837849399,-2.34301827085134,376.472645029959));
#37515=CARTESIAN_POINT('Ctrl Pts',(-3.45207841488762,-2.91491409664169,
376.499020988446));
#37516=CARTESIAN_POINT('Ctrl Pts',(-2.96917304483534,-3.48680992243204,
376.525396946932));
#37517=CARTESIAN_POINT('Ctrl Pts',(-2.34109882561295,-3.93612605158971,
376.551772905419));
#37518=CARTESIAN_POINT('Ctrl Pts',(-1.64389457655484,-4.20846530156397,
376.578148863906));
#37519=CARTESIAN_POINT('Ctrl Pts',(-0.946690327496738,-4.48080455153823,
376.604524822392));
#37520=CARTESIAN_POINT('Ctrl Pts',(-0.180356048602913,-4.57616692232909,
376.630900780879));
#37521=CARTESIAN_POINT('Ctrl Pts',(0.562330763470305,-4.48300721455655,
376.657276739365));
#37522=CARTESIAN_POINT('Ctrl Pts',(1.30501757554357,-4.38984750678402,376.683652697852));
#37523=CARTESIAN_POINT('Ctrl Pts',(2.02405692079622,-4.10816572044807,376.710028656339));
#37524=CARTESIAN_POINT('Ctrl Pts',(2.6323971400614,-3.67206411576684,376.736404614825));
#37525=CARTESIAN_POINT('Ctrl Pts',(3.24073735932655,-3.23596251108564,376.762780573312));
#37526=CARTESIAN_POINT('Ctrl Pts',(3.73837845260424,-2.64544108805917,376.789156531798));
#37527=CARTESIAN_POINT('Ctrl Pts',(4.0650726975356,-1.97199227611499,376.815532490285));
#37528=CARTESIAN_POINT('Ctrl Pts',(4.39176694246694,-1.29854346417084,376.841908448771));
#37529=CARTESIAN_POINT('Ctrl Pts',(4.54751433905197,-0.542167263308996,
376.868284407258));
#37530=CARTESIAN_POINT('Ctrl Pts',(4.51345907728089,0.205564420603285,376.894660365745));
#37531=CARTESIAN_POINT('Ctrl Pts',(4.4794038155098,0.953296104515694,376.921036324231));
#37532=CARTESIAN_POINT('Ctrl Pts',(4.25554589538254,1.69238327147853,376.947412282718));
#37533=CARTESIAN_POINT('Ctrl Pts',(3.86898703740037,2.33334714042606,376.973788241204));
#37534=CARTESIAN_POINT('Ctrl Pts',(3.48242817941824,2.97431100937351,377.000164199691));
#37535=CARTESIAN_POINT('Ctrl Pts',(2.93316838358124,3.51715158030568,377.026540158178));
#37536=CARTESIAN_POINT('Ctrl Pts',(2.28770467380867,3.89614898312949,377.052916116664));
#37537=CARTESIAN_POINT('Ctrl Pts',(1.6422409640361,4.27514638595329,377.079292075151));
#37538=CARTESIAN_POINT('Ctrl Pts',(0.900573340327957,4.49030062066872,377.105668033637));
#37539=CARTESIAN_POINT('Ctrl Pts',(0.152492990912077,4.51556369250058,377.132043992124));
#37540=CARTESIAN_POINT('Ctrl Pts',(-0.595587358503804,4.54082676433243,
377.158419950611));
#37541=CARTESIAN_POINT('Ctrl Pts',(-1.35008043362742,4.3761986732807,377.184795909097));
#37542=CARTESIAN_POINT('Ctrl Pts',(-2.01964231224972,4.04161038496754,377.211171867584));
#37543=CARTESIAN_POINT('Ctrl Pts',(-2.68920419087202,3.70702209665437,377.23754782607));
#37544=CARTESIAN_POINT('Ctrl Pts',(-3.27383487299299,3.20247361107977,377.263923784557));
#37545=CARTESIAN_POINT('Ctrl Pts',(-3.70275510124179,2.58904890520336,377.290299743043));
#37546=CARTESIAN_POINT('Ctrl Pts',(-4.13167532949061,1.97562419932691,377.31667570153));
#37547=CARTESIAN_POINT('Ctrl Pts',(-4.40488510386723,1.25332327314864,377.343051660017));
#37548=CARTESIAN_POINT('Ctrl Pts',(-4.48930784196123,0.509592654393879,
377.369427618503));
#37549=CARTESIAN_POINT('Ctrl Pts',(-4.50850066492699,0.340511546362542,
377.375423978172));
#37550=CARTESIAN_POINT('Ctrl Pts',(-4.51793615737842,0.170322859138234,
377.38142033784));
#37551=CARTESIAN_POINT('Ctrl Pts',(-4.51776278108284,0.000115059314115817,
377.387416697508));
#37552=CARTESIAN_POINT('Origin',(0.,0.,387.));
#37553=CARTESIAN_POINT('',(-4.51797310231548,-9.04168125550817E-5,378.387416697508));
#37554=CARTESIAN_POINT('',(-4.51753028950122,9.61292306860575E-5,378.112583302492));
#37555=CARTESIAN_POINT('',(-4.51775,5.53264807684796E-16,387.));
#37556=CARTESIAN_POINT('Ctrl Pts',(-4.51753028950122,9.61292306860575E-5,
378.112583302492));
#37557=CARTESIAN_POINT('Ctrl Pts',(-4.51772668562278,0.251779003793691,
378.103717915972));
#37558=CARTESIAN_POINT('Ctrl Pts',(-4.49704602585537,0.503429942291254,
378.094852529451));
#37559=CARTESIAN_POINT('Ctrl Pts',(-4.4551993669653,0.751510564258943,378.085987142931));
#37560=CARTESIAN_POINT('Ctrl Pts',(-4.33069878989798,1.48959053081815,378.059611184445));
#37561=CARTESIAN_POINT('Ctrl Pts',(-4.01884552637064,2.19606752935734,378.033235225958));
#37562=CARTESIAN_POINT('Ctrl Pts',(-3.55739459519457,2.78541078149727,378.006859267472));
#37563=CARTESIAN_POINT('Ctrl Pts',(-3.09594366401851,3.3747540336372,377.980483308985));
#37564=CARTESIAN_POINT('Ctrl Pts',(-2.48489506519372,3.84696353937788,377.954107350499));
#37565=CARTESIAN_POINT('Ctrl Pts',(-1.79822638382644,4.14487049256201,377.927731392012));
#37566=CARTESIAN_POINT('Ctrl Pts',(-1.11155770245912,4.44277744574616,377.901355433525));
#37567=CARTESIAN_POINT('Ctrl Pts',(-0.349268938549303,4.56638184637374,
377.874979475039));
#37568=CARTESIAN_POINT('Ctrl Pts',(0.396352188045507,4.50071932813326,377.848603516552));
#37569=CARTESIAN_POINT('Ctrl Pts',(1.14197331464023,4.43505680989279,377.822227558065));
#37570=CARTESIAN_POINT('Ctrl Pts',(1.87092680391995,4.18012737278432,377.795851599579));
#37571=CARTESIAN_POINT('Ctrl Pts',(2.49496072486742,3.76679446067473,377.769475641092));
#37572=CARTESIAN_POINT('Ctrl Pts',(3.11899464581496,3.35346154856509,377.743099682606));
#37573=CARTESIAN_POINT('Ctrl Pts',(3.63810899843023,2.7817251614543,377.716723724119));
#37574=CARTESIAN_POINT('Ctrl Pts',(3.98945636554489,2.120803488071,377.690347765632));
#37575=CARTESIAN_POINT('Ctrl Pts',(4.34080373265956,1.45988181468769,377.663971807146));
#37576=CARTESIAN_POINT('Ctrl Pts',(4.52438411427362,0.709774855031875,377.637595848659));
#37577=CARTESIAN_POINT('Ctrl Pts',(4.517972055111,-0.0387044808375217,377.611219890173));
#37578=CARTESIAN_POINT('Ctrl Pts',(4.51155999594838,-0.787183816706875,
377.584843931686));
#37579=CARTESIAN_POINT('Ctrl Pts',(4.3151554960091,-1.53403552878981,377.558467973199));
#37580=CARTESIAN_POINT('Ctrl Pts',(3.9525365831578,-2.18884080883012,377.532092014713));
#37581=CARTESIAN_POINT('Ctrl Pts',(3.5899176703065,-2.84364608887043,377.505716056226));
#37582=CARTESIAN_POINT('Ctrl Pts',(3.06108434454318,-3.40640493686811,377.47934009774));
#37583=CARTESIAN_POINT('Ctrl Pts',(2.43006066621085,-3.80898604436084,377.452964139253));
#37584=CARTESIAN_POINT('Ctrl Pts',(1.79903698787851,-4.21156715185356,377.426588180766));
#37585=CARTESIAN_POINT('Ctrl Pts',(1.06582295697716,-4.45397051884133,377.40021222228));
#37586=CARTESIAN_POINT('Ctrl Pts',(0.319186313873781,-4.50684919035867,
377.373836263793));
#37587=CARTESIAN_POINT('Ctrl Pts',(-0.427450329229602,-4.55972786187601,
377.347460305307));
#37588=CARTESIAN_POINT('Ctrl Pts',(-1.18750958453502,-4.42308183792293,
377.32108434682));
#37589=CARTESIAN_POINT('Ctrl Pts',(-1.86897365124353,-4.11345438999364,
377.294708388334));
#37590=CARTESIAN_POINT('Ctrl Pts',(-2.55043771795204,-3.80382694206434,
377.268332429847));
#37591=CARTESIAN_POINT('Ctrl Pts',(-3.15330659606364,-3.32121807015883,
377.24195647136));
#37592=CARTESIAN_POINT('Ctrl Pts',(-3.60459299156575,-2.72405559648777,
377.215580512874));
#37593=CARTESIAN_POINT('Ctrl Pts',(-4.05587938706785,-2.1268931228167,377.189204554387));
#37594=CARTESIAN_POINT('Ctrl Pts',(-4.35558329996046,-1.41517704738009,
377.162828595901));
#37595=CARTESIAN_POINT('Ctrl Pts',(-4.46742059218106,-0.675072425860511,
377.136452637414));
#37596=CARTESIAN_POINT('Ctrl Pts',(-4.50115689268563,-0.451816019874252,
377.12849619244));
#37597=CARTESIAN_POINT('Ctrl Pts',(-4.51779810878667,-0.225976373769842,
377.120539747466));
#37598=CARTESIAN_POINT('Ctrl Pts',(-4.51759690135649,-0.00010734614409786,
377.112583302492));
#37599=CARTESIAN_POINT('Ctrl Pts',(-4.51776278108284,0.000115059314115817,
377.387416697508));
#37600=CARTESIAN_POINT('Ctrl Pts',(-4.51717353368206,-0.578363695817441,
377.407796296326));
#37601=CARTESIAN_POINT('Ctrl Pts',(-4.40559318176197,-1.15706321872293,
377.428175895145));
#37602=CARTESIAN_POINT('Ctrl Pts',(-4.18884997964351,-1.69325291121775,
377.448555493963));
#37603=CARTESIAN_POINT('Ctrl Pts',(-3.90833367742039,-2.38720754674346,
377.47493145245));
#37604=CARTESIAN_POINT('Ctrl Pts',(-3.45166537116277,-3.0099565064637,377.501307410936));
#37605=CARTESIAN_POINT('Ctrl Pts',(-2.87413234662247,-3.48610568219112,
377.527683369423));
#37606=CARTESIAN_POINT('Ctrl Pts',(-2.29659932208215,-3.96225485791856,
377.55405932791));
#37607=CARTESIAN_POINT('Ctrl Pts',(-1.59820157925914,-4.29180424965317,
377.580435286396));
#37608=CARTESIAN_POINT('Ctrl Pts',(-0.863491768396101,-4.43485642825323,
377.606811244883));
#37609=CARTESIAN_POINT('Ctrl Pts',(-0.128781957533104,-4.57790860685328,
377.633187203369));
#37610=CARTESIAN_POINT('Ctrl Pts',(0.642239921369918,-4.5344635723188,377.659563161856));
#37611=CARTESIAN_POINT('Ctrl Pts',(1.35622885978989,-4.30978106789426,377.685939120342));
#37612=CARTESIAN_POINT('Ctrl Pts',(2.07021779820986,-4.08509856346973,377.712315078829));
#37613=CARTESIAN_POINT('Ctrl Pts',(2.72717379614679,-3.67917858915515,377.738691037316));
#37614=CARTESIAN_POINT('Ctrl Pts',(3.24756141510707,-3.14116450196653,377.765066995802));
#37615=CARTESIAN_POINT('Ctrl Pts',(3.76794903406735,-2.6031504147779,377.791442954289));
#37616=CARTESIAN_POINT('Ctrl Pts',(4.15176827405098,-1.93304221471522,377.817818912776));
#37617=CARTESIAN_POINT('Ctrl Pts',(4.35255143912362,-1.21196763285564,377.844194871262));
#37618=CARTESIAN_POINT('Ctrl Pts',(4.55333460419626,-0.49089305099606,377.870570829749));
#37619=CARTESIAN_POINT('Ctrl Pts',(4.57108169435792,0.28114791266043,377.896946788235));
#37620=CARTESIAN_POINT('Ctrl Pts',(4.40364412948689,1.01068687244984,377.923322746722));
#37621=CARTESIAN_POINT('Ctrl Pts',(4.23620656461585,1.7402258322393,377.949698705208));
#37622=CARTESIAN_POINT('Ctrl Pts',(3.88358434471212,2.42726278816168,377.976074663695));
#37623=CARTESIAN_POINT('Ctrl Pts',(3.38846824810894,2.98862050198153,378.002450622182));
#37624=CARTESIAN_POINT('Ctrl Pts',(2.89335215150579,3.54997821580136,378.028826580668));
#37625=CARTESIAN_POINT('Ctrl Pts',(2.25574217820322,3.98565668751868,378.055202539155));
#37626=CARTESIAN_POINT('Ctrl Pts',(1.55283160898984,4.2429097995867,378.081578497641));
#37627=CARTESIAN_POINT('Ctrl Pts',(0.849921039776497,4.5001629116547,378.107954456128));
#37628=CARTESIAN_POINT('Ctrl Pts',(0.0817098746523573,4.57899066407343,
378.134330414615));
#37629=CARTESIAN_POINT('Ctrl Pts',(-0.658797161460833,4.46984964773514,
378.160706373101));
#37630=CARTESIAN_POINT('Ctrl Pts',(-1.39930419757415,4.36070863139684,378.187082331588));
#37631=CARTESIAN_POINT('Ctrl Pts',(-2.11210710467651,4.06359884630146,378.213458290074));
#37632=CARTESIAN_POINT('Ctrl Pts',(-2.71090924805577,3.61449036824177,378.239834248561));
#37633=CARTESIAN_POINT('Ctrl Pts',(-3.309711391435,3.16538189018211,378.266210207048));
#37634=CARTESIAN_POINT('Ctrl Pts',(-3.79451277109115,2.56427471915816,378.292586165534));
#37635=CARTESIAN_POINT('Ctrl Pts',(-4.10662012532275,1.8839428652698,378.318962124021));
#37636=CARTESIAN_POINT('Ctrl Pts',(-4.37662833282249,1.29537876422316,378.341780315183));
#37637=CARTESIAN_POINT('Ctrl Pts',(-4.5173887163544,0.647521251956349,378.364598506346));
#37638=CARTESIAN_POINT('Ctrl Pts',(-4.51797310231548,-9.04168125550817E-5,
378.387416697508));
#37639=CARTESIAN_POINT('Origin',(0.,0.,387.));
#37640=CARTESIAN_POINT('',(-4.51737365644452,-1.98811769755447E-6,379.387416697508));
#37641=CARTESIAN_POINT('',(-4.51813007169143,-2.03714566067892E-5,379.112583302492));
#37642=CARTESIAN_POINT('',(-4.51775,5.53264807684796E-16,387.));
#37643=CARTESIAN_POINT('Ctrl Pts',(-4.51813007169143,-2.03714566067892E-5,
379.112583302492));
#37644=CARTESIAN_POINT('Ctrl Pts',(-4.517945231463,0.728944748987095,379.086896084477));
#37645=CARTESIAN_POINT('Ctrl Pts',(-4.33810981632971,1.45799779441603,379.061208866463));
#37646=CARTESIAN_POINT('Ctrl Pts',(-3.99878265125311,2.10316590777759,379.035521648449));
#37647=CARTESIAN_POINT('Ctrl Pts',(-3.65035725094643,2.76563263988363,379.009145689962));
#37648=CARTESIAN_POINT('Ctrl Pts',(-3.13377267064052,3.33965579170571,378.982769731476));
#37649=CARTESIAN_POINT('Ctrl Pts',(-2.51157005653494,3.75574032365363,378.956393772989));
#37650=CARTESIAN_POINT('Ctrl Pts',(-1.88936744242933,4.17182485560157,378.930017814502));
#37651=CARTESIAN_POINT('Ctrl Pts',(-1.16154679452404,4.42997076767533,378.903641856016));
#37652=CARTESIAN_POINT('Ctrl Pts',(-0.416222894566461,4.49892520827358,
378.877265897529));
#37653=CARTESIAN_POINT('Ctrl Pts',(0.329101005391076,4.56787964887184,378.850889939042));
#37654=CARTESIAN_POINT('Ctrl Pts',(1.0919281574009,4.44764261799461,378.824513980556));
#37655=CARTESIAN_POINT('Ctrl Pts',(1.779905660781,4.15277080589822,378.798138022069));
#37656=CARTESIAN_POINT('Ctrl Pts',(2.46788316416111,3.85789899380182,378.771762063583));
#37657=CARTESIAN_POINT('Ctrl Pts',(3.08101101891148,3.38839240048625,378.745386105096));
#37658=CARTESIAN_POINT('Ctrl Pts',(3.54505991145048,2.80109259965241,378.71901014661));
#37659=CARTESIAN_POINT('Ctrl Pts',(4.00910880398948,2.21379279881858,378.692634188123));
#37660=CARTESIAN_POINT('Ctrl Pts',(4.3240787343171,1.50869979046648,378.666258229636));
#37661=CARTESIAN_POINT('Ctrl Pts',(4.45183735932425,0.771176797969019,378.63988227115));
#37662=CARTESIAN_POINT('Ctrl Pts',(4.57959598433139,0.0336538054715552,
378.613506312663));
#37663=CARTESIAN_POINT('Ctrl Pts',(4.52014330401807,-0.736299171171277,
378.587130354177));
#37664=CARTESIAN_POINT('Ctrl Pts',(4.28067705310806,-1.44546653181419,378.56075439569));
#37665=CARTESIAN_POINT('Ctrl Pts',(4.04121080219804,-2.1546338924571,378.534378437203));
#37666=CARTESIAN_POINT('Ctrl Pts',(3.62173098069132,-2.80301563710009,378.508002478717));
#37667=CARTESIAN_POINT('Ctrl Pts',(3.07302259039553,-3.31211438306704,378.48162652023));
#37668=CARTESIAN_POINT('Ctrl Pts',(2.5243142000997,-3.82121312903403,378.455250561744));
#37669=CARTESIAN_POINT('Ctrl Pts',(1.84637724101477,-4.19102887632496,378.428874603257));
#37670=CARTESIAN_POINT('Ctrl Pts',(1.12128724556784,-4.37678928445587,378.40249864477));
#37671=CARTESIAN_POINT('Ctrl Pts',(0.396197250120947,-4.56254969258676,
378.376122686284));
#37672=CARTESIAN_POINT('Ctrl Pts',(-0.37604578168795,-4.56425476155764,
378.349746727797));
#37673=CARTESIAN_POINT('Ctrl Pts',(-1.10194900048777,-4.38169806444086,
378.323370769311));
#37674=CARTESIAN_POINT('Ctrl Pts',(-1.82785221928764,-4.19914136732407,
378.296994810824));
#37675=CARTESIAN_POINT('Ctrl Pts',(-2.50741562507842,-3.83232290411959,
378.270618852338));
#37676=CARTESIAN_POINT('Ctrl Pts',(-3.05836677703682,-3.32565214427459,
378.244242893851));
#37677=CARTESIAN_POINT('Ctrl Pts',(-3.60931792899519,-2.81898138442963,
378.217866935364));
#37678=CARTESIAN_POINT('Ctrl Pts',(-4.0316568271212,-2.17245832794416,378.191490976878));
#37679=CARTESIAN_POINT('Ctrl Pts',(-4.27425233088056,-1.46435533241182,
378.165115018391));
#37680=CARTESIAN_POINT('Ctrl Pts',(-4.435307559621,-0.99425721373283,378.147604446425));
#37681=CARTESIAN_POINT('Ctrl Pts',(-4.51714237540265,-0.497018246743604,
378.130093874458));
#37682=CARTESIAN_POINT('Ctrl Pts',(-4.51753028950122,9.61292306860575E-5,
378.112583302492));
#37683=CARTESIAN_POINT('Ctrl Pts',(-4.51797310231548,-9.04168125550817E-5,
378.387416697508));
#37684=CARTESIAN_POINT('Ctrl Pts',(-4.51806421862098,-0.101064749856769,
378.390974464832));
#37685=CARTESIAN_POINT('Ctrl Pts',(-4.51474759603089,-0.202033106339626,
378.394532232156));
#37686=CARTESIAN_POINT('Ctrl Pts',(-4.50798181202017,-0.302769806622464,
378.398089999481));
#37687=CARTESIAN_POINT('Ctrl Pts',(-4.45782281567894,-1.04959408787382,
378.424465957967));
#37688=CARTESIAN_POINT('Ctrl Pts',(-4.2180914941894,-1.78368611362381,378.450841916454));
#37689=CARTESIAN_POINT('Ctrl Pts',(-3.81781130701489,-2.41617184764166,
378.47721787494));
#37690=CARTESIAN_POINT('Ctrl Pts',(-3.41753111984037,-3.04865758165951,
378.503593833427));
#37691=CARTESIAN_POINT('Ctrl Pts',(-2.85670206698089,-3.57953702394521,
378.529969791913));
#37692=CARTESIAN_POINT('Ctrl Pts',(-2.20322182313489,-3.94453839775569,
378.5563457504));
#37693=CARTESIAN_POINT('Ctrl Pts',(-1.54974157928885,-4.30953977156619,
378.582721708887));
#37694=CARTESIAN_POINT('Ctrl Pts',(-0.803610144456304,-4.50866307690144,
378.609097667373));
#37695=CARTESIAN_POINT('Ctrl Pts',(-0.0551591253652737,-4.51780112933225,
378.63547362586));
#37696=CARTESIAN_POINT('Ctrl Pts',(0.693291893725671,-4.52693918176306,
378.661849584346));
#37697=CARTESIAN_POINT('Ctrl Pts',(1.44406249707508,-4.34609198128947,378.688225542833));
#37698=CARTESIAN_POINT('Ctrl Pts',(2.10625942952888,-3.99715408620027,378.71460150132));
#37699=CARTESIAN_POINT('Ctrl Pts',(2.76845636198275,-3.64821619111103,378.740977459806));
#37700=CARTESIAN_POINT('Ctrl Pts',(3.34207962354098,-3.13118760140616,378.767353418293));
#37701=CARTESIAN_POINT('Ctrl Pts',(3.75768258797375,-2.50866321799992,378.793729376779));
#37702=CARTESIAN_POINT('Ctrl Pts',(4.1732855524065,-1.88613883459371,378.820105335266));
#37703=CARTESIAN_POINT('Ctrl Pts',(4.43086821971381,-1.15811865748618,378.846481293753));
#37704=CARTESIAN_POINT('Ctrl Pts',(4.49924592843132,-0.412741624749648,
378.872857252239));
#37705=CARTESIAN_POINT('Ctrl Pts',(4.56762363714884,0.332635407986881,378.899233210726));
#37706=CARTESIAN_POINT('Ctrl Pts',(4.44679638727653,1.09536929635249,378.925609169213));
#37707=CARTESIAN_POINT('Ctrl Pts',(4.15139232488624,1.78311843077862,378.951985127699));
#37708=CARTESIAN_POINT('Ctrl Pts',(3.85598826249595,2.47086756520474,378.978361086186));
#37709=CARTESIAN_POINT('Ctrl Pts',(3.38600738758769,3.08363194569147,379.004737044672));
#37710=CARTESIAN_POINT('Ctrl Pts',(2.79834869352904,3.54722626325572,379.031113003159));
#37711=CARTESIAN_POINT('Ctrl Pts',(2.2106899994704,4.01082058081996,379.057488961645));
#37712=CARTESIAN_POINT('Ctrl Pts',(1.5053534862614,4.32524483546169,379.083864920132));
#37713=CARTESIAN_POINT('Ctrl Pts',(0.767731857583539,4.4524327471797,379.110240878618));
#37714=CARTESIAN_POINT('Ctrl Pts',(0.030110228905678,4.5796206588977,379.136616837105));
#37715=CARTESIAN_POINT('Ctrl Pts',(-0.739796515241018,4.51957222769198,
379.162992795591));
#37716=CARTESIAN_POINT('Ctrl Pts',(-1.44877837192307,4.27955731382987,379.189368754078));
#37717=CARTESIAN_POINT('Ctrl Pts',(-2.15776022860516,4.03954239996775,379.215744712565));
#37718=CARTESIAN_POINT('Ctrl Pts',(-2.80581719782259,3.61956100344924,379.242120671052));
#37719=CARTESIAN_POINT('Ctrl Pts',(-3.31449121636045,3.0704588500705,379.268496629538));
#37720=CARTESIAN_POINT('Ctrl Pts',(-3.82316523489829,2.52135669669179,379.294872588025));
#37721=CARTESIAN_POINT('Ctrl Pts',(-4.19245630275656,1.84313378645288,379.321248546511));
#37722=CARTESIAN_POINT('Ctrl Pts',(-4.37765560061389,1.11790027091894,379.347624504998));
#37723=CARTESIAN_POINT('Ctrl Pts',(-4.4707894813135,0.753191481541508,379.360888569168));
#37724=CARTESIAN_POINT('Ctrl Pts',(-4.51736785070585,0.376594041376692,
379.374152633338));
#37725=CARTESIAN_POINT('Ctrl Pts',(-4.51737365644452,-1.98811769755447E-6,
379.387416697508));
#37726=CARTESIAN_POINT('Origin',(0.,0.,387.));
#37727=CARTESIAN_POINT('',(-4.51796103056296,9.30366574888874E-5,380.387416697508));
#37728=CARTESIAN_POINT('',(-4.51744861143269,-7.15418913582019E-5,380.112583302492));
#37729=CARTESIAN_POINT('',(-4.51775,5.53264807684796E-16,387.));
#37730=CARTESIAN_POINT('Ctrl Pts',(-4.51744861143269,-7.15418913582019E-5,
380.112583302492));
#37731=CARTESIAN_POINT('Ctrl Pts',(-4.51718913038702,0.45796072853139,380.09645021147));
#37732=CARTESIAN_POINT('Ctrl Pts',(-4.44792028854276,0.916069730534027,
380.080317120448));
#37733=CARTESIAN_POINT('Ctrl Pts',(-4.31082918580142,1.35289366117352,380.064184029426));
#37734=CARTESIAN_POINT('Ctrl Pts',(-4.08669921406521,2.0670562382494,380.037808070939));
#37735=CARTESIAN_POINT('Ctrl Pts',(-3.68128769636301,2.72432612859277,380.011432112453));
#37736=CARTESIAN_POINT('Ctrl Pts',(-3.14367643259018,3.24512989181911,379.985056153966));
#37737=CARTESIAN_POINT('Ctrl Pts',(-2.60606516881736,3.76593365504543,379.958680195479));
#37738=CARTESIAN_POINT('Ctrl Pts',(-1.93625415897387,4.15027129115475,379.932304236993));
#37739=CARTESIAN_POINT('Ctrl Pts',(-1.21533515432327,4.35161234374879,379.905928278506));
#37740=CARTESIAN_POINT('Ctrl Pts',(-0.494416149672638,4.55295339634284,
379.87955232002));
#37741=CARTESIAN_POINT('Ctrl Pts',(0.27761084978516,4.57129786542164,379.853176361533));
#37742=CARTESIAN_POINT('Ctrl Pts',(1.0072791489844,4.40442484822049,379.826800403046));
#37743=CARTESIAN_POINT('Ctrl Pts',(1.73694744818368,4.23755183101932,379.80042444456));
#37744=CARTESIAN_POINT('Ctrl Pts',(2.4242570471244,3.88546132753817,379.774048486073));
#37745=CARTESIAN_POINT('Ctrl Pts',(2.98599769960395,3.39077974300318,379.747672527587));
#37746=CARTESIAN_POINT('Ctrl Pts',(3.5477383520835,2.89609815846819,379.7212965691));
#37747=CARTESIAN_POINT('Ctrl Pts',(3.98391005810188,2.25882549287937,379.694920610614));
#37748=CARTESIAN_POINT('Ctrl Pts',(4.24170698590533,1.55611419032241,379.668544652127));
#37749=CARTESIAN_POINT('Ctrl Pts',(4.49950391370875,0.853402887765529,379.64216869364));
#37750=CARTESIAN_POINT('Ctrl Pts',(4.57892606329728,0.0852529482405344,
379.615792735154));
#37751=CARTESIAN_POINT('Ctrl Pts',(4.47035806391024,-0.655338315706838,
379.589416776667));
#37752=CARTESIAN_POINT('Ctrl Pts',(4.36179006452319,-1.39592957965429,379.56304081818));
#37753=CARTESIAN_POINT('Ctrl Pts',(4.06523191616051,-2.10896216802411,379.536664859694));
#37754=CARTESIAN_POINT('Ctrl Pts',(3.61658690982335,-2.70811163937072,379.510288901207));
#37755=CARTESIAN_POINT('Ctrl Pts',(3.16794190348622,-3.30726111071731,379.483912942721));
#37756=CARTESIAN_POINT('Ctrl Pts',(2.56721003917463,-3.79252746504069,379.457536984234));
#37757=CARTESIAN_POINT('Ctrl Pts',(1.88711988987541,-4.10516114773068,379.431161025748));
#37758=CARTESIAN_POINT('Ctrl Pts',(1.20702974057619,-4.41779483042066,379.404785067261));
#37759=CARTESIAN_POINT('Ctrl Pts',(0.447581306289357,-4.55779584147724,
379.378409108774));
#37760=CARTESIAN_POINT('Ctrl Pts',(-0.299281562218895,-4.50821473247633,
379.352033150288));
#37761=CARTESIAN_POINT('Ctrl Pts',(-1.04614443072715,-4.45863362347542,
379.325657191801));
#37762=CARTESIAN_POINT('Ctrl Pts',(-1.7804217334568,-4.21947039441701,379.299281233315));
#37763=CARTESIAN_POINT('Ctrl Pts',(-2.41321700332044,-3.81967972773712,
379.272905274828));
#37764=CARTESIAN_POINT('Ctrl Pts',(-3.04601227318407,-3.41988906105724,
379.246529316342));
#37765=CARTESIAN_POINT('Ctrl Pts',(-3.57732551018167,-2.85947095675588,
379.220153357855));
#37766=CARTESIAN_POINT('Ctrl Pts',(-3.94283241951303,-2.20627333738088,
379.193777399368));
#37767=CARTESIAN_POINT('Ctrl Pts',(-4.30833932884442,-1.55307571800585,
379.167401440882));
#37768=CARTESIAN_POINT('Ctrl Pts',(-4.50803991050956,-0.807098583557167,
379.141025482395));
#37769=CARTESIAN_POINT('Ctrl Pts',(-4.51775709118839,-0.0586548601377958,
379.114649523908));
#37770=CARTESIAN_POINT('Ctrl Pts',(-4.51801083042644,-0.0391111728918336,
379.113960783436));
#37771=CARTESIAN_POINT('Ctrl Pts',(-4.51813502773401,-0.0195658037794806,
379.113272042964));
#37772=CARTESIAN_POINT('Ctrl Pts',(-4.51813007169143,-2.03714566067892E-5,
379.112583302492));
#37773=CARTESIAN_POINT('Ctrl Pts',(-4.51737365644452,-1.98811769755447E-6,
379.387416697508));
#37774=CARTESIAN_POINT('Ctrl Pts',(-4.51737939557777,-0.372277579931259,
379.400528591825));
#37775=CARTESIAN_POINT('Ctrl Pts',(-4.47187503399554,-0.744551793256104,
379.413640486141));
#37776=CARTESIAN_POINT('Ctrl Pts',(-4.38084409953505,-1.10533911035289,
379.426752380458));
#37777=CARTESIAN_POINT('Ctrl Pts',(-4.19772577274251,-1.83110085526187,
379.453128338944));
#37778=CARTESIAN_POINT('Ctrl Pts',(-3.83038159130104,-2.51038022425081,
379.479504297431));
#37779=CARTESIAN_POINT('Ctrl Pts',(-3.32328467158491,-3.06093916387039,
379.505880255917));
#37780=CARTESIAN_POINT('Ctrl Pts',(-2.81618775186881,-3.61149810348995,
379.532256214404));
#37781=CARTESIAN_POINT('Ctrl Pts',(-2.16933809387807,-4.03333661374015,
379.558632172891));
#37782=CARTESIAN_POINT('Ctrl Pts',(-1.46104759574481,-4.27538413435274,
379.585008131377));
#37783=CARTESIAN_POINT('Ctrl Pts',(-0.752757097611556,-4.51743165496533,
379.611384089864));
#37784=CARTESIAN_POINT('Ctrl Pts',(0.0169742406642152,-4.57968818594031,
379.63776004835));
#37785=CARTESIAN_POINT('Ctrl Pts',(0.75495765194394,-4.45461653984696,379.664136006837));
#37786=CARTESIAN_POINT('Ctrl Pts',(1.49294106322366,-4.32954489375361,379.690511965324));
#37787=CARTESIAN_POINT('Ctrl Pts',(2.19917654750734,-4.01714507059193,379.71688792381));
#37788=CARTESIAN_POINT('Ctrl Pts',(2.78816256572898,-3.55523825929773,379.743263882297));
#37789=CARTESIAN_POINT('Ctrl Pts',(3.37714858395063,-3.09333144800353,379.769639840783));
#37790=CARTESIAN_POINT('Ctrl Pts',(3.84888513611024,-2.48191764857682,379.79601579927));
#37791=CARTESIAN_POINT('Ctrl Pts',(4.14626067493935,-1.79501865972427,379.822391757756));
#37792=CARTESIAN_POINT('Ctrl Pts',(4.44363621376846,-1.10811967087172,379.848767716243));
#37793=CARTESIAN_POINT('Ctrl Pts',(4.56665073926708,-0.34573549259334,379.87514367473));
#37794=CARTESIAN_POINT('Ctrl Pts',(4.50041129930853,0.399834603758797,379.901519633216));
#37795=CARTESIAN_POINT('Ctrl Pts',(4.43417185934997,1.14540470011094,379.927895591703));
#37796=CARTESIAN_POINT('Ctrl Pts',(4.17867845393423,1.87416071453683,379.954271550189));
#37797=CARTESIAN_POINT('Ctrl Pts',(3.76486280466181,2.49787462363122,379.980647508676));
#37798=CARTESIAN_POINT('Ctrl Pts',(3.35104715538937,3.12158853272565,380.007023467163));
#37799=CARTESIAN_POINT('Ctrl Pts',(2.77890926226022,3.64026033648856,380.033399425649));
#37800=CARTESIAN_POINT('Ctrl Pts',(2.11771592297733,3.99109619564288,380.059775384136));
#37801=CARTESIAN_POINT('Ctrl Pts',(1.45652258369447,4.34193205479719,380.086151342622));
#37802=CARTESIAN_POINT('Ctrl Pts',(0.706273798257865,4.52493196934294,380.112527301109));
#37803=CARTESIAN_POINT('Ctrl Pts',(-0.0422003529064303,4.5179407591868,
380.138903259596));
#37804=CARTESIAN_POINT('Ctrl Pts',(-0.790674504070726,4.51094954903066,
380.165279218082));
#37805=CARTESIAN_POINT('Ctrl Pts',(-1.53737402096271,4.31396721417262,380.191655176569));
#37806=CARTESIAN_POINT('Ctrl Pts',(-2.19189852108271,3.95084173899465,380.218031135055));
#37807=CARTESIAN_POINT('Ctrl Pts',(-2.84642302120274,3.58771626381665,380.244407093542));
#37808=CARTESIAN_POINT('Ctrl Pts',(-3.40877250455077,3.05844764831869,380.270783052029));
#37809=CARTESIAN_POINT('Ctrl Pts',(-3.81086522305661,2.42711265189824,380.297159010515));
#37810=CARTESIAN_POINT('Ctrl Pts',(-4.21295794156245,1.7957776554778,380.323534969002));
#37811=CARTESIAN_POINT('Ctrl Pts',(-4.4547938952261,1.06237627813486,380.349910927489));
#37812=CARTESIAN_POINT('Ctrl Pts',(-4.50709482389231,0.315698941635839,
380.376286885975));
#37813=CARTESIAN_POINT('Ctrl Pts',(-4.51445126403015,0.210674283980221,
380.379996823153));
#37814=CARTESIAN_POINT('Ctrl Pts',(-4.51805792159162,0.105386973232761,
380.38370676033));
#37815=CARTESIAN_POINT('Ctrl Pts',(-4.51796103056296,9.30366574888874E-5,
380.387416697508));
#37816=CARTESIAN_POINT('Origin',(0.,0.,387.));
#37817=CARTESIAN_POINT('',(-4.51777632728029,-0.000114640610663838,381.387416697508));
#37818=CARTESIAN_POINT('',(-4.51771140424386,0.000115276608145368,381.112583302492));
#37819=CARTESIAN_POINT('',(-4.51775,5.53264807684796E-16,387.));
#37820=CARTESIAN_POINT('Ctrl Pts',(-4.51771140424386,0.000115276608145367,
381.112583302492));
#37821=CARTESIAN_POINT('Ctrl Pts',(-4.51789787410811,0.186866521003934,
381.106004338462));
#37822=CARTESIAN_POINT('Ctrl Pts',(-4.50653449305084,0.373595224723727,
381.099425374433));
#37823=CARTESIAN_POINT('Ctrl Pts',(-4.48344098370869,0.558861765736475,
381.092846410403));
#37824=CARTESIAN_POINT('Ctrl Pts',(-4.3908559747359,1.30162043908853,381.066470451916));
#37825=CARTESIAN_POINT('Ctrl Pts',(-4.10973064608376,2.02087752596908,381.04009449343));
#37826=CARTESIAN_POINT('Ctrl Pts',(-3.6740998895201,2.62955500597139,381.013718534943));
#37827=CARTESIAN_POINT('Ctrl Pts',(-3.23846913295646,3.23823248597366,380.987342576457));
#37828=CARTESIAN_POINT('Ctrl Pts',(-2.6483329484813,3.73633035909772,380.96096661797));
#37829=CARTESIAN_POINT('Ctrl Pts',(-1.9751371259962,4.06354560219426,380.934590659483));
#37830=CARTESIAN_POINT('Ctrl Pts',(-1.30194130351109,4.3907608452908,380.908214700997));
#37831=CARTESIAN_POINT('Ctrl Pts',(-0.545685843016022,4.54709345835984,
380.88183874251));
#37832=CARTESIAN_POINT('Ctrl Pts',(0.202071967249689,4.51361678121356,380.855462784024));
#37833=CARTESIAN_POINT('Ctrl Pts',(0.949829777515443,4.48014010406728,380.829086825537));
#37834=CARTESIAN_POINT('Ctrl Pts',(1.68908993755185,4.25685413670566,380.802710867051));
#37835=CARTESIAN_POINT('Ctrl Pts',(2.33035272260718,3.87079135524483,380.776334908564));
#37836=CARTESIAN_POINT('Ctrl Pts',(2.97161550766248,3.48472857378402,380.749958950077));
#37837=CARTESIAN_POINT('Ctrl Pts',(3.51488091773671,2.93588897822401,380.723582991591));
#37838=CARTESIAN_POINT('Ctrl Pts',(3.89437764890032,2.29071872025929,380.697207033104));
#37839=CARTESIAN_POINT('Ctrl Pts',(4.27387438006393,1.64554846229457,380.670831074617));
#37840=CARTESIAN_POINT('Ctrl Pts',(4.48960243231693,0.904047541925131,380.644455116131));
#37841=CARTESIAN_POINT('Ctrl Pts',(4.51544434073745,0.155986965169938,380.618079157644));
#37842=CARTESIAN_POINT('Ctrl Pts',(4.54128624915798,-0.592073611585275,
380.591703199158));
#37843=CARTESIAN_POINT('Ctrl Pts',(4.37724201374605,-1.34669384472619,380.565327240671));
#37844=CARTESIAN_POINT('Ctrl Pts',(4.04317191469819,-2.01651441745319,380.538951282185));
#37845=CARTESIAN_POINT('Ctrl Pts',(3.70910181565035,-2.68633499018016,380.512575323698));
#37846=CARTESIAN_POINT('Ctrl Pts',(3.20500585296659,-3.27135590249316,380.486199365211));
#37847=CARTESIAN_POINT('Ctrl Pts',(2.59191321819219,-3.70075065317313,380.459823406725));
#37848=CARTESIAN_POINT('Ctrl Pts',(1.9788205834178,-4.13014540385311,380.433447448238));
#37849=CARTESIAN_POINT('Ctrl Pts',(1.25673127655275,-4.40391399290007,380.407071489751));
#37850=CARTESIAN_POINT('Ctrl Pts',(0.513066205288616,-4.48891218410335,
380.380695531265));
#37851=CARTESIAN_POINT('Ctrl Pts',(-0.230598865975566,-4.57391037530665,
380.354319572778));
#37852=CARTESIAN_POINT('Ctrl Pts',(-0.995839701638859,-4.47013816866624,
380.327943614292));
#37853=CARTESIAN_POINT('Ctrl Pts',(-1.69001118451102,-4.19015891391108,
380.301567655805));
#37854=CARTESIAN_POINT('Ctrl Pts',(-2.38418266738314,-3.91017965915592,
380.275191697319));
#37855=CARTESIAN_POINT('Ctrl Pts',(-3.00728479746414,-3.45399335628602,
380.248815738832));
#37856=CARTESIAN_POINT('Ctrl Pts',(-3.48388070942679,-2.87682893653492,
380.222439780345));
#37857=CARTESIAN_POINT('Ctrl Pts',(-3.96047662138947,-2.2996645167838,380.196063821859));
#37858=CARTESIAN_POINT('Ctrl Pts',(-4.29056631523378,-1.60152198015145,
380.169687863372));
#37859=CARTESIAN_POINT('Ctrl Pts',(-4.43418694927082,-0.866923079931074,
380.143311904886));
#37860=CARTESIAN_POINT('Ctrl Pts',(-4.48996073737275,-0.581648170267025,
380.133069037421));
#37861=CARTESIAN_POINT('Ctrl Pts',(-4.5176133554335,-0.290875321156064,
380.122826169956));
#37862=CARTESIAN_POINT('Ctrl Pts',(-4.51744861143269,-7.15418913582019E-5,
380.112583302492));
#37863=CARTESIAN_POINT('Ctrl Pts',(-4.51796103056296,9.30366574888874E-5,
380.387416697508));
#37864=CARTESIAN_POINT('Ctrl Pts',(-4.5173690706415,-0.643204813367623,
380.410082718817));
#37865=CARTESIAN_POINT('Ctrl Pts',(-4.37853653898567,-1.28674998247137,
380.432748740126));
#37866=CARTESIAN_POINT('Ctrl Pts',(-4.11200700232459,-1.87215597270644,
380.455414761435));
#37867=CARTESIAN_POINT('Ctrl Pts',(-3.80185234842186,-2.55338025489479,
380.481790719921));
#37868=CARTESIAN_POINT('Ctrl Pts',(-3.3187771369476,-3.15587552361643,380.508166678408));
#37869=CARTESIAN_POINT('Ctrl Pts',(-2.72126564826557,-3.60669971648272,
380.534542636895));
#37870=CARTESIAN_POINT('Ctrl Pts',(-2.12375415958355,-4.05752390934902,
380.560918595381));
#37871=CARTESIAN_POINT('Ctrl Pts',(-1.41180639369374,-4.35667702635998,
380.587294553868));
#37872=CARTESIAN_POINT('Ctrl Pts',(-0.671615456256834,-4.46794161244568,
380.613670512354));
#37873=CARTESIAN_POINT('Ctrl Pts',(0.0685754811800957,-4.57920619853139,
380.640046470841));
#37874=CARTESIAN_POINT('Ctrl Pts',(0.837009590164088,-4.50258225369185,
380.666422429328));
#37875=CARTESIAN_POINT('Ctrl Pts',(1.54065515471516,-4.24734637951232,380.692798387814));
#37876=CARTESIAN_POINT('Ctrl Pts',(2.24430071926626,-3.99211050533279,380.719174346301));
#37877=CARTESIAN_POINT('Ctrl Pts',(2.88315773938438,-3.55826270181326,380.745550304787));
#37878=CARTESIAN_POINT('Ctrl Pts',(3.37988195854491,-2.99832745369971,380.771926263274));
#37879=CARTESIAN_POINT('Ctrl Pts',(3.87660617770542,-2.4383922055862,380.79830222176));
#37880=CARTESIAN_POINT('Ctrl Pts',(4.23119759590837,-1.75236951287867,380.824678180247));
#37881=CARTESIAN_POINT('Ctrl Pts',(4.40072703064927,-1.02331382039902,380.851054138734));
#37882=CARTESIAN_POINT('Ctrl Pts',(4.57025646539019,-0.294258127919331,
380.87743009722));
#37883=CARTESIAN_POINT('Ctrl Pts',(4.55472391666906,0.477830564332509,380.903806055707));
#37884=CARTESIAN_POINT('Ctrl Pts',(4.35600985757286,1.19947809235303,380.930182014193));
#37885=CARTESIAN_POINT('Ctrl Pts',(4.15729579847668,1.92112562037352,380.95655797268));
#37886=CARTESIAN_POINT('Ctrl Pts',(3.77540022900545,2.59233198416271,380.982933931167));
#37887=CARTESIAN_POINT('Ctrl Pts',(3.25655795281734,3.131836501679,381.009309889653));
#37888=CARTESIAN_POINT('Ctrl Pts',(2.73771567662922,3.6713410191953,381.03568584814));
#37889=CARTESIAN_POINT('Ctrl Pts',(2.08192669372421,4.07914369043871,381.062061806626));
#37890=CARTESIAN_POINT('Ctrl Pts',(1.36858515603701,4.30587322665008,381.088437765113));
#37891=CARTESIAN_POINT('Ctrl Pts',(0.655243618349795,4.53260276286145,381.1148137236));
#37892=CARTESIAN_POINT('Ctrl Pts',(-0.11565047411956,4.57825916404077,381.141189682086));
#37893=CARTESIAN_POINT('Ctrl Pts',(-0.850767583518968,4.43731496427064,
381.167565640573));
#37894=CARTESIAN_POINT('Ctrl Pts',(-1.58588469291835,4.2963707645005,381.193941599059));
#37895=CARTESIAN_POINT('Ctrl Pts',(-2.28522481924775,3.96882596378091,381.220317557546));
#37896=CARTESIAN_POINT('Ctrl Pts',(-2.8641212210839,3.49433530220608,381.246693516033));
#37897=CARTESIAN_POINT('Ctrl Pts',(-3.44301762292008,3.01984464063123,381.273069474519));
#37898=CARTESIAN_POINT('Ctrl Pts',(-3.90147030026302,2.39840811820112,381.299445433006));
#37899=CARTESIAN_POINT('Ctrl Pts',(-4.18397593959467,1.70526095076376,381.325821391492));
#37900=CARTESIAN_POINT('Ctrl Pts',(-4.40388606866954,1.16569620642928,381.346353160164));
#37901=CARTESIAN_POINT('Ctrl Pts',(-4.51718122901344,0.58267845338523,381.366884928836));
#37902=CARTESIAN_POINT('Ctrl Pts',(-4.51777632728029,-0.000114640610663838,
381.387416697508));
#37903=CARTESIAN_POINT('Origin',(0.,0.,387.));
#37904=CARTESIAN_POINT('',(-4.51741634198117,5.54534861180178E-5,382.387416697508));
#37905=CARTESIAN_POINT('',(-4.51801683772092,-7.91791388051273E-5,382.112583302492));
#37906=CARTESIAN_POINT('',(-4.51775,5.53264807684796E-16,387.));
#37907=CARTESIAN_POINT('Ctrl Pts',(-4.51801683772092,-7.91791388051273E-5,
382.112583302492));
#37908=CARTESIAN_POINT('Ctrl Pts',(-4.51747244268795,0.664048991360067,
382.089182506968));
#37909=CARTESIAN_POINT('Ctrl Pts',(-4.36919765227329,1.32841221793627,382.065781711444));
#37910=CARTESIAN_POINT('Ctrl Pts',(-4.08568376167234,1.92892657382487,382.04238091592));
#37911=CARTESIAN_POINT('Ctrl Pts',(-3.76612408682134,2.60578996102738,382.016004957434));
#37912=CARTESIAN_POINT('Ctrl Pts',(-3.27475081492882,3.20153698377045,381.989628998947));
#37913=CARTESIAN_POINT('Ctrl Pts',(-2.67105284443962,3.64404256695937,381.963253040461));
#37914=CARTESIAN_POINT('Ctrl Pts',(-2.06735487395043,4.08654815014828,381.936877081974));
#37915=CARTESIAN_POINT('Ctrl Pts',(-1.35133220486457,4.37581229378304,381.910501123487));
#37916=CARTESIAN_POINT('Ctrl Pts',(-0.609671277576736,4.47681476732048,
381.884125165001));
#37917=CARTESIAN_POINT('Ctrl Pts',(0.131989649711098,4.57781724085793,381.857749206514));
#37918=CARTESIAN_POINT('Ctrl Pts',(0.899288835200903,4.49055804429805,381.831373248027));
#37919=CARTESIAN_POINT('Ctrl Pts',(1.59933196425767,4.22560135314543,381.804997289541));
#37920=CARTESIAN_POINT('Ctrl Pts',(2.29937509331447,3.9606446619928,381.778621331054));
#37921=CARTESIAN_POINT('Ctrl Pts',(2.93216216593823,3.5179904762474,381.752245372568));
#37922=CARTESIAN_POINT('Ctrl Pts',(3.42108379359719,2.95122943953659,381.725869414081));
#37923=CARTESIAN_POINT('Ctrl Pts',(3.91000542125612,2.38446840282581,381.699493455595));
#37924=CARTESIAN_POINT('Ctrl Pts',(4.25506160395026,1.69360051514964,381.673117497108));
#37925=CARTESIAN_POINT('Ctrl Pts',(4.41447755785592,0.962266812681007,381.646741538621));
#37926=CARTESIAN_POINT('Ctrl Pts',(4.57389351176158,0.23093311021233,381.620365580135));
#37927=CARTESIAN_POINT('Ctrl Pts',(4.54766923687872,-0.540866407048814,
381.593989621648));
#37928=CARTESIAN_POINT('Ctrl Pts',(4.33897961738306,-1.25969258453608,381.567613663161));
#37929=CARTESIAN_POINT('Ctrl Pts',(4.1302899978874,-1.9785187620233,381.541237704675));
#37930=CARTESIAN_POINT('Ctrl Pts',(3.73913503377896,-2.64437159973664,381.514861746188));
#37931=CARTESIAN_POINT('Ctrl Pts',(3.21287053227619,-3.17663854891175,381.488485787702));
#37932=CARTESIAN_POINT('Ctrl Pts',(2.68660603077342,-3.70890549808685,381.462109829215));
#37933=CARTESIAN_POINT('Ctrl Pts',(2.02523199187631,-4.1075865587237,381.435733870728));
#37934=CARTESIAN_POINT('Ctrl Pts',(1.3088187313399,-4.32441476457735,381.409357912242));
#37935=CARTESIAN_POINT('Ctrl Pts',(0.592405470803483,-4.54124297043101,
381.382981953755));
#37936=CARTESIAN_POINT('Ctrl Pts',(-0.179047011372244,-4.57621832150146,
381.356605995269));
#37937=CARTESIAN_POINT('Ctrl Pts',(-0.912141574983824,-4.42510647044643,
381.330230036782));
#37938=CARTESIAN_POINT('Ctrl Pts',(-1.64523613859541,-4.2739946193914,381.303854078296));
#37939=CARTESIAN_POINT('Ctrl Pts',(-2.33997278364284,-3.93679556621089,
381.277478119809));
#37940=CARTESIAN_POINT('Ctrl Pts',(-2.91224209659624,-3.45433285865933,
381.251102161322));
#37941=CARTESIAN_POINT('Ctrl Pts',(-3.48451140954963,-2.97187015110778,
381.224726202836));
#37942=CARTESIAN_POINT('Ctrl Pts',(-3.93431339040899,-2.34414378918517,
381.198350244349));
#37943=CARTESIAN_POINT('Ctrl Pts',(-4.20719203619195,-1.64715047831211,
381.171974285863));
#37944=CARTESIAN_POINT('Ctrl Pts',(-4.4120064713043,-1.1240084389856,381.152177291406));
#37945=CARTESIAN_POINT('Ctrl Pts',(-4.51715029114881,-0.561844529442614,
381.132380296949));
#37946=CARTESIAN_POINT('Ctrl Pts',(-4.51771140424386,0.000115276608145367,
381.112583302492));
#37947=CARTESIAN_POINT('Ctrl Pts',(-4.51777632728029,-0.000114640610663838,
381.387416697508));
#37948=CARTESIAN_POINT('Ctrl Pts',(-4.51794571683875,-0.166001638386794,
381.393260887323));
#37949=CARTESIAN_POINT('Ctrl Pts',(-4.50898407036945,-0.331870434133353,
381.399105077137));
#37950=CARTESIAN_POINT('Ctrl Pts',(-4.49075105445655,-0.496713740704063,
381.404949266952));
#37951=CARTESIAN_POINT('Ctrl Pts',(-4.40846192866641,-1.24068345228999,
381.431325225439));
#37952=CARTESIAN_POINT('Ctrl Pts',(-4.13732507576575,-1.96376506301729,
381.457701183925));
#37953=CARTESIAN_POINT('Ctrl Pts',(-3.71016611657994,-2.57841753032532,
381.484077142412));
#37954=CARTESIAN_POINT('Ctrl Pts',(-3.28300715739413,-3.19306999763336,
381.510453100898));
#37955=CARTESIAN_POINT('Ctrl Pts',(-2.69982609192317,-3.69929332152213,
381.536829059385));
#37956=CARTESIAN_POINT('Ctrl Pts',(-2.03122667735788,-4.03580075802764,
381.563205017872));
#37957=CARTESIAN_POINT('Ctrl Pts',(-1.36262726279259,-4.37230819453315,
381.589580976358));
#37958=CARTESIAN_POINT('Ctrl Pts',(-0.608609499132967,-4.5390997436554,
381.615956934845));
#37959=CARTESIAN_POINT('Ctrl Pts',(0.139540235761641,-4.51598251722816,
381.642332893331));
#37960=CARTESIAN_POINT('Ctrl Pts',(0.887689970656269,-4.49286529080092,
381.668708851818));
#37961=CARTESIAN_POINT('Ctrl Pts',(1.62997167678589,-4.2798392888242,381.695084810305));
#37962=CARTESIAN_POINT('Ctrl Pts',(2.27651982104296,-3.90269484814088,381.721460768791));
#37963=CARTESIAN_POINT('Ctrl Pts',(2.92306796530002,-3.52555040745756,381.747836727278));
#37964=CARTESIAN_POINT('Ctrl Pts',(3.47388254768454,-2.98428752806765,381.774212685764));
#37965=CARTESIAN_POINT('Ctrl Pts',(3.86227831153366,-2.3444350742905,381.800588644251));
#37966=CARTESIAN_POINT('Ctrl Pts',(4.25067407538277,-1.70458262051336,381.826964602737));
#37967=CARTESIAN_POINT('Ctrl Pts',(4.47665102069649,-0.966140592348972,
381.853340561224));
#37968=CARTESIAN_POINT('Ctrl Pts',(4.51285088376856,-0.21850966609316,381.879716519711));
#37969=CARTESIAN_POINT('Ctrl Pts',(4.54905074684063,0.529121260162651,381.906092478197));
#37970=CARTESIAN_POINT('Ctrl Pts',(4.39547352767104,1.28594108450989,381.932468436684));
#37971=CARTESIAN_POINT('Ctrl Pts',(4.07071230023681,1.96032419308837,381.95884439517));
#37972=CARTESIAN_POINT('Ctrl Pts',(3.74595107280257,2.63470730166687,381.985220353657));
#37973=CARTESIAN_POINT('Ctrl Pts',(3.25000583710367,3.2266536944766,382.011596312144));
#37974=CARTESIAN_POINT('Ctrl Pts',(2.64291900376427,3.66449842582154,382.03797227063));
#37975=CARTESIAN_POINT('Ctrl Pts',(2.03583217042486,4.10234315716648,382.064348229117));
#37976=CARTESIAN_POINT('Ctrl Pts',(1.31760373944494,4.38608622704663,382.090724187603));
#37977=CARTESIAN_POINT('Ctrl Pts',(0.575187195343948,4.48137582262626,382.11710014609));
#37978=CARTESIAN_POINT('Ctrl Pts',(-0.167229348757025,4.57666541820589,
382.143476104577));
#37979=CARTESIAN_POINT('Ctrl Pts',(-0.933834005979071,4.48350153948501,
382.169852063063));
#37980=CARTESIAN_POINT('Ctrl Pts',(-1.63181654587318,4.21316322184666,382.19622802155));
#37981=CARTESIAN_POINT('Ctrl Pts',(-2.32979908576728,3.94282490420832,382.222603980037));
#37982=CARTESIAN_POINT('Ctrl Pts',(-2.95915950833345,3.4953121476525,382.248979938523));
#37983=CARTESIAN_POINT('Ctrl Pts',(-3.44370327796121,2.9248038065255,382.27535589701));
#37984=CARTESIAN_POINT('Ctrl Pts',(-3.92824704758899,2.35429546539847,382.301731855496));
#37985=CARTESIAN_POINT('Ctrl Pts',(-4.26797416427836,1.66079153970024,382.328107813983));
#37986=CARTESIAN_POINT('Ctrl Pts',(-4.42175501618481,0.928252201802573,
382.354483772469));
#37987=CARTESIAN_POINT('Ctrl Pts',(-4.48575841876287,0.623370224843185,
382.365461414149));
#37988=CARTESIAN_POINT('Ctrl Pts',(-4.5175519448549,0.311726478256462,382.376439055828));
#37989=CARTESIAN_POINT('Ctrl Pts',(-4.51741634198117,5.54534861180178E-5,
382.387416697508));
#37990=CARTESIAN_POINT('Origin',(0.,0.,387.));
#37991=CARTESIAN_POINT('',(-4.51810647145572,4.12515443024009E-5,383.387416697508));
#37992=CARTESIAN_POINT('',(-4.51737744603353,-1.71510238390164E-5,383.112583302492));
#37993=CARTESIAN_POINT('',(-4.51775,5.53264807684796E-16,387.));
#37994=CARTESIAN_POINT('Ctrl Pts',(-4.51737744603353,-1.71510238390164E-5,
383.112583302492));
#37995=CARTESIAN_POINT('Ctrl Pts',(-4.51732510787532,0.393119355640695,
383.09873663396));
#37996=CARTESIAN_POINT('Ctrl Pts',(-4.46651507043149,0.786269138328428,
383.084889965429));
#37997=CARTESIAN_POINT('Ctrl Pts',(-4.36511527641182,1.16590657912072,383.071043296898));
#37998=CARTESIAN_POINT('Ctrl Pts',(-4.17196291261205,1.8890625754899,383.044667338411));
#37999=CARTESIAN_POINT('Ctrl Pts',(-3.79524613196318,2.56318917681575,383.018291379924));
#38000=CARTESIAN_POINT('Ctrl Pts',(-3.28057275969385,3.10667215778483,382.991915421438));
#38001=CARTESIAN_POINT('Ctrl Pts',(-2.76589938742451,3.65015513875392,382.965539462951));
#38002=CARTESIAN_POINT('Ctrl Pts',(-2.11326942353471,4.06299449936623,382.939163504465));
#38003=CARTESIAN_POINT('Ctrl Pts',(-1.40169456822207,4.29520917593283,382.912787545978));
#38004=CARTESIAN_POINT('Ctrl Pts',(-0.690119712909428,4.52742385249943,
382.886411587491));
#38005=CARTESIAN_POINT('Ctrl Pts',(0.0804000338260355,4.57901384502031,
382.860035629005));
#38006=CARTESIAN_POINT('Ctrl Pts',(0.816580454902776,4.44373332776299,382.833659670518));
#38007=CARTESIAN_POINT('Ctrl Pts',(1.55276087597956,4.30845281050567,382.807283712031));
#38008=CARTESIAN_POINT('Ctrl Pts',(2.2546019713976,3.98630178347012,382.780907753545));
#38009=CARTESIAN_POINT('Ctrl Pts',(2.83713421587333,3.51628198083169,382.754531795058));
#38010=CARTESIAN_POINT('Ctrl Pts',(3.41966646034902,3.04626217819329,382.728155836572));
#38011=CARTESIAN_POINT('Ctrl Pts',(3.88288985388241,2.42837359995203,382.701779878085));
#38012=CARTESIAN_POINT('Ctrl Pts',(4.17072350849794,1.7374219243648,382.675403919598));
#38013=CARTESIAN_POINT('Ctrl Pts',(4.45855716311345,1.04647024877758,382.649027961112));
#38014=CARTESIAN_POINT('Ctrl Pts',(4.57100107881112,0.282455475844346,382.622652002625));
#38015=CARTESIAN_POINT('Ctrl Pts',(4.4944420514052,-0.462125712508384,382.596276044139));
#38016=CARTESIAN_POINT('Ctrl Pts',(4.41788302399928,-1.20670690086118,382.569900085652));
#38017=CARTESIAN_POINT('Ctrl Pts',(4.15232105348975,-1.93185450463351,382.543524127166));
#38018=CARTESIAN_POINT('Ctrl Pts',(3.72990682856509,-2.54977735848138,382.517148168679));
#38019=CARTESIAN_POINT('Ctrl Pts',(3.30749260364046,-3.16770021232922,382.490772210192));
#38020=CARTESIAN_POINT('Ctrl Pts',(2.72822612430073,-3.6783983162526,382.464396251706));
#38021=CARTESIAN_POINT('Ctrl Pts',(2.06223722204694,-4.02004317981846,382.438020293219));
#38022=CARTESIAN_POINT('Ctrl Pts',(1.39624831979316,-4.36168804338432,382.411644334732));
#38023=CARTESIAN_POINT('Ctrl Pts',(0.643536994625335,-4.53427966659265,
382.385268376246));
#38024=CARTESIAN_POINT('Ctrl Pts',(-0.104768541682353,-4.51692296594424,
382.358892417759));
#38025=CARTESIAN_POINT('Ctrl Pts',(-0.853074077990042,-4.49956626529584,
382.332516459273));
#38026=CARTESIAN_POINT('Ctrl Pts',(-1.59697382543758,-4.29226124079071,
382.306140500786));
#38027=CARTESIAN_POINT('Ctrl Pts',(-2.2464063601331,-3.92010560989808,382.2797645423));
#38028=CARTESIAN_POINT('Ctrl Pts',(-2.89583889482865,-3.54794997900543,
382.253388583813));
#38029=CARTESIAN_POINT('Ctrl Pts',(-3.45080421677215,-3.01094374172526,
382.227012625326));
#38030=CARTESIAN_POINT('Ctrl Pts',(-3.84411455331502,-2.37410042512789,
382.20063666684));
#38031=CARTESIAN_POINT('Ctrl Pts',(-4.23742488985787,-1.73725710853056,
382.174260708353));
#38032=CARTESIAN_POINT('Ctrl Pts',(-4.46908024100009,-1.00057671261605,
382.147884749867));
#38033=CARTESIAN_POINT('Ctrl Pts',(-4.51103487766645,-0.253246638827817,
382.12150879138));
#38034=CARTESIAN_POINT('Ctrl Pts',(-4.51576728885779,-0.168949085903131,
382.118533628417));
#38035=CARTESIAN_POINT('Ctrl Pts',(-4.51808605177553,-0.0845160322941951,
382.115558465455));
#38036=CARTESIAN_POINT('Ctrl Pts',(-4.51801683772092,-7.91791388051273E-5,
382.112583302492));
#38037=CARTESIAN_POINT('Ctrl Pts',(-4.51741634198117,5.54534861180178E-5,
382.387416697508));
#38038=CARTESIAN_POINT('Ctrl Pts',(-4.51722613209177,-0.43712489171991,
382.402815014315));
#38039=CARTESIAN_POINT('Ctrl Pts',(-4.45421338524669,-0.874358908440133,
382.418213331122));
#38040=CARTESIAN_POINT('Ctrl Pts',(-4.32915293519383,-1.29306010572185,
382.433611647929));
#38041=CARTESIAN_POINT('Ctrl Pts',(-4.11493541517289,-2.01025832525158,
382.459987606416));
#38042=CARTESIAN_POINT('Ctrl Pts',(-3.71866578800746,-2.67308001421398,
382.486363564902));
#38043=CARTESIAN_POINT('Ctrl Pts',(-3.1883190758562,-3.2012795947618,382.512739523389));
#38044=CARTESIAN_POINT('Ctrl Pts',(-2.65797236370492,-3.72947917530964,
382.539115481875));
#38045=CARTESIAN_POINT('Ctrl Pts',(-1.99354856656775,-4.1230566474429,382.565491440362));
#38046=CARTESIAN_POINT('Ctrl Pts',(-1.27548722410474,-4.33436291909808,
382.591867398849));
#38047=CARTESIAN_POINT('Ctrl Pts',(-0.557425881641732,-4.54566919075325,
382.618243357335));
#38048=CARTESIAN_POINT('Ctrl Pts',(0.214273006147169,-4.57470426193039,
382.644619315822));
#38049=CARTESIAN_POINT('Ctrl Pts',(0.94618246756513,-4.4179529548626,382.670995274309));
#38050=CARTESIAN_POINT('Ctrl Pts',(1.67809192898305,-4.26120164779482,382.697371232795));
#38051=CARTESIAN_POINT('Ctrl Pts',(2.37021196402998,-3.91866396248217,382.723747191282));
#38052=CARTESIAN_POINT('Ctrl Pts',(2.93874994329017,-3.4318097767969,382.750123149768));
#38053=CARTESIAN_POINT('Ctrl Pts',(3.50728792255042,-2.94495559111159,382.776499108255));
#38054=CARTESIAN_POINT('Ctrl Pts',(3.95224384602383,-2.31378490505366,382.802875066742));
#38055=CARTESIAN_POINT('Ctrl Pts',(4.21974840648906,-1.61471141670574,382.829251025228));
#38056=CARTESIAN_POINT('Ctrl Pts',(4.48725296695428,-0.91563792835784,382.855626983715));
#38057=CARTESIAN_POINT('Ctrl Pts',(4.57730616441131,-0.148661637719957,
382.882002942201));
#38058=CARTESIAN_POINT('Ctrl Pts',(4.47900556312629,0.593362232359432,382.908378900688));
#38059=CARTESIAN_POINT('Ctrl Pts',(4.38070496184126,1.33538610243882,382.934754859174));
#38060=CARTESIAN_POINT('Ctrl Pts',(4.09405056181417,2.05245755195971,382.961130817661));
#38061=CARTESIAN_POINT('Ctrl Pts',(3.6537466407651,2.65776316823087,382.987506776148));
#38062=CARTESIAN_POINT('Ctrl Pts',(3.21344271971605,3.26306878450199,383.013882734634));
#38063=CARTESIAN_POINT('Ctrl Pts',(2.61948927764498,3.75660856752342,383.040258693121));
#38064=CARTESIAN_POINT('Ctrl Pts',(1.94379424690704,4.07863132668275,383.066634651607));
#38065=CARTESIAN_POINT('Ctrl Pts',(1.26809921616909,4.4006540858421,383.093010610094));
#38066=CARTESIAN_POINT('Ctrl Pts',(0.510662596764224,4.55115982113938,383.119386568581));
#38067=CARTESIAN_POINT('Ctrl Pts',(-0.236815324157952,4.51192731275126,
383.145762527067));
#38068=CARTESIAN_POINT('Ctrl Pts',(-0.984293245080149,4.47269480436314,
383.172138485554));
#38069=CARTESIAN_POINT('Ctrl Pts',(-1.72181246751965,4.24372405228961,383.19851444404));
#38070=CARTESIAN_POINT('Ctrl Pts',(-2.36008403614551,3.85273577028557,383.224890402527));
#38071=CARTESIAN_POINT('Ctrl Pts',(-2.99835560477138,3.46174748828153,383.251266361013));
#38072=CARTESIAN_POINT('Ctrl Pts',(-3.53737951958361,2.90874167634699,383.2776423195));
#38073=CARTESIAN_POINT('Ctrl Pts',(-3.91189798012409,2.26066887588782,383.304018277987));
#38074=CARTESIAN_POINT('Ctrl Pts',(-4.28641644066456,1.61259607542868,383.330394236473));
#38075=CARTESIAN_POINT('Ctrl Pts',(-4.49642944693329,0.869456286444925,
383.35677019496));
#38076=CARTESIAN_POINT('Ctrl Pts',(-4.51651143527701,0.121218927230134,
383.383146153446));
#38077=CARTESIAN_POINT('Ctrl Pts',(-4.5175952633915,0.0808364375906089,
383.384569668134));
#38078=CARTESIAN_POINT('Ctrl Pts',(-4.51812586459283,0.0404390998600549,
383.385993182821));
#38079=CARTESIAN_POINT('Ctrl Pts',(-4.51810647145572,4.12515443024009E-5,
383.387416697508));
#38080=CARTESIAN_POINT('Origin',(0.,0.,387.));
#38081=CARTESIAN_POINT('',(-4.51758348284472,-0.000105543616906456,384.387416697508));
#38082=CARTESIAN_POINT('',(-4.51791286673421,0.000101789655423226,384.112583302492));
#38083=CARTESIAN_POINT('',(-4.51775,5.53264807684796E-16,387.));
#38084=CARTESIAN_POINT('Ctrl Pts',(-4.51791286673421,0.000101789655423226,
384.112583302492));
#38085=CARTESIAN_POINT('Ctrl Pts',(-4.51803160945122,0.121934720290465,
384.108290760953));
#38086=CARTESIAN_POINT('Ctrl Pts',(-4.51320179205148,0.243758262585871,
384.103998219414));
#38087=CARTESIAN_POINT('Ctrl Pts',(-4.50335615873677,0.365175074681226,
384.099705677874));
#38088=CARTESIAN_POINT('Ctrl Pts',(-4.4428586625063,1.11123303735971,384.073329719388));
#38089=CARTESIAN_POINT('Ctrl Pts',(-4.19298336184317,1.84193444118764,384.046953760901));
#38090=CARTESIAN_POINT('Ctrl Pts',(-3.78398181342604,2.46881574105112,384.020577802415));
#38091=CARTESIAN_POINT('Ctrl Pts',(-3.37498026500888,3.09569704091462,383.994201843928));
#38092=CARTESIAN_POINT('Ctrl Pts',(-2.80685246883769,3.61875823681367,383.967825885442));
#38093=CARTESIAN_POINT('Ctrl Pts',(-2.14837973375322,3.97467408062589,383.941449926955));
#38094=CARTESIAN_POINT('Ctrl Pts',(-1.48990699866878,4.33058992443809,383.915073968468));
#38095=CARTESIAN_POINT('Ctrl Pts',(-0.741089324671071,4.5193604161635,383.888698009982));
#38096=CARTESIAN_POINT('Ctrl Pts',(0.00741646763062709,4.51813175146638,
383.862322051495));
#38097=CARTESIAN_POINT('Ctrl Pts',(0.755922259932325,4.51690308676927,383.835946093009));
#38098=CARTESIAN_POINT('Ctrl Pts',(1.50411617053801,4.32567526564963,383.809570134522));
#38099=CARTESIAN_POINT('Ctrl Pts',(2.16141689576047,3.96759959299347,383.783194176035));
#38100=CARTESIAN_POINT('Ctrl Pts',(2.81871762098293,3.60952392033731,383.756818217549));
#38101=CARTESIAN_POINT('Ctrl Pts',(3.38512516082216,3.08460039614464,383.730442259062));
#38102=CARTESIAN_POINT('Ctrl Pts',(3.79206647204748,2.45637973431923,383.704066300576));
#38103=CARTESIAN_POINT('Ctrl Pts',(4.19900778327279,1.82815907249382,383.677690342089));
#38104=CARTESIAN_POINT('Ctrl Pts',(4.44648286588418,1.09664127303568,383.651314383602));
#38105=CARTESIAN_POINT('Ctrl Pts',(4.50453074947641,0.35038871931369,383.624938425116));
#38106=CARTESIAN_POINT('Ctrl Pts',(4.56257863306864,-0.395863834408303,
383.598562466629));
#38107=CARTESIAN_POINT('Ctrl Pts',(4.4311993176417,-1.15685114239415,383.572186508143));
#38108=CARTESIAN_POINT('Ctrl Pts',(4.12629845211925,-1.84044304764888,383.545810549656));
#38109=CARTESIAN_POINT('Ctrl Pts',(3.8213975865968,-2.52403495290361,383.519434591169));
#38110=CARTESIAN_POINT('Ctrl Pts',(3.34297517097883,-3.13023145542722,383.493058632683));
#38111=CARTESIAN_POINT('Ctrl Pts',(2.74895218738718,-3.58564239698551,383.466682674196));
#38112=CARTESIAN_POINT('Ctrl Pts',(2.15492920379552,-4.04105333854382,383.44030671571));
#38113=CARTESIAN_POINT('Ctrl Pts',(1.44530565223012,-4.34567871913682,383.413930757223));
#38114=CARTESIAN_POINT('Ctrl Pts',(0.705993253592304,-4.46263857526945,
383.387554798737));
#38115=CARTESIAN_POINT('Ctrl Pts',(-0.0333191450455116,-4.57959843140208,
383.36117884025));
#38116=CARTESIAN_POINT('Ctrl Pts',(-0.802320390755788,-4.50889276307437,
383.334802881763));
#38117=CARTESIAN_POINT('Ctrl Pts',(-1.50791010623509,-4.25908166617111,
383.308426923277));
#38118=CARTESIAN_POINT('Ctrl Pts',(-2.21349982171436,-4.00927056926786,
383.28205096479));
#38119=CARTESIAN_POINT('Ctrl Pts',(-2.8556780069626,-3.58035404378911,383.255675006304));
#38120=CARTESIAN_POINT('Ctrl Pts',(-3.35669832323709,-3.02425956134359,
383.229299047817));
#38121=CARTESIAN_POINT('Ctrl Pts',(-3.85771863951158,-2.46816507889806,
383.20292308933));
#38122=CARTESIAN_POINT('Ctrl Pts',(-4.21758108681228,-1.78489263948572,
383.176547130844));
#38123=CARTESIAN_POINT('Ctrl Pts',(-4.39271833698727,-1.05716372407332,
383.150171172357));
#38124=CARTESIAN_POINT('Ctrl Pts',(-4.4759132430793,-0.711472908911519,
383.137641882402));
#38125=CARTESIAN_POINT('Ctrl Pts',(-4.51742480471468,-0.355750464977554,
383.125112592447));
#38126=CARTESIAN_POINT('Ctrl Pts',(-4.51737744603353,-1.71510238390164E-5,
383.112583302492));
#38127=CARTESIAN_POINT('Ctrl Pts',(-4.51810647145572,4.12515443024009E-5,
383.387416697508));
#38128=CARTESIAN_POINT('Ctrl Pts',(-4.51776653385746,-0.70808283654263,
383.412369141307));
#38129=CARTESIAN_POINT('Ctrl Pts',(-4.34843679840707,-1.41636380567975,
383.437321585107));
#38130=CARTESIAN_POINT('Ctrl Pts',(-4.0275273935072,-2.04758215167448,383.462274028906));
#38131=CARTESIAN_POINT('Ctrl Pts',(-3.68831039297495,-2.71481094191849,
383.488649987393));
#38132=CARTESIAN_POINT('Ctrl Pts',(-3.17972542149173,-3.29593359296068,
383.515025945879));
#38133=CARTESIAN_POINT('Ctrl Pts',(-2.56334513970026,-3.72059555287616,
383.541401904366));
#38134=CARTESIAN_POINT('Ctrl Pts',(-1.94696485790879,-4.14525751279165,
383.567777862853));
#38135=CARTESIAN_POINT('Ctrl Pts',(-1.22278926580908,-4.41345878158044,
383.594153821339));
#38136=CARTESIAN_POINT('Ctrl Pts',(-0.478491850582746,-4.49272913964694,
383.620529779826));
#38137=CARTESIAN_POINT('Ctrl Pts',(0.265805564643564,-4.57199949771343,
383.646905738312));
#38138=CARTESIAN_POINT('Ctrl Pts',(1.0302248029965,-4.46233894505765,383.673281696799));
#38139=CARTESIAN_POINT('Ctrl Pts',(1.72222021529061,-4.17702371352512,383.699657655286));
#38140=CARTESIAN_POINT('Ctrl Pts',(2.41421562758474,-3.89170848199258,383.726033613772));
#38141=CARTESIAN_POINT('Ctrl Pts',(3.03378721382,-3.43073857158334,383.752409572259));
#38142=CARTESIAN_POINT('Ctrl Pts',(3.50592553965972,-2.84992204870037,383.778785530746));
#38143=CARTESIAN_POINT('Ctrl Pts',(3.97806386549944,-2.2691055258174,383.805161489232));
#38144=CARTESIAN_POINT('Ctrl Pts',(4.30276893094358,-1.56844239046068,383.831537447719));
#38145=CARTESIAN_POINT('Ctrl Pts',(4.44072979303352,-0.832759556277373,
383.857913406205));
#38146=CARTESIAN_POINT('Ctrl Pts',(4.57869065512346,-0.0970767220940631,
383.884289364692));
#38147=CARTESIAN_POINT('Ctrl Pts',(4.52990731385923,0.673625810915847,383.910665323178));
#38148=CARTESIAN_POINT('Ctrl Pts',(4.30028580320783,1.38604169635549,383.937041281665));
#38149=CARTESIAN_POINT('Ctrl Pts',(4.07066429255644,2.0984575817951,383.963417240152));
#38150=CARTESIAN_POINT('Ctrl Pts',(3.66020461251785,2.75258681966445,383.989793198638));
#38151=CARTESIAN_POINT('Ctrl Pts',(3.11859972691059,3.26923619774099,384.016169157125));
#38152=CARTESIAN_POINT('Ctrl Pts',(2.57699484130331,3.78588557581757,384.042545115611));
#38153=CARTESIAN_POINT('Ctrl Pts',(1.90424475012738,4.16505509410136,384.068921074098));
#38154=CARTESIAN_POINT('Ctrl Pts',(1.18179702927259,4.36083998272228,384.095297032584));
#38155=CARTESIAN_POINT('Ctrl Pts',(0.459349308417798,4.55662487134321,384.121672991071));
#38156=CARTESIAN_POINT('Ctrl Pts',(-0.312796042115809,4.56902513030122,
384.148048949558));
#38157=CARTESIAN_POINT('Ctrl Pts',(-1.04115799889843,4.39653950222634,384.174424908044));
#38158=CARTESIAN_POINT('Ctrl Pts',(-1.76951995568104,4.22405387415146,384.200800866531));
#38159=CARTESIAN_POINT('Ctrl Pts',(-2.45409851871268,3.86668235904368,384.227176825017));
#38160=CARTESIAN_POINT('Ctrl Pts',(-3.0120140790621,3.36769071632751,384.253552783504));
#38161=CARTESIAN_POINT('Ctrl Pts',(-3.56992963941149,2.86869907361137,384.279928741991));
#38162=CARTESIAN_POINT('Ctrl Pts',(-4.00118219707867,2.22808730328684,384.306304700477));
#38163=CARTESIAN_POINT('Ctrl Pts',(-4.25356146494663,1.52341210354517,384.332680658964));
#38164=CARTESIAN_POINT('Ctrl Pts',(-4.42814268873775,1.0359589946372,384.350926005145));
#38165=CARTESIAN_POINT('Ctrl Pts',(-4.51713190568983,0.51785112729682,384.369171351326));
#38166=CARTESIAN_POINT('Ctrl Pts',(-4.51758348284472,-0.000105543616906456,
384.387416697508));
#38167=CARTESIAN_POINT('Origin',(0.,0.,387.));
#38168=CARTESIAN_POINT('',(-4.51754236316255,9.86160820556914E-5,385.387416697508));
#38169=CARTESIAN_POINT('',(-4.51782825948384,-0.000111641905798056,385.112583302492));
#38170=CARTESIAN_POINT('',(-4.51775,5.53264807684796E-16,387.));
#38171=CARTESIAN_POINT('Ctrl Pts',(-4.51782825948384,-0.000111641905798056,
385.112583302492));
#38172=CARTESIAN_POINT('Ctrl Pts',(-4.51721726779753,0.599198793910267,
385.091468929459));
#38173=CARTESIAN_POINT('Ctrl Pts',(-4.39722715972494,1.19874658011254,385.070354556425));
#38174=CARTESIAN_POINT('Ctrl Pts',(-4.16499712691276,1.75110492558535,385.049240183392));
#38175=CARTESIAN_POINT('Ctrl Pts',(-3.87489664914265,2.44110792813221,385.022864224905));
#38176=CARTESIAN_POINT('Ctrl Pts',(-3.40964724164981,3.05747242764947,384.996488266419));
#38177=CARTESIAN_POINT('Ctrl Pts',(-2.82557507506063,3.52557726093145,384.970112307932));
#38178=CARTESIAN_POINT('Ctrl Pts',(-2.24150290847142,3.99368209421345,384.943736349446));
#38179=CARTESIAN_POINT('Ctrl Pts',(-1.53860798278584,4.31352726126017,384.917360390959));
#38180=CARTESIAN_POINT('Ctrl Pts',(-0.801987406950171,4.44639019055842,
384.890984432472));
#38181=CARTESIAN_POINT('Ctrl Pts',(-0.065366831114539,4.57925311985666,
384.864608473986));
#38182=CARTESIAN_POINT('Ctrl Pts',(0.7049793948712,4.52513381140646,384.838232515499));
#38183=CARTESIAN_POINT('Ctrl Pts',(1.41578806149518,4.29058430665667,384.811856557012));
#38184=CARTESIAN_POINT('Ctrl Pts',(2.12659672811916,4.05603480190689,384.785480598526));
#38185=CARTESIAN_POINT('Ctrl Pts',(2.77786783538139,3.64105510085751,384.759104640039));
#38186=CARTESIAN_POINT('Ctrl Pts',(3.29075419525559,3.09588539096791,384.732728681553));
#38187=CARTESIAN_POINT('Ctrl Pts',(3.8036405551298,2.55071568107831,384.706352723066));
#38188=CARTESIAN_POINT('Ctrl Pts',(4.178142167616,1.87535596234848,384.67997676458));
#38189=CARTESIAN_POINT('Ctrl Pts',(4.36891939039539,1.15156974944116,384.653600806093));
#38190=CARTESIAN_POINT('Ctrl Pts',(4.55969661317478,0.427783536533828,384.627224847606));
#38191=CARTESIAN_POINT('Ctrl Pts',(4.56674944624736,-0.344429170550942,
384.60084888912));
#38192=CARTESIAN_POINT('Ctrl Pts',(4.38922402699095,-1.07157919375385,384.574472930633));
#38193=CARTESIAN_POINT('Ctrl Pts',(4.21169860773453,-1.79872921695679,384.548096972147));
#38194=CARTESIAN_POINT('Ctrl Pts',(3.84959493614911,-2.48081655627781,384.52172101366));
#38195=CARTESIAN_POINT('Ctrl Pts',(3.34675167782285,-3.03526320680608,384.495345055174));
#38196=CARTESIAN_POINT('Ctrl Pts',(2.84390841949662,-3.58970985733432,384.468969096687));
#38197=CARTESIAN_POINT('Ctrl Pts',(2.20032557442955,-4.01651581906983,384.4425931382));
#38198=CARTESIAN_POINT('Ctrl Pts',(1.49391953877316,-4.26400913921072,384.416217179714));
#38199=CARTESIAN_POINT('Ctrl Pts',(0.787513503116781,-4.51150245935161,
384.389841221227));
#38200=CARTESIAN_POINT('Ctrl Pts',(0.0182842768710745,-4.57968313789789,
384.363465262741));
#38201=CARTESIAN_POINT('Ctrl Pts',(-0.720640161828923,-4.46029677092904,
384.337089304254));
#38202=CARTESIAN_POINT('Ctrl Pts',(-1.45956460052894,-4.34091040396018,
384.310713345767));
#38203=CARTESIAN_POINT('Ctrl Pts',(-2.16818425168326,-4.03395699147619,
384.284337387281));
#38204=CARTESIAN_POINT('Ctrl Pts',(-2.76070893321464,-3.57659834391139,
384.257961428794));
#38205=CARTESIAN_POINT('Ctrl Pts',(-3.35323361474601,-3.11923969634659,
384.231585470308));
#38206=CARTESIAN_POINT('Ctrl Pts',(-3.82966332665445,-2.51147581370097,
384.205209511821));
#38207=CARTESIAN_POINT('Ctrl Pts',(-4.13231833670975,-1.82688661161363,
384.178833553334));
#38208=CARTESIAN_POINT('Ctrl Pts',(-4.38571791578798,-1.25371052039765,
384.156750136387));
#38209=CARTESIAN_POINT('Ctrl Pts',(-4.51730198273802,-0.626680125117799,
384.134666719439));
#38210=CARTESIAN_POINT('Ctrl Pts',(-4.51791286673421,0.000101789655423226,
384.112583302492));
#38211=CARTESIAN_POINT('Ctrl Pts',(-4.51758348284472,-0.000105543616906456,
384.387416697508));
#38212=CARTESIAN_POINT('Ctrl Pts',(-4.51778471765472,-0.230920834279876,
384.395547309813));
#38213=CARTESIAN_POINT('Ctrl Pts',(-4.50040387332536,-0.461706099887457,
384.403677922118));
#38214=CARTESIAN_POINT('Ctrl Pts',(-4.46518027924831,-0.689735200724739,
384.411808534423));
#38215=CARTESIAN_POINT('Ctrl Pts',(-4.35091384761331,-1.42946867609407,
384.43818449291));
#38216=CARTESIAN_POINT('Ctrl Pts',(-4.04887500627456,-2.14019699767394,
384.464560451397));
#38217=CARTESIAN_POINT('Ctrl Pts',(-3.59563057517656,-2.73587469379764,
384.490936409884));
#38218=CARTESIAN_POINT('Ctrl Pts',(-3.14238614407856,-3.33155238992132,
384.51731236837));
#38219=CARTESIAN_POINT('Ctrl Pts',(-2.53793612322135,-3.81217946058886,
384.543688326857));
#38220=CARTESIAN_POINT('Ctrl Pts',(-1.85545923021652,-4.11956801355568,
384.570064285343));
#38221=CARTESIAN_POINT('Ctrl Pts',(-1.17298233721168,-4.42695656652252,
384.59644024383));
#38222=CARTESIAN_POINT('Ctrl Pts',(-0.412478572059261,-4.56110660178858,
384.622816202316));
#38223=CARTESIAN_POINT('Ctrl Pts',(0.333980449139521,-4.50577702875979,
384.649192160803));
#38224=CARTESIAN_POINT('Ctrl Pts',(1.08043947033828,-4.450447455731,384.67556811929));
#38225=CARTESIAN_POINT('Ctrl Pts',(1.81285374758341,-4.20563827440736,384.701944077776));
#38226=CARTESIAN_POINT('Ctrl Pts',(2.44255236397545,-3.80098770355085,384.728320036263));
#38227=CARTESIAN_POINT('Ctrl Pts',(3.0722509803675,-3.39633713269433,384.754695994749));
#38228=CARTESIAN_POINT('Ctrl Pts',(3.59923393590646,-2.83184517230493,384.781071953236));
#38229=CARTESIAN_POINT('Ctrl Pts',(3.95970118830781,-2.17585295289468,384.807447911723));
#38230=CARTESIAN_POINT('Ctrl Pts',(4.32016844070917,-1.51986073348444,384.833823870209));
#38231=CARTESIAN_POINT('Ctrl Pts',(4.51411998997293,-0.772368255053362,
384.860199828696));
#38232=CARTESIAN_POINT('Ctrl Pts',(4.51807477866807,-0.023871901270034,
384.886575787182));
#38233=CARTESIAN_POINT('Ctrl Pts',(4.52202956736322,0.724624452513337,384.912951745669));
#38234=CARTESIAN_POINT('Ctrl Pts',(4.33598759548973,1.47412468164896,384.939327704155));
#38235=CARTESIAN_POINT('Ctrl Pts',(3.98247233472248,2.13388933088782,384.965703662642));
#38236=CARTESIAN_POINT('Ctrl Pts',(3.62895707395525,2.79365398012665,384.992079621129));
#38237=CARTESIAN_POINT('Ctrl Pts',(3.10796852429429,3.36368304946875,385.018455579615));
#38238=CARTESIAN_POINT('Ctrl Pts',(2.48258100559898,3.77496504936747,385.044831538102));
#38239=CARTESIAN_POINT('Ctrl Pts',(1.8571934869037,4.18624704926618,385.071207496588));
#38240=CARTESIAN_POINT('Ctrl Pts',(1.12740699917409,4.43878197972154,385.097583455075));
#38241=CARTESIAN_POINT('Ctrl Pts',(0.38157432172954,4.50199629168033,385.123959413562));
#38242=CARTESIAN_POINT('Ctrl Pts',(-0.364258355715052,4.56521060363914,
385.150335372048));
#38243=CARTESIAN_POINT('Ctrl Pts',(-1.12613722287458,4.43910429710136,385.176711330535));
#38244=CARTESIAN_POINT('Ctrl Pts',(-1.81182418470336,4.13894463565663,385.203087289021));
#38245=CARTESIAN_POINT('Ctrl Pts',(-2.49751114653216,3.8387849742119,385.229463247508));
#38246=CARTESIAN_POINT('Ctrl Pts',(-3.1070062030302,3.36457195786021,385.255839205995));
#38247=CARTESIAN_POINT('Ctrl Pts',(-3.56651985120111,2.7737169510055,385.282215164481));
#38248=CARTESIAN_POINT('Ctrl Pts',(-4.02603349937199,2.18286194415082,385.308591122968));
#38249=CARTESIAN_POINT('Ctrl Pts',(-4.33556573921576,1.47536494679312,385.334967081454));
#38250=CARTESIAN_POINT('Ctrl Pts',(-4.45764255040047,0.736880225115328,
385.361343039941));
#38251=CARTESIAN_POINT('Ctrl Pts',(-4.49786843733614,0.493539965571841,
385.37003425913));
#38252=CARTESIAN_POINT('Ctrl Pts',(-4.51774064501623,0.246835097138747,
385.378725478319));
#38253=CARTESIAN_POINT('Ctrl Pts',(-4.51754236316255,9.86160820556914E-5,
385.387416697508));
#38254=CARTESIAN_POINT('Origin',(0.,0.,387.));
#38255=CARTESIAN_POINT('',(-4.51812581071634,-2.54303748789628E-5,386.387416697508));
#38256=CARTESIAN_POINT('',(-4.51739693228094,4.16105383547416E-5,386.112583302492));
#38257=CARTESIAN_POINT('',(-4.51775,5.53264807684796E-16,387.));
#38258=CARTESIAN_POINT('Ctrl Pts',(-4.51739693228094,4.16105383547416E-5,
386.112583302492));
#38259=CARTESIAN_POINT('Ctrl Pts',(-4.51750350848484,0.328257645647765,
386.101023056451));
#38260=CARTESIAN_POINT('Ctrl Pts',(-4.48221658085224,0.656451107309221,
386.08946281041));
#38261=CARTESIAN_POINT('Ctrl Pts',(-4.41129467440341,0.976754228647579,
386.077902564369));
#38262=CARTESIAN_POINT('Ctrl Pts',(-4.24947863228365,1.70756063203963,386.051526605882));
#38263=CARTESIAN_POINT('Ctrl Pts',(-3.90215620987833,2.39729198722953,386.025150647396));
#38264=CARTESIAN_POINT('Ctrl Pts',(-3.41137655698045,2.96244485418463,385.998774688909));
#38265=CARTESIAN_POINT('Ctrl Pts',(-2.92059690408257,3.52759772113973,385.972398730423));
#38266=CARTESIAN_POINT('Ctrl Pts',(-2.28636002069214,3.96817209986003,385.946022771936));
#38267=CARTESIAN_POINT('Ctrl Pts',(-1.58545081902196,4.23082914191337,385.91964681345));
#38268=CARTESIAN_POINT('Ctrl Pts',(-0.884541617351764,4.49348618396671,
385.893270854963));
#38269=CARTESIAN_POINT('Ctrl Pts',(-0.116960097401826,4.57822588935307,
385.866894896476));
#38270=CARTESIAN_POINT('Ctrl Pts',(0.624365244915622,4.47478910883432,385.84051893799));
#38271=CARTESIAN_POINT('Ctrl Pts',(1.36569058723307,4.37135232831557,385.814142979503));
#38272=CARTESIAN_POINT('Ctrl Pts',(2.08075975191802,4.07973906189171,385.787767021017));
#38273=CARTESIAN_POINT('Ctrl Pts',(2.68300173612543,3.63525394044883,385.76139106253));
#38274=CARTESIAN_POINT('Ctrl Pts',(3.28524372033282,3.19076881900596,385.735015104043));
#38275=CARTESIAN_POINT('Ctrl Pts',(3.77465852406267,2.5934118425441,385.708639145557));
#38276=CARTESIAN_POINT('Ctrl Pts',(4.09199435398004,1.91550299780405,385.68226318707));
#38277=CARTESIAN_POINT('Ctrl Pts',(4.4093301838974,1.23759415306402,385.655887228584));
#38278=CARTESIAN_POINT('Ctrl Pts',(4.55458704000229,0.479133440045757,385.629511270097));
#38279=CARTESIAN_POINT('Ctrl Pts',(4.51017916650468,-0.268054870554405,
385.60313531161));
#38280=CARTESIAN_POINT('Ctrl Pts',(4.46577129300707,-1.01524318115463,385.576759353124));
#38281=CARTESIAN_POINT('Ctrl Pts',(4.23169868990694,-1.7511590893368,385.550383394637));
#38282=CARTESIAN_POINT('Ctrl Pts',(3.83629973479027,-2.38670774759897,385.524007436151));
#38283=CARTESIAN_POINT('Ctrl Pts',(3.44090077967361,-3.0222564058611,385.497631477664));
#38284=CARTESIAN_POINT('Ctrl Pts',(2.88417547254044,-3.55743781420323,385.471255519177));
#38285=CARTESIAN_POINT('Ctrl Pts',(2.23352466148768,-3.92745937141648,385.444879560691));
#38286=CARTESIAN_POINT('Ctrl Pts',(1.58287385043492,-4.29748092862973,385.418503602204));
#38287=CARTESIAN_POINT('Ctrl Pts',(0.838297535462584,-4.5023426347141,385.392127643717));
#38288=CARTESIAN_POINT('Ctrl Pts',(0.0899390502021953,-4.5172425764895,
385.365751685231));
#38289=CARTESIAN_POINT('Ctrl Pts',(-0.658419435058194,-4.53214251826491,
385.339375726744));
#38290=CARTESIAN_POINT('Ctrl Pts',(-1.41056009060662,-4.35708069573135,
385.312999768258));
#38291=CARTESIAN_POINT('Ctrl Pts',(-2.07542379370768,-4.01325125105728,
385.286623809771));
#38292=CARTESIAN_POINT('Ctrl Pts',(-2.74028749680876,-3.6694218063832,385.260247851285));
#38293=CARTESIAN_POINT('Ctrl Pts',(-3.31787424746246,-3.15682473956861,
385.233871892798));
#38294=CARTESIAN_POINT('Ctrl Pts',(-3.73825757323288,-2.53751844205472,
385.207495934311));
#38295=CARTESIAN_POINT('Ctrl Pts',(-4.15864089900331,-1.91821214454083,
385.181119975825));
#38296=CARTESIAN_POINT('Ctrl Pts',(-4.42182079989046,-1.19219661632765,
385.154744017338));
#38297=CARTESIAN_POINT('Ctrl Pts',(-4.49593497631034,-0.44736809943281,
385.128368058852));
#38298=CARTESIAN_POINT('Ctrl Pts',(-4.51071957921785,-0.298786621658729,
385.123106473398));
#38299=CARTESIAN_POINT('Ctrl Pts',(-4.51798051524647,-0.149456501261902,
385.117844887945));
#38300=CARTESIAN_POINT('Ctrl Pts',(-4.51782825948384,-0.000111641905798056,
385.112583302492));
#38301=CARTESIAN_POINT('Ctrl Pts',(-4.51754236316255,9.86160820556914E-5,
385.387416697508));
#38302=CARTESIAN_POINT('Ctrl Pts',(-4.51713890274882,-0.501956417601758,
385.405101436806));
#38303=CARTESIAN_POINT('Ctrl Pts',(-4.43363680853372,-1.00414233826904,
385.422786176103));
#38304=CARTESIAN_POINT('Ctrl Pts',(-4.26942186585053,-1.47837968895145,
385.440470915401));
#38305=CARTESIAN_POINT('Ctrl Pts',(-4.02450298759024,-2.18568243534247,
385.466846873887));
#38306=CARTESIAN_POINT('Ctrl Pts',(-3.60004384854402,-2.83081548212662,
385.493222832374));
#38307=CARTESIAN_POINT('Ctrl Pts',(-3.04743227963612,-3.33567475547881,
385.519598790861));
#38308=CARTESIAN_POINT('Ctrl Pts',(-2.49482071072822,-3.84053402883101,
385.545974749347));
#38309=CARTESIAN_POINT('Ctrl Pts',(-1.81405671195863,-4.20511952875126,
385.572350707834));
#38310=CARTESIAN_POINT('Ctrl Pts',(-1.0875580758779,-4.38529212309734,385.59872666632));
#38311=CARTESIAN_POINT('Ctrl Pts',(-0.361059439797152,-4.56546471744342,
385.625102624807));
#38312=CARTESIAN_POINT('Ctrl Pts',(0.411173833594756,-4.56122440621533,
385.651478583294));
#38313=CARTESIAN_POINT('Ctrl Pts',(1.13565007634523,-4.37308454953753,385.67785454178));
#38314=CARTESIAN_POINT('Ctrl Pts',(1.86012631909569,-4.18494469285974,385.704230500267));
#38315=CARTESIAN_POINT('Ctrl Pts',(2.53684553120472,-3.81290529073225,385.730606458753));
#38316=CARTESIAN_POINT('Ctrl Pts',(3.08387960874885,-3.30200789400175,385.75698241724));
#38317=CARTESIAN_POINT('Ctrl Pts',(3.63091368629297,-2.79111049727125,385.783358375726));
#38318=CARTESIAN_POINT('Ctrl Pts',(4.04826262927219,-2.14135510593772,385.809734334213));
#38319=CARTESIAN_POINT('Ctrl Pts',(4.28539941412795,-1.43140540543153,385.8361102927));
#38320=CARTESIAN_POINT('Ctrl Pts',(4.52253619898372,-0.721455704925321,
385.862486251186));
#38321=CARTESIAN_POINT('Ctrl Pts',(4.57946082571602,0.048688304753508,385.888862209673));
#38322=CARTESIAN_POINT('Ctrl Pts',(4.44928162248921,0.785787895736858,385.915238168159));
#38323=CARTESIAN_POINT('Ctrl Pts',(4.31910241926241,1.52288748672023,385.941614126646));
#38324=CARTESIAN_POINT('Ctrl Pts',(4.00181938607647,2.22694265900807,385.967990085133));
#38325=CARTESIAN_POINT('Ctrl Pts',(3.53584490557238,2.81271583652609,385.994366043619));
#38326=CARTESIAN_POINT('Ctrl Pts',(3.06987042506831,3.39848901404408,386.020742002106));
#38327=CARTESIAN_POINT('Ctrl Pts',(2.45520449724608,3.86598019679227,386.047117960592));
#38328=CARTESIAN_POINT('Ctrl Pts',(1.76626264498691,4.1585918100038,386.073493919079));
#38329=CARTESIAN_POINT('Ctrl Pts',(1.07732079272774,4.45120342321533,386.099869877566));
#38330=CARTESIAN_POINT('Ctrl Pts',(0.3141030160316,4.56893546689021,386.126245836052));
#38331=CARTESIAN_POINT('Ctrl Pts',(-0.43099049281119,4.49753452109188,386.152621794539));
#38332=CARTESIAN_POINT('Ctrl Pts',(-1.17608400165398,4.42613357529356,386.178997753025));
#38333=CARTESIAN_POINT('Ctrl Pts',(-1.90305324264344,4.16559964002203,386.205373711512));
#38334=CARTESIAN_POINT('Ctrl Pts',(-2.52388651098497,3.74747467676233,386.231749669998));
#38335=CARTESIAN_POINT('Ctrl Pts',(-3.14471977932654,3.3293497135026,386.258125628485));
#38336=CARTESIAN_POINT('Ctrl Pts',(-3.65941707502018,2.75363372225468,386.284501586972));
#38337=CARTESIAN_POINT('Ctrl Pts',(-4.00566573902476,2.09002668894682,386.310877545458));
#38338=CARTESIAN_POINT('Ctrl Pts',(-4.34058663747219,1.44813002069409,386.336390596142));
#38339=CARTESIAN_POINT('Ctrl Pts',(-4.51790043884109,0.723999072118772,
386.361903646825));
#38340=CARTESIAN_POINT('Ctrl Pts',(-4.51812581071634,-2.54303748789628E-5,
386.387416697508));
#38341=CARTESIAN_POINT('Origin',(0.,0.,387.));
#38342=CARTESIAN_POINT('',(-4.51744020728156,-6.7888199640348E-5,387.387416697508));
#38343=CARTESIAN_POINT('',(-4.51807831563064,5.66723631286815E-5,387.112583302492));
#38344=CARTESIAN_POINT('',(-4.51775,5.53264807684796E-16,387.));
#38345=CARTESIAN_POINT('Ctrl Pts',(-4.51807831563064,5.66723631286815E-5,
387.112583302492));
#38346=CARTESIAN_POINT('Ctrl Pts',(-4.51811411951228,0.0569892498064094,
387.110577183443));
#38347=CARTESIAN_POINT('Ctrl Pts',(-4.51706018525489,0.113920500037806,
387.108571064395));
#38348=CARTESIAN_POINT('Ctrl Pts',(-4.51490790649659,0.170810197164546,
387.106564945346));
#38349=CARTESIAN_POINT('Ctrl Pts',(-4.4866102761939,0.918781904413813,387.08018898686));
#38350=CARTESIAN_POINT('Ctrl Pts',(-4.26844906050963,1.65957059993282,387.053813028373));
#38351=CARTESIAN_POINT('Ctrl Pts',(-3.88683629922459,2.30349150435396,387.027437069886));
#38352=CARTESIAN_POINT('Ctrl Pts',(-3.50522353793953,2.94741240877514,387.0010611114));
#38353=CARTESIAN_POINT('Ctrl Pts',(-2.96015923105368,3.49446552209844,386.974685152913));
#38354=CARTESIAN_POINT('Ctrl Pts',(-2.31763246884327,3.87842097598549,386.948309194426));
#38355=CARTESIAN_POINT('Ctrl Pts',(-1.67510570663291,4.26237642987252,386.92193323594));
#38356=CARTESIAN_POINT('Ctrl Pts',(-0.935116489098005,4.48323422432332,
386.895557277453));
#38357=CARTESIAN_POINT('Ctrl Pts',(-0.187252805513337,4.51425585389532,
386.869181318967));
#38358=CARTESIAN_POINT('Ctrl Pts',(0.560610878071331,4.54527748346732,386.84280536048));
#38359=CARTESIAN_POINT('Ctrl Pts',(1.31634902770576,4.38646294816051,386.816429401993));
#38360=CARTESIAN_POINT('Ctrl Pts',(1.98846698422516,4.05703938608529,386.790053443507));
#38361=CARTESIAN_POINT('Ctrl Pts',(2.66058494074455,3.72761582401007,386.76367748502));
#38362=CARTESIAN_POINT('Ctrl Pts',(3.2490827041489,3.22758323516643,386.737301526534));
#38363=CARTESIAN_POINT('Ctrl Pts',(3.68271284262869,2.6174788721857,386.710925568047));
#38364=CARTESIAN_POINT('Ctrl Pts',(4.1163429811085,2.00737450920494,386.684549609561));
#38365=CARTESIAN_POINT('Ctrl Pts',(4.39510549466373,1.28719837208709,386.658173651074));
#38366=CARTESIAN_POINT('Ctrl Pts',(4.48525154955086,0.544139747539571,386.631797692587));
#38367=CARTESIAN_POINT('Ctrl Pts',(4.57539760443799,-0.198918877007948,
386.605421734101));
#38368=CARTESIAN_POINT('Ctrl Pts',(4.47692720065701,-0.96485998898513,386.579045775614));
#38369=CARTESIAN_POINT('Ctrl Pts',(4.20176181661432,-1.66095369111926,386.552669817128));
#38370=CARTESIAN_POINT('Ctrl Pts',(3.92659643257165,-2.35704739325338,386.526293858641));
#38371=CARTESIAN_POINT('Ctrl Pts',(3.47473606826728,-2.98329368554445,386.499917900154));
#38372=CARTESIAN_POINT('Ctrl Pts',(2.90088592819845,-3.46387504959129,386.473541941668));
#38373=CARTESIAN_POINT('Ctrl Pts',(2.32703578812962,-3.94445641363812,386.447165983181));
#38374=CARTESIAN_POINT('Ctrl Pts',(1.63119587229633,-4.27937284944072,386.420790024695));
#38375=CARTESIAN_POINT('Ctrl Pts',(0.897609163487301,-4.4280771580026,386.394414066208));
#38376=CARTESIAN_POINT('Ctrl Pts',(0.164022454678273,-4.57678146656449,
386.368038107722));
#38377=CARTESIAN_POINT('Ctrl Pts',(-0.607311047106494,-4.53927364788568,
386.341662149235));
#38378=CARTESIAN_POINT('Ctrl Pts',(-1.32300860621665,-4.3200946465879,386.315286190748));
#38379=CARTESIAN_POINT('Ctrl Pts',(-2.03870616532682,-4.10091564529013,
386.288910232262));
#38380=CARTESIAN_POINT('Ctrl Pts',(-2.69876778176237,-3.7000654613734,386.262534273775));
#38381=CARTESIAN_POINT('Ctrl Pts',(-3.22328203031241,-3.16607366949443,
386.236158315289));
#38382=CARTESIAN_POINT('Ctrl Pts',(-3.74779627886247,-2.63208187761544,
386.209782356802));
#38383=CARTESIAN_POINT('Ctrl Pts',(-4.136763159527,-1.9649484777742,386.183406398315));
#38384=CARTESIAN_POINT('Ctrl Pts',(-4.34309176894218,-1.24544105205646,
386.157030439829));
#38385=CARTESIAN_POINT('Ctrl Pts',(-4.45898918165419,-0.84128454994014,
386.142214727383));
#38386=CARTESIAN_POINT('Ctrl Pts',(-4.51726034328579,-0.420602931019958,
386.127399014937));
#38387=CARTESIAN_POINT('Ctrl Pts',(-4.51739693228094,4.16105383547416E-5,
386.112583302492));
#38388=CARTESIAN_POINT('Ctrl Pts',(-4.51812581071634,-2.54303748789628E-5,
386.387416697508));
#38389=CARTESIAN_POINT('Ctrl Pts',(-4.51813343329163,-0.024513540432781,
386.388279605311));
#38390=CARTESIAN_POINT('Ctrl Pts',(-4.51793847697299,-0.049001528722538,
386.389142513115));
#38391=CARTESIAN_POINT('Ctrl Pts',(-4.51754018801501,-0.0734862094280138,
386.390005420918));
#38392=CARTESIAN_POINT('Ctrl Pts',(-4.50536594068517,-0.821893999127264,
386.416381379405));
#38393=CARTESIAN_POINT('Ctrl Pts',(-4.30321741370996,-1.56721150315799,
386.442757337891));
#38394=CARTESIAN_POINT('Ctrl Pts',(-3.9355680448604,-2.21920565463873,386.469133296378));
#38395=CARTESIAN_POINT('Ctrl Pts',(-3.56791867601083,-2.87119980611948,
386.495509254864));
#38396=CARTESIAN_POINT('Ctrl Pts',(-3.03476846528691,-3.42987060505022,
386.521885213351));
#38397=CARTESIAN_POINT('Ctrl Pts',(-2.40066410367865,-3.8275816692287,386.548261171838));
#38398=CARTESIAN_POINT('Ctrl Pts',(-1.76655974207041,-4.22529273340718,
386.574637130324));
#38399=CARTESIAN_POINT('Ctrl Pts',(-1.0315012295778,-4.46204406283341,386.601013088811));
#38400=CARTESIAN_POINT('Ctrl Pts',(-0.28447961170951,-4.50917297559413,
386.627389047297));
#38401=CARTESIAN_POINT('Ctrl Pts',(0.4625420061588,-4.55630188835485,386.653765005784));
#38402=CARTESIAN_POINT('Ctrl Pts',(1.22152672940277,-4.4138083844501,386.68014096427));
#38403=CARTESIAN_POINT('Ctrl Pts',(1.90058684718235,-4.09894366997453,386.706516922757));
#38404=CARTESIAN_POINT('Ctrl Pts',(2.57964696496189,-3.78407895549898,386.732892881244));
#38405=CARTESIAN_POINT('Ctrl Pts',(3.17878247727702,-3.29684303045261,386.75926883973));
#38406=CARTESIAN_POINT('Ctrl Pts',(3.62545807607245,-2.69622389870498,386.785644798217));
#38407=CARTESIAN_POINT('Ctrl Pts',(4.07213367486792,-2.0956047669573,386.812020756704));
#38408=CARTESIAN_POINT('Ctrl Pts',(4.3663493601437,-1.38160242850832,386.83839671519));
#38409=CARTESIAN_POINT('Ctrl Pts',(4.47248543497401,-0.64065872916252,386.864772673677));
#38410=CARTESIAN_POINT('Ctrl Pts',(4.57862150980431,0.10028497018324,386.891148632163));
#38411=CARTESIAN_POINT('Ctrl Pts',(4.49667797418915,0.868170030425805,386.91752459065));
#38412=CARTESIAN_POINT('Ctrl Pts',(4.23657545455911,1.57003120705739,386.943900549137));
#38413=CARTESIAN_POINT('Ctrl Pts',(3.97647293492907,2.27189238368897,386.970276507623));
#38414=CARTESIAN_POINT('Ctrl Pts',(3.53821143128416,2.90772967670955,386.99665246611));
#38415=CARTESIAN_POINT('Ctrl Pts',(2.97484978010159,3.40056441773073,387.023028424596));
#38416=CARTESIAN_POINT('Ctrl Pts',(2.41148812891902,3.8933991587519,387.049404383083));
#38417=CARTESIAN_POINT('Ctrl Pts',(1.72302633019879,4.24323134777366,387.07578034157));
#38418=CARTESIAN_POINT('Ctrl Pts',(0.992814123069943,4.40770798605575,387.102156300056));
#38419=CARTESIAN_POINT('Ctrl Pts',(0.262601915941074,4.57218462433785,387.128532258543));
#38420=CARTESIAN_POINT('Ctrl Pts',(-0.509360699596469,4.55130571188027,
387.154908217029));
#38421=CARTESIAN_POINT('Ctrl Pts',(-1.2296148232201,4.34759898792704,387.181284175516));
#38422=CARTESIAN_POINT('Ctrl Pts',(-1.94986894684372,4.14389226397381,387.207660134002));
#38423=CARTESIAN_POINT('Ctrl Pts',(-2.61841457855343,3.75735772852497,387.234036092489));
#38424=CARTESIAN_POINT('Ctrl Pts',(-3.15431316213248,3.23479180914392,387.260412050976));
#38425=CARTESIAN_POINT('Ctrl Pts',(-3.69021174571151,2.71222588976291,387.286788009462));
#38426=CARTESIAN_POINT('Ctrl Pts',(-4.09346328115986,2.05362858644968,387.313163967949));
#38427=CARTESIAN_POINT('Ctrl Pts',(-4.3152474703208,1.33873404498307,387.339539926435));
#38428=CARTESIAN_POINT('Ctrl Pts',(-4.4494392553304,0.906183036834296,387.355498850126));
#38429=CARTESIAN_POINT('Ctrl Pts',(-4.51719722678179,0.453022038514597,
387.371457773817));
#38430=CARTESIAN_POINT('Ctrl Pts',(-4.51744020728156,-6.7888199640348E-5,
387.387416697508));
#38431=CARTESIAN_POINT('Origin',(0.,0.,387.));
#38432=CARTESIAN_POINT('',(-4.51772665650122,0.000115440622527052,388.387416697508));
#38433=CARTESIAN_POINT('',(-4.51762944300479,-0.000110891096316518,388.112583302492));
#38434=CARTESIAN_POINT('',(-4.51775,5.53264807684796E-16,387.));
#38435=CARTESIAN_POINT('Ctrl Pts',(-4.51762944300479,-0.000110891096316518,
388.112583302492));
#38436=CARTESIAN_POINT('Ctrl Pts',(-4.51713192095981,0.534369387836516,
388.093755351949));
#38437=CARTESIAN_POINT('Ctrl Pts',(-4.42224443214638,1.0690216395804,388.074927401406));
#38438=CARTESIAN_POINT('Ctrl Pts',(-4.23657544981682,1.57003120529822,388.056099450863));
#38439=CARTESIAN_POINT('Ctrl Pts',(-3.97647293047822,2.27189238114416,388.029723492377));
#38440=CARTESIAN_POINT('Ctrl Pts',(-3.53821142732417,2.90772967345308,388.00334753389));
#38441=CARTESIAN_POINT('Ctrl Pts',(-2.97484977677246,3.40056441392273,387.976971575404));
#38442=CARTESIAN_POINT('Ctrl Pts',(-2.41148812622074,3.89339915439239,387.950595616917));
#38443=CARTESIAN_POINT('Ctrl Pts',(-1.72302632827134,4.24323134302276,387.924219658431));
#38444=CARTESIAN_POINT('Ctrl Pts',(-0.992814121960003,4.40770798112098,
387.897843699944));
#38445=CARTESIAN_POINT('Ctrl Pts',(-0.262601915648666,4.5721846192192,387.871467741457));
#38446=CARTESIAN_POINT('Ctrl Pts',(0.509360699024613,4.55130570678527,387.845091782971));
#38447=CARTESIAN_POINT('Ctrl Pts',(1.22961482184198,4.34759898306034,387.818715824484));
#38448=CARTESIAN_POINT('Ctrl Pts',(1.94986894465933,4.14389225933542,387.792339865998));
#38449=CARTESIAN_POINT('Ctrl Pts',(2.61841457562078,3.75735772431952,387.765963907511));
#38450=CARTESIAN_POINT('Ctrl Pts',(3.15431315860007,3.2347918055237,387.739587949024));
#38451=CARTESIAN_POINT('Ctrl Pts',(3.69021174157935,2.71222588672787,387.713211990538));
#38452=CARTESIAN_POINT('Ctrl Pts',(4.09346327657648,2.05362858415213,387.686836032051));
#38453=CARTESIAN_POINT('Ctrl Pts',(4.3152474654894,1.3387340434859,387.660460073565));
#38454=CARTESIAN_POINT('Ctrl Pts',(4.53703165440232,0.62383950281966,387.634084115078));
#38455=CARTESIAN_POINT('Ctrl Pts',(4.57734849723102,-0.147352275937061,
387.607708156591));
#38456=CARTESIAN_POINT('Ctrl Pts',(4.4313169703101,-0.881475715061101,387.581332198105));
#38457=CARTESIAN_POINT('Ctrl Pts',(4.28528544338918,-1.61559915418514,387.554956239618));
#38458=CARTESIAN_POINT('Ctrl Pts',(3.95290554671864,-2.3126542536765,387.528580281132));
#38459=CARTESIAN_POINT('Ctrl Pts',(3.47441738908987,-2.88825091257507,387.502204322645));
#38460=CARTESIAN_POINT('Ctrl Pts',(2.99592923146112,-3.46384757147362,387.475828364158));
#38461=CARTESIAN_POINT('Ctrl Pts',(2.37133281287417,-3.91798578977939,387.449452405672));
#38462=CARTESIAN_POINT('Ctrl Pts',(1.67624590710662,-4.19568459092305,387.423076447185));
#38463=CARTESIAN_POINT('Ctrl Pts',(0.981159001339069,-4.47338339206671,
387.396700488698));
#38464=CARTESIAN_POINT('Ctrl Pts',(0.215581608390928,-4.57464277604826,
387.370324530212));
#38465=CARTESIAN_POINT('Ctrl Pts',(-0.527800408696545,-4.48720361207072,
387.343948571725));
#38466=CARTESIAN_POINT('Ctrl Pts',(-1.27118242578404,-4.39976444809319,
387.317572613239));
#38467=CARTESIAN_POINT('Ctrl Pts',(-1.99236906701087,-4.12362673615656,
387.291196654752));
#38468=CARTESIAN_POINT('Ctrl Pts',(-2.60404870735825,-3.69222153415889,
387.264820696266));
#38469=CARTESIAN_POINT('Ctrl Pts',(-3.21572834770564,-3.26081633216121,
387.238444737779));
#38470=CARTESIAN_POINT('Ctrl Pts',(-3.71790098717359,-2.67414364010249,
387.212068779293));
#38471=CARTESIAN_POINT('Ctrl Pts',(-4.049770284447,-2.00322993458336,387.185692820806));
#38472=CARTESIAN_POINT('Ctrl Pts',(-4.35639806038402,-1.38334500078815,
387.161322981368));
#38473=CARTESIAN_POINT('Ctrl Pts',(-4.51764337890668,-0.691546237269266,
387.13695314193));
#38474=CARTESIAN_POINT('Ctrl Pts',(-4.51807831563064,5.66723631286815E-5,
387.112583302492));
#38475=CARTESIAN_POINT('Ctrl Pts',(-4.51744020728156,-6.7888199640348E-5,
387.387416697508));
#38476=CARTESIAN_POINT('Ctrl Pts',(-4.51759881047873,-0.295818004161051,
387.397833732304));
#38477=CARTESIAN_POINT('Ctrl Pts',(-4.48899129636465,-0.591537838638136,
387.408250767099));
#38478=CARTESIAN_POINT('Ctrl Pts',(-4.43131697527066,-0.881475716049439,
387.418667801895));
#38479=CARTESIAN_POINT('Ctrl Pts',(-4.28528544818601,-1.61559915599528,
387.445043760382));
#38480=CARTESIAN_POINT('Ctrl Pts',(-3.95290555114312,-2.31265425626688,
387.471419718868));
#38481=CARTESIAN_POINT('Ctrl Pts',(-3.47441739297849,-2.88825091580966,
387.497795677355));
#38482=CARTESIAN_POINT('Ctrl Pts',(-2.99592923481386,-3.46384757535244,
387.524171635842));
#38483=CARTESIAN_POINT('Ctrl Pts',(-2.37133281552749,-3.91798579416642,
387.550547594328));
#38484=CARTESIAN_POINT('Ctrl Pts',(-1.67624590898167,-4.19568459562072,
387.576923552815));
#38485=CARTESIAN_POINT('Ctrl Pts',(-0.981159002435877,-4.47338339707502,
387.603299511301));
#38486=CARTESIAN_POINT('Ctrl Pts',(-0.215581608630632,-4.57464278116965,
387.629675469788));
#38487=CARTESIAN_POINT('Ctrl Pts',(0.527800409289026,-4.48720361709396,
387.656051428274));
#38488=CARTESIAN_POINT('Ctrl Pts',(1.27118242720868,-4.39976445301828,387.682427386761));
#38489=CARTESIAN_POINT('Ctrl Pts',(1.99236906924277,-4.12362674077227,387.708803345248));
#38490=CARTESIAN_POINT('Ctrl Pts',(2.60404871027476,-3.69222153829144,387.735179303734));
#38491=CARTESIAN_POINT('Ctrl Pts',(3.21572835130679,-3.26081633581058,387.761555262221));
#38492=CARTESIAN_POINT('Ctrl Pts',(3.71790099133673,-2.67414364309488,387.787931220707));
#38493=CARTESIAN_POINT('Ctrl Pts',(4.04977028898144,-2.00322993682453,387.814307179194));
#38494=CARTESIAN_POINT('Ctrl Pts',(4.38163958662613,-1.33231623055421,387.840683137681));
#38495=CARTESIAN_POINT('Ctrl Pts',(4.54320554188561,-0.577161510729227,
387.867059096167));
#38496=CARTESIAN_POINT('Ctrl Pts',(4.51490791155097,0.170810197357385,387.893435054654));
#38497=CARTESIAN_POINT('Ctrl Pts',(4.48661028121633,0.918781905443997,387.919811013141));
#38498=CARTESIAN_POINT('Ctrl Pts',(4.26844906528759,1.65957060179219,387.946186971627));
#38499=CARTESIAN_POINT('Ctrl Pts',(3.88683630357511,2.30349150693406,387.972562930114));
#38500=CARTESIAN_POINT('Ctrl Pts',(3.50522354186264,2.94741241207594,387.9989388886));
#38501=CARTESIAN_POINT('Ctrl Pts',(2.96015923436644,3.49446552601145,388.025314847087));
#38502=CARTESIAN_POINT('Ctrl Pts',(2.31763247143664,3.87842098032811,388.051690805573));
#38503=CARTESIAN_POINT('Ctrl Pts',(1.67510570850681,4.2623764346448,388.07806676406));
#38504=CARTESIAN_POINT('Ctrl Pts',(0.935116490143367,4.48323422934263,388.104442722547));
#38505=CARTESIAN_POINT('Ctrl Pts',(0.187252805721414,4.5142558589491,388.130818681033));
#38506=CARTESIAN_POINT('Ctrl Pts',(-0.560610878700497,4.54527748855557,
388.15719463952));
#38507=CARTESIAN_POINT('Ctrl Pts',(-1.31634902918093,4.38646295307071,388.183570598006));
#38508=CARTESIAN_POINT('Ctrl Pts',(-1.98846698645264,4.05703939062647,388.209946556493));
#38509=CARTESIAN_POINT('Ctrl Pts',(-2.66058494372436,3.72761582818222,388.23632251498));
#38510=CARTESIAN_POINT('Ctrl Pts',(-3.24908270778736,3.22758323877859,388.262698473466));
#38511=CARTESIAN_POINT('Ctrl Pts',(-3.68271284675239,2.6174788751147,388.289074431953));
#38512=CARTESIAN_POINT('Ctrl Pts',(-4.11634298571743,2.00737451145079,388.315450390439));
#38513=CARTESIAN_POINT('Ctrl Pts',(-4.3951054995845,1.28719837352659,388.341826348926));
#38514=CARTESIAN_POINT('Ctrl Pts',(-4.48525155457229,0.544139748147192,
388.368202307413));
#38515=CARTESIAN_POINT('Ctrl Pts',(-4.50714145691119,0.363704999850856,
388.374607104111));
#38516=CARTESIAN_POINT('Ctrl Pts',(-4.51790959247399,0.181920986011914,
388.381011900809));
#38517=CARTESIAN_POINT('Ctrl Pts',(-4.51772665650122,0.000115440622527052,
388.387416697508));
#38518=CARTESIAN_POINT('Origin',(0.,0.,387.));
#38519=CARTESIAN_POINT('',(-4.51800421755028,-8.27334347235434E-5,389.387416697508));
#38520=CARTESIAN_POINT('',(-4.51750342669873,8.9713446903977E-5,389.112583302492));
#38521=CARTESIAN_POINT('',(-4.51775,5.53264807684796E-16,387.));
#38522=CARTESIAN_POINT('Ctrl Pts',(-4.51750342669873,8.9713446903977E-5,
389.112583302492));
#38523=CARTESIAN_POINT('Ctrl Pts',(-4.51769355714261,0.263372352578081,
389.103309478941));
#38524=CARTESIAN_POINT('Ctrl Pts',(-4.49505280568826,0.526622657629559,
389.094035655391));
#38525=CARTESIAN_POINT('Ctrl Pts',(-4.4492816175085,0.7857878948557,389.084761831841));
#38526=CARTESIAN_POINT('Ctrl Pts',(-4.31910241442768,1.52288748501391,389.058385873354));
#38527=CARTESIAN_POINT('Ctrl Pts',(-4.00181938159719,2.22694265651365,389.032009914867));
#38528=CARTESIAN_POINT('Ctrl Pts',(-3.53584490161497,2.81271583337604,389.005633956381));
#38529=CARTESIAN_POINT('Ctrl Pts',(-3.06987042163275,3.39848901023841,388.979257997894));
#38530=CARTESIAN_POINT('Ctrl Pts',(-2.45520449449881,3.86598019246346,388.952882039408));
#38531=CARTESIAN_POINT('Ctrl Pts',(-1.76626264301101,4.15859180534764,388.926506080921));
#38532=CARTESIAN_POINT('Ctrl Pts',(-1.07732079152318,4.45120341823184,388.900130122435));
#38533=CARTESIAN_POINT('Ctrl Pts',(-0.314103015681492,4.56893546177518,
388.873754163948));
#38534=CARTESIAN_POINT('Ctrl Pts',(0.430990492327212,4.49753451605703,388.847378205461));
#38535=CARTESIAN_POINT('Ctrl Pts',(1.1760840003359,4.42613357033888,388.821002246975));
#38536=CARTESIAN_POINT('Ctrl Pts',(1.90305324051159,4.16559963535927,388.794626288488));
#38537=CARTESIAN_POINT('Ctrl Pts',(2.52388650815824,3.74747467256786,388.768250330001));
#38538=CARTESIAN_POINT('Ctrl Pts',(3.14471977580489,3.32934970977646,388.741874371515));
#38539=CARTESIAN_POINT('Ctrl Pts',(3.65941707092249,2.75363371917326,388.715498413028));
#38540=CARTESIAN_POINT('Ctrl Pts',(4.00566573453967,2.09002668660847,388.689122454542));
#38541=CARTESIAN_POINT('Ctrl Pts',(4.35191439815685,1.42641965404367,388.662746496055));
#38542=CARTESIAN_POINT('Ctrl Pts',(4.52971443027359,0.67492157951728,388.636370537568));
#38543=CARTESIAN_POINT('Ctrl Pts',(4.51754018295765,-0.0734862093441271,
388.609994579082));
#38544=CARTESIAN_POINT('Ctrl Pts',(4.50536593564171,-0.821893998205556,
388.583618620595));
#38545=CARTESIAN_POINT('Ctrl Pts',(4.30321740889306,-1.567211501402,388.557242662109));
#38546=CARTESIAN_POINT('Ctrl Pts',(3.93556804045529,-2.21920565215297,388.530866703622));
#38547=CARTESIAN_POINT('Ctrl Pts',(3.56791867201753,-2.87119980290394,388.504490745136));
#38548=CARTESIAN_POINT('Ctrl Pts',(3.03476846189066,-3.42987060120944,388.478114786649));
#38549=CARTESIAN_POINT('Ctrl Pts',(2.40066410099242,-3.8275816649429,388.451738828162));
#38550=CARTESIAN_POINT('Ctrl Pts',(1.7665597400942,-4.22529272867635,388.425362869676));
#38551=CARTESIAN_POINT('Ctrl Pts',(1.03150122842463,-4.46204405783778,388.398986911189));
#38552=CARTESIAN_POINT('Ctrl Pts',(0.284479611392651,-4.509172970546,388.372610952703));
#38553=CARTESIAN_POINT('Ctrl Pts',(-0.462542005639328,-4.55630188325423,
388.346234994216));
#38554=CARTESIAN_POINT('Ctrl Pts',(-1.22152672803371,-4.41380837950926,
388.319859035729));
#38555=CARTESIAN_POINT('Ctrl Pts',(-1.90058684505317,-4.09894366538644,
388.293483077243));
#38556=CARTESIAN_POINT('Ctrl Pts',(-2.57964696207265,-3.78407895126361,
388.267107118756));
#38557=CARTESIAN_POINT('Ctrl Pts',(-3.17878247371721,-3.29684302676292,
388.24073116027));
#38558=CARTESIAN_POINT('Ctrl Pts',(-3.62545807201282,-2.6962238956878,388.214355201783));
#38559=CARTESIAN_POINT('Ctrl Pts',(-4.07213367030842,-2.09560476461269,
388.187979243296));
#38560=CARTESIAN_POINT('Ctrl Pts',(-4.36634935525508,-1.38160242696316,
388.16160328481));
#38561=CARTESIAN_POINT('Ctrl Pts',(-4.47248542996683,-0.640658728446904,
388.135227326323));
#38562=CARTESIAN_POINT('Ctrl Pts',(-4.50285839007941,-0.428622872948985,
388.127679318379));
#38563=CARTESIAN_POINT('Ctrl Pts',(-4.51782889648961,-0.2143807013974,388.120131310436));
#38564=CARTESIAN_POINT('Ctrl Pts',(-4.51762944300479,-0.000110891096316518,
388.112583302492));
#38565=CARTESIAN_POINT('Ctrl Pts',(-4.51772665650122,0.000115440622527052,
388.387416697508));
#38566=CARTESIAN_POINT('Ctrl Pts',(-4.51715623341347,-0.566782797039444,
388.407387859296));
#38567=CARTESIAN_POINT('Ctrl Pts',(-4.41010960182223,-1.13389038388221,
388.427359021084));
#38568=CARTESIAN_POINT('Ctrl Pts',(-4.20176182131765,-1.66095369298009,
388.447330182872));
#38569=CARTESIAN_POINT('Ctrl Pts',(-3.9265964369667,-2.35704739589339,388.473706141359));
#38570=CARTESIAN_POINT('Ctrl Pts',(-3.47473607215626,-2.9832936888854,388.500082099846));
#38571=CARTESIAN_POINT('Ctrl Pts',(-2.90088593144485,-3.46387505347005,
388.526458058332));
#38572=CARTESIAN_POINT('Ctrl Pts',(-2.32703579073342,-3.94445641805472,
388.552834016819));
#38573=CARTESIAN_POINT('Ctrl Pts',(-1.631195874121,-4.27937285423203,388.579209975305));
#38574=CARTESIAN_POINT('Ctrl Pts',(-0.897609164490652,-4.42807716296015,
388.605585933792));
#38575=CARTESIAN_POINT('Ctrl Pts',(-0.164022454860301,-4.57678147168827,
388.631961892278));
#38576=CARTESIAN_POINT('Ctrl Pts',(0.607311047787985,-4.53927365296719,
388.658337850765));
#38577=CARTESIAN_POINT('Ctrl Pts',(1.32300860769931,-4.32009465142378,388.684713809252));
#38578=CARTESIAN_POINT('Ctrl Pts',(2.03870616761062,-4.10091564988038,388.711089767738));
#38579=CARTESIAN_POINT('Ctrl Pts',(2.69876778478497,-3.70006546551466,388.737465726225));
#38580=CARTESIAN_POINT('Ctrl Pts',(3.22328203392201,-3.16607367303769,388.763841684711));
#38581=CARTESIAN_POINT('Ctrl Pts',(3.74779628305905,-2.63208188056073,388.790217643198));
#38582=CARTESIAN_POINT('Ctrl Pts',(4.13676316415879,-1.96494847997252,388.816593601685));
#38583=CARTESIAN_POINT('Ctrl Pts',(4.3430917738047,-1.24544105344924,388.842969560171));
#38584=CARTESIAN_POINT('Ctrl Pts',(4.54942038345061,-0.525933626925946,
388.869345518658));
#38585=CARTESIAN_POINT('Ctrl Pts',(4.57311072164268,0.245947825532416,388.895721477144));
#38586=CARTESIAN_POINT('Ctrl Pts',(4.41129467934152,0.976754229742574,388.922097435631));
#38587=CARTESIAN_POINT('Ctrl Pts',(4.24947863704035,1.70756063395273,388.948473394118));
#38588=CARTESIAN_POINT('Ctrl Pts',(3.90215621424595,2.39729198991468,388.974849352604));
#38589=CARTESIAN_POINT('Ctrl Pts',(3.41137656079843,2.96244485750231,389.001225311091));
#38590=CARTESIAN_POINT('Ctrl Pts',(2.92059690735092,3.52759772508993,389.027601269577));
#38591=CARTESIAN_POINT('Ctrl Pts',(2.2863600232503,3.96817210430322,389.053977228064));
#38592=CARTESIAN_POINT('Ctrl Pts',(1.58545082079536,4.23082914665035,389.08035318655));
#38593=CARTESIAN_POINT('Ctrl Pts',(0.88454161834042,4.49348618899748,389.106729145037));
#38594=CARTESIAN_POINT('Ctrl Pts',(0.116960097531164,4.57822589447844,389.133105103524));
#38595=CARTESIAN_POINT('Ctrl Pts',(-0.624365245616139,4.47478911384364,
389.15948106201));
#38596=CARTESIAN_POINT('Ctrl Pts',(-1.36569058876346,4.37135233320883,389.185857020497));
#38597=CARTESIAN_POINT('Ctrl Pts',(-2.08075975424883,4.07973906645826,389.212232978983));
#38598=CARTESIAN_POINT('Ctrl Pts',(-2.6830017391303,3.63525394451758,389.23860893747));
#38599=CARTESIAN_POINT('Ctrl Pts',(-3.28524372401176,3.19076882257689,389.264984895957));
#38600=CARTESIAN_POINT('Ctrl Pts',(-3.77465852828932,2.59341184544609,389.291360854443));
#38601=CARTESIAN_POINT('Ctrl Pts',(-4.09199435856171,1.91550299994699,389.31773681293));
#38602=CARTESIAN_POINT('Ctrl Pts',(-4.37143979921575,1.3185375205331,389.340963441123));
#38603=CARTESIAN_POINT('Ctrl Pts',(-4.51744597443699,0.659107802205375,
389.364190069315));
#38604=CARTESIAN_POINT('Ctrl Pts',(-4.51800421755028,-8.27334347235434E-5,
389.387416697508));
#38605=CARTESIAN_POINT('Origin',(0.,0.,387.));
#38606=CARTESIAN_POINT('',(-4.51737568732049,-1.26367906908009E-5,390.387416697508));
#38607=CARTESIAN_POINT('',(-4.51813713037119,-8.34916185418341E-6,390.112583302492));
#38608=CARTESIAN_POINT('',(-4.51775,5.53264807684796E-16,387.));
#38609=CARTESIAN_POINT('Ctrl Pts',(-4.5181365124173,-8.33583456870006E-6,
390.112583302492));
#38610=CARTESIAN_POINT('Ctrl Pts',(-4.51805642563476,0.740544543431,390.086487647447));
#38611=CARTESIAN_POINT('Ctrl Pts',(-4.33223070178982,1.48113615227849,390.060391992403));
#38612=CARTESIAN_POINT('Ctrl Pts',(-3.98247233026486,2.13388932849751,390.034296337358));
#38613=CARTESIAN_POINT('Ctrl Pts',(-3.62895706989363,2.79365397699786,390.007920378871));
#38614=CARTESIAN_POINT('Ctrl Pts',(-3.10796852081612,3.36368304570199,389.981544420385));
#38615=CARTESIAN_POINT('Ctrl Pts',(-2.48258100282108,3.7749650451405,389.955168461898));
#38616=CARTESIAN_POINT('Ctrl Pts',(-1.85719348482602,4.18624704457905,389.928792503412));
#38617=CARTESIAN_POINT('Ctrl Pts',(-1.12740699791342,4.43878197475195,389.902416544925));
#38618=CARTESIAN_POINT('Ctrl Pts',(-0.381574321303787,4.50199628664022,
389.876040586438));
#38619=CARTESIAN_POINT('Ctrl Pts',(0.364258355305801,4.56521059852849,389.849664627952));
#38620=CARTESIAN_POINT('Ctrl Pts',(1.12613722161242,4.43910429213214,389.823288669465));
#38621=CARTESIAN_POINT('Ctrl Pts',(1.81182418267365,4.13894463102368,389.796912710979));
#38622=CARTESIAN_POINT('Ctrl Pts',(2.49751114373488,3.83878496991522,389.770536752492));
#38623=CARTESIAN_POINT('Ctrl Pts',(3.10700619955072,3.36457195409465,389.744160794005));
#38624=CARTESIAN_POINT('Ctrl Pts',(3.56651984720739,2.7737169479016,389.717784835519));
#38625=CARTESIAN_POINT('Ctrl Pts',(4.02603349486408,2.18286194170853,389.691408877032));
#38626=CARTESIAN_POINT('Ctrl Pts',(4.33556573436158,1.47536494514296,389.665032918546));
#38627=CARTESIAN_POINT('Ctrl Pts',(4.45764254540988,0.736880224291923,389.638656960059));
#38628=CARTESIAN_POINT('Ctrl Pts',(4.57971935645818,-0.0016044965591186,
389.612281001572));
#38629=CARTESIAN_POINT('Ctrl Pts',(4.51434073905728,-0.77107694169564,389.585905043086));
#38630=CARTESIAN_POINT('Ctrl Pts',(4.26942186107142,-1.47837968729494,389.559529084599));
#38631=CARTESIAN_POINT('Ctrl Pts',(4.02450298308556,-2.18568243289422,389.533153126113));
#38632=CARTESIAN_POINT('Ctrl Pts',(3.60004384451474,-2.83081547895628,389.506777167626));
#38633=CARTESIAN_POINT('Ctrl Pts',(3.04743227622566,-3.33567475174347,389.480401209139));
#38634=CARTESIAN_POINT('Ctrl Pts',(2.49482070793658,-3.84053402453067,389.454025250653));
#38635=CARTESIAN_POINT('Ctrl Pts',(1.81405670992924,-4.205119524043,389.427649292166));
#38636=CARTESIAN_POINT('Ctrl Pts',(1.08755807466189,-4.38529211818763,389.40127333368));
#38637=CARTESIAN_POINT('Ctrl Pts',(0.361059439394515,-4.56546471233226,
389.374897375193));
#38638=CARTESIAN_POINT('Ctrl Pts',(-0.411173833132874,-4.56122440110918,
389.348521416706));
#38639=CARTESIAN_POINT('Ctrl Pts',(-1.13565007507237,-4.37308454464225,
389.32214545822));
#38640=CARTESIAN_POINT('Ctrl Pts',(-1.86012631701186,-4.18494468817533,
389.295769499733));
#38641=CARTESIAN_POINT('Ctrl Pts',(-2.53684552836345,-3.81290528646455,
389.269393541247));
#38642=CARTESIAN_POINT('Ctrl Pts',(-3.08387960529535,-3.30200789030617,
389.24301758276));
#38643=CARTESIAN_POINT('Ctrl Pts',(-3.63091368222724,-2.79111049414779,
389.216641624274));
#38644=CARTESIAN_POINT('Ctrl Pts',(-4.04826262473945,-2.14135510354181,
389.190265665787));
#38645=CARTESIAN_POINT('Ctrl Pts',(-4.28539940932997,-1.43140540383048,
389.1638897073));
#38646=CARTESIAN_POINT('Ctrl Pts',(-4.43915857188131,-0.971075002245244,
389.146787572364));
#38647=CARTESIAN_POINT('Ctrl Pts',(-4.51715280146967,-0.485437663288439,
389.129685437428));
#38648=CARTESIAN_POINT('Ctrl Pts',(-4.51750342669873,8.9713446903977E-5,
389.112583302492));
#38649=CARTESIAN_POINT('Ctrl Pts',(-4.51800421755028,-8.27334347235434E-5,
389.387416697508));
#38650=CARTESIAN_POINT('Ctrl Pts',(-4.51807991049777,-0.089463280026118,
389.390566027802));
#38651=CARTESIAN_POINT('Ctrl Pts',(-4.5154815404334,-0.178839429239229,
389.393715358096));
#38652=CARTESIAN_POINT('Ctrl Pts',(-4.51017917155373,-0.268054870856108,
389.39686468839));
#38653=CARTESIAN_POINT('Ctrl Pts',(-4.46577129800614,-1.01524318229275,
389.423240646876));
#38654=CARTESIAN_POINT('Ctrl Pts',(-4.23169869464373,-1.75115909129866,
389.449616605363));
#38655=CARTESIAN_POINT('Ctrl Pts',(-3.83629973908422,-2.38670775027215,
389.475992563849));
#38656=CARTESIAN_POINT('Ctrl Pts',(-3.4409007835247,-3.02225640924567,389.502368522336));
#38657=CARTESIAN_POINT('Ctrl Pts',(-2.88417547576807,-3.55743781818676,
389.528744480823));
#38658=CARTESIAN_POINT('Ctrl Pts',(-2.23352466398677,-3.92745937581404,
389.555120439309));
#38659=CARTESIAN_POINT('Ctrl Pts',(-1.58287385220546,-4.29748093344132,
389.581496397796));
#38660=CARTESIAN_POINT('Ctrl Pts',(-0.838297536399466,-4.50234263975477,
389.607872356282));
#38661=CARTESIAN_POINT('Ctrl Pts',(-0.0899390503012636,-4.51724258154659,
389.634248314769));
#38662=CARTESIAN_POINT('Ctrl Pts',(0.658419435796918,-4.53214252333841,
389.660624273256));
#38663=CARTESIAN_POINT('Ctrl Pts',(1.4105600921873,-4.3570807006086,389.687000231742));
#38664=CARTESIAN_POINT('Ctrl Pts',(2.07542379603256,-4.01325125554937,389.713376190229));
#38665=CARTESIAN_POINT('Ctrl Pts',(2.74028749987779,-3.66942181049016,389.739752148715));
#38666=CARTESIAN_POINT('Ctrl Pts',(3.31787425117789,-3.15682474310154,389.766128107202));
#38667=CARTESIAN_POINT('Ctrl Pts',(3.7382575774187,-2.53751844489424,389.792504065688));
#38668=CARTESIAN_POINT('Ctrl Pts',(4.15864090365956,-1.91821214668688,389.818880024175));
#38669=CARTESIAN_POINT('Ctrl Pts',(4.4218208048411,-1.19219661766082,389.845255982662));
#38670=CARTESIAN_POINT('Ctrl Pts',(4.4959349813437,-0.447368099932093,389.871631941148));
#38671=CARTESIAN_POINT('Ctrl Pts',(4.5700491578463,0.297460417796599,389.898007899635));
#38672=CARTESIAN_POINT('Ctrl Pts',(4.45509760966997,1.06110192422797,389.924383858122));
#38673=CARTESIAN_POINT('Ctrl Pts',(4.16499713157485,1.7511049275472,389.950759816608));
#38674=CARTESIAN_POINT('Ctrl Pts',(3.87489665347973,2.44110793086643,389.977135775095));
#38675=CARTESIAN_POINT('Ctrl Pts',(3.40964724546582,3.05747243107353,390.003511733581));
#38676=CARTESIAN_POINT('Ctrl Pts',(2.8255750782226,3.52557726487935,390.029887692068));
#38677=CARTESIAN_POINT('Ctrl Pts',(2.24150291097938,3.99368209868516,390.056263650554));
#38678=CARTESIAN_POINT('Ctrl Pts',(1.53860798450686,4.31352726608968,390.082639609041));
#38679=CARTESIAN_POINT('Ctrl Pts',(0.80198740784653,4.44639019553642,390.109015567528));
#38680=CARTESIAN_POINT('Ctrl Pts',(0.0653668311861832,4.57925312498317,
390.135391526014));
#38681=CARTESIAN_POINT('Ctrl Pts',(-0.704979395661959,4.52513381647212,
390.161767484501));
#38682=CARTESIAN_POINT('Ctrl Pts',(-1.41578806308163,4.2905843114595,390.188143442987));
#38683=CARTESIAN_POINT('Ctrl Pts',(-2.1265967305013,4.05603480644688,390.214519401474));
#38684=CARTESIAN_POINT('Ctrl Pts',(-2.7778678384925,3.64105510493269,390.240895359961));
#38685=CARTESIAN_POINT('Ctrl Pts',(-3.2907541989407,3.09588539443257,390.267271318447));
#38686=CARTESIAN_POINT('Ctrl Pts',(-3.8036405593889,2.55071568393247,390.293647276934));
#38687=CARTESIAN_POINT('Ctrl Pts',(-4.17814217229411,1.87535596444644,390.320023235421));
#38688=CARTESIAN_POINT('Ctrl Pts',(-4.36891939528681,1.15156975072878,390.346399193907));
#38689=CARTESIAN_POINT('Ctrl Pts',(-4.46781255254173,0.776380811874881,
390.360071695107));
#38690=CARTESIAN_POINT('Ctrl Pts',(-4.51733762799004,0.388179321285348,
390.373744196308));
#38691=CARTESIAN_POINT('Ctrl Pts',(-4.51737568732049,-1.26367906908009E-5,
390.387416697508));
#38692=CARTESIAN_POINT('Origin',(0.,0.,387.));
#38693=CARTESIAN_POINT('',(-4.51792755410097,9.93894350090341E-5,391.387416697508));
#38694=CARTESIAN_POINT('',(-4.51747010126728,-7.96701847477171E-5,391.112583302492));
#38695=CARTESIAN_POINT('',(-4.51775,5.53264807684796E-16,387.));
#38696=CARTESIAN_POINT('Ctrl Pts',(-4.51747010126728,-7.96701847477171E-5,
391.112583302492));
#38697=CARTESIAN_POINT('Ctrl Pts',(-4.51717195077355,0.469542077919004,
391.09604177444));
#38698=CARTESIAN_POINT('Ctrl Pts',(-4.44429158523714,0.939254240738123,
391.079500246387));
#38699=CARTESIAN_POINT('Ctrl Pts',(-4.30028579839415,1.38604169480228,391.062958718335));
#38700=CARTESIAN_POINT('Ctrl Pts',(-4.07066428800006,2.09845757944446,391.036582759848));
#38701=CARTESIAN_POINT('Ctrl Pts',(-3.66020460842122,2.75258681658163,391.010206801362));
#38702=CARTESIAN_POINT('Ctrl Pts',(-3.11859972342044,3.26923619408001,390.983830842875));
#38703=CARTESIAN_POINT('Ctrl Pts',(-2.57699483841966,3.78588557157838,390.957454884389));
#38704=CARTESIAN_POINT('Ctrl Pts',(-1.90424474799695,4.16505508943795,390.931078925902));
#38705=CARTESIAN_POINT('Ctrl Pts',(-1.181797027951,4.36083997783993,390.904702967415));
#38706=CARTESIAN_POINT('Ctrl Pts',(-0.459349307905077,4.55662486624191,
390.878327008929));
#38707=CARTESIAN_POINT('Ctrl Pts',(0.312796041764081,4.5690251251863,390.851951050442));
#38708=CARTESIAN_POINT('Ctrl Pts',(1.04115799773134,4.39653949730477,390.825575091955));
#38709=CARTESIAN_POINT('Ctrl Pts',(1.76951995369859,4.22405386942324,390.799199133469));
#38710=CARTESIAN_POINT('Ctrl Pts',(2.45409851596394,3.86668235471579,390.772823174982));
#38711=CARTESIAN_POINT('Ctrl Pts',(3.01201407568894,3.36769071255846,390.746447216496));
#38712=CARTESIAN_POINT('Ctrl Pts',(3.56992963541394,2.86869907040112,390.720071258009));
#38713=CARTESIAN_POINT('Ctrl Pts',(4.00118219259857,2.22808730079389,390.693695299523));
#38714=CARTESIAN_POINT('Ctrl Pts',(4.25356146018424,1.52341210184117,390.667319341036));
#38715=CARTESIAN_POINT('Ctrl Pts',(4.5059407277699,0.818736902888453,390.640943382549));
#38716=CARTESIAN_POINT('Ctrl Pts',(4.5794467057566,0.0499982745902433,390.614567424063));
#38717=CARTESIAN_POINT('Ctrl Pts',(4.46518027424979,-0.68973519995098,390.588191465576));
#38718=CARTESIAN_POINT('Ctrl Pts',(4.35091384274297,-1.42946867449225,390.56181550709));
#38719=CARTESIAN_POINT('Ctrl Pts',(4.04887500174263,-2.14019699527652,390.535439548603));
#38720=CARTESIAN_POINT('Ctrl Pts',(3.59563057115222,-2.73587469073354,390.509063590117));
#38721=CARTESIAN_POINT('Ctrl Pts',(3.14238614056185,-3.33155238619052,390.48268763163));
#38722=CARTESIAN_POINT('Ctrl Pts',(2.53793612038144,-3.81217945632025,390.456311673143));
#38723=CARTESIAN_POINT('Ctrl Pts',(1.85545922814075,-4.11956800894318,390.429935714657));
#38724=CARTESIAN_POINT('Ctrl Pts',(1.17298233590006,-4.42695656156612,390.40355975617));
#38725=CARTESIAN_POINT('Ctrl Pts',(0.412478571599103,-4.56110659668227,
390.377183797684));
#38726=CARTESIAN_POINT('Ctrl Pts',(-0.333980448764015,-4.50577702371569,
390.350807839197));
#38727=CARTESIAN_POINT('Ctrl Pts',(-1.08043946912713,-4.45044745074911,
390.32443188071));
#38728=CARTESIAN_POINT('Ctrl Pts',(-1.81285374555241,-4.2056382696998,390.298055922224));
#38729=CARTESIAN_POINT('Ctrl Pts',(-2.44255236123965,-3.80098769929651,
390.271679963737));
#38730=CARTESIAN_POINT('Ctrl Pts',(-3.07225097692695,-3.39633712889319,
390.245304005251));
#38731=CARTESIAN_POINT('Ctrl Pts',(-3.59923393187618,-2.83184516913586,
390.218928046764));
#38732=CARTESIAN_POINT('Ctrl Pts',(-3.95970118387424,-2.17585295046006,
390.192552088277));
#38733=CARTESIAN_POINT('Ctrl Pts',(-4.32016843587225,-1.51986073178434,
390.166176129791));
#38734=CARTESIAN_POINT('Ctrl Pts',(-4.51411998491911,-0.772368254190162,
390.139800171304));
#38735=CARTESIAN_POINT('Ctrl Pts',(-4.51807477361008,-0.0238719012447998,
390.113424212818));
#38736=CARTESIAN_POINT('Ctrl Pts',(-4.51811680206878,-0.0159174565147239,
390.113143909376));
#38737=CARTESIAN_POINT('Ctrl Pts',(-4.51813737266016,-0.00796289840890401,
390.112863605934));
#38738=CARTESIAN_POINT('Ctrl Pts',(-4.5181365124173,-8.33583456870006E-6,
390.112583302492));
#38739=CARTESIAN_POINT('Ctrl Pts',(-4.51737568732049,-1.26367906908009E-5,
390.387416697508));
#38740=CARTESIAN_POINT('Ctrl Pts',(-4.51741104918088,-0.360691336761726,
390.400120154794));
#38741=CARTESIAN_POINT('Ctrl Pts',(-4.47472562929359,-0.721361807575693,
390.412823612081));
#38742=CARTESIAN_POINT('Ctrl Pts',(-4.38922403190431,-1.07157919495506,
390.425527069367));
#38743=CARTESIAN_POINT('Ctrl Pts',(-4.2116986124489,-1.79872921897196,390.451903027853));
#38744=CARTESIAN_POINT('Ctrl Pts',(-3.84959494045787,-2.48081655905642,
390.47827898634));
#38745=CARTESIAN_POINT('Ctrl Pts',(-3.3467516815685,-3.03526321020521,390.504654944827));
#38746=CARTESIAN_POINT('Ctrl Pts',(-2.84390842267912,-3.589709861354,390.531030903313));
#38747=CARTESIAN_POINT('Ctrl Pts',(-2.2003255768914,-4.01651582356711,390.5574068618));
#38748=CARTESIAN_POINT('Ctrl Pts',(-1.49391954044408,-4.26400914398482,
390.583782820286));
#38749=CARTESIAN_POINT('Ctrl Pts',(-0.787513503996787,-4.51150246440253,
390.610158778773));
#38750=CARTESIAN_POINT('Ctrl Pts',(-0.018284276889904,-4.57968314302485,
390.636534737259));
#38751=CARTESIAN_POINT('Ctrl Pts',(0.720640162637278,-4.46029677592208,
390.662910695746));
#38752=CARTESIAN_POINT('Ctrl Pts',(1.45956460216448,-4.34091040881931,390.689286654233));
#38753=CARTESIAN_POINT('Ctrl Pts',(2.16818425411199,-4.03395699599143,390.715662612719));
#38754=CARTESIAN_POINT('Ctrl Pts',(2.76070893630653,-3.57659834791441,390.742038571206));
#38755=CARTESIAN_POINT('Ctrl Pts',(3.35323361850104,-3.11923969983741,390.768414529692));
#38756=CARTESIAN_POINT('Ctrl Pts',(3.8296633309426,-2.51147581651127,390.794790488179));
#38757=CARTESIAN_POINT('Ctrl Pts',(4.13231834133649,-1.82688661365747,390.821166446666));
#38758=CARTESIAN_POINT('Ctrl Pts',(4.43497335173039,-1.14229741080364,390.847542405152));
#38759=CARTESIAN_POINT('Ctrl Pts',(4.5638536600766,-0.380882888422163,390.873918363639));
#38760=CARTESIAN_POINT('Ctrl Pts',(4.50335616377816,0.365175075091525,390.900294322126));
#38761=CARTESIAN_POINT('Ctrl Pts',(4.44285866747971,1.11123303860522,390.926670280612));
#38762=CARTESIAN_POINT('Ctrl Pts',(4.1929833665366,1.84193444325112,390.953046239099));
#38763=CARTESIAN_POINT('Ctrl Pts',(3.78398181766136,2.46881574381626,390.979422197585));
#38764=CARTESIAN_POINT('Ctrl Pts',(3.37498026878612,3.0956970443814,391.005798156072));
#38765=CARTESIAN_POINT('Ctrl Pts',(2.80685247197875,3.61875824086581,391.032174114558));
#38766=CARTESIAN_POINT('Ctrl Pts',(2.14837973615702,3.97467408507625,391.058550073045));
#38767=CARTESIAN_POINT('Ctrl Pts',(1.48990700033531,4.33058992928668,391.084926031532));
#38768=CARTESIAN_POINT('Ctrl Pts',(0.74108932549923,4.51936042122317,391.111301990018));
#38769=CARTESIAN_POINT('Ctrl Pts',(-0.00741646764041988,4.51813175652443,
391.137677948505));
#38770=CARTESIAN_POINT('Ctrl Pts',(-0.75592226078007,4.51690309182569,391.164053906991));
#38771=CARTESIAN_POINT('Ctrl Pts',(-1.5041161722233,4.32567527049173,391.190429865478));
#38772=CARTESIAN_POINT('Ctrl Pts',(-2.16141689818149,3.96759959743449,391.216805823964));
#38773=CARTESIAN_POINT('Ctrl Pts',(-2.81871762413969,3.60952392437724,391.243181782451));
#38774=CARTESIAN_POINT('Ctrl Pts',(-3.38512516461286,3.0846003995967,391.269557740938));
#38775=CARTESIAN_POINT('Ctrl Pts',(-3.79206647629354,2.45637973706784,391.295933699424));
#38776=CARTESIAN_POINT('Ctrl Pts',(-4.19900778797422,1.82815907453898,391.322309657911));
#38777=CARTESIAN_POINT('Ctrl Pts',(-4.44648287086241,1.0966412742618,391.348685616397));
#38778=CARTESIAN_POINT('Ctrl Pts',(-4.50453075451936,0.350388719704337,
391.375061574884));
#38779=CARTESIAN_POINT('Ctrl Pts',(-4.51359442160846,0.233867939052437,
391.379179949092));
#38780=CARTESIAN_POINT('Ctrl Pts',(-4.51803983860459,0.116987923926286,
391.3832983233));
#38781=CARTESIAN_POINT('Ctrl Pts',(-4.51792755410097,9.93894350090341E-5,
391.387416697508));
#38782=CARTESIAN_POINT('Origin',(0.,0.,387.));
#38783=CARTESIAN_POINT('',(-4.51781275651133,-0.000112770352403077,392.387416697508));
#38784=CARTESIAN_POINT('',(-4.51767617872592,0.000114137193723671,392.112583302492));
#38785=CARTESIAN_POINT('',(-4.51775,5.53264807684796E-16,387.));
#38786=CARTESIAN_POINT('Ctrl Pts',(-4.51767617872592,0.000114137193723671,
392.112583302492));
#38787=CARTESIAN_POINT('Ctrl Pts',(-4.5178695555558,0.198463769522385,392.105595901432));
#38788=CARTESIAN_POINT('Ctrl Pts',(-4.5050469141142,0.396788584023774,392.098608500372));
#38789=CARTESIAN_POINT('Ctrl Pts',(-4.47900555811224,0.593362231693622,
392.091621099312));
#38790=CARTESIAN_POINT('Ctrl Pts',(-4.38070495693752,1.33538610094233,392.065245140825));
#38791=CARTESIAN_POINT('Ctrl Pts',(-4.0940505572316,2.05245754966054,392.038869182339));
#38792=CARTESIAN_POINT('Ctrl Pts',(-3.65374663667568,2.65776316525419,392.012493223852));
#38793=CARTESIAN_POINT('Ctrl Pts',(-3.21344271611974,3.26306878084786,391.986117265366));
#38794=CARTESIAN_POINT('Ctrl Pts',(-2.61948927471379,3.75660856331697,391.959741306879));
#38795=CARTESIAN_POINT('Ctrl Pts',(-1.94379424473237,4.07863132211605,391.933365348393));
#38796=CARTESIAN_POINT('Ctrl Pts',(-1.26809921475095,4.40065408091513,391.906989389906));
#38797=CARTESIAN_POINT('Ctrl Pts',(-0.510662596194056,4.55115981604418,
391.88061343142));
#38798=CARTESIAN_POINT('Ctrl Pts',(0.236815323891349,4.51192730770023,391.854237472933));
#38799=CARTESIAN_POINT('Ctrl Pts',(0.984293243976733,4.47269479935628,391.827861514446));
#38800=CARTESIAN_POINT('Ctrl Pts',(1.72181246559064,4.24372404753933,391.80148555596));
#38801=CARTESIAN_POINT('Ctrl Pts',(2.36008403350207,3.85273576597324,391.775109597473));
#38802=CARTESIAN_POINT('Ctrl Pts',(2.99835560141351,3.46174748440714,391.748733638986));
#38803=CARTESIAN_POINT('Ctrl Pts',(3.53737951562248,2.90874167309189,391.7223576805));
#38804=CARTESIAN_POINT('Ctrl Pts',(3.9118979757439,2.2606688733584,391.695981722013));
#38805=CARTESIAN_POINT('Ctrl Pts',(4.28641643586534,1.6125960736249,391.669605763527));
#38806=CARTESIAN_POINT('Ctrl Pts',(4.49642944189922,0.869456285473188,391.64322980504));
#38807=CARTESIAN_POINT('Ctrl Pts',(4.51651143022073,0.121218927096046,391.616853846553));
#38808=CARTESIAN_POINT('Ctrl Pts',(4.53659341854224,-0.627018431281127,
391.590477888067));
#38809=CARTESIAN_POINT('Ctrl Pts',(4.36674438915135,-1.3803533598837,391.56410192958));
#38810=CARTESIAN_POINT('Ctrl Pts',(4.02752738899906,-2.04758214938088,391.537725971094));
#38811=CARTESIAN_POINT('Ctrl Pts',(3.68831038884679,-2.71481093887802,391.511350012607));
#38812=CARTESIAN_POINT('Ctrl Pts',(3.17972541793314,-3.29593358926979,391.48497405412));
#38813=CARTESIAN_POINT('Ctrl Pts',(2.56334513683187,-3.72059554871007,391.458598095634));
#38814=CARTESIAN_POINT('Ctrl Pts',(1.94696485573061,-4.14525750815035,391.432222137147));
#38815=CARTESIAN_POINT('Ctrl Pts',(1.22278926444172,-4.41345877663913,391.405846178661));
#38816=CARTESIAN_POINT('Ctrl Pts',(0.478491850048684,-4.49272913461715,
391.379470220174));
#38817=CARTESIAN_POINT('Ctrl Pts',(-0.265805564344378,-4.57199949259517,
391.353094261688));
#38818=CARTESIAN_POINT('Ctrl Pts',(-1.03022480184161,-4.46233894006242,
391.326718303201));
#38819=CARTESIAN_POINT('Ctrl Pts',(-1.72222021336115,-4.17702370884953,
391.300342344714));
#38820=CARTESIAN_POINT('Ctrl Pts',(-2.41421562488067,-3.89170847763665,
391.273966386228));
#38821=CARTESIAN_POINT('Ctrl Pts',(-3.03378721042251,-3.43073856774365,
391.247590427741));
#38822=CARTESIAN_POINT('Ctrl Pts',(-3.50592553573386,-2.84992204551108,
391.221214469255));
#38823=CARTESIAN_POINT('Ctrl Pts',(-3.97806386104521,-2.26910552327851,
391.194838510768));
#38824=CARTESIAN_POINT('Ctrl Pts',(-4.30276892612607,-1.56844238870636,
391.168462552281));
#38825=CARTESIAN_POINT('Ctrl Pts',(-4.44072978806182,-0.83275955534669,
391.142086593795));
#38826=CARTESIAN_POINT('Ctrl Pts',(-4.4921693025746,-0.558455906816085,
391.13225216336));
#38827=CARTESIAN_POINT('Ctrl Pts',(-4.51764736060392,-0.279283767746957,
391.122417732926));
#38828=CARTESIAN_POINT('Ctrl Pts',(-4.51747010126728,-7.96701847477171E-5,
391.112583302492));
#38829=CARTESIAN_POINT('Ctrl Pts',(-4.51792755410097,9.93894350090341E-5,
391.387416697508));
#38830=CARTESIAN_POINT('Ctrl Pts',(-4.51732071711229,-0.631619894993005,
391.409674281787));
#38831=CARTESIAN_POINT('Ctrl Pts',(-4.38359173091614,-1.26358801454013,
391.431931866065));
#38832=CARTESIAN_POINT('Ctrl Pts',(-4.12629845673798,-1.84044304971073,
391.454189450344));
#38833=CARTESIAN_POINT('Ctrl Pts',(-3.82139759087395,-2.52403495573063,
391.48056540883));
#38834=CARTESIAN_POINT('Ctrl Pts',(-3.34297517472017,-3.13023145893271,
391.506941367317));
#38835=CARTESIAN_POINT('Ctrl Pts',(-2.74895219046335,-3.58564240100063,
391.533317325804));
#38836=CARTESIAN_POINT('Ctrl Pts',(-2.15492920620652,-4.04105334306855,
391.55969328429));
#38837=CARTESIAN_POINT('Ctrl Pts',(-1.44530565384664,-4.34567872400231,
391.586069242777));
#38838=CARTESIAN_POINT('Ctrl Pts',(-0.705993254381129,-4.46263858026562,
391.612445201263));
#38839=CARTESIAN_POINT('Ctrl Pts',(0.0333191450843864,-4.57959843652893,
391.63882115975));
#38840=CARTESIAN_POINT('Ctrl Pts',(0.802320391655539,-4.5088927681218,391.665197118237));
#38841=CARTESIAN_POINT('Ctrl Pts',(1.50791010792466,-4.25908167093864,391.691573076723));
#38842=CARTESIAN_POINT('Ctrl Pts',(2.21349982419377,-4.00927057375548,391.71794903521));
#38843=CARTESIAN_POINT('Ctrl Pts',(2.85567801016084,-3.58035404779628,391.744324993696));
#38844=CARTESIAN_POINT('Ctrl Pts',(3.35669832699602,-3.02425956472802,391.770700952183));
#38845=CARTESIAN_POINT('Ctrl Pts',(3.85771864383119,-2.46816508165977,391.79707691067));
#38846=CARTESIAN_POINT('Ctrl Pts',(4.21758109153447,-1.78489264148247,391.823452869156));
#38847=CARTESIAN_POINT('Ctrl Pts',(4.39271834190528,-1.05716372525534,391.849828827643));
#38848=CARTESIAN_POINT('Ctrl Pts',(4.56785559227609,-0.329434809028198,
391.876204786129));
#38849=CARTESIAN_POINT('Ctrl Pts',(4.55826764531442,0.442750583248765,391.902580744616));
#38850=CARTESIAN_POINT('Ctrl Pts',(4.36511528129817,1.16590658042746,391.928956703102));
#38851=CARTESIAN_POINT('Ctrl Pts',(4.17196291728192,1.88906257760614,391.955332661589));
#38852=CARTESIAN_POINT('Ctrl Pts',(3.79524613621108,2.56318917968655,391.981708620076));
#38853=CARTESIAN_POINT('Ctrl Pts',(3.28057276336538,3.10667216126389,392.008084578562));
#38854=CARTESIAN_POINT('Ctrl Pts',(2.76589939051967,3.65015514284124,392.034460537049));
#38855=CARTESIAN_POINT('Ctrl Pts',(2.11326942589908,4.0629945039155,392.060836495535));
#38856=CARTESIAN_POINT('Ctrl Pts',(1.40169456978973,4.29520918074182,392.087212454022));
#38857=CARTESIAN_POINT('Ctrl Pts',(0.690119713680387,4.52742385756813,392.113588412509));
#38858=CARTESIAN_POINT('Ctrl Pts',(-0.0804000339177079,4.57901385014649,
392.139964370995));
#38859=CARTESIAN_POINT('Ctrl Pts',(-0.816580455818562,4.44373333273746,
392.166340329482));
#38860=CARTESIAN_POINT('Ctrl Pts',(-1.55276087771942,4.30845281532842,392.192716287968));
#38861=CARTESIAN_POINT('Ctrl Pts',(-2.25460197392303,3.98630178793199,392.219092246455));
#38862=CARTESIAN_POINT('Ctrl Pts',(-2.83713421905071,3.51628198476719,392.245468204942));
#38863=CARTESIAN_POINT('Ctrl Pts',(-3.4196664641784,3.0462621816024,392.271844163428));
#38864=CARTESIAN_POINT('Ctrl Pts',(-3.88288985823016,2.42837360266924,392.298220121915));
#38865=CARTESIAN_POINT('Ctrl Pts',(-4.17072351316767,1.73742192630838,392.324596080401));
#38866=CARTESIAN_POINT('Ctrl Pts',(-4.3992382776818,1.18886668648237,392.345536286104));
#38867=CARTESIAN_POINT('Ctrl Pts',(-4.51720537865769,0.59425998006379,392.366476491806));
#38868=CARTESIAN_POINT('Ctrl Pts',(-4.51781275651133,-0.000112770352403077,
392.387416697508));
#38869=CARTESIAN_POINT('Origin',(0.,0.,387.));
#38870=CARTESIAN_POINT('',(-4.51740214664894,4.58334405226135E-5,393.387416697508));
#38871=CARTESIAN_POINT('',(-4.51804470017939,-7.02313581118758E-5,393.112583302492));
#38872=CARTESIAN_POINT('',(-4.51775,5.53264807684796E-16,387.));
#38873=CARTESIAN_POINT('Ctrl Pts',(-4.51804470017939,-7.02313581118758E-5,
393.112583302492));
#38874=CARTESIAN_POINT('Ctrl Pts',(-4.51753951069973,0.675637543377085,
393.088774069938));
#38875=CARTESIAN_POINT('Ctrl Pts',(-4.36387000533556,1.351567384844,393.064964837384));
#38876=CARTESIAN_POINT('Ctrl Pts',(-4.07071229568028,1.96032419089247,393.04115560483));
#38877=CARTESIAN_POINT('Ctrl Pts',(-3.74595106860983,2.63470729871608,393.014779646343));
#38878=CARTESIAN_POINT('Ctrl Pts',(-3.25000583346633,3.2266536908633,392.988403687856));
#38879=CARTESIAN_POINT('Ctrl Pts',(-2.64291900080672,3.66449842171826,392.96202772937));
#38880=CARTESIAN_POINT('Ctrl Pts',(-2.03583216814709,4.10234315257323,392.935651770883));
#38881=CARTESIAN_POINT('Ctrl Pts',(-1.31760373797134,4.38608622213596,392.909275812397));
#38882=CARTESIAN_POINT('Ctrl Pts',(-0.575187194701503,4.48137581760917,
392.88289985391));
#38883=CARTESIAN_POINT('Ctrl Pts',(0.167229348568301,4.57666541308236,392.856523895423));
#38884=CARTESIAN_POINT('Ctrl Pts',(0.933834004932164,4.48350153446603,392.830147936937));
#38885=CARTESIAN_POINT('Ctrl Pts',(1.63181654404497,4.21316321713056,392.80377197845));
#38886=CARTESIAN_POINT('Ctrl Pts',(2.32979908315777,3.94282489979509,392.777396019963));
#38887=CARTESIAN_POINT('Ctrl Pts',(2.95915950501951,3.49531214374047,392.751020061477));
#38888=CARTESIAN_POINT('Ctrl Pts',(3.44370327410501,2.92480380325231,392.72464410299));
#38889=CARTESIAN_POINT('Ctrl Pts',(3.92824704319053,2.35429546276414,392.698268144504));
#38890=CARTESIAN_POINT('Ctrl Pts',(4.26797415949979,1.66079153784243,392.671892186017));
#38891=CARTESIAN_POINT('Ctrl Pts',(4.42175501123433,0.928252200764915,392.64551622753));
#38892=CARTESIAN_POINT('Ctrl Pts',(4.57553586296886,0.195712863687411,392.619140269044));
#38893=CARTESIAN_POINT('Ctrl Pts',(4.54337045012868,-0.575861885545891,
392.592764310557));
#38894=CARTESIAN_POINT('Ctrl Pts',(4.32915293034778,-1.29306010427281,392.566388352071));
#38895=CARTESIAN_POINT('Ctrl Pts',(4.11493541056688,-2.01025832299973,392.540012393584));
#38896=CARTESIAN_POINT('Ctrl Pts',(3.71866578384527,-2.67308001122027,392.513636435098));
#38897=CARTESIAN_POINT('Ctrl Pts',(3.18831907228789,-3.20127959117695,392.487260476611));
#38898=CARTESIAN_POINT('Ctrl Pts',(2.65797236073051,-3.72947917113363,392.460884518124));
#38899=CARTESIAN_POINT('Ctrl Pts',(1.99354856433737,-4.12305664282645,392.434508559638));
#38900=CARTESIAN_POINT('Ctrl Pts',(1.27548722267832,-4.33436291424531,392.408132601151));
#38901=CARTESIAN_POINT('Ctrl Pts',(0.557425881019256,-4.54566918566418,
392.381756642665));
#38902=CARTESIAN_POINT('Ctrl Pts',(-0.214273005905716,-4.57470425680908,
392.355380684178));
#38903=CARTESIAN_POINT('Ctrl Pts',(-0.946182466504358,-4.41795294991702,
392.329004725691));
#38904=CARTESIAN_POINT('Ctrl Pts',(-1.678091927103,-4.26120164302497,392.302628767205));
#38905=CARTESIAN_POINT('Ctrl Pts',(-2.37021196137532,-3.91866395809597,
392.276252808718));
#38906=CARTESIAN_POINT('Ctrl Pts',(-2.93874993999921,-3.43180977295588,
392.249876850232));
#38907=CARTESIAN_POINT('Ctrl Pts',(-3.50728791862308,-2.9449555878158,392.223500891745));
#38908=CARTESIAN_POINT('Ctrl Pts',(-3.95224384159854,-2.31378490246464,
392.197124933258));
#38909=CARTESIAN_POINT('Ctrl Pts',(-4.21974840176451,-1.61471141489946,
392.170748974772));
#38910=CARTESIAN_POINT('Ctrl Pts',(-4.41638684920909,-1.1008333518145,392.151360417345));
#38911=CARTESIAN_POINT('Ctrl Pts',(-4.51713959899635,-0.550264065511563,
392.131971859919));
#38912=CARTESIAN_POINT('Ctrl Pts',(-4.51767617872592,0.000114137193723671,
392.112583302492));
#38913=CARTESIAN_POINT('Ctrl Pts',(-4.51781275651133,-0.000112770352403077,
392.387416697508));
#38914=CARTESIAN_POINT('Ctrl Pts',(-4.51797042238654,-0.154402722371687,
392.392852450292));
#38915=CARTESIAN_POINT('Ctrl Pts',(-4.51021990758361,-0.308676909473601,
392.398288203077));
#38916=CARTESIAN_POINT('Ctrl Pts',(-4.49444205643657,-0.462125713027313,
392.403723955861));
#38917=CARTESIAN_POINT('Ctrl Pts',(-4.41788302894468,-1.20670690221361,
392.430099914348));
#38918=CARTESIAN_POINT('Ctrl Pts',(-4.15232105813761,-1.93185450679764,
392.456475872834));
#38919=CARTESIAN_POINT('Ctrl Pts',(-3.72990683273987,-2.54977736133712,
392.482851831321));
#38920=CARTESIAN_POINT('Ctrl Pts',(-3.30749260734213,-3.16770021587658,
392.509227789807));
#38921=CARTESIAN_POINT('Ctrl Pts',(-2.72822612735372,-3.67839832037151,
392.535603748294));
#38922=CARTESIAN_POINT('Ctrl Pts',(-2.06223722435424,-4.02004318431961,
392.561979706781));
#38923=CARTESIAN_POINT('Ctrl Pts',(-1.39624832135474,-4.36168804826772,
392.588355665267));
#38924=CARTESIAN_POINT('Ctrl Pts',(-0.643536995344169,-4.53427967166901,
392.614731623754));
#38925=CARTESIAN_POINT('Ctrl Pts',(0.10476854180126,-4.5169229710009,392.64110758224));
#38926=CARTESIAN_POINT('Ctrl Pts',(0.853074078946657,-4.4995662703328,392.667483540727));
#38927=CARTESIAN_POINT('Ctrl Pts',(1.59697382722691,-4.29226124559533,392.693859499214));
#38928=CARTESIAN_POINT('Ctrl Pts',(2.24640636264933,-3.92010561428585,392.7202354577));
#38929=CARTESIAN_POINT('Ctrl Pts',(2.89583889807178,-3.54794998297635,392.746611416187));
#38930=CARTESIAN_POINT('Ctrl Pts',(3.45080422063637,-3.01094374509482,392.772987374673));
#38931=CARTESIAN_POINT('Ctrl Pts',(3.84411455761933,-2.37410042778438,392.79936333316));
#38932=CARTESIAN_POINT('Ctrl Pts',(4.23742489460227,-1.73725711047397,392.825739291647));
#38933=CARTESIAN_POINT('Ctrl Pts',(4.46908024600357,-1.00057671373466,392.852115250133));
#38934=CARTESIAN_POINT('Ctrl Pts',(4.51103488271665,-0.253246639109774,
392.87849120862));
#38935=CARTESIAN_POINT('Ctrl Pts',(4.55298951942973,0.494083435515108,392.904867167106));
#38936=CARTESIAN_POINT('Ctrl Pts',(4.40524344145459,1.25206318802556,392.931243125593));
#38937=CARTESIAN_POINT('Ctrl Pts',(4.0856837662456,1.92892657598571,392.95761908408));
#38938=CARTESIAN_POINT('Ctrl Pts',(3.76612409103661,2.60578996394588,392.983995042566));
#38939=CARTESIAN_POINT('Ctrl Pts',(3.27475081859377,3.20153698735573,393.010371001053));
#38940=CARTESIAN_POINT('Ctrl Pts',(2.67105284742856,3.64404257103983,393.03674695954));
#38941=CARTESIAN_POINT('Ctrl Pts',(2.06735487626337,4.08654815472391,393.063122918026));
#38942=CARTESIAN_POINT('Ctrl Pts',(1.35133220637582,4.37581229868225,393.089498876512));
#38943=CARTESIAN_POINT('Ctrl Pts',(0.60967127825766,4.4768147723325,393.115874834999));
#38944=CARTESIAN_POINT('Ctrl Pts',(-0.131989649860521,4.57781724598275,
393.142250793486));
#38945=CARTESIAN_POINT('Ctrl Pts',(-0.89928883620931,4.49055804932491,393.168626751973));
#38946=CARTESIAN_POINT('Ctrl Pts',(-1.5993319660497,4.2256013578754,393.195002710459));
#38947=CARTESIAN_POINT('Ctrl Pts',(-2.29937509589006,3.9606446664259,393.221378668946));
#38948=CARTESIAN_POINT('Ctrl Pts',(-2.93216216922203,3.51799048018475,393.247754627432));
#38949=CARTESIAN_POINT('Ctrl Pts',(-3.42108379742811,2.95122944283932,393.274130585919));
#38950=CARTESIAN_POINT('Ctrl Pts',(-3.91000542563421,2.38446840549387,393.300506544405));
#38951=CARTESIAN_POINT('Ctrl Pts',(-4.25506160871441,1.69360051704413,393.326882502892));
#38952=CARTESIAN_POINT('Ctrl Pts',(-4.41447756279827,0.962266813756684,
393.353258461379));
#38953=CARTESIAN_POINT('Ctrl Pts',(-4.4832948761755,0.646561770734553,393.364644540088));
#38954=CARTESIAN_POINT('Ctrl Pts',(-4.51751793652066,0.323315880315216,
393.376030618798));
#38955=CARTESIAN_POINT('Ctrl Pts',(-4.51740214664894,4.58334405226135E-5,
393.387416697508));
#38956=CARTESIAN_POINT('Origin',(0.,0.,387.));
#38957=CARTESIAN_POINT('',(-4.51808751818987,5.21912322906659E-5,394.387416697508));
#38958=CARTESIAN_POINT('',(-4.5173836733729,-2.76243915998559E-5,394.112583302492));
#38959=CARTESIAN_POINT('',(-4.51775,5.53264807684796E-16,387.));
#38960=CARTESIAN_POINT('Ctrl Pts',(-4.5173836733729,-2.76243915998559E-5,
394.112583302492));
#38961=CARTESIAN_POINT('Ctrl Pts',(-4.51729674156455,0.40470368583773,394.09832819693));
#38962=CARTESIAN_POINT('Ctrl Pts',(-4.46340651421681,0.809457698610517,
394.084073091368));
#38963=CARTESIAN_POINT('Ctrl Pts',(-4.35600985269673,1.19947809100869,394.069817985807));
#38964=CARTESIAN_POINT('Ctrl Pts',(-4.15729579382325,1.92112561822137,394.04344202732));
#38965=CARTESIAN_POINT('Ctrl Pts',(-3.77540022477979,2.59233198125928,394.017066068833));
#38966=CARTESIAN_POINT('Ctrl Pts',(-3.2565579491727,3.13183649817179,393.990690110347));
#38967=CARTESIAN_POINT('Ctrl Pts',(-2.7377156735656,3.6713410150843,393.96431415186));
#38968=CARTESIAN_POINT('Ctrl Pts',(-2.08192669139488,4.0791436858714,393.937938193374));
#38969=CARTESIAN_POINT('Ctrl Pts',(-1.36858515450633,4.30587322182919,393.911562234887));
#38970=CARTESIAN_POINT('Ctrl Pts',(-0.655243617617784,4.53260275778698,
393.885186276401));
#38971=CARTESIAN_POINT('Ctrl Pts',(0.115650473988585,4.57825915891545,393.858810317914));
#38972=CARTESIAN_POINT('Ctrl Pts',(0.850767582565068,4.43731495930334,393.832434359427));
#38973=CARTESIAN_POINT('Ctrl Pts',(1.58588469114154,4.29637075969123,393.806058400941));
#38974=CARTESIAN_POINT('Ctrl Pts',(2.28522481668813,3.96882595933856,393.779682442454));
#38975=CARTESIAN_POINT('Ctrl Pts',(2.86412121787636,3.49433529829511,393.753306483967));
#38976=CARTESIAN_POINT('Ctrl Pts',(3.44301761906461,3.01984463725166,393.726930525481));
#38977=CARTESIAN_POINT('Ctrl Pts',(3.9014702958945,2.39840811551743,393.700554566994));
#38978=CARTESIAN_POINT('Ctrl Pts',(4.18397593491012,1.70526094885616,393.674178608508));
#38979=CARTESIAN_POINT('Ctrl Pts',(4.46648157392573,1.0121137821949,393.647802650021));
#38980=CARTESIAN_POINT('Ctrl Pts',(4.57304017512708,0.247255970606617,393.621426691535));
#38981=CARTESIAN_POINT('Ctrl Pts',(4.49075104942932,-0.496713740146479,
393.595050733048));
#38982=CARTESIAN_POINT('Ctrl Pts',(4.40846192373155,-1.24068345089957,393.568674774561));
#38983=CARTESIAN_POINT('Ctrl Pts',(4.13732507113467,-1.96376506081748,393.542298816075));
#38984=CARTESIAN_POINT('Ctrl Pts',(3.71016611242726,-2.57841752743756,393.515922857588));
#38985=CARTESIAN_POINT('Ctrl Pts',(3.28300715371985,-3.19306999405764,393.489546899101));
#38986=CARTESIAN_POINT('Ctrl Pts',(2.69982608890194,-3.69929331737988,393.463170940615));
#38987=CARTESIAN_POINT('Ctrl Pts',(2.03122667508525,-4.03580075350889,393.436794982129));
#38988=CARTESIAN_POINT('Ctrl Pts',(1.36262726126856,-4.37230818963791,393.410419023642));
#38989=CARTESIAN_POINT('Ctrl Pts',(0.60860949845307,-4.53909973857368,393.384043065155));
#38990=CARTESIAN_POINT('Ctrl Pts',(-0.139540235604001,-4.51598251217256,
393.357667106668));
#38991=CARTESIAN_POINT('Ctrl Pts',(-0.887689969661061,-4.49286528577144,
393.331291148182));
#38992=CARTESIAN_POINT('Ctrl Pts',(-1.62997167495974,-4.27983928403344,
393.304915189695));
#38993=CARTESIAN_POINT('Ctrl Pts',(-2.2765198184931,-3.90269484377256,393.278539231209));
#38994=CARTESIAN_POINT('Ctrl Pts',(-2.92306796202647,-3.52555040351167,
393.252163272722));
#38995=CARTESIAN_POINT('Ctrl Pts',(-3.47388254379453,-2.9842875247279,393.225787314236));
#38996=CARTESIAN_POINT('Ctrl Pts',(-3.86227830720905,-2.3444350716672,393.199411355749));
#38997=CARTESIAN_POINT('Ctrl Pts',(-4.25067407062357,-1.7045826186065,393.173035397262));
#38998=CARTESIAN_POINT('Ctrl Pts',(-4.47665101568456,-0.966140591268864,
393.146659438776));
#38999=CARTESIAN_POINT('Ctrl Pts',(-4.51285087871635,-0.218509665850027,
393.120283480289));
#39000=CARTESIAN_POINT('Ctrl Pts',(-4.51637359912257,-0.145755392857762,
393.117716754357));
#39001=CARTESIAN_POINT('Ctrl Pts',(-4.51809916152901,-0.0729141025000744,
393.115150028424));
#39002=CARTESIAN_POINT('Ctrl Pts',(-4.51804470017939,-7.02313581118758E-5,
393.112583302492));
#39003=CARTESIAN_POINT('Ctrl Pts',(-4.51740214664894,4.58334405226135E-5,
393.387416697508));
#39004=CARTESIAN_POINT('Ctrl Pts',(-4.51724970819312,-0.425542225591553,
393.402406577285));
#39005=CARTESIAN_POINT('Ctrl Pts',(-4.4575812765459,-0.851172152520294,
393.417396457061));
#39006=CARTESIAN_POINT('Ctrl Pts',(-4.33897962224013,-1.25969258594773,
393.432386336838));
#39007=CARTESIAN_POINT('Ctrl Pts',(-4.13029000251061,-1.97851876423963,
393.458762295325));
#39008=CARTESIAN_POINT('Ctrl Pts',(-3.73913503796403,-2.64437160269829,
393.485138253812));
#39009=CARTESIAN_POINT('Ctrl Pts',(-3.21287053587191,-3.1766385524691,393.511514212298));
#39010=CARTESIAN_POINT('Ctrl Pts',(-2.68660603377979,-3.7089055022399,393.537890170785));
#39011=CARTESIAN_POINT('Ctrl Pts',(-2.02523199414213,-4.10758656332286,
393.564266129271));
#39012=CARTESIAN_POINT('Ctrl Pts',(-1.3088187328036,-4.324414769419,393.590642087758));
#39013=CARTESIAN_POINT('Ctrl Pts',(-0.592405471465078,-4.54124297551514,
393.617018046244));
#39014=CARTESIAN_POINT('Ctrl Pts',(0.179047011574318,-4.57621832662447,
393.643394004731));
#39015=CARTESIAN_POINT('Ctrl Pts',(0.912141576006553,-4.42510647540001,
393.669769963218));
#39016=CARTESIAN_POINT('Ctrl Pts',(1.6452361404388,-4.27399462417554,393.696145921704));
#39017=CARTESIAN_POINT('Ctrl Pts',(2.33997278626389,-3.93679557061728,393.722521880191));
#39018=CARTESIAN_POINT('Ctrl Pts',(2.91224209985778,-3.45433286252538,393.748897838677));
#39019=CARTESIAN_POINT('Ctrl Pts',(3.48451141345166,-2.97187015443348,393.775273797164));
#39020=CARTESIAN_POINT('Ctrl Pts',(3.93431339481433,-2.34414379180799,393.801649755651));
#39021=CARTESIAN_POINT('Ctrl Pts',(4.20719204090252,-1.64715048015453,393.828025714137));
#39022=CARTESIAN_POINT('Ctrl Pts',(4.48007068699071,-0.950157168501087,
393.854401672624));
#39023=CARTESIAN_POINT('Ctrl Pts',(4.5760259978044,-0.183896907819673,393.88077763111));
#39024=CARTESIAN_POINT('Ctrl Pts',(4.48344098872769,0.558861766363823,393.907153589597));
#39025=CARTESIAN_POINT('Ctrl Pts',(4.39085597965098,1.30162044054734,393.933529548083));
#39026=CARTESIAN_POINT('Ctrl Pts',(4.10973065068387,2.02087752823294,393.95990550657));
#39027=CARTESIAN_POINT('Ctrl Pts',(3.67409989363231,2.62955500891649,393.986281465057));
#39028=CARTESIAN_POINT('Ctrl Pts',(3.23846913658077,3.23823248960003,394.012657423543));
#39029=CARTESIAN_POINT('Ctrl Pts',(2.64833295144478,3.73633036328149,394.03903338203));
#39030=CARTESIAN_POINT('Ctrl Pts',(1.97513712820591,4.06354560674411,394.065409340517));
#39031=CARTESIAN_POINT('Ctrl Pts',(1.30194130496704,4.39076085020672,394.091785299003));
#39032=CARTESIAN_POINT('Ctrl Pts',(0.54568584362529,4.54709346345051,394.11816125749));
#39033=CARTESIAN_POINT('Ctrl Pts',(-0.202071967477526,4.51361678626648,
394.144537215976));
#39034=CARTESIAN_POINT('Ctrl Pts',(-0.949829778580352,4.48014010908246,
394.170913174463));
#39035=CARTESIAN_POINT('Ctrl Pts',(-1.68908993944425,4.25685414147062,394.19728913295));
#39036=CARTESIAN_POINT('Ctrl Pts',(-2.33035272521732,3.8707913595774,394.223665091436));
#39037=CARTESIAN_POINT('Ctrl Pts',(-2.97161551099039,3.48472857768417,394.250041049923));
#39038=CARTESIAN_POINT('Ctrl Pts',(-3.51488092167263,2.93588898150954,394.276417008409));
#39039=CARTESIAN_POINT('Ctrl Pts',(-3.89437765326087,2.29071872282242,394.302792966896));
#39040=CARTESIAN_POINT('Ctrl Pts',(-4.27387438484911,1.64554846413529,394.329168925382));
#39041=CARTESIAN_POINT('Ctrl Pts',(-4.48960243734335,0.904047542935649,
394.355544883869));
#39042=CARTESIAN_POINT('Ctrl Pts',(-4.51544434579255,0.15598696534298,394.381920842355));
#39043=CARTESIAN_POINT('Ctrl Pts',(-4.51723920487186,0.104030147904069,
394.383752794073));
#39044=CARTESIAN_POINT('Ctrl Pts',(-4.51811804423603,0.0520416863733224,
394.38558474579));
#39045=CARTESIAN_POINT('Ctrl Pts',(-4.51808751818987,5.21912322906659E-5,
394.387416697508));
#39046=CARTESIAN_POINT('Origin',(0.,0.,387.));
#39047=CARTESIAN_POINT('',(-4.51761539860092,-0.000109498206778275,395.387416697508));
#39048=CARTESIAN_POINT('',(-4.51787769339044,0.000106674156513836,395.112583302492));
#39049=CARTESIAN_POINT('',(-4.51775,5.53264807684796E-16,387.));
#39050=CARTESIAN_POINT('Ctrl Pts',(-4.51787769339044,0.000106674156513836,
395.112583302492));
#39051=CARTESIAN_POINT('Ctrl Pts',(-4.51801115526906,0.13353505519604,395.107882323922));
#39052=CARTESIAN_POINT('Ctrl Pts',(-4.51221712826522,0.266951885784635,
395.103181345353));
#39053=CARTESIAN_POINT('Ctrl Pts',(-4.50041129427044,0.39983460330973,395.098480366784));
#39054=CARTESIAN_POINT('Ctrl Pts',(-4.43417185438628,1.14540469882723,395.072104408297));
#39055=CARTESIAN_POINT('Ctrl Pts',(-4.17867844925679,1.87416071243738,395.04572844981));
#39056=CARTESIAN_POINT('Ctrl Pts',(-3.76486280044783,2.49787462083366,395.019352491324));
#39057=CARTESIAN_POINT('Ctrl Pts',(-3.35104715163886,3.12158852922995,394.992976532837));
#39058=CARTESIAN_POINT('Ctrl Pts',(-2.77890925915041,3.64026033241238,394.966600574351));
#39059=CARTESIAN_POINT('Ctrl Pts',(-2.11771592060786,3.99109619117415,394.940224615864));
#39060=CARTESIAN_POINT('Ctrl Pts',(-1.45652258206532,4.34193204993591,394.913848657377));
#39061=CARTESIAN_POINT('Ctrl Pts',(-0.706273797468684,4.52493196427704,
394.887472698891));
#39062=CARTESIAN_POINT('Ctrl Pts',(0.0422003528576968,4.51794075412897,
394.861096740404));
#39063=CARTESIAN_POINT('Ctrl Pts',(0.790674503184078,4.51094954398091,394.834720781918));
#39064=CARTESIAN_POINT('Ctrl Pts',(1.5373740192402,4.31396720934364,394.808344823431));
#39065=CARTESIAN_POINT('Ctrl Pts',(2.19189851862757,3.9508417345724,394.781968864945));
#39066=CARTESIAN_POINT('Ctrl Pts',(2.84642301801496,3.58771625980115,394.755592906458));
#39067=CARTESIAN_POINT('Ctrl Pts',(3.4087725007336,3.05844764489591,394.729216947971));
#39068=CARTESIAN_POINT('Ctrl Pts',(3.81086521878951,2.4271126491824,394.702840989485));
#39069=CARTESIAN_POINT('Ctrl Pts',(4.2129579368454,1.79577765346891,394.676465030998));
#39070=CARTESIAN_POINT('Ctrl Pts',(4.45479389023857,1.06237627694715,394.650089072511));
#39071=CARTESIAN_POINT('Ctrl Pts',(4.50709481884649,0.315698941284091,394.623713114025));
#39072=CARTESIAN_POINT('Ctrl Pts',(4.55939574745442,-0.430978394378985,
394.597337155538));
#39073=CARTESIAN_POINT('Ctrl Pts',(4.4221616512771,-1.19093168918336,394.570961197052));
#39074=CARTESIAN_POINT('Ctrl Pts',(4.11200699772181,-1.8721559706092,394.544585238565));
#39075=CARTESIAN_POINT('Ctrl Pts',(3.80185234416652,-2.55338025203503,394.518209280079));
#39076=CARTESIAN_POINT('Ctrl Pts',(3.31877713323327,-3.15587552008233,394.491833321592));
#39077=CARTESIAN_POINT('Ctrl Pts',(2.72126564522031,-3.60669971244412,394.465457363105));
#39078=CARTESIAN_POINT('Ctrl Pts',(2.12375415720733,-4.05752390480593,394.439081404619));
#39079=CARTESIAN_POINT('Ctrl Pts',(1.41180639211463,-4.35667702148223,394.412705446132));
#39080=CARTESIAN_POINT('Ctrl Pts',(0.67161545550637,-4.46794160744361,394.386329487646));
#39081=CARTESIAN_POINT('Ctrl Pts',(-0.0685754811018632,-4.57920619340499,
394.359953529159));
#39082=CARTESIAN_POINT('Ctrl Pts',(-0.837009589225651,-4.50258224865146,
394.333577570673));
#39083=CARTESIAN_POINT('Ctrl Pts',(-1.54065515298906,-4.2473463747579,394.307201612186));
#39084=CARTESIAN_POINT('Ctrl Pts',(-2.24430071675247,-3.99211050086433,
394.280825653699));
#39085=CARTESIAN_POINT('Ctrl Pts',(-2.88315773615551,-3.55826269783073,
394.254449695213));
#39086=CARTESIAN_POINT('Ctrl Pts',(-3.37988195476012,-2.99832745034422,
394.228073736726));
#39087=CARTESIAN_POINT('Ctrl Pts',(-3.87660617336475,-2.43839220285771,
394.20169777824));
#39088=CARTESIAN_POINT('Ctrl Pts',(-4.23119759117096,-1.75236951091828,
394.175321819753));
#39089=CARTESIAN_POINT('Ctrl Pts',(-4.40072702572232,-1.02331381925484,
394.148945861266));
#39090=CARTESIAN_POINT('Ctrl Pts',(-4.47863287106505,-0.688282323920289,
394.136825008341));
#39091=CARTESIAN_POINT('Ctrl Pts',(-4.51745758988365,-0.34416318088334,
394.124704155417));
#39092=CARTESIAN_POINT('Ctrl Pts',(-4.5173836733729,-2.76243915998559E-5,
394.112583302492));
#39093=CARTESIAN_POINT('Ctrl Pts',(-4.51808751818987,5.21912322906659E-5,
394.387416697508));
#39094=CARTESIAN_POINT('Ctrl Pts',(-4.51767853826069,-0.696489376170657,
394.411960704277));
#39095=CARTESIAN_POINT('Ctrl Pts',(-4.35403905930357,-1.39321647594668,
394.436504711046));
#39096=CARTESIAN_POINT('Ctrl Pts',(-4.0431719192238,-2.01651441971212,394.461048717815));
#39097=CARTESIAN_POINT('Ctrl Pts',(-3.70910181980172,-2.68633499318885,
394.487424676302));
#39098=CARTESIAN_POINT('Ctrl Pts',(-3.20500585655341,-3.27135590615661,
394.513800634789));
#39099=CARTESIAN_POINT('Ctrl Pts',(-2.59191322109249,-3.70075065731708,
394.540176593275));
#39100=CARTESIAN_POINT('Ctrl Pts',(-1.97882058563158,-4.13014540847754,
394.566552551762));
#39101=CARTESIAN_POINT('Ctrl Pts',(-1.25673127795806,-4.40391399783071,
394.592928510249));
#39102=CARTESIAN_POINT('Ctrl Pts',(-0.513066205861354,-4.48891218912888,
394.619304468735));
#39103=CARTESIAN_POINT('Ctrl Pts',(0.230598866235364,-4.57391038042705,
394.645680427222));
#39104=CARTESIAN_POINT('Ctrl Pts',(0.995839702755266,-4.47013817367021,
394.672056385708));
#39105=CARTESIAN_POINT('Ctrl Pts',(1.69001118640443,-4.19015891860138,394.698432344195));
#39106=CARTESIAN_POINT('Ctrl Pts',(2.3841826700536,-3.91017966353254,394.724808302681));
#39107=CARTESIAN_POINT('Ctrl Pts',(3.00728480083202,-3.45399336015171,394.751184261168));
#39108=CARTESIAN_POINT('Ctrl Pts',(3.48388071332803,-2.87682893975429,394.777560219655));
#39109=CARTESIAN_POINT('Ctrl Pts',(3.96047662582402,-2.29966451935688,394.803936178141));
#39110=CARTESIAN_POINT('Ctrl Pts',(4.29056632003761,-1.6015219819429,394.830312136628));
#39111=CARTESIAN_POINT('Ctrl Pts',(4.43418695423518,-0.866923080900132,
394.856688095114));
#39112=CARTESIAN_POINT('Ctrl Pts',(4.57780758843275,-0.132324179857343,
394.883064053601));
#39113=CARTESIAN_POINT('Ctrl Pts',(4.5349591626143,0.638731084814249,394.909440012088));
#39114=CARTESIAN_POINT('Ctrl Pts',(4.31082919062693,1.35289366268957,394.935815970574));
#39115=CARTESIAN_POINT('Ctrl Pts',(4.08669921863955,2.06705624056489,394.962191929061));
#39116=CARTESIAN_POINT('Ctrl Pts',(3.68128770048325,2.72432613164396,394.988567887547));
#39117=CARTESIAN_POINT('Ctrl Pts',(3.14367643610836,3.24512989545316,395.014943846034));
#39118=CARTESIAN_POINT('Ctrl Pts',(2.60606517173349,3.76593365926234,395.04131980452));
#39119=CARTESIAN_POINT('Ctrl Pts',(1.93625416114004,4.15027129580166,395.067695763007));
#39120=CARTESIAN_POINT('Ctrl Pts',(1.21533515568228,4.35161234862086,395.094071721494));
#39121=CARTESIAN_POINT('Ctrl Pts',(0.494416150224501,4.55295340144005,395.12044767998));
#39122=CARTESIAN_POINT('Ctrl Pts',(-0.277610850097608,4.57129787053912,
395.146823638467));
#39123=CARTESIAN_POINT('Ctrl Pts',(-1.00727915011366,4.40442485315088,395.173199596953));
#39124=CARTESIAN_POINT('Ctrl Pts',(-1.73694745012971,4.23755183576263,395.19957555544));
#39125=CARTESIAN_POINT('Ctrl Pts',(-2.42425704983972,3.88546133188709,395.225951513927));
#39126=CARTESIAN_POINT('Ctrl Pts',(-2.98599770294795,3.39077974679813,395.252327472413));
#39127=CARTESIAN_POINT('Ctrl Pts',(-3.54773835605617,2.89609816170917,395.2787034309));
#39128=CARTESIAN_POINT('Ctrl Pts',(-3.9839100625626,2.25882549540681,395.305079389386));
#39129=CARTESIAN_POINT('Ctrl Pts',(-4.24170699065442,1.55611419206311,395.331455347873));
#39130=CARTESIAN_POINT('Ctrl Pts',(-4.42402787244154,1.05913796579184,395.350109131085));
#39131=CARTESIAN_POINT('Ctrl Pts',(-4.5171311009058,0.529431318295306,395.368762914296));
#39132=CARTESIAN_POINT('Ctrl Pts',(-4.51761539860092,-0.000109498206778275,
395.387416697508));
#39133=CARTESIAN_POINT('Origin',(0.,0.,387.));
#39134=CARTESIAN_POINT('',(-4.51751463264715,9.2546932777271E-5,396.387416697508));
#39135=CARTESIAN_POINT('',(-4.51786437784292,-0.000108222965875699,396.112583302492));
#39136=CARTESIAN_POINT('',(-4.51775,5.53264807684796E-16,387.));
#39137=CARTESIAN_POINT('Ctrl Pts',(-4.51786437784292,-0.000108222965875699,
396.112583302492));
#39138=CARTESIAN_POINT('Ctrl Pts',(-4.5172490555957,0.610781207776803,396.091060492428));
#39139=CARTESIAN_POINT('Ctrl Pts',(-4.39244234778488,1.22191440722307,396.069537682365));
#39140=CARTESIAN_POINT('Ctrl Pts',(-4.15139232023937,1.78311842878099,396.048014872301));
#39141=CARTESIAN_POINT('Ctrl Pts',(-3.85598825818002,2.47086756243728,396.021638913814));
#39142=CARTESIAN_POINT('Ctrl Pts',(-3.38600738379809,3.0836319422382,395.995262955328));
#39143=CARTESIAN_POINT('Ctrl Pts',(-2.79834869039748,3.54722625928365,395.968886996841));
#39144=CARTESIAN_POINT('Ctrl Pts',(-2.21068999699688,4.0108205763291,395.942511038355));
#39145=CARTESIAN_POINT('Ctrl Pts',(-1.50535348457759,4.32524483061908,395.916135079868));
#39146=CARTESIAN_POINT('Ctrl Pts',(-0.767731856725531,4.45243274219494,
395.889759121381));
#39147=CARTESIAN_POINT('Ctrl Pts',(-0.0301102288734742,4.5796206537708,
395.863383162895));
#39148=CARTESIAN_POINT('Ctrl Pts',(0.739796514411352,4.51957222263255,395.837007204408));
#39149=CARTESIAN_POINT('Ctrl Pts',(1.44877837029978,4.27955730903937,395.810631245922));
#39150=CARTESIAN_POINT('Ctrl Pts',(2.15776022618821,4.03954239544619,395.784255287435));
#39151=CARTESIAN_POINT('Ctrl Pts',(2.80581719468025,3.61956099939807,395.757879328948));
#39152=CARTESIAN_POINT('Ctrl Pts',(3.31449121264882,3.07045884663426,395.731503370462));
#39153=CARTESIAN_POINT('Ctrl Pts',(3.82316523061738,2.52135669387044,395.705127411975));
#39154=CARTESIAN_POINT('Ctrl Pts',(4.19245629806247,1.84313378439093,395.678751453489));
#39155=CARTESIAN_POINT('Ctrl Pts',(4.37765559571272,1.11790026966896,395.652375495002));
#39156=CARTESIAN_POINT('Ctrl Pts',(4.56285489336297,0.392666754946975,395.625999536516));
#39157=CARTESIAN_POINT('Ctrl Pts',(4.56396242121836,-0.379577365017472,
395.599623578029));
#39158=CARTESIAN_POINT('Ctrl Pts',(4.38084409463107,-1.10533910911399,395.573247619542));
#39159=CARTESIAN_POINT('Ctrl Pts',(4.19772576804378,-1.8311008532105,395.546871661056));
#39160=CARTESIAN_POINT('Ctrl Pts',(3.8303815870138,-2.51038022143909,395.520495702569));
#39161=CARTESIAN_POINT('Ctrl Pts',(3.32328466786559,-3.06093916044248,395.494119744083));
#39162=CARTESIAN_POINT('Ctrl Pts',(2.81618774871737,-3.61149809944587,395.467743785596));
#39163=CARTESIAN_POINT('Ctrl Pts',(2.16933809145092,-4.03333660922406,395.441367827109));
#39164=CARTESIAN_POINT('Ctrl Pts',(1.46104759411067,-4.27538412956593,395.414991868623));
#39165=CARTESIAN_POINT('Ctrl Pts',(0.75275709677042,-4.5174316499078,395.388615910136));
#39166=CARTESIAN_POINT('Ctrl Pts',(-0.0169742406436262,-4.57968818081335,
395.36223995165));
#39167=CARTESIAN_POINT('Ctrl Pts',(-0.754957651097232,-4.45461653486027,
395.335863993163));
#39168=CARTESIAN_POINT('Ctrl Pts',(-1.49294106155083,-4.3295448889072,395.309488034676));
#39169=CARTESIAN_POINT('Ctrl Pts',(-2.19917654504398,-4.01714506609549,
395.28311207619));
#39170=CARTESIAN_POINT('Ctrl Pts',(-2.78816256260641,-3.5552382553186,395.256736117703));
#39171=CARTESIAN_POINT('Ctrl Pts',(-3.37714858016886,-3.0933314445417,395.230360159217));
#39172=CARTESIAN_POINT('Ctrl Pts',(-3.84888513180058,-2.4819176457996,395.20398420073));
#39173=CARTESIAN_POINT('Ctrl Pts',(-4.14626067029702,-1.79501865771611,
395.177608242243));
#39174=CARTESIAN_POINT('Ctrl Pts',(-4.39063506253172,-1.23054545461321,
395.155933262326));
#39175=CARTESIAN_POINT('Ctrl Pts',(-4.51726233565243,-0.615096615266284,
395.134258282409));
#39176=CARTESIAN_POINT('Ctrl Pts',(-4.51787769339044,0.000106674156513836,
395.112583302492));
#39177=CARTESIAN_POINT('Ctrl Pts',(-4.51761539860092,-0.000109498206778275,
395.387416697508));
#39178=CARTESIAN_POINT('Ctrl Pts',(-4.51781588509979,-0.219325458522322,
395.395138872783));
#39179=CARTESIAN_POINT('Ctrl Pts',(-4.5021438757463,-0.438512999682626,
395.402861048058));
#39180=CARTESIAN_POINT('Ctrl Pts',(-4.47035806891458,-0.655338316442091,
395.410583223333));
#39181=CARTESIAN_POINT('Ctrl Pts',(-4.36179006940572,-1.39592958121857,
395.436959181819));
#39182=CARTESIAN_POINT('Ctrl Pts',(-4.06523192071081,-2.10896217038649,
395.463335140306));
#39183=CARTESIAN_POINT('Ctrl Pts',(-3.61658691387121,-2.70811164240368,
395.489711098793));
#39184=CARTESIAN_POINT('Ctrl Pts',(-3.16794190703161,-3.30726111442086,
395.516087057279));
#39185=CARTESIAN_POINT('Ctrl Pts',(-2.56721004204732,-3.79252746928731,
395.542463015766));
#39186=CARTESIAN_POINT('Ctrl Pts',(-1.88711989198663,-4.10516115232706,
395.568838974252));
#39187=CARTESIAN_POINT('Ctrl Pts',(-1.20702974192593,-4.4177948353668,395.595214932739));
#39188=CARTESIAN_POINT('Ctrl Pts',(-0.447581306788832,-4.55779584657986,
395.621590891225));
#39189=CARTESIAN_POINT('Ctrl Pts',(0.299281562555524,-4.50821473752317,
395.647966849712));
#39190=CARTESIAN_POINT('Ctrl Pts',(1.04614443189988,-4.45863362846649,395.674342808199));
#39191=CARTESIAN_POINT('Ctrl Pts',(1.78042173545149,-4.21947039914007,395.700718766685));
#39192=CARTESIAN_POINT('Ctrl Pts',(2.4132170060234,-3.81967973201239,395.727094725172));
#39193=CARTESIAN_POINT('Ctrl Pts',(3.04601227659532,-3.41988906488471,395.753470683659));
#39194=CARTESIAN_POINT('Ctrl Pts',(3.57732551418753,-2.85947095995576,395.779846642145));
#39195=CARTESIAN_POINT('Ctrl Pts',(3.94283242392784,-2.20627333984937,395.806222600631));
#39196=CARTESIAN_POINT('Ctrl Pts',(4.30833933366816,-1.55307571974297,395.832598559118));
#39197=CARTESIAN_POINT('Ctrl Pts',(4.50803991555659,-0.807098584459129,
395.858974517605));
#39198=CARTESIAN_POINT('Ctrl Pts',(4.51775709624605,-0.0586548602019053,
395.885350476092));
#39199=CARTESIAN_POINT('Ctrl Pts',(4.5274742769355,0.689788864055318,395.911726434578));
#39200=CARTESIAN_POINT('Ctrl Pts',(4.34720805642599,1.44069917728592,395.938102393065));
#39201=CARTESIAN_POINT('Ctrl Pts',(3.99878265572902,2.10316591013349,395.964478351551));
#39202=CARTESIAN_POINT('Ctrl Pts',(3.65035725503204,2.76563264298105,395.990854310038));
#39203=CARTESIAN_POINT('Ctrl Pts',(3.13377267414759,3.33965579544558,396.017230268524));
#39204=CARTESIAN_POINT('Ctrl Pts',(2.5115700593453,3.75574032785908,396.043606227011));
#39205=CARTESIAN_POINT('Ctrl Pts',(1.88936744454301,4.17182486027259,396.069982185498));
#39206=CARTESIAN_POINT('Ctrl Pts',(1.16154679582287,4.42997077263507,396.096358143984));
#39207=CARTESIAN_POINT('Ctrl Pts',(0.416222895030907,4.49892521331027,396.122734102471));
#39208=CARTESIAN_POINT('Ctrl Pts',(-0.329101005761055,4.56787965398547,
396.149110060957));
#39209=CARTESIAN_POINT('Ctrl Pts',(-1.09192815862484,4.44764262297338,396.175486019444));
#39210=CARTESIAN_POINT('Ctrl Pts',(-1.77990566277504,4.15277081054664,396.201861977931));
#39211=CARTESIAN_POINT('Ctrl Pts',(-2.46788316692524,3.85789899811989,396.228237936417));
#39212=CARTESIAN_POINT('Ctrl Pts',(-3.08101102236186,3.38839240427848,396.254613894904));
#39213=CARTESIAN_POINT('Ctrl Pts',(-3.54505991542016,2.80109260278699,396.28098985339));
#39214=CARTESIAN_POINT('Ctrl Pts',(-4.00910880847846,2.2137928012955,396.307365811877));
#39215=CARTESIAN_POINT('Ctrl Pts',(-4.32407873915844,1.50869979215393,396.333741770364));
#39216=CARTESIAN_POINT('Ctrl Pts',(-4.45183736430835,0.771176798830757,
396.36011772885));
#39217=CARTESIAN_POINT('Ctrl Pts',(-4.4959138504198,0.516732749092945,396.369217385069));
#39218=CARTESIAN_POINT('Ctrl Pts',(-4.51770775311255,0.258428762447222,
396.378317041289));
#39219=CARTESIAN_POINT('Ctrl Pts',(-4.51751463264715,9.2546932777271E-5,
396.387416697508));
#39220=CARTESIAN_POINT('Origin',(0.,0.,387.));
#39221=CARTESIAN_POINT('',(-4.51813440218219,-1.34914224690988E-5,397.387416697508));
#39222=CARTESIAN_POINT('',(-4.51738673749921,3.14726202902737E-5,397.112583302492));
#39223=CARTESIAN_POINT('',(-4.51775,5.53264807684796E-16,387.));
#39224=CARTESIAN_POINT('Ctrl Pts',(-4.51738673749921,3.14726202902737E-5,
397.112583302492));
#39225=CARTESIAN_POINT('Ctrl Pts',(-4.51746996308395,0.339845959287686,
397.100614619421));
#39226=CARTESIAN_POINT('Ctrl Pts',(-4.47962267703118,0.67964219695818,397.088645936349));
#39227=CARTESIAN_POINT('Ctrl Pts',(-4.40364412455734,1.01068687131693,397.076677253278));
#39228=CARTESIAN_POINT('Ctrl Pts',(-4.236206559874,1.7402258302897,397.050301294792));
#39229=CARTESIAN_POINT('Ctrl Pts',(-3.88358434036526,2.42726278544303,397.023925336305));
#39230=CARTESIAN_POINT('Ctrl Pts',(-3.38846824431658,2.9886204986346,396.997549377818));
#39231=CARTESIAN_POINT('Ctrl Pts',(-2.89335214826789,3.54997821182617,396.971173419332));
#39232=CARTESIAN_POINT('Ctrl Pts',(-2.25574217567927,3.98565668305597,396.944797460845));
#39233=CARTESIAN_POINT('Ctrl Pts',(-1.55283160725287,4.24290979483623,396.918421502359));
#39234=CARTESIAN_POINT('Ctrl Pts',(-0.849921038826476,4.5001629066165,396.892045543872));
#39235=CARTESIAN_POINT('Ctrl Pts',(-0.0817098745623172,4.57899065894722,
396.865669585385));
#39236=CARTESIAN_POINT('Ctrl Pts',(0.658797160721962,4.46984964273134,396.839293626899));
#39237=CARTESIAN_POINT('Ctrl Pts',(1.39930419600623,4.36070862651545,396.812917668412));
#39238=CARTESIAN_POINT('Ctrl Pts',(2.11210710231061,4.06359884175296,396.786541709925));
#39239=CARTESIAN_POINT('Ctrl Pts',(2.71090924501961,3.61449036419631,396.760165751439));
#39240=CARTESIAN_POINT('Ctrl Pts',(3.30971138772862,3.16538188663966,396.733789792952));
#39241=CARTESIAN_POINT('Ctrl Pts',(3.79451276684224,2.56427471628884,396.707413834466));
#39242=CARTESIAN_POINT('Ctrl Pts',(4.10662012072468,1.88394286316225,396.681037875979));
#39243=CARTESIAN_POINT('Ctrl Pts',(4.41872747460713,1.20361101003566,396.654661917493));
#39244=CARTESIAN_POINT('Ctrl Pts',(4.5581408032584,0.444054474133294,396.628285959006));
#39245=CARTESIAN_POINT('Ctrl Pts',(4.50798180697358,-0.302769806282027,
396.601910000519));
#39246=CARTESIAN_POINT('Ctrl Pts',(4.45782281068875,-1.04959408669733,396.575534042033));
#39247=CARTESIAN_POINT('Ctrl Pts',(4.21809148946783,-1.78368611162558,396.549158083546));
#39248=CARTESIAN_POINT('Ctrl Pts',(3.81781130274164,-2.41617184493549,396.52278212506));
#39249=CARTESIAN_POINT('Ctrl Pts',(3.41753111601545,-3.0486575782454,396.496406166573));
#39250=CARTESIAN_POINT('Ctrl Pts',(2.85670206378398,-3.57953701993697,396.470030208087));
#39251=CARTESIAN_POINT('Ctrl Pts',(2.20322182066968,-3.94453839333905,396.4436542496));
#39252=CARTESIAN_POINT('Ctrl Pts',(1.54974157755536,-4.30953976674113,396.417278291113));
#39253=CARTESIAN_POINT('Ctrl Pts',(0.803610143558188,-4.50866307185371,
396.390902332627));
#39254=CARTESIAN_POINT('Ctrl Pts',(0.0551591253050773,-4.51780112427455,
396.36452637414));
#39255=CARTESIAN_POINT('Ctrl Pts',(-0.693291892948023,-4.52693917669538,
396.338150415653));
#39256=CARTESIAN_POINT('Ctrl Pts',(-1.44406249545706,-4.34609197642448,
396.311774457167));
#39257=CARTESIAN_POINT('Ctrl Pts',(-2.10625942716968,-3.9971540817261,396.28539849868));
#39258=CARTESIAN_POINT('Ctrl Pts',(-2.7684563588823,-3.64821618702772,396.259022540194));
#39259=CARTESIAN_POINT('Ctrl Pts',(-3.3420796197985,-3.13118759790186,396.232646581707));
#39260=CARTESIAN_POINT('Ctrl Pts',(-3.7576825837662,-2.5086632151927,396.206270623221));
#39261=CARTESIAN_POINT('Ctrl Pts',(-4.17328554773389,-1.88613883248355,
396.179894664734));
#39262=CARTESIAN_POINT('Ctrl Pts',(-4.43086821475307,-1.15811865619109,
396.153518706247));
#39263=CARTESIAN_POINT('Ctrl Pts',(-4.49924592339428,-0.412741624289035,
396.127142747761));
#39264=CARTESIAN_POINT('Ctrl Pts',(-4.51182734935556,-0.275593039955457,
396.122289599338));
#39265=CARTESIAN_POINT('Ctrl Pts',(-4.51800312599824,-0.137856828684076,
396.117436450915));
#39266=CARTESIAN_POINT('Ctrl Pts',(-4.51786437784292,-0.000108222965875699,
396.112583302492));
#39267=CARTESIAN_POINT('Ctrl Pts',(-4.51751463264715,9.2546932777271E-5,
396.387416697508));
#39268=CARTESIAN_POINT('Ctrl Pts',(-4.51714798060515,-0.490375932126388,
396.404692999775));
#39269=CARTESIAN_POINT('Ctrl Pts',(-4.43752790145426,-0.98096058190497,
396.421969302042));
#39270=CARTESIAN_POINT('Ctrl Pts',(-4.28067705789975,-1.44546653343395,
396.43924560431));
#39271=CARTESIAN_POINT('Ctrl Pts',(-4.04121080672139,-2.1546338948707,396.465621562796));
#39272=CARTESIAN_POINT('Ctrl Pts',(-3.62173098474482,-2.80301564023941,
396.491997521283));
#39273=CARTESIAN_POINT('Ctrl Pts',(-3.07302259383454,-3.3121143867761,396.51837347977));
#39274=CARTESIAN_POINT('Ctrl Pts',(-2.52431420292427,-3.8212131333128,396.544749438256));
#39275=CARTESIAN_POINT('Ctrl Pts',(-1.84637724308029,-4.19102888101748,
396.571125396743));
#39276=CARTESIAN_POINT('Ctrl Pts',(-1.12128724682158,-4.37678928935608,
396.597501355229));
#39277=CARTESIAN_POINT('Ctrl Pts',(-0.396197250562878,-4.56254969769468,
396.623877313716));
#39278=CARTESIAN_POINT('Ctrl Pts',(0.376045782110559,-4.5642547666672,396.650253272203));
#39279=CARTESIAN_POINT('Ctrl Pts',(1.10194900172297,-4.38169806934578,396.676629230689));
#39280=CARTESIAN_POINT('Ctrl Pts',(1.82785222133539,-4.19914137202436,396.703005189176));
#39281=CARTESIAN_POINT('Ctrl Pts',(2.50741562788679,-3.83232290840901,396.729381147662));
#39282=CARTESIAN_POINT('Ctrl Pts',(3.05836678046179,-3.32565214799663,396.755757106149));
#39283=CARTESIAN_POINT('Ctrl Pts',(3.60931793303678,-2.81898138758426,396.782133064635));
#39284=CARTESIAN_POINT('Ctrl Pts',(4.03165683163537,-2.17245833037488,396.808509023122));
#39285=CARTESIAN_POINT('Ctrl Pts',(4.27425233566608,-1.46435533404973,396.834884981609));
#39286=CARTESIAN_POINT('Ctrl Pts',(4.51684783969678,-0.756252337724576,
396.861260940095));
#39287=CARTESIAN_POINT('Ctrl Pts',(4.57969994915959,0.0134305977163408,
396.887636898582));
#39288=CARTESIAN_POINT('Ctrl Pts',(4.45519937195264,0.751510565101793,396.914012857069));
#39289=CARTESIAN_POINT('Ctrl Pts',(4.33069879474569,1.48959053248724,396.940388815555));
#39290=CARTESIAN_POINT('Ctrl Pts',(4.01884553086897,2.19606753181724,396.966764774042));
#39291=CARTESIAN_POINT('Ctrl Pts',(3.5573945991761,2.78541078461679,396.993140732528));
#39292=CARTESIAN_POINT('Ctrl Pts',(3.09594366748323,3.37475403741634,397.019516691015));
#39293=CARTESIAN_POINT('Ctrl Pts',(2.4848950679742,3.84696354368545,397.045892649502));
#39294=CARTESIAN_POINT('Ctrl Pts',(1.79822638583807,4.14487049720285,397.072268607988));
#39295=CARTESIAN_POINT('Ctrl Pts',(1.11155770370195,4.44277745072024,397.098644566475));
#39296=CARTESIAN_POINT('Ctrl Pts',(0.349268938938723,4.56638185148592,397.125020524961));
#39297=CARTESIAN_POINT('Ctrl Pts',(-0.396352188490757,4.50071933317169,
397.151396483448));
#39298=CARTESIAN_POINT('Ctrl Pts',(-1.14197331592023,4.43505681485745,397.177772441934));
#39299=CARTESIAN_POINT('Ctrl Pts',(-1.87092680601596,4.18012737746331,397.204148400421));
#39300=CARTESIAN_POINT('Ctrl Pts',(-2.49496072766192,3.76679446489074,397.230524358908));
#39301=CARTESIAN_POINT('Ctrl Pts',(-3.1189946493079,3.35346155231816,397.256900317394));
#39302=CARTESIAN_POINT('Ctrl Pts',(-3.63810900250409,2.78172516456714,397.283276275881));
#39303=CARTESIAN_POINT('Ctrl Pts',(-3.98945637001185,2.12080349044383,397.309652234368));
#39304=CARTESIAN_POINT('Ctrl Pts',(-4.33474984909618,1.47126982272609,397.335573722081));
#39305=CARTESIAN_POINT('Ctrl Pts',(-4.51800794997827,0.735597803364803,
397.361495209794));
#39306=CARTESIAN_POINT('Ctrl Pts',(-4.51813440218219,-1.34914224690988E-5,
397.387416697508));
#39307=CARTESIAN_POINT('Origin',(0.,0.,387.));
#39308=CARTESIAN_POINT('',(-4.51746064445937,-7.62825515632226E-5,398.387416697508));
#39309=CARTESIAN_POINT('',(-4.51805439081064,6.66898104614677E-5,398.112583302492));
#39310=CARTESIAN_POINT('',(-4.51775,5.53264807684796E-16,387.));
#39311=CARTESIAN_POINT('Ctrl Pts',(-4.51805439081064,6.66898104614677E-5,
398.112583302492));
#39312=CARTESIAN_POINT('Ctrl Pts',(-4.51810357212516,0.0685915430668216,
398.110168746413));
#39313=CARTESIAN_POINT('Ctrl Pts',(-4.51657662108523,0.137114203419027,
398.107754190334));
#39314=CARTESIAN_POINT('Ctrl Pts',(-4.51345907222813,0.205564420371811,
398.105339634255));
#39315=CARTESIAN_POINT('Ctrl Pts',(-4.47940381049539,0.953296103447074,
398.078963675769));
#39316=CARTESIAN_POINT('Ctrl Pts',(-4.255545890619,1.6923832695825,398.052587717282));
#39317=CARTESIAN_POINT('Ctrl Pts',(-3.86898703306984,2.33334713781254,398.026211758796));
#39318=CARTESIAN_POINT('Ctrl Pts',(-3.48242817552068,2.97431100604258,397.999835800309));
#39319=CARTESIAN_POINT('Ctrl Pts',(-2.93316838029875,3.51715157636723,397.973459841822));
#39320=CARTESIAN_POINT('Ctrl Pts',(-2.28770467124889,3.89614897876697,397.947083883336));
#39321=CARTESIAN_POINT('Ctrl Pts',(-1.64224096219904,4.27514638116671,397.920707924849));
#39322=CARTESIAN_POINT('Ctrl Pts',(-0.900573339321256,4.49030061564153,
397.894331966363));
#39323=CARTESIAN_POINT('Ctrl Pts',(-0.15249299074285,4.51556368744535,397.867956007876));
#39324=CARTESIAN_POINT('Ctrl Pts',(0.595587357835559,4.54082675924917,397.841580049389));
#39325=CARTESIAN_POINT('Ctrl Pts',(1.35008043211458,4.37619866838198,397.815204090903));
#39326=CARTESIAN_POINT('Ctrl Pts',(2.01964230998743,4.0416103804436,397.788828132416));
#39327=CARTESIAN_POINT('Ctrl Pts',(2.68920418786027,3.70702209250522,397.76245217393));
#39328=CARTESIAN_POINT('Ctrl Pts',(3.27383486932692,3.20247360749564,397.736076215443));
#39329=CARTESIAN_POINT('Ctrl Pts',(3.70275509709574,2.58904890230608,397.709700256956));
#39330=CARTESIAN_POINT('Ctrl Pts',(4.13167532486456,1.97562419711653,397.68332429847));
#39331=CARTESIAN_POINT('Ctrl Pts',(4.40488509893554,1.25332327174699,397.656948339983));
#39332=CARTESIAN_POINT('Ctrl Pts',(4.48930783693528,0.509592653824902,397.630572381497));
#39333=CARTESIAN_POINT('Ctrl Pts',(4.57373057493501,-0.234137964097188,
397.60419642301));
#39334=CARTESIAN_POINT('Ctrl Pts',(4.4693662768635,-0.999298274571833,397.577820464523));
#39335=CARTESIAN_POINT('Ctrl Pts',(4.18884997495465,-1.69325290932077,397.551444506037));
#39336=CARTESIAN_POINT('Ctrl Pts',(3.9083336730458,-2.3872075440697,397.52506854755));
#39337=CARTESIAN_POINT('Ctrl Pts',(3.4516653672996,-3.00995650309293,397.498692589064));
#39338=CARTESIAN_POINT('Ctrl Pts',(2.87413234340601,-3.48610567828749,397.472316630577));
#39339=CARTESIAN_POINT('Ctrl Pts',(2.29659931951241,-3.96225485348206,397.44594067209));
#39340=CARTESIAN_POINT('Ctrl Pts',(1.5982015774714,-4.29180424484795,397.419564713604));
#39341=CARTESIAN_POINT('Ctrl Pts',(0.863491767430947,-4.43485642328811,
397.393188755117));
#39342=CARTESIAN_POINT('Ctrl Pts',(0.128781957390508,-4.57790860172826,
397.366812796631));
#39343=CARTESIAN_POINT('Ctrl Pts',(-0.642239920649369,-4.53446356724268,
397.340436838144));
#39344=CARTESIAN_POINT('Ctrl Pts',(-1.35622885827011,-4.30978106306993,
397.314060879658));
#39345=CARTESIAN_POINT('Ctrl Pts',(-2.07021779589086,-4.08509855889717,
397.287684921171));
#39346=CARTESIAN_POINT('Ctrl Pts',(-2.72717379309247,-3.67917858503723,
397.261308962684));
#39347=CARTESIAN_POINT('Ctrl Pts',(-3.24756141147036,-3.14116449845108,
397.234933004198));
#39348=CARTESIAN_POINT('Ctrl Pts',(-3.76794902984825,-2.60315041186493,
397.208557045711));
#39349=CARTESIAN_POINT('Ctrl Pts',(-4.15176826940243,-1.93304221255256,
397.182181087224));
#39350=CARTESIAN_POINT('Ctrl Pts',(-4.35255143425054,-1.21196763150028,
397.155805128738));
#39351=CARTESIAN_POINT('Ctrl Pts',(-4.46222473223498,-0.818096823374597,
397.141397853322));
#39352=CARTESIAN_POINT('Ctrl Pts',(-4.51728655488816,-0.409019453899831,
397.126990577907));
#39353=CARTESIAN_POINT('Ctrl Pts',(-4.51738673749921,3.14726202902737E-5,
397.112583302492));
#39354=CARTESIAN_POINT('Ctrl Pts',(-4.51813440218219,-1.34914224690988E-5,
397.387416697508));
#39355=CARTESIAN_POINT('Ctrl Pts',(-4.51813661921663,-0.0129106614282636,
397.387871168281));
#39356=CARTESIAN_POINT('Ctrl Pts',(-4.51808254311073,-0.0258078127678308,
397.388325639054));
#39357=CARTESIAN_POINT('Ctrl Pts',(-4.51797206016886,-0.0387044808823415,
397.388780109827));
#39358=CARTESIAN_POINT('Ctrl Pts',(-4.51156000099881,-0.787183817589628,
397.415156068314));
#39359=CARTESIAN_POINT('Ctrl Pts',(-4.31515550083941,-1.5340355305086,397.4415320268));
#39360=CARTESIAN_POINT('Ctrl Pts',(-3.95253658758193,-2.18884081128186,
397.467907985287));
#39361=CARTESIAN_POINT('Ctrl Pts',(-3.58991767432445,-2.84364609205511,
397.494283943774));
#39362=CARTESIAN_POINT('Ctrl Pts',(-3.06108434796891,-3.40640494068263,
397.52065990226));
#39363=CARTESIAN_POINT('Ctrl Pts',(-2.43006066892999,-3.80898604862584,
397.547035860747));
#39364=CARTESIAN_POINT('Ctrl Pts',(-1.79903698989108,-4.21156715656904,
397.573411819233));
#39365=CARTESIAN_POINT('Ctrl Pts',(-1.0658229581688,-4.45397052382792,397.59978777772));
#39366=CARTESIAN_POINT('Ctrl Pts',(-0.319186314229528,-4.5068491954042,
397.626163736207));
#39367=CARTESIAN_POINT('Ctrl Pts',(0.427450329709741,-4.55972786698048,
397.652539694693));
#39368=CARTESIAN_POINT('Ctrl Pts',(1.18750958586602,-4.42308184287416,397.67891565318));
#39369=CARTESIAN_POINT('Ctrl Pts',(1.86897365333732,-4.11345439459799,397.705291611666));
#39370=CARTESIAN_POINT('Ctrl Pts',(2.55043772080863,-3.80382694632181,397.731667570153));
#39371=CARTESIAN_POINT('Ctrl Pts',(3.15330659959498,-3.32121807387579,397.75804352864));
#39372=CARTESIAN_POINT('Ctrl Pts',(3.60459299560209,-2.72405559953603,397.784419487126));
#39373=CARTESIAN_POINT('Ctrl Pts',(4.0558793916092,-2.12689312519627,397.810795445613));
#39374=CARTESIAN_POINT('Ctrl Pts',(4.35558330483707,-1.41517704896277,397.837171404099));
#39375=CARTESIAN_POINT('Ctrl Pts',(4.46742059718259,-0.675072426614591,
397.863547362586));
#39376=CARTESIAN_POINT('Ctrl Pts',(4.57925788952811,0.065032195733587,397.889923321072));
#39377=CARTESIAN_POINT('Ctrl Pts',(4.50322856099129,0.833525364196443,397.916299279559));
#39378=CARTESIAN_POINT('Ctrl Pts',(4.24853722497469,1.53736821266419,397.942675238046));
#39379=CARTESIAN_POINT('Ctrl Pts',(3.9938458889581,2.24121106113193,397.969051196532));
#39380=CARTESIAN_POINT('Ctrl Pts',(3.56049254546173,2.88040358960456,397.995427155019));
#39381=CARTESIAN_POINT('Ctrl Pts',(3.00094181663071,3.37756092269383,398.021803113505));
#39382=CARTESIAN_POINT('Ctrl Pts',(2.44139108779969,3.87471825578309,398.048179071992));
#39383=CARTESIAN_POINT('Ctrl Pts',(1.75564297363402,4.22984039348899,398.074555030479));
#39384=CARTESIAN_POINT('Ctrl Pts',(1.02671867666087,4.39993390090012,398.100930988965));
#39385=CARTESIAN_POINT('Ctrl Pts',(0.297794379687701,4.57002740831124,398.127306947452));
#39386=CARTESIAN_POINT('Ctrl Pts',(-0.474306100092957,4.55509228542758,
398.153682905938));
#39387=CARTESIAN_POINT('Ctrl Pts',(-1.19610717160092,4.35693667699891,398.180058864425));
#39388=CARTESIAN_POINT('Ctrl Pts',(-1.91790824310887,4.15878106857024,398.206434822912));
#39389=CARTESIAN_POINT('Ctrl Pts',(-2.58940990634414,3.77740497459655,398.232810781398));
#39390=CARTESIAN_POINT('Ctrl Pts',(-3.12931572836207,3.25898030762527,398.259186739885));
#39391=CARTESIAN_POINT('Ctrl Pts',(-3.66922155038001,2.74055564065398,398.285562698372));
#39392=CARTESIAN_POINT('Ctrl Pts',(-4.07753153118063,2.08508240068509,398.311938656858));
#39393=CARTESIAN_POINT('Ctrl Pts',(-4.30481296375181,1.37191651366358,398.338314615345));
#39394=CARTESIAN_POINT('Ctrl Pts',(-4.44585038591782,0.929367920299095,
398.354681976066));
#39395=CARTESIAN_POINT('Ctrl Pts',(-4.51717896496231,0.464603561951737,
398.371049336787));
#39396=CARTESIAN_POINT('Ctrl Pts',(-4.51746064445937,-7.62825515632226E-5,
398.387416697508));
#39397=CARTESIAN_POINT('Origin',(0.,0.,387.));
#39398=CARTESIAN_POINT('',(-4.51769110620511,0.00011483889287206,399.387416697508));
#39399=CARTESIAN_POINT('',(-4.51766328535307,-0.00011344722995056,399.112583302492));
#39400=CARTESIAN_POINT('',(-4.51775,5.53264807684796E-16,387.));
#39401=CARTESIAN_POINT('',(3.43378788736219,2.93584158412962,400.));
#39402=CARTESIAN_POINT('Ctrl Pts',(-4.51769110620511,0.00011483889287206,
399.387416697508));
#39403=CARTESIAN_POINT('Ctrl Pts',(-4.51714363756808,-0.555201766580607,
399.406979422266));
#39404=CARTESIAN_POINT('Ctrl Pts',(-4.41453063358526,-1.11071503909854,
399.426542147024));
#39405=CARTESIAN_POINT('Ctrl Pts',(-4.21442463507641,-1.62855553809715,
399.446104871782));
#39406=CARTESIAN_POINT('Ctrl Pts',(-3.94462645640127,-2.32674761887018,
399.472480830268));
#39407=CARTESIAN_POINT('Ctrl Pts',(-3.49760073249453,-2.95645628495937,
399.498856788754));
#39408=CARTESIAN_POINT('Ctrl Pts',(-2.92746753734289,-3.44144015063649,
399.525232747241));
#39409=CARTESIAN_POINT('Ctrl Pts',(-2.35733434219124,-3.92642401631361,
399.551608705728));
#39410=CARTESIAN_POINT('Ctrl Pts',(-1.66409367579469,-4.26668308157866,
399.577984664215));
#39411=CARTESIAN_POINT('Ctrl Pts',(-0.931673462414912,-4.42103326728196,
399.604360622701));
#39412=CARTESIAN_POINT('Ctrl Pts',(-0.199253249035141,-4.57538345298525,
399.630736581188));
#39413=CARTESIAN_POINT('Ctrl Pts',(0.572346511327848,-4.5438247591268,399.657112539674));
#39414=CARTESIAN_POINT('Ctrl Pts',(1.28970997251907,-4.33015694611576,399.683488498161));
#39415=CARTESIAN_POINT('Ctrl Pts',(2.00707343371029,-4.11648913310473,399.709864456647));
#39416=CARTESIAN_POINT('Ctrl Pts',(2.67020059572975,-3.72071220094113,399.736240415134));
#39417=CARTESIAN_POINT('Ctrl Pts',(3.19881015567137,-3.19078644074148,399.762616373621));
#39418=CARTESIAN_POINT('Ctrl Pts',(3.72741971561299,-2.66086068054184,399.788992332107));
#39419=CARTESIAN_POINT('Ctrl Pts',(4.12151167347679,-1.99678609230616,399.815368290594));
#39420=CARTESIAN_POINT('Ctrl Pts',(4.33336809368492,-1.27886829832022,399.84174424908));
#39421=CARTESIAN_POINT('Ctrl Pts',(4.54522451389304,-0.560950504334284,
399.868120207567));
#39422=CARTESIAN_POINT('Ctrl Pts',(4.57484539644551,0.210810495401909,399.894496166054));
#39423=CARTESIAN_POINT('Ctrl Pts',(4.41862185200597,0.942742363213577,399.92087212454));
#39424=CARTESIAN_POINT('Ctrl Pts',(4.26239830756643,1.67467423102524,399.947248083027));
#39425=CARTESIAN_POINT('Ctrl Pts',(3.92033033613488,2.36677696691239,399.973624041513));
#39426=CARTESIAN_POINT('Ctrl Pts',(3.43378788736214,2.93584158412968,400.));
#39427=CARTESIAN_POINT('',(-3.43408816619742,2.93604416807593,400.));
#39428=CARTESIAN_POINT('Origin',(0.,0.,400.));
#39429=CARTESIAN_POINT('Ctrl Pts',(-3.43408816619742,2.93604416807593,400.));
#39430=CARTESIAN_POINT('Ctrl Pts',(-2.97450238708434,3.47304931101404,399.975093589943));
#39431=CARTESIAN_POINT('Ctrl Pts',(-2.38685943846713,3.90077490879642,399.950187179887));
#39432=CARTESIAN_POINT('Ctrl Pts',(-1.73419289785415,4.17206489997238,399.92528076983));
#39433=CARTESIAN_POINT('Ctrl Pts',(-1.04301719081029,4.45936176567177,399.898904811344));
#39434=CARTESIAN_POINT('Ctrl Pts',(-0.278918372417421,4.57121813647734,
399.872528852857));
#39435=CARTESIAN_POINT('Ctrl Pts',(0.465602633104777,4.49408395991645,399.84615289437));
#39436=CARTESIAN_POINT('Ctrl Pts',(1.21012363862699,4.41694978335555,399.819776935884));
#39437=CARTESIAN_POINT('Ctrl Pts',(1.93506683127852,4.15082505942817,399.793400977397));
#39438=CARTESIAN_POINT('Ctrl Pts',(2.55266298782158,3.72793237180886,399.767025018911));
#39439=CARTESIAN_POINT('Ctrl Pts',(3.17025914436463,3.30503968418955,399.740649060424));
#39440=CARTESIAN_POINT('Ctrl Pts',(3.68050826479921,2.72537903287831,399.714273101937));
#39441=CARTESIAN_POINT('Ctrl Pts',(4.02163754117277,2.05912619043133,399.687897143451));
#39442=CARTESIAN_POINT('Ctrl Pts',(4.36276681754633,1.39287334798434,399.661521184964));
#39443=CARTESIAN_POINT('Ctrl Pts',(4.53477624985888,0.640028314401621,399.635145226478));
#39444=CARTESIAN_POINT('Ctrl Pts',(4.51684061200005,-0.108263669819661,
399.608769267991));
#39445=CARTESIAN_POINT('Ctrl Pts',(4.49890497414122,-0.856555654040941,
399.582393309504));
#39446=CARTESIAN_POINT('Ctrl Pts',(4.29102426611101,-1.60029458890078,399.556017351018));
#39447=CARTESIAN_POINT('Ctrl Pts',(3.91836619751067,-2.24943891706491,399.529641392531));
#39448=CARTESIAN_POINT('Ctrl Pts',(3.54570812891033,-2.89858324522903,399.503265434045));
#39449=CARTESIAN_POINT('Ctrl Pts',(3.00827269973986,-3.45313296669745,399.476889475558));
#39450=CARTESIAN_POINT('Ctrl Pts',(2.37112525795217,-3.84595043629749,399.450513517072));
#39451=CARTESIAN_POINT('Ctrl Pts',(1.73397781616448,-4.23876790589754,399.424137558585));
#39452=CARTESIAN_POINT('Ctrl Pts',(0.99711836175957,-4.4698531236292,399.397761600098));
#39453=CARTESIAN_POINT('Ctrl Pts',(0.249756040315393,-4.51122947332523,
399.371385641612));
#39454=CARTESIAN_POINT('Ctrl Pts',(-0.497606281128785,-4.55260582302126,
399.345009683125));
#39455=CARTESIAN_POINT('Ctrl Pts',(-1.25547146961223,-4.40427330468165,
399.318633724638));
#39456=CARTESIAN_POINT('Ctrl Pts',(-1.93208738383067,-4.08418999214993,
399.292257766152));
#39457=CARTESIAN_POINT('Ctrl Pts',(-2.60870329804912,-3.7641066796182,399.265881807665));
#39458=CARTESIAN_POINT('Ctrl Pts',(-3.20406993800257,-3.27227257289437,
399.239505849179));
#39459=CARTESIAN_POINT('Ctrl Pts',(-3.64610826548277,-2.6682323819666,399.213129890692));
#39460=CARTESIAN_POINT('Ctrl Pts',(-4.08814659296297,-2.06419219103883,
399.186753932205));
#39461=CARTESIAN_POINT('Ctrl Pts',(-4.37685660796992,-1.34794591590712,
399.160377973719));
#39462=CARTESIAN_POINT('Ctrl Pts',(-4.47728517341772,-0.606207058821207,
399.134002015232));
#39463=CARTESIAN_POINT('Ctrl Pts',(-4.50446965905899,-0.405429628414596,
399.126862444319));
#39464=CARTESIAN_POINT('Ctrl Pts',(-4.51785871427772,-0.20278434994614,
399.119722873405));
#39465=CARTESIAN_POINT('Ctrl Pts',(-4.51766328535307,-0.00011344722995056,
399.112583302492));
#39466=CARTESIAN_POINT('Origin',(0.,0.,402.208336844637));
#39467=CARTESIAN_POINT('',(-5.07399177313997,5.16404304284901E-5,375.791663155363));
#39468=CARTESIAN_POINT('',(-5.07400718786956,-4.16755268873004E-5,375.708336844637));
#39469=CARTESIAN_POINT('',(-5.0736,-1.59740085886799E-13,402.208336844637));
#39470=CARTESIAN_POINT('',(1.3130361863572,-4.90075024188303,375.));
#39471=CARTESIAN_POINT('Ctrl Pts',(-5.07400718786956,-4.16755268873182E-5,
375.708336844637));
#39472=CARTESIAN_POINT('Ctrl Pts',(-5.07365763063996,0.800054575924722,
375.683232230984));
#39473=CARTESIAN_POINT('Ctrl Pts',(-4.67875473787853,2.4410987772414,375.631751658845));
#39474=CARTESIAN_POINT('Ctrl Pts',(-2.98728944096456,4.36266186682328,375.553895128218));
#39475=CARTESIAN_POINT('Ctrl Pts',(-0.544875549618088,5.2592655277028,375.474767252759));
#39476=CARTESIAN_POINT('Ctrl Pts',(2.02945798133318,4.88240903418803,375.395639377299));
#39477=CARTESIAN_POINT('Ctrl Pts',(4.1124194375256,3.3233956145555,375.316511501839));
#39478=CARTESIAN_POINT('Ctrl Pts',(5.19956989745793,0.959601216722932,375.237383626379));
#39479=CARTESIAN_POINT('Ctrl Pts',(5.02785240284651,-1.63637626402564,375.15825575092));
#39480=CARTESIAN_POINT('Ctrl Pts',(3.63845954881624,-3.83644847785649,375.07912787546));
#39481=CARTESIAN_POINT('Ctrl Pts',(2.1252131908655,-4.68314727417153,375.026375958487));
#39482=CARTESIAN_POINT('Ctrl Pts',(1.3130361863572,-4.90075024188303,375.));
#39483=CARTESIAN_POINT('',(-1.31318542874413,-4.90112866933894,375.));
#39484=CARTESIAN_POINT('Origin',(0.,0.,375.));
#39485=CARTESIAN_POINT('Ctrl Pts',(-5.07399177313997,5.16404304287937E-5,
375.791663155363));
#39486=CARTESIAN_POINT('Ctrl Pts',(-5.07401862443284,0.0509709830336597,
375.790065473344));
#39487=CARTESIAN_POINT('Ctrl Pts',(-5.06087568855098,0.942498320863251,
375.762091832839));
#39488=CARTESIAN_POINT('Ctrl Pts',(-4.56924148341307,2.66059337382158,375.707742233848));
#39489=CARTESIAN_POINT('Ctrl Pts',(-2.74710339271414,4.51775908713646,375.628614358388));
#39490=CARTESIAN_POINT('Ctrl Pts',(-0.25980027835232,5.28102544478076,375.549486482929));
#39491=CARTESIAN_POINT('Ctrl Pts',(2.29040909674433,4.76557955369675,375.470358607468));
#39492=CARTESIAN_POINT('Ctrl Pts',(4.28603436317887,3.09622956904483,375.391230732009));
#39493=CARTESIAN_POINT('Ctrl Pts',(5.24386820297344,0.677177255244125,375.312102856549));
#39494=CARTESIAN_POINT('Ctrl Pts',(4.93198748823577,-1.90583737857549,375.232974981089));
#39495=CARTESIAN_POINT('Ctrl Pts',(3.42590832840442,-4.02739560248487,375.153847105629));
#39496=CARTESIAN_POINT('Ctrl Pts',(1.13368018117025,-5.15247588128094,375.0761887786));
#39497=CARTESIAN_POINT('Ctrl Pts',(-0.546344062323364,-5.10618409554666,
375.024906410057));
#39498=CARTESIAN_POINT('Ctrl Pts',(-1.31318542874413,-4.90112866933894,
375.));
#39499=CARTESIAN_POINT('Origin',(0.,0.,402.208336844637));
#39500=CARTESIAN_POINT('',(-5.07342806457247,-0.000120553681964564,376.791663155363));
#39501=CARTESIAN_POINT('',(-5.0732320111606,-6.61733612274322E-5,376.708336844637));
#39502=CARTESIAN_POINT('',(-5.0736,-1.59740085886799E-13,402.208336844637));
#39503=CARTESIAN_POINT('Ctrl Pts',(-5.0732320111606,-6.61733612272383E-5,
376.708336844637));
#39504=CARTESIAN_POINT('Ctrl Pts',(-5.07300240190748,0.495753489740335,
376.692786357976));
#39505=CARTESIAN_POINT('Ctrl Pts',(-4.87836138639172,1.83273410665417,376.650859912829));
#39506=CARTESIAN_POINT('Ctrl Pts',(-3.72041242686768,3.75702756739127,376.582557509196));
#39507=CARTESIAN_POINT('Ctrl Pts',(-1.47810086816716,5.0766073897426,376.503429633736));
#39508=CARTESIAN_POINT('Ctrl Pts',(1.12210802704861,5.16697187426544,376.424301758276));
#39509=CARTESIAN_POINT('Ctrl Pts',(3.45061728097363,4.00624077340234,376.345173882816));
#39510=CARTESIAN_POINT('Ctrl Pts',(4.94361743453053,1.87546566308182,376.266046007357));
#39511=CARTESIAN_POINT('Ctrl Pts',(5.23960352937691,-0.709422013391795,
376.186918131896));
#39512=CARTESIAN_POINT('Ctrl Pts',(4.2669075188957,-3.12253502690154,376.107790256437));
#39513=CARTESIAN_POINT('Ctrl Pts',(2.26105138176727,-4.77957859502704,376.028662380977));
#39514=CARTESIAN_POINT('Ctrl Pts',(-0.292280359441297,-5.27932727476591,
375.949534505517));
#39515=CARTESIAN_POINT('Ctrl Pts',(-2.77484145645776,-4.50077558721857,
375.870406630058));
#39516=CARTESIAN_POINT('Ctrl Pts',(-4.58552092957851,-2.63243616845826,
375.791278754598));
#39517=CARTESIAN_POINT('Ctrl Pts',(-5.06368921675185,-0.921683996926001,
375.737255492791));
#39518=CARTESIAN_POINT('Ctrl Pts',(-5.07402489010486,-0.0405600539318397,
375.709608189471));
#39519=CARTESIAN_POINT('Ctrl Pts',(-5.07400718786956,-4.16755268873182E-5,
375.708336844637));
#39520=CARTESIAN_POINT('Ctrl Pts',(-5.07342806457247,-0.000120553681964737,
376.791663155363));
#39521=CARTESIAN_POINT('Ctrl Pts',(-5.07290494961689,0.587111569129446,
376.77324364185));
#39522=CARTESIAN_POINT('Ctrl Pts',(-4.82510106239333,2.01566514286781,376.728448169851));
#39523=CARTESIAN_POINT('Ctrl Pts',(-3.51189274247934,3.95263634434836,376.657276739365));
#39524=CARTESIAN_POINT('Ctrl Pts',(-1.20153141562281,5.1490821475793,376.578148863906));
#39525=CARTESIAN_POINT('Ctrl Pts',(1.39976059245402,5.09876406487689,376.499020988446));
#39526=CARTESIAN_POINT('Ctrl Pts',(3.66212404867255,3.81386577598244,376.419893112986));
#39527=CARTESIAN_POINT('Ctrl Pts',(5.03776558457334,1.60550385251465,376.340765237526));
#39528=CARTESIAN_POINT('Ctrl Pts',(5.19359667332446,-0.99160390296118,376.261637362067));
#39529=CARTESIAN_POINT('Ctrl Pts',(4.09188543028651,-3.34861140308599,376.182509486607));
#39530=CARTESIAN_POINT('Ctrl Pts',(1.99939275591558,-4.89480881330613,376.103381611147));
#39531=CARTESIAN_POINT('Ctrl Pts',(-0.577219342064538,-5.2558103583336,
376.024253735687));
#39532=CARTESIAN_POINT('Ctrl Pts',(-3.01406745721832,-4.34420557675964,
375.945125860227));
#39533=CARTESIAN_POINT('Ctrl Pts',(-4.68664255775979,-2.42036918652462,
375.867595666786));
#39534=CARTESIAN_POINT('Ctrl Pts',(-5.0735753393625,-0.789650899948463,
375.816441431831));
#39535=CARTESIAN_POINT('Ctrl Pts',(-5.07399177313997,5.16404304287937E-5,
375.791663155363));
#39536=CARTESIAN_POINT('Origin',(0.,0.,402.208336844637));
#39537=CARTESIAN_POINT('',(-5.07335325700037,0.000107956674043064,377.791663155363));
#39538=CARTESIAN_POINT('',(-5.07361435362778,0.000129215856731547,377.708336844637));
#39539=CARTESIAN_POINT('',(-5.0736,-1.59740085886799E-13,402.208336844637));
#39540=CARTESIAN_POINT('Ctrl Pts',(-5.07361435362778,0.000129215856731774,
377.708336844637));
#39541=CARTESIAN_POINT('Ctrl Pts',(-5.07380906160703,0.191278857423315,
377.702340484969));
#39542=CARTESIAN_POINT('Ctrl Pts',(-5.01660264728387,1.22311525648581,377.669968166814));
#39543=CARTESIAN_POINT('Ctrl Pts',(-4.33319923422642,3.02986949626759,377.611219890172));
#39544=CARTESIAN_POINT('Ctrl Pts',(-2.36351373006459,4.72974921277116,377.532092014713));
#39545=CARTESIAN_POINT('Ctrl Pts',(0.178456984968689,5.28439948077629,377.452964139253));
#39546=CARTESIAN_POINT('Ctrl Pts',(2.67721733402229,4.55952104001336,377.373836263793));
#39547=CARTESIAN_POINT('Ctrl Pts',(4.52773440567874,2.73063104786141,377.294708388334));
#39548=CARTESIAN_POINT('Ctrl Pts',(5.28193652635228,0.240564543316707,377.215580512874));
#39549=CARTESIAN_POINT('Ctrl Pts',(4.75720630136386,-2.3077506308472,377.136452637414));
#39550=CARTESIAN_POINT('Ctrl Pts',(3.08059835436342,-4.29728269340077,377.057324761954));
#39551=CARTESIAN_POINT('Ctrl Pts',(0.658075181053442,-5.24629982216222,
376.978196886494));
#39552=CARTESIAN_POINT('Ctrl Pts',(-1.923789860657,-4.92501343550216,376.899069011035));
#39553=CARTESIAN_POINT('Ctrl Pts',(-4.03984145181191,-3.4112176436405,376.819941135575));
#39554=CARTESIAN_POINT('Ctrl Pts',(-4.95409465736432,-1.5312714924381,376.756363746775));
#39555=CARTESIAN_POINT('Ctrl Pts',(-5.07339185365009,-0.345231048960516,
376.719162316463));
#39556=CARTESIAN_POINT('Ctrl Pts',(-5.0732320111606,-6.61733612272383E-5,
376.708336844637));
#39557=CARTESIAN_POINT('Ctrl Pts',(-5.07335325700037,0.00010795667404348,
377.791663155363));
#39558=CARTESIAN_POINT('Ctrl Pts',(-5.07357381709386,0.28275711441475,377.782797768842));
#39559=CARTESIAN_POINT('Ctrl Pts',(-4.98125011308217,1.40619065190393,377.747556423836));
#39560=CARTESIAN_POINT('Ctrl Pts',(-4.16308913613231,3.25966463764834,377.685939120343));
#39561=CARTESIAN_POINT('Ctrl Pts',(-2.1043987453421,4.85059075019948,377.606811244883));
#39562=CARTESIAN_POINT('Ctrl Pts',(0.463836508427624,5.26702766261653,377.527683369423));
#39563=CARTESIAN_POINT('Ctrl Pts',(2.91976153075723,4.40814216068722,377.448555493963));
#39564=CARTESIAN_POINT('Ctrl Pts',(4.66871526619766,2.48189896419878,377.369427618503));
#39565=CARTESIAN_POINT('Ctrl Pts',(5.28721789969248,-0.0452944421492617,
377.290299743044));
#39566=CARTESIAN_POINT('Ctrl Pts',(4.62550939154664,-2.56152055897115,377.211171867584));
#39567=CARTESIAN_POINT('Ctrl Pts',(2.84381135938942,-4.45751743210561,377.132043992124));
#39568=CARTESIAN_POINT('Ctrl Pts',(0.373532100567371,-5.27420121678766,
377.052916116664));
#39569=CARTESIAN_POINT('Ctrl Pts',(-2.18719169184094,-4.81382563128935,
376.973788241204));
#39570=CARTESIAN_POINT('Ctrl Pts',(-4.21832369780876,-3.18786290260816,
376.894660365745));
#39571=CARTESIAN_POINT('Ctrl Pts',(-4.99301148124094,-1.34818805955531,
376.833952003797));
#39572=CARTESIAN_POINT('Ctrl Pts',(-5.07365402794313,-0.253779808523861,
376.799619600337));
#39573=CARTESIAN_POINT('Ctrl Pts',(-5.07342806457247,-0.000120553681964737,
376.791663155363));
#39574=CARTESIAN_POINT('Origin',(0.,0.,402.208336844637));
#39575=CARTESIAN_POINT('',(-5.07402683453791,-2.287789782323E-5,378.791663155363));
#39576=CARTESIAN_POINT('',(-5.07385055213498,-0.000101541417780425,378.708336844637));
#39577=CARTESIAN_POINT('',(-5.0736,-1.59740085886799E-13,402.208336844637));
#39578=CARTESIAN_POINT('Ctrl Pts',(-5.07385055213498,-0.000101541417780338,
378.708336844637));
#39579=CARTESIAN_POINT('Ctrl Pts',(-5.07319426513103,0.727190265934581,
378.685518653475));
#39580=CARTESIAN_POINT('Ctrl Pts',(-4.73238867060224,2.2957670138656,378.636324503826));
#39581=CARTESIAN_POINT('Ctrl Pts',(-3.17247821056078,4.22990623671853,378.56075439569));
#39582=CARTESIAN_POINT('Ctrl Pts',(-0.770966287939471,5.23090200164121,
378.48162652023));
#39583=CARTESIAN_POINT('Ctrl Pts',(1.81722219130848,4.96532257515351,378.40249864477));
#39584=CARTESIAN_POINT('Ctrl Pts',(3.96540079385267,3.49747356130477,378.323370769311));
#39585=CARTESIAN_POINT('Ctrl Pts',(5.15342409853101,1.18276998126983,378.244242893851));
#39586=CARTESIAN_POINT('Ctrl Pts',(5.09363218664291,-1.41832151330666,378.165115018391));
#39587=CARTESIAN_POINT('Ctrl Pts',(3.80050266687247,-3.67599024033094,378.085987142931));
#39588=CARTESIAN_POINT('Ctrl Pts',(1.58714516515185,-5.04357958127442,378.006859267472));
#39589=CARTESIAN_POINT('Ctrl Pts',(-1.01051292004705,-5.18995071328536,
377.927731392012));
#39590=CARTESIAN_POINT('Ctrl Pts',(-3.36349224912901,-4.07966232156074,
377.848603516552));
#39591=CARTESIAN_POINT('Ctrl Pts',(-4.78546484347183,-2.14054821676427,
377.77547200076));
#39592=CARTESIAN_POINT('Ctrl Pts',(-5.07295260704762,-0.649523777787379,
377.728716443455));
#39593=CARTESIAN_POINT('Ctrl Pts',(-5.07361435362778,0.000129215856731774,
377.708336844637));
#39594=CARTESIAN_POINT('Ctrl Pts',(-5.07402683453791,-2.28778978229567E-5,
378.791663155363));
#39595=CARTESIAN_POINT('Ctrl Pts',(-5.07381925213896,0.818631858438491,
378.765975937348));
#39596=CARTESIAN_POINT('Ctrl Pts',(-4.66448051806342,2.47809170659261,378.713912760847));
#39597=CARTESIAN_POINT('Ctrl Pts',(-2.9391988257698,4.39520590733944,378.63547362586));
#39598=CARTESIAN_POINT('Ctrl Pts',(-0.487090471470337,5.2649280695866,378.5563457504));
#39599=CARTESIAN_POINT('Ctrl Pts',(2.08295867142411,4.85983619872698,378.47721787494));
#39600=CARTESIAN_POINT('Ctrl Pts',(4.1486543056634,3.27801649742928,378.398089999481));
#39601=CARTESIAN_POINT('Ctrl Pts',(5.20982287752563,0.902480077413658,378.318962124021));
#39602=CARTESIAN_POINT('Ctrl Pts',(5.00952021436078,-1.69157675771122,378.239834248561));
#39603=CARTESIAN_POINT('Ctrl Pts',(3.59624624674644,-3.8760466506584,378.160706373101));
#39604=CARTESIAN_POINT('Ctrl Pts',(1.31220156369858,-5.12199685294173,378.081578497641));
#39605=CARTESIAN_POINT('Ctrl Pts',(-1.28957072085835,-5.12774141910675,
378.002450622182));
#39606=CARTESIAN_POINT('Ctrl Pts',(-3.57909508295452,-3.89188939879962,
377.923322746722));
#39607=CARTESIAN_POINT('Ctrl Pts',(-4.84258096039032,-1.9577252596909,377.853060257782));
#39608=CARTESIAN_POINT('Ctrl Pts',(-5.07291761514975,-0.558169836019873,
377.809173727329));
#39609=CARTESIAN_POINT('Ctrl Pts',(-5.07335325700037,0.00010795667404348,
377.791663155363));
#39610=CARTESIAN_POINT('Origin',(0.,0.,402.208336844637));
#39611=CARTESIAN_POINT('',(-5.07326152951467,-8.03441847486985E-5,379.791663155363));
#39612=CARTESIAN_POINT('',(-5.07317735229637,-2.23272941127382E-6,379.708336844637));
#39613=CARTESIAN_POINT('',(-5.0736,-1.59740085886799E-13,402.208336844637));
#39614=CARTESIAN_POINT('Ctrl Pts',(-5.07317735229636,-2.23272941118208E-6,
379.708336844637));
#39615=CARTESIAN_POINT('Ctrl Pts',(-5.07317083223754,0.422929008539474,
379.695072780467));
#39616=CARTESIAN_POINT('Ctrl Pts',(-4.91684325738401,1.68687545589345,379.65543275781));
#39617=CARTESIAN_POINT('Ctrl Pts',(-3.87882817196482,3.59324599495851,379.589416776668));
#39618=CARTESIAN_POINT('Ctrl Pts',(-1.69545248338881,5.00820982432685,379.510288901207));
#39619=CARTESIAN_POINT('Ctrl Pts',(0.898448589337301,5.21051963821565,379.431161025747));
#39620=CARTESIAN_POINT('Ctrl Pts',(3.27480540417913,4.15118950816177,379.352033150288));
#39621=CARTESIAN_POINT('Ctrl Pts',(4.85822301267979,2.08671845896413,379.272905274828));
#39622=CARTESIAN_POINT('Ctrl Pts',(5.26530339668872,-0.483016468385486,
379.193777399368));
#39623=CARTESIAN_POINT('Ctrl Pts',(4.39747886842774,-2.93579705866137,379.114649523908));
#39624=CARTESIAN_POINT('Ctrl Pts',(2.4648785829925,-4.67772362790043,379.035521648449));
#39625=CARTESIAN_POINT('Ctrl Pts',(-0.0645507124447473,-5.28701787148826,
378.956393772989));
#39626=CARTESIAN_POINT('Ctrl Pts',(-2.57835013545374,-4.61614940691036,
378.877265897529));
#39627=CARTESIAN_POINT('Ctrl Pts',(-4.46784531508162,-2.82755778162292,
378.798138022069));
#39628=CARTESIAN_POINT('Ctrl Pts',(-5.04261473172305,-1.0675305862618,378.741828337772));
#39629=CARTESIAN_POINT('Ctrl Pts',(-5.07395287910916,-0.113499444385656,
378.711894611961));
#39630=CARTESIAN_POINT('Ctrl Pts',(-5.07385055213498,-0.000101541417780338,
378.708336844637));
#39631=CARTESIAN_POINT('Ctrl Pts',(-5.07326152951467,-8.03441847485598E-5,
379.791663155363));
#39632=CARTESIAN_POINT('Ctrl Pts',(-5.07297012272296,0.514306801455685,
379.775530064341));
#39633=CARTESIAN_POINT('Ctrl Pts',(-4.86799754311315,1.86989152588461,379.733021014832));
#39634=CARTESIAN_POINT('Ctrl Pts',(-3.67892986111526,3.7976571438602,379.664136006837));
#39635=CARTESIAN_POINT('Ctrl Pts',(-1.42226240084736,5.09253319757995,379.585008131377));
#39636=CARTESIAN_POINT('Ctrl Pts',(1.17878204679748,5.15433774518764,379.505880255918));
#39637=CARTESIAN_POINT('Ctrl Pts',(3.49440419135096,3.9681058520139,379.426752380457));
#39638=CARTESIAN_POINT('Ctrl Pts',(4.96391496617568,1.82106367650753,379.347624504998));
#39639=CARTESIAN_POINT('Ctrl Pts',(5.2314969825461,-0.766918526917405,379.268496629538));
#39640=CARTESIAN_POINT('Ctrl Pts',(4.23235974285854,-3.16920427116154,379.189368754078));
#39641=CARTESIAN_POINT('Ctrl Pts',(2.20842757301423,-4.80412035237133,379.110240878619));
#39642=CARTESIAN_POINT('Ctrl Pts',(-0.350238295746339,-5.27579926091873,
379.031113003158));
#39643=CARTESIAN_POINT('Ctrl Pts',(-2.82409983509395,-4.47003185970082,
378.951985127699));
#39644=CARTESIAN_POINT('Ctrl Pts',(-4.61415296279982,-2.58192121126957,
378.872857252239));
#39645=CARTESIAN_POINT('Ctrl Pts',(-5.06855147600533,-0.884525550463806,
378.819416594794));
#39646=CARTESIAN_POINT('Ctrl Pts',(-5.07403240035665,-0.0219731198176094,
378.792351895835));
#39647=CARTESIAN_POINT('Ctrl Pts',(-5.07402683453791,-2.28778978229567E-5,
378.791663155363));
#39648=CARTESIAN_POINT('Origin',(0.,0.,402.208336844637));
#39649=CARTESIAN_POINT('',(-5.07355665554129,0.000129459885802874,380.791663155363));
#39650=CARTESIAN_POINT('',(-5.07383699511133,0.000104483598321417,380.708336844637));
#39651=CARTESIAN_POINT('',(-5.0736,-1.59740085886799E-13,402.208336844637));
#39652=CARTESIAN_POINT('Ctrl Pts',(-5.07383699511133,0.000104483598321794,
380.708336844637));
#39653=CARTESIAN_POINT('Ctrl Pts',(-5.07394580731281,0.118353460768718,
380.704626907459));
#39654=CARTESIAN_POINT('Ctrl Pts',(-5.04109883614377,1.0772383012794,380.674541011795));
#39655=CARTESIAN_POINT('Ctrl Pts',(-4.45971656638884,2.84036140577044,380.618079157644));
#39656=CARTESIAN_POINT('Ctrl Pts',(-2.56509888808806,4.6235259772432,380.538951282184));
#39657=CARTESIAN_POINT('Ctrl Pts',(-0.0493855337170155,5.28718127521391,
380.459823406725));
#39658=CARTESIAN_POINT('Ctrl Pts',(2.47828569939099,4.67063429954727,380.380695531265));
#39659=CARTESIAN_POINT('Ctrl Pts',(4.40588161411396,2.92317156019379,380.301567655805));
#39660=CARTESIAN_POINT('Ctrl Pts',(5.26666718771851,0.467911852513223,380.222439780345));
#39661=CARTESIAN_POINT('Ctrl Pts',(4.8522176299277,-2.10064486282949,380.143311904886));
#39662=CARTESIAN_POINT('Ctrl Pts',(3.26288495036134,-4.1605656548862,380.064184029426));
#39663=CARTESIAN_POINT('Ctrl Pts',(0.883499402425967,-5.21307525111868,
379.985056153966));
#39664=CARTESIAN_POINT('Ctrl Pts',(-1.70981070849824,-5.0033261046046,379.905928278506));
#39665=CARTESIAN_POINT('Ctrl Pts',(-3.88911883186622,-3.58210545343612,
379.826800403046));
#39666=CARTESIAN_POINT('Ctrl Pts',(-4.91928148884334,-1.67716650260946,
379.760936591757));
#39667=CARTESIAN_POINT('Ctrl Pts',(-5.07318379755486,-0.418081463015616,
379.721448738954));
#39668=CARTESIAN_POINT('Ctrl Pts',(-5.07317735229636,-2.23272941118208E-6,
379.708336844637));
#39669=CARTESIAN_POINT('Ctrl Pts',(-5.07355665554129,0.000129459885803325,
380.791663155363));
#39670=CARTESIAN_POINT('Ctrl Pts',(-5.07376606808144,0.209858000324401,
380.785084191333));
#39671=CARTESIAN_POINT('Ctrl Pts',(-5.00984200321542,1.26028988400143,380.752129268817));
#39672=CARTESIAN_POINT('Ctrl Pts',(-4.29966508516876,3.07727230850615,380.692798387814));
#39673=CARTESIAN_POINT('Ctrl Pts',(-2.31143093395199,4.75541919738815,380.613670512354));
#39674=CARTESIAN_POINT('Ctrl Pts',(0.236477452546483,5.28212108151216,380.534542636895));
#39675=CARTESIAN_POINT('Ctrl Pts',(2.7271267899117,4.52984593303835,380.455414761435));
#39676=CARTESIAN_POINT('Ctrl Pts',(4.55744811217567,2.68074456264382,380.376286885975));
#39677=CARTESIAN_POINT('Ctrl Pts',(5.28425980776137,0.182545855597361,380.297159010515));
#39678=CARTESIAN_POINT('Ctrl Pts',(4.73157661405697,-2.35985326887651,380.218031135055));
#39679=CARTESIAN_POINT('Ctrl Pts',(3.03322149728047,-4.33085350176541,380.138903259596));
#39680=CARTESIAN_POINT('Ctrl Pts',(0.600422665576261,-5.25321019263273,
380.059775384136));
#39681=CARTESIAN_POINT('Ctrl Pts',(-1.97775844481349,-4.90359013777528,
379.980647508676));
#39682=CARTESIAN_POINT('Ctrl Pts',(-4.07705851709219,-3.36664796994342,
379.901519633216));
#39683=CARTESIAN_POINT('Ctrl Pts',(-4.96242349460837,-1.49409344074893,
379.838524848778));
#39684=CARTESIAN_POINT('Ctrl Pts',(-5.07344654310827,-0.326663721856642,
379.801906022827));
#39685=CARTESIAN_POINT('Ctrl Pts',(-5.07326152951467,-8.03441847485598E-5,
379.791663155363));
#39686=CARTESIAN_POINT('Origin',(0.,0.,402.208336844637));
#39687=CARTESIAN_POINT('',(-5.07389966860957,-8.89210953775033E-5,381.791663155363));
#39688=CARTESIAN_POINT('',(-5.0736295665075,-0.000128745637012367,381.708336844637));
#39689=CARTESIAN_POINT('',(-5.0736,-1.59740085886799E-13,402.208336844637));
#39690=CARTESIAN_POINT('Ctrl Pts',(-5.0736295665075,-0.000128745637012449,
381.708336844637));
#39691=CARTESIAN_POINT('Ctrl Pts',(-5.07296124918876,0.654369409793758,
381.687805075965));
#39692=CARTESIAN_POINT('Ctrl Pts',(-4.78227571732073,2.15023935796871,381.640897348807));
#39693=CARTESIAN_POINT('Ctrl Pts',(-3.35177659407457,4.08929314568265,381.567613663161));
#39694=CARTESIAN_POINT('Ctrl Pts',(-0.995622270609436,5.1928278483096,381.488485787702));
#39695=CARTESIAN_POINT('Ctrl Pts',(1.60160528794473,5.03900637720777,381.409357912242));
#39696=CARTESIAN_POINT('Ctrl Pts',(3.81103098679937,3.66507402184023,381.330230036782));
#39697=CARTESIAN_POINT('Ctrl Pts',(5.09767944760569,1.40370545962173,381.251102161322));
#39698=CARTESIAN_POINT('Ctrl Pts',(5.15001032416474,-1.1975468378773,381.171974285863));
#39699=CARTESIAN_POINT('Ctrl Pts',(3.95535257236717,-3.50883325283227,381.092846410403));
#39700=CARTESIAN_POINT('Ctrl Pts',(1.8029725310162,-4.97051454281288,381.013718534943));
#39701=CARTESIAN_POINT('Ctrl Pts',(-0.785967070782117,-5.22866909753901,
380.934590659483));
#39702=CARTESIAN_POINT('Ctrl Pts',(-3.18459792796892,-4.22078912113472,
380.855462784024));
#39703=CARTESIAN_POINT('Ctrl Pts',(-4.73582433047741,-2.28608714092918,
380.780044845741));
#39704=CARTESIAN_POINT('Ctrl Pts',(-5.07317220227002,-0.722342746081139,
380.731002865946));
#39705=CARTESIAN_POINT('Ctrl Pts',(-5.07383699511133,0.000104483598321794,
380.708336844637));
#39706=CARTESIAN_POINT('Ctrl Pts',(-5.07389966860957,-8.89210953773471E-5,
381.791663155363));
#39707=CARTESIAN_POINT('Ctrl Pts',(-5.07328829289394,0.745751527323211,
381.768262359839));
#39708=CARTESIAN_POINT('Ctrl Pts',(-4.71908116243226,2.33281964194823,381.718485605828));
#39709=CARTESIAN_POINT('Ctrl Pts',(-3.12583571520092,4.26449009693918,381.642332893332));
#39710=CARTESIAN_POINT('Ctrl Pts',(-0.713476057932961,5.23905302703404,
381.563205017871));
#39711=CARTESIAN_POINT('Ctrl Pts',(1.87163986094335,4.94506713162178,381.484077142412));
#39712=CARTESIAN_POINT('Ctrl Pts',(4.00356957706116,3.45371616479241,381.404949266952));
#39713=CARTESIAN_POINT('Ctrl Pts',(5.16610206459392,1.12610575148009,381.325821391492));
#39714=CARTESIAN_POINT('Ctrl Pts',(5.07774957870228,-1.47417228345499,381.246693516033));
#39715=CARTESIAN_POINT('Ctrl Pts',(3.75990519207135,-3.71750422352859,381.167565640573));
#39716=CARTESIAN_POINT('Ctrl Pts',(1.53166282114666,-5.06070486272762,381.088437765113));
#39717=CARTESIAN_POINT('Ctrl Pts',(-1.0674460141586,-5.17854069330105,381.009309889653));
#39718=CARTESIAN_POINT('Ctrl Pts',(-3.40809069944175,-4.04247974511891,
380.930182014193));
#39719=CARTESIAN_POINT('Ctrl Pts',(-4.79752508832052,-2.10343849769112,
380.857633102763));
#39720=CARTESIAN_POINT('Ctrl Pts',(-5.07292650482488,-0.630972144226672,
380.81146014982));
#39721=CARTESIAN_POINT('Ctrl Pts',(-5.07355665554129,0.000129459885803325,
380.791663155363));
#39722=CARTESIAN_POINT('Origin',(0.,0.,402.208336844637));
#39723=CARTESIAN_POINT('',(-5.0731816081447,-1.92612327425123E-5,382.791663155363));
#39724=CARTESIAN_POINT('',(-5.07322528972955,6.22763117692481E-5,382.708336844637));
#39725=CARTESIAN_POINT('',(-5.0736,-1.59740085886799E-13,402.208336844637));
#39726=CARTESIAN_POINT('Ctrl Pts',(-5.07322528972955,6.22763117691383E-5,
382.708336844637));
#39727=CARTESIAN_POINT('Ctrl Pts',(-5.07337757676184,0.350080340895845,
382.697359202958));
#39728=CARTESIAN_POINT('Ctrl Pts',(-4.95188321010373,1.54098189440445,382.660005602791));
#39729=CARTESIAN_POINT('Ctrl Pts',(-4.03004033454984,3.42279121037416,382.596276044139));
#39730=CARTESIAN_POINT('Ctrl Pts',(-1.90965538190854,4.93051124025298,382.517148168679));
#39731=CARTESIAN_POINT('Ctrl Pts',(0.673120594328623,5.24439066369047,382.438020293219));
#39732=CARTESIAN_POINT('Ctrl Pts',(3.09291170766135,4.28842884242289,382.35889241776));
#39733=CARTESIAN_POINT('Ctrl Pts',(4.76380612269667,2.29409589888282,382.2797645423));
#39734=CARTESIAN_POINT('Ctrl Pts',(5.28122477966896,-0.255713891925586,
382.20063666684));
#39735=CARTESIAN_POINT('Ctrl Pts',(4.51988342850276,-2.74360685242242,382.12150879138));
#39736=CARTESIAN_POINT('Ctrl Pts',(2.66412810880644,-4.56718142707082,382.04238091592));
#39737=CARTESIAN_POINT('Ctrl Pts',(0.16329884807764,-5.28488961607806,381.96325304046));
#39738=CARTESIAN_POINT('Ctrl Pts',(-2.37707049000228,-4.72295041827389,
381.884125165001));
#39739=CARTESIAN_POINT('Ctrl Pts',(-4.3418720751543,-3.0174279860352,381.804997289541));
#39740=CARTESIAN_POINT('Ctrl Pts',(-5.01833358746616,-1.21340586700331,
381.746401182753));
#39741=CARTESIAN_POINT('Ctrl Pts',(-5.07381979723383,-0.186425967023143,
381.714181034452));
#39742=CARTESIAN_POINT('Ctrl Pts',(-5.0736295665075,-0.000128745637012449,
381.708336844637));
#39743=CARTESIAN_POINT('Ctrl Pts',(-5.0731816081447,-1.92612327423736E-5,
382.791663155363));
#39744=CARTESIAN_POINT('Ctrl Pts',(-5.07312283046122,0.441487546406695,
382.777816486831));
#39745=CARTESIAN_POINT('Ctrl Pts',(-4.90736705066614,1.72404611325897,382.737593859813));
#39746=CARTESIAN_POINT('Ctrl Pts',(-3.83913463932894,3.63562510806912,382.670995274309));
#39747=CARTESIAN_POINT('Ctrl Pts',(-1.64035202533435,5.0265266276326,382.591867398849));
#39748=CARTESIAN_POINT('Ctrl Pts',(0.955614320991023,5.2003390249901,382.512739523389));
#39749=CARTESIAN_POINT('Ctrl Pts',(3.32019468624774,4.11497654315675,382.433611647929));
#39750=CARTESIAN_POINT('Ctrl Pts',(4.8808455917412,2.03324150432223,382.354483772469));
#39751=CARTESIAN_POINT('Ctrl Pts',(5.25968159463003,-0.540808864968189,
382.27535589701));
#39752=CARTESIAN_POINT('Ctrl Pts',(4.36497391033337,-2.98391143759783,382.19622802155));
#39753=CARTESIAN_POINT('Ctrl Pts',(2.41336099931917,-4.70450989926509,382.11710014609));
#39754=CARTESIAN_POINT('Ctrl Pts',(-0.122606802820077,-5.28599018890692,
382.03797227063));
#39755=CARTESIAN_POINT('Ctrl Pts',(-2.6288874239146,-4.58755660648474,381.958844395171));
#39756=CARTESIAN_POINT('Ctrl Pts',(-4.49862704479611,-2.77832313044165,
381.879716519711));
#39757=CARTESIAN_POINT('Ctrl Pts',(-5.04828738596174,-1.03036438158544,
381.823989439775));
#39758=CARTESIAN_POINT('Ctrl Pts',(-5.07397739854758,-0.0949146237502798,
381.794638318325));
#39759=CARTESIAN_POINT('Ctrl Pts',(-5.07389966860957,-8.89210953773471E-5,
381.791663155363));
#39760=CARTESIAN_POINT('Origin',(0.,0.,402.208336844637));
#39761=CARTESIAN_POINT('',(-5.07378290535392,0.000114313540020838,383.791663155363));
#39762=CARTESIAN_POINT('',(-5.07400033060213,4.63270069165547E-5,383.708336844637));
#39763=CARTESIAN_POINT('',(-5.0736,-1.59740085886799E-13,402.208336844637));
#39764=CARTESIAN_POINT('Ctrl Pts',(-5.07400033060213,4.63270069167923E-5,
383.708336844637));
#39765=CARTESIAN_POINT('Ctrl Pts',(-5.0740221098109,0.0454146017487004,
383.70691332995));
#39766=CARTESIAN_POINT('Ctrl Pts',(-5.06238522132993,0.931389441082911,
383.679113856776));
#39767=CARTESIAN_POINT('Ctrl Pts',(-4.57795151673967,2.64557832586642,383.624938425116));
#39768=CARTESIAN_POINT('Ctrl Pts',(-2.76192026167378,4.50871614055144,383.545810549656));
#39769=CARTESIAN_POINT('Ctrl Pts',(-0.277136335846315,5.28014395819535,
383.466682674197));
#39770=CARTESIAN_POINT('Ctrl Pts',(2.27475150580887,4.77307347049397,383.387554798736));
#39771=CARTESIAN_POINT('Ctrl Pts',(4.27584642055071,3.11028329188466,383.308426923277));
#39772=CARTESIAN_POINT('Ctrl Pts',(5.24161683545466,0.6943901771998,383.229299047817));
#39773=CARTESIAN_POINT('Ctrl Pts',(4.93821764164047,-1.8896378731662,383.150171172357));
#39774=CARTESIAN_POINT('Ctrl Pts',(3.43911186553428,-4.01612180396144,383.071043296897));
#39775=CARTESIAN_POINT('Ctrl Pts',(1.1072828290795,-5.17016919494313,382.991915421438));
#39776=CARTESIAN_POINT('Ctrl Pts',(-1.49265617402097,-5.07234682509687,
382.912787545978));
#39777=CARTESIAN_POINT('Ctrl Pts',(-3.73117351815568,-3.74634074068643,
382.833659670518));
#39778=CARTESIAN_POINT('Ctrl Pts',(-4.88103073617416,-1.82302830121342,
382.765509436738));
#39779=CARTESIAN_POINT('Ctrl Pts',(-5.07301167700312,-0.490907387666408,
382.723735161444));
#39780=CARTESIAN_POINT('Ctrl Pts',(-5.07322528972955,6.22763117691383E-5,
382.708336844637));
#39781=CARTESIAN_POINT('Ctrl Pts',(-5.07378290535392,0.000114313540020942,
383.791663155363));
#39782=CARTESIAN_POINT('Ctrl Pts',(-5.07391625780791,0.136937191492554,
383.787370613824));
#39783=CARTESIAN_POINT('Ctrl Pts',(-5.03516348602304,1.11440684342152,383.756702113798));
#39784=CARTESIAN_POINT('Ctrl Pts',(-4.42825589269063,2.88916500985471,383.699657655286));
#39785=CARTESIAN_POINT('Ctrl Pts',(-2.51417043865664,4.65141609735177,383.620529779826));
#39786=CARTESIAN_POINT('Ctrl Pts',(0.00867922154690349,5.28740478651213,
383.541401904366));
#39787=CARTESIAN_POINT('Ctrl Pts',(2.52942735381344,4.6431370825228,383.462274028906));
#39788=CARTESIAN_POINT('Ctrl Pts',(4.43771707378134,2.87461160478899,383.383146153446));
#39789=CARTESIAN_POINT('Ctrl Pts',(5.27148802998996,0.410047137522666,383.304018277987));
#39790=CARTESIAN_POINT('Ctrl Pts',(4.82885656869832,-2.15380336712922,383.224890402527));
#39791=CARTESIAN_POINT('Ctrl Pts',(3.2169984748157,-4.19614650820864,383.145762527067));
#39792=CARTESIAN_POINT('Ctrl Pts',(0.82619815304806,-5.22246314656389,383.066634651607));
#39793=CARTESIAN_POINT('Ctrl Pts',(-1.76465219517988,-4.98424792073636,
382.987506776148));
#39794=CARTESIAN_POINT('Ctrl Pts',(-3.92822160960685,-3.5391806525149,382.908378900688));
#39795=CARTESIAN_POINT('Ctrl Pts',(-4.9284760402056,-1.63999308805888,382.84309769376));
#39796=CARTESIAN_POINT('Ctrl Pts',(-5.07323479369165,-0.399520902907398,
382.804192445318));
#39797=CARTESIAN_POINT('Ctrl Pts',(-5.0731816081447,-1.92612327423736E-5,
382.791663155363));
#39798=CARTESIAN_POINT('Origin',(0.,0.,402.208336844637));
#39799=CARTESIAN_POINT('',(-5.07368788828891,-0.000125377980982264,384.791663155363));
#39800=CARTESIAN_POINT('',(-5.07341299508847,-0.000118529377325131,384.708336844637));
#39801=CARTESIAN_POINT('',(-5.0736,-1.59740085886799E-13,402.208336844637));
#39802=CARTESIAN_POINT('Ctrl Pts',(-5.07341299508847,-0.000118529377325025,
384.708336844637));
#39803=CARTESIAN_POINT('Ctrl Pts',(-5.07290585727583,0.581565929821983,
384.690091498456));
#39804=CARTESIAN_POINT('Ctrl Pts',(-4.82849439364024,2.00456420438781,384.645470193788));
#39805=CARTESIAN_POINT('Ctrl Pts',(-3.52485021126398,3.94108560628483,384.574472930633));
#39806=CARTESIAN_POINT('Ctrl Pts',(-1.21842922909547,5.14510981239459,384.495345055173));
#39807=CARTESIAN_POINT('Ctrl Pts',(1.38301395642869,5.10333196688562,384.416217179714));
#39808=CARTESIAN_POINT('Ctrl Pts',(3.64958350715001,3.82586787438508,384.337089304254));
#39809=CARTESIAN_POINT('Ctrl Pts',(5.03246761935876,1.62203404033908,384.257961428794));
#39810=CARTESIAN_POINT('Ctrl Pts',(5.19682409785237,-0.974548133184912,
384.178833553334));
#39811=CARTESIAN_POINT('Ctrl Pts',(4.10285677781212,-3.33515982055948,384.099705677875));
#39812=CARTESIAN_POINT('Ctrl Pts',(2.0154514986864,-4.88821849187982,384.020577802414));
#39813=CARTESIAN_POINT('Ctrl Pts',(-0.559961559389509,-5.25767703647906,
383.941449926955));
#39814=CARTESIAN_POINT('Ctrl Pts',(-2.99978931706339,-4.3540772640303,383.862322051495));
#39815=CARTESIAN_POINT('Ctrl Pts',(-4.68244282170845,-2.43143282852321,
383.784617690723));
#39816=CARTESIAN_POINT('Ctrl Pts',(-5.0736185681322,-0.795203160750922,
383.733289288436));
#39817=CARTESIAN_POINT('Ctrl Pts',(-5.07400033060213,4.63270069167923E-5,
383.708336844637));
#39818=CARTESIAN_POINT('Ctrl Pts',(-5.07368788828891,-0.000125377980982003,
384.791663155363));
#39819=CARTESIAN_POINT('Ctrl Pts',(-5.07300172207351,0.67292236196844,384.770548782329));
#39820=CARTESIAN_POINT('Ctrl Pts',(-4.76991529656479,2.18733716132669,384.72305845081));
#39821=CARTESIAN_POINT('Ctrl Pts',(-3.30666744538294,4.12585447040522,384.649192160803));
#39822=CARTESIAN_POINT('Ctrl Pts',(-0.93853660926441,5.20344825460853,384.570064285343));
#39823=CARTESIAN_POINT('Ctrl Pts',(1.65684512644118,5.02111431181428,384.490936409884));
#39824=CARTESIAN_POINT('Ctrl Pts',(3.85104960199139,3.62300174831864,384.411808534424));
#39825=CARTESIAN_POINT('Ctrl Pts',(5.11278700298303,1.34764007340457,384.332680658964));
#39826=CARTESIAN_POINT('Ctrl Pts',(5.13654877856401,-1.25403004379905,384.253552783504));
#39827=CARTESIAN_POINT('Ctrl Pts',(3.91658141328989,-3.55205781743347,384.174424908044));
#39828=CARTESIAN_POINT('Ctrl Pts',(1.74827954439566,-4.99001436270134,384.095297032584));
#39829=CARTESIAN_POINT('Ctrl Pts',(-0.843338895500463,-5.21972261836337,
384.016169157125));
#39830=CARTESIAN_POINT('Ctrl Pts',(-3.23075696562154,-4.18556258278454,
383.937041281665));
#39831=CARTESIAN_POINT('Ctrl Pts',(-4.74882528908407,-2.24901858620394,
383.862205947744));
#39832=CARTESIAN_POINT('Ctrl Pts',(-5.07309686007849,-0.703784911249602,
383.81374657231));
#39833=CARTESIAN_POINT('Ctrl Pts',(-5.07378290535392,0.000114313540020942,
383.791663155363));
#39834=CARTESIAN_POINT('Origin',(0.,0.,402.208336844637));
#39835=CARTESIAN_POINT('',(-5.07320349191978,4.67301704154544E-5,385.791663155363));
#39836=CARTESIAN_POINT('',(-5.07336681616767,0.000110749500208817,385.708336844637));
#39837=CARTESIAN_POINT('',(-5.0736,-1.59740085886799E-13,402.208336844637));
#39838=CARTESIAN_POINT('Ctrl Pts',(-5.07336681616767,0.000110749500209159,
385.708336844637));
#39839=CARTESIAN_POINT('Ctrl Pts',(-5.07358949400792,0.277204924762013,
385.699645625448));
#39840=CARTESIAN_POINT('Ctrl Pts',(-4.98354435800546,1.39507636552693,385.664578447772));
#39841=CARTESIAN_POINT('Ctrl Pts',(-4.1737680903862,3.24597977436508,385.60313531161));
#39842=CARTESIAN_POINT('Ctrl Pts',(-2.12031175571847,4.84365593601313,385.524007436151));
#39843=CARTESIAN_POINT('Ctrl Pts',(0.446542510511727,5.26852204647746,385.44487956069));
#39844=CARTESIAN_POINT('Ctrl Pts',(2.90527399685678,4.41770390260608,385.365751685231));
#39845=CARTESIAN_POINT('Ctrl Pts',(4.66054210967394,2.4972128487314,385.286623809771));
#39846=CARTESIAN_POINT('Ctrl Pts',(5.2873381133244,-0.0279364153108744,
385.207495934311));
#39847=CARTESIAN_POINT('Ctrl Pts',(4.63389386761938,-2.54632134491165,385.128368058852));
#39848=CARTESIAN_POINT('Ctrl Pts',(2.85842993763932,-4.44815726560116,385.049240183392));
#39849=CARTESIAN_POINT('Ctrl Pts',(0.390845137441743,-5.27294650517633,
384.970112307932));
#39850=CARTESIAN_POINT('Ctrl Pts',(-2.1713762578616,-4.82098018194518,384.890984432472));
#39851=CARTESIAN_POINT('Ctrl Pts',(-4.20783530881936,-3.2016943610792,384.811856557012));
#39852=CARTESIAN_POINT('Ctrl Pts',(-4.99079834853979,-1.35930215545066,
384.750974027734));
#39853=CARTESIAN_POINT('Ctrl Pts',(-5.07363898920769,-0.259332620176451,
384.716467456942));
#39854=CARTESIAN_POINT('Ctrl Pts',(-5.07341299508847,-0.000118529377325025,
384.708336844637));
#39855=CARTESIAN_POINT('Ctrl Pts',(-5.07320349191978,4.6730170415385E-5,
385.791663155363));
#39856=CARTESIAN_POINT('Ctrl Pts',(-5.07332318093048,0.368645452041058,
385.780102909322));
#39857=CARTESIAN_POINT('Ctrl Pts',(-4.94327787593756,1.57815905047111,385.742166704794));
#39858=CARTESIAN_POINT('Ctrl Pts',(-3.99220955212729,3.46684115546438,385.67785454178));
#39859=CARTESIAN_POINT('Ctrl Pts',(-1.85539526299902,4.95118502212943,385.59872666632));
#39860=CARTESIAN_POINT('Ctrl Pts',(0.73067187193628,5.23668247279509,385.51959879086));
#39861=CARTESIAN_POINT('Ctrl Pts',(3.13981906729605,4.25420508790564,385.440470915401));
#39862=CARTESIAN_POINT('Ctrl Pts',(4.78871173391359,2.24164328892807,385.361343039941));
#39863=CARTESIAN_POINT('Ctrl Pts',(5.27809816640793,-0.313694837508304,
385.282215164481));
#39864=CARTESIAN_POINT('Ctrl Pts',(4.48948164772799,-2.79307702006795,385.203087289022));
#39865=CARTESIAN_POINT('Ctrl Pts',(2.61381244185943,-4.59616244535579,385.123959413562));
#39866=CARTESIAN_POINT('Ctrl Pts',(0.105252389857621,-5.28636421747,385.044831538102));
#39867=CARTESIAN_POINT('Ctrl Pts',(-2.42879276314368,-4.69656155277656,
384.965703662642));
#39868=CARTESIAN_POINT('Ctrl Pts',(-4.3747464822184,-2.96956527485689,384.886575787182));
#39869=CARTESIAN_POINT('Ctrl Pts',(-5.02482764874857,-1.17623295765146,
384.828562284756));
#39870=CARTESIAN_POINT('Ctrl Pts',(-5.0738588771301,-0.167845167351579,
384.796924740816));
#39871=CARTESIAN_POINT('Ctrl Pts',(-5.07368788828891,-0.000125377980982003,
384.791663155363));
#39872=CARTESIAN_POINT('Origin',(0.,0.,402.208336844637));
#39873=CARTESIAN_POINT('',(-5.07396871057133,6.36451556410011E-5,386.791663155363));
#39874=CARTESIAN_POINT('',(-5.07402204930561,-2.85592496231871E-5,386.708336844637));
#39875=CARTESIAN_POINT('',(-5.0736,-1.59740085886799E-13,402.208336844637));
#39876=CARTESIAN_POINT('Ctrl Pts',(-5.07402204930561,-2.85592496232024E-5,
386.708336844637));
#39877=CARTESIAN_POINT('Ctrl Pts',(-5.07376894837123,0.813077680770696,
386.682823793954));
#39878=CARTESIAN_POINT('Ctrl Pts',(-4.66877404608003,2.46703434122352,386.630934784784));
#39879=CARTESIAN_POINT('Ctrl Pts',(-2.95361232316089,4.38553292227813,386.552669817127));
#39880=CARTESIAN_POINT('Ctrl Pts',(-0.504372453036948,5.26330059910421,
386.473541941668));
#39881=CARTESIAN_POINT('Ctrl Pts',(2.06699274767947,4.86664830750627,386.394414066208));
#39882=CARTESIAN_POINT('Ctrl Pts',(4.1378703204085,3.29161874757629,386.315286190749));
#39883=CARTESIAN_POINT('Ctrl Pts',(5.20683199193,0.919578912180737,386.236158315288));
#39884=CARTESIAN_POINT('Ctrl Pts',(5.01504662121074,-1.67512153439562,386.157030439829));
#39885=CARTESIAN_POINT('Ctrl Pts',(3.60895181930755,-3.86421939514695,386.077902564369));
#39886=CARTESIAN_POINT('Ctrl Pts',(1.32900986066236,-5.11766133679979,385.998774688909));
#39887=CARTESIAN_POINT('Ctrl Pts',(-1.2727295467071,-5.13194741485647,385.91964681345));
#39888=CARTESIAN_POINT('Ctrl Pts',(-3.5662988394905,-3.90361849510962,385.84051893799));
#39889=CARTESIAN_POINT('Ctrl Pts',(-4.83927537814081,-1.96882864770619,
385.770082281719));
#39890=CARTESIAN_POINT('Ctrl Pts',(-5.07291371523136,-0.563715584161085,
385.726021583935));
#39891=CARTESIAN_POINT('Ctrl Pts',(-5.07336681616767,0.000110749500209159,
385.708336844637));
#39892=CARTESIAN_POINT('Ctrl Pts',(-5.07396871057133,6.36451556408537E-5,
386.791663155363));
#39893=CARTESIAN_POINT('Ctrl Pts',(-5.07400891965194,0.0640010310039327,
386.789657036314));
#39894=CARTESIAN_POINT('Ctrl Pts',(-5.05726353871135,0.968550309919132,
386.761274958779));
#39895=CARTESIAN_POINT('Ctrl Pts',(-4.54862274572651,2.695692085973,386.706516922757));
#39896=CARTESIAN_POINT('Ctrl Pts',(-2.71224074091265,4.53877459989496,386.627389047297));
#39897=CARTESIAN_POINT('Ctrl Pts',(-0.219135128106394,5.28286896496098,
386.548261171838));
#39898=CARTESIAN_POINT('Ctrl Pts',(2.32703038082081,4.74780520999492,386.469133296378));
#39899=CARTESIAN_POINT('Ctrl Pts',(4.30974451002784,3.06314004962277,386.390005420918));
#39900=CARTESIAN_POINT('Ctrl Pts',(5.24892628554031,0.636786898642001,386.310877545458));
#39901=CARTESIAN_POINT('Ctrl Pts',(4.91716859158436,-1.94375352019086,386.231749669999));
#39902=CARTESIAN_POINT('Ctrl Pts',(3.39480098979053,-4.05364662310803,386.152621794539));
#39903=CARTESIAN_POINT('Ctrl Pts',(1.05043926306477,-5.18201718059,386.073493919079));
#39904=CARTESIAN_POINT('Ctrl Pts',(-1.54826871412865,-5.0556491862241,385.994366043619));
#39905=CARTESIAN_POINT('Ctrl Pts',(-3.772089388456,-3.70514053050835,385.91523816816));
#39906=CARTESIAN_POINT('Ctrl Pts',(-4.89110742269369,-1.78586579845603,
385.84767053874));
#39907=CARTESIAN_POINT('Ctrl Pts',(-5.07305009743672,-0.472352615975399,
385.806478867808));
#39908=CARTESIAN_POINT('Ctrl Pts',(-5.07320349191978,4.6730170415385E-5,
385.791663155363));
#39909=CARTESIAN_POINT('Origin',(0.,0.,402.208336844637));
#39910=CARTESIAN_POINT('',(-5.07346461004462,-0.000124534794222197,387.791663155363));
#39911=CARTESIAN_POINT('',(-5.07325209134275,-7.62409538748165E-5,387.708336844637));
#39912=CARTESIAN_POINT('',(-5.0736,-1.59740085886799E-13,402.208336844637));
#39913=CARTESIAN_POINT('Ctrl Pts',(-5.07325209134275,-7.62409538748038E-5,
387.708336844637));
#39914=CARTESIAN_POINT('Ctrl Pts',(-5.0729792152731,0.508760470280088,387.692377920946));
#39915=CARTESIAN_POINT('Ctrl Pts',(-4.87111972002504,1.85878392032608,387.650043038769));
#39916=CARTESIAN_POINT('Ctrl Pts',(-3.69137763771595,3.78555886279474,387.581332198105));
#39917=CARTESIAN_POINT('Ctrl Pts',(-1.43897337649567,5.08783651365194,387.502204322645));
#39918=CARTESIAN_POINT('Ctrl Pts',(1.16185415459233,5.15817988164137,387.423076447186));
#39919=CARTESIAN_POINT('Ctrl Pts',(3.48135818778607,3.97955649994419,387.343948571725));
#39920=CARTESIAN_POINT('Ctrl Pts',(4.95790972221771,1.83735025355874,387.264820696266));
#39921=CARTESIAN_POINT('Ctrl Pts',(5.23398656730458,-0.749739542233496,
387.185692820806));
#39922=CARTESIAN_POINT('Ctrl Pts',(4.24274134513742,-3.15529248187465,387.106564945346));
#39923=CARTESIAN_POINT('Ctrl Pts',(2.22418746193322,-4.79684426494046,387.027437069886));
#39924=CARTESIAN_POINT('Ctrl Pts',(-0.332916112977428,-5.27692065788687,
386.948309194427));
#39925=CARTESIAN_POINT('Ctrl Pts',(-2.80940963451955,-4.47927921359921,
386.869181318967));
#39926=CARTESIAN_POINT('Ctrl Pts',(-4.6056517301173,-2.59705543044056,386.790053443507));
#39927=CARTESIAN_POINT('Ctrl Pts',(-5.06711936969965,-0.895633636916161,
386.73643861873));
#39928=CARTESIAN_POINT('Ctrl Pts',(-5.07403060973901,-0.0275296106999626,
386.70919975244));
#39929=CARTESIAN_POINT('Ctrl Pts',(-5.07402204930561,-2.85592496232024E-5,
386.708336844637));
#39930=CARTESIAN_POINT('Ctrl Pts',(-5.07346461004462,-0.000124534794222232,
387.791663155363));
#39931=CARTESIAN_POINT('Ctrl Pts',(-5.07290587442459,0.600116546096426,
387.77283520482));
#39932=CARTESIAN_POINT('Ctrl Pts',(-4.81706146775411,2.04169530250574,387.727631295791));
#39933=CARTESIAN_POINT('Ctrl Pts',(-3.48135818389009,3.97955649548785,387.656051428275));
#39934=CARTESIAN_POINT('Ctrl Pts',(-1.16185415329344,5.15817987586638,387.576923552815));
#39935=CARTESIAN_POINT('Ctrl Pts',(1.43897337488296,5.0878365079566,387.497795677355));
#39936=CARTESIAN_POINT('Ctrl Pts',(3.69137763358211,3.7855588585581,387.418667801895));
#39937=CARTESIAN_POINT('Ctrl Pts',(5.04997670698908,1.56667161976776,387.339539926436));
#39938=CARTESIAN_POINT('Ctrl Pts',(5.1858086147589,-1.03155887685117,387.260412050976));
#39939=CARTESIAN_POINT('Ctrl Pts',(4.06598393848355,-3.38001469187811,387.181284175516));
#39940=CARTESIAN_POINT('Ctrl Pts',(1.96164944276588,-4.91005663602919,387.102156300056));
#39941=CARTESIAN_POINT('Ctrl Pts',(-0.617665566383616,-5.25121071310437,
387.023028424596));
#39942=CARTESIAN_POINT('Ctrl Pts',(-3.04742321760052,-4.32087218488899,
386.943900549136));
#39943=CARTESIAN_POINT('Ctrl Pts',(-4.69640454618417,-2.39441853297418,
386.866778792725));
#39944=CARTESIAN_POINT('Ctrl Pts',(-5.07348026057684,-0.776631949401611,
386.816032994801));
#39945=CARTESIAN_POINT('Ctrl Pts',(-5.07396871057133,6.36451556408537E-5,
386.791663155363));
#39946=CARTESIAN_POINT('Origin',(0.,0.,402.208336844637));
#39947=CARTESIAN_POINT('',(-5.07332308908166,0.000100751512192854,388.791663155363));
#39948=CARTESIAN_POINT('',(-5.07357378438926,0.00012964408007953,388.708336844637));
#39949=CARTESIAN_POINT('',(-5.0736,-1.59740085886799E-13,402.208336844637));
#39950=CARTESIAN_POINT('Ctrl Pts',(-5.07357378438926,0.000129644080079632,
388.708336844637));
#39951=CARTESIAN_POINT('Ctrl Pts',(-5.07377922823885,0.204303981988881,
388.701932047939));
#39952=CARTESIAN_POINT('Ctrl Pts',(-5.01188528533374,1.24917654214382,388.669151292754));
#39953=CARTESIAN_POINT('Ctrl Pts',(-4.30974451485365,3.06314005305047,388.609994579082));
#39954=CARTESIAN_POINT('Ctrl Pts',(-2.32703038342756,4.74780521530929,388.530866703622));
#39955=CARTESIAN_POINT('Ctrl Pts',(0.2191351283499,5.28286897087523,388.451738828163));
#39956=CARTESIAN_POINT('Ctrl Pts',(2.71224074394742,4.53877460497707,388.372610952702));
#39957=CARTESIAN_POINT('Ctrl Pts',(4.54862275081774,2.69569208899244,388.293483077243));
#39958=CARTESIAN_POINT('Ctrl Pts',(5.28363204425109,0.199892943537846,388.214355201783));
#39959=CARTESIAN_POINT('Ctrl Pts',(4.73929845080001,-2.34430692575821,388.135227326323));
#39960=CARTESIAN_POINT('Ctrl Pts',(3.04742322101362,-4.32087218972514,388.056099450863));
#39961=CARTESIAN_POINT('Ctrl Pts',(0.617665567076949,-5.25121071898288,
387.976971575404));
#39962=CARTESIAN_POINT('Ctrl Pts',(-1.96164944496022,-4.9100566415267,387.897843699944));
#39963=CARTESIAN_POINT('Ctrl Pts',(-4.06598394303424,-3.38001469566346,
387.818715824484));
#39964=CARTESIAN_POINT('Ctrl Pts',(-4.95995652391698,-1.50520772763894,
387.755546872715));
#39965=CARTESIAN_POINT('Ctrl Pts',(-5.07343020858722,-0.332214537305361,
387.718753879433));
#39966=CARTESIAN_POINT('Ctrl Pts',(-5.07325209134275,-7.62409538748038E-5,
387.708336844637));
#39967=CARTESIAN_POINT('Ctrl Pts',(-5.07332308908166,0.000100751512193097,
388.791663155363));
#39968=CARTESIAN_POINT('Ctrl Pts',(-5.07353661258784,0.295776873009828,
388.782389331812));
#39969=CARTESIAN_POINT('Ctrl Pts',(-4.97579423080698,1.43225469143156,388.746739549775));
#39970=CARTESIAN_POINT('Ctrl Pts',(-4.13787031577727,3.29161874388992,388.684713809251));
#39971=CARTESIAN_POINT('Ctrl Pts',(-2.0669927453671,4.86664830205737,388.605585933792));
#39972=CARTESIAN_POINT('Ctrl Pts',(0.504372452470541,5.2633005932121,388.526458058332));
#39973=CARTESIAN_POINT('Ctrl Pts',(2.95361231985281,4.38553291736953,388.447330182872));
#39974=CARTESIAN_POINT('Ctrl Pts',(4.68768449948338,2.44588199605403,388.368202307412));
#39975=CARTESIAN_POINT('Ctrl Pts',(5.28671249546426,-0.0859982303311033,
388.289074431953));
#39976=CARTESIAN_POINT('Ctrl Pts',(4.60565172496217,-2.59705542753155,388.209946556493));
#39977=CARTESIAN_POINT('Ctrl Pts',(2.80940963137597,-4.47927920858367,388.130818681033));
#39978=CARTESIAN_POINT('Ctrl Pts',(0.332916112606594,-5.27692065197923,
388.051690805573));
#39979=CARTESIAN_POINT('Ctrl Pts',(-2.22418745944155,-4.79684425957118,
387.972562930114));
#39980=CARTESIAN_POINT('Ctrl Pts',(-4.24274134038657,-3.15529247834378,
387.893435054654));
#39981=CARTESIAN_POINT('Ctrl Pts',(-4.99812636818859,-1.3221248286521,387.833135129737));
#39982=CARTESIAN_POINT('Ctrl Pts',(-5.07368860366989,-0.240757440453781,
387.799211163307));
#39983=CARTESIAN_POINT('Ctrl Pts',(-5.07346461004462,-0.000124534794222232,
387.791663155363));
#39984=CARTESIAN_POINT('Origin',(0.,0.,402.208336844637));
#39985=CARTESIAN_POINT('',(-5.07403406771079,-9.36144982375056E-6,389.791663155363));
#39986=CARTESIAN_POINT('',(-5.07388549569213,-9.2912700738374E-5,389.708336844637));
#39987=CARTESIAN_POINT('',(-5.0736,-1.59740085886799E-13,402.208336844637));
#39988=CARTESIAN_POINT('Ctrl Pts',(-5.07388549569213,-9.2912700738277E-5,
389.708336844637));
#39989=CARTESIAN_POINT('Ctrl Pts',(-5.07325856807114,0.740202389523463,
389.685110216444));
#39990=CARTESIAN_POINT('Ctrl Pts',(-4.72308495981242,2.32174429013103,389.635507629765));
#39991=CARTESIAN_POINT('Ctrl Pts',(-3.13981907081257,4.25420509266713,389.559529084599));
#39992=CARTESIAN_POINT('Ctrl Pts',(-0.730671872756092,5.23668247865729,
389.48040120914));
#39993=CARTESIAN_POINT('Ctrl Pts',(1.85539526507438,4.95118502767294,389.401273333679));
#39994=CARTESIAN_POINT('Ctrl Pts',(3.99220955659535,3.46684115934693,389.32214545822));
#39995=CARTESIAN_POINT('Ctrl Pts',(5.16237725796638,1.14305984722794,389.24301758276));
#39996=CARTESIAN_POINT('Ctrl Pts',(5.08256188536855,-1.45749423645932,389.1638897073));
#39997=CARTESIAN_POINT('Ctrl Pts',(3.77208939268016,-3.70514053465492,389.08476183184));
#39998=CARTESIAN_POINT('Ctrl Pts',(1.54826871586373,-5.05564919188336,389.005633956381));
#39999=CARTESIAN_POINT('Ctrl Pts',(-1.05043926423896,-5.18201718639165,
388.926506080921));
#40000=CARTESIAN_POINT('Ctrl Pts',(-3.39480099358967,-4.05364662764723,
388.847378205461));
#40001=CARTESIAN_POINT('Ctrl Pts',(-4.79394457591898,-2.1145332421108,388.7746551267));
#40002=CARTESIAN_POINT('Ctrl Pts',(-5.07293317820744,-0.636518001009154,
388.728308006425));
#40003=CARTESIAN_POINT('Ctrl Pts',(-5.07357378438926,0.000129644080079632,
388.708336844637));
#40004=CARTESIAN_POINT('Ctrl Pts',(-5.07403406771079,-9.36144982382212E-6,
389.791663155363));
#40005=CARTESIAN_POINT('Ctrl Pts',(-5.07394412729799,0.831658855747162,
389.765567500318));
#40006=CARTESIAN_POINT('Ctrl Pts',(-4.65432422371577,2.50401601420859,389.713095886787));
#40007=CARTESIAN_POINT('Ctrl Pts',(-2.90527399360582,4.41770389765948,389.634248314769));
#40008=CARTESIAN_POINT('Ctrl Pts',(-0.446542510013585,5.2685220405792,389.55512043931));
#40009=CARTESIAN_POINT('Ctrl Pts',(2.12031175334316,4.84365593059135,389.475992563849));
#40010=CARTESIAN_POINT('Ctrl Pts',(4.17376808571255,3.24597977073262,389.39686468839));
#40011=CARTESIAN_POINT('Ctrl Pts',(5.21661647505316,0.862344048232485,389.31773681293));
#40012=CARTESIAN_POINT('Ctrl Pts',(4.99634867366186,-1.73009382303836,389.23860893747));
#40013=CARTESIAN_POINT('Ctrl Pts',(3.56629883549932,-3.90361849073832,389.15948106201));
#40014=CARTESIAN_POINT('Ctrl Pts',(1.27272954528402,-5.13194740911081,389.08035318655));
#40015=CARTESIAN_POINT('Ctrl Pts',(-1.3290098591728,-5.11766133107102,389.001225311091));
#40016=CARTESIAN_POINT('Ctrl Pts',(-3.60895181526604,-3.86421939082217,
388.922097435631));
#40017=CARTESIAN_POINT('Ctrl Pts',(-4.85025165556801,-1.93168481258741,
388.852243383721));
#40018=CARTESIAN_POINT('Ctrl Pts',(-5.07292932400786,-0.545164413360684,
388.808765290299));
#40019=CARTESIAN_POINT('Ctrl Pts',(-5.07332308908166,0.000100751512193097,
388.791663155363));
#40020=CARTESIAN_POINT('Origin',(0.,0.,402.208336844637));
#40021=CARTESIAN_POINT('',(-5.0732856633921,-8.9472558095216E-5,390.791663155363));
#40022=CARTESIAN_POINT('',(-5.07317963304504,-1.41915822972106E-5,390.708336844637));
#40023=CARTESIAN_POINT('',(-5.0736,-1.59740085886799E-13,402.208336844637));
#40024=CARTESIAN_POINT('Ctrl Pts',(-5.07317963304504,-1.41915822972002E-5,
390.708336844637));
#40025=CARTESIAN_POINT('Ctrl Pts',(-5.07313689101218,0.435939705489138,
390.694664343437));
#40026=CARTESIAN_POINT('Ctrl Pts',(-4.9102234101679,1.71293434968472,390.65461588375));
#40027=CARTESIAN_POINT('Ctrl Pts',(-3.85104960630393,3.62300175237324,390.588191465576));
#40028=CARTESIAN_POINT('Ctrl Pts',(-1.65684512829777,5.02111431743484,390.509063590116));
#40029=CARTESIAN_POINT('Ctrl Pts',(0.938536610313288,5.20344826043412,390.429935714657));
#40030=CARTESIAN_POINT('Ctrl Pts',(3.30666744908329,4.12585447502528,390.350807839197));
#40031=CARTESIAN_POINT('Ctrl Pts',(4.874144221702,2.04925422384882,390.271679963737));
#40032=CARTESIAN_POINT('Ctrl Pts',(5.26142871608132,-0.523538569265068,
390.192552088277));
#40033=CARTESIAN_POINT('Ctrl Pts',(4.37474648711696,-2.96956527817979,390.113424212818));
#40034=CARTESIAN_POINT('Ctrl Pts',(2.42879276586438,-4.69656155803349,390.034296337358));
#40035=CARTESIAN_POINT('Ctrl Pts',(-0.105252389973582,-5.28636422338813,
389.955168461898));
#40036=CARTESIAN_POINT('Ctrl Pts',(-2.61381244478399,-4.59616245050211,
389.876040586438));
#40037=CARTESIAN_POINT('Ctrl Pts',(-4.48948165275299,-2.79307702319636,
389.796912710979));
#40038=CARTESIAN_POINT('Ctrl Pts',(-5.04661334373894,-1.04147487532298,
389.741011463711));
#40039=CARTESIAN_POINT('Ctrl Pts',(-5.07397050166598,-0.10047056555588,
389.711486174931));
#40040=CARTESIAN_POINT('Ctrl Pts',(-5.07388549569213,-9.2912700738277E-5,
389.708336844637));
#40041=CARTESIAN_POINT('Ctrl Pts',(-5.0732856633921,-8.94725580950079E-5,
390.791663155363));
#40042=CARTESIAN_POINT('Ctrl Pts',(-5.07295082938292,0.527313084285289,
390.77512162731));
#40043=CARTESIAN_POINT('Ctrl Pts',(-4.86059546998445,1.89593815106623,390.732204140772));
#40044=CARTESIAN_POINT('Ctrl Pts',(-3.64958350306562,3.82586787010077,390.662910695746));
#40045=CARTESIAN_POINT('Ctrl Pts',(-1.38301395488213,5.10333196117197,390.583782820286));
#40046=CARTESIAN_POINT('Ctrl Pts',(1.21842922772966,5.14510980663504,390.504654944826));
#40047=CARTESIAN_POINT('Ctrl Pts',(3.52485020731651,3.94108560187402,390.425527069367));
#40048=CARTESIAN_POINT('Ctrl Pts',(4.97778782502355,1.78279361519087,390.346399193907));
#40049=CARTESIAN_POINT('Ctrl Pts',(5.2254376041702,-0.807171945896316,390.267271318447));
#40050=CARTESIAN_POINT('Ctrl Pts',(4.2078353041098,-3.20169435749343,390.188143442988));
#40051=CARTESIAN_POINT('Ctrl Pts',(2.17137625543244,-4.82098017654731,390.109015567527));
#40052=CARTESIAN_POINT('Ctrl Pts',(-0.390845137002325,-5.27294649927341,
390.029887692068));
#40053=CARTESIAN_POINT('Ctrl Pts',(-2.85842993443779,-4.44815726062243,
389.950759816608));
#40054=CARTESIAN_POINT('Ctrl Pts',(-4.63389386243089,-2.54632134206259,
389.871631941148));
#40055=CARTESIAN_POINT('Ctrl Pts',(-5.07183812704173,-0.858476903537314,
389.818599720733));
#40056=CARTESIAN_POINT('Ctrl Pts',(-5.07403503379527,-0.00894262882346251,
389.791943458805));
#40057=CARTESIAN_POINT('Ctrl Pts',(-5.07403406771079,-9.36144982382212E-6,
389.791663155363));
#40058=CARTESIAN_POINT('Origin',(0.,0.,402.208336844637));
#40059=CARTESIAN_POINT('',(-5.07351709598447,0.000128180283586465,391.791663155363));
#40060=CARTESIAN_POINT('',(-5.07379939980891,0.000111618004047815,391.708336844637));
#40061=CARTESIAN_POINT('',(-5.0736,-1.59740085886799E-13,402.208336844637));
#40062=CARTESIAN_POINT('Ctrl Pts',(-5.07379939980891,0.000111618004048301,
391.708336844637));
#40063=CARTESIAN_POINT('Ctrl Pts',(-5.07392549945089,0.131381756589591,
391.704218470429));
#40064=CARTESIAN_POINT('Ctrl Pts',(-5.03695972030326,1.10329526429473,391.673724137734));
#40065=CARTESIAN_POINT('Ctrl Pts',(-4.43771707875037,2.8746116080056,391.616853846554));
#40066=CARTESIAN_POINT('Ctrl Pts',(-2.52942735664669,4.64313708771996,391.537725971094));
#40067=CARTESIAN_POINT('Ctrl Pts',(-0.00867922155838994,5.28740479243137,
391.458598095634));
#40068=CARTESIAN_POINT('Ctrl Pts',(2.51417044146968,4.65141610255989,391.379470220174));
#40069=CARTESIAN_POINT('Ctrl Pts',(4.42825589764708,2.88916501309064,391.300342344714));
#40070=CARTESIAN_POINT('Ctrl Pts',(5.27011345519119,0.427351070346123,391.221214469255));
#40071=CARTESIAN_POINT('Ctrl Pts',(4.8359014254693,-2.1379387669101,391.142086593795));
#40072=CARTESIAN_POINT('Ctrl Pts',(3.23075696923981,-4.18556258746916,391.062958718335));
#40073=CARTESIAN_POINT('Ctrl Pts',(0.843338896446427,-5.21972262420654,
390.983830842875));
#40074=CARTESIAN_POINT('Ctrl Pts',(-1.7482795463511,-4.99001436828829,390.904702967415));
#40075=CARTESIAN_POINT('Ctrl Pts',(-3.91658141767327,-3.55205782141137,
390.825575091956));
#40076=CARTESIAN_POINT('Ctrl Pts',(-4.92575069087544,-1.65110613686035,
390.760119717696));
#40077=CARTESIAN_POINT('Ctrl Pts',(-5.07321934571947,-0.405069684288436,
390.721040301923));
#40078=CARTESIAN_POINT('Ctrl Pts',(-5.07317963304504,-1.41915822972002E-5,
390.708336844637));
#40079=CARTESIAN_POINT('Ctrl Pts',(-5.07351709598447,0.0001281802835865,
391.791663155363));
#40080=CARTESIAN_POINT('Ctrl Pts',(-5.07373426530186,0.222882138466162,
391.784675754303));
#40081=CARTESIAN_POINT('Ctrl Pts',(-5.00497588579108,1.28635201118677,391.751312394756));
#40082=CARTESIAN_POINT('Ctrl Pts',(-4.27584641576499,3.1102832884012,391.691573076723));
#40083=CARTESIAN_POINT('Ctrl Pts',(-2.27475150326393,4.77307346514974,391.612445201264));
#40084=CARTESIAN_POINT('Ctrl Pts',(0.277136335534271,5.28014395228432,391.533317325804));
#40085=CARTESIAN_POINT('Ctrl Pts',(2.76192025858026,4.50871613550486,391.454189450344));
#40086=CARTESIAN_POINT('Ctrl Pts',(4.57795151161372,2.64557832290629,391.375061574885));
#40087=CARTESIAN_POINT('Ctrl Pts',(5.28550858366077,0.141858088829558,391.295933699424));
#40088=CARTESIAN_POINT('Ctrl Pts',(4.71326839627705,-2.39621070233275,391.216805823965));
#40089=CARTESIAN_POINT('Ctrl Pts',(2.99978931370662,-4.35407725915487,391.137677948505));
#40090=CARTESIAN_POINT('Ctrl Pts',(0.559961558764467,-5.2576770305929,391.058550073045));
#40091=CARTESIAN_POINT('Ctrl Pts',(-2.01545149642842,-4.88821848640817,
390.979422197585));
#40092=CARTESIAN_POINT('Ctrl Pts',(-4.10285677321784,-3.33515981682715,
390.900294322126));
#40093=CARTESIAN_POINT('Ctrl Pts',(-4.96813235745424,-1.46802940120253,
390.837707974718));
#40094=CARTESIAN_POINT('Ctrl Pts',(-5.07348473216978,-0.313645979534272,
390.801497585797));
#40095=CARTESIAN_POINT('Ctrl Pts',(-5.0732856633921,-8.94725580950079E-5,
390.791663155363));
#40096=CARTESIAN_POINT('Origin',(0.,0.,402.208336844637));
#40097=CARTESIAN_POINT('',(-5.07393095917883,-7.88724074329838E-5,392.791663155363));
#40098=CARTESIAN_POINT('',(-5.07367047787857,-0.000126645267990005,392.708336844637));
#40099=CARTESIAN_POINT('',(-5.0736,-1.59740085886799E-13,402.208336844637));
#40100=CARTESIAN_POINT('Ctrl Pts',(-5.07367047787857,-0.000126645267989993,
392.708336844637));
#40101=CARTESIAN_POINT('Ctrl Pts',(-5.07298837013062,0.667375891727513,
392.687396638935));
#40102=CARTESIAN_POINT('Ctrl Pts',(-4.77363543308555,2.17624796267435,392.640080474746));
#40103=CARTESIAN_POINT('Ctrl Pts',(-3.32019468996614,4.11497654776232,392.566388352071));
#40104=CARTESIAN_POINT('Ctrl Pts',(-0.955614322062658,5.20033903081154,
392.487260476611));
#40105=CARTESIAN_POINT('Ctrl Pts',(1.64035202716895,5.02652663326038,392.408132601151));
#40106=CARTESIAN_POINT('Ctrl Pts',(3.83913464362559,3.63562511214056,392.329004725691));
#40107=CARTESIAN_POINT('Ctrl Pts',(5.10833519286426,1.36441794376124,392.249876850232));
#40108=CARTESIAN_POINT('Ctrl Pts',(5.14063804785052,-1.23716014683014,392.170748974772));
#40109=CARTESIAN_POINT('Ctrl Pts',(3.92822161400576,-3.53918065647562,392.091621099312));
#40110=CARTESIAN_POINT('Ctrl Pts',(1.76465219715718,-4.98424792631562,392.012493223852));
#40111=CARTESIAN_POINT('Ctrl Pts',(-0.826198153971171,-5.22246315241074,
391.933365348392));
#40112=CARTESIAN_POINT('Ctrl Pts',(-3.21699847841567,-4.19614651290735,
391.854237472933));
#40113=CARTESIAN_POINT('Ctrl Pts',(-4.74496408021847,-2.26010134957161,
391.779227971681));
#40114=CARTESIAN_POINT('Ctrl Pts',(-5.07311789947229,-0.7093324551461,391.730594428916));
#40115=CARTESIAN_POINT('Ctrl Pts',(-5.07379939980891,0.000111618004048301,
391.708336844637));
#40116=CARTESIAN_POINT('Ctrl Pts',(-5.07393095917883,-7.88724074328884E-5,
392.791663155363));
#40117=CARTESIAN_POINT('Ctrl Pts',(-5.07336361274665,0.758765898971362,
392.767853922809));
#40118=CARTESIAN_POINT('Ctrl Pts',(-4.7096061531202,2.35878746105711,392.717668731768));
#40119=CARTESIAN_POINT('Ctrl Pts',(-3.09291170420029,4.28842883762094,392.64110758224));
#40120=CARTESIAN_POINT('Ctrl Pts',(-0.67312059357683,5.24439065781915,392.561979706781));
#40121=CARTESIAN_POINT('Ctrl Pts',(1.90965537976903,4.9305112347339,392.482851831321));
#40122=CARTESIAN_POINT('Ctrl Pts',(4.03004033003705,3.4227912065437,392.403723955861));
#40123=CARTESIAN_POINT('Ctrl Pts',(5.17461860283211,1.0862996918631,392.324596080401));
#40124=CARTESIAN_POINT('Ctrl Pts',(5.06624976530063,-1.51322107469774,392.245468204942));
#40125=CARTESIAN_POINT('Ctrl Pts',(3.73117351397988,-3.74634073649114,392.166340329482));
#40126=CARTESIAN_POINT('Ctrl Pts',(1.49265617235166,-5.07234681941786,392.087212454022));
#40127=CARTESIAN_POINT('Ctrl Pts',(-1.10728282783815,-5.1701691891555,392.008084578562));
#40128=CARTESIAN_POINT('Ctrl Pts',(-3.43911186168285,-4.01612179946654,
391.928956703103));
#40129=CARTESIAN_POINT('Ctrl Pts',(-4.80583883513493,-2.07741741105628,
391.856816228703));
#40130=CARTESIAN_POINT('Ctrl Pts',(-5.07291449714329,-0.617966855796078,
391.811051712789));
#40131=CARTESIAN_POINT('Ctrl Pts',(-5.07351709598447,0.0001281802835865,
391.791663155363));
#40132=CARTESIAN_POINT('Origin',(0.,0.,402.208336844637));
#40133=CARTESIAN_POINT('',(-5.07318860167667,-3.10232113821807E-5,393.791663155363));
#40134=CARTESIAN_POINT('',(-5.07320934784751,5.14726455261062E-5,393.708336844637));
#40135=CARTESIAN_POINT('',(-5.0736,-1.59740085886799E-13,402.208336844637));
#40136=CARTESIAN_POINT('Ctrl Pts',(-5.07320934784751,5.14726455259906E-5,
393.708336844637));
#40137=CARTESIAN_POINT('Ctrl Pts',(-5.07333938414724,0.363095667172288,
393.696950765927));
#40138=CARTESIAN_POINT('Ctrl Pts',(-4.94587345760415,1.56704518273248,393.659188728731));
#40139=CARTESIAN_POINT('Ctrl Pts',(-4.00356958154437,3.45371616865744,393.595050733048));
#40140=CARTESIAN_POINT('Ctrl Pts',(-1.8716398630404,4.94506713715712,393.515922857588));
#40141=CARTESIAN_POINT('Ctrl Pts',(0.713476058729831,5.23905303289941,393.436794982128));
#40142=CARTESIAN_POINT('Ctrl Pts',(3.12583571869877,4.26449010171441,393.357667106669));
#40143=CARTESIAN_POINT('Ctrl Pts',(4.78132668327137,2.25735241283907,393.278539231209));
#40144=CARTESIAN_POINT('Ctrl Pts',(5.2790995798779,-0.296365304389928,393.199411355749));
#40145=CARTESIAN_POINT('Ctrl Pts',(4.49862704983328,-2.77832313355043,393.120283480289));
#40146=CARTESIAN_POINT('Ctrl Pts',(2.62888742685924,-4.58755661161959,393.041155604829));
#40147=CARTESIAN_POINT('Ctrl Pts',(0.122606802959192,-5.28599019482455,
392.96202772937));
#40148=CARTESIAN_POINT('Ctrl Pts',(-2.41336100201929,-4.70450990453263,
392.88289985391));
#40149=CARTESIAN_POINT('Ctrl Pts',(-4.3649739152189,-2.98391144093985,392.80377197845));
#40150=CARTESIAN_POINT('Ctrl Pts',(-5.02290836650147,-1.18734550240995,
392.745584308693));
#40151=CARTESIAN_POINT('Ctrl Pts',(-5.07384754247588,-0.173399956222615,
392.713772597422));
#40152=CARTESIAN_POINT('Ctrl Pts',(-5.07367047787857,-0.000126645267989993,
392.708336844637));
#40153=CARTESIAN_POINT('Ctrl Pts',(-5.07318860167666,-3.10232113822501E-5,
393.791663155363));
#40154=CARTESIAN_POINT('Ctrl Pts',(-5.07309097404724,0.454497176795154,
393.777408049801));
#40155=CARTESIAN_POINT('Ctrl Pts',(-4.90058989979703,1.75010317897161,393.736776985753));
#40156=CARTESIAN_POINT('Ctrl Pts',(-3.81103098253419,3.66507401773587,393.669769963218));
#40157=CARTESIAN_POINT('Ctrl Pts',(-1.60160528615343,5.03900637156607,393.590642087758));
#40158=CARTESIAN_POINT('Ctrl Pts',(0.995622269493122,5.19282784249655,393.511514212298));
#40159=CARTESIAN_POINT('Ctrl Pts',(3.3517765903209,4.08929314110579,393.432386336838));
#40160=CARTESIAN_POINT('Ctrl Pts',(4.89635442297923,1.99560468778007,393.353258461378));
#40161=CARTESIAN_POINT('Ctrl Pts',(5.2553621496497,-0.581285972088894,393.274130585919));
#40162=CARTESIAN_POINT('Ctrl Pts',(4.34187207029457,-3.01742798265574,393.195002710459));
#40163=CARTESIAN_POINT('Ctrl Pts',(2.37707048734272,-4.72295041298575,393.115874834999));
#40164=CARTESIAN_POINT('Ctrl Pts',(-0.163298847893048,-5.28488961016167,
393.03674695954));
#40165=CARTESIAN_POINT('Ctrl Pts',(-2.66412810582239,-4.56718142195876,
392.957619084079));
#40166=CARTESIAN_POINT('Ctrl Pts',(-4.51988342344183,-2.74360684935247,
392.87849120862));
#40167=CARTESIAN_POINT('Ctrl Pts',(-5.05214048257081,-1.00431002992741,
392.823172565714));
#40168=CARTESIAN_POINT('Ctrl Pts',(-5.07399212128462,-0.0818852283646697,
392.794229881295));
#40169=CARTESIAN_POINT('Ctrl Pts',(-5.07393095917883,-7.88724074328884E-5,
392.791663155363));
#40170=CARTESIAN_POINT('Origin',(0.,0.,402.208336844637));
#40171=CARTESIAN_POINT('',(-5.07374340439062,0.000119799015104727,394.791663155363));
#40172=CARTESIAN_POINT('',(-5.07397904538501,5.86126803115486E-5,394.708336844637));
#40173=CARTESIAN_POINT('',(-5.0736,-1.59740085886799E-13,402.208336844637));
#40174=CARTESIAN_POINT('Ctrl Pts',(-5.07397904538501,5.86126803111056E-5,
394.708336844637));
#40175=CARTESIAN_POINT('Ctrl Pts',(-5.07401332726156,0.0584447346541764,
394.706504892919));
#40176=CARTESIAN_POINT('Ctrl Pts',(-5.05881623778616,0.957440994697868,
394.678296982715));
#40177=CARTESIAN_POINT('Ctrl Pts',(-4.55744811727866,2.68074456564335,394.623713114025));
#40178=CARTESIAN_POINT('Ctrl Pts',(-2.72712679296628,4.52984593810856,394.544585238565));
#40179=CARTESIAN_POINT('Ctrl Pts',(-0.236477452813074,5.28212108742541,
394.465457363106));
#40180=CARTESIAN_POINT('Ctrl Pts',(2.31143093653793,4.75541920271268,394.386329487645));
#40181=CARTESIAN_POINT('Ctrl Pts',(4.29966508998112,3.07727231195273,394.307201612186));
#40182=CARTESIAN_POINT('Ctrl Pts',(5.2468074522505,0.654015540275394,394.228073736726));
#40183=CARTESIAN_POINT('Ctrl Pts',(4.92352338499734,-1.92760012588128,394.148945861266));
#40184=CARTESIAN_POINT('Ctrl Pts',(3.40809070325859,-4.04247974964323,394.069817985806));
#40185=CARTESIAN_POINT('Ctrl Pts',(1.06744601535546,-5.17854069909805,393.990690110347));
#40186=CARTESIAN_POINT('Ctrl Pts',(-1.53166282285958,-5.06070486839363,
393.911562234887));
#40187=CARTESIAN_POINT('Ctrl Pts',(-3.75990519627929,-3.71750422769163,
393.832434359427));
#40188=CARTESIAN_POINT('Ctrl Pts',(-4.88811881465991,-1.79697577151505,
393.764692562677));
#40189=CARTESIAN_POINT('Ctrl Pts',(-5.07303815383513,-0.477899626088436,
393.723326724414));
#40190=CARTESIAN_POINT('Ctrl Pts',(-5.07320934784751,5.14726455259906E-5,
393.708336844637));
#40191=CARTESIAN_POINT('Ctrl Pts',(-5.07374340439062,0.000119799015104727,
394.791663155363));
#40192=CARTESIAN_POINT('Ctrl Pts',(-5.07389328700639,0.149964795759533,
394.786962176793));
#40193=CARTESIAN_POINT('Ctrl Pts',(-5.03087783588661,1.1404650386697,394.755885239737));
#40194=CARTESIAN_POINT('Ctrl Pts',(-4.40588160918252,2.92317155691987,394.698432344195));
#40195=CARTESIAN_POINT('Ctrl Pts',(-2.47828569661807,4.67063429431767,394.619304468735));
#40196=CARTESIAN_POINT('Ctrl Pts',(0.0493855336599835,5.28718126929493,
394.540176593275));
#40197=CARTESIAN_POINT('Ctrl Pts',(2.56509888521489,4.623525972068,394.461048717816));
#40198=CARTESIAN_POINT('Ctrl Pts',(4.45971656139522,2.84036140259214,394.381920842355));
#40199=CARTESIAN_POINT('Ctrl Pts',(5.27448866684743,0.369450955630144,394.302792966896));
#40200=CARTESIAN_POINT('Ctrl Pts',(4.81213180090847,-2.19091584411711,394.223665091436));
#40201=CARTESIAN_POINT('Ctrl Pts',(3.18459792440514,-4.2207891164085,394.144537215977));
#40202=CARTESIAN_POINT('Ctrl Pts',(0.785967069903959,-5.22866909168525,
394.065409340517));
#40203=CARTESIAN_POINT('Ctrl Pts',(-1.8029725289961,-4.97051453724898,393.986281465057));
#40204=CARTESIAN_POINT('Ctrl Pts',(-3.95535256793798,-3.50883324890547,
393.907153589597));
#40205=CARTESIAN_POINT('Ctrl Pts',(-4.9347894212868,-1.61393147469998,393.842280819699));
#40206=CARTESIAN_POINT('Ctrl Pts',(-5.0732716126465,-0.386507955183392,
393.803784008288));
#40207=CARTESIAN_POINT('Ctrl Pts',(-5.07318860167666,-3.10232113822501E-5,
393.791663155363));
#40208=CARTESIAN_POINT('Origin',(0.,0.,402.208336844637));
#40209=CARTESIAN_POINT('',(-5.07372845053928,-0.000121538385184292,395.791663155363));
#40210=CARTESIAN_POINT('',(-5.07344883766069,-0.000122970527678777,395.708336844637));
#40211=CARTESIAN_POINT('',(-5.0736,-1.59740085886799E-13,402.208336844637));
#40212=CARTESIAN_POINT('Ctrl Pts',(-5.07344883766069,-0.000122970527678921,
395.708336844637));
#40213=CARTESIAN_POINT('Ctrl Pts',(-5.07290495347366,0.594570911737787,
395.689683061425));
#40214=CARTESIAN_POINT('Ctrl Pts',(-4.82050381961586,2.03059585572183,395.644653319727));
#40215=CARTESIAN_POINT('Ctrl Pts',(-3.49440419526435,3.96810585645496,395.573247619542));
#40216=CARTESIAN_POINT('Ctrl Pts',(-1.17878204811896,5.1543377509575,395.494119744082));
#40217=CARTESIAN_POINT('Ctrl Pts',(1.42226240243777,5.09253320328156,395.414991868623));
#40218=CARTESIAN_POINT('Ctrl Pts',(3.67892986523249,3.79765714811298,395.335863993163));
#40219=CARTESIAN_POINT('Ctrl Pts',(5.0448061610774,1.58324210563915,395.256736117703));
#40220=CARTESIAN_POINT('Ctrl Pts',(5.18916725226161,-1.01452845991075,395.177608242243));
#40221=CARTESIAN_POINT('Ctrl Pts',(4.07705852165763,-3.36664797371096,395.098480366784));
#40222=CARTESIAN_POINT('Ctrl Pts',(1.97775844702931,-4.90359014326416,395.019352491324));
#40223=CARTESIAN_POINT('Ctrl Pts',(-0.60042266624658,-5.25321019851391,
394.940224615864));
#40224=CARTESIAN_POINT('Ctrl Pts',(-3.03322150067462,-4.33085350661488,
394.861096740404));
#40225=CARTESIAN_POINT('Ctrl Pts',(-4.69225666341608,-2.40548544911562,
394.783800816662));
#40226=CARTESIAN_POINT('Ctrl Pts',(-5.07351974582911,-0.782183276838963,
394.732880851406));
#40227=CARTESIAN_POINT('Ctrl Pts',(-5.07397904538501,5.86126803111056E-5,
394.708336844637));
#40228=CARTESIAN_POINT('Ctrl Pts',(-5.07372845053928,-0.000121538385184274,
395.791663155363));
#40229=CARTESIAN_POINT('Ctrl Pts',(-5.07303742094413,0.685929840247112,
395.770140345299));
#40230=CARTESIAN_POINT('Ctrl Pts',(-4.76110728643783,2.2133386185757,395.722241576749));
#40231=CARTESIAN_POINT('Ctrl Pts',(-3.27480540051438,4.15118950351341,395.647966849712));
#40232=CARTESIAN_POINT('Ctrl Pts',(-0.898448588333209,5.21051963238218,
395.568838974252));
#40233=CARTESIAN_POINT('Ctrl Pts',(1.69545248148909,5.00820981872071,395.489711098793));
#40234=CARTESIAN_POINT('Ctrl Pts',(3.87882816762124,3.59324599093717,395.410583223333));
#40235=CARTESIAN_POINT('Ctrl Pts',(5.12301066540628,1.30823790934658,395.331455347873));
#40236=CARTESIAN_POINT('Ctrl Pts',(5.12674204938754,-1.29353804132683,395.252327472413));
#40237=CARTESIAN_POINT('Ctrl Pts',(3.88911882751359,-3.58210544942458,395.173199596953));
#40238=CARTESIAN_POINT('Ctrl Pts',(1.70981070658587,-5.00332609900278,395.094071721494));
#40239=CARTESIAN_POINT('Ctrl Pts',(-0.883499401435098,-5.21307524528295,
395.014943846034));
#40240=CARTESIAN_POINT('Ctrl Pts',(-3.26288494670713,-4.16056565022955,
394.935815970574));
#40241=CARTESIAN_POINT('Ctrl Pts',(-4.7577955410693,-2.22302453301642,394.861389073684));
#40242=CARTESIAN_POINT('Ctrl Pts',(-5.07305233493801,-0.690776202139344,
394.81333813528));
#40243=CARTESIAN_POINT('Ctrl Pts',(-5.07374340439062,0.000119799015104727,
394.791663155363));
#40244=CARTESIAN_POINT('Origin',(0.,0.,402.208336844637));
#40245=CARTESIAN_POINT('',(-5.07319204280361,3.5344916511082E-5,396.791663155363));
#40246=CARTESIAN_POINT('',(-5.07333567377535,0.000103933621521292,396.708336844637));
#40247=CARTESIAN_POINT('',(-5.0736,-1.59740085886799E-13,402.208336844637));
#40248=CARTESIAN_POINT('Ctrl Pts',(-5.07333567377534,0.000103933621520939,
396.708336844637));
#40249=CARTESIAN_POINT('Ctrl Pts',(-5.07355255518605,0.290225038825201,
396.699237188418));
#40250=CARTESIAN_POINT('Ctrl Pts',(-4.9781337482961,1.42114034886055,396.663761573712));
#40251=CARTESIAN_POINT('Ctrl Pts',(-4.14865431030898,3.27801650109757,396.601910000519));
#40252=CARTESIAN_POINT('Ctrl Pts',(-2.08295867375766,4.85983620416686,396.52278212506));
#40253=CARTESIAN_POINT('Ctrl Pts',(0.487090472013812,5.26492807548086,396.4436542496));
#40254=CARTESIAN_POINT('Ctrl Pts',(2.93919882905869,4.3952059122609,396.36452637414));
#40255=CARTESIAN_POINT('Ctrl Pts',(4.67962948341671,2.46125835008237,396.28539849868));
#40256=CARTESIAN_POINT('Ctrl Pts',(5.2869663411736,-0.0686416434144708,
396.206270623221));
#40257=CARTESIAN_POINT('Ctrl Pts',(4.61415296796628,-2.58192121415839,396.127142747761));
#40258=CARTESIAN_POINT('Ctrl Pts',(2.82409983825713,-4.47003186470401,396.048014872301));
#40259=CARTESIAN_POINT('Ctrl Pts',(0.350238296140284,-5.27579926682488,
395.968886996841));
#40260=CARTESIAN_POINT('Ctrl Pts',(-2.20842757548492,-4.80412035775031,
395.889759121382));
#40261=CARTESIAN_POINT('Ctrl Pts',(-4.23235974759556,-3.16920427471092,
395.810631245921));
#40262=CARTESIAN_POINT('Ctrl Pts',(-4.99595812955649,-1.33323876922698,
395.750157153674));
#40263=CARTESIAN_POINT('Ctrl Pts',(-5.07367399139889,-0.246310585215766,
395.716059019912));
#40264=CARTESIAN_POINT('Ctrl Pts',(-5.07344883766069,-0.000122970527678921,
395.708336844637));
#40265=CARTESIAN_POINT('Ctrl Pts',(-5.07319204280361,3.53449165107697E-5,
396.791663155363));
#40266=CARTESIAN_POINT('Ctrl Pts',(-5.07328550820695,0.381659555984483,
396.779694472291));
#40267=CARTESIAN_POINT('Ctrl Pts',(-4.93711373649749,1.60422160810075,396.741349830733));
#40268=CARTESIAN_POINT('Ctrl Pts',(-3.96540078941456,3.49747355738801,396.676629230689));
#40269=CARTESIAN_POINT('Ctrl Pts',(-1.81722218927578,4.96532256959422,396.597501355229));
#40270=CARTESIAN_POINT('Ctrl Pts',(0.770966287074601,5.23090199578547,396.51837347977));
#40271=CARTESIAN_POINT('Ctrl Pts',(3.17247820700774,4.22990623198423,396.43924560431));
#40272=CARTESIAN_POINT('Ctrl Pts',(4.8058277352491,2.20470961453625,396.36011772885));
#40273=CARTESIAN_POINT('Ctrl Pts',(5.275526676699,-0.354320460537079,396.28098985339));
#40274=CARTESIAN_POINT('Ctrl Pts',(4.46784531008081,-2.82755777845599,396.201861977931));
#40275=CARTESIAN_POINT('Ctrl Pts',(2.57835013256881,-4.61614940174172,396.122734102471));
#40276=CARTESIAN_POINT('Ctrl Pts',(0.0645507123742531,-5.2870178655694,
396.043606227011));
#40277=CARTESIAN_POINT('Ctrl Pts',(-2.46487858023149,-4.67772362266456,
395.964478351551));
#40278=CARTESIAN_POINT('Ctrl Pts',(-4.39747886350376,-2.93579705537622,
395.885350476092));
#40279=CARTESIAN_POINT('Ctrl Pts',(-5.02925481295834,-1.15017365368594,
395.827745410695));
#40280=CARTESIAN_POINT('Ctrl Pts',(-5.0738842698389,-0.154818306903111,
395.796516303786));
#40281=CARTESIAN_POINT('Ctrl Pts',(-5.07372845053928,-0.000121538385184274,
395.791663155363));
#40282=CARTESIAN_POINT('Origin',(0.,0.,402.208336844637));
#40283=CARTESIAN_POINT('',(-5.0739418421154,7.48951186854696E-5,397.791663155363));
#40284=CARTESIAN_POINT('',(-5.07403169783887,-1.51513653288439E-5,397.708336844637));
#40285=CARTESIAN_POINT('',(-5.0736,-1.59740085886799E-13,402.208336844637));
#40286=CARTESIAN_POINT('Ctrl Pts',(-5.07403169783887,-1.51513653288493E-5,
397.708336844637));
#40287=CARTESIAN_POINT('Ctrl Pts',(-5.07388968734652,0.82610348406882,397.682415356923));
#40288=CARTESIAN_POINT('Ctrl Pts',(-4.6586701596041,2.49296234041498,397.630117910723));
#40289=CARTESIAN_POINT('Ctrl Pts',(-2.91976153402742,4.40814216562114,397.551444506037));
#40290=CARTESIAN_POINT('Ctrl Pts',(-0.463836508948714,5.26702766851281,
397.472316630577));
#40291=CARTESIAN_POINT('Ctrl Pts',(2.10439874769627,4.85059075563045,397.393188755117));
#40292=CARTESIAN_POINT('Ctrl Pts',(4.16308914079174,3.25966464129901,397.314060879657));
#40293=CARTESIAN_POINT('Ctrl Pts',(5.21375731827273,0.87946540242969,397.234933004198));
#40294=CARTESIAN_POINT('Ctrl Pts',(5.00200160188481,-1.71368163398425,397.155805128738));
#40295=CARTESIAN_POINT('Ctrl Pts',(3.57909508696266,-3.89188940315535,397.076677253278));
#40296=CARTESIAN_POINT('Ctrl Pts',(1.28957072230382,-5.12774142484681,396.997549377819));
#40297=CARTESIAN_POINT('Ctrl Pts',(-1.31220156516579,-5.12199685867627,
396.918421502358));
#40298=CARTESIAN_POINT('Ctrl Pts',(-3.59624625077107,-3.87604665499891,
396.839293626899));
#40299=CARTESIAN_POINT('Ctrl Pts',(-4.84699459687274,-1.94278943218135,
396.769265407658));
#40300=CARTESIAN_POINT('Ctrl Pts',(-5.07292390999909,-0.550710271536964,
396.725613146904));
#40301=CARTESIAN_POINT('Ctrl Pts',(-5.07333567377534,0.000103933621520939,
396.708336844637));
#40302=CARTESIAN_POINT('Ctrl Pts',(-5.0739418421154,7.48951186850533E-5,
397.791663155363));
#40303=CARTESIAN_POINT('Ctrl Pts',(-5.07399707454689,0.0770308345755981,
397.789248599284));
#40304=CARTESIAN_POINT('Ctrl Pts',(-5.05354999565328,0.994603307815543,
397.760458084718));
#40305=CARTESIAN_POINT('Ctrl Pts',(-4.52773440061085,2.73063104480294,397.705291611666));
#40306=CARTESIAN_POINT('Ctrl Pts',(-2.67721733102668,4.55952103490808,397.626163736206));
#40307=CARTESIAN_POINT('Ctrl Pts',(-0.178456984770649,5.28439947486034,
397.547035860747));
#40308=CARTESIAN_POINT('Ctrl Pts',(2.36351372741711,4.72974920747697,397.467907985287));
#40309=CARTESIAN_POINT('Ctrl Pts',(4.33319922937441,3.02986949287705,397.388780109827));
#40310=CARTESIAN_POINT('Ctrl Pts',(5.25367321071018,0.596357694998765,397.309652234368));
#40311=CARTESIAN_POINT('Ctrl Pts',(4.90205833425909,-1.98155211711401,397.230524358907));
#40312=CARTESIAN_POINT('Ctrl Pts',(3.36349224536493,-4.07966231699243,397.151396483448));
#40313=CARTESIAN_POINT('Ctrl Pts',(1.01051291891753,-5.18995070747486,397.072268607988));
#40314=CARTESIAN_POINT('Ctrl Pts',(-1.58714516337332,-5.04357957562867,
396.993140732529));
#40315=CARTESIAN_POINT('Ctrl Pts',(-3.80050266261658,-3.67599023621695,
396.914012857068));
#40316=CARTESIAN_POINT('Ctrl Pts',(-4.89803666817087,-1.7598107945601,396.84685366468));
#40317=CARTESIAN_POINT('Ctrl Pts',(-5.07307953403386,-0.459343943622233,
396.806070430778));
#40318=CARTESIAN_POINT('Ctrl Pts',(-5.07319204280361,3.53449165107697E-5,
396.791663155363));
#40319=CARTESIAN_POINT('Origin',(0.,0.,402.208336844637));
#40320=CARTESIAN_POINT('',(-5.07350261625086,-0.000127405426567639,398.791663155363));
#40321=CARTESIAN_POINT('',(-5.07327504304777,-8.56681209023223E-5,398.708336844637));
#40322=CARTESIAN_POINT('',(-5.0736,-1.59740085886799E-13,402.208336844637));
#40323=CARTESIAN_POINT('Ctrl Pts',(-5.07327504304777,-8.56681209025073E-5,
398.708336844637));
#40324=CARTESIAN_POINT('Ctrl Pts',(-5.07295870657578,0.521766948573649,
398.691969483916));
#40325=CARTESIAN_POINT('Ctrl Pts',(-4.86376568515234,1.88483153888263,398.649226164708));
#40326=CARTESIAN_POINT('Ctrl Pts',(-3.66212405277363,3.81386578025083,398.580106887014));
#40327=CARTESIAN_POINT('Ctrl Pts',(-1.39976059402284,5.09876407058445,398.500979011554));
#40328=CARTESIAN_POINT('Ctrl Pts',(1.2015314169661,5.14908215334412,398.421851136094));
#40329=CARTESIAN_POINT('Ctrl Pts',(3.51189274640949,3.9526363487746,398.342723260634));
#40330=CARTESIAN_POINT('Ctrl Pts',(4.97190814582059,1.79912594262636,398.263595385175));
#40331=CARTESIAN_POINT('Ctrl Pts',(5.22805937238099,-0.790012637095727,
398.184467509715));
#40332=CARTESIAN_POINT('Ctrl Pts',(4.21832370253235,-3.18786290617544,398.105339634255));
#40333=CARTESIAN_POINT('Ctrl Pts',(2.18719169429123,-4.81382563667766,398.026211758795));
#40334=CARTESIAN_POINT('Ctrl Pts',(-0.37353210098369,-5.27420122269227,
397.947083883336));
#40335=CARTESIAN_POINT('Ctrl Pts',(-2.84381136257153,-4.45751743709679,
397.867956007876));
#40336=CARTESIAN_POINT('Ctrl Pts',(-4.62550939672404,-2.56152056184034,
397.788828132416));
#40337=CARTESIAN_POINT('Ctrl Pts',(-5.07044892396789,-0.869584543074369,
397.73562174467));
#40338=CARTESIAN_POINT('Ctrl Pts',(-5.07403418765037,-0.0144991493159696,
397.70879131541));
#40339=CARTESIAN_POINT('Ctrl Pts',(-5.07403169783887,-1.51513653288493E-5,
397.708336844637));
#40340=CARTESIAN_POINT('Ctrl Pts',(-5.07350261625086,-0.000127405426567848,
398.791663155363));
#40341=CARTESIAN_POINT('Ctrl Pts',(-5.07291128030502,0.613121580961722,
398.77242676779));
#40342=CARTESIAN_POINT('Ctrl Pts',(-4.80890661569317,2.06772180201207,398.72681442173));
#40343=CARTESIAN_POINT('Ctrl Pts',(-3.45061727711166,4.00624076891526,398.654826117184));
#40344=CARTESIAN_POINT('Ctrl Pts',(-1.12210802579434,5.16697186848109,398.575698241724));
#40345=CARTESIAN_POINT('Ctrl Pts',(1.47810086651078,5.07660738405961,398.496570366264));
#40346=CARTESIAN_POINT('Ctrl Pts',(3.72041242270134,3.75702756318667,398.417442490805));
#40347=CARTESIAN_POINT('Ctrl Pts',(5.06188850671742,1.52774652711538,398.338314615344));
#40348=CARTESIAN_POINT('Ctrl Pts',(5.17771318239863,-1.0714527081918,398.259186739885));
#40349=CARTESIAN_POINT('Ctrl Pts',(4.03984144729043,-3.41121763982034,398.180058864425));
#40350=CARTESIAN_POINT('Ctrl Pts',(1.92378985850489,-4.92501342998799,398.100930988965));
#40351=CARTESIAN_POINT('Ctrl Pts',(-0.658075180315041,-5.24629981628919,
398.021803113506));
#40352=CARTESIAN_POINT('Ctrl Pts',(-3.08059835091328,-4.29728268859095,
397.942675238046));
#40353=CARTESIAN_POINT('Ctrl Pts',(-4.70604526230202,-2.36846041862021,
397.865961918665));
#40354=CARTESIAN_POINT('Ctrl Pts',(-5.07339373038246,-0.763615063923845,
397.81562455777));
#40355=CARTESIAN_POINT('Ctrl Pts',(-5.0739418421154,7.48951186850533E-5,
397.791663155363));
#40356=CARTESIAN_POINT('Origin',(0.,0.,402.208336844637));
#40357=CARTESIAN_POINT('',(-5.07330191118131,0.000105688062508047,399.791663155363));
#40358=CARTESIAN_POINT('',(-5.07353386009457,0.000128968315485679,399.708336844637));
#40359=CARTESIAN_POINT('',(-5.0736,-1.59740085886799E-13,402.208336844637));
#40360=CARTESIAN_POINT('',(-1.31303618635556,-4.90075024188347,400.));
#40361=CARTESIAN_POINT('Ctrl Pts',(-1.31303618635555,-4.90075024188347,
400.));
#40362=CARTESIAN_POINT('Ctrl Pts',(-2.12521319086393,-4.68314727417224,
399.973624041513));
#40363=CARTESIAN_POINT('Ctrl Pts',(-3.63845957255092,-3.83644859241818,
399.92087212454));
#40364=CARTESIAN_POINT('Ctrl Pts',(-4.85784323874867,-1.90558193017489,
399.851426509661));
#40365=CARTESIAN_POINT('Ctrl Pts',(-5.07295978880057,-0.532132079631421,
399.808356853268));
#40366=CARTESIAN_POINT('Ctrl Pts',(-5.07330191118131,0.000105688062508012,
399.791663155363));
#40367=CARTESIAN_POINT('',(1.31318543090008,-4.90112867346845,400.));
#40368=CARTESIAN_POINT('Origin',(0.,0.,400.));
#40369=CARTESIAN_POINT('Ctrl Pts',(1.31318543090008,-4.90112867346845,400.));
#40370=CARTESIAN_POINT('Ctrl Pts',(0.546344064728336,-5.10618409880194,
399.975093589943));
#40371=CARTESIAN_POINT('Ctrl Pts',(-1.13368018453605,-5.15247589033718,
399.923811221401));
#40372=CARTESIAN_POINT('Ctrl Pts',(-3.42590833126468,-4.02739560525483,
399.84615289437));
#40373=CARTESIAN_POINT('Ctrl Pts',(-4.8023079180703,-2.08851222235156,399.77383825264));
#40374=CARTESIAN_POINT('Ctrl Pts',(-5.07291903260815,-0.623512076348425,
399.727899569395));
#40375=CARTESIAN_POINT('Ctrl Pts',(-5.07353386009457,0.000128968315485402,
399.708336844637));
#40376=CARTESIAN_POINT('Origin',(0.,0.,20.5));
#40377=CARTESIAN_POINT('',(4.51807726312575,-5.77016670283426E-5,39.6125833024919));
#40378=CARTESIAN_POINT('',(4.51743491291879,0.00013078575649096,39.887416697508));
#40379=CARTESIAN_POINT('',(4.51775,5.53264807684796E-16,20.5));
#40380=CARTESIAN_POINT('',(3.43378788736186,2.93584158413001,40.));
#40381=CARTESIAN_POINT('Ctrl Pts',(4.51743491291879,0.00013078575649096,
39.887416697508));
#40382=CARTESIAN_POINT('Ctrl Pts',(4.51757757737092,0.314458352690014,39.8984871683209));
#40383=CARTESIAN_POINT('Ctrl Pts',(4.48524528727997,0.628740973485904,39.9095576391338));
#40384=CARTESIAN_POINT('Ctrl Pts',(4.42014586550123,0.936043740039879,39.9206281099466));
#40385=CARTESIAN_POINT('Ctrl Pts',(4.26456488388791,1.67046602470259,39.9470854066311));
#40386=CARTESIAN_POINT('Ctrl Pts',(3.92183073605335,2.36502208507763,39.9735427033156));
#40387=CARTESIAN_POINT('Ctrl Pts',(3.43378788736169,2.9358415841302,40.));
#40388=CARTESIAN_POINT('',(4.51775,5.53264807684796E-16,40.));
#40389=CARTESIAN_POINT('Origin',(0.,0.,40.));
#40390=CARTESIAN_POINT('',(4.51775,-5.53264807684796E-16,41.));
#40391=CARTESIAN_POINT('',(4.51775,5.53264807684796E-16,20.5));
#40392=CARTESIAN_POINT('Origin',(0.,0.,41.));
#40393=CARTESIAN_POINT('',(-3.4340910891448,2.93606647242268,40.));
#40394=CARTESIAN_POINT('Origin',(0.,0.,40.));
#40395=CARTESIAN_POINT('Ctrl Pts',(-3.4340910891448,2.93606647242268,40.));
#40396=CARTESIAN_POINT('Ctrl Pts',(-2.96705577784696,3.4818800261268,39.974686898954));
#40397=CARTESIAN_POINT('Ctrl Pts',(-2.36757358452893,3.91460873741648,39.949373797908));
#40398=CARTESIAN_POINT('Ctrl Pts',(-1.70215900486053,4.18523117809469,39.9240606968621));
#40399=CARTESIAN_POINT('Ctrl Pts',(-1.00666654344796,4.46808621784234,39.8976034001776));
#40400=CARTESIAN_POINT('Ctrl Pts',(-0.239146468763622,4.57384880856985,
39.8711461034931));
#40401=CARTESIAN_POINT('Ctrl Pts',(0.506923795872781,4.48961228541996,39.8446888068086));
#40402=CARTESIAN_POINT('Ctrl Pts',(1.25299406050918,4.40537576227008,39.8182315101241));
#40403=CARTESIAN_POINT('Ctrl Pts',(1.97761451509765,4.1311401252428,39.7917742134397));
#40404=CARTESIAN_POINT('Ctrl Pts',(2.59252418705981,3.70032015205324,39.7653169167552));
#40405=CARTESIAN_POINT('Ctrl Pts',(3.2074338590219,3.26950017886373,39.7388596200708));
#40406=CARTESIAN_POINT('Ctrl Pts',(3.71263274835769,2.68209586951196,39.7124023233863));
#40407=CARTESIAN_POINT('Ctrl Pts',(4.0465897798431,2.00964543895381,39.6859450267018));
#40408=CARTESIAN_POINT('Ctrl Pts',(4.35525905337691,1.38811402527266,39.6614911186319));
#40409=CARTESIAN_POINT('Ctrl Pts',(4.51763802149368,0.693928511700309,39.6370372105619));
#40410=CARTESIAN_POINT('Ctrl Pts',(4.51807726312575,-5.77016670283426E-5,
39.6125833024919));
#40411=CARTESIAN_POINT('Origin',(0.,0.,20.5));
#40412=CARTESIAN_POINT('',(4.5173663293175,-1.61899228900975E-5,38.6125833024919));
#40413=CARTESIAN_POINT('',(4.51813342681501,1.37750411066654E-5,38.887416697508));
#40414=CARTESIAN_POINT('',(4.51775,5.53264807684796E-16,20.5));
#40415=CARTESIAN_POINT('Ctrl Pts',(4.51813342681501,1.37750411066654E-5,
38.887416697508));
#40416=CARTESIAN_POINT('Ctrl Pts',(4.51813570137199,0.0130379216071904,
38.8878756447561));
#40417=CARTESIAN_POINT('Ctrl Pts',(4.51808056261842,0.0260620488529043,
38.8883345920043));
#40418=CARTESIAN_POINT('Ctrl Pts',(4.51796789313227,0.039085678406741,38.8887935392524));
#40419=CARTESIAN_POINT('Ctrl Pts',(4.5114727457387,0.789869199672342,38.9152508359369));
#40420=CARTESIAN_POINT('Ctrl Pts',(4.31378754306059,1.53899875733816,38.9417081326213));
#40421=CARTESIAN_POINT('Ctrl Pts',(3.94899006576268,2.19523105353971,38.9681654293058));
#40422=CARTESIAN_POINT('Ctrl Pts',(3.58419258846473,2.85146334974134,38.9946227259902));
#40423=CARTESIAN_POINT('Ctrl Pts',(3.05228283654696,3.41479838447868,39.0210800226747));
#40424=CARTESIAN_POINT('Ctrl Pts',(2.4180469390752,3.81662285121831,39.0475373193592));
#40425=CARTESIAN_POINT('Ctrl Pts',(1.78381104160343,4.21844731795794,39.0739946160436));
#40426=CARTESIAN_POINT('Ctrl Pts',(1.04724899857768,4.45876121669985,39.1004519127281));
#40427=CARTESIAN_POINT('Ctrl Pts',(0.298073044029034,4.50829405706009,39.1269092094126));
#40428=CARTESIAN_POINT('Ctrl Pts',(-0.45110291051953,4.55782689742033,39.1533665060971));
#40429=CARTESIAN_POINT('Ctrl Pts',(-1.21289277659099,4.41657867939895,39.1798238027815));
#40430=CARTESIAN_POINT('Ctrl Pts',(-1.89451099954058,4.10175426806426,39.206281099466));
#40431=CARTESIAN_POINT('Ctrl Pts',(-2.57612922249017,3.78692985672956,39.2327383961504));
#40432=CARTESIAN_POINT('Ctrl Pts',(-3.17757580231788,3.29852925208155,39.2591956928349));
#40433=CARTESIAN_POINT('Ctrl Pts',(-3.62559595151898,2.69603724086566,39.2856529895194));
#40434=CARTESIAN_POINT('Ctrl Pts',(-4.07361610072013,2.0935452296497,39.3121102862039));
#40435=CARTESIAN_POINT('Ctrl Pts',(-4.36820981929462,1.37696181186582,39.3385675828883));
#40436=CARTESIAN_POINT('Ctrl Pts',(-4.4734945205513,0.633569578843569,39.3650248795728));
#40437=CARTESIAN_POINT('Ctrl Pts',(-4.57877922180797,-0.109822654178678,
39.3914821762572));
#40438=CARTESIAN_POINT('Ctrl Pts',(-4.49475490574683,-0.880023702439293,
39.4179394729417));
#40439=CARTESIAN_POINT('Ctrl Pts',(-4.23165828048028,-1.5832305850457,39.4443967696262));
#40440=CARTESIAN_POINT('Ctrl Pts',(-3.96856165521376,-2.28643746765202,
39.4708540663107));
#40441=CARTESIAN_POINT('Ctrl Pts',(-3.52639272074186,-2.92265018460415,
39.4973113629951));
#40442=CARTESIAN_POINT('Ctrl Pts',(-2.95900217961984,-3.41436616507676,
39.5237686596796));
#40443=CARTESIAN_POINT('Ctrl Pts',(-2.39161163849769,-3.90608214554949,
39.5502259563641));
#40444=CARTESIAN_POINT('Ctrl Pts',(-1.69899949072535,-4.25330138954263,
39.5766832530485));
#40445=CARTESIAN_POINT('Ctrl Pts',(-0.965534545329121,-4.41375671437606,
39.603140549733));
#40446=CARTESIAN_POINT('Ctrl Pts',(-0.232069599933061,-4.57421203920946,
39.6295978464175));
#40447=CARTESIAN_POINT('Ctrl Pts',(0.542248143086867,-4.54790344488323,
39.6560551431019));
#40448=CARTESIAN_POINT('Ctrl Pts',(1.26312545635919,-4.33799038903366,39.6825124397864));
#40449=CARTESIAN_POINT('Ctrl Pts',(1.98400276963152,-4.12807733318409,39.7089697364709));
#40450=CARTESIAN_POINT('Ctrl Pts',(2.65143965315624,-3.73455981581118,39.7354270331553));
#40451=CARTESIAN_POINT('Ctrl Pts',(3.18410908512153,-3.20545326780569,39.7618843298398));
#40452=CARTESIAN_POINT('Ctrl Pts',(3.71677851708688,-2.67634671980015,39.7883416265243));
#40453=CARTESIAN_POINT('Ctrl Pts',(4.11468049749276,-2.01165114116199,39.8147989232087));
#40454=CARTESIAN_POINT('Ctrl Pts',(4.32941757999969,-1.29215909736769,39.8412562198932));
#40455=CARTESIAN_POINT('Ctrl Pts',(4.45430267828147,-0.873722590951435,
39.8566430457648));
#40456=CARTESIAN_POINT('Ctrl Pts',(4.51723662387398,-0.436752488749845,
39.8720298716364));
#40457=CARTESIAN_POINT('Ctrl Pts',(4.51743491291879,0.00013078575649096,
39.887416697508));
#40458=CARTESIAN_POINT('Ctrl Pts',(4.51807726312575,-5.77016670283426E-5,
39.6125833024919));
#40459=CARTESIAN_POINT('Ctrl Pts',(4.51811324803589,-0.0569125845144851,
39.6105799138774));
#40460=CARTESIAN_POINT('Ctrl Pts',(4.51706233879025,-0.113766129714702,
39.6085765252629));
#40461=CARTESIAN_POINT('Ctrl Pts',(4.51491593042487,-0.170578278221581,
39.6065731366484));
#40462=CARTESIAN_POINT('Ctrl Pts',(4.48656987588623,-0.920855013074376,
39.580115839964));
#40463=CARTESIAN_POINT('Ctrl Pts',(4.26716259317389,-1.66391193101533,39.5536585432795));
#40464=CARTESIAN_POINT('Ctrl Pts',(3.88341809255801,-2.30924747945226,39.527201246595));
#40465=CARTESIAN_POINT('Ctrl Pts',(3.49967359194214,-2.9545830278892,39.5007439499106));
#40466=CARTESIAN_POINT('Ctrl Pts',(2.95159187342274,-3.50219720682209,39.4742866532261));
#40467=CARTESIAN_POINT('Ctrl Pts',(2.305928447501,-3.88539017854137,39.4478293565416));
#40468=CARTESIAN_POINT('Ctrl Pts',(1.66026502157934,-4.2685831502606,39.4213720598571));
#40469=CARTESIAN_POINT('Ctrl Pts',(0.917019888255395,-4.48735491476624,
39.3949147631727));
#40470=CARTESIAN_POINT('Ctrl Pts',(0.16671960730651,-4.51505986234427,39.3684574664882));
#40471=CARTESIAN_POINT('Ctrl Pts',(-0.58358067364246,-4.54276480992229,
39.3420001698038));
#40472=CARTESIAN_POINT('Ctrl Pts',(-1.34093610221634,-4.37940294057267,
39.3155428731193));
#40473=CARTESIAN_POINT('Ctrl Pts',(-2.0131016916631,-4.0448712583889,39.2890855764348));
#40474=CARTESIAN_POINT('Ctrl Pts',(-2.68526728110987,-3.71033957620513,
39.2626282797503));
#40475=CARTESIAN_POINT('Ctrl Pts',(-3.27224303142949,-3.20463808118724,
39.2361709830659));
#40476=CARTESIAN_POINT('Ctrl Pts',(-3.70253591076623,-2.58936080975925,
39.2097136863814));
#40477=CARTESIAN_POINT('Ctrl Pts',(-4.13282879010292,-1.97408353833133,
39.1832563896969));
#40478=CARTESIAN_POINT('Ctrl Pts',(-4.40643879845674,-1.24923049049336,
39.1567990930125));
#40479=CARTESIAN_POINT('Ctrl Pts',(-4.49004055820742,-0.503087883692005,
39.130341796328));
#40480=CARTESIAN_POINT('Ctrl Pts',(-4.5736423179581,0.243054723109393,39.1038844996435));
#40481=CARTESIAN_POINT('Ctrl Pts',(-4.46723582910558,1.01048688887427,39.0774272029591));
#40482=CARTESIAN_POINT('Ctrl Pts',(-4.18378127438633,1.70573618195759,39.0509699062746));
#40483=CARTESIAN_POINT('Ctrl Pts',(-3.90032671966707,2.40098547504095,39.0245126095901));
#40484=CARTESIAN_POINT('Ctrl Pts',(-3.43982409908106,3.02405189544285,38.9980553129056));
#40485=CARTESIAN_POINT('Ctrl Pts',(-2.85836212737563,3.49904666560209,38.9715980162212));
#40486=CARTESIAN_POINT('Ctrl Pts',(-2.27690015567025,3.97404143576128,38.9451407195367));
#40487=CARTESIAN_POINT('Ctrl Pts',(-1.5744788328455,4.30096455567782,38.9186834228523));
#40488=CARTESIAN_POINT('Ctrl Pts',(-0.836652295869176,4.43999713904635,
38.8922261261678));
#40489=CARTESIAN_POINT('Ctrl Pts',(-0.0988257588928058,4.57902972241489,
38.8657688294833));
#40490=CARTESIAN_POINT('Ctrl Pts',(0.67440599223512,4.53017176923538,38.8393115327988));
#40491=CARTESIAN_POINT('Ctrl Pts',(1.38886418452495,4.29937413054893,38.8128542361144));
#40492=CARTESIAN_POINT('Ctrl Pts',(2.10332237681477,4.06857649186248,38.7863969394299));
#40493=CARTESIAN_POINT('Ctrl Pts',(2.75900701026648,3.6558391676691,38.7599396427455));
#40494=CARTESIAN_POINT('Ctrl Pts',(3.27605642296661,3.11143310386805,38.733482346061));
#40495=CARTESIAN_POINT('Ctrl Pts',(3.79310583566678,2.56702704006697,38.7070250493765));
#40496=CARTESIAN_POINT('Ctrl Pts',(4.17152002761535,1.89095223665823,38.680567752692));
#40497=CARTESIAN_POINT('Ctrl Pts',(4.36520856862573,1.1655538582636,38.6541104560076));
#40498=CARTESIAN_POINT('Ctrl Pts',(4.46654587798484,0.786027431472861,38.6402680715023));
#40499=CARTESIAN_POINT('Ctrl Pts',(4.51731724698707,0.392999398715342,38.6264256869971));
#40500=CARTESIAN_POINT('Ctrl Pts',(4.5173663293175,-1.61899228900975E-5,
38.6125833024919));
#40501=CARTESIAN_POINT('Origin',(0.,0.,20.5));
#40502=CARTESIAN_POINT('',(4.51799626797168,8.54686663623316E-5,37.6125833024919));
#40503=CARTESIAN_POINT('',(4.51744515673179,-7.51896715610657E-5,37.887416697508));
#40504=CARTESIAN_POINT('',(4.51775,5.53264807684796E-16,20.5));
#40505=CARTESIAN_POINT('Ctrl Pts',(4.51744515673179,-7.51896715610657E-5,
37.887416697508));
#40506=CARTESIAN_POINT('Ctrl Pts',(4.51717073079397,0.462828384782965,37.9037214178759));
#40507=CARTESIAN_POINT('Ctrl Pts',(4.44640538068968,0.925813963613659,37.9200261382437));
#40508=CARTESIAN_POINT('Ctrl Pts',(4.30642900683072,1.36683241594085,37.9363308586115));
#40509=CARTESIAN_POINT('Ctrl Pts',(4.07929254766704,2.0824629679108,37.962788155296));
#40510=CARTESIAN_POINT('Ctrl Pts',(3.66991785444932,2.74025229569321,37.9892454519805));
#40511=CARTESIAN_POINT('Ctrl Pts',(3.12816631171535,3.26008238708871,38.0157027486649));
#40512=CARTESIAN_POINT('Ctrl Pts',(2.58641476898142,3.77991247848417,38.0421600453494));
#40513=CARTESIAN_POINT('Ctrl Pts',(1.91228637673127,4.16178333349271,38.0686173420339));
#40514=CARTESIAN_POINT('Ctrl Pts',(1.18788922711554,4.35918350473768,38.0950746387183));
#40515=CARTESIAN_POINT('Ctrl Pts',(0.463492077499819,4.55658367598265,38.1215319354028));
#40516=CARTESIAN_POINT('Ctrl Pts',(-0.311173829481454,4.56951316346404,
38.1479892320873));
#40517=CARTESIAN_POINT('Ctrl Pts',(-1.04175504380602,4.39639716966122,38.1744465287717));
#40518=CARTESIAN_POINT('Ctrl Pts',(-1.77233625813064,4.2232811758584,38.2009038254562));
#40519=CARTESIAN_POINT('Ctrl Pts',(-2.45883277979851,3.86411970077134,38.2273611221407));
#40520=CARTESIAN_POINT('Ctrl Pts',(-3.01763009204679,3.36265821505168,38.2538184188251));
#40521=CARTESIAN_POINT('Ctrl Pts',(-3.57642740429506,2.86119672933201,38.2802757155096));
#40522=CARTESIAN_POINT('Ctrl Pts',(-4.00752550712371,2.21743523297976,38.3067330121941));
#40523=CARTESIAN_POINT('Ctrl Pts',(-4.25841712907836,1.50978316287097,38.3331903088785));
#40524=CARTESIAN_POINT('Ctrl Pts',(-4.50930875103297,0.802131092762298,
38.359647605563));
#40525=CARTESIAN_POINT('Ctrl Pts',(-4.57999389211364,0.0305884488970126,
38.3861049022475));
#40526=CARTESIAN_POINT('Ctrl Pts',(-4.46186317968564,-0.710871726876464,
38.412562198932));
#40527=CARTESIAN_POINT('Ctrl Pts',(-4.34373246725763,-1.45233190264998,
38.4390194956164));
#40528=CARTESIAN_POINT('Ctrl Pts',(-4.03678590132095,-2.16370961033178,
38.4654767923008));
#40529=CARTESIAN_POINT('Ctrl Pts',(-3.57840923518433,-2.75835983566992,
38.4919340889853));
#40530=CARTESIAN_POINT('Ctrl Pts',(-3.12003256904766,-3.35301006100813,
38.5183913856698));
#40531=CARTESIAN_POINT('Ctrl Pts',(-2.51022580271103,-3.83093280400264,
38.5448486823543));
#40532=CARTESIAN_POINT('Ctrl Pts',(-1.82326272299569,-4.13391759737145,
38.5713059790388));
#40533=CARTESIAN_POINT('Ctrl Pts',(-1.13629964328034,-4.43690239074026,
38.5977632757232));
#40534=CARTESIAN_POINT('Ctrl Pts',(-0.372180250186292,-4.56494923448336,
38.6242205724077));
#40535=CARTESIAN_POINT('Ctrl Pts',(0.376026555300945,-4.50246217629699,
38.6506778690921));
#40536=CARTESIAN_POINT('Ctrl Pts',(1.12423336078818,-4.4399751181106,38.6771351657766));
#40537=CARTESIAN_POINT('Ctrl Pts',(1.85652757866858,-4.18695415799474,38.7035924624611));
#40538=CARTESIAN_POINT('Ctrl Pts',(2.48371659230794,-3.77421694705527,38.7300497591456));
#40539=CARTESIAN_POINT('Ctrl Pts',(3.1109056059473,-3.3614797361158,38.7565070558301));
#40540=CARTESIAN_POINT('Ctrl Pts',(3.63298941534561,-2.78902627435273,38.7829643525145));
#40541=CARTESIAN_POINT('Ctrl Pts',(3.98637877399025,-2.12658080103845,38.8094216491989));
#40542=CARTESIAN_POINT('Ctrl Pts',(4.33363798730682,-1.47562658212673,38.8354199986353));
#40543=CARTESIAN_POINT('Ctrl Pts',(4.51800457817832,-0.737775404274226,
38.8614183480717));
#40544=CARTESIAN_POINT('Ctrl Pts',(4.51813342681501,1.37750411066654E-5,
38.887416697508));
#40545=CARTESIAN_POINT('Ctrl Pts',(4.5173663293175,-1.61899228900975E-5,
38.6125833024919));
#40546=CARTESIAN_POINT('Ctrl Pts',(4.51741105927625,-0.358181153038861,
38.5999683903127));
#40547=CARTESIAN_POINT('Ctrl Pts',(4.4753302503181,-0.71633578114697,38.5873534781335));
#40548=CARTESIAN_POINT('Ctrl Pts',(4.39100556896819,-1.06425172631817,38.5747385659542));
#40549=CARTESIAN_POINT('Ctrl Pts',(4.21415113822809,-1.79393697912487,38.5482812692697));
#40550=CARTESIAN_POINT('Ctrl Pts',(3.85147938667571,-2.47858553135783,38.5218239725852));
#40551=CARTESIAN_POINT('Ctrl Pts',(3.34716333215496,-3.0348079465722,38.4953666759008));
#40552=CARTESIAN_POINT('Ctrl Pts',(2.84284727763424,-3.59103036178655,38.4689093792163));
#40553=CARTESIAN_POINT('Ctrl Pts',(2.19688692014516,-4.01882663998234,38.4424520825318));
#40554=CARTESIAN_POINT('Ctrl Pts',(1.48795951638629,-4.26609166819816,38.4159947858474));
#40555=CARTESIAN_POINT('Ctrl Pts',(0.779032112627345,-4.513356696414,38.3895374891629));
#40556=CARTESIAN_POINT('Ctrl Pts',(0.00713766259859555,-4.58009047464984,
38.3630801924784));
#40557=CARTESIAN_POINT('Ctrl Pts',(-0.733707943998393,-4.45816490243132,
38.336622895794));
#40558=CARTESIAN_POINT('Ctrl Pts',(-1.4745535505953,-4.33623933021282,38.3101655991095));
#40559=CARTESIAN_POINT('Ctrl Pts',(-2.18435031376045,-4.02565440754,38.283708302425));
#40560=CARTESIAN_POINT('Ctrl Pts',(-2.77664577327751,-3.56423903433536,
38.2572510057406));
#40561=CARTESIAN_POINT('Ctrl Pts',(-3.36894123279463,-3.10282366113066,
38.2307937090561));
#40562=CARTESIAN_POINT('Ctrl Pts',(-3.84373538866364,-2.49057783739411,
38.2043364123716));
#40563=CARTESIAN_POINT('Ctrl Pts',(-4.14319883817823,-1.80207242682554,
38.1778791156872));
#40564=CARTESIAN_POINT('Ctrl Pts',(-4.44266228769283,-1.11356701625697,
38.1514218190027));
#40565=CARTESIAN_POINT('Ctrl Pts',(-4.56679503085301,-0.348802018856373,
38.1249645223182));
#40566=CARTESIAN_POINT('Ctrl Pts',(-4.50047783691868,0.399075035061113,
38.0985072256338));
#40567=CARTESIAN_POINT('Ctrl Pts',(-4.43416064298434,1.14695208897856,38.0720499289493));
#40568=CARTESIAN_POINT('Ctrl Pts',(-4.17739351195555,1.87794119941278,38.0455926322648));
#40569=CARTESIAN_POINT('Ctrl Pts',(-3.76145039622188,2.50300870173274,38.0191353355804));
#40570=CARTESIAN_POINT('Ctrl Pts',(-3.34550728048821,3.1280762040527,37.9926780388959));
#40571=CARTESIAN_POINT('Ctrl Pts',(-2.77038818004956,3.64722209825836,37.9662207422114));
#40572=CARTESIAN_POINT('Ctrl Pts',(-2.10614196483595,3.99721498898437,37.9397634455269));
#40573=CARTESIAN_POINT('Ctrl Pts',(-1.4418957496223,4.34720787971039,37.9133061488425));
#40574=CARTESIAN_POINT('Ctrl Pts',(-0.688522419633467,4.52804776695686,
37.886848852158));
#40575=CARTESIAN_POINT('Ctrl Pts',(0.0622179873187612,4.51770855260138,
37.8603915554735));
#40576=CARTESIAN_POINT('Ctrl Pts',(0.812958394270905,4.5073693382459,37.8339342587891));
#40577=CARTESIAN_POINT('Ctrl Pts',(1.56106587818642,4.30585102228859,37.8074769621046));
#40578=CARTESIAN_POINT('Ctrl Pts',(2.21542177547896,3.93769831258472,37.7810196654202));
#40579=CARTESIAN_POINT('Ctrl Pts',(2.86977767277154,3.56954560288082,37.7545623687357));
#40580=CARTESIAN_POINT('Ctrl Pts',(3.43038198344099,3.03475849943036,37.7281050720512));
#40581=CARTESIAN_POINT('Ctrl Pts',(3.82895372288588,2.3984734795689,37.7016477753667));
#40582=CARTESIAN_POINT('Ctrl Pts',(4.22752546233078,1.76218845970743,37.6751904786822));
#40583=CARTESIAN_POINT('Ctrl Pts',(4.46406463055111,1.02440552343496,37.6487331819978));
#40584=CARTESIAN_POINT('Ctrl Pts',(4.50976101864303,0.274985815861593,37.6222758853133));
#40585=CARTESIAN_POINT('Ctrl Pts',(4.51534128170496,0.18346963073906,37.6190450243729));
#40586=CARTESIAN_POINT('Ctrl Pts',(4.51807563365308,0.0917799142062647,
37.6158141634324));
#40587=CARTESIAN_POINT('Ctrl Pts',(4.51799626797168,8.54686663623316E-5,
37.6125833024919));
#40588=CARTESIAN_POINT('Origin',(0.,0.,20.5));
#40589=CARTESIAN_POINT('',(4.51763788794132,-0.000113968307276224,36.612583302492));
#40590=CARTESIAN_POINT('',(4.51778606435352,0.000115791782295315,36.887416697508));
#40591=CARTESIAN_POINT('',(4.51775,5.53264807684796E-16,20.5));
#40592=CARTESIAN_POINT('Ctrl Pts',(4.51778606435352,0.000115791782295315,
36.887416697508));
#40593=CARTESIAN_POINT('Ctrl Pts',(4.51795287012522,0.16171502012428,36.8931098943111));
#40594=CARTESIAN_POINT('Ctrl Pts',(4.50945045543959,0.323296786803073,36.8988030911142));
#40595=CARTESIAN_POINT('Ctrl Pts',(4.49214571371295,0.483930295567246,36.9044962879172));
#40596=CARTESIAN_POINT('Ctrl Pts',(4.41172750549954,1.23042274011835,36.9309535846017));
#40597=CARTESIAN_POINT('Ctrl Pts',(4.14121195660595,1.9564363604895,36.9574108812862));
#40598=CARTESIAN_POINT('Ctrl Pts',(3.71354756149943,2.57354350122142,36.9838681779707));
#40599=CARTESIAN_POINT('Ctrl Pts',(3.28588316639293,3.1906506419533,37.0103254746552));
#40600=CARTESIAN_POINT('Ctrl Pts',(2.70106992507351,3.69885130304599,37.0367827713396));
#40601=CARTESIAN_POINT('Ctrl Pts',(2.0303374431028,4.03624720641988,37.0632400680241));
#40602=CARTESIAN_POINT('Ctrl Pts',(1.35960496113208,4.37364310979377,37.0896973647085));
#40603=CARTESIAN_POINT('Ctrl Pts',(0.602953238510051,4.54023425544888,37.116154661393));
#40604=CARTESIAN_POINT('Ctrl Pts',(-0.147458382357975,4.51573002621609,
37.1426119580775));
#40605=CARTESIAN_POINT('Ctrl Pts',(-0.897870003226045,4.49122579698331,
37.169069254762));
#40606=CARTESIAN_POINT('Ctrl Pts',(-1.64204152234013,4.27562619286261,37.1955265514464));
#40607=CARTESIAN_POINT('Ctrl Pts',(-2.28933367227002,3.89519100702498,37.2219838481309));
#40608=CARTESIAN_POINT('Ctrl Pts',(-2.93662582219991,3.51475582118734,37.2484411448154));
#40609=CARTESIAN_POINT('Ctrl Pts',(-3.48703860294563,2.96948505363274,37.2748984414998));
#40610=CARTESIAN_POINT('Ctrl Pts',(-3.87353234697123,2.32579208038141,37.3013557381843));
#40611=CARTESIAN_POINT('Ctrl Pts',(-4.26002609099678,1.68209910713015,37.3278130348688));
#40612=CARTESIAN_POINT('Ctrl Pts',(-4.48260079830228,0.939983928182159,
37.3542703315532));
#40613=CARTESIAN_POINT('Ctrl Pts',(-4.51414711586847,0.18983535101083,37.3807276282377));
#40614=CARTESIAN_POINT('Ctrl Pts',(-4.54569343343466,-0.560313226160541,
37.4071849249222));
#40615=CARTESIAN_POINT('Ctrl Pts',(-4.38621136126154,-1.31849520155516,
37.4336422216066));
#40616=CARTESIAN_POINT('Ctrl Pts',(-4.05512563923565,-1.99236484967302,
37.4600995182911));
#40617=CARTESIAN_POINT('Ctrl Pts',(-3.72403991720973,-2.66623449779091,
37.4865568149756));
#40618=CARTESIAN_POINT('Ctrl Pts',(-3.22135054533102,-3.25579181863192,
37.51301411166));
#40619=CARTESIAN_POINT('Ctrl Pts',(-2.60828453275295,-3.68922938300066,
37.5394714083445));
#40620=CARTESIAN_POINT('Ctrl Pts',(-1.99521852017489,-4.1226669473694,37.565928705029));
#40621=CARTESIAN_POINT('Ctrl Pts',(-1.27177586689746,-4.39998475526589,
37.5923860017135));
#40622=CARTESIAN_POINT('Ctrl Pts',(-0.52607108743212,-4.48740580460162,
37.6188432983979));
#40623=CARTESIAN_POINT('Ctrl Pts',(0.219633692033175,-4.57482685393735,
37.6453005950824));
#40624=CARTESIAN_POINT('Ctrl Pts',(0.987600597686399,-4.47235114471234,
37.6717578917668));
#40625=CARTESIAN_POINT('Ctrl Pts',(1.68429211034969,-4.19246010490277,37.6982151884513));
#40626=CARTESIAN_POINT('Ctrl Pts',(2.38098362301298,-3.9125690650932,37.7246724851358));
#40627=CARTESIAN_POINT('Ctrl Pts',(3.00639974268637,-3.45526269469905,37.7511297818202));
#40628=CARTESIAN_POINT('Ctrl Pts',(3.48436547816537,-2.87624040350849,37.7775870785047));
#40629=CARTESIAN_POINT('Ctrl Pts',(3.96233121364435,-2.29721811231796,37.8040443751892));
#40630=CARTESIAN_POINT('Ctrl Pts',(4.29284656492897,-1.596479900331,37.8305016718736));
#40631=CARTESIAN_POINT('Ctrl Pts',(4.43565512801649,-0.859374906258841,
37.8569589685581));
#40632=CARTESIAN_POINT('Ctrl Pts',(4.49045569410255,-0.576522323285484,
37.8671115448747));
#40633=CARTESIAN_POINT('Ctrl Pts',(4.51761603548433,-0.288314654125513,
37.8772641211914));
#40634=CARTESIAN_POINT('Ctrl Pts',(4.51744515673179,-7.51896715610657E-5,
37.887416697508));
#40635=CARTESIAN_POINT('Ctrl Pts',(4.51799626797168,8.54686663623316E-5,
37.6125833024919));
#40636=CARTESIAN_POINT('Ctrl Pts',(4.51742571357972,-0.659099555590392,
37.5893568667479));
#40637=CARTESIAN_POINT('Ctrl Pts',(4.37144018896989,-1.31852897836833,37.5661304310039));
#40638=CARTESIAN_POINT('Ctrl Pts',(4.09200051244546,-1.91548778391919,37.5429039952599));
#40639=CARTESIAN_POINT('Ctrl Pts',(3.77369001019247,-2.59548519725224,37.5164466985755));
#40640=CARTESIAN_POINT('Ctrl Pts',(3.282215397723,-3.19442354504401,37.489989401891));
#40641=CARTESIAN_POINT('Ctrl Pts',(2.67743773890556,-3.63935279939737,37.4635321052065));
#40642=CARTESIAN_POINT('Ctrl Pts',(2.07266008008816,-4.08428205375071,37.4370748085221));
#40643=CARTESIAN_POINT('Ctrl Pts',(1.3545793749228,-4.37520221466565,37.4106175118376));
#40644=CARTESIAN_POINT('Ctrl Pts',(0.610657058576267,-4.47667952851312,
37.3841602151531));
#40645=CARTESIAN_POINT('Ctrl Pts',(-0.133265257770265,-4.57815684236059,
37.3577029184686));
#40646=CARTESIAN_POINT('Ctrl Pts',(-0.903029185297969,-4.49019130914057,
37.3312456217842));
#40647=CARTESIAN_POINT('Ctrl Pts',(-1.60487832955574,-4.22349703344512,
37.3047883250997));
#40648=CARTESIAN_POINT('Ctrl Pts',(-2.30672747381355,-3.95680275774965,
37.2783310284153));
#40649=CARTESIAN_POINT('Ctrl Pts',(-2.94066183480143,-3.51137973957871,
37.2518737317308));
#40650=CARTESIAN_POINT('Ctrl Pts',(-3.42946890894599,-2.94148000958195,
37.2254164350463));
#40651=CARTESIAN_POINT('Ctrl Pts',(-3.91827598309049,-2.37158027958525,
37.1989591383619));
#40652=CARTESIAN_POINT('Ctrl Pts',(-4.26195577039172,-1.67720383776276,
37.1725018416774));
#40653=CARTESIAN_POINT('Ctrl Pts',(-4.41864845311754,-0.942924966240358,
37.1460445449929));
#40654=CARTESIAN_POINT('Ctrl Pts',(-4.57534113584337,-0.208646094717874,
37.1195872483085));
#40655=CARTESIAN_POINT('Ctrl Pts',(-4.54504671399375,0.565535206504528,
37.093129951624));
#40656=CARTESIAN_POINT('Ctrl Pts',(-4.33145501462218,1.28532451174858,37.0666726549395));
#40657=CARTESIAN_POINT('Ctrl Pts',(-4.11786331525061,2.00511381699263,37.040215358255));
#40658=CARTESIAN_POINT('Ctrl Pts',(-3.72097433835709,2.67051112625834,37.0137580615706));
#40659=CARTESIAN_POINT('Ctrl Pts',(-3.18912872207783,3.20047178369309,36.9873007648861));
#40660=CARTESIAN_POINT('Ctrl Pts',(-2.65728310579862,3.73043244112779,36.9608434682017));
#40661=CARTESIAN_POINT('Ctrl Pts',(-1.99048085013371,4.12495644673157,36.9343861715172));
#40662=CARTESIAN_POINT('Ctrl Pts',(-1.26993773185218,4.33599121325395,36.9079288748327));
#40663=CARTESIAN_POINT('Ctrl Pts',(-0.549394613570651,4.54702597977633,
36.8814715781482));
#40664=CARTESIAN_POINT('Ctrl Pts',(0.224889367327489,4.57457150721731,36.8550142814638));
#40665=CARTESIAN_POINT('Ctrl Pts',(0.958607278893124,4.41527278082006,36.8285569847793));
#40666=CARTESIAN_POINT('Ctrl Pts',(1.69232519045884,4.25597405442279,36.8020996880948));
#40667=CARTESIAN_POINT('Ctrl Pts',(2.38547703269204,3.90983107418726,36.7756423914104));
#40668=CARTESIAN_POINT('Ctrl Pts',(2.95363767834151,3.4190036720189,36.7491850947259));
#40669=CARTESIAN_POINT('Ctrl Pts',(3.52179832399097,2.92817626985055,36.7227277980414));
#40670=CARTESIAN_POINT('Ctrl Pts',(3.9649677730567,2.29266444574938,36.6962705013569));
#40671=CARTESIAN_POINT('Ctrl Pts',(4.22916847711195,1.58987283655014,36.6698132046725));
#40672=CARTESIAN_POINT('Ctrl Pts',(4.41966640325359,1.08313556444126,36.6507365706123));
#40673=CARTESIAN_POINT('Ctrl Pts',(4.51712003309545,0.541420116342586,36.6316599365521));
#40674=CARTESIAN_POINT('Ctrl Pts',(4.51763788794132,-0.000113968307276224,
36.612583302492));
#40675=CARTESIAN_POINT('Origin',(0.,0.,20.5));
#40676=CARTESIAN_POINT('',(4.51755220121239,0.000103541448102373,35.6125833024919));
#40677=CARTESIAN_POINT('',(4.51785557016588,-0.00011040733672244,35.887416697508));
#40678=CARTESIAN_POINT('',(4.51775,5.53264807684796E-16,20.5));
#40679=CARTESIAN_POINT('Ctrl Pts',(4.51785557016588,-0.000110407336722441,
35.887416697508));
#40680=CARTESIAN_POINT('Ctrl Pts',(4.51723269271139,0.611237967146432,35.9089556674308));
#40681=CARTESIAN_POINT('Ctrl Pts',(4.39224914626368,1.22283323831731,35.9304946373536));
#40682=CARTESIAN_POINT('Ctrl Pts',(4.1508481772843,1.78438254119822,35.9520336072764));
#40683=CARTESIAN_POINT('Ctrl Pts',(3.85432438440574,2.47415909794758,35.9784909039609));
#40684=CARTESIAN_POINT('Ctrl Pts',(3.38214618261964,3.08842466341222,36.0049482006454));
#40685=CARTESIAN_POINT('Ctrl Pts',(2.79182435432918,3.55236237154543,36.0314054973298));
#40686=CARTESIAN_POINT('Ctrl Pts',(2.20150252603872,4.01630007967864,36.0578627940143));
#40687=CARTESIAN_POINT('Ctrl Pts',(1.4930370712439,4.32990993048042,36.0843200906988));
#40688=CARTESIAN_POINT('Ctrl Pts',(0.752718298257879,4.45499459120493,36.1107773873832));
#40689=CARTESIAN_POINT('Ctrl Pts',(0.0123995252718205,4.58007925192944,
36.1372346840677));
#40690=CARTESIAN_POINT('Ctrl Pts',(-0.759772565905438,4.51663872257667,
36.1636919807522));
#40691=CARTESIAN_POINT('Ctrl Pts',(-1.46974826915546,4.27239998941016,36.1901492774366));
#40692=CARTESIAN_POINT('Ctrl Pts',(-2.17972397240549,4.02816125624364,36.2166065741211));
#40693=CARTESIAN_POINT('Ctrl Pts',(-2.82750328772828,3.60312431926339,36.2430638708056));
#40694=CARTESIAN_POINT('Ctrl Pts',(-3.33418741143512,3.04905820699195,36.26952116749));
#40695=CARTESIAN_POINT('Ctrl Pts',(-3.84087153514189,2.49499209472058,36.2959784641745));
#40696=CARTESIAN_POINT('Ctrl Pts',(-4.20646046723274,1.81189680715804,36.322435760859));
#40697=CARTESIAN_POINT('Ctrl Pts',(-4.3864258803877,1.08297259432656,36.3488930575434));
#40698=CARTESIAN_POINT('Ctrl Pts',(-4.56639129354267,0.354048381494999,
36.3753503542279));
#40699=CARTESIAN_POINT('Ctrl Pts',(-4.56073318776171,-0.420704756605515,
36.4018076509124));
#40700=CARTESIAN_POINT('Ctrl Pts',(-4.37014071406692,-1.14692274519782,
36.4282649475969));
#40701=CARTESIAN_POINT('Ctrl Pts',(-4.17954824037214,-1.87314073379008,
36.4547222442813));
#40702=CARTESIAN_POINT('Ctrl Pts',(-3.80402139876356,-2.55082357287414,
36.4811795409658));
#40703=CARTESIAN_POINT('Ctrl Pts',(-3.28929894294182,-3.09743024266232,
36.5076368376502));
#40704=CARTESIAN_POINT('Ctrl Pts',(-2.77457648712008,-3.64403691245051,
36.5340941343347));
#40705=CARTESIAN_POINT('Ctrl Pts',(-2.12065841708519,-4.05956741294281,
36.5605514310192));
#40706=CARTESIAN_POINT('Ctrl Pts',(-1.40719123005584,-4.29341058905986,
36.5870087277037));
#40707=CARTESIAN_POINT('Ctrl Pts',(-0.693724043026525,-4.52725376517689,
36.6134660243881));
#40708=CARTESIAN_POINT('Ctrl Pts',(0.0792922609972423,-4.57940961691868,
36.6399233210726));
#40709=CARTESIAN_POINT('Ctrl Pts',(0.817705151706661,-4.4435256192656,36.6663806177571));
#40710=CARTESIAN_POINT('Ctrl Pts',(1.55611804241612,-4.30764162161251,36.6928379144415));
#40711=CARTESIAN_POINT('Ctrl Pts',(2.25992751981123,-3.98371777456452,36.719295211126));
#40712=CARTESIAN_POINT('Ctrl Pts',(2.84341036847319,-3.51120764419544,36.7457525078105));
#40713=CARTESIAN_POINT('Ctrl Pts',(3.42689321713519,-3.03869751382634,36.7722098044949));
#40714=CARTESIAN_POINT('Ctrl Pts',(3.89004943706403,-2.41760110013612,36.7986671011794));
#40715=CARTESIAN_POINT('Ctrl Pts',(4.17646711326182,-1.72356725892547,36.8251243978639));
#40716=CARTESIAN_POINT('Ctrl Pts',(4.40125218133937,-1.17887865480133,36.8458884977453));
#40717=CARTESIAN_POINT('Ctrl Pts',(4.51717769407857,-0.589265294821556,
36.8666525976266));
#40718=CARTESIAN_POINT('Ctrl Pts',(4.51778606435352,0.000115791782295315,
36.887416697508));
#40719=CARTESIAN_POINT('Ctrl Pts',(4.51763788794132,-0.000113968307276224,
36.612583302492));
#40720=CARTESIAN_POINT('Ctrl Pts',(4.51783824361694,-0.209631033306269,
36.6052026398677));
#40721=CARTESIAN_POINT('Ctrl Pts',(4.50352846951492,-0.419120950359322,
36.5978219772434));
#40722=CARTESIAN_POINT('Ctrl Pts',(4.47448319596349,-0.626547502778321,
36.5904413146191));
#40723=CARTESIAN_POINT('Ctrl Pts',(4.37036525171502,-1.37010483861031,36.5639840179346));
#40724=CARTESIAN_POINT('Ctrl Pts',(4.07689740417331,-2.08714811597701,36.5375267212501));
#40725=CARTESIAN_POINT('Ctrl Pts',(3.62982371237891,-2.69034225726936,36.5110694245657));
#40726=CARTESIAN_POINT('Ctrl Pts',(3.18275002058453,-3.29353639856167,36.4846121278812));
#40727=CARTESIAN_POINT('Ctrl Pts',(2.58207048453748,-3.78288140377964,36.4581548311967));
#40728=CARTESIAN_POINT('Ctrl Pts',(1.90094720693747,-4.09877559286112,36.4316975345123));
#40729=CARTESIAN_POINT('Ctrl Pts',(1.21982392933739,-4.41466978194264,36.4052402378278));
#40730=CARTESIAN_POINT('Ctrl Pts',(0.458256910184331,-4.55711315488762,
36.3787829411434));
#40731=CARTESIAN_POINT('Ctrl Pts',(-0.290995830438852,-4.50875626651792,
36.3523256444589));
#40732=CARTESIAN_POINT('Ctrl Pts',(-1.04024857106204,-4.46039937814821,
36.3258683477744));
#40733=CARTESIAN_POINT('Ctrl Pts',(-1.77718703315534,-4.2212422284638,36.2994110510899));
#40734=CARTESIAN_POINT('Ctrl Pts',(-2.41205292762861,-3.82041389361357,
36.2729537544055));
#40735=CARTESIAN_POINT('Ctrl Pts',(-3.04691882210185,-3.41958555876337,
36.246496457721));
#40736=CARTESIAN_POINT('Ctrl Pts',(-3.57971214895505,-2.85708603874736,
36.2200391610366));
#40737=CARTESIAN_POINT('Ctrl Pts',(-3.94553927063653,-2.20142715256771,
36.1935818643521));
#40738=CARTESIAN_POINT('Ctrl Pts',(-4.311366392318,-1.54576826638806,36.1671245676676));
#40739=CARTESIAN_POINT('Ctrl Pts',(-4.51022730882774,-0.796950014044777,
36.1406672709831));
#40740=CARTESIAN_POINT('Ctrl Pts',(-4.51790098062044,-0.0461776299327186,
36.1142099742986));
#40741=CARTESIAN_POINT('Ctrl Pts',(-4.52557465241315,0.70459475417934,36.0877526776142));
#40742=CARTESIAN_POINT('Ctrl Pts',(-4.34206107948882,1.45732127006017,36.0612953809297));
#40743=CARTESIAN_POINT('Ctrl Pts',(-3.98971201192945,2.12032066114143,36.0348380842453));
#40744=CARTESIAN_POINT('Ctrl Pts',(-3.63736294437007,2.78332005222269,36.0083807875608));
#40745=CARTESIAN_POINT('Ctrl Pts',(-3.11617838217574,3.3565923185043,35.9819234908763));
#40746=CARTESIAN_POINT('Ctrl Pts',(-2.48963802821032,3.77031353241165,35.9554661941919));
#40747=CARTESIAN_POINT('Ctrl Pts',(-1.86309767424487,4.18403474631902,35.9290088975074));
#40748=CARTESIAN_POINT('Ctrl Pts',(-1.13120152850826,4.43820490785206,35.9025516008229));
#40749=CARTESIAN_POINT('Ctrl Pts',(-0.383093731539153,4.501866372634,35.8760943041385));
#40750=CARTESIAN_POINT('Ctrl Pts',(0.365014065429868,4.56552783741593,35.849637007454));
#40751=CARTESIAN_POINT('Ctrl Pts',(1.12933351363151,4.43868060544686,35.8231797107695));
#40752=CARTESIAN_POINT('Ctrl Pts',(1.81677135017102,4.13677452919484,35.7967224140851));
#40753=CARTESIAN_POINT('Ctrl Pts',(2.50420918671061,3.83486845294278,35.7702651174006));
#40754=CARTESIAN_POINT('Ctrl Pts',(3.11476541158806,3.35790353240771,35.7438078207161));
#40755=CARTESIAN_POINT('Ctrl Pts',(3.57407495233493,2.76397356703885,35.7173505240316));
#40756=CARTESIAN_POINT('Ctrl Pts',(4.03338449308179,2.17004360166999,35.6908932273472));
#40757=CARTESIAN_POINT('Ctrl Pts',(4.34144734969803,1.45914859146745,35.6644359306627));
#40758=CARTESIAN_POINT('Ctrl Pts',(4.46074180719067,0.717874761903989,35.6379786339782));
#40759=CARTESIAN_POINT('Ctrl Pts',(4.49891051264125,0.480701442593838,35.6295135234828));
#40760=CARTESIAN_POINT('Ctrl Pts',(4.51775492478579,0.240418231912197,35.6210484129874));
#40761=CARTESIAN_POINT('Ctrl Pts',(4.51755220121239,0.000103541448102373,
35.6125833024919));
#40762=CARTESIAN_POINT('Origin',(0.,0.,20.5));
#40763=CARTESIAN_POINT('',(4.51806911322653,-6.09724841136444E-5,34.6125833024919));
#40764=CARTESIAN_POINT('',(4.51740954388543,5.82741782004033E-5,34.887416697508));
#40765=CARTESIAN_POINT('',(4.51775,5.53264807684796E-16,20.5));
#40766=CARTESIAN_POINT('Ctrl Pts',(4.51740954388543,5.82741782004033E-5,
34.887416697508));
#40767=CARTESIAN_POINT('Ctrl Pts',(4.51755065915555,0.31030389790581,34.8983441438661));
#40768=CARTESIAN_POINT('Ctrl Pts',(4.48605373157874,0.620521268509011,34.9092715902241));
#40769=CARTESIAN_POINT('Ctrl Pts',(4.42263045256682,0.924067921868281,34.9201990365822));
#40770=CARTESIAN_POINT('Ctrl Pts',(4.26907138171545,1.65900851112936,34.9466563332667));
#40771=CARTESIAN_POINT('Ctrl Pts',(3.92835669717202,2.35484465771423,34.9731136299511));
#40772=CARTESIAN_POINT('Ctrl Pts',(3.44198507043434,2.92682428907246,34.9995709266356));
#40773=CARTESIAN_POINT('Ctrl Pts',(2.95561344369671,3.49880392043062,35.02602822332));
#40774=CARTESIAN_POINT('Ctrl Pts',(2.32358487476487,3.94692703656216,35.0524855200045));
#40775=CARTESIAN_POINT('Ctrl Pts',(1.62287974384894,4.21661273787411,35.078942816689));
#40776=CARTESIAN_POINT('Ctrl Pts',(0.922174612932932,4.48629843918609,35.1054001133734));
#40777=CARTESIAN_POINT('Ctrl Pts',(0.152792920032838,4.57754672567843,35.1318574100579));
#40778=CARTESIAN_POINT('Ctrl Pts',(-0.591555496154874,4.47924365704371,
35.1583147067424));
#40779=CARTESIAN_POINT('Ctrl Pts',(-1.3359039123425,4.380940588409,35.1847720034269));
#40780=CARTESIAN_POINT('Ctrl Pts',(-2.05521905181772,4.09308616464727,35.2112293001113));
#40781=CARTESIAN_POINT('Ctrl Pts',(-2.66188912668102,3.65074073599519,35.2376865967958));
#40782=CARTESIAN_POINT('Ctrl Pts',(-3.26855920154439,3.20839530734307,35.2641438934803));
#40783=CARTESIAN_POINT('Ctrl Pts',(-3.76258421179579,2.61155887380058,35.2906011901647));
#40784=CARTESIAN_POINT('Ctrl Pts',(-4.08379245793952,1.93292545243568,35.3170584868492));
#40785=CARTESIAN_POINT('Ctrl Pts',(-4.40500070408323,1.25429203107082,35.3435157835337));
#40786=CARTESIAN_POINT('Ctrl Pts',(-4.55339218611928,0.493861621883449,
35.3699730802181));
#40787=CARTESIAN_POINT('Ctrl Pts',(-4.51089298576514,-0.255746192879281,
35.3964303769026));
#40788=CARTESIAN_POINT('Ctrl Pts',(-4.468393785411,-1.00535400764205,35.4228876735871));
#40789=CARTESIAN_POINT('Ctrl Pts',(-4.23500390266671,-1.74413922798016,
35.4493449702715));
#40790=CARTESIAN_POINT('Ctrl Pts',(-3.83914996695061,-2.38211863169333,
35.475802266956));
#40791=CARTESIAN_POINT('Ctrl Pts',(-3.44329603123454,-3.02009803540644,
35.5022595636405));
#40792=CARTESIAN_POINT('Ctrl Pts',(-2.88497804254663,-3.55727162249458,
35.5287168603249));
#40793=CARTESIAN_POINT('Ctrl Pts',(-2.23219851400125,-3.92821224455706,
35.5551741570094));
#40794=CARTESIAN_POINT('Ctrl Pts',(-1.57941898545579,-4.29915286661958,
35.5816314536939));
#40795=CARTESIAN_POINT('Ctrl Pts',(-0.83217791705278,-4.50386052365648,
35.6080887503783));
#40796=CARTESIAN_POINT('Ctrl Pts',(-0.081488443928666,-4.51740204959703,
35.6345460470628));
#40797=CARTESIAN_POINT('Ctrl Pts',(0.669201029195319,-4.53094357553758,
35.6610033437473));
#40798=CARTESIAN_POINT('Ctrl Pts',(1.42333890704038,-4.35331897038184,35.6874606404318));
#40799=CARTESIAN_POINT('Ctrl Pts',(2.08907203071298,-4.00616271445508,35.7139179371162));
#40800=CARTESIAN_POINT('Ctrl Pts',(2.75480515438577,-3.65900645852822,35.7403752338007));
#40801=CARTESIAN_POINT('Ctrl Pts',(3.33213352388603,-3.14231855183025,35.7668325304851));
#40802=CARTESIAN_POINT('Ctrl Pts',(3.75073918275594,-2.51903100956234,35.7932898271696));
#40803=CARTESIAN_POINT('Ctrl Pts',(4.16934484162576,-1.89574346729458,35.8197471238541));
#40804=CARTESIAN_POINT('Ctrl Pts',(4.42922778986531,-1.16585628945694,35.8462044205385));
#40805=CARTESIAN_POINT('Ctrl Pts',(4.49873457199958,-0.4182689265211,35.872661717223));
#40806=CARTESIAN_POINT('Ctrl Pts',(4.51165566030144,-0.279294828839705,
35.8775800439847));
#40807=CARTESIAN_POINT('Ctrl Pts',(4.51799780142692,-0.139709054890449,
35.8824983707463));
#40808=CARTESIAN_POINT('Ctrl Pts',(4.51785557016588,-0.000110407336722441,
35.887416697508));
#40809=CARTESIAN_POINT('Ctrl Pts',(4.51755220121239,0.000103541448102373,
35.6125833024919));
#40810=CARTESIAN_POINT('Ctrl Pts',(4.51712132198412,-0.510673802465055,
35.5945911163029));
#40811=CARTESIAN_POINT('Ctrl Pts',(4.43064412559555,-1.02159335775301,35.5765989301139));
#40812=CARTESIAN_POINT('Ctrl Pts',(4.26078183149926,-1.50309674624197,35.5586067439248));
#40813=CARTESIAN_POINT('Ctrl Pts',(4.01100133994626,-2.21114177590013,35.5321494472404));
#40814=CARTESIAN_POINT('Ctrl Pts',(3.58091429847129,-2.85557918629222,35.5056921505559));
#40815=CARTESIAN_POINT('Ctrl Pts',(3.02290483273525,-3.35791721405148,35.4792348538714));
#40816=CARTESIAN_POINT('Ctrl Pts',(2.46489536699924,-3.86025524181071,35.452777557187));
#40817=CARTESIAN_POINT('Ctrl Pts',(1.77896347700217,-4.22049388693713,35.4263202605025));
#40818=CARTESIAN_POINT('Ctrl Pts',(1.04865490780343,-4.39475648114172,35.399862963818));
#40819=CARTESIAN_POINT('Ctrl Pts',(0.318346338604615,-4.56901907534632,
35.3734056671336));
#40820=CARTESIAN_POINT('Ctrl Pts',(-0.456338909795902,-4.55730561862904,
35.3469483704491));
#40821=CARTESIAN_POINT('Ctrl Pts',(-1.18104503151125,-4.36104279705439,
35.3204910737646));
#40822=CARTESIAN_POINT('Ctrl Pts',(-1.9057511532266,-4.16477997547974,35.2940337770802));
#40823=CARTESIAN_POINT('Ctrl Pts',(-2.5804781482568,-3.78396778904771,35.2675764803957));
#40824=CARTESIAN_POINT('Ctrl Pts',(-3.1230450153486,-3.26498874060901,35.2411191837112));
#40825=CARTESIAN_POINT('Ctrl Pts',(-3.66561188244036,-2.74600969217034,
35.2146618870268));
#40826=CARTESIAN_POINT('Ctrl Pts',(-4.07601862159375,-2.08886378172499,
35.1882045903423));
#40827=CARTESIAN_POINT('Ctrl Pts',(-4.30427814618982,-1.37359065388133,
35.1617472936578));
#40828=CARTESIAN_POINT('Ctrl Pts',(-4.53253767078589,-0.658317526037631,
35.1352899969733));
#40829=CARTESIAN_POINT('Ctrl Pts',(-4.57864998082464,0.115082819204295,
35.1088327002889));
#40830=CARTESIAN_POINT('Ctrl Pts',(-4.43699864797729,0.852411075740494,
35.0823754036044));
#40831=CARTESIAN_POINT('Ctrl Pts',(-4.29534731512995,1.58973933227665,35.0559181069199));
#40832=CARTESIAN_POINT('Ctrl Pts',(-3.9659323393965,2.29099550010699,35.0294608102355));
#40833=CARTESIAN_POINT('Ctrl Pts',(-3.48887610024745,2.87076735409185,35.003003513551));
#40834=CARTESIAN_POINT('Ctrl Pts',(-3.0118198610984,3.45053920807671,34.9765462168666));
#40835=CARTESIAN_POINT('Ctrl Pts',(-2.38712235853373,3.90882674821612,34.9500889201821));
#40836=CARTESIAN_POINT('Ctrl Pts',(-1.69087105699361,4.18981105932221,34.9236316234976));
#40837=CARTESIAN_POINT('Ctrl Pts',(-0.994619755453442,4.47079537042831,
34.8971743268131));
#40838=CARTESIAN_POINT('Ctrl Pts',(-0.22681465493779,4.57447645250109,34.8707170301287));
#40839=CARTESIAN_POINT('Ctrl Pts',(0.519026433064394,4.48822606449116,34.8442597334442));
#40840=CARTESIAN_POINT('Ctrl Pts',(1.26486752106653,4.40197567648124,34.8178024367597));
#40841=CARTESIAN_POINT('Ctrl Pts',(1.98874459655524,4.12579381838863,34.7913451400753));
#40842=CARTESIAN_POINT('Ctrl Pts',(2.60249023287332,3.69331913486993,34.7648878433908));
#40843=CARTESIAN_POINT('Ctrl Pts',(3.2162358691914,3.26084445135124,34.7384305467063));
#40844=CARTESIAN_POINT('Ctrl Pts',(3.71985006633887,2.67207694240644,34.7119732500218));
#40845=CARTESIAN_POINT('Ctrl Pts',(4.05199317246873,1.99872783901765,34.6855159533374));
#40846=CARTESIAN_POINT('Ctrl Pts',(4.35719035466755,1.38000583275685,34.6612050697222));
#40847=CARTESIAN_POINT('Ctrl Pts',(4.51760990627478,0.689869322963186,34.6368941861071));
#40848=CARTESIAN_POINT('Ctrl Pts',(4.51806911322653,-6.09724841136444E-5,
34.6125833024919));
#40849=CARTESIAN_POINT('Origin',(0.,0.,20.5));
#40850=CARTESIAN_POINT('',(4.5173649459528,-1.24327273773317E-5,33.6125833024919));
#40851=CARTESIAN_POINT('',(4.51813527504661,9.51052893547258E-6,33.887416697508));
#40852=CARTESIAN_POINT('',(4.51775,5.53264807684796E-16,20.5));
#40853=CARTESIAN_POINT('Ctrl Pts',(4.51813527504661,9.51052893547258E-6,
33.887416697508));
#40854=CARTESIAN_POINT('Ctrl Pts',(4.51813637042829,0.00897485417732503,
33.8877326203013));
#40855=CARTESIAN_POINT('Ctrl Pts',(4.51811024333632,0.0179401914138076,
33.8880485430946));
#40856=CARTESIAN_POINT('Ctrl Pts',(4.51805685504966,0.0269053663078375,
33.8883644658879));
#40857=CARTESIAN_POINT('Ctrl Pts',(4.51358579512714,0.777703653204736,33.9148217625724));
#40858=CARTESIAN_POINT('Ctrl Pts',(4.31792089423795,1.52736336648647,33.9412790592569));
#40859=CARTESIAN_POINT('Ctrl Pts',(3.95489392076193,2.18457678274711,33.9677363559413));
#40860=CARTESIAN_POINT('Ctrl Pts',(3.59186694728593,2.84179019900772,33.9941936526258));
#40861=CARTESIAN_POINT('Ctrl Pts',(3.06147790122311,3.40655731824726,34.0206509493103));
#40862=CARTESIAN_POINT('Ctrl Pts',(2.42832758138582,3.81009013038776,34.0471082459947));
#40863=CARTESIAN_POINT('Ctrl Pts',(1.79517726154854,4.21362294252827,34.0735655426792));
#40864=CARTESIAN_POINT('Ctrl Pts',(1.05926566793676,4.45592144756974,34.1000228393637));
#40865=CARTESIAN_POINT('Ctrl Pts',(0.310226018196078,4.50747395575744,34.1264801360482));
#40866=CARTESIAN_POINT('Ctrl Pts',(-0.438813631544642,4.55902646394514,
34.1529374327326));
#40867=CARTESIAN_POINT('Ctrl Pts',(-1.20098133741429,4.41983297527906,34.1793947294171));
#40868=CARTESIAN_POINT('Ctrl Pts',(-1.8834459163527,4.10684710262894,34.2058520261016));
#40869=CARTESIAN_POINT('Ctrl Pts',(-2.56591049529112,3.79386122997882,34.232309322786));
#40870=CARTESIAN_POINT('Ctrl Pts',(-3.16867194729824,3.30708297334475,34.2587666194705));
#40871=CARTESIAN_POINT('Ctrl Pts',(-3.61831459461467,2.70580138565192,34.2852239161549));
#40872=CARTESIAN_POINT('Ctrl Pts',(-4.06795724193109,2.10451979795912,34.3116812128394));
#40873=CARTESIAN_POINT('Ctrl Pts',(-4.36448108455674,1.38873487920764,34.3381385095239));
#40874=CARTESIAN_POINT('Ctrl Pts',(-4.47176984663203,0.645628440319887,
34.3645958062084));
#40875=CARTESIAN_POINT('Ctrl Pts',(-4.57905860870732,-0.0974779985678242,
34.3910531028928));
#40876=CARTESIAN_POINT('Ctrl Pts',(-4.49711229023226,-0.86790595759181,
34.4175103995773));
#40877=CARTESIAN_POINT('Ctrl Pts',(-4.23591186210457,-1.57181816399963,
34.4439676962618));
#40878=CARTESIAN_POINT('Ctrl Pts',(-3.97471143397686,-2.27573037040753,
34.4704249929462));
#40879=CARTESIAN_POINT('Ctrl Pts',(-3.53425689619645,-2.91312682419928,
34.4968822896307));
#40880=CARTESIAN_POINT('Ctrl Pts',(-2.96819512400025,-3.40637334272956,
34.5233395863152));
#40881=CARTESIAN_POINT('Ctrl Pts',(-2.40213335180411,-3.89961986125978,
34.5497968829996));
#40882=CARTESIAN_POINT('Ctrl Pts',(-1.71046434519219,-4.24871644452859,
34.5762541796841));
#40883=CARTESIAN_POINT('Ctrl Pts',(-0.977432623678127,-4.41114351504993,
34.6027114763686));
#40884=CARTESIAN_POINT('Ctrl Pts',(-0.244400902164024,-4.57357058557128,
34.629168773053));
#40885=CARTESIAN_POINT('Ctrl Pts',(0.529993534252376,-4.54932814334514,
34.6556260697375));
#40886=CARTESIAN_POINT('Ctrl Pts',(1.25143030026179,-4.34136889100478,34.682083366422));
#40887=CARTESIAN_POINT('Ctrl Pts',(1.97286706627129,-4.13340963866439,34.7085406631064));
#40888=CARTESIAN_POINT('Ctrl Pts',(2.64134616187382,-3.74173357620983,34.7349979597909));
#40889=CARTESIAN_POINT('Ctrl Pts',(3.17544757305189,-3.21404641456781,34.7614552564754));
#40890=CARTESIAN_POINT('Ctrl Pts',(3.70954898422987,-2.68635925292589,34.7879125531598));
#40891=CARTESIAN_POINT('Ctrl Pts',(4.10927271098332,-2.0226609920966,34.8143698498443));
#40892=CARTESIAN_POINT('Ctrl Pts',(4.3259328457804,-1.30378934571338,34.8408271465288));
#40893=CARTESIAN_POINT('Ctrl Pts',(4.45310757210366,-0.881827525298336,
34.8563569968552));
#40894=CARTESIAN_POINT('Ctrl Pts',(4.51720899391685,-0.440856093465167,
34.8718868471816));
#40895=CARTESIAN_POINT('Ctrl Pts',(4.51740954388543,5.82741782004033E-5,
34.887416697508));
#40896=CARTESIAN_POINT('Ctrl Pts',(4.51806911322653,-6.09724841136444E-5,
34.6125833024919));
#40897=CARTESIAN_POINT('Ctrl Pts',(4.51810965670567,-0.0609750645635587,
34.6104368894226));
#40898=CARTESIAN_POINT('Ctrl Pts',(4.51690328345783,-0.121887549168861,
34.6082904763533));
#40899=CARTESIAN_POINT('Ctrl Pts',(4.51443954418555,-0.182749134310292,
34.606144063284));
#40900=CARTESIAN_POINT('Ctrl Pts',(4.48407079466025,-0.932946306416683,
34.5796867665996));
#40901=CARTESIAN_POINT('Ctrl Pts',(4.26266128049739,-1.67540995279661,34.5532294699151));
#40902=CARTESIAN_POINT('Ctrl Pts',(3.87717843548116,-2.3197088230287,34.5267721732306));
#40903=CARTESIAN_POINT('Ctrl Pts',(3.49169559046496,-2.96400769326076,34.5003148765461));
#40904=CARTESIAN_POINT('Ctrl Pts',(2.94213941459544,-3.51014178734499,34.4738575798616));
#40905=CARTESIAN_POINT('Ctrl Pts',(2.2954452418825,-3.8915925770456,34.4474002831772));
#40906=CARTESIAN_POINT('Ctrl Pts',(1.64875106916955,-4.2730433667462,34.4209429864927));
#40907=CARTESIAN_POINT('Ctrl Pts',(0.904918899613214,-4.48981085206318,
34.3944856898083));
#40908=CARTESIAN_POINT('Ctrl Pts',(0.154546668243127,-4.51549299318827,
34.3680283931238));
#40909=CARTESIAN_POINT('Ctrl Pts',(-0.595825563126962,-4.54117513431336,
34.3415710964393));
#40910=CARTESIAN_POINT('Ctrl Pts',(-1.35273785631077,-4.37577193124655,
34.3151137997548));
#40911=CARTESIAN_POINT('Ctrl Pts',(-2.02399913169702,-4.03942931106451,
34.2886565030704));
#40912=CARTESIAN_POINT('Ctrl Pts',(-2.69526040708323,-3.70308669088248,
34.2621992063859));
#40913=CARTESIAN_POINT('Ctrl Pts',(-3.28087066467185,-3.19580465358524,
34.2357419097014));
#40914=CARTESIAN_POINT('Ctrl Pts',(-3.7095032232018,-2.57936958989069,34.209284613017));
#40915=CARTESIAN_POINT('Ctrl Pts',(-4.13813578173176,-1.9629345261961,34.1828273163325));
#40916=CARTESIAN_POINT('Ctrl Pts',(-4.40979064120305,-1.23734643610409,
34.1563700196481));
#40917=CARTESIAN_POINT('Ctrl Pts',(-4.49138054038088,-0.490981145957072,
34.1299127229636));
#40918=CARTESIAN_POINT('Ctrl Pts',(-4.57297043955872,0.255384144190028,
34.1034554262791));
#40919=CARTESIAN_POINT('Ctrl Pts',(-4.46449537844313,1.02252663439224,34.0769981295946));
#40920=CARTESIAN_POINT('Ctrl Pts',(-4.17916749942524,1.71700921836348,34.0505408329102));
#40921=CARTESIAN_POINT('Ctrl Pts',(-3.89383962040737,2.41149180233465,34.0240835362257));
#40922=CARTESIAN_POINT('Ctrl Pts',(-3.43165892348727,3.03331448007484,33.9976262395413));
#40923=CARTESIAN_POINT('Ctrl Pts',(-2.84891850603996,3.50673993762589,33.9711689428568));
#40924=CARTESIAN_POINT('Ctrl Pts',(-2.26617808859268,3.98016539517692,33.9447116461723));
#40925=CARTESIAN_POINT('Ctrl Pts',(-1.56287795061823,4.30519363253881,33.9182543494878));
#40926=CARTESIAN_POINT('Ctrl Pts',(-0.824679270557638,4.44223657011982,
33.8917970528033));
#40927=CARTESIAN_POINT('Ctrl Pts',(-0.0864805904969625,4.57927950770084,
33.8653397561189));
#40928=CARTESIAN_POINT('Ctrl Pts',(0.686616631649836,4.52833714550091,33.8388824594344));
#40929=CARTESIAN_POINT('Ctrl Pts',(1.40045000983613,4.2956142068565,33.81242516275));
#40930=CARTESIAN_POINT('Ctrl Pts',(2.11428338802235,4.0628912682121,33.7859678660655));
#40931=CARTESIAN_POINT('Ctrl Pts',(2.76885292224806,3.64838775312326,33.759510569381));
#40932=CARTESIAN_POINT('Ctrl Pts',(3.28443276767714,3.10258973098379,33.7330532726965));
#40933=CARTESIAN_POINT('Ctrl Pts',(3.80001261310627,2.55679170884426,33.7065959760121));
#40934=CARTESIAN_POINT('Ctrl Pts',(4.17660276973874,1.87969917965409,33.6801386793276));
#40935=CARTESIAN_POINT('Ctrl Pts',(4.36833497328078,1.15378126410918,33.6536813826432));
#40936=CARTESIAN_POINT('Ctrl Pts',(4.46761225473945,0.777907227895749,33.6399820225928));
#40937=CARTESIAN_POINT('Ctrl Pts',(4.51732765695876,0.388942719447438,33.6262826625424));
#40938=CARTESIAN_POINT('Ctrl Pts',(4.5173649459528,-1.24327273773317E-5,
33.6125833024919));
#40939=CARTESIAN_POINT('Origin',(0.,0.,20.5));
#40940=CARTESIAN_POINT('',(4.51800690475437,8.25810157162321E-5,32.6125833024919));
#40941=CARTESIAN_POINT('',(4.5174378855045,-7.22228901865168E-5,32.887416697508));
#40942=CARTESIAN_POINT('',(4.51775,5.53264807684796E-16,20.5));
#40943=CARTESIAN_POINT('Ctrl Pts',(4.5174378855045,-7.22228901865168E-5,
32.887416697508));
#40944=CARTESIAN_POINT('Ctrl Pts',(4.51717714450692,0.458772891828189,32.9035783934211));
#40945=CARTESIAN_POINT('Ctrl Pts',(4.44766773093088,0.917695233524441,32.9197400893341));
#40946=CARTESIAN_POINT('Ctrl Pts',(4.31009826091021,1.35521755651858,32.9359017852471));
#40947=CARTESIAN_POINT('Ctrl Pts',(4.08489192720295,2.07145785505129,32.9623590819316));
#40948=CARTESIAN_POINT('Ctrl Pts',(3.67729208498414,2.73034844367792,32.988816378616));
#40949=CARTESIAN_POINT('Ctrl Pts',(3.13694394393257,3.25163717791855,33.0152736753005));
#40950=CARTESIAN_POINT('Ctrl Pts',(2.596595802881,3.77292591215919,33.0417309719849));
#40951=CARTESIAN_POINT('Ctrl Pts',(1.92349936299679,4.15661279201376,33.0681882686694));
#40952=CARTESIAN_POINT('Ctrl Pts',(1.19963702572075,4.35596518015436,33.0946455653539));
#40953=CARTESIAN_POINT('Ctrl Pts',(0.475774688444753,4.55531756829496,33.1211028620384));
#40954=CARTESIAN_POINT('Ctrl Pts',(-0.298853546223071,4.57033546472152,
33.1475601587228));
#40955=CARTESIAN_POINT('Ctrl Pts',(-1.02989881660521,4.39918970627007,33.1740174554073));
#40956=CARTESIAN_POINT('Ctrl Pts',(-1.76094408698744,4.2280439478186,33.2004747520918));
#40957=CARTESIAN_POINT('Ctrl Pts',(-2.4484063930841,3.87073453448909,33.2269320487762));
#40958=CARTESIAN_POINT('Ctrl Pts',(-3.00855358684862,3.37078135737958,33.2533893454607));
#40959=CARTESIAN_POINT('Ctrl Pts',(-3.56870078061313,2.87082818027007,33.2798466421452));
#40960=CARTESIAN_POINT('Ctrl Pts',(-4.0015328620455,2.22823123938057,33.3063039388296));
#40961=CARTESIAN_POINT('Ctrl Pts',(-4.25433136265604,1.52125813092933,33.3327612355141));
#40962=CARTESIAN_POINT('Ctrl Pts',(-4.50712986326656,0.814285022478126,
33.3592185321986));
#40963=CARTESIAN_POINT('Ctrl Pts',(-4.57989478305528,0.0429357464651833,
33.3856758288831));
#40964=CARTESIAN_POINT('Ctrl Pts',(-4.46376343532313,-0.698840208967454,
33.4121331255675));
#40965=CARTESIAN_POINT('Ctrl Pts',(-4.34763208759097,-1.44061616440009,
33.438590422252));
#40966=CARTESIAN_POINT('Ctrl Pts',(-4.04260447233795,-2.15281879925242,
33.4650477189364));
#40967=CARTESIAN_POINT('Ctrl Pts',(-3.5858326155183,-2.74870262081633,33.4915050156209));
#40968=CARTESIAN_POINT('Ctrl Pts',(-3.12906075869862,-3.34458644238028,
33.5179623123054));
#40969=CARTESIAN_POINT('Ctrl Pts',(-2.52054466031228,-3.82415145065579,
33.5444196089899));
#40970=CARTESIAN_POINT('Ctrl Pts',(-1.83440090767899,-4.12898715838447,
33.5708769056743));
#40971=CARTESIAN_POINT('Ctrl Pts',(-1.14825715504573,-4.43382286611314,
33.5973342023588));
#40972=CARTESIAN_POINT('Ctrl Pts',(-0.384485748165517,-4.56392927329501,
33.6237914990433));
#40973=CARTESIAN_POINT('Ctrl Pts',(0.363886800893304,-4.50345956352814,
33.6502487957277));
#40974=CARTESIAN_POINT('Ctrl Pts',(1.11225934995217,-4.44298985376126,33.6767060924122));
#40975=CARTESIAN_POINT('Ctrl Pts',(1.84523304118964,-4.19194402704563,33.7031633890966));
#40976=CARTESIAN_POINT('Ctrl Pts',(2.47353249021786,-3.78089918723496,33.7296206857811));
#40977=CARTESIAN_POINT('Ctrl Pts',(3.10183193924602,-3.36985434742433,33.7560779824656));
#40978=CARTESIAN_POINT('Ctrl Pts',(3.62545714606495,-2.7988104945187,33.7825352791501));
#40979=CARTESIAN_POINT('Ctrl Pts',(3.98063113999648,-2.1373201378099,33.8089925758346));
#40980=CARTESIAN_POINT('Ctrl Pts',(4.3315640520969,-1.48372854278193,33.8351339497257));
#40981=CARTESIAN_POINT('Ctrl Pts',(4.51804463650222,-0.741837565236255,
33.8612753236169));
#40982=CARTESIAN_POINT('Ctrl Pts',(4.51813527504661,9.51052893547258E-6,
33.887416697508));
#40983=CARTESIAN_POINT('Ctrl Pts',(4.5173649459528,-1.24327273773317E-5,
33.6125833024919));
#40984=CARTESIAN_POINT('Ctrl Pts',(4.51739967243793,-0.362238490490815,
33.5998253658579));
#40985=CARTESIAN_POINT('Ctrl Pts',(4.47434946667155,-0.724456433726874,
33.5870674292238));
#40986=CARTESIAN_POINT('Ctrl Pts',(4.38812044853862,-1.07608576485082,33.5743094925897));
#40987=CARTESIAN_POINT('Ctrl Pts',(4.20929946980279,-1.80529157636637,33.5478521959053));
#40988=CARTESIAN_POINT('Ctrl Pts',(3.84478326187951,-2.48895989749788,33.5213948992208));
#40989=CARTESIAN_POINT('Ctrl Pts',(3.33896949547234,-3.04382068336861,33.4949376025364));
#40990=CARTESIAN_POINT('Ctrl Pts',(2.83315572906515,-3.59868146923937,33.4684803058519));
#40991=CARTESIAN_POINT('Ctrl Pts',(2.18604440417407,-4.02473471984934,33.4420230091674));
#40992=CARTESIAN_POINT('Ctrl Pts',(1.47645296399252,-4.27008762080067,33.4155657124829));
#40993=CARTESIAN_POINT('Ctrl Pts',(0.766861523811012,-4.51544052175197,
33.3891084157985));
#40994=CARTESIAN_POINT('Ctrl Pts',(-0.00521003166095199,-4.58009307304465,
33.362651119114));
#40995=CARTESIAN_POINT('Ctrl Pts',(-0.745724241442587,-4.45617066548424,
33.3361938224295));
#40996=CARTESIAN_POINT('Ctrl Pts',(-1.48623845122422,-4.33224825792383,
33.3097365257451));
#40997=CARTESIAN_POINT('Ctrl Pts',(-2.19519531531565,-4.01975089151028,
33.2832792290606));
#40998=CARTESIAN_POINT('Ctrl Pts',(-2.78624467229499,-3.55674039962226,
33.2568219323761));
#40999=CARTESIAN_POINT('Ctrl Pts',(-3.37729402927434,-3.09372990773425,
33.2303646356917));
#41000=CARTESIAN_POINT('Ctrl Pts',(-3.85043587914167,-2.48020629037183,
33.2039073390072));
#41001=CARTESIAN_POINT('Ctrl Pts',(-4.14804206822415,-1.7908960451238,33.1774500423227));
#41002=CARTESIAN_POINT('Ctrl Pts',(-4.44564825730663,-1.10158579987578,
33.1509927456383));
#41003=CARTESIAN_POINT('Ctrl Pts',(-4.56771878560417,-0.33648892674225,
33.1245354489538));
#41004=CARTESIAN_POINT('Ctrl Pts',(-4.49938559786941,0.411206621885727,
33.0980781522693));
#41005=CARTESIAN_POINT('Ctrl Pts',(-4.43105241013465,1.15890217051366,33.0716208555848));
#41006=CARTESIAN_POINT('Ctrl Pts',(-4.17231550636761,1.88919639463604,33.0451635589004));
#41007=CARTESIAN_POINT('Ctrl Pts',(-3.75468875509488,2.51314026599421,33.0187062622159));
#41008=CARTESIAN_POINT('Ctrl Pts',(-3.33706200382211,3.13708413735244,32.9922489655315));
#41009=CARTESIAN_POINT('Ctrl Pts',(-2.76054540504362,3.65467765594643,32.965791668847));
#41010=CARTESIAN_POINT('Ctrl Pts',(-2.09535804244172,4.00287850404833,32.9393343721625));
#41011=CARTESIAN_POINT('Ctrl Pts',(-1.43017067983982,4.35107935215023,32.912877075478));
#41012=CARTESIAN_POINT('Ctrl Pts',(-0.676312553414512,4.52988752976003,
32.8864197787936));
#41013=CARTESIAN_POINT('Ctrl Pts',(0.0743972513539278,4.51752439873747,
32.8599624821091));
#41014=CARTESIAN_POINT('Ctrl Pts',(0.825107056122282,4.50516126771491,32.8335051854247));
#41015=CARTESIAN_POINT('Ctrl Pts',(1.57266853923377,4.30162682806002,32.8070478887402));
#41016=CARTESIAN_POINT('Ctrl Pts',(2.22602953939506,3.93171134926485,32.7805905920557));
#41017=CARTESIAN_POINT('Ctrl Pts',(2.87939053955642,3.56179587046963,32.7541332953712));
#41018=CARTESIAN_POINT('Ctrl Pts',(3.43855105676757,3.02549935253409,32.7276759986868));
#41019=CARTESIAN_POINT('Ctrl Pts',(3.83540595887257,2.38814211780667,32.7012187020023));
#41020=CARTESIAN_POINT('Ctrl Pts',(4.23226086097758,1.75078488307926,32.6747614053179));
#41021=CARTESIAN_POINT('Ctrl Pts',(4.46681014797645,1.01236693155997,32.6483041086334));
#41022=CARTESIAN_POINT('Ctrl Pts',(4.51048597629574,0.262826752513661,32.6218468119489));
#41023=CARTESIAN_POINT('Ctrl Pts',(4.51558339111607,0.175347765528612,32.6187589754633));
#41024=CARTESIAN_POINT('Ctrl Pts',(4.51808086670496,0.0877172796610649,
32.6156711389776));
#41025=CARTESIAN_POINT('Ctrl Pts',(4.51800690475437,8.25810157162321E-5,
32.6125833024919));
#41026=CARTESIAN_POINT('Origin',(0.,0.,20.5));
#41027=CARTESIAN_POINT('',(4.51762600826661,-0.000112987348963034,31.612583302492));
#41028=CARTESIAN_POINT('',(4.51779894817057,0.000115094980599771,31.887416697508));
#41029=CARTESIAN_POINT('',(4.51775,5.53264807684796E-16,20.5));
#41030=CARTESIAN_POINT('Ctrl Pts',(4.51779894817057,0.000115094980599771,
31.887416697508));
#41031=CARTESIAN_POINT('Ctrl Pts',(4.51796156278444,0.157653334629133,31.8929668698563));
#41032=CARTESIAN_POINT('Ctrl Pts',(4.50988180917274,0.315174976505045,31.8985170422046));
#41033=CARTESIAN_POINT('Ctrl Pts',(4.49343403803756,0.471817962781026,31.9040672145528));
#41034=CARTESIAN_POINT('Ctrl Pts',(4.41502862404034,1.21852449753214,31.9305245112373));
#41035=CARTESIAN_POINT('Ctrl Pts',(4.14647135042176,1.94526477434642,31.9569818079218));
#41036=CARTESIAN_POINT('Ctrl Pts',(3.72047219588784,2.56352263181406,31.9834391046062));
#41037=CARTESIAN_POINT('Ctrl Pts',(3.29447304135392,3.1817804892817,32.0098964012907));
#41038=CARTESIAN_POINT('Ctrl Pts',(2.71103200590467,3.69155592740269,32.0363536979752));
#41039=CARTESIAN_POINT('Ctrl Pts',(2.04121156194539,4.0307588619983,32.0628109946597));
#41040=CARTESIAN_POINT('Ctrl Pts',(1.37139111798607,4.36996179659393,32.0892682913441));
#41041=CARTESIAN_POINT('Ctrl Pts',(0.615191265516699,4.53859222766416,32.1157255880286));
#41042=CARTESIAN_POINT('Ctrl Pts',(-0.135283690341923,4.51611115533319,
32.1421828847131));
#41043=CARTESIAN_POINT('Ctrl Pts',(-0.885758646200546,4.49363008300222,
32.1686401813975));
#41044=CARTESIAN_POINT('Ctrl Pts',(-1.63050870544842,4.28003750727005,32.195097478082));
#41045=CARTESIAN_POINT('Ctrl Pts',(-2.27882413510731,3.9013487674713,32.2215547747665));
#41046=CARTESIAN_POINT('Ctrl Pts',(-2.92713956476612,3.52266002767259,32.2480120714509));
#41047=CARTESIAN_POINT('Ctrl Pts',(-3.47902036483595,2.97887512380733,32.2744693681354));
#41048=CARTESIAN_POINT('Ctrl Pts',(-3.86724806465204,2.33622645534256,32.3009266648198));
#41049=CARTESIAN_POINT('Ctrl Pts',(-4.25547576446814,1.69357778687776,32.3273839615043));
#41050=CARTESIAN_POINT('Ctrl Pts',(-4.48005036403047,0.952065353813438,
32.3538412581888));
#41051=CARTESIAN_POINT('Ctrl Pts',(-4.51361892565606,0.202004549841869,
32.3802985548733));
#41052=CARTESIAN_POINT('Ctrl Pts',(-4.54718748728165,-0.548056254129699,
32.4067558515577));
#41053=CARTESIAN_POINT('Ctrl Pts',(-4.38975001097049,-1.30666542900852,
32.4332131482422));
#41054=CARTESIAN_POINT('Ctrl Pts',(-4.06048220709632,-1.98142521687081,
32.4596704449267));
#41055=CARTESIAN_POINT('Ctrl Pts',(-3.73121440322213,-2.65618500473315,
32.4861277416111));
#41056=CARTESIAN_POINT('Ctrl Pts',(-3.23011627178491,-3.24709540557894,
32.5125850382956));
#41057=CARTESIAN_POINT('Ctrl Pts',(-2.61822101061276,-3.68218418656418,
32.5390423349801));
#41058=CARTESIAN_POINT('Ctrl Pts',(-2.00632574944065,-4.11727296754938,
32.5654996316645));
#41059=CARTESIAN_POINT('Ctrl Pts',(-1.28363335853361,-4.39654012867405,
32.591956928349));
#41060=CARTESIAN_POINT('Ctrl Pts',(-0.538166971277905,-4.48597123878686,
32.6184142250335));
#41061=CARTESIAN_POINT('Ctrl Pts',(0.207299415977802,-4.57540234889968,
32.6448715217179));
#41062=CARTESIAN_POINT('Ctrl Pts',(0.975539799582185,-4.47499740800066,
32.6713288184024));
#41063=CARTESIAN_POINT('Ctrl Pts',(1.67298335104786,-4.19698562677001,32.6977861150869));
#41064=CARTESIAN_POINT('Ctrl Pts',(2.37042690251357,-3.91897384553935,32.7242434117713));
#41065=CARTESIAN_POINT('Ctrl Pts',(2.99707362184056,-3.46335522397704,32.7507007084558));
#41066=CARTESIAN_POINT('Ctrl Pts',(3.47659863214429,-2.88562360594202,32.7771580051403));
#41067=CARTESIAN_POINT('Ctrl Pts',(3.95612364244802,-2.30789198790701,32.8036153018248));
#41068=CARTESIAN_POINT('Ctrl Pts',(4.28852694372849,-1.60804737339928,32.8300725985092));
#41069=CARTESIAN_POINT('Ctrl Pts',(4.43332218177084,-0.871330061926005,
32.8565298951937));
#41070=CARTESIAN_POINT('Ctrl Pts',(4.48966784634383,-0.584643655117203,
32.8668254959651));
#41071=CARTESIAN_POINT('Ctrl Pts',(4.51760398720758,-0.292373608988289,
32.8771210967366));
#41072=CARTESIAN_POINT('Ctrl Pts',(4.5174378855045,-7.22228901865168E-5,
32.887416697508));
#41073=CARTESIAN_POINT('Ctrl Pts',(4.51800690475437,8.25810157162321E-5,
32.6125833024919));
#41074=CARTESIAN_POINT('Ctrl Pts',(4.51744714361788,-0.663157072879468,
32.5892138422931));
#41075=CARTESIAN_POINT('Ctrl Pts',(4.36960026846028,-1.32663802677704,32.5658443820943));
#41076=CARTESIAN_POINT('Ctrl Pts',(4.08682159368458,-1.92651262793442,32.5424749218955));
#41077=CARTESIAN_POINT('Ctrl Pts',(3.76667901311444,-2.60564942276291,32.516017625211));
#41078=CARTESIAN_POINT('Ctrl Pts',(3.27359148233441,-3.20326060584664,32.4895603285266));
#41079=CARTESIAN_POINT('Ctrl Pts',(2.66761651687815,-3.64655779648099,32.4631030318421));
#41080=CARTESIAN_POINT('Ctrl Pts',(2.06164155142182,-4.08985498711538,32.4366457351576));
#41081=CARTESIAN_POINT('Ctrl Pts',(1.34277915128922,-4.37883818530036,32.4101884384731));
#41082=CARTESIAN_POINT('Ctrl Pts',(0.598585961229044,-4.47830955732371,
32.3837311417887));
#41083=CARTESIAN_POINT('Ctrl Pts',(-0.14560722883109,-4.57778092934705,
32.3572738451042));
#41084=CARTESIAN_POINT('Ctrl Pts',(-0.915131208818801,-4.4877404752088,
32.3308165484198));
#41085=CARTESIAN_POINT('Ctrl Pts',(-1.6162588096278,-4.2191550225724,32.3043592517353));
#41086=CARTESIAN_POINT('Ctrl Pts',(-2.31738641043684,-3.95056956993598,
32.2779019550508));
#41087=CARTESIAN_POINT('Ctrl Pts',(-2.95011763206717,-3.5034391188014,32.2514446583663));
#41088=CARTESIAN_POINT('Ctrl Pts',(-3.4373865119876,-2.93222366326361,32.2249873616819));
#41089=CARTESIAN_POINT('Ctrl Pts',(-3.924655391908,-2.36100820772586,32.1985300649974));
#41090=CARTESIAN_POINT('Ctrl Pts',(-4.26646193011853,-1.66570774778492,
32.172072768313));
#41091=CARTESIAN_POINT('Ctrl Pts',(-4.42117446855311,-0.931009109950869,
32.1456154716285));
#41092=CARTESIAN_POINT('Ctrl Pts',(-4.57588700698769,-0.196310472116814,
32.119158174944));
#41093=CARTESIAN_POINT('Ctrl Pts',(-4.54350554564632,0.577786343610359,
32.0927008782595));
#41094=CARTESIAN_POINT('Ctrl Pts',(-4.3279741106828,1.2969972017922,32.0662435815751));
#41095=CARTESIAN_POINT('Ctrl Pts',(-4.11244267571929,2.01620805997403,32.0397862848906));
#41096=CARTESIAN_POINT('Ctrl Pts',(-3.71376126713363,2.68053296061054,32.0133289882062));
#41097=CARTESIAN_POINT('Ctrl Pts',(-3.18048883925839,3.2090578660333,31.9868716915217));
#41098=CARTESIAN_POINT('Ctrl Pts',(-2.64721641138316,3.73758277145606,31.9604143948372));
#41099=CARTESIAN_POINT('Ctrl Pts',(-1.97935296421834,4.13030768166508,31.9339570981527));
#41100=CARTESIAN_POINT('Ctrl Pts',(-1.25824352648329,4.33939913723781,31.9074998014683));
#41101=CARTESIAN_POINT('Ctrl Pts',(-0.537134088748201,4.54849059281056,
31.8810425047838));
#41102=CARTESIAN_POINT('Ctrl Pts',(0.237221339557133,4.57394859374701,31.8545852080993));
#41103=CARTESIAN_POINT('Ctrl Pts',(0.970507124268449,4.41267238370826,31.8281279114149));
#41104=CARTESIAN_POINT('Ctrl Pts',(1.70379290897972,4.25139617366952,31.8016706147304));
#41105=CARTESIAN_POINT('Ctrl Pts',(2.39600905009698,3.90338575265561,31.7752133180459));
#41106=CARTESIAN_POINT('Ctrl Pts',(2.96284438772936,3.41102840479202,31.7487560213615));
#41107=CARTESIAN_POINT('Ctrl Pts',(3.52967972536174,2.91867105692843,31.722298724677));
#41108=CARTESIAN_POINT('Ctrl Pts',(3.97113425950925,2.28196678221515,31.6958414279925));
#41109=CARTESIAN_POINT('Ctrl Pts',(4.23343931648423,1.57846545665177,31.669384131308));
#41110=CARTESIAN_POINT('Ctrl Pts',(4.42115243039411,1.07501948430126,31.6504505217027));
#41111=CARTESIAN_POINT('Ctrl Pts',(4.5171186342718,0.537365078236716,31.6315169120973));
#41112=CARTESIAN_POINT('Ctrl Pts',(4.51762600826661,-0.000112987348963034,
31.612583302492));
#41113=CARTESIAN_POINT('Origin',(0.,0.,20.5));
#41114=CARTESIAN_POINT('',(4.5175628644093,0.000105298910395568,30.612583302492));
#41115=CARTESIAN_POINT('',(4.51784283093286,-0.000111697445491984,30.8874166975081));
#41116=CARTESIAN_POINT('',(4.51775,5.53264807684796E-16,20.5));
#41117=CARTESIAN_POINT('Ctrl Pts',(4.51784283093286,-0.000111697445491984,
30.8874166975081));
#41118=CARTESIAN_POINT('Ctrl Pts',(4.51722105684837,0.607182099716009,30.908812642976));
#41119=CARTESIAN_POINT('Ctrl Pts',(4.39393696701912,1.21472067967305,30.930208588444));
#41120=CARTESIAN_POINT('Ctrl Pts',(4.15564368858641,1.77318560159654,30.951604533912));
#41121=CARTESIAN_POINT('Ctrl Pts',(3.86098057239723,2.46375906325124,30.9780618305965));
#41122=CARTESIAN_POINT('Ctrl Pts',(3.3904601122214,3.07929536251675,31.0045191272809));
#41123=CARTESIAN_POINT('Ctrl Pts',(2.80139117936865,3.54482285937575,31.0309764239654));
#41124=CARTESIAN_POINT('Ctrl Pts',(2.21232224651588,4.01035035623478,31.0574337206499));
#41125=CARTESIAN_POINT('Ctrl Pts',(1.50470484098616,4.32586905068731,31.0838910173343));
#41126=CARTESIAN_POINT('Ctrl Pts',(0.764725979630773,4.45294911494339,31.1103483140188));
#41127=CARTESIAN_POINT('Ctrl Pts',(0.0247471182753856,4.58002917919947,
31.1368056107033));
#41128=CARTESIAN_POINT('Ctrl Pts',(-0.747593198905696,4.51867061325911,
31.1632629073878));
#41129=CARTESIAN_POINT('Ctrl Pts',(-1.45822477605293,4.27634682254641,31.1897202040722));
#41130=CARTESIAN_POINT('Ctrl Pts',(-2.16885635320013,4.03402303183372,31.2161775007567));
#41131=CARTESIAN_POINT('Ctrl Pts',(-2.81777919031341,3.61073401634878,31.2426347974411));
#41132=CARTESIAN_POINT('Ctrl Pts',(-3.32595520401574,3.05803590971036,31.2690920941256));
#41133=CARTESIAN_POINT('Ctrl Pts',(-3.83413121771806,2.50533780307193,31.2955493908101));
#41134=CARTESIAN_POINT('Ctrl Pts',(-4.20156040800938,1.82323060527995,31.3220066874946));
#41135=CARTESIAN_POINT('Ctrl Pts',(-4.38349030615745,1.09479421811638,31.348463984179));
#41136=CARTESIAN_POINT('Ctrl Pts',(-4.56542020430551,0.366357830952816,
31.3749212808635));
#41137=CARTESIAN_POINT('Ctrl Pts',(-4.56185081031042,-0.408407745582352,
31.4013785775479));
#41138=CARTESIAN_POINT('Ctrl Pts',(-4.3732168724104,-1.13513692172461,31.4278358742324));
#41139=CARTESIAN_POINT('Ctrl Pts',(-4.18458293451036,-1.86186609786691,
31.4542931709169));
#41140=CARTESIAN_POINT('Ctrl Pts',(-3.81088445270536,-2.54055887361621,
31.4807504676013));
#41141=CARTESIAN_POINT('Ctrl Pts',(-3.29763748849549,-3.08855122001668,
31.5072077642858));
#41142=CARTESIAN_POINT('Ctrl Pts',(-2.78439052428562,-3.63654356641715,
31.5336650609703));
#41143=CARTESIAN_POINT('Ctrl Pts',(-2.13159507767086,-4.05383548346882,
31.5601223576548));
#41144=CARTESIAN_POINT('Ctrl Pts',(-1.4187609115798,-4.28960127750478,31.5865796543392));
#41145=CARTESIAN_POINT('Ctrl Pts',(-0.705926745488817,-4.52536707154071,
31.6130369510237));
#41146=CARTESIAN_POINT('Ctrl Pts',(0.0669461400784679,-4.57960674256098,
31.6394942477081));
#41147=CARTESIAN_POINT('Ctrl Pts',(0.805722683022508,-4.44571395866405,
31.6659515443926));
#41148=CARTESIAN_POINT('Ctrl Pts',(1.54449922596663,-4.31182117476711,31.6924088410771));
#41149=CARTESIAN_POINT('Ctrl Pts',(2.24917942628753,-3.98979593595292,31.7188661377616));
#41150=CARTESIAN_POINT('Ctrl Pts',(2.83393401547767,-3.51886055991368,31.745323434446));
#41151=CARTESIAN_POINT('Ctrl Pts',(3.41868860466777,-3.04792518387447,31.7717807311305));
#41152=CARTESIAN_POINT('Ctrl Pts',(3.88351758272714,-2.42807967061021,31.798238027815));
#41153=CARTESIAN_POINT('Ctrl Pts',(4.1718052945689,-1.73482051763412,31.8246953244994));
#41154=CARTESIAN_POINT('Ctrl Pts',(4.39961643899369,-1.18699223867807,31.8456024488356));
#41155=CARTESIAN_POINT('Ctrl Pts',(4.51718638990429,-0.593320812476893,
31.8665095731718));
#41156=CARTESIAN_POINT('Ctrl Pts',(4.51779894817057,0.000115094980599771,
31.887416697508));
#41157=CARTESIAN_POINT('Ctrl Pts',(4.51762600826661,-0.000112987348963034,
31.612583302492));
#41158=CARTESIAN_POINT('Ctrl Pts',(4.51782762450612,-0.213691742886314,
31.6050596154129));
#41159=CARTESIAN_POINT('Ctrl Pts',(4.50295585827573,-0.42724265346175,31.5975359283338));
#41160=CARTESIAN_POINT('Ctrl Pts',(4.47277779830256,-0.638608182854815,
31.5900122412547));
#41161=CARTESIAN_POINT('Ctrl Pts',(4.36665564334343,-1.38188212038452,31.5635549445702));
#41162=CARTESIAN_POINT('Ctrl Pts',(4.07125575362272,-2.09813161903045,31.5370976478857));
#41163=CARTESIAN_POINT('Ctrl Pts',(3.62255750878013,-2.70011828255321,31.5106403512012));
#41164=CARTESIAN_POINT('Ctrl Pts',(3.17385926393751,-3.302104946076,31.4841830545168));
#41165=CARTESIAN_POINT('Ctrl Pts',(2.57186266397298,-3.78982877447561,31.4577257578323));
#41166=CARTESIAN_POINT('Ctrl Pts',(1.88989022851381,-4.10388554523215,31.4312684611479));
#41167=CARTESIAN_POINT('Ctrl Pts',(1.20791779305463,-4.4179423159887,31.4048111644634));
#41168=CARTESIAN_POINT('Ctrl Pts',(0.44596952210079,-4.55833202910217,31.3783538677789));
#41169=CARTESIAN_POINT('Ctrl Pts',(-0.303150128217454,-4.50795537288904,
31.3518965710945));
#41170=CARTESIAN_POINT('Ctrl Pts',(-1.05226977853561,-4.45757871667591,
31.32543927441));
#41171=CARTESIAN_POINT('Ctrl Pts',(-1.7885608082182,-4.2164356911362,31.2989819777255));
#41172=CARTESIAN_POINT('Ctrl Pts',(-2.42234378472615,-3.81389724990016,
31.272524681041));
#41173=CARTESIAN_POINT('Ctrl Pts',(-3.05612676123416,-3.41135880866406,
31.2460673843566));
#41174=CARTESIAN_POINT('Ctrl Pts',(-3.58740168456753,-2.84742495173157,
31.2196100876721));
#41175=CARTESIAN_POINT('Ctrl Pts',(-3.95145985704278,-2.19078219875388,
31.1931527909876));
#41176=CARTESIAN_POINT('Ctrl Pts',(-4.31551802951802,-1.53413944577618,
31.1666954943032));
#41177=CARTESIAN_POINT('Ctrl Pts',(-4.51235945113515,-0.784787796753247,
31.1402381976187));
#41178=CARTESIAN_POINT('Ctrl Pts',(-4.51800905459174,-0.0339974532052471,
31.1137809009342));
#41179=CARTESIAN_POINT('Ctrl Pts',(-4.52365865804833,0.716792890342667,
31.0873236042498));
#41180=CARTESIAN_POINT('Ctrl Pts',(-4.33811644334446,1.46902192841556,31.0608663075653));
#41181=CARTESIAN_POINT('Ctrl Pts',(-3.98398124688566,2.13106899669175,31.0344090108808));
#41182=CARTESIAN_POINT('Ctrl Pts',(-3.62984605042683,2.79311606496798,31.0079517141964));
#41183=CARTESIAN_POINT('Ctrl Pts',(-3.10711787221305,3.36498116344739,30.9814944175119));
#41184=CARTESIAN_POINT('Ctrl Pts',(-2.47946442583117,3.77701175603613,30.9550371208274));
#41185=CARTESIAN_POINT('Ctrl Pts',(-1.85181097944929,4.18904234862487,30.928579824143));
#41186=CARTESIAN_POINT('Ctrl Pts',(-1.11923226489916,4.44123843532298,30.9021225274585));
#41187=CARTESIAN_POINT('Ctrl Pts',(-0.370955558845505,4.50288281188385,
30.875665230774));
#41188=CARTESIAN_POINT('Ctrl Pts',(0.377321147208236,4.56452718844472,30.8492079340895));
#41189=CARTESIAN_POINT('Ctrl Pts',(1.14129584476551,4.43561985486838,30.8227506374051));
#41190=CARTESIAN_POINT('Ctrl Pts',(1.82791726117872,4.13186158171862,30.7962933407206));
#41191=CARTESIAN_POINT('Ctrl Pts',(2.51453867759182,3.82810330856891,30.7698360440361));
#41192=CARTESIAN_POINT('Ctrl Pts',(3.12380681286076,3.34949409584584,30.7433787473517));
#41193=CARTESIAN_POINT('Ctrl Pts',(3.58151348240585,2.75432801596732,30.7169214506672));
#41194=CARTESIAN_POINT('Ctrl Pts',(4.039220151951,2.15916193608874,30.6904641539828));
#41195=CARTESIAN_POINT('Ctrl Pts',(4.34536535577227,1.44743898905468,30.6640068572983));
#41196=CARTESIAN_POINT('Ctrl Pts',(4.4626609468647,0.705846242127884,30.6375495606138));
#41197=CARTESIAN_POINT('Ctrl Pts',(4.49955602397321,0.47257983095123,30.6292274745732));
#41198=CARTESIAN_POINT('Ctrl Pts',(4.5177662531821,0.236358091141789,30.6209053885326));
#41199=CARTESIAN_POINT('Ctrl Pts',(4.5175628644093,0.000105298910395568,
30.612583302492));
#41200=CARTESIAN_POINT('Origin',(0.,0.,20.5));
#41201=CARTESIAN_POINT('',(4.51806064718817,-6.4525231641549E-5,29.612583302492));
#41202=CARTESIAN_POINT('',(4.51741540695923,6.15435095971417E-5,29.887416697508));
#41203=CARTESIAN_POINT('',(4.51775,5.53264807684796E-16,20.5));
#41204=CARTESIAN_POINT('Ctrl Pts',(4.51741540695923,6.15435095971417E-5,
29.887416697508));
#41205=CARTESIAN_POINT('Ctrl Pts',(4.51756272899121,0.306245363704865,29.8982011194113));
#41206=CARTESIAN_POINT('Ctrl Pts',(4.48689091473443,0.612400072796405,29.9089855413145));
#41207=CARTESIAN_POINT('Ctrl Pts',(4.42510561599225,0.912141398858333,29.9197699632178));
#41208=CARTESIAN_POINT('Ctrl Pts',(4.27352846199847,1.64749330398352,29.9462272599022));
#41209=CARTESIAN_POINT('Ctrl Pts',(3.93469095105298,2.34424546963053,29.9726845565867));
#41210=CARTESIAN_POINT('Ctrl Pts',(3.44986311698689,2.91753425314097,29.9991418532711));
#41211=CARTESIAN_POINT('Ctrl Pts',(2.96503528292081,3.49082303665141,30.0255991499556));
#41212=CARTESIAN_POINT('Ctrl Pts',(2.33421712573414,3.94064843802526,30.0520564466401));
#41213=CARTESIAN_POINT('Ctrl Pts',(1.63424159882604,4.21222222121102,30.0785137433246));
#41214=CARTESIAN_POINT('Ctrl Pts',(0.934266071917943,4.48379600439678,30.104971040009));
#41215=CARTESIAN_POINT('Ctrl Pts',(0.165133175288441,4.57711816939443,30.1314283366935));
#41216=CARTESIAN_POINT('Ctrl Pts',(-0.579477555476409,4.48082217978983,
30.157885633378));
#41217=CARTESIAN_POINT('Ctrl Pts',(-1.32408828624126,4.38452619018523,30.1843429300624));
#41218=CARTESIAN_POINT('Ctrl Pts',(-2.04417685114143,4.09861204597837,30.2108002267469));
#41219=CARTESIAN_POINT('Ctrl Pts',(-2.65203725991661,3.65790377350353,30.2372575234314));
#41220=CARTESIAN_POINT('Ctrl Pts',(-3.2598976686918,3.21719550102869,30.2637148201158));
#41221=CARTESIAN_POINT('Ctrl Pts',(-3.75552992134198,2.62169310028588,30.2901721168003));
#41222=CARTESIAN_POINT('Ctrl Pts',(-4.07856655802606,1.94392810462446,30.3166294134847));
#41223=CARTESIAN_POINT('Ctrl Pts',(-4.40160319471017,1.26616310896299,30.3430867101692));
#41224=CARTESIAN_POINT('Ctrl Pts',(-4.55204421542814,0.506135518382923,
30.3695440068537));
#41225=CARTESIAN_POINT('Ctrl Pts',(-4.51156607035432,-0.243584147729374,
30.3960013035382));
#41226=CARTESIAN_POINT('Ctrl Pts',(-4.47108792528051,-0.993303813841587,
30.4224586002227));
#41227=CARTESIAN_POINT('Ctrl Pts',(-4.2396906144149,-1.73271555548614,30.4489158969071));
#41228=CARTESIAN_POINT('Ctrl Pts',(-3.84555807412635,-2.37175984086058,
30.4753731935916));
#41229=CARTESIAN_POINT('Ctrl Pts',(-3.45142553383776,-3.01080412623509,
30.501830490276));
#41230=CARTESIAN_POINT('Ctrl Pts',(-2.89455776412619,-3.54948095533957,
30.5282877869605));
#41231=CARTESIAN_POINT('Ctrl Pts',(-2.24278064303953,-3.92218008655959,
30.554745083645));
#41232=CARTESIAN_POINT('Ctrl Pts',(-1.59100352195292,-4.29487921777957,
30.5812023803295));
#41233=CARTESIAN_POINT('Ctrl Pts',(-0.844317049491253,-4.5016006511151,
30.6076596770139));
#41234=CARTESIAN_POINT('Ctrl Pts',(-0.0936668116191134,-4.51716594477096,
30.6341169736984));
#41235=CARTESIAN_POINT('Ctrl Pts',(0.656983426253069,-4.53273123842682,
30.6605742703828));
#41236=CARTESIAN_POINT('Ctrl Pts',(1.4115974295357,-4.35714039240299,30.6870315670673));
#41237=CARTESIAN_POINT('Ctrl Pts',(2.07826404778386,-4.01178017741331,30.7134888637518));
#41238=CARTESIAN_POINT('Ctrl Pts',(2.74493066603195,-3.66641996242367,30.7399461604362));
#41239=CARTESIAN_POINT('Ctrl Pts',(3.32364989924556,-3.15129037846822,30.7664034571207));
#41240=CARTESIAN_POINT('Ctrl Pts',(3.74393438530595,-2.52913363876272,30.7928607538052));
#41241=CARTESIAN_POINT('Ctrl Pts',(4.16421887136636,-1.90697689905718,30.8193180504897));
#41242=CARTESIAN_POINT('Ctrl Pts',(4.42606861027353,-1.17779300360159,30.8457753471741));
#41243=CARTESIAN_POINT('Ctrl Pts',(4.49759059362584,-0.430395743851834,
30.8722326438586));
#41244=CARTESIAN_POINT('Ctrl Pts',(4.51127293924728,-0.287416660427361,
30.8772939950751));
#41245=CARTESIAN_POINT('Ctrl Pts',(4.51798991567019,-0.143771027837287,
30.8823553462916));
#41246=CARTESIAN_POINT('Ctrl Pts',(4.51784283093286,-0.000111697445491984,
30.8874166975081));
#41247=CARTESIAN_POINT('Ctrl Pts',(4.5175628644093,0.000105298910395568,
30.612583302492));
#41248=CARTESIAN_POINT('Ctrl Pts',(4.51711964642055,-0.514728858223211,
30.5944480918481));
#41249=CARTESIAN_POINT('Ctrl Pts',(4.42923445822943,-1.02971047605454,30.5763128812042));
#41250=CARTESIAN_POINT('Ctrl Pts',(4.25671408259971,-1.51457811392965,30.5581776705604));
#41251=CARTESIAN_POINT('Ctrl Pts',(4.00502564887872,-2.22194717624094,30.5317203738759));
#41252=CARTESIAN_POINT('Ctrl Pts',(3.57320280307314,-2.86522275404404,30.5052630771915));
#41253=CARTESIAN_POINT('Ctrl Pts',(3.01384108989026,-3.36605459389572,30.478805780507));
#41254=CARTESIAN_POINT('Ctrl Pts',(2.45447937670739,-3.86688643374739,30.4523484838226));
#41255=CARTESIAN_POINT('Ctrl Pts',(1.7675787961471,-4.22527453564767,30.425891187138));
#41256=CARTESIAN_POINT('Ctrl Pts',(1.03680307870754,-4.3975676254243,30.3994338904536));
#41257=CARTESIAN_POINT('Ctrl Pts',(0.306027361267937,-4.56986071520095,
30.3729765937691));
#41258=CARTESIAN_POINT('Ctrl Pts',(-0.468623493050924,-4.55605879285401,
30.3465192970847));
#41259=CARTESIAN_POINT('Ctrl Pts',(-1.19279786752355,-4.35784291725031,
30.3200620004002));
#41260=CARTESIAN_POINT('Ctrl Pts',(-1.91697224199613,-4.15962704164662,
30.2936047037158));
#41261=CARTESIAN_POINT('Ctrl Pts',(-2.59067013662245,-3.77699721278612,
30.2671474070313));
#41262=CARTESIAN_POINT('Ctrl Pts',(-3.1318358934393,-3.25655732035575,30.2406901103468));
#41263=CARTESIAN_POINT('Ctrl Pts',(-3.67300165025612,-2.73611742792542,
30.2142328136623));
#41264=CARTESIAN_POINT('Ctrl Pts',(-4.08163526926355,-2.0778674719253,30.1877755169779));
#41265=CARTESIAN_POINT('Ctrl Pts',(-4.30796562791422,-1.3619815684902,30.1613182202934));
#41266=CARTESIAN_POINT('Ctrl Pts',(-4.5342959865649,-0.64609566505506,30.1348609236089));
#41267=CARTESIAN_POINT('Ctrl Pts',(-4.5783230848587,0.127426185815075,30.1084036269244));
#41268=CARTESIAN_POINT('Ctrl Pts',(-4.4346844709496,0.864369878764792,30.08194633024));
#41269=CARTESIAN_POINT('Ctrl Pts',(-4.29104585704049,1.60131357171455,30.0554890335555));
#41270=CARTESIAN_POINT('Ctrl Pts',(-3.95974153092847,2.30167910674398,30.029031736871));
#41271=CARTESIAN_POINT('Ctrl Pts',(-3.48112399286914,2.88016273680294,30.0025744401866));
#41272=CARTESIAN_POINT('Ctrl Pts',(-3.00250645480984,3.45864636686186,29.9761171435021));
#41273=CARTESIAN_POINT('Ctrl Pts',(-2.37657570480325,3.91524809195029,29.9496598468177));
#41274=CARTESIAN_POINT('Ctrl Pts',(-1.67956941546306,4.19435432728787,29.9232025501332));
#41275=CARTESIAN_POINT('Ctrl Pts',(-0.982563126122875,4.47346056262544,
29.8967452534487));
#41276=CARTESIAN_POINT('Ctrl Pts',(-0.214481297449103,4.57507130821215,
29.8702879567642));
#41277=CARTESIAN_POINT('Ctrl Pts',(0.53112455388596,4.48681048769132,29.8438306600798));
#41278=CARTESIAN_POINT('Ctrl Pts',(1.27673040522102,4.39854966717049,29.8173733633953));
#41279=CARTESIAN_POINT('Ctrl Pts',(1.99986027921735,4.12041728054213,29.7909160667108));
#41280=CARTESIAN_POINT('Ctrl Pts',(2.61243775753263,3.68628954467976,29.7644587700264));
#41281=CARTESIAN_POINT('Ctrl Pts',(3.22501523584791,3.25216180881739,29.7380014733419));
#41282=CARTESIAN_POINT('Ctrl Pts',(3.72704031848211,2.66203872372102,29.7115441766574));
#41283=CARTESIAN_POINT('Ctrl Pts',(4.05736690597726,1.98779662804773,29.685086879973));
#41284=CARTESIAN_POINT('Ctrl Pts',(4.35910923962182,1.37189893439675,29.6609190208126));
#41285=CARTESIAN_POINT('Ctrl Pts',(4.51758267646005,0.685810539097339,29.6367511616523));
#41286=CARTESIAN_POINT('Ctrl Pts',(4.51806064718817,-6.4525231641549E-5,
29.612583302492));
#41287=CARTESIAN_POINT('Origin',(0.,0.,20.5));
#41288=CARTESIAN_POINT('',(4.51736349586412,-8.67285085925565E-6,28.612583302492));
#41289=CARTESIAN_POINT('',(4.51813672578305,5.21363961469835E-6,28.8874166975081));
#41290=CARTESIAN_POINT('',(4.51775,5.53264807684796E-16,20.5));
#41291=CARTESIAN_POINT('Ctrl Pts',(4.51813645424719,5.20997890686523E-6,
28.8874166975081));
#41292=CARTESIAN_POINT('Ctrl Pts',(4.51813678764949,0.00491176269805106,
28.8875895958466));
#41293=CARTESIAN_POINT('Ctrl Pts',(4.51812896220818,0.00981831434884656,
28.887762494185));
#41294=CARTESIAN_POINT('Ctrl Pts',(4.51811297150728,0.0147248393885022,
28.8879353925235));
#41295=CARTESIAN_POINT('Ctrl Pts',(4.51566603811481,0.7655324515643,28.914392689208));
#41296=CARTESIAN_POINT('Ctrl Pts',(4.32202288903541,1.51571694218793,28.9408499858924));
#41297=CARTESIAN_POINT('Ctrl Pts',(3.96076904551605,2.17390667055403,28.9673072825769));
#41298=CARTESIAN_POINT('Ctrl Pts',(3.59951520199672,2.83209639892005,28.9937645792614));
#41299=CARTESIAN_POINT('Ctrl Pts',(3.07065066403746,3.39829136502856,29.0202218759458));
#41300=CARTESIAN_POINT('Ctrl Pts',(2.43859054705081,3.8035296486332,29.0466791726303));
#41301=CARTESIAN_POINT('Ctrl Pts',(1.80653043006408,4.20876793223789,29.0731364693148));
#41302=CARTESIAN_POINT('Ctrl Pts',(1.07127473404993,4.45304953333867,29.0995937659992));
#41303=CARTESIAN_POINT('Ctrl Pts',(0.32237678905244,4.50662122327555,29.1260510626837));
#41304=CARTESIAN_POINT('Ctrl Pts',(-0.426521155945046,4.56019291321243,
29.1525083593682));
#41305=CARTESIAN_POINT('Ctrl Pts',(-1.18906134992587,4.42305469198539,29.1789656560527));
#41306=CARTESIAN_POINT('Ctrl Pts',(-1.87236724119019,4.11190984316476,29.2054229527371));
#41307=CARTESIAN_POINT('Ctrl Pts',(-2.55567313245444,3.80076499434415,29.2318802494216));
#41308=CARTESIAN_POINT('Ctrl Pts',(-3.15974472100221,3.31561351792999,29.258337546106));
#41309=CARTESIAN_POINT('Ctrl Pts',(-3.61100675589329,2.7155463268172,29.2847948427905));
#41310=CARTESIAN_POINT('Ctrl Pts',(-4.06226879078437,2.11547913570442,29.311252139475));
#41311=CARTESIAN_POINT('Ctrl Pts',(-4.36072127201875,1.40049622989302,29.3377094361595));
#41312=CARTESIAN_POINT('Ctrl Pts',(-4.47001301768878,0.657681736016911,
29.3641667328439));
#41313=CARTESIAN_POINT('Ctrl Pts',(-4.57930476335883,-0.0851327578592831,
29.3906240295284));
#41314=CARTESIAN_POINT('Ctrl Pts',(-4.49943577346447,-0.855778839800193,
29.4170813262128));
#41315=CARTESIAN_POINT('Ctrl Pts',(-4.24013400258134,-1.56039266992349,
29.4435386228973));
#41316=CARTESIAN_POINT('Ctrl Pts',(-3.98083223169821,-2.26500650004679,
29.4699959195818));
#41317=CARTESIAN_POINT('Ctrl Pts',(-3.54209767982631,-2.90358807835248,
29.4964532162663));
#41318=CARTESIAN_POINT('Ctrl Pts',(-2.97736772982241,-3.39835887534109,
29.5229105129507));
#41319=CARTESIAN_POINT('Ctrl Pts',(-2.41263777981851,-3.8931296723297,29.5493678096352));
#41320=CARTESIAN_POINT('Ctrl Pts',(-1.72191243168261,-4.24408968800123,
29.5758251063197));
#41321=CARTESIAN_POINT('Ctrl Pts',(-0.989321268370363,-4.40849238086531,
29.6022824030041));
#41322=CARTESIAN_POINT('Ctrl Pts',(-0.256730105058199,-4.57289507372936,
29.6287396996886));
#41323=CARTESIAN_POINT('Ctrl Pts',(0.517726873430306,-4.55074044378599,
29.655196996373));
#41324=CARTESIAN_POINT('Ctrl Pts',(1.23972166423099,-4.34472690044308,29.6816542930575));
#41325=CARTESIAN_POINT('Ctrl Pts',(1.96171645503171,-4.13871335710016,29.708111589742));
#41326=CARTESIAN_POINT('Ctrl Pts',(2.63124905814461,-3.74884090035768,29.7345688864265));
#41327=CARTESIAN_POINT('Ctrl Pts',(3.16677114350317,-3.22259556396285,29.761026183111));
#41328=CARTESIAN_POINT('Ctrl Pts',(3.70229322886173,-2.69635022756802,29.7874834797954));
#41329=CARTESIAN_POINT('Ctrl Pts',(4.10380479646594,-2.03373201152084,29.8139407764799));
#41330=CARTESIAN_POINT('Ctrl Pts',(4.32240218174702,-1.31544708119558,29.8403980731643));
#41331=CARTESIAN_POINT('Ctrl Pts',(4.45189573839702,-0.889946702056473,
29.8560709479456));
#41332=CARTESIAN_POINT('Ctrl Pts',(4.51720130556553,-0.444911837263118,
29.8717438227268));
#41333=CARTESIAN_POINT('Ctrl Pts',(4.51741540695923,6.15435095971417E-5,
29.887416697508));
#41334=CARTESIAN_POINT('Ctrl Pts',(4.51806064718817,-6.4525231641549E-5,
29.612583302492));
#41335=CARTESIAN_POINT('Ctrl Pts',(4.51810592567614,-0.065037930559881,
29.6102938649678));
#41336=CARTESIAN_POINT('Ctrl Pts',(4.51673336863491,-0.130009421477303,
29.6080044274437));
#41337=CARTESIAN_POINT('Ctrl Pts',(4.51393045695516,-0.194919147263631,
29.6057149899196));
#41338=CARTESIAN_POINT('Ctrl Pts',(4.48153932808183,-0.945031720651385,
29.5792576932351));
#41339=CARTESIAN_POINT('Ctrl Pts',(4.25812897797913,-1.68689576117669,29.5528003965506));
#41340=CARTESIAN_POINT('Ctrl Pts',(3.87091054003435,-2.33015304974767,29.5263430998662));
#41341=CARTESIAN_POINT('Ctrl Pts',(3.48369210208957,-2.97341033831866,29.4998858031817));
#41342=CARTESIAN_POINT('Ctrl Pts',(2.9326655763027,-3.51806087493531,29.4734285064972));
#41343=CARTESIAN_POINT('Ctrl Pts',(2.28494538367634,-3.89776682701949,29.4469712098128));
#41344=CARTESIAN_POINT('Ctrl Pts',(1.63722519105001,-4.27747277910364,29.4205139131283));
#41345=CARTESIAN_POINT('Ctrl Pts',(0.892811331584192,-4.49223414665534,
29.3940566164438));
#41346=CARTESIAN_POINT('Ctrl Pts',(0.142372589495739,-4.5158932327899,29.3675993197594));
#41347=CARTESIAN_POINT('Ctrl Pts',(-0.608066152592799,-4.53955231892447,
29.3411420230749));
#41348=CARTESIAN_POINT('Ctrl Pts',(-1.36452977730397,-4.37210912364185,
29.3146847263904));
#41349=CARTESIAN_POINT('Ctrl Pts',(-2.03488185234987,-4.03395804281286,
29.288227429706));
#41350=CARTESIAN_POINT('Ctrl Pts',(-2.70523392739576,-3.69580696198387,
29.2617701330215));
#41351=CARTESIAN_POINT('Ctrl Pts',(-3.28947445277638,-3.18694799560851,
29.235312836337));
#41352=CARTESIAN_POINT('Ctrl Pts',(-3.71644357909758,-2.56935960262119,
29.2088555396525));
#41353=CARTESIAN_POINT('Ctrl Pts',(-4.14341270541876,-1.95177120963391,
29.1823982429681));
#41354=CARTESIAN_POINT('Ctrl Pts',(-4.41311043268056,-1.22545339003468,
29.1559409462836));
#41355=CARTESIAN_POINT('Ctrl Pts',(-4.49268787618537,-0.478870850412086,
29.1294836495992));
#41356=CARTESIAN_POINT('Ctrl Pts',(-4.57226531969018,0.267711689210511,
29.1030263529147));
#41357=CARTESIAN_POINT('Ctrl Pts',(-4.46172247943801,1.03455894885648,29.0765690562302));
#41358=CARTESIAN_POINT('Ctrl Pts',(-4.17452335103036,1.72826978099475,29.0501117595457));
#41359=CARTESIAN_POINT('Ctrl Pts',(-3.88732422262269,2.42198061313306,29.0236544628612));
#41360=CARTESIAN_POINT('Ctrl Pts',(-3.42346880605953,3.04255501776367,28.9971971661768));
#41361=CARTESIAN_POINT('Ctrl Pts',(-2.83945417771499,3.51440771921163,28.9707398694923));
#41362=CARTESIAN_POINT('Ctrl Pts',(-2.25543954937045,3.98626042065959,28.9442825728079));
#41363=CARTESIAN_POINT('Ctrl Pts',(-1.55126570924453,4.3093914189249,28.9178252761234));
#41364=CARTESIAN_POINT('Ctrl Pts',(-0.812700251733401,4.44444371603802,
28.8913679794389));
#41365=CARTESIAN_POINT('Ctrl Pts',(-0.0741347942223568,4.57949601315112,
28.8649106827545));
#41366=CARTESIAN_POINT('Ctrl Pts',(0.698822280673891,4.52646960911207,28.83845338607));
#41367=CARTESIAN_POINT('Ctrl Pts',(1.41202565668872,4.29182306124684,28.8119960893855));
#41368=CARTESIAN_POINT('Ctrl Pts',(2.12522903270359,4.05717651338159,28.785538792701));
#41369=CARTESIAN_POINT('Ctrl Pts',(2.77867870983704,3.64090982169015,28.7590814960166));
#41370=CARTESIAN_POINT('Ctrl Pts',(3.29278524060738,3.09372380852518,28.7326241993321));
#41371=CARTESIAN_POINT('Ctrl Pts',(3.80689177137772,2.54653779536021,28.7061669026477));
#41372=CARTESIAN_POINT('Ctrl Pts',(4.18165515578495,1.86843246072172,28.6797096059632));
#41373=CARTESIAN_POINT('Ctrl Pts',(4.37142962837061,1.14200028388831,28.6532523092787));
#41374=CARTESIAN_POINT('Ctrl Pts',(4.46866731930057,0.769786958618117,28.6396959736831));
#41375=CARTESIAN_POINT('Ctrl Pts',(4.517338221792,0.384885956569512,28.6261396380875));
#41376=CARTESIAN_POINT('Ctrl Pts',(4.51736392670147,-8.66318320566495E-6,
28.612583302492));
#41377=CARTESIAN_POINT('Origin',(0.,0.,20.5));
#41378=CARTESIAN_POINT('',(4.51801726226543,7.95831363512023E-5,27.612583302492));
#41379=CARTESIAN_POINT('',(4.51743092439869,-6.91819792334251E-5,27.8874166975081));
#41380=CARTESIAN_POINT('',(4.51775,5.53264807684796E-16,20.5));
#41381=CARTESIAN_POINT('Ctrl Pts',(4.51743092439869,-6.91819792334251E-5,
27.8874166975081));
#41382=CARTESIAN_POINT('Ctrl Pts',(4.51718386244179,0.454717345983238,27.9034353689663));
#41383=CARTESIAN_POINT('Ctrl Pts',(4.44891863177309,0.909576397762494,27.9194540404245));
#41384=CARTESIAN_POINT('Ctrl Pts',(4.31373618863887,1.34359284719174,27.9354727118827));
#41385=CARTESIAN_POINT('Ctrl Pts',(4.09046161721975,2.06043768656892,27.9619300085671));
#41386=CARTESIAN_POINT('Ctrl Pts',(3.68463958850139,2.72042474717273,27.9883873052516));
#41387=CARTESIAN_POINT('Ctrl Pts',(3.14569877644576,3.24316833544992,28.0148446019361));
#41388=CARTESIAN_POINT('Ctrl Pts',(2.60675796439011,3.76591192372714,28.0413018986205));
#41389=CARTESIAN_POINT('Ctrl Pts',(1.93469836899718,4.15141203967772,28.067759195305));
#41390=CARTESIAN_POINT('Ctrl Pts',(1.21137610519651,4.3527151958239,28.0942164919895));
#41391=CARTESIAN_POINT('Ctrl Pts',(0.48805384139591,4.55401835197006,28.1206737886739));
#41392=CARTESIAN_POINT('Ctrl Pts',(-0.286531090812426,4.57112454831186,
28.1471310853584));
#41393=CARTESIAN_POINT('Ctrl Pts',(-1.01803510394287,4.40195026906682,28.1735883820429));
#41394=CARTESIAN_POINT('Ctrl Pts',(-1.7495391170734,4.23277598982176,28.2000456787273));
#41395=CARTESIAN_POINT('Ctrl Pts',(-2.43796221112602,3.87732123498983,28.2265029754118));
#41396=CARTESIAN_POINT('Ctrl Pts',(-2.99945521514446,3.37888000031668,28.2529602720963));
#41397=CARTESIAN_POINT('Ctrl Pts',(-3.56094821916288,2.88043876564355,28.2794175687807));
#41398=CARTESIAN_POINT('Ctrl Pts',(-3.99551113314713,2.23901105112923,28.3058748654652));
#41399=CARTESIAN_POINT('Ctrl Pts',(-4.25021467511827,1.53272204251347,28.3323321621497));
#41400=CARTESIAN_POINT('Ctrl Pts',(-4.50491821708942,0.826433033897707,
28.3587894588341));
#41401=CARTESIAN_POINT('Ctrl Pts',(-4.57976238704747,0.0552827311804979,
28.3852467555186));
#41402=CARTESIAN_POINT('Ctrl Pts',(-4.4656312479239,-0.686803612223317,
28.4117040522031));
#41403=CARTESIAN_POINT('Ctrl Pts',(-4.35150010880033,-1.42888995562718,
28.4381613488875));
#41404=CARTESIAN_POINT('Ctrl Pts',(-4.04839366059513,-2.14191233971764,
28.464618645572));
#41405=CARTESIAN_POINT('Ctrl Pts',(-3.59322993324233,-2.73902542723662,
28.4910759422565));
#41406=CARTESIAN_POINT('Ctrl Pts',(-3.13806620588952,-3.3361385147556,28.517533238941));
#41407=CARTESIAN_POINT('Ctrl Pts',(-2.5308451993891,-3.8173423057031,28.5439905356254));
#41408=CARTESIAN_POINT('Ctrl Pts',(-1.84552576030239,-4.12402671090497,
28.5704478323099));
#41409=CARTESIAN_POINT('Ctrl Pts',(-1.16020632121576,-4.4307111161068,28.5969051289944));
#41410=CARTESIAN_POINT('Ctrl Pts',(-0.396788449542842,-4.56287613556305,
28.6233624256788));
#41411=CARTESIAN_POINT('Ctrl Pts',(0.351744402845005,-4.50442421617509,
28.6498197223633));
#41412=CARTESIAN_POINT('Ctrl Pts',(1.10027725523294,-4.44597229678712,28.6762770190477));
#41413=CARTESIAN_POINT('Ctrl Pts',(1.8339250883358,-4.19690343855492,28.7027343157322));
#41414=CARTESIAN_POINT('Ctrl Pts',(2.46333040803262,-3.78755395275886,28.7291916124167));
#41415=CARTESIAN_POINT('Ctrl Pts',(3.09273572772936,-3.37820446696285,28.7556489091012));
#41416=CARTESIAN_POINT('Ctrl Pts',(3.61789853402009,-2.80857435360303,28.7821062057856));
#41417=CARTESIAN_POINT('Ctrl Pts',(3.97485457831268,-2.14804393005918,28.8085635024701));
#41418=CARTESIAN_POINT('Ctrl Pts',(4.32947791614233,-1.49183007045257,28.8348479008161));
#41419=CARTESIAN_POINT('Ctrl Pts',(4.51808576967277,-0.745900085055985,
28.8611322991621));
#41420=CARTESIAN_POINT('Ctrl Pts',(4.51813645424719,5.20997890686523E-6,
28.8874166975081));
#41421=CARTESIAN_POINT('Ctrl Pts',(4.51736392670147,-8.66318320566495E-6,
28.612583302492));
#41422=CARTESIAN_POINT('Ctrl Pts',(4.5173883889195,-0.366295738162854,28.5996823414031));
#41423=CARTESIAN_POINT('Ctrl Pts',(4.47335741760473,-0.732577033027994,
28.5867813803142));
#41424=CARTESIAN_POINT('Ctrl Pts',(4.38520343465814,-1.08791198212899,28.5738804192253));
#41425=CARTESIAN_POINT('Ctrl Pts',(4.20441720759592,-1.81663305228457,28.5474231225409));
#41426=CARTESIAN_POINT('Ctrl Pts',(3.8380591927074,-2.49931617356742,28.5209658258564));
#41427=CARTESIAN_POINT('Ctrl Pts',(3.33075139074614,-3.05281129735201,28.4945085291719));
#41428=CARTESIAN_POINT('Ctrl Pts',(2.82344358878484,-3.60630642113663,28.4680512324875));
#41429=CARTESIAN_POINT('Ctrl Pts',(2.17518599975079,-4.03061354742298,28.441593935803));
#41430=CARTESIAN_POINT('Ctrl Pts',(1.46493568054142,-4.27405253782332,28.4151366391185));
#41431=CARTESIAN_POINT('Ctrl Pts',(0.754685361332094,-4.51749152822365,
28.388679342434));
#41432=CARTESIAN_POINT('Ctrl Pts',(-0.0175576880525484,-4.580062382738,
28.3622220457496));
#41433=CARTESIAN_POINT('Ctrl Pts',(-0.757735118862955,-4.45414404053564,
28.3357647490651));
#41434=CARTESIAN_POINT('Ctrl Pts',(-1.49791254967336,-4.32822569833327,
28.3093074523807));
#41435=CARTESIAN_POINT('Ctrl Pts',(-2.20602436190953,-4.01381815941419,
28.2828501556962));
#41436=CARTESIAN_POINT('Ctrl Pts',(-2.79582332053056,-3.54921591405409,
28.2563928590117));
#41437=CARTESIAN_POINT('Ctrl Pts',(-3.38562227915162,-3.08461366869397,
28.2299355623272));
#41438=CARTESIAN_POINT('Ctrl Pts',(-3.85710838415752,-2.46981671689283,
28.2034782656428));
#41439=CARTESIAN_POINT('Ctrl Pts',(-4.15285514976694,-1.77970664696505,
28.1770209689583));
#41440=CARTESIAN_POINT('Ctrl Pts',(-4.44860191537634,-1.08959657703732,
28.1505636722738));
#41441=CARTESIAN_POINT('Ctrl Pts',(-4.56860934158928,-0.32417338898296,
28.1241063755894));
#41442=CARTESIAN_POINT('Ctrl Pts',(-4.49826065670898,0.423335220010742,
28.0976490789049));
#41443=CARTESIAN_POINT('Ctrl Pts',(-4.42791197182868,1.17084382900444,28.0711917822204));
#41444=CARTESIAN_POINT('Ctrl Pts',(-4.16720717585513,1.90043785893749,28.0447344855359));
#41445=CARTESIAN_POINT('Ctrl Pts',(-3.7478998244078,2.52325356442854,28.0182771888515));
#41446=CARTESIAN_POINT('Ctrl Pts',(-3.32859247296047,3.14606926991958,27.991819892167));
#41447=CARTESIAN_POINT('Ctrl Pts',(-2.75068256603934,3.66210665096863,27.9653625954826));
#41448=CARTESIAN_POINT('Ctrl Pts',(-2.08455889071647,4.00851292567859,27.9389052987981));
#41449=CARTESIAN_POINT('Ctrl Pts',(-1.41843521539359,4.35491920038855,27.9124480021136));
#41450=CARTESIAN_POINT('Ctrl Pts',(-0.664097771668966,4.53169436875941,
27.8859907054291));
#41451=CARTESIAN_POINT('Ctrl Pts',(0.0865759746605513,4.51730741092622,
27.8595334087447));
#41452=CARTESIAN_POINT('Ctrl Pts',(0.837249720990026,4.50292045309303,27.8330761120602));
#41453=CARTESIAN_POINT('Ctrl Pts',(1.58425976992439,4.2973713690558,27.8066188153758));
#41454=CARTESIAN_POINT('Ctrl Pts',(2.23662112424281,3.92569580976267,27.7801615186913));
#41455=CARTESIAN_POINT('Ctrl Pts',(2.88898247856131,3.5540202504695,27.7537042220068));
#41456=CARTESIAN_POINT('Ctrl Pts',(3.44669513826383,3.0162182159204,27.7272469253223));
#41457=CARTESIAN_POINT('Ctrl Pts',(3.84183031863663,2.37779339872113,27.7007896286379));
#41458=CARTESIAN_POINT('Ctrl Pts',(4.23696549900942,1.73936858152187,27.6743323319534));
#41459=CARTESIAN_POINT('Ctrl Pts',(4.46952320005248,1.00032098167245,27.647875035269));
#41460=CARTESIAN_POINT('Ctrl Pts',(4.51117815115764,0.250665778907488,27.6214177385845));
#41461=CARTESIAN_POINT('Ctrl Pts',(4.51581452813225,0.167225898922454,27.6184729265537));
#41462=CARTESIAN_POINT('Ctrl Pts',(4.51808587645197,0.0836546049852204,
27.6155281145228));
#41463=CARTESIAN_POINT('Ctrl Pts',(4.51801726226543,7.95831363512023E-5,
27.612583302492));
#41464=CARTESIAN_POINT('Origin',(0.,0.,20.5));
#41465=CARTESIAN_POINT('',(4.51761428595877,-0.000111883206665997,26.612583302492));
#41466=CARTESIAN_POINT('',(4.51781182322151,0.000114263439177032,26.8874166975081));
#41467=CARTESIAN_POINT('',(4.51775,5.53264807684796E-16,20.5));
#41468=CARTESIAN_POINT('Ctrl Pts',(4.51781182322151,0.000114263439177032,
26.8874166975081));
#41469=CARTESIAN_POINT('Ctrl Pts',(4.51797007849026,0.153591581624792,26.8928238454015));
#41470=CARTESIAN_POINT('Ctrl Pts',(4.51030214935632,0.307053160819986,26.898230993295));
#41471=CARTESIAN_POINT('Ctrl Pts',(4.49468970350708,0.459702200761322,26.9036381411884));
#41472=CARTESIAN_POINT('Ctrl Pts',(4.41829765358665,1.20661739855353,26.9300954378729));
#41473=CARTESIAN_POINT('Ctrl Pts',(4.1517006071518,1.93407904976938,26.9565527345573));
#41474=CARTESIAN_POINT('Ctrl Pts',(3.727369789407,2.55348313039531,26.9830100312418));
#41475=CARTESIAN_POINT('Ctrl Pts',(3.30303897166215,3.17288721102131,27.0094673279263));
#41476=CARTESIAN_POINT('Ctrl Pts',(2.72097438260733,3.68423372105737,27.0359246246107));
#41477=CARTESIAN_POINT('Ctrl Pts',(2.05207084500035,4.02524122150424,27.0623819212952));
#41478=CARTESIAN_POINT('Ctrl Pts',(1.38316730739341,4.36624872195109,27.0888392179797));
#41479=CARTESIAN_POINT('Ctrl Pts',(0.627424821234327,4.53691721280878,27.1152965146642));
#41480=CARTESIAN_POINT('Ctrl Pts',(-0.123108015066531,4.51645946077497,
27.1417538113486));
#41481=CARTESIAN_POINT('Ctrl Pts',(-0.873640851367389,4.49600170874117,
27.1682111080331));
#41482=CARTESIAN_POINT('Ctrl Pts',(-1.61896403781002,4.28441771381588,27.1946684047176));
#41483=CARTESIAN_POINT('Ctrl Pts',(-2.26829803515817,3.9074781724144,27.221125701402));
#41484=CARTESIAN_POINT('Ctrl Pts',(-2.91763203250632,3.53053863101291,27.2475829980865));
#41485=CARTESIAN_POINT('Ctrl Pts',(-3.47097684075998,2.98824354313522,27.274040294771));
#41486=CARTESIAN_POINT('Ctrl Pts',(-3.86093567467783,2.34664385030993,27.3004975914554));
#41487=CARTESIAN_POINT('Ctrl Pts',(-4.25089450859569,1.70504415748464,27.3269548881399));
#41488=CARTESIAN_POINT('Ctrl Pts',(-4.47746736817774,0.96413985971173,27.3534121848244));
#41489=CARTESIAN_POINT('Ctrl Pts',(-4.51305792988216,0.214172280478033,
27.3798694815088));
#41490=CARTESIAN_POINT('Ctrl Pts',(-4.54864849158657,-0.535795298755707,
27.4063267781933));
#41491=CARTESIAN_POINT('Ctrl Pts',(-4.39325675541333,-1.29482615945024,
27.4327840748778));
#41492=CARTESIAN_POINT('Ctrl Pts',(-4.06580926285144,-1.97047118281612,
27.4592413715622));
#41493=CARTESIAN_POINT('Ctrl Pts',(-3.73836177028958,-2.64611620618197,
27.4856986682467));
#41494=CARTESIAN_POINT('Ctrl Pts',(-3.23885852133909,-3.23837539221917,
27.5121559649312));
#41495=CARTESIAN_POINT('Ctrl Pts',(-2.62813845890629,-3.67511222754014,
27.5386132616156));
#41496=CARTESIAN_POINT('Ctrl Pts',(-2.0174183964735,-4.11184906286111,27.5650705583001));
#41497=CARTESIAN_POINT('Ctrl Pts',(-1.29548152055841,-4.39306354746584,
27.5915278549846));
#41498=CARTESIAN_POINT('Ctrl Pts',(-0.550258943657392,-4.48450406835833,
27.617985151669));
#41499=CARTESIAN_POINT('Ctrl Pts',(0.194963633243671,-4.57594458925083,
27.6444424483535));
#41500=CARTESIAN_POINT('Ctrl Pts',(0.963471911130666,-4.47761114643107,
27.670899745038));
#41501=CARTESIAN_POINT('Ctrl Pts',(1.66166243228906,-4.20148064440581,27.6973570417224));
#41502=CARTESIAN_POINT('Ctrl Pts',(2.35985295344741,-3.92535014238055,27.7238143384069));
#41503=CARTESIAN_POINT('Ctrl Pts',(2.98772571787716,-3.47142258114982,27.7502716350914));
#41504=CARTESIAN_POINT('Ctrl Pts',(3.46880651775718,-2.89498583529569,27.7767289317758));
#41505=CARTESIAN_POINT('Ctrl Pts',(3.94988731763719,-2.31854908944157,27.8031862284603));
#41506=CARTESIAN_POINT('Ctrl Pts',(4.28417615296746,-1.61960315896406,27.8296435251448));
#41507=CARTESIAN_POINT('Ctrl Pts',(4.43095701357266,-0.883278884650025,
27.8561008218292));
#41508=CARTESIAN_POINT('Ctrl Pts',(4.48886884079068,-0.592764958142916,
27.8665394470555));
#41509=CARTESIAN_POINT('Ctrl Pts',(4.517591923217,-0.296432468768919,27.8769780722818));
#41510=CARTESIAN_POINT('Ctrl Pts',(4.51743092439869,-6.91819792334251E-5,
27.8874166975081));
#41511=CARTESIAN_POINT('Ctrl Pts',(4.51801726226543,7.95831363512023E-5,
27.612583302492));
#41512=CARTESIAN_POINT('Ctrl Pts',(4.5174694208443,-0.667214763012837,27.5890708178383));
#41513=CARTESIAN_POINT('Ctrl Pts',(4.36774838447631,-1.33474676446109,27.5655583331847));
#41514=CARTESIAN_POINT('Ctrl Pts',(4.08161297138008,-1.93752346980862,27.5420458485311));
#41515=CARTESIAN_POINT('Ctrl Pts',(3.7596406393301,-2.61579471007933,27.5155885518466));
#41516=CARTESIAN_POINT('Ctrl Pts',(3.26494377406285,-3.21207438494031,27.4891312551621));
#41517=CARTESIAN_POINT('Ctrl Pts',(2.65777590627143,-3.65373628991481,27.4626739584777));
#41518=CARTESIAN_POINT('Ctrl Pts',(2.05060803847998,-4.09539819488933,27.4362166617932));
#41519=CARTESIAN_POINT('Ctrl Pts',(1.33096916816432,-4.38244232997737,27.4097593651087));
#41520=CARTESIAN_POINT('Ctrl Pts',(0.586510513282131,-4.47990703720589,
27.3833020684243));
#41521=CARTESIAN_POINT('Ctrl Pts',(-0.15794814160006,-4.57737174443442,
27.3568447717398));
#41522=CARTESIAN_POINT('Ctrl Pts',(-0.927226581048814,-4.48525702380344,
27.3303874750553));
#41523=CARTESIAN_POINT('Ctrl Pts',(-1.62762754252371,-4.21478234633956,
27.3039301783709));
#41524=CARTESIAN_POINT('Ctrl Pts',(-2.32802850399852,-3.94430766887572,
27.2774728816864));
#41525=CARTESIAN_POINT('Ctrl Pts',(-2.95955198749952,-3.49547303457901,
27.2510155850019));
#41526=CARTESIAN_POINT('Ctrl Pts',(-3.44527913166303,-2.92294600516749,
27.2245582883174));
#41527=CARTESIAN_POINT('Ctrl Pts',(-3.93100627582659,-2.35041897575591,
27.198100991633));
#41528=CARTESIAN_POINT('Ctrl Pts',(-4.27093708065265,-1.65419955122946,
27.1716436949485));
#41529=CARTESIAN_POINT('Ctrl Pts',(-4.42366835032541,-0.919086486967716,
27.1451863982641));
#41530=CARTESIAN_POINT('Ctrl Pts',(-4.57639961999816,-0.183973422706017,
27.1187291015796));
#41531=CARTESIAN_POINT('Ctrl Pts',(-4.54193135451766,0.590033281290875,
27.0922718048951));
#41532=CARTESIAN_POINT('Ctrl Pts',(-4.32446175047231,1.30866046509374,27.0658145082107));
#41533=CARTESIAN_POINT('Ctrl Pts',(-4.10699214642695,2.02728764889665,27.0393572115262));
#41534=CARTESIAN_POINT('Ctrl Pts',(-3.7065212038167,2.69053531250543,27.0128999148417));
#41535=CARTESIAN_POINT('Ctrl Pts',(-3.17182584023783,3.21762062452939,26.9864426181572));
#41536=CARTESIAN_POINT('Ctrl Pts',(-2.63713047665899,3.74470593655333,26.9599853214728));
#41537=CARTESIAN_POINT('Ctrl Pts',(-1.96821069211152,4.13562889699249,26.9335280247883));
#41538=CARTESIAN_POINT('Ctrl Pts',(-1.2465401760389,4.34277552191203,26.9070707281038));
#41539=CARTESIAN_POINT('Ctrl Pts',(-0.524869659966319,4.54992214683155,
26.8806134314194));
#41540=CARTESIAN_POINT('Ctrl Pts',(0.249551587631431,4.57329243623147,26.8541561347349));
#41541=CARTESIAN_POINT('Ctrl Pts',(0.982399915873105,4.41003991472752,26.8276988380504));
#41542=CARTESIAN_POINT('Ctrl Pts',(1.71524824411482,4.24678739322355,26.801241541366));
#41543=CARTESIAN_POINT('Ctrl Pts',(2.40652365300059,3.89691206081561,26.7747842446815));
#41544=CARTESIAN_POINT('Ctrl Pts',(2.97202956278397,3.40302834577314,26.748326947997));
#41545=CARTESIAN_POINT('Ctrl Pts',(3.53753547256739,2.90914463073064,26.7218696513126));
#41546=CARTESIAN_POINT('Ctrl Pts',(3.97727188324847,2.27125253305366,26.6954123546281));
#41547=CARTESIAN_POINT('Ctrl Pts',(4.23767938667642,1.56704660426395,26.6689550579436));
#41548=CARTESIAN_POINT('Ctrl Pts',(4.42262682954492,1.06690323639616,26.6501644727931));
#41549=CARTESIAN_POINT('Ctrl Pts',(4.5171177314681,0.533310047910147,26.6313738876425));
#41550=CARTESIAN_POINT('Ctrl Pts',(4.51761428595877,-0.000111883206665997,
26.612583302492));
#41551=CARTESIAN_POINT('Origin',(0.,0.,20.5));
#41552=CARTESIAN_POINT('',(4.51757373878986,0.000106944042679857,25.612583302492));
#41553=CARTESIAN_POINT('',(4.51783003468408,-0.000112853895665516,25.8874166975081));
#41554=CARTESIAN_POINT('',(4.51775,5.53264807684796E-16,20.5));
#41555=CARTESIAN_POINT('Ctrl Pts',(4.51783003468408,-0.000112853895665516,
25.8874166975081));
#41556=CARTESIAN_POINT('Ctrl Pts',(4.51721010591009,0.603126320584693,25.9086696185212));
#41557=CARTESIAN_POINT('Ctrl Pts',(4.39561298077165,1.20660788106352,25.9299225395344));
#41558=CARTESIAN_POINT('Ctrl Pts',(4.16040899613699,1.76197577425452,25.9511754605476));
#41559=CARTESIAN_POINT('Ctrl Pts',(3.86760869828648,2.45334112163804,25.977632757232));
#41560=CARTESIAN_POINT('Ctrl Pts',(3.39874939952398,3.0701436809076,26.0040900539165));
#41561=CARTESIAN_POINT('Ctrl Pts',(2.81093764353751,3.53725758297881,26.030547350601));
#41562=CARTESIAN_POINT('Ctrl Pts',(2.22312588755105,4.00437148505003,26.0570046472854));
#41563=CARTESIAN_POINT('Ctrl Pts',(1.51636167434063,4.32179672992291,26.0834619439699));
#41564=CARTESIAN_POINT('Ctrl Pts',(0.776728102877261,4.45087127407636,26.1099192406544));
#41565=CARTESIAN_POINT('Ctrl Pts',(0.0370945314138876,4.57994581822981,
26.1363765373388));
#41566=CARTESIAN_POINT('Ctrl Pts',(-0.735408398302442,4.52066966166383,
26.1628338340233));
#41567=CARTESIAN_POINT('Ctrl Pts',(-1.4466906843854,4.28026257464538,26.1892911307078));
#41568=CARTESIAN_POINT('Ctrl Pts',(-2.15797297046839,4.03985548762692,26.2157484273923));
#41569=CARTESIAN_POINT('Ctrl Pts',(-2.80803461291801,3.61831747015598,26.2422057240767));
#41570=CARTESIAN_POINT('Ctrl Pts',(-3.31769882312739,3.06699138623123,26.2686630207612));
#41571=CARTESIAN_POINT('Ctrl Pts',(-3.82736303333674,2.51566530230651,26.2951203174456));
#41572=CARTESIAN_POINT('Ctrl Pts',(-4.19662981130587,1.834551151928,26.3215776141301));
#41573=CARTESIAN_POINT('Ctrl Pts',(-4.38052287215722,1.1066078848015,26.3480349108146));
#41574=CARTESIAN_POINT('Ctrl Pts',(-4.56441593300857,0.378664617674993,
26.3744922074991));
#41575=CARTESIAN_POINT('Ctrl Pts',(-4.56293527674215,-0.396107766199503,
26.4009495041835));
#41576=CARTESIAN_POINT('Ctrl Pts',(-4.3762612456525,-1.12334284793087,26.427406800868));
#41577=CARTESIAN_POINT('Ctrl Pts',(-4.18958721456285,-1.85057792966224,
26.4538640975524));
#41578=CARTESIAN_POINT('Ctrl Pts',(-3.81771980864998,-2.53027570925048,
26.4803213942369));
#41579=CARTESIAN_POINT('Ctrl Pts',(-3.30595206639681,-3.0796497493845,26.5067786909214));
#41580=CARTESIAN_POINT('Ctrl Pts',(-2.79418432414364,-3.62902378951853,
26.5332359876059));
#41581=CARTESIAN_POINT('Ctrl Pts',(-2.14251624555017,-4.04807409019834,
26.5596932842903));
#41582=CARTESIAN_POINT('Ctrl Pts',(-1.43032028136767,-4.28576078857718,
26.5861505809748));
#41583=CARTESIAN_POINT('Ctrl Pts',(-0.718124317185119,-4.52344748695604,
26.6126078776593));
#41584=CARTESIAN_POINT('Ctrl Pts',(0.0545995325864684,-4.57977058303392,
26.6390651743437));
#41585=CARTESIAN_POINT('Ctrl Pts',(0.793734358242524,-4.44786998604306,
26.6655224710282));
#41586=CARTESIAN_POINT('Ctrl Pts',(1.53286918389854,-4.31596938905221,26.6919797677127));
#41587=CARTESIAN_POINT('Ctrl Pts',(2.23841498543902,-3.99584509899264,26.7184370643971));
#41588=CARTESIAN_POINT('Ctrl Pts',(2.82443706508592,-3.52648790010206,26.7448943610816));
#41589=CARTESIAN_POINT('Ctrl Pts',(3.41045914473281,-3.05713070121148,26.7713516577661));
#41590=CARTESIAN_POINT('Ctrl Pts',(3.87695750248613,-2.43854059348989,26.7978089544505));
#41591=CARTESIAN_POINT('Ctrl Pts',(4.1671131546598,-1.74606116744478,26.824266251135));
#41592=CARTESIAN_POINT('Ctrl Pts',(4.39796892664792,-1.19510559829445,26.845316399926));
#41593=CARTESIAN_POINT('Ctrl Pts',(4.51719573188836,-0.59737640031138,26.8663665487171));
#41594=CARTESIAN_POINT('Ctrl Pts',(4.51781182322151,0.000114263439177032,
26.8874166975081));
#41595=CARTESIAN_POINT('Ctrl Pts',(4.51761428595877,-0.000111883206665997,
26.612583302492));
#41596=CARTESIAN_POINT('Ctrl Pts',(4.51781688422861,-0.217752368533235,
26.604916590958));
#41597=CARTESIAN_POINT('Ctrl Pts',(4.50237218377303,-0.435364344536763,
26.5972498794241));
#41598=CARTESIAN_POINT('Ctrl Pts',(4.47103989191871,-0.65066422144523,26.5895831678902));
#41599=CARTESIAN_POINT('Ctrl Pts',(4.36291429755835,-1.39364935846232,26.5631258712058));
#41600=CARTESIAN_POINT('Ctrl Pts',(4.06558451266292,-2.10909987259421,26.5366685745213));
#41601=CARTESIAN_POINT('Ctrl Pts',(3.61526497596852,-2.70987468303106,26.5102112778368));
#41602=CARTESIAN_POINT('Ctrl Pts',(3.16494543927413,-3.31064949346792,26.4837539811524));
#41603=CARTESIAN_POINT('Ctrl Pts',(2.56163615078078,-3.79674860020972,26.4572966844679));
#41604=CARTESIAN_POINT('Ctrl Pts',(1.87881951412572,-4.10896567003641,26.4308393877834));
#41605=CARTESIAN_POINT('Ctrl Pts',(1.19600287747066,-4.4211827398631,26.4043820910989));
#41606=CARTESIAN_POINT('Ctrl Pts',(0.433678892653904,-4.55951777277466,
26.3779247944145));
#41607=CARTESIAN_POINT('Ctrl Pts',(-0.315302222661645,-4.50712171486216,
26.35146749773));
#41608=CARTESIAN_POINT('Ctrl Pts',(-1.06428333797715,-4.45472565694967,
26.3250102010456));
#41609=CARTESIAN_POINT('Ctrl Pts',(-1.79992158379143,-4.21159850821314,
26.2985529043611));
#41610=CARTESIAN_POINT('Ctrl Pts',(-2.43261703591816,-3.80735288629228,
26.2720956076766));
#41611=CARTESIAN_POINT('Ctrl Pts',(-3.06531248804499,-3.40310726437134,
26.2456383109922));
#41612=CARTESIAN_POINT('Ctrl Pts',(-3.59506514648422,-2.83774316926603,
26.2191810143077));
#41613=CARTESIAN_POINT('Ctrl Pts',(-3.95735172373175,-2.18012132205405,
26.1927237176232));
#41614=CARTESIAN_POINT('Ctrl Pts',(-4.31963830097924,-1.52249947484215,
26.1662664209387));
#41615=CARTESIAN_POINT('Ctrl Pts',(-4.51445879703509,-0.772619875523507,
26.1398091242543));
#41616=CARTESIAN_POINT('Ctrl Pts',(-4.51808429109356,-0.0218170293801812,
26.1133518275698));
#41617=CARTESIAN_POINT('Ctrl Pts',(-4.52170978515203,0.728985816763102,
26.0868945308853));
#41618=CARTESIAN_POINT('Ctrl Pts',(-4.33414027721319,1.48071190973118,26.0604372342009));
#41619=CARTESIAN_POINT('Ctrl Pts',(-3.97822152575495,2.1418018433593,26.0339799375164));
#41620=CARTESIAN_POINT('Ctrl Pts',(-3.62230277429665,2.80289177698754,26.0075226408319));
#41621=CARTESIAN_POINT('Ctrl Pts',(-3.09803477931891,3.37334555127578,25.9810653441475));
#41622=CARTESIAN_POINT('Ctrl Pts',(-2.46927280238623,3.78368252785471,25.954608047463));
#41623=CARTESIAN_POINT('Ctrl Pts',(-1.84051082545367,4.19401950443358,25.9281507507785));
#41624=CARTESIAN_POINT('Ctrl Pts',(-1.10725486656624,4.44423968330318,25.9016934540941));
#41625=CARTESIAN_POINT('Ctrl Pts',(-0.358814689999135,4.50386652360371,
25.8752361574096));
#41626=CARTESIAN_POINT('Ctrl Pts',(0.389625486568016,4.56349336390425,25.8487788607251));
#41627=CARTESIAN_POINT('Ctrl Pts',(1.15324988081482,4.43252686563568,25.8223215640406));
#41628=CARTESIAN_POINT('Ctrl Pts',(1.83904988664902,4.1269186033424,25.7958642673562));
#41629=CARTESIAN_POINT('Ctrl Pts',(2.52484989248321,3.82131034104913,25.7694069706717));
#41630=CARTESIAN_POINT('Ctrl Pts',(3.13282550990476,3.34106031473115,25.7429496739873));
#41631=CARTESIAN_POINT('Ctrl Pts',(3.58892598157735,2.74466244608629,25.7164923773028));
#41632=CARTESIAN_POINT('Ctrl Pts',(4.04502645324994,2.14826457744144,25.6900350806183));
#41633=CARTESIAN_POINT('Ctrl Pts',(4.34925177917356,1.43571886646971,25.6635777839338));
#41634=CARTESIAN_POINT('Ctrl Pts',(4.46454765134638,0.693812592170858,25.6371204872494));
#41635=CARTESIAN_POINT('Ctrl Pts',(4.50019044774909,0.464458203445785,25.6289414256636));
#41636=CARTESIAN_POINT('Ctrl Pts',(4.51777748758952,0.232297861633777,25.6207623640778));
#41637=CARTESIAN_POINT('Ctrl Pts',(4.51757373878986,0.000106944042679857,
25.612583302492));
#41638=CARTESIAN_POINT('Origin',(0.,0.,20.5));
#41639=CARTESIAN_POINT('',(4.51805179992706,-6.79869438786201E-5,24.612583302492));
#41640=CARTESIAN_POINT('',(4.51742159705025,6.47500723078405E-5,24.8874166975081));
#41641=CARTESIAN_POINT('',(4.51775,5.53264807684796E-16,20.5));
#41642=CARTESIAN_POINT('Ctrl Pts',(4.51742159705025,6.47500723078405E-5,
24.8874166975081));
#41643=CARTESIAN_POINT('Ctrl Pts',(4.51757480489056,0.3021867342129,24.8980580949565));
#41644=CARTESIAN_POINT('Ctrl Pts',(4.4877169204789,0.604278844221435,24.9086994924049));
#41645=CARTESIAN_POINT('Ctrl Pts',(4.42754861718235,0.90020824628754,24.9193408898533));
#41646=CARTESIAN_POINT('Ctrl Pts',(4.27795448172836,1.63596612264488,24.9457981865378));
#41647=CARTESIAN_POINT('Ctrl Pts',(3.94099660709531,2.33362924326996,24.9722554832222));
#41648=CARTESIAN_POINT('Ctrl Pts',(3.4577160894917,2.90822301219621,24.9987127799067));
#41649=CARTESIAN_POINT('Ctrl Pts',(2.97443557188809,3.48281678112246,25.0251700765912));
#41650=CARTESIAN_POINT('Ctrl Pts',(2.34483241131392,3.93434119834988,25.0516273732757));
#41651=CARTESIAN_POINT('Ctrl Pts',(1.64559157592564,4.20780108957635,25.0780846699601));
#41652=CARTESIAN_POINT('Ctrl Pts',(0.946350740537367,4.48126098080282,25.1045419666446));
#41653=CARTESIAN_POINT('Ctrl Pts',(0.177472230334982,4.57665634602833,25.1309992633291));
#41654=CARTESIAN_POINT('Ctrl Pts',(-0.567395403080719,4.48236813534545,
25.1574565600135));
#41655=CARTESIAN_POINT('Ctrl Pts',(-1.31226303649646,4.38807992466257,25.183913856698));
#41656=CARTESIAN_POINT('Ctrl Pts',(-2.03311979312552,4.10410813807126,25.2103711533825));
#41657=CARTESIAN_POINT('Ctrl Pts',(-2.64216611780515,3.66504022489793,25.2368284500669));
#41658=CARTESIAN_POINT('Ctrl Pts',(-3.25121244248478,3.22597231172459,25.2632857467514));
#41659=CARTESIAN_POINT('Ctrl Pts',(-3.74844833521498,2.63180827196922,25.2897430434359));
#41660=CARTESIAN_POINT('Ctrl Pts',(-4.07331101456769,1.95491662809413,25.3162003401203));
#41661=CARTESIAN_POINT('Ctrl Pts',(-4.39817369392037,1.27802498421911,25.3426576368048));
#41662=CARTESIAN_POINT('Ctrl Pts',(-4.55066315989561,0.518405736224393,
25.3691149334893));
#41663=CARTESIAN_POINT('Ctrl Pts',(-4.51220636430247,-0.231420332178628,
25.3955722301737));
#41664=CARTESIAN_POINT('Ctrl Pts',(-4.47374956870933,-0.981246400581734,
25.4220295268582));
#41665=CARTESIAN_POINT('Ctrl Pts',(-4.24434651154778,-1.72127928939314,
25.4484868235427));
#41666=CARTESIAN_POINT('Ctrl Pts',(-3.85193823129256,-2.36138381177311,
25.4749441202271));
#41667=CARTESIAN_POINT('Ctrl Pts',(-3.45952995103737,-3.00148833415305,
25.5014014169116));
#41668=CARTESIAN_POINT('Ctrl Pts',(-2.90411644768853,-3.54166449010157,
25.5278587135961));
#41669=CARTESIAN_POINT('Ctrl Pts',(-2.25334647126047,-3.91611942165396,
25.5543160102806));
#41670=CARTESIAN_POINT('Ctrl Pts',(-1.60257649483241,-4.29057435320635,
25.580773306965));
#41671=CARTESIAN_POINT('Ctrl Pts',(-0.856450045325122,-4.49930806036262,
25.6072306036495));
#41672=CARTESIAN_POINT('Ctrl Pts',(-0.105844498527155,-4.51689700860324,
25.6336879003339));
#41673=CARTESIAN_POINT('Ctrl Pts',(0.644761048270813,-4.53448595684386,
25.6601451970184));
#41674=CARTESIAN_POINT('Ctrl Pts',(1.39984569235946,-4.36093014616883,25.6866024937029));
#41675=CARTESIAN_POINT('Ctrl Pts',(2.06744095976455,-4.01736848223874,25.7130597903874));
#41676=CARTESIAN_POINT('Ctrl Pts',(2.73503622716964,-3.67380681830865,25.7395170870718));
#41677=CARTESIAN_POINT('Ctrl Pts',(3.31514211789117,-3.16023930112349,25.7659743837563));
#41678=CARTESIAN_POINT('Ctrl Pts',(3.73710237646057,-2.53921788589521,25.7924316804407));
#41679=CARTESIAN_POINT('Ctrl Pts',(4.15906263502999,-1.9181964706669,25.8188889771252));
#41680=CARTESIAN_POINT('Ctrl Pts',(4.42287726144725,-1.18972115739545,25.8453462738097));
#41681=CARTESIAN_POINT('Ctrl Pts',(4.49641392618663,-0.442519433010954,
25.8718035704942));
#41682=CARTESIAN_POINT('Ctrl Pts',(4.51087921466574,-0.295538487742104,
25.8770079461655));
#41683=CARTESIAN_POINT('Ctrl Pts',(4.51798184168639,-0.147832938193592,
25.8822123218368));
#41684=CARTESIAN_POINT('Ctrl Pts',(4.51783003468408,-0.000112853895665516,
25.8874166975081));
#41685=CARTESIAN_POINT('Ctrl Pts',(4.51757373878986,0.000106944042679857,
25.612583302492));
#41686=CARTESIAN_POINT('Ctrl Pts',(4.51711840923619,-0.518783901194552,
25.5943050673933));
#41687=CARTESIAN_POINT('Ctrl Pts',(4.42781321686835,-1.03782744645157,25.5760268322946));
#41688=CARTESIAN_POINT('Ctrl Pts',(4.25261539535607,-1.52604847346927,25.557748597196));
#41689=CARTESIAN_POINT('Ctrl Pts',(3.99902084877091,-2.2327364271846,25.5312913005115));
#41690=CARTESIAN_POINT('Ctrl Pts',(3.56546533717857,-2.87484549698929,25.504834003827));
#41691=CARTESIAN_POINT('Ctrl Pts',(3.00475544206156,-3.3741675088233,25.4783767071426));
#41692=CARTESIAN_POINT('Ctrl Pts',(2.44404554694452,-3.87348952065733,25.4519194104581));
#41693=CARTESIAN_POINT('Ctrl Pts',(1.7561812683028,-4.23002447452067,25.4254621137736));
#41694=CARTESIAN_POINT('Ctrl Pts',(1.0249437139941,-4.40034680762112,25.3990048170892));
#41695=CARTESIAN_POINT('Ctrl Pts',(0.293706159685441,-4.57066914072155,
25.3725475204047));
#41696=CARTESIAN_POINT('Ctrl Pts',(-0.4809046702902,-4.55477885305912,25.3460902237202));
#41697=CARTESIAN_POINT('Ctrl Pts',(-1.20454203412779,-4.35461136408482,
25.3196329270358));
#41698=CARTESIAN_POINT('Ctrl Pts',(-1.92817939796537,-4.15444387511052,
25.2931756303513));
#41699=CARTESIAN_POINT('Ctrl Pts',(-2.60084329566491,-3.76999918482436,
25.2667183336669));
#41700=CARTESIAN_POINT('Ctrl Pts',(-3.14060400894472,-3.24810223102625,
25.2402610369824));
#41701=CARTESIAN_POINT('Ctrl Pts',(-3.68036472222457,-2.72620527722811,
25.2138037402979));
#41702=CARTESIAN_POINT('Ctrl Pts',(-4.08722225108469,-2.066856059918,25.1873464436134));
#41703=CARTESIAN_POINT('Ctrl Pts',(-4.31162179879184,-1.35036258404192,
25.1608891469289));
#41704=CARTESIAN_POINT('Ctrl Pts',(-4.53602134649897,-0.633869108165933,
25.1344318502445));
#41705=CARTESIAN_POINT('Ctrl Pts',(-4.57796291305318,0.139768626276003,
25.1079745535601));
#41706=CARTESIAN_POINT('Ctrl Pts',(-4.4323380620662,0.876322399437911,25.0815172568756));
#41707=CARTESIAN_POINT('Ctrl Pts',(-4.28671321107921,1.6128761725999,25.0550599601911));
#41708=CARTESIAN_POINT('Ctrl Pts',(-3.95352194255099,2.31234598448186,25.0286026635066));
#41709=CARTESIAN_POINT('Ctrl Pts',(-3.4733465842351,2.88953718612163,25.0021453668221));
#41710=CARTESIAN_POINT('Ctrl Pts',(-2.99317122591925,3.46672838776137,24.9756880701377));
#41711=CARTESIAN_POINT('Ctrl Pts',(-2.36601177781574,3.92164097915893,24.9492307734532));
#41712=CARTESIAN_POINT('Ctrl Pts',(-1.66825556660664,4.19886711014808,24.9227734767688));
#41713=CARTESIAN_POINT('Ctrl Pts',(-0.970499355397546,4.47609324113723,
24.8963161800843));
#41714=CARTESIAN_POINT('Ctrl Pts',(-0.202146381082855,4.57563291171796,
24.8698588833998));
#41715=CARTESIAN_POINT('Ctrl Pts',(0.543218814426126,4.4853623001772,24.8434015867153));
#41716=CARTESIAN_POINT('Ctrl Pts',(1.28858400993515,4.39509168863642,24.8169442900309));
#41717=CARTESIAN_POINT('Ctrl Pts',(2.01096142663846,4.11501079497414,24.7904869933464));
#41718=CARTESIAN_POINT('Ctrl Pts',(2.62236629465924,3.67923316206414,24.7640296966619));
#41719=CARTESIAN_POINT('Ctrl Pts',(3.23377116267999,3.24345552915417,24.7375723999775));
#41720=CARTESIAN_POINT('Ctrl Pts',(3.73420348201823,2.65198115699651,24.711115103293));
#41721=CARTESIAN_POINT('Ctrl Pts',(4.06271115002261,1.97685096951678,24.6846578066085));
#41722=CARTESIAN_POINT('Ctrl Pts',(4.36101609468216,1.3637916931913,24.660632971903));
#41723=CARTESIAN_POINT('Ctrl Pts',(4.51755636187948,0.681751967669245,24.6366081371975));
#41724=CARTESIAN_POINT('Ctrl Pts',(4.51805179992706,-6.79869438786201E-5,
24.612583302492));
#41725=CARTESIAN_POINT('Origin',(0.,0.,20.5));
#41726=CARTESIAN_POINT('',(4.5173631353831,-4.88662610135722E-6,23.612583302492));
#41727=CARTESIAN_POINT('',(4.51813699104787,9.0065690785813E-7,23.8874166975081));
#41728=CARTESIAN_POINT('',(4.51775,5.53264807684796E-16,20.5));
#41729=CARTESIAN_POINT('Ctrl Pts',(4.51813695063288,9.0056284873609E-7,
23.8874166975081));
#41730=CARTESIAN_POINT('Ctrl Pts',(4.51814591729222,0.751660275924123,23.9139038680762));
#41731=CARTESIAN_POINT('Ctrl Pts',(4.32649937043261,1.5033152188212,23.9403910386443));
#41732=CARTESIAN_POINT('Ctrl Pts',(3.96661538289285,2.16322075812818,23.9668782092125));
#41733=CARTESIAN_POINT('Ctrl Pts',(3.6071372949696,2.8223820147924,23.9933355058969));
#41734=CARTESIAN_POINT('Ctrl Pts',(3.07980110896882,3.39000071259223,24.0197928025814));
#41735=CARTESIAN_POINT('Ctrl Pts',(2.44883578872663,3.7969415223372,24.0462500992659));
#41736=CARTESIAN_POINT('Ctrl Pts',(1.81787046848448,4.20388233208215,24.0727073959503));
#41737=CARTESIAN_POINT('Ctrl Pts',(1.08327601400093,4.45014525377226,24.0991646926348));
#41738=CARTESIAN_POINT('Ctrl Pts',(0.334525216833109,4.50573573609242,24.1256219893193));
#41739=CARTESIAN_POINT('Ctrl Pts',(-0.414225580334709,4.56132621841258,
24.1520792860037));
#41740=CARTESIAN_POINT('Ctrl Pts',(-1.17713272018679,4.4262442613628,24.1785365826882));
#41741=CARTESIAN_POINT('Ctrl Pts',(-1.86127495742213,4.11694269781237,24.2049938793727));
#41742=CARTESIAN_POINT('Ctrl Pts',(-2.54541719465748,3.80764113426195,24.2314511760572));
#41743=CARTESIAN_POINT('Ctrl Pts',(-3.15079452927609,3.32411996421088,24.2579084727416));
#41744=CARTESIAN_POINT('Ctrl Pts',(-3.6036726719115,2.72527153104338,24.2843657694261));
#41745=CARTESIAN_POINT('Ctrl Pts',(-4.05655081454692,2.12642309787588,24.3108230661106));
#41746=CARTESIAN_POINT('Ctrl Pts',(-4.35692976519914,1.41224740159195,24.337280362795));
#41747=CARTESIAN_POINT('Ctrl Pts',(-4.46822370011745,0.669730251598438,
24.3637376594795));
#41748=CARTESIAN_POINT('Ctrl Pts',(-4.57951763503577,-0.0727868983951169,
24.390194956164));
#41749=CARTESIAN_POINT('Ctrl Pts',(-4.50172655422016,-0.843645502098255,
24.4166522528484));
#41750=CARTESIAN_POINT('Ctrl Pts',(-4.24432532522016,-1.54895583471323,
24.4431095495329));
#41751=CARTESIAN_POINT('Ctrl Pts',(-3.98692409622017,-2.25426616732816,
24.4695668462174));
#41752=CARTESIAN_POINT('Ctrl Pts',(-3.54991271903582,-2.89402822885493,
24.4960241429018));
#41753=CARTESIAN_POINT('Ctrl Pts',(-2.98651869575401,-3.39031970824422,
24.5224814395863));
#41754=CARTESIAN_POINT('Ctrl Pts',(-2.42312467247219,-3.88661118763352,
24.5489387362708));
#41755=CARTESIAN_POINT('Ctrl Pts',(-1.73334800309291,-4.23943208488534,
24.5753960329552));
#41756=CARTESIAN_POINT('Ctrl Pts',(-1.00120272254919,-4.40580920519233,
24.6018533296397));
#41757=CARTESIAN_POINT('Ctrl Pts',(-0.269057442005433,-4.57218632549932,
24.6283106263242));
#41758=CARTESIAN_POINT('Ctrl Pts',(0.505456449702776,-4.55211966886146,
24.6547679230086));
#41759=CARTESIAN_POINT('Ctrl Pts',(1.22800401774408,-4.34805333184884,24.6812252196931));
#41760=CARTESIAN_POINT('Ctrl Pts',(1.95055158578534,-4.14398699483623,24.7076825163776));
#41761=CARTESIAN_POINT('Ctrl Pts',(2.6211328301597,-3.75592097744887,24.7341398130621));
#41762=CARTESIAN_POINT('Ctrl Pts',(3.15807169745557,-3.23112129111977,24.7605971097465));
#41763=CARTESIAN_POINT('Ctrl Pts',(3.69501056475143,-2.70632160479067,24.787054406431));
#41764=CARTESIAN_POINT('Ctrl Pts',(4.0983070549688,-2.04478824951983,24.8135117031154));
#41765=CARTESIAN_POINT('Ctrl Pts',(4.31884010194003,-1.32709525583961,24.8399689997999));
#41766=CARTESIAN_POINT('Ctrl Pts',(4.45067248416388,-0.898065782199879,
24.855784899036));
#41767=CARTESIAN_POINT('Ctrl Pts',(4.51719389013711,-0.448967520484957,
24.871600798272));
#41768=CARTESIAN_POINT('Ctrl Pts',(4.51742159705025,6.47500723078405E-5,
24.8874166975081));
#41769=CARTESIAN_POINT('Ctrl Pts',(4.51805179992706,-6.79869438786201E-5,
24.612583302492));
#41770=CARTESIAN_POINT('Ctrl Pts',(4.51810196194601,-0.0691007664161157,
24.610150840513));
#41771=CARTESIAN_POINT('Ctrl Pts',(4.51655248974293,-0.13813129299046,24.6077183785341));
#41772=CARTESIAN_POINT('Ctrl Pts',(4.51338856189906,-0.207087743519482,
24.6052859165551));
#41773=CARTESIAN_POINT('Ctrl Pts',(4.47897528910062,-0.957110266274211,
24.5788286198707));
#41774=CARTESIAN_POINT('Ctrl Pts',(4.25356572683319,-1.69836930898188,24.5523713231862));
#41775=CARTESIAN_POINT('Ctrl Pts',(3.8646145103131,-2.3405803406153,24.5259140265017));
#41776=CARTESIAN_POINT('Ctrl Pts',(3.47566329379301,-2.98279137224871,24.4994567298173));
#41777=CARTESIAN_POINT('Ctrl Pts',(2.92317042302025,-3.52595439280789,24.4729994331328));
#41778=CARTESIAN_POINT('Ctrl Pts',(2.27442891819395,-3.90391274752403,24.4465421364483));
#41779=CARTESIAN_POINT('Ctrl Pts',(1.62568741336761,-4.2818711022402,24.4200848397639));
#41780=CARTESIAN_POINT('Ctrl Pts',(0.88069727448771,-4.49462479111332,24.3936275430794));
#41781=CARTESIAN_POINT('Ctrl Pts',(0.130197475965773,-4.51626065030008,
24.3671702463949));
#41782=CARTESIAN_POINT('Ctrl Pts',(-0.620302322556121,-4.53789650948684,
24.3407129497104));
#41783=CARTESIAN_POINT('Ctrl Pts',(-1.37631178072007,-4.36841453898727,
24.314255653026));
#41784=CARTESIAN_POINT('Ctrl Pts',(-2.04574978322055,-4.02845745523667,
24.2877983563415));
#41785=CARTESIAN_POINT('Ctrl Pts',(-2.71518778572104,-3.68850037148608,
24.2613410596571));
#41786=CARTESIAN_POINT('Ctrl Pts',(-3.29805433255807,-3.17806817448446,
24.2348837629726));
#41787=CARTESIAN_POINT('Ctrl Pts',(-3.72335692340428,-2.55933094091641,
24.2084264662881));
#41788=CARTESIAN_POINT('Ctrl Pts',(-4.14865951425051,-1.94059370734831,
24.1819691696036));
#41789=CARTESIAN_POINT('Ctrl Pts',(-4.41639814910591,-1.21355143721374,
24.1555118729192));
#41790=CARTESIAN_POINT('Ctrl Pts',(-4.49396255855832,-0.466757074372799,
24.1290545762347));
#41791=CARTESIAN_POINT('Ctrl Pts',(-4.57152696801073,0.280037288468098,
24.1025972795502));
#41792=CARTESIAN_POINT('Ctrl Pts',(-4.4589171520602,1.04658374401527,24.0761399828658));
#41793=CARTESIAN_POINT('Ctrl Pts',(-4.16984886166344,1.73951778234053,24.0496826861813));
#41794=CARTESIAN_POINT('Ctrl Pts',(-3.88078057126667,2.43245182066584,24.0232253894968));
#41795=CARTESIAN_POINT('Ctrl Pts',(-3.41525380642364,3.05177344176913,23.9967680928124));
#41796=CARTESIAN_POINT('Ctrl Pts',(-2.82996921187404,3.52204995762946,23.9703107961279));
#41797=CARTESIAN_POINT('Ctrl Pts',(-2.24468461732448,3.99232647348976,23.9438534994434));
#41798=CARTESIAN_POINT('Ctrl Pts',(-1.53964219306833,4.31355788410714,23.917396202759));
#41799=CARTESIAN_POINT('Ctrl Pts',(-0.800715326097399,4.44661855917222,
23.8909389060745));
#41800=CARTESIAN_POINT('Ctrl Pts',(-0.0617884591264724,4.5796792342373,
23.86448160939));
#41801=CARTESIAN_POINT('Ctrl Pts',(0.711022850559258,4.5245691737501,23.8380243127056));
#41802=CARTESIAN_POINT('Ctrl Pts',(1.42359104075306,4.28800072211045,23.8115670160211));
#41803=CARTESIAN_POINT('Ctrl Pts',(2.13615923094691,4.05143227047079,23.7851097193366));
#41804=CARTESIAN_POINT('Ctrl Pts',(2.78848430164884,3.63340542767864,23.7586524226522));
#41805=CARTESIAN_POINT('Ctrl Pts',(3.30111378116074,3.08483540049647,23.7321951259677));
#41806=CARTESIAN_POINT('Ctrl Pts',(3.81374326067261,2.53626537331434,23.7057378292832));
#41807=CARTESIAN_POINT('Ctrl Pts',(4.18667714899447,1.85715216174218,23.6792805325988));
#41808=CARTESIAN_POINT('Ctrl Pts',(4.37449251133263,1.13021100344109,23.6528232359143));
#41809=CARTESIAN_POINT('Ctrl Pts',(4.46971107890219,0.761666625925485,23.6394099247735));
#41810=CARTESIAN_POINT('Ctrl Pts',(4.51734893340559,0.380829109202114,23.6259966136328));
#41811=CARTESIAN_POINT('Ctrl Pts',(4.51736327228765,-4.88489681080284E-6,
23.612583302492));
#41812=CARTESIAN_POINT('Origin',(0.,0.,20.5));
#41813=CARTESIAN_POINT('',(4.51802736372575,7.65320072124154E-5,22.612583302492));
#41814=CARTESIAN_POINT('',(4.51742427980126,-6.60698246896739E-5,22.8874166975081));
#41815=CARTESIAN_POINT('',(4.51775,5.53264807684796E-16,20.5));
#41816=CARTESIAN_POINT('Ctrl Pts',(4.51742427980126,-6.60698246896739E-5,
22.8874166975081));
#41817=CARTESIAN_POINT('Ctrl Pts',(4.51719087600353,0.450661745130009,22.9032923445115));
#41818=CARTESIAN_POINT('Ctrl Pts',(4.450158091451,0.901457458944964,22.9191679915148));
#41819=CARTESIAN_POINT('Ctrl Pts',(4.31734276296,1.3319583722546,22.9350436385182));
#41820=CARTESIAN_POINT('Ctrl Pts',(4.09600157608532,2.04940254217993,22.9615009352027));
#41821=CARTESIAN_POINT('Ctrl Pts',(3.69196031163168,2.71048127828687,22.9879582318872));
#41822=CARTESIAN_POINT('Ctrl Pts',(3.15443074594463,3.23467592132643,23.0144155285716));
#41823=CARTESIAN_POINT('Ctrl Pts',(2.61690118025762,3.75887056436596,23.0408728252561));
#41824=CARTESIAN_POINT('Ctrl Pts',(1.94588331333721,4.14618111433815,23.0673301219406));
#41825=CARTESIAN_POINT('Ctrl Pts',(1.22310638006181,4.34943357534335,23.093787418625));
#41826=CARTESIAN_POINT('Ctrl Pts',(0.500329446786407,4.55268603634856,23.1202447153095));
#41827=CARTESIAN_POINT('Ctrl Pts',(-0.274206552844009,4.5718804083868,23.146702011994));
#41828=CARTESIAN_POINT('Ctrl Pts',(-1.00616399197876,4.4046788379547,23.1731593086784));
#41829=CARTESIAN_POINT('Ctrl Pts',(-1.73812143111355,4.23747726752258,23.1996166053629));
#41830=CARTESIAN_POINT('Ctrl Pts',(-2.4275003097527,3.88387975462009,23.2260739020474));
#41831=CARTESIAN_POINT('Ctrl Pts',(-2.99033504306372,3.38695408510429,23.2525311987318));
#41832=CARTESIAN_POINT('Ctrl Pts',(-3.55316977637471,2.89002841558852,23.2789884954163));
#41833=CARTESIAN_POINT('Ctrl Pts',(-3.98946036435762,2.24977458945944,23.3054457921008));
#41834=CARTESIAN_POINT('Ctrl Pts',(-4.24606709644918,1.54417481408558,23.3319030887853));
#41835=CARTESIAN_POINT('Ctrl Pts',(-4.50267382854076,0.838575038711681,
23.3583603854697));
#41836=CARTESIAN_POINT('Ctrl Pts',(-4.57959670474098,0.0676293140930979,
23.3848176821541));
#41837=CARTESIAN_POINT('Ctrl Pts',(-4.46746660375748,-0.674762023707061,
23.4112749788386));
#41838=CARTESIAN_POINT('Ctrl Pts',(-4.35533650277398,-1.41715336150718,
23.4377322755231));
#41839=CARTESIAN_POINT('Ctrl Pts',(-4.05415342460676,-2.13099031248878,
23.4641895722076));
#41840=CARTESIAN_POINT('Ctrl Pts',(-3.60060113490302,-2.72932832606618,
23.4906468688921));
#41841=CARTESIAN_POINT('Ctrl Pts',(-3.14704884519929,-3.32766633964359,
23.5171041655765));
#41842=CARTESIAN_POINT('Ctrl Pts',(-2.54112734395902,-3.81050541581682,
23.543561462261));
#41843=CARTESIAN_POINT('Ctrl Pts',(-1.85663719941186,-4.11903628947138,
23.5700187589454));
#41844=CARTESIAN_POINT('Ctrl Pts',(-1.17214705486469,-4.42756716312594,
23.5964760556299));
#41845=CARTESIAN_POINT('Ctrl Pts',(-0.409088267010601,-4.56178983426184,
23.6229333523144));
#41846=CARTESIAN_POINT('Ctrl Pts',(0.339599448275288,-4.50535613008826,
23.6493906489989));
#41847=CARTESIAN_POINT('Ctrl Pts',(1.08828716356118,-4.44892242591468,23.6758479456834));
#41848=CARTESIAN_POINT('Ctrl Pts',(1.82260380627889,-4.20183234643162,23.7023052423678));
#41849=CARTESIAN_POINT('Ctrl Pts',(2.45311042204474,-3.7941811898551,23.7287625390522));
#41850=CARTESIAN_POINT('Ctrl Pts',(3.08361703781062,-3.38653003327857,23.7552198357367));
#41851=CARTESIAN_POINT('Ctrl Pts',(3.61031362662464,-2.81831779960855,23.7816771324212));
#41852=CARTESIAN_POINT('Ctrl Pts',(3.96904912687646,-2.15875211004929,23.8081344291057));
#41853=CARTESIAN_POINT('Ctrl Pts',(4.32737956599415,-1.49993115979256,23.8345618519065));
#41854=CARTESIAN_POINT('Ctrl Pts',(4.51812800419987,-0.749962938110063,
23.8609892747073));
#41855=CARTESIAN_POINT('Ctrl Pts',(4.51813695063288,9.0056284873609E-7,
23.8874166975081));
#41856=CARTESIAN_POINT('Ctrl Pts',(4.51736327228765,-4.88489681080284E-6,
23.612583302492));
#41857=CARTESIAN_POINT('Ctrl Pts',(4.51737721635919,-0.370352896766723,
23.5995393169483));
#41858=CARTESIAN_POINT('Ctrl Pts',(4.47235409625982,-0.740697577327283,
23.5864953314046));
#41859=CARTESIAN_POINT('Ctrl Pts',(4.38225454858748,-1.09973029228254,23.5734513458609));
#41860=CARTESIAN_POINT('Ctrl Pts',(4.19950438714968,-1.82796132467507,23.5469940491764));
#41861=CARTESIAN_POINT('Ctrl Pts',(3.83130722791959,-2.50965428443002,23.5205367524919));
#41862=CARTESIAN_POINT('Ctrl Pts',(3.3225090776327,-3.06177972318861,23.4940794558075));
#41863=CARTESIAN_POINT('Ctrl Pts',(2.81371092734586,-3.61390516194714,23.467622159123));
#41864=CARTESIAN_POINT('Ctrl Pts',(2.16431178600224,-4.03646307970933,23.4411648624385));
#41865=CARTESIAN_POINT('Ctrl Pts',(1.45340774986053,-4.27798639033802,23.4147075657541));
#41866=CARTESIAN_POINT('Ctrl Pts',(0.742503713718783,-4.51950970096672,
23.3882502690696));
#41867=CARTESIAN_POINT('Ctrl Pts',(-0.0299052172210591,-4.5799984044619,
23.3617929723851));
#41868=CARTESIAN_POINT('Ctrl Pts',(-0.769740489176251,-4.4520850425719,
23.3353356757007));
#41869=CARTESIAN_POINT('Ctrl Pts',(-1.50957576113144,-4.32417168068191,
23.3088783790162));
#41870=CARTESIAN_POINT('Ctrl Pts',(-2.21683737410199,-4.00785625340675,
23.2824210823318));
#41871=CARTESIAN_POINT('Ctrl Pts',(-2.80538164796902,-3.54166563180954,
23.2559637856473));
#41872=CARTESIAN_POINT('Ctrl Pts',(-3.39392592183609,-3.0754750102123,23.2295064889628));
#41873=CARTESIAN_POINT('Ctrl Pts',(-3.86375285659963,-2.459409194293,23.2030491922783));
#41874=CARTESIAN_POINT('Ctrl Pts',(-4.15763804857074,-1.76850431465145,
23.1765918955939));
#41875=CARTESIAN_POINT('Ctrl Pts',(-4.45152324054182,-1.07759943500997,
23.1501345989094));
#41876=CARTESIAN_POINT('Ctrl Pts',(-4.56946668972051,-0.311855491646258,
23.123677302225));
#41877=CARTESIAN_POINT('Ctrl Pts',(-4.49710302020607,0.435460743133651,
23.0972200055405));
#41878=CARTESIAN_POINT('Ctrl Pts',(-4.42473935069162,1.18277697791365,23.070762708856));
#41879=CARTESIAN_POINT('Ctrl Pts',(-4.162068562484,1.91166550410983,23.0443054121715));
#41880=CARTESIAN_POINT('Ctrl Pts',(-3.74108365616062,2.53334852003347,23.017848115487));
#41881=CARTESIAN_POINT('Ctrl Pts',(-3.32009874983724,3.15503153595711,22.9913908188026));
#41882=CARTESIAN_POINT('Ctrl Pts',(-2.74079972539808,3.66950904160819,22.9649335221181));
#41883=CARTESIAN_POINT('Ctrl Pts',(-2.07374458313369,4.01411821952858,22.9384762254337));
#41884=CARTESIAN_POINT('Ctrl Pts',(-1.40668944086933,4.35872739744894,22.9120189287492));
#41885=CARTESIAN_POINT('Ctrl Pts',(-0.651878180779734,4.53346824763863,
22.8855616320647));
#41886=CARTESIAN_POINT('Ctrl Pts',(0.0987540592506666,4.51705757827173,
22.8591043353802));
#41887=CARTESIAN_POINT('Ctrl Pts',(0.849386299281067,4.50064690890482,22.8326470386958));
#41888=CARTESIAN_POINT('Ctrl Pts',(1.59583951925228,4.29308471998132,22.8061897420113));
#41889=CARTESIAN_POINT('Ctrl Pts',(2.24719647092532,3.91965176135188,22.7797324453269));
#41890=CARTESIAN_POINT('Ctrl Pts',(2.89855342259837,3.54621880272245,22.7532751486424));
#41891=CARTESIAN_POINT('Ctrl Pts',(3.45481410597325,3.00691507438708,22.7268178519579));
#41892=CARTESIAN_POINT('Ctrl Pts',(3.8482267217168,2.3674273530564,22.7003605552734));
#41893=CARTESIAN_POINT('Ctrl Pts',(4.24163933746037,1.72793963172568,22.673903258589));
#41894=CARTESIAN_POINT('Ctrl Pts',(4.47220388557259,0.988267917399649,22.6474459619045));
#41895=CARTESIAN_POINT('Ctrl Pts',(4.51183760195935,0.238503067401548,22.6209886652201));
#41896=CARTESIAN_POINT('Ctrl Pts',(4.51603475238966,0.159104107382582,22.618186877644));
#41897=CARTESIAN_POINT('Ctrl Pts',(4.51809071117569,0.0795919580082339,
22.615385090068));
#41898=CARTESIAN_POINT('Ctrl Pts',(4.51802736372575,7.65320072124154E-5,
22.612583302492));
#41899=CARTESIAN_POINT('Origin',(0.,0.,20.5));
#41900=CARTESIAN_POINT('',(4.51732076945549,-0.00048196737157627,21.612583302492));
#41901=CARTESIAN_POINT('',(4.51782520267197,0.000113471772791779,21.8874166975081));
#41902=CARTESIAN_POINT('',(4.51775,5.53264807684796E-16,20.5));
#41903=CARTESIAN_POINT('Ctrl Pts',(4.51782520267197,0.000113471772791779,
21.8874166975081));
#41904=CARTESIAN_POINT('Ctrl Pts',(4.51797972979194,0.149530198200455,21.8926808209467));
#41905=CARTESIAN_POINT('Ctrl Pts',(4.51071347097486,0.298931999583376,21.8979449443854));
#41906=CARTESIAN_POINT('Ctrl Pts',(4.49591510340165,0.447583892947329,21.903209067824));
#41907=CARTESIAN_POINT('Ctrl Pts',(4.4215390356869,1.19470300808371,21.9296663645084));
#41908=CARTESIAN_POINT('Ctrl Pts',(4.15689950898611,1.92287920852908,21.9561236611929));
#41909=CARTESIAN_POINT('Ctrl Pts',(3.73423901960025,2.54342464869698,21.9825809578774));
#41910=CARTESIAN_POINT('Ctrl Pts',(3.3115785302144,3.16397008886483,22.0090382545618));
#41911=CARTESIAN_POINT('Ctrl Pts',(2.7308970781435,3.67688476875521,22.0354955512463));
#41912=CARTESIAN_POINT('Ctrl Pts',(2.06291588716907,4.0196945481291,22.0619528479308));
#41913=CARTESIAN_POINT('Ctrl Pts',(1.39493469619467,4.36250432750298,22.0884101446153));
#41914=CARTESIAN_POINT('Ctrl Pts',(0.639653766316767,4.53520920636039,22.1148674412997));
#41915=CARTESIAN_POINT('Ctrl Pts',(-0.110931801888053,4.51677482186132,
22.1413247379842));
#41916=CARTESIAN_POINT('Ctrl Pts',(-0.861517370093001,4.49834043736225,
22.1677820346687));
#41917=CARTESIAN_POINT('Ctrl Pts',(-1.60740757662484,4.28876678950664,22.1942393313531));
#41918=CARTESIAN_POINT('Ctrl Pts',(-2.25775525993264,3.91357923987666,22.2206966280376));
#41919=CARTESIAN_POINT('Ctrl Pts',(-2.90810294324037,3.53839169024672,22.2471539247221));
#41920=CARTESIAN_POINT('Ctrl Pts',(-3.46290810332406,2.99759023884246,22.2736112214065));
#41921=CARTESIAN_POINT('Ctrl Pts',(-3.85459532302061,2.35704415643024,22.300068518091));
#41922=CARTESIAN_POINT('Ctrl Pts',(-4.24628254271713,1.71649807401806,22.3265258147755));
#41923=CARTESIAN_POINT('Ctrl Pts',(-4.4748518220265,0.976207360597959,22.3529831114599));
#41924=CARTESIAN_POINT('Ctrl Pts',(-4.51246407961468,0.226338472032797,
22.3794404081444));
#41925=CARTESIAN_POINT('Ctrl Pts',(-4.55007633720287,-0.523530416532452,
22.4058977048289));
#41926=CARTESIAN_POINT('Ctrl Pts',(-4.39673157306978,-1.28297748024285,
22.4323550015133));
#41927=CARTESIAN_POINT('Ctrl Pts',(-4.07110679585725,-1.95950283641873,
22.4588122981978));
#41928=CARTESIAN_POINT('Ctrl Pts',(-3.74548201864475,-2.63602819259453,
22.4852695948823));
#41929=CARTESIAN_POINT('Ctrl Pts',(-3.24757722835284,-3.22963184123592,
22.5117268915668));
#41930=CARTESIAN_POINT('Ctrl Pts',(-2.63803679068419,-3.66801355240642,
22.5381841882512));
#41931=CARTESIAN_POINT('Ctrl Pts',(-2.02849635301547,-4.10639526357697,
22.5646414849357));
#41932=CARTESIAN_POINT('Ctrl Pts',(-1.30732026797,-4.38955503727659,22.5910987816201));
#41933=CARTESIAN_POINT('Ctrl Pts',(-0.562346924558367,-4.48300430658586,
22.6175560783046));
#41934=CARTESIAN_POINT('Ctrl Pts',(0.182626418853268,-4.57645357589513,
22.6440133749891));
#41935=CARTESIAN_POINT('Ctrl Pts',(0.951397020631046,-4.48019234081406,
22.6704706716736));
#41936=CARTESIAN_POINT('Ctrl Pts',(1.65032944052472,-4.20594512376056,22.696927968358));
#41937=CARTESIAN_POINT('Ctrl Pts',(2.34926186041832,-3.93169790670708,22.7233852650425));
#41938=CARTESIAN_POINT('Ctrl Pts',(2.97835609842781,-3.47946470768123,22.749842561727));
#41939=CARTESIAN_POINT('Ctrl Pts',(3.46098918943069,-2.90432702425209,22.7762998584114));
#41940=CARTESIAN_POINT('Ctrl Pts',(3.94362228043359,-2.32918934082292,22.8027571550959));
#41941=CARTESIAN_POINT('Ctrl Pts',(4.27979422442984,-1.63114717299047,22.8292144517804));
#41942=CARTESIAN_POINT('Ctrl Pts',(4.42855964178011,-0.89522128720241,22.8556717484648));
#41943=CARTESIAN_POINT('Ctrl Pts',(4.48805867336429,-0.600886230695128,
22.8662533981459));
#41944=CARTESIAN_POINT('Ctrl Pts',(4.51757985123852,-0.300491232865703,
22.876835047827));
#41945=CARTESIAN_POINT('Ctrl Pts',(4.51742427980126,-6.60698246896739E-5,
22.8874166975081));
#41946=CARTESIAN_POINT('Ctrl Pts',(4.51802736372575,7.65320072124154E-5,
22.612583302492));
#41947=CARTESIAN_POINT('Ctrl Pts',(4.51749252083047,-0.671272680948583,
22.5889277933835));
#41948=CARTESIAN_POINT('Ctrl Pts',(4.36588431242158,-1.34285546610394,22.5652722842751));
#41949=CARTESIAN_POINT('Ctrl Pts',(4.07637456299432,-1.94852038806885,22.5416167751666));
#41950=CARTESIAN_POINT('Ctrl Pts',(3.75257492298122,-2.62592100787102,22.5151594784822));
#41951=CARTESIAN_POINT('Ctrl Pts',(3.2562727582937,-3.22086426180528,22.4887021817977));
#41952=CARTESIAN_POINT('Ctrl Pts',(2.64791620593777,-3.66088792814019,22.4622448851133));
#41953=CARTESIAN_POINT('Ctrl Pts',(2.03955965358178,-4.10091159447515,22.4357875884288));
#41954=CARTESIAN_POINT('Ctrl Pts',(1.31914871355735,-4.38601567321071,22.4093302917443));
#41955=CARTESIAN_POINT('Ctrl Pts',(0.574430373257849,-4.48147252184727,
22.3828729950598));
#41956=CARTESIAN_POINT('Ctrl Pts',(-0.17028796704161,-4.57692937048383,
22.3564156983754));
#41957=CARTESIAN_POINT('Ctrl Pts',(-0.939313707616121,-4.48273898902142,
22.3299584016909));
#41958=CARTESIAN_POINT('Ctrl Pts',(-1.63898363511379,-4.21037796912979,
22.3035011050064));
#41959=CARTESIAN_POINT('Ctrl Pts',(-2.33865356261146,-3.93801694923817,
22.277043808322));
#41960=CARTESIAN_POINT('Ctrl Pts',(-2.96896767703227,-3.48748529091735,
22.2505865116375));
#41961=CARTESIAN_POINT('Ctrl Pts',(-3.4531482409959,-2.91364911818973,22.224129214953));
#41962=CARTESIAN_POINT('Ctrl Pts',(-3.93732880495957,-2.33981294546208,
22.1976719182685));
#41963=CARTESIAN_POINT('Ctrl Pts',(-4.27537581846602,-1.64267225832765,
22.1712146215841));
#41964=CARTESIAN_POINT('Ctrl Pts',(-4.42612719062429,-0.907153378338295,
22.1447573248996));
#41965=CARTESIAN_POINT('Ctrl Pts',(-4.57687856278254,-0.171634498348981,
22.1183000282152));
#41966=CARTESIAN_POINT('Ctrl Pts',(-4.5403342935926,0.602262574495347,22.0918427315307));
#41967=CARTESIAN_POINT('Ctrl Pts',(-4.32092341583129,1.32030703112007,22.0653854348462));
#41968=CARTESIAN_POINT('Ctrl Pts',(-4.10151253806998,2.03835148774475,22.0389281381617));
#41969=CARTESIAN_POINT('Ctrl Pts',(-3.69923505173734,2.70054332814993,22.0124708414773));
#41970=CARTESIAN_POINT('Ctrl Pts',(-3.16312948534619,3.2261735651419,21.9860135447928));
#41971=CARTESIAN_POINT('Ctrl Pts',(-2.62702391895502,3.7518038021339,21.9595562481083));
#41972=CARTESIAN_POINT('Ctrl Pts',(-1.95709027250536,4.14087243571266,21.9330989514239));
#41973=CARTESIAN_POINT('Ctrl Pts',(-1.23484721910289,4.34609472311248,21.9066416547394));
#41974=CARTESIAN_POINT('Ctrl Pts',(-0.512604165700429,4.5513170105123,21.880184358055));
#41975=CARTESIAN_POINT('Ctrl Pts',(0.261948294654812,4.57269295173318,21.8537270613705));
#41976=CARTESIAN_POINT('Ctrl Pts',(0.994322299916156,4.40742376897541,21.827269764686));
#41977=CARTESIAN_POINT('Ctrl Pts',(1.72669630517754,4.24215458621763,21.8008124680015));
#41978=CARTESIAN_POINT('Ctrl Pts',(2.41689185534501,3.89024027948119,21.7743551713171));
#41979=CARTESIAN_POINT('Ctrl Pts',(2.9811237744369,3.39491220205643,21.7478978746326));
#41980=CARTESIAN_POINT('Ctrl Pts',(3.54535569352876,2.8995841246317,21.7214405779481));
#41981=CARTESIAN_POINT('Ctrl Pts',(3.98362398154505,2.26084227651867,21.6949832812637));
#41982=CARTESIAN_POINT('Ctrl Pts',(4.24201965646871,1.55578891217676,21.6685259845792));
#41983=CARTESIAN_POINT('Ctrl Pts',(4.42414140114732,1.05885509606931,21.6498784238835));
#41984=CARTESIAN_POINT('Ctrl Pts',(4.51690828804801,0.528979877711725,21.6312308631877));
#41985=CARTESIAN_POINT('Ctrl Pts',(4.51732076945549,-0.00048196737157627,
21.612583302492));
#41986=CARTESIAN_POINT('Origin',(0.,0.,20.5));
#41987=CARTESIAN_POINT('',(4.52133925202235,0.00376432143610439,20.612583302492));
#41988=CARTESIAN_POINT('',(4.50983715083838,-0.000439487622834945,20.8874166975081));
#41989=CARTESIAN_POINT('',(4.51775,5.53264807684796E-16,20.5));
#41990=CARTESIAN_POINT('Ctrl Pts',(4.50983715083838,-0.000439487622834945,
20.8874166975081));
#41991=CARTESIAN_POINT('Ctrl Pts',(4.51223989494407,0.600272225419278,20.9085265940664));
#41992=CARTESIAN_POINT('Ctrl Pts',(4.40045147683232,1.20075832380094,20.9296364906248));
#41993=CARTESIAN_POINT('Ctrl Pts',(4.16995632188889,1.7527710518725,20.9507463871831));
#41994=CARTESIAN_POINT('Ctrl Pts',(3.88107386896856,2.44461548985082,20.9772036838676));
#41995=CARTESIAN_POINT('Ctrl Pts',(3.40572780474968,3.06031833788172,21.0036609805521));
#41996=CARTESIAN_POINT('Ctrl Pts',(2.81753981467946,3.528620768205,21.0301182772365));
#41997=CARTESIAN_POINT('Ctrl Pts',(2.22935182460931,3.99692319852822,21.056575573921));
#41998=CARTESIAN_POINT('Ctrl Pts',(1.52832190868785,4.31782521114387,21.0830328706055));
#41999=CARTESIAN_POINT('Ctrl Pts',(0.790149843231595,4.44924273175288,21.1094901672899));
#42000=CARTESIAN_POINT('Ctrl Pts',(0.051977777775257,4.58066025236192,21.1359474639744));
#42001=CARTESIAN_POINT('Ctrl Pts',(-0.723336437215882,4.52259328096428,
21.1624047606589));
#42002=CARTESIAN_POINT('Ctrl Pts',(-1.43588412720356,4.28390166798379,21.1888620573433));
#42003=CARTESIAN_POINT('Ctrl Pts',(-2.14843181719121,4.04521005500332,21.2153193540278));
#42004=CARTESIAN_POINT('Ctrl Pts',(-2.7982129821754,3.62589380044002,21.2417766507123));
#42005=CARTESIAN_POINT('Ctrl Pts',(-3.30902952393807,3.07605344225317,21.2682339473967));
#42006=CARTESIAN_POINT('Ctrl Pts',(-3.81984606570073,2.52621308406631,21.2946912440812));
#42007=CARTESIAN_POINT('Ctrl Pts',(-4.19169798424187,1.84584862225589,21.3211485407657));
#42008=CARTESIAN_POINT('Ctrl Pts',(-4.37772925931563,1.11834540158705,21.3476058374502));
#42009=CARTESIAN_POINT('Ctrl Pts',(-4.56376053438938,0.390842180918212,
21.3740631341346));
#42010=CARTESIAN_POINT('Ctrl Pts',(-4.56397116599575,-0.383799798609046,
21.4005204308191));
#42011=CARTESIAN_POINT('Ctrl Pts',(-4.37916492462626,-1.11150455739398,
21.4269777275035));
#42012=CARTESIAN_POINT('Ctrl Pts',(-4.19435868325677,-1.83920931617892,
21.453435024188));
#42013=CARTESIAN_POINT('Ctrl Pts',(-3.82453556891143,-2.51997685422154,
21.4798923208725));
#42014=CARTESIAN_POINT('Ctrl Pts',(-3.31430027943462,-3.07074498667336,
21.5063496175569));
#42015=CARTESIAN_POINT('Ctrl Pts',(-2.80406498995777,-3.62151311912521,
21.5328069142414));
#42016=CARTESIAN_POINT('Ctrl Pts',(-2.15341752534944,-4.04228184598626,
21.5592642109259));
#42017=CARTESIAN_POINT('Ctrl Pts',(-1.44183871719702,-4.28187903967218,
21.5857215076104));
#42018=CARTESIAN_POINT('Ctrl Pts',(-0.730259909044641,-4.5214762333581,
21.6121788042948));
#42019=CARTESIAN_POINT('Ctrl Pts',(0.0422502426518133,-4.57990189386891,
21.6386361009793));
#42020=CARTESIAN_POINT('Ctrl Pts',(0.781724091400323,-4.44999904027082,
21.6650933976638));
#42021=CARTESIAN_POINT('Ctrl Pts',(1.52119794014883,-4.32009618667273,21.6915506943482));
#42022=CARTESIAN_POINT('Ctrl Pts',(2.2276354859494,-4.00186481896572,21.7180079910327));
#42023=CARTESIAN_POINT('Ctrl Pts',(2.81492815165366,-3.53408677354305,21.7444652877172));
#42024=CARTESIAN_POINT('Ctrl Pts',(3.40222081735796,-3.06630872812035,21.7709225844016));
#42025=CARTESIAN_POINT('Ctrl Pts',(3.87036860296593,-2.44898400498197,21.7973798810861));
#42026=CARTESIAN_POINT('Ctrl Pts',(4.16238619140555,-1.75729062849908,21.8238371777706));
#42027=CARTESIAN_POINT('Ctrl Pts',(4.39630197715038,-1.20322126398217,21.8450303510164));
#42028=CARTESIAN_POINT('Ctrl Pts',(4.51720308199739,-0.601432940640185,
21.8662235242623));
#42029=CARTESIAN_POINT('Ctrl Pts',(4.51782520267197,0.000113471772791779,
21.8874166975081));
#42030=CARTESIAN_POINT('Ctrl Pts',(4.51732076945549,-0.00048196737157627,
21.612583302492));
#42031=CARTESIAN_POINT('Ctrl Pts',(4.51749351971195,-0.222224494111391,
21.6047735665033));
#42032=CARTESIAN_POINT('Ctrl Pts',(4.50146734240306,-0.44389451533626,21.5969638305145));
#42033=CARTESIAN_POINT('Ctrl Pts',(4.46902189478939,-0.663041834113329,
21.5891540945258));
#42034=CARTESIAN_POINT('Ctrl Pts',(4.35910539635538,-1.40545433549076,21.5626967978413));
#42035=CARTESIAN_POINT('Ctrl Pts',(4.06074933765633,-2.11891445767478,21.5362395011569));
#42036=CARTESIAN_POINT('Ctrl Pts',(3.60841564297682,-2.71899122382358,21.5097822044724));
#42037=CARTESIAN_POINT('Ctrl Pts',(3.15608194829734,-3.31906798997234,21.4833249077879));
#42038=CARTESIAN_POINT('Ctrl Pts',(2.54977061763742,-3.80576140008588,21.4568676111035));
#42039=CARTESIAN_POINT('Ctrl Pts',(1.86683275295722,-4.11521969441498,21.430410314419));
#42040=CARTESIAN_POINT('Ctrl Pts',(1.18389488827701,-4.42467798874409,21.4039530177345));
#42041=CARTESIAN_POINT('Ctrl Pts',(0.424330489576522,-4.55690116728877,
21.37749572105));
#42042=CARTESIAN_POINT('Ctrl Pts',(-0.325633495564533,-4.50373822059831,
21.3510384243656));
#42043=CARTESIAN_POINT('Ctrl Pts',(-1.07559748070559,-4.45057527390784,
21.3245811276811));
#42044=CARTESIAN_POINT('Ctrl Pts',(-1.81596105228721,-4.21202620198225,
21.2981238309967));
#42045=CARTESIAN_POINT('Ctrl Pts',(-2.44569775560519,-3.80516814017082,
21.2716665343122));
#42046=CARTESIAN_POINT('Ctrl Pts',(-3.70517116224116,-2.99145201654798,
21.2187519409433));
#42047=CARTESIAN_POINT('Ctrl Pts',(-4.52213709582257,-1.50449993338184,
21.1658373475743));
#42048=CARTESIAN_POINT('Ctrl Pts',(-4.5251392293927,-0.0110172863203392,
21.1129227542054));
#42049=CARTESIAN_POINT('Ctrl Pts',(-4.52814136296284,1.4824653607412,21.0600081608364));
#42050=CARTESIAN_POINT('Ctrl Pts',(-3.71717969652165,2.98247857169809,21.0070935674675));
#42051=CARTESIAN_POINT('Ctrl Pts',(-2.46290199004371,3.79700220422752,20.9541789740986));
#42052=CARTESIAN_POINT('Ctrl Pts',(-1.20862428356581,4.61152583675692,20.9012643807296));
#42053=CARTESIAN_POINT('Ctrl Pts',(0.488969462948824,4.7405598908589,20.8483497873607));
#42054=CARTESIAN_POINT('Ctrl Pts',(1.85305394748095,4.12790602103174,20.7954351939918));
#42055=CARTESIAN_POINT('Ctrl Pts',(3.21713843201311,3.51525215120457,20.7425206006228));
#42056=CARTESIAN_POINT('Ctrl Pts',(4.24771365456276,2.16091035744822,20.6896060072539));
#42057=CARTESIAN_POINT('Ctrl Pts',(4.47332054780559,0.68305737845925,20.636691413885));
#42058=CARTESIAN_POINT('Ctrl Pts',(4.5075830310957,0.458618699879782,20.628655376754));
#42059=CARTESIAN_POINT('Ctrl Pts',(4.52327979691323,0.231331370382945,20.620619339623));
#42060=CARTESIAN_POINT('Ctrl Pts',(4.52133925202235,0.00376432143610439,
20.612583302492));
#42061=CARTESIAN_POINT('Origin',(0.,0.,20.5));
#42062=CARTESIAN_POINT('',(4.51048356578783,0.00141370502139415,19.612583302492));
#42063=CARTESIAN_POINT('',(4.51474283421141,-0.0038924084009401,19.8874166975081));
#42064=CARTESIAN_POINT('',(4.51775,5.53264807684796E-16,20.5));
#42065=CARTESIAN_POINT('Ctrl Pts',(4.51474283421141,-0.00389240840094011,
19.8874166975081));
#42066=CARTESIAN_POINT('Ctrl Pts',(4.50621483686762,1.04654996357473,19.9243723671861));
#42067=CARTESIAN_POINT('Ctrl Pts',(4.14085607956887,2.10234645737149,19.9613280368642));
#42068=CARTESIAN_POINT('Ctrl Pts',(3.4708839066554,2.90334883526624,19.9982837065423));
#42069=CARTESIAN_POINT('Ctrl Pts',(2.51159118088301,4.05025580469952,20.0511982999112));
#42070=CARTESIAN_POINT('Ctrl Pts',(0.927790752426727,4.6747928461432,20.1041128932802));
#42071=CARTESIAN_POINT('Ctrl Pts',(-0.556105607180406,4.49092827001162,
20.1570274866491));
#42072=CARTESIAN_POINT('Ctrl Pts',(-2.04000196678754,4.30706369388004,20.209942080018));
#42073=CARTESIAN_POINT('Ctrl Pts',(-3.42399425754553,3.3147975001732,20.262856673387));
#42074=CARTESIAN_POINT('Ctrl Pts',(-4.07445610293379,1.9687487323051,20.3157712667559));
#42075=CARTESIAN_POINT('Ctrl Pts',(-4.72491794832207,0.622699964436965,
20.3686858601248));
#42076=CARTESIAN_POINT('Ctrl Pts',(-4.64184934834058,-1.07713137759245,
20.4216004534938));
#42077=CARTESIAN_POINT('Ctrl Pts',(-3.86404219126196,-2.3542716484918,20.4745150468627));
#42078=CARTESIAN_POINT('Ctrl Pts',(-3.08623503418336,-3.63141191939111,
20.5274296402316));
#42079=CARTESIAN_POINT('Ctrl Pts',(-1.61368932000766,-4.48586111916038,
20.5803442336006));
#42080=CARTESIAN_POINT('Ctrl Pts',(-0.118635503777389,-4.52427204848619,
20.6332588269695));
#42081=CARTESIAN_POINT('Ctrl Pts',(1.37641831245292,-4.56268297781199,20.6861734203384));
#42082=CARTESIAN_POINT('Ctrl Pts',(2.89398023073781,-3.78505563669429,20.7390880137074));
#42083=CARTESIAN_POINT('Ctrl Pts',(3.73680595955696,-2.55211434826229,20.7920026070763));
#42084=CARTESIAN_POINT('Ctrl Pts',(4.24339242394412,-1.81104612176332,20.8238073038869));
#42085=CARTESIAN_POINT('Ctrl Pts',(4.50621711662441,-0.905486741220779,
20.8556120006975));
#42086=CARTESIAN_POINT('Ctrl Pts',(4.50983715083838,-0.000439487622834945,
20.8874166975081));
#42087=CARTESIAN_POINT('Ctrl Pts',(4.52133925202235,0.00376432143610439,
20.612583302492));
#42088=CARTESIAN_POINT('Ctrl Pts',(4.51050196349347,-1.26712087204873,20.567704746254));
#42089=CARTESIAN_POINT('Ctrl Pts',(3.94958417430038,-2.54673008347757,20.5228261900161));
#42090=CARTESIAN_POINT('Ctrl Pts',(3.00029299713898,-3.38761451526673,20.4779476337781));
#42091=CARTESIAN_POINT('Ctrl Pts',(1.88101998929342,-4.37906926578227,20.4250330404092));
#42092=CARTESIAN_POINT('Ctrl Pts',(0.221835409666229,-4.76061460259175,
20.3721184470403));
#42093=CARTESIAN_POINT('Ctrl Pts',(-1.21815646492133,-4.35804593593179,
20.3192038536714));
#42094=CARTESIAN_POINT('Ctrl Pts',(-2.65814833950885,-3.95547726927185,
20.2662892603024));
#42095=CARTESIAN_POINT('Ctrl Pts',(-3.87894750905677,-2.76879459914251,
20.2133746669335));
#42096=CARTESIAN_POINT('Ctrl Pts',(-4.32195458228653,-1.34081481536639,
20.1604600735645));
#42097=CARTESIAN_POINT('Ctrl Pts',(-4.76496165551631,0.0871649684097867,
20.1075454801956));
#42098=CARTESIAN_POINT('Ctrl Pts',(-4.43017663242789,1.75644186583272,20.0546308868267));
#42099=CARTESIAN_POINT('Ctrl Pts',(-3.47088390665552,2.90334883526609,20.0017162934577));
#42100=CARTESIAN_POINT('Ctrl Pts',(-2.51159118088318,4.05025580469941,19.9488017000888));
#42101=CARTESIAN_POINT('Ctrl Pts',(-0.927790752426926,4.67479284614316,
19.8958871067198));
#42102=CARTESIAN_POINT('Ctrl Pts',(0.556105607180211,4.49092827001165,19.8429725133509));
#42103=CARTESIAN_POINT('Ctrl Pts',(2.04000196678735,4.30706369388013,19.790057919982));
#42104=CARTESIAN_POINT('Ctrl Pts',(3.42399425754539,3.31479750017334,19.737143326613));
#42105=CARTESIAN_POINT('Ctrl Pts',(4.07445610293371,1.96874873230528,19.6842287332441));
#42106=CARTESIAN_POINT('Ctrl Pts',(4.36802741054216,1.36123992961467,19.6603469229934));
#42107=CARTESIAN_POINT('Ctrl Pts',(4.51218113590681,0.681666855829588,19.6364651127427));
#42108=CARTESIAN_POINT('Ctrl Pts',(4.51048356578783,0.00141370502139415,
19.612583302492));
#42109=CARTESIAN_POINT('Origin',(0.,0.,20.5));
#42110=CARTESIAN_POINT('',(4.51751172608841,-5.0340792907555E-5,18.612583302492));
#42111=CARTESIAN_POINT('',(4.52514732618828,-0.0014363825736758,18.8874166975081));
#42112=CARTESIAN_POINT('',(4.51775,5.53264807684796E-16,20.5));
#42113=CARTESIAN_POINT('Ctrl Pts',(4.52514732618828,-0.0014363825736758,
18.8874166975081));
#42114=CARTESIAN_POINT('Ctrl Pts',(4.52467107616349,1.48887736965158,18.9402181403059));
#42115=CARTESIAN_POINT('Ctrl Pts',(3.71449759637046,2.98422031831989,18.9930195831037));
#42116=CARTESIAN_POINT('Ctrl Pts',(2.46290199004355,3.79700220422763,19.0458210259014));
#42117=CARTESIAN_POINT('Ctrl Pts',(1.20862428356557,4.611525836757,19.0987356192704));
#42118=CARTESIAN_POINT('Ctrl Pts',(-0.488969462949119,4.74055989085888,
19.1516502126393));
#42119=CARTESIAN_POINT('Ctrl Pts',(-1.85305394748124,4.12790602103161,19.2045648060083));
#42120=CARTESIAN_POINT('Ctrl Pts',(-3.21713843201331,3.51525215120436,19.2574793993772));
#42121=CARTESIAN_POINT('Ctrl Pts',(-4.24771365456286,2.16091035744797,19.3103939927461));
#42122=CARTESIAN_POINT('Ctrl Pts',(-4.47332054780562,0.683057378459056,
19.3633085861151));
#42123=CARTESIAN_POINT('Ctrl Pts',(-4.69892744104839,-0.794795600529883,
19.416223179484));
#42124=CARTESIAN_POINT('Ctrl Pts',(-4.1195660049844,-2.3961597647514,19.4691377728529));
#42125=CARTESIAN_POINT('Ctrl Pts',(-3.00029299713883,-3.38761451526686,
19.5220523662219));
#42126=CARTESIAN_POINT('Ctrl Pts',(-1.8810199892932,-4.37906926578239,19.5749669595908));
#42127=CARTESIAN_POINT('Ctrl Pts',(-0.221835409665938,-4.76061460259178,
19.6278815529597));
#42128=CARTESIAN_POINT('Ctrl Pts',(1.21815646492164,-4.35804593593171,19.6807961463287));
#42129=CARTESIAN_POINT('Ctrl Pts',(2.6581483395091,-3.95547726927166,19.7337107396976));
#42130=CARTESIAN_POINT('Ctrl Pts',(3.8789475090569,-2.76879459914231,19.7866253330665));
#42131=CARTESIAN_POINT('Ctrl Pts',(4.32195458228659,-1.3408148153662,19.8395399264355));
#42132=CARTESIAN_POINT('Ctrl Pts',(4.45556453043254,-0.910139288059504,
19.8554988501263));
#42133=CARTESIAN_POINT('Ctrl Pts',(4.51842556165299,-0.457515081242471,
19.8714577738172));
#42134=CARTESIAN_POINT('Ctrl Pts',(4.51474283421141,-0.00389240840094011,
19.8874166975081));
#42135=CARTESIAN_POINT('Ctrl Pts',(4.51048356578783,0.00141370502139415,
19.612583302492));
#42136=CARTESIAN_POINT('Ctrl Pts',(4.50841985350745,-0.825560548001291,
19.5835505193738));
#42137=CARTESIAN_POINT('Ctrl Pts',(4.29080360170741,-1.65353988177363,19.5545177362555));
#42138=CARTESIAN_POINT('Ctrl Pts',(3.86404219126206,-2.35427164849163,19.5254849531373));
#42139=CARTESIAN_POINT('Ctrl Pts',(3.08623503418352,-3.63141191939097,19.4725703597684));
#42140=CARTESIAN_POINT('Ctrl Pts',(1.61368932000785,-4.48586111916031,19.4196557663994));
#42141=CARTESIAN_POINT('Ctrl Pts',(0.118635503777585,-4.52427204848618,
19.3667411730305));
#42142=CARTESIAN_POINT('Ctrl Pts',(-1.37641831245272,-4.56268297781205,
19.3138265796616));
#42143=CARTESIAN_POINT('Ctrl Pts',(-2.89398023073765,-3.78505563669441,
19.2609119862926));
#42144=CARTESIAN_POINT('Ctrl Pts',(-3.73680595955685,-2.55211434826245,
19.2079973929237));
#42145=CARTESIAN_POINT('Ctrl Pts',(-4.57963168837605,-1.3191730598305,19.1550827995547));
#42146=CARTESIAN_POINT('Ctrl Pts',(-4.74772122772955,0.369082175915713,
19.1021682061858));
#42147=CARTESIAN_POINT('Ctrl Pts',(-4.16995632188897,1.75277105187232,19.0492536128169));
#42148=CARTESIAN_POINT('Ctrl Pts',(-3.88107386896868,2.44461548985061,19.0227963161324));
#42149=CARTESIAN_POINT('Ctrl Pts',(-3.40572780474986,3.0603183378815,18.9963390194479));
#42150=CARTESIAN_POINT('Ctrl Pts',(-2.81753981467971,3.5286207682048,18.9698817227635));
#42151=CARTESIAN_POINT('Ctrl Pts',(-2.22935182460953,3.99692319852811,18.943424426079));
#42152=CARTESIAN_POINT('Ctrl Pts',(-1.52832190868799,4.31782521114383,18.9169671293945));
#42153=CARTESIAN_POINT('Ctrl Pts',(-0.790149843231659,4.44924273175287,
18.8905098327101));
#42154=CARTESIAN_POINT('Ctrl Pts',(-0.0519777777753676,4.58066025236191,
18.8640525360256));
#42155=CARTESIAN_POINT('Ctrl Pts',(0.72333643721573,4.5225932809643,18.8375952393411));
#42156=CARTESIAN_POINT('Ctrl Pts',(1.43588412720338,4.28390166798386,18.8111379426567));
#42157=CARTESIAN_POINT('Ctrl Pts',(2.14843181719103,4.04521005500342,18.7846806459722));
#42158=CARTESIAN_POINT('Ctrl Pts',(2.79821298217524,3.62589380044014,18.7582233492877));
#42159=CARTESIAN_POINT('Ctrl Pts',(3.30902952393793,3.07605344225331,18.7317660526033));
#42160=CARTESIAN_POINT('Ctrl Pts',(3.81984606570062,2.52621308406647,18.7053087559188));
#42161=CARTESIAN_POINT('Ctrl Pts',(4.19169798424179,1.84584862225607,18.6788514592343));
#42162=CARTESIAN_POINT('Ctrl Pts',(4.37772925931557,1.11834540158724,18.6523941625499));
#42163=CARTESIAN_POINT('Ctrl Pts',(4.47103767181987,0.753448850803234,18.6391238758639));
#42164=CARTESIAN_POINT('Ctrl Pts',(4.51759801973486,0.3766933068382,18.625853589178));
#42165=CARTESIAN_POINT('Ctrl Pts',(4.51751172608841,-5.0340792907555E-5,
18.612583302492));
#42166=CARTESIAN_POINT('Origin',(0.,0.,20.5));
#42167=CARTESIAN_POINT('',(4.51803700570725,7.32895604327321E-5,17.612583302492));
#42168=CARTESIAN_POINT('',(4.51742050630483,-6.62530376704942E-5,17.8874166975081));
#42169=CARTESIAN_POINT('',(4.51775,5.53264807684796E-16,20.5));
#42170=CARTESIAN_POINT('Ctrl Pts',(4.51742050630483,-6.62530376705099E-5,
17.8874166975081));
#42171=CARTESIAN_POINT('Ctrl Pts',(4.5172038153436,0.446598657046559,17.9031493200567));
#42172=CARTESIAN_POINT('Ctrl Pts',(4.4513943616742,0.893327565156709,17.9188819426052));
#42173=CARTESIAN_POINT('Ctrl Pts',(4.32092341583127,1.32030703112013,17.9346145651538));
#42174=CARTESIAN_POINT('Ctrl Pts',(4.10151253806993,2.03835148774488,17.9610718618383));
#42175=CARTESIAN_POINT('Ctrl Pts',(3.6992350517372,2.70054332815014,17.9875291585227));
#42176=CARTESIAN_POINT('Ctrl Pts',(3.16312948534596,3.22617356514213,18.0139864552072));
#42177=CARTESIAN_POINT('Ctrl Pts',(2.62702391895476,3.75180380213408,18.0404437518917));
#42178=CARTESIAN_POINT('Ctrl Pts',(1.95709027250505,4.1408724357128,18.0669010485761));
#42179=CARTESIAN_POINT('Ctrl Pts',(1.23484721910258,4.34609472311257,18.0933583452606));
#42180=CARTESIAN_POINT('Ctrl Pts',(0.51260416570011,4.55131701051233,18.1198156419451));
#42181=CARTESIAN_POINT('Ctrl Pts',(-0.261948294655145,4.57269295173316,
18.1462729386295));
#42182=CARTESIAN_POINT('Ctrl Pts',(-0.994322299916471,4.40742376897534,
18.172730235314));
#42183=CARTESIAN_POINT('Ctrl Pts',(-1.72669630517784,4.24215458621751,18.1991875319985));
#42184=CARTESIAN_POINT('Ctrl Pts',(-2.41689185534529,3.89024027948101,18.225644828683));
#42185=CARTESIAN_POINT('Ctrl Pts',(-2.98112377443714,3.39491220205621,18.2521021253674));
#42186=CARTESIAN_POINT('Ctrl Pts',(-3.54535569352893,2.89958412463147,18.2785594220519));
#42187=CARTESIAN_POINT('Ctrl Pts',(-3.98362398154516,2.26084227651845,18.3050167187363));
#42188=CARTESIAN_POINT('Ctrl Pts',(-4.24201965646877,1.55578891217658,18.3314740154208));
#42189=CARTESIAN_POINT('Ctrl Pts',(-4.50041533139241,0.85073554783464,18.3579313121053));
#42190=CARTESIAN_POINT('Ctrl Pts',(-4.5789383932234,0.0793706672638789,
18.3843886087897));
#42191=CARTESIAN_POINT('Ctrl Pts',(-4.46902189478936,-0.663041834113523,
18.4108459054742));
#42192=CARTESIAN_POINT('Ctrl Pts',(-4.35910539635533,-1.4054543354909,18.4373032021587));
#42193=CARTESIAN_POINT('Ctrl Pts',(-4.06074933765627,-2.11891445767488,
18.4637604988432));
#42194=CARTESIAN_POINT('Ctrl Pts',(-3.60841564297678,-2.71899122382363,
18.4902177955276));
#42195=CARTESIAN_POINT('Ctrl Pts',(-3.15608194829727,-3.31906798997241,
18.5166750922121));
#42196=CARTESIAN_POINT('Ctrl Pts',(-2.54977061763729,-3.80576140008597,
18.5431323888965));
#42197=CARTESIAN_POINT('Ctrl Pts',(-1.86683275295704,-4.11521969441507,
18.569589685581));
#42198=CARTESIAN_POINT('Ctrl Pts',(-1.18389488827682,-4.42467798874415,
18.5960469822655));
#42199=CARTESIAN_POINT('Ctrl Pts',(-0.424330489576326,-4.55690116728879,
18.62250427895));
#42200=CARTESIAN_POINT('Ctrl Pts',(0.325633495564726,-4.5037382205983,18.6489615756344));
#42201=CARTESIAN_POINT('Ctrl Pts',(1.07559748070578,-4.4505752739078,18.6754188723189));
#42202=CARTESIAN_POINT('Ctrl Pts',(1.8159610522874,-4.21202620198217,18.7018761690034));
#42203=CARTESIAN_POINT('Ctrl Pts',(2.44569775560536,-3.80516814017072,18.7283334656878));
#42204=CARTESIAN_POINT('Ctrl Pts',(3.70517116224129,-2.99145201654782,18.7812480590567));
#42205=CARTESIAN_POINT('Ctrl Pts',(4.52213709582263,-1.50449993338164,18.8341626524257));
#42206=CARTESIAN_POINT('Ctrl Pts',(4.5251392293927,-0.0110172863201459,
18.8870772457947));
#42207=CARTESIAN_POINT('Ctrl Pts',(4.52514564904193,-0.00782367934410926,
18.8871903963658));
#42208=CARTESIAN_POINT('Ctrl Pts',(4.52514834676573,-0.00463004250646042,
18.887303546937));
#42209=CARTESIAN_POINT('Ctrl Pts',(4.52514732618828,-0.00143638257367575,
18.8874166975081));
#42210=CARTESIAN_POINT('Ctrl Pts',(4.51751172608841,-5.0340792907555E-5,
18.612583302492));
#42211=CARTESIAN_POINT('Ctrl Pts',(4.51742597397124,-0.374429761958339,
18.5993962924935));
#42212=CARTESIAN_POINT('Ctrl Pts',(4.47127719829474,-0.748797435630456,
18.586209282495));
#42213=CARTESIAN_POINT('Ctrl Pts',(4.37916492462631,-1.11150455739379,18.5730222724965));
#42214=CARTESIAN_POINT('Ctrl Pts',(4.19435868325684,-1.83920931617878,18.546564975812));
#42215=CARTESIAN_POINT('Ctrl Pts',(3.8245355689115,-2.51997685422145,18.5201076791275));
#42216=CARTESIAN_POINT('Ctrl Pts',(3.31430027943466,-3.07074498667331,18.493650382443));
#42217=CARTESIAN_POINT('Ctrl Pts',(2.80406498995785,-3.62151311912514,18.4671930857586));
#42218=CARTESIAN_POINT('Ctrl Pts',(2.15341752534957,-4.04228184598617,18.4407357890741));
#42219=CARTESIAN_POINT('Ctrl Pts',(1.4418387171972,-4.28187903967212,18.4142784923896));
#42220=CARTESIAN_POINT('Ctrl Pts',(0.730259909044834,-4.52147623335806,
18.3878211957052));
#42221=CARTESIAN_POINT('Ctrl Pts',(-0.0422502426516132,-4.57990189386892,
18.3613638990207));
#42222=CARTESIAN_POINT('Ctrl Pts',(-0.781724091400131,-4.44999904027085,
18.3349066023362));
#42223=CARTESIAN_POINT('Ctrl Pts',(-1.52119794014869,-4.32009618667279,
18.3084493056518));
#42224=CARTESIAN_POINT('Ctrl Pts',(-2.2276354859493,-4.00186481896578,18.2819920089673));
#42225=CARTESIAN_POINT('Ctrl Pts',(-2.81492815165361,-3.53408677354309,
18.2555347122828));
#42226=CARTESIAN_POINT('Ctrl Pts',(-3.40222081735788,-3.06630872812042,
18.2290774155984));
#42227=CARTESIAN_POINT('Ctrl Pts',(-3.87036860296584,-2.4489840049821,18.2026201189139));
#42228=CARTESIAN_POINT('Ctrl Pts',(-4.16238619140547,-1.75729062849926,
18.1761628222294));
#42229=CARTESIAN_POINT('Ctrl Pts',(-4.45440377984509,-1.06559725201643,
18.149705525545));
#42230=CARTESIAN_POINT('Ctrl Pts',(-4.57029117111638,-0.299535222189059,
18.1232482288605));
#42231=CARTESIAN_POINT('Ctrl Pts',(-4.49591510340165,0.447583892947263,
18.096790932176));
#42232=CARTESIAN_POINT('Ctrl Pts',(-4.42153903568692,1.19470300808361,18.0703336354916));
#42233=CARTESIAN_POINT('Ctrl Pts',(-4.15689950898618,1.92287920852894,18.0438763388071));
#42234=CARTESIAN_POINT('Ctrl Pts',(-3.73423901960036,2.54342464869681,18.0174190421226));
#42235=CARTESIAN_POINT('Ctrl Pts',(-3.31157853021454,3.16397008886469,17.9909617454381));
#42236=CARTESIAN_POINT('Ctrl Pts',(-2.73089707814366,3.67688476875509,17.9645044487537));
#42237=CARTESIAN_POINT('Ctrl Pts',(-2.06291588716924,4.01969454812901,17.9380471520692));
#42238=CARTESIAN_POINT('Ctrl Pts',(-1.39493469619478,4.36250432750296,17.9115898553848));
#42239=CARTESIAN_POINT('Ctrl Pts',(-0.639653766316788,4.53520920636039,
17.8851325587003));
#42240=CARTESIAN_POINT('Ctrl Pts',(0.110931801888114,4.51677482186132,17.8586752620158));
#42241=CARTESIAN_POINT('Ctrl Pts',(0.861517370092973,4.49834043736224,17.8322179653313));
#42242=CARTESIAN_POINT('Ctrl Pts',(1.60740757662473,4.28876678950667,17.8057606686469));
#42243=CARTESIAN_POINT('Ctrl Pts',(2.25775525993247,3.91357923987676,17.7793033719624));
#42244=CARTESIAN_POINT('Ctrl Pts',(2.90810294324022,3.53839169024685,17.7528460752779));
#42245=CARTESIAN_POINT('Ctrl Pts',(3.46290810332394,2.99759023884261,17.7263887785935));
#42246=CARTESIAN_POINT('Ctrl Pts',(3.8545953230205,2.35704415643041,17.699931481909));
#42247=CARTESIAN_POINT('Ctrl Pts',(4.24628254271708,1.71649807401819,17.6734741852245));
#42248=CARTESIAN_POINT('Ctrl Pts',(4.47485182202649,0.976207360598019,17.6470168885401));
#42249=CARTESIAN_POINT('Ctrl Pts',(4.51246407961468,0.226338472032798,17.6205595918556));
#42250=CARTESIAN_POINT('Ctrl Pts',(4.51624383400808,0.150982181084616,17.6179008287344));
#42251=CARTESIAN_POINT('Ctrl Pts',(4.5180951579083,0.0755291623761646,17.6152420656132));
#42252=CARTESIAN_POINT('Ctrl Pts',(4.51803700570725,7.32895604327322E-5,
17.612583302492));
#42253=CARTESIAN_POINT('Origin',(0.,0.,20.5));
#42254=CARTESIAN_POINT('',(4.51759135405446,-0.000109312323752775,16.612583302492));
#42255=CARTESIAN_POINT('',(4.51783748975292,0.000112199089269072,16.8874166975081));
#42256=CARTESIAN_POINT('',(4.51775,5.53264807684796E-16,20.5));
#42257=CARTESIAN_POINT('Ctrl Pts',(4.51783748975292,0.000112199089269072,
16.8874166975081));
#42258=CARTESIAN_POINT('Ctrl Pts',(4.5179865637855,0.145467881021208,16.8925377964919));
#42259=CARTESIAN_POINT('Ctrl Pts',(4.51110979946378,0.290809516813962,16.8976588954757));
#42260=CARTESIAN_POINT('Ctrl Pts',(4.49710302020602,0.435460743134165,16.9027799944596));
#42261=CARTESIAN_POINT('Ctrl Pts',(4.42473935069149,1.18277697791411,16.929237291144));
#42262=CARTESIAN_POINT('Ctrl Pts',(4.16206856248382,1.91166550411022,16.9556945878285));
#42263=CARTESIAN_POINT('Ctrl Pts',(3.7410836561604,2.53334852003379,16.9821518845129));
#42264=CARTESIAN_POINT('Ctrl Pts',(3.320098749837,3.15503153595733,17.0086091811974));
#42265=CARTESIAN_POINT('Ctrl Pts',(2.74079972539787,3.66950904160833,17.0350664778819));
#42266=CARTESIAN_POINT('Ctrl Pts',(2.07374458313351,4.01411821952866,17.0615237745663));
#42267=CARTESIAN_POINT('Ctrl Pts',(1.40668944086914,4.358727397449,17.0879810712508));
#42268=CARTESIAN_POINT('Ctrl Pts',(0.651878180779539,4.53346824763866,17.1144383679353));
#42269=CARTESIAN_POINT('Ctrl Pts',(-0.0987540592508608,4.51705757827172,
17.1408956646198));
#42270=CARTESIAN_POINT('Ctrl Pts',(-0.849386299281262,4.50064690890479,
17.1673529613042));
#42271=CARTESIAN_POINT('Ctrl Pts',(-1.59583951925246,4.29308471998125,17.1938102579887));
#42272=CARTESIAN_POINT('Ctrl Pts',(-2.24719647092549,3.91965176135179,17.2202675546731));
#42273=CARTESIAN_POINT('Ctrl Pts',(-2.89855342259852,3.54621880272232,17.2467248513576));
#42274=CARTESIAN_POINT('Ctrl Pts',(-3.45481410597338,3.00691507438693,17.2731821480421));
#42275=CARTESIAN_POINT('Ctrl Pts',(-3.8482267217169,2.36742735305624,17.2996394447266));
#42276=CARTESIAN_POINT('Ctrl Pts',(-4.24163933746045,1.7279396317255,17.326096741411));
#42277=CARTESIAN_POINT('Ctrl Pts',(-4.47220388557264,0.988267917399458,
17.3525540380955));
#42278=CARTESIAN_POINT('Ctrl Pts',(-4.51183760195937,0.238503067401354,
17.37901133478));
#42279=CARTESIAN_POINT('Ctrl Pts',(-4.55147131834609,-0.511261782596708,
17.4054686314644));
#42280=CARTESIAN_POINT('Ctrl Pts',(-4.40017420300738,-1.27111976826683,
17.4319259281489));
#42281=CARTESIAN_POINT('Ctrl Pts',(-4.07637456299423,-1.94852038806902,
17.4583832248334));
#42282=CARTESIAN_POINT('Ctrl Pts',(-3.75257492298108,-2.62592100787122,
17.4848405215178));
#42283=CARTESIAN_POINT('Ctrl Pts',(-3.25627275829351,-3.22086426180549,
17.5112978182023));
#42284=CARTESIAN_POINT('Ctrl Pts',(-2.64791620593751,-3.66088792814038,
17.5377551148868));
#42285=CARTESIAN_POINT('Ctrl Pts',(-2.0395596535815,-4.10091159447528,17.5642124115712));
#42286=CARTESIAN_POINT('Ctrl Pts',(-1.31914871355708,-4.38601567321079,
17.5906697082557));
#42287=CARTESIAN_POINT('Ctrl Pts',(-0.574430373257593,-4.48147252184731,
17.6171270049402));
#42288=CARTESIAN_POINT('Ctrl Pts',(0.17028796704189,-4.57692937048383,17.6435843016246));
#42289=CARTESIAN_POINT('Ctrl Pts',(0.939313707616428,-4.48273898902136,
17.6700415983091));
#42290=CARTESIAN_POINT('Ctrl Pts',(1.63898363511409,-4.21037796912968,17.6964988949936));
#42291=CARTESIAN_POINT('Ctrl Pts',(2.33865356261174,-3.93801694923801,17.7229561916781));
#42292=CARTESIAN_POINT('Ctrl Pts',(2.96896767703252,-3.48748529091713,17.7494134883625));
#42293=CARTESIAN_POINT('Ctrl Pts',(3.45314824099611,-2.91364911818949,17.775870785047));
#42294=CARTESIAN_POINT('Ctrl Pts',(3.9373288049597,-2.33981294546184,17.8023280817315));
#42295=CARTESIAN_POINT('Ctrl Pts',(4.27537581846611,-1.64267225832742,17.8287853784159));
#42296=CARTESIAN_POINT('Ctrl Pts',(4.42612719062433,-0.907153378338104,
17.8552426751004));
#42297=CARTESIAN_POINT('Ctrl Pts',(4.48723544976425,-0.609004992176015,
17.8659673492363));
#42298=CARTESIAN_POINT('Ctrl Pts',(4.51756822102564,-0.304550492318464,
17.8766920233722));
#42299=CARTESIAN_POINT('Ctrl Pts',(4.51742050630483,-6.62530376704943E-5,
17.8874166975081));
#42300=CARTESIAN_POINT('Ctrl Pts',(4.51803700570725,7.32895604327322E-5,
17.612583302492));
#42301=CARTESIAN_POINT('Ctrl Pts',(4.5175164865615,-0.675330663287972,17.5887847689287));
#42302=CARTESIAN_POINT('Ctrl Pts',(4.36400868534142,-1.35096328729663,17.5649862353655));
#42303=CARTESIAN_POINT('Ctrl Pts',(4.07110679585739,-1.95950283641844,17.5411877018022));
#42304=CARTESIAN_POINT('Ctrl Pts',(3.74548201864491,-2.63602819259433,17.5147304051177));
#42305=CARTESIAN_POINT('Ctrl Pts',(3.24757722835295,-3.22963184123583,17.4882731084333));
#42306=CARTESIAN_POINT('Ctrl Pts',(2.63803679068424,-3.66801355240638,17.4618158117488));
#42307=CARTESIAN_POINT('Ctrl Pts',(2.02849635301557,-4.10639526357692,17.4353585150643));
#42308=CARTESIAN_POINT('Ctrl Pts',(1.30732026797015,-4.38955503727653,17.4089012183799));
#42309=CARTESIAN_POINT('Ctrl Pts',(0.562346924558562,-4.48300430658583,
17.3824439216954));
#42310=CARTESIAN_POINT('Ctrl Pts',(-0.182626418853022,-4.57645357589513,
17.3559866250109));
#42311=CARTESIAN_POINT('Ctrl Pts',(-0.95139702063077,-4.48019234081411,
17.3295293283265));
#42312=CARTESIAN_POINT('Ctrl Pts',(-1.65032944052442,-4.20594512376068,
17.303072031642));
#42313=CARTESIAN_POINT('Ctrl Pts',(-2.34926186041808,-3.93169790670724,
17.2766147349575));
#42314=CARTESIAN_POINT('Ctrl Pts',(-2.97835609842763,-3.47946470768139,
17.2501574382731));
#42315=CARTESIAN_POINT('Ctrl Pts',(-3.46098918943056,-2.90432702425224,
17.2237001415886));
#42316=CARTESIAN_POINT('Ctrl Pts',(-3.94362228043348,-2.32918934082309,
17.1972428449041));
#42317=CARTESIAN_POINT('Ctrl Pts',(-4.27979422442977,-1.63114717299066,
17.1707855482197));
#42318=CARTESIAN_POINT('Ctrl Pts',(-4.42855964178007,-0.895221287202602,
17.1443282515352));
#42319=CARTESIAN_POINT('Ctrl Pts',(-4.57732505913038,-0.159295401414506,
17.1178709548507));
#42320=CARTESIAN_POINT('Ctrl Pts',(-4.53868394983468,0.614514202329214,
17.0914136581662));
#42321=CARTESIAN_POINT('Ctrl Pts',(-4.31734276296002,1.33195837225454,17.0649563614818));
#42322=CARTESIAN_POINT('Ctrl Pts',(-4.09600157608536,2.04940254217985,17.0384990647973));
#42323=CARTESIAN_POINT('Ctrl Pts',(-3.69196031163174,2.71048127828677,17.0120417681128));
#42324=CARTESIAN_POINT('Ctrl Pts',(-3.15443074594472,3.23467592132634,16.9855844714284));
#42325=CARTESIAN_POINT('Ctrl Pts',(-2.61690118025774,3.75887056436587,16.9591271747439));
#42326=CARTESIAN_POINT('Ctrl Pts',(-1.94588331333737,4.14618111433807,16.9326698780594));
#42327=CARTESIAN_POINT('Ctrl Pts',(-1.223106380062,4.3494335753433,16.906212581375));
#42328=CARTESIAN_POINT('Ctrl Pts',(-0.500329446786581,4.55268603634855,
16.8797552846905));
#42329=CARTESIAN_POINT('Ctrl Pts',(0.274206552843852,4.57188040838682,16.853297988006));
#42330=CARTESIAN_POINT('Ctrl Pts',(1.00616399197863,4.40467883795473,16.8268406913216));
#42331=CARTESIAN_POINT('Ctrl Pts',(1.73812143111341,4.23747726752264,16.8003833946371));
#42332=CARTESIAN_POINT('Ctrl Pts',(2.42750030975254,3.88387975462018,16.7739260979526));
#42333=CARTESIAN_POINT('Ctrl Pts',(2.99033504306357,3.38695408510442,16.7474688012682));
#42334=CARTESIAN_POINT('Ctrl Pts',(3.55316977637459,2.89002841558867,16.7210115045837));
#42335=CARTESIAN_POINT('Ctrl Pts',(3.98946036435752,2.24977458945961,16.6945542078992));
#42336=CARTESIAN_POINT('Ctrl Pts',(4.24606709644911,1.54417481408576,16.6680969112148));
#42337=CARTESIAN_POINT('Ctrl Pts',(4.42554078305754,1.05067025197154,16.6495923749738));
#42338=CARTESIAN_POINT('Ctrl Pts',(4.51711737210933,0.525199995180907,16.6310878387329));
#42339=CARTESIAN_POINT('Ctrl Pts',(4.51759135405446,-0.000109312323752775,
16.612583302492));
#42340=CARTESIAN_POINT('Origin',(0.,0.,20.5));
#42341=CARTESIAN_POINT('',(4.51759608459634,0.0001098887360651,15.612583302492));
#42342=CARTESIAN_POINT('',(4.5178043285159,-0.000114763987914418,15.8874166975081));
#42343=CARTESIAN_POINT('',(4.51775,5.53264807684796E-16,20.5));
#42344=CARTESIAN_POINT('Ctrl Pts',(4.5178043285159,-0.000114763987914418,
15.8874166975081));
#42345=CARTESIAN_POINT('Ctrl Pts',(4.51719021324072,0.595015005655344,15.9083835696116));
#42346=CARTESIAN_POINT('Ctrl Pts',(4.39892963080694,1.19038158256103,15.9293504417152));
#42347=CARTESIAN_POINT('Ctrl Pts',(4.16984886166331,1.73951778234083,15.9503173138187));
#42348=CARTESIAN_POINT('Ctrl Pts',(3.88078057126651,2.43245182066608,15.9767746105032));
#42349=CARTESIAN_POINT('Ctrl Pts',(3.41525380642348,3.05177344176931,16.0032319071877));
#42350=CARTESIAN_POINT('Ctrl Pts',(2.82996921187389,3.52204995762958,16.0296892038721));
#42351=CARTESIAN_POINT('Ctrl Pts',(2.2446846173243,3.99232647348986,16.0561465005566));
#42352=CARTESIAN_POINT('Ctrl Pts',(1.53964219306814,4.3135578841072,16.082603797241));
#42353=CARTESIAN_POINT('Ctrl Pts',(0.800715326097207,4.44661855917225,16.1090610939255));
#42354=CARTESIAN_POINT('Ctrl Pts',(0.0617884591262693,4.57967923423731,
16.13551839061));
#42355=CARTESIAN_POINT('Ctrl Pts',(-0.711022850559448,4.52456917375008,
16.1619756872944));
#42356=CARTESIAN_POINT('Ctrl Pts',(-1.42359104075325,4.28800072211039,16.1884329839789));
#42357=CARTESIAN_POINT('Ctrl Pts',(-2.13615923094709,4.0514322704707,16.2148902806634));
#42358=CARTESIAN_POINT('Ctrl Pts',(-2.788484301649,3.63340542767853,16.2413475773478));
#42359=CARTESIAN_POINT('Ctrl Pts',(-3.30111378116087,3.08483540049633,16.2678048740323));
#42360=CARTESIAN_POINT('Ctrl Pts',(-3.81374326067272,2.53626537331417,16.2942621707168));
#42361=CARTESIAN_POINT('Ctrl Pts',(-4.18667714899455,1.857152161742,16.3207194674013));
#42362=CARTESIAN_POINT('Ctrl Pts',(-4.37449251133268,1.1302110034409,16.3471767640857));
#42363=CARTESIAN_POINT('Ctrl Pts',(-4.56230787367082,0.403269845139789,
16.3736340607702));
#42364=CARTESIAN_POINT('Ctrl Pts',(-4.56500471002526,-0.371499259890255,
16.4000913574546));
#42365=CARTESIAN_POINT('Ctrl Pts',(-4.38225454858744,-1.09973029228273,
16.4265486541391));
#42366=CARTESIAN_POINT('Ctrl Pts',(-4.19950438714961,-1.82796132467523,
16.4530059508236));
#42367=CARTESIAN_POINT('Ctrl Pts',(-3.8313072279195,-2.50965428443015,16.4794632475081));
#42368=CARTESIAN_POINT('Ctrl Pts',(-3.3225090776326,-3.06177972318871,16.5059205441925));
#42369=CARTESIAN_POINT('Ctrl Pts',(-2.81371092734571,-3.61390516194727,
16.532377840877));
#42370=CARTESIAN_POINT('Ctrl Pts',(-2.16431178600201,-4.03646307970946,
16.5588351375615));
#42371=CARTESIAN_POINT('Ctrl Pts',(-1.45340774986022,-4.27798639033812,
16.5852924342459));
#42372=CARTESIAN_POINT('Ctrl Pts',(-0.742503713718461,-4.51950970096678,
16.6117497309304));
#42373=CARTESIAN_POINT('Ctrl Pts',(0.0299052172213853,-4.5799984044619,
16.6382070276149));
#42374=CARTESIAN_POINT('Ctrl Pts',(0.769740489176569,-4.45208504257185,
16.6646643242993));
#42375=CARTESIAN_POINT('Ctrl Pts',(1.50957576113175,-4.32417168068181,16.6911216209838));
#42376=CARTESIAN_POINT('Ctrl Pts',(2.21683737410228,-4.00785625340658,16.7175789176683));
#42377=CARTESIAN_POINT('Ctrl Pts',(2.80538164796928,-3.54166563180933,16.7440362143527));
#42378=CARTESIAN_POINT('Ctrl Pts',(3.39392592183629,-3.07547501021207,16.7704935110372));
#42379=CARTESIAN_POINT('Ctrl Pts',(3.86375285659978,-2.45940919429276,16.7969508077217));
#42380=CARTESIAN_POINT('Ctrl Pts',(4.15763804857084,-1.76850431465121,16.8234081044061));
#42381=CARTESIAN_POINT('Ctrl Pts',(4.39463854911208,-1.21133162689784,16.8447443021068));
#42382=CARTESIAN_POINT('Ctrl Pts',(4.51721639786597,-0.605487805208481,
16.8660804998074));
#42383=CARTESIAN_POINT('Ctrl Pts',(4.51783748975292,0.000112199089269072,
16.8874166975081));
#42384=CARTESIAN_POINT('Ctrl Pts',(4.51759135405446,-0.000109312323752775,
16.612583302492));
#42385=CARTESIAN_POINT('Ctrl Pts',(4.51779505896309,-0.225873364281351,
16.6046305420484));
#42386=CARTESIAN_POINT('Ctrl Pts',(4.50117162820754,-0.451607688050524,
16.5966777816049));
#42387=CARTESIAN_POINT('Ctrl Pts',(4.46746660375751,-0.674762023706868,
16.5887250211614));
#42388=CARTESIAN_POINT('Ctrl Pts',(4.35533650277404,-1.417153361507,16.5622677244769));
#42389=CARTESIAN_POINT('Ctrl Pts',(4.05415342460685,-2.1309903124886,16.5358104277924));
#42390=CARTESIAN_POINT('Ctrl Pts',(3.60060113490314,-2.72932832606603,16.509353131108));
#42391=CARTESIAN_POINT('Ctrl Pts',(3.14704884519943,-3.32766633964346,16.4828958344235));
#42392=CARTESIAN_POINT('Ctrl Pts',(2.54112734395919,-3.81050541581671,16.456438537739));
#42393=CARTESIAN_POINT('Ctrl Pts',(1.85663719941204,-4.1190362894713,16.4299812410546));
#42394=CARTESIAN_POINT('Ctrl Pts',(1.17214705486486,-4.4275671631259,16.4035239443701));
#42395=CARTESIAN_POINT('Ctrl Pts',(0.409088267010757,-4.56178983426182,
16.3770666476856));
#42396=CARTESIAN_POINT('Ctrl Pts',(-0.33959944827516,-4.50535613008826,
16.3506093510012));
#42397=CARTESIAN_POINT('Ctrl Pts',(-1.08828716356108,-4.4489224259147,16.3241520543167));
#42398=CARTESIAN_POINT('Ctrl Pts',(-1.82260380627881,-4.20183234643166,
16.2976947576322));
#42399=CARTESIAN_POINT('Ctrl Pts',(-2.45311042204468,-3.79418118985514,
16.2712374609477));
#42400=CARTESIAN_POINT('Ctrl Pts',(-3.08361703781053,-3.38653003327864,
16.2447801642633));
#42401=CARTESIAN_POINT('Ctrl Pts',(-3.61031362662454,-2.81831779960867,
16.2183228675788));
#42402=CARTESIAN_POINT('Ctrl Pts',(-3.96904912687637,-2.15875211004946,
16.1918655708943));
#42403=CARTESIAN_POINT('Ctrl Pts',(-4.3277846271282,-1.49918642049025,16.1654082742099));
#42404=CARTESIAN_POINT('Ctrl Pts',(-4.51855903881786,-0.748267275041791,
16.1389509775254));
#42405=CARTESIAN_POINT('Ctrl Pts',(-4.51813624973985,0.00254420544672257,
16.1124936808409));
#42406=CARTESIAN_POINT('Ctrl Pts',(-4.51771346066184,0.753355685935258,
16.0860363841565));
#42407=CARTESIAN_POINT('Ctrl Pts',(-4.32609347081614,1.50405950146385,16.059579087472));
#42408=CARTESIAN_POINT('Ctrl Pts',(-3.96661538289292,2.16322075812806,16.0331217907875));
#42409=CARTESIAN_POINT('Ctrl Pts',(-3.6071372949697,2.82238201479228,16.0066644941031));
#42410=CARTESIAN_POINT('Ctrl Pts',(-3.07980110896895,3.39000071259211,15.9802071974186));
#42411=CARTESIAN_POINT('Ctrl Pts',(-2.4488357887268,3.7969415223371,15.9537499007341));
#42412=CARTESIAN_POINT('Ctrl Pts',(-1.81787046848466,4.20388233208208,15.9272926040497));
#42413=CARTESIAN_POINT('Ctrl Pts',(-1.08327601400112,4.45014525377221,15.9008353073652));
#42414=CARTESIAN_POINT('Ctrl Pts',(-0.334525216833305,4.50573573609241,
15.8743780106807));
#42415=CARTESIAN_POINT('Ctrl Pts',(0.41422558033451,4.5613262184126,15.8479207139963));
#42416=CARTESIAN_POINT('Ctrl Pts',(1.1771327201866,4.42624426136285,15.8214634173118));
#42417=CARTESIAN_POINT('Ctrl Pts',(1.86127495742196,4.11694269781245,15.7950061206273));
#42418=CARTESIAN_POINT('Ctrl Pts',(2.54541719465734,3.80764113426205,15.7685488239429));
#42419=CARTESIAN_POINT('Ctrl Pts',(3.15079452927597,3.32411996421099,15.7420915272584));
#42420=CARTESIAN_POINT('Ctrl Pts',(3.60367267191142,2.72527153104349,15.7156342305739));
#42421=CARTESIAN_POINT('Ctrl Pts',(4.05655081454687,2.12642309787598,15.6891769338895));
#42422=CARTESIAN_POINT('Ctrl Pts',(4.35692976519912,1.41224740159204,15.662719637205));
#42423=CARTESIAN_POINT('Ctrl Pts',(4.46822370011744,0.669730251598505,15.6362623405205));
#42424=CARTESIAN_POINT('Ctrl Pts',(4.50142605066627,0.448214903788299,15.6283693278443));
#42425=CARTESIAN_POINT('Ctrl Pts',(4.51779965427679,0.224177139537577,15.6204763151682));
#42426=CARTESIAN_POINT('Ctrl Pts',(4.51759608459634,0.0001098887360651,
15.612583302492));
#42427=CARTESIAN_POINT('Origin',(0.,0.,20.5));
#42428=CARTESIAN_POINT('',(4.51803303654689,-7.46219232266102E-5,14.612583302492));
#42429=CARTESIAN_POINT('',(4.51743493951217,7.09613961932946E-5,14.8874166975081));
#42430=CARTESIAN_POINT('',(4.51775,5.53264807684796E-16,20.5));
#42431=CARTESIAN_POINT('Ctrl Pts',(4.51743493951217,7.09613961932946E-5,
14.8874166975081));
#42432=CARTESIAN_POINT('Ctrl Pts',(4.51759894908653,0.294069189408427,14.8977720460469));
#42433=CARTESIAN_POINT('Ctrl Pts',(4.48933542297813,0.588036293354993,14.9081273945857));
#42434=CARTESIAN_POINT('Ctrl Pts',(4.43233806206614,0.876322399438229,14.9184827431245));
#42435=CARTESIAN_POINT('Ctrl Pts',(4.2867132110791,1.61287617260017,14.9449400398089));
#42436=CARTESIAN_POINT('Ctrl Pts',(3.95352194255086,2.31234598448206,14.9713973364934));
#42437=CARTESIAN_POINT('Ctrl Pts',(3.47334658423498,2.88953718612178,14.9978546331779));
#42438=CARTESIAN_POINT('Ctrl Pts',(2.99317122591908,3.46672838776151,15.0243119298623));
#42439=CARTESIAN_POINT('Ctrl Pts',(2.36601177781554,3.92164097915906,15.0507692265468));
#42440=CARTESIAN_POINT('Ctrl Pts',(1.6682555666064,4.19886711014818,15.0772265232313));
#42441=CARTESIAN_POINT('Ctrl Pts',(0.97049935539727,4.4760932411373,15.1036838199157));
#42442=CARTESIAN_POINT('Ctrl Pts',(0.20214638108255,4.57563291171798,15.1301411166002));
#42443=CARTESIAN_POINT('Ctrl Pts',(-0.543218814426446,4.48536230017716,
15.1565984132847));
#42444=CARTESIAN_POINT('Ctrl Pts',(-1.28858400993542,4.39509168863634,15.1830557099691));
#42445=CARTESIAN_POINT('Ctrl Pts',(-2.01096142663867,4.11501079497402,15.2095130066536));
#42446=CARTESIAN_POINT('Ctrl Pts',(-2.6223662946594,3.67923316206403,15.2359703033381));
#42447=CARTESIAN_POINT('Ctrl Pts',(-3.23377116268013,3.24345552915403,15.2624276000225));
#42448=CARTESIAN_POINT('Ctrl Pts',(-3.73420348201834,2.65198115699635,15.288884896707));
#42449=CARTESIAN_POINT('Ctrl Pts',(-4.06271115002269,1.9768509695166,15.3153421933915));
#42450=CARTESIAN_POINT('Ctrl Pts',(-4.39121881802704,1.30172078203686,15.3417994900759));
#42451=CARTESIAN_POINT('Ctrl Pts',(-4.54780183469754,0.542934779235054,
15.3682567867604));
#42452=CARTESIAN_POINT('Ctrl Pts',(-4.51338856189906,-0.207087743519677,
15.3947140834449));
#42453=CARTESIAN_POINT('Ctrl Pts',(-4.47897528910057,-0.957110266274451,
15.4211713801293));
#42454=CARTESIAN_POINT('Ctrl Pts',(-4.2535657268331,-1.69836930898215,15.4476286768138));
#42455=CARTESIAN_POINT('Ctrl Pts',(-3.86461451031294,-2.34058034061557,
15.4740859734983));
#42456=CARTESIAN_POINT('Ctrl Pts',(-3.4756632937928,-2.98279137224897,15.5005432701827));
#42457=CARTESIAN_POINT('Ctrl Pts',(-2.92317042302,-3.5259543928081,15.5270005668672));
#42458=CARTESIAN_POINT('Ctrl Pts',(-2.27442891819367,-3.9039127475242,15.5534578635517));
#42459=CARTESIAN_POINT('Ctrl Pts',(-1.62568741336734,-4.28187110224029,
15.5799151602362));
#42460=CARTESIAN_POINT('Ctrl Pts',(-0.880697274487477,-4.49462479111335,
15.6063724569206));
#42461=CARTESIAN_POINT('Ctrl Pts',(-0.130197475965578,-4.51626065030008,
15.6328297536051));
#42462=CARTESIAN_POINT('Ctrl Pts',(0.620302322556342,-4.53789650948681,
15.6592870502896));
#42463=CARTESIAN_POINT('Ctrl Pts',(1.3763117807203,-4.3684145389872,15.685744346974));
#42464=CARTESIAN_POINT('Ctrl Pts',(2.04574978322079,-4.02845745523656,15.7122016436585));
#42465=CARTESIAN_POINT('Ctrl Pts',(2.71518778572125,-3.68850037148593,15.738658940343));
#42466=CARTESIAN_POINT('Ctrl Pts',(3.29805433255825,-3.17806817448428,15.7651162370274));
#42467=CARTESIAN_POINT('Ctrl Pts',(3.72335692340443,-2.55933094091619,15.7915735337119));
#42468=CARTESIAN_POINT('Ctrl Pts',(4.14865951425061,-1.94059370734809,15.8180308303964));
#42469=CARTESIAN_POINT('Ctrl Pts',(4.41639814910596,-1.21355143721353,15.8444881270808));
#42470=CARTESIAN_POINT('Ctrl Pts',(4.49396255855834,-0.466757074372606,
15.8709454237653));
#42471=CARTESIAN_POINT('Ctrl Pts',(4.51005874349141,-0.311782128309925,
15.8764358483462));
#42472=CARTESIAN_POINT('Ctrl Pts',(4.51796514189739,-0.155956565280692,
15.8819262729272));
#42473=CARTESIAN_POINT('Ctrl Pts',(4.5178043285159,-0.000114763987914418,
15.8874166975081));
#42474=CARTESIAN_POINT('Ctrl Pts',(4.51759608459634,0.0001098887360651,
15.612583302492));
#42475=CARTESIAN_POINT('Ctrl Pts',(4.5171172908178,-0.526893962833933,15.5940190184837));
#42476=CARTESIAN_POINT('Ctrl Pts',(4.42493597400368,-1.05406092973462,15.5754547344754));
#42477=CARTESIAN_POINT('Ctrl Pts',(4.24432532522022,-1.54895583471304,15.5568904504671));
#42478=CARTESIAN_POINT('Ctrl Pts',(3.98692409622027,-2.25426616732798,15.5304331537826));
#42479=CARTESIAN_POINT('Ctrl Pts',(3.54991271903595,-2.89402822885477,15.5039758570982));
#42480=CARTESIAN_POINT('Ctrl Pts',(2.98651869575415,-3.39031970824409,15.4775185604137));
#42481=CARTESIAN_POINT('Ctrl Pts',(2.42312467247236,-3.88661118763341,15.4510612637292));
#42482=CARTESIAN_POINT('Ctrl Pts',(1.73334800309309,-4.23943208488526,15.4246039670448));
#42483=CARTESIAN_POINT('Ctrl Pts',(1.00120272254938,-4.40580920519228,15.3981466703603));
#42484=CARTESIAN_POINT('Ctrl Pts',(0.269057442005672,-4.5721863254993,15.3716893736758));
#42485=CARTESIAN_POINT('Ctrl Pts',(-0.505456449702493,-4.55211966886149,
15.3452320769914));
#42486=CARTESIAN_POINT('Ctrl Pts',(-1.22800401774377,-4.34805333184893,
15.3187747803069));
#42487=CARTESIAN_POINT('Ctrl Pts',(-1.95055158578508,-4.14398699483636,
15.2923174836224));
#42488=CARTESIAN_POINT('Ctrl Pts',(-2.62113283015951,-3.75592097744901,
15.265860186938));
#42489=CARTESIAN_POINT('Ctrl Pts',(-3.15807169745543,-3.23112129111991,
15.2394028902535));
#42490=CARTESIAN_POINT('Ctrl Pts',(-3.69501056475133,-2.70632160479082,
15.212945593569));
#42491=CARTESIAN_POINT('Ctrl Pts',(-4.09830705496871,-2.04478824952003,
15.1864882968846));
#42492=CARTESIAN_POINT('Ctrl Pts',(-4.31884010193997,-1.3270952558398,15.1600310002001));
#42493=CARTESIAN_POINT('Ctrl Pts',(-4.53937314891122,-0.609402262159613,
15.1335737035156));
#42494=CARTESIAN_POINT('Ctrl Pts',(-4.57714275263633,0.164450369930026,
15.1071164068312));
#42495=CARTESIAN_POINT('Ctrl Pts',(-4.42754861718238,0.90020824628735,15.0806591101467));
#42496=CARTESIAN_POINT('Ctrl Pts',(-4.27795448172842,1.63596612264472,15.0542018134622));
#42497=CARTESIAN_POINT('Ctrl Pts',(-3.94099660709542,2.33362924326977,15.0277445167778));
#42498=CARTESIAN_POINT('Ctrl Pts',(-3.45771608949183,2.90822301219606,15.0012872200933));
#42499=CARTESIAN_POINT('Ctrl Pts',(-2.97443557188824,3.48281678112233,14.9748299234088));
#42500=CARTESIAN_POINT('Ctrl Pts',(-2.34483241131409,3.93434119834979,14.9483726267244));
#42501=CARTESIAN_POINT('Ctrl Pts',(-1.64559157592583,4.20780108957628,14.9219153300399));
#42502=CARTESIAN_POINT('Ctrl Pts',(-0.946350740537523,4.4812609808028,14.8954580333554));
#42503=CARTESIAN_POINT('Ctrl Pts',(-0.17747223033509,4.57665634602833,14.8690007366709));
#42504=CARTESIAN_POINT('Ctrl Pts',(0.567395403080653,4.48236813534546,14.8425434399865));
#42505=CARTESIAN_POINT('Ctrl Pts',(1.31226303649637,4.38807992466259,14.816086143302));
#42506=CARTESIAN_POINT('Ctrl Pts',(2.03311979312542,4.10410813807131,14.7896288466175));
#42507=CARTESIAN_POINT('Ctrl Pts',(2.64216611780504,3.665040224898,14.7631715499331));
#42508=CARTESIAN_POINT('Ctrl Pts',(3.25121244248463,3.22597231172472,14.7367142532486));
#42509=CARTESIAN_POINT('Ctrl Pts',(3.74844833521482,2.63180827196943,14.7102569565641));
#42510=CARTESIAN_POINT('Ctrl Pts',(4.07331101456755,1.95491662809442,14.6837996598797));
#42511=CARTESIAN_POINT('Ctrl Pts',(4.36479376317213,1.347576205805,14.6600608740838));
#42512=CARTESIAN_POINT('Ctrl Pts',(4.51750642932664,0.673635432917883,14.6363220882879));
#42513=CARTESIAN_POINT('Ctrl Pts',(4.51803303654689,-7.46219232266102E-5,
14.612583302492));
#42514=CARTESIAN_POINT('Origin',(0.,0.,20.5));
#42515=CARTESIAN_POINT('',(4.51736301819297,2.68279993319077E-6,13.612583302492));
#42516=CARTESIAN_POINT('',(4.51813640225623,-7.72658854479727E-6,13.8874166975081));
#42517=CARTESIAN_POINT('',(4.51775,5.53264807684796E-16,20.5));
#42518=CARTESIAN_POINT('Ctrl Pts',(4.51813584929441,-7.71553139285741E-6,
13.8874166975081));
#42519=CARTESIAN_POINT('Ctrl Pts',(4.5180616865618,0.743534623094937,13.9136178191666));
#42520=CARTESIAN_POINT('Ctrl Pts',(4.33069406362294,1.48711296925487,13.9398189408251));
#42521=CARTESIAN_POINT('Ctrl Pts',(3.97822152575483,2.14180184335953,13.9660200624836));
#42522=CARTESIAN_POINT('Ctrl Pts',(3.62230277429653,2.80289177698769,13.9924773591681));
#42523=CARTESIAN_POINT('Ctrl Pts',(3.0980347793188,3.37334555127586,14.0189346558525));
#42524=CARTESIAN_POINT('Ctrl Pts',(2.46927280238618,3.78368252785474,14.045391952537));
#42525=CARTESIAN_POINT('Ctrl Pts',(1.84051082545358,4.19401950443362,14.0718492492215));
#42526=CARTESIAN_POINT('Ctrl Pts',(1.10725486656609,4.44423968330323,14.0983065459059));
#42527=CARTESIAN_POINT('Ctrl Pts',(0.358814689998941,4.50386652360373,14.1247638425904));
#42528=CARTESIAN_POINT('Ctrl Pts',(-0.389625486568206,4.56349336390423,
14.1512211392749));
#42529=CARTESIAN_POINT('Ctrl Pts',(-1.15324988081502,4.43252686563563,14.1776784359594));
#42530=CARTESIAN_POINT('Ctrl Pts',(-1.83904988664919,4.12691860334233,14.2041357326438));
#42531=CARTESIAN_POINT('Ctrl Pts',(-2.52484989248339,3.82131034104901,14.2305930293283));
#42532=CARTESIAN_POINT('Ctrl Pts',(-3.13282550990494,3.34106031473099,14.2570503260128));
#42533=CARTESIAN_POINT('Ctrl Pts',(-3.58892598157751,2.74466244608609,14.2835076226972));
#42534=CARTESIAN_POINT('Ctrl Pts',(-4.04502645325008,2.14826457744119,14.3099649193817));
#42535=CARTESIAN_POINT('Ctrl Pts',(-4.34925177917366,1.43571886646941,14.3364222160662));
#42536=CARTESIAN_POINT('Ctrl Pts',(-4.46454765134644,0.693812592170538,
14.3628795127506));
#42537=CARTESIAN_POINT('Ctrl Pts',(-4.57984352351921,-0.0480936821283345,
14.3893368094351));
#42538=CARTESIAN_POINT('Ctrl Pts',(-4.50620994194118,-0.819360519754252,
14.4157941061196));
#42539=CARTESIAN_POINT('Ctrl Pts',(-4.25261539535597,-1.52604847346958,
14.442251402804));
#42540=CARTESIAN_POINT('Ctrl Pts',(-3.99902084877075,-2.23273642718488,
14.4687086994885));
#42541=CARTESIAN_POINT('Ctrl Pts',(-3.56546533717836,-2.87484549698955,
14.495165996173));
#42542=CARTESIAN_POINT('Ctrl Pts',(-3.00475544206132,-3.37416750882351,
14.5216232928574));
#42543=CARTESIAN_POINT('Ctrl Pts',(-2.44404554694427,-3.87348952065748,
14.5480805895419));
#42544=CARTESIAN_POINT('Ctrl Pts',(-1.75618126830258,-4.23002447452076,
14.5745378862264));
#42545=CARTESIAN_POINT('Ctrl Pts',(-1.02494371399391,-4.40034680762116,
14.6009951829108));
#42546=CARTESIAN_POINT('Ctrl Pts',(-0.293706159685227,-4.57066914072157,
14.6274524795953));
#42547=CARTESIAN_POINT('Ctrl Pts',(0.480904670290444,-4.5547788530591,14.6539097762798));
#42548=CARTESIAN_POINT('Ctrl Pts',(1.20454203412804,-4.35461136408475,14.6803670729642));
#42549=CARTESIAN_POINT('Ctrl Pts',(1.92817939796561,-4.15444387511041,14.7068243696487));
#42550=CARTESIAN_POINT('Ctrl Pts',(2.60084329566512,-3.76999918482422,14.7332816663332));
#42551=CARTESIAN_POINT('Ctrl Pts',(3.14060400894491,-3.24810223102607,14.7597389630176));
#42552=CARTESIAN_POINT('Ctrl Pts',(3.68036472222471,-2.72620527722791,14.7861962597021));
#42553=CARTESIAN_POINT('Ctrl Pts',(4.08722225108478,-2.0668560599178,14.8126535563866));
#42554=CARTESIAN_POINT('Ctrl Pts',(4.3116217987919,-1.35036258404174,14.839110853071));
#42555=CARTESIAN_POINT('Ctrl Pts',(4.44819168059748,-0.91430364223594,14.8552128012167));
#42556=CARTESIAN_POINT('Ctrl Pts',(4.51717991442519,-0.457078713927616,
14.8713147493624));
#42557=CARTESIAN_POINT('Ctrl Pts',(4.51743493951217,7.09613961932946E-5,
14.8874166975081));
#42558=CARTESIAN_POINT('Ctrl Pts',(4.51803303654689,-7.46219232266102E-5,
14.612583302492));
#42559=CARTESIAN_POINT('Ctrl Pts',(4.51809334238876,-0.0772263404472327,
14.6098647916034));
#42560=CARTESIAN_POINT('Ctrl Pts',(4.51615783443211,-0.154375033265316,
14.6071462807148));
#42561=CARTESIAN_POINT('Ctrl Pts',(4.51220636430248,-0.231420332178498,
14.6044277698263));
#42562=CARTESIAN_POINT('Ctrl Pts',(4.47374956870936,-0.981246400581585,
14.5779704731418));
#42563=CARTESIAN_POINT('Ctrl Pts',(4.24434651154784,-1.72127928939297,14.5515131764573));
#42564=CARTESIAN_POINT('Ctrl Pts',(3.85193823129266,-2.36138381177295,14.5250558797729));
#42565=CARTESIAN_POINT('Ctrl Pts',(3.4595299510375,-3.0014883341529,14.4985985830884));
#42566=CARTESIAN_POINT('Ctrl Pts',(2.90411644768869,-3.54166449010144,14.4721412864039));
#42567=CARTESIAN_POINT('Ctrl Pts',(2.25334647126064,-3.91611942165386,14.4456839897195));
#42568=CARTESIAN_POINT('Ctrl Pts',(1.60257649483259,-4.29057435320629,14.419226693035));
#42569=CARTESIAN_POINT('Ctrl Pts',(0.856450045325319,-4.49930806036259,
14.3927693963505));
#42570=CARTESIAN_POINT('Ctrl Pts',(0.10584449852735,-4.51689700860324,14.3663120996661));
#42571=CARTESIAN_POINT('Ctrl Pts',(-0.644761048270598,-4.53448595684389,
14.3398548029816));
#42572=CARTESIAN_POINT('Ctrl Pts',(-1.39984569235923,-4.36093014616891,
14.3133975062971));
#42573=CARTESIAN_POINT('Ctrl Pts',(-2.06744095976432,-4.01736848223886,
14.2869402096127));
#42574=CARTESIAN_POINT('Ctrl Pts',(-2.73503622716945,-3.67380681830879,
14.2604829129282));
#42575=CARTESIAN_POINT('Ctrl Pts',(-3.31514211789102,-3.16023930112366,
14.2340256162437));
#42576=CARTESIAN_POINT('Ctrl Pts',(-3.73710237646046,-2.53921788589538,
14.2075683195593));
#42577=CARTESIAN_POINT('Ctrl Pts',(-4.15906263502989,-1.91819647066709,
14.1811110228748));
#42578=CARTESIAN_POINT('Ctrl Pts',(-4.42287726144721,-1.18972115739562,
14.1546537261903));
#42579=CARTESIAN_POINT('Ctrl Pts',(-4.49641392618661,-0.442519433011148,
14.1281964295058));
#42580=CARTESIAN_POINT('Ctrl Pts',(-4.56995059092601,0.3046822913733,14.1017391328214));
#42581=CARTESIAN_POINT('Ctrl Pts',(-4.45320929398754,1.07061042687079,14.0752818361369));
#42582=CARTESIAN_POINT('Ctrl Pts',(-4.16040899613706,1.76197577425433,14.0488245394525));
#42583=CARTESIAN_POINT('Ctrl Pts',(-3.86760869828659,2.45334112163787,14.022367242768));
#42584=CARTESIAN_POINT('Ctrl Pts',(-3.39874939952411,3.07014368090745,13.9959099460835));
#42585=CARTESIAN_POINT('Ctrl Pts',(-2.81093764353767,3.53725758297869,13.969452649399));
#42586=CARTESIAN_POINT('Ctrl Pts',(-2.22312588755121,4.00437148504995,13.9429953527146));
#42587=CARTESIAN_POINT('Ctrl Pts',(-1.51636167434084,4.32179672992284,13.9165380560301));
#42588=CARTESIAN_POINT('Ctrl Pts',(-0.776728102877452,4.45087127407632,
13.8900807593456));
#42589=CARTESIAN_POINT('Ctrl Pts',(-0.0370945314140622,4.5799458182298,
13.8636234626612));
#42590=CARTESIAN_POINT('Ctrl Pts',(0.735408398302354,4.52066966166384,13.8371661659767));
#42591=CARTESIAN_POINT('Ctrl Pts',(1.44669068438533,4.2802625746454,13.8107088692922));
#42592=CARTESIAN_POINT('Ctrl Pts',(2.15797297046829,4.03985548762697,13.7842515726078));
#42593=CARTESIAN_POINT('Ctrl Pts',(2.80803461291788,3.61831747015607,13.7577942759233));
#42594=CARTESIAN_POINT('Ctrl Pts',(3.31769882312725,3.06699138623137,13.7313369792388));
#42595=CARTESIAN_POINT('Ctrl Pts',(3.82736303333661,2.51566530230669,13.7048796825544));
#42596=CARTESIAN_POINT('Ctrl Pts',(4.19662981130577,1.83455115192822,13.6784223858699));
#42597=CARTESIAN_POINT('Ctrl Pts',(4.38052287215716,1.10660788480175,13.6519650891854));
#42598=CARTESIAN_POINT('Ctrl Pts',(4.47176471220886,0.745425777992701,13.6388378269543));
#42599=CARTESIAN_POINT('Ctrl Pts',(4.5173707651647,0.372715156596874,13.6257105647231));
#42600=CARTESIAN_POINT('Ctrl Pts',(4.51736305946108,2.68251383689355E-6,
13.612583302492));
#42601=CARTESIAN_POINT('Origin',(0.,0.,20.5));
#42602=CARTESIAN_POINT('',(4.51804648040592,6.99590604930078E-5,12.612583302492));
#42603=CARTESIAN_POINT('',(4.51741195309898,-5.96473381690886E-5,12.8874166975081));
#42604=CARTESIAN_POINT('',(4.51775,5.53264807684796E-16,20.5));
#42605=CARTESIAN_POINT('Ctrl Pts',(4.51741195309898,-5.96473381690886E-5,
12.8874166975081));
#42606=CARTESIAN_POINT('Ctrl Pts',(4.51720574953279,0.442550368129689,12.9030062956018));
#42607=CARTESIAN_POINT('Ctrl Pts',(4.45260272288938,0.885219283315433,12.9185958936956));
#42608=CARTESIAN_POINT('Ctrl Pts',(4.32446175047221,1.30866046509405,12.9341854917894));
#42609=CARTESIAN_POINT('Ctrl Pts',(4.10699214642681,2.02728764889691,12.9606427884738));
#42610=CARTESIAN_POINT('Ctrl Pts',(3.70652120381657,2.69053531250561,12.9871000851583));
#42611=CARTESIAN_POINT('Ctrl Pts',(3.1718258402377,3.21762062452953,13.0135573818428));
#42612=CARTESIAN_POINT('Ctrl Pts',(2.63713047665883,3.74470593655345,13.0400146785272));
#42613=CARTESIAN_POINT('Ctrl Pts',(1.96821069211135,4.13562889699258,13.0664719752117));
#42614=CARTESIAN_POINT('Ctrl Pts',(1.24654017603871,4.34277552191208,13.0929292718962));
#42615=CARTESIAN_POINT('Ctrl Pts',(0.524869659966072,4.54992214683159,13.1193865685806));
#42616=CARTESIAN_POINT('Ctrl Pts',(-0.249551587631711,4.57329243623147,
13.1458438652651));
#42617=CARTESIAN_POINT('Ctrl Pts',(-0.98239991587342,4.41003991472745,13.1723011619496));
#42618=CARTESIAN_POINT('Ctrl Pts',(-1.71524824411517,4.24678739322342,13.198758458634));
#42619=CARTESIAN_POINT('Ctrl Pts',(-2.40652365300083,3.89691206081547,13.2252157553185));
#42620=CARTESIAN_POINT('Ctrl Pts',(-2.97202956278422,3.40302834577293,13.251673052003));
#42621=CARTESIAN_POINT('Ctrl Pts',(-3.53753547256757,2.90914463073042,13.2781303486874));
#42622=CARTESIAN_POINT('Ctrl Pts',(-3.97727188324865,2.27125253305334,13.3045876453719));
#42623=CARTESIAN_POINT('Ctrl Pts',(-4.23767938667653,1.56704660426365,13.3310449420564));
#42624=CARTESIAN_POINT('Ctrl Pts',(-4.49808689010441,0.862840675473956,
13.3575022387408));
#42625=CARTESIAN_POINT('Ctrl Pts',(-4.57916548627907,0.0923209155716644,
13.3839595354253));
#42626=CARTESIAN_POINT('Ctrl Pts',(-4.47103989191868,-0.650664221445422,
13.4104168321098));
#42627=CARTESIAN_POINT('Ctrl Pts',(-4.36291429755829,-1.39364935846249,
13.4368741287942));
#42628=CARTESIAN_POINT('Ctrl Pts',(-4.06558451266282,-2.1090998725944,13.4633314254787));
#42629=CARTESIAN_POINT('Ctrl Pts',(-3.61526497596841,-2.70987468303122,
13.4897887221632));
#42630=CARTESIAN_POINT('Ctrl Pts',(-3.16494543927398,-3.31064949346807,
13.5162460188477));
#42631=CARTESIAN_POINT('Ctrl Pts',(-2.56163615078063,-3.79674860020983,
13.5427033155321));
#42632=CARTESIAN_POINT('Ctrl Pts',(-1.87881951412554,-4.10896567003649,
13.5691606122166));
#42633=CARTESIAN_POINT('Ctrl Pts',(-1.19600287747047,-4.42118273986315,
13.5956179089011));
#42634=CARTESIAN_POINT('Ctrl Pts',(-0.43367889265364,-4.55951777277468,
13.6220752055855));
#42635=CARTESIAN_POINT('Ctrl Pts',(0.315302222661903,-4.50712171486214,
13.64853250227));
#42636=CARTESIAN_POINT('Ctrl Pts',(1.06428333797747,-4.4547256569496,13.6749897989545));
#42637=CARTESIAN_POINT('Ctrl Pts',(1.7999215837918,-4.211598508213,13.7014470956389));
#42638=CARTESIAN_POINT('Ctrl Pts',(2.43261703591854,-3.80735288629203,13.7279043923234));
#42639=CARTESIAN_POINT('Ctrl Pts',(3.06531248804526,-3.40310726437108,13.7543616890079));
#42640=CARTESIAN_POINT('Ctrl Pts',(3.59506514648438,-2.8377431692658,13.7808189856923));
#42641=CARTESIAN_POINT('Ctrl Pts',(3.95735172373184,-2.18012132205388,13.8072762823768));
#42642=CARTESIAN_POINT('Ctrl Pts',(4.3196383009793,-1.52249947484199,13.8337335790613));
#42643=CARTESIAN_POINT('Ctrl Pts',(4.51445879703509,-0.772619875523486,
13.8601908757457));
#42644=CARTESIAN_POINT('Ctrl Pts',(4.51808429109356,-0.0218170293801791,
13.8866481724302));
#42645=CARTESIAN_POINT('Ctrl Pts',(4.51811939524822,-0.0145473169490636,
13.8869043474562));
#42646=CARTESIAN_POINT('Ctrl Pts',(4.5181365744023,-0.0072775179612929,
13.8871605224821));
#42647=CARTESIAN_POINT('Ctrl Pts',(4.51813584929441,-7.71553139285741E-6,
13.8874166975081));
#42648=CARTESIAN_POINT('Ctrl Pts',(4.51736305946108,2.68251383689355E-6,
13.612583302492));
#42649=CARTESIAN_POINT('Ctrl Pts',(4.51735523473014,-0.378466950622669,
13.5992532680387));
#42650=CARTESIAN_POINT('Ctrl Pts',(4.47031360843327,-0.756938494124053,
13.5859232335853));
#42651=CARTESIAN_POINT('Ctrl Pts',(4.37626124565255,-1.12334284793068,13.572593199132));
#42652=CARTESIAN_POINT('Ctrl Pts',(4.18958721456293,-1.85057792966208,13.5461359024476));
#42653=CARTESIAN_POINT('Ctrl Pts',(3.81771980865007,-2.53027570925035,13.5196786057631));
#42654=CARTESIAN_POINT('Ctrl Pts',(3.3059520663969,-3.07964974938441,13.4932213090786));
#42655=CARTESIAN_POINT('Ctrl Pts',(2.79418432414376,-3.62902378951843,13.4667640123941));
#42656=CARTESIAN_POINT('Ctrl Pts',(2.14251624555032,-4.04807409019825,13.4403067157097));
#42657=CARTESIAN_POINT('Ctrl Pts',(1.43032028136785,-4.28576078857712,13.4138494190252));
#42658=CARTESIAN_POINT('Ctrl Pts',(0.718124317185353,-4.523447486956,13.3873921223408));
#42659=CARTESIAN_POINT('Ctrl Pts',(-0.0545995325861841,-4.57977058303392,
13.3609348256563));
#42660=CARTESIAN_POINT('Ctrl Pts',(-0.793734358242206,-4.44786998604312,
13.3344775289718));
#42661=CARTESIAN_POINT('Ctrl Pts',(-1.53286918389827,-4.31596938905231,
13.3080202322873));
#42662=CARTESIAN_POINT('Ctrl Pts',(-2.23841498543881,-3.99584509899276,
13.2815629356029));
#42663=CARTESIAN_POINT('Ctrl Pts',(-2.82443706508576,-3.52648790010218,
13.2551056389184));
#42664=CARTESIAN_POINT('Ctrl Pts',(-3.41045914473268,-3.05713070121163,
13.2286483422339));
#42665=CARTESIAN_POINT('Ctrl Pts',(-3.87695750248602,-2.43854059349005,
13.2021910455495));
#42666=CARTESIAN_POINT('Ctrl Pts',(-4.16711315465972,-1.74606116744496,
13.175733748865));
#42667=CARTESIAN_POINT('Ctrl Pts',(-4.45726880683343,-1.05358174139987,
13.1492764521805));
#42668=CARTESIAN_POINT('Ctrl Pts',(-4.57108175342749,-0.287212997031258,
13.1228191554961));
#42669=CARTESIAN_POINT('Ctrl Pts',(-4.49468970350711,0.459702200761001,
13.0963618588116));
#42670=CARTESIAN_POINT('Ctrl Pts',(-4.41829765358673,1.20661739855328,13.0699045621271));
#42671=CARTESIAN_POINT('Ctrl Pts',(-4.15170060715189,1.93407904976921,13.0434472654427));
#42672=CARTESIAN_POINT('Ctrl Pts',(-3.72736978940707,2.5534831303952,13.0169899687582));
#42673=CARTESIAN_POINT('Ctrl Pts',(-3.30303897166226,3.1728872110212,12.9905326720737));
#42674=CARTESIAN_POINT('Ctrl Pts',(-2.72097438260746,3.68423372105726,12.9640753753893));
#42675=CARTESIAN_POINT('Ctrl Pts',(-2.05207084500052,4.02524122150415,12.9376180787048));
#42676=CARTESIAN_POINT('Ctrl Pts',(-1.3831673073936,4.36624872195103,12.9111607820203));
#42677=CARTESIAN_POINT('Ctrl Pts',(-0.627424821234523,4.53691721280875,
12.8847034853359));
#42678=CARTESIAN_POINT('Ctrl Pts',(0.123108015066336,4.51645946077498,12.8582461886514));
#42679=CARTESIAN_POINT('Ctrl Pts',(0.873640851367194,4.49600170874121,12.8317888919669));
#42680=CARTESIAN_POINT('Ctrl Pts',(1.61896403780984,4.28441771381596,12.8053315952824));
#42681=CARTESIAN_POINT('Ctrl Pts',(2.268298035158,3.9074781724145,12.778874298598));
#42682=CARTESIAN_POINT('Ctrl Pts',(2.91763203250619,3.53053863101303,12.7524170019135));
#42683=CARTESIAN_POINT('Ctrl Pts',(3.47097684075988,2.98824354313534,12.7259597052291));
#42684=CARTESIAN_POINT('Ctrl Pts',(3.86093567467777,2.34664385031004,12.6995024085446));
#42685=CARTESIAN_POINT('Ctrl Pts',(4.25089450859566,1.70504415748472,12.6730451118601));
#42686=CARTESIAN_POINT('Ctrl Pts',(4.47746736817774,0.964139859711776,12.6465878151756));
#42687=CARTESIAN_POINT('Ctrl Pts',(4.51305792988216,0.214172280478037,12.6201305184912));
#42688=CARTESIAN_POINT('Ctrl Pts',(4.51644212114351,0.142860291950876,12.6176147798248));
#42689=CARTESIAN_POINT('Ctrl Pts',(4.51809954743677,0.0714663578345357,
12.6150990411584));
#42690=CARTESIAN_POINT('Ctrl Pts',(4.51804648040592,6.99590604930078E-5,
12.612583302492));
#42691=CARTESIAN_POINT('Origin',(0.,0.,20.5));
#42692=CARTESIAN_POINT('',(4.5175801641472,-0.000107849321499542,11.612583302492));
#42693=CARTESIAN_POINT('',(4.5178502562812,0.000110962492481057,11.8874166975081));
#42694=CARTESIAN_POINT('',(4.51775,5.53264807684796E-16,20.5));
#42695=CARTESIAN_POINT('Ctrl Pts',(4.5178502562812,0.000110962492481057,
11.8874166975081));
#42696=CARTESIAN_POINT('Ctrl Pts',(4.51799453028332,0.141405931765494,11.8923947720371));
#42697=CARTESIAN_POINT('Ctrl Pts',(4.51149711848843,0.282687684813822,11.8973728465661));
#42698=CARTESIAN_POINT('Ctrl Pts',(4.49826065670895,0.423335220010937,11.9023509210951));
#42699=CARTESIAN_POINT('Ctrl Pts',(4.42791197182862,1.17084382900464,11.9288082177796));
#42700=CARTESIAN_POINT('Ctrl Pts',(4.16720717585505,1.90043785893767,11.955265514464));
#42701=CARTESIAN_POINT('Ctrl Pts',(3.7478998244077,2.5232535644287,11.9817228111485));
#42702=CARTESIAN_POINT('Ctrl Pts',(3.32859247296032,3.14606926991974,12.008180107833));
#42703=CARTESIAN_POINT('Ctrl Pts',(2.75068256603915,3.66210665096878,12.0346374045175));
#42704=CARTESIAN_POINT('Ctrl Pts',(2.08455889071624,4.00851292567871,12.0610947012019));
#42705=CARTESIAN_POINT('Ctrl Pts',(1.41843521539332,4.35491920038864,12.0875519978864));
#42706=CARTESIAN_POINT('Ctrl Pts',(0.664097771668666,4.53169436875946,12.1140092945709));
#42707=CARTESIAN_POINT('Ctrl Pts',(-0.0865759746608722,4.51730741092621,
12.1404665912553));
#42708=CARTESIAN_POINT('Ctrl Pts',(-0.83724972099039,4.50292045309296,12.1669238879398));
#42709=CARTESIAN_POINT('Ctrl Pts',(-1.58425976992479,4.29737136905566,12.1933811846243));
#42710=CARTESIAN_POINT('Ctrl Pts',(-2.23662112424321,3.92569580976245,12.2198384813087));
#42711=CARTESIAN_POINT('Ctrl Pts',(-2.88898247856163,3.55402025046923,12.2462957779932));
#42712=CARTESIAN_POINT('Ctrl Pts',(-3.44669513826407,3.01621821592011,12.2727530746777));
#42713=CARTESIAN_POINT('Ctrl Pts',(-3.84183031863679,2.37779339872086,12.2992103713621));
#42714=CARTESIAN_POINT('Ctrl Pts',(-4.23696549900952,1.7393685815216,12.3256676680466));
#42715=CARTESIAN_POINT('Ctrl Pts',(-4.46952320005253,1.00032098167222,12.3521249647311));
#42716=CARTESIAN_POINT('Ctrl Pts',(-4.51117815115765,0.250665778907295,
12.3785822614155));
#42717=CARTESIAN_POINT('Ctrl Pts',(-4.55283310226278,-0.498989423857626,
12.4050395581));
#42718=CARTESIAN_POINT('Ctrl Pts',(-4.40358530343001,-1.25925222953809,
12.4314968547845));
#42719=CARTESIAN_POINT('Ctrl Pts',(-4.08161297138,-1.93752346980879,12.4579541514689));
#42720=CARTESIAN_POINT('Ctrl Pts',(-3.75964063932998,-2.61579471007952,
12.4844114481534));
#42721=CARTESIAN_POINT('Ctrl Pts',(-3.26494377406269,-3.21207438494048,
12.5108687448379));
#42722=CARTESIAN_POINT('Ctrl Pts',(-2.65777590627122,-3.65373628991496,
12.5373260415223));
#42723=CARTESIAN_POINT('Ctrl Pts',(-2.05060803847976,-4.09539819488944,
12.5637833382068));
#42724=CARTESIAN_POINT('Ctrl Pts',(-1.33096916816412,-4.38244232997743,
12.5902406348913));
#42725=CARTESIAN_POINT('Ctrl Pts',(-0.586510513281939,-4.47990703720592,
12.6166979315757));
#42726=CARTESIAN_POINT('Ctrl Pts',(0.15794814160022,-4.57737174443441,12.6431552282602));
#42727=CARTESIAN_POINT('Ctrl Pts',(0.927226581048916,-4.48525702380341,
12.6696125249447));
#42728=CARTESIAN_POINT('Ctrl Pts',(1.62762754252377,-4.21478234633953,12.6960698216291));
#42729=CARTESIAN_POINT('Ctrl Pts',(2.32802850399863,-3.94430766887566,12.7225271183136));
#42730=CARTESIAN_POINT('Ctrl Pts',(2.95955198749964,-3.49547303457892,12.7489844149981));
#42731=CARTESIAN_POINT('Ctrl Pts',(3.44527913166315,-2.92294600516735,12.7754417116826));
#42732=CARTESIAN_POINT('Ctrl Pts',(3.93100627582668,-2.35041897575576,12.801899008367));
#42733=CARTESIAN_POINT('Ctrl Pts',(4.2709370806527,-1.65419955122932,12.8283563050515));
#42734=CARTESIAN_POINT('Ctrl Pts',(4.42366835032544,-0.919086486967588,
12.854813601736));
#42735=CARTESIAN_POINT('Ctrl Pts',(4.48640482049374,-0.617128682745771,
12.8656813003267));
#42736=CARTESIAN_POINT('Ctrl Pts',(4.51755570011492,-0.308608476653881,
12.8765489989174));
#42737=CARTESIAN_POINT('Ctrl Pts',(4.51741195309898,-5.96473381690886E-5,
12.8874166975081));
#42738=CARTESIAN_POINT('Ctrl Pts',(4.51804648040592,6.99590604930078E-5,
12.612583302492));
#42739=CARTESIAN_POINT('Ctrl Pts',(4.51754145680588,-0.679388939577024,
12.5886417444739));
#42740=CARTESIAN_POINT('Ctrl Pts',(4.36212083370235,-1.35907105681478,12.5647001864558));
#42741=CARTESIAN_POINT('Ctrl Pts',(4.06580926285153,-1.97047118281595,12.5407586284378));
#42742=CARTESIAN_POINT('Ctrl Pts',(3.73836177028969,-2.64611620618181,12.5143013317533));
#42743=CARTESIAN_POINT('Ctrl Pts',(3.23885852133923,-3.23837539221903,12.4878440350688));
#42744=CARTESIAN_POINT('Ctrl Pts',(2.62813845890645,-3.67511222754003,12.4613867383844));
#42745=CARTESIAN_POINT('Ctrl Pts',(2.01741839647366,-4.11184906286103,12.4349294416999));
#42746=CARTESIAN_POINT('Ctrl Pts',(1.29548152055856,-4.3930635474658,12.4084721450154));
#42747=CARTESIAN_POINT('Ctrl Pts',(0.550258943657521,-4.48450406835832,
12.382014848331));
#42748=CARTESIAN_POINT('Ctrl Pts',(-0.194963633243496,-4.57594458925083,
12.3555575516465));
#42749=CARTESIAN_POINT('Ctrl Pts',(-0.963471911130448,-4.47761114643111,
12.329100254962));
#42750=CARTESIAN_POINT('Ctrl Pts',(-1.66166243228881,-4.2014806444059,12.3026429582776));
#42751=CARTESIAN_POINT('Ctrl Pts',(-2.35985295344718,-3.92535014238069,
12.2761856615931));
#42752=CARTESIAN_POINT('Ctrl Pts',(-2.98772571787696,-3.47142258114999,
12.2497283649086));
#42753=CARTESIAN_POINT('Ctrl Pts',(-3.46880651775701,-2.89498583529589,
12.2232710682242));
#42754=CARTESIAN_POINT('Ctrl Pts',(-3.94988731763707,-2.31854908944178,
12.1968137715397));
#42755=CARTESIAN_POINT('Ctrl Pts',(-4.28417615296739,-1.61960315896426,
12.1703564748552));
#42756=CARTESIAN_POINT('Ctrl Pts',(-4.43095701357263,-0.883278884650216,
12.1438991781708));
#42757=CARTESIAN_POINT('Ctrl Pts',(-4.57773787417786,-0.146954610336191,
12.1174418814863));
#42758=CARTESIAN_POINT('Ctrl Pts',(-4.53701076005802,0.626748007814359,
12.0909845848018));
#42759=CARTESIAN_POINT('Ctrl Pts',(-4.31373618863893,1.34359284719155,12.0645272881174));
#42760=CARTESIAN_POINT('Ctrl Pts',(-4.09046161721984,2.06043768656874,12.0380699914329));
#42761=CARTESIAN_POINT('Ctrl Pts',(-3.6846395885015,2.72042474717257,12.0116126947484));
#42762=CARTESIAN_POINT('Ctrl Pts',(-3.1456987764459,3.24316833544978,11.985155398064));
#42763=CARTESIAN_POINT('Ctrl Pts',(-2.60675796439029,3.76591192372701,11.9586981013795));
#42764=CARTESIAN_POINT('Ctrl Pts',(-1.9346983689974,4.15141203967762,11.932240804695));
#42765=CARTESIAN_POINT('Ctrl Pts',(-1.21137610519676,4.35271519582384,11.9057835080105));
#42766=CARTESIAN_POINT('Ctrl Pts',(-0.488053841396109,4.55401835197005,
11.8793262113261));
#42767=CARTESIAN_POINT('Ctrl Pts',(0.286531090812296,4.57112454831187,11.8528689146416));
#42768=CARTESIAN_POINT('Ctrl Pts',(1.0180351039428,4.40195026906683,11.8264116179572));
#42769=CARTESIAN_POINT('Ctrl Pts',(1.74953911707329,4.2327759898218,11.7999543212727));
#42770=CARTESIAN_POINT('Ctrl Pts',(2.43796221112589,3.8773212349899,11.7734970245882));
#42771=CARTESIAN_POINT('Ctrl Pts',(2.99945521514432,3.37888000031681,11.7470397279037));
#42772=CARTESIAN_POINT('Ctrl Pts',(3.56094821916276,2.88043876564371,11.7205824312193));
#42773=CARTESIAN_POINT('Ctrl Pts',(3.99551113314703,2.23901105112941,11.6941251345348));
#42774=CARTESIAN_POINT('Ctrl Pts',(4.2502146751182,1.53272204251365,11.6676678378503));
#42775=CARTESIAN_POINT('Ctrl Pts',(4.42698035695052,1.0425535226241,11.6493063260642));
#42776=CARTESIAN_POINT('Ctrl Pts',(4.51711789485057,0.521144965264365,11.6309448142781));
#42777=CARTESIAN_POINT('Ctrl Pts',(4.5175801641472,-0.000107849321499542,
11.612583302492));
#42778=CARTESIAN_POINT('Origin',(0.,0.,20.5));
#42779=CARTESIAN_POINT('',(4.517607537138,0.000111184246189833,10.612583302492));
#42780=CARTESIAN_POINT('',(4.51779144669394,-0.000115517084662978,10.8874166975081));
#42781=CARTESIAN_POINT('',(4.51775,5.53264807684796E-16,20.5));
#42782=CARTESIAN_POINT('Ctrl Pts',(4.51779144669394,-0.000115517084662978,
10.8874166975081));
#42783=CARTESIAN_POINT('Ctrl Pts',(4.51718124885461,0.590959459307199,10.9082405451568));
#42784=CARTESIAN_POINT('Ctrl Pts',(4.40057028871007,1.18226809182004,10.9290643928055));
#42785=CARTESIAN_POINT('Ctrl Pts',(4.17452335103026,1.72826978099499,10.9498882404543));
#42786=CARTESIAN_POINT('Ctrl Pts',(3.88732422262257,2.42198061313325,10.9763455371387));
#42787=CARTESIAN_POINT('Ctrl Pts',(3.42346880605941,3.0425550177638,11.0028028338232));
#42788=CARTESIAN_POINT('Ctrl Pts',(2.83945417771489,3.51440771921171,11.0292601305077));
#42789=CARTESIAN_POINT('Ctrl Pts',(2.25543954937037,3.98626042065963,11.0557174271921));
#42790=CARTESIAN_POINT('Ctrl Pts',(1.55126570924448,4.30939141892491,11.0821747238766));
#42791=CARTESIAN_POINT('Ctrl Pts',(0.812700251733397,4.44444371603802,11.1086320205611));
#42792=CARTESIAN_POINT('Ctrl Pts',(0.0741347942222902,4.57949601315113,
11.1350893172455));
#42793=CARTESIAN_POINT('Ctrl Pts',(-0.698822280674023,4.52646960911206,
11.16154661393));
#42794=CARTESIAN_POINT('Ctrl Pts',(-1.41202565668891,4.29182306124677,11.1880039106145));
#42795=CARTESIAN_POINT('Ctrl Pts',(-2.12522903270377,4.0571765133815,11.2144612072989));
#42796=CARTESIAN_POINT('Ctrl Pts',(-2.7786787098372,3.64090982169003,11.2409185039834));
#42797=CARTESIAN_POINT('Ctrl Pts',(-3.29278524060752,3.09372380852504,11.2673758006679));
#42798=CARTESIAN_POINT('Ctrl Pts',(-3.80689177137783,2.54653779536005,11.2938330973523));
#42799=CARTESIAN_POINT('Ctrl Pts',(-4.18165515578503,1.86843246072154,11.3202903940368));
#42800=CARTESIAN_POINT('Ctrl Pts',(-4.37142962837066,1.14200028388812,11.3467476907213));
#42801=CARTESIAN_POINT('Ctrl Pts',(-4.56120410095629,0.415568107054687,
11.3732049874058));
#42802=CARTESIAN_POINT('Ctrl Pts',(-4.56598966172034,-0.359190911973653,
11.3996622840902));
#42803=CARTESIAN_POINT('Ctrl Pts',(-4.38520343465808,-1.08791198212924,
11.4261195807747));
#42804=CARTESIAN_POINT('Ctrl Pts',(-4.20441720759582,-1.81663305228484,
11.4525768774592));
#42805=CARTESIAN_POINT('Ctrl Pts',(-3.83805919270723,-2.49931617356768,
11.4790341741436));
#42806=CARTESIAN_POINT('Ctrl Pts',(-3.33075139074592,-3.05281129735225,
11.5054914708281));
#42807=CARTESIAN_POINT('Ctrl Pts',(-2.82344358878461,-3.6063064211368,11.5319487675126));
#42808=CARTESIAN_POINT('Ctrl Pts',(-2.17518599975058,-4.03061354742309,
11.558406064197));
#42809=CARTESIAN_POINT('Ctrl Pts',(-1.46493568054124,-4.27405253782339,
11.5848633608815));
#42810=CARTESIAN_POINT('Ctrl Pts',(-0.7546853613319,-4.51749152822369,11.611320657566));
#42811=CARTESIAN_POINT('Ctrl Pts',(0.017557688052746,-4.580062382738,11.6377779542504));
#42812=CARTESIAN_POINT('Ctrl Pts',(0.757735118863148,-4.4541440405356,11.6642352509349));
#42813=CARTESIAN_POINT('Ctrl Pts',(1.49791254967357,-4.3282256983332,11.6906925476194));
#42814=CARTESIAN_POINT('Ctrl Pts',(2.20602436190975,-4.01381815941408,11.7171498443038));
#42815=CARTESIAN_POINT('Ctrl Pts',(2.79582332053076,-3.54921591405394,11.7436071409883));
#42816=CARTESIAN_POINT('Ctrl Pts',(3.38562227915178,-3.0846136686938,11.7700644376728));
#42817=CARTESIAN_POINT('Ctrl Pts',(3.85710838415764,-2.46981671689265,11.7965217343572));
#42818=CARTESIAN_POINT('Ctrl Pts',(4.15285514976701,-1.77970664696488,11.8229790310417));
#42819=CARTESIAN_POINT('Ctrl Pts',(4.39295566177474,-1.21944428605644,11.8444582531972));
#42820=CARTESIAN_POINT('Ctrl Pts',(4.51722774785459,-0.609543637247958,
11.8659374753526));
#42821=CARTESIAN_POINT('Ctrl Pts',(4.5178502562812,0.000110962492481057,
11.8874166975081));
#42822=CARTESIAN_POINT('Ctrl Pts',(4.5175801641472,-0.000107849321499542,
11.612583302492));
#42823=CARTESIAN_POINT('Ctrl Pts',(4.51778398357309,-0.229933732598545,
11.6044875175936));
#42824=CARTESIAN_POINT('Ctrl Pts',(4.50055473854231,-0.45972933914648,11.5963917326953));
#42825=CARTESIAN_POINT('Ctrl Pts',(4.46563124792392,-0.686803612223187,
11.5882959477969));
#42826=CARTESIAN_POINT('Ctrl Pts',(4.35150010880038,-1.42888995562703,11.5618386511125));
#42827=CARTESIAN_POINT('Ctrl Pts',(4.04839366059521,-2.14191233971748,11.535381354428));
#42828=CARTESIAN_POINT('Ctrl Pts',(3.59322993324244,-2.73902542723646,11.5089240577435));
#42829=CARTESIAN_POINT('Ctrl Pts',(3.13806620588969,-3.33613851475543,11.4824667610591));
#42830=CARTESIAN_POINT('Ctrl Pts',(2.53084519938934,-3.81734230570294,11.4560094643746));
#42831=CARTESIAN_POINT('Ctrl Pts',(1.84552576030269,-4.12402671090484,11.4295521676901));
#42832=CARTESIAN_POINT('Ctrl Pts',(1.16020632121604,-4.43071111610674,11.4030948710056));
#42833=CARTESIAN_POINT('Ctrl Pts',(0.396788449543078,-4.56287613556304,
11.3766375743212));
#42834=CARTESIAN_POINT('Ctrl Pts',(-0.351744402844812,-4.50442421617511,
11.3501802776367));
#42835=CARTESIAN_POINT('Ctrl Pts',(-1.10027725523272,-4.44597229678718,
11.3237229809523));
#42836=CARTESIAN_POINT('Ctrl Pts',(-1.83392508833558,-4.196903438555,11.2972656842678));
#42837=CARTESIAN_POINT('Ctrl Pts',(-2.4633304080324,-3.787553952759,11.2708083875833));
#42838=CARTESIAN_POINT('Ctrl Pts',(-3.0927357277292,-3.378204466963,11.2443510908988));
#42839=CARTESIAN_POINT('Ctrl Pts',(-3.61789853401999,-2.80857435360317,
11.2178937942144));
#42840=CARTESIAN_POINT('Ctrl Pts',(-3.97485457831262,-2.1480439300593,11.1914364975299));
#42841=CARTESIAN_POINT('Ctrl Pts',(-4.33181062260526,-1.48751350651541,
11.1649792008454));
#42842=CARTESIAN_POINT('Ctrl Pts',(-4.52055990489972,-0.736082772787468,
11.138521904161));
#42843=CARTESIAN_POINT('Ctrl Pts',(-4.51811297150728,0.0147248393883086,
11.1120646074765));
#42844=CARTESIAN_POINT('Ctrl Pts',(-4.51566603811484,0.765532451564064,
11.085607310792));
#42845=CARTESIAN_POINT('Ctrl Pts',(-4.32202288903552,1.5157169421876,11.0591500141076));
#42846=CARTESIAN_POINT('Ctrl Pts',(-3.96076904551623,2.17390667055369,11.0326927174231));
#42847=CARTESIAN_POINT('Ctrl Pts',(-3.59951520199693,2.83209639891979,11.0062354207386));
#42848=CARTESIAN_POINT('Ctrl Pts',(-3.07065066403766,3.3982913650284,10.9797781240542));
#42849=CARTESIAN_POINT('Ctrl Pts',(-2.43859054705097,3.8035296486331,10.9533208273697));
#42850=CARTESIAN_POINT('Ctrl Pts',(-1.8065304300643,4.20876793223779,10.9268635306852));
#42851=CARTESIAN_POINT('Ctrl Pts',(-1.0712747340502,4.4530495333386,10.9004062340008));
#42852=CARTESIAN_POINT('Ctrl Pts',(-0.322376789052762,4.50662122327553,
10.8739489373163));
#42853=CARTESIAN_POINT('Ctrl Pts',(0.426521155944698,4.56019291321245,10.8474916406318));
#42854=CARTESIAN_POINT('Ctrl Pts',(1.18906134992551,4.42305469198549,10.8210343439474));
#42855=CARTESIAN_POINT('Ctrl Pts',(1.87236724118984,4.11190984316492,10.7945770472629));
#42856=CARTESIAN_POINT('Ctrl Pts',(2.55567313245417,3.80076499434435,10.7681197505784));
#42857=CARTESIAN_POINT('Ctrl Pts',(3.15974472100203,3.31561351793017,10.741662453894));
#42858=CARTESIAN_POINT('Ctrl Pts',(3.61100675589317,2.71554632681736,10.7152051572095));
#42859=CARTESIAN_POINT('Ctrl Pts',(4.0622687907843,2.11547913570456,10.688747860525));
#42860=CARTESIAN_POINT('Ctrl Pts',(4.36072127201872,1.40049622989312,10.6622905638405));
#42861=CARTESIAN_POINT('Ctrl Pts',(4.47001301768877,0.657681736016976,10.6358332671561));
#42862=CARTESIAN_POINT('Ctrl Pts',(4.5020272386327,0.440093233047143,10.6280832789347));
#42863=CARTESIAN_POINT('Ctrl Pts',(4.51781057668589,0.220116648612125,10.6203332907133));
#42864=CARTESIAN_POINT('Ctrl Pts',(4.517607537138,0.000111184246189833,
10.612583302492));
#42865=CARTESIAN_POINT('Origin',(0.,0.,20.5));
#42866=CARTESIAN_POINT('',(4.51802315729813,-7.77880120685776E-5,9.61258330249199));
#42867=CARTESIAN_POINT('',(4.5174420818448,7.39595355181285E-5,9.88741669750808));
#42868=CARTESIAN_POINT('',(4.51775,5.53264807684796E-16,20.5));
#42869=CARTESIAN_POINT('Ctrl Pts',(4.5174420818448,7.39595355181285E-5,
9.88741669750808));
#42870=CARTESIAN_POINT('Ctrl Pts',(4.51761100468578,0.290010274247371,9.89762902159206));
#42871=CARTESIAN_POINT('Ctrl Pts',(4.49012793116805,0.579914973420611,9.90784134567604));
#42872=CARTESIAN_POINT('Ctrl Pts',(4.43468447094956,0.864369878764984,9.91805366976002));
#42873=CARTESIAN_POINT('Ctrl Pts',(4.29104585704042,1.60131357171471,9.94451096644449));
#42874=CARTESIAN_POINT('Ctrl Pts',(3.95974153092839,2.30167910674412,9.97096826312895));
#42875=CARTESIAN_POINT('Ctrl Pts',(3.48112399286906,2.88016273680304,9.99742555981342));
#42876=CARTESIAN_POINT('Ctrl Pts',(3.00250645480973,3.45864636686196,10.0238828564979));
#42877=CARTESIAN_POINT('Ctrl Pts',(2.3765757048031,3.91524809195038,10.0503401531824));
#42878=CARTESIAN_POINT('Ctrl Pts',(1.67956941546288,4.19435432728793,10.0767974498668));
#42879=CARTESIAN_POINT('Ctrl Pts',(0.982563126122689,4.47346056262548,10.1032547465513));
#42880=CARTESIAN_POINT('Ctrl Pts',(0.214481297448898,4.57507130821216,10.1297120432358));
#42881=CARTESIAN_POINT('Ctrl Pts',(-0.531124553886154,4.4868104876913,10.1561693399202));
#42882=CARTESIAN_POINT('Ctrl Pts',(-1.27673040522121,4.39854966717044,10.1826266366047));
#42883=CARTESIAN_POINT('Ctrl Pts',(-1.99986027921753,4.12041728054204,10.2090839332892));
#42884=CARTESIAN_POINT('Ctrl Pts',(-2.61243775753278,3.68628954467964,10.2355412299736));
#42885=CARTESIAN_POINT('Ctrl Pts',(-3.22501523584806,3.25216180881724,10.2619985266581));
#42886=CARTESIAN_POINT('Ctrl Pts',(-3.72704031848226,2.66203872372082,10.2884558233426));
#42887=CARTESIAN_POINT('Ctrl Pts',(-4.05736690597737,1.9877966280475,10.314913120027));
#42888=CARTESIAN_POINT('Ctrl Pts',(-4.38769349347249,1.31355453237416,10.3413704167115));
#42889=CARTESIAN_POINT('Ctrl Pts',(-4.54632158582851,0.555193426123966,
10.367827713396));
#42890=CARTESIAN_POINT('Ctrl Pts',(-4.51393045695515,-0.194919147263826,
10.3942850100804));
#42891=CARTESIAN_POINT('Ctrl Pts',(-4.48153932808179,-0.945031720651576,
10.4207423067649));
#42892=CARTESIAN_POINT('Ctrl Pts',(-4.25812897797905,-1.68689576117688,
10.4471996034494));
#42893=CARTESIAN_POINT('Ctrl Pts',(-3.87091054003425,-2.33015304974784,
10.4736569001339));
#42894=CARTESIAN_POINT('Ctrl Pts',(-3.48369210208944,-2.9734103383188,10.5001141968183));
#42895=CARTESIAN_POINT('Ctrl Pts',(-2.93266557630255,-3.51806087493544,
10.5265714935028));
#42896=CARTESIAN_POINT('Ctrl Pts',(-2.28494538367617,-3.89776682701959,
10.5530287901872));
#42897=CARTESIAN_POINT('Ctrl Pts',(-1.63722519104977,-4.27747277910375,
10.5794860868717));
#42898=CARTESIAN_POINT('Ctrl Pts',(-0.892811331583869,-4.49223414665542,
10.6059433835562));
#42899=CARTESIAN_POINT('Ctrl Pts',(-0.142372589495352,-4.51589323278992,
10.6324006802407));
#42900=CARTESIAN_POINT('Ctrl Pts',(0.608066152593165,-4.53955231892441,
10.6588579769251));
#42901=CARTESIAN_POINT('Ctrl Pts',(1.36452977730431,-4.37210912364174,10.6853152736096));
#42902=CARTESIAN_POINT('Ctrl Pts',(2.03488185235016,-4.03395804281271,10.7117725702941));
#42903=CARTESIAN_POINT('Ctrl Pts',(2.70523392739599,-3.6958069619837,10.7382298669785));
#42904=CARTESIAN_POINT('Ctrl Pts',(3.28947445277654,-3.18694799560833,10.764687163663));
#42905=CARTESIAN_POINT('Ctrl Pts',(3.71644357909769,-2.56935960262103,10.7911444603475));
#42906=CARTESIAN_POINT('Ctrl Pts',(4.14341270541885,-1.95177120963373,10.8176017570319));
#42907=CARTESIAN_POINT('Ctrl Pts',(4.41311043268061,-1.22545339003449,10.8440590537164));
#42908=CARTESIAN_POINT('Ctrl Pts',(4.49268787618539,-0.478870850411892,
10.8705163504009));
#42909=CARTESIAN_POINT('Ctrl Pts',(4.50963199098762,-0.319903940901298,
10.8761497994366));
#42910=CARTESIAN_POINT('Ctrl Pts',(4.51795652273981,-0.160018279147252,
10.8817832484723));
#42911=CARTESIAN_POINT('Ctrl Pts',(4.51779144669394,-0.000115517084662978,
10.8874166975081));
#42912=CARTESIAN_POINT('Ctrl Pts',(4.517607537138,0.000111184246189833,
10.612583302492));
#42913=CARTESIAN_POINT('Ctrl Pts',(4.51711743014117,-0.530948988737395,
10.5938759940289));
#42914=CARTESIAN_POINT('Ctrl Pts',(4.42347995325767,-1.06217743558981,10.5751686855658));
#42915=CARTESIAN_POINT('Ctrl Pts',(4.24013400258143,-1.56039266992325,10.5564613771027));
#42916=CARTESIAN_POINT('Ctrl Pts',(3.98083223169834,-2.26500650004656,10.5300040804182));
#42917=CARTESIAN_POINT('Ctrl Pts',(3.54209767982647,-2.90358807835227,10.5035467837338));
#42918=CARTESIAN_POINT('Ctrl Pts',(2.9773677298226,-3.39835887534092,10.4770894870493));
#42919=CARTESIAN_POINT('Ctrl Pts',(2.41263777981875,-3.89312967232955,10.4506321903648));
#42920=CARTESIAN_POINT('Ctrl Pts',(1.7219124316829,-4.24408968800111,10.4241748936803));
#42921=CARTESIAN_POINT('Ctrl Pts',(0.989321268370679,-4.40849238086523,
10.3977175969959));
#42922=CARTESIAN_POINT('Ctrl Pts',(0.256730105058482,-4.57289507372935,
10.3712603003114));
#42923=CARTESIAN_POINT('Ctrl Pts',(-0.517726873430066,-4.55074044378602,
10.3448030036269));
#42924=CARTESIAN_POINT('Ctrl Pts',(-1.2397216642308,-4.34472690044313,10.3183457069425));
#42925=CARTESIAN_POINT('Ctrl Pts',(-1.96171645503154,-4.13871335710024,
10.291888410258));
#42926=CARTESIAN_POINT('Ctrl Pts',(-2.63124905814445,-3.74884090035779,
10.2654311135735));
#42927=CARTESIAN_POINT('Ctrl Pts',(-3.16677114350303,-3.22259556396298,
10.2389738168891));
#42928=CARTESIAN_POINT('Ctrl Pts',(-3.70229322886161,-2.69635022756818,
10.2125165202046));
#42929=CARTESIAN_POINT('Ctrl Pts',(-4.10380479646586,-2.033732011521,10.1860592235201));
#42930=CARTESIAN_POINT('Ctrl Pts',(-4.32240218174696,-1.31544708119576,
10.1596019268357));
#42931=CARTESIAN_POINT('Ctrl Pts',(-4.54099956702807,-0.597162150870509,
10.1331446301512));
#42932=CARTESIAN_POINT('Ctrl Pts',(-4.57668276998605,0.176789493732823,
10.1066873334667));
#42933=CARTESIAN_POINT('Ctrl Pts',(-4.42510561599232,0.912141398858014,
10.0802300367823));
#42934=CARTESIAN_POINT('Ctrl Pts',(-4.27352846199858,1.64749330398323,10.0537727400978));
#42935=CARTESIAN_POINT('Ctrl Pts',(-3.93469095105313,2.34424546963029,10.0273154434133));
#42936=CARTESIAN_POINT('Ctrl Pts',(-3.44986311698706,2.91753425314077,10.0008581467289));
#42937=CARTESIAN_POINT('Ctrl Pts',(-2.965035282921,3.49082303665126,9.97440085004439));
#42938=CARTESIAN_POINT('Ctrl Pts',(-2.33421712573433,3.94064843802516,9.94794355335992));
#42939=CARTESIAN_POINT('Ctrl Pts',(-1.63424159882622,4.21222222121095,9.92148625667545));
#42940=CARTESIAN_POINT('Ctrl Pts',(-0.93426607191815,4.48379600439673,9.89502895999098));
#42941=CARTESIAN_POINT('Ctrl Pts',(-0.165133175288626,4.57711816939442,
9.86857166330652));
#42942=CARTESIAN_POINT('Ctrl Pts',(0.579477555476215,4.48082217978985,9.84211436662205));
#42943=CARTESIAN_POINT('Ctrl Pts',(1.32408828624107,4.38452619018528,9.81565706993759));
#42944=CARTESIAN_POINT('Ctrl Pts',(2.04417685114126,4.09861204597845,9.78919977325312));
#42945=CARTESIAN_POINT('Ctrl Pts',(2.65203725991646,3.65790377350364,9.76274247656865));
#42946=CARTESIAN_POINT('Ctrl Pts',(3.25989766869166,3.21719550102883,9.73628517988418));
#42947=CARTESIAN_POINT('Ctrl Pts',(3.75552992134187,2.62169310028604,9.70982788319971));
#42948=CARTESIAN_POINT('Ctrl Pts',(4.07856655802598,1.94392810462463,9.68337058651525));
#42949=CARTESIAN_POINT('Ctrl Pts',(4.36666460048778,1.33946797123696,9.65977482517416));
#42950=CARTESIAN_POINT('Ctrl Pts',(4.51748278690866,0.669577455247932,9.63617906383307));
#42951=CARTESIAN_POINT('Ctrl Pts',(4.51802315729813,-7.77880120685776E-5,
9.61258330249199));
#42952=CARTESIAN_POINT('Origin',(0.,0.,20.5));
#42953=CARTESIAN_POINT('',(4.51736326149566,6.46810088806768E-6,8.61258330249198));
#42954=CARTESIAN_POINT('',(4.51813428255233,-1.20076389504314E-5,8.88741669750808));
#42955=CARTESIAN_POINT('',(4.51775,5.53264807684796E-16,20.5));
#42956=CARTESIAN_POINT('Ctrl Pts',(4.51813428255233,-1.20076389504314E-5,
8.88741669750808));
#42957=CARTESIAN_POINT('Ctrl Pts',(4.51802118875718,0.73947229319191,8.91347479471178));
#42958=CARTESIAN_POINT('Ctrl Pts',(4.3327730937107,1.47901118956561,8.93953289191547));
#42959=CARTESIAN_POINT('Ctrl Pts',(3.9839812468855,2.13106899669204,8.96559098911917));
#42960=CARTESIAN_POINT('Ctrl Pts',(3.62984605042663,2.79311606496825,8.99204828580364));
#42961=CARTESIAN_POINT('Ctrl Pts',(3.10711787221281,3.36498116344761,9.01850558248812));
#42962=CARTESIAN_POINT('Ctrl Pts',(2.47946442583089,3.77701175603631,9.04496287917258));
#42963=CARTESIAN_POINT('Ctrl Pts',(1.85181097944898,4.189042348625,9.07142017585705));
#42964=CARTESIAN_POINT('Ctrl Pts',(1.11923226489897,4.44123843532303,9.09787747254152));
#42965=CARTESIAN_POINT('Ctrl Pts',(0.370955558845314,4.50288281188386,9.12433476922598));
#42966=CARTESIAN_POINT('Ctrl Pts',(-0.377321147208358,4.5645271884447,9.15079206591045));
#42967=CARTESIAN_POINT('Ctrl Pts',(-1.14129584476571,4.43561985486832,9.17724936259492));
#42968=CARTESIAN_POINT('Ctrl Pts',(-1.82791726117885,4.13186158171856,9.20370665927939));
#42969=CARTESIAN_POINT('Ctrl Pts',(-2.51453867759199,3.82810330856881,9.23016395596386));
#42970=CARTESIAN_POINT('Ctrl Pts',(-3.12380681286095,3.34949409584567,9.25662125264832));
#42971=CARTESIAN_POINT('Ctrl Pts',(-3.58151348240605,2.75432801596707,9.28307854933279));
#42972=CARTESIAN_POINT('Ctrl Pts',(-4.03922015195113,2.15916193608848,9.30953584601726));
#42973=CARTESIAN_POINT('Ctrl Pts',(-4.34536535577235,1.44743898905445,9.33599314270173));
#42974=CARTESIAN_POINT('Ctrl Pts',(-4.46266094686473,0.705846242127692,
9.3624504393862));
#42975=CARTESIAN_POINT('Ctrl Pts',(-4.57995653795712,-0.0357465047990668,
9.38890773607066));
#42976=CARTESIAN_POINT('Ctrl Pts',(-4.50840251632067,-0.807209051618545,
9.41536503275513));
#42977=CARTESIAN_POINT('Ctrl Pts',(-4.25671408259964,-1.51457811392983,
9.4418223294396));
#42978=CARTESIAN_POINT('Ctrl Pts',(-4.00502564887861,-2.22194717624114,
9.46827962612407));
#42979=CARTESIAN_POINT('Ctrl Pts',(-3.57320280307299,-2.86522275404424,
9.49473692280854));
#42980=CARTESIAN_POINT('Ctrl Pts',(-3.01384108989007,-3.36605459389589,
9.521194219493));
#42981=CARTESIAN_POINT('Ctrl Pts',(-2.45447937670717,-3.86688643374753,
9.54765151617747));
#42982=CARTESIAN_POINT('Ctrl Pts',(-1.76757879614698,-4.22527453564772,
9.57410881286193));
#42983=CARTESIAN_POINT('Ctrl Pts',(-1.03680307870741,-4.39756762542433,
9.6005661095464));
#42984=CARTESIAN_POINT('Ctrl Pts',(-0.306027361267855,-4.56986071520094,
9.62702340623087));
#42985=CARTESIAN_POINT('Ctrl Pts',(0.468623493051109,-4.55605879285398,
9.65348070291534));
#42986=CARTESIAN_POINT('Ctrl Pts',(1.19279786752367,-4.35784291725027,9.67993799959981));
#42987=CARTESIAN_POINT('Ctrl Pts',(1.91697224199627,-4.15962704164656,9.70639529628428));
#42988=CARTESIAN_POINT('Ctrl Pts',(2.59067013662248,-3.7769972127861,9.73285259296875));
#42989=CARTESIAN_POINT('Ctrl Pts',(3.13183589343935,-3.25655732035571,9.75930988965321));
#42990=CARTESIAN_POINT('Ctrl Pts',(3.67300165025619,-2.73611742792533,9.78576718633768));
#42991=CARTESIAN_POINT('Ctrl Pts',(4.08163526926369,-2.07786747192505,9.81222448302215));
#42992=CARTESIAN_POINT('Ctrl Pts',(4.30796562791432,-1.3619815684899,9.83868177970662));
#42993=CARTESIAN_POINT('Ctrl Pts',(4.44693411433176,-0.922422416809593,
9.8549267523071));
#42994=CARTESIAN_POINT('Ctrl Pts',(4.51717337249904,-0.461134228693464,
9.87117172490759));
#42995=CARTESIAN_POINT('Ctrl Pts',(4.5174420818448,7.39595355181285E-5,
9.88741669750808));
#42996=CARTESIAN_POINT('Ctrl Pts',(4.51802315729813,-7.77880120685776E-5,
9.61258330249199));
#42997=CARTESIAN_POINT('Ctrl Pts',(4.51808868978702,-0.081289075021137,
9.60972176714861));
#42998=CARTESIAN_POINT('Ctrl Pts',(4.51594405515544,-0.162496901825208,
9.60686023180522));
#42999=CARTESIAN_POINT('Ctrl Pts',(4.51156607035433,-0.243584147729178,
9.60399869646184));
#43000=CARTESIAN_POINT('Ctrl Pts',(4.47108792528055,-0.993303813841435,
9.57754139977738));
#43001=CARTESIAN_POINT('Ctrl Pts',(4.23969061441499,-1.73271555548592,9.5510841030929));
#43002=CARTESIAN_POINT('Ctrl Pts',(3.84555807412645,-2.37175984086041,9.52462680640843));
#43003=CARTESIAN_POINT('Ctrl Pts',(3.45142553383792,-3.0108041262349,9.49816950972396));
#43004=CARTESIAN_POINT('Ctrl Pts',(2.8945577641264,-3.54948095533939,9.47171221303951));
#43005=CARTESIAN_POINT('Ctrl Pts',(2.24278064303981,-3.92218008655942,9.44525491635504));
#43006=CARTESIAN_POINT('Ctrl Pts',(1.59100352195321,-4.29487921777947,9.41879761967057));
#43007=CARTESIAN_POINT('Ctrl Pts',(0.844317049491529,-4.50160065111505,
9.3923403229861));
#43008=CARTESIAN_POINT('Ctrl Pts',(0.0936668116193721,-4.51716594477095,
9.36588302630163));
#43009=CARTESIAN_POINT('Ctrl Pts',(-0.656983426252764,-4.53273123842686,
9.33942572961716));
#43010=CARTESIAN_POINT('Ctrl Pts',(-1.41159742953537,-4.3571403924031,9.3129684329327));
#43011=CARTESIAN_POINT('Ctrl Pts',(-2.07826404778352,-4.01178017741349,
9.28651113624823));
#43012=CARTESIAN_POINT('Ctrl Pts',(-2.74493066603167,-3.66641996242389,
9.26005383956376));
#43013=CARTESIAN_POINT('Ctrl Pts',(-3.32364989924536,-3.15129037846845,
9.23359654287929));
#43014=CARTESIAN_POINT('Ctrl Pts',(-3.7439343853058,-2.52913363876293,9.20713924619482));
#43015=CARTESIAN_POINT('Ctrl Pts',(-4.16421887136626,-1.9069768990574,9.18068194951035));
#43016=CARTESIAN_POINT('Ctrl Pts',(-4.42606861027347,-1.1777930036018,9.15422465282589));
#43017=CARTESIAN_POINT('Ctrl Pts',(-4.49759059362582,-0.430395743852028,
9.12776735614142));
#43018=CARTESIAN_POINT('Ctrl Pts',(-4.56911257697816,0.317001515897712,
9.10131005945695));
#43019=CARTESIAN_POINT('Ctrl Pts',(-4.45030680477565,1.08261213994165,9.07485276277248));
#43020=CARTESIAN_POINT('Ctrl Pts',(-4.15564368858649,1.77318560159636,9.04839546608801));
#43021=CARTESIAN_POINT('Ctrl Pts',(-3.86098057239734,2.46375906325108,9.02193816940354));
#43022=CARTESIAN_POINT('Ctrl Pts',(-3.39046011222153,3.0792953625166,8.99548087271908));
#43023=CARTESIAN_POINT('Ctrl Pts',(-2.8013911793688,3.54482285937563,8.96902357603462));
#43024=CARTESIAN_POINT('Ctrl Pts',(-2.21232224651606,4.01035035623468,8.94256627935015));
#43025=CARTESIAN_POINT('Ctrl Pts',(-1.50470484098639,4.32586905068723,8.91610898266568));
#43026=CARTESIAN_POINT('Ctrl Pts',(-0.76472597963103,4.45294911494335,8.88965168598121));
#43027=CARTESIAN_POINT('Ctrl Pts',(-0.0247471182756658,4.58002917919947,
8.86319438929674));
#43028=CARTESIAN_POINT('Ctrl Pts',(0.747593198905389,4.51867061325916,8.83673709261227));
#43029=CARTESIAN_POINT('Ctrl Pts',(1.45822477605263,4.27634682254651,8.8102797959278));
#43030=CARTESIAN_POINT('Ctrl Pts',(2.16885635319985,4.03402303183387,8.78382249924334));
#43031=CARTESIAN_POINT('Ctrl Pts',(2.81777919031325,3.6107340163489,8.75736520255887));
#43032=CARTESIAN_POINT('Ctrl Pts',(3.3259552040156,3.0580359097105,8.7309079058744));
#43033=CARTESIAN_POINT('Ctrl Pts',(3.83413121771795,2.5053378030721,8.70445060918993));
#43034=CARTESIAN_POINT('Ctrl Pts',(4.20156040800925,1.82323060528026,8.67799331250546));
#43035=CARTESIAN_POINT('Ctrl Pts',(4.38349030615737,1.0947942181167,8.65153601582099));
#43036=CARTESIAN_POINT('Ctrl Pts',(4.47277460017851,0.737305266442263,8.63855177804465));
#43037=CARTESIAN_POINT('Ctrl Pts',(4.51738186963902,0.368658049377594,8.62556754026832));
#43038=CARTESIAN_POINT('Ctrl Pts',(4.51736350124836,6.46409108656654E-6,
8.61258330249198));
#43039=CARTESIAN_POINT('Origin',(0.,0.,20.5));
#43040=CARTESIAN_POINT('',(4.51805554098247,6.65521552928316E-5,7.61258330249197));
#43041=CARTESIAN_POINT('',(4.51740628246061,-5.63430382605529E-5,7.88741669750807));
#43042=CARTESIAN_POINT('',(4.51775,5.53264807684796E-16,20.5));
#43043=CARTESIAN_POINT('Ctrl Pts',(4.51740628246061,-5.63430382605529E-5,
7.88741669750807));
#43044=CARTESIAN_POINT('Ctrl Pts',(4.51721359264065,0.438494588092411,7.90286327114702));
#43045=CARTESIAN_POINT('Ctrl Pts',(4.45380791076361,0.877100051477632,7.91830984478598));
#43046=CARTESIAN_POINT('Ctrl Pts',(4.32797411068275,1.29699720179238,7.93375641842493));
#43047=CARTESIAN_POINT('Ctrl Pts',(4.1124426757192,2.01620805997421,7.9602137151094));
#43048=CARTESIAN_POINT('Ctrl Pts',(3.71376126713352,2.68053296061069,7.98667101179386));
#43049=CARTESIAN_POINT('Ctrl Pts',(3.18048883925826,3.20905786603343,8.01312830847833));
#43050=CARTESIAN_POINT('Ctrl Pts',(2.64721641138298,3.73758277145619,8.0395856051628));
#43051=CARTESIAN_POINT('Ctrl Pts',(1.97935296421813,4.13030768166519,8.06604290184727));
#43052=CARTESIAN_POINT('Ctrl Pts',(1.25824352648304,4.33939913723789,8.09250019853174));
#43053=CARTESIAN_POINT('Ctrl Pts',(0.53713408874796,4.54849059281059,8.11895749521621));
#43054=CARTESIAN_POINT('Ctrl Pts',(-0.237221339557352,4.57394859374699,
8.14541479190067));
#43055=CARTESIAN_POINT('Ctrl Pts',(-0.970507124268639,4.41267238370822,
8.17187208858514));
#43056=CARTESIAN_POINT('Ctrl Pts',(-1.70379290897991,4.25139617366945,8.19832938526961));
#43057=CARTESIAN_POINT('Ctrl Pts',(-2.39600905009715,3.90338575265551,8.22478668195408));
#43058=CARTESIAN_POINT('Ctrl Pts',(-2.96284438772951,3.4110284047919,8.25124397863854));
#43059=CARTESIAN_POINT('Ctrl Pts',(-3.52967972536187,2.91867105692828,8.27770127532301));
#43060=CARTESIAN_POINT('Ctrl Pts',(-3.97113425950935,2.28196678221498,8.30415857200748));
#43061=CARTESIAN_POINT('Ctrl Pts',(-4.2334393164843,1.57846545665159,8.33061586869195));
#43062=CARTESIAN_POINT('Ctrl Pts',(-4.49574437345926,0.874964131088192,
8.35707316537641));
#43063=CARTESIAN_POINT('Ctrl Pts',(-4.57889995326168,0.104665754674698,
8.38353046206088));
#43064=CARTESIAN_POINT('Ctrl Pts',(-4.47277779830253,-0.638608182855007,
8.40998775874535));
#43065=CARTESIAN_POINT('Ctrl Pts',(-4.36665564334337,-1.38188212038471,
8.43644505542982));
#43066=CARTESIAN_POINT('Ctrl Pts',(-4.07125575362263,-2.09813161903063,
8.46290235211428));
#43067=CARTESIAN_POINT('Ctrl Pts',(-3.62255750878001,-2.70011828255337,
8.48935964879875));
#43068=CARTESIAN_POINT('Ctrl Pts',(-3.17385926393738,-3.30210494607612,
8.51581694548322));
#43069=CARTESIAN_POINT('Ctrl Pts',(-2.57186266397286,-3.78982877447569,
8.54227424216769));
#43070=CARTESIAN_POINT('Ctrl Pts',(-1.88989022851369,-4.10388554523221,
8.56873153885216));
#43071=CARTESIAN_POINT('Ctrl Pts',(-1.20791779305452,-4.41794231598872,
8.59518883553663));
#43072=CARTESIAN_POINT('Ctrl Pts',(-0.445969522100707,-4.55833202910218,
8.62164613222109));
#43073=CARTESIAN_POINT('Ctrl Pts',(0.30315012821752,-4.50795537288903,8.64810342890556));
#43074=CARTESIAN_POINT('Ctrl Pts',(1.05226977853573,-4.45757871667589,8.67456072559003));
#43075=CARTESIAN_POINT('Ctrl Pts',(1.78856080821834,-4.21643569113615,8.7010180222745));
#43076=CARTESIAN_POINT('Ctrl Pts',(2.42234378472631,-3.81389724990005,8.72747531895897));
#43077=CARTESIAN_POINT('Ctrl Pts',(3.05612676123428,-3.41135880866395,8.75393261564343));
#43078=CARTESIAN_POINT('Ctrl Pts',(3.58740168456759,-2.84742495173149,8.78038991232789));
#43079=CARTESIAN_POINT('Ctrl Pts',(3.95145985704281,-2.19078219875382,8.80684720901236));
#43080=CARTESIAN_POINT('Ctrl Pts',(4.31551802951803,-1.53413944577613,8.83330450569683));
#43081=CARTESIAN_POINT('Ctrl Pts',(4.51235945113515,-0.78478779675323,8.85976180238131));
#43082=CARTESIAN_POINT('Ctrl Pts',(4.51800905459174,-0.0339974532052447,
8.88621909906578));
#43083=CARTESIAN_POINT('Ctrl Pts',(4.51809429832594,-0.0226691939774265,
8.88661829854654));
#43084=CARTESIAN_POINT('Ctrl Pts',(4.5181360151034,-0.0113406072147017,
8.88701749802731));
#43085=CARTESIAN_POINT('Ctrl Pts',(4.51813428255233,-1.20076389504314E-5,
8.88741669750808));
#43086=CARTESIAN_POINT('Ctrl Pts',(4.51736350124836,6.46409108656654E-6,
8.61258330249198));
#43087=CARTESIAN_POINT('Ctrl Pts',(4.5173444413379,-0.382523847714403,8.59911024358385));
#43088=CARTESIAN_POINT('Ctrl Pts',(4.46927642784078,-0.765058862836159,
8.58563718467573));
#43089=CARTESIAN_POINT('Ctrl Pts',(4.37321687241043,-1.13513692172449,8.5721641257676));
#43090=CARTESIAN_POINT('Ctrl Pts',(4.18458293451042,-1.86186609786678,8.54570682908313));
#43091=CARTESIAN_POINT('Ctrl Pts',(3.81088445270546,-2.54055887361605,8.51924953239865));
#43092=CARTESIAN_POINT('Ctrl Pts',(3.29763748849563,-3.08855122001653,8.49279223571418));
#43093=CARTESIAN_POINT('Ctrl Pts',(2.78439052428581,-3.636543566417,8.46633493902971));
#43094=CARTESIAN_POINT('Ctrl Pts',(2.13159507767111,-4.05383548346868,8.43987764234525));
#43095=CARTESIAN_POINT('Ctrl Pts',(1.4187609115801,-4.28960127750468,8.41342034566079));
#43096=CARTESIAN_POINT('Ctrl Pts',(0.705926745489094,-4.52536707154067,
8.38696304897632));
#43097=CARTESIAN_POINT('Ctrl Pts',(-0.0669461400782259,-4.57960674256099,
8.36050575229184));
#43098=CARTESIAN_POINT('Ctrl Pts',(-0.805722683022316,-4.44571395866409,
8.33404845560738));
#43099=CARTESIAN_POINT('Ctrl Pts',(-1.54449922596642,-4.31182117476718,
8.30759115892291));
#43100=CARTESIAN_POINT('Ctrl Pts',(-2.24917942628729,-3.98979593595305,
8.28113386223845));
#43101=CARTESIAN_POINT('Ctrl Pts',(-2.83393401547744,-3.51886055991386,
8.25467656555398));
#43102=CARTESIAN_POINT('Ctrl Pts',(-3.41868860466758,-3.04792518387468,
8.22821926886951));
#43103=CARTESIAN_POINT('Ctrl Pts',(-3.88351758272698,-2.42807967061047,
8.20176197218504));
#43104=CARTESIAN_POINT('Ctrl Pts',(-4.17180529456878,-1.73482051763438,
8.17530467550057));
#43105=CARTESIAN_POINT('Ctrl Pts',(-4.46009300641058,-1.0415613646583,8.1488473788161));
#43106=CARTESIAN_POINT('Ctrl Pts',(-4.57183945203477,-0.274888571970355,
8.12239008213164));
#43107=CARTESIAN_POINT('Ctrl Pts',(-4.49343403803759,0.471817962780769,
8.09593278544718));
#43108=CARTESIAN_POINT('Ctrl Pts',(-4.41502862404041,1.21852449753188,8.06947548876271));
#43109=CARTESIAN_POINT('Ctrl Pts',(-4.14647135042187,1.94526477434618,8.04301819207824));
#43110=CARTESIAN_POINT('Ctrl Pts',(-3.72047219588799,2.56352263181385,8.01656089539377));
#43111=CARTESIAN_POINT('Ctrl Pts',(-3.2944730413541,3.18178048928153,7.9901035987093));
#43112=CARTESIAN_POINT('Ctrl Pts',(-2.71103200590485,3.69155592740257,7.96364630202483));
#43113=CARTESIAN_POINT('Ctrl Pts',(-2.04121156194556,4.03075886199821,7.93718900534037));
#43114=CARTESIAN_POINT('Ctrl Pts',(-1.37139111798628,4.36996179659386,7.9107317086559));
#43115=CARTESIAN_POINT('Ctrl Pts',(-0.615191265516958,4.53859222766412,
7.88427441197143));
#43116=CARTESIAN_POINT('Ctrl Pts',(0.135283690341632,4.5161111553332,7.85781711528696));
#43117=CARTESIAN_POINT('Ctrl Pts',(0.885758646200222,4.49363008300228,7.83135981860249));
#43118=CARTESIAN_POINT('Ctrl Pts',(1.63050870544808,4.28003750727018,7.80490252191802));
#43119=CARTESIAN_POINT('Ctrl Pts',(2.27882413510697,3.90134876747149,7.77844522523355));
#43120=CARTESIAN_POINT('Ctrl Pts',(2.92713956476585,3.52266002767282,7.75198792854908));
#43121=CARTESIAN_POINT('Ctrl Pts',(3.47902036483576,2.97887512380756,7.72553063186463));
#43122=CARTESIAN_POINT('Ctrl Pts',(3.8672480646519,2.33622645534278,7.69907333518016));
#43123=CARTESIAN_POINT('Ctrl Pts',(4.25547576446805,1.69357778687799,7.67261603849569));
#43124=CARTESIAN_POINT('Ctrl Pts',(4.48005036403042,0.952065353813674,7.64615874181121));
#43125=CARTESIAN_POINT('Ctrl Pts',(4.51361892565605,0.202004549842097,7.61970144512674));
#43126=CARTESIAN_POINT('Ctrl Pts',(4.51662938451667,0.134738420941428,7.61732873091515));
#43127=CARTESIAN_POINT('Ctrl Pts',(4.51810364598245,0.0674035403653694,
7.61495601670356));
#43128=CARTESIAN_POINT('Ctrl Pts',(4.51805554098247,6.65521552928316E-5,
7.61258330249197));
#43129=CARTESIAN_POINT('Origin',(0.,0.,20.5));
#43130=CARTESIAN_POINT('',(4.51756917096255,-0.000106270599391639,6.61258330249198));
#43131=CARTESIAN_POINT('',(4.5178629555887,0.000109594847417262,6.88741669750807));
#43132=CARTESIAN_POINT('',(4.51775,5.53264807684796E-16,20.5));
#43133=CARTESIAN_POINT('Ctrl Pts',(4.5178629555887,0.000109594847417262,
6.88741669750807));
#43134=CARTESIAN_POINT('Ctrl Pts',(4.51800230500779,0.137343923060939,6.89225174758228));
#43135=CARTESIAN_POINT('Ctrl Pts',(4.5118734339612,0.274565850873291,6.89708679765648));
#43136=CARTESIAN_POINT('Ctrl Pts',(4.4993855978694,0.411206621885887,6.90192184773068));
#43137=CARTESIAN_POINT('Ctrl Pts',(4.43105241013461,1.15890217051388,6.92837914441515));
#43138=CARTESIAN_POINT('Ctrl Pts',(4.17231550636749,1.88919639463632,6.95483644109962));
#43139=CARTESIAN_POINT('Ctrl Pts',(3.75468875509468,2.51314026599451,6.98129373778408));
#43140=CARTESIAN_POINT('Ctrl Pts',(3.33706200382187,3.13708413735269,7.00775103446855));
#43141=CARTESIAN_POINT('Ctrl Pts',(2.76054540504339,3.6546776559466,7.03420833115302));
#43142=CARTESIAN_POINT('Ctrl Pts',(2.09535804244149,4.00287850404845,7.06066562783749));
#43143=CARTESIAN_POINT('Ctrl Pts',(1.4301706798396,4.35107935215029,7.08712292452196));
#43144=CARTESIAN_POINT('Ctrl Pts',(0.676312553414283,4.52988752976006,7.11358022120642));
#43145=CARTESIAN_POINT('Ctrl Pts',(-0.074397251354124,4.51752439873747,
7.14003751789089));
#43146=CARTESIAN_POINT('Ctrl Pts',(-0.82510705612252,4.50516126771487,7.16649481457536));
#43147=CARTESIAN_POINT('Ctrl Pts',(-1.57266853923404,4.30162682805993,7.19295211125983));
#43148=CARTESIAN_POINT('Ctrl Pts',(-2.22602953939534,3.93171134926469,7.2194094079443));
#43149=CARTESIAN_POINT('Ctrl Pts',(-2.87939053955664,3.56179587046945,7.24586670462877));
#43150=CARTESIAN_POINT('Ctrl Pts',(-3.43855105676772,3.0254993525339,7.27232400131323));
#43151=CARTESIAN_POINT('Ctrl Pts',(-3.83540595887268,2.38814211780651,7.2987812979977));
#43152=CARTESIAN_POINT('Ctrl Pts',(-4.23226086097764,1.7507848830791,7.32523859468216));
#43153=CARTESIAN_POINT('Ctrl Pts',(-4.46681014797648,1.01236693155982,7.35169589136664));
#43154=CARTESIAN_POINT('Ctrl Pts',(-4.51048597629575,0.26282675251353,7.37815318805111));
#43155=CARTESIAN_POINT('Ctrl Pts',(-4.55416180461501,-0.486713426532748,
7.40461048473557));
#43156=CARTESIAN_POINT('Ctrl Pts',(-4.40696417425471,-1.24737583310602,
7.43106778142003));
#43157=CARTESIAN_POINT('Ctrl Pts',(-4.08682159368453,-1.92651262793454,
7.4575250781045));
#43158=CARTESIAN_POINT('Ctrl Pts',(-3.76667901311434,-2.60564942276306,
7.48398237478897));
#43159=CARTESIAN_POINT('Ctrl Pts',(-3.27359148233425,-3.20326060584682,
7.51043967147344));
#43160=CARTESIAN_POINT('Ctrl Pts',(-2.66761651687792,-3.64655779648116,
7.53689696815791));
#43161=CARTESIAN_POINT('Ctrl Pts',(-2.06164155142159,-4.0898549871155,7.56335426484238));
#43162=CARTESIAN_POINT('Ctrl Pts',(-1.342779151289,-4.37883818530042,7.58981156152685));
#43163=CARTESIAN_POINT('Ctrl Pts',(-0.59858596122885,-4.47830955732374,
7.61626885821132));
#43164=CARTESIAN_POINT('Ctrl Pts',(0.145607228831289,-4.57778092934705,
7.64272615489578));
#43165=CARTESIAN_POINT('Ctrl Pts',(0.915131208818995,-4.48774047520876,
7.66918345158024));
#43166=CARTESIAN_POINT('Ctrl Pts',(1.61625880962798,-4.21915502257233,7.69564074826471));
#43167=CARTESIAN_POINT('Ctrl Pts',(2.31738641043699,-3.95056956993589,7.72209804494918));
#43168=CARTESIAN_POINT('Ctrl Pts',(2.95011763206728,-3.5034391188013,7.74855534163365));
#43169=CARTESIAN_POINT('Ctrl Pts',(3.43738651198769,-2.93222366326352,7.77501263831812));
#43170=CARTESIAN_POINT('Ctrl Pts',(3.92465539190809,-2.36100820772573,7.80146993500259));
#43171=CARTESIAN_POINT('Ctrl Pts',(4.2664619301186,-1.66570774778476,7.82792723168706));
#43172=CARTESIAN_POINT('Ctrl Pts',(4.42117446855315,-0.931009109950678,
7.85438452837153));
#43173=CARTESIAN_POINT('Ctrl Pts',(4.4855611265208,-0.625249858747316,7.86539525141704));
#43174=CARTESIAN_POINT('Ctrl Pts',(4.51754363682092,-0.312666955391513,
7.87640597446256));
#43175=CARTESIAN_POINT('Ctrl Pts',(4.51740628246061,-5.63430382605529E-5,
7.88741669750807));
#43176=CARTESIAN_POINT('Ctrl Pts',(4.51805554098247,6.65521552928316E-5,
7.61258330249197));
#43177=CARTESIAN_POINT('Ctrl Pts',(4.51756724414766,-0.683447390694716,
7.58849872001909));
#43178=CARTESIAN_POINT('Ctrl Pts',(4.36022097756292,-1.36717849491845,7.56441413754622));
#43179=CARTESIAN_POINT('Ctrl Pts',(4.06048220709641,-1.98142521687064,7.54032955507335));
#43180=CARTESIAN_POINT('Ctrl Pts',(3.73121440322227,-2.65618500473295,7.51387225838888));
#43181=CARTESIAN_POINT('Ctrl Pts',(3.23011627178511,-3.24709540557874,7.48741496170441));
#43182=CARTESIAN_POINT('Ctrl Pts',(2.61822101061302,-3.68218418656399,7.46095766501995));
#43183=CARTESIAN_POINT('Ctrl Pts',(2.00632574944092,-4.11727296754925,7.43450036833548));
#43184=CARTESIAN_POINT('Ctrl Pts',(1.28363335853389,-4.39654012867397,7.40804307165101));
#43185=CARTESIAN_POINT('Ctrl Pts',(0.538166971278164,-4.48597123878683,
7.38158577496654));
#43186=CARTESIAN_POINT('Ctrl Pts',(-0.207299415977548,-4.57540234889969,
7.35512847828207));
#43187=CARTESIAN_POINT('Ctrl Pts',(-0.975539799581951,-4.47499740800071,
7.3286711815976));
#43188=CARTESIAN_POINT('Ctrl Pts',(-1.67298335104765,-4.1969856267701,7.30221388491313));
#43189=CARTESIAN_POINT('Ctrl Pts',(-2.37042690251334,-3.91897384553948,
7.27575658822867));
#43190=CARTESIAN_POINT('Ctrl Pts',(-2.99707362184033,-3.46335522397723,
7.2492992915442));
#43191=CARTESIAN_POINT('Ctrl Pts',(-3.47659863214408,-2.88562360594227,
7.22284199485973));
#43192=CARTESIAN_POINT('Ctrl Pts',(-3.95612364244783,-2.30789198790732,
7.19638469817527));
#43193=CARTESIAN_POINT('Ctrl Pts',(-4.28852694372834,-1.60804737339967,
7.1699274014908));
#43194=CARTESIAN_POINT('Ctrl Pts',(-4.43332218177076,-0.871330061926449,
7.14347010480633));
#43195=CARTESIAN_POINT('Ctrl Pts',(-4.57811741981318,-0.134612750453221,
7.11701280812186));
#43196=CARTESIAN_POINT('Ctrl Pts',(-4.53530459461751,0.63897725798557,7.09055551143739));
#43197=CARTESIAN_POINT('Ctrl Pts',(-4.31009826091029,1.3552175565183,7.06409821475293));
#43198=CARTESIAN_POINT('Ctrl Pts',(-4.08489192720307,2.07145785505103,7.03764091806846));
#43199=CARTESIAN_POINT('Ctrl Pts',(-3.67729208498431,2.7303484436777,7.01118362138399));
#43200=CARTESIAN_POINT('Ctrl Pts',(-3.13694394393276,3.25163717791837,6.98472632469952));
#43201=CARTESIAN_POINT('Ctrl Pts',(-2.59659580288121,3.77292591215904,6.95826902801505));
#43202=CARTESIAN_POINT('Ctrl Pts',(-1.92349936299689,4.15661279201372,6.93181173133059));
#43203=CARTESIAN_POINT('Ctrl Pts',(-1.19963702572085,4.35596518015434,6.90535443464612));
#43204=CARTESIAN_POINT('Ctrl Pts',(-0.475774688444814,4.55531756829496,
6.87889713796165));
#43205=CARTESIAN_POINT('Ctrl Pts',(0.298853546222961,4.57033546472154,6.85243984127718));
#43206=CARTESIAN_POINT('Ctrl Pts',(1.02989881660515,4.39918970627009,6.82598254459271));
#43207=CARTESIAN_POINT('Ctrl Pts',(1.76094408698735,4.22804394781863,6.79952524790824));
#43208=CARTESIAN_POINT('Ctrl Pts',(2.44840639308396,3.87073453448917,6.77306795122378));
#43209=CARTESIAN_POINT('Ctrl Pts',(3.00855358684847,3.37078135737971,6.74661065453931));
#43210=CARTESIAN_POINT('Ctrl Pts',(3.56870078061298,2.87082818027025,6.72015335785485));
#43211=CARTESIAN_POINT('Ctrl Pts',(4.00153286204536,2.22823123938082,6.69369606117038));
#43212=CARTESIAN_POINT('Ctrl Pts',(4.25433136265593,1.52125813092963,6.66723876448591));
#43213=CARTESIAN_POINT('Ctrl Pts',(4.42840834170919,1.03443663992461,6.6490202771546));
#43214=CARTESIAN_POINT('Ctrl Pts',(4.51711887209743,0.517089928133967,6.63080178982329));
#43215=CARTESIAN_POINT('Ctrl Pts',(4.51756917096255,-0.000106270599391639,
6.61258330249198));
#43216=CARTESIAN_POINT('Origin',(0.,0.,20.5));
#43217=CARTESIAN_POINT('',(4.51761916309611,0.000112359330087797,5.61258330249198));
#43218=CARTESIAN_POINT('',(4.51777856404949,-0.00011613542669066,5.88741669750807));
#43219=CARTESIAN_POINT('',(4.51775,5.53264807684796E-16,20.5));
#43220=CARTESIAN_POINT('Ctrl Pts',(4.51777856404949,-0.00011613542669066,
5.88741669750807));
#43221=CARTESIAN_POINT('Ctrl Pts',(4.51717292408202,0.586903980160037,5.90809752070199));
#43222=CARTESIAN_POINT('Ctrl Pts',(4.40219918284471,1.17415437942607,5.92877834389592));
#43223=CARTESIAN_POINT('Ctrl Pts',(4.17916749942524,1.71700921836349,5.94945916708984));
#43224=CARTESIAN_POINT('Ctrl Pts',(3.89383962040738,2.41149180233464,5.97591646377431));
#43225=CARTESIAN_POINT('Ctrl Pts',(3.43165892348727,3.03331448007484,6.00237376045877));
#43226=CARTESIAN_POINT('Ctrl Pts',(2.84891850603996,3.50673993762589,6.02883105714324));
#43227=CARTESIAN_POINT('Ctrl Pts',(2.26617808859264,3.98016539517695,6.05528835382771));
#43228=CARTESIAN_POINT('Ctrl Pts',(1.56287795061812,4.30519363253886,6.08174565051218));
#43229=CARTESIAN_POINT('Ctrl Pts',(0.82467927055748,4.44223657011985,6.10820294719664));
#43230=CARTESIAN_POINT('Ctrl Pts',(0.086480590496836,4.57927950770083,6.13466024388111));
#43231=CARTESIAN_POINT('Ctrl Pts',(-0.686616631649936,4.5283371455009,6.16111754056558));
#43232=CARTESIAN_POINT('Ctrl Pts',(-1.4004500098362,4.29561420685648,6.18757483725005));
#43233=CARTESIAN_POINT('Ctrl Pts',(-2.11428338802246,4.06289126821206,6.21403213393451));
#43234=CARTESIAN_POINT('Ctrl Pts',(-2.76885292224821,3.64838775312316,6.24048943061899));
#43235=CARTESIAN_POINT('Ctrl Pts',(-3.28443276767729,3.10258973098363,6.26694672730345));
#43236=CARTESIAN_POINT('Ctrl Pts',(-3.80001261310638,2.5567917088441,6.29340402398792));
#43237=CARTESIAN_POINT('Ctrl Pts',(-4.1766027697388,1.87969917965394,6.31986132067238));
#43238=CARTESIAN_POINT('Ctrl Pts',(-4.36833497328082,1.15378126410905,6.34631861735685));
#43239=CARTESIAN_POINT('Ctrl Pts',(-4.56006717682283,0.427863348564182,
6.37277591404132));
#43240=CARTESIAN_POINT('Ctrl Pts',(-4.56694142727444,-0.346879953335408,
6.39923321072579));
#43241=CARTESIAN_POINT('Ctrl Pts',(-4.38812044853859,-1.07608576485095,
6.42569050741026));
#43242=CARTESIAN_POINT('Ctrl Pts',(-4.20929946980274,-1.80529157636651,
6.45214780409473));
#43243=CARTESIAN_POINT('Ctrl Pts',(-3.84478326187941,-2.48895989749803,
6.4786051007792));
#43244=CARTESIAN_POINT('Ctrl Pts',(-3.33896949547221,-3.04382068336875,
6.50506239746367));
#43245=CARTESIAN_POINT('Ctrl Pts',(-2.83315572906502,-3.59868146923946,
6.53151969414813));
#43246=CARTESIAN_POINT('Ctrl Pts',(-2.18604440417397,-4.02473471984939,
6.55797699083259));
#43247=CARTESIAN_POINT('Ctrl Pts',(-1.47645296399246,-4.27008762080069,
6.58443428751706));
#43248=CARTESIAN_POINT('Ctrl Pts',(-0.766861523810935,-4.51544052175199,
6.61089158420153));
#43249=CARTESIAN_POINT('Ctrl Pts',(0.00521003166104095,-4.58009307304465,
6.637348880886));
#43250=CARTESIAN_POINT('Ctrl Pts',(0.745724241442684,-4.45617066548422,
6.66380617757047));
#43251=CARTESIAN_POINT('Ctrl Pts',(1.48623845122433,-4.3322482579238,6.69026347425494));
#43252=CARTESIAN_POINT('Ctrl Pts',(2.19519531531564,-4.01975089151029,6.7167207709394));
#43253=CARTESIAN_POINT('Ctrl Pts',(2.78624467229499,-3.55674039962227,6.74317806762387));
#43254=CARTESIAN_POINT('Ctrl Pts',(3.37729402927435,-3.09372990773424,6.76963536430834));
#43255=CARTESIAN_POINT('Ctrl Pts',(3.85043587914176,-2.4802062903717,6.79609266099281));
#43256=CARTESIAN_POINT('Ctrl Pts',(4.14804206822422,-1.79089604512366,6.82254995767728));
#43257=CARTESIAN_POINT('Ctrl Pts',(4.39126096128897,-1.22755670280584,6.84417220428754));
#43258=CARTESIAN_POINT('Ctrl Pts',(4.51723978779142,-0.613599558623174,
6.86579445089781));
#43259=CARTESIAN_POINT('Ctrl Pts',(4.5178629555887,0.000109594847417262,
6.88741669750807));
#43260=CARTESIAN_POINT('Ctrl Pts',(4.51756917096255,-0.000106270599391639,
6.61258330249198));
#43261=CARTESIAN_POINT('Ctrl Pts',(4.51777280622788,-0.233994013420898,
6.60434449313882));
#43262=CARTESIAN_POINT('Ctrl Pts',(4.49992676845961,-0.467850975545092,
6.59610568378566));
#43263=CARTESIAN_POINT('Ctrl Pts',(4.46376343532316,-0.698840208967197,
6.5878668744325));
#43264=CARTESIAN_POINT('Ctrl Pts',(4.34763208759105,-1.44061616439985,6.56140957774804));
#43265=CARTESIAN_POINT('Ctrl Pts',(4.04260447233807,-2.15281879925221,6.53495228106357));
#43266=CARTESIAN_POINT('Ctrl Pts',(3.58583261551844,-2.74870262081615,6.5084949843791));
#43267=CARTESIAN_POINT('Ctrl Pts',(3.1290607586988,-3.3445864423801,6.48203768769463));
#43268=CARTESIAN_POINT('Ctrl Pts',(2.52054466031253,-3.82415145065562,6.45558039101016));
#43269=CARTESIAN_POINT('Ctrl Pts',(1.83440090767928,-4.12898715838434,6.42912309432569));
#43270=CARTESIAN_POINT('Ctrl Pts',(1.14825715504604,-4.43382286611306,6.40266579764122));
#43271=CARTESIAN_POINT('Ctrl Pts',(0.384485748165844,-4.56392927329498,
6.37620850095676));
#43272=CARTESIAN_POINT('Ctrl Pts',(-0.363886800892981,-4.50345956352816,
6.34975120427229));
#43273=CARTESIAN_POINT('Ctrl Pts',(-1.11225934995183,-4.44298985376135,
6.32329390758782));
#43274=CARTESIAN_POINT('Ctrl Pts',(-1.84523304118933,-4.19194402704577,
6.29683661090335));
#43275=CARTESIAN_POINT('Ctrl Pts',(-2.47353249021757,-3.78089918723516,
6.27037931421889));
#43276=CARTESIAN_POINT('Ctrl Pts',(-3.10183193924579,-3.36985434742456,
6.24392201753442));
#43277=CARTESIAN_POINT('Ctrl Pts',(-3.62545714606476,-2.79881049451895,
6.21746472084996));
#43278=CARTESIAN_POINT('Ctrl Pts',(-3.98063113999636,-2.13732013781012,
6.19100742416549));
#43279=CARTESIAN_POINT('Ctrl Pts',(-4.33580513392796,-1.47582978110128,
6.16455012748102));
#43280=CARTESIAN_POINT('Ctrl Pts',(-4.52252791497214,-0.723892920589236,
6.13809283079655));
#43281=CARTESIAN_POINT('Ctrl Pts',(-4.51805685504966,0.0269053663076428,
6.11163553411208));
#43282=CARTESIAN_POINT('Ctrl Pts',(-4.51358579512718,0.777703653204501,
6.08517823742761));
#43283=CARTESIAN_POINT('Ctrl Pts',(-4.31792089423804,1.52736336648619,6.05872094074314));
#43284=CARTESIAN_POINT('Ctrl Pts',(-3.95489392076209,2.18457678274683,6.03226364405868));
#43285=CARTESIAN_POINT('Ctrl Pts',(-3.59186694728612,2.84179019900748,6.00580634737421));
#43286=CARTESIAN_POINT('Ctrl Pts',(-3.06147790122333,3.40655731824708,5.97934905068974));
#43287=CARTESIAN_POINT('Ctrl Pts',(-2.42832758138604,3.81009013038763,5.95289175400527));
#43288=CARTESIAN_POINT('Ctrl Pts',(-1.79517726154877,4.21362294252816,5.9264344573208));
#43289=CARTESIAN_POINT('Ctrl Pts',(-1.05926566793702,4.45592144756967,5.89997716063634));
#43290=CARTESIAN_POINT('Ctrl Pts',(-0.310226018196338,4.50747395575742,
5.87351986395187));
#43291=CARTESIAN_POINT('Ctrl Pts',(0.438813631544363,4.55902646394516,5.8470625672674));
#43292=CARTESIAN_POINT('Ctrl Pts',(1.20098133741399,4.41983297527914,5.82060527058293));
#43293=CARTESIAN_POINT('Ctrl Pts',(1.88344591635241,4.10684710262907,5.79414797389846));
#43294=CARTESIAN_POINT('Ctrl Pts',(2.56591049529081,3.79386122997902,5.767690677214));
#43295=CARTESIAN_POINT('Ctrl Pts',(3.16867194729802,3.30708297334494,5.74123338052953));
#43296=CARTESIAN_POINT('Ctrl Pts',(3.61831459461448,2.70580138565218,5.71477608384506));
#43297=CARTESIAN_POINT('Ctrl Pts',(4.06795724193093,2.10451979795941,5.68831878716059));
#43298=CARTESIAN_POINT('Ctrl Pts',(4.36448108455665,1.38873487920795,5.66186149047613));
#43299=CARTESIAN_POINT('Ctrl Pts',(4.47176984663199,0.645628440320207,5.63540419379166));
#43300=CARTESIAN_POINT('Ctrl Pts',(4.50261735669319,0.431971549265432,5.6277972300251));
#43301=CARTESIAN_POINT('Ctrl Pts',(4.51782138536506,0.216056072273327,5.62019026625854));
#43302=CARTESIAN_POINT('Ctrl Pts',(4.51761916309611,0.000112359330087797,
5.61258330249198));
#43303=CARTESIAN_POINT('Origin',(0.,0.,20.5));
#43304=CARTESIAN_POINT('',(4.51801297056466,-8.08487039419617E-5,4.61258330249197));
#43305=CARTESIAN_POINT('',(4.51744953111884,7.68816669171638E-5,4.88741669750807));
#43306=CARTESIAN_POINT('',(4.51775,5.53264807684796E-16,20.5));
#43307=CARTESIAN_POINT('Ctrl Pts',(4.51744953111884,7.68816669171638E-5,
4.88741669750807));
#43308=CARTESIAN_POINT('Ctrl Pts',(4.51762304095457,0.28595126409645,4.89748599713724));
#43309=CARTESIAN_POINT('Ctrl Pts',(4.49090928481679,0.571793625338861,4.90755529676642));
#43310=CARTESIAN_POINT('Ctrl Pts',(4.43699864797727,0.852411075740623,4.91762459639559));
#43311=CARTESIAN_POINT('Ctrl Pts',(4.2953473151299,1.58973933227679,4.94408189308006));
#43312=CARTESIAN_POINT('Ctrl Pts',(3.96593233939643,2.29099550010712,4.97053918976452));
#43313=CARTESIAN_POINT('Ctrl Pts',(3.48887610024735,2.87076735409198,4.99699648644899));
#43314=CARTESIAN_POINT('Ctrl Pts',(3.01181986109827,3.45053920807684,5.02345378313346));
#43315=CARTESIAN_POINT('Ctrl Pts',(2.38712235853358,3.90882674821622,5.04991107981793));
#43316=CARTESIAN_POINT('Ctrl Pts',(1.69087105699343,4.18981105932229,5.0763683765024));
#43317=CARTESIAN_POINT('Ctrl Pts',(0.994619755453274,4.47079537042835,5.10282567318686));
#43318=CARTESIAN_POINT('Ctrl Pts',(0.226814654937662,4.57447645250109,5.12928296987133));
#43319=CARTESIAN_POINT('Ctrl Pts',(-0.519026433064492,4.48822606449115,
5.1557402665558));
#43320=CARTESIAN_POINT('Ctrl Pts',(-1.26486752106665,4.40197567648121,5.18219756324027));
#43321=CARTESIAN_POINT('Ctrl Pts',(-1.98874459655534,4.12579381838858,5.20865485992474));
#43322=CARTESIAN_POINT('Ctrl Pts',(-2.60249023287342,3.69331913486986,5.2351121566092));
#43323=CARTESIAN_POINT('Ctrl Pts',(-3.21623586919149,3.26084445135114,5.26156945329367));
#43324=CARTESIAN_POINT('Ctrl Pts',(-3.71985006633895,2.67207694240634,5.28802674997814));
#43325=CARTESIAN_POINT('Ctrl Pts',(-4.05199317246879,1.99872783901753,5.31448404666261));
#43326=CARTESIAN_POINT('Ctrl Pts',(-4.38413627859864,1.32537873562872,5.34094134334707));
#43327=CARTESIAN_POINT('Ctrl Pts',(-4.54480829371086,0.567448037795898,
5.36739864003154));
#43328=CARTESIAN_POINT('Ctrl Pts',(-4.51443954418554,-0.182749134310455,
5.39385593671601));
#43329=CARTESIAN_POINT('Ctrl Pts',(-4.48407079466022,-0.932946306416809,
5.42031323340048));
#43330=CARTESIAN_POINT('Ctrl Pts',(-4.26266128049735,-1.6754099527967,5.44677053008495));
#43331=CARTESIAN_POINT('Ctrl Pts',(-3.87717843548113,-2.31970882302876,
5.47322782676942));
#43332=CARTESIAN_POINT('Ctrl Pts',(-3.49169559046492,-2.96400769326083,
5.49968512345388));
#43333=CARTESIAN_POINT('Ctrl Pts',(-2.94213941459537,-3.51014178734505,
5.52614242013835));
#43334=CARTESIAN_POINT('Ctrl Pts',(-2.29544524188241,-3.89159257704565,
5.55259971682282));
#43335=CARTESIAN_POINT('Ctrl Pts',(-1.64875106916946,-4.27304336674624,
5.57905701350729));
#43336=CARTESIAN_POINT('Ctrl Pts',(-0.904918899613081,-4.48981085206321,
5.60551431019175));
#43337=CARTESIAN_POINT('Ctrl Pts',(-0.154546668242997,-4.51549299318827,
5.63197160687622));
#43338=CARTESIAN_POINT('Ctrl Pts',(0.595825563127097,-4.54117513431334,
5.65842890356069));
#43339=CARTESIAN_POINT('Ctrl Pts',(1.35273785631093,-4.37577193124651,5.68488620024516));
#43340=CARTESIAN_POINT('Ctrl Pts',(2.02399913169717,-4.03942931106444,5.71134349692963));
#43341=CARTESIAN_POINT('Ctrl Pts',(2.69526040708341,-3.70308669088236,5.73780079361409));
#43342=CARTESIAN_POINT('Ctrl Pts',(3.28087066467206,-3.19580465358505,5.76425809029856));
#43343=CARTESIAN_POINT('Ctrl Pts',(3.70950322320198,-2.57936958989042,5.79071538698303));
#43344=CARTESIAN_POINT('Ctrl Pts',(4.13813578173191,-1.9629345261958,5.8171726836675));
#43345=CARTESIAN_POINT('Ctrl Pts',(4.40979064120311,-1.23734643610387,5.84362998035196));
#43346=CARTESIAN_POINT('Ctrl Pts',(4.49138054038091,-0.490981145956846,
5.87008727703643));
#43347=CARTESIAN_POINT('Ctrl Pts',(4.50919422313609,-0.328025747897277,
5.87586375052698));
#43348=CARTESIAN_POINT('Ctrl Pts',(4.51794772865112,-0.164079924696943,
5.88164022401752));
#43349=CARTESIAN_POINT('Ctrl Pts',(4.51777856404949,-0.00011613542669066,
5.88741669750807));
#43350=CARTESIAN_POINT('Ctrl Pts',(4.51761916309611,0.000112359330087797,
5.61258330249198));
#43351=CARTESIAN_POINT('Ctrl Pts',(4.51711804895781,-0.535004016325972,
5.59373296957407));
#43352=CARTESIAN_POINT('Ctrl Pts',(4.42201232003226,-1.07029377947848,5.57488263665616));
#43353=CARTESIAN_POINT('Ctrl Pts',(4.23591186210463,-1.57181816399948,5.55603230373826));
#43354=CARTESIAN_POINT('Ctrl Pts',(3.97471143397694,-2.27573037040736,5.52957500705379));
#43355=CARTESIAN_POINT('Ctrl Pts',(3.5342568961966,-2.91312682419909,5.50311771036932));
#43356=CARTESIAN_POINT('Ctrl Pts',(2.96819512400045,-3.40637334272939,5.47666041368485));
#43357=CARTESIAN_POINT('Ctrl Pts',(2.4021333518043,-3.89961986125968,5.45020311700038));
#43358=CARTESIAN_POINT('Ctrl Pts',(1.71046434519234,-4.24871644452854,5.42374582031592));
#43359=CARTESIAN_POINT('Ctrl Pts',(0.977432623678222,-4.41114351504991,
5.39728852363145));
#43360=CARTESIAN_POINT('Ctrl Pts',(0.244400902164107,-4.57357058557128,
5.37083122694698));
#43361=CARTESIAN_POINT('Ctrl Pts',(-0.529993534252169,-4.54932814334517,
5.34437393026251));
#43362=CARTESIAN_POINT('Ctrl Pts',(-1.2514303002616,-4.34136889100483,5.31791663357804));
#43363=CARTESIAN_POINT('Ctrl Pts',(-1.97286706627105,-4.1334096386645,5.29145933689358));
#43364=CARTESIAN_POINT('Ctrl Pts',(-2.64134616187366,-3.74173357620994,
5.2650020402091));
#43365=CARTESIAN_POINT('Ctrl Pts',(-3.17544757305171,-3.214046414568,5.23854474352464));
#43366=CARTESIAN_POINT('Ctrl Pts',(-3.70954898422975,-2.68635925292607,
5.21208744684017));
#43367=CARTESIAN_POINT('Ctrl Pts',(-4.10927271098324,-2.02266099209677,
5.1856301501557));
#43368=CARTESIAN_POINT('Ctrl Pts',(-4.32593284578035,-1.3037893457135,5.15917285347124));
#43369=CARTESIAN_POINT('Ctrl Pts',(-4.54259298057747,-0.584917699330228,
5.13271555678677));
#43370=CARTESIAN_POINT('Ctrl Pts',(-4.57618952341819,0.189127332607011,
5.1062582601023));
#43371=CARTESIAN_POINT('Ctrl Pts',(-4.42263045256687,0.924067921868061,
5.07980096341783));
#43372=CARTESIAN_POINT('Ctrl Pts',(-4.26907138171554,1.65900851112912,5.05334366673336));
#43373=CARTESIAN_POINT('Ctrl Pts',(-3.92835669717217,2.35484465771397,5.0268863700489));
#43374=CARTESIAN_POINT('Ctrl Pts',(-3.44198507043455,2.92682428907221,5.00042907336443));
#43375=CARTESIAN_POINT('Ctrl Pts',(-2.95561344369694,3.49880392043043,4.97397177667996));
#43376=CARTESIAN_POINT('Ctrl Pts',(-2.3235848747651,3.94692703656203,4.9475144799955));
#43377=CARTESIAN_POINT('Ctrl Pts',(-1.62287974384915,4.21661273787403,4.92105718331103));
#43378=CARTESIAN_POINT('Ctrl Pts',(-0.922174612933183,4.48629843918604,
4.89459988662656));
#43379=CARTESIAN_POINT('Ctrl Pts',(-0.152792920033106,4.57754672567842,
4.86814258994209));
#43380=CARTESIAN_POINT('Ctrl Pts',(0.591555496154586,4.47924365704375,4.84168529325762));
#43381=CARTESIAN_POINT('Ctrl Pts',(1.33590391234227,4.38094058840908,4.81522799657315));
#43382=CARTESIAN_POINT('Ctrl Pts',(2.05521905181757,4.09308616464735,4.78877069988869));
#43383=CARTESIAN_POINT('Ctrl Pts',(2.66188912668092,3.65074073599527,4.76231340320422));
#43384=CARTESIAN_POINT('Ctrl Pts',(3.26855920154427,3.20839530734318,4.73585610651975));
#43385=CARTESIAN_POINT('Ctrl Pts',(3.76258421179568,2.61155887380074,4.70939880983528));
#43386=CARTESIAN_POINT('Ctrl Pts',(4.08379245793942,1.93292545243589,4.68294151315081));
#43387=CARTESIAN_POINT('Ctrl Pts',(4.36852345568096,1.33135941704992,4.65948877626453));
#43388=CARTESIAN_POINT('Ctrl Pts',(4.51746001083452,0.665519661321642,4.63603603937825));
#43389=CARTESIAN_POINT('Ctrl Pts',(4.51801297056466,-8.08487039419617E-5,
4.61258330249197));
#43390=CARTESIAN_POINT('Origin',(0.,0.,20.5));
#43391=CARTESIAN_POINT('',(4.51736370604735,1.02551535238581E-5,3.61258330249198));
#43392=CARTESIAN_POINT('',(4.51813206731963,-1.62797693238861E-5,3.88741669750807));
#43393=CARTESIAN_POINT('',(4.51775,5.53264807684796E-16,20.5));
#43394=CARTESIAN_POINT('Ctrl Pts',(4.51813206731963,-1.62797693238861E-5,
3.88741669750807));
#43395=CARTESIAN_POINT('Ctrl Pts',(4.51798177204935,0.735410282480124,3.91333177025696));
#43396=CARTESIAN_POINT('Ctrl Pts',(4.33483992986086,1.47090898249386,3.93924684300585));
#43397=CARTESIAN_POINT('Ctrl Pts',(3.98971201192936,2.12032066114161,3.96516191575474));
#43398=CARTESIAN_POINT('Ctrl Pts',(3.63736294436994,2.78332005222287,3.99161921243921));
#43399=CARTESIAN_POINT('Ctrl Pts',(3.11617838217547,3.35659231850456,4.01807650912368));
#43400=CARTESIAN_POINT('Ctrl Pts',(2.48963802820999,3.77031353241187,4.04453380580815));
#43401=CARTESIAN_POINT('Ctrl Pts',(1.86309767424454,4.18403474631916,4.07099110249262));
#43402=CARTESIAN_POINT('Ctrl Pts',(1.13120152850809,4.4382049078521,4.09744839917709));
#43403=CARTESIAN_POINT('Ctrl Pts',(0.383093731539025,4.50186637263401,4.12390569586155));
#43404=CARTESIAN_POINT('Ctrl Pts',(-0.365014065430051,4.56552783741592,
4.15036299254602));
#43405=CARTESIAN_POINT('Ctrl Pts',(-1.12933351363175,4.43868060544681,4.17682028923049));
#43406=CARTESIAN_POINT('Ctrl Pts',(-1.81677135017129,4.13677452919472,4.20327758591496));
#43407=CARTESIAN_POINT('Ctrl Pts',(-2.50420918671083,3.83486845294263,4.22973488259942));
#43408=CARTESIAN_POINT('Ctrl Pts',(-3.11476541158823,3.35790353240755,4.25619217928389));
#43409=CARTESIAN_POINT('Ctrl Pts',(-3.57407495233505,2.7639735670387,4.28264947596836));
#43410=CARTESIAN_POINT('Ctrl Pts',(-4.03338449308186,2.17004360166985,4.30910677265283));
#43411=CARTESIAN_POINT('Ctrl Pts',(-4.3414473496981,1.45914859146723,4.3355640693373));
#43412=CARTESIAN_POINT('Ctrl Pts',(-4.4607418071907,0.717874761903797,4.36202136602176));
#43413=CARTESIAN_POINT('Ctrl Pts',(-4.5800362646833,-0.0233990676596439,
4.38847866270623));
#43414=CARTESIAN_POINT('Ctrl Pts',(-4.51056232305225,-0.795051716583895,
4.4149359593907));
#43415=CARTESIAN_POINT('Ctrl Pts',(-4.26078183149923,-1.50309674624206,
4.44139325607517));
#43416=CARTESIAN_POINT('Ctrl Pts',(-4.01100133994621,-2.21114177590023,
4.46785055275963));
#43417=CARTESIAN_POINT('Ctrl Pts',(-3.58091429847122,-2.85557918629231,
4.4943078494441));
#43418=CARTESIAN_POINT('Ctrl Pts',(-3.02290483273516,-3.35791721405156,
4.52076514612857));
#43419=CARTESIAN_POINT('Ctrl Pts',(-2.4648953669991,-3.86025524181081,4.54722244281304));
#43420=CARTESIAN_POINT('Ctrl Pts',(-1.77896347700197,-4.22049388693723,
4.57367973949751));
#43421=CARTESIAN_POINT('Ctrl Pts',(-1.04865490780318,-4.39475648114178,
4.60013703618198));
#43422=CARTESIAN_POINT('Ctrl Pts',(-0.318346338604368,-4.56901907534634,
4.62659433286644));
#43423=CARTESIAN_POINT('Ctrl Pts',(0.456338909796113,-4.55730561862902,
4.65305162955091));
#43424=CARTESIAN_POINT('Ctrl Pts',(1.18104503151144,-4.36104279705434,4.67950892623538));
#43425=CARTESIAN_POINT('Ctrl Pts',(1.90575115322676,-4.16477997547966,4.70596622291985));
#43426=CARTESIAN_POINT('Ctrl Pts',(2.58047814825693,-3.78396778904763,4.73242351960431));
#43427=CARTESIAN_POINT('Ctrl Pts',(3.1230450153487,-3.26498874060892,4.75888081628878));
#43428=CARTESIAN_POINT('Ctrl Pts',(3.66561188244045,-2.74600969217023,4.78533811297325));
#43429=CARTESIAN_POINT('Ctrl Pts',(4.07601862159381,-2.08886378172488,4.81179540965772));
#43430=CARTESIAN_POINT('Ctrl Pts',(4.30427814618986,-1.37359065388121,4.83825270634219));
#43431=CARTESIAN_POINT('Ctrl Pts',(4.4456650936749,-0.930541084129997,4.85464070339748));
#43432=CARTESIAN_POINT('Ctrl Pts',(4.51716714020965,-0.465189691975021,
4.87102870045278));
#43433=CARTESIAN_POINT('Ctrl Pts',(4.51744953111884,7.68816669171638E-5,
4.88741669750807));
#43434=CARTESIAN_POINT('Ctrl Pts',(4.51801297056466,-8.08487039419617E-5,
4.61258330249197));
#43435=CARTESIAN_POINT('Ctrl Pts',(4.51808381093537,-0.0853517722542952,
4.60957874269379));
#43436=CARTESIAN_POINT('Ctrl Pts',(4.51571930609417,-0.170618769185437,
4.6065741828956));
#43437=CARTESIAN_POINT('Ctrl Pts',(4.51089298576516,-0.255746192878958,
4.60356962309741));
#43438=CARTESIAN_POINT('Ctrl Pts',(4.46839378541107,-1.00535400764169,4.57711232641294));
#43439=CARTESIAN_POINT('Ctrl Pts',(4.23500390266681,-1.74413922797991,4.55065502972848));
#43440=CARTESIAN_POINT('Ctrl Pts',(3.83914996695076,-2.38211863169309,4.52419773304401));
#43441=CARTESIAN_POINT('Ctrl Pts',(3.44329603123471,-3.02009803540626,4.49774043635954));
#43442=CARTESIAN_POINT('Ctrl Pts',(2.88497804254688,-3.55727162249439,4.47128313967507));
#43443=CARTESIAN_POINT('Ctrl Pts',(2.23219851400147,-3.92821224455693,4.4448258429906));
#43444=CARTESIAN_POINT('Ctrl Pts',(1.57941898545608,-4.29915286661947,4.41836854630613));
#43445=CARTESIAN_POINT('Ctrl Pts',(0.832177917053118,-4.50386052365641,
4.39191124962167));
#43446=CARTESIAN_POINT('Ctrl Pts',(0.0814884439290546,-4.51740204959703,
4.3654539529372));
#43447=CARTESIAN_POINT('Ctrl Pts',(-0.66920102919502,-4.53094357553764,
4.33899665625273));
#43448=CARTESIAN_POINT('Ctrl Pts',(-1.42333890704021,-4.35331897038192,
4.31253935956826));
#43449=CARTESIAN_POINT('Ctrl Pts',(-2.08907203071289,-4.00616271445513,
4.28608206288379));
#43450=CARTESIAN_POINT('Ctrl Pts',(-2.75480515438558,-3.65900645852834,
4.25962476619933));
#43451=CARTESIAN_POINT('Ctrl Pts',(-3.33213352388578,-3.14231855183048,
4.23316746951486));
#43452=CARTESIAN_POINT('Ctrl Pts',(-3.75073918275569,-2.51903100956272,
4.20671017283039));
#43453=CARTESIAN_POINT('Ctrl Pts',(-4.1693448416256,-1.89574346729495,4.18025287614593));
#43454=CARTESIAN_POINT('Ctrl Pts',(-4.42922778986523,-1.16585628945725,
4.15379557946146));
#43455=CARTESIAN_POINT('Ctrl Pts',(-4.49873457199956,-0.418268926521358,
4.12733828277699));
#43456=CARTESIAN_POINT('Ctrl Pts',(-4.56824135413388,0.329318436414523,
4.10088098609252));
#43457=CARTESIAN_POINT('Ctrl Pts',(-4.44737197016292,1.0946059844486,4.07442368940805));
#43458=CARTESIAN_POINT('Ctrl Pts',(-4.1508481772844,1.78438254119798,4.04796639272359));
#43459=CARTESIAN_POINT('Ctrl Pts',(-3.85432438440588,2.47415909794737,4.02150909603912));
#43460=CARTESIAN_POINT('Ctrl Pts',(-3.3821461826198,3.08842466341204,3.99505179935465));
#43461=CARTESIAN_POINT('Ctrl Pts',(-2.79182435432936,3.55236237154529,3.96859450267018));
#43462=CARTESIAN_POINT('Ctrl Pts',(-2.20150252603891,4.01630007967853,3.94213720598571));
#43463=CARTESIAN_POINT('Ctrl Pts',(-1.49303707124409,4.32990993048035,3.91567990930125));
#43464=CARTESIAN_POINT('Ctrl Pts',(-0.752718298258071,4.45499459120489,
3.88922261261678));
#43465=CARTESIAN_POINT('Ctrl Pts',(-0.0123995252720613,4.58007925192944,
3.86276531593231));
#43466=CARTESIAN_POINT('Ctrl Pts',(0.759772565905157,4.51663872257671,3.83630801924784));
#43467=CARTESIAN_POINT('Ctrl Pts',(1.46974826915516,4.27239998941026,3.80985072256337));
#43468=CARTESIAN_POINT('Ctrl Pts',(2.17972397240517,4.02816125624381,3.78339342587891));
#43469=CARTESIAN_POINT('Ctrl Pts',(2.82750328772796,3.60312431926363,3.75693612919444));
#43470=CARTESIAN_POINT('Ctrl Pts',(3.33418741143483,3.04905820699226,3.73047883250997));
#43471=CARTESIAN_POINT('Ctrl Pts',(3.84087153514169,2.49499209472089,3.7040215358255));
#43472=CARTESIAN_POINT('Ctrl Pts',(4.20646046723263,1.81189680715833,3.67756423914103));
#43473=CARTESIAN_POINT('Ctrl Pts',(4.38642588038764,1.08297259432681,3.65110694245657));
#43474=CARTESIAN_POINT('Ctrl Pts',(4.47377321176399,0.729184698918257,3.63826572913504));
#43475=CARTESIAN_POINT('Ctrl Pts',(4.51739308950363,0.364600853640814,3.62542451581351));
#43476=CARTESIAN_POINT('Ctrl Pts',(4.51736430815743,1.02391689833781E-5,
3.61258330249198));
#43477=CARTESIAN_POINT('Origin',(0.,0.,20.5));
#43478=CARTESIAN_POINT('',(4.51806423128285,6.30519293007281E-5,2.61258330249198));
#43479=CARTESIAN_POINT('',(4.5174009456275,-5.29814202112051E-5,2.88741669750807));
#43480=CARTESIAN_POINT('',(4.51775,5.53264807684796E-16,20.5));
#43481=CARTESIAN_POINT('Ctrl Pts',(4.5174009456275,-5.29814202112051E-5,
2.88741669750807));
#43482=CARTESIAN_POINT('Ctrl Pts',(4.5172216944486,0.434438744202657,2.90272024669221));
#43483=CARTESIAN_POINT('Ctrl Pts',(4.45500169120217,0.868980727030553,2.91802379587635));
#43484=CARTESIAN_POINT('Ctrl Pts',(4.33145501462215,1.28532451174868,2.9333273450605));
#43485=CARTESIAN_POINT('Ctrl Pts',(4.11786331525058,2.00511381699269,2.95978464174497));
#43486=CARTESIAN_POINT('Ctrl Pts',(3.72097433835707,2.67051112625836,2.98624193842943));
#43487=CARTESIAN_POINT('Ctrl Pts',(3.18912872207782,3.2004717836931,3.0126992351139));
#43488=CARTESIAN_POINT('Ctrl Pts',(2.65728310579859,3.73043244112782,3.03915653179837));
#43489=CARTESIAN_POINT('Ctrl Pts',(1.99048085013363,4.12495644673162,3.06561382848284));
#43490=CARTESIAN_POINT('Ctrl Pts',(1.26993773185205,4.33599121325399,3.0920711251673));
#43491=CARTESIAN_POINT('Ctrl Pts',(0.54939461357047,4.54702597977637,3.11852842185177));
#43492=CARTESIAN_POINT('Ctrl Pts',(-0.22488936732773,4.57457150721731,3.14498571853624));
#43493=CARTESIAN_POINT('Ctrl Pts',(-0.958607278893408,4.41527278082,3.17144301522071));
#43494=CARTESIAN_POINT('Ctrl Pts',(-1.69232519045908,4.25597405442269,3.19790031190518));
#43495=CARTESIAN_POINT('Ctrl Pts',(-2.38547703269224,3.90983107418713,3.22435760858964));
#43496=CARTESIAN_POINT('Ctrl Pts',(-2.95363767834166,3.41900367201878,3.25081490527411));
#43497=CARTESIAN_POINT('Ctrl Pts',(-3.52179832399109,2.92817626985041,3.27727220195858));
#43498=CARTESIAN_POINT('Ctrl Pts',(-3.96496777305678,2.29266444574925,3.30372949864305));
#43499=CARTESIAN_POINT('Ctrl Pts',(-4.229168477112,1.58987283655001,3.33018679532752));
#43500=CARTESIAN_POINT('Ctrl Pts',(-4.49336918116721,0.887081227350804,
3.35664409201199));
#43501=CARTESIAN_POINT('Ctrl Pts',(-4.57860114021196,0.117009833053533,
3.38310138869645));
#43502=CARTESIAN_POINT('Ctrl Pts',(-4.47448319596347,-0.62654750277845,
3.40955868538092));
#43503=CARTESIAN_POINT('Ctrl Pts',(-4.37036525171498,-1.37010483861044,
3.43601598206539));
#43504=CARTESIAN_POINT('Ctrl Pts',(-4.07689740417324,-2.08714811597715,
3.46247327874986));
#43505=CARTESIAN_POINT('Ctrl Pts',(-3.62982371237881,-2.69034225726949,
3.48893057543432));
#43506=CARTESIAN_POINT('Ctrl Pts',(-3.18275002058438,-3.29353639856183,
3.51538787211879));
#43507=CARTESIAN_POINT('Ctrl Pts',(-2.58207048453726,-3.7828814037798,3.54184516880326));
#43508=CARTESIAN_POINT('Ctrl Pts',(-1.90094720693718,-4.09877559286125,
3.56830246548773));
#43509=CARTESIAN_POINT('Ctrl Pts',(-1.2198239293371,-4.41466978194271,3.59475976217219));
#43510=CARTESIAN_POINT('Ctrl Pts',(-0.45825691018407,-4.55711315488765,
3.62121705885666));
#43511=CARTESIAN_POINT('Ctrl Pts',(0.290995830439079,-4.5087562665179,3.64767435554113));
#43512=CARTESIAN_POINT('Ctrl Pts',(1.04024857106223,-4.46039937814816,3.6741316522256));
#43513=CARTESIAN_POINT('Ctrl Pts',(1.77718703315549,-4.22124222846373,3.70058894891007));
#43514=CARTESIAN_POINT('Ctrl Pts',(2.41205292762872,-3.8204138936135,3.72704624559453));
#43515=CARTESIAN_POINT('Ctrl Pts',(3.04691882210195,-3.41958555876328,3.753503542279));
#43516=CARTESIAN_POINT('Ctrl Pts',(3.57971214895514,-2.85708603874726,3.77996083896347));
#43517=CARTESIAN_POINT('Ctrl Pts',(3.94553927063659,-2.2014271525676,3.80641813564794));
#43518=CARTESIAN_POINT('Ctrl Pts',(4.31136639231804,-1.54576826638794,3.83287543233241));
#43519=CARTESIAN_POINT('Ctrl Pts',(4.51022730882776,-0.796950014044647,
3.85933272901687));
#43520=CARTESIAN_POINT('Ctrl Pts',(4.51790098062045,-0.0461776299325883,
3.88579002570134));
#43521=CARTESIAN_POINT('Ctrl Pts',(4.51805824719871,-0.0307910709167367,
3.88633224963692));
#43522=CARTESIAN_POINT('Ctrl Pts',(4.5181352119642,-0.0154036911331415,
3.88687447357249));
#43523=CARTESIAN_POINT('Ctrl Pts',(4.51813206731963,-1.62797693238861E-5,
3.88741669750807));
#43524=CARTESIAN_POINT('Ctrl Pts',(4.51736430815743,1.02391689833781E-5,
3.61258330249198));
#43525=CARTESIAN_POINT('Ctrl Pts',(4.51733379007481,-0.386580659657543,
3.59896721912904));
#43526=CARTESIAN_POINT('Ctrl Pts',(4.46822794652789,-0.773179169265813,
3.5853511357661));
#43527=CARTESIAN_POINT('Ctrl Pts',(4.370140714067,-1.14692274519747,3.57173505240317));
#43528=CARTESIAN_POINT('Ctrl Pts',(4.17954824037228,-1.87314073378976,3.5452777557187));
#43529=CARTESIAN_POINT('Ctrl Pts',(3.80402139876375,-2.55082357287386,3.51882045903423));
#43530=CARTESIAN_POINT('Ctrl Pts',(3.28929894294204,-3.09743024266209,3.49236316234976));
#43531=CARTESIAN_POINT('Ctrl Pts',(2.77457648712035,-3.64403691245031,3.46590586566529));
#43532=CARTESIAN_POINT('Ctrl Pts',(2.12065841708548,-4.05956741294266,3.43944856898082));
#43533=CARTESIAN_POINT('Ctrl Pts',(1.40719123005614,-4.29341058905976,3.41299127229636));
#43534=CARTESIAN_POINT('Ctrl Pts',(0.693724043026795,-4.52725376517686,
3.38653397561189));
#43535=CARTESIAN_POINT('Ctrl Pts',(-0.0792922609970231,-4.5794096169187,
3.36007667892742));
#43536=CARTESIAN_POINT('Ctrl Pts',(-0.8177051517065,-4.44352561926563,3.33361938224295));
#43537=CARTESIAN_POINT('Ctrl Pts',(-1.55611804241598,-4.30764162161257,
3.30716208555848));
#43538=CARTESIAN_POINT('Ctrl Pts',(-2.2599275198111,-3.9837177745646,3.28070478887401));
#43539=CARTESIAN_POINT('Ctrl Pts',(-2.84341036847309,-3.51120764419552,
3.25424749218955));
#43540=CARTESIAN_POINT('Ctrl Pts',(-3.42689321713508,-3.03869751382645,
3.22779019550508));
#43541=CARTESIAN_POINT('Ctrl Pts',(-3.89004943706392,-2.41760110013629,
3.20133289882062));
#43542=CARTESIAN_POINT('Ctrl Pts',(-4.17646711326174,-1.72356725892568,
3.17487560213615));
#43543=CARTESIAN_POINT('Ctrl Pts',(-4.46288478945955,-1.02953341771508,
3.14841830545168));
#43544=CARTESIAN_POINT('Ctrl Pts',(-4.57256392192634,-0.262562148984027,
3.12196100876721));
#43545=CARTESIAN_POINT('Ctrl Pts',(-4.49214571371297,0.483930295567052,
3.09550371208274));
#43546=CARTESIAN_POINT('Ctrl Pts',(-4.41172750549959,1.23042274011814,3.06904641539827));
#43547=CARTESIAN_POINT('Ctrl Pts',(-4.14121195660606,1.95643636048925,3.04258911871381));
#43548=CARTESIAN_POINT('Ctrl Pts',(-3.71354756149959,2.57354350122118,3.01613182202934));
#43549=CARTESIAN_POINT('Ctrl Pts',(-3.28588316639313,3.1906506419531,2.98967452534487));
#43550=CARTESIAN_POINT('Ctrl Pts',(-2.70106992507374,3.69885130304582,2.9632172286604));
#43551=CARTESIAN_POINT('Ctrl Pts',(-2.03033744310303,4.03624720641976,2.93675993197593));
#43552=CARTESIAN_POINT('Ctrl Pts',(-1.35960496113232,4.3736431097937,2.91030263529147));
#43553=CARTESIAN_POINT('Ctrl Pts',(-0.602953238510295,4.54023425544885,
2.883845338607));
#43554=CARTESIAN_POINT('Ctrl Pts',(0.147458382357749,4.5157300262161,2.85738804192253));
#43555=CARTESIAN_POINT('Ctrl Pts',(0.897870003225787,4.49122579698336,2.83093074523806));
#43556=CARTESIAN_POINT('Ctrl Pts',(1.64204152233985,4.27562619286271,2.80447344855359));
#43557=CARTESIAN_POINT('Ctrl Pts',(2.28933367226974,3.89519100702514,2.77801615186913));
#43558=CARTESIAN_POINT('Ctrl Pts',(2.93662582219963,3.51475582118756,2.75155885518466));
#43559=CARTESIAN_POINT('Ctrl Pts',(3.48703860294536,2.96948505363305,2.72510155850019));
#43560=CARTESIAN_POINT('Ctrl Pts',(3.873532346971,2.32579208038178,2.69864426181572));
#43561=CARTESIAN_POINT('Ctrl Pts',(4.26002609099665,1.68209910713051,2.67218696513126));
#43562=CARTESIAN_POINT('Ctrl Pts',(4.48260079830222,0.939983928182504,2.64572966844679));
#43563=CARTESIAN_POINT('Ctrl Pts',(4.51414711586846,0.189835351011121,2.61927237176232));
#43564=CARTESIAN_POINT('Ctrl Pts',(4.51680568306753,0.126616549085492,2.61704268200554));
#43565=CARTESIAN_POINT('Ctrl Pts',(4.51810751267774,0.063340691696271,2.61481299224876));
#43566=CARTESIAN_POINT('Ctrl Pts',(4.51806423128285,6.30519293007281E-5,
2.61258330249198));
#43567=CARTESIAN_POINT('Origin',(0.,0.,20.5));
#43568=CARTESIAN_POINT('',(4.51755838390264,-0.00010457874560596,1.61258330249198));
#43569=CARTESIAN_POINT('',(4.51787557461174,0.000108094638884985,1.88741669750807));
#43570=CARTESIAN_POINT('',(4.51775,5.53264807684796E-16,20.5));
#43571=CARTESIAN_POINT('Ctrl Pts',(4.51787557461174,0.000108094638884985,
1.88741669750807));
#43572=CARTESIAN_POINT('Ctrl Pts',(4.51800988663209,0.133281854142107,1.89210872312746));
#43573=CARTESIAN_POINT('Ctrl Pts',(4.5122387502371,0.266444013117212,1.89680074874686));
#43574=CARTESIAN_POINT('Ctrl Pts',(4.50047783691867,0.399075035061228,1.90149277436625));
#43575=CARTESIAN_POINT('Ctrl Pts',(4.43416064298431,1.14695208897868,1.92795007105072));
#43576=CARTESIAN_POINT('Ctrl Pts',(4.17739351195545,1.87794119941301,1.95440736773518));
#43577=CARTESIAN_POINT('Ctrl Pts',(3.76145039622174,2.50300870173296,1.98086466441965));
#43578=CARTESIAN_POINT('Ctrl Pts',(3.34550728048802,3.1280762040529,2.00732196110412));
#43579=CARTESIAN_POINT('Ctrl Pts',(2.77038818004944,3.64722209825845,2.03377925778859));
#43580=CARTESIAN_POINT('Ctrl Pts',(2.10614196483581,3.99721498898444,2.06023655447306));
#43581=CARTESIAN_POINT('Ctrl Pts',(1.44189574962217,4.34720787971043,2.08669385115753));
#43582=CARTESIAN_POINT('Ctrl Pts',(0.688522419633492,4.52804776695686,2.11315114784199));
#43583=CARTESIAN_POINT('Ctrl Pts',(-0.0622179873186998,4.51770855260139,
2.13960844452646));
#43584=CARTESIAN_POINT('Ctrl Pts',(-0.812958394270891,4.50736933824591,
2.16606574121093));
#43585=CARTESIAN_POINT('Ctrl Pts',(-1.56106587818659,4.30585102228854,2.1925230378954));
#43586=CARTESIAN_POINT('Ctrl Pts',(-2.21542177547916,3.9376983125846,2.21898033457986));
#43587=CARTESIAN_POINT('Ctrl Pts',(-2.86977767277172,3.56954560288067,2.24543763126433));
#43588=CARTESIAN_POINT('Ctrl Pts',(-3.43038198344116,3.03475849943017,2.2718949279488));
#43589=CARTESIAN_POINT('Ctrl Pts',(-3.82895372288602,2.39847347956868,2.29835222463327));
#43590=CARTESIAN_POINT('Ctrl Pts',(-4.22752546233088,1.76218845970719,2.32480952131774));
#43591=CARTESIAN_POINT('Ctrl Pts',(-4.46406463055117,1.0244055234347,2.35126681800221));
#43592=CARTESIAN_POINT('Ctrl Pts',(-4.50976101864305,0.274985815861316,
2.37772411468667));
#43593=CARTESIAN_POINT('Ctrl Pts',(-4.55545740673492,-0.474433891712066,
2.40418141137114));
#43594=CARTESIAN_POINT('Ctrl Pts',(-4.41031101469838,-1.23549037058635,
2.43063870805561));
#43595=CARTESIAN_POINT('Ctrl Pts',(-4.09200051244538,-1.91548778391935,
2.45709600474008));
#43596=CARTESIAN_POINT('Ctrl Pts',(-3.77369001019238,-2.59548519725235,
2.48355330142454));
#43597=CARTESIAN_POINT('Ctrl Pts',(-3.28221539772292,-3.19442354504408,
2.51001059810901));
#43598=CARTESIAN_POINT('Ctrl Pts',(-2.67743773890551,-3.63935279939741,
2.53646789479348));
#43599=CARTESIAN_POINT('Ctrl Pts',(-2.07266008008808,-4.08428205375076,
2.56292519147795));
#43600=CARTESIAN_POINT('Ctrl Pts',(-1.35457937492269,-4.37520221466569,
2.58938248816241));
#43601=CARTESIAN_POINT('Ctrl Pts',(-0.610657058576137,-4.47667952851314,
2.61583978484688));
#43602=CARTESIAN_POINT('Ctrl Pts',(0.133265257770398,-4.57815684236058,
2.64229708153135));
#43603=CARTESIAN_POINT('Ctrl Pts',(0.9030291852981,-4.49019130914055,2.66875437821582));
#43604=CARTESIAN_POINT('Ctrl Pts',(1.60487832955586,-4.22349703344507,2.69521167490029));
#43605=CARTESIAN_POINT('Ctrl Pts',(2.30672747381364,-3.95680275774959,2.72166897158476));
#43606=CARTESIAN_POINT('Ctrl Pts',(2.94066183480147,-3.51137973957866,2.74812626826922));
#43607=CARTESIAN_POINT('Ctrl Pts',(3.42946890894601,-2.94148000958192,2.77458356495369));
#43608=CARTESIAN_POINT('Ctrl Pts',(3.91827598309054,-2.37158027958518,2.80104086163816));
#43609=CARTESIAN_POINT('Ctrl Pts',(4.26195577039178,-1.67720383776263,2.82749815832263));
#43610=CARTESIAN_POINT('Ctrl Pts',(4.41864845311758,-0.94292496624017,2.85395545500709));
#43611=CARTESIAN_POINT('Ctrl Pts',(4.4847062457604,-0.633370999882247,2.86510920250742));
#43612=CARTESIAN_POINT('Ctrl Pts',(4.51753158998749,-0.316725338941023,
2.87626295000774));
#43613=CARTESIAN_POINT('Ctrl Pts',(4.5174009456275,-5.29814202112051E-5,
2.88741669750807));
#43614=CARTESIAN_POINT('Ctrl Pts',(4.51806423128285,6.30519293007281E-5,
2.61258330249198));
#43615=CARTESIAN_POINT('Ctrl Pts',(4.51759393956657,-0.687506049970836,
2.58835569556429));
#43616=CARTESIAN_POINT('Ctrl Pts',(4.35830909853907,-1.37528559362468,2.5641280886366));
#43617=CARTESIAN_POINT('Ctrl Pts',(4.0551256392357,-1.9923648496729,2.53990048170891));
#43618=CARTESIAN_POINT('Ctrl Pts',(3.72403991720982,-2.66623449779077,2.51344318502445));
#43619=CARTESIAN_POINT('Ctrl Pts',(3.22135054533116,-3.25579181863177,2.48698588833998));
#43620=CARTESIAN_POINT('Ctrl Pts',(2.60828453275314,-3.68922938300052,2.46052859165551));
#43621=CARTESIAN_POINT('Ctrl Pts',(1.99521852017512,-4.12266694736928,2.43407129497105));
#43622=CARTESIAN_POINT('Ctrl Pts',(1.27177586689775,-4.3999847552658,2.40761399828658));
#43623=CARTESIAN_POINT('Ctrl Pts',(0.526071087432441,-4.48740580460158,
2.38115670160211));
#43624=CARTESIAN_POINT('Ctrl Pts',(-0.219633692032863,-4.57482685393736,
2.35469940491764));
#43625=CARTESIAN_POINT('Ctrl Pts',(-0.987600597686097,-4.47235114471241,
2.32824210823317));
#43626=CARTESIAN_POINT('Ctrl Pts',(-1.68429211034942,-4.19246010490287,
2.3017848115487));
#43627=CARTESIAN_POINT('Ctrl Pts',(-2.38098362301274,-3.91256906509334,
2.27532751486424));
#43628=CARTESIAN_POINT('Ctrl Pts',(-3.00639974268614,-3.45526269469925,
2.24887021817977));
#43629=CARTESIAN_POINT('Ctrl Pts',(-3.48436547816518,-2.87624040350871,
2.2224129214953));
#43630=CARTESIAN_POINT('Ctrl Pts',(-3.96233121364423,-2.29721811231817,
2.19595562481083));
#43631=CARTESIAN_POINT('Ctrl Pts',(-4.29284656492891,-1.59647990033118,
2.16949832812637));
#43632=CARTESIAN_POINT('Ctrl Pts',(-4.43565512801646,-0.859374906258969,
2.1430410314419));
#43633=CARTESIAN_POINT('Ctrl Pts',(-4.578463691104,-0.122269912186753,2.11658373475743));
#43634=CARTESIAN_POINT('Ctrl Pts',(-4.53356546599441,0.651201863970698,
2.09012643807296));
#43635=CARTESIAN_POINT('Ctrl Pts',(-4.30642900683079,1.36683241594063,2.06366914138849));
#43636=CARTESIAN_POINT('Ctrl Pts',(-4.07929254766716,2.08246296791056,2.03721184470403));
#43637=CARTESIAN_POINT('Ctrl Pts',(-3.66991785444949,2.74025229569297,2.01075454801956));
#43638=CARTESIAN_POINT('Ctrl Pts',(-3.12816631171559,3.26008238708848,1.98429725133509));
#43639=CARTESIAN_POINT('Ctrl Pts',(-2.58641476898168,3.77991247848399,1.95783995465062));
#43640=CARTESIAN_POINT('Ctrl Pts',(-1.91228637673154,4.16178333349259,1.93138265796616));
#43641=CARTESIAN_POINT('Ctrl Pts',(-1.18788922711582,4.3591835047376,1.90492536128169));
#43642=CARTESIAN_POINT('Ctrl Pts',(-0.463492077500105,4.55658367598262,
1.87846806459722));
#43643=CARTESIAN_POINT('Ctrl Pts',(0.311173829481187,4.56951316346406,1.85201076791275));
#43644=CARTESIAN_POINT('Ctrl Pts',(1.04175504380577,4.39639716966128,1.82555347122828));
#43645=CARTESIAN_POINT('Ctrl Pts',(1.77233625813035,4.2232811758585,1.79909617454381));
#43646=CARTESIAN_POINT('Ctrl Pts',(2.45883277979823,3.86411970077152,1.77263887785935));
#43647=CARTESIAN_POINT('Ctrl Pts',(3.01763009204651,3.36265821505193,1.74618158117488));
#43648=CARTESIAN_POINT('Ctrl Pts',(3.57642740429479,2.86119672933234,1.71972428449041));
#43649=CARTESIAN_POINT('Ctrl Pts',(4.00752550712348,2.21743523298015,1.69326698780594));
#43650=CARTESIAN_POINT('Ctrl Pts',(4.2584171290782,1.50978316287142,1.66680969112148));
#43651=CARTESIAN_POINT('Ctrl Pts',(4.42982474689917,1.02631960741915,1.64873422824498));
#43652=CARTESIAN_POINT('Ctrl Pts',(4.51712029378003,0.513034879908299,1.63065876536848));
#43653=CARTESIAN_POINT('Ctrl Pts',(4.51755838390264,-0.00010457874560596,
1.61258330249198));
#43654=CARTESIAN_POINT('Origin',(0.,0.,20.5));
#43655=CARTESIAN_POINT('',(4.51763087883895,0.00011359767064345,0.612583302491977));
#43656=CARTESIAN_POINT('',(4.5177656910975,-0.000116631996953637,0.887416697508071));
#43657=CARTESIAN_POINT('',(4.51775,5.53264807684796E-16,20.5));
#43658=CARTESIAN_POINT('',(-3.4337878873619,2.93584158412996,0.));
#43659=CARTESIAN_POINT('Ctrl Pts',(4.51763087883895,0.00011359767064345,
0.612583302491977));
#43660=CARTESIAN_POINT('Ctrl Pts',(4.51711863846112,-0.539057740350668,
0.59358994511926));
#43661=CARTESIAN_POINT('Ctrl Pts',(4.42053200733307,-1.07840729234144,0.574596587746541));
#43662=CARTESIAN_POINT('Ctrl Pts',(4.23165828048039,-1.58323058504537,0.555603230373824));
#43663=CARTESIAN_POINT('Ctrl Pts',(3.96856165521391,-2.28643746765176,0.529145933689356));
#43664=CARTESIAN_POINT('Ctrl Pts',(3.52639272074203,-2.92265018460396,0.502688637004889));
#43665=CARTESIAN_POINT('Ctrl Pts',(2.95900217961999,-3.41436616507663,0.476231340320421));
#43666=CARTESIAN_POINT('Ctrl Pts',(2.39161163849795,-3.90608214554931,0.449774043635953));
#43667=CARTESIAN_POINT('Ctrl Pts',(1.69899949072575,-4.25330138954245,0.423316746951485));
#43668=CARTESIAN_POINT('Ctrl Pts',(0.965534545329656,-4.41375671437595,
0.396859450267017));
#43669=CARTESIAN_POINT('Ctrl Pts',(0.232069599933564,-4.57421203920944,
0.370402153582549));
#43670=CARTESIAN_POINT('Ctrl Pts',(-0.542248143086422,-4.54790344488329,
0.343944856898081));
#43671=CARTESIAN_POINT('Ctrl Pts',(-1.26312545635881,-4.33799038903376,
0.317487560213613));
#43672=CARTESIAN_POINT('Ctrl Pts',(-1.9840027696312,-4.12807733318424,0.291030263529145));
#43673=CARTESIAN_POINT('Ctrl Pts',(-2.651439653156,-3.73455981581135,0.264572966844678));
#43674=CARTESIAN_POINT('Ctrl Pts',(-3.18410908512135,-3.20545326780586,
0.23811567016021));
#43675=CARTESIAN_POINT('Ctrl Pts',(-3.71677851708671,-2.67634671980037,
0.211658373475742));
#43676=CARTESIAN_POINT('Ctrl Pts',(-4.11468049749262,-2.01165114116227,
0.185201076791274));
#43677=CARTESIAN_POINT('Ctrl Pts',(-4.32941757999959,-1.29215909736801,
0.158743780106806));
#43678=CARTESIAN_POINT('Ctrl Pts',(-4.54415466250656,-0.572667053573755,
0.132286483422338));
#43679=CARTESIAN_POINT('Ctrl Pts',(-4.57572684711458,0.201621455376676,
0.10582918673787));
#43680=CARTESIAN_POINT('Ctrl Pts',(-4.42014586550132,0.936043740039453,
0.0793718900534021));
#43681=CARTESIAN_POINT('Ctrl Pts',(-4.26456488388806,1.67046602470223,0.0529145933689342));
#43682=CARTESIAN_POINT('Ctrl Pts',(-3.92183073605352,2.36502208507736,0.0264572966844666));
#43683=CARTESIAN_POINT('Ctrl Pts',(-3.43378788736187,2.93584158412999,-1.38777878078145E-15));
#43684=CARTESIAN_POINT('',(3.43409108914489,2.93606647242259,-1.66533453693773E-15));
#43685=CARTESIAN_POINT('Origin',(0.,0.,0.));
#43686=CARTESIAN_POINT('Ctrl Pts',(3.43409108914489,2.93606647242259,-1.66533453693773E-15));
#43687=CARTESIAN_POINT('Ctrl Pts',(2.96705577784701,3.48188002612677,0.0253131010459874));
#43688=CARTESIAN_POINT('Ctrl Pts',(2.36757358452891,3.91460873741651,0.0506262020919764));
#43689=CARTESIAN_POINT('Ctrl Pts',(1.70215900486043,4.18523117809474,0.0759393031379656));
#43690=CARTESIAN_POINT('Ctrl Pts',(1.00666654344788,4.46808621784236,0.102396599822434));
#43691=CARTESIAN_POINT('Ctrl Pts',(0.23914646876357,4.57384880856985,0.128853896506902));
#43692=CARTESIAN_POINT('Ctrl Pts',(-0.506923795872801,4.48961228541997,
0.15531119319137));
#43693=CARTESIAN_POINT('Ctrl Pts',(-1.25299406050917,4.40537576227008,0.181768489875837));
#43694=CARTESIAN_POINT('Ctrl Pts',(-1.9776145150976,4.13114012524282,0.208225786560305));
#43695=CARTESIAN_POINT('Ctrl Pts',(-2.59252418705973,3.70032015205329,0.234683083244772));
#43696=CARTESIAN_POINT('Ctrl Pts',(-3.20743385902187,3.26950017886376,0.26114037992924));
#43697=CARTESIAN_POINT('Ctrl Pts',(-3.71263274835771,2.68209586951196,0.287597676613709));
#43698=CARTESIAN_POINT('Ctrl Pts',(-4.04658977984313,2.00964543895375,0.314054973298177));
#43699=CARTESIAN_POINT('Ctrl Pts',(-4.38054681132855,1.33719500839555,0.340512269982645));
#43700=CARTESIAN_POINT('Ctrl Pts',(-4.54326198496355,0.579698456630952,
0.366969566667112));
#43701=CARTESIAN_POINT('Ctrl Pts',(-4.51491593042486,-0.170578278221808,
0.39342686335158));
#43702=CARTESIAN_POINT('Ctrl Pts',(-4.48656987588618,-0.920855013074566,
0.419884160036048));
#43703=CARTESIAN_POINT('Ctrl Pts',(-4.26716259317382,-1.66391193101549,
0.446341456720516));
#43704=CARTESIAN_POINT('Ctrl Pts',(-3.88341809255795,-2.30924747945238,
0.472798753404984));
#43705=CARTESIAN_POINT('Ctrl Pts',(-3.49967359194208,-2.95458302788927,
0.499256050089452));
#43706=CARTESIAN_POINT('Ctrl Pts',(-2.95159187342268,-3.50219720682213,
0.52571334677392));
#43707=CARTESIAN_POINT('Ctrl Pts',(-2.30592844750098,-3.88539017854139,
0.552170643458388));
#43708=CARTESIAN_POINT('Ctrl Pts',(-1.66026502157927,-4.26858315026064,
0.578627940142856));
#43709=CARTESIAN_POINT('Ctrl Pts',(-0.91701988825525,-4.48735491476628,
0.605085236827324));
#43710=CARTESIAN_POINT('Ctrl Pts',(-0.166719607306316,-4.51505986234428,
0.631542533511792));
#43711=CARTESIAN_POINT('Ctrl Pts',(0.583580673642613,-4.54276480992227,
0.65799983019626));
#43712=CARTESIAN_POINT('Ctrl Pts',(1.34093610221646,-4.37940294057262,0.684457126880727));
#43713=CARTESIAN_POINT('Ctrl Pts',(2.01310169166318,-4.04487125838886,0.710914423565195));
#43714=CARTESIAN_POINT('Ctrl Pts',(2.68526728110991,-3.7103395762051,0.737371720249663));
#43715=CARTESIAN_POINT('Ctrl Pts',(3.27224303142951,-3.20463808118722,0.763829016934131));
#43716=CARTESIAN_POINT('Ctrl Pts',(3.70253591076623,-2.58936080975925,0.790286313618599));
#43717=CARTESIAN_POINT('Ctrl Pts',(4.13282879010294,-1.9740835383313,0.816743610303067));
#43718=CARTESIAN_POINT('Ctrl Pts',(4.40643879845678,-1.24923049049327,0.843200906987535));
#43719=CARTESIAN_POINT('Ctrl Pts',(4.49004055820744,-0.503087883691874,
0.869658203672002));
#43720=CARTESIAN_POINT('Ctrl Pts',(4.50874543387838,-0.336147561686243,
0.875577701617358));
#43721=CARTESIAN_POINT('Ctrl Pts',(4.51793876013751,-0.168141513884366,
0.881497199562714));
#43722=CARTESIAN_POINT('Ctrl Pts',(4.5177656910975,-0.000116631996953637,
0.887416697508071));
#43723=CARTESIAN_POINT('Origin',(0.,0.,-2.20833684463713));
#43724=CARTESIAN_POINT('',(5.07403060246553,1.54698778687123E-5,39.208336844637));
#43725=CARTESIAN_POINT('',(5.07396752856948,-6.48011021279027E-5,39.2916631553629));
#43726=CARTESIAN_POINT('',(5.0736,-1.85409460923845E-12,-2.20833684463713));
#43727=CARTESIAN_POINT('',(-1.31303618635666,-4.90075024188317,40.));
#43728=CARTESIAN_POINT('Ctrl Pts',(5.07396752856948,-6.48011021277175E-5,
39.2916631553629));
#43729=CARTESIAN_POINT('Ctrl Pts',(5.07347424400433,0.779307331517198,39.3161170634328));
#43730=CARTESIAN_POINT('Ctrl Pts',(4.69381943413572,2.40236770827343,39.3670282681872));
#43731=CARTESIAN_POINT('Ctrl Pts',(3.03470961035893,4.33144609848054,39.4443967696262));
#43732=CARTESIAN_POINT('Ctrl Pts',(0.593383061700927,5.25537632570972,39.5237686596795));
#43733=CARTESIAN_POINT('Ctrl Pts',(-1.99247705733066,4.8990504464678,39.603140549733));
#43734=CARTESIAN_POINT('Ctrl Pts',(-4.09299916691649,3.34943642687039,39.6825124397864));
#43735=CARTESIAN_POINT('Ctrl Pts',(-5.19642846461573,0.983699440459269,
39.7618843298398));
#43736=CARTESIAN_POINT('Ctrl Pts',(-5.03410925482033,-1.62126816458454,
39.8412562198932));
#43737=CARTESIAN_POINT('Ctrl Pts',(-3.6453165085118,-3.83208153227987,39.9206281099466));
#43738=CARTESIAN_POINT('Ctrl Pts',(-2.12771778283764,-4.68247622999901,
39.9735427033155));
#43739=CARTESIAN_POINT('Ctrl Pts',(-1.31303618635638,-4.90075024188325,
40.));
#43740=CARTESIAN_POINT('',(1.31317395760221,-4.90115117757563,40.));
#43741=CARTESIAN_POINT('Origin',(0.,0.,40.));
#43742=CARTESIAN_POINT('Ctrl Pts',(5.07403060246553,1.54698778688793E-5,
39.208336844637));
#43743=CARTESIAN_POINT('Ctrl Pts',(5.07403315687698,0.0146420671929676,
39.2087957918851));
#43744=CARTESIAN_POINT('Ctrl Pts',(5.07040151797183,0.872458469457581,39.2357120358177));
#43745=CARTESIAN_POINT('Ctrl Pts',(4.62253485344793,2.56965255248844,39.2890855764349));
#43746=CARTESIAN_POINT('Ctrl Pts',(2.83047200092405,4.46759066254981,39.3684574664882));
#43747=CARTESIAN_POINT('Ctrl Pts',(0.34891291852996,5.27723479734496,39.4478293565417));
#43748=CARTESIAN_POINT('Ctrl Pts',(-2.21764149317963,4.80135391043001,39.527201246595));
#43749=CARTESIAN_POINT('Ctrl Pts',(-4.24398161873814,3.15587819282133,39.6065731366485));
#43750=CARTESIAN_POINT('Ctrl Pts',(-5.23650047694821,0.74162931109825,39.6859450267018));
#43751=CARTESIAN_POINT('Ctrl Pts',(-4.9534132521342,-1.85326330477585,39.7653169167553));
#43752=CARTESIAN_POINT('Ctrl Pts',(-3.46369715057683,-3.99673439595749,
39.8446888068086));
#43753=CARTESIAN_POINT('Ctrl Pts',(-1.1638488125998,-5.14969078544563,39.9229165012236));
#43754=CARTESIAN_POINT('Ctrl Pts',(0.533836595431815,-5.10962665469158,
39.974686898954));
#43755=CARTESIAN_POINT('Ctrl Pts',(1.31317395760221,-4.90115117757563,40.));
#43756=CARTESIAN_POINT('Origin',(0.,0.,-2.20833684463713));
#43757=CARTESIAN_POINT('',(5.07325764975804,-8.44407784307555E-5,38.208336844637));
#43758=CARTESIAN_POINT('',(5.07316912366228,-1.81818814078922E-5,38.2916631553629));
#43759=CARTESIAN_POINT('',(5.0736,-1.85409460923845E-12,-2.20833684463713));
#43760=CARTESIAN_POINT('Ctrl Pts',(5.07316912366228,-1.81818814076751E-5,
38.2916631553629));
#43761=CARTESIAN_POINT('Ctrl Pts',(5.07311400239361,0.441352830351579,38.3055055398681));
#43762=CARTESIAN_POINT('Ctrl Pts',(4.90711571561459,1.72636801461904,38.3458052210578));
#43763=CARTESIAN_POINT('Ctrl Pts',(3.83482475204887,3.64212307300276,38.4125621989319));
#43764=CARTESIAN_POINT('Ctrl Pts',(1.62575061805696,5.03268082057242,38.4919340889853));
#43765=CARTESIAN_POINT('Ctrl Pts',(-0.979352771366501,5.19728867487039,
38.5713059790387));
#43766=CARTESIAN_POINT('Ctrl Pts',(-3.3458879870052,4.09584848370752,38.6506778690921));
#43767=CARTESIAN_POINT('Ctrl Pts',(-4.89737230716795,1.99666872129193,38.7300497591456));
#43768=CARTESIAN_POINT('Ctrl Pts',(-5.2558675504918,-0.588895222855594,
38.809421649199));
#43769=CARTESIAN_POINT('Ctrl Pts',(-4.33404513553914,-3.03100540392653,
38.8887935392523));
#43770=CARTESIAN_POINT('Ctrl Pts',(-2.35645883694701,-4.73476973691708,
38.9681654293058));
#43771=CARTESIAN_POINT('Ctrl Pts',(0.195155463808245,-5.28515396379923,
39.0475373193592));
#43772=CARTESIAN_POINT('Ctrl Pts',(2.69923061743519,-4.54808766460433,39.1269092094126));
#43773=CARTESIAN_POINT('Ctrl Pts',(4.5457786161602,-2.70311485851688,39.2062810994659));
#43774=CARTESIAN_POINT('Ctrl Pts',(5.05724155748156,-0.970965988519946,
39.2611990814494));
#43775=CARTESIAN_POINT('Ctrl Pts',(5.07400794095178,-0.063914933051532,
39.2896597667484));
#43776=CARTESIAN_POINT('Ctrl Pts',(5.07396752856948,-6.48011021277175E-5,
39.2916631553629));
#43777=CARTESIAN_POINT('Ctrl Pts',(5.07325764975804,-8.44407784305126E-5,
38.208336844637));
#43778=CARTESIAN_POINT('Ctrl Pts',(5.07294945930103,0.51977335908998,38.2246415650049));
#43779=CARTESIAN_POINT('Ctrl Pts',(4.86451980067584,1.88343404898941,38.2674035820572));
#43780=CARTESIAN_POINT('Ctrl Pts',(3.66171031660113,3.81612616476472,38.336622895794));
#43781=CARTESIAN_POINT('Ctrl Pts',(1.39049711694169,5.10269135980963,38.4159947858473));
#43782=CARTESIAN_POINT('Ctrl Pts',(-1.21943810235573,5.14625223481529,38.4953666759008));
#43783=CARTESIAN_POINT('Ctrl Pts',(-3.53232089954511,3.93619745533324,38.5747385659542));
#43784=CARTESIAN_POINT('Ctrl Pts',(-4.98473814342406,1.76729369047725,38.6541104560076));
#43785=CARTESIAN_POINT('Ctrl Pts',(-5.22288421068334,-0.832118909543577,
38.733482346061));
#43786=CARTESIAN_POINT('Ctrl Pts',(-4.18874724188046,-3.22882917750522,
38.8128542361144));
#43787=CARTESIAN_POINT('Ctrl Pts',(-2.13424072225093,-4.83900381899058,
38.8922261261678));
#43788=CARTESIAN_POINT('Ctrl Pts',(0.440162123945958,-5.27040781417516,
38.9715980162212));
#43789=CARTESIAN_POINT('Ctrl Pts',(2.90734243084964,-4.41795218255951,39.0509699062746));
#43790=CARTESIAN_POINT('Ctrl Pts',(4.65612987828293,-2.500445050276,39.1298828490799));
#43791=CARTESIAN_POINT('Ctrl Pts',(5.07388590069044,-0.828549010266373,
39.1823384952007));
#43792=CARTESIAN_POINT('Ctrl Pts',(5.07403060246553,1.54698778688793E-5,
39.208336844637));
#43793=CARTESIAN_POINT('Origin',(0.,0.,-2.20833684463713));
#43794=CARTESIAN_POINT('',(5.07364050160013,0.000130038443658109,37.208336844637));
#43795=CARTESIAN_POINT('',(5.07387656802193,9.59844669708175E-5,37.2916631553629));
#43796=CARTESIAN_POINT('',(5.0736,-1.85409460923845E-12,-2.20833684463713));
#43797=CARTESIAN_POINT('Ctrl Pts',(5.07387656802193,9.59844669710073E-5,
37.2916631553629));
#43798=CARTESIAN_POINT('Ctrl Pts',(5.07396569861154,0.103072231247123,37.2948940163033));
#43799=CARTESIAN_POINT('Ctrl Pts',(5.04574853055582,1.04926503651591,37.3245821739283));
#43800=CARTESIAN_POINT('Ctrl Pts',(4.48202491545551,2.80756015154514,37.3807276282377));
#43801=CARTESIAN_POINT('Ctrl Pts',(2.59328691715162,4.6093171199916,37.4600995182911));
#43802=CARTESIAN_POINT('Ctrl Pts',(0.0728299659736646,5.28825464055466,
37.5394714083445));
#43803=CARTESIAN_POINT('Ctrl Pts',(-2.46536820371075,4.67898503603898,37.6188432983979));
#43804=CARTESIAN_POINT('Ctrl Pts',(-4.40300813596802,2.92992503348812,37.6982151884513));
#43805=CARTESIAN_POINT('Ctrl Pts',(-5.26808503220261,0.467141778084607,
37.7775870785047));
#43806=CARTESIAN_POINT('Ctrl Pts',(-4.84986807528987,-2.10943618050861,
37.8569589685581));
#43807=CARTESIAN_POINT('Ctrl Pts',(-3.2502339902585,-4.17216015459505,37.9363308586115));
#43808=CARTESIAN_POINT('Ctrl Pts',(-0.858850099431265,-5.21855515011692,
38.0157027486649));
#43809=CARTESIAN_POINT('Ctrl Pts',(1.74174777450972,-4.99372166181591,38.0950746387183));
#43810=CARTESIAN_POINT('Ctrl Pts',(3.91805974601555,-3.55242863073569,38.1744465287717));
#43811=CARTESIAN_POINT('Ctrl Pts',(4.92684606433671,-1.64805066527608,38.2399760343199));
#43812=CARTESIAN_POINT('Ctrl Pts',(5.0732193570569,-0.402250655317197,38.2790482431836));
#43813=CARTESIAN_POINT('Ctrl Pts',(5.07316912366228,-1.81818814076751E-5,
38.2916631553629));
#43814=CARTESIAN_POINT('Ctrl Pts',(5.07364050160013,0.000130038443658265,
37.208336844637));
#43815=CARTESIAN_POINT('Ctrl Pts',(5.07382783063862,0.181611936494348,37.2140300414401));
#43816=CARTESIAN_POINT('Ctrl Pts',(5.01990561118457,1.20636170521342,37.2461805349277));
#43817=CARTESIAN_POINT('Ctrl Pts',(4.34693493313475,3.01249033764469,37.3047883250998));
#43818=CARTESIAN_POINT('Ctrl Pts',(2.37663436681862,4.72467463787371,37.3841602151531));
#43819=CARTESIAN_POINT('Ctrl Pts',(-0.17260907066365,5.28593865420645,37.4635321052065));
#43820=CARTESIAN_POINT('Ctrl Pts',(-2.67980532059584,4.55955971460153,37.54290399526));
#43821=CARTESIAN_POINT('Ctrl Pts',(-4.53420692607955,2.72248212093334,37.6222758853133));
#43822=CARTESIAN_POINT('Ctrl Pts',(-5.28408576066665,0.222213908718847,
37.7016477753668));
#43823=CARTESIAN_POINT('Ctrl Pts',(-4.74677300008161,-2.33218511979937,
37.7810196654201));
#43824=CARTESIAN_POINT('Ctrl Pts',(-3.05315684347904,-4.31846901533503,
37.8603915554736));
#43825=CARTESIAN_POINT('Ctrl Pts',(-0.615798437855754,-5.25278341751105,
37.9397634455269));
#43826=CARTESIAN_POINT('Ctrl Pts',(1.97156710418767,-4.90753140600709,38.0191353355804));
#43827=CARTESIAN_POINT('Ctrl Pts',(4.07866326363087,-3.36681560666115,38.0985072256337));
#43828=CARTESIAN_POINT('Ctrl Pts',(4.96346005639167,-1.49092415374923,38.1615743953193));
#43829=CARTESIAN_POINT('Ctrl Pts',(5.07344955290414,-0.323787998268402,
38.1981842683204));
#43830=CARTESIAN_POINT('Ctrl Pts',(5.07325764975804,-8.44407784305126E-5,
38.208336844637));
#43831=CARTESIAN_POINT('Origin',(0.,0.,-2.20833684463713));
#43832=CARTESIAN_POINT('',(5.07371855919287,-0.000123991516001801,36.208336844637));
#43833=CARTESIAN_POINT('',(5.07347409402005,-0.000127990615926579,36.2916631553629));
#43834=CARTESIAN_POINT('',(5.0736,-1.85409460923845E-12,-2.20833684463713));
#43835=CARTESIAN_POINT('Ctrl Pts',(5.07347409402005,-0.00012799061592652,
36.2916631553629));
#43836=CARTESIAN_POINT('Ctrl Pts',(5.07289252391416,0.608034774450749,36.3107397894231));
#43837=CARTESIAN_POINT('Ctrl Pts',(4.81166108430775,2.06014185956918,36.3562737201677));
#43838=CARTESIAN_POINT('Ctrl Pts',(3.45741385862894,4.002153265115,36.4282649475969));
#43839=CARTESIAN_POINT('Ctrl Pts',(1.12210854951209,5.16834729390565,36.5076368376502));
#43840=CARTESIAN_POINT('Ctrl Pts',(-1.4865399185207,5.07554336184357,36.5870087277037));
#43841=CARTESIAN_POINT('Ctrl Pts',(-3.73307055280216,3.74634830136112,36.666380617757));
#43842=CARTESIAN_POINT('Ctrl Pts',(-5.07023346343257,1.50455108706837,36.7457525078105));
#43843=CARTESIAN_POINT('Ctrl Pts',(-5.17229872514219,-1.10375144176689,
36.8251243978638));
#43844=CARTESIAN_POINT('Ctrl Pts',(-4.01440346609619,-3.44318256250012,
36.9044962879173));
#43845=CARTESIAN_POINT('Ctrl Pts',(-1.87860840844056,-4.94386203236358,
36.9838681779707));
#43846=CARTESIAN_POINT('Ctrl Pts',(0.71481149928202,-5.24022765419639,37.0632400680241));
#43847=CARTESIAN_POINT('Ctrl Pts',(3.13410490798792,-4.26008541851396,37.1426119580775));
#43848=CARTESIAN_POINT('Ctrl Pts',(4.72253605350391,-2.32433471697507,37.2187529871904));
#43849=CARTESIAN_POINT('Ctrl Pts',(5.07323581438062,-0.740193128270358,
37.2684367196189));
#43850=CARTESIAN_POINT('Ctrl Pts',(5.07387656802193,9.59844669710073E-5,
37.2916631553629));
#43851=CARTESIAN_POINT('Ctrl Pts',(5.07371855919287,-0.000123991516001801,
36.208336844637));
#43852=CARTESIAN_POINT('Ctrl Pts',(5.07301904482133,0.686442797877024,36.2298758145598));
#43853=CARTESIAN_POINT('Ctrl Pts',(4.76024594010631,2.21696867292356,36.2778720811671));
#43854=CARTESIAN_POINT('Ctrl Pts',(3.26800144929601,4.15825779320007,36.3523256444589));
#43855=CARTESIAN_POINT('Ctrl Pts',(0.881102883784141,5.2148441065383,36.4316975345123));
#43856=CARTESIAN_POINT('Ctrl Pts',(-1.72043039392939,5.00110593838543,36.5110694245656));
#43857=CARTESIAN_POINT('Ctrl Pts',(-3.90287063578981,3.56910943340206,36.5904413146191));
#43858=CARTESIAN_POINT('Ctrl Pts',(-5.13458022962944,1.26768577053169,36.6698132046725));
#43859=CARTESIAN_POINT('Ctrl Pts',(-5.11551744473188,-1.34254334006536,
36.7491850947259));
#43860=CARTESIAN_POINT('Ctrl Pts',(-3.85032593330342,-3.62573186469175,
36.8285569847793));
#43861=CARTESIAN_POINT('Ctrl Pts',(-1.64720354707418,-5.02570013250056,
36.9079288748327));
#43862=CARTESIAN_POINT('Ctrl Pts',(0.957173977199105,-5.20141897223083,
36.9873007648861));
#43863=CARTESIAN_POINT('Ctrl Pts',(3.32838603929536,-4.11008366347129,37.0666726549395));
#43864=CARTESIAN_POINT('Ctrl Pts',(4.77688430036561,-2.16763522711972,37.1403513481898));
#43865=CARTESIAN_POINT('Ctrl Pts',(5.07295727932621,-0.661766675847902,
37.1875727447556));
#43866=CARTESIAN_POINT('Ctrl Pts',(5.07364050160013,0.000130038443658265,
37.208336844637));
#43867=CARTESIAN_POINT('Origin',(0.,0.,-2.20833684463713));
#43868=CARTESIAN_POINT('',(5.07321765521711,6.54440514302745E-5,35.208336844637));
#43869=CARTESIAN_POINT('',(5.07337786466077,0.000116280867786642,35.2916631553629));
#43870=CARTESIAN_POINT('',(5.0736,-1.85409460923845E-12,-2.20833684463713));
#43871=CARTESIAN_POINT('Ctrl Pts',(5.07337786466077,0.000116280867786742,
35.2916631553629));
#43872=CARTESIAN_POINT('Ctrl Pts',(5.07360553071623,0.269998548266127,35.3001282658583));
#43873=CARTESIAN_POINT('Ctrl Pts',(4.98629871182508,1.38323904612086,35.3350506730382));
#43874=CARTESIAN_POINT('Ctrl Pts',(4.18367369924664,3.23540039647985,35.3964303769026));
#43875=CARTESIAN_POINT('Ctrl Pts',(2.12664217080567,4.8423480280398,35.4758022669559));
#43876=CARTESIAN_POINT('Ctrl Pts',(-0.448434683200953,5.2697103983248,35.5551741570095));
#43877=CARTESIAN_POINT('Ctrl Pts',(-2.91427384097317,4.41338297988397,35.6345460470627));
#43878=CARTESIAN_POINT('Ctrl Pts',(-4.67020234172003,2.48196523640092,35.7139179371163));
#43879=CARTESIAN_POINT('Ctrl Pts',(-5.28847988934142,-0.0540537449324728,
35.7932898271696));
#43880=CARTESIAN_POINT('Ctrl Pts',(-4.61849544177097,-2.57690535364626,
35.872661717223));
#43881=CARTESIAN_POINT('Ctrl Pts',(-2.82345572745135,-4.47202852209511,
35.9520336072764));
#43882=CARTESIAN_POINT('Ctrl Pts',(-0.340628447537815,-5.27777544122882,
36.0314054973298));
#43883=CARTESIAN_POINT('Ctrl Pts',(2.22517516822766,-4.79786794503694,36.1107773873833));
#43884=CARTESIAN_POINT('Ctrl Pts',(4.2489310383545,-3.14921043733466,36.1901492774366));
#43885=CARTESIAN_POINT('Ctrl Pts',(5.00002147582269,-1.31403716914749,36.2504445334299));
#43886=CARTESIAN_POINT('Ctrl Pts',(5.07369910083888,-0.235423387877496,
36.2842824927386));
#43887=CARTESIAN_POINT('Ctrl Pts',(5.07347409402005,-0.00012799061592652,
36.2916631553629));
#43888=CARTESIAN_POINT('Ctrl Pts',(5.07321765521711,6.54440514305868E-5,
35.208336844637));
#43889=CARTESIAN_POINT('Ctrl Pts',(5.07337613287412,0.348482730653562,35.2192642909951));
#43890=CARTESIAN_POINT('Ctrl Pts',(4.95236148577976,1.54037186125541,35.2566490340376));
#43891=CARTESIAN_POINT('Ctrl Pts',(4.02905439992751,3.42602714375337,35.3204910737646));
#43892=CARTESIAN_POINT('Ctrl Pts',(1.8996801667365,4.93580354262787,35.3998629638181));
#43893=CARTESIAN_POINT('Ctrl Pts',(-0.69245195020073,5.24322912373406,35.4792348538714));
#43894=CARTESIAN_POINT('Ctrl Pts',(-3.11590430478548,4.27341569598948,35.5586067439249));
#43895=CARTESIAN_POINT('Ctrl Pts',(-4.78032926766171,2.26260766374704,35.6379786339782));
#43896=CARTESIAN_POINT('Ctrl Pts',(-5.28027660201491,-0.299366587187078,
35.7173505240316));
#43897=CARTESIAN_POINT('Ctrl Pts',(-4.49396024381123,-2.78841580011912,
35.7967224140851));
#43898=CARTESIAN_POINT('Ctrl Pts',(-2.61292511742748,-4.59821309619579,
35.8760943041384));
#43899=CARTESIAN_POINT('Ctrl Pts',(-0.0953872160500441,-5.28789586001125,
35.9554661941919));
#43900=CARTESIAN_POINT('Ctrl Pts',(2.4453868000212,-4.68945889688694,36.0348380842453));
#43901=CARTESIAN_POINT('Ctrl Pts',(4.39047000437915,-2.94868012642215,36.1142099742987));
#43902=CARTESIAN_POINT('Ctrl Pts',(5.02844178521537,-1.15692185290368,36.1720428944293));
#43903=CARTESIAN_POINT('Ctrl Pts',(5.07387829014872,-0.156898425299628,
36.2034185178754));
#43904=CARTESIAN_POINT('Ctrl Pts',(5.07371855919287,-0.000123991516001801,
36.208336844637));
#43905=CARTESIAN_POINT('Origin',(0.,0.,-2.20833684463713));
#43906=CARTESIAN_POINT('',(5.07403267809782,1.0680673442065E-5,34.208336844637));
#43907=CARTESIAN_POINT('',(5.07395837593185,-6.84743504405761E-5,34.2916631553629));
#43908=CARTESIAN_POINT('',(5.0736,-1.85409460923845E-12,-2.20833684463713));
#43909=CARTESIAN_POINT('Ctrl Pts',(5.07395837593184,-6.84743504405106E-5,
34.2916631553629));
#43910=CARTESIAN_POINT('Ctrl Pts',(5.07344266957576,0.774748712740892,34.315974038978));
#43911=CARTESIAN_POINT('Ctrl Pts',(4.69722240792898,2.39327548011594,34.3667422192777));
#43912=CARTESIAN_POINT('Ctrl Pts',(3.04637426047967,4.32325632045994,34.4439676962618));
#43913=CARTESIAN_POINT('Ctrl Pts',(0.607552238322964,5.25374358196314,34.5233395863151));
#43914=CARTESIAN_POINT('Ctrl Pts',(-1.97926816429518,4.90443053586424,34.6027114763686));
#43915=CARTESIAN_POINT('Ctrl Pts',(-4.08394322312674,3.36040906700167,34.6820833664219));
#43916=CARTESIAN_POINT('Ctrl Pts',(-5.19377875245966,0.997799387556786,
34.7614552564754));
#43917=CARTESIAN_POINT('Ctrl Pts',(-5.03842127392763,-1.60787201410546,
34.8408271465287));
#43918=CARTESIAN_POINT('Ctrl Pts',(-3.65571552542313,-3.82186935209593,
34.9201990365822));
#43919=CARTESIAN_POINT('Ctrl Pts',(-1.38248556671468,-5.10486777548014,
34.9995709266355));
#43920=CARTESIAN_POINT('Ctrl Pts',(1.22751481596557,-5.14433170819057,35.078942816689));
#43921=CARTESIAN_POINT('Ctrl Pts',(3.53849530653457,-3.93064782357091,35.1583147067423));
#43922=CARTESIAN_POINT('Ctrl Pts',(4.83296736710027,-1.99102597475866,35.2292214863004));
#43923=CARTESIAN_POINT('Ctrl Pts',(5.07289397138366,-0.573505529121166,
35.2736709691739));
#43924=CARTESIAN_POINT('Ctrl Pts',(5.07337786466077,0.000116280867786742,
35.2916631553629));
#43925=CARTESIAN_POINT('Ctrl Pts',(5.07403267809783,1.06806734422689E-5,
34.208336844637));
#43926=CARTESIAN_POINT('Ctrl Pts',(5.07403390825189,0.0100790925016438,
34.2086527674304));
#43927=CARTESIAN_POINT('Ctrl Pts',(5.07154731505229,0.863336953552071,34.2354259869081));
#43928=CARTESIAN_POINT('Ctrl Pts',(4.62944563286023,2.55718096342464,34.2886565030704));
#43929=CARTESIAN_POINT('Ctrl Pts',(2.84250620674923,4.45994392474861,34.3680283931238));
#43930=CARTESIAN_POINT('Ctrl Pts',(0.363138560454883,5.27627441792225,34.4474002831772));
#43931=CARTESIAN_POINT('Ctrl Pts',(-2.20468883537271,4.80731614172534,34.5267721732306));
#43932=CARTESIAN_POINT('Ctrl Pts',(-4.23545891089946,3.1673062942179,34.606144063284));
#43933=CARTESIAN_POINT('Ctrl Pts',(-5.23448057076036,0.755747644152594,
34.6855159533374));
#43934=CARTESIAN_POINT('Ctrl Pts',(-4.95839434991029,-1.83990945920924,
34.7648878433908));
#43935=CARTESIAN_POINT('Ctrl Pts',(-3.47445424064183,-3.98736869087822,
34.8442597334442));
#43936=CARTESIAN_POINT('Ctrl Pts',(-1.14414476892706,-5.16351373534018,
34.9236316234976));
#43937=CARTESIAN_POINT('Ctrl Pts',(1.4648758359769,-5.0818382631171,35.003003513551));
#43938=CARTESIAN_POINT('Ctrl Pts',(3.71705592968454,-3.76223823845686,35.0823754036044));
#43939=CARTESIAN_POINT('Ctrl Pts',(4.87836197951498,-1.83401443292226,35.1508198472998));
#43940=CARTESIAN_POINT('Ctrl Pts',(5.07299243019996,-0.495097664945923,
35.1928069943106));
#43941=CARTESIAN_POINT('Ctrl Pts',(5.07321765521711,6.54440514305868E-5,
35.208336844637));
#43942=CARTESIAN_POINT('Origin',(0.,0.,-2.20833684463713));
#43943=CARTESIAN_POINT('',(5.07324948390142,-8.11089730112791E-5,33.208336844637));
#43944=CARTESIAN_POINT('',(5.07316757009266,-1.39624117367057E-5,33.2916631553629));
#43945=CARTESIAN_POINT('',(5.0736,-1.85409460923845E-12,-2.20833684463713));
#43946=CARTESIAN_POINT('Ctrl Pts',(5.07316757009266,-1.39624117367898E-5,
33.2916631553629));
#43947=CARTESIAN_POINT('Ctrl Pts',(5.07312569317602,0.436797029802116,33.3053625154133));
#43948=CARTESIAN_POINT('Ctrl Pts',(4.90946580291021,1.7172430470973,33.3455191721481));
#43949=CARTESIAN_POINT('Ctrl Pts',(3.84462977702742,3.63177136187071,33.4121331255675));
#43950=CARTESIAN_POINT('Ctrl Pts',(1.63931253580255,5.02827960213734,33.4915050156209));
#43951=CARTESIAN_POINT('Ctrl Pts',(-0.965337610587002,5.19991006123145,
33.5708769056743));
#43952=CARTESIAN_POINT('Ctrl Pts',(-3.33483365177614,4.1048539392153,33.6502487957277));
#43953=CARTESIAN_POINT('Ctrl Pts',(-4.89197159692173,2.00986448354636,33.7296206857811));
#43954=CARTESIAN_POINT('Ctrl Pts',(-5.25743608925264,-0.574723511554913,
33.8089925758345));
#43955=CARTESIAN_POINT('Ctrl Pts',(-4.34220078737896,-3.01931013137032,
33.888364465888));
#43956=CARTESIAN_POINT('Ctrl Pts',(-2.36921498499824,-4.72839948631349,
33.9677363559413));
#43957=CARTESIAN_POINT('Ctrl Pts',(0.18090634355963,-5.28566119252548,34.0471082459947));
#43958=CARTESIAN_POINT('Ctrl Pts',(2.68695928725581,-4.55534753185087,34.1264801360481));
#43959=CARTESIAN_POINT('Ctrl Pts',(4.53847489605999,-2.71536129550809,34.2058520261016));
#43960=CARTESIAN_POINT('Ctrl Pts',(5.05594943598948,-0.980087925357289,
34.2609130325398));
#43961=CARTESIAN_POINT('Ctrl Pts',(5.07400390775537,-0.0684772480926434,
34.2895167422936));
#43962=CARTESIAN_POINT('Ctrl Pts',(5.07395837593184,-6.84743504405106E-5,
34.2916631553629));
#43963=CARTESIAN_POINT('Ctrl Pts',(5.07324948390142,-8.1108973011175E-5,
33.208336844637));
#43964=CARTESIAN_POINT('Ctrl Pts',(5.07295666213735,0.515218890813949,33.22449854055));
#43965=CARTESIAN_POINT('Ctrl Pts',(4.86710522495599,1.87431284273704,33.2671175331475));
#43966=CARTESIAN_POINT('Ctrl Pts',(3.67198507285579,3.80624052997629,33.3361938224296));
#43967=CARTESIAN_POINT('Ctrl Pts',(1.40424863498483,5.09892411381589,33.4155657124829));
#43968=CARTESIAN_POINT('Ctrl Pts',(-1.20555966211678,5.14952106980705,33.4949376025364));
#43969=CARTESIAN_POINT('Ctrl Pts',(-3.52169629398785,3.94570609146478,33.5743094925897));
#43970=CARTESIAN_POINT('Ctrl Pts',(-4.979955503786,1.78072584291395,33.6536813826432));
#43971=CARTESIAN_POINT('Ctrl Pts',(-5.22510857580638,-0.818035279400921,
33.7330532726965));
#43972=CARTESIAN_POINT('Ctrl Pts',(-4.19743676434199,-3.2175248183441,33.81242516275));
#43973=CARTESIAN_POINT('Ctrl Pts',(-2.14727864795256,-4.83323243340904,
33.8917970528034));
#43974=CARTESIAN_POINT('Ctrl Pts',(0.425951794157462,-5.27157532587404,
33.9711689428568));
#43975=CARTESIAN_POINT('Ctrl Pts',(2.89542132203897,-4.4257741373902,34.0505408329101));
#43976=CARTESIAN_POINT('Ctrl Pts',(4.6525507987008,-2.50952187653605,34.1295968001703));
#43977=CARTESIAN_POINT('Ctrl Pts',(5.07393088766675,-0.833110966960862,
34.1821954707459));
#43978=CARTESIAN_POINT('Ctrl Pts',(5.07403267809783,1.06806734422689E-5,
34.208336844637));
#43979=CARTESIAN_POINT('Origin',(0.,0.,-2.20833684463713));
#43980=CARTESIAN_POINT('',(5.07365497060222,0.000129255909634973,32.208336844637));
#43981=CARTESIAN_POINT('',(5.0738885135215,9.2741528424134E-5,32.2916631553629));
#43982=CARTESIAN_POINT('',(5.0736,-1.85409460923845E-12,-2.20833684463713));
#43983=CARTESIAN_POINT('Ctrl Pts',(5.0738885135215,9.27415284240896E-5,
32.2916631553629));
#43984=CARTESIAN_POINT('Ctrl Pts',(5.07397157552195,0.0985097427010157,
32.2947509918485));
#43985=CARTESIAN_POINT('Ctrl Pts',(5.04713500973232,1.0401410882179,32.3242961250187));
#43986=CARTESIAN_POINT('Ctrl Pts',(4.48957765297736,2.79546665964672,32.3802985548733));
#43987=CARTESIAN_POINT('Ctrl Pts',(2.60570395470567,4.60230901263064,32.4596704449267));
#43988=CARTESIAN_POINT('Ctrl Pts',(0.0870865406955613,5.28803907717593,
32.5390423349801));
#43989=CARTESIAN_POINT('Ctrl Pts',(-2.45274496186521,4.68561452739711,32.6184142250335));
#43990=CARTESIAN_POINT('Ctrl Pts',(-4.39509322077448,2.94178465017617,32.6977861150869));
#43991=CARTESIAN_POINT('Ctrl Pts',(-5.26680649947691,0.48134254370224,32.7771580051403));
#43992=CARTESIAN_POINT('Ctrl Pts',(-4.85553737278523,-2.09635354098391,
32.8565298951937));
#43993=CARTESIAN_POINT('Ctrl Pts',(-3.26147008963279,-4.16338254328624,
32.9359017852471));
#43994=CARTESIAN_POINT('Ctrl Pts',(-0.8729159117874,-5.21622077353502,33.0152736753005));
#43995=CARTESIAN_POINT('Ctrl Pts',(1.72827865000283,-4.99839916925953,33.0946455653539));
#43996=CARTESIAN_POINT('Ctrl Pts',(3.9084683581323,-3.5629785911213,33.1740174554073));
#43997=CARTESIAN_POINT('Ctrl Pts',(4.92459807825024,-1.65717664129123,33.2396899854103));
#43998=CARTESIAN_POINT('Ctrl Pts',(5.07320656921722,-0.406807195031642,
33.2789052187288));
#43999=CARTESIAN_POINT('Ctrl Pts',(5.07316757009266,-1.39624117367898E-5,
33.2916631553629));
#44000=CARTESIAN_POINT('Ctrl Pts',(5.07365497060222,0.000129255909635077,
32.208336844637));
#44001=CARTESIAN_POINT('Ctrl Pts',(5.07383759281576,0.177050513766622,32.2138870169853));
#44002=CARTESIAN_POINT('Ctrl Pts',(5.02150924629178,1.19723596214486,32.2458944860181));
#44003=CARTESIAN_POINT('Ctrl Pts',(4.35504064192764,3.00076029606972,32.3043592517354));
#44004=CARTESIAN_POINT('Ctrl Pts',(2.3893631891323,4.71825019448202,32.3837311417886));
#44005=CARTESIAN_POINT('Ctrl Pts',(-0.158357847769981,5.28638478918814,
32.4631030318421));
#44006=CARTESIAN_POINT('Ctrl Pts',(-2.66750326347463,4.56676775046226,32.5424749218955));
#44007=CARTESIAN_POINT('Ctrl Pts',(-4.52685078861515,2.73469619609277,32.6218468119489));
#44008=CARTESIAN_POINT('Ctrl Pts',(-5.28346748166331,0.23645870150246,32.7012187020024));
#44009=CARTESIAN_POINT('Ctrl Pts',(-4.75304319093522,-2.31937960938145,
32.7805905920557));
#44010=CARTESIAN_POINT('Ctrl Pts',(-3.06478809957792,-4.3102221812797,32.8599624821091));
#44011=CARTESIAN_POINT('Ctrl Pts',(-0.629957410956834,-5.25110417033318,
32.9393343721625));
#44012=CARTESIAN_POINT('Ctrl Pts',(1.95832950858626,-4.91282880661543,33.0187062622159));
#44013=CARTESIAN_POINT('Ctrl Pts',(4.06957169452659,-3.37779921996823,33.0980781522693));
#44014=CARTESIAN_POINT('Ctrl Pts',(4.96144058461863,-1.50005120370765,33.1612883464097));
#44015=CARTESIAN_POINT('Ctrl Pts',(5.07343602224469,-0.328346354394994,
33.1980412438656));
#44016=CARTESIAN_POINT('Ctrl Pts',(5.07324948390142,-8.1108973011175E-5,
33.208336844637));
#44017=CARTESIAN_POINT('Origin',(0.,0.,-2.20833684463713));
#44018=CARTESIAN_POINT('',(5.073704252564,-0.000125440355911652,31.2083368446371));
#44019=CARTESIAN_POINT('',(5.07346075270687,-0.000126888963244813,31.2916631553629));
#44020=CARTESIAN_POINT('',(5.0736,-1.85409460923845E-12,-2.20833684463713));
#44021=CARTESIAN_POINT('Ctrl Pts',(5.07346075270687,-0.000126888963244594,
31.2916631553629));
#44022=CARTESIAN_POINT('Ctrl Pts',(5.07289095298355,0.60348081698673,31.3105967649683));
#44023=CARTESIAN_POINT('Ctrl Pts',(4.81451756387892,2.05102782258644,31.3559876712581));
#44024=CARTESIAN_POINT('Ctrl Pts',(3.46819087602115,3.99281772621712,31.4278358742324));
#44025=CARTESIAN_POINT('Ctrl Pts',(1.13603804757386,5.16530336977167,31.5072077642858));
#44026=CARTESIAN_POINT('Ctrl Pts',(-1.47285113468488,5.07953254565492,31.5865796543392));
#44027=CARTESIAN_POINT('Ctrl Pts',(-3.72295704063504,3.75639883677117,31.6659515443926));
#44028=CARTESIAN_POINT('Ctrl Pts',(-5.06615885211213,1.51821468589782,31.745323434446));
#44029=CARTESIAN_POINT('Ctrl Pts',(-5.17525558096714,-1.08980320194903,
31.8246953244994));
#44030=CARTESIAN_POINT('Ctrl Pts',(-4.02367150553249,-3.43234744203962,
31.9040672145529));
#44031=CARTESIAN_POINT('Ctrl Pts',(-1.89192995759591,-4.93877944262154,
31.9834391046062));
#44032=CARTESIAN_POINT('Ctrl Pts',(0.70068154029511,-5.24213570278371,32.0628109946597));
#44033=CARTESIAN_POINT('Ctrl Pts',(3.12260856590247,-4.26851930901834,32.142182884713));
#44034=CARTESIAN_POINT('Ctrl Pts',(4.71924613978307,-2.33342987779042,32.2184669382808));
#44035=CARTESIAN_POINT('Ctrl Pts',(5.07325988110442,-0.74474986994901,32.2682936951641));
#44036=CARTESIAN_POINT('Ctrl Pts',(5.0738885135215,9.27415284240896E-5,
32.2916631553629));
#44037=CARTESIAN_POINT('Ctrl Pts',(5.073704252564,-0.000125440355911652,
31.2083368446371));
#44038=CARTESIAN_POINT('Ctrl Pts',(5.0730059773177,0.681887909050636,31.2297327901051));
#44039=CARTESIAN_POINT('Ctrl Pts',(4.76334894417968,2.20786416800771,31.2775860322575));
#44040=CARTESIAN_POINT('Ctrl Pts',(3.27920000412114,4.14943233229341,31.3518965710945));
#44041=CARTESIAN_POINT('Ctrl Pts',(0.895158610487983,5.21244975125701,31.4312684611478));
#44042=CARTESIAN_POINT('Ctrl Pts',(-1.70694143926006,5.00572594837619,31.5106403512013));
#44043=CARTESIAN_POINT('Ctrl Pts',(-3.89323433265515,3.57961838445739,31.5900122412546));
#44044=CARTESIAN_POINT('Ctrl Pts',(-5.13114396014345,1.28152370543563,31.6693841313081));
#44045=CARTESIAN_POINT('Ctrl Pts',(-5.11911827653528,-1.32874731162563,
31.7487560213615));
#44046=CARTESIAN_POINT('Ctrl Pts',(-3.86008671173927,-3.61533842470713,
31.8281279114149));
#44047=CARTESIAN_POINT('Ctrl Pts',(-1.6607465681206,-5.02124109994587,31.9074998014683));
#44048=CARTESIAN_POINT('Ctrl Pts',(0.943147763492109,-5.20398055756647,
31.9868716915216));
#44049=CARTESIAN_POINT('Ctrl Pts',(3.31729338754031,-4.11904187017945,32.0662435815751));
#44050=CARTESIAN_POINT('Ctrl Pts',(4.77384508508688,-2.17674249303873,32.1400652992802));
#44051=CARTESIAN_POINT('Ctrl Pts',(5.07296704505946,-0.666321171863868,
32.1874297203008));
#44052=CARTESIAN_POINT('Ctrl Pts',(5.07365497060222,0.000129255909635077,
32.208336844637));
#44053=CARTESIAN_POINT('Origin',(0.,0.,-2.20833684463713));
#44054=CARTESIAN_POINT('',(5.0732242396654,6.91156314036601E-5,30.208336844637));
#44055=CARTESIAN_POINT('',(5.07338983982448,0.000118254562807938,30.2916631553629));
#44056=CARTESIAN_POINT('',(5.0736,-1.85409460923845E-12,-2.20833684463713));
#44057=CARTESIAN_POINT('Ctrl Pts',(5.07338983982448,0.000118254562808118,
30.2916631553629));
#44058=CARTESIAN_POINT('Ctrl Pts',(5.07361825292341,0.265438860321299,30.2999852414035));
#44059=CARTESIAN_POINT('Ctrl Pts',(4.98815112489718,1.37411209267241,30.3347646241286));
#44060=CARTESIAN_POINT('Ctrl Pts',(4.19238095442003,3.22410968801099,30.3960013035382));
#44061=CARTESIAN_POINT('Ctrl Pts',(2.13968914249988,4.83659712202475,30.4753731935916));
#44062=CARTESIAN_POINT('Ctrl Pts',(-0.434226208411599,5.27090020273941,
30.554745083645));
#44063=CARTESIAN_POINT('Ctrl Pts',(-2.90236501609743,4.4212236610065,30.6341169736984));
#44064=CARTESIAN_POINT('Ctrl Pts',(-4.66349413013793,2.49454682166501,30.7134888637518));
#44065=CARTESIAN_POINT('Ctrl Pts',(-5.28860639654603,-0.0397961018483339,
30.7928607538052));
#44066=CARTESIAN_POINT('Ctrl Pts',(-4.62542585088724,-2.56444478303865,
30.8722326438586));
#44067=CARTESIAN_POINT('Ctrl Pts',(-2.83550180615875,-4.46440039138299,
30.951604533912));
#44068=CARTESIAN_POINT('Ctrl Pts',(-0.354855797726762,-5.27683794616905,
31.0309764239654));
#44069=CARTESIAN_POINT('Ctrl Pts',(2.21223229757146,-4.80384945735102,31.1103483140188));
#44070=CARTESIAN_POINT('Ctrl Pts',(4.24042550187443,-3.16065387386267,31.1897202040722));
#44071=CARTESIAN_POINT('Ctrl Pts',(4.99825410162456,-1.32316383571886,31.2501584845202));
#44072=CARTESIAN_POINT('Ctrl Pts',(5.07368717518548,-0.239983714616348,
31.2841394682838));
#44073=CARTESIAN_POINT('Ctrl Pts',(5.07346075270687,-0.000126888963244594,
31.2916631553629));
#44074=CARTESIAN_POINT('Ctrl Pts',(5.0732242396654,6.91156314035213E-5,
30.208336844637));
#44075=CARTESIAN_POINT('Ctrl Pts',(5.07338968774506,0.343924846945636,30.2191212665403));
#44076=CARTESIAN_POINT('Ctrl Pts',(4.95443916911164,1.53124494231641,30.256362985128));
#44077=CARTESIAN_POINT('Ctrl Pts',(4.0382761360698,3.41515258753676,30.3200620004003));
#44078=CARTESIAN_POINT('Ctrl Pts',(1.91297991407722,4.93066417388641,30.3994338904535));
#44079=CARTESIAN_POINT('Ctrl Pts',(-0.678313980675348,5.24507688131741,
30.4788057805071));
#44080=CARTESIAN_POINT('Ctrl Pts',(-3.10437209115798,4.28180047024023,30.5581776705604));
#44081=CARTESIAN_POINT('Ctrl Pts',(-4.77421203164559,2.2754869422171,30.6375495606138));
#44082=CARTESIAN_POINT('Ctrl Pts',(-5.28106448876339,-0.285130168225216,
30.7169214506672));
#44083=CARTESIAN_POINT('Ctrl Pts',(-4.50146132585641,-2.77629020081278,
30.7962933407206));
#44084=CARTESIAN_POINT('Ctrl Pts',(-2.62531214778642,-4.59115208569648,
30.8756652307741));
#44085=CARTESIAN_POINT('Ctrl Pts',(-0.109642741545517,-5.28761948484725,
30.9550371208274));
#44086=CARTESIAN_POINT('Ctrl Pts',(2.43273539384572,-4.69603448143646,31.0344090108809));
#44087=CARTESIAN_POINT('Ctrl Pts',(4.38250457206463,-2.96050587284378,31.1137809009342));
#44088=CARTESIAN_POINT('Ctrl Pts',(5.02689419953704,-1.16604718553494,31.1717568455196));
#44089=CARTESIAN_POINT('Ctrl Pts',(5.07386943415284,-0.161460170846308,
31.2032754934206));
#44090=CARTESIAN_POINT('Ctrl Pts',(5.073704252564,-0.000125440355911652,
31.2083368446371));
#44091=CARTESIAN_POINT('Origin',(0.,0.,-2.20833684463713));
#44092=CARTESIAN_POINT('',(5.07403430731529,5.85510781675173E-6,29.2083368446371));
#44093=CARTESIAN_POINT('',(5.07394886825829,-7.2464216758803E-5,29.2916631553629));
#44094=CARTESIAN_POINT('',(5.0736,-1.85409460923845E-12,-2.20833684463713));
#44095=CARTESIAN_POINT('Ctrl Pts',(5.07394886825829,-7.24642167588933E-5,
29.2916631553629));
#44096=CARTESIAN_POINT('Ctrl Pts',(5.07341208948874,0.770190548650157,29.3158310145232));
#44097=CARTESIAN_POINT('Ctrl Pts',(4.70060969038705,2.3841859592787,29.3664561703681));
#44098=CARTESIAN_POINT('Ctrl Pts',(3.05801844753361,4.31502775447088,29.4435386228973));
#44099=CARTESIAN_POINT('Ctrl Pts',(0.621713829942241,5.25208656259286,29.5229105129507));
#44100=CARTESIAN_POINT('Ctrl Pts',(-1.96603890048284,4.90974870936366,29.6022824030042));
#44101=CARTESIAN_POINT('Ctrl Pts',(-4.07486890650364,3.37140693807791,29.6816542930575));
#44102=CARTESIAN_POINT('Ctrl Pts',(-5.19106986646947,1.01179789915904,29.7610261831109));
#44103=CARTESIAN_POINT('Ctrl Pts',(-5.04273769720158,-1.59428286841832,
29.8403980731643));
#44104=CARTESIAN_POINT('Ctrl Pts',(-3.66600578680595,-3.81199985813419,
29.9197699632177));
#44105=CARTESIAN_POINT('Ctrl Pts',(-1.39624298131062,-5.10112212012718,
29.9991418532712));
#44106=CARTESIAN_POINT('Ctrl Pts',(1.21364152390063,-5.1476223247995,30.0785137433246));
#44107=CARTESIAN_POINT('Ctrl Pts',(3.52788564023963,-3.94017312521939,30.157885633378));
#44108=CARTESIAN_POINT('Ctrl Pts',(4.83020369710336,-2.00014283583164,30.2289354373907));
#44109=CARTESIAN_POINT('Ctrl Pts',(5.07289208966392,-0.578059506409542,
30.2735279447191));
#44110=CARTESIAN_POINT('Ctrl Pts',(5.07338983982448,0.000118254562808118,
30.2916631553629));
#44111=CARTESIAN_POINT('Ctrl Pts',(5.07403400238361,5.85099688312179E-6,
29.2083368446371));
#44112=CARTESIAN_POINT('Ctrl Pts',(5.07403437680669,0.00551609080175396,
29.2085097429756));
#44113=CARTESIAN_POINT('Ctrl Pts',(5.07268078911905,0.854215563279166,29.2351399379985));
#44114=CARTESIAN_POINT('Ctrl Pts',(4.6363228263275,2.54469094339263,29.2882274297059));
#44115=CARTESIAN_POINT('Ctrl Pts',(2.85451963682592,4.45226447892365,29.3675993197594));
#44116=CARTESIAN_POINT('Ctrl Pts',(0.377361782165573,5.2752762423091,29.4469712098127));
#44117=CARTESIAN_POINT('Ctrl Pts',(-2.19172056735417,4.81324238969394,29.5263430998662));
#44118=CARTESIAN_POINT('Ctrl Pts',(-4.22690463795758,3.17871334488069,29.6057149899195));
#44119=CARTESIAN_POINT('Ctrl Pts',(-5.23242409484928,0.769856765217166,
29.6850868799731));
#44120=CARTESIAN_POINT('Ctrl Pts',(-4.96333662400999,-1.82653521840426,
29.7644587700263));
#44121=CARTESIAN_POINT('Ctrl Pts',(-3.48519133772112,-3.97798726578954,
29.8438306600798));
#44122=CARTESIAN_POINT('Ctrl Pts',(-1.15806115590354,-5.16041042035391,
29.9232025501331));
#44123=CARTESIAN_POINT('Ctrl Pts',(1.45117016016719,-5.08576901889481,30.0025744401866));
#44124=CARTESIAN_POINT('Ctrl Pts',(3.70689963733188,-3.77224554159173,30.08194633024));
#44125=CARTESIAN_POINT('Ctrl Pts',(4.87583741971579,-1.84313681714053,30.1505337983901));
#44126=CARTESIAN_POINT('Ctrl Pts',(5.07298379589765,-0.499652414928338,
30.1926639698558));
#44127=CARTESIAN_POINT('Ctrl Pts',(5.0732242396654,6.91156314035213E-5,
30.208336844637));
#44128=CARTESIAN_POINT('Origin',(0.,0.,-2.20833684463713));
#44129=CARTESIAN_POINT('',(5.07324166632265,-7.76939179139569E-5,28.2083368446371));
#44130=CARTESIAN_POINT('',(5.07316594158954,-9.7399319174236E-6,28.2916631553629));
#44131=CARTESIAN_POINT('',(5.0736,-1.85409460923845E-12,-2.20833684463713));
#44132=CARTESIAN_POINT('Ctrl Pts',(5.0731664254358,-9.72907478691276E-6,
28.2916631553629));
#44133=CARTESIAN_POINT('Ctrl Pts',(5.07313755787372,0.432241135355033,28.3052194909585));
#44134=CARTESIAN_POINT('Ctrl Pts',(4.91180237168408,1.70811792520993,28.3452331232385));
#44135=CARTESIAN_POINT('Ctrl Pts',(3.85440685831077,3.62139325645763,28.4117040522031));
#44136=CARTESIAN_POINT('Ctrl Pts',(1.6528625396316,5.02384183393471,28.4910759422564));
#44137=CARTESIAN_POINT('Ctrl Pts',(-0.951315435152638,5.20249366075061,
28.5704478323099));
#44138=CARTESIAN_POINT('Ctrl Pts',(-3.32375507563475,4.11382954733206,28.6498197223633));
#44139=CARTESIAN_POINT('Ctrl Pts',(-4.8865353366993,2.02304566199065,28.7291916124167));
#44140=CARTESIAN_POINT('Ctrl Pts',(-5.25896640590637,-0.560547668676075,
28.8085635024701));
#44141=CARTESIAN_POINT('Ctrl Pts',(-4.35032489915935,-3.00759282800452,
28.8879353925235));
#44142=CARTESIAN_POINT('Ctrl Pts',(-2.38195387625792,-4.72199503162487,
28.9673072825769));
#44143=CARTESIAN_POINT('Ctrl Pts',(0.166655838534471,-5.28612969750008,
29.0466791726303));
#44144=CARTESIAN_POINT('Ctrl Pts',(2.67466855994625,-4.56257486971391,29.1260510626837));
#44145=CARTESIAN_POINT('Ctrl Pts',(4.53113794043359,-2.72758690275364,29.2054229527372));
#44146=CARTESIAN_POINT('Ctrl Pts',(5.05464511995301,-0.989211078787786,
29.2606269836302));
#44147=CARTESIAN_POINT('Ctrl Pts',(5.07399971767151,-0.0730399965665694,
29.2893737178388));
#44148=CARTESIAN_POINT('Ctrl Pts',(5.07394886825829,-7.24642167588933E-5,
29.2916631553629));
#44149=CARTESIAN_POINT('Ctrl Pts',(5.07324166632265,-7.76939179139916E-5,
28.2083368446371));
#44150=CARTESIAN_POINT('Ctrl Pts',(5.07296420662618,0.510664363139913,28.2243555160953));
#44151=CARTESIAN_POINT('Ctrl Pts',(4.86967684263928,1.86519135610718,28.266831484238));
#44152=CARTESIAN_POINT('Ctrl Pts',(3.68223314068176,3.79632723101881,28.3357647490651));
#44153=CARTESIAN_POINT('Ctrl Pts',(1.41798994671214,5.09511980804509,28.4151366391186));
#44154=CARTESIAN_POINT('Ctrl Pts',(-1.19167245960906,5.15275247768794,28.4945085291719));
#44155=CARTESIAN_POINT('Ctrl Pts',(-3.51104609249168,3.9551860491902,28.5738804192253));
#44156=CARTESIAN_POINT('Ctrl Pts',(-4.97513666881207,1.79414505376557,28.6532523092787));
#44157=CARTESIAN_POINT('Ctrl Pts',(-5.22729496488809,-0.803945705483672,
28.7326241993322));
#44158=CARTESIAN_POINT('Ctrl Pts',(-4.2060957779385,-3.20619707038074,28.8119960893855));
#44159=CARTESIAN_POINT('Ctrl Pts',(-2.16030096951815,-4.82742592572986,
28.891367979439));
#44160=CARTESIAN_POINT('Ctrl Pts',(0.41173837333167,-5.27270451089724,28.9707398694923));
#44161=CARTESIAN_POINT('Ctrl Pts',(2.88347915980534,-4.43356394814356,29.0501117595458));
#44162=CARTESIAN_POINT('Ctrl Pts',(4.64895661344711,-2.51859756056696,29.1293107512606));
#44163=CARTESIAN_POINT('Ctrl Pts',(5.07397708173548,-0.837673326665985,
29.1820524462911));
#44164=CARTESIAN_POINT('Ctrl Pts',(5.07403400238361,5.85099688312179E-6,
29.2083368446371));
#44165=CARTESIAN_POINT('Origin',(0.,0.,-2.20833684463713));
#44166=CARTESIAN_POINT('',(5.07366942975965,0.000128322057781627,27.2083368446371));
#44167=CARTESIAN_POINT('',(5.07390014538872,8.93747992460227E-5,27.2916631553629));
#44168=CARTESIAN_POINT('',(5.0736,-1.85409460923845E-12,-2.20833684463713));
#44169=CARTESIAN_POINT('Ctrl Pts',(5.07390014538872,8.93747992459192E-5,
27.2916631553629));
#44170=CARTESIAN_POINT('Ctrl Pts',(5.07397720165276,0.0939472090868575,
27.2946079673937));
#44171=CARTESIAN_POINT('Ctrl Pts',(5.04850897709501,1.03101725778952,27.324010076109));
#44172=CARTESIAN_POINT('Ctrl Pts',(4.49709775967288,2.7833528499375,27.3798694815089));
#44173=CARTESIAN_POINT('Ctrl Pts',(2.61810205366886,4.59526745509821,27.4592413715622));
#44174=CARTESIAN_POINT('Ctrl Pts',(0.101342482461748,5.28778507964899,27.5386132616156));
#44175=CARTESIAN_POINT('Ctrl Pts',(-2.44010389315526,4.69220996311103,27.617985151669));
#44176=CARTESIAN_POINT('Ctrl Pts',(-4.38714636147802,2.95362288558985,27.6973570417224));
#44177=CARTESIAN_POINT('Ctrl Pts',(-5.26548968692851,0.495539810872365,
27.7767289317758));
#44178=CARTESIAN_POINT('Ctrl Pts',(-4.86117137960698,-2.08325566491491,
27.8561008218293));
#44179=CARTESIAN_POINT('Ctrl Pts',(-3.27268248423349,-4.15457467193712,
27.9354727118826));
#44180=CARTESIAN_POINT('Ctrl Pts',(-0.886975379660524,-5.21384848487045,
28.0148446019361));
#44181=CARTESIAN_POINT('Ctrl Pts',(1.71479696411104,-5.00304034754724,28.0942164919895));
#44182=CARTESIAN_POINT('Ctrl Pts',(3.89884856306386,-3.57350265560346,28.1735883820429));
#44183=CARTESIAN_POINT('Ctrl Pts',(4.92233667869786,-1.66630250443567,28.2394039365007));
#44184=CARTESIAN_POINT('Ctrl Pts',(5.07319389740952,-0.411363633920409,
28.278762194274));
#44185=CARTESIAN_POINT('Ctrl Pts',(5.0731664254358,-9.72907478691276E-6,
28.2916631553629));
#44186=CARTESIAN_POINT('Ctrl Pts',(5.07366942975965,0.000128322057781714,
27.2083368446371));
#44187=CARTESIAN_POINT('Ctrl Pts',(5.07384715626772,0.172489015223486,27.2137439925305));
#44188=CARTESIAN_POINT('Ctrl Pts',(5.02310017357893,1.18811030837938,27.2456084371085));
#44189=CARTESIAN_POINT('Ctrl Pts',(4.36311469772634,2.98900844458398,27.3039301783709));
#44190=CARTESIAN_POINT('Ctrl Pts',(2.40207464524773,4.7117914582426,27.3833020684242));
#44191=CARTESIAN_POINT('Ctrl Pts',(-0.144105473911181,5.28679250204684,
27.4626739584777));
#44192=CARTESIAN_POINT('Ctrl Pts',(-2.65518181859737,4.57394259446923,27.542045848531));
#44193=CARTESIAN_POINT('Ctrl Pts',(-4.51946174941854,2.74689039512913,27.6214177385845));
#44194=CARTESIAN_POINT('Ctrl Pts',(-5.28281080174027,0.25070177567431,27.7007896286378));
#44195=CARTESIAN_POINT('Ctrl Pts',(-4.75927883606144,-2.30655724141581,
27.7801615186913));
#44196=CARTESIAN_POINT('Ctrl Pts',(-3.07639708040302,-4.30194401997489,
27.8595334087447));
#44197=CARTESIAN_POINT('Ctrl Pts',(-0.644111805447875,-5.24938675745965,
27.9389052987981));
#44198=CARTESIAN_POINT('Ctrl Pts',(1.94507767959709,-4.91809050014772,28.0182771888515));
#44199=CARTESIAN_POINT('Ctrl Pts',(4.06045054724861,-3.38875828300845,28.0976490789049));
#44200=CARTESIAN_POINT('Ctrl Pts',(4.95940796121397,-1.50917823199387,28.1610022975001));
#44201=CARTESIAN_POINT('Ctrl Pts',(5.07342247393797,-0.332904603741066,
28.1978982194108));
#44202=CARTESIAN_POINT('Ctrl Pts',(5.07324166632265,-7.76939179139916E-5,
28.2083368446371));
#44203=CARTESIAN_POINT('Origin',(0.,0.,-2.20833684463713));
#44204=CARTESIAN_POINT('',(5.07368988190431,-0.000126739092140837,26.2083368446371));
#44205=CARTESIAN_POINT('',(5.07344758812249,-0.000125648970980255,26.2916631553629));
#44206=CARTESIAN_POINT('',(5.0736,-1.85409460923845E-12,-2.20833684463713));
#44207=CARTESIAN_POINT('Ctrl Pts',(5.07344758812249,-0.000125648970980205,
26.2916631553629));
#44208=CARTESIAN_POINT('Ctrl Pts',(5.0728899391017,0.598926868258771,26.3104537405135));
#44209=CARTESIAN_POINT('Ctrl Pts',(4.81735989282913,2.0419133290656,26.3557016223485));
#44210=CARTESIAN_POINT('Ctrl Pts',(3.47894268615705,3.98345316700778,26.427406800868));
#44211=CARTESIAN_POINT('Ctrl Pts',(1.14995928876529,5.16222190355009,26.5067786909214));
#44212=CARTESIAN_POINT('Ctrl Pts',(-1.45915164597797,5.08348481077201,26.5861505809748));
#44213=CARTESIAN_POINT('Ctrl Pts',(-3.71281646953845,3.76642207019263,26.6655224710282));
#44214=CARTESIAN_POINT('Ctrl Pts',(-5.06204741929919,1.53186725014815,26.7448943610816));
#44215=CARTESIAN_POINT('Ctrl Pts',(-5.17817482237054,-1.07584704130177,
26.824266251135));
#44216=CARTESIAN_POINT('Ctrl Pts',(-4.032910300408,-3.42148737483758,26.9036381411884));
#44217=CARTESIAN_POINT('Ctrl Pts',(-1.90523775596165,-4.93366095719681,
26.9830100312419));
#44218=CARTESIAN_POINT('Ctrl Pts',(0.686546488664775,-5.24400565085624,
27.0623819212952));
#44219=CARTESIAN_POINT('Ctrl Pts',(3.11108952829732,-4.27692217537667,27.1417538113486));
#44220=CARTESIAN_POINT('Ctrl Pts',(4.71594148821095,-2.34252421969056,27.2181808893712));
#44221=CARTESIAN_POINT('Ctrl Pts',(5.07328489925194,-0.749306805737992,
27.2681506707093));
#44222=CARTESIAN_POINT('Ctrl Pts',(5.07390014538872,8.93747992459192E-5,
27.2916631553629));
#44223=CARTESIAN_POINT('Ctrl Pts',(5.07368988190431,-0.000126739092140768,
26.2083368446371));
#44224=CARTESIAN_POINT('Ctrl Pts',(5.07299367900981,0.677333119387493,26.2295897656503));
#44225=CARTESIAN_POINT('Ctrl Pts',(4.76643747661854,2.19875901809265,26.2772999833479));
#44226=CARTESIAN_POINT('Ctrl Pts',(3.29037472529985,4.14057671278022,26.35146749773));
#44227=CARTESIAN_POINT('Ctrl Pts',(0.909207831064193,5.21001751122215,26.4308393877834));
#44228=CARTESIAN_POINT('Ctrl Pts',(-1.69344007832135,5.01030957610855,26.5102112778369));
#44229=CARTESIAN_POINT('Ctrl Pts',(-3.88356973299385,3.59010131838702,26.5895831678902));
#44230=CARTESIAN_POINT('Ctrl Pts',(-5.12767039684481,1.29535232606086,26.6689550579437));
#44231=CARTESIAN_POINT('Ctrl Pts',(-5.12268190193029,-1.31494162567991,
26.748326947997));
#44232=CARTESIAN_POINT('Ctrl Pts',(-3.86981943456965,-3.604918707979,26.8276988380504));
#44233=CARTESIAN_POINT('Ctrl Pts',(-1.67427751864785,-5.01674557236666,
26.9070707281038));
#44234=CARTESIAN_POINT('Ctrl Pts',(0.929114694866165,-5.20650431970375,
26.9864426181573));
#44235=CARTESIAN_POINT('Ctrl Pts',(3.30617662527125,-4.12797013916282,27.0658145082107));
#44236=CARTESIAN_POINT('Ctrl Pts',(4.77079146294434,-2.18584915384965,27.1397792503706));
#44237=CARTESIAN_POINT('Ctrl Pts',(5.07297753645236,-0.6708757466937,27.1872866958461));
#44238=CARTESIAN_POINT('Ctrl Pts',(5.07366942975965,0.000128322057781714,
27.2083368446371));
#44239=CARTESIAN_POINT('Origin',(0.,0.,-2.20833684463713));
#44240=CARTESIAN_POINT('',(5.07323119136609,7.27167192501876E-5,25.2083368446371));
#44241=CARTESIAN_POINT('',(5.07340205215522,0.00012010210694157,25.2916631553629));
#44242=CARTESIAN_POINT('',(5.0736,-1.85409460923845E-12,-2.20833684463713));
#44243=CARTESIAN_POINT('Ctrl Pts',(5.07340205215522,0.000120102106941772,
25.2916631553629));
#44244=CARTESIAN_POINT('Ctrl Pts',(5.07363086957761,0.260879072720769,25.2998422169487));
#44245=CARTESIAN_POINT('Ctrl Pts',(4.98999058102238,1.36498517337352,25.334478575219));
#44246=CARTESIAN_POINT('Ctrl Pts',(4.20105773883081,3.21279554629917,25.3955722301737));
#44247=CARTESIAN_POINT('Ctrl Pts',(2.15272056265901,4.83081106300121,25.4749441202272));
#44248=CARTESIAN_POINT('Ctrl Pts',(-0.420014577610356,5.27205169757513,
25.5543160102805));
#44249=CARTESIAN_POINT('Ctrl Pts',(-2.89043509646038,4.42903220810823,25.6336879003339));
#44250=CARTESIAN_POINT('Ctrl Pts',(-4.65675202368223,2.50711027624266,25.7130597903873));
#44251=CARTESIAN_POINT('Ctrl Pts',(-5.28869446548081,-0.0255381695211706,
25.7924316804408));
#44252=CARTESIAN_POINT('Ctrl Pts',(-4.63232264181493,-2.55196557371741,
25.8718035704942));
#44253=CARTESIAN_POINT('Ctrl Pts',(-2.84752727607513,-4.45673981283608,
25.9511754605475));
#44254=CARTESIAN_POINT('Ctrl Pts',(-0.369080568778156,-5.27586209837409,
26.030547350601));
#44255=CARTESIAN_POINT('Ctrl Pts',(2.19927334812716,-4.80979605467087,26.1099192406543));
#44256=CARTESIAN_POINT('Ctrl Pts',(4.23188914543768,-3.17207433835284,26.1892911307078));
#44257=CARTESIAN_POINT('Ctrl Pts',(4.99647384522203,-1.33229055500106,26.2498724356106));
#44258=CARTESIAN_POINT('Ctrl Pts',(5.0736751134574,-0.244543947095586,26.283996443829));
#44259=CARTESIAN_POINT('Ctrl Pts',(5.07344758812249,-0.000125648970980205,
26.2916631553629));
#44260=CARTESIAN_POINT('Ctrl Pts',(5.07323119136609,7.2716719250257E-5,
25.2083368446371));
#44261=CARTESIAN_POINT('Ctrl Pts',(5.07340324942578,0.339366856221997,25.2189782420855));
#44262=CARTESIAN_POINT('Ctrl Pts',(4.95650365046512,1.52211798561692,25.2560769362184));
#44263=CARTESIAN_POINT('Ctrl Pts',(4.04746852150308,3.40425320955296,25.3196329270358));
#44264=CARTESIAN_POINT('Ctrl Pts',(1.92626575763449,4.92548896844514,25.3990048170892));
#44265=CARTESIAN_POINT('Ctrl Pts',(-0.664171081076968,5.24688651700902,
25.4783767071426));
#44266=CARTESIAN_POINT('Ctrl Pts',(-3.09281731455583,4.2901541238158,25.5577485971959));
#44267=CARTESIAN_POINT('Ctrl Pts',(-4.76806009604388,2.2883496821561,25.6371204872494));
#44268=CARTESIAN_POINT('Ctrl Pts',(-5.28181399205765,-0.2708916769007,25.7164923773028));
#44269=CARTESIAN_POINT('Ctrl Pts',(-4.50892969070311,-2.76414442307307,
25.7958642673562));
#44270=CARTESIAN_POINT('Ctrl Pts',(-2.63768009703987,-4.58405770611471,
25.8752361574096));
#44271=CARTESIAN_POINT('Ctrl Pts',(-0.123897470143628,-5.28730467858643,
25.9546080474629));
#44272=CARTESIAN_POINT('Ctrl Pts',(2.42006630623721,-4.70257593460492,26.0339799375165));
#44273=CARTESIAN_POINT('Ctrl Pts',(4.37450728714461,-2.97231010192892,26.1133518275698));
#44274=CARTESIAN_POINT('Ctrl Pts',(5.02533394688967,-1.17517261458846,26.17147079661));
#44275=CARTESIAN_POINT('Ctrl Pts',(5.07386036677103,-0.166021846101412,
26.2031324689658));
#44276=CARTESIAN_POINT('Ctrl Pts',(5.07368988190431,-0.000126739092140768,
26.2083368446371));
#44277=CARTESIAN_POINT('Origin',(0.,0.,-2.20833684463713));
#44278=CARTESIAN_POINT('',(5.07403460521456,1.01146903839872E-6,24.2083368446371));
#44279=CARTESIAN_POINT('',(5.07393893245752,-7.63518475177419E-5,24.2916631553629));
#44280=CARTESIAN_POINT('',(5.0736,-1.85409460923845E-12,-2.20833684463713));
#44281=CARTESIAN_POINT('Ctrl Pts',(5.07393893245752,-7.63518475176573E-5,
24.2916631553629));
#44282=CARTESIAN_POINT('Ctrl Pts',(5.0733825372435,0.765632623134578,24.3156879900684));
#44283=CARTESIAN_POINT('Ctrl Pts',(4.70398212533016,2.37509554318665,24.3661701214584));
#44284=CARTESIAN_POINT('Ctrl Pts',(3.0696404085172,4.30676782630642,24.4431095495329));
#44285=CARTESIAN_POINT('Ctrl Pts',(0.635870902865647,5.25039137038364,24.5224814395863));
#44286=CARTESIAN_POINT('Ctrl Pts',(-1.95279534724764,4.9150311981795,24.6018533296397));
#44287=CARTESIAN_POINT('Ctrl Pts',(-4.06576497321052,3.38238030533593,24.6812252196931));
#44288=CARTESIAN_POINT('Ctrl Pts',(-5.18832325111748,1.02578905688434,24.7605971097465));
#44289=CARTESIAN_POINT('Ctrl Pts',(-5.04701746921096,-1.58068213527875,
24.8399689997999));
#44290=CARTESIAN_POINT('Ctrl Pts',(-3.67626940318832,-3.80210265806849,
24.9193408898533));
#44291=CARTESIAN_POINT('Ctrl Pts',(-1.40999024783327,-5.09733938916421,
24.9987127799067));
#44292=CARTESIAN_POINT('Ctrl Pts',(1.19975941093347,-5.1508755278289,25.0780846699601));
#44293=CARTESIAN_POINT('Ctrl Pts',(3.51725033281924,-3.94966978918403,25.1574565600135));
#44294=CARTESIAN_POINT('Ctrl Pts',(4.82742597758186,-2.00925929492118,25.2286493884811));
#44295=CARTESIAN_POINT('Ctrl Pts',(5.07289070026022,-0.582613469337955,
25.2733849202643));
#44296=CARTESIAN_POINT('Ctrl Pts',(5.07340205215522,0.000120102106941772,
25.2916631553629));
#44297=CARTESIAN_POINT('Ctrl Pts',(5.07403455984306,1.01136344364921E-6,
24.2083368446371));
#44298=CARTESIAN_POINT('Ctrl Pts',(5.07403457120051,0.000953086505682821,
24.2083667185208));
#44299=CARTESIAN_POINT('Ctrl Pts',(5.07380195086792,0.845094303182403,24.2348538890889));
#44300=CARTESIAN_POINT('Ctrl Pts',(4.64316632240633,2.53218242822061,24.2877983563415));
#44301=CARTESIAN_POINT('Ctrl Pts',(2.86651231988729,4.4445526734691,24.3671702463949));
#44302=CARTESIAN_POINT('Ctrl Pts',(0.391582261162602,5.27423972531146,24.4465421364484));
#44303=CARTESIAN_POINT('Ctrl Pts',(-2.1787363696294,4.81913365439931,24.5259140265017));
#44304=CARTESIAN_POINT('Ctrl Pts',(-4.21831964333045,3.19009729224708,24.6052859165552));
#44305=CARTESIAN_POINT('Ctrl Pts',(-5.23032958900859,0.783960290863936,
24.6846578066085));
#44306=CARTESIAN_POINT('Ctrl Pts',(-4.9682428239423,-1.81314770210696,24.764029696662));
#44307=CARTESIAN_POINT('Ctrl Pts',(-3.49590310398264,-3.96857692817898,
24.8434015867153));
#44308=CARTESIAN_POINT('Ctrl Pts',(-1.17196912594307,-5.15726959884261,
24.9227734767688));
#44309=CARTESIAN_POINT('Ctrl Pts',(1.43745393706658,-5.08966281065081,25.0021453668222));
#44310=CARTESIAN_POINT('Ctrl Pts',(3.69671640275713,-3.78222542756197,25.0815172568756));
#44311=CARTESIAN_POINT('Ctrl Pts',(4.87329911188321,-1.85225894830422,25.1502477494805));
#44312=CARTESIAN_POINT('Ctrl Pts',(5.07297546809779,-0.504207096881882,
25.192520945401));
#44313=CARTESIAN_POINT('Ctrl Pts',(5.07323119136609,7.2716719250257E-5,
25.2083368446371));
#44314=CARTESIAN_POINT('Origin',(0.,0.,-2.20833684463713));
#44315=CARTESIAN_POINT('',(5.07323420419449,-7.41988534934401E-5,23.2083368446371));
#44316=CARTESIAN_POINT('',(5.07316553675605,-5.48786176412603E-6,23.2916631553629));
#44317=CARTESIAN_POINT('',(5.0736,-1.85409460923845E-12,-2.20833684463713));
#44318=CARTESIAN_POINT('Ctrl Pts',(5.07316569050492,-5.48591970746248E-6,
23.2916631553629));
#44319=CARTESIAN_POINT('Ctrl Pts',(5.07314958741115,0.42768514602335,23.3050764665037));
#44320=CARTESIAN_POINT('Ctrl Pts',(4.91412543793041,1.69899265595715,23.344947074329));
#44321=CARTESIAN_POINT('Ctrl Pts',(3.86415592530766,3.6109888303426,23.4112749788386));
#44322=CARTESIAN_POINT('Ctrl Pts',(1.66640053022393,5.01936755177924,23.4906468688921));
#44323=CARTESIAN_POINT('Ctrl Pts',(-0.937286345425383,5.20503944789203,
23.5700187589454));
#44324=CARTESIAN_POINT('Ctrl Pts',(-3.31265234202061,4.12277525560054,23.6493906489989));
#44325=CARTESIAN_POINT('Ctrl Pts',(-4.88106356050821,2.03621213668325,23.7287625390522));
#44326=CARTESIAN_POINT('Ctrl Pts',(-5.26045849971908,-0.546367751667005,
23.8081344291057));
#44327=CARTESIAN_POINT('Ctrl Pts',(-4.35841739221935,-2.99585366506712,
23.887506319159));
#44328=CARTESIAN_POINT('Ctrl Pts',(-2.3946754551717,-4.71555625687105,23.9668782092125));
#44329=CARTESIAN_POINT('Ctrl Pts',(0.152404122233421,-5.28655978220554,
24.0462500992659));
#44330=CARTESIAN_POINT('Ctrl Pts',(2.66235839280233,-4.56976904619763,24.1256219893193));
#44331=CARTESIAN_POINT('Ctrl Pts',(4.52376805191542,-2.73979268554746,24.2049938793727));
#44332=CARTESIAN_POINT('Ctrl Pts',(5.05332835032277,-0.998334355631039,
24.2603409347206));
#44333=CARTESIAN_POINT('Ctrl Pts',(5.07399526625627,-0.0776027111923523,
24.289230693384));
#44334=CARTESIAN_POINT('Ctrl Pts',(5.07393893245752,-7.63518475176573E-5,
24.2916631553629));
#44335=CARTESIAN_POINT('Ctrl Pts',(5.07323420419449,-7.41988534933707E-5,
23.2083368446371));
#44336=CARTESIAN_POINT('Ctrl Pts',(5.07297208311489,0.506109773689648,23.2242124916405));
#44337=CARTESIAN_POINT('Ctrl Pts',(4.87223466883649,1.85606959653113,23.2665454353283));
#44338=CARTESIAN_POINT('Ctrl Pts',(3.69245444696201,3.78638634033052,23.3353356757007));
#44339=CARTESIAN_POINT('Ctrl Pts',(1.43172095156667,5.09127847004479,23.4147075657541));
#44340=CARTESIAN_POINT('Ctrl Pts',(-1.17777659548102,5.1559464348325,23.4940794558075));
#44341=CARTESIAN_POINT('Ctrl Pts',(-3.50037037246962,3.96463726004727,23.5734513458609));
#44342=CARTESIAN_POINT('Ctrl Pts',(-4.97028167379665,1.80755122457705,23.6528232359143));
#44343=CARTESIAN_POINT('Ctrl Pts',(-5.22944336137752,-0.789850288405212,
23.7321951259677));
#44344=CARTESIAN_POINT('Ctrl Pts',(-4.21472422106041,-3.19484601935549,
23.8115670160211));
#44345=CARTESIAN_POINT('Ctrl Pts',(-2.17330758975551,-4.82158433170509,
23.8909389060745));
#44346=CARTESIAN_POINT('Ctrl Pts',(0.397521959947206,-5.27379537322471,
23.9703107961279));
#44347=CARTESIAN_POINT('Ctrl Pts',(2.87151604007067,-4.4413215351868,24.0496826861813));
#44348=CARTESIAN_POINT('Ctrl Pts',(4.64534728528402,-2.52767212981305,24.129024702351));
#44349=CARTESIAN_POINT('Ctrl Pts',(5.07402451266825,-0.842236060605585,
24.1819094218363));
#44350=CARTESIAN_POINT('Ctrl Pts',(5.07403455984306,1.01136344364921E-6,
24.2083368446371));
#44351=CARTESIAN_POINT('Origin',(0.,0.,-2.20833684463713));
#44352=CARTESIAN_POINT('',(5.07368445537635,0.000127432987209741,22.2083368446371));
#44353=CARTESIAN_POINT('',(5.0739114897015,8.59482686052055E-5,22.2916631553629));
#44354=CARTESIAN_POINT('',(5.0736,-1.85409460923845E-12,-2.20833684463713));
#44355=CARTESIAN_POINT('Ctrl Pts',(5.0739114897015,8.59482686050433E-5,
22.2916631553629));
#44356=CARTESIAN_POINT('Ctrl Pts',(5.07398263122595,0.0893847065795861,
22.2944649429389));
#44357=CARTESIAN_POINT('Ctrl Pts',(5.04987059102411,1.02189374093949,22.3237240271994));
#44358=CARTESIAN_POINT('Ctrl Pts',(4.50458503707303,2.77121862106756,22.3794404081444));
#44359=CARTESIAN_POINT('Ctrl Pts',(2.63048120009391,4.58819259887664,22.4588122981978));
#44360=CARTESIAN_POINT('Ctrl Pts',(0.115597647321455,5.28749259670008,22.5381841882512));
#44361=CARTESIAN_POINT('Ctrl Pts',(-2.42744506809483,4.69877132337436,22.6175560783046));
#44362=CARTESIAN_POINT('Ctrl Pts',(-4.37916762715256,2.96543963879382,22.696927968358));
#44363=CARTESIAN_POINT('Ctrl Pts',(-5.26413459813381,0.509733484286287,
22.7762998584114));
#44364=CARTESIAN_POINT('Ctrl Pts',(-4.86677005798463,-2.07014265165558,
22.8556717484648));
#44365=CARTESIAN_POINT('Ctrl Pts',(-3.28387109087741,-4.14573660239302,
22.9350436385182));
#44366=CARTESIAN_POINT('Ctrl Pts',(-0.901028401772815,-5.21143830245831,
23.0144155285717));
#44367=CARTESIAN_POINT('Ctrl Pts',(1.70130281532621,-5.00764516247504,23.093787418625));
#44368=CARTESIAN_POINT('Ctrl Pts',(3.88920043041414,-3.58400074773866,23.1731593086785));
#44369=CARTESIAN_POINT('Ctrl Pts',(4.92006185002291,-1.67542824897262,23.239117887591));
#44370=CARTESIAN_POINT('Ctrl Pts',(5.07318135021192,-0.415919972782139,
23.2786191698192));
#44371=CARTESIAN_POINT('Ctrl Pts',(5.07316569050492,-5.48591970746248E-6,
23.2916631553629));
#44372=CARTESIAN_POINT('Ctrl Pts',(5.07368445537635,0.000127432987209863,
22.2083368446371));
#44373=CARTESIAN_POINT('Ctrl Pts',(5.07385799503573,0.167927931732477,22.2136009680757));
#44374=CARTESIAN_POINT('Ctrl Pts',(5.02468445773871,1.17898674996513,22.2453223881989));
#44375=CARTESIAN_POINT('Ctrl Pts',(4.37115162329097,2.97723307464397,22.3035011050064));
#44376=CARTESIAN_POINT('Ctrl Pts',(2.4147715124657,4.70529942618521,22.3828729950599));
#44377=CARTESIAN_POINT('Ctrl Pts',(-0.129853572474074,5.28716128664959,
22.4622448851132));
#44378=CARTESIAN_POINT('Ctrl Pts',(-2.64284027062663,4.58108446095525,22.5416167751666));
#44379=CARTESIAN_POINT('Ctrl Pts',(-4.51204028846786,2.7590644882843,22.62098866522));
#44380=CARTESIAN_POINT('Ctrl Pts',(-5.28211549991429,0.264943102456049,
22.7003605552734));
#44381=CARTESIAN_POINT('Ctrl Pts',(-4.76548000969985,-2.2937181486802,22.7797324453269));
#44382=CARTESIAN_POINT('Ctrl Pts',(-3.08798363825926,-4.29363457062517,
22.8591043353802));
#44383=CARTESIAN_POINT('Ctrl Pts',(-0.658261551986295,-5.24763120247219,
22.9384762254337));
#44384=CARTESIAN_POINT('Ctrl Pts',(1.93181173129385,-4.92331644248731,23.017848115487));
#44385=CARTESIAN_POINT('Ctrl Pts',(4.05129987868926,-3.39969271923279,23.0972200055405));
#44386=CARTESIAN_POINT('Ctrl Pts',(4.95736217363157,-1.51830523331034,23.1607162485905));
#44387=CARTESIAN_POINT('Ctrl Pts',(5.07340891666056,-0.3374627456306,23.197755194956));
#44388=CARTESIAN_POINT('Ctrl Pts',(5.07323420419449,-7.41988534933707E-5,
23.2083368446371));
#44389=CARTESIAN_POINT('Origin',(0.,0.,-2.20833684463713));
#44390=CARTESIAN_POINT('',(5.0647135783285,-0.000493560823505712,21.2083368446371));
#44391=CARTESIAN_POINT('',(5.07311795825563,-0.000541267147824199,21.2916631553629));
#44392=CARTESIAN_POINT('',(5.0736,-1.85409460923845E-12,-2.20833684463713));
#44393=CARTESIAN_POINT('Ctrl Pts',(5.07311795825563,-0.000541267147824084,
21.2916631553629));
#44394=CARTESIAN_POINT('Ctrl Pts',(5.07265472641037,0.594063927299599,21.3103107160587));
#44395=CARTESIAN_POINT('Ctrl Pts',(4.82066183061084,2.03342224951305,21.3554155734389));
#44396=CARTESIAN_POINT('Ctrl Pts',(3.48937383888172,3.97367066688458,21.4269777275036));
#44397=CARTESIAN_POINT('Ctrl Pts',(1.16402860508423,5.15930893371516,21.5063496175569));
#44398=CARTESIAN_POINT('Ctrl Pts',(-1.44552439996815,5.08729102078623,21.5857215076104));
#44399=CARTESIAN_POINT('Ctrl Pts',(-3.70260503654192,3.77647571272897,21.6650933976637));
#44400=CARTESIAN_POINT('Ctrl Pts',(-5.057922432142,1.54547807796832,21.7444652877172));
#44401=CARTESIAN_POINT('Ctrl Pts',(-5.18104412158608,-1.06186685398839,
21.8238371777705));
#44402=CARTESIAN_POINT('Ctrl Pts',(-4.04212630117128,-3.41061102326193,
21.903209067824));
#44403=CARTESIAN_POINT('Ctrl Pts',(-1.91852825506946,-4.92850206746972,
21.9825809578774));
#44404=CARTESIAN_POINT('Ctrl Pts',(0.672404619068471,-5.245839892308,22.0619528479308));
#44405=CARTESIAN_POINT('Ctrl Pts',(3.09954884704109,-4.28529268150223,22.1413247379842));
#44406=CARTESIAN_POINT('Ctrl Pts',(4.71262161876037,-2.35161833566565,22.2178948404616));
#44407=CARTESIAN_POINT('Ctrl Pts',(5.07331084138903,-0.753863997357442,
22.2680076462545));
#44408=CARTESIAN_POINT('Ctrl Pts',(5.0739114897015,8.59482686050433E-5,
22.2916631553629));
#44409=CARTESIAN_POINT('Ctrl Pts',(5.0647135783285,-0.000493560823505643,
21.2083368446371));
#44410=CARTESIAN_POINT('Ctrl Pts',(5.06741194864459,0.674127865172368,21.2294467411954));
#44411=CARTESIAN_POINT('Ctrl Pts',(4.7845254230904,2.19368980981962,21.2770139344383));
#44412=CARTESIAN_POINT('Ctrl Pts',(3.29092685490723,4.12830747359771,21.3510384243656));
#44413=CARTESIAN_POINT('Ctrl Pts',(0.929079443196039,5.20946188754723,21.430410314419));
#44414=CARTESIAN_POINT('Ctrl Pts',(-1.68303999757346,5.01382783115869,21.5097822044724));
#44415=CARTESIAN_POINT('Ctrl Pts',(-3.8722246926078,3.60110493868854,21.5891540945258));
#44416=CARTESIAN_POINT('Ctrl Pts',(-5.12503498129818,1.30888173016128,21.6685259845792));
#44417=CARTESIAN_POINT('Ctrl Pts',(-5.12574462250326,-1.300972874894,21.7478978746326));
#44418=CARTESIAN_POINT('Ctrl Pts',(-3.87976959979778,-3.59455409188016,
21.827269764686));
#44419=CARTESIAN_POINT('Ctrl Pts',(-1.68766624540451,-5.01217052435348,
21.9066416547394));
#44420=CARTESIAN_POINT('Ctrl Pts',(0.915005995631755,-5.2090130440819,21.9860135447928));
#44421=CARTESIAN_POINT('Ctrl Pts',(3.29507231119182,-4.13685632854986,22.0653854348462));
#44422=CARTESIAN_POINT('Ctrl Pts',(4.76770779675958,-2.19496036885575,22.139493201461));
#44423=CARTESIAN_POINT('Ctrl Pts',(5.07298579089609,-0.675431391209716,
22.1871436713913));
#44424=CARTESIAN_POINT('Ctrl Pts',(5.07368445537635,0.000127432987209863,
22.2083368446371));
#44425=CARTESIAN_POINT('Origin',(0.,0.,-2.20833684463713));
#44426=CARTESIAN_POINT('',(5.07022284182504,-0.00437131830465176,20.2083368446371));
#44427=CARTESIAN_POINT('',(5.07763086250027,0.00422747191343611,20.2916631553629));
#44428=CARTESIAN_POINT('',(5.0736,-1.85409460923845E-12,-2.20833684463713));
#44429=CARTESIAN_POINT('Ctrl Pts',(5.07763086250027,0.00422747191343598,
20.2916631553629));
#44430=CARTESIAN_POINT('Ctrl Pts',(5.07981016603818,0.259793667372929,20.2996991924939));
#44431=CARTESIAN_POINT('Ctrl Pts',(4.94610737387947,2.19579442888697,20.3606498229938));
#44432=CARTESIAN_POINT('Ctrl Pts',(2.45559119020176,5.46873373673919,20.4745150468627));
#44433=CARTESIAN_POINT('Ctrl Pts',(-3.26379011618977,5.03400372054189,20.6332588269695));
#44434=CARTESIAN_POINT('Ctrl Pts',(-5.99600976813329,-0.0197068834827358,
20.7920026070763));
#44435=CARTESIAN_POINT('Ctrl Pts',(-3.70230252414087,-4.19446206534972,
20.9242890904987));
#44436=CARTESIAN_POINT('Ctrl Pts',(-0.376480053418488,-5.26605971579228,
21.0301182772365));
#44437=CARTESIAN_POINT('Ctrl Pts',(2.18257651229242,-4.8205851862161,21.10949016729));
#44438=CARTESIAN_POINT('Ctrl Pts',(4.22530652207796,-3.18086119603153,21.1888620573433));
#44439=CARTESIAN_POINT('Ctrl Pts',(4.99434160286696,-1.34186431057878,21.249586386701));
#44440=CARTESIAN_POINT('Ctrl Pts',(5.07331196316984,-0.249566309185764,
21.2838534193742));
#44441=CARTESIAN_POINT('Ctrl Pts',(5.07311795825563,-0.000541267147824084,
21.2916631553629));
#44442=CARTESIAN_POINT('Ctrl Pts',(5.07022284182504,-0.00437131830465176,
20.2083368446371));
#44443=CARTESIAN_POINT('Ctrl Pts',(5.06064558604025,1.17531423721709,20.2452925143152));
#44444=CARTESIAN_POINT('Ctrl Pts',(4.06283412548092,4.05874270439873,20.3351627773622));
#44445=CARTESIAN_POINT('Ctrl Pts',(-0.73672307947618,5.95134306184733,20.4779476337782));
#44446=CARTESIAN_POINT('Ctrl Pts',(-5.3995463563661,2.60828838171381,20.6366914138849));
#44447=CARTESIAN_POINT('Ctrl Pts',(-5.1196790448508,-3.11863163173554,20.7954351939918));
#44448=CARTESIAN_POINT('Ctrl Pts',(-0.158509478954971,-5.99736559883163,
20.9541789740985));
#44449=CARTESIAN_POINT('Ctrl Pts',(4.27441519030586,-3.72585141387614,21.091812857647));
#44450=CARTESIAN_POINT('Ctrl Pts',(5.06064814629056,-1.01689503187705,21.1765321478265));
#44451=CARTESIAN_POINT('Ctrl Pts',(5.0647135783285,-0.000493560823505643,
21.2083368446371));
#44452=CARTESIAN_POINT('Origin',(0.,0.,-2.20833684463713));
#44453=CARTESIAN_POINT('',(5.08190747034449,-0.0016131106486481,19.2083368446371));
#44454=CARTESIAN_POINT('',(5.0654395261759,0.00158764291868628,19.2916631553629));
#44455=CARTESIAN_POINT('',(5.0736,-1.85409460923845E-12,-2.20833684463713));
#44456=CARTESIAN_POINT('Ctrl Pts',(5.0654395261759,0.00158764291868674,
19.2916631553629));
#44457=CARTESIAN_POINT('Ctrl Pts',(5.06734596007678,0.765537039397172,19.3155449656136));
#44458=CARTESIAN_POINT('Ctrl Pts',(4.5467586954857,3.21970245674355,19.3923413692333));
#44459=CARTESIAN_POINT('Ctrl Pts',(0.736723079475925,5.95134306184737,19.5220523662219));
#44460=CARTESIAN_POINT('Ctrl Pts',(-4.59927593805429,3.84720861430001,19.6807961463287));
#44461=CARTESIAN_POINT('Ctrl Pts',(-5.72720375155086,-1.77677009197966,
19.8395399264355));
#44462=CARTESIAN_POINT('Ctrl Pts',(-1.61419617037545,-5.77483540889735,
19.9982837065423));
#44463=CARTESIAN_POINT('Ctrl Pts',(3.69280075007907,-4.55444079317796,20.1489914495181));
#44464=CARTESIAN_POINT('Ctrl Pts',(5.0654601874783,-1.42302350869954,20.246784599125));
#44465=CARTESIAN_POINT('Ctrl Pts',(5.07763086250027,0.00422747191343598,
20.2916631553629));
#44466=CARTESIAN_POINT('Ctrl Pts',(5.08190747034449,-0.00161311064864815,
19.2083368446371));
#44467=CARTESIAN_POINT('Ctrl Pts',(5.08137262398886,1.67206424053112,19.2611382874349));
#44468=CARTESIAN_POINT('Ctrl Pts',(3.25971341308398,5.0343135906333,19.3668543236016));
#44469=CARTESIAN_POINT('Ctrl Pts',(-2.45559119020206,5.46873373673905,19.5254849531373));
#44470=CARTESIAN_POINT('Ctrl Pts',(-5.92771323046149,0.905806267444168,
19.6842287332441));
#44471=CARTESIAN_POINT('Ctrl Pts',(-3.97578039972873,-4.48936692070992,
19.8429725133509));
#44472=CARTESIAN_POINT('Ctrl Pts',(1.61419617037569,-5.77483540889728,20.0017162934577));
#44473=CARTESIAN_POINT('Ctrl Pts',(4.76969253787625,-2.70752266133374,20.1235044038864));
#44474=CARTESIAN_POINT('Ctrl Pts',(5.0743586806711,-0.513806323102652,20.1923779209462));
#44475=CARTESIAN_POINT('Ctrl Pts',(5.07022284182504,-0.00437131830465176,
20.2083368446371));
#44476=CARTESIAN_POINT('Origin',(0.,0.,-2.20833684463713));
#44477=CARTESIAN_POINT('',(5.07322996641872,-7.44046081432859E-5,18.2083368446371));
#44478=CARTESIAN_POINT('',(5.0733324096026,-5.65345686568016E-5,18.2916631553629));
#44479=CARTESIAN_POINT('',(5.0736,-1.85409460923845E-12,-2.20833684463713));
#44480=CARTESIAN_POINT('Ctrl Pts',(5.0733324096026,-5.65345686565077E-5,
18.2916631553629));
#44481=CARTESIAN_POINT('Ctrl Pts',(5.07342932055268,0.423040487316443,18.3049334420489));
#44482=CARTESIAN_POINT('Ctrl Pts',(4.9168904884294,1.68971643561363,18.3446610254193));
#44483=CARTESIAN_POINT('Ctrl Pts',(3.87222469260764,3.60110493868871,18.4108459054742));
#44484=CARTESIAN_POINT('Ctrl Pts',(1.68303999757325,5.01382783115876,18.4902177955276));
#44485=CARTESIAN_POINT('Ctrl Pts',(-0.929079443196312,5.2094618875472,18.569589685581));
#44486=CARTESIAN_POINT('Ctrl Pts',(-3.29092685490746,4.12830747359753,18.6489615756344));
#44487=CARTESIAN_POINT('Ctrl Pts',(-5.42625155540715,1.36247937795741,18.7547907623723));
#44488=CARTESIAN_POINT('Ctrl Pts',(-4.95432466322409,-3.37745298000962,
18.8870772457946));
#44489=CARTESIAN_POINT('Ctrl Pts',(0.158509478955228,-5.99736559883162,
19.0458210259014));
#44490=CARTESIAN_POINT('Ctrl Pts',(4.3733083201864,-3.5517155504766,19.1806829957575));
#44491=CARTESIAN_POINT('Ctrl Pts',(5.06312190111345,-0.927134966817506,
19.2626303722447));
#44492=CARTESIAN_POINT('Ctrl Pts',(5.0654395261759,0.00158764291868674,
19.2916631553629));
#44493=CARTESIAN_POINT('Ctrl Pts',(5.07322996641872,-7.44046081432165E-5,
18.2083368446371));
#44494=CARTESIAN_POINT('Ctrl Pts',(5.07298661447134,0.501546775803683,18.2240694671857));
#44495=CARTESIAN_POINT('Ctrl Pts',(4.87479289587003,1.8469289142109,18.2662593864187));
#44496=CARTESIAN_POINT('Ctrl Pts',(3.70260503654169,3.77647571272922,18.3349066023362));
#44497=CARTESIAN_POINT('Ctrl Pts',(1.44552439996779,5.08729102078633,18.4142784923897));
#44498=CARTESIAN_POINT('Ctrl Pts',(-1.16402860508455,5.15930893371508,18.4936503824431));
#44499=CARTESIAN_POINT('Ctrl Pts',(-3.48937383888192,3.97367066688439,18.5730222724965));
#44500=CARTESIAN_POINT('Ctrl Pts',(-4.96594823061187,1.82167865277138,18.6523941625499));
#44501=CARTESIAN_POINT('Ctrl Pts',(-5.23050112077116,-0.77713504302674,
18.7317660526033));
#44502=CARTESIAN_POINT('Ctrl Pts',(-4.22530652207786,-3.18086119603167,
18.8111379426567));
#44503=CARTESIAN_POINT('Ctrl Pts',(-2.18257651229225,-4.82058518621618,
18.8905098327101));
#44504=CARTESIAN_POINT('Ctrl Pts',(0.37648005341871,-5.26605971579227,18.9698817227635));
#44505=CARTESIAN_POINT('Ctrl Pts',(3.70230252414111,-4.19446206534953,19.0757109095013));
#44506=CARTESIAN_POINT('Ctrl Pts',(5.08048878136776,-1.68603810060634,19.1551959501259));
#44507=CARTESIAN_POINT('Ctrl Pts',(5.08190861649065,-0.00519970863047212,
19.2082236940659));
#44508=CARTESIAN_POINT('Ctrl Pts',(5.08190747034449,-0.00161311064864815,
19.2083368446371));
#44509=CARTESIAN_POINT('Origin',(0.,0.,-2.20833684463713));
#44510=CARTESIAN_POINT('',(5.07369825422177,0.000126003717071388,17.2083368446371));
#44511=CARTESIAN_POINT('',(5.07392231800261,8.23068815517256E-5,17.2916631553629));
#44512=CARTESIAN_POINT('',(5.0736,-1.85409460923845E-12,-2.20833684463713));
#44513=CARTESIAN_POINT('Ctrl Pts',(5.07392231800261,8.23068815519051E-5,
17.2916631553629));
#44514=CARTESIAN_POINT('Ctrl Pts',(5.07398762507078,0.0848220371273371,
17.2943219184842));
#44515=CARTESIAN_POINT('Ctrl Pts',(5.05121938853888,1.01276996498335,17.3234379782898));
#44516=CARTESIAN_POINT('Ctrl Pts',(4.51204028846775,2.7590644882845,17.3790113347799));
#44517=CARTESIAN_POINT('Ctrl Pts',(2.64284027062647,4.58108446095533,17.4583832248334));
#44518=CARTESIAN_POINT('Ctrl Pts',(0.129853572473924,5.28716128664959,17.5377551148867));
#44519=CARTESIAN_POINT('Ctrl Pts',(-2.41477151246584,4.70529942618515,17.6171270049402));
#44520=CARTESIAN_POINT('Ctrl Pts',(-4.37115162329109,2.9772330746438,17.6964988949936));
#44521=CARTESIAN_POINT('Ctrl Pts',(-5.2627514922539,0.523926824466488,17.775870785047));
#44522=CARTESIAN_POINT('Ctrl Pts',(-4.87231403886184,-2.05702097999283,
17.8552426751004));
#44523=CARTESIAN_POINT('Ctrl Pts',(-3.29507231119166,-4.13685632854999,
17.9346145651538));
#44524=CARTESIAN_POINT('Ctrl Pts',(-0.915005995631555,-5.20901304408194,
18.0139864552072));
#44525=CARTESIAN_POINT('Ctrl Pts',(1.68766624540468,-5.01217052435341,18.0933583452606));
#44526=CARTESIAN_POINT('Ctrl Pts',(3.8797695997979,-3.59455409188004,18.172730235314));
#44527=CARTESIAN_POINT('Ctrl Pts',(4.9174284825737,-1.68443961943593,18.2388318386815));
#44528=CARTESIAN_POINT('Ctrl Pts',(5.07323610680991,-0.420498442869185,
18.2784761453644));
#44529=CARTESIAN_POINT('Ctrl Pts',(5.0733324096026,-5.65345686565077E-5,
18.2916631553629));
#44530=CARTESIAN_POINT('Ctrl Pts',(5.07369825422177,0.000126003717071926,
17.2083368446371));
#44531=CARTESIAN_POINT('Ctrl Pts',(5.07386566986272,0.163365799600409,17.2134579436209));
#44532=CARTESIAN_POINT('Ctrl Pts',(5.02624395147431,1.16985927909857,17.2450363392892));
#44533=CARTESIAN_POINT('Ctrl Pts',(4.37916762715237,2.96543963879408,17.303072031642));
#44534=CARTESIAN_POINT('Ctrl Pts',(2.42744506809458,4.69877132337447,17.3824439216954));
#44535=CARTESIAN_POINT('Ctrl Pts',(-0.115597647321682,5.28749259670007,
17.4618158117488));
#44536=CARTESIAN_POINT('Ctrl Pts',(-2.63048120009413,4.58819259887652,17.5411877018022));
#44537=CARTESIAN_POINT('Ctrl Pts',(-4.5045850370732,2.7712186210673,17.6205595918556));
#44538=CARTESIAN_POINT('Ctrl Pts',(-5.28138253005218,0.27918271172893,17.699931481909));
#44539=CARTESIAN_POINT('Ctrl Pts',(-4.77164579536179,-2.28086298099153,
17.7793033719624));
#44540=CARTESIAN_POINT('Ctrl Pts',(-3.09954884704088,-4.28529268150238,
17.8586752620158));
#44541=CARTESIAN_POINT('Ctrl Pts',(-0.672404619068171,-5.24583989230806,
17.9380471520692));
#44542=CARTESIAN_POINT('Ctrl Pts',(1.91852825506979,-4.9285020674696,18.0174190421226));
#44543=CARTESIAN_POINT('Ctrl Pts',(4.04212630117149,-3.41061102326166,18.096790932176));
#44544=CARTESIAN_POINT('Ctrl Pts',(4.95529462550652,-1.52742091164643,18.1604301996809));
#44545=CARTESIAN_POINT('Ctrl Pts',(5.07339585550224,-0.342021443822988,
18.1976121705012));
#44546=CARTESIAN_POINT('Ctrl Pts',(5.07322996641872,-7.44046081432165E-5,
18.2083368446371));
#44547=CARTESIAN_POINT('Origin',(0.,0.,-2.20833684463713));
#44548=CARTESIAN_POINT('',(5.07366101292862,-0.000128884195875409,16.2083368446371));
#44549=CARTESIAN_POINT('',(5.07342183474754,-0.000122761774360241,16.2916631553629));
#44550=CARTESIAN_POINT('',(5.0736,-1.85409460923845E-12,-2.20833684463713));
#44551=CARTESIAN_POINT('Ctrl Pts',(5.07342183474754,-0.000122761774360089,
16.2916631553629));
#44552=CARTESIAN_POINT('Ctrl Pts',(5.07288953552851,0.589818979702204,16.3101676916039));
#44553=CARTESIAN_POINT('Ctrl Pts',(4.82300217163475,2.02368301235074,16.3551295245292));
#44554=CARTESIAN_POINT('Ctrl Pts',(3.50037037246945,3.9646372600474,16.4265486541391));
#44555=CARTESIAN_POINT('Ctrl Pts',(1.17777659548083,5.15594643483254,16.5059205441925));
#44556=CARTESIAN_POINT('Ctrl Pts',(-1.43172095156687,5.09127847004474,16.5852924342459));
#44557=CARTESIAN_POINT('Ctrl Pts',(-3.69245444696213,3.78638634033038,16.6646643242993));
#44558=CARTESIAN_POINT('Ctrl Pts',(-5.05371420635461,1.5591388772047,16.7440362143527));
#44559=CARTESIAN_POINT('Ctrl Pts',(-5.18390038229795,-1.04791136166686,
16.8234081044061));
#44560=CARTESIAN_POINT('Ctrl Pts',(-4.05129987868913,-3.39969271923294,
16.9027799944595));
#44561=CARTESIAN_POINT('Ctrl Pts',(-1.93181173129365,-4.9233164424874,16.9821518845129));
#44562=CARTESIAN_POINT('Ctrl Pts',(0.658261551986501,-5.24763120247215,
17.0615237745663));
#44563=CARTESIAN_POINT('Ctrl Pts',(3.08798363825942,-4.29363457062506,17.1408956646198));
#44564=CARTESIAN_POINT('Ctrl Pts',(4.70928800664519,-2.36071043051411,17.2176087915519));
#44565=CARTESIAN_POINT('Ctrl Pts',(5.0733377557896,-0.758421261304332,17.2678646217997));
#44566=CARTESIAN_POINT('Ctrl Pts',(5.07392231800261,8.23068815519051E-5,
17.2916631553629));
#44567=CARTESIAN_POINT('Ctrl Pts',(5.07366101292862,-0.000128884195875374,
16.2083368446371));
#44568=CARTESIAN_POINT('Ctrl Pts',(5.07297133880781,0.668223813333716,16.2293037167406));
#44569=CARTESIAN_POINT('Ctrl Pts',(4.77257120255655,2.18054683036438,16.2767278855287));
#44570=CARTESIAN_POINT('Ctrl Pts',(3.31265234202039,4.12277525560071,16.3506093510011));
#44571=CARTESIAN_POINT('Ctrl Pts',(0.937286345425132,5.20503944789207,16.4299812410546));
#44572=CARTESIAN_POINT('Ctrl Pts',(-1.66640053022416,5.01936755177917,16.509353131108));
#44573=CARTESIAN_POINT('Ctrl Pts',(-3.86415592530783,3.6109888303424,16.5887250211614));
#44574=CARTESIAN_POINT('Ctrl Pts',(-5.12061148999576,1.32298122241861,16.6680969112148));
#44575=CARTESIAN_POINT('Ctrl Pts',(-5.1296974302943,-1.28730168253218,16.7474688012682));
#44576=CARTESIAN_POINT('Ctrl Pts',(-3.88920043041393,-3.58400074773889,
16.8268406913216));
#44577=CARTESIAN_POINT('Ctrl Pts',(-1.70130281532588,-5.00764516247516,
16.906212581375));
#44578=CARTESIAN_POINT('Ctrl Pts',(0.90102840177319,-5.21143830245825,16.9855844714284));
#44579=CARTESIAN_POINT('Ctrl Pts',(3.28387109087768,-4.1457366023928,17.0649563614818));
#44580=CARTESIAN_POINT('Ctrl Pts',(4.76464092528408,-2.20406061763576,17.1392071525514));
#44581=CARTESIAN_POINT('Ctrl Pts',(5.07300074510805,-0.679985153784537,
17.1870006469365));
#44582=CARTESIAN_POINT('Ctrl Pts',(5.07369825422177,0.000126003717071926,
17.2083368446371));
#44583=CARTESIAN_POINT('Origin',(0.,0.,-2.20833684463713));
#44584=CARTESIAN_POINT('',(5.07324617544329,7.96922658102828E-5,15.2083368446371));
#44585=CARTESIAN_POINT('',(5.07342714732068,0.00012340910666319,15.2916631553629));
#44586=CARTESIAN_POINT('',(5.0736,-1.85409460923845E-12,-2.20833684463713));
#44587=CARTESIAN_POINT('Ctrl Pts',(5.07342714732068,0.000123409106663336,
15.2916631553629));
#44588=CARTESIAN_POINT('Ctrl Pts',(5.07365576358557,0.251759202071401,15.2995561680391));
#44589=CARTESIAN_POINT('Ctrl Pts',(4.99363067660841,1.34673145111339,15.3339064773998));
#44590=CARTESIAN_POINT('Ctrl Pts',(4.21831964333036,3.19009729224721,15.3947140834449));
#44591=CARTESIAN_POINT('Ctrl Pts',(2.17873636962922,4.81913365439941,15.4740859734983));
#44592=CARTESIAN_POINT('Ctrl Pts',(-0.391582261162836,5.27423972531144,
15.5534578635517));
#44593=CARTESIAN_POINT('Ctrl Pts',(-2.86651231988745,4.44455267346898,15.6328297536051));
#44594=CARTESIAN_POINT('Ctrl Pts',(-4.64316632240643,2.53218242822043,15.7122016436585));
#44595=CARTESIAN_POINT('Ctrl Pts',(-5.28875528625864,0.00297814834715876,
15.7915735337119));
#44596=CARTESIAN_POINT('Ctrl Pts',(-4.64601516884489,-2.52695160186966,
15.8709454237653));
#44597=CARTESIAN_POINT('Ctrl Pts',(-2.87151604007055,-4.44132153518687,
15.9503173138187));
#44598=CARTESIAN_POINT('Ctrl Pts',(-0.397521959947054,-5.27379537322474,
16.0296892038721));
#44599=CARTESIAN_POINT('Ctrl Pts',(2.1733075897557,-4.82158433170501,16.1090610939255));
#44600=CARTESIAN_POINT('Ctrl Pts',(4.21472422106055,-3.1948460193553,16.1884329839789));
#44601=CARTESIAN_POINT('Ctrl Pts',(4.99287463290549,-1.35054413899492,16.2493003377914));
#44602=CARTESIAN_POINT('Ctrl Pts',(5.07365060287866,-0.253664125066255,
16.2837103949194));
#44603=CARTESIAN_POINT('Ctrl Pts',(5.07342183474754,-0.000122761774360089,
16.2916631553629));
#44604=CARTESIAN_POINT('Ctrl Pts',(5.07324617544329,7.96922658102828E-5,
15.2083368446371));
#44605=CARTESIAN_POINT('Ctrl Pts',(5.07343036424897,0.330250553788653,15.2186921931759));
#44606=CARTESIAN_POINT('Ctrl Pts',(4.96059306642381,1.5038639780885,15.2555048383992));
#44607=CARTESIAN_POINT('Ctrl Pts',(4.06576497321036,3.38238030533612,15.3187747803069));
#44608=CARTESIAN_POINT('Ctrl Pts',(1.95279534724736,4.91503119817963,15.3981466703603));
#44609=CARTESIAN_POINT('Ctrl Pts',(-0.635870902865948,5.2503913703836,15.4775185604137));
#44610=CARTESIAN_POINT('Ctrl Pts',(-3.06964040851742,4.30676782630626,15.5568904504671));
#44611=CARTESIAN_POINT('Ctrl Pts',(-4.75565230518791,2.31402517260967,15.6362623405205));
#44612=CARTESIAN_POINT('Ctrl Pts',(-5.28319782677237,-0.24240889112691,
15.7156342305739));
#44613=CARTESIAN_POINT('Ctrl Pts',(-4.52376805191524,-2.73979268554778,
15.7950061206273));
#44614=CARTESIAN_POINT('Ctrl Pts',(-2.66235839280204,-4.56976904619777,
15.8743780106807));
#44615=CARTESIAN_POINT('Ctrl Pts',(-0.15240412223312,-5.28655978220556,
15.9537499007341));
#44616=CARTESIAN_POINT('Ctrl Pts',(2.39467545517194,-4.71555625687092,16.0331217907875));
#44617=CARTESIAN_POINT('Ctrl Pts',(4.35841739221953,-2.99585366506689,16.112493680841));
#44618=CARTESIAN_POINT('Ctrl Pts',(5.02217539318898,-1.19342375387563,16.1708986987908));
#44619=CARTESIAN_POINT('Ctrl Pts',(5.0738416122916,-0.175144979162809,16.2028464200562));
#44620=CARTESIAN_POINT('Ctrl Pts',(5.07366101292862,-0.000128884195875374,
16.2083368446371));
#44621=CARTESIAN_POINT('Origin',(0.,0.,-2.20833684463713));
#44622=CARTESIAN_POINT('',(5.07403332299931,-8.66482790312043E-6,14.2083368446371));
#44623=CARTESIAN_POINT('',(5.07391786048903,-8.38031740753252E-5,14.2916631553629));
#44624=CARTESIAN_POINT('',(5.0736,-1.85409460923845E-12,-2.20833684463713));
#44625=CARTESIAN_POINT('Ctrl Pts',(5.07391786048903,-8.38031740754523E-5,
14.2916631553629));
#44626=CARTESIAN_POINT('Ctrl Pts',(5.07332646114364,0.756517455027875,14.3154019411588));
#44627=CARTESIAN_POINT('Ctrl Pts',(4.7106825315255,2.35691208085668,14.3655980236392));
#44628=CARTESIAN_POINT('Ctrl Pts',(3.09281731455568,4.29015412381589,14.442251402804));
#44629=CARTESIAN_POINT('Ctrl Pts',(0.664171081076821,5.24688651700904,14.5216232928574));
#44630=CARTESIAN_POINT('Ctrl Pts',(-1.92626575763464,4.9254889684451,14.6009951829108));
#44631=CARTESIAN_POINT('Ctrl Pts',(-4.04746852150321,3.4042532095528,14.6803670729642));
#44632=CARTESIAN_POINT('Ctrl Pts',(-5.1827169124532,1.05374890400015,14.7597389630177));
#44633=CARTESIAN_POINT('Ctrl Pts',(-5.05546693527891,-1.55344630213332,
14.839110853071));
#44634=CARTESIAN_POINT('Ctrl Pts',(-3.69671640275692,-3.78222542756219,
14.9184827431245));
#44635=CARTESIAN_POINT('Ctrl Pts',(-1.43745393706629,-5.08966281065088,
14.9978546331779));
#44636=CARTESIAN_POINT('Ctrl Pts',(1.17196912594334,-5.15726959884254,15.0772265232312));
#44637=CARTESIAN_POINT('Ctrl Pts',(3.49590310398282,-3.96857692817882,15.1565984132847));
#44638=CARTESIAN_POINT('Ctrl Pts',(4.82182831793198,-2.02749096887971,15.2280772906619));
#44639=CARTESIAN_POINT('Ctrl Pts',(5.07288944423512,-0.591721367900843,
15.2730988713546));
#44640=CARTESIAN_POINT('Ctrl Pts',(5.07342714732068,0.000123409106663336,
15.2916631553629));
#44641=CARTESIAN_POINT('Ctrl Pts',(5.07403332299931,-8.66482790325162E-6,
14.2083368446371));
#44642=CARTESIAN_POINT('Ctrl Pts',(5.07395003551347,0.835016825572543,14.2345379662956));
#44643=CARTESIAN_POINT('Ctrl Pts',(4.65105118571099,2.51331333377907,14.2871963846386));
#44644=CARTESIAN_POINT('Ctrl Pts',(2.89043509646017,4.42903220810837,14.3663120996661));
#44645=CARTESIAN_POINT('Ctrl Pts',(0.420014577610126,5.27205169757513,14.4456839897195));
#44646=CARTESIAN_POINT('Ctrl Pts',(-2.15272056265924,4.83081106300113,14.5250558797729));
#44647=CARTESIAN_POINT('Ctrl Pts',(-4.201057738831,3.21279554629894,14.6044277698263));
#44648=CARTESIAN_POINT('Ctrl Pts',(-5.22602654870706,0.81215014592063,14.6837996598797));
#44649=CARTESIAN_POINT('Ctrl Pts',(-4.97794685893165,-1.78633323234006,
14.7631715499331));
#44650=CARTESIAN_POINT('Ctrl Pts',(-3.51725033281897,-3.94966978918425,
14.8425434399865));
#44651=CARTESIAN_POINT('Ctrl Pts',(-1.19975941093315,-5.15087552782897,
14.9219153300399));
#44652=CARTESIAN_POINT('Ctrl Pts',(1.40999024783357,-5.09733938916413,15.0012872200933));
#44653=CARTESIAN_POINT('Ctrl Pts',(3.67626940318851,-3.8021026580683,15.0806591101467));
#44654=CARTESIAN_POINT('Ctrl Pts',(4.86818118380815,-1.87050241988135,15.1496756516613));
#44655=CARTESIAN_POINT('Ctrl Pts',(5.07295977285751,-0.513316266501481,
15.1922348964914));
#44656=CARTESIAN_POINT('Ctrl Pts',(5.07324617544329,7.96922658102828E-5,
15.2083368446371));
#44657=CARTESIAN_POINT('Origin',(0.,0.,-2.20833684463713));
#44658=CARTESIAN_POINT('',(5.07322036085286,-6.69861637152269E-5,13.2083368446371));
#44659=CARTESIAN_POINT('',(5.07316540514723,3.01288341894208E-6,13.2916631553629));
#44660=CARTESIAN_POINT('',(5.0736,-1.85409460923845E-12,-2.20833684463713));
#44661=CARTESIAN_POINT('Ctrl Pts',(5.07316545149283,3.01256212205392E-6,
13.2916631553629));
#44662=CARTESIAN_POINT('Ctrl Pts',(5.07317410528241,0.418572877762161,13.3047904175941));
#44663=CARTESIAN_POINT('Ctrl Pts',(4.91873112752187,1.68074170142874,13.3443749765097));
#44664=CARTESIAN_POINT('Ctrl Pts',(3.8835697329937,3.59010131838716,13.4104168321098));
#44665=CARTESIAN_POINT('Ctrl Pts',(1.69344007832116,5.01030957610862,13.4897887221632));
#44666=CARTESIAN_POINT('Ctrl Pts',(-0.909207831064397,5.21001751122212,
13.5691606122166));
#44667=CARTESIAN_POINT('Ctrl Pts',(-3.29037472530003,4.14057671278008,13.64853250227));
#44668=CARTESIAN_POINT('Ctrl Pts',(-4.87001361957351,2.06250059211591,13.7279043923234));
#44669=CARTESIAN_POINT('Ctrl Pts',(-5.26332797571119,-0.517996107520081,
13.8072762823768));
#44670=CARTESIAN_POINT('Ctrl Pts',(-4.37450728714447,-2.97231010192914,
13.8866481724302));
#44671=CARTESIAN_POINT('Ctrl Pts',(-2.420066306237,-4.70257593460501,13.9660200624836));
#44672=CARTESIAN_POINT('Ctrl Pts',(0.123897470143854,-5.28730467858643,
14.045391952537));
#44673=CARTESIAN_POINT('Ctrl Pts',(2.63768009704007,-4.58405770611459,14.1247638425904));
#44674=CARTESIAN_POINT('Ctrl Pts',(4.50892969070322,-2.76414442307289,14.2041357326438));
#44675=CARTESIAN_POINT('Ctrl Pts',(5.05065740926092,-1.01658127603429,14.2597688369013));
#44676=CARTESIAN_POINT('Ctrl Pts',(5.07398558617533,-0.0867280307438605,
14.2889446444744));
#44677=CARTESIAN_POINT('Ctrl Pts',(5.07391786048903,-8.38031740754523E-5,
14.2916631553629));
#44678=CARTESIAN_POINT('Ctrl Pts',(5.07322036085286,-6.69861637153657E-5,
13.2083368446371));
#44679=CARTESIAN_POINT('Ctrl Pts',(5.07298878663719,0.497000397927876,13.2239264427309));
#44680=CARTESIAN_POINT('Ctrl Pts',(4.87730902789417,1.83782529464356,13.2659733375091));
#44681=CARTESIAN_POINT('Ctrl Pts',(3.71281646953824,3.76642207019282,13.3344775289718));
#44682=CARTESIAN_POINT('Ctrl Pts',(1.45915164597774,5.08348481077208,13.4138494190252));
#44683=CARTESIAN_POINT('Ctrl Pts',(-1.14995928876559,5.16222190355004,13.4932213090786));
#44684=CARTESIAN_POINT('Ctrl Pts',(-3.47894268615732,3.98345316700755,13.572593199132));
#44685=CARTESIAN_POINT('Ctrl Pts',(-4.96046334571011,1.83432405620607,13.6519650891854));
#44686=CARTESIAN_POINT('Ctrl Pts',(-5.23362611404733,-0.761642334479749,
13.7313369792388));
#44687=CARTESIAN_POINT('Ctrl Pts',(-4.23188914543755,-3.17207433835303,
13.8107088692922));
#44688=CARTESIAN_POINT('Ctrl Pts',(-2.19927334812693,-4.80979605467098,
13.8900807593456));
#44689=CARTESIAN_POINT('Ctrl Pts',(0.369080568778457,-5.27586209837409,
13.9694526493991));
#44690=CARTESIAN_POINT('Ctrl Pts',(2.84752727607539,-4.45673981283591,14.0488245394524));
#44691=CARTESIAN_POINT('Ctrl Pts',(4.63232264181505,-2.55196557371717,14.1281964295059));
#44692=CARTESIAN_POINT('Ctrl Pts',(5.07202231626624,-0.859526521495883,
14.1813671979007));
#44693=CARTESIAN_POINT('Ctrl Pts',(5.07403413732223,-0.00817292128436273,
14.2080806696111));
#44694=CARTESIAN_POINT('Ctrl Pts',(5.07403332299931,-8.66482790325162E-6,
14.2083368446371));
#44695=CARTESIAN_POINT('Origin',(0.,0.,-2.20833684463713));
#44696=CARTESIAN_POINT('',(5.07371259150425,0.000124614973235349,12.2083368446371));
#44697=CARTESIAN_POINT('',(5.07393295843892,7.85666071205126E-5,12.2916631553629));
#44698=CARTESIAN_POINT('',(5.0736,-1.85409460923845E-12,-2.20833684463713));
#44699=CARTESIAN_POINT('Ctrl Pts',(5.07393295843892,7.85666071204203E-5,
12.2916631553629));
#44700=CARTESIAN_POINT('Ctrl Pts',(5.07399255467328,0.080259357669063,12.2941788940293));
#44701=CARTESIAN_POINT('Ctrl Pts',(5.0525559141232,1.00364648464526,12.3231519293802));
#44702=CARTESIAN_POINT('Ctrl Pts',(4.51946174941847,2.74689039512926,12.3785822614155));
#44703=CARTESIAN_POINT('Ctrl Pts',(2.6551818185972,4.57394259446934,12.4579541514689));
#44704=CARTESIAN_POINT('Ctrl Pts',(0.144105473910954,5.28679250204684,12.5373260415223));
#44705=CARTESIAN_POINT('Ctrl Pts',(-2.40207464524796,4.7117914582425,12.6166979315757));
#44706=CARTESIAN_POINT('Ctrl Pts',(-4.36311469772651,2.98900844458373,12.6960698216291));
#44707=CARTESIAN_POINT('Ctrl Pts',(-5.26130966742946,0.538109589882336,
12.7754417116825));
#44708=CARTESIAN_POINT('Ctrl Pts',(-4.87786124785798,-2.043871569829,12.854813601736));
#44709=CARTESIAN_POINT('Ctrl Pts',(-3.30617662527107,-4.12797013916298,
12.9341854917893));
#44710=CARTESIAN_POINT('Ctrl Pts',(-0.929114694865931,-5.20650431970379,
13.0135573818428));
#44711=CARTESIAN_POINT('Ctrl Pts',(1.67427751864803,-5.01674557236658,13.0929292718962));
#44712=CARTESIAN_POINT('Ctrl Pts',(3.86981943456978,-3.60491870797887,13.1723011619496));
#44713=CARTESIAN_POINT('Ctrl Pts',(4.91547184132152,-1.69367935817457,13.2385457897718));
#44714=CARTESIAN_POINT('Ctrl Pts',(5.07315666403118,-0.425032354751582,
13.2783331209096));
#44715=CARTESIAN_POINT('Ctrl Pts',(5.07316545149283,3.01256212205392E-6,
13.2916631553629));
#44716=CARTESIAN_POINT('Ctrl Pts',(5.07371259150425,0.000124614973235296,
12.2083368446371));
#44717=CARTESIAN_POINT('Ctrl Pts',(5.07387461653381,0.158804080659856,12.2133149191661));
#44718=CARTESIAN_POINT('Ctrl Pts',(5.02779682862049,1.1607339041827,12.2447502903796));
#44719=CARTESIAN_POINT('Ctrl Pts',(4.38714636147788,2.95362288559007,12.3026429582776));
#44720=CARTESIAN_POINT('Ctrl Pts',(2.44010389315499,4.69220996311119,12.382014848331));
#44721=CARTESIAN_POINT('Ctrl Pts',(-0.101342482462103,5.28778507964898,
12.4613867383844));
#44722=CARTESIAN_POINT('Ctrl Pts',(-2.61810205366918,4.59526745509803,12.5407586284378));
#44723=CARTESIAN_POINT('Ctrl Pts',(-4.49709775967304,2.78335284993721,12.6201305184912));
#44724=CARTESIAN_POINT('Ctrl Pts',(-5.28061040557763,0.293419651378745,
12.6995024085446));
#44725=CARTESIAN_POINT('Ctrl Pts',(-4.7777780451164,-2.26798992478223,12.778874298598));
#44726=CARTESIAN_POINT('Ctrl Pts',(-3.11108952829712,-4.27692217537683,
12.8582461886514));
#44727=CARTESIAN_POINT('Ctrl Pts',(-0.686546488664521,-5.24400565085626,
12.9376180787048));
#44728=CARTESIAN_POINT('Ctrl Pts',(1.90523775596186,-4.93366095719673,13.0169899687582));
#44729=CARTESIAN_POINT('Ctrl Pts',(4.03291030040817,-3.42148737483739,13.0963618588116));
#44730=CARTESIAN_POINT('Ctrl Pts',(4.95323103438167,-1.53655914035534,13.1601441507712));
#44731=CARTESIAN_POINT('Ctrl Pts',(5.07338179405736,-0.346578710011678,
13.1974691460464));
#44732=CARTESIAN_POINT('Ctrl Pts',(5.07322036085286,-6.69861637153657E-5,
13.2083368446371));
#44733=CARTESIAN_POINT('Origin',(0.,0.,-2.20833684463713));
#44734=CARTESIAN_POINT('',(5.0736465461671,-0.000129729951178492,11.2083368446371));
#44735=CARTESIAN_POINT('',(5.07340926806867,-0.000121118768615341,11.2916631553629));
#44736=CARTESIAN_POINT('',(5.0736,-1.85409460923845E-12,-2.20833684463713));
#44737=CARTESIAN_POINT('Ctrl Pts',(5.07340926806867,-0.000121118768615022,
11.2916631553629));
#44738=CARTESIAN_POINT('Ctrl Pts',(5.07289012258619,0.585265031435054,11.310024667149));
#44739=CARTESIAN_POINT('Ctrl Pts',(4.82580215794652,2.01456720880964,11.3548434756196));
#44740=CARTESIAN_POINT('Ctrl Pts',(3.51104609249152,3.95518604919035,11.4261195807747));
#44741=CARTESIAN_POINT('Ctrl Pts',(1.19167245960881,5.152752477688,11.5054914708281));
#44742=CARTESIAN_POINT('Ctrl Pts',(-1.41798994671238,5.09511980804502,11.5848633608815));
#44743=CARTESIAN_POINT('Ctrl Pts',(-3.68223314068194,3.79632723101863,11.6642352509349));
#44744=CARTESIAN_POINT('Ctrl Pts',(-5.04949249206616,1.57275774354392,11.7436071409883));
#44745=CARTESIAN_POINT('Ctrl Pts',(-5.18670664924514,-1.03393204901786,
11.8229790310417));
#44746=CARTESIAN_POINT('Ctrl Pts',(-4.06045054724843,-3.38875828300867,
11.9023509210951));
#44747=CARTESIAN_POINT('Ctrl Pts',(-1.94507767959685,-4.91809050014781,
11.9817228111485));
#44748=CARTESIAN_POINT('Ctrl Pts',(0.644111805448097,-5.24938675745961,
12.0610947012019));
#44749=CARTESIAN_POINT('Ctrl Pts',(3.0763970804032,-4.30194401997477,12.1404665912553));
#44750=CARTESIAN_POINT('Ctrl Pts',(4.70593891054333,-2.36980219715329,12.2173227426423));
#44751=CARTESIAN_POINT('Ctrl Pts',(5.07336579829568,-0.762978855367823,
12.2677215973449));
#44752=CARTESIAN_POINT('Ctrl Pts',(5.07393295843892,7.85666071204203E-5,
12.2916631553629));
#44753=CARTESIAN_POINT('Ctrl Pts',(5.0736465461671,-0.000129729951178388,
11.2083368446371));
#44754=CARTESIAN_POINT('Ctrl Pts',(5.07296127147132,0.663669285094766,11.2291606922858));
#44755=CARTESIAN_POINT('Ctrl Pts',(4.77561643393883,2.17143981582611,11.276441836619));
#44756=CARTESIAN_POINT('Ctrl Pts',(3.32375507563458,4.11382954733217,11.3501802776367));
#44757=CARTESIAN_POINT('Ctrl Pts',(0.951315435152466,5.20249366075065,11.4295521676901));
#44758=CARTESIAN_POINT('Ctrl Pts',(-1.6528625396318,5.02384183393465,11.5089240577436));
#44759=CARTESIAN_POINT('Ctrl Pts',(-3.85440685831092,3.62139325645746,11.5882959477969));
#44760=CARTESIAN_POINT('Ctrl Pts',(-5.11702619789041,1.33678129752526,11.6676678378503));
#44761=CARTESIAN_POINT('Ctrl Pts',(-5.13314928200913,-1.27346762656892,
11.7470397279037));
#44762=CARTESIAN_POINT('Ctrl Pts',(-3.89884856306365,-3.57350265560368,
11.8264116179572));
#44763=CARTESIAN_POINT('Ctrl Pts',(-1.71479696411077,-5.00304034754732,
11.9057835080105));
#44764=CARTESIAN_POINT('Ctrl Pts',(0.886975379660772,-5.21384848487043,
11.985155398064));
#44765=CARTESIAN_POINT('Ctrl Pts',(3.27268248423369,-4.15457467193696,12.0645272881174));
#44766=CARTESIAN_POINT('Ctrl Pts',(4.76154396611873,-2.21316538967253,12.1389211036417));
#44767=CARTESIAN_POINT('Ctrl Pts',(5.0730134915642,-0.684540002865494,12.1868576224816));
#44768=CARTESIAN_POINT('Ctrl Pts',(5.07371259150425,0.000124614973235296,
12.2083368446371));
#44769=CARTESIAN_POINT('Origin',(0.,0.,-2.20833684463713));
#44770=CARTESIAN_POINT('',(5.07325419654647,8.30592867887003E-5,10.2083368446371));
#44771=CARTESIAN_POINT('',(5.07344000894767,0.000124864012350097,10.2916631553629));
#44772=CARTESIAN_POINT('',(5.0736,-1.85409460923845E-12,-2.20833684463713));
#44773=CARTESIAN_POINT('Ctrl Pts',(5.07344000894767,0.000124864012350061,
10.2916631553629));
#44774=CARTESIAN_POINT('Ctrl Pts',(5.07366802985413,0.247199120889535,10.2994131435843));
#44775=CARTESIAN_POINT('Ctrl Pts',(4.99543134296861,1.33760465491503,10.3336204284901));
#44776=CARTESIAN_POINT('Ctrl Pts',(4.22690463795744,3.1787133448809,10.3942850100804));
#44777=CARTESIAN_POINT('Ctrl Pts',(2.1917205673539,4.81324238969408,10.4736569001339));
#44778=CARTESIAN_POINT('Ctrl Pts',(-0.377361782165876,5.27527624230907,
10.5530287901872));
#44779=CARTESIAN_POINT('Ctrl Pts',(-2.85451963682615,4.45226447892349,10.6324006802407));
#44780=CARTESIAN_POINT('Ctrl Pts',(-4.63632282632763,2.54469094339242,10.711772570294));
#44781=CARTESIAN_POINT('Ctrl Pts',(-5.28872803766221,0.0172363266288179,
10.7911444603475));
#44782=CARTESIAN_POINT('Ctrl Pts',(-4.65281080542322,-2.5144170211496,10.8705163504009));
#44783=CARTESIAN_POINT('Ctrl Pts',(-2.88347915980519,-4.43356394814365,
10.9498882404543));
#44784=CARTESIAN_POINT('Ctrl Pts',(-0.411738373331464,-5.27270451089727,
11.0292601305077));
#44785=CARTESIAN_POINT('Ctrl Pts',(2.16030096951836,-4.82742592572977,11.1086320205611));
#44786=CARTESIAN_POINT('Ctrl Pts',(4.20609577793862,-3.20619707038057,11.1880039106145));
#44787=CARTESIAN_POINT('Ctrl Pts',(4.99105565025759,-1.3596709971465,11.2490142888818));
#44788=CARTESIAN_POINT('Ctrl Pts',(5.07363816480692,-0.25822406855438,11.2835673704646));
#44789=CARTESIAN_POINT('Ctrl Pts',(5.07340926806867,-0.000121118768615022,
11.2916631553629));
#44790=CARTESIAN_POINT('Ctrl Pts',(5.07325419654647,8.30592867889779E-5,
10.2083368446371));
#44791=CARTESIAN_POINT('Ctrl Pts',(5.07344390313192,0.32569224224827,10.2185491687211));
#44792=CARTESIAN_POINT('Ctrl Pts',(4.96261803044706,1.49473693663548,10.2552187894896));
#44793=CARTESIAN_POINT('Ctrl Pts',(4.07486890650351,3.37140693807807,10.3183457069425));
#44794=CARTESIAN_POINT('Ctrl Pts',(1.96603890048266,4.90974870936374,10.3977175969959));
#44795=CARTESIAN_POINT('Ctrl Pts',(-0.621713829942471,5.25208656259283,
10.4770894870493));
#44796=CARTESIAN_POINT('Ctrl Pts',(-3.05801844753381,4.31502775447074,10.5564613771027));
#44797=CARTESIAN_POINT('Ctrl Pts',(-4.74939654011498,2.32683773651149,10.6358332671561));
#44798=CARTESIAN_POINT('Ctrl Pts',(-5.28383214813503,-0.228164803694007,
10.7152051572095));
#44799=CARTESIAN_POINT('Ctrl Pts',(-4.53113794043347,-2.72758690275384,
10.7945770472629));
#44800=CARTESIAN_POINT('Ctrl Pts',(-2.67466855994604,-4.56257486971405,
10.8739489373163));
#44801=CARTESIAN_POINT('Ctrl Pts',(-0.166655838534166,-5.2861296975001,
10.9533208273697));
#44802=CARTESIAN_POINT('Ctrl Pts',(2.38195387625819,-4.72199503162473,11.0326927174231));
#44803=CARTESIAN_POINT('Ctrl Pts',(4.3503248991595,-3.00759282800428,11.1120646074765));
#44804=CARTESIAN_POINT('Ctrl Pts',(5.02057706818124,-1.20254945990408,11.1706126498812));
#44805=CARTESIAN_POINT('Ctrl Pts',(5.07383193265951,-0.17970643375256,11.2027033956014));
#44806=CARTESIAN_POINT('Ctrl Pts',(5.0736465461671,-0.000129729951178388,
11.2083368446371));
#44807=CARTESIAN_POINT('Origin',(0.,0.,-2.20833684463713));
#44808=CARTESIAN_POINT('',(5.07403156349013,-1.34850231131101E-5,9.20833684463708));
#44809=CARTESIAN_POINT('',(5.07390676572803,-8.73588085612467E-5,9.29166315536294));
#44810=CARTESIAN_POINT('',(5.0736,-1.85409460923845E-12,-2.20833684463713));
#44811=CARTESIAN_POINT('Ctrl Pts',(5.07390676572803,-8.73588085611478E-5,
9.29166315536294));
#44812=CARTESIAN_POINT('Ctrl Pts',(5.07329990983557,0.75196019632477,9.31525891670402));
#44813=CARTESIAN_POINT('Ctrl Pts',(4.71401054212216,2.34781906214645,9.36531197472956));
#44814=CARTESIAN_POINT('Ctrl Pts',(3.10437209115777,4.28180047024037,9.44182232943961));
#44815=CARTESIAN_POINT('Ctrl Pts',(0.67831398067512,5.24507688131743,9.52119421949299));
#44816=CARTESIAN_POINT('Ctrl Pts',(-1.91297991407746,4.93066417388633,9.6005661095464));
#44817=CARTESIAN_POINT('Ctrl Pts',(-4.03827613607002,3.41515258753654,9.6799379995998));
#44818=CARTESIAN_POINT('Ctrl Pts',(-5.1798572298885,1.06771739017486,9.75930988965322));
#44819=CARTESIAN_POINT('Ctrl Pts',(-5.05963656792565,-1.53981140008104,
9.8386817797066));
#44820=CARTESIAN_POINT('Ctrl Pts',(-3.70689963733171,-3.77224554159189,
9.91805366976003));
#44821=CARTESIAN_POINT('Ctrl Pts',(-1.45117016016697,-5.08576901889487,
9.99742555981341));
#44822=CARTESIAN_POINT('Ctrl Pts',(1.1580611559038,-5.16041042035386,10.0767974498668));
#44823=CARTESIAN_POINT('Ctrl Pts',(3.48519133772131,-3.97798726578937,10.1561693399202));
#44824=CARTESIAN_POINT('Ctrl Pts',(4.81900834166099,-2.03660616436304,10.2277912417523));
#44825=CARTESIAN_POINT('Ctrl Pts',(5.07288960070042,-0.596275311661321,
10.2729558468998));
#44826=CARTESIAN_POINT('Ctrl Pts',(5.07344000894767,0.000124864012350061,
10.2916631553629));
#44827=CARTESIAN_POINT('Ctrl Pts',(5.07403156349013,-1.34850231132098E-5,
9.20833684463708));
#44828=CARTESIAN_POINT('Ctrl Pts',(5.07390455498411,0.830454679150979,9.2343949418408));
#44829=CARTESIAN_POINT('Ctrl Pts',(4.65463656321598,2.50423700786744,9.28691033572898));
#44830=CARTESIAN_POINT('Ctrl Pts',(2.90236501609723,4.42122366100663,9.36588302630163));
#44831=CARTESIAN_POINT('Ctrl Pts',(0.434226208411351,5.27090020273944,9.44525491635504));
#44832=CARTESIAN_POINT('Ctrl Pts',(-2.13968914250016,4.83659712202464,9.52462680640844));
#44833=CARTESIAN_POINT('Ctrl Pts',(-4.1923809544202,3.22410968801074,9.60399869646184));
#44834=CARTESIAN_POINT('Ctrl Pts',(-5.22381804552131,0.826236270443201,
9.68337058651526));
#44835=CARTESIAN_POINT('Ctrl Pts',(-4.98274462345855,-1.77290647376134,
9.76274247656865));
#44836=CARTESIAN_POINT('Ctrl Pts',(-3.52788564023945,-3.94017312521954,
9.84211436662205));
#44837=CARTESIAN_POINT('Ctrl Pts',(-1.21364152390043,-5.14762232479954,
9.92148625667546));
#44838=CARTESIAN_POINT('Ctrl Pts',(1.39624298131078,-5.10112212012714,10.0008581467289));
#44839=CARTESIAN_POINT('Ctrl Pts',(3.66600578680612,-3.81199985813406,10.0802300367823));
#44840=CARTESIAN_POINT('Ctrl Pts',(4.86560152926764,-1.87962374426628,10.1493896027517));
#44841=CARTESIAN_POINT('Ctrl Pts',(5.07295242603298,-0.517870759272535,
10.1920918720366));
#44842=CARTESIAN_POINT('Ctrl Pts',(5.07325419654647,8.30592867889779E-5,
10.2083368446371));
#44843=CARTESIAN_POINT('Origin',(0.,0.,-2.20833684463713));
#44844=CARTESIAN_POINT('',(5.07321399251666,-6.32753131005193E-5,8.20833684463707));
#44845=CARTESIAN_POINT('',(5.07316567838514,7.26391603613751E-6,8.29166315536292));
#44846=CARTESIAN_POINT('',(5.0736,-1.85409460923845E-12,-2.20833684463713));
#44847=CARTESIAN_POINT('Ctrl Pts',(5.07316594763625,7.25941288019782E-6,
8.29166315536292));
#44848=CARTESIAN_POINT('Ctrl Pts',(5.07318657601694,0.414016596607197,8.30464739313926));
#44849=CARTESIAN_POINT('Ctrl Pts',(4.92101378278626,1.67161602862595,8.34408892760008));
#44850=CARTESIAN_POINT('Ctrl Pts',(3.89323433265495,3.57961838445758,8.40998775874535));
#44851=CARTESIAN_POINT('Ctrl Pts',(1.70694143925982,5.00572594837628,8.48935964879875));
#44852=CARTESIAN_POINT('Ctrl Pts',(-0.895158610488236,5.21244975125697,
8.56873153885215));
#44853=CARTESIAN_POINT('Ctrl Pts',(-3.27920000412133,4.14943233229326,8.64810342890557));
#44854=CARTESIAN_POINT('Ctrl Pts',(-4.86443553513654,2.0756223817956,8.72747531895896));
#44855=CARTESIAN_POINT('Ctrl Pts',(-5.26470533703792,-0.503804586595236,
8.80684720901237));
#44856=CARTESIAN_POINT('Ctrl Pts',(-4.38250457206448,-2.96050587284403,
8.88621909906576));
#44857=CARTESIAN_POINT('Ctrl Pts',(-2.43273539384546,-4.69603448143659,
8.96559098911917));
#44858=CARTESIAN_POINT('Ctrl Pts',(0.109642741545844,-5.28761948484726,
9.04496287917257));
#44859=CARTESIAN_POINT('Ctrl Pts',(2.62531214778668,-4.59115208569632,9.12433476922599));
#44860=CARTESIAN_POINT('Ctrl Pts',(4.50146132585655,-2.77629020081255,9.20370665927937));
#44861=CARTESIAN_POINT('Ctrl Pts',(5.04930321710503,-1.02570491769659,9.25948278799171));
#44862=CARTESIAN_POINT('Ctrl Pts',(5.07398036113186,-0.0912906316256552,
9.28880162001956));
#44863=CARTESIAN_POINT('Ctrl Pts',(5.07390676572803,-8.73588085611478E-5,
9.29166315536294));
#44864=CARTESIAN_POINT('Ctrl Pts',(5.07321399251666,-6.32753131006233E-5,
8.20833684463707));
#44865=CARTESIAN_POINT('Ctrl Pts',(5.07299759473682,0.492445607247212,8.22378341827604));
#44866=CARTESIAN_POINT('Ctrl Pts',(4.87982559067105,1.82870276667211,8.26568728859948));
#44867=CARTESIAN_POINT('Ctrl Pts',(3.72295704063487,3.75639883677136,8.33404845560738));
#44868=CARTESIAN_POINT('Ctrl Pts',(1.47285113468463,5.07953254565499,8.41342034566079));
#44869=CARTESIAN_POINT('Ctrl Pts',(-1.1360380475741,5.16530336977162,8.49279223571419));
#44870=CARTESIAN_POINT('Ctrl Pts',(-3.46819087602133,3.99281772621695,8.57216412576759));
#44871=CARTESIAN_POINT('Ctrl Pts',(-4.95550008378004,1.84769052250801,8.651536015821));
#44872=CARTESIAN_POINT('Ctrl Pts',(-5.23566043994335,-0.74753000269027,
8.7309079058744));
#44873=CARTESIAN_POINT('Ctrl Pts',(-4.24042550187429,-3.16065387386283,
8.81027979592781));
#44874=CARTESIAN_POINT('Ctrl Pts',(-2.21223229757129,-4.8038494573511,8.88965168598121));
#44875=CARTESIAN_POINT('Ctrl Pts',(0.354855797726969,-5.27683794616905,
8.96902357603462));
#44876=CARTESIAN_POINT('Ctrl Pts',(2.83550180615889,-4.46440039138287,9.04839546608801));
#44877=CARTESIAN_POINT('Ctrl Pts',(4.6254258508873,-2.56444478303851,9.12776735614143));
#44878=CARTESIAN_POINT('Ctrl Pts',(5.0708816691802,-0.868647987514843,9.18108114899111));
#44879=CARTESIAN_POINT('Ctrl Pts',(5.07403350920893,-0.0127359204844534,
9.20793764515633));
#44880=CARTESIAN_POINT('Ctrl Pts',(5.07403156349013,-1.34850231132098E-5,
9.20833684463708));
#44881=CARTESIAN_POINT('Origin',(0.,0.,-2.20833684463713));
#44882=CARTESIAN_POINT('',(5.0737268532953,0.000123079057421927,7.20833684463709));
#44883=CARTESIAN_POINT('',(5.07394313380083,7.47405269748897E-5,7.29166315536293));
#44884=CARTESIAN_POINT('',(5.0736,-1.85409460923845E-12,-2.20833684463713));
#44885=CARTESIAN_POINT('Ctrl Pts',(5.07394313380082,7.47405269749084E-5,
7.29166315536293));
#44886=CARTESIAN_POINT('Ctrl Pts',(5.07399715749136,0.0756966636928046,
7.29403586957452));
#44887=CARTESIAN_POINT('Ctrl Pts',(5.05387993962774,0.994523136339973,7.32286588047058));
#44888=CARTESIAN_POINT('Ctrl Pts',(4.52685078861501,2.73469619609302,7.37815318805109));
#44889=CARTESIAN_POINT('Ctrl Pts',(2.66750326347436,4.56676775046241,7.45752507810451));
#44890=CARTESIAN_POINT('Ctrl Pts',(0.158357847769689,5.28638478918814,7.5368969681579));
#44891=CARTESIAN_POINT('Ctrl Pts',(-2.38936318913255,4.71825019448189,7.61626885821132));
#44892=CARTESIAN_POINT('Ctrl Pts',(-4.3550406419278,3.0007602960695,7.69564074826471));
#44893=CARTESIAN_POINT('Ctrl Pts',(-5.25983983406839,0.552291831604834,
7.77501263831812));
#44894=CARTESIAN_POINT('Ctrl Pts',(-4.88335368508791,-2.03071370056153,
7.85438452837152));
#44895=CARTESIAN_POINT('Ctrl Pts',(-3.31729338754006,-4.11904187017964,
7.93375641842492));
#44896=CARTESIAN_POINT('Ctrl Pts',(-0.943147763491834,-5.20398055756651,
8.01312830847834));
#44897=CARTESIAN_POINT('Ctrl Pts',(1.66074656812082,-5.02124109994579,8.09250019853171));
#44898=CARTESIAN_POINT('Ctrl Pts',(3.86008671173945,-3.61533842470695,8.17187208858515));
#44899=CARTESIAN_POINT('Ctrl Pts',(4.91315662948087,-1.70280471015196,8.23825974086219));
#44900=CARTESIAN_POINT('Ctrl Pts',(5.07314454265331,-0.429588399925582,
8.27819009645479));
#44901=CARTESIAN_POINT('Ctrl Pts',(5.07316594763625,7.25941288019782E-6,
8.29166315536292));
#44902=CARTESIAN_POINT('Ctrl Pts',(5.0737268532953,0.000123079057421736,
7.20833684463709));
#44903=CARTESIAN_POINT('Ctrl Pts',(5.07388334783635,0.154242294956097,7.2131718947113));
#44904=CARTESIAN_POINT('Ctrl Pts',(5.02933704432274,1.15160862859258,7.24446424146999));
#44905=CARTESIAN_POINT('Ctrl Pts',(4.39509322077433,2.9417846501764,7.30221388491313));
#44906=CARTESIAN_POINT('Ctrl Pts',(2.45274496186498,4.68561452739722,7.38158577496654));
#44907=CARTESIAN_POINT('Ctrl Pts',(-0.0870865406957981,5.28803907717593,
7.46095766501995));
#44908=CARTESIAN_POINT('Ctrl Pts',(-2.60570395470586,4.60230901263053,7.54032955507335));
#44909=CARTESIAN_POINT('Ctrl Pts',(-4.48957765297745,2.79546665964655,7.61970144512676));
#44910=CARTESIAN_POINT('Ctrl Pts',(-5.27980017249532,0.307654816033177,
7.69907333518014));
#44911=CARTESIAN_POINT('Ctrl Pts',(-4.78387505663278,-2.25510105978351,
7.77844522523357));
#44912=CARTESIAN_POINT('Ctrl Pts',(-3.12260856590233,-4.26851930901846,
7.85781711528695));
#44913=CARTESIAN_POINT('Ctrl Pts',(-0.70068154029489,-5.24213570278374,
7.93718900534038));
#44914=CARTESIAN_POINT('Ctrl Pts',(1.8919299575961,-4.93877944262147,8.01656089539376));
#44915=CARTESIAN_POINT('Ctrl Pts',(4.02367150553262,-3.43234744203947,8.09593278544719));
#44916=CARTESIAN_POINT('Ctrl Pts',(4.95114565728143,-1.54568603506211,8.15985810186161));
#44917=CARTESIAN_POINT('Ctrl Pts',(5.07336824653293,-0.351136531432447,
8.19732612159157));
#44918=CARTESIAN_POINT('Ctrl Pts',(5.07321399251666,-6.32753131006233E-5,
8.20833684463707));
#44919=CARTESIAN_POINT('Origin',(0.,0.,-2.20833684463713));
#44920=CARTESIAN_POINT('',(5.07363207848188,-0.00013042437206158,6.20833684463708));
#44921=CARTESIAN_POINT('',(5.07339692231655,-0.000119345805453296,6.29166315536293));
#44922=CARTESIAN_POINT('',(5.0736,-1.85409460923845E-12,-2.20833684463713));
#44923=CARTESIAN_POINT('Ctrl Pts',(5.07339692231655,-0.000119345805453183,
6.29166315536293));
#44924=CARTESIAN_POINT('Ctrl Pts',(5.07289122007049,0.580711075066297,6.30988164269423));
#44925=CARTESIAN_POINT('Ctrl Pts',(4.82858806615863,2.00545098816607,6.35455742671001));
#44926=CARTESIAN_POINT('Ctrl Pts',(3.52169629398765,3.94570609146495,6.42569050741027));
#44927=CARTESIAN_POINT('Ctrl Pts',(1.20555966211655,5.14952106980711,6.50506239746365));
#44928=CARTESIAN_POINT('Ctrl Pts',(-1.40424863498509,5.09892411381582,6.58443428751707));
#44929=CARTESIAN_POINT('Ctrl Pts',(-3.67198507285601,3.80624052997609,6.66380617757046));
#44930=CARTESIAN_POINT('Ctrl Pts',(-5.04523407478029,1.58636517800468,6.74317806762388));
#44931=CARTESIAN_POINT('Ctrl Pts',(-5.1894752235243,-1.01994521996889,6.82254995767727));
#44932=CARTESIAN_POINT('Ctrl Pts',(-4.06957169452636,-3.37779921996849,
6.90192184773068));
#44933=CARTESIAN_POINT('Ctrl Pts',(-1.95832950858598,-4.91282880661553,
6.98129373778407));
#44934=CARTESIAN_POINT('Ctrl Pts',(0.629957410957137,-5.25110417033315,
7.06066562783749));
#44935=CARTESIAN_POINT('Ctrl Pts',(3.06478809957816,-4.31022218127953,7.14003751789089));
#44936=CARTESIAN_POINT('Ctrl Pts',(4.70257511155161,-2.37889312808664,7.2170366937327));
#44937=CARTESIAN_POINT('Ctrl Pts',(5.07339475843234,-0.767536645770191,
7.26757857289005));
#44938=CARTESIAN_POINT('Ctrl Pts',(5.07394313380082,7.47405269749084E-5,
7.29166315536293));
#44939=CARTESIAN_POINT('Ctrl Pts',(5.07363207848188,-0.000130424372061667,
6.20833684463708));
#44940=CARTESIAN_POINT('Ctrl Pts',(5.07295192244443,0.659114832324929,6.22901766783102));
#44941=CARTESIAN_POINT('Ctrl Pts',(4.77864726944019,2.16233220285461,6.27615578770943));
#44942=CARTESIAN_POINT('Ctrl Pts',(3.33483365177601,4.10485393921541,6.34975120427228));
#44943=CARTESIAN_POINT('Ctrl Pts',(0.96533761058682,5.19991006123149,6.42912309432572));
#44944=CARTESIAN_POINT('Ctrl Pts',(-1.63931253580277,5.02827960213728,6.50849498437909));
#44945=CARTESIAN_POINT('Ctrl Pts',(-3.84462977702757,3.63177136187054,6.58786687443252));
#44946=CARTESIAN_POINT('Ctrl Pts',(-5.11340371451209,1.35057165664169,6.6672387644859));
#44947=CARTESIAN_POINT('Ctrl Pts',(-5.13656382546863,-1.25962431470543,
6.74661065453933));
#44948=CARTESIAN_POINT('Ctrl Pts',(-3.90846835813217,-3.56297859112141,
6.82598254459271));
#44949=CARTESIAN_POINT('Ctrl Pts',(-1.72827865000271,-4.99839916925957,
6.90535443464612));
#44950=CARTESIAN_POINT('Ctrl Pts',(0.872915911787522,-5.21622077353501,
6.98472632469953));
#44951=CARTESIAN_POINT('Ctrl Pts',(3.26147008963291,-4.16338254328616,7.06409821475292));
#44952=CARTESIAN_POINT('Ctrl Pts',(4.7584325270959,-2.22226951355623,7.13863505473211));
#44953=CARTESIAN_POINT('Ctrl Pts',(5.07302701285767,-0.689094952273734,
7.18671459802684));
#44954=CARTESIAN_POINT('Ctrl Pts',(5.0737268532953,0.000123079057421736,
7.20833684463709));
#44955=CARTESIAN_POINT('Origin',(0.,0.,-2.20833684463713));
#44956=CARTESIAN_POINT('',(5.07326256235615,8.6340948239616E-5,5.20833684463708));
#44957=CARTESIAN_POINT('',(5.07345306532775,0.000126183674940957,5.29166315536293));
#44958=CARTESIAN_POINT('',(5.0736,-1.85409460923845E-12,-2.20833684463713));
#44959=CARTESIAN_POINT('Ctrl Pts',(5.07345306532775,0.000126183674940827,
5.29166315536293));
#44960=CARTESIAN_POINT('Ctrl Pts',(5.07368016839978,0.24263894378533,5.29927011912949));
#44961=CARTESIAN_POINT('Ctrl Pts',(4.99721910617995,1.32847790639321,5.33333437958052));
#44962=CARTESIAN_POINT('Ctrl Pts',(4.23545891089922,3.1673062942182,5.39385593671601));
#44963=CARTESIAN_POINT('Ctrl Pts',(2.20468883537238,4.80731614172549,5.47322782676942));
#44964=CARTESIAN_POINT('Ctrl Pts',(-0.363138560455233,5.27627441792221,
5.55259971682281));
#44965=CARTESIAN_POINT('Ctrl Pts',(-2.84250620674952,4.45994392474844,5.63197160687622));
#44966=CARTESIAN_POINT('Ctrl Pts',(-4.62944563286038,2.55718096342436,5.71134349692963));
#44967=CARTESIAN_POINT('Ctrl Pts',(-5.28866234991055,0.0314943796341776,
5.79071538698302));
#44968=CARTESIAN_POINT('Ctrl Pts',(-4.65957262477808,-2.50186416532327,
5.87008727703643));
#44969=CARTESIAN_POINT('Ctrl Pts',(-2.89542132203872,-4.42577413739037,
5.94945916708984));
#44970=CARTESIAN_POINT('Ctrl Pts',(-0.425951794157121,-5.27157532587407,
6.02883105714324));
#44971=CARTESIAN_POINT('Ctrl Pts',(2.14727864795285,-4.8332324334089,6.10820294719664));
#44972=CARTESIAN_POINT('Ctrl Pts',(4.19743676434218,-3.21752481834385,6.18757483725004));
#44973=CARTESIAN_POINT('Ctrl Pts',(4.98922373212554,-1.36879789494917,6.24872823997214));
#44974=CARTESIAN_POINT('Ctrl Pts',(5.0736256122357,-0.262783913782733,6.28342434600977));
#44975=CARTESIAN_POINT('Ctrl Pts',(5.07339692231655,-0.000119345805453183,
6.29166315536293));
#44976=CARTESIAN_POINT('Ctrl Pts',(5.07326256235615,8.63409482398936E-5,
5.20833684463708));
#44977=CARTESIAN_POINT('Ctrl Pts',(5.07345742030602,0.321133824030879,5.21840614426627));
#44978=CARTESIAN_POINT('Ctrl Pts',(4.96462985132702,1.48560987617541,5.25493274057992));
#44979=CARTESIAN_POINT('Ctrl Pts',(4.08394322312664,3.36040906700182,5.31791663357805));
#44980=CARTESIAN_POINT('Ctrl Pts',(1.979268164295,4.90443053586431,5.39728852363145));
#44981=CARTESIAN_POINT('Ctrl Pts',(-0.607552238323124,5.25374358196311,
5.47666041368485));
#44982=CARTESIAN_POINT('Ctrl Pts',(-3.04637426047979,4.32325632045987,5.55603230373826));
#44983=CARTESIAN_POINT('Ctrl Pts',(-4.74310625581864,2.33963338865815,5.63540419379165));
#44984=CARTESIAN_POINT('Ctrl Pts',(-5.28442806592769,-0.213919057930008,
5.71477608384507));
#44985=CARTESIAN_POINT('Ctrl Pts',(-4.53847489605989,-2.71536129550824,
5.79414797389846));
#44986=CARTESIAN_POINT('Ctrl Pts',(-2.68695928725567,-4.55534753185094,
5.87351986395187));
#44987=CARTESIAN_POINT('Ctrl Pts',(-0.180906343559476,-5.28566119252549,
5.95289175400528));
#44988=CARTESIAN_POINT('Ctrl Pts',(2.36921498499841,-4.72839948631341,6.03226364405867));
#44989=CARTESIAN_POINT('Ctrl Pts',(4.3422007873791,-3.01931013137013,6.1116355341121));
#44990=CARTESIAN_POINT('Ctrl Pts',(5.01896602830084,-1.21167525394927,6.17032660097155));
#44991=CARTESIAN_POINT('Ctrl Pts',(5.07382205657331,-0.184267811620037,
6.20256037114655));
#44992=CARTESIAN_POINT('Ctrl Pts',(5.07363207848188,-0.000130424372061667,
6.20833684463708));
#44993=CARTESIAN_POINT('Origin',(0.,0.,-2.20833684463713));
#44994=CARTESIAN_POINT('',(5.07402907570203,-1.82827833135855E-5,4.20833684463708));
#44995=CARTESIAN_POINT('',(5.07389532565035,-9.07960786141478E-5,4.29166315536292));
#44996=CARTESIAN_POINT('',(5.0736,-1.85409460923845E-12,-2.20833684463713));
#44997=CARTESIAN_POINT('Ctrl Pts',(5.07389532565035,-9.07960786142303E-5,
4.29166315536292));
#44998=CARTESIAN_POINT('Ctrl Pts',(5.07327433146367,0.747403143972462,4.3151158922492));
#44999=CARTESIAN_POINT('Ctrl Pts',(4.7173237838915,2.33872520323751,4.36502592581995));
#45000=CARTESIAN_POINT('Ctrl Pts',(3.11590430478523,4.27341569598967,4.44139325607517));
#45001=CARTESIAN_POINT('Ctrl Pts',(0.692451950200399,5.24322912373411,4.52076514612856));
#45002=CARTESIAN_POINT('Ctrl Pts',(-1.89968016673685,4.93580354262775,4.60013703618198));
#45003=CARTESIAN_POINT('Ctrl Pts',(-4.02905439992773,3.42602714375309,4.67950892623537));
#45004=CARTESIAN_POINT('Ctrl Pts',(-5.17695989945686,1.08167811604265,4.75888081628878));
#45005=CARTESIAN_POINT('Ctrl Pts',(-5.06376942648468,-1.5261653064819,4.83825270634218));
#45006=CARTESIAN_POINT('Ctrl Pts',(-3.71705592968434,-3.76223823845706,
4.91762459639559));
#45007=CARTESIAN_POINT('Ctrl Pts',(-1.46487583597662,-5.08183826311717,
4.996996486449));
#45008=CARTESIAN_POINT('Ctrl Pts',(1.14414476892732,-5.16351373534013,5.07636837650239));
#45009=CARTESIAN_POINT('Ctrl Pts',(3.47445424064207,-3.98736869087803,5.15574026655581));
#45010=CARTESIAN_POINT('Ctrl Pts',(4.81617424358115,-2.04572091909076,5.22750519284264));
#45011=CARTESIAN_POINT('Ctrl Pts',(5.07289029565433,-0.600829257314202,
5.27281282244502));
#45012=CARTESIAN_POINT('Ctrl Pts',(5.07345306532775,0.000126183674940827,
5.29166315536293));
#45013=CARTESIAN_POINT('Ctrl Pts',(5.07402907570203,-1.82827833134858E-5,
4.20833684463708));
#45014=CARTESIAN_POINT('Ctrl Pts',(5.07386028856637,0.825892891192897,4.23425191738599));
#45015=CARTESIAN_POINT('Ctrl Pts',(4.65820682968666,2.49515959185088,4.28662428681936));
#45016=CARTESIAN_POINT('Ctrl Pts',(2.91427384097298,4.41338297988409,4.36545395293721));
#45017=CARTESIAN_POINT('Ctrl Pts',(0.44843468320075,5.26971039832481,4.44482584299061));
#45018=CARTESIAN_POINT('Ctrl Pts',(-2.12664217080585,4.84234802803972,4.52419773304401));
#45019=CARTESIAN_POINT('Ctrl Pts',(-4.18367369924674,3.23540039647972,4.60356962309741));
#45020=CARTESIAN_POINT('Ctrl Pts',(-5.22157157495578,0.840316389774564,
4.68294151315082));
#45021=CARTESIAN_POINT('Ctrl Pts',(-4.98750617275825,-1.75946682947089,
4.76231340320422));
#45022=CARTESIAN_POINT('Ctrl Pts',(-3.53849530653447,-3.93064782357102,
4.84168529325762));
#45023=CARTESIAN_POINT('Ctrl Pts',(-1.22751481596538,-5.14433170819062,
4.92105718331103));
#45024=CARTESIAN_POINT('Ctrl Pts',(1.3824855667149,-5.10486777548008,5.00042907336443));
#45025=CARTESIAN_POINT('Ctrl Pts',(3.65571552542333,-3.82186935209575,5.07980096341784));
#45026=CARTESIAN_POINT('Ctrl Pts',(4.86300805809873,-1.88874478353847,5.14910355384205));
#45027=CARTESIAN_POINT('Ctrl Pts',(5.07294542694196,-0.522425194224716,
5.1919488475818));
#45028=CARTESIAN_POINT('Ctrl Pts',(5.07326256235615,8.63409482398936E-5,
5.20833684463708));
#45029=CARTESIAN_POINT('Origin',(0.,0.,-2.20833684463713));
#45030=CARTESIAN_POINT('',(5.0732079990561,-5.95000919163813E-5,3.20833684463708));
#45031=CARTESIAN_POINT('',(5.07316685382493,1.14989646604178E-5,3.29166315536292));
#45032=CARTESIAN_POINT('',(5.0736,-1.85409460923845E-12,-2.20833684463713));
#45033=CARTESIAN_POINT('Ctrl Pts',(5.07316685382493,1.14989646600797E-5,
3.29166315536292));
#45034=CARTESIAN_POINT('Ctrl Pts',(5.07319917633903,0.409460216043812,3.30450436868445));
#45035=CARTESIAN_POINT('Ctrl Pts',(4.923282999623,1.66249023374937,3.34380287869045));
#45036=CARTESIAN_POINT('Ctrl Pts',(3.90287063578958,3.56910943340232,3.40955868538091));
#45037=CARTESIAN_POINT('Ctrl Pts',(1.7204303939291,5.00110593838552,3.48893057543432));
#45038=CARTESIAN_POINT('Ctrl Pts',(-0.881102883784432,5.21484410653825,
3.56830246548772));
#45039=CARTESIAN_POINT('Ctrl Pts',(-3.26800144929621,4.15825779319991,3.64767435554113));
#45040=CARTESIAN_POINT('Ctrl Pts',(-4.85882209535798,2.08872908558557,3.72704624559453));
#45041=CARTESIAN_POINT('Ctrl Pts',(-5.2660444338108,-0.489609403954008,
3.80641813564793));
#45042=CARTESIAN_POINT('Ctrl Pts',(-4.39047000437897,-2.94868012642242,
3.88579002570134));
#45043=CARTESIAN_POINT('Ctrl Pts',(-2.44538680002092,-4.68945889688708,
3.96516191575474));
#45044=CARTESIAN_POINT('Ctrl Pts',(0.0953872160503347,-5.28789586001125,
4.04453380580815));
#45045=CARTESIAN_POINT('Ctrl Pts',(2.61292511742776,-4.59821309619564,4.12390569586154));
#45046=CARTESIAN_POINT('Ctrl Pts',(4.49396024381142,-2.78841580011883,4.20327758591496));
#45047=CARTESIAN_POINT('Ctrl Pts',(5.04793652990732,-1.03482867897542,4.25919673908208));
#45048=CARTESIAN_POINT('Ctrl Pts',(5.07397488200138,-0.0958531905725829,
4.28865859556473));
#45049=CARTESIAN_POINT('Ctrl Pts',(5.07389532565035,-9.07960786142303E-5,
4.29166315536292));
#45050=CARTESIAN_POINT('Ctrl Pts',(5.0732079990561,-5.95000919163813E-5,
3.20833684463708));
#45051=CARTESIAN_POINT('Ctrl Pts',(5.07300669336618,0.487890744857983,3.22364039382123));
#45052=CARTESIAN_POINT('Ctrl Pts',(4.88232843229471,1.81957999791209,3.26540123968986));
#45053=CARTESIAN_POINT('Ctrl Pts',(3.73307055280206,3.74634830136122,3.33361938224296));
#45054=CARTESIAN_POINT('Ctrl Pts',(1.48653991852054,5.07554336184363,3.41299127229636));
#45055=CARTESIAN_POINT('Ctrl Pts',(-1.12210854951228,5.16834729390561,3.49236316234976));
#45056=CARTESIAN_POINT('Ctrl Pts',(-3.45741385862906,4.00215326511488,3.57173505240317));
#45057=CARTESIAN_POINT('Ctrl Pts',(-4.95050080463958,1.86104355955814,3.65110694245657));
#45058=CARTESIAN_POINT('Ctrl Pts',(-5.23765671238755,-0.733412237756895,
3.73047883250997));
#45059=CARTESIAN_POINT('Ctrl Pts',(-4.24893103835441,-3.14921043733482,
3.80985072256337));
#45060=CARTESIAN_POINT('Ctrl Pts',(-2.22517516822744,-4.79786794503704,
3.88922261261678));
#45061=CARTESIAN_POINT('Ctrl Pts',(0.340628447538026,-5.2777754412288,3.96859450267018));
#45062=CARTESIAN_POINT('Ctrl Pts',(2.82345572745151,-4.472028522095,4.04796639272359));
#45063=CARTESIAN_POINT('Ctrl Pts',(4.61849544177105,-2.57690535364612,4.12733828277699));
#45064=CARTESIAN_POINT('Ctrl Pts',(5.06972869559084,-0.877769583505955,
4.18079510008149));
#45065=CARTESIAN_POINT('Ctrl Pts',(5.07403260725396,-0.0172989136932101,
4.20779462070152));
#45066=CARTESIAN_POINT('Ctrl Pts',(5.07402907570203,-1.82827833134858E-5,
4.20833684463708));
#45067=CARTESIAN_POINT('Origin',(0.,0.,-2.20833684463713));
#45068=CARTESIAN_POINT('',(5.07374102492394,0.00012139426775859,2.20833684463708));
#45069=CARTESIAN_POINT('',(5.07395289332891,7.08096438841769E-5,2.29166315536292));
#45070=CARTESIAN_POINT('',(5.0736,-1.85409460923845E-12,-2.20833684463713));
#45071=CARTESIAN_POINT('Ctrl Pts',(5.07395289332891,7.08096438841854E-5,
2.29166315536292));
#45072=CARTESIAN_POINT('Ctrl Pts',(5.07400149993288,0.0711339346777274,
2.2938928451197));
#45073=CARTESIAN_POINT('Ctrl Pts',(5.05519150559033,0.985399910949532,2.32257983156095));
#45074=CARTESIAN_POINT('Ctrl Pts',(4.53420692607935,2.72248212093367,2.37772411468667));
#45075=CARTESIAN_POINT('Ctrl Pts',(2.67980532059554,4.5595597146017,2.45709600474007));
#45076=CARTESIAN_POINT('Ctrl Pts',(0.172609070663326,5.28593865420646,2.53646789479348));
#45077=CARTESIAN_POINT('Ctrl Pts',(-2.37663436681889,4.72467463787357,2.61583978484688));
#45078=CARTESIAN_POINT('Ctrl Pts',(-4.34693493313492,3.01249033764445,2.69521167490029));
#45079=CARTESIAN_POINT('Ctrl Pts',(-5.25833177151656,0.56647005919948,2.77458356495369));
#45080=CARTESIAN_POINT('Ctrl Pts',(-4.88881062947673,-2.01754107180632,
2.85395545500709));
#45081=CARTESIAN_POINT('Ctrl Pts',(-3.32838603929513,-4.11008366347149,
2.93332734506049));
#45082=CARTESIAN_POINT('Ctrl Pts',(-0.957173977198773,-5.20141897223089,
3.0126992351139));
#45083=CARTESIAN_POINT('Ctrl Pts',(1.64720354707453,-5.02570013250045,3.0920711251673));
#45084=CARTESIAN_POINT('Ctrl Pts',(3.85032593330369,-3.62573186469146,3.1714430152207));
#45085=CARTESIAN_POINT('Ctrl Pts',(4.91082792455161,-1.71192991859137,3.23797369195258));
#45086=CARTESIAN_POINT('Ctrl Pts',(5.07313258089171,-0.434144349474542,
3.27804707199999));
#45087=CARTESIAN_POINT('Ctrl Pts',(5.07316685382493,1.14989646600797E-5,
3.29166315536292));
#45088=CARTESIAN_POINT('Ctrl Pts',(5.07374102492394,0.000121394267758555,
2.20833684463708));
#45089=CARTESIAN_POINT('Ctrl Pts',(5.07389186228029,0.149680441629337,2.21302887025649));
#45090=CARTESIAN_POINT('Ctrl Pts',(5.03086461164817,1.14248345247706,2.24417819256036));
#45091=CARTESIAN_POINT('Ctrl Pts',(4.40300813596794,2.92992503348825,2.3017848115487));
#45092=CARTESIAN_POINT('Ctrl Pts',(2.46536820371062,4.67898503603904,2.38115670160211));
#45093=CARTESIAN_POINT('Ctrl Pts',(-0.0728299659737919,5.28825464055465,
2.46052859165552));
#45094=CARTESIAN_POINT('Ctrl Pts',(-2.59328691715172,4.60931711999155,2.53990048170891));
#45095=CARTESIAN_POINT('Ctrl Pts',(-4.4820249154556,2.80756015154502,2.61927237176233));
#45096=CARTESIAN_POINT('Ctrl Pts',(-5.27895156514789,0.321887744613165,
2.69864426181572));
#45097=CARTESIAN_POINT('Ctrl Pts',(-4.7899372983315,-2.2421958044211,2.77801615186913));
#45098=CARTESIAN_POINT('Ctrl Pts',(-3.13410490798781,-4.26008541851404,
2.85738804192253));
#45099=CARTESIAN_POINT('Ctrl Pts',(-0.714811499281904,-5.2402276541964,
2.93675993197593));
#45100=CARTESIAN_POINT('Ctrl Pts',(1.8786084084407,-4.94386203236353,3.01613182202934));
#45101=CARTESIAN_POINT('Ctrl Pts',(4.01440346609632,-3.44318256249998,3.09550371208274));
#45102=CARTESIAN_POINT('Ctrl Pts',(4.9490470546202,-1.55481288423713,3.15957205295199));
#45103=CARTESIAN_POINT('Ctrl Pts',(5.07335471749433,-0.355694245953322,
3.19718309713677));
#45104=CARTESIAN_POINT('Ctrl Pts',(5.0732079990561,-5.95000919163813E-5,
3.20833684463708));
#45105=CARTESIAN_POINT('Origin',(0.,0.,-2.20833684463713));
#45106=CARTESIAN_POINT('',(5.07361762168166,-0.000130982038957922,1.20833684463708));
#45107=CARTESIAN_POINT('',(5.07338480805012,-0.000117445791330803,1.29166315536292));
#45108=CARTESIAN_POINT('',(5.0736,-1.85409460923845E-12,-2.20833684463713));
#45109=CARTESIAN_POINT('Ctrl Pts',(5.07338480805012,-0.000117445791331001,
1.29166315536292));
#45110=CARTESIAN_POINT('Ctrl Pts',(5.07289281667254,0.576157106237108,1.30973861823942));
#45111=CARTESIAN_POINT('Ctrl Pts',(4.83135991405541,1.99633436079896,1.35427137780039));
#45112=CARTESIAN_POINT('Ctrl Pts',(3.53232089954478,3.93619745533352,1.42526143404583));
#45113=CARTESIAN_POINT('Ctrl Pts',(1.21943810235538,5.14625223481536,1.50463332409923));
#45114=CARTESIAN_POINT('Ctrl Pts',(-1.39049711694202,5.10269135980955,1.58400521415263));
#45115=CARTESIAN_POINT('Ctrl Pts',(-3.66171031660135,3.81612616476449,1.66337710420604));
#45116=CARTESIAN_POINT('Ctrl Pts',(-5.04093898807,1.59996108251987,1.74274899425944));
#45117=CARTESIAN_POINT('Ctrl Pts',(-5.19220608004013,-1.00595097780601,
1.82212088431284));
#45118=CARTESIAN_POINT('Ctrl Pts',(-4.07866326363067,-3.3668156066614,1.90149277436625));
#45119=CARTESIAN_POINT('Ctrl Pts',(-1.97156710418735,-4.90753140600723,
1.98086466441965));
#45120=CARTESIAN_POINT('Ctrl Pts',(0.61579843785608,-5.25278341751101,2.06023655447306));
#45121=CARTESIAN_POINT('Ctrl Pts',(3.0531568434793,-4.31846901533485,2.13960844452646));
#45122=CARTESIAN_POINT('Ctrl Pts',(4.69919647653223,-2.38798317189229,2.21675064482308));
#45123=CARTESIAN_POINT('Ctrl Pts',(5.07342473837308,-0.772094669942323,
2.26743554843524));
#45124=CARTESIAN_POINT('Ctrl Pts',(5.07395289332891,7.08096438841854E-5,
2.29166315536292));
#45125=CARTESIAN_POINT('Ctrl Pts',(5.07361762168166,-0.000130982038957766,
1.20833684463708));
#45126=CARTESIAN_POINT('Ctrl Pts',(5.07294327622754,0.654560436527497,1.2288746433762));
#45127=CARTESIAN_POINT('Ctrl Pts',(4.78166373276894,2.15322402421039,1.2758697387998));
#45128=CARTESIAN_POINT('Ctrl Pts',(3.34588798700519,4.09584848370755,1.34932213090786));
#45129=CARTESIAN_POINT('Ctrl Pts',(0.979352771366438,5.19728867487042,1.42869402096127));
#45130=CARTESIAN_POINT('Ctrl Pts',(-1.6257506180571,5.03268082057239,1.50806591101467));
#45131=CARTESIAN_POINT('Ctrl Pts',(-3.83482475204895,3.64212307300266,1.58743780106807));
#45132=CARTESIAN_POINT('Ctrl Pts',(-5.10974406648874,1.36435219862418,1.66680969112148));
#45133=CARTESIAN_POINT('Ctrl Pts',(-5.13994103560183,-1.2457718471981,1.74618158117488));
#45134=CARTESIAN_POINT('Ctrl Pts',(-3.91805974601548,-3.55242863073578,
1.82555347122828));
#45135=CARTESIAN_POINT('Ctrl Pts',(-1.74174777450957,-4.99372166181597,
1.90492536128169));
#45136=CARTESIAN_POINT('Ctrl Pts',(0.858850099431454,-5.21855515011689,
1.98429725133509));
#45137=CARTESIAN_POINT('Ctrl Pts',(3.25023399025869,-4.17216015459491,2.0636691413885));
#45138=CARTESIAN_POINT('Ctrl Pts',(4.75530658628425,-2.2313729735679,2.13834900582249));
#45139=CARTESIAN_POINT('Ctrl Pts',(5.0730413237258,-0.693650010686127,2.18657157357202));
#45140=CARTESIAN_POINT('Ctrl Pts',(5.07374102492394,0.000121394267758555,
2.20833684463708));
#45141=CARTESIAN_POINT('Origin',(0.,0.,-2.20833684463713));
#45142=CARTESIAN_POINT('',(5.07327550687406,0.000108476183186546,0.208336844637077));
#45143=CARTESIAN_POINT('',(5.07346622253939,0.000127574377019038,0.291663155362924));
#45144=CARTESIAN_POINT('',(5.0736,-1.85409460923845E-12,-2.20833684463713));
#45145=CARTESIAN_POINT('',(1.3130361863565,-4.90075024188322,0.));
#45146=CARTESIAN_POINT('Ctrl Pts',(1.3130361863565,-4.90075024188322,0.));
#45147=CARTESIAN_POINT('Ctrl Pts',(2.12771778283771,-4.68247622999897,0.0264572966844678));
#45148=CARTESIAN_POINT('Ctrl Pts',(3.64531650851188,-3.8320815322798,0.0793718900534037));
#45149=CARTESIAN_POINT('Ctrl Pts',(4.86042636846397,-1.89775322538081,0.148817504932429));
#45150=CARTESIAN_POINT('Ctrl Pts',(5.07294944175775,-0.526932428119567,
0.191805823126987));
#45151=CARTESIAN_POINT('Ctrl Pts',(5.07327550687406,0.000108476183186372,
0.208336844637077));
#45152=CARTESIAN_POINT('',(-1.31317395760259,-4.90115117757553,2.08166817117217E-16));
#45153=CARTESIAN_POINT('Origin',(0.,0.,0.));
#45154=CARTESIAN_POINT('Ctrl Pts',(-1.31317395760259,-4.90115117757553,
2.32154790183459E-16));
#45155=CARTESIAN_POINT('Ctrl Pts',(-0.533836595431888,-5.10962665469163,
0.025313101045988));
#45156=CARTESIAN_POINT('Ctrl Pts',(1.16384881260007,-5.14969078544564,0.0770834987764434));
#45157=CARTESIAN_POINT('Ctrl Pts',(3.46369715057722,-3.99673439595713,0.155311193191368));
#45158=CARTESIAN_POINT('Ctrl Pts',(4.8133239766203,-2.05483010796368,0.22721914393302));
#45159=CARTESIAN_POINT('Ctrl Pts',(5.0728909576883,-0.605381739016801,0.272669797990206));
#45160=CARTESIAN_POINT('Ctrl Pts',(5.07346622253938,0.000127574377019116,
0.291663155362924));
#45161=CARTESIAN_POINT('Origin',(4.45462538595717E-16,-1.65775395963113E-16,
40.));
#45162=CARTESIAN_POINT('Ctrl Pts',(3.43378788736169,2.9358415841302,40.));
#45163=CARTESIAN_POINT('Ctrl Pts',(3.52814292550769,2.83820823955091,40.));
#45164=CARTESIAN_POINT('Ctrl Pts',(3.61787392647867,2.73637499985595,40.));
#45165=CARTESIAN_POINT('Ctrl Pts',(3.7028436241849,2.63075402506017,40.));
#45166=CARTESIAN_POINT('Ctrl Pts',(3.78889648523297,2.52378663182211,40.));
#45167=CARTESIAN_POINT('Ctrl Pts',(3.87006637156126,2.41293377092847,40.));
#45168=CARTESIAN_POINT('Ctrl Pts',(3.94617716449749,2.2985820569619,40.));
#45169=CARTESIAN_POINT('Ctrl Pts',(3.98452054291682,2.24097352507873,40.));
#45170=CARTESIAN_POINT('Ctrl Pts',(4.02157936104048,2.18247639180456,40.));
#45171=CARTESIAN_POINT('Ctrl Pts',(4.0573273224032,2.12313686354418,40.));
#45172=CARTESIAN_POINT('Ctrl Pts',(4.07057108419318,2.10115299237913,40.));
#45173=CARTESIAN_POINT('Ctrl Pts',(4.08363549665298,2.07905229886435,40.));
#45174=CARTESIAN_POINT('Ctrl Pts',(4.09651028112638,2.05685278711327,40.));
#45175=CARTESIAN_POINT('Ctrl Pts',(4.16636767341313,1.93640028523473,40.));
#45176=CARTESIAN_POINT('Ctrl Pts',(4.23070798356748,1.81293936852798,40.));
#45177=CARTESIAN_POINT('Ctrl Pts',(4.28936081037521,1.68687424953695,40.));
#45178=CARTESIAN_POINT('Ctrl Pts',(4.34350578332916,1.57049806053275,40.));
#45179=CARTESIAN_POINT('Ctrl Pts',(4.39280381894615,1.45190174917925,40.));
#45180=CARTESIAN_POINT('Ctrl Pts',(4.4370895395389,1.33137973638483,40.));
#45181=CARTESIAN_POINT('Ctrl Pts',(4.45048806014006,1.29491613932226,40.));
#45182=CARTESIAN_POINT('Ctrl Pts',(4.46342755329992,1.25827614359673,40.));
#45183=CARTESIAN_POINT('Ctrl Pts',(4.47590283035858,1.22146759434429,40.));
#45184=CARTESIAN_POINT('Ctrl Pts',(4.48543045669819,1.19335614625929,40.));
#45185=CARTESIAN_POINT('Ctrl Pts',(4.49468731429383,1.16514638329788,40.));
#45186=CARTESIAN_POINT('Ctrl Pts',(4.50367097326761,1.13684175481395,40.));
#45187=CARTESIAN_POINT('Ctrl Pts',(4.50984234488601,1.11739774192287,40.));
#45188=CARTESIAN_POINT('Ctrl Pts',(4.51588427541961,1.09791040265649,40.));
#45189=CARTESIAN_POINT('Ctrl Pts',(4.52179265714445,1.0783924896528,40.));
#45190=CARTESIAN_POINT('Ctrl Pts',(4.53324480098953,1.04056115821829,40.));
#45191=CARTESIAN_POINT('Ctrl Pts',(4.54419899621228,1.00260320591424,40.));
#45192=CARTESIAN_POINT('Ctrl Pts',(4.5546518960517,0.964527761093808,40.));
#45193=CARTESIAN_POINT('Ctrl Pts',(4.59117593379611,0.831486307992675,40.));
#45194=CARTESIAN_POINT('Ctrl Pts',(4.62158314424656,0.697012525339414,40.));
#45195=CARTESIAN_POINT('Ctrl Pts',(4.64596931935994,0.561539349137144,40.));
#45196=CARTESIAN_POINT('Ctrl Pts',(4.67073918176772,0.42393466456182,40.));
#45197=CARTESIAN_POINT('Ctrl Pts',(4.68929722659476,0.28529820513645,40.));
#45198=CARTESIAN_POINT('Ctrl Pts',(4.70169535323682,0.146060437529888,40.));
#45199=CARTESIAN_POINT('Ctrl Pts',(4.71417778478848,0.00587587951314419,
40.));
#45200=CARTESIAN_POINT('Ctrl Pts',(4.7204163646451,-0.134918963378981,40.));
#45201=CARTESIAN_POINT('Ctrl Pts',(4.72041312729179,-0.275897046739804,
40.));
#45202=CARTESIAN_POINT('Ctrl Pts',(4.72041101510801,-0.367877004659711,
40.));
#45203=CARTESIAN_POINT('Ctrl Pts',(4.71775084452937,-0.459935190334389,
40.));
#45204=CARTESIAN_POINT('Ctrl Pts',(4.71242122767243,-0.55195336772424,40.));
#45205=CARTESIAN_POINT('Ctrl Pts',(4.71074982773409,-0.580810822236322,
40.));
#45206=CARTESIAN_POINT('Ctrl Pts',(4.70881582061262,-0.609664336690085,
40.));
#45207=CARTESIAN_POINT('Ctrl Pts',(4.70661866095158,-0.638510242454293,
40.));
#45208=CARTESIAN_POINT('Ctrl Pts',(4.70521659891363,-0.65691752988966,40.));
#45209=CARTESIAN_POINT('Ctrl Pts',(4.70370712995809,-0.675324500804579,
40.));
#45210=CARTESIAN_POINT('Ctrl Pts',(4.70209092940465,-0.693720810758238,
40.));
#45211=CARTESIAN_POINT('Ctrl Pts',(4.68953110086222,-0.836682337618008,
40.));
#45212=CARTESIAN_POINT('Ctrl Pts',(4.67055276432277,-0.978761795279802,
40.));
#45213=CARTESIAN_POINT('Ctrl Pts',(4.64522498551854,-1.11951304986637,40.));
#45214=CARTESIAN_POINT('Ctrl Pts',(4.63006091029742,-1.20378268237205,40.));
#45215=CARTESIAN_POINT('Ctrl Pts',(4.61261985737539,-1.28757653832611,40.));
#45216=CARTESIAN_POINT('Ctrl Pts',(4.59290787692688,-1.37080047994428,40.));
#45217=CARTESIAN_POINT('Ctrl Pts',(4.56017758990635,-1.5089876856012,40.));
#45218=CARTESIAN_POINT('Ctrl Pts',(4.52118921321033,-1.64560413309505,40.));
#45219=CARTESIAN_POINT('Ctrl Pts',(4.47619425969956,-1.78030079004358,40.));
#45220=CARTESIAN_POINT('Ctrl Pts',(4.43085717885509,-1.91602163758472,40.));
#45221=CARTESIAN_POINT('Ctrl Pts',(4.3794215892058,-2.04979410792511,40.));
#45222=CARTESIAN_POINT('Ctrl Pts',(4.32209322112883,-2.18124988516394,40.));
#45223=CARTESIAN_POINT('Ctrl Pts',(4.29589299313303,-2.24132784395735,40.));
#45224=CARTESIAN_POINT('Ctrl Pts',(4.26846127047772,-2.30092169976294,40.));
#45225=CARTESIAN_POINT('Ctrl Pts',(4.23981435864377,-2.35999488119432,40.));
#45226=CARTESIAN_POINT('Ctrl Pts',(4.22808815540088,-2.38417564230685,40.));
#45227=CARTESIAN_POINT('Ctrl Pts',(4.21615831686625,-2.40826914901153,40.));
#45228=CARTESIAN_POINT('Ctrl Pts',(4.20402586547368,-2.43227283763382,40.));
#45229=CARTESIAN_POINT('Ctrl Pts',(4.19226175293326,-2.45554777896271,40.));
#45230=CARTESIAN_POINT('Ctrl Pts',(4.18030467857245,-2.47874278381504,40.));
#45231=CARTESIAN_POINT('Ctrl Pts',(4.16817016036066,-2.50182817485463,40.));
#45232=CARTESIAN_POINT('Ctrl Pts',(4.10062993280007,-2.63032050861895,40.));
#45233=CARTESIAN_POINT('Ctrl Pts',(4.02752679248241,-2.75556160907446,40.));
#45234=CARTESIAN_POINT('Ctrl Pts',(3.94914189359867,-2.87720021634157,40.));
#45235=CARTESIAN_POINT('Ctrl Pts',(3.87013649228652,-2.99980172656921,40.));
#45236=CARTESIAN_POINT('Ctrl Pts',(3.78576510402317,-3.11874421706065,40.));
#45237=CARTESIAN_POINT('Ctrl Pts',(3.69626453833047,-3.23365468399741,40.));
#45238=CARTESIAN_POINT('Ctrl Pts',(3.6256051940776,-3.3243747613366,40.));
#45239=CARTESIAN_POINT('Ctrl Pts',(3.55174784325694,-3.41258159925288,40.));
#45240=CARTESIAN_POINT('Ctrl Pts',(3.4747885470066,-3.49808125449705,40.));
#45241=CARTESIAN_POINT('Ctrl Pts',(3.37754842452615,-3.60611234824477,40.));
#45242=CARTESIAN_POINT('Ctrl Pts',(3.27535698426899,-3.70982288325437,40.));
#45243=CARTESIAN_POINT('Ctrl Pts',(3.16857103825032,-3.80899091582305,40.));
#45244=CARTESIAN_POINT('Ctrl Pts',(3.13709749914945,-3.83821919039451,40.));
#45245=CARTESIAN_POINT('Ctrl Pts',(3.10522459675968,-3.86705262006651,40.));
#45246=CARTESIAN_POINT('Ctrl Pts',(3.07296088810501,-3.89548488187744,40.));
#45247=CARTESIAN_POINT('Ctrl Pts',(3.05413623645007,-3.91207402945752,40.));
#45248=CARTESIAN_POINT('Ctrl Pts',(3.03517853882814,-3.92852660249152,40.));
#45249=CARTESIAN_POINT('Ctrl Pts',(3.01608945850777,-3.94484129509693,40.));
#45250=CARTESIAN_POINT('Ctrl Pts',(3.00324987792049,-3.95581478396849,40.));
#45251=CARTESIAN_POINT('Ctrl Pts',(2.99035184084321,-3.96672500977969,40.));
#45252=CARTESIAN_POINT('Ctrl Pts',(2.97740348730282,-3.97756535219416,40.));
#45253=CARTESIAN_POINT('Ctrl Pts',(2.86172546572695,-4.07441082060052,40.));
#45254=CARTESIAN_POINT('Ctrl Pts',(2.74187291014631,-4.16582105105552,40.));
#45255=CARTESIAN_POINT('Ctrl Pts',(2.61830752500134,-4.25161650299712,40.));
#45256=CARTESIAN_POINT('Ctrl Pts',(2.49666368456262,-4.33607776416752,40.));
#45257=CARTESIAN_POINT('Ctrl Pts',(2.37142082394795,-4.41509790443455,40.));
#45258=CARTESIAN_POINT('Ctrl Pts',(2.24297630552737,-4.4884725438774,40.));
#45259=CARTESIAN_POINT('Ctrl Pts',(2.11148832986889,-4.56358577505025,40.));
#45260=CARTESIAN_POINT('Ctrl Pts',(1.97664462468232,-4.63278348201276,40.));
#45261=CARTESIAN_POINT('Ctrl Pts',(1.83883549494666,-4.69580305762063,40.));
#45262=CARTESIAN_POINT('Ctrl Pts',(1.701026365211,-4.7588226332285,40.));
#45263=CARTESIAN_POINT('Ctrl Pts',(1.56025109502399,-4.81566463443687,40.));
#45264=CARTESIAN_POINT('Ctrl Pts',(1.41687422066896,-4.86601447289837,40.));
#45265=CARTESIAN_POINT('Ctrl Pts',(1.38245545626202,-4.8781013539643,40.));
#45266=CARTESIAN_POINT('Ctrl Pts',(1.34788667776073,-4.88981384734562,40.));
#45267=CARTESIAN_POINT('Ctrl Pts',(1.31317395760249,-4.90115117757556,40.));
#45268=CARTESIAN_POINT('Ctrl Pts',(-1.31303618635638,-4.90075024188325,
40.));
#45269=CARTESIAN_POINT('Ctrl Pts',(-1.45437915259461,-4.85452838596849,
40.));
#45270=CARTESIAN_POINT('Ctrl Pts',(-1.59345673045457,-4.80203124199391,
40.));
#45271=CARTESIAN_POINT('Ctrl Pts',(-1.72991111250498,-4.74351762389719,
40.));
#45272=CARTESIAN_POINT('Ctrl Pts',(-1.86679415923463,-4.68482018816886,
40.));
#45273=CARTESIAN_POINT('Ctrl Pts',(-2.001038164382,-4.62006797676633,40.));
#45274=CARTESIAN_POINT('Ctrl Pts',(-2.1322557155067,-4.54947707893507,40.));
#45275=CARTESIAN_POINT('Ctrl Pts',(-2.19315308373731,-4.5167162183481,40.));
#45276=CARTESIAN_POINT('Ctrl Pts',(-2.25339817251141,-4.48269720490963,
40.));
#45277=CARTESIAN_POINT('Ctrl Pts',(-2.31294973629581,-4.44743875160342,
40.));
#45278=CARTESIAN_POINT('Ctrl Pts',(-2.33562884151057,-4.43401122558351,
40.));
#45279=CARTESIAN_POINT('Ctrl Pts',(-2.35820900730168,-4.42040290103079,
40.));
#45280=CARTESIAN_POINT('Ctrl Pts',(-2.38068262652232,-4.40661797963936,
40.));
#45281=CARTESIAN_POINT('Ctrl Pts',(-2.50650561756839,-4.32944037759069,
40.));
#45282=CARTESIAN_POINT('Ctrl Pts',(-2.62877991395688,-4.24686153480494,
40.));
#45283=CARTESIAN_POINT('Ctrl Pts',(-2.74713717330506,-4.15910670751388,
40.));
#45284=CARTESIAN_POINT('Ctrl Pts',(-2.86467013316358,-4.07196304898213,
40.));
#45285=CARTESIAN_POINT('Ctrl Pts',(-2.97834099898066,-3.97971476207056,
40.));
#45286=CARTESIAN_POINT('Ctrl Pts',(-3.08775357309594,-3.88254556003572,
40.));
#45287=CARTESIAN_POINT('Ctrl Pts',(-3.14513584653695,-3.8315844180802,40.));
#45288=CARTESIAN_POINT('Ctrl Pts',(-3.2013462077245,-3.77926917964798,40.));
#45289=CARTESIAN_POINT('Ctrl Pts',(-3.25632275100474,-3.72562292402786,
40.));
#45290=CARTESIAN_POINT('Ctrl Pts',(-3.27574922848208,-3.70666651617886,
40.));
#45291=CARTESIAN_POINT('Ctrl Pts',(-3.29502416873062,-3.6875411953518,40.));
#45292=CARTESIAN_POINT('Ctrl Pts',(-3.31412620910246,-3.66826697432299,
40.));
#45293=CARTESIAN_POINT('Ctrl Pts',(-3.34404060290358,-3.63808294021764,
40.));
#45294=CARTESIAN_POINT('Ctrl Pts',(-3.37353997543889,-3.60752519082335,
40.));
#45295=CARTESIAN_POINT('Ctrl Pts',(-3.40261591802411,-3.57659932769541,
40.));
#45296=CARTESIAN_POINT('Ctrl Pts',(-3.50164274205642,-3.47127204562902,
40.));
#45297=CARTESIAN_POINT('Ctrl Pts',(-3.59576101414824,-3.36167756876611,
40.));
#45298=CARTESIAN_POINT('Ctrl Pts',(-3.68480291336662,-3.24822038520781,
40.));
#45299=CARTESIAN_POINT('Ctrl Pts',(-3.77450749603108,-3.13391881043548,
40.));
#45300=CARTESIAN_POINT('Ctrl Pts',(-3.85906025603562,-3.01569612122462,
40.));
#45301=CARTESIAN_POINT('Ctrl Pts',(-3.93824649098464,-2.893935566612,40.));
#45302=CARTESIAN_POINT('Ctrl Pts',(-4.01670520549023,-2.7732936823433,40.));
#45303=CARTESIAN_POINT('Ctrl Pts',(-4.08989581732523,-2.64917791019356,
40.));
#45304=CARTESIAN_POINT('Ctrl Pts',(-4.15756259897637,-2.52194215997081,
40.));
#45305=CARTESIAN_POINT('Ctrl Pts',(-4.20177691057784,-2.43880474793609,
40.));
#45306=CARTESIAN_POINT('Ctrl Pts',(-4.24363187369716,-2.35433490941293,
40.));
#45307=CARTESIAN_POINT('Ctrl Pts',(-4.2830443332661,-2.26862918510464,40.));
#45308=CARTESIAN_POINT('Ctrl Pts',(-4.30136127527663,-2.22879744663171,
40.));
#45309=CARTESIAN_POINT('Ctrl Pts',(-4.31915051766851,-2.18869875186795,
40.));
#45310=CARTESIAN_POINT('Ctrl Pts',(-4.33640298127534,-2.14834275431588,
40.));
#45311=CARTESIAN_POINT('Ctrl Pts',(-4.3436590160159,-2.13136984384344,40.));
#45312=CARTESIAN_POINT('Ctrl Pts',(-4.35081962128211,-2.11435240712678,
40.));
#45313=CARTESIAN_POINT('Ctrl Pts',(-4.35787943356684,-2.09730289812436,
40.));
#45314=CARTESIAN_POINT('Ctrl Pts',(-4.41262610226673,-1.96508920982698,
40.));
#45315=CARTESIAN_POINT('Ctrl Pts',(-4.46139597719794,-1.83076168016892,
40.));
#45316=CARTESIAN_POINT('Ctrl Pts',(-4.50399603348697,-1.69468832090704,
40.));
#45317=CARTESIAN_POINT('Ctrl Pts',(-4.527154798591,-1.62071445235899,40.));
#45318=CARTESIAN_POINT('Ctrl Pts',(-4.54848933959424,-1.54622425456777,
40.));
#45319=CARTESIAN_POINT('Ctrl Pts',(-4.56796247846724,-1.47127487515815,
40.));
#45320=CARTESIAN_POINT('Ctrl Pts',(-4.60386684913915,-1.33308398988268,
40.));
#45321=CARTESIAN_POINT('Ctrl Pts',(-4.633446346586,-1.19333212031901,40.));
#45322=CARTESIAN_POINT('Ctrl Pts',(-4.65669710227076,-1.05245525970538,
40.));
#45323=CARTESIAN_POINT('Ctrl Pts',(-4.67988218362711,-0.911976321350021,
40.));
#45324=CARTESIAN_POINT('Ctrl Pts',(-4.6967741641367,-0.770377936579903,
40.));
#45325=CARTESIAN_POINT('Ctrl Pts',(-4.70731777033656,-0.628096038990404,
40.));
#45326=CARTESIAN_POINT('Ctrl Pts',(-4.71196239382317,-0.565418637090442,
40.));
#45327=CARTESIAN_POINT('Ctrl Pts',(-4.71537442348699,-0.502608716141042,
40.));
#45328=CARTESIAN_POINT('Ctrl Pts',(-4.71754599609844,-0.439704378705418,
40.));
#45329=CARTESIAN_POINT('Ctrl Pts',(-4.71847271903558,-0.412859827415833,
40.));
#45330=CARTESIAN_POINT('Ctrl Pts',(-4.71917350957111,-0.385998089715844,
40.));
#45331=CARTESIAN_POINT('Ctrl Pts',(-4.71964765055488,-0.359122168611144,
40.));
#45332=CARTESIAN_POINT('Ctrl Pts',(-4.72007766112019,-0.334747709487924,
40.));
#45333=CARTESIAN_POINT('Ctrl Pts',(-4.72032117948226,-0.310357499793734,
40.));
#45334=CARTESIAN_POINT('Ctrl Pts',(-4.72037779701569,-0.28598141917232,
40.));
#45335=CARTESIAN_POINT('Ctrl Pts',(-4.72070503729545,-0.145091575346323,
40.));
#45336=CARTESIAN_POINT('Ctrl Pts',(-4.71479792201471,-0.00450394063596596,
40.));
#45337=CARTESIAN_POINT('Ctrl Pts',(-4.7026779767235,0.135364936808135,40.));
#45338=CARTESIAN_POINT('Ctrl Pts',(-4.6906385436001,0.274304672555548,40.));
#45339=CARTESIAN_POINT('Ctrl Pts',(-4.67246842821977,0.412535934949348,
40.));
#45340=CARTESIAN_POINT('Ctrl Pts',(-4.64813815685378,0.549644620304502,
40.));
#45341=CARTESIAN_POINT('Ctrl Pts',(-4.62922788638654,0.656209906177027,
40.));
#45342=CARTESIAN_POINT('Ctrl Pts',(-4.60659531784607,0.762097046731738,
40.));
#45343=CARTESIAN_POINT('Ctrl Pts',(-4.58020591978812,0.867104757427845,
40.));
#45344=CARTESIAN_POINT('Ctrl Pts',(-4.54608550784896,1.00287543085781,40.));
#45345=CARTESIAN_POINT('Ctrl Pts',(-4.5056856677851,1.13717725960422,40.));
#45346=CARTESIAN_POINT('Ctrl Pts',(-4.45916773762384,1.26960241773677,40.));
#45347=CARTESIAN_POINT('Ctrl Pts',(-4.44595800567878,1.30720729043101,40.));
#45348=CARTESIAN_POINT('Ctrl Pts',(-4.43225465907289,1.34466063579127,40.));
#45349=CARTESIAN_POINT('Ctrl Pts',(-4.41806080497834,1.381952618119,40.));
#45350=CARTESIAN_POINT('Ctrl Pts',(-4.41034395548629,1.40222735202608,40.));
#45351=CARTESIAN_POINT('Ctrl Pts',(-4.40248211604979,1.42245438558641,40.));
#45352=CARTESIAN_POINT('Ctrl Pts',(-4.39447575604619,1.44263210700853,40.));
#45353=CARTESIAN_POINT('Ctrl Pts',(-4.38774337392406,1.45959913458491,40.));
#45354=CARTESIAN_POINT('Ctrl Pts',(-4.38091020364865,1.47652766568619,40.));
#45355=CARTESIAN_POINT('Ctrl Pts',(-4.37398035764513,1.49340802308437,40.));
#45356=CARTESIAN_POINT('Ctrl Pts',(-4.32139777601335,1.62149352028206,40.));
#45357=CARTESIAN_POINT('Ctrl Pts',(-4.26319329324451,1.74695839038908,40.));
#45358=CARTESIAN_POINT('Ctrl Pts',(-4.19959993118347,1.86944841739778,40.));
#45359=CARTESIAN_POINT('Ctrl Pts',(-4.13606105752427,1.99183349185173,40.));
#45360=CARTESIAN_POINT('Ctrl Pts',(-4.06714208355231,2.1112494937512,40.));
#45361=CARTESIAN_POINT('Ctrl Pts',(-3.99303011697524,2.22731770598438,40.));
#45362=CARTESIAN_POINT('Ctrl Pts',(-3.9202059518248,2.34136906700981,40.));
#45363=CARTESIAN_POINT('Ctrl Pts',(-3.84236718991447,2.45218850722107,40.));
#45364=CARTESIAN_POINT('Ctrl Pts',(-3.75965485123955,2.55938335127685,40.));
#45365=CARTESIAN_POINT('Ctrl Pts',(-3.67819754057762,2.66495168429094,40.));
#45366=CARTESIAN_POINT('Ctrl Pts',(-3.59201299654429,2.76700506575445,40.));
#45367=CARTESIAN_POINT('Ctrl Pts',(-3.50120707213067,2.86512829543056,40.));
#45368=CARTESIAN_POINT('Ctrl Pts',(-3.47910751146495,2.88900867857677,40.));
#45369=CARTESIAN_POINT('Ctrl Pts',(-3.45673410716774,2.91265607078183,40.));
#45370=CARTESIAN_POINT('Ctrl Pts',(-3.43409108914464,2.93606647242288,40.));
#45371=CARTESIAN_POINT('Origin',(0.,0.,-2.20833684463713));
#45372=CARTESIAN_POINT('Ctrl Pts',(5.07346622253938,0.000127574377019116,
0.291663155362924));
#45373=CARTESIAN_POINT('Ctrl Pts',(5.07369228799229,0.238078384188188,0.299127094674674));
#45374=CARTESIAN_POINT('Ctrl Pts',(4.99899491470862,1.31934885093053,0.333048330670892));
#45375=CARTESIAN_POINT('Ctrl Pts',(4.24398161873799,3.15587819282154,0.393426863351577));
#45376=CARTESIAN_POINT('Ctrl Pts',(2.21764149317933,4.80135391043019,0.472798753404982));
#45377=CARTESIAN_POINT('Ctrl Pts',(-0.348912918530393,5.27723479734493,
0.552170643458385));
#45378=CARTESIAN_POINT('Ctrl Pts',(-2.83047200092439,4.46759066254957,0.631542533511789));
#45379=CARTESIAN_POINT('Ctrl Pts',(-4.62253485344812,2.56965255248809,0.710914423565193));
#45380=CARTESIAN_POINT('Ctrl Pts',(-5.28855819093304,0.045752121671659,
0.790286313618596));
#45381=CARTESIAN_POINT('Ctrl Pts',(-4.66630059499956,-2.48929308216644,
0.869658203672));
#45382=CARTESIAN_POINT('Ctrl Pts',(-2.90734243084918,-4.4179521825598,0.949030093725403));
#45383=CARTESIAN_POINT('Ctrl Pts',(-0.440162123945536,-5.27040781417518,
1.02840198377881));
#45384=CARTESIAN_POINT('Ctrl Pts',(2.1342407222512,-4.83900381899044,1.10777387383221));
#45385=CARTESIAN_POINT('Ctrl Pts',(4.18874724188064,-3.228829177505,1.18714576388562));
#45386=CARTESIAN_POINT('Ctrl Pts',(4.9873788651986,-1.37792482956251,1.24844219106252));
#45387=CARTESIAN_POINT('Ctrl Pts',(5.07361295102991,-0.267343660459586,
1.28328132155495));
#45388=CARTESIAN_POINT('Ctrl Pts',(5.07338480805012,-0.000117445791331001,
1.29166315536292));
#45389=CARTESIAN_POINT('Ctrl Pts',(5.07327550687406,0.000108476183186372,
0.208336844637077));
#45390=CARTESIAN_POINT('Ctrl Pts',(5.07347129707779,0.316577306682802,0.218263119811455));
#45391=CARTESIAN_POINT('Ctrl Pts',(4.96661393653962,1.47641857544861,0.254646691670301));
#45392=CARTESIAN_POINT('Ctrl Pts',(4.09299916691648,3.34943642687043,0.317487560213614));
#45393=CARTESIAN_POINT('Ctrl Pts',(1.99247705733062,4.89905044646781,0.396859450267019));
#45394=CARTESIAN_POINT('Ctrl Pts',(-0.593383061700938,5.2553763257097,0.476231340320422));
#45395=CARTESIAN_POINT('Ctrl Pts',(-3.03470961035893,4.33144609848054,0.555603230373826));
#45396=CARTESIAN_POINT('Ctrl Pts',(-4.73678060915323,2.35241593705463,0.634975120427228));
#45397=CARTESIAN_POINT('Ctrl Pts',(-5.28498604656423,-0.199673823356779,
0.714347010480634));
#45398=CARTESIAN_POINT('Ctrl Pts',(-4.5457786161601,-2.703114858517,0.793718900534037));
#45399=CARTESIAN_POINT('Ctrl Pts',(-2.69923061743508,-4.5480876646044,0.87309079058744));
#45400=CARTESIAN_POINT('Ctrl Pts',(-0.195155463808127,-5.28515396379925,
0.952462680640845));
#45401=CARTESIAN_POINT('Ctrl Pts',(2.35645883694709,-4.73476973691702,1.03183457069425));
#45402=CARTESIAN_POINT('Ctrl Pts',(4.33404513553918,-3.03100540392648,1.11120646074765));
#45403=CARTESIAN_POINT('Ctrl Pts',(5.01734225874463,-1.22080114526538,1.17004055206193));
#45404=CARTESIAN_POINT('Ctrl Pts',(5.0738119846015,-0.188829126190742,1.20241734669174));
#45405=CARTESIAN_POINT('Ctrl Pts',(5.07361762168166,-0.000130982038957766,
1.20833684463708));
#45406=CARTESIAN_POINT('Ctrl Pts',(-3.43378788736187,2.93584158412999,-1.38777878078145E-15));
#45407=CARTESIAN_POINT('Ctrl Pts',(-3.92183073605352,2.36502208507736,0.0264572966844665));
#45408=CARTESIAN_POINT('Ctrl Pts',(-4.60729903172261,0.975909964327098,
0.0793718900534022));
#45409=CARTESIAN_POINT('Ctrl Pts',(-4.51258247789853,-1.34695556252418,
0.158743780106806));
#45410=CARTESIAN_POINT('Ctrl Pts',(-3.3188765366808,-3.34104229843846,0.23811567016021));
#45411=CARTESIAN_POINT('Ctrl Pts',(-1.31656588610641,-4.52159485055713,
0.317487560213613));
#45412=CARTESIAN_POINT('Ctrl Pts',(1.00638734295355,-4.60052063353559,0.396859450267017));
#45413=CARTESIAN_POINT('Ctrl Pts',(3.08422378627015,-3.55886290155616,0.476231340320421));
#45414=CARTESIAN_POINT('Ctrl Pts',(4.41073058968579,-1.65022475069956,0.555603230373823));
#45415=CARTESIAN_POINT('Ctrl Pts',(4.66280353786907,0.660378394082181,0.634975120427229));
#45416=CARTESIAN_POINT('Ctrl Pts',(3.77902238214553,2.81012864743368,0.71434701048063));
#45417=CARTESIAN_POINT('Ctrl Pts',(1.9746826426622,4.27533046137772,0.793718900534036));
#45418=CARTESIAN_POINT('Ctrl Pts',(-0.310686955552407,4.69907511544172,
0.873090790587439));
#45419=CARTESIAN_POINT('Ctrl Pts',(-2.52037308462949,3.97813341921581,0.952462680640842));
#45420=CARTESIAN_POINT('Ctrl Pts',(-4.11610234038262,2.28812831500376,1.03183457069425));
#45421=CARTESIAN_POINT('Ctrl Pts',(-4.70915794841686,0.0407396420060994,
1.11120646074765));
#45422=CARTESIAN_POINT('Ctrl Pts',(-4.15507322474362,-2.21657281259016,
1.19057835080105));
#45423=CARTESIAN_POINT('Ctrl Pts',(-2.58882179654858,-3.93393319787912,
1.26995024085446));
#45424=CARTESIAN_POINT('Ctrl Pts',(-0.391939142907391,-4.69299607822649,
1.34932213090786));
#45425=CARTESIAN_POINT('Ctrl Pts',(1.90041903637464,-4.30885554699701,1.42869402096126));
#45426=CARTESIAN_POINT('Ctrl Pts',(3.72983933538439,-2.87508731801348,1.50806591101467));
#45427=CARTESIAN_POINT('Ctrl Pts',(4.65067903319439,-0.740954194967835,
1.58743780106807));
#45428=CARTESIAN_POINT('Ctrl Pts',(4.43862360995218,1.57367373662795,1.66680969112148));
#45429=CARTESIAN_POINT('Ctrl Pts',(3.1453293014661,3.50495822568453,1.74618158117488));
#45430=CARTESIAN_POINT('Ctrl Pts',(1.08583973646247,4.58244265094549,1.82555347122828));
#45431=CARTESIAN_POINT('Ctrl Pts',(-1.2381579844814,4.54365418850119,1.90492536128169));
#45432=CARTESIAN_POINT('Ctrl Pts',(-3.26054316123182,3.39804162347539,1.98429725133509));
#45433=CARTESIAN_POINT('Ctrl Pts',(-4.48866724088482,1.42467364012815,2.0636691413885));
#45434=CARTESIAN_POINT('Ctrl Pts',(-4.62336191621359,-0.895741688344198,
2.1430410314419));
#45435=CARTESIAN_POINT('Ctrl Pts',(-3.63181586235956,-2.99795632430514,
2.2224129214953));
#45436=CARTESIAN_POINT('Ctrl Pts',(-1.75556750333933,-4.36987543548745,
2.30178481154871));
#45437=CARTESIAN_POINT('Ctrl Pts',(0.548333213620371,-4.67730256316232,
2.38115670160211));
#45438=CARTESIAN_POINT('Ctrl Pts',(2.71866117345249,-3.84534913947276,2.46052859165552));
#45439=CARTESIAN_POINT('Ctrl Pts',(4.22672928908848,-2.07667717694978,2.53990048170891));
#45440=CARTESIAN_POINT('Ctrl Pts',(4.7051755056078,0.19786874923449,2.61927237176232));
#45441=CARTESIAN_POINT('Ctrl Pts',(4.03745138369107,2.42421428607854,2.69864426181572));
#45442=CARTESIAN_POINT('Ctrl Pts',(2.38621304145389,4.06002658874208,2.77801615186912));
#45443=CARTESIAN_POINT('Ctrl Pts',(0.153698484111727,4.70682540110399,2.85738804192253));
#45444=CARTESIAN_POINT('Ctrl Pts',(-2.11625668375435,4.20705196413855,2.93675993197593));
#45445=CARTESIAN_POINT('Ctrl Pts',(-3.87069640771252,2.68244998086038,3.01613182202934));
#45446=CARTESIAN_POINT('Ctrl Pts',(-4.68224305439313,0.504409119747013,
3.09550371208274));
#45447=CARTESIAN_POINT('Ctrl Pts',(-4.35320565699276,-1.79650468644612,
3.17487560213615));
#45448=CARTESIAN_POINT('Ctrl Pts',(-2.96373699720624,-3.65979392751662,
3.25424749218954));
#45449=CARTESIAN_POINT('Ctrl Pts',(-0.852308565020845,-4.63156546866054,
3.33361938224295));
#45450=CARTESIAN_POINT('Ctrl Pts',(1.46674034705061,-4.47509791343502,3.41299127229636));
#45451=CARTESIAN_POINT('Ctrl Pts',(3.42849455715522,-3.22850641195795,3.49236316234976));
#45452=CARTESIAN_POINT('Ctrl Pts',(4.55507508198081,-1.19545789470566,3.57173505240317));
#45453=CARTESIAN_POINT('Ctrl Pts',(4.57204939932356,1.12880151959577,3.65110694245656));
#45454=CARTESIAN_POINT('Ctrl Pts',(3.47528260305076,3.17808738228345,3.73047883250997));
#45455=CARTESIAN_POINT('Ctrl Pts',(1.53194465708238,4.45319819322398,3.80985072256337));
#45456=CARTESIAN_POINT('Ctrl Pts',(-0.784571616449287,4.64351978128216,
3.88922261261678));
#45457=CARTESIAN_POINT('Ctrl Pts',(-2.90996798083373,3.70269022887672,3.96859450267018));
#45458=CARTESIAN_POINT('Ctrl Pts',(-4.32650258619195,1.85989353248269,4.04796639272359));
#45459=CARTESIAN_POINT('Ctrl Pts',(-4.68911073810485,-0.4359691116196,4.12733828277699));
#45460=CARTESIAN_POINT('Ctrl Pts',(-3.90946189338598,-2.62563064513263,
4.2067101728304));
#45461=CARTESIAN_POINT('Ctrl Pts',(-2.17747678488539,-4.17569436522619,
4.28608206288379));
#45462=CARTESIAN_POINT('Ctrl Pts',(0.0849368486501527,-4.70856818069336,
4.3654539529372));
#45463=CARTESIAN_POINT('Ctrl Pts',(2.32666005385904,-4.09444520958252,4.4448258429906));
#45464=CARTESIAN_POINT('Ctrl Pts',(4.00161401992256,-2.48292444831813,4.52419773304401));
#45465=CARTESIAN_POINT('Ctrl Pts',(4.70178366815532,-0.266568787303479,
4.60356962309741));
#45466=CARTESIAN_POINT('Ctrl Pts',(4.25660922204708,2.0147224402583,4.68294151315081));
#45467=CARTESIAN_POINT('Ctrl Pts',(2.77453419129287,3.80523174088563,4.76231340320422));
#45468=CARTESIAN_POINT('Ctrl Pts',(0.616588772866969,4.6687950121708,4.84168529325762));
#45469=CARTESIAN_POINT('Ctrl Pts',(-1.69155630583321,4.39505015269366,4.92105718331103));
#45470=CARTESIAN_POINT('Ctrl Pts',(-3.5876420126288,3.05068080429882,5.00042907336443));
#45471=CARTESIAN_POINT('Ctrl Pts',(-4.60978606625892,0.96317236454425,5.07980096341783));
#45472=CARTESIAN_POINT('Ctrl Pts',(-4.50899643773674,-1.35896273126747,
5.15917285347124));
#45473=CARTESIAN_POINT('Ctrl Pts',(-3.30982525747623,-3.3500575137554,5.23854474352463));
#45474=CARTESIAN_POINT('Ctrl Pts',(-1.30438797066844,-4.52508570111905,
5.31791663357805));
#45475=CARTESIAN_POINT('Ctrl Pts',(1.01879533858038,-4.5978130277974,5.39728852363144));
#45476=CARTESIAN_POINT('Ctrl Pts',(3.09380235841625,-3.55052327799082,5.47666041368486));
#45477=CARTESIAN_POINT('Ctrl Pts',(4.41516597175728,-1.63833391661564,5.55603230373825));
#45478=CARTESIAN_POINT('Ctrl Pts',(4.66100492718236,0.672949960456484,5.63540419379167));
#45479=CARTESIAN_POINT('Ctrl Pts',(3.77143339930522,2.82030471671088,5.71477608384506));
#45480=CARTESIAN_POINT('Ctrl Pts',(1.96314904328358,4.28063948661312,5.79414797389847));
#45481=CARTESIAN_POINT('Ctrl Pts',(-0.323354074325263,4.69821995261119,
5.87351986395187));
#45482=CARTESIAN_POINT('Ctrl Pts',(-2.53108885516056,3.97132443748664,5.95289175400528));
#45483=CARTESIAN_POINT('Ctrl Pts',(-4.1222559933489,2.2770230797679,6.03226364405868));
#45484=CARTESIAN_POINT('Ctrl Pts',(-4.70925069601632,0.0280439399227974,
6.11163553411208));
#45485=CARTESIAN_POINT('Ctrl Pts',(-4.14908235288379,-2.22776664161329,
6.19100742416549));
#45486=CARTESIAN_POINT('Ctrl Pts',(-2.57820673242676,-3.94089820033021,
6.27037931421889));
#45487=CARTESIAN_POINT('Ctrl Pts',(-0.37928565871439,-4.6940356804769,6.34975120427229));
#45488=CARTESIAN_POINT('Ctrl Pts',(1.91202856192625,-4.30371645893114,6.42912309432569));
#45489=CARTESIAN_POINT('Ctrl Pts',(3.73757685708508,-2.86502143410457,6.5084949843791));
#45490=CARTESIAN_POINT('Ctrl Pts',(4.65265970284404,-0.728413529547492,
6.58786687443251));
#45491=CARTESIAN_POINT('Ctrl Pts',(4.43436494347775,1.58563429849135,6.6672387644859));
#45492=CARTESIAN_POINT('Ctrl Pts',(3.13586869918061,3.51342512115968,6.74661065453932));
#45493=CARTESIAN_POINT('Ctrl Pts',(1.07348178089069,4.58535336114812,6.8259825445927));
#45494=CARTESIAN_POINT('Ctrl Pts',(-1.25040292311256,4.54029967186839,6.90535443464612));
#45495=CARTESIAN_POINT('Ctrl Pts',(-3.26969224276554,3.38923903230437,6.98472632469952));
#45496=CARTESIAN_POINT('Ctrl Pts',(-4.49249176942184,1.41256726642436,7.06409821475293));
#45497=CARTESIAN_POINT('Ctrl Pts',(-4.62093024500886,-0.908202758892002,
7.14347010480633));
#45498=CARTESIAN_POINT('Ctrl Pts',(-3.62372034116731,-3.00773660241498,
7.22284199485974));
#45499=CARTESIAN_POINT('Ctrl Pts',(-1.74378018318635,-4.37459246710173,
7.30221388491313));
#45500=CARTESIAN_POINT('Ctrl Pts',(0.560940967626854,-4.67580728979868,
7.38158577496654));
#45501=CARTESIAN_POINT('Ctrl Pts',(2.72901814034792,-3.83800580642455,7.46095766501994));
#45502=CARTESIAN_POINT('Ctrl Pts',(4.23231253465944,-2.06527460388716,7.54032955507336));
#45503=CARTESIAN_POINT('Ctrl Pts',(4.70462496359279,0.210552920749357,7.61970144512673));
#45504=CARTESIAN_POINT('Ctrl Pts',(4.03090116490568,2.4350902199423,7.69907333518017));
#45505=CARTESIAN_POINT('Ctrl Pts',(2.37525876469593,4.06644493153808,7.77844522523354));
#45506=CARTESIAN_POINT('Ctrl Pts',(0.141008586952364,4.70722265873438,7.85781711528697));
#45507=CARTESIAN_POINT('Ctrl Pts',(-2.1275909704556,4.2013313655236,7.93718900534037));
#45508=CARTESIAN_POINT('Ctrl Pts',(-3.87791407680332,2.67200505116051,8.01656089539376));
#45509=CARTESIAN_POINT('Ctrl Pts',(-4.68358589765895,0.491784220717585,
8.09593278544718));
#45510=CARTESIAN_POINT('Ctrl Pts',(-4.3483465607864,-1.80823415734624,8.17530467550056));
#45511=CARTESIAN_POINT('Ctrl Pts',(-2.95385962660815,-3.66777069713892,
8.25467656555399));
#45512=CARTESIAN_POINT('Ctrl Pts',(-0.839819025645543,-4.63384641358131,
8.33404845560737));
#45513=CARTESIAN_POINT('Ctrl Pts',(1.47879963105641,-4.47112740052035,8.41342034566079));
#45514=CARTESIAN_POINT('Ctrl Pts',(3.43718597090052,-3.21925164936531,8.49279223571418));
#45515=CARTESIAN_POINT('Ctrl Pts',(4.55828141631537,-1.1831733221175,8.57216412576761));
#45516=CARTESIAN_POINT('Ctrl Pts',(4.56898959830056,1.1411234074884,8.65153601582098));
#45517=CARTESIAN_POINT('Ctrl Pts',(3.46670202742665,3.18744500086393,8.73090790587441));
#45518=CARTESIAN_POINT('Ctrl Pts',(1.51993351608642,4.45731204731885,8.8102797959278));
#45519=CARTESIAN_POINT('Ctrl Pts',(-0.797087435456723,4.64138774513978,
8.88965168598121));
#45520=CARTESIAN_POINT('Ctrl Pts',(-2.91993965204571,3.69483166178214,8.96902357603462));
#45521=CARTESIAN_POINT('Ctrl Pts',(-4.33150103257314,1.84822276398555,9.04839546608801));
#45522=CARTESIAN_POINT('Ctrl Pts',(-4.68791834918067,-0.448609108146216,
9.12776735614143));
#45523=CARTESIAN_POINT('Ctrl Pts',(-3.90236913245906,-2.63616079451299,
9.20713924619481));
#45524=CARTESIAN_POINT('Ctrl Pts',(-2.16621143281798,-4.18154954637933,
9.28651113624823));
#45525=CARTESIAN_POINT('Ctrl Pts',(0.0976305770298679,-4.70832208445062,
9.36588302630162));
#45526=CARTESIAN_POINT('Ctrl Pts',(2.33768999441487,-4.08815778444389,9.44525491635505));
#45527=CARTESIAN_POINT('Ctrl Pts',(4.00829330354943,-2.47212729713041,9.52462680640842));
#45528=CARTESIAN_POINT('Ctrl Pts',(4.70248523614611,-0.253892072196923,
9.60399869646185));
#45529=CARTESIAN_POINT('Ctrl Pts',(4.25116217399211,2.02619069954319,9.68337058651524));
#45530=CARTESIAN_POINT('Ctrl Pts',(2.76426541604147,3.81269790177162,9.76274247656865));
#45531=CARTESIAN_POINT('Ctrl Pts',(0.603999721340871,4.67044033439211,9.84211436662206));
#45532=CARTESIAN_POINT('Ctrl Pts',(-1.70339896854767,4.39047383939904,9.92148625667545));
#45533=CARTESIAN_POINT('Ctrl Pts',(-3.59585344010767,3.04099763527736,10.0008581467289));
#45534=CARTESIAN_POINT('Ctrl Pts',(-4.61236597294403,0.95074113833618,10.0802300367823));
#45535=CARTESIAN_POINT('Ctrl Pts',(-4.5053163640701,-1.37111379547384,10.1596019268357));
#45536=CARTESIAN_POINT('Ctrl Pts',(-3.30078166125737,-3.35896844361534,
10.2389738168891));
#45537=CARTESIAN_POINT('Ctrl Pts',(-1.29218385191862,-4.5285858138427,10.3183457069425));
#45538=CARTESIAN_POINT('Ctrl Pts',(1.03118708354706,-4.59504970367267,10.3977175969959));
#45539=CARTESIAN_POINT('Ctrl Pts',(3.1033631279546,-3.54216965665798,10.4770894870493));
#45540=CARTESIAN_POINT('Ctrl Pts',(4.41956678357015,-1.62642492174092,10.5564613771027));
#45541=CARTESIAN_POINT('Ctrl Pts',(4.65917375325315,0.68551332408169,10.6358332671561));
#45542=CARTESIAN_POINT('Ctrl Pts',(3.76381630954987,2.83046204151602,10.7152051572095));
#45543=CARTESIAN_POINT('Ctrl Pts',(1.95160154390631,4.28591647075852,10.7945770472629));
#45544=CARTESIAN_POINT('Ctrl Pts',(-0.336019038036085,4.69733113443942,
10.8739489373163));
#45545=CARTESIAN_POINT('Ctrl Pts',(-2.54178612607839,3.96448633113698,10.9533208273697));
#45546=CARTESIAN_POINT('Ctrl Pts',(-4.12837973995617,2.26590143281123,11.0326927174231));
#45547=CARTESIAN_POINT('Ctrl Pts',(-4.70930918719419,0.0153479609404256,
11.1120646074765));
#45548=CARTESIAN_POINT('Ctrl Pts',(-4.14306134031078,-2.23894424024334,
11.1914364975299));
#45549=CARTESIAN_POINT('Ctrl Pts',(-2.5675729214384,-3.94783458032284,11.2708083875833));
#45550=CARTESIAN_POINT('Ctrl Pts',(-0.366629422129896,-4.69504115501934,
11.3501802776367));
#45551=CARTESIAN_POINT('Ctrl Pts',(1.92362419288899,-4.29854609665044,11.4295521676901));
#45552=CARTESIAN_POINT('Ctrl Pts',(3.74528721239005,-2.85493472380791,11.5089240577435));
#45553=CARTESIAN_POINT('Ctrl Pts',(4.65460655700554,-0.715867571536574,
11.5882959477969));
#45554=CARTESIAN_POINT('Ctrl Pts',(4.43007404713131,1.59758333661508,11.6676678378504));
#45555=CARTESIAN_POINT('Ctrl Pts',(3.12638530517848,3.52186648015801,11.7470397279037));
#45556=CARTESIAN_POINT('Ctrl Pts',(1.06111602302068,4.5882307446537,11.8264116179572));
#45557=CARTESIAN_POINT('Ctrl Pts',(-1.26263877360451,4.53691215562823,11.9057835080105));
#45558=CARTESIAN_POINT('Ctrl Pts',(-3.27881755978316,3.38041180777642,11.985155398064));
#45559=CARTESIAN_POINT('Ctrl Pts',(-4.49628364593817,1.40045062596491,12.0645272881173));
#45560=CARTESIAN_POINT('Ctrl Pts',(-4.6184649882977,-0.920657228486762,
12.1438991781708));
#45561=CARTESIAN_POINT('Ctrl Pts',(-3.61559848230676,-3.01749501991928,
12.2232710682242));
#45562=CARTESIAN_POINT('Ctrl Pts',(-1.7319801890174,-4.37927770361138,12.3026429582776));
#45563=CARTESIAN_POINT('Ctrl Pts',(0.573544644643477,-4.67427803207056,
12.382014848331));
#45564=CARTESIAN_POINT('Ctrl Pts',(2.73935527238874,-3.83063457825627,12.4613867383844));
#45565=CARTESIAN_POINT('Ctrl Pts',(4.23786501924016,-2.05385702014458,12.5407586284378));
#45566=CARTESIAN_POINT('Ctrl Pts',(4.7040402277598,0.22323556193892,12.6201305184912));
#45567=CARTESIAN_POINT('Ctrl Pts',(4.02432164901358,2.44594845525766,12.6995024085446));
#45568=CARTESIAN_POINT('Ctrl Pts',(2.3642872242525,4.0728337188907,12.778874298598));
#45569=CARTESIAN_POINT('Ctrl Pts',(0.12831766492455,4.70758570366646,12.8582461886514));
#45570=CARTESIAN_POINT('Ctrl Pts',(-2.13890979355269,4.19558023109331,12.9376180787048));
#45571=CARTESIAN_POINT('Ctrl Pts',(-3.88510356071705,2.66154070098513,13.0169899687582));
#45572=CARTESIAN_POINT('Ctrl Pts',(-4.68489470002156,0.479155747337376,
13.0963618588116));
#45573=CARTESIAN_POINT('Ctrl Pts',(-4.34345586023936,-1.81995048576848,
13.175733748865));
#45574=CARTESIAN_POINT('Ctrl Pts',(-2.94396078697933,-3.67572080893321,
13.2551056389184));
#45575=CARTESIAN_POINT('Ctrl Pts',(-0.827323382357809,-4.63609367911183,
13.3344775289718));
#45576=CARTESIAN_POINT('Ctrl Pts',(1.49084816695683,-4.4671243908781,13.4138494190252));
#45577=CARTESIAN_POINT('Ctrl Pts',(3.44585240273723,-3.2099734888386,13.4932213090786));
#45578=CARTESIAN_POINT('Ctrl Pts',(4.56145462047577,-1.17088015007382,13.572593199132));
#45579=CARTESIAN_POINT('Ctrl Pts',(4.56589658927495,1.15343700154968,13.6519650891854));
#45580=CARTESIAN_POINT('Ctrl Pts',(3.45809625536746,3.19677945268519,13.7313369792388));
#45581=CARTESIAN_POINT('Ctrl Pts',(1.50791132801865,4.4613935050979,13.8107088692922));
#45582=CARTESIAN_POINT('Ctrl Pts',(-0.809597461130395,4.63922197479575,
13.8900807593457));
#45583=CARTESIAN_POINT('Ctrl Pts',(-2.92989010076163,3.68694624017703,13.969452649399));
#45584=CARTESIAN_POINT('Ctrl Pts',(-4.33646799704908,1.83653856236827,14.0488245394525));
#45585=CARTESIAN_POINT('Ctrl Pts',(-4.68669188786449,-0.461245844124263,
14.1281964295058));
#45586=CARTESIAN_POINT('Ctrl Pts',(-3.8952480086126,-2.64667178393849,14.2075683195593));
#45587=CARTESIAN_POINT('Ctrl Pts',(-2.15493033644793,-4.1873743354939,14.2869402096127));
#45588=CARTESIAN_POINT('Ctrl Pts',(0.110323595818042,-4.70804176751889,
14.3663120996661));
#45589=CARTESIAN_POINT('Ctrl Pts',(2.34870294433987,-4.08184064604999,14.4456839897195));
#45590=CARTESIAN_POINT('Ctrl Pts',(4.01494345438633,-2.46131217820434,14.5250558797729));
#45591=CARTESIAN_POINT('Ctrl Pts',(4.70315262587088,-0.241213511770193,
14.6044277698263));
#45592=CARTESIAN_POINT('Ctrl Pts',(4.24568422794502,2.03764423221413,14.6837996598797));
#45593=CARTESIAN_POINT('Ctrl Pts',(2.7539765497544,3.82013635148006,14.7631715499331));
#45594=CARTESIAN_POINT('Ctrl Pts',(0.591406279867313,4.67205171125386,14.8425434399865));
#45595=CARTESIAN_POINT('Ctrl Pts',(-1.71522925073988,4.38586561557727,14.9219153300399));
#45596=CARTESIAN_POINT('Ctrl Pts',(-3.60403873246238,3.0312923638949,15.0012872200933));
#45597=CARTESIAN_POINT('Ctrl Pts',(-4.61491235636145,0.938303002019602,
15.0806591101467));
#45598=CARTESIAN_POINT('Ctrl Pts',(-4.50160354518612,-1.38325489424921,
15.1600310002001));
#45599=CARTESIAN_POINT('Ctrl Pts',(-3.29171407453388,-3.36785496006171,
15.2394028902535));
#45600=CARTESIAN_POINT('Ctrl Pts',(-1.27997034141067,-4.53205301222367,
15.3187747803069));
#45601=CARTESIAN_POINT('Ctrl Pts',(1.04357133371383,-4.59225298213712,15.3981466703603));
#45602=CARTESIAN_POINT('Ctrl Pts',(3.11290134185163,-3.53379029038156,15.4775185604137));
#45603=CARTESIAN_POINT('Ctrl Pts',(4.42393547340459,-1.6145041058012,15.5568904504671));
#45604=CARTESIAN_POINT('Ctrl Pts',(4.65730871585136,0.69807170530811,15.6362623405205));
#45605=CARTESIAN_POINT('Ctrl Pts',(3.75617186389461,2.84059879415993,15.7156342305739));
#45606=CARTESIAN_POINT('Ctrl Pts',(1.94003986003872,4.2911623043131,15.7950061206273));
#45607=CARTESIAN_POINT('Ctrl Pts',(-0.348681559517582,4.69640817546235,
15.8743780106807));
#45608=CARTESIAN_POINT('Ctrl Pts',(-2.55246492296822,3.95761941039193,15.9537499007341));
#45609=CARTESIAN_POINT('Ctrl Pts',(-4.13447348097045,2.25476331699244,16.0331217907876));
#45610=CARTESIAN_POINT('Ctrl Pts',(-4.70933345050753,0.00265187040668795,
16.1124936808409));
#45611=CARTESIAN_POINT('Ctrl Pts',(-4.13701021543854,-2.25010556593871,
16.1918655708943));
#45612=CARTESIAN_POINT('Ctrl Pts',(-2.55692044899651,-3.95474226694862,
16.2712374609477));
#45613=CARTESIAN_POINT('Ctrl Pts',(-0.353970520843347,-4.69601250539775,
16.3506093510012));
#45614=CARTESIAN_POINT('Ctrl Pts',(1.93520584271894,-4.29334449198998,16.4299812410546));
#45615=CARTESIAN_POINT('Ctrl Pts',(3.75297034643966,-2.8448272634702,16.509353131108));
#45616=CARTESIAN_POINT('Ctrl Pts',(4.65651958094123,-0.703316410525392,
16.5887250211614));
#45617=CARTESIAN_POINT('Ctrl Pts',(4.42575095234045,1.60952076333056,16.6680969112148));
#45618=CARTESIAN_POINT('Ctrl Pts',(3.11687918839165,3.53028224171774,16.7474688012682));
#45619=CARTESIAN_POINT('Ctrl Pts',(1.04874255247428,4.59107478042509,16.8268406913216));
#45620=CARTESIAN_POINT('Ctrl Pts',(-1.27486544641699,4.53349166431028,16.906212581375));
#45621=CARTESIAN_POINT('Ctrl Pts',(-3.28791904717816,3.37156001439364,16.9855844714284));
#45622=CARTESIAN_POINT('Ctrl Pts',(-4.50004284053898,1.38832380607291,17.0649563614818));
#45623=CARTESIAN_POINT('Ctrl Pts',(-4.61596616842608,-0.933105005158158,
17.1443282515352));
#45624=CARTESIAN_POINT('Ctrl Pts',(-3.60745033643721,-3.02723150865552,
17.2237001415886));
#45625=CARTESIAN_POINT('Ctrl Pts',(-1.72016762240852,-4.3839311057331,17.303072031642));
#45626=CARTESIAN_POINT('Ctrl Pts',(0.586144182924747,-4.67271481097615,
17.3824439216954));
#45627=CARTESIAN_POINT('Ctrl Pts',(2.74967243806105,-3.82323548987727,17.4618158117488));
#45628=CARTESIAN_POINT('Ctrl Pts',(4.24338680893684,-2.04242454395285,17.5411877018022));
#45629=CARTESIAN_POINT('Ctrl Pts',(4.70342110133588,0.235916647177909,17.6205595918556));
#45630=CARTESIAN_POINT('Ctrl Pts',(4.01771326340766,2.45678878743836,17.699931481909));
#45631=CARTESIAN_POINT('Ctrl Pts',(2.35329778315649,4.07919314165109,17.7793033719624));
#45632=CARTESIAN_POINT('Ctrl Pts',(0.115627163561191,4.70791408521782,17.8586752620158));
#45633=CARTESIAN_POINT('Ctrl Pts',(-2.15021562607272,4.18979944864554,17.9380471520692));
#45634=CARTESIAN_POINT('Ctrl Pts',(-3.89225998228542,2.6510554089743,18.0174190421226));
#45635=CARTESIAN_POINT('Ctrl Pts',(-4.68617856238767,0.466526807638264,
18.096790932176));
#45636=CARTESIAN_POINT('Ctrl Pts',(-4.33851638857381,-1.83165928184378,
18.1761628222294));
#45637=CARTESIAN_POINT('Ctrl Pts',(-2.93407303174987,-3.68363345125881,
18.2555347122828));
#45638=CARTESIAN_POINT('Ctrl Pts',(-0.814760394348088,-4.63832755437977,
18.3349066023362));
#45639=CARTESIAN_POINT('Ctrl Pts',(1.50277006074129,-4.46305057284721,18.4142784923896));
#45640=CARTESIAN_POINT('Ctrl Pts',(3.45471245456617,-3.20074439226408,18.493650382443));
#45641=CARTESIAN_POINT('Ctrl Pts',(4.56418179760217,-1.15844177813615,18.5730222724965));
#45642=CARTESIAN_POINT('Ctrl Pts',(4.56354990278295,1.16548416044567,18.6523941625499));
#45643=CARTESIAN_POINT('Ctrl Pts',(3.44799414715945,3.20657754587687,18.7317660526033));
#45644=CARTESIAN_POINT('Ctrl Pts',(1.49865065220682,4.46452630956668,18.8111379426567));
#45645=CARTESIAN_POINT('Ctrl Pts',(-0.827291992766502,4.63872722375952,
18.8905098327101));
#45646=CARTESIAN_POINT('Ctrl Pts',(-2.93038174053102,3.67602118591242,18.9698817227635));
#45647=CARTESIAN_POINT('Ctrl Pts',(-4.8317659974063,1.21320979378885,19.0757109095013));
#45648=CARTESIAN_POINT('Ctrl Pts',(-4.41154214902252,-3.00742829557681,
19.2079973929237));
#45649=CARTESIAN_POINT('Ctrl Pts',(0.14114360583215,-5.34031031892966,19.3667411730305));
#45650=CARTESIAN_POINT('Ctrl Pts',(4.55878074835922,-2.77696271962162,19.5254849531373));
#45651=CARTESIAN_POINT('Ctrl Pts',(4.80798654830346,2.32253130646654,19.6842287332441));
#45652=CARTESIAN_POINT('Ctrl Pts',(0.656009676029318,5.29932988758691,19.8429725133509));
#45653=CARTESIAN_POINT('Ctrl Pts',(-4.09539160933947,3.42571876325565,20.0017162934577));
#45654=CARTESIAN_POINT('Ctrl Pts',(-5.09974667860472,-1.58211192901314,
20.1604600735645));
#45655=CARTESIAN_POINT('Ctrl Pts',(-1.43734916996091,-5.14215993940121,
20.3192038536714));
#45656=CARTESIAN_POINT('Ctrl Pts',(3.54020456892056,-3.99752392897281,20.4779476337781));
#45657=CARTESIAN_POINT('Ctrl Pts',(5.27828887711237,0.806568563691912,20.636691413885));
#45658=CARTESIAN_POINT('Ctrl Pts',(2.1865632094635,4.86959394496087,20.7954351939918));
#45659=CARTESIAN_POINT('Ctrl Pts',(-2.90621803008048,4.48249178265495,20.9541789740986));
#45660=CARTESIAN_POINT('Ctrl Pts',(-5.339103029404,-0.0175478502156508,
21.1129227542054));
#45661=CARTESIAN_POINT('Ctrl Pts',(-3.29668819545046,-3.73492805813105,
21.2452092376277));
#45662=CARTESIAN_POINT('Ctrl Pts',(-0.335233909123966,-4.68912434583344,
21.3510384243656));
#45663=CARTESIAN_POINT('Ctrl Pts',(1.9434592869775,-4.29245481019942,21.430410314419));
#45664=CARTESIAN_POINT('Ctrl Pts',(3.76239327895729,-2.83237457985877,21.5097822044724));
#45665=CARTESIAN_POINT('Ctrl Pts',(4.65746145505442,-0.691994213306775,
21.5891540945258));
#45666=CARTESIAN_POINT('Ctrl Pts',(4.42189226956134,1.62210042840564,21.6685259845792));
#45667=CARTESIAN_POINT('Ctrl Pts',(3.10708740551244,3.53832597274477,21.7478978746326));
#45668=CARTESIAN_POINT('Ctrl Pts',(1.03650075501011,4.59406889295405,21.827269764686));
#45669=CARTESIAN_POINT('Ctrl Pts',(-1.28715662605568,4.52994106929143,21.9066416547395));
#45670=CARTESIAN_POINT('Ctrl Pts',(-3.29695756540469,3.36273516855513,21.9860135447928));
#45671=CARTESIAN_POINT('Ctrl Pts',(-4.5037900244027,1.37615964733944,22.0653854348462));
#45672=CARTESIAN_POINT('Ctrl Pts',(-4.61342283197247,-0.945531571193242,
22.1447573248996));
#45673=CARTESIAN_POINT('Ctrl Pts',(-3.59928179145312,-3.03695363259649,
22.224129214953));
#45674=CARTESIAN_POINT('Ctrl Pts',(-1.70833944819064,-4.388548607559,22.3035011050065));
#45675=CARTESIAN_POINT('Ctrl Pts',(0.598737773532913,-4.67111975194625,
22.3828729950598));
#45676=CARTESIAN_POINT('Ctrl Pts',(2.75997059360609,-3.81580751573965,22.4622448851133));
#45677=CARTESIAN_POINT('Ctrl Pts',(4.24887708766878,-2.03097775393672,22.5416167751666));
#45678=CARTESIAN_POINT('Ctrl Pts',(4.7027684336848,0.248596203073706,22.6209886652201));
#45679=CARTESIAN_POINT('Ctrl Pts',(4.01107478934813,2.46761134605171,22.7003605552734));
#45680=CARTESIAN_POINT('Ctrl Pts',(2.34229273922348,4.08552253105782,22.7797324453269));
#45681=CARTESIAN_POINT('Ctrl Pts',(0.10293307930986,4.70820909782832,22.8591043353802));
#45682=CARTESIAN_POINT('Ctrl Pts',(-2.16150070095897,4.18398654725925,22.9384762254337));
#45683=CARTESIAN_POINT('Ctrl Pts',(-3.89939777427635,2.64055403030605,23.017848115487));
#45684=CARTESIAN_POINT('Ctrl Pts',(-4.6874101388992,0.453888451717589,23.0972200055405));
#45685=CARTESIAN_POINT('Ctrl Pts',(-4.33357979136315,-1.84334337837373,
23.1765918955938));
#45686=CARTESIAN_POINT('Ctrl Pts',(-2.92409898707257,-3.69154082613157,
23.2559637856473));
#45687=CARTESIAN_POINT('Ctrl Pts',(-0.802314148160901,-4.64048710795707,
23.3353356757007));
#45688=CARTESIAN_POINT('Ctrl Pts',(1.51491264465863,-4.45902099747155,23.4147075657541));
#45689=CARTESIAN_POINT('Ctrl Pts',(3.46311006868958,-3.19134724418486,23.4940794558075));
#45690=CARTESIAN_POINT('Ctrl Pts',(4.56770154637975,-1.14626836492011,23.5734513458609));
#45691=CARTESIAN_POINT('Ctrl Pts',(4.55961103731633,1.17803895017003,23.6528232359143));
#45692=CARTESIAN_POINT('Ctrl Pts',(3.44080937235073,3.21537858488653,23.7321951259677));
#45693=CARTESIAN_POINT('Ctrl Pts',(1.48383416024502,4.46945911326291,23.8115670160211));
#45694=CARTESIAN_POINT('Ctrl Pts',(-0.834599768812189,4.6347892947245,23.8909389060745));
#45695=CARTESIAN_POINT('Ctrl Pts',(-2.94972704158065,3.67109506287238,23.9703107961279));
#45696=CARTESIAN_POINT('Ctrl Pts',(-4.34630733610966,1.81313019956259,24.0496826861813));
#45697=CARTESIAN_POINT('Ctrl Pts',(-4.68413678396127,-0.486509167079313,
24.1290545762347));
#45698=CARTESIAN_POINT('Ctrl Pts',(-3.8809208793951,-2.66763597748286,24.2084264662881));
#45699=CARTESIAN_POINT('Ctrl Pts',(-2.13232123888401,-4.19893256848769,
24.2877983563416));
#45700=CARTESIAN_POINT('Ctrl Pts',(0.13570713560786,-4.70737847998643,24.3671702463949));
#45701=CARTESIAN_POINT('Ctrl Pts',(2.37067755224746,-4.06911741336709,24.4465421364484));
#45702=CARTESIAN_POINT('Ctrl Pts',(4.02815616456577,-2.43962835168955,24.5259140265017));
#45703=CARTESIAN_POINT('Ctrl Pts',(4.70438485136804,-0.215851223566548,
24.6052859165551));
#45704=CARTESIAN_POINT('Ctrl Pts',(4.23463580135646,2.06050678483885,24.6846578066085));
#45705=CARTESIAN_POINT('Ctrl Pts',(2.73333884334173,3.83492990131186,24.7640296966619));
#45706=CARTESIAN_POINT('Ctrl Pts',(0.566206593231879,4.6751725822987,24.8434015867153));
#45707=CARTESIAN_POINT('Ctrl Pts',(-1.73885232971224,4.3765535705565,24.9227734767688));
#45708=CARTESIAN_POINT('Ctrl Pts',(-3.62033067402275,3.0118157963638,25.0021453668221));
#45709=CARTESIAN_POINT('Ctrl Pts',(-4.61990447960738,0.913406360718075,
25.0815172568756));
#45710=CARTESIAN_POINT('Ctrl Pts',(-4.49407977994478,-1.40750684260792,
25.1608891469289));
#45711=CARTESIAN_POINT('Ctrl Pts',(-3.27350719336448,-3.38555449453819,
25.2402610369824));
#45712=CARTESIAN_POINT('Ctrl Pts',(-1.25551550026584,-4.53888856539668,
25.3196329270357));
#45713=CARTESIAN_POINT('Ctrl Pts',(1.06831698966113,-4.58655942838399,25.3990048170892));
#45714=CARTESIAN_POINT('Ctrl Pts',(3.1319098255862,-3.51695456679402,25.4783767071426));
#45715=CARTESIAN_POINT('Ctrl Pts',(4.43257636036326,-1.59062735737991,25.557748597196));
#45716=CARTESIAN_POINT('Ctrl Pts',(4.65347710509718,0.723173155497971,25.6371204872493));
#45717=CARTESIAN_POINT('Ctrl Pts',(3.74080112732632,2.86081028841317,25.7164923773028));
#45718=CARTESIAN_POINT('Ctrl Pts',(1.91687427506164,4.30156036736711,25.7958642673562));
#45719=CARTESIAN_POINT('Ctrl Pts',(-0.373998907678805,4.69445986217281,
25.8752361574096));
#45720=CARTESIAN_POINT('Ctrl Pts',(-2.57376678434128,3.9437993255639,25.954608047463));
#45721=CARTESIAN_POINT('Ctrl Pts',(-4.14657076927436,2.23243800269932,26.0339799375164));
#45722=CARTESIAN_POINT('Ctrl Pts',(-4.70927929309089,-0.0227402762051125,
26.1133518275698));
#45723=CARTESIAN_POINT('Ctrl Pts',(-4.1248178049234,-2.27237907416072,26.1927237176232));
#45724=CARTESIAN_POINT('Ctrl Pts',(-2.53555982960589,-3.96847135947655,
26.2720956076766));
#45725=CARTESIAN_POINT('Ctrl Pts',(-0.328645092162861,-4.69785280568621,
26.35146749773));
#45726=CARTESIAN_POINT('Ctrl Pts',(1.95832686228742,-4.28284770695154,26.4308393877834));
#45727=CARTESIAN_POINT('Ctrl Pts',(3.76825472776749,-2.8245503867261,26.5102112778369));
#45728=CARTESIAN_POINT('Ctrl Pts',(4.66024408245379,-0.67819884433039,26.5895831678902));
#45729=CARTESIAN_POINT('Ctrl Pts',(4.41700829392964,1.63336043537654,26.6689550579436));
#45730=CARTESIAN_POINT('Ctrl Pts',(3.09779906188623,3.54703672840772,26.748326947997));
#45731=CARTESIAN_POINT('Ctrl Pts',(1.0239728352293,4.59666272563139,26.8276988380504));
#45732=CARTESIAN_POINT('Ctrl Pts',(-1.29929090756406,4.52655185743165,26.9070707281039));
#45733=CARTESIAN_POINT('Ctrl Pts',(-3.30605026120649,3.35378297611415,26.9864426181572));
#45734=CARTESIAN_POINT('Ctrl Pts',(-4.50746308903716,1.36403998528792,27.0658145082107));
#45735=CARTESIAN_POINT('Ctrl Pts',(-4.61086788547865,-0.957980126703151,
27.1451863982641));
#45736=CARTESIAN_POINT('Ctrl Pts',(-3.59107547100053,-3.04663840028233,
27.2245582883174));
#45737=CARTESIAN_POINT('Ctrl Pts',(-1.69650502049742,-4.39314230317249,
27.3039301783709));
#45738=CARTESIAN_POINT('Ctrl Pts',(0.611330297848721,-4.66948646506538,
27.3833020684242));
#45739=CARTESIAN_POINT('Ctrl Pts',(2.77024690879558,-3.80835405980132,27.4626739584777));
#45740=CARTESIAN_POINT('Ctrl Pts',(4.25433750459734,-2.01951503521836,27.542045848531));
#45741=CARTESIAN_POINT('Ctrl Pts',(4.70208090109553,0.261273381823074,27.6214177385845));
#45742=CARTESIAN_POINT('Ctrl Pts',(4.00440779796637,2.47841618137125,27.7007896286379));
#45743=CARTESIAN_POINT('Ctrl Pts',(2.33126981885889,4.09182228501852,27.7801615186913));
#45744=CARTESIAN_POINT('Ctrl Pts',(0.0902396720556605,4.70846953713028,
27.8595334087446));
#45745=CARTESIAN_POINT('Ctrl Pts',(-2.17277265911822,4.17814403201768,27.9389052987981));
#45746=CARTESIAN_POINT('Ctrl Pts',(-3.90650237988159,2.63003188887054,28.0182771888515));
#45747=CARTESIAN_POINT('Ctrl Pts',(-4.68861676780222,0.441249799071397,
28.0976490789049));
#45748=CARTESIAN_POINT('Ctrl Pts',(-4.32859448916339,-1.85501976509172,
28.1770209689583));
#45749=CARTESIAN_POINT('Ctrl Pts',(-2.91413617414575,-3.69941062049508,
28.2563928590117));
#45750=CARTESIAN_POINT('Ctrl Pts',(-0.78980073743719,-4.64263323725236,
28.3357647490651));
#45751=CARTESIAN_POINT('Ctrl Pts',(1.52692841071678,-4.4549206737093,28.4151366391185));
#45752=CARTESIAN_POINT('Ctrl Pts',(3.47170117781886,-3.18199929485031,28.494508529172));
#45753=CARTESIAN_POINT('Ctrl Pts',(4.57077522248444,-1.13394993100173,28.5738804192253));
#45754=CARTESIAN_POINT('Ctrl Pts',(4.55641854019218,1.19032712608322,28.6532523092787));
#45755=CARTESIAN_POINT('Ctrl Pts',(3.43212838697049,3.22464312999871,28.7326241993321));
#45756=CARTESIAN_POINT('Ctrl Pts',(1.47177935557015,4.47344320507303,28.8119960893855));
#45757=CARTESIAN_POINT('Ctrl Pts',(-0.84709186911874,4.63252241719017,28.891367979439));
#45758=CARTESIAN_POINT('Ctrl Pts',(-2.95961338949639,3.66312942239424,28.9707398694923));
#45759=CARTESIAN_POINT('Ctrl Pts',(-4.35117963918583,1.80140620850249,29.0501117595457));
#45760=CARTESIAN_POINT('Ctrl Pts',(-4.68280815994235,-0.499135570435458,
29.1294836495992));
#45761=CARTESIAN_POINT('Ctrl Pts',(-3.87371497815696,-2.67808902923317,
29.2088555396525));
#45762=CARTESIAN_POINT('Ctrl Pts',(-2.12099340201518,-4.2046659283592,29.288227429706));
#45763=CARTESIAN_POINT('Ctrl Pts',(0.148397472118242,-4.70699551420707,
29.3675993197594));
#45764=CARTESIAN_POINT('Ctrl Pts',(2.38163905051584,-4.06271141155196,29.4469712098127));
#45765=CARTESIAN_POINT('Ctrl Pts',(4.03471862787643,-2.428759801702,29.5263430998662));
#45766=CARTESIAN_POINT('Ctrl Pts',(4.70494967818454,-0.203167680126035,
29.6057149899196));
#45767=CARTESIAN_POINT('Ctrl Pts',(4.22906540111636,2.07191563862461,29.685086879973));
#45768=CARTESIAN_POINT('Ctrl Pts',(2.72299015321369,3.84228489391376,29.7644587700264));
#45769=CARTESIAN_POINT('Ctrl Pts',(0.553600531224683,4.67668205379885,29.8438306600798));
#45770=CARTESIAN_POINT('Ctrl Pts',(-1.75064495479666,4.37184981703873,29.9232025501332));
#45771=CARTESIAN_POINT('Ctrl Pts',(-3.62843720481647,3.00204464177339,30.0025744401866));
#45772=CARTESIAN_POINT('Ctrl Pts',(-4.62235018315249,0.900948036685143,
30.08194633024));
#45773=CARTESIAN_POINT('Ctrl Pts',(-4.49026888827113,-1.41961751592495,
30.1613182202934));
#45774=CARTESIAN_POINT('Ctrl Pts',(-3.26436803124854,-3.39436738392576,
30.2406901103467));
#45775=CARTESIAN_POINT('Ctrl Pts',(-1.24327434736992,-4.54225687050705,
30.3200620004003));
#45776=CARTESIAN_POINT('Ctrl Pts',(1.08067821558697,-4.58366263754788,30.3994338904535));
#45777=CARTESIAN_POINT('Ctrl Pts',(3.14137995726753,-3.50849833184719,30.4788057805071));
#45778=CARTESIAN_POINT('Ctrl Pts',(4.4368484946843,-1.57867159843783,30.5581776705604));
#45779=CARTESIAN_POINT('Ctrl Pts',(4.65151055959353,0.735716042020659,30.6375495606138));
#45780=CARTESIAN_POINT('Ctrl Pts',(3.73307494812974,2.87088488312276,30.7169214506672));
#45781=CARTESIAN_POINT('Ctrl Pts',(1.90527054232277,4.30671252129204,30.7962933407206));
#45782=CARTESIAN_POINT('Ctrl Pts',(-0.386653550349159,4.69343452202104,
30.875665230774));
#45783=CARTESIAN_POINT('Ctrl Pts',(-2.58438969399916,3.93684626192686,30.9550371208274));
#45784=CARTESIAN_POINT('Ctrl Pts',(-4.15257422864054,2.2212509664887,31.0344090108808));
#45785=CARTESIAN_POINT('Ctrl Pts',(-4.70920087275226,-0.0354361477304668,
31.1137809009342));
#45786=CARTESIAN_POINT('Ctrl Pts',(-4.11867660790086,-2.28349109479913,
31.1931527909877));
#45787=CARTESIAN_POINT('Ctrl Pts',(-2.52485183790083,-3.97529266559651,
31.272524681041));
#45788=CARTESIAN_POINT('Ctrl Pts',(-0.315978748852904,-4.69872174221564,
31.3518965710945));
#45789=CARTESIAN_POINT('Ctrl Pts',(1.9698660640085,-4.27755260287519,31.4312684611479));
#45790=CARTESIAN_POINT('Ctrl Pts',(3.77585586390199,-2.81438111767642,31.5106403512012));
#45791=CARTESIAN_POINT('Ctrl Pts',(4.66205553306415,-0.665632621738598,
31.5900122412547));
#45792=CARTESIAN_POINT('Ctrl Pts',(4.41258879365675,1.64526250750188,31.669384131308));
#45793=CARTESIAN_POINT('Ctrl Pts',(3.08822519121424,3.55537533164171,31.7487560213615));
#45794=CARTESIAN_POINT('Ctrl Pts',(1.01157676786242,4.59940659468345,31.8281279114149));
#45795=CARTESIAN_POINT('Ctrl Pts',(-1.31148951705349,4.52303259187412,31.9074998014683));
#45796=CARTESIAN_POINT('Ctrl Pts',(-3.31507985854797,3.34485786124704,31.9868716915217));
#45797=CARTESIAN_POINT('Ctrl Pts',(-4.51112408430495,1.35188315933753,32.066243581575));
#45798=CARTESIAN_POINT('Ctrl Pts',(-4.60826846832906,-0.970407287843986,
32.1456154716285));
#45799=CARTESIAN_POINT('Ctrl Pts',(-3.58284885369746,-3.05630866766684,
32.2249873616819));
#45800=CARTESIAN_POINT('Ctrl Pts',(-1.68465518880656,-4.39770002107054,
32.3043592517353));
#45801=CARTESIAN_POINT('Ctrl Pts',(0.623916751156621,-4.66782138348531,
32.3837311417887));
#45802=CARTESIAN_POINT('Ctrl Pts',(2.7805039515543,-3.80087178893047,32.4631030318421));
#45803=CARTESIAN_POINT('Ctrl Pts',(4.25976654389448,-2.00803823967918,32.5424749218955));
#45804=CARTESIAN_POINT('Ctrl Pts',(4.7013594349753,0.273948980040725,32.6218468119489));
#45805=CARTESIAN_POINT('Ctrl Pts',(3.99771157397872,2.4892028345985,32.7012187020023));
#45806=CARTESIAN_POINT('Ctrl Pts',(2.32023002234538,4.09809238840509,32.7805905920557));
#45807=CARTESIAN_POINT('Ctrl Pts',(0.0775455730107522,4.70869570736983,
32.8599624821091));
#45808=CARTESIAN_POINT('Ctrl Pts',(-2.18402880626508,4.17227117454043,32.9393343721625));
#45809=CARTESIAN_POINT('Ctrl Pts',(-3.91357860260051,2.61949061875855,33.018706262216));
#45810=CARTESIAN_POINT('Ctrl Pts',(-4.68978931390171,0.42860794639128,33.0980781522693));
#45811=CARTESIAN_POINT('Ctrl Pts',(-4.32357772900909,-1.86668267300931,
33.1774500423228));
#45812=CARTESIAN_POINT('Ctrl Pts',(-2.90415217940683,-3.70725352509686,
33.2568219323761));
#45813=CARTESIAN_POINT('Ctrl Pts',(-0.777281587132916,-4.64474562433732,
33.3361938224295));
#45814=CARTESIAN_POINT('Ctrl Pts',(1.53893307928302,-4.45078797045929,33.4155657124829));
#45815=CARTESIAN_POINT('Ctrl Pts',(3.4802670539562,-3.17262821862943,33.4949376025364));
#45816=CARTESIAN_POINT('Ctrl Pts',(4.57381567772608,-1.12162325523486,33.5743094925897));
#45817=CARTESIAN_POINT('Ctrl Pts',(4.55319292637118,1.20260665046394,33.6536813826432));
#45818=CARTESIAN_POINT('Ctrl Pts',(3.42342245647383,3.23388423803441,33.7330532726965));
#45819=CARTESIAN_POINT('Ctrl Pts',(1.45971385379651,4.47739478330101,33.81242516275));
#45820=CARTESIAN_POINT('Ctrl Pts',(-0.859577812643769,4.63022186990074,
33.8917970528033));
#45821=CARTESIAN_POINT('Ctrl Pts',(-2.96947822656726,3.65513715781495,33.9711689428568));
#45822=CARTESIAN_POINT('Ctrl Pts',(-4.35602031732756,1.78966912459429,34.0505408329101));
#45823=CARTESIAN_POINT('Ctrl Pts',(-4.6814455006743,-0.511758346012144,
34.1299127229636));
#45824=CARTESIAN_POINT('Ctrl Pts',(-3.86648092226059,-2.68852261628789,
34.209284613017));
#45825=CARTESIAN_POINT('Ctrl Pts',(-2.1096501494946,-4.21036872817975,34.2886565030704));
#45826=CARTESIAN_POINT('Ctrl Pts',(0.161086730056863,-4.70657833738016,
34.3680283931238));
#45827=CARTESIAN_POINT('Ctrl Pts',(2.39258323872595,-4.05627588142921,34.4474002831772));
#45828=CARTESIAN_POINT('Ctrl Pts',(4.04125176633455,-2.41787359917646,34.5267721732306));
#45829=CARTESIAN_POINT('Ctrl Pts',(4.7054803088231,-0.190482660036747,34.606144063284));
#45830=CARTESIAN_POINT('Ctrl Pts',(4.22346426348634,2.08330943346165,34.6855159533374));
#45831=CARTESIAN_POINT('Ctrl Pts',(2.71262167204393,3.84961196029602,34.7648878433908));
#45832=CARTESIAN_POINT('Ctrl Pts',(0.540990445577805,4.67815753457386,34.8442597334442));
#45833=CARTESIAN_POINT('Ctrl Pts',(-1.76242485596904,4.36711428835555,34.9236316234976));
#45834=CARTESIAN_POINT('Ctrl Pts',(-3.63651736366306,2.99225166793732,35.0030035135511));
#45835=CARTESIAN_POINT('Ctrl Pts',(-4.62476229086341,0.888483164446288,
35.0823754036044));
#45836=CARTESIAN_POINT('Ctrl Pts',(-4.48642536074711,-1.43171787127975,
35.1617472936579));
#45837=CARTESIAN_POINT('Ctrl Pts',(-3.25520514328689,-3.40315560261577,
35.2411191837112));
#45838=CARTESIAN_POINT('Ctrl Pts',(-1.2310241581964,-4.54559216191174,35.3204910737646));
#45839=CARTESIAN_POINT('Ctrl Pts',(1.09303158700498,-4.58073253206361,35.399862963818));
#45840=CARTESIAN_POINT('Ctrl Pts',(3.15082725699632,-3.50001659668431,35.4792348538714));
#45841=CARTESIAN_POINT('Ctrl Pts',(4.44108838142123,-1.56670436550804,35.5586067439248));
#45842=CARTESIAN_POINT('Ctrl Pts',(4.64951020631433,0.748253581264717,35.6379786339782));
#45843=CARTESIAN_POINT('Ctrl Pts',(3.72532163646553,2.8809386118726,35.7173505240316));
#45844=CARTESIAN_POINT('Ctrl Pts',(1.89365296183327,4.31183337347777,35.7967224140851));
#45845=CARTESIAN_POINT('Ctrl Pts',(-0.399305382771815,4.69237506938502,
35.8760943041384));
#45846=CARTESIAN_POINT('Ctrl Pts',(-2.59499381998119,3.92986458478612,35.9554661941919));
#45847=CARTESIAN_POINT('Ctrl Pts',(-4.1585475065645,2.210047785941,36.0348380842453));
#45848=CARTESIAN_POINT('Ctrl Pts',(-4.70908822533747,-0.0481317617014899,
36.1142099742986));
#45849=CARTESIAN_POINT('Ctrl Pts',(-4.11250547580826,-2.29458651873135,
36.1935818643521));
#45850=CARTESIAN_POINT('Ctrl Pts',(-2.51412549524861,-3.98208507877941,
36.2729537544055));
#45851=CARTESIAN_POINT('Ctrl Pts',(-0.303310108968769,-4.6995565278326,
36.3523256444589));
#45852=CARTESIAN_POINT('Ctrl Pts',(1.98139094849032,-4.27222640899768,36.4316975345123));
#45853=CARTESIAN_POINT('Ctrl Pts',(3.7834295566316,-2.80419139334371,36.5110694245656));
#45854=CARTESIAN_POINT('Ctrl Pts',(4.66383309925673,-0.653061561243602,
36.5904413146191));
#45855=CARTESIAN_POINT('Ctrl Pts',(4.4081372221224,1.65715262164824,36.6698132046725));
#45856=CARTESIAN_POINT('Ctrl Pts',(3.07862887492527,3.56368809395169,36.7491850947259));
#45857=CARTESIAN_POINT('Ctrl Pts',(0.999173348225765,4.60211703465827,36.8285569847793));
#45858=CARTESIAN_POINT('Ctrl Pts',(-1.3236785944688,4.51948045233538,36.9079288748327));
#45859=CARTESIAN_POINT('Ctrl Pts',(-3.32408536146365,3.33590843552393,36.9873007648862));
#45860=CARTESIAN_POINT('Ctrl Pts',(-4.51475229214413,1.33971650772689,37.0666726549395));
#45861=CARTESIAN_POINT('Ctrl Pts',(-4.60563555769299,-0.982827395940232,
37.146044544993));
#45862=CARTESIAN_POINT('Ctrl Pts',(-3.57459619578919,-3.06595672140786,
37.2254164350463));
#45863=CARTESIAN_POINT('Ctrl Pts',(-1.67279311282567,-4.40222577592056,
37.3047883250997));
#45864=CARTESIAN_POINT('Ctrl Pts',(0.636498669757439,-4.6661223755806,37.3841602151531));
#45865=CARTESIAN_POINT('Ctrl Pts',(2.79074078525356,-3.79336189283575,37.4635321052066));
#45866=CARTESIAN_POINT('Ctrl Pts',(4.26516462266191,-1.9965468494605,37.5429039952599));
#45867=CARTESIAN_POINT('Ctrl Pts',(4.70060379877145,0.286622587162363,37.6222758853134));
#45868=CARTESIAN_POINT('Ctrl Pts',(3.99098629411051,2.49997139597979,37.7016477753667));
#45869=CARTESIAN_POINT('Ctrl Pts',(2.3091733621022,4.10433270633122,37.7810196654202));
#45870=CARTESIAN_POINT('Ctrl Pts',(0.0648509103550771,4.70888765420329,
37.8603915554735));
#45871=CARTESIAN_POINT('Ctrl Pts',(-2.19526907961097,4.16636799246395,37.9397634455269));
#45872=CARTESIAN_POINT('Ctrl Pts',(-3.92062638092667,2.60893030984724,38.0191353355804));
#45873=CARTESIAN_POINT('Ctrl Pts',(-4.69092777401319,0.415962978544177,
38.0985072256337));
#45874=CARTESIAN_POINT('Ctrl Pts',(-4.31852954453265,-1.87833201365752,
38.1778791156872));
#45875=CARTESIAN_POINT('Ctrl Pts',(-2.89414707692572,-3.71506948486711,
38.2572510057405));
#45876=CARTESIAN_POINT('Ctrl Pts',(-0.764756787430149,-4.64682425288566,
38.336622895794));
#45877=CARTESIAN_POINT('Ctrl Pts',(1.55092656265596,-4.44662291817819,38.4159947858474));
#45878=CARTESIAN_POINT('Ctrl Pts',(3.48880763512333,-3.16323408359078,38.4953666759007));
#45879=CARTESIAN_POINT('Ctrl Pts',(4.57682288978048,-1.10928842689192,38.5747385659542));
#45880=CARTESIAN_POINT('Ctrl Pts',(4.5499342195639,1.21487743324952,38.6541104560075));
#45881=CARTESIAN_POINT('Ctrl Pts',(3.41469164371823,3.24310184347568,38.733482346061));
#45882=CARTESIAN_POINT('Ctrl Pts',(1.44763774336306,4.48131381605587,38.8128542361143));
#45883=CARTESIAN_POINT('Ctrl Pts',(-0.872057510020701,4.62788767559439,
38.8922261261678));
#45884=CARTESIAN_POINT('Ctrl Pts',(-2.9793214784951,3.6471183158447,38.9715980162212));
#45885=CARTESIAN_POINT('Ctrl Pts',(-4.36082934025308,1.77791905463904,39.0509699062746));
#45886=CARTESIAN_POINT('Ctrl Pts',(-4.68004880681061,-0.524377442655287,
39.130341796328));
#45887=CARTESIAN_POINT('Ctrl Pts',(-3.85921878174905,-2.6989365861694,39.2097136863814));
#45888=CARTESIAN_POINT('Ctrl Pts',(-2.09829153079023,-4.21604107122303,
39.2890855764348));
#45889=CARTESIAN_POINT('Ctrl Pts',(0.173774754931348,-4.70612667927191,
39.3684574664882));
#45890=CARTESIAN_POINT('Ctrl Pts',(2.40351015490339,-4.04981138575493,39.4478293565416));
#45891=CARTESIAN_POINT('Ctrl Pts',(4.04775531046155,-2.40696884895629,39.527201246595));
#45892=CARTESIAN_POINT('Ctrl Pts',(4.70597715859854,-0.177798095133498,
39.6065731366484));
#45893=CARTESIAN_POINT('Ctrl Pts',(4.21783163769349,2.0946915601602,39.6859450267019));
#45894=CARTESIAN_POINT('Ctrl Pts',(2.70223496968604,3.85690448821556,39.7653169167552));
#45895=CARTESIAN_POINT('Ctrl Pts',(0.528373605920714,4.67961139929736,39.8446888068086));
#45896=CARTESIAN_POINT('Ctrl Pts',(-1.77418661813221,4.36232362711485,39.9240606968621));
#45897=CARTESIAN_POINT('Ctrl Pts',(-3.6445811625546,2.98248116081159,40.0034325869154));
#45898=CARTESIAN_POINT('Ctrl Pts',(-4.62712170766669,0.875927969712799,
40.0828044769689));
#45899=CARTESIAN_POINT('Ctrl Pts',(-4.48258575488106,-1.44364637546354,
40.1621763670223));
#45900=CARTESIAN_POINT('Ctrl Pts',(-3.24594541476057,-3.41224896374515,
40.2415482570757));
#45901=CARTESIAN_POINT('Ctrl Pts',(-1.89461073269764,-4.16947670058303,
40.2944628504446));
#45902=CARTESIAN_POINT('Ctrl Pts',(-1.16918346556913,-4.36383719750631,
40.3209201471291));
#45903=CARTESIAN_POINT('Ctrl Pts',(-3.57461543774205,3.05624720968391,-0.106973382376353));
#45904=CARTESIAN_POINT('Ctrl Pts',(-4.08267404777841,2.46201708819397,-0.0805160856918847));
#45905=CARTESIAN_POINT('Ctrl Pts',(-4.79625497710715,1.01593427979912,-0.027601492322949));
#45906=CARTESIAN_POINT('Ctrl Pts',(-4.69765387924802,-1.40219731261579,
0.051770397730455));
#45907=CARTESIAN_POINT('Ctrl Pts',(-3.45499130789169,-3.47806613859392,
0.131142287783858));
#45908=CARTESIAN_POINT('Ctrl Pts',(-1.37056128557091,-4.70703587006775,
0.210514177837262));
#45909=CARTESIAN_POINT('Ctrl Pts',(1.04766160592227,-4.78919858119765,0.289886067890666));
#45910=CARTESIAN_POINT('Ctrl Pts',(3.21071490770584,-3.70482006635648,0.36925795794407));
#45911=CARTESIAN_POINT('Ctrl Pts',(4.59162481050196,-1.71790426872487,0.448629847997472));
#45912=CARTESIAN_POINT('Ctrl Pts',(4.85403585089543,0.687462033087635,0.528001738050878));
#45913=CARTESIAN_POINT('Ctrl Pts',(3.93400879434301,2.92537849589629,0.607373628104279));
#45914=CARTESIAN_POINT('Ctrl Pts',(2.05566892616791,4.45067161106188,0.686745518157684));
#45915=CARTESIAN_POINT('Ctrl Pts',(-0.323428943211738,4.89179500940945,
0.766117408211087));
#45916=CARTESIAN_POINT('Ctrl Pts',(-2.62373939006112,4.1412858336604,0.845489298264492));
#45917=CARTESIAN_POINT('Ctrl Pts',(-4.28491317807112,2.38196972749854,0.924861188317894));
#45918=CARTESIAN_POINT('Ctrl Pts',(-4.90229136258891,0.042410468561284,
1.0042330783713));
#45919=CARTESIAN_POINT('Ctrl Pts',(-4.32548234816227,-2.30747956911558,
1.0836049684247));
#45920=CARTESIAN_POINT('Ctrl Pts',(-2.69499534131545,-4.09527285943935,
1.16297685847811));
#45921=CARTESIAN_POINT('Ctrl Pts',(-0.408013469920106,-4.88546665687605,
1.24234874853151));
#45922=CARTESIAN_POINT('Ctrl Pts',(1.97835959833349,-4.48557163766149,1.32172063858491));
#45923=CARTESIAN_POINT('Ctrl Pts',(3.8828086375498,-2.99300127117732,1.40109252863832));
#45924=CARTESIAN_POINT('Ctrl Pts',(4.84141409235741,-0.771342433159628,
1.48046441869172));
#45925=CARTESIAN_POINT('Ctrl Pts',(4.62066178777609,1.63821372124453,1.55983630874512));
#45926=CARTESIAN_POINT('Ctrl Pts',(3.27432650082566,3.64870463556752,1.63920819879853));
#45927=CARTESIAN_POINT('Ctrl Pts',(1.13037252509344,4.77037917890212,1.71858008885193));
#45928=CARTESIAN_POINT('Ctrl Pts',(-1.2889376953016,4.72999991227064,1.79795197890533));
#45929=CARTESIAN_POINT('Ctrl Pts',(-3.394265546355,3.53740313723842,1.87732386895874));
#45930=CARTESIAN_POINT('Ctrl Pts',(-4.67275782327988,1.48310278759205,1.95669575901214));
#45931=CARTESIAN_POINT('Ctrl Pts',(-4.81297663748911,-0.9324781181648,2.03606764906555));
#45932=CARTESIAN_POINT('Ctrl Pts',(-3.78076499611659,-3.12090941842389,
2.11543953911895));
#45933=CARTESIAN_POINT('Ctrl Pts',(-1.82756737028867,-4.54909409232738,
2.19481142917235));
#45934=CARTESIAN_POINT('Ctrl Pts',(0.57082162169894,-4.86912951461188,2.27418331922576));
#45935=CARTESIAN_POINT('Ctrl Pts',(2.8301597301281,-4.00305576476012,2.35355520927916));
#45936=CARTESIAN_POINT('Ctrl Pts',(4.40007719275289,-2.16184649123289,2.43292709933256));
#45937=CARTESIAN_POINT('Ctrl Pts',(4.89814559062742,0.205983802396055,2.51229898938597));
#45938=CARTESIAN_POINT('Ctrl Pts',(4.20303656448716,2.52363689769692,2.59167087943937));
#45939=CARTESIAN_POINT('Ctrl Pts',(2.48407713450111,4.22653763069529,2.67104276949277));
#45940=CARTESIAN_POINT('Ctrl Pts',(0.160002012962259,4.89986315213815,2.75041465954618));
#45941=CARTESIAN_POINT('Ctrl Pts',(-2.20304924477586,4.37959285538356,2.82978654959959));
#45942=CARTESIAN_POINT('Ctrl Pts',(-4.02944258285332,2.79246343312173,2.90915843965298));
#45943=CARTESIAN_POINT('Ctrl Pts',(-4.8742726267676,0.525096099564501,2.9885303297064));
#45944=CARTESIAN_POINT('Ctrl Pts',(-4.53174064782075,-1.87018348156618,
3.06790221975979));
#45945=CARTESIAN_POINT('Ctrl Pts',(-3.08528667790254,-3.80989050616825,
3.1472741098132));
#45946=CARTESIAN_POINT('Ctrl Pts',(-0.887263702413488,-4.82151663651732,
3.2266459998666));
#45947=CARTESIAN_POINT('Ctrl Pts',(1.52689474705858,-4.65863198645683,3.30601788992001));
#45948=CARTESIAN_POINT('Ctrl Pts',(3.56910501587138,-3.36091489620245,3.38538977997341));
#45949=CARTESIAN_POINT('Ctrl Pts',(4.74188920289787,-1.24448637649211,3.46476167002681));
#45950=CARTESIAN_POINT('Ctrl Pts',(4.75955967609216,1.17509626990786,3.54413356008022));
#45951=CARTESIAN_POINT('Ctrl Pts',(3.61781194729703,3.30842806598974,3.62350545013362));
#45952=CARTESIAN_POINT('Ctrl Pts',(1.59477323603129,4.63583410827783,3.70287734018703));
#45953=CARTESIAN_POINT('Ctrl Pts',(-0.816748705561003,4.83396122303419,
3.78224923024042));
#45954=CARTESIAN_POINT('Ctrl Pts',(-3.02931247032122,3.85454608365112,3.86162112029383));
#45955=CARTESIAN_POINT('Ctrl Pts',(-4.50394242258063,1.93617205018365,3.94099301034724));
#45956=CARTESIAN_POINT('Ctrl Pts',(-4.88142197000684,-0.453849209064403,
4.02036490040064));
#45957=CARTESIAN_POINT('Ctrl Pts',(-4.06979793038364,-2.73331380556256,
4.09973679045404));
#45958=CARTESIAN_POINT('Ctrl Pts',(-2.2667801232639,-4.34694920911316,4.17910868050745));
#45959=CARTESIAN_POINT('Ctrl Pts',(0.0884203044502142,-4.90167740713265,
4.25848057056085));
#45960=CARTESIAN_POINT('Ctrl Pts',(2.42208174171528,-4.26236783845356,4.33785246061425));
#45961=CARTESIAN_POINT('Ctrl Pts',(4.16572942788551,-2.58475489891836,4.41722435066765));
#45962=CARTESIAN_POINT('Ctrl Pts',(4.89461464610853,-0.277501387264568,
4.49659624072106));
#45963=CARTESIAN_POINT('Ctrl Pts',(4.43118257058524,2.09735084808797,4.57596813077446));
#45964=CARTESIAN_POINT('Ctrl Pts',(2.88832422912366,3.96129305925364,4.65534002082787));
#45965=CARTESIAN_POINT('Ctrl Pts',(0.641876498644775,4.86027304935857,4.73471191088126));
#45966=CARTESIAN_POINT('Ctrl Pts',(-1.76093092613442,4.57530128267169,4.81408380093468));
#45967=CARTESIAN_POINT('Ctrl Pts',(-3.73477947506178,3.17579625078358,4.89345569098808));
#45968=CARTESIAN_POINT('Ctrl Pts',(-4.79884401065823,1.00267428171038,4.97282758104148));
#45969=CARTESIAN_POINT('Ctrl Pts',(-4.6939207673194,-1.41469692300561,5.05219947109488));
#45970=CARTESIAN_POINT('Ctrl Pts',(-3.44556881487893,-3.48745108865595,
5.13157136114829));
#45971=CARTESIAN_POINT('Ctrl Pts',(-1.35788392577118,-4.71066988845176,
5.21094325120169));
#45972=CARTESIAN_POINT('Ctrl Pts',(1.06057848202937,-4.78637993031164,5.2903151412551));
#45973=CARTESIAN_POINT('Ctrl Pts',(3.22068631915819,-3.69613841561989,5.3696870313085));
#45974=CARTESIAN_POINT('Ctrl Pts',(4.59624209780833,-1.70552576414673,5.44905892136191));
#45975=CARTESIAN_POINT('Ctrl Pts',(4.85216347504167,0.700549188355308,5.52843081141531));
#45976=CARTESIAN_POINT('Ctrl Pts',(3.92610856983656,2.93597190921332,5.60780270146871));
#45977=CARTESIAN_POINT('Ctrl Pts',(2.04366230731317,4.45619837165057,5.68717459152211));
#45978=CARTESIAN_POINT('Ctrl Pts',(-0.336615569701915,4.89090477438153,
5.76654648157553));
#45979=CARTESIAN_POINT('Ctrl Pts',(-2.63489463902355,4.13419759990724,5.84591837162891));
#45980=CARTESIAN_POINT('Ctrl Pts',(-4.29131920651939,2.37040904098672,5.92529026168234));
#45981=CARTESIAN_POINT('Ctrl Pts',(-4.90238791398106,0.0291940864932555,
6.00466215173572));
#45982=CARTESIAN_POINT('Ctrl Pts',(-4.31924577684855,-2.31913248284995,
6.08403404178914));
#45983=CARTESIAN_POINT('Ctrl Pts',(-2.68394492896408,-4.1025235126836,6.16340593184253));
#45984=CARTESIAN_POINT('Ctrl Pts',(-0.394841037195299,-4.88654889560929,
6.24277782189594));
#45985=CARTESIAN_POINT('Ctrl Pts',(1.99044525726845,-4.48022178375707,6.32214971194934));
#45986=CARTESIAN_POINT('Ctrl Pts',(3.89086349283745,-2.98252256218433,6.40152160200274));
#45987=CARTESIAN_POINT('Ctrl Pts',(4.84347599383151,-0.758287446165202,
6.48089349205615));
#45988=CARTESIAN_POINT('Ctrl Pts',(4.61622846358046,1.65066481329898,6.56026538210956));
#45989=CARTESIAN_POINT('Ctrl Pts',(3.26447789744962,3.65751877792811,6.63963727216296));
#45990=CARTESIAN_POINT('Ctrl Pts',(1.11750774129931,4.77340926403445,6.71900916221636));
#45991=CARTESIAN_POINT('Ctrl Pts',(-1.30168482707007,4.7265078191842,6.79838105226977));
#45992=CARTESIAN_POINT('Ctrl Pts',(-3.4037898527957,3.52823953152828,6.87775294232317));
#45993=CARTESIAN_POINT('Ctrl Pts',(-4.67673920454132,1.4704999036178,6.95712483237657));
#45994=CARTESIAN_POINT('Ctrl Pts',(-4.81044523784733,-0.945450245917632,
7.03649672242998));
#45995=CARTESIAN_POINT('Ctrl Pts',(-3.77233745895366,-3.13109080826615,
7.11586861248337));
#45996=CARTESIAN_POINT('Ctrl Pts',(-1.81529662498623,-4.554004580273,7.19524050253679));
#45997=CARTESIAN_POINT('Ctrl Pts',(0.583946448736947,-4.8675729166435,7.27461239259018));
#45998=CARTESIAN_POINT('Ctrl Pts',(2.84094146009133,-3.99541126470955,7.3539842826436));
#45999=CARTESIAN_POINT('Ctrl Pts',(4.40588942008474,-2.14997627238517,7.433356172697));
#46000=CARTESIAN_POINT('Ctrl Pts',(4.8975724696163,0.219188181000477,7.51272806275039));
#46001=CARTESIAN_POINT('Ctrl Pts',(4.19621770614212,2.53495887865921,7.59209995280381));
#46002=CARTESIAN_POINT('Ctrl Pts',(2.47267359762208,4.23321920451286,7.6714718428572));
#46003=CARTESIAN_POINT('Ctrl Pts',(0.14679167389147,4.90027670221897,7.75084373291062));
#46004=CARTESIAN_POINT('Ctrl Pts',(-2.21484837668125,4.37363764184302,7.83021562296401));
#46005=CARTESIAN_POINT('Ctrl Pts',(-4.03695626517815,2.78159013279685,7.90958751301742));
#46006=CARTESIAN_POINT('Ctrl Pts',(-4.87567054312876,0.511953424346666,
7.98895940307082));
#46007=CARTESIAN_POINT('Ctrl Pts',(-4.52668226888691,-1.88239400508467,
8.06833129312423));
#46008=CARTESIAN_POINT('Ctrl Pts',(-3.07500421358545,-3.81819442148583,
8.14770318317762));
#46009=CARTESIAN_POINT('Ctrl Pts',(-0.874261938260974,-4.82389112824304,
8.22707507323104));
#46010=CARTESIAN_POINT('Ctrl Pts',(1.53944861007788,-4.65449863366217,8.30644696328443));
#46011=CARTESIAN_POINT('Ctrl Pts',(3.5781528845135,-3.35128057447919,8.38581885333784));
#46012=CARTESIAN_POINT('Ctrl Pts',(4.74522703638871,-1.23169798528678,8.46519074339124));
#46013=CARTESIAN_POINT('Ctrl Pts',(4.75637438558149,1.18792350680425,8.54456263344465));
#46014=CARTESIAN_POINT('Ctrl Pts',(3.60887946250276,3.31816946206181,8.62393452349805));
#46015=CARTESIAN_POINT('Ctrl Pts',(1.58226949047756,4.64011668100466,8.70330641355145));
#46016=CARTESIAN_POINT('Ctrl Pts',(-0.829777827133893,4.83174174717884,
8.78267830360486));
#46017=CARTESIAN_POINT('Ctrl Pts',(-3.03969310273758,3.84636521861918,8.86205019365827));
#46018=CARTESIAN_POINT('Ctrl Pts',(-4.50914586676094,1.9240226365889,8.94142208371166));
#46019=CARTESIAN_POINT('Ctrl Pts',(-4.88018067846642,-0.467007600962554,
9.02079397376508));
#46020=CARTESIAN_POINT('Ctrl Pts',(-4.0624142789942,-2.74427582062334,9.10016586381847));
#46021=CARTESIAN_POINT('Ctrl Pts',(-2.25505275316047,-4.35304452473175,
9.17953775387187));
#46022=CARTESIAN_POINT('Ctrl Pts',(0.101634631868527,-4.90142121791617,
9.25890964392528));
#46023=CARTESIAN_POINT('Ctrl Pts',(2.4335640455388,-4.25582255152803,9.33828153397868));
#46024=CARTESIAN_POINT('Ctrl Pts',(4.17268264431847,-2.57351493169112,9.41765342403209));
#46025=CARTESIAN_POINT('Ctrl Pts',(4.89534498701854,-0.264304770872935,
9.49702531408549));
#46026=CARTESIAN_POINT('Ctrl Pts',(4.42551212654324,2.10928944710123,9.57639720413889));
#46027=CARTESIAN_POINT('Ctrl Pts',(2.8776343077469,3.96906542459454,9.65576909419229));
#46028=CARTESIAN_POINT('Ctrl Pts',(0.628771141118955,4.86198585003388,9.73514098424571));
#46029=CARTESIAN_POINT('Ctrl Pts',(-1.77325928372426,4.57053728422814,9.81451287429909));
#46030=CARTESIAN_POINT('Ctrl Pts',(-3.74332767209512,3.16571595269709,9.89388476435253));
#46031=CARTESIAN_POINT('Ctrl Pts',(-4.80152972525885,0.989733222282404,
9.97325665440589));
#46032=CARTESIAN_POINT('Ctrl Pts',(-4.69008976535528,-1.42734633034291,
10.0526285444593));
#46033=CARTESIAN_POINT('Ctrl Pts',(-3.43615431994881,-3.49672747627419,
10.1320004345127));
#46034=CARTESIAN_POINT('Ctrl Pts',(-1.34517928800141,-4.71431354886008,
10.2113723245661));
#46035=CARTESIAN_POINT('Ctrl Pts',(1.07347844099931,-4.78350327589974,10.2907442146195));
#46036=CARTESIAN_POINT('Ctrl Pts',(3.23063919787684,-3.68744219303511,10.3701161046729));
#46037=CARTESIAN_POINT('Ctrl Pts',(4.60082339705013,-1.69312835396196,10.4494879947263));
#46038=CARTESIAN_POINT('Ctrl Pts',(4.85025720045185,0.713627804460256,10.5288598847798));
#46039=CARTESIAN_POINT('Ctrl Pts',(3.91817908568572,2.94654580930431,10.6082317748331));
#46040=CARTESIAN_POINT('Ctrl Pts',(2.03164121838884,4.46169177707037,10.6876036648866));
#46041=CARTESIAN_POINT('Ctrl Pts',(-0.349799952746016,4.8899795037293,10.7669755549399));
#46042=CARTESIAN_POINT('Ctrl Pts',(-2.64603062966098,4.12707904706582,10.8463474449934));
#46043=CARTESIAN_POINT('Ctrl Pts',(-4.29769410207999,2.35883126967163,10.9257193350467));
#46044=CARTESIAN_POINT('Ctrl Pts',(-4.90244880401686,0.0159774161698882,
11.0050912251002));
#46045=CARTESIAN_POINT('Ctrl Pts',(-4.31297782868159,-2.33076850054543,
11.0844631151536));
#46046=CARTESIAN_POINT('Ctrl Pts',(-2.672875000894,-4.10974436959645,11.163835005207));
#46047=CARTESIAN_POINT('Ctrl Pts',(-0.381665739197088,-4.88759560697865,
11.2432068952604));
#46048=CARTESIAN_POINT('Ctrl Pts',(2.00251645176545,-4.47483937301022,11.3225787853138));
#46049=CARTESIAN_POINT('Ctrl Pts',(3.89889006757291,-2.97202217266546,11.4019506753672));
#46050=CARTESIAN_POINT('Ctrl Pts',(4.84550269296641,-0.745226949518873,
11.4813225654206));
#46051=CARTESIAN_POINT('Ctrl Pts',(4.61176158769154,1.66310390899864,11.560694455474));
#46052=CARTESIAN_POINT('Ctrl Pts',(3.25460556761616,3.66630633650213,11.6400663455274));
#46053=CARTESIAN_POINT('Ctrl Pts',(1.10463483521672,4.77640465566513,11.7194382355808));
#46054=CARTESIAN_POINT('Ctrl Pts',(-1.3144224979738,4.72298137310049,11.7988101256342));
#46055=CARTESIAN_POINT('Ctrl Pts',(-3.41328942008276,3.51905028219049,11.8781820156876));
#46056=CARTESIAN_POINT('Ctrl Pts',(-4.6806865946475,1.45788633182458,11.957553905741));
#46057=CARTESIAN_POINT('Ctrl Pts',(-4.80787887528018,-0.95841550199713,
12.0369257957944));
#46058=CARTESIAN_POINT('Ctrl Pts',(-3.76388250395398,-3.14124944094907,
12.1162976858478));
#46059=CARTESIAN_POINT('Ctrl Pts',(-1.80301268587722,-4.55888196912352,
12.1956695759012));
#46060=CARTESIAN_POINT('Ctrl Pts',(0.59706703157835,-4.86598094053357,12.2750414659546));
#46061=CARTESIAN_POINT('Ctrl Pts',(2.8517025417269,-3.98773772549578,12.354413356008));
#46062=CARTESIAN_POINT('Ctrl Pts',(4.41166962484727,-2.13809042723494,12.4337852460614));
#46063=CARTESIAN_POINT('Ctrl Pts',(4.89696375241996,0.232390966517433,12.5131571361148));
#46064=CARTESIAN_POINT('Ctrl Pts',(4.18936834914853,2.54626243521486,12.5925290261683));
#46065=CARTESIAN_POINT('Ctrl Pts',(2.46125208903407,4.23987001075024,12.6719009162216));
#46066=CARTESIAN_POINT('Ctrl Pts',(0.133580267920011,4.90065463645993,12.751272806275));
#46067=CARTESIAN_POINT('Ctrl Pts',(-2.22663141078444,4.36765064014303,12.8306446963284));
#46068=CARTESIAN_POINT('Ctrl Pts',(-4.04444060638688,2.770696615518,12.9100165863818));
#46069=CARTESIAN_POINT('Ctrl Pts',(-4.87703302249085,0.498807028185692,
12.9893884764353));
#46070=CARTESIAN_POINT('Ctrl Pts',(-4.52159098944558,-1.89459084712199,
13.0687603664886));
#46071=CARTESIAN_POINT('Ctrl Pts',(-3.06469939974324,-3.82647058567648,
13.1481322565421));
#46072=CARTESIAN_POINT('Ctrl Pts',(-0.861253819860521,-4.82623055930914,
13.2275041465954));
#46073=CARTESIAN_POINT('Ctrl Pts',(1.55199128418723,-4.65033145137426,13.3068760366489));
#46074=CARTESIAN_POINT('Ctrl Pts',(3.58717474668141,-3.34162189521869,13.3862479267023));
#46075=CARTESIAN_POINT('Ctrl Pts',(4.74853038096063,-1.21890064194246,13.4656198167557));
#46076=CARTESIAN_POINT('Ctrl Pts',(4.75315452513156,1.20074210972015,13.5449917068091));
#46077=CARTESIAN_POINT('Ctrl Pts',(3.59992074790953,3.32788674125251,13.6243635968625));
#46078=CARTESIAN_POINT('Ctrl Pts',(1.56975424478615,4.64436552876813,13.7037354869159));
#46079=CARTESIAN_POINT('Ctrl Pts',(-0.842800917775063,4.82948715360455,
13.7831073769693));
#46080=CARTESIAN_POINT('Ctrl Pts',(-3.05005164227443,3.83815639771137,13.8624792670227));
#46081=CARTESIAN_POINT('Ctrl Pts',(-4.51431653789056,1.91185923895083,13.9418511570761));
#46082=CARTESIAN_POINT('Ctrl Pts',(-4.87890391714672,-0.480162598589543,
14.0212230471295));
#46083=CARTESIAN_POINT('Ctrl Pts',(-4.05500110145656,-2.75521788993537,
14.1005949371829));
#46084=CARTESIAN_POINT('Ctrl Pts',(-2.24330899304429,-4.35910820186428,
14.1799668272363));
#46085=CARTESIAN_POINT('Ctrl Pts',(0.114848220593315,-4.90112940454139,
14.2593387172897));
#46086=CARTESIAN_POINT('Ctrl Pts',(2.4450286619066,-4.2492463327382,14.3387106073431));
#46087=CARTESIAN_POINT('Ctrl Pts',(4.17960553315863,-2.56225625982719,14.4180824973965));
#46088=CARTESIAN_POINT('Ctrl Pts',(4.89603974793314,-0.2511062334803,14.4974543874499));
#46089=CARTESIAN_POINT('Ctrl Pts',(4.41980951731128,2.12121271552818,14.5768262775033));
#46090=CARTESIAN_POINT('Ctrl Pts',(2.86692347135483,3.97680894225867,14.6561981675567));
#46091=CARTESIAN_POINT('Ctrl Pts',(0.615661213603817,4.86366331317225,14.7355700576101));
#46092=CARTESIAN_POINT('Ctrl Pts',(-1.78557475303814,4.56574006653321,14.8149419476636));
#46093=CARTESIAN_POINT('Ctrl Pts',(-3.75184866214265,3.15561264578087,14.8943138377169));
#46094=CARTESIAN_POINT('Ctrl Pts',(-4.80418054172537,0.976784969346447,
14.9736857277704));
#46095=CARTESIAN_POINT('Ctrl Pts',(-4.68622467521704,-1.43998536354391,
15.0530576178237));
#46096=CARTESIAN_POINT('Ctrl Pts',(-3.42671485060823,-3.50597844922854,
15.1324295078772));
#46097=CARTESIAN_POINT('Ctrl Pts',(-1.33246487329588,-4.71792294503274,
15.2118013979305));
#46098=CARTESIAN_POINT('Ctrl Pts',(1.08637059779033,-4.78059185437226,15.291173287984));
#46099=CARTESIAN_POINT('Ctrl Pts',(3.24056859589536,-3.67871916964732,15.3705451780373));
#46100=CARTESIAN_POINT('Ctrl Pts',(4.60537125691718,-1.68071863790306,15.4499170680908));
#46101=CARTESIAN_POINT('Ctrl Pts',(4.84831567357043,0.726701233826767,15.5292889581442));
#46102=CARTESIAN_POINT('Ctrl Pts',(3.91022112370653,2.95709829352236,15.6086608481976));
#46103=CARTESIAN_POINT('Ctrl Pts',(2.01960536323555,4.46715275434186,15.688032738251));
#46104=CARTESIAN_POINT('Ctrl Pts',(-0.362981793399331,4.88901869207872,
15.7674046283044));
#46105=CARTESIAN_POINT('Ctrl Pts',(-2.65714738860797,4.11993049808428,15.8467765183578));
#46106=CARTESIAN_POINT('Ctrl Pts',(-4.3040377614491,2.34723635406844,15.9261484084112));
#46107=CARTESIAN_POINT('Ctrl Pts',(-4.90247406242457,0.00276062972017743,
16.0055202984646));
#46108=CARTESIAN_POINT('Ctrl Pts',(-4.30667853324066,-2.34238757791569,
16.084892188518));
#46109=CARTESIAN_POINT('Ctrl Pts',(-2.66178564602119,-4.11693535636137,
16.1642640785714));
#46110=CARTESIAN_POINT('Ctrl Pts',(-0.368487667211246,-4.88860679467341,
16.2436359686248));
#46111=CARTESIAN_POINT('Ctrl Pts',(2.01457309173119,-4.46942443856166,16.3230078586782));
#46112=CARTESIAN_POINT('Ctrl Pts',(3.90688830464663,-2.96150018209857,16.4023797487316));
#46113=CARTESIAN_POINT('Ctrl Pts',(4.84749417442,-0.732161036485258,16.481751638785));
#46114=CARTESIAN_POINT('Ctrl Pts',(4.60726119282582,1.67553091707946,16.5611235288384));
#46115=CARTESIAN_POINT('Ctrl Pts',(3.24470958308425,3.67506724782763,16.6404954188918));
#46116=CARTESIAN_POINT('Ctrl Pts',(1.09175390014313,4.77936533189424,16.7198673089452));
#46117=CARTESIAN_POINT('Ctrl Pts',(-1.32715061480029,4.7194205995551,16.7992391989986));
#46118=CARTESIAN_POINT('Ctrl Pts',(-3.42276418043948,3.50983545637255,16.878611089052));
#46119=CARTESIAN_POINT('Ctrl Pts',(-4.68459996247752,1.44526216311684,16.9579829791054));
#46120=CARTESIAN_POINT('Ctrl Pts',(-4.80527757305004,-0.971373790661056,
17.0373548691589));
#46121=CARTESIAN_POINT('Ctrl Pts',(-3.75540018385452,-3.15138524551466,
17.1167267592122));
#46122=CARTESIAN_POINT('Ctrl Pts',(-1.79071565870356,-4.56372621798453,
17.1960986492656));
#46123=CARTESIAN_POINT('Ctrl Pts',(0.610183305945333,-4.86435360814148,
17.275470539319));
#46124=CARTESIAN_POINT('Ctrl Pts',(2.86244283812717,-3.98003518345987,17.3548424293725));
#46125=CARTESIAN_POINT('Ctrl Pts',(4.41741787585788,-2.1261890788619,17.4342143194258));
#46126=CARTESIAN_POINT('Ctrl Pts',(4.89631923419534,0.245592132270697,17.5135862094793));
#46127=CARTESIAN_POINT('Ctrl Pts',(4.1824889384277,2.55754735438707,17.5929580995327));
#46128=CARTESIAN_POINT('Ctrl Pts',(2.44981194564648,4.24649024808584,17.6723299895861));
#46129=CARTESIAN_POINT('Ctrl Pts',(0.120369299865439,4.90099648569508,17.7517018796395));
#46130=CARTESIAN_POINT('Ctrl Pts',(-2.2384009215371,4.36163277449207,17.8310737696929));
#46131=CARTESIAN_POINT('Ctrl Pts',(-4.0518905292873,2.75978129753081,17.9104456597463));
#46132=CARTESIAN_POINT('Ctrl Pts',(-4.87836953900975,0.485660146581001,
17.9898175497997));
#46133=CARTESIAN_POINT('Ctrl Pts',(-4.51644893866981,-1.90677984789346,
18.0691894398531));
#46134=CARTESIAN_POINT('Ctrl Pts',(-3.05440612489714,-3.83470774368921,
18.1485613299065));
#46135=CARTESIAN_POINT('Ctrl Pts',(-0.848175594775907,-4.82855605094715,
18.2279332199599));
#46136=CARTESIAN_POINT('Ctrl Pts',(1.56440212229575,-4.64609055668262,18.3073051100133));
#46137=CARTESIAN_POINT('Ctrl Pts',(3.59639816964341,-3.33201429213606,18.3866770000667));
#46138=CARTESIAN_POINT('Ctrl Pts',(4.75136940590255,-1.20595214372204,18.4660488901201));
#46139=CARTESIAN_POINT('Ctrl Pts',(4.75071159562135,1.21328335035095,18.5454207801735));
#46140=CARTESIAN_POINT('Ctrl Pts',(3.58940432897552,3.33808667681415,18.6247926702269));
#46141=CARTESIAN_POINT('Ctrl Pts',(1.56011376732896,4.64762681676405,18.7041645602803));
#46142=CARTESIAN_POINT('Ctrl Pts',(-0.861221142909775,4.82897211168874,
18.7835364503337));
#46143=CARTESIAN_POINT('Ctrl Pts',(-3.05056344532316,3.82678328180746,18.8629083403871));
#46144=CARTESIAN_POINT('Ctrl Pts',(-5.02992785007326,1.26296632184503,18.968737527125));
#46145=CARTESIAN_POINT('Ctrl Pts',(-4.59246965375637,-3.13076985705441,
19.1010240105473));
#46146=CARTESIAN_POINT('Ctrl Pts',(0.146932230206506,-5.55932874556365,
19.2597677906541));
#46147=CARTESIAN_POINT('Ctrl Pts',(4.74574684718979,-2.89085235699285,19.418511570761));
#46148=CARTESIAN_POINT('Ctrl Pts',(5.00517315099097,2.41778366488237,19.5772553508677));
#46149=CARTESIAN_POINT('Ctrl Pts',(0.682914143844855,5.5166676123404,19.7359991309746));
#46150=CARTESIAN_POINT('Ctrl Pts',(-4.26335305224441,3.56621538027044,19.8947429110814));
#46151=CARTESIAN_POINT('Ctrl Pts',(-5.30889903625343,-1.64699798333531,
20.0534866911882));
#46152=CARTESIAN_POINT('Ctrl Pts',(-1.49629817009909,-5.35305176256659,
20.212230471295));
#46153=CARTESIAN_POINT('Ctrl Pts',(3.68539651252336,-4.16147159288513,20.3709742514018));
#46154=CARTESIAN_POINT('Ctrl Pts',(5.49476366156206,0.839647798276105,20.5297180315086));
#46155=CARTESIAN_POINT('Ctrl Pts',(2.27623920304293,5.06930720888698,20.6884618116154));
#46156=CARTESIAN_POINT('Ctrl Pts',(-3.02540872545025,4.66632909528393,20.8472055917223));
#46157=CARTESIAN_POINT('Ctrl Pts',(-5.55807194231375,-0.0182675279713449,
21.005949371829));
#46158=CARTESIAN_POINT('Ctrl Pts',(-3.4318929716806,-3.88810606053727,21.1382358552514));
#46159=CARTESIAN_POINT('Ctrl Pts',(-0.348982623888803,-4.88143613581972,
21.2440650419892));
#46160=CARTESIAN_POINT('Ctrl Pts',(2.02316502874914,-4.46849826887164,21.3234369320426));
#46161=CARTESIAN_POINT('Ctrl Pts',(3.91669769333085,-2.94853678524969,21.4028088220961));
#46162=CARTESIAN_POINT('Ctrl Pts',(4.84847467696001,-0.720374489880037,
21.4821807121494));
#46163=CARTESIAN_POINT('Ctrl Pts',(4.60324425657816,1.68862650319429,21.5615526022029));
#46164=CARTESIAN_POINT('Ctrl Pts',(3.23451621663553,3.68344087079137,21.6409244922562));
#46165=CARTESIAN_POINT('Ctrl Pts',(1.07901003836815,4.78248223987442,21.7202963823097));
#46166=CARTESIAN_POINT('Ctrl Pts',(-1.33994588402651,4.71572438645636,21.7996682723631));
#46167=CARTESIAN_POINT('Ctrl Pts',(-3.4321733891171,3.50064868327975,21.8790401624164));
#46168=CARTESIAN_POINT('Ctrl Pts',(-4.68850082698247,1.43259912421573,21.9584120524699));
#46169=CARTESIAN_POINT('Ctrl Pts',(-4.80262992851033,-0.984309998791622,
22.0377839425233));
#46170=CARTESIAN_POINT('Ctrl Pts',(-3.74689662802585,-3.16150609615164,
22.1171558325767));
#46171=CARTESIAN_POINT('Ctrl Pts',(-1.77840238381691,-4.56853309419591,
22.1965277226301));
#46172=CARTESIAN_POINT('Ctrl Pts',(0.62329338871143,-4.86269313206684,22.2758996126835));
#46173=CARTESIAN_POINT('Ctrl Pts',(2.87316334475109,-3.97230257099384,22.3552715027369));
#46174=CARTESIAN_POINT('Ctrl Pts',(4.4231333235665,-2.11427282962158,22.4346433927903));
#46175=CARTESIAN_POINT('Ctrl Pts',(4.89563979914059,0.258791705958885,22.5140152828437));
#46176=CARTESIAN_POINT('Ctrl Pts',(4.17557820525643,2.56881377105699,22.5933871728971));
#46177=CARTESIAN_POINT('Ctrl Pts',(2.43835555951363,4.25307922033076,22.6727590629505));
#46178=CARTESIAN_POINT('Ctrl Pts',(0.107154601980389,4.90130359745224,22.7521309530039));
#46179=CARTESIAN_POINT('Ctrl Pts',(-2.25014882333759,4.35558147263095,22.8315028430573));
#46180=CARTESIAN_POINT('Ctrl Pts',(-4.05932105856842,2.74884923313531,22.9108747331107));
#46181=CARTESIAN_POINT('Ctrl Pts',(-4.87965162531074,0.472503462573818,
22.9902466231641));
#46182=CARTESIAN_POINT('Ctrl Pts',(-4.51130988023697,-1.91894313613435,
23.0696185132175));
#46183=CARTESIAN_POINT('Ctrl Pts',(-3.04402302167418,-3.84293941821872,
23.1489904032709));
#46184=CARTESIAN_POINT('Ctrl Pts',(-0.835218899364871,-4.83080417279082,
23.2283622933243));
#46185=CARTESIAN_POINT('Ctrl Pts',(1.57704270154782,-4.64189571913938,23.3077341833777));
#46186=CARTESIAN_POINT('Ctrl Pts',(3.60514018926443,-3.32223174536946,23.3871060734312));
#46187=CARTESIAN_POINT('Ctrl Pts',(4.75503350768461,-1.19327947079072,23.4664779634845));
#46188=CARTESIAN_POINT('Ctrl Pts',(4.74661118820946,1.22635304091963,23.545849853538));
#46189=CARTESIAN_POINT('Ctrl Pts',(3.58192489000304,3.34724866670522,23.6252217435913));
#46190=CARTESIAN_POINT('Ctrl Pts',(1.54468961690465,4.65276192610169,23.7045936336447));
#46191=CARTESIAN_POINT('Ctrl Pts',(-0.868828627683255,4.82487267911367,
23.7839655236982));
#46192=CARTESIAN_POINT('Ctrl Pts',(-3.0707021417273,3.8216551271151,23.8633374137516));
#46193=CARTESIAN_POINT('Ctrl Pts',(-4.52455941090918,1.88749084526948,23.9427093038049));
#46194=CARTESIAN_POINT('Ctrl Pts',(-4.8762440225472,-0.506462028608541,
24.0220811938584));
#46195=CARTESIAN_POINT('Ctrl Pts',(-4.04008638366986,-2.77704187334428,
24.1014530839117));
#46196=CARTESIAN_POINT('Ctrl Pts',(-2.21977264431323,-4.37114046461548,
24.1808249739652));
#46197=CARTESIAN_POINT('Ctrl Pts',(0.141272797816377,-4.90043891405946,
24.2601968640185));
#46198=CARTESIAN_POINT('Ctrl Pts',(2.46790449909909,-4.23600129097727,24.339568754072));
#46199=CARTESIAN_POINT('Ctrl Pts',(4.19336012701565,-2.53968312964219,24.4189406441254));
#46200=CARTESIAN_POINT('Ctrl Pts',(4.89732250983615,-0.224703779419903,
24.4983125341788));
#46201=CARTESIAN_POINT('Ctrl Pts',(4.40830796930024,2.14501291409586,24.5776844242322));
#46202=CARTESIAN_POINT('Ctrl Pts',(2.84543936506689,3.99220920964338,24.6570563142856));
#46203=CARTESIAN_POINT('Ctrl Pts',(0.589428029776467,4.86691217832701,24.736428204339));
#46204=CARTESIAN_POINT('Ctrl Pts',(-1.8101666688907,4.5560461130975,24.8158000943924));
#46205=CARTESIAN_POINT('Ctrl Pts',(-3.76880877375201,3.13533729935451,24.8951719844458));
#46206=CARTESIAN_POINT('Ctrl Pts',(-4.80937740344408,0.950867259440163,
24.9745438744992));
#46207=CARTESIAN_POINT('Ctrl Pts',(-4.67839234303351,-1.46523194016486,
25.0539157645526));
#46208=CARTESIAN_POINT('Ctrl Pts',(-3.40776126330575,-3.52440388238162,
25.133287654606));
#46209=CARTESIAN_POINT('Ctrl Pts',(-1.30700708278832,-4.72503883998586,
25.2126595446594));
#46210=CARTESIAN_POINT('Ctrl Pts',(1.11213113008524,-4.77466479486562,25.2920314347128));
#46211=CARTESIAN_POINT('Ctrl Pts',(3.26035666133054,-3.66119297425736,25.3714033247662));
#46212=CARTESIAN_POINT('Ctrl Pts',(4.61436652655277,-1.65586264903317,25.4507752148196));
#46213=CARTESIAN_POINT('Ctrl Pts',(4.84432691963378,0.752832152305638,25.530147104873));
#46214=CARTESIAN_POINT('Ctrl Pts',(3.89421999782782,2.97813870770851,25.6095189949265));
#46215=CARTESIAN_POINT('Ctrl Pts',(1.99548970426076,4.47797726591181,25.6888908849798));
#46216=CARTESIAN_POINT('Ctrl Pts',(-0.389337464322654,4.88699047397359,
25.7682627750333));
#46217=CARTESIAN_POINT('Ctrl Pts',(-2.67932288838098,4.10554361974534,25.8476346650867));
#46218=CARTESIAN_POINT('Ctrl Pts',(-4.31663118741032,2.32399542721376,25.92700655514));
#46219=CARTESIAN_POINT('Ctrl Pts',(-4.90241768388754,-0.0236729073104641,
26.0063784451935));
#46220=CARTESIAN_POINT('Ctrl Pts',(-4.29398608388724,-2.36557457401295,
26.0857503352468));
#46221=CARTESIAN_POINT('Ctrl Pts',(-2.63954897842897,-4.13122751059639,
26.1651222253003));
#46222=CARTESIAN_POINT('Ctrl Pts',(-0.342123584367958,-4.89052256991551,
26.2444941153537));
#46223=CARTESIAN_POINT('Ctrl Pts',(2.03864235756733,-4.45849715619131,26.323866005407));
#46224=CARTESIAN_POINT('Ctrl Pts',(3.92279953365755,-2.94039170393502,26.4032378954605));
#46225=CARTESIAN_POINT('Ctrl Pts',(4.85137142631832,-0.706013341046749,
26.4826097855139));
#46226=CARTESIAN_POINT('Ctrl Pts',(4.59815997785643,1.70034830898648,26.5619816755673));
#46227=CARTESIAN_POINT('Ctrl Pts',(3.22484693664317,3.69250887460774,26.6413535656207));
#46228=CARTESIAN_POINT('Ctrl Pts',(1.06596831974129,4.78518245160429,26.7207254556741));
#46229=CARTESIAN_POINT('Ctrl Pts',(-1.3525778203687,4.71219617521178,26.8000973457275));
#46230=CARTESIAN_POINT('Ctrl Pts',(-3.44163899731715,3.49132934080697,26.8794692357809));
#46231=CARTESIAN_POINT('Ctrl Pts',(-4.69232453245783,1.419982406908,26.9588411258343));
#46232=CARTESIAN_POINT('Ctrl Pts',(-4.79997019777595,-0.997269098236029,
27.0382130158877));
#46233=CARTESIAN_POINT('Ctrl Pts',(-3.73835374746968,-3.17158805846741,
27.1175849059411));
#46234=CARTESIAN_POINT('Ctrl Pts',(-1.7660825989855,-4.57331518784726,27.1969567959945));
#46235=CARTESIAN_POINT('Ctrl Pts',(0.636402361454069,-4.860992860329,27.2763286860479));
#46236=CARTESIAN_POINT('Ctrl Pts',(2.88386111529617,-3.96454343165977,27.3557005761013));
#46237=CARTESIAN_POINT('Ctrl Pts',(4.42881768477039,-2.10233999840624,27.4350724661547));
#46238=CARTESIAN_POINT('Ctrl Pts',(4.89492406925623,0.271988805008393,27.5144443562081));
#46239=CARTESIAN_POINT('Ctrl Pts',(4.16863778520187,2.58006173756,27.5938162462615));
#46240=CARTESIAN_POINT('Ctrl Pts',(2.42688056379555,4.25963734171175,27.673188136315));
#46241=CARTESIAN_POINT('Ctrl Pts',(0.0939406088576867,4.90157471796985,
27.7525600263683));
#46242=CARTESIAN_POINT('Ctrl Pts',(-2.2618830704639,4.34949934238213,27.8319319164218));
#46243=CARTESIAN_POINT('Ctrl Pts',(-4.06671704041374,2.73789555444364,27.9113038064751));
#46244=CARTESIAN_POINT('Ctrl Pts',(-4.88090774084432,0.45934646967172,27.9906756965286));
#46245=CARTESIAN_POINT('Ctrl Pts',(-4.50612011931125,-1.93109839836612,
28.0700475865819));
#46246=CARTESIAN_POINT('Ctrl Pts',(-3.03365161084166,-3.85113197097576,
28.1494194766353));
#46247=CARTESIAN_POINT('Ctrl Pts',(-0.822192284844965,-4.83303831979172,
28.2287913666888));
#46248=CARTESIAN_POINT('Ctrl Pts',(1.5895512618482,-4.63762723165528,28.3081632567421));
#46249=CARTESIAN_POINT('Ctrl Pts',(3.61408363956719,-3.31250041510136,28.3875351467956));
#46250=CARTESIAN_POINT('Ctrl Pts',(4.75823324232603,-1.18045582952402,28.4669070368489));
#46251=CARTESIAN_POINT('Ctrl Pts',(4.7432877594249,1.23914518323065,28.5462789269024));
#46252=CARTESIAN_POINT('Ctrl Pts',(3.57288787741725,3.35689317215169,28.6256508169558));
#46253=CARTESIAN_POINT('Ctrl Pts',(1.53214041692396,4.65690941469359,28.7050227070092));
#46254=CARTESIAN_POINT('Ctrl Pts',(-0.881833057796704,4.82251283171032,
28.7843945970626));
#46255=CARTESIAN_POINT('Ctrl Pts',(-3.08099395154251,3.81336279737351,28.863766487116));
#46256=CARTESIAN_POINT('Ctrl Pts',(-4.52963153835698,1.87528602633188,28.9431383771694));
#46257=CARTESIAN_POINT('Ctrl Pts',(-4.87486090859702,-0.519606269848997,
29.0225102672228));
#46258=CARTESIAN_POINT('Ctrl Pts',(-4.03258495182442,-2.78792362882362,
29.1018821572762));
#46259=CARTESIAN_POINT('Ctrl Pts',(-2.20798022676276,-4.37710896278109,
29.1812540473296));
#46260=CARTESIAN_POINT('Ctrl Pts',(0.154483594256982,-4.90004024197141,
29.260625937383));
#46261=CARTESIAN_POINT('Ctrl Pts',(2.47931555365931,-4.22933256427261,29.3399978274364));
#46262=CARTESIAN_POINT('Ctrl Pts',(4.20019173206215,-2.52836883538588,29.4193697174898));
#46263=CARTESIAN_POINT('Ctrl Pts',(4.89791050150138,-0.211500054648609,
29.4987416075432));
#46264=CARTESIAN_POINT('Ctrl Pts',(4.40250911411586,2.15688967125365,29.5781134975966));
#46265=CARTESIAN_POINT('Ctrl Pts',(2.83466625132033,3.9998658474328,29.65748538765));
#46266=CARTESIAN_POINT('Ctrl Pts',(0.576304964130538,4.86848355673019,29.7368572777034));
#46267=CARTESIAN_POINT('Ctrl Pts',(-1.82244293669206,4.55114944781371,29.8162291677568));
#46268=CARTESIAN_POINT('Ctrl Pts',(-3.77724777204552,3.12516540720823,29.8956010578102));
#46269=CARTESIAN_POINT('Ctrl Pts',(-4.81192341092482,0.937897990843109,
29.9749729478637));
#46270=CARTESIAN_POINT('Ctrl Pts',(-4.67442515791461,-1.47783930008941,
30.0543448379171));
#46271=CARTESIAN_POINT('Ctrl Pts',(-3.39824728310101,-3.5335782086619,30.1337167279704));
#46272=CARTESIAN_POINT('Ctrl Pts',(-1.29426389201682,-4.7285452870471,30.2130886180239));
#46273=CARTESIAN_POINT('Ctrl Pts',(1.12499931835819,-4.77164919996508,30.2924605080772));
#46274=CARTESIAN_POINT('Ctrl Pts',(3.27021518492489,-3.65238992963792,30.3718323981307));
#46275=CARTESIAN_POINT('Ctrl Pts',(4.61881387094242,-1.64341655687892,30.451204288184));
#46276=CARTESIAN_POINT('Ctrl Pts',(4.84227972156944,0.765889451494932,30.5305761782375));
#46277=CARTESIAN_POINT('Ctrl Pts',(3.88617695022651,2.98862648475217,30.6099480682908));
#46278=CARTESIAN_POINT('Ctrl Pts',(1.98341007571514,4.48334072153628,30.6893199583443));
#46279=CARTESIAN_POINT('Ctrl Pts',(-0.40251110303664,4.8859230822605,30.7686918483976));
#46280=CARTESIAN_POINT('Ctrl Pts',(-2.69038146803192,4.09830539495341,30.8480637384511));
#46281=CARTESIAN_POINT('Ctrl Pts',(-4.322880862473,2.3123495848808,30.9274356285044));
#46282=CARTESIAN_POINT('Ctrl Pts',(-4.90233604735018,-0.0368894657697565,
31.0068075185579));
#46283=CARTESIAN_POINT('Ctrl Pts',(-4.28759302222965,-2.3771423242123,31.0861794086113));
#46284=CARTESIAN_POINT('Ctrl Pts',(-2.62840182732014,-4.13832857419201,
31.1655512986647));
#46285=CARTESIAN_POINT('Ctrl Pts',(-0.328937765144189,-4.89142714353344,
31.2449231887181));
#46286=CARTESIAN_POINT('Ctrl Pts',(2.05065480852948,-4.45298488770047,31.3242950787715));
#46287=CARTESIAN_POINT('Ctrl Pts',(3.93071240989281,-2.9298053697385,31.4036669688249));
#46288=CARTESIAN_POINT('Ctrl Pts',(4.85325716869055,-0.692931748722414,
31.4830388588783));
#46289=CARTESIAN_POINT('Ctrl Pts',(4.59355922369783,1.712738512504,31.5624107489317));
#46290=CARTESIAN_POINT('Ctrl Pts',(3.21488041948321,3.70118946316684,31.6417826389851));
#46291=CARTESIAN_POINT('Ctrl Pts',(1.05306386109957,4.78803885304619,31.7211545290385));
#46292=CARTESIAN_POINT('Ctrl Pts',(-1.36527672293062,4.70853257646772,31.8005264190919));
#46293=CARTESIAN_POINT('Ctrl Pts',(-3.45103891924366,3.48203818642175,31.8798983091454));
#46294=CARTESIAN_POINT('Ctrl Pts',(-4.69613567357401,1.40732700152429,31.9592701991987));
#46295=CARTESIAN_POINT('Ctrl Pts',(-4.79726417254176,-1.010205925879,32.0386420892522));
#46296=CARTESIAN_POINT('Ctrl Pts',(-3.72978973764247,-3.1816549257911,32.1180139793055));
#46297=CARTESIAN_POINT('Ctrl Pts',(-1.75374677840301,-4.57805982825421,
32.197385869359));
#46298=CARTESIAN_POINT('Ctrl Pts',(0.649505014202782,-4.85925948991811,
32.2767577594123));
#46299=CARTESIAN_POINT('Ctrl Pts',(2.89453882300369,-3.95675429562642,32.3561296494657));
#46300=CARTESIAN_POINT('Ctrl Pts',(4.43446938147393,-2.09039251304725,32.4355015395192));
#46301=CARTESIAN_POINT('Ctrl Pts',(4.89417301414864,0.285184258704931,32.5148734295725));
#46302=CARTESIAN_POINT('Ctrl Pts',(4.16166693364494,2.59129077628124,32.594245319626));
#46303=CARTESIAN_POINT('Ctrl Pts',(2.41538799979881,4.26616459648027,32.6736172096793));
#46304=CARTESIAN_POINT('Ctrl Pts',(0.0807258955723594,4.90181016397187,
32.7529890997328));
#46305=CARTESIAN_POINT('Ctrl Pts',(-2.2736008581318,4.34338562549266,32.8323609897862));
#46306=CARTESIAN_POINT('Ctrl Pts',(-4.07408347532516,2.72692196256443,32.9117328798396));
#46307=CARTESIAN_POINT('Ctrl Pts',(-4.88212837576012,0.446186145494932,
32.991104769893));
#46308=CARTESIAN_POINT('Ctrl Pts',(-4.5008976102678,-1.94323962900084,33.0704766599464));
#46309=CARTESIAN_POINT('Ctrl Pts',(-3.02325814948215,-3.85929653115999,
33.1498485499998));
#46310=CARTESIAN_POINT('Ctrl Pts',(-0.809159695351077,-4.83523734073656,
33.2292204400532));
#46311=CARTESIAN_POINT('Ctrl Pts',(1.60204826952296,-4.63332503672604,33.3085923301066));
#46312=CARTESIAN_POINT('Ctrl Pts',(3.6230008220149,-3.30274500946005,33.3879642201599));
#46313=CARTESIAN_POINT('Ctrl Pts',(4.76139839364027,-1.16762360839165,33.4673361102135));
#46314=CARTESIAN_POINT('Ctrl Pts',(4.73992985575147,1.25192831918992,33.5467080002668));
#46315=CARTESIAN_POINT('Ctrl Pts',(3.56382489665835,3.36651327931318,33.6260798903203));
#46316=CARTESIAN_POINT('Ctrl Pts',(1.51958008113186,4.66102305624645,33.7054517803736));
#46317=CARTESIAN_POINT('Ctrl Pts',(-0.894831078624851,4.82011793367764,
33.784823670427));
#46318=CARTESIAN_POINT('Ctrl Pts',(-3.09126336830355,3.80504275161507,33.8641955604804));
#46319=CARTESIAN_POINT('Ctrl Pts',(-4.53467074385896,1.86306757757831,33.9435674505338));
#46320=CARTESIAN_POINT('Ctrl Pts',(-4.87344236353374,-0.532746734526401,
34.0229393405872));
#46321=CARTESIAN_POINT('Ctrl Pts',(-4.02505421063338,-2.79878512131536,
34.1023112306406));
#46322=CARTESIAN_POINT('Ctrl Pts',(-2.19617176132914,-4.38304564755766,
34.181683120694));
#46323=CARTESIAN_POINT('Ctrl Pts',(0.167693267891119,-4.89960595576193,
34.2610550107475));
#46324=CARTESIAN_POINT('Ctrl Pts',(2.4907085882359,-4.22263309823643,34.3404269008008));
#46325=CARTESIAN_POINT('Ctrl Pts',(4.20699280957637,-2.51703616462034,34.4197987908543));
#46326=CARTESIAN_POINT('Ctrl Pts',(4.89846289452463,-0.198294792667773,
34.4991706809077));
#46327=CARTESIAN_POINT('Ctrl Pts',(4.39667826093041,2.16875075186054,34.578542570961));
#46328=CARTESIAN_POINT('Ctrl Pts',(2.82387253485585,4.00749341368399,34.6579144610145));
#46329=CARTESIAN_POINT('Ctrl Pts',(0.563177709826186,4.87001955037029,34.7372863510678));
#46330=CARTESIAN_POINT('Ctrl Pts',(-1.83470595874441,4.54621970419178,34.8166582411213));
#46331=CARTESIAN_POINT('Ctrl Pts',(-3.78565931681763,3.11497080095877,34.8960301311746));
#46332=CARTESIAN_POINT('Ctrl Pts',(-4.81443444472882,0.924921905483118,
34.9754020212281));
#46333=CARTESIAN_POINT('Ctrl Pts',(-4.67042399847396,-1.49043591888832,
35.0547739112815));
#46334=CARTESIAN_POINT('Ctrl Pts',(-3.38870860399896,-3.5427268524425,35.1341458013349));
#46335=CARTESIAN_POINT('Ctrl Pts',(-1.28151129436916,-4.73201736643453,
35.2135176913883));
#46336=CARTESIAN_POINT('Ctrl Pts',(1.13785932999185,-4.76859892410594,35.2928895814417));
#46337=CARTESIAN_POINT('Ctrl Pts',(3.28004994017574,-3.64356033897983,35.3722614714951));
#46338=CARTESIAN_POINT('Ctrl Pts',(4.62322764520025,-1.63095852016229,35.4516333615485));
#46339=CARTESIAN_POINT('Ctrl Pts',(4.84019732919482,0.77894118410138,35.5310052516019));
#46340=CARTESIAN_POINT('Ctrl Pts',(3.87810565739256,2.99909254007502,35.6103771416553));
#46341=CARTESIAN_POINT('Ctrl Pts',(1.97131603149074,4.48867159166511,35.6897490317087));
#46342=CARTESIAN_POINT('Ctrl Pts',(-0.415681816248198,4.88482017903162,
35.7691209217621));
#46343=CARTESIAN_POINT('Ctrl Pts',(-2.70142049364518,4.09103738315207,35.8484928118155));
#46344=CARTESIAN_POINT('Ctrl Pts',(-4.32909911828301,2.30068693609431,35.9278647018689));
#46345=CARTESIAN_POINT('Ctrl Pts',(-4.90221878000546,-0.0501057561118174,
36.0072365919223));
#46346=CARTESIAN_POINT('Ctrl Pts',(-4.28116879779583,-2.38869279703632,
36.0866084819757));
#46347=CARTESIAN_POINT('Ctrl Pts',(-2.61723557264952,-4.14539955988464,
36.1659803720291));
#46348=CARTESIAN_POINT('Ctrl Pts',(-0.315749555158452,-4.89229616563135,
36.2453522620825));
#46349=CARTESIAN_POINT('Ctrl Pts',(2.06265235506943,-4.44744025434409,36.3247241521359));
#46350=CARTESIAN_POINT('Ctrl Pts',(3.93859671720591,-2.9191977413407,36.4040960421893));
#46351=CARTESIAN_POINT('Ctrl Pts',(4.85510763696701,-0.679845120081316,
36.4834679322428));
#46352=CARTESIAN_POINT('Ctrl Pts',(4.58892508296144,1.72511626761826,36.5628398222961));
#46353=CARTESIAN_POINT('Ctrl Pts',(3.20489053615983,3.70984315100612,36.6422117123496));
#46354=CARTESIAN_POINT('Ctrl Pts',(1.04015174865454,4.7908604544074,36.721583602403));
#46355=CARTESIAN_POINT('Ctrl Pts',(-1.37796570248609,4.70483475550478,36.8009554924563));
#46356=CARTESIAN_POINT('Ctrl Pts',(-3.46041375857649,3.47272172413633,36.8803273825098));
#46357=CARTESIAN_POINT('Ctrl Pts',(-4.69991268257361,1.39466136750738,36.9596992725631));
#46358=CARTESIAN_POINT('Ctrl Pts',(-4.79452328017606,-1.02313541121578,
37.0390711626166));
#46359=CARTESIAN_POINT('Ctrl Pts',(-3.72119861922486,-3.19169866843862,
37.11844305267));
#46360=CARTESIAN_POINT('Ctrl Pts',(-1.74139821136397,-4.5827711947349,37.1978149427234));
#46361=CARTESIAN_POINT('Ctrl Pts',(0.66260294626563,-4.85749080178586,37.2771868327768));
#46362=CARTESIAN_POINT('Ctrl Pts',(2.90519549283168,-3.94893640139516,37.3565587228302));
#46363=CARTESIAN_POINT('Ctrl Pts',(4.44008884788513,-2.07842983444732,37.4359306128835));
#46364=CARTESIAN_POINT('Ctrl Pts',(4.8933863875636,0.298377639646022,37.515302502937));
#46365=CARTESIAN_POINT('Ctrl Pts',(4.15466583455884,2.60250098116825,37.5946743929904));
#46366=CARTESIAN_POINT('Ctrl Pts',(2.40387788045201,4.272660844218,37.6740462830438));
#46367=CARTESIAN_POINT('Ctrl Pts',(0.0675105955612736,4.90200998298708,
37.7534181730972));
#46368=CARTESIAN_POINT('Ctrl Pts',(-2.28530212097756,4.33724034032229,37.8327900631506));
#46369=CARTESIAN_POINT('Ctrl Pts',(-4.08142029927378,2.71592855106086,37.9121619532041));
#46370=CARTESIAN_POINT('Ctrl Pts',(-4.883313526743,0.433022578390986,37.9915338432574));
#46371=CARTESIAN_POINT('Ctrl Pts',(-4.49564238811839,-1.95536673594121,
38.0709057333108));
#46372=CARTESIAN_POINT('Ctrl Pts',(-3.01284271470332,-3.86743304144309,
38.1502776233642));
#46373=CARTESIAN_POINT('Ctrl Pts',(-0.796121224763853,-4.8374012186294,
38.2296495134176));
#46374=CARTESIAN_POINT('Ctrl Pts',(1.61453363327388,-4.62898916605744,38.309021403471));
#46375=CARTESIAN_POINT('Ctrl Pts',(3.63189167208741,-3.29296559930574,38.3883932935244));
#46376=CARTESIAN_POINT('Ctrl Pts',(4.76452893838759,-1.15478290032729,38.4677651835778));
#46377=CARTESIAN_POINT('Ctrl Pts',(4.73653750187218,1.26470235504111,38.5471370736312));
#46378=CARTESIAN_POINT('Ctrl Pts',(3.55473601316178,3.37610891998471,38.6265089636846));
#46379=CARTESIAN_POINT('Ctrl Pts',(1.50700870159436,4.66510281756139,38.705880853738));
#46380=CARTESIAN_POINT('Ctrl Pts',(-0.907822597135966,4.81768800868639,
38.7852527437914));
#46381=CARTESIAN_POINT('Ctrl Pts',(-3.10151031466514,3.79669503846564,38.8646246338448));
#46382=CARTESIAN_POINT('Ctrl Pts',(-4.53967699589137,1.85083561019,38.9439965238982));
#46383=CARTESIAN_POINT('Ctrl Pts',(-4.87198838803768,-0.545883369388725,
39.0233684139517));
#46384=CARTESIAN_POINT('Ctrl Pts',(-4.01749423301241,-2.80962619208844,
39.102740304005));
#46385=CARTESIAN_POINT('Ctrl Pts',(-2.18434729950916,-4.38895062645438,
39.1821121940585));
#46386=CARTESIAN_POINT('Ctrl Pts',(0.180901657890313,-4.89913577411435,
39.2614840841118));
#46387=CARTESIAN_POINT('Ctrl Pts',(2.50208364241399,-4.21590347870473,39.3408559741653));
#46388=CARTESIAN_POINT('Ctrl Pts',(4.21376307902776,-2.50568418547649,39.4202278642187));
#46389=CARTESIAN_POINT('Ctrl Pts',(4.89898012125377,-0.185090004541199,
39.4995997542721));
#46390=CARTESIAN_POINT('Ctrl Pts',(4.39081462818005,2.18059968579169,39.5789716443255));
#46391=CARTESIAN_POINT('Ctrl Pts',(2.81305984991034,4.01508502497055,39.6583435343788));
#46392=CARTESIAN_POINT('Ctrl Pts',(0.55004342451412,4.87153304143481,39.7377154244323));
#46393=CARTESIAN_POINT('Ctrl Pts',(-1.84695009786503,4.54123256689917,39.8170873144857));
#46394=CARTESIAN_POINT('Ctrl Pts',(-3.79405383067523,3.10479958283119,39.8964592045391));
#46395=CARTESIAN_POINT('Ctrl Pts',(-4.8168906266497,0.911851793294956,39.9758310945925));
#46396=CARTESIAN_POINT('Ctrl Pts',(-4.66642692152748,-1.50285363850387,
40.0552029846459));
#46397=CARTESIAN_POINT('Ctrl Pts',(-3.37906911267765,-3.55219315325672,
40.1345748746994));
#46398=CARTESIAN_POINT('Ctrl Pts',(-1.9723130827443,-4.34047654372169,40.1874894680682));
#46399=CARTESIAN_POINT('Ctrl Pts',(-1.21713437249821,-4.54280821229862,
40.2139467647527));
#46400=CARTESIAN_POINT('Ctrl Pts',(-3.71544298812222,3.17665283523783,-0.213946764752703));
#46401=CARTESIAN_POINT('Ctrl Pts',(-4.2435173595033,2.55901209131059,-0.187489468068236));
#46402=CARTESIAN_POINT('Ctrl Pts',(-4.98521092249169,1.05595859527115,-0.1345748746993));
#46403=CARTESIAN_POINT('Ctrl Pts',(-4.8827252805975,-1.45743906270739,-0.0552029846458962));
#46404=CARTESIAN_POINT('Ctrl Pts',(-3.59110607910258,-3.61508997874938,
0.0241689054075074));
#46405=CARTESIAN_POINT('Ctrl Pts',(-1.42455668503541,-4.89247688957836,
0.103540795460911));
#46406=CARTESIAN_POINT('Ctrl Pts',(1.08893586889099,-4.9778765288597,0.182912685514315));
#46407=CARTESIAN_POINT('Ctrl Pts',(3.33720602914152,-3.85077723115681,0.262284575567719));
#46408=CARTESIAN_POINT('Ctrl Pts',(4.77251903131815,-1.78558378675016,0.341656465621122));
#46409=CARTESIAN_POINT('Ctrl Pts',(5.04526816392178,0.714545672093079,0.421028355674526));
#46410=CARTESIAN_POINT('Ctrl Pts',(4.0889952065405,3.04062834435892,0.500400245727928));
#46411=CARTESIAN_POINT('Ctrl Pts',(2.13665520967362,4.62601276074604,0.579772135781332));
#46412=CARTESIAN_POINT('Ctrl Pts',(-0.336170930871067,5.08451490337719,
0.659144025834737));
#46413=CARTESIAN_POINT('Ctrl Pts',(-2.72710569549275,4.30443824810499,0.738515915888139));
#46414=CARTESIAN_POINT('Ctrl Pts',(-4.45372401575963,2.47581113999331,0.817887805941545));
#46415=CARTESIAN_POINT('Ctrl Pts',(-5.09542477676098,0.0440812951164733,
0.897259695994947));
#46416=CARTESIAN_POINT('Ctrl Pts',(-4.49589147158092,-2.39838632564101,
0.976631586048351));
#46417=CARTESIAN_POINT('Ctrl Pts',(-2.80116888608231,-4.25661252099957,
1.05600347610176));
#46418=CARTESIAN_POINT('Ctrl Pts',(-0.424087796932823,-5.07793723552562,
1.13537536615516));
#46419=CARTESIAN_POINT('Ctrl Pts',(2.05630016029234,-4.66228772832596,1.21474725620856));
#46420=CARTESIAN_POINT('Ctrl Pts',(4.03577793971522,-3.11091522434116,1.29411914626197));
#46421=CARTESIAN_POINT('Ctrl Pts',(5.03214915152042,-0.801730671351417,
1.37349103631537));
#46422=CARTESIAN_POINT('Ctrl Pts',(4.80269996559999,1.70275370586111,1.45286292636877));
#46423=CARTESIAN_POINT('Ctrl Pts',(3.40332370018522,3.79245104545052,1.53223481642218));
#46424=CARTESIAN_POINT('Ctrl Pts',(1.17490531372441,4.95831570685873,1.61160670647558));
#46425=CARTESIAN_POINT('Ctrl Pts',(-1.33971740612181,4.9163456360401,1.69097859652898));
#46426=CARTESIAN_POINT('Ctrl Pts',(-3.52798793147818,3.67676465100145,1.77035048658239));
#46427=CARTESIAN_POINT('Ctrl Pts',(-4.85684840567494,1.54153193505596,1.84972237663579));
#46428=CARTESIAN_POINT('Ctrl Pts',(-5.00259135876462,-0.969214547985408,
1.9290942666892));
#46429=CARTESIAN_POINT('Ctrl Pts',(-3.92971412987363,-3.24386251254264,
2.0084661567426));
#46430=CARTESIAN_POINT('Ctrl Pts',(-1.89956723723801,-4.72831274916731,
2.087838046796));
#46431=CARTESIAN_POINT('Ctrl Pts',(0.593310029777512,-5.06095646606144,
2.16720993684941));
#46432=CARTESIAN_POINT('Ctrl Pts',(2.94165828680369,-4.16076239004749,2.24658182690281));
#46433=CARTESIAN_POINT('Ctrl Pts',(4.57342509641733,-2.24701580551599,2.32595371695621));
#46434=CARTESIAN_POINT('Ctrl Pts',(5.09111567564703,0.214098855557618,2.40532560700962));
#46435=CARTESIAN_POINT('Ctrl Pts',(4.36862174528326,2.62305950931529,2.48469749706302));
#46436=CARTESIAN_POINT('Ctrl Pts',(2.58194122754832,4.39304867264849,2.56406938711643));
#46437=CARTESIAN_POINT('Ctrl Pts',(0.166305541812792,5.09290090317231,2.64344127716983));
#46438=CARTESIAN_POINT('Ctrl Pts',(-2.28984180579737,4.55213374662856,2.72281316722323));
#46439=CARTESIAN_POINT('Ctrl Pts',(-4.18818875799412,2.90247688538309,2.80218505727664));
#46440=CARTESIAN_POINT('Ctrl Pts',(-5.06630219914209,0.545783079381991,
2.88155694733003));
#46441=CARTESIAN_POINT('Ctrl Pts',(-4.71027563864874,-1.94386227668626,
2.96092883738345));
#46442=CARTESIAN_POINT('Ctrl Pts',(-3.20683635859883,-3.95998708481986,
3.04030072743684));
#46443=CARTESIAN_POINT('Ctrl Pts',(-0.922218839806132,-5.01146780437411,
3.11967261749025));
#46444=CARTESIAN_POINT('Ctrl Pts',(1.58704914706656,-4.84216605947864,3.19904450754365));
#46445=CARTESIAN_POINT('Ctrl Pts',(3.70971547458753,-3.49332338044696,3.27841639759706));
#46446=CARTESIAN_POINT('Ctrl Pts',(4.92870332381492,-1.29351485827855,3.35778828765046));
#46447=CARTESIAN_POINT('Ctrl Pts',(4.94706995286075,1.22139102021994,3.43716017770387));
#46448=CARTESIAN_POINT('Ctrl Pts',(3.76034129154331,3.43876874969603,3.51653206775727));
#46449=CARTESIAN_POINT('Ctrl Pts',(1.65760181498019,4.81847002333168,3.59590395781068));
#46450=CARTESIAN_POINT('Ctrl Pts',(-0.848925794672718,5.02440266478622,
3.67527584786407));
#46451=CARTESIAN_POINT('Ctrl Pts',(-3.14865695980872,4.00640193842551,3.75464773791748));
#46452=CARTESIAN_POINT('Ctrl Pts',(-4.68138225896931,2.01245056788461,3.83401962797088));
#46453=CARTESIAN_POINT('Ctrl Pts',(-5.07373320190881,-0.471729306509208,
3.91339151802429));
#46454=CARTESIAN_POINT('Ctrl Pts',(-4.23013396738131,-2.84099696599249,
3.99276340807769));
#46455=CARTESIAN_POINT('Ctrl Pts',(-2.3560834616424,-4.51820405300012,4.0721352981311));
#46456=CARTESIAN_POINT('Ctrl Pts',(0.0919037602502722,-5.09478663357196,
4.1515071881845));
#46457=CARTESIAN_POINT('Ctrl Pts',(2.51750342957152,-4.43029046732459,4.2308790782379));
#46458=CARTESIAN_POINT('Ctrl Pts',(4.32984483584847,-2.6865853495186,4.3102509682913));
#46459=CARTESIAN_POINT('Ctrl Pts',(5.08744562406172,-0.288433987225658,
4.38962285834471));
#46460=CARTESIAN_POINT('Ctrl Pts',(4.60575591912341,2.17997925591765,4.46899474839811));
#46461=CARTESIAN_POINT('Ctrl Pts',(3.00211426695445,4.11735437762165,4.54836663845152));
#46462=CARTESIAN_POINT('Ctrl Pts',(0.667164224422586,5.05175108654635,4.62773852850492));
#46463=CARTESIAN_POINT('Ctrl Pts',(-1.83030554643563,4.75555241264972,4.70711041855833));
#46464=CARTESIAN_POINT('Ctrl Pts',(-3.88191693749475,3.30091169726834,4.78648230861172));
#46465=CARTESIAN_POINT('Ctrl Pts',(-4.98790195505755,1.04217619887652,4.86585419866514));
#46466=CARTESIAN_POINT('Ctrl Pts',(-4.87884509690204,-1.47043111474375,
4.94522608871853));
#46467=CARTESIAN_POINT('Ctrl Pts',(-3.58131237228163,-3.62484466355651,
5.02459797877194));
#46468=CARTESIAN_POINT('Ctrl Pts',(-1.4113798808739,-4.89625407578446,5.10396986882534));
#46469=CARTESIAN_POINT('Ctrl Pts',(1.10236162547835,-4.97494683282589,5.18334175887874));
#46470=CARTESIAN_POINT('Ctrl Pts',(3.34757027990012,-3.84175355324895,5.26271364893216));
#46471=CARTESIAN_POINT('Ctrl Pts',(4.77731822385938,-1.77271761167783,5.34208553898555));
#46472=CARTESIAN_POINT('Ctrl Pts',(5.04332202290099,0.728148416254135,5.42145742903896));
#46473=CARTESIAN_POINT('Ctrl Pts',(4.0807837403679,3.05163910171577,5.50082931909235));
#46474=CARTESIAN_POINT('Ctrl Pts',(2.12417557134277,4.63175725668802,5.58020120914577));
#46475=CARTESIAN_POINT('Ctrl Pts',(-0.349877065078572,5.08358959615188,
5.65957309919917));
#46476=CARTESIAN_POINT('Ctrl Pts',(-2.73870042288654,4.29707076232783,5.73894498925257));
#46477=CARTESIAN_POINT('Ctrl Pts',(-4.46038241968988,2.46379500220554,5.81831687930597));
#46478=CARTESIAN_POINT('Ctrl Pts',(-5.09552513194581,0.0303442330637155,
5.89768876935938));
#46479=CARTESIAN_POINT('Ctrl Pts',(-4.48940920081331,-2.41049832408661,
5.97706065941278));
#46480=CARTESIAN_POINT('Ctrl Pts',(-2.78968312550141,-4.26414882503699,
6.05643254946618));
#46481=CARTESIAN_POINT('Ctrl Pts',(-0.410396415676208,-5.07906211074168,
6.13580443951959));
#46482=CARTESIAN_POINT('Ctrl Pts',(2.06886195261065,-4.65672710858298,6.21517632957299));
#46483=CARTESIAN_POINT('Ctrl Pts',(4.04415012858982,-3.10002369026409,6.2945482196264));
#46484=CARTESIAN_POINT('Ctrl Pts',(5.03429228481897,-0.788161362782912,
6.37392010967979));
#46485=CARTESIAN_POINT('Ctrl Pts',(4.79809198368318,1.7156953281066,6.45329199973321));
#46486=CARTESIAN_POINT('Ctrl Pts',(3.39308709571864,3.80161243469653,6.5326638897866));
#46487=CARTESIAN_POINT('Ctrl Pts',(1.16153370170793,4.96146516692078,6.61203577984001));
#46488=CARTESIAN_POINT('Ctrl Pts',(-1.35296673102758,4.91271596650001,6.69140766989341));
#46489=CARTESIAN_POINT('Ctrl Pts',(-3.53788746282585,3.66724003075218,6.77077955994682));
#46490=CARTESIAN_POINT('Ctrl Pts',(-4.8609866396608,1.52843254081124,6.85015145000022));
#46491=CARTESIAN_POINT('Ctrl Pts',(-4.99996023068582,-0.982697732943262,
6.92952334005363));
#46492=CARTESIAN_POINT('Ctrl Pts',(-3.92095457674001,-3.25444501411732,
7.00889523010702));
#46493=CARTESIAN_POINT('Ctrl Pts',(-1.8868130667861,-4.73341669344426,7.08826712016043));
#46494=CARTESIAN_POINT('Ctrl Pts',(0.606951929847044,-5.05933854348832,
7.16763901021384));
#46495=CARTESIAN_POINT('Ctrl Pts',(2.95286477983474,-4.15281672299454,7.24701090026724));
#46496=CARTESIAN_POINT('Ctrl Pts',(4.57946630551004,-2.23467794088318,7.32638279032065));
#46497=CARTESIAN_POINT('Ctrl Pts',(5.0905199756398,0.227823441251604,7.40575468037404));
#46498=CARTESIAN_POINT('Ctrl Pts',(4.36153424737857,2.63482753737611,7.48512657042746));
#46499=CARTESIAN_POINT('Ctrl Pts',(2.57008843054822,4.39999347748764,7.56449846048085));
#46500=CARTESIAN_POINT('Ctrl Pts',(0.152574760830579,5.09333074570355,7.64387035053426));
#46501=CARTESIAN_POINT('Ctrl Pts',(-2.3021057829069,4.54594391816246,7.72324224058766));
#46502=CARTESIAN_POINT('Ctrl Pts',(-4.19599845355297,2.89117521443317,7.80261413064106));
#46503=CARTESIAN_POINT('Ctrl Pts',(-5.06775518859857,0.532122627975753,
7.88198602069447));
#46504=CARTESIAN_POINT('Ctrl Pts',(-4.70501797698741,-1.95655385282311,
7.96135791074787));
#46505=CARTESIAN_POINT('Ctrl Pts',(-3.19614880056275,-3.96861814583273,
8.04072980080128));
#46506=CARTESIAN_POINT('Ctrl Pts',(-0.908704850876407,-5.01393584290478,
8.12010169085468));
#46507=CARTESIAN_POINT('Ctrl Pts',(1.60009758909935,-4.83786986680398,8.19947358090808));
#46508=CARTESIAN_POINT('Ctrl Pts',(3.71911979812647,-3.48330949959307,8.27884547096148));
#46509=CARTESIAN_POINT('Ctrl Pts',(4.93217265646204,-1.28022264845606,8.3582173610149));
#46510=CARTESIAN_POINT('Ctrl Pts',(4.94375917286243,1.23472360612009,8.43758925106829));
#46511=CARTESIAN_POINT('Ctrl Pts',(3.75105689757885,3.4488939232597,8.5169611411217));
#46512=CARTESIAN_POINT('Ctrl Pts',(1.64460546486869,4.82292131469047,8.5963330311751));
#46513=CARTESIAN_POINT('Ctrl Pts',(-0.862468218811062,5.02209574921791,
8.67570492122851));
#46514=CARTESIAN_POINT('Ctrl Pts',(-3.15944655342946,3.99789877545622,8.75507681128191));
#46515=CARTESIAN_POINT('Ctrl Pts',(-4.68679070094874,1.99982250919225,8.83444870133531));
#46516=CARTESIAN_POINT('Ctrl Pts',(-5.07244300775217,-0.485406093778898,
8.91382059138872));
#46517=CARTESIAN_POINT('Ctrl Pts',(-4.22245942552934,-2.85239084673368,
8.99319248144211));
#46518=CARTESIAN_POINT('Ctrl Pts',(-2.34389407350296,-4.52453950308418,
9.07256437149552));
#46519=CARTESIAN_POINT('Ctrl Pts',(0.105638686707185,-5.09452035138171,
9.15193626154893));
#46520=CARTESIAN_POINT('Ctrl Pts',(2.52943809666274,-4.42348731861218,9.23130815160232));
#46521=CARTESIAN_POINT('Ctrl Pts',(4.33707198508751,-2.67490256625183,9.31068004165574));
#46522=CARTESIAN_POINT('Ctrl Pts',(5.08820473789098,-0.274717469548947,
9.39005193170913));
#46523=CARTESIAN_POINT('Ctrl Pts',(4.59986207909436,2.19238819465928,9.46942382176255));
#46524=CARTESIAN_POINT('Ctrl Pts',(2.99100319945234,4.12543294741746,9.54879571181595));
#46525=CARTESIAN_POINT('Ctrl Pts',(0.653542560897033,5.05353136567566,9.62816760186935));
#46526=CARTESIAN_POINT('Ctrl Pts',(-1.84311959890086,4.75060072905723,9.70753949192275));
#46527=CARTESIAN_POINT('Ctrl Pts',(-3.89080190408257,3.29043427011681,9.78691138197615));
#46528=CARTESIAN_POINT('Ctrl Pts',(-4.99069347757367,1.02872530622863,9.86628327202957));
#46529=CARTESIAN_POINT('Ctrl Pts',(-4.87486316664046,-1.48357886521197,
9.94565516208295));
#46530=CARTESIAN_POINT('Ctrl Pts',(-3.57152697864026,-3.63448650893304,
10.0250270521364));
#46531=CARTESIAN_POINT('Ctrl Pts',(-1.39817472408419,-4.90004128387748,
10.1043989421898));
#46532=CARTESIAN_POINT('Ctrl Pts',(1.11576979845155,-4.9719568481268,10.1837708322432));
#46533=CARTESIAN_POINT('Ctrl Pts',(3.35791526779908,-3.83271472941224,10.2631427222966));
#46534=CARTESIAN_POINT('Ctrl Pts',(4.7820800105301,-1.75983178618299,10.34251461235));
#46535=CARTESIAN_POINT('Ctrl Pts',(5.04134064765054,0.741742284838825,10.4218865024034));
#46536=CARTESIAN_POINT('Ctrl Pts',(4.07254186182158,3.0626295770926,10.5012583924568));
#46537=CARTESIAN_POINT('Ctrl Pts',(2.11168089287137,4.63746708338223,10.5806302825102));
#46538=CARTESIAN_POINT('Ctrl Pts',(-0.363580867455945,5.08262787301918,
10.6600021725636));
#46539=CARTESIAN_POINT('Ctrl Pts',(-2.75027513324356,4.28967176299466,10.739374062617));
#46540=CARTESIAN_POINT('Ctrl Pts',(-4.46700846420381,2.45176110653202,10.8187459526704));
#46541=CARTESIAN_POINT('Ctrl Pts',(-5.09558842083953,0.0166068713993523,
10.8981178427238));
#46542=CARTESIAN_POINT('Ctrl Pts',(-4.48289431705241,-2.42259276084751,
10.9774897327772));
#46543=CARTESIAN_POINT('Ctrl Pts',(-2.77817708034959,-4.27165415887005,
11.0568616228306));
#46544=CARTESIAN_POINT('Ctrl Pts',(-0.396702056264276,-5.08015005893795,
11.136233512884));
#46545=CARTESIAN_POINT('Ctrl Pts',(2.0814087106419,-4.65113264937,11.2156054029374));
#46546=CARTESIAN_POINT('Ctrl Pts',(4.05249292275577,-3.08910962152302,11.2949772929908));
#46547=CARTESIAN_POINT('Ctrl Pts',(5.03639882892726,-0.774586327501172,
11.3743491830442));
#46548=CARTESIAN_POINT('Ctrl Pts',(4.79344912825178,1.7286244813822,11.4537210730976));
#46549=CARTESIAN_POINT('Ctrl Pts',(3.38282583005384,3.81074619284624,11.533092963151));
#46550=CARTESIAN_POINT('Ctrl Pts',(1.14815364741277,4.96457856667656,11.6124648532044));
#46551=CARTESIAN_POINT('Ctrl Pts',(-1.36620622234309,4.90905059057276,11.6918367432579));
#46552=CARTESIAN_POINT('Ctrl Pts',(-3.54776128038234,3.65768875660455,11.7712086333112));
#46553=CARTESIAN_POINT('Ctrl Pts',(-4.86508954335683,1.51532203768426,11.8505805233647));
#46554=CARTESIAN_POINT('Ctrl Pts',(-4.99729276226266,-0.9961737755075,11.9299524134181));
#46555=CARTESIAN_POINT('Ctrl Pts',(-3.91216652560121,-3.26500386197887,
12.0093243034715));
#46556=CARTESIAN_POINT('Ctrl Pts',(-1.87404518273703,-4.73848623463566,
12.0886961935249));
#46557=CARTESIAN_POINT('Ctrl Pts',(0.620589418513222,-5.05768384899659,
12.1680680835782));
#46558=CARTESIAN_POINT('Ctrl Pts',(2.96404981106505,-4.14484087273527,12.2474399736317));
#46559=CARTESIAN_POINT('Ctrl Pts',(4.58547423045439,-2.2223238343253,12.3268118636851));
#46560=CARTESIAN_POINT('Ctrl Pts',(5.08988727708011,0.241546371095948,12.4061837537385));
#46561=CARTESIAN_POINT('Ctrl Pts',(4.3544150492835,2.64657641517207,12.4855556437919));
#46562=CARTESIAN_POINT('Ctrl Pts',(2.55821695381563,4.40690630260979,12.5649275338453));
#46563=CARTESIAN_POINT('Ctrl Pts',(0.138842870915485,5.09372356925339,12.6442994238987));
#46564=CARTESIAN_POINT('Ctrl Pts',(-2.3143530280162,4.53972104919276,12.7236713139521));
#46565=CARTESIAN_POINT('Ctrl Pts',(-4.20377765205669,2.87985253005087,12.8030432040055));
#46566=CARTESIAN_POINT('Ctrl Pts',(-5.06917134496016,0.518458309034014,
12.8824150940589));
#46567=CARTESIAN_POINT('Ctrl Pts',(-4.69972611865178,-1.9692312084755,12.9617869841123));
#46568=CARTESIAN_POINT('Ctrl Pts',(-3.18543801250715,-3.97722036241972,
13.0411588741657));
#46569=CARTESIAN_POINT('Ctrl Pts',(-0.895184257363228,-5.01636743950647,
13.1205307642191));
#46570=CARTESIAN_POINT('Ctrl Pts',(1.61313440141763,-4.83353851187042,13.1999026542725));
#46571=CARTESIAN_POINT('Ctrl Pts',(3.72849709062559,-3.47327030159879,13.2792745443259));
#46572=CARTESIAN_POINT('Ctrl Pts',(4.93560614144549,-1.26692113381109,13.3586464343793));
#46573=CARTESIAN_POINT('Ctrl Pts',(4.94041246098816,1.24804721789062,13.4380183244327));
#46574=CARTESIAN_POINT('Ctrl Pts',(3.74174524045162,3.45899402981983,13.5173902144861));
#46575=CARTESIAN_POINT('Ctrl Pts',(1.63159716155366,4.82733755243838,13.5967621045395));
#46576=CARTESIAN_POINT('Ctrl Pts',(-0.87600437441973,5.01975233241333,13.6761339945929));
#46577=CARTESIAN_POINT('Ctrl Pts',(-3.17021318378723,3.98936655524573,13.7555058846463));
#46578=CARTESIAN_POINT('Ctrl Pts',(-4.69216507873203,1.98717991553337,13.8348777746998));
#46579=CARTESIAN_POINT('Ctrl Pts',(-5.07111594642896,-0.499079353054812,
13.9142496647532));
#46580=CARTESIAN_POINT('Ctrl Pts',(-4.21475419430051,-2.86376399593225,
13.9936215548066));
#46581=CARTESIAN_POINT('Ctrl Pts',(-2.33168764964064,-4.53084206823465,
14.07299344486));
#46582=CARTESIAN_POINT('Ctrl Pts',(0.119372845368581,-5.09421704156391,
14.1523653349133));
#46583=CARTESIAN_POINT('Ctrl Pts',(2.54135437947334,-4.4166520194264,14.2317372249668));
#46584=CARTESIAN_POINT('Ctrl Pts',(4.34426761193091,-2.66320034145004,14.3111091150202));
#46585=CARTESIAN_POINT('Ctrl Pts',(5.08892686999541,-0.260998955190403,
14.3904810050736));
#46586=CARTESIAN_POINT('Ctrl Pts',(4.59393480667753,2.20478119884224,14.469852895127));
#46587=CARTESIAN_POINT('Ctrl Pts',(2.97987039295526,4.13348153303728,14.5492247851804));
#46588=CARTESIAN_POINT('Ctrl Pts',(0.639916147340316,5.05527491509065,14.6285966752338));
#46589=CARTESIAN_POINT('Ctrl Pts',(-1.85592025533638,4.74561451748915,14.7079685652872));
#46590=CARTESIAN_POINT('Ctrl Pts',(-3.89965859182293,3.27993292766684,14.7873404553406));
#46591=CARTESIAN_POINT('Ctrl Pts',(-4.99344872708928,1.01526693667329,14.866712345394));
#46592=CARTESIAN_POINT('Ctrl Pts',(-4.87084580524798,-1.49671583283861,
14.9460842354474));
#46593=CARTESIAN_POINT('Ctrl Pts',(-3.56171562668257,-3.64410193839537,
15.0254561255008));
#46594=CARTESIAN_POINT('Ctrl Pts',(-1.38495940518108,-4.90379287784181,
15.1048280155542));
#46595=CARTESIAN_POINT('Ctrl Pts',(1.12916986186683,-4.9689307266074,15.1841999056076));
#46596=CARTESIAN_POINT('Ctrl Pts',(3.36823584993909,-3.82364804891307,15.263571795661));
#46597=CARTESIAN_POINT('Ctrl Pts',(4.78680704042976,-1.74693317000493,15.3429436857144));
#46598=CARTESIAN_POINT('Ctrl Pts',(5.0393226312895,0.755330762345426,15.4223155757678));
#46599=CARTESIAN_POINT('Ctrl Pts',(4.06427038351844,3.07359779288479,15.5016874658212));
#46600=CARTESIAN_POINT('Ctrl Pts',(2.09917086643239,4.64314320437064,15.5810593558746));
#46601=CARTESIAN_POINT('Ctrl Pts',(-0.377282027281083,5.08162920869508,
15.660431245928));
#46602=CARTESIAN_POINT('Ctrl Pts',(-2.76182985424771,4.28224158577663,15.7398031359814));
#46603=CARTESIAN_POINT('Ctrl Pts',(-4.47360204192776,2.43970939114443,15.8191750260348));
#46604=CARTESIAN_POINT('Ctrl Pts',(-5.09561467434161,0.00286938903366673,
15.8985469160882));
#46605=CARTESIAN_POINT('Ctrl Pts',(-4.47634685104277,-2.43466958989267,
15.9779188061416));
#46606=CARTESIAN_POINT('Ctrl Pts',(-2.76665084304587,-4.27912844577413,
16.0572906961951));
#46607=CARTESIAN_POINT('Ctrl Pts',(-0.383004813579153,-5.08120108394907,
16.1366625862484));
#46608=CARTESIAN_POINT('Ctrl Pts',(2.09394034074345,-4.64550438513334,16.2160344763019));
#46609=CARTESIAN_POINT('Ctrl Pts',(4.06080626285358,-3.07817310072693,16.2954063663552));
#46610=CARTESIAN_POINT('Ctrl Pts',(5.03846876789878,-0.761005662445124,
16.3747782564087));
#46611=CARTESIAN_POINT('Ctrl Pts',(4.7887714333112,1.74154107082836,16.4541501464621));
#46612=CARTESIAN_POINT('Ctrl Pts',(3.37253997777685,3.81985225393751,16.5335220365155));
#46613=CARTESIAN_POINT('Ctrl Pts',(1.13476524781198,4.96765588336339,16.6128939265689));
#46614=CARTESIAN_POINT('Ctrl Pts',(-1.37943578318358,4.90534953479992,16.6922658166222));
#46615=CARTESIAN_POINT('Ctrl Pts',(-3.5576093137008,3.64811089835147,16.7716377066757));
#46616=CARTESIAN_POINT('Ctrl Pts',(-4.86915708441607,1.50220052016076,16.851009596729));
#46617=CARTESIAN_POINT('Ctrl Pts',(-4.99458897767399,-1.00964257616395,
16.9303814867825));
#46618=CARTESIAN_POINT('Ctrl Pts',(-3.90335003127183,-3.2755389823738,17.0097533768359));
#46619=CARTESIAN_POINT('Ctrl Pts',(-1.8612636949986,-4.74352133023597,17.0891252668893));
#46620=CARTESIAN_POINT('Ctrl Pts',(0.634222428965914,-5.05599240530682,
17.1684971569427));
#46621=CARTESIAN_POINT('Ctrl Pts',(2.9752132381933,-4.13683487704247,17.2478690469961));
#46622=CARTESIAN_POINT('Ctrl Pts',(4.59144894277892,-2.20995361377096,17.3272409370495));
#46623=CARTESIAN_POINT('Ctrl Pts',(5.08921736705481,0.255267617363485,17.4066128271029));
#46624=CARTESIAN_POINT('Ctrl Pts',(4.34726461344772,2.65830592133578,17.4859847171563));
#46625=CARTESIAN_POINT('Ctrl Pts',(2.54632610813648,4.41378735452059,17.5653566072097));
#46626=CARTESIAN_POINT('Ctrl Pts',(0.125111436169681,5.09407888617233,17.6447284972631));
#46627=CARTESIAN_POINT('Ctrl Pts',(-2.32658621700147,4.53346610033861,17.7241003873165));
#46628=CARTESIAN_POINT('Ctrl Pts',(-4.21152107628919,2.8685071860873,17.8034722773699));
#46629=CARTESIAN_POINT('Ctrl Pts',(-5.07056051563183,0.504793485523745,
17.8828441674233));
#46630=CARTESIAN_POINT('Ctrl Pts',(-4.69438148876582,-1.98190041394314,
17.9622160574767));
#46631=CARTESIAN_POINT('Ctrl Pts',(-3.1747392180444,-3.9857820361196,18.0415879475301));
#46632=CARTESIAN_POINT('Ctrl Pts',(-0.881590795203727,-5.01878454751455,
18.1209598375835));
#46633=CARTESIAN_POINT('Ctrl Pts',(1.62603418385021,-4.82913054051801,18.2003317276369));
#46634=CARTESIAN_POINT('Ctrl Pts',(3.73808388472066,-3.46328419200805,18.2797036176903));
#46635=CARTESIAN_POINT('Ctrl Pts',(4.93855701420293,-1.25346250930793,18.3590755077438));
#46636=CARTESIAN_POINT('Ctrl Pts',(4.93787328845974,1.26108254025623,18.4384473977971));
#46637=CARTESIAN_POINT('Ctrl Pts',(3.73081451079157,3.46959580775143,18.5178192878506));
#46638=CARTESIAN_POINT('Ctrl Pts',(1.62157688245111,4.83072732396141,18.597191177904));
#46639=CARTESIAN_POINT('Ctrl Pts',(-0.895150293053049,5.01921699961797,
18.6765630679574));
#46640=CARTESIAN_POINT('Ctrl Pts',(-3.17074515011531,3.97754537770249,18.7559349580108));
#46641=CARTESIAN_POINT('Ctrl Pts',(-5.22808970274021,1.31272284990122,18.8617641447486));
#46642=CARTESIAN_POINT('Ctrl Pts',(-4.77339715849023,-3.25411141853201,
18.994050628171));
#46643=CARTESIAN_POINT('Ctrl Pts',(0.152720854580862,-5.77834717219764,
19.1527944082778));
#46644=CARTESIAN_POINT('Ctrl Pts',(4.93271294602037,-3.00474199436408,19.3115381883846));
#46645=CARTESIAN_POINT('Ctrl Pts',(5.20235975367847,2.51303602329821,19.4702819684914));
#46646=CARTESIAN_POINT('Ctrl Pts',(0.709818611660393,5.73400533709388,19.6290257485982));
#46647=CARTESIAN_POINT('Ctrl Pts',(-4.43131449514935,3.70671199728522,19.787769528705));
#46648=CARTESIAN_POINT('Ctrl Pts',(-5.51805139390214,-1.71188403765749,
19.9465133088118));
#46649=CARTESIAN_POINT('Ctrl Pts',(-1.55524717023727,-5.56394358573197,
20.1052570889187));
#46650=CARTESIAN_POINT('Ctrl Pts',(3.83058845612614,-4.32541925679744,20.2640008690254));
#46651=CARTESIAN_POINT('Ctrl Pts',(5.71123844601177,0.87272703286029,20.4227446491323));
#46652=CARTESIAN_POINT('Ctrl Pts',(2.36591519662234,5.26902047281308,20.581488429239));
#46653=CARTESIAN_POINT('Ctrl Pts',(-3.14459942082001,4.85016640791291,20.7402322093459));
#46654=CARTESIAN_POINT('Ctrl Pts',(-5.77704085522352,-0.0189872057270379,
20.8989759894526));
#46655=CARTESIAN_POINT('Ctrl Pts',(-3.56709774791074,-4.0412840629435,21.031262472875));
#46656=CARTESIAN_POINT('Ctrl Pts',(-0.362731338653644,-5.07374792580599,
21.1370916596129));
#46657=CARTESIAN_POINT('Ctrl Pts',(2.10287077052077,-4.64454172754387,21.2164635496663));
#46658=CARTESIAN_POINT('Ctrl Pts',(4.07100210770441,-3.06469899064061,21.2958354397197));
#46659=CARTESIAN_POINT('Ctrl Pts',(5.03948789886561,-0.748754766453301,
21.3752073297731));
#46660=CARTESIAN_POINT('Ctrl Pts',(4.78459624359497,1.75515257798294,21.4545792198265));
#46661=CARTESIAN_POINT('Ctrl Pts',(3.36194502775863,3.82855576883798,21.5339511098799));
#46662=CARTESIAN_POINT('Ctrl Pts',(1.12151932172619,4.97089558679479,21.6133229999333));
#46663=CARTESIAN_POINT('Ctrl Pts',(-1.39273514199732,4.9015077036213,21.6926948899867));
#46664=CARTESIAN_POINT('Ctrl Pts',(-3.56738921282951,3.63856219800436,21.7720667800401));
#46665=CARTESIAN_POINT('Ctrl Pts',(-4.87321162956223,1.48903860109202,21.8514386700935));
#46666=CARTESIAN_POINT('Ctrl Pts',(-4.99183702504821,-1.02308842639,21.9308105601469));
#46667=CARTESIAN_POINT('Ctrl Pts',(-3.89451146459856,-3.28605855970678,
22.0101824502003));
#46668=CARTESIAN_POINT('Ctrl Pts',(-1.84846531944319,-4.74851758083281,
22.0895543402537));
#46669=CARTESIAN_POINT('Ctrl Pts',(0.647849003889951,-5.05426651218743,
22.1689262303072));
#46670=CARTESIAN_POINT('Ctrl Pts',(2.98635609589609,-4.12879762624803,22.2482981203605));
#46671=CARTESIAN_POINT('Ctrl Pts',(4.59738955946421,-2.19756790530644,22.3276700104139));
#46672=CARTESIAN_POINT('Ctrl Pts',(5.08851116459638,0.268987208844064,22.4070419004674));
#46673=CARTESIAN_POINT('Ctrl Pts',(4.34008162116472,2.67001619606227,22.4864137905207));
#46674=CARTESIAN_POINT('Ctrl Pts',(2.53441837980377,4.4206359096037,22.5657856805742));
#46675=CARTESIAN_POINT('Ctrl Pts',(0.11137612465092,5.09439809707615,22.6451575706275));
#46676=CARTESIAN_POINT('Ctrl Pts',(-2.3387969457162,4.52717639800266,22.724529460681));
#46677=CARTESIAN_POINT('Ctrl Pts',(-4.2192443428605,2.85714443596456,22.8039013507343));
#46678=CARTESIAN_POINT('Ctrl Pts',(-5.07189311172227,0.491118473430054,
22.8832732407878));
#46679=CARTESIAN_POINT('Ctrl Pts',(-4.6890399691108,-1.99454289389497,22.9626451308412));
#46680=CARTESIAN_POINT('Ctrl Pts',(-3.1639470562758,-3.99433801030587,23.0420170208946));
#46681=CARTESIAN_POINT('Ctrl Pts',(-0.868123650568842,-5.02112123762457,
23.121388910948));
#46682=CARTESIAN_POINT('Ctrl Pts',(1.63917275843702,-4.82477044080721,23.2007608010014));
#46683=CARTESIAN_POINT('Ctrl Pts',(3.74717030983928,-3.45311624655406,23.2801326910548));
#46684=CARTESIAN_POINT('Ctrl Pts',(4.94236546898948,-1.24029057666132,23.3595045811082));
#46685=CARTESIAN_POINT('Ctrl Pts',(4.93361133910258,1.27466713166923,23.4388764711616));
#46686=CARTESIAN_POINT('Ctrl Pts',(3.72304040765536,3.47911874852391,23.518248361215));
#46687=CARTESIAN_POINT('Ctrl Pts',(1.60554507356429,4.83606473894047,23.5976202512684));
#46688=CARTESIAN_POINT('Ctrl Pts',(-0.903057486554317,5.01495606350285,
23.6769921413218));
#46689=CARTESIAN_POINT('Ctrl Pts',(-3.19167724187396,3.97221519135782,23.7563640313752));
#46690=CARTESIAN_POINT('Ctrl Pts',(-4.70281148570869,1.96185149097637,23.8357359214286));
#46691=CARTESIAN_POINT('Ctrl Pts',(-5.06835126113314,-0.526414890137771,
23.915107811482));
#46692=CARTESIAN_POINT('Ctrl Pts',(-4.1992518879446,-2.88644776920571,23.9944797015354));
#46693=CARTESIAN_POINT('Ctrl Pts',(-2.30722404974247,-4.54334836074326,
24.0738515915888));
#46694=CARTESIAN_POINT('Ctrl Pts',(0.1468384600249,-5.09349934813251,24.1532234816422));
#46695=CARTESIAN_POINT('Ctrl Pts',(2.56513144595071,-4.40288516858744,24.2325953716957));
#46696=CARTESIAN_POINT('Ctrl Pts',(4.35856408946553,-2.63973790759483,24.311967261749));
#46697=CARTESIAN_POINT('Ctrl Pts',(5.09026016830426,-0.23355633527326,24.3913391518024));
#46698=CARTESIAN_POINT('Ctrl Pts',(4.58198013724401,2.22951904335289,24.4707110418559));
#46699=CARTESIAN_POINT('Ctrl Pts',(2.95753988679205,4.1494885179749,24.5500829319092));
#46700=CARTESIAN_POINT('Ctrl Pts',(0.612649466321058,5.05865177435533,24.6294548219626));
#46701=CARTESIAN_POINT('Ctrl Pts',(-1.88148100806917,4.73553865563851,24.7088267120161));
#46702=CARTESIAN_POINT('Ctrl Pts',(-3.91728687348126,3.25885880234522,24.7881986020694));
#46703=CARTESIAN_POINT('Ctrl Pts',(-4.99885032728078,0.988328158162253,
24.8675704921229));
#46704=CARTESIAN_POINT('Ctrl Pts',(-4.86270490612224,-1.5229570377218,24.9469423821763));
#46705=CARTESIAN_POINT('Ctrl Pts',(-3.54201533324704,-3.66325327022505,
25.0263142722297));
#46706=CARTESIAN_POINT('Ctrl Pts',(-1.3584986653108,-4.91118911457504,25.1056861622831));
#46707=CARTESIAN_POINT('Ctrl Pts',(1.15594527050936,-4.96277016134726,25.1850580523365));
#46708=CARTESIAN_POINT('Ctrl Pts',(3.38880349707489,-3.80543138172069,25.2644299423899));
#46709=CARTESIAN_POINT('Ctrl Pts',(4.79615669274227,-1.72109794068643,25.3438018324433));
#46710=CARTESIAN_POINT('Ctrl Pts',(5.0351767341704,0.782491149113306,25.4231737224967));
#46711=CARTESIAN_POINT('Ctrl Pts',(4.04763886832931,3.09546712700384,25.5025456125501));
#46712=CARTESIAN_POINT('Ctrl Pts',(2.07410513345989,4.65439416445651,25.5819175026035));
#46713=CARTESIAN_POINT('Ctrl Pts',(-0.404676020966502,5.07952108577436,
25.6612893926569));
#46714=CARTESIAN_POINT('Ctrl Pts',(-2.78487899242069,4.26728791392678,25.7406612827102));
#46715=CARTESIAN_POINT('Ctrl Pts',(-4.48669160554627,2.41555285172821,25.8200331727637));
#46716=CARTESIAN_POINT('Ctrl Pts',(-5.09555607468418,-0.0246055384158182,
25.8994050628171));
#46717=CARTESIAN_POINT('Ctrl Pts',(-4.46315436285108,-2.45877007386518,
25.9787769528705));
#46718=CARTESIAN_POINT('Ctrl Pts',(-2.74353812725205,-4.29398366171623,
26.0581488429239));
#46719=CARTESIAN_POINT('Ctrl Pts',(-0.355602076573053,-5.0831923341448,
26.1375207329773));
#46720=CARTESIAN_POINT('Ctrl Pts',(2.11895785284724,-4.63414660543109,26.2168926230307));
#46721=CARTESIAN_POINT('Ctrl Pts',(4.07734433954763,-3.05623302114393,26.2962645130841));
#46722=CARTESIAN_POINT('Ctrl Pts',(5.04249877018284,-0.733827837763115,
26.3756364031375));
#46723=CARTESIAN_POINT('Ctrl Pts',(4.77931166178323,1.76733618259643,26.4550082931909));
#46724=CARTESIAN_POINT('Ctrl Pts',(3.3518948114001,3.83798102080776,26.5343801832444));
#46725=CARTESIAN_POINT('Ctrl Pts',(1.10796380425329,4.97370217757719,26.6137520732977));
#46726=CARTESIAN_POINT('Ctrl Pts',(-1.40586473317334,4.89784049299189,26.6931239633511));
#46727=CARTESIAN_POINT('Ctrl Pts',(-3.57722773342779,3.62887570549981,26.7724958534045));
#46728=CARTESIAN_POINT('Ctrl Pts',(-4.87718597587851,1.47592482852807,26.851867743458));
#46729=CARTESIAN_POINT('Ctrl Pts',(-4.98907251007324,-1.0365580697689,26.9312396335114));
#46730=CARTESIAN_POINT('Ctrl Pts',(-3.88563202393884,-3.29653771665249,
27.0106115235647));
#46731=CARTESIAN_POINT('Ctrl Pts',(-1.83566017747357,-4.75348807252204,
27.0899834136182));
#46732=CARTESIAN_POINT('Ctrl Pts',(0.661474425059423,-5.05249925559262,
27.1693553036715));
#46733=CARTESIAN_POINT('Ctrl Pts',(2.99747532179674,-4.12073280351822,27.248727193725));
#46734=CARTESIAN_POINT('Ctrl Pts',(4.60329786494346,-2.18516496159412,27.3280990837784));
#46735=CARTESIAN_POINT('Ctrl Pts',(5.08776723741692,0.282704228193704,27.4074709738318));
#46736=CARTESIAN_POINT('Ctrl Pts',(4.33286777243738,2.68170729374875,27.4868428638852));
#46737=CARTESIAN_POINT('Ctrl Pts',(2.5224913087322,4.42745239840498,27.5662147539386));
#46738=CARTESIAN_POINT('Ctrl Pts',(0.0976415456597213,5.09467989880942,
27.6455866439919));
#46739=CARTESIAN_POINT('Ctrl Pts',(-2.35099348180958,4.52085465274658,27.7249585340454));
#46740=CARTESIAN_POINT('Ctrl Pts',(-4.22693170094588,2.84575922001675,27.8043304240988));
#46741=CARTESIAN_POINT('Ctrl Pts',(-5.07319871388641,0.477443140272041,
27.8837023141522));
#46742=CARTESIAN_POINT('Ctrl Pts',(-4.68364574945911,-2.00717703164051,
27.9630742042056));
#46743=CARTESIAN_POINT('Ctrl Pts',(-3.15316704753758,-4.00285332145644,
28.042446094259));
#46744=CARTESIAN_POINT('Ctrl Pts',(-0.854583832252744,-5.02344340233109,
28.1218179843124));
#46745=CARTESIAN_POINT('Ctrl Pts',(1.65217411297962,-4.82033378960126,28.2011898743658));
#46746=CARTESIAN_POINT('Ctrl Pts',(3.75646610131553,-3.44300153535241,28.2805617644192));
#46747=CARTESIAN_POINT('Ctrl Pts',(4.94569126216762,-1.22696172804632,28.3599336544726));
#46748=CARTESIAN_POINT('Ctrl Pts',(4.93015697865761,1.28796324037807,28.439305544526));
#46749=CARTESIAN_POINT('Ctrl Pts',(3.71364736786401,3.48914321430466,28.5186774345794));
#46750=CARTESIAN_POINT('Ctrl Pts',(1.59250147827778,4.84037562431415,28.5980493246328));
#46751=CARTESIAN_POINT('Ctrl Pts',(-0.916574246474672,5.01250324623047,
28.6774212146862));
#46752=CARTESIAN_POINT('Ctrl Pts',(-3.20237451358863,3.96359617235279,28.7567931047396));
#46753=CARTESIAN_POINT('Ctrl Pts',(-4.70808343752814,1.94916584416126,28.836164994793));
#46754=CARTESIAN_POINT('Ctrl Pts',(-5.0669136572517,-0.540076969262536,
28.9155368848465));
#46755=CARTESIAN_POINT('Ctrl Pts',(-4.19145492549188,-2.89775822841407,
28.9949087748998));
#46756=CARTESIAN_POINT('Ctrl Pts',(-2.29496705151034,-4.54955199720298,
29.0742806649532));
#46757=CARTESIAN_POINT('Ctrl Pts',(0.160569716395729,-5.09308496973575,
29.1536525550067));
#46758=CARTESIAN_POINT('Ctrl Pts',(2.57699205680278,-4.39595371699326,29.23302444506));
#46759=CARTESIAN_POINT('Ctrl Pts',(4.36566483624787,-2.62797786906977,29.3123963351135));
#46760=CARTESIAN_POINT('Ctrl Pts',(5.09087132481821,-0.219832429171176,
29.3917682251668));
#46761=CARTESIAN_POINT('Ctrl Pts',(4.57595282711536,2.24186370388268,29.4711401152203));
#46762=CARTESIAN_POINT('Ctrl Pts',(2.94634234942697,4.15744680095185,29.5505120052737));
#46763=CARTESIAN_POINT('Ctrl Pts',(0.599009397036387,5.06028505966152,29.6298838953271));
#46764=CARTESIAN_POINT('Ctrl Pts',(-1.89424091858745,4.73044907858869,29.7092557853805));
#46765=CARTESIAN_POINT('Ctrl Pts',(-3.92605833927458,3.24828617264307,29.7886276754339));
#46766=CARTESIAN_POINT('Ctrl Pts',(-5.00149663869715,0.974847945001076,
29.8679995654873));
#46767=CARTESIAN_POINT('Ctrl Pts',(-4.85858142755809,-1.53606108425386,
29.9473714555407));
#46768=CARTESIAN_POINT('Ctrl Pts',(-3.53212653495348,-3.67278903339805,
30.026743345594));
#46769=CARTESIAN_POINT('Ctrl Pts',(-1.34525343666372,-4.91483370358714,
30.1061152356475));
#46770=CARTESIAN_POINT('Ctrl Pts',(1.16932042112941,-4.95963576238229,30.1854871257009));
#46771=CARTESIAN_POINT('Ctrl Pts',(3.39905041258226,-3.79628152742866,30.2648590157543));
#46772=CARTESIAN_POINT('Ctrl Pts',(4.80077924720052,-1.70816151532001,30.3442309058077));
#46773=CARTESIAN_POINT('Ctrl Pts',(5.03304888354535,0.796062860969203,30.4236027958611));
#46774=CARTESIAN_POINT('Ctrl Pts',(4.03927895232327,3.10636808638158,30.5029746859145));
#46775=CARTESIAN_POINT('Ctrl Pts',(2.06154960910751,4.65996892178051,30.5823465759679));
#46776=CARTESIAN_POINT('Ctrl Pts',(-0.418368655724119,5.07841164249995,
30.6617184660213));
#46777=CARTESIAN_POINT('Ctrl Pts',(-2.79637324206467,4.25976452797996,30.7410903560747));
#46778=CARTESIAN_POINT('Ctrl Pts',(-4.49318749630546,2.4034482032729,30.8204622461281));
#46779=CARTESIAN_POINT('Ctrl Pts',(-5.09547122194811,-0.0383427838090456,
30.8998341361815));
#46780=CARTESIAN_POINT('Ctrl Pts',(-4.45650943655845,-2.47079355362547,
30.9792060262349));
#46781=CARTESIAN_POINT('Ctrl Pts',(-2.73195181673944,-4.3013644827875,31.0585779162883));
#46782=CARTESIAN_POINT('Ctrl Pts',(-0.341896781435476,-5.08413254485124,
31.1379498063417));
#46783=CARTESIAN_POINT('Ctrl Pts',(2.13144355305047,-4.62841717252575,31.2173216963952));
#46784=CARTESIAN_POINT('Ctrl Pts',(4.08556895588362,-3.04522962180058,31.2966935864485));
#46785=CARTESIAN_POINT('Ctrl Pts',(5.04445880431697,-0.720230875706232,
31.376065476502));
#46786=CARTESIAN_POINT('Ctrl Pts',(4.77452965373889,1.78021451750611,31.4554373665553));
#46787=CARTESIAN_POINT('Ctrl Pts',(3.34153564775218,3.84700359469197,31.5348092566088));
#46788=CARTESIAN_POINT('Ctrl Pts',(1.09455095433672,4.97667111140894,31.6141811466621));
#46789=CARTESIAN_POINT('Ctrl Pts',(-1.41906392880775,4.89403256106132,31.6935530367156));
#46790=CARTESIAN_POINT('Ctrl Pts',(-3.58699797993935,3.61921851159646,31.772924926769));
#46791=CARTESIAN_POINT('Ctrl Pts',(-4.88114726284307,1.46277084371106,31.8522968168224));
#46792=CARTESIAN_POINT('Ctrl Pts',(-4.98625987675445,-1.05000456391402,
31.9316687068758));
#46793=CARTESIAN_POINT('Ctrl Pts',(-3.87673062158748,-3.30700118391536,
32.0110405969292));
#46794=CARTESIAN_POINT('Ctrl Pts',(-1.82283836799946,-4.75841963543788,
32.0904124869826));
#46795=CARTESIAN_POINT('Ctrl Pts',(0.675093277248947,-5.0506975963509,32.169784377036));
#46796=CARTESIAN_POINT('Ctrl Pts',(3.00857369445308,-4.11263680232238,32.2491562670894));
#46797=CARTESIAN_POINT('Ctrl Pts',(4.60917221905339,-2.17274678641531,32.3285281571428));
#46798=CARTESIAN_POINT('Ctrl Pts',(5.08698659332197,0.296419537369132,32.4079000471962));
#46799=CARTESIAN_POINT('Ctrl Pts',(4.32562229331115,2.69337871796399,32.4872719372496));
#46800=CARTESIAN_POINT('Ctrl Pts',(2.51054597725224,4.43423680455544,32.566643827303));
#46801=CARTESIAN_POINT('Ctrl Pts',(0.0839062181339619,5.09492462057391,
32.6460157173564));
#46802=CARTESIAN_POINT('Ctrl Pts',(-2.3631729099985,4.51450007644488,32.7253876074099));
#46803=CARTESIAN_POINT('Ctrl Pts',(-4.23458834804982,2.8343533063703,32.8047594974632));
#46804=CARTESIAN_POINT('Ctrl Pts',(-5.07446743761851,0.463764344598583,
32.8841313875167));
#46805=CARTESIAN_POINT('Ctrl Pts',(-4.67821749152652,-2.01979658499237,
32.96350327757));
#46806=CARTESIAN_POINT('Ctrl Pts',(-3.14236411955747,-4.01133953722311,
33.0428751676235));
#46807=CARTESIAN_POINT('Ctrl Pts',(-0.841037803569241,-5.02572905713579,
33.1222470576768));
#46808=CARTESIAN_POINT('Ctrl Pts',(1.6651634597629,-4.81586210299279,33.2016189477303));
#46809=CARTESIAN_POINT('Ctrl Pts',(3.76573459007359,-3.43286180029067,33.2809908377836));
#46810=CARTESIAN_POINT('Ctrl Pts',(4.94898110955447,-1.21362396154845,33.3603627278371));
#46811=CARTESIAN_POINT('Ctrl Pts',(4.92666678513176,1.3012499879159,33.4397346178904));
#46812=CARTESIAN_POINT('Ctrl Pts',(3.70422733684289,3.49914232059194,33.5191065079439));
#46813=CARTESIAN_POINT('Ctrl Pts',(1.5794463084672,4.8446513291919,33.5984783979973));
#46814=CARTESIAN_POINT('Ctrl Pts',(-0.930084344605925,5.01001399745455,
33.6778502880506));
#46815=CARTESIAN_POINT('Ctrl Pts',(-3.21304851003985,3.95494834541518,33.7572221781041));
#46816=CARTESIAN_POINT('Ctrl Pts',(-4.71332117039034,1.93646603056234,33.8365940681574));
#46817=CARTESIAN_POINT('Ctrl Pts',(-5.06543922639319,-0.553735123040657,
33.9159659582109));
#46818=CARTESIAN_POINT('Ctrl Pts',(-4.18362749900617,-2.90904762634284,
33.9953378482642));
#46819=CARTESIAN_POINT('Ctrl Pts',(-2.28269337316369,-4.55572256693558,
34.0747097383177));
#46820=CARTESIAN_POINT('Ctrl Pts',(0.174299805725373,-5.0926335741437,34.154081628371));
#46821=CARTESIAN_POINT('Ctrl Pts',(2.58883393774586,-4.38899031504365,34.2334535184245));
#46822=CARTESIAN_POINT('Ctrl Pts',(4.37273385281817,-2.61619873006421,34.3128254084779));
#46823=CARTESIAN_POINT('Ctrl Pts',(5.09144548022617,-0.206106925298799,
34.3921972985313));
#46824=CARTESIAN_POINT('Ctrl Pts',(4.56989225837449,2.25419207025942,34.4715691885847));
#46825=CARTESIAN_POINT('Ctrl Pts',(2.93512339766776,4.16537486707196,34.5509410786381));
#46826=CARTESIAN_POINT('Ctrl Pts',(0.585364974074578,5.06188156616671,34.6303129686915));
#46827=CARTESIAN_POINT('Ctrl Pts',(-1.9069870615198,4.72532512002801,34.7096848587449));
#46828=CARTESIAN_POINT('Ctrl Pts',(-3.93480126997218,3.23768993398022,34.7890567487983));
#46829=CARTESIAN_POINT('Ctrl Pts',(-5.00410659859424,0.961360646519953,
34.8684286388517));
#46830=CARTESIAN_POINT('Ctrl Pts',(-4.85442263620079,-1.54915396649689,
34.9478005289051));
#46831=CARTESIAN_POINT('Ctrl Pts',(-3.52221206471105,-3.68229810226921,
35.0271724189585));
#46832=CARTESIAN_POINT('Ctrl Pts',(-1.33199843054191,-4.91844257095733,
35.1065443090119));
#46833=CARTESIAN_POINT('Ctrl Pts',(1.1826870729787,-4.95646531614826,35.1859161990653));
#46834=CARTESIAN_POINT('Ctrl Pts',(3.40927262335516,-3.78710408127537,35.2652880891187));
#46835=CARTESIAN_POINT('Ctrl Pts',(4.80536690897926,-1.69521267481654,35.3446599791721));
#46836=CARTESIAN_POINT('Ctrl Pts',(5.03088445207529,0.809628786938043,35.4240318692255));
#46837=CARTESIAN_POINT('Ctrl Pts',(4.0308896783196,3.11724646827744,35.503403759279));
#46838=CARTESIAN_POINT('Ctrl Pts',(2.04897910114821,4.66550980985245,35.5827756493324));
#46839=CARTESIAN_POINT('Ctrl Pts',(-0.432058249724576,5.0772652886782,35.6621475393857));
#46840=CARTESIAN_POINT('Ctrl Pts',(-2.80784716730917,4.25221018151802,35.7415194294392));
#46841=CARTESIAN_POINT('Ctrl Pts',(-4.49965073000152,2.39132608624762,35.8208913194925));
#46842=CARTESIAN_POINT('Ctrl Pts',(-5.09534933467344,-0.052079750522149,
35.9002632095459));
#46843=CARTESIAN_POINT('Ctrl Pts',(-4.4498321197834,-2.48279907534128,35.9796350995994));
#46844=CARTESIAN_POINT('Ctrl Pts',(-2.72034565005043,-4.30871404098988,
36.0590069896527));
#46845=CARTESIAN_POINT('Ctrl Pts',(-0.328189001348134,-5.08503580343008,
36.1383788797062));
#46846=CARTESIAN_POINT('Ctrl Pts',(2.14391376164854,-4.62265409969052,36.2177507697596));
#46847=CARTESIAN_POINT('Ctrl Pts',(4.0937638777802,-3.03420408933768,36.2971226598129));
#46848=CARTESIAN_POINT('Ctrl Pts',(5.0463821746773,-0.706628678919033,36.3764945498664));
#46849=CARTESIAN_POINT('Ctrl Pts',(4.76971294380048,1.79307991358828,36.4558664399198));
#46850=CARTESIAN_POINT('Ctrl Pts',(3.33115219739438,3.85599820806056,36.5352383299732));
#46851=CARTESIAN_POINT('Ctrl Pts',(1.08113014908331,4.97960387415652,36.6146102200266));
#46852=CARTESIAN_POINT('Ctrl Pts',(-1.4322528105034,4.89018905867418,36.69398211008));
#46853=CARTESIAN_POINT('Ctrl Pts',(-3.59674215568932,3.60953501274872,36.7733540001334));
#46854=CARTESIAN_POINT('Ctrl Pts',(-4.88507307300309,1.44960622728788,36.8527258901868));
#46855=CARTESIAN_POINT('Ctrl Pts',(-4.98341100265913,-1.06344342649134,
36.9320977802402));
#46856=CARTESIAN_POINT('Ctrl Pts',(-3.86780104266052,-3.31744061546937,
37.0114696702936));
#46857=CARTESIAN_POINT('Ctrl Pts',(-1.81000330990226,-4.76331661354924,
37.090841560347));
#46858=CARTESIAN_POINT('Ctrl Pts',(0.688707222773825,-5.04885922799112,
37.1702134504005));
#46859=CARTESIAN_POINT('Ctrl Pts',(3.0196502004098,-4.10451090995456,37.2495853404537));
#46860=CARTESIAN_POINT('Ctrl Pts',(4.61501307310836,-2.16031281943414,37.3289572305073));
#46861=CARTESIAN_POINT('Ctrl Pts',(5.08616897635574,0.310132692129688,37.4083291205606));
#46862=CARTESIAN_POINT('Ctrl Pts',(4.31834537500717,2.70503056635669,37.4877010106141));
#46863=CARTESIAN_POINT('Ctrl Pts',(2.49858239880182,4.44098898210481,37.5670729006674));
#46864=CARTESIAN_POINT('Ctrl Pts',(0.0701702807674692,5.09513231177087,
37.6464447907209));
#46865=CARTESIAN_POINT('Ctrl Pts',(-2.37533516234416,4.50811268818063,37.7258166807742));
#46866=CARTESIAN_POINT('Ctrl Pts',(-4.2422142176209,2.82292679227449,37.8051885708277));
#46867=CARTESIAN_POINT('Ctrl Pts',(-5.07569927947281,0.450082178237795,
37.884560460881));
#46868=CARTESIAN_POINT('Ctrl Pts',(-4.67275523170413,-2.03240145822491,
37.9639323509345));
#46869=CARTESIAN_POINT('Ctrl Pts',(-3.13153835248091,-4.01979659801907,
38.0433042409878));
#46870=CARTESIAN_POINT('Ctrl Pts',(-0.827485662097561,-5.02797818437316,
38.1226761310413));
#46871=CARTESIAN_POINT('Ctrl Pts',(1.6781407038918,-4.81135541393667,38.2020480210947));
#46872=CARTESIAN_POINT('Ctrl Pts',(3.77497570905148,-3.42269711502072,38.281419911148));
#46873=CARTESIAN_POINT('Ctrl Pts',(4.95223498699472,-1.20027737376265,38.3607918012015));
#46874=CARTESIAN_POINT('Ctrl Pts',(4.92314078418044,1.31452727683269,38.4401636912548));
#46875=CARTESIAN_POINT('Ctrl Pts',(3.69478038260533,3.50911599649374,38.5195355813083));
#46876=CARTESIAN_POINT('Ctrl Pts',(1.56637965982565,4.8488918190669,38.5989074713616));
#46877=CARTESIAN_POINT('Ctrl Pts',(-0.943587684251231,5.00748834177839,
38.6782793614151));
#46878=CARTESIAN_POINT('Ctrl Pts',(-3.22369915083517,3.94627176108658,38.7576512514684));
#46879=CARTESIAN_POINT('Ctrl Pts',(-4.71852465152966,1.92375216574096,38.8370231415219));
#46880=CARTESIAN_POINT('Ctrl Pts',(-5.06392796926474,-0.567389296122155,
38.9163950315753));
#46881=CARTESIAN_POINT('Ctrl Pts',(-4.17576968427578,-2.92031579800749,
38.9957669216287));
#46882=CARTESIAN_POINT('Ctrl Pts',(-2.27040306822808,-4.56186018168572,
39.0751388116821));
#46883=CARTESIAN_POINT('Ctrl Pts',(0.188028560849278,-5.0921448689568,39.1545107017355));
#46884=CARTESIAN_POINT('Ctrl Pts',(2.60065712992459,-4.38199557165452,39.2338825917889));
#46885=CARTESIAN_POINT('Ctrl Pts',(4.37977084759398,-2.60439952199669,39.3132544818424));
#46886=CARTESIAN_POINT('Ctrl Pts',(5.091983083909,-0.192381913948899,39.3926263718957));
#46887=CARTESIAN_POINT('Ctrl Pts',(4.56379761866661,2.26650781142318,39.4719982619492));
#46888=CARTESIAN_POINT('Ctrl Pts',(2.92388473013463,4.17326556172555,39.5513701520025));
#46889=CARTESIAN_POINT('Ctrl Pts',(0.571713243107522,5.06345468357226,39.6307420420559));
#46890=CARTESIAN_POINT('Ctrl Pts',(-1.91971357759784,4.72014150668349,39.7101139321093));
#46891=CARTESIAN_POINT('Ctrl Pts',(-3.94352649879586,3.22711800485078,39.7894858221628));
#46892=CARTESIAN_POINT('Ctrl Pts',(-5.00665954563271,0.947775616877117,
39.8688577122161));
#46893=CARTESIAN_POINT('Ctrl Pts',(-4.85026808817391,-1.56206090154421,
39.9482296022695));
#46894=CARTESIAN_POINT('Ctrl Pts',(-3.51219281059473,-3.69213734276829,
40.027601492323));
#46895=CARTESIAN_POINT('Ctrl Pts',(-2.05001543279097,-4.51147638686035,
40.0805160856919));
#46896=CARTESIAN_POINT('Ctrl Pts',(-1.2650852794273,-4.72177922709094,40.1069733823764));
#46897=CARTESIAN_POINT('Ctrl Pts',(-3.8562705385024,3.29705846079174,-0.320920147129055));
#46898=CARTESIAN_POINT('Ctrl Pts',(-4.40436067122819,2.6560070944272,-0.294462850444587));
#46899=CARTESIAN_POINT('Ctrl Pts',(-5.17416686787623,1.09598291074317,-0.241548257075651));
#46900=CARTESIAN_POINT('Ctrl Pts',(-5.06779668194698,-1.512680812799,-0.162176367022247));
#46901=CARTESIAN_POINT('Ctrl Pts',(-3.72722085031348,-3.75211381890485,
-0.0828044769688437));
#46902=CARTESIAN_POINT('Ctrl Pts',(-1.47855208449991,-5.07791790908896,
-0.00343258691543986));
#46903=CARTESIAN_POINT('Ctrl Pts',(1.1302101318597,-5.16655447652177,0.0759393031379633));
#46904=CARTESIAN_POINT('Ctrl Pts',(3.46369715057722,-3.99673439595713,0.155311193191368));
#46905=CARTESIAN_POINT('Ctrl Pts',(4.95341325213432,-1.85326330477546,0.23468308324477));
#46906=CARTESIAN_POINT('Ctrl Pts',(5.23650047694814,0.741629311098527,0.314054973298175));
#46907=CARTESIAN_POINT('Ctrl Pts',(4.24398161873799,3.15587819282154,0.393426863351577));
#46908=CARTESIAN_POINT('Ctrl Pts',(2.21764149317933,4.80135391043019,0.472798753404982));
#46909=CARTESIAN_POINT('Ctrl Pts',(-0.348912918530393,5.27723479734493,
0.552170643458385));
#46910=CARTESIAN_POINT('Ctrl Pts',(-2.83047200092439,4.46759066254957,0.631542533511789));
#46911=CARTESIAN_POINT('Ctrl Pts',(-4.62253485344812,2.56965255248809,0.710914423565193));
#46912=CARTESIAN_POINT('Ctrl Pts',(-5.28855819093304,0.045752121671659,
0.790286313618596));
#46913=CARTESIAN_POINT('Ctrl Pts',(-4.66630059499956,-2.48929308216644,
0.869658203672));
#46914=CARTESIAN_POINT('Ctrl Pts',(-2.90734243084918,-4.4179521825598,0.949030093725403));
#46915=CARTESIAN_POINT('Ctrl Pts',(-0.440162123945536,-5.27040781417518,
1.02840198377881));
#46916=CARTESIAN_POINT('Ctrl Pts',(2.1342407222512,-4.83900381899044,1.10777387383221));
#46917=CARTESIAN_POINT('Ctrl Pts',(4.18874724188064,-3.228829177505,1.18714576388562));
#46918=CARTESIAN_POINT('Ctrl Pts',(5.22288421068343,-0.832118909543204,
1.26651765393902));
#46919=CARTESIAN_POINT('Ctrl Pts',(4.98473814342391,1.76729369047769,1.34588954399242));
#46920=CARTESIAN_POINT('Ctrl Pts',(3.53232089954478,3.93619745533352,1.42526143404583));
#46921=CARTESIAN_POINT('Ctrl Pts',(1.21943810235538,5.14625223481536,1.50463332409923));
#46922=CARTESIAN_POINT('Ctrl Pts',(-1.39049711694202,5.10269135980955,1.58400521415263));
#46923=CARTESIAN_POINT('Ctrl Pts',(-3.66171031660135,3.81612616476449,1.66337710420604));
#46924=CARTESIAN_POINT('Ctrl Pts',(-5.04093898807,1.59996108251987,1.74274899425944));
#46925=CARTESIAN_POINT('Ctrl Pts',(-5.19220608004013,-1.00595097780601,
1.82212088431284));
#46926=CARTESIAN_POINT('Ctrl Pts',(-4.07866326363067,-3.3668156066614,1.90149277436625));
#46927=CARTESIAN_POINT('Ctrl Pts',(-1.97156710418735,-4.90753140600723,
1.98086466441965));
#46928=CARTESIAN_POINT('Ctrl Pts',(0.61579843785608,-5.25278341751101,2.06023655447306));
#46929=CARTESIAN_POINT('Ctrl Pts',(3.0531568434793,-4.31846901533485,2.13960844452646));
#46930=CARTESIAN_POINT('Ctrl Pts',(4.74677300008174,-2.3321851197991,2.21898033457986));
#46931=CARTESIAN_POINT('Ctrl Pts',(5.28408576066664,0.222213908719184,2.29835222463327));
#46932=CARTESIAN_POINT('Ctrl Pts',(4.53420692607935,2.72248212093367,2.37772411468667));
#46933=CARTESIAN_POINT('Ctrl Pts',(2.67980532059554,4.5595597146017,2.45709600474007));
#46934=CARTESIAN_POINT('Ctrl Pts',(0.172609070663326,5.28593865420646,2.53646789479348));
#46935=CARTESIAN_POINT('Ctrl Pts',(-2.37663436681889,4.72467463787357,2.61583978484688));
#46936=CARTESIAN_POINT('Ctrl Pts',(-4.34693493313492,3.01249033764445,2.69521167490029));
#46937=CARTESIAN_POINT('Ctrl Pts',(-5.25833177151656,0.56647005919948,2.77458356495369));
#46938=CARTESIAN_POINT('Ctrl Pts',(-4.88881062947673,-2.01754107180632,
2.85395545500709));
#46939=CARTESIAN_POINT('Ctrl Pts',(-3.32838603929513,-4.11008366347149,
2.93332734506049));
#46940=CARTESIAN_POINT('Ctrl Pts',(-0.957173977198773,-5.20141897223089,
3.0126992351139));
#46941=CARTESIAN_POINT('Ctrl Pts',(1.64720354707453,-5.02570013250045,3.0920711251673));
#46942=CARTESIAN_POINT('Ctrl Pts',(3.85032593330369,-3.62573186469146,3.1714430152207));
#46943=CARTESIAN_POINT('Ctrl Pts',(5.11551744473197,-1.342543340065,3.25081490527411));
#46944=CARTESIAN_POINT('Ctrl Pts',(5.13458022962935,1.26768577053204,3.33018679532751));
#46945=CARTESIAN_POINT('Ctrl Pts',(3.90287063578958,3.56910943340232,3.40955868538091));
#46946=CARTESIAN_POINT('Ctrl Pts',(1.7204303939291,5.00110593838552,3.48893057543432));
#46947=CARTESIAN_POINT('Ctrl Pts',(-0.881102883784432,5.21484410653825,
3.56830246548772));
#46948=CARTESIAN_POINT('Ctrl Pts',(-3.26800144929621,4.15825779319991,3.64767435554113));
#46949=CARTESIAN_POINT('Ctrl Pts',(-4.85882209535798,2.08872908558557,3.72704624559453));
#46950=CARTESIAN_POINT('Ctrl Pts',(-5.2660444338108,-0.489609403954008,
3.80641813564793));
#46951=CARTESIAN_POINT('Ctrl Pts',(-4.39047000437897,-2.94868012642242,
3.88579002570134));
#46952=CARTESIAN_POINT('Ctrl Pts',(-2.44538680002092,-4.68945889688708,
3.96516191575474));
#46953=CARTESIAN_POINT('Ctrl Pts',(0.0953872160503347,-5.28789586001125,
4.04453380580815));
#46954=CARTESIAN_POINT('Ctrl Pts',(2.61292511742776,-4.59821309619564,4.12390569586154));
#46955=CARTESIAN_POINT('Ctrl Pts',(4.49396024381142,-2.78841580011883,4.20327758591496));
#46956=CARTESIAN_POINT('Ctrl Pts',(5.28027660201492,-0.299366587186749,
4.28264947596836));
#46957=CARTESIAN_POINT('Ctrl Pts',(4.78032926766157,2.26260766374733,4.36202136602176));
#46958=CARTESIAN_POINT('Ctrl Pts',(3.11590430478523,4.27341569598967,4.44139325607517));
#46959=CARTESIAN_POINT('Ctrl Pts',(0.692451950200399,5.24322912373411,4.52076514612856));
#46960=CARTESIAN_POINT('Ctrl Pts',(-1.89968016673685,4.93580354262775,4.60013703618198));
#46961=CARTESIAN_POINT('Ctrl Pts',(-4.02905439992773,3.42602714375309,4.67950892623537));
#46962=CARTESIAN_POINT('Ctrl Pts',(-5.17695989945686,1.08167811604265,4.75888081628878));
#46963=CARTESIAN_POINT('Ctrl Pts',(-5.06376942648468,-1.5261653064819,4.83825270634218));
#46964=CARTESIAN_POINT('Ctrl Pts',(-3.71705592968434,-3.76223823845706,
4.91762459639559));
#46965=CARTESIAN_POINT('Ctrl Pts',(-1.46487583597662,-5.08183826311717,
4.996996486449));
#46966=CARTESIAN_POINT('Ctrl Pts',(1.14414476892732,-5.16351373534013,5.07636837650239));
#46967=CARTESIAN_POINT('Ctrl Pts',(3.47445424064207,-3.98736869087803,5.15574026655581));
#46968=CARTESIAN_POINT('Ctrl Pts',(4.95839434991041,-1.83990945920892,5.2351121566092));
#46969=CARTESIAN_POINT('Ctrl Pts',(5.23448057076031,0.75574764415296,5.31448404666261));
#46970=CARTESIAN_POINT('Ctrl Pts',(4.23545891089922,3.1673062942182,5.39385593671601));
#46971=CARTESIAN_POINT('Ctrl Pts',(2.20468883537238,4.80731614172549,5.47322782676942));
#46972=CARTESIAN_POINT('Ctrl Pts',(-0.363138560455233,5.27627441792221,
5.55259971682281));
#46973=CARTESIAN_POINT('Ctrl Pts',(-2.84250620674952,4.45994392474844,5.63197160687622));
#46974=CARTESIAN_POINT('Ctrl Pts',(-4.62944563286038,2.55718096342436,5.71134349692963));
#46975=CARTESIAN_POINT('Ctrl Pts',(-5.28866234991055,0.0314943796341776,
5.79071538698302));
#46976=CARTESIAN_POINT('Ctrl Pts',(-4.65957262477808,-2.50186416532327,
5.87008727703643));
#46977=CARTESIAN_POINT('Ctrl Pts',(-2.89542132203872,-4.42577413739037,
5.94945916708984));
#46978=CARTESIAN_POINT('Ctrl Pts',(-0.425951794157121,-5.27157532587407,
6.02883105714324));
#46979=CARTESIAN_POINT('Ctrl Pts',(2.14727864795285,-4.8332324334089,6.10820294719664));
#46980=CARTESIAN_POINT('Ctrl Pts',(4.19743676434218,-3.21752481834385,6.18757483725004));
#46981=CARTESIAN_POINT('Ctrl Pts',(5.22510857580644,-0.81803527940062,6.26694672730345));
#46982=CARTESIAN_POINT('Ctrl Pts',(4.97995550378589,1.78072584291422,6.34631861735685));
#46983=CARTESIAN_POINT('Ctrl Pts',(3.52169629398765,3.94570609146495,6.42569050741027));
#46984=CARTESIAN_POINT('Ctrl Pts',(1.20555966211655,5.14952106980711,6.50506239746365));
#46985=CARTESIAN_POINT('Ctrl Pts',(-1.40424863498509,5.09892411381582,6.58443428751707));
#46986=CARTESIAN_POINT('Ctrl Pts',(-3.67198507285601,3.80624052997609,6.66380617757046));
#46987=CARTESIAN_POINT('Ctrl Pts',(-5.04523407478029,1.58636517800468,6.74317806762388));
#46988=CARTESIAN_POINT('Ctrl Pts',(-5.1894752235243,-1.01994521996889,6.82254995767727));
#46989=CARTESIAN_POINT('Ctrl Pts',(-4.06957169452636,-3.37779921996849,
6.90192184773068));
#46990=CARTESIAN_POINT('Ctrl Pts',(-1.95832950858598,-4.91282880661553,
6.98129373778407));
#46991=CARTESIAN_POINT('Ctrl Pts',(0.629957410957137,-5.25110417033315,
7.06066562783749));
#46992=CARTESIAN_POINT('Ctrl Pts',(3.06478809957816,-4.31022218127953,7.14003751789089));
#46993=CARTESIAN_POINT('Ctrl Pts',(4.75304319093534,-2.31937960938119,7.21940940794429));
#46994=CARTESIAN_POINT('Ctrl Pts',(5.28346748166331,0.236458701502723,7.2987812979977));
#46995=CARTESIAN_POINT('Ctrl Pts',(4.52685078861501,2.73469619609302,7.37815318805109));
#46996=CARTESIAN_POINT('Ctrl Pts',(2.66750326347436,4.56676775046241,7.45752507810451));
#46997=CARTESIAN_POINT('Ctrl Pts',(0.158357847769689,5.28638478918814,7.5368969681579));
#46998=CARTESIAN_POINT('Ctrl Pts',(-2.38936318913255,4.71825019448189,7.61626885821132));
#46999=CARTESIAN_POINT('Ctrl Pts',(-4.3550406419278,3.0007602960695,7.69564074826471));
#47000=CARTESIAN_POINT('Ctrl Pts',(-5.25983983406839,0.552291831604834,
7.77501263831812));
#47001=CARTESIAN_POINT('Ctrl Pts',(-4.88335368508791,-2.03071370056153,
7.85438452837152));
#47002=CARTESIAN_POINT('Ctrl Pts',(-3.31729338754006,-4.11904187017964,
7.93375641842492));
#47003=CARTESIAN_POINT('Ctrl Pts',(-0.943147763491834,-5.20398055756651,
8.01312830847834));
#47004=CARTESIAN_POINT('Ctrl Pts',(1.66074656812082,-5.02124109994579,8.09250019853171));
#47005=CARTESIAN_POINT('Ctrl Pts',(3.86008671173945,-3.61533842470695,8.17187208858515));
#47006=CARTESIAN_POINT('Ctrl Pts',(5.11911827653537,-1.32874731162534,8.25124397863853));
#47007=CARTESIAN_POINT('Ctrl Pts',(5.13114396014337,1.28152370543593,8.33061586869195));
#47008=CARTESIAN_POINT('Ctrl Pts',(3.89323433265495,3.57961838445758,8.40998775874535));
#47009=CARTESIAN_POINT('Ctrl Pts',(1.70694143925982,5.00572594837628,8.48935964879875));
#47010=CARTESIAN_POINT('Ctrl Pts',(-0.895158610488236,5.21244975125697,
8.56873153885215));
#47011=CARTESIAN_POINT('Ctrl Pts',(-3.27920000412133,4.14943233229326,8.64810342890557));
#47012=CARTESIAN_POINT('Ctrl Pts',(-4.86443553513654,2.0756223817956,8.72747531895896));
#47013=CARTESIAN_POINT('Ctrl Pts',(-5.26470533703792,-0.503804586595236,
8.80684720901237));
#47014=CARTESIAN_POINT('Ctrl Pts',(-4.38250457206448,-2.96050587284403,
8.88621909906576));
#47015=CARTESIAN_POINT('Ctrl Pts',(-2.43273539384546,-4.69603448143659,
8.96559098911917));
#47016=CARTESIAN_POINT('Ctrl Pts',(0.109642741545844,-5.28761948484726,
9.04496287917257));
#47017=CARTESIAN_POINT('Ctrl Pts',(2.62531214778668,-4.59115208569632,9.12433476922599));
#47018=CARTESIAN_POINT('Ctrl Pts',(4.50146132585655,-2.77629020081255,9.20370665927937));
#47019=CARTESIAN_POINT('Ctrl Pts',(5.28106448876342,-0.285130168224959,
9.28307854933281));
#47020=CARTESIAN_POINT('Ctrl Pts',(4.77421203164548,2.27548694221733,9.36245043938617));
#47021=CARTESIAN_POINT('Ctrl Pts',(3.10437209115777,4.28180047024037,9.44182232943961));
#47022=CARTESIAN_POINT('Ctrl Pts',(0.67831398067512,5.24507688131743,9.52119421949299));
#47023=CARTESIAN_POINT('Ctrl Pts',(-1.91297991407746,4.93066417388633,9.6005661095464));
#47024=CARTESIAN_POINT('Ctrl Pts',(-4.03827613607002,3.41515258753654,9.6799379995998));
#47025=CARTESIAN_POINT('Ctrl Pts',(-5.1798572298885,1.06771739017486,9.75930988965322));
#47026=CARTESIAN_POINT('Ctrl Pts',(-5.05963656792565,-1.53981140008104,
9.8386817797066));
#47027=CARTESIAN_POINT('Ctrl Pts',(-3.70689963733171,-3.77224554159189,
9.91805366976003));
#47028=CARTESIAN_POINT('Ctrl Pts',(-1.45117016016697,-5.08576901889487,
9.99742555981341));
#47029=CARTESIAN_POINT('Ctrl Pts',(1.1580611559038,-5.16041042035386,10.0767974498668));
#47030=CARTESIAN_POINT('Ctrl Pts',(3.48519133772131,-3.97798726578937,10.1561693399202));
#47031=CARTESIAN_POINT('Ctrl Pts',(4.96333662401008,-1.82653521840402,10.2355412299736));
#47032=CARTESIAN_POINT('Ctrl Pts',(5.23242409484924,0.769856765217389,10.314913120027));
#47033=CARTESIAN_POINT('Ctrl Pts',(4.22690463795744,3.1787133448809,10.3942850100804));
#47034=CARTESIAN_POINT('Ctrl Pts',(2.1917205673539,4.81324238969408,10.4736569001339));
#47035=CARTESIAN_POINT('Ctrl Pts',(-0.377361782165876,5.27527624230907,
10.5530287901872));
#47036=CARTESIAN_POINT('Ctrl Pts',(-2.85451963682615,4.45226447892349,10.6324006802407));
#47037=CARTESIAN_POINT('Ctrl Pts',(-4.63632282632763,2.54469094339242,10.711772570294));
#47038=CARTESIAN_POINT('Ctrl Pts',(-5.28872803766221,0.0172363266288179,
10.7911444603475));
#47039=CARTESIAN_POINT('Ctrl Pts',(-4.65281080542322,-2.5144170211496,10.8705163504009));
#47040=CARTESIAN_POINT('Ctrl Pts',(-2.88347915980519,-4.43356394814365,
10.9498882404543));
#47041=CARTESIAN_POINT('Ctrl Pts',(-0.411738373331464,-5.27270451089727,
11.0292601305077));
#47042=CARTESIAN_POINT('Ctrl Pts',(2.16030096951836,-4.82742592572977,11.1086320205611));
#47043=CARTESIAN_POINT('Ctrl Pts',(4.20609577793862,-3.20619707038057,11.1880039106145));
#47044=CARTESIAN_POINT('Ctrl Pts',(5.22729496488813,-0.803945705483474,
11.2673758006679));
#47045=CARTESIAN_POINT('Ctrl Pts',(4.975136668812,1.79414505376576,11.3467476907213));
#47046=CARTESIAN_POINT('Ctrl Pts',(3.51104609249152,3.95518604919035,11.4261195807747));
#47047=CARTESIAN_POINT('Ctrl Pts',(1.19167245960881,5.152752477688,11.5054914708281));
#47048=CARTESIAN_POINT('Ctrl Pts',(-1.41798994671238,5.09511980804502,11.5848633608815));
#47049=CARTESIAN_POINT('Ctrl Pts',(-3.68223314068194,3.79632723101863,11.6642352509349));
#47050=CARTESIAN_POINT('Ctrl Pts',(-5.04949249206616,1.57275774354392,11.7436071409883));
#47051=CARTESIAN_POINT('Ctrl Pts',(-5.18670664924514,-1.03393204901786,
11.8229790310417));
#47052=CARTESIAN_POINT('Ctrl Pts',(-4.06045054724843,-3.38875828300867,
11.9023509210951));
#47053=CARTESIAN_POINT('Ctrl Pts',(-1.94507767959685,-4.91809050014781,
11.9817228111485));
#47054=CARTESIAN_POINT('Ctrl Pts',(0.644111805448097,-5.24938675745961,
12.0610947012019));
#47055=CARTESIAN_POINT('Ctrl Pts',(3.0763970804032,-4.30194401997477,12.1404665912553));
#47056=CARTESIAN_POINT('Ctrl Pts',(4.7592788360615,-2.30655724141565,12.2198384813087));
#47057=CARTESIAN_POINT('Ctrl Pts',(5.28281080174027,0.250701775674464,12.2992103713621));
#47058=CARTESIAN_POINT('Ctrl Pts',(4.51946174941847,2.74689039512926,12.3785822614155));
#47059=CARTESIAN_POINT('Ctrl Pts',(2.6551818185972,4.57394259446934,12.4579541514689));
#47060=CARTESIAN_POINT('Ctrl Pts',(0.144105473910954,5.28679250204684,12.5373260415223));
#47061=CARTESIAN_POINT('Ctrl Pts',(-2.40207464524796,4.7117914582425,12.6166979315757));
#47062=CARTESIAN_POINT('Ctrl Pts',(-4.36311469772651,2.98900844458373,12.6960698216291));
#47063=CARTESIAN_POINT('Ctrl Pts',(-5.26130966742946,0.538109589882336,
12.7754417116825));
#47064=CARTESIAN_POINT('Ctrl Pts',(-4.87786124785798,-2.043871569829,12.854813601736));
#47065=CARTESIAN_POINT('Ctrl Pts',(-3.30617662527107,-4.12797013916298,
12.9341854917893));
#47066=CARTESIAN_POINT('Ctrl Pts',(-0.929114694865931,-5.20650431970379,
13.0135573818428));
#47067=CARTESIAN_POINT('Ctrl Pts',(1.67427751864803,-5.01674557236658,13.0929292718962));
#47068=CARTESIAN_POINT('Ctrl Pts',(3.86981943456978,-3.60491870797887,13.1723011619496));
#47069=CARTESIAN_POINT('Ctrl Pts',(5.12268190193035,-1.31494162567972,13.251673052003));
#47070=CARTESIAN_POINT('Ctrl Pts',(5.12767039684476,1.29535232606109,13.3310449420564));
#47071=CARTESIAN_POINT('Ctrl Pts',(3.8835697329937,3.59010131838716,13.4104168321098));
#47072=CARTESIAN_POINT('Ctrl Pts',(1.69344007832116,5.01030957610862,13.4897887221632));
#47073=CARTESIAN_POINT('Ctrl Pts',(-0.909207831064397,5.21001751122212,
13.5691606122166));
#47074=CARTESIAN_POINT('Ctrl Pts',(-3.29037472530003,4.14057671278008,13.64853250227));
#47075=CARTESIAN_POINT('Ctrl Pts',(-4.87001361957351,2.06250059211591,13.7279043923234));
#47076=CARTESIAN_POINT('Ctrl Pts',(-5.26332797571119,-0.517996107520081,
13.8072762823768));
#47077=CARTESIAN_POINT('Ctrl Pts',(-4.37450728714447,-2.97231010192914,
13.8866481724302));
#47078=CARTESIAN_POINT('Ctrl Pts',(-2.420066306237,-4.70257593460501,13.9660200624836));
#47079=CARTESIAN_POINT('Ctrl Pts',(0.123897470143854,-5.28730467858643,
14.045391952537));
#47080=CARTESIAN_POINT('Ctrl Pts',(2.63768009704007,-4.58405770611459,14.1247638425904));
#47081=CARTESIAN_POINT('Ctrl Pts',(4.50892969070322,-2.76414442307289,14.2041357326438));
#47082=CARTESIAN_POINT('Ctrl Pts',(5.28181399205766,-0.270891676900501,
14.2835076226972));
#47083=CARTESIAN_POINT('Ctrl Pts',(4.7680600960438,2.28834968215629,14.3628795127506));
#47084=CARTESIAN_POINT('Ctrl Pts',(3.09281731455568,4.29015412381589,14.442251402804));
#47085=CARTESIAN_POINT('Ctrl Pts',(0.664171081076821,5.24688651700904,14.5216232928574));
#47086=CARTESIAN_POINT('Ctrl Pts',(-1.92626575763464,4.9254889684451,14.6009951829108));
#47087=CARTESIAN_POINT('Ctrl Pts',(-4.04746852150321,3.4042532095528,14.6803670729642));
#47088=CARTESIAN_POINT('Ctrl Pts',(-5.1827169124532,1.05374890400015,14.7597389630177));
#47089=CARTESIAN_POINT('Ctrl Pts',(-5.05546693527891,-1.55344630213332,
14.839110853071));
#47090=CARTESIAN_POINT('Ctrl Pts',(-3.69671640275692,-3.78222542756219,
14.9184827431245));
#47091=CARTESIAN_POINT('Ctrl Pts',(-1.43745393706629,-5.08966281065088,
14.9978546331779));
#47092=CARTESIAN_POINT('Ctrl Pts',(1.17196912594334,-5.15726959884254,15.0772265232312));
#47093=CARTESIAN_POINT('Ctrl Pts',(3.49590310398282,-3.96857692817882,15.1565984132847));
#47094=CARTESIAN_POINT('Ctrl Pts',(4.96824282394235,-1.81314770210679,15.2359703033381));
#47095=CARTESIAN_POINT('Ctrl Pts',(5.23032958900857,0.783960290864088,15.3153421933915));
#47096=CARTESIAN_POINT('Ctrl Pts',(4.21831964333036,3.19009729224721,15.3947140834449));
#47097=CARTESIAN_POINT('Ctrl Pts',(2.17873636962922,4.81913365439941,15.4740859734983));
#47098=CARTESIAN_POINT('Ctrl Pts',(-0.391582261162836,5.27423972531144,
15.5534578635517));
#47099=CARTESIAN_POINT('Ctrl Pts',(-2.86651231988745,4.44455267346898,15.6328297536051));
#47100=CARTESIAN_POINT('Ctrl Pts',(-4.64316632240643,2.53218242822043,15.7122016436585));
#47101=CARTESIAN_POINT('Ctrl Pts',(-5.28875528625864,0.00297814834715876,
15.7915735337119));
#47102=CARTESIAN_POINT('Ctrl Pts',(-4.64601516884489,-2.52695160186966,
15.8709454237653));
#47103=CARTESIAN_POINT('Ctrl Pts',(-2.87151604007055,-4.44132153518687,
15.9503173138187));
#47104=CARTESIAN_POINT('Ctrl Pts',(-0.397521959947054,-5.27379537322474,
16.0296892038721));
#47105=CARTESIAN_POINT('Ctrl Pts',(2.1733075897557,-4.82158433170501,16.1090610939255));
#47106=CARTESIAN_POINT('Ctrl Pts',(4.21472422106055,-3.1948460193553,16.1884329839789));
#47107=CARTESIAN_POINT('Ctrl Pts',(5.22944336137754,-0.789850288404984,
16.2678048740323));
#47108=CARTESIAN_POINT('Ctrl Pts',(4.97028167379658,1.80755122457726,16.3471767640857));
#47109=CARTESIAN_POINT('Ctrl Pts',(3.50037037246945,3.9646372600474,16.4265486541391));
#47110=CARTESIAN_POINT('Ctrl Pts',(1.17777659548083,5.15594643483254,16.5059205441925));
#47111=CARTESIAN_POINT('Ctrl Pts',(-1.43172095156687,5.09127847004474,16.5852924342459));
#47112=CARTESIAN_POINT('Ctrl Pts',(-3.69245444696213,3.78638634033038,16.6646643242993));
#47113=CARTESIAN_POINT('Ctrl Pts',(-5.05371420635461,1.5591388772047,16.7440362143527));
#47114=CARTESIAN_POINT('Ctrl Pts',(-5.18390038229795,-1.04791136166686,
16.8234081044061));
#47115=CARTESIAN_POINT('Ctrl Pts',(-4.05129987868913,-3.39969271923294,
16.9027799944595));
#47116=CARTESIAN_POINT('Ctrl Pts',(-1.93181173129365,-4.9233164424874,16.9821518845129));
#47117=CARTESIAN_POINT('Ctrl Pts',(0.658261551986501,-5.24763120247215,
17.0615237745663));
#47118=CARTESIAN_POINT('Ctrl Pts',(3.08798363825942,-4.29363457062506,17.1408956646198));
#47119=CARTESIAN_POINT('Ctrl Pts',(4.76548000969996,-2.29371814868002,17.2202675546731));
#47120=CARTESIAN_POINT('Ctrl Pts',(5.28211549991427,0.264943102456271,17.2996394447266));
#47121=CARTESIAN_POINT('Ctrl Pts',(4.51204028846775,2.7590644882845,17.3790113347799));
#47122=CARTESIAN_POINT('Ctrl Pts',(2.64284027062647,4.58108446095533,17.4583832248334));
#47123=CARTESIAN_POINT('Ctrl Pts',(0.129853572473924,5.28716128664959,17.5377551148867));
#47124=CARTESIAN_POINT('Ctrl Pts',(-2.41477151246584,4.70529942618515,17.6171270049402));
#47125=CARTESIAN_POINT('Ctrl Pts',(-4.37115162329109,2.9772330746438,17.6964988949936));
#47126=CARTESIAN_POINT('Ctrl Pts',(-5.2627514922539,0.523926824466488,17.775870785047));
#47127=CARTESIAN_POINT('Ctrl Pts',(-4.87231403886184,-2.05702097999283,
17.8552426751004));
#47128=CARTESIAN_POINT('Ctrl Pts',(-3.29507231119166,-4.13685632854999,
17.9346145651538));
#47129=CARTESIAN_POINT('Ctrl Pts',(-0.915005995631555,-5.20901304408194,
18.0139864552072));
#47130=CARTESIAN_POINT('Ctrl Pts',(1.68766624540468,-5.01217052435341,18.0933583452606));
#47131=CARTESIAN_POINT('Ctrl Pts',(3.8797695997979,-3.59455409188004,18.172730235314));
#47132=CARTESIAN_POINT('Ctrl Pts',(5.12574462250332,-1.30097287489382,18.2521021253674));
#47133=CARTESIAN_POINT('Ctrl Pts',(5.12503498129813,1.3088817301615,18.3314740154208));
#47134=CARTESIAN_POINT('Ctrl Pts',(3.87222469260764,3.60110493868871,18.4108459054742));
#47135=CARTESIAN_POINT('Ctrl Pts',(1.68303999757325,5.01382783115876,18.4902177955276));
#47136=CARTESIAN_POINT('Ctrl Pts',(-0.929079443196312,5.2094618875472,18.569589685581));
#47137=CARTESIAN_POINT('Ctrl Pts',(-3.29092685490746,4.12830747359753,18.6489615756344));
#47138=CARTESIAN_POINT('Ctrl Pts',(-5.42625155540715,1.36247937795741,18.7547907623723));
#47139=CARTESIAN_POINT('Ctrl Pts',(-4.95432466322409,-3.37745298000962,
18.8870772457946));
#47140=CARTESIAN_POINT('Ctrl Pts',(0.158509478955228,-5.99736559883162,
19.0458210259014));
#47141=CARTESIAN_POINT('Ctrl Pts',(5.11967904485094,-3.11863163173532,19.2045648060083));
#47142=CARTESIAN_POINT('Ctrl Pts',(5.39954635636598,2.60828838171404,19.363308586115));
#47143=CARTESIAN_POINT('Ctrl Pts',(0.736723079475925,5.95134306184737,19.5220523662219));
#47144=CARTESIAN_POINT('Ctrl Pts',(-4.59927593805429,3.84720861430001,19.6807961463287));
#47145=CARTESIAN_POINT('Ctrl Pts',(-5.72720375155086,-1.77677009197966,
19.8395399264355));
#47146=CARTESIAN_POINT('Ctrl Pts',(-1.61419617037545,-5.77483540889735,
19.9982837065423));
#47147=CARTESIAN_POINT('Ctrl Pts',(3.97578039972893,-4.48936692070975,20.1570274866491));
#47148=CARTESIAN_POINT('Ctrl Pts',(5.92771323046147,0.905806267444479,20.3157712667559));
#47149=CARTESIAN_POINT('Ctrl Pts',(2.45559119020176,5.46873373673919,20.4745150468627));
#47150=CARTESIAN_POINT('Ctrl Pts',(-3.26379011618977,5.03400372054189,20.6332588269695));
#47151=CARTESIAN_POINT('Ctrl Pts',(-5.99600976813329,-0.0197068834827358,
20.7920026070763));
#47152=CARTESIAN_POINT('Ctrl Pts',(-3.70230252414087,-4.19446206534972,
20.9242890904987));
#47153=CARTESIAN_POINT('Ctrl Pts',(-0.376480053418488,-5.26605971579228,
21.0301182772365));
#47154=CARTESIAN_POINT('Ctrl Pts',(2.18257651229242,-4.8205851862161,21.10949016729));
#47155=CARTESIAN_POINT('Ctrl Pts',(4.22530652207796,-3.18086119603153,21.1888620573433));
#47156=CARTESIAN_POINT('Ctrl Pts',(5.23050112077121,-0.777135043026565,
21.2682339473968));
#47157=CARTESIAN_POINT('Ctrl Pts',(4.96594823061178,1.82167865277159,21.3476058374501));
#47158=CARTESIAN_POINT('Ctrl Pts',(3.48937383888172,3.97367066688458,21.4269777275036));
#47159=CARTESIAN_POINT('Ctrl Pts',(1.16402860508423,5.15930893371516,21.5063496175569));
#47160=CARTESIAN_POINT('Ctrl Pts',(-1.44552439996815,5.08729102078623,21.5857215076104));
#47161=CARTESIAN_POINT('Ctrl Pts',(-3.70260503654192,3.77647571272897,21.6650933976637));
#47162=CARTESIAN_POINT('Ctrl Pts',(-5.057922432142,1.54547807796832,21.7444652877172));
#47163=CARTESIAN_POINT('Ctrl Pts',(-5.18104412158608,-1.06186685398839,
21.8238371777705));
#47164=CARTESIAN_POINT('Ctrl Pts',(-4.04212630117128,-3.41061102326193,
21.903209067824));
#47165=CARTESIAN_POINT('Ctrl Pts',(-1.91852825506946,-4.92850206746972,
21.9825809578774));
#47166=CARTESIAN_POINT('Ctrl Pts',(0.672404619068471,-5.245839892308,22.0619528479308));
#47167=CARTESIAN_POINT('Ctrl Pts',(3.09954884704109,-4.28529268150223,22.1413247379842));
#47168=CARTESIAN_POINT('Ctrl Pts',(4.77164579536192,-2.28086298099128,22.2206966280376));
#47169=CARTESIAN_POINT('Ctrl Pts',(5.28138253005217,0.279182711729235,22.300068518091));
#47170=CARTESIAN_POINT('Ctrl Pts',(4.50458503707303,2.77121862106756,22.3794404081444));
#47171=CARTESIAN_POINT('Ctrl Pts',(2.63048120009391,4.58819259887664,22.4588122981978));
#47172=CARTESIAN_POINT('Ctrl Pts',(0.115597647321455,5.28749259670008,22.5381841882512));
#47173=CARTESIAN_POINT('Ctrl Pts',(-2.42744506809483,4.69877132337436,22.6175560783046));
#47174=CARTESIAN_POINT('Ctrl Pts',(-4.37916762715256,2.96543963879382,22.696927968358));
#47175=CARTESIAN_POINT('Ctrl Pts',(-5.26413459813381,0.509733484286287,
22.7762998584114));
#47176=CARTESIAN_POINT('Ctrl Pts',(-4.86677005798463,-2.07014265165558,
22.8556717484648));
#47177=CARTESIAN_POINT('Ctrl Pts',(-3.28387109087741,-4.14573660239302,
22.9350436385182));
#47178=CARTESIAN_POINT('Ctrl Pts',(-0.901028401772815,-5.21143830245831,
23.0144155285717));
#47179=CARTESIAN_POINT('Ctrl Pts',(1.70130281532621,-5.00764516247504,23.093787418625));
#47180=CARTESIAN_POINT('Ctrl Pts',(3.88920043041414,-3.58400074773866,23.1731593086785));
#47181=CARTESIAN_POINT('Ctrl Pts',(5.12969743029434,-1.28730168253193,23.2525311987318));
#47182=CARTESIAN_POINT('Ctrl Pts',(5.12061148999571,1.32298122241883,23.3319030887853));
#47183=CARTESIAN_POINT('Ctrl Pts',(3.86415592530766,3.6109888303426,23.4112749788386));
#47184=CARTESIAN_POINT('Ctrl Pts',(1.66640053022393,5.01936755177924,23.4906468688921));
#47185=CARTESIAN_POINT('Ctrl Pts',(-0.937286345425383,5.20503944789203,
23.5700187589454));
#47186=CARTESIAN_POINT('Ctrl Pts',(-3.31265234202061,4.12277525560054,23.6493906489989));
#47187=CARTESIAN_POINT('Ctrl Pts',(-4.88106356050821,2.03621213668325,23.7287625390522));
#47188=CARTESIAN_POINT('Ctrl Pts',(-5.26045849971908,-0.546367751667005,
23.8081344291057));
#47189=CARTESIAN_POINT('Ctrl Pts',(-4.35841739221935,-2.99585366506712,
23.887506319159));
#47190=CARTESIAN_POINT('Ctrl Pts',(-2.3946754551717,-4.71555625687105,23.9668782092125));
#47191=CARTESIAN_POINT('Ctrl Pts',(0.152404122233421,-5.28655978220554,
24.0462500992659));
#47192=CARTESIAN_POINT('Ctrl Pts',(2.66235839280233,-4.56976904619763,24.1256219893193));
#47193=CARTESIAN_POINT('Ctrl Pts',(4.52376805191542,-2.73979268554746,24.2049938793727));
#47194=CARTESIAN_POINT('Ctrl Pts',(5.28319782677237,-0.242408891126616,
24.2843657694261));
#47195=CARTESIAN_POINT('Ctrl Pts',(4.75565230518779,2.3140251726099,24.3637376594795));
#47196=CARTESIAN_POINT('Ctrl Pts',(3.0696404085172,4.30676782630642,24.4431095495329));
#47197=CARTESIAN_POINT('Ctrl Pts',(0.635870902865647,5.25039137038364,24.5224814395863));
#47198=CARTESIAN_POINT('Ctrl Pts',(-1.95279534724764,4.9150311981795,24.6018533296397));
#47199=CARTESIAN_POINT('Ctrl Pts',(-4.06576497321052,3.38238030533593,24.6812252196931));
#47200=CARTESIAN_POINT('Ctrl Pts',(-5.18832325111748,1.02578905688434,24.7605971097465));
#47201=CARTESIAN_POINT('Ctrl Pts',(-5.04701746921096,-1.58068213527875,
24.8399689997999));
#47202=CARTESIAN_POINT('Ctrl Pts',(-3.67626940318832,-3.80210265806849,
24.9193408898533));
#47203=CARTESIAN_POINT('Ctrl Pts',(-1.40999024783327,-5.09733938916421,
24.9987127799067));
#47204=CARTESIAN_POINT('Ctrl Pts',(1.19975941093347,-5.1508755278289,25.0780846699601));
#47205=CARTESIAN_POINT('Ctrl Pts',(3.51725033281924,-3.94966978918403,25.1574565600135));
#47206=CARTESIAN_POINT('Ctrl Pts',(4.97794685893178,-1.7863332323397,25.2368284500669));
#47207=CARTESIAN_POINT('Ctrl Pts',(5.226026548707,0.812150145920977,25.3162003401203));
#47208=CARTESIAN_POINT('Ctrl Pts',(4.20105773883081,3.21279554629917,25.3955722301737));
#47209=CARTESIAN_POINT('Ctrl Pts',(2.15272056265901,4.83081106300121,25.4749441202272));
#47210=CARTESIAN_POINT('Ctrl Pts',(-0.420014577610356,5.27205169757513,
25.5543160102805));
#47211=CARTESIAN_POINT('Ctrl Pts',(-2.89043509646038,4.42903220810823,25.6336879003339));
#47212=CARTESIAN_POINT('Ctrl Pts',(-4.65675202368223,2.50711027624266,25.7130597903873));
#47213=CARTESIAN_POINT('Ctrl Pts',(-5.28869446548081,-0.0255381695211706,
25.7924316804408));
#47214=CARTESIAN_POINT('Ctrl Pts',(-4.63232264181493,-2.55196557371741,
25.8718035704942));
#47215=CARTESIAN_POINT('Ctrl Pts',(-2.84752727607513,-4.45673981283608,
25.9511754605475));
#47216=CARTESIAN_POINT('Ctrl Pts',(-0.369080568778156,-5.27586209837409,
26.030547350601));
#47217=CARTESIAN_POINT('Ctrl Pts',(2.19927334812716,-4.80979605467087,26.1099192406543));
#47218=CARTESIAN_POINT('Ctrl Pts',(4.23188914543768,-3.17207433835284,26.1892911307078));
#47219=CARTESIAN_POINT('Ctrl Pts',(5.23362611404738,-0.761642334479479,
26.2686630207611));
#47220=CARTESIAN_POINT('Ctrl Pts',(4.96046334571002,1.83432405620638,26.3480349108146));
#47221=CARTESIAN_POINT('Ctrl Pts',(3.47894268615705,3.98345316700778,26.427406800868));
#47222=CARTESIAN_POINT('Ctrl Pts',(1.14995928876529,5.16222190355009,26.5067786909214));
#47223=CARTESIAN_POINT('Ctrl Pts',(-1.45915164597797,5.08348481077201,26.5861505809748));
#47224=CARTESIAN_POINT('Ctrl Pts',(-3.71281646953845,3.76642207019263,26.6655224710282));
#47225=CARTESIAN_POINT('Ctrl Pts',(-5.06204741929919,1.53186725014815,26.7448943610816));
#47226=CARTESIAN_POINT('Ctrl Pts',(-5.17817482237054,-1.07584704130177,
26.824266251135));
#47227=CARTESIAN_POINT('Ctrl Pts',(-4.032910300408,-3.42148737483758,26.9036381411884));
#47228=CARTESIAN_POINT('Ctrl Pts',(-1.90523775596165,-4.93366095719681,
26.9830100312419));
#47229=CARTESIAN_POINT('Ctrl Pts',(0.686546488664775,-5.24400565085624,
27.0623819212952));
#47230=CARTESIAN_POINT('Ctrl Pts',(3.11108952829732,-4.27692217537667,27.1417538113486));
#47231=CARTESIAN_POINT('Ctrl Pts',(4.77777804511651,-2.267989924782,27.221125701402));
#47232=CARTESIAN_POINT('Ctrl Pts',(5.28061040557762,0.293419651379019,27.3004975914554));
#47233=CARTESIAN_POINT('Ctrl Pts',(4.49709775967288,2.7833528499375,27.3798694815089));
#47234=CARTESIAN_POINT('Ctrl Pts',(2.61810205366886,4.59526745509821,27.4592413715622));
#47235=CARTESIAN_POINT('Ctrl Pts',(0.101342482461748,5.28778507964899,27.5386132616156));
#47236=CARTESIAN_POINT('Ctrl Pts',(-2.44010389315526,4.69220996311103,27.617985151669));
#47237=CARTESIAN_POINT('Ctrl Pts',(-4.38714636147802,2.95362288558985,27.6973570417224));
#47238=CARTESIAN_POINT('Ctrl Pts',(-5.26548968692851,0.495539810872365,
27.7767289317758));
#47239=CARTESIAN_POINT('Ctrl Pts',(-4.86117137960698,-2.08325566491491,
27.8561008218293));
#47240=CARTESIAN_POINT('Ctrl Pts',(-3.27268248423349,-4.15457467193712,
27.9354727118826));
#47241=CARTESIAN_POINT('Ctrl Pts',(-0.886975379660524,-5.21384848487045,
28.0148446019361));
#47242=CARTESIAN_POINT('Ctrl Pts',(1.71479696411104,-5.00304034754724,28.0942164919895));
#47243=CARTESIAN_POINT('Ctrl Pts',(3.89884856306386,-3.57350265560346,28.1735883820429));
#47244=CARTESIAN_POINT('Ctrl Pts',(5.1331492820092,-1.27346762656861,28.2529602720963));
#47245=CARTESIAN_POINT('Ctrl Pts',(5.11702619789033,1.3367812975255,28.3323321621497));
#47246=CARTESIAN_POINT('Ctrl Pts',(3.85440685831077,3.62139325645763,28.4117040522031));
#47247=CARTESIAN_POINT('Ctrl Pts',(1.6528625396316,5.02384183393471,28.4910759422564));
#47248=CARTESIAN_POINT('Ctrl Pts',(-0.951315435152638,5.20249366075061,
28.5704478323099));
#47249=CARTESIAN_POINT('Ctrl Pts',(-3.32375507563475,4.11382954733206,28.6498197223633));
#47250=CARTESIAN_POINT('Ctrl Pts',(-4.8865353366993,2.02304566199065,28.7291916124167));
#47251=CARTESIAN_POINT('Ctrl Pts',(-5.25896640590637,-0.560547668676075,
28.8085635024701));
#47252=CARTESIAN_POINT('Ctrl Pts',(-4.35032489915935,-3.00759282800452,
28.8879353925235));
#47253=CARTESIAN_POINT('Ctrl Pts',(-2.38195387625792,-4.72199503162487,
28.9673072825769));
#47254=CARTESIAN_POINT('Ctrl Pts',(0.166655838534471,-5.28612969750008,
29.0466791726303));
#47255=CARTESIAN_POINT('Ctrl Pts',(2.67466855994625,-4.56257486971391,29.1260510626837));
#47256=CARTESIAN_POINT('Ctrl Pts',(4.53113794043359,-2.72758690275364,29.2054229527372));
#47257=CARTESIAN_POINT('Ctrl Pts',(5.28383214813505,-0.228164803693758,
29.2847948427905));
#47258=CARTESIAN_POINT('Ctrl Pts',(4.74939654011487,2.32683773651173,29.3641667328439));
#47259=CARTESIAN_POINT('Ctrl Pts',(3.05801844753361,4.31502775447088,29.4435386228973));
#47260=CARTESIAN_POINT('Ctrl Pts',(0.621713829942241,5.25208656259286,29.5229105129507));
#47261=CARTESIAN_POINT('Ctrl Pts',(-1.96603890048284,4.90974870936366,29.6022824030042));
#47262=CARTESIAN_POINT('Ctrl Pts',(-4.07486890650364,3.37140693807791,29.6816542930575));
#47263=CARTESIAN_POINT('Ctrl Pts',(-5.19106986646947,1.01179789915904,29.7610261831109));
#47264=CARTESIAN_POINT('Ctrl Pts',(-5.04273769720158,-1.59428286841832,
29.8403980731643));
#47265=CARTESIAN_POINT('Ctrl Pts',(-3.66600578680595,-3.81199985813419,
29.9197699632177));
#47266=CARTESIAN_POINT('Ctrl Pts',(-1.39624298131062,-5.10112212012718,
29.9991418532712));
#47267=CARTESIAN_POINT('Ctrl Pts',(1.21364152390063,-5.1476223247995,30.0785137433246));
#47268=CARTESIAN_POINT('Ctrl Pts',(3.52788564023963,-3.94017312521939,30.157885633378));
#47269=CARTESIAN_POINT('Ctrl Pts',(4.98274462345863,-1.7729064737611,30.2372575234313));
#47270=CARTESIAN_POINT('Ctrl Pts',(5.22381804552127,0.826236270443475,30.3166294134848));
#47271=CARTESIAN_POINT('Ctrl Pts',(4.19238095442003,3.22410968801099,30.3960013035382));
#47272=CARTESIAN_POINT('Ctrl Pts',(2.13968914249988,4.83659712202475,30.4753731935916));
#47273=CARTESIAN_POINT('Ctrl Pts',(-0.434226208411599,5.27090020273941,
30.554745083645));
#47274=CARTESIAN_POINT('Ctrl Pts',(-2.90236501609743,4.4212236610065,30.6341169736984));
#47275=CARTESIAN_POINT('Ctrl Pts',(-4.66349413013793,2.49454682166501,30.7134888637518));
#47276=CARTESIAN_POINT('Ctrl Pts',(-5.28860639654603,-0.0397961018483339,
30.7928607538052));
#47277=CARTESIAN_POINT('Ctrl Pts',(-4.62542585088724,-2.56444478303865,
30.8722326438586));
#47278=CARTESIAN_POINT('Ctrl Pts',(-2.83550180615875,-4.46440039138299,
30.951604533912));
#47279=CARTESIAN_POINT('Ctrl Pts',(-0.354855797726762,-5.27683794616905,
31.0309764239654));
#47280=CARTESIAN_POINT('Ctrl Pts',(2.21223229757146,-4.80384945735102,31.1103483140188));
#47281=CARTESIAN_POINT('Ctrl Pts',(4.24042550187443,-3.16065387386267,31.1897202040722));
#47282=CARTESIAN_POINT('Ctrl Pts',(5.23566043994338,-0.747530002690045,
31.2690920941256));
#47283=CARTESIAN_POINT('Ctrl Pts',(4.95550008377996,1.84769052250822,31.348463984179));
#47284=CARTESIAN_POINT('Ctrl Pts',(3.46819087602115,3.99281772621712,31.4278358742324));
#47285=CARTESIAN_POINT('Ctrl Pts',(1.13603804757386,5.16530336977167,31.5072077642858));
#47286=CARTESIAN_POINT('Ctrl Pts',(-1.47285113468488,5.07953254565492,31.5865796543392));
#47287=CARTESIAN_POINT('Ctrl Pts',(-3.72295704063504,3.75639883677117,31.6659515443926));
#47288=CARTESIAN_POINT('Ctrl Pts',(-5.06615885211213,1.51821468589782,31.745323434446));
#47289=CARTESIAN_POINT('Ctrl Pts',(-5.17525558096714,-1.08980320194903,
31.8246953244994));
#47290=CARTESIAN_POINT('Ctrl Pts',(-4.02367150553249,-3.43234744203962,
31.9040672145529));
#47291=CARTESIAN_POINT('Ctrl Pts',(-1.89192995759591,-4.93877944262154,
31.9834391046062));
#47292=CARTESIAN_POINT('Ctrl Pts',(0.70068154029511,-5.24213570278371,32.0628109946597));
#47293=CARTESIAN_POINT('Ctrl Pts',(3.12260856590247,-4.26851930901834,32.142182884713));
#47294=CARTESIAN_POINT('Ctrl Pts',(4.78387505663285,-2.25510105978337,32.2215547747665));
#47295=CARTESIAN_POINT('Ctrl Pts',(5.27980017249531,0.307654816033343,32.3009266648198));
#47296=CARTESIAN_POINT('Ctrl Pts',(4.48957765297736,2.79546665964672,32.3802985548733));
#47297=CARTESIAN_POINT('Ctrl Pts',(2.60570395470567,4.60230901263064,32.4596704449267));
#47298=CARTESIAN_POINT('Ctrl Pts',(0.0870865406955613,5.28803907717593,
32.5390423349801));
#47299=CARTESIAN_POINT('Ctrl Pts',(-2.45274496186521,4.68561452739711,32.6184142250335));
#47300=CARTESIAN_POINT('Ctrl Pts',(-4.39509322077448,2.94178465017617,32.6977861150869));
#47301=CARTESIAN_POINT('Ctrl Pts',(-5.26680649947691,0.48134254370224,32.7771580051403));
#47302=CARTESIAN_POINT('Ctrl Pts',(-4.85553737278523,-2.09635354098391,
32.8565298951937));
#47303=CARTESIAN_POINT('Ctrl Pts',(-3.26147008963279,-4.16338254328624,
32.9359017852471));
#47304=CARTESIAN_POINT('Ctrl Pts',(-0.8729159117874,-5.21622077353502,33.0152736753005));
#47305=CARTESIAN_POINT('Ctrl Pts',(1.72827865000283,-4.99839916925953,33.0946455653539));
#47306=CARTESIAN_POINT('Ctrl Pts',(3.9084683581323,-3.5629785911213,33.1740174554073));
#47307=CARTESIAN_POINT('Ctrl Pts',(5.13656382546866,-1.25962431470524,33.2533893454607));
#47308=CARTESIAN_POINT('Ctrl Pts',(5.11340371451205,1.35057165664188,33.3327612355141));
#47309=CARTESIAN_POINT('Ctrl Pts',(3.84462977702742,3.63177136187071,33.4121331255675));
#47310=CARTESIAN_POINT('Ctrl Pts',(1.63931253580255,5.02827960213734,33.4915050156209));
#47311=CARTESIAN_POINT('Ctrl Pts',(-0.965337610587002,5.19991006123145,
33.5708769056743));
#47312=CARTESIAN_POINT('Ctrl Pts',(-3.33483365177614,4.1048539392153,33.6502487957277));
#47313=CARTESIAN_POINT('Ctrl Pts',(-4.89197159692173,2.00986448354636,33.7296206857811));
#47314=CARTESIAN_POINT('Ctrl Pts',(-5.25743608925264,-0.574723511554913,
33.8089925758345));
#47315=CARTESIAN_POINT('Ctrl Pts',(-4.34220078737896,-3.01931013137032,
33.888364465888));
#47316=CARTESIAN_POINT('Ctrl Pts',(-2.36921498499824,-4.72839948631349,
33.9677363559413));
#47317=CARTESIAN_POINT('Ctrl Pts',(0.18090634355963,-5.28566119252548,34.0471082459947));
#47318=CARTESIAN_POINT('Ctrl Pts',(2.68695928725581,-4.55534753185087,34.1264801360481));
#47319=CARTESIAN_POINT('Ctrl Pts',(4.53847489605999,-2.71536129550809,34.2058520261016));
#47320=CARTESIAN_POINT('Ctrl Pts',(5.28442806592769,-0.21391905792982,34.2852239161549));
#47321=CARTESIAN_POINT('Ctrl Pts',(4.74310625581857,2.3396333886583,34.3645958062084));
#47322=CARTESIAN_POINT('Ctrl Pts',(3.04637426047967,4.32325632045994,34.4439676962618));
#47323=CARTESIAN_POINT('Ctrl Pts',(0.607552238322964,5.25374358196314,34.5233395863151));
#47324=CARTESIAN_POINT('Ctrl Pts',(-1.97926816429518,4.90443053586424,34.6027114763686));
#47325=CARTESIAN_POINT('Ctrl Pts',(-4.08394322312674,3.36040906700167,34.6820833664219));
#47326=CARTESIAN_POINT('Ctrl Pts',(-5.19377875245966,0.997799387556786,
34.7614552564754));
#47327=CARTESIAN_POINT('Ctrl Pts',(-5.03842127392763,-1.60787201410546,
34.8408271465287));
#47328=CARTESIAN_POINT('Ctrl Pts',(-3.65571552542313,-3.82186935209593,
34.9201990365822));
#47329=CARTESIAN_POINT('Ctrl Pts',(-1.38248556671468,-5.10486777548014,
34.9995709266355));
#47330=CARTESIAN_POINT('Ctrl Pts',(1.22751481596557,-5.14433170819057,35.078942816689));
#47331=CARTESIAN_POINT('Ctrl Pts',(3.53849530653457,-3.93064782357091,35.1583147067423));
#47332=CARTESIAN_POINT('Ctrl Pts',(4.98750617275828,-1.75946682947078,35.2376865967958));
#47333=CARTESIAN_POINT('Ctrl Pts',(5.22157157495577,0.840316389774704,35.3170584868492));
#47334=CARTESIAN_POINT('Ctrl Pts',(4.18367369924664,3.23540039647985,35.3964303769026));
#47335=CARTESIAN_POINT('Ctrl Pts',(2.12664217080567,4.8423480280398,35.4758022669559));
#47336=CARTESIAN_POINT('Ctrl Pts',(-0.448434683200953,5.2697103983248,35.5551741570095));
#47337=CARTESIAN_POINT('Ctrl Pts',(-2.91427384097317,4.41338297988397,35.6345460470627));
#47338=CARTESIAN_POINT('Ctrl Pts',(-4.67020234172003,2.48196523640092,35.7139179371163));
#47339=CARTESIAN_POINT('Ctrl Pts',(-5.28847988934142,-0.0540537449324728,
35.7932898271696));
#47340=CARTESIAN_POINT('Ctrl Pts',(-4.61849544177097,-2.57690535364626,
35.872661717223));
#47341=CARTESIAN_POINT('Ctrl Pts',(-2.82345572745135,-4.47202852209511,
35.9520336072764));
#47342=CARTESIAN_POINT('Ctrl Pts',(-0.340628447537815,-5.27777544122882,
36.0314054973298));
#47343=CARTESIAN_POINT('Ctrl Pts',(2.22517516822766,-4.79786794503694,36.1107773873833));
#47344=CARTESIAN_POINT('Ctrl Pts',(4.2489310383545,-3.14921043733466,36.1901492774366));
#47345=CARTESIAN_POINT('Ctrl Pts',(5.23765671238758,-0.733412237756749,
36.2695211674901));
#47346=CARTESIAN_POINT('Ctrl Pts',(4.95050080463952,1.8610435595583,36.3488930575434));
#47347=CARTESIAN_POINT('Ctrl Pts',(3.45741385862894,4.002153265115,36.4282649475969));
#47348=CARTESIAN_POINT('Ctrl Pts',(1.12210854951209,5.16834729390565,36.5076368376502));
#47349=CARTESIAN_POINT('Ctrl Pts',(-1.4865399185207,5.07554336184357,36.5870087277037));
#47350=CARTESIAN_POINT('Ctrl Pts',(-3.73307055280216,3.74634830136112,36.666380617757));
#47351=CARTESIAN_POINT('Ctrl Pts',(-5.07023346343257,1.50455108706837,36.7457525078105));
#47352=CARTESIAN_POINT('Ctrl Pts',(-5.17229872514219,-1.10375144176689,
36.8251243978638));
#47353=CARTESIAN_POINT('Ctrl Pts',(-4.01440346609619,-3.44318256250012,
36.9044962879173));
#47354=CARTESIAN_POINT('Ctrl Pts',(-1.87860840844056,-4.94386203236358,
36.9838681779707));
#47355=CARTESIAN_POINT('Ctrl Pts',(0.71481149928202,-5.24022765419639,37.0632400680241));
#47356=CARTESIAN_POINT('Ctrl Pts',(3.13410490798792,-4.26008541851396,37.1426119580775));
#47357=CARTESIAN_POINT('Ctrl Pts',(4.78993729833158,-2.24219580442096,37.2219838481309));
#47358=CARTESIAN_POINT('Ctrl Pts',(5.27895156514787,0.321887744613352,37.3013557381843));
#47359=CARTESIAN_POINT('Ctrl Pts',(4.48202491545551,2.80756015154514,37.3807276282377));
#47360=CARTESIAN_POINT('Ctrl Pts',(2.59328691715162,4.6093171199916,37.4600995182911));
#47361=CARTESIAN_POINT('Ctrl Pts',(0.0728299659736646,5.28825464055466,
37.5394714083445));
#47362=CARTESIAN_POINT('Ctrl Pts',(-2.46536820371075,4.67898503603898,37.6188432983979));
#47363=CARTESIAN_POINT('Ctrl Pts',(-4.40300813596802,2.92992503348812,37.6982151884513));
#47364=CARTESIAN_POINT('Ctrl Pts',(-5.26808503220261,0.467141778084607,
37.7775870785047));
#47365=CARTESIAN_POINT('Ctrl Pts',(-4.84986807528987,-2.10943618050861,
37.8569589685581));
#47366=CARTESIAN_POINT('Ctrl Pts',(-3.2502339902585,-4.17216015459505,37.9363308586115));
#47367=CARTESIAN_POINT('Ctrl Pts',(-0.858850099431265,-5.21855515011692,
38.0157027486649));
#47368=CARTESIAN_POINT('Ctrl Pts',(1.74174777450972,-4.99372166181591,38.0950746387183));
#47369=CARTESIAN_POINT('Ctrl Pts',(3.91805974601555,-3.55242863073569,38.1744465287717));
#47370=CARTESIAN_POINT('Ctrl Pts',(5.13994103560184,-1.24577184719802,38.2538184188251));
#47371=CARTESIAN_POINT('Ctrl Pts',(5.10974406648872,1.36435219862427,38.3331903088785));
#47372=CARTESIAN_POINT('Ctrl Pts',(3.83482475204887,3.64212307300276,38.4125621989319));
#47373=CARTESIAN_POINT('Ctrl Pts',(1.62575061805696,5.03268082057242,38.4919340889853));
#47374=CARTESIAN_POINT('Ctrl Pts',(-0.979352771366501,5.19728867487039,
38.5713059790387));
#47375=CARTESIAN_POINT('Ctrl Pts',(-3.3458879870052,4.09584848370752,38.6506778690921));
#47376=CARTESIAN_POINT('Ctrl Pts',(-4.89737230716795,1.99666872129193,38.7300497591456));
#47377=CARTESIAN_POINT('Ctrl Pts',(-5.2558675504918,-0.588895222855594,
38.809421649199));
#47378=CARTESIAN_POINT('Ctrl Pts',(-4.33404513553914,-3.03100540392653,
38.8887935392523));
#47379=CARTESIAN_POINT('Ctrl Pts',(-2.35645883694701,-4.73476973691708,
38.9681654293058));
#47380=CARTESIAN_POINT('Ctrl Pts',(0.195155463808245,-5.28515396379923,
39.0475373193592));
#47381=CARTESIAN_POINT('Ctrl Pts',(2.69923061743519,-4.54808766460433,39.1269092094126));
#47382=CARTESIAN_POINT('Ctrl Pts',(4.5457786161602,-2.70311485851688,39.2062810994659));
#47383=CARTESIAN_POINT('Ctrl Pts',(5.28498604656423,-0.199673823356607,
39.2856529895194));
#47384=CARTESIAN_POINT('Ctrl Pts',(4.73678060915317,2.35241593705468,39.3650248795727));
#47385=CARTESIAN_POINT('Ctrl Pts',(3.03470961035893,4.33144609848054,39.4443967696262));
#47386=CARTESIAN_POINT('Ctrl Pts',(0.593383061700927,5.25537632570972,39.5237686596795));
#47387=CARTESIAN_POINT('Ctrl Pts',(-1.99247705733066,4.8990504464678,39.603140549733));
#47388=CARTESIAN_POINT('Ctrl Pts',(-4.09299916691649,3.34943642687039,39.6825124397864));
#47389=CARTESIAN_POINT('Ctrl Pts',(-5.19642846461573,0.983699440459269,
39.7618843298398));
#47390=CARTESIAN_POINT('Ctrl Pts',(-5.03410925482033,-1.62126816458454,
39.8412562198932));
#47391=CARTESIAN_POINT('Ctrl Pts',(-3.6453165085118,-3.83208153227987,39.9206281099466));
#47392=CARTESIAN_POINT('Ctrl Pts',(-2.12771778283764,-4.68247622999901,
39.9735427033155));
#47393=CARTESIAN_POINT('Ctrl Pts',(-1.31303618635638,-4.90075024188325,
40.));
#47394=CARTESIAN_POINT('Ctrl Pts',(-3.43378788736187,2.93584158412999,-1.38777878078145E-15));
#47395=CARTESIAN_POINT('Ctrl Pts',(-3.5274298169339,2.83894612463338,-1.38777878078145E-15));
#47396=CARTESIAN_POINT('Ctrl Pts',(-3.61644080326455,2.73799316940158,-1.70682494898246E-15));
#47397=CARTESIAN_POINT('Ctrl Pts',(-3.70070760607863,2.63340714286309,-1.68962066560141E-15));
#47398=CARTESIAN_POINT('Ctrl Pts',(-3.78643913867677,2.52700319677679,-1.67211733650556E-15));
#47399=CARTESIAN_POINT('Ctrl Pts',(-3.86726060843671,2.41683829132909,-1.52825423918462E-15));
#47400=CARTESIAN_POINT('Ctrl Pts',(-3.9430233259709,2.30331415642333,-1.42247325030098E-15));
#47401=CARTESIAN_POINT('Ctrl Pts',(-4.01958942326278,2.18858622372678,-1.31557057111923E-15));
#47402=CARTESIAN_POINT('Ctrl Pts',(-4.09098941448581,2.07042685422507,-1.45703061823736E-15));
#47403=CARTESIAN_POINT('Ctrl Pts',(-4.15703260143776,1.94921318851517,-1.40165656858926E-15));
#47404=CARTESIAN_POINT('Ctrl Pts',(-4.22276474819078,1.82857039656885,-1.34654331125317E-15));
#47405=CARTESIAN_POINT('Ctrl Pts',(-4.28319084758819,1.70490133278768,-1.76868280947178E-15));
#47406=CARTESIAN_POINT('Ctrl Pts',(-4.33807945470206,1.57855051046471,-1.88044024795886E-15));
#47407=CARTESIAN_POINT('Ctrl Pts',(-4.35502796120398,1.53953589802935,-1.91494871469599E-15));
#47408=CARTESIAN_POINT('Ctrl Pts',(-4.37144815676901,1.50026543549027,-1.30689270547165E-15));
#47409=CARTESIAN_POINT('Ctrl Pts',(-4.38733228779962,1.46074889051522,-1.32532873564628E-15));
#47410=CARTESIAN_POINT('Ctrl Pts',(-4.39376253093777,1.44475173009898,-1.33279204328941E-15));
#47411=CARTESIAN_POINT('Ctrl Pts',(-4.40010357988131,1.42871748389362,-1.28259685789569E-15));
#47412=CARTESIAN_POINT('Ctrl Pts',(-4.4063520165592,1.41265478977856,-1.29063426612674E-15));
#47413=CARTESIAN_POINT('Ctrl Pts',(-4.45729152748394,1.28170591015729,-1.35615811881152E-15));
#47414=CARTESIAN_POINT('Ctrl Pts',(-4.50214144181921,1.14871482526442,-2.13815754900839E-15));
#47415=CARTESIAN_POINT('Ctrl Pts',(-4.54074327371246,1.0140904790896,-2.05391259555654E-15));
#47416=CARTESIAN_POINT('Ctrl Pts',(-4.54547345988333,0.997593898764086,
-2.0435893985931E-15));
#47417=CARTESIAN_POINT('Ctrl Pts',(-4.55010977859188,0.981072752949281,
-1.00791691148873E-15));
#47418=CARTESIAN_POINT('Ctrl Pts',(-4.55465189605181,0.964527761093366,
-1.01307850997046E-15));
#47419=CARTESIAN_POINT('Ctrl Pts',(-4.59134817932549,0.830858891175244,
-1.05169067743968E-15));
#47420=CARTESIAN_POINT('Ctrl Pts',(-4.62189967399316,0.695635489793831,
-1.41485248297211E-15));
#47421=CARTESIAN_POINT('Ctrl Pts',(-4.64637428491341,0.559286455771474,
-1.36002320516582E-15));
#47422=CARTESIAN_POINT('Ctrl Pts',(-4.67110897469857,0.42148851201501,-1.30461128535625E-15));
#47423=CARTESIAN_POINT('Ctrl Pts',(-4.68963709540601,0.282540149701787,
-1.43104411647104E-15));
#47424=CARTESIAN_POINT('Ctrl Pts',(-4.70197867697062,0.142866308633218,
-1.36002320516582E-15));
#47425=CARTESIAN_POINT('Ctrl Pts',(-4.71314718957453,0.0164684846393732,
-1.29575284087739E-15));
#47426=CARTESIAN_POINT('Ctrl Pts',(-4.71924875509872,-0.110524098082,-1.66579323769632E-15));
#47427=CARTESIAN_POINT('Ctrl Pts',(-4.72026194547141,-0.237801095913712,
-1.67921232474555E-15));
#47428=CARTESIAN_POINT('Ctrl Pts',(-4.72045200129662,-0.261675913030809,
-1.68172949795545E-15));
#47429=CARTESIAN_POINT('Ctrl Pts',(-4.72046291446759,-0.285560737563283,
-9.9370225703457E-16));
#47430=CARTESIAN_POINT('Ctrl Pts',(-4.72029440609211,-0.309453515786201,
-9.71445146547012E-16));
#47431=CARTESIAN_POINT('Ctrl Pts',(-4.72016631155934,-0.327616021086772,
-9.54526022139039E-16));
#47432=CARTESIAN_POINT('Ctrl Pts',(-4.7199344986873,-0.345781850732525,
-1.1165476318937E-15));
#47433=CARTESIAN_POINT('Ctrl Pts',(-4.7195992402228,-0.363937763232007,
-1.12410081243297E-15));
#47434=CARTESIAN_POINT('Ctrl Pts',(-4.7169715342115,-0.506241106673104,
-1.18330151878048E-15));
#47435=CARTESIAN_POINT('Ctrl Pts',(-4.70799214533038,-0.648137600560786,
-1.67849620506959E-15));
#47436=CARTESIAN_POINT('Ctrl Pts',(-4.69273559502703,-0.789185289486343,
-1.60982338570648E-15));
#47437=CARTESIAN_POINT('Ctrl Pts',(-4.67736001919945,-0.931333376259461,
-1.5406148083796E-15));
#47438=CARTESIAN_POINT('Ctrl Pts',(-4.65560906635571,-1.07262015451611,
-1.29947818212301E-15));
#47439=CARTESIAN_POINT('Ctrl Pts',(-4.62750766548139,-1.21260443247969,
-1.38777878078145E-15));
#47440=CARTESIAN_POINT('Ctrl Pts',(-4.61688292082861,-1.26553052023664,
-1.42116399590398E-15));
#47441=CARTESIAN_POINT('Ctrl Pts',(-4.60534985624838,-1.31827046839259,
-1.10373700911438E-15));
#47442=CARTESIAN_POINT('Ctrl Pts',(-4.59290787692679,-1.37080047994465,
-1.0547118733939E-15));
#47443=CARTESIAN_POINT('Ctrl Pts',(-4.56011975477607,-1.50923186540429,
-9.25516823562078E-16));
#47444=CARTESIAN_POINT('Ctrl Pts',(-4.52102317103095,-1.64620611480812,
-1.41788356490645E-15));
#47445=CARTESIAN_POINT('Ctrl Pts',(-4.47583839059365,-1.78136570298785,
-1.36002320516582E-15));
#47446=CARTESIAN_POINT('Ctrl Pts',(-4.44941052359499,-1.86041841908909,
-1.32618159130998E-15));
#47447=CARTESIAN_POINT('Ctrl Pts',(-4.42089896739826,-1.93885019183042,
-1.30868430769761E-15));
#47448=CARTESIAN_POINT('Ctrl Pts',(-4.3903399301827,-2.01658705378289,-1.30451205393456E-15));
#47449=CARTESIAN_POINT('Ctrl Pts',(-4.37718466105246,-2.05005176450371,
-1.30271595280921E-15));
#47450=CARTESIAN_POINT('Ctrl Pts',(-4.36364988420426,-2.08338766611273,
-1.16152748166208E-15));
#47451=CARTESIAN_POINT('Ctrl Pts',(-4.3497381750326,-2.11658871139626,-1.13797860024079E-15));
#47452=CARTESIAN_POINT('Ctrl Pts',(-4.34244585283277,-2.13399223217085,
-1.12563460794976E-15));
#47453=CARTESIAN_POINT('Ctrl Pts',(-4.33504992528714,-2.15135862906508,
-1.92978013206096E-15));
#47454=CARTESIAN_POINT('Ctrl Pts',(-4.32755662758879,-2.16867384922929,
-1.9151347174784E-15));
#47455=CARTESIAN_POINT('Ctrl Pts',(-4.2701680431329,-2.30128515265925,-1.80297053483165E-15));
#47456=CARTESIAN_POINT('Ctrl Pts',(-4.20699158680529,-2.43109046195038,
-1.71043044263751E-15));
#47457=CARTESIAN_POINT('Ctrl Pts',(-4.13831811099888,-2.55774085897211,
-1.72084568816899E-15));
#47458=CARTESIAN_POINT('Ctrl Pts',(-4.0690864175418,-2.68542074352523,-1.73134559482798E-15));
#47459=CARTESIAN_POINT('Ctrl Pts',(-3.99426770892291,-2.80989493979695,
-1.80815084065395E-15));
#47460=CARTESIAN_POINT('Ctrl Pts',(-3.91410750939009,-2.93079631633735,
-1.80411241501588E-15));
#47461=CARTESIAN_POINT('Ctrl Pts',(-3.83416065570548,-3.05137591465264,
-1.8000847376213E-15));
#47462=CARTESIAN_POINT('Ctrl Pts',(-3.74890035710146,-3.16840239753955,
-1.26386791065628E-15));
#47463=CARTESIAN_POINT('Ctrl Pts',(-3.6585229556131,-3.28149127673775,-1.27675647831893E-15));
#47464=CARTESIAN_POINT('Ctrl Pts',(-3.59945026249498,-3.35540870018578,
-1.2851807347119E-15));
#47465=CARTESIAN_POINT('Ctrl Pts',(-3.5381904788592,-3.42764345712454,-1.45186396209174E-15));
#47466=CARTESIAN_POINT('Ctrl Pts',(-3.47478854700661,-3.49808125449704,
-1.41553435639707E-15));
#47467=CARTESIAN_POINT('Ctrl Pts',(-3.4391425896078,-3.5376829298883,-1.39540507371065E-15));
#47468=CARTESIAN_POINT('Ctrl Pts',(-3.40281937333393,-3.57671648450509,
-1.55816047969468E-15));
#47469=CARTESIAN_POINT('Ctrl Pts',(-3.36583573983685,-3.61517046963578,
-1.55431223447522E-15));
#47470=CARTESIAN_POINT('Ctrl Pts',(-3.34056943595204,-3.64144128139824,
-1.55168320849956E-15));
#47471=CARTESIAN_POINT('Ctrl Pts',(-3.31499488246685,-3.66744157776442,
-1.71311115652187E-15));
#47472=CARTESIAN_POINT('Ctrl Pts',(-3.28911728144163,-3.6931675174981,-1.69309011255336E-15));
#47473=CARTESIAN_POINT('Ctrl Pts',(-3.27259035745335,-3.70959758186502,
-1.68030352265613E-15));
#47474=CARTESIAN_POINT('Ctrl Pts',(-3.25594506354961,-3.7259104717157,-1.35072386705874E-15));
#47475=CARTESIAN_POINT('Ctrl Pts',(-3.23918904311522,-3.74209965697934,
-1.36002320516582E-15));
#47476=CARTESIAN_POINT('Ctrl Pts',(-3.13422859724164,-3.84350942251737,
-1.41827466635674E-15));
#47477=CARTESIAN_POINT('Ctrl Pts',(-3.02485537861799,-3.94013896638234,
-1.29586046630586E-15));
#47478=CARTESIAN_POINT('Ctrl Pts',(-2.91147703861897,-4.03180594754837,
-1.33226762955019E-15));
#47479=CARTESIAN_POINT('Ctrl Pts',(-2.80007805253152,-4.12187261071949,
-1.36803919819172E-15));
#47480=CARTESIAN_POINT('Ctrl Pts',(-2.68481190070853,-4.20714879945784,
-1.75330405072015E-15));
#47481=CARTESIAN_POINT('Ctrl Pts',(-2.5660285220091,-4.28743071443088,-1.77635683940025E-15));
#47482=CARTESIAN_POINT('Ctrl Pts',(-2.51557747120272,-4.32152897813987,
-1.78614808650622E-15));
#47483=CARTESIAN_POINT('Ctrl Pts',(-2.46449152304015,-4.35472587736193,
-1.31186991621621E-15));
#47484=CARTESIAN_POINT('Ctrl Pts',(-2.41279587231268,-4.38700384624999,
-1.27675647831893E-15));
#47485=CARTESIAN_POINT('Ctrl Pts',(-2.38543234505614,-4.40408921163422,
-1.2581702432788E-15));
#47486=CARTESIAN_POINT('Ctrl Pts',(-2.35789457340209,-4.42091901104391,
-1.50863034215941E-15));
#47487=CARTESIAN_POINT('Ctrl Pts',(-2.3302097471481,-4.43747675896359,-1.49880108324396E-15));
#47488=CARTESIAN_POINT('Ctrl Pts',(-2.2023530709709,-4.51394531233533,-1.45340667250483E-15));
#47489=CARTESIAN_POINT('Ctrl Pts',(-2.07127177001784,-4.58467311410489,
-7.9672741319199E-16));
#47490=CARTESIAN_POINT('Ctrl Pts',(-1.93736496285559,-4.64944928440847,
-4.9960036108132E-16));
#47491=CARTESIAN_POINT('Ctrl Pts',(-1.80364190208402,-4.71413656910759,
-2.02881025535331E-16));
#47492=CARTESIAN_POINT('Ctrl Pts',(-1.66710043882179,-4.77288900981815,
-3.16087603122754E-17));
#47493=CARTESIAN_POINT('Ctrl Pts',(-1.52810715957136,-4.82545526764581,
-5.55111512312578E-17));
#47494=CARTESIAN_POINT('Ctrl Pts',(-1.49120032503771,-4.83941316683462,
-6.1857944337824E-17));
#47495=CARTESIAN_POINT('Ctrl Pts',(-1.4541204835251,-4.85293465562285,3.75650465851052E-17));
#47496=CARTESIAN_POINT('Ctrl Pts',(-1.41687422066829,-4.86601447289862,
5.55111512312578E-17));
#47497=CARTESIAN_POINT('Ctrl Pts',(-1.38244754401982,-4.87810413251642,
1.27205291019773E-16));
#47498=CARTESIAN_POINT('Ctrl Pts',(-1.3478786871628,-4.88981645711078,2.24269765851654E-16));
#47499=CARTESIAN_POINT('Ctrl Pts',(-1.31317395760259,-4.90115117757553,
2.22044604925031E-16));
#47500=CARTESIAN_POINT('Ctrl Pts',(4.51755838390264,-0.00010457874560596,
1.61258330249198));
#47501=CARTESIAN_POINT('Ctrl Pts',(4.51776153214983,-0.238054206488734,
1.60420146868401));
#47502=CARTESIAN_POINT('Ctrl Pts',(4.49928771368086,-0.475972597056525,
1.59581963487604));
#47503=CARTESIAN_POINT('Ctrl Pts',(4.46186317968569,-0.710871726876144,
1.58743780106807));
#47504=CARTESIAN_POINT('Ctrl Pts',(4.34373246725773,-1.45233190264972,1.5609805043836));
#47505=CARTESIAN_POINT('Ctrl Pts',(4.03678590132105,-2.16370961033161,1.53452320769914));
#47506=CARTESIAN_POINT('Ctrl Pts',(3.57840923518442,-2.75835983566981,1.50806591101467));
#47507=CARTESIAN_POINT('Ctrl Pts',(3.1200325690478,-3.353010061008,1.4816086143302));
#47508=CARTESIAN_POINT('Ctrl Pts',(2.51022580271121,-3.8309328040025,1.45515131764573));
#47509=CARTESIAN_POINT('Ctrl Pts',(1.82326272299592,-4.13391759737134,1.42869402096126));
#47510=CARTESIAN_POINT('Ctrl Pts',(1.13629964328063,-4.43690239074017,1.4022367242768));
#47511=CARTESIAN_POINT('Ctrl Pts',(0.372180250186614,-4.56494923448333,
1.37577942759233));
#47512=CARTESIAN_POINT('Ctrl Pts',(-0.37602655530059,-4.50246217629702,
1.34932213090786));
#47513=CARTESIAN_POINT('Ctrl Pts',(-1.1242333607878,-4.4399751181107,1.32286483422339));
#47514=CARTESIAN_POINT('Ctrl Pts',(-1.85652757866819,-4.18695415799491,
1.29640753753892));
#47515=CARTESIAN_POINT('Ctrl Pts',(-2.48371659230757,-3.77421694705552,
1.26995024085446));
#47516=CARTESIAN_POINT('Ctrl Pts',(-3.11090560594693,-3.36147973611613,
1.24349294416999));
#47517=CARTESIAN_POINT('Ctrl Pts',(-3.63298941534527,-2.78902627435314,
1.21703564748552));
#47518=CARTESIAN_POINT('Ctrl Pts',(-3.98637877398998,-2.12658080103894,
1.19057835080105));
#47519=CARTESIAN_POINT('Ctrl Pts',(-4.3397681326347,-1.46413532772474,1.16412105411659));
#47520=CARTESIAN_POINT('Ctrl Pts',(-4.52446304052578,-0.711697842859317,
1.13766375743212));
#47521=CARTESIAN_POINT('Ctrl Pts',(-4.51796789313228,0.039085678406338,
1.11120646074765));
#47522=CARTESIAN_POINT('Ctrl Pts',(-4.51147274573878,0.789869199671988,
1.08474916406318));
#47523=CARTESIAN_POINT('Ctrl Pts',(-4.3137875430607,1.53899875733787,1.05829186737871));
#47524=CARTESIAN_POINT('Ctrl Pts',(-3.94899006576281,2.19523105353949,1.03183457069425));
#47525=CARTESIAN_POINT('Ctrl Pts',(-3.58419258846491,2.85146334974111,1.00537727400978));
#47526=CARTESIAN_POINT('Ctrl Pts',(-3.0522828365472,3.41479838447846,0.97891997732531));
#47527=CARTESIAN_POINT('Ctrl Pts',(-2.4180469390755,3.81662285121812,0.952462680640842));
#47528=CARTESIAN_POINT('Ctrl Pts',(-1.78381104160379,4.21844731795778,0.926005383956374));
#47529=CARTESIAN_POINT('Ctrl Pts',(-1.0472489985781,4.45876121669975,0.899548087271906));
#47530=CARTESIAN_POINT('Ctrl Pts',(-0.298073044029486,4.50829405706007,
0.873090790587439));
#47531=CARTESIAN_POINT('Ctrl Pts',(0.451102910519128,4.55782689742038,0.846633493902971));
#47532=CARTESIAN_POINT('Ctrl Pts',(1.21289277659066,4.41657867939905,0.820176197218503));
#47533=CARTESIAN_POINT('Ctrl Pts',(1.89451099954032,4.10175426806438,0.793718900534035));
#47534=CARTESIAN_POINT('Ctrl Pts',(2.57612922248998,3.7869298567297,0.767261603849567));
#47535=CARTESIAN_POINT('Ctrl Pts',(3.17757580231775,3.29852925208169,0.740804307165098));
#47536=CARTESIAN_POINT('Ctrl Pts',(3.6255959515189,2.69603724086577,0.71434701048063));
#47537=CARTESIAN_POINT('Ctrl Pts',(4.07361610072004,2.09354522964985,0.687889713796163));
#47538=CARTESIAN_POINT('Ctrl Pts',(4.36820981929455,1.37696181186601,0.661432417111696));
#47539=CARTESIAN_POINT('Ctrl Pts',(4.47349452055126,0.633569578843809,0.634975120427228));
#47540=CARTESIAN_POINT('Ctrl Pts',(4.50319667153093,0.423849191372714,0.627511181115478));
#47541=CARTESIAN_POINT('Ctrl Pts',(4.51783217716753,0.211995155346536,0.620047241803728));
#47542=CARTESIAN_POINT('Ctrl Pts',(4.51763087883895,0.00011359767064345,
0.612583302491977));
#47543=CARTESIAN_POINT('Ctrl Pts',(1.3130361863565,-4.90075024188322,0.));
#47544=CARTESIAN_POINT('Ctrl Pts',(2.12771778283771,-4.68247622999897,0.0264572966844678));
#47545=CARTESIAN_POINT('Ctrl Pts',(3.64531650851188,-3.8320815322798,0.0793718900534037));
#47546=CARTESIAN_POINT('Ctrl Pts',(5.03410925482037,-1.62126816458446,0.158743780106807));
#47547=CARTESIAN_POINT('Ctrl Pts',(5.19642846461569,0.98369944045933,0.238115670160212));
#47548=CARTESIAN_POINT('Ctrl Pts',(4.09299916691648,3.34943642687043,0.317487560213614));
#47549=CARTESIAN_POINT('Ctrl Pts',(1.99247705733062,4.89905044646781,0.396859450267019));
#47550=CARTESIAN_POINT('Ctrl Pts',(-0.593383061700938,5.2553763257097,0.476231340320422));
#47551=CARTESIAN_POINT('Ctrl Pts',(-3.03470961035893,4.33144609848054,0.555603230373826));
#47552=CARTESIAN_POINT('Ctrl Pts',(-4.73678060915323,2.35241593705463,0.634975120427228));
#47553=CARTESIAN_POINT('Ctrl Pts',(-5.28498604656423,-0.199673823356779,
0.714347010480634));
#47554=CARTESIAN_POINT('Ctrl Pts',(-4.5457786161601,-2.703114858517,0.793718900534037));
#47555=CARTESIAN_POINT('Ctrl Pts',(-2.69923061743508,-4.5480876646044,0.87309079058744));
#47556=CARTESIAN_POINT('Ctrl Pts',(-0.195155463808127,-5.28515396379925,
0.952462680640845));
#47557=CARTESIAN_POINT('Ctrl Pts',(2.35645883694709,-4.73476973691702,1.03183457069425));
#47558=CARTESIAN_POINT('Ctrl Pts',(4.33404513553918,-3.03100540392648,1.11120646074765));
#47559=CARTESIAN_POINT('Ctrl Pts',(5.25586755049182,-0.58889522285553,1.19057835080105));
#47560=CARTESIAN_POINT('Ctrl Pts',(4.89737230716791,1.99666872129196,1.26995024085446));
#47561=CARTESIAN_POINT('Ctrl Pts',(3.34588798700519,4.09584848370755,1.34932213090786));
#47562=CARTESIAN_POINT('Ctrl Pts',(0.979352771366438,5.19728867487042,1.42869402096127));
#47563=CARTESIAN_POINT('Ctrl Pts',(-1.6257506180571,5.03268082057239,1.50806591101467));
#47564=CARTESIAN_POINT('Ctrl Pts',(-3.83482475204895,3.64212307300266,1.58743780106807));
#47565=CARTESIAN_POINT('Ctrl Pts',(-5.10974406648874,1.36435219862418,1.66680969112148));
#47566=CARTESIAN_POINT('Ctrl Pts',(-5.13994103560183,-1.2457718471981,1.74618158117488));
#47567=CARTESIAN_POINT('Ctrl Pts',(-3.91805974601548,-3.55242863073578,
1.82555347122828));
#47568=CARTESIAN_POINT('Ctrl Pts',(-1.74174777450957,-4.99372166181597,
1.90492536128169));
#47569=CARTESIAN_POINT('Ctrl Pts',(0.858850099431454,-5.21855515011689,
1.98429725133509));
#47570=CARTESIAN_POINT('Ctrl Pts',(3.25023399025869,-4.17216015459491,2.0636691413885));
#47571=CARTESIAN_POINT('Ctrl Pts',(4.84986807528995,-2.10943618050841,2.1430410314419));
#47572=CARTESIAN_POINT('Ctrl Pts',(5.26808503220259,0.467141778084788,2.22241292149531));
#47573=CARTESIAN_POINT('Ctrl Pts',(4.40300813596794,2.92992503348825,2.3017848115487));
#47574=CARTESIAN_POINT('Ctrl Pts',(2.46536820371062,4.67898503603904,2.38115670160211));
#47575=CARTESIAN_POINT('Ctrl Pts',(-0.0728299659737919,5.28825464055465,
2.46052859165552));
#47576=CARTESIAN_POINT('Ctrl Pts',(-2.59328691715172,4.60931711999155,2.53990048170891));
#47577=CARTESIAN_POINT('Ctrl Pts',(-4.4820249154556,2.80756015154502,2.61927237176233));
#47578=CARTESIAN_POINT('Ctrl Pts',(-5.27895156514789,0.321887744613165,
2.69864426181572));
#47579=CARTESIAN_POINT('Ctrl Pts',(-4.7899372983315,-2.2421958044211,2.77801615186913));
#47580=CARTESIAN_POINT('Ctrl Pts',(-3.13410490798781,-4.26008541851404,
2.85738804192253));
#47581=CARTESIAN_POINT('Ctrl Pts',(-0.714811499281904,-5.2402276541964,
2.93675993197593));
#47582=CARTESIAN_POINT('Ctrl Pts',(1.8786084084407,-4.94386203236353,3.01613182202934));
#47583=CARTESIAN_POINT('Ctrl Pts',(4.01440346609632,-3.44318256249998,3.09550371208274));
#47584=CARTESIAN_POINT('Ctrl Pts',(5.17229872514222,-1.10375144176671,3.17487560213615));
#47585=CARTESIAN_POINT('Ctrl Pts',(5.07023346343252,1.50455108706853,3.25424749218955));
#47586=CARTESIAN_POINT('Ctrl Pts',(3.73307055280206,3.74634830136122,3.33361938224296));
#47587=CARTESIAN_POINT('Ctrl Pts',(1.48653991852054,5.07554336184363,3.41299127229636));
#47588=CARTESIAN_POINT('Ctrl Pts',(-1.12210854951228,5.16834729390561,3.49236316234976));
#47589=CARTESIAN_POINT('Ctrl Pts',(-3.45741385862906,4.00215326511488,3.57173505240317));
#47590=CARTESIAN_POINT('Ctrl Pts',(-4.95050080463958,1.86104355955814,3.65110694245657));
#47591=CARTESIAN_POINT('Ctrl Pts',(-5.23765671238755,-0.733412237756895,
3.73047883250997));
#47592=CARTESIAN_POINT('Ctrl Pts',(-4.24893103835441,-3.14921043733482,
3.80985072256337));
#47593=CARTESIAN_POINT('Ctrl Pts',(-2.22517516822744,-4.79786794503704,
3.88922261261678));
#47594=CARTESIAN_POINT('Ctrl Pts',(0.340628447538026,-5.2777754412288,3.96859450267018));
#47595=CARTESIAN_POINT('Ctrl Pts',(2.82345572745151,-4.472028522095,4.04796639272359));
#47596=CARTESIAN_POINT('Ctrl Pts',(4.61849544177105,-2.57690535364612,4.12733828277699));
#47597=CARTESIAN_POINT('Ctrl Pts',(5.28847988934143,-0.0540537449322821,
4.2067101728304));
#47598=CARTESIAN_POINT('Ctrl Pts',(4.67020234171992,2.48196523640112,4.2860820628838));
#47599=CARTESIAN_POINT('Ctrl Pts',(2.91427384097298,4.41338297988409,4.36545395293721));
#47600=CARTESIAN_POINT('Ctrl Pts',(0.44843468320075,5.26971039832481,4.44482584299061));
#47601=CARTESIAN_POINT('Ctrl Pts',(-2.12664217080585,4.84234802803972,4.52419773304401));
#47602=CARTESIAN_POINT('Ctrl Pts',(-4.18367369924674,3.23540039647972,4.60356962309741));
#47603=CARTESIAN_POINT('Ctrl Pts',(-5.22157157495578,0.840316389774564,
4.68294151315082));
#47604=CARTESIAN_POINT('Ctrl Pts',(-4.98750617275825,-1.75946682947089,
4.76231340320422));
#47605=CARTESIAN_POINT('Ctrl Pts',(-3.53849530653447,-3.93064782357102,
4.84168529325762));
#47606=CARTESIAN_POINT('Ctrl Pts',(-1.22751481596538,-5.14433170819062,
4.92105718331103));
#47607=CARTESIAN_POINT('Ctrl Pts',(1.3824855667149,-5.10486777548008,5.00042907336443));
#47608=CARTESIAN_POINT('Ctrl Pts',(3.65571552542333,-3.82186935209575,5.07980096341784));
#47609=CARTESIAN_POINT('Ctrl Pts',(5.03842127392769,-1.60787201410522,5.15917285347124));
#47610=CARTESIAN_POINT('Ctrl Pts',(5.1937787524596,0.997799387556994,5.23854474352464));
#47611=CARTESIAN_POINT('Ctrl Pts',(4.08394322312664,3.36040906700182,5.31791663357805));
#47612=CARTESIAN_POINT('Ctrl Pts',(1.979268164295,4.90443053586431,5.39728852363145));
#47613=CARTESIAN_POINT('Ctrl Pts',(-0.607552238323124,5.25374358196311,
5.47666041368485));
#47614=CARTESIAN_POINT('Ctrl Pts',(-3.04637426047979,4.32325632045987,5.55603230373826));
#47615=CARTESIAN_POINT('Ctrl Pts',(-4.74310625581864,2.33963338865815,5.63540419379165));
#47616=CARTESIAN_POINT('Ctrl Pts',(-5.28442806592769,-0.213919057930008,
5.71477608384507));
#47617=CARTESIAN_POINT('Ctrl Pts',(-4.53847489605989,-2.71536129550824,
5.79414797389846));
#47618=CARTESIAN_POINT('Ctrl Pts',(-2.68695928725567,-4.55534753185094,
5.87351986395187));
#47619=CARTESIAN_POINT('Ctrl Pts',(-0.180906343559476,-5.28566119252549,
5.95289175400528));
#47620=CARTESIAN_POINT('Ctrl Pts',(2.36921498499841,-4.72839948631341,6.03226364405867));
#47621=CARTESIAN_POINT('Ctrl Pts',(4.3422007873791,-3.01931013137013,6.1116355341121));
#47622=CARTESIAN_POINT('Ctrl Pts',(5.25743608925265,-0.574723511554695,
6.19100742416548));
#47623=CARTESIAN_POINT('Ctrl Pts',(4.89197159692165,2.00986448354653,6.2703793142189));
#47624=CARTESIAN_POINT('Ctrl Pts',(3.33483365177601,4.10485393921541,6.34975120427228));
#47625=CARTESIAN_POINT('Ctrl Pts',(0.96533761058682,5.19991006123149,6.42912309432572));
#47626=CARTESIAN_POINT('Ctrl Pts',(-1.63931253580277,5.02827960213728,6.50849498437909));
#47627=CARTESIAN_POINT('Ctrl Pts',(-3.84462977702757,3.63177136187054,6.58786687443252));
#47628=CARTESIAN_POINT('Ctrl Pts',(-5.11340371451209,1.35057165664169,6.6672387644859));
#47629=CARTESIAN_POINT('Ctrl Pts',(-5.13656382546863,-1.25962431470543,
6.74661065453933));
#47630=CARTESIAN_POINT('Ctrl Pts',(-3.90846835813217,-3.56297859112141,
6.82598254459271));
#47631=CARTESIAN_POINT('Ctrl Pts',(-1.72827865000271,-4.99839916925957,
6.90535443464612));
#47632=CARTESIAN_POINT('Ctrl Pts',(0.872915911787522,-5.21622077353501,
6.98472632469953));
#47633=CARTESIAN_POINT('Ctrl Pts',(3.26147008963291,-4.16338254328616,7.06409821475292));
#47634=CARTESIAN_POINT('Ctrl Pts',(4.85553737278532,-2.09635354098373,7.14347010480633));
#47635=CARTESIAN_POINT('Ctrl Pts',(5.26680649947689,0.481342543702463,7.22284199485974));
#47636=CARTESIAN_POINT('Ctrl Pts',(4.39509322077433,2.9417846501764,7.30221388491313));
#47637=CARTESIAN_POINT('Ctrl Pts',(2.45274496186498,4.68561452739722,7.38158577496654));
#47638=CARTESIAN_POINT('Ctrl Pts',(-0.0870865406957981,5.28803907717593,
7.46095766501995));
#47639=CARTESIAN_POINT('Ctrl Pts',(-2.60570395470586,4.60230901263053,7.54032955507335));
#47640=CARTESIAN_POINT('Ctrl Pts',(-4.48957765297745,2.79546665964655,7.61970144512676));
#47641=CARTESIAN_POINT('Ctrl Pts',(-5.27980017249532,0.307654816033177,
7.69907333518014));
#47642=CARTESIAN_POINT('Ctrl Pts',(-4.78387505663278,-2.25510105978351,
7.77844522523357));
#47643=CARTESIAN_POINT('Ctrl Pts',(-3.12260856590233,-4.26851930901846,
7.85781711528695));
#47644=CARTESIAN_POINT('Ctrl Pts',(-0.70068154029489,-5.24213570278374,
7.93718900534038));
#47645=CARTESIAN_POINT('Ctrl Pts',(1.8919299575961,-4.93877944262147,8.01656089539376));
#47646=CARTESIAN_POINT('Ctrl Pts',(4.02367150553262,-3.43234744203947,8.09593278544719));
#47647=CARTESIAN_POINT('Ctrl Pts',(5.1752555809672,-1.08980320194883,8.17530467550057));
#47648=CARTESIAN_POINT('Ctrl Pts',(5.06615885211206,1.51821468589804,8.25467656555398));
#47649=CARTESIAN_POINT('Ctrl Pts',(3.72295704063487,3.75639883677136,8.33404845560738));
#47650=CARTESIAN_POINT('Ctrl Pts',(1.47285113468463,5.07953254565499,8.41342034566079));
#47651=CARTESIAN_POINT('Ctrl Pts',(-1.1360380475741,5.16530336977162,8.49279223571419));
#47652=CARTESIAN_POINT('Ctrl Pts',(-3.46819087602133,3.99281772621695,8.57216412576759));
#47653=CARTESIAN_POINT('Ctrl Pts',(-4.95550008378004,1.84769052250801,8.651536015821));
#47654=CARTESIAN_POINT('Ctrl Pts',(-5.23566043994335,-0.74753000269027,
8.7309079058744));
#47655=CARTESIAN_POINT('Ctrl Pts',(-4.24042550187429,-3.16065387386283,
8.81027979592781));
#47656=CARTESIAN_POINT('Ctrl Pts',(-2.21223229757129,-4.8038494573511,8.88965168598121));
#47657=CARTESIAN_POINT('Ctrl Pts',(0.354855797726969,-5.27683794616905,
8.96902357603462));
#47658=CARTESIAN_POINT('Ctrl Pts',(2.83550180615889,-4.46440039138287,9.04839546608801));
#47659=CARTESIAN_POINT('Ctrl Pts',(4.6254258508873,-2.56444478303851,9.12776735614143));
#47660=CARTESIAN_POINT('Ctrl Pts',(5.28860639654605,-0.0397961018481786,
9.20713924619482));
#47661=CARTESIAN_POINT('Ctrl Pts',(4.66349413013784,2.49454682166519,9.28651113624823));
#47662=CARTESIAN_POINT('Ctrl Pts',(2.90236501609723,4.42122366100663,9.36588302630163));
#47663=CARTESIAN_POINT('Ctrl Pts',(0.434226208411351,5.27090020273944,9.44525491635504));
#47664=CARTESIAN_POINT('Ctrl Pts',(-2.13968914250016,4.83659712202464,9.52462680640844));
#47665=CARTESIAN_POINT('Ctrl Pts',(-4.1923809544202,3.22410968801074,9.60399869646184));
#47666=CARTESIAN_POINT('Ctrl Pts',(-5.22381804552131,0.826236270443201,
9.68337058651526));
#47667=CARTESIAN_POINT('Ctrl Pts',(-4.98274462345855,-1.77290647376134,
9.76274247656865));
#47668=CARTESIAN_POINT('Ctrl Pts',(-3.52788564023945,-3.94017312521954,
9.84211436662205));
#47669=CARTESIAN_POINT('Ctrl Pts',(-1.21364152390043,-5.14762232479954,
9.92148625667546));
#47670=CARTESIAN_POINT('Ctrl Pts',(1.39624298131078,-5.10112212012714,10.0008581467289));
#47671=CARTESIAN_POINT('Ctrl Pts',(3.66600578680612,-3.81199985813406,10.0802300367823));
#47672=CARTESIAN_POINT('Ctrl Pts',(5.04273769720163,-1.5942828684181,10.1596019268357));
#47673=CARTESIAN_POINT('Ctrl Pts',(5.19106986646944,1.01179789915923,10.2389738168891));
#47674=CARTESIAN_POINT('Ctrl Pts',(4.07486890650351,3.37140693807807,10.3183457069425));
#47675=CARTESIAN_POINT('Ctrl Pts',(1.96603890048266,4.90974870936374,10.3977175969959));
#47676=CARTESIAN_POINT('Ctrl Pts',(-0.621713829942471,5.25208656259283,
10.4770894870493));
#47677=CARTESIAN_POINT('Ctrl Pts',(-3.05801844753381,4.31502775447074,10.5564613771027));
#47678=CARTESIAN_POINT('Ctrl Pts',(-4.74939654011498,2.32683773651149,10.6358332671561));
#47679=CARTESIAN_POINT('Ctrl Pts',(-5.28383214813503,-0.228164803694007,
10.7152051572095));
#47680=CARTESIAN_POINT('Ctrl Pts',(-4.53113794043347,-2.72758690275384,
10.7945770472629));
#47681=CARTESIAN_POINT('Ctrl Pts',(-2.67466855994604,-4.56257486971405,
10.8739489373163));
#47682=CARTESIAN_POINT('Ctrl Pts',(-0.166655838534166,-5.2861296975001,
10.9533208273697));
#47683=CARTESIAN_POINT('Ctrl Pts',(2.38195387625819,-4.72199503162473,11.0326927174231));
#47684=CARTESIAN_POINT('Ctrl Pts',(4.3503248991595,-3.00759282800428,11.1120646074765));
#47685=CARTESIAN_POINT('Ctrl Pts',(5.2589664059064,-0.560547668675828,11.1914364975299));
#47686=CARTESIAN_POINT('Ctrl Pts',(4.8865353366992,2.02304566199086,11.2708083875833));
#47687=CARTESIAN_POINT('Ctrl Pts',(3.32375507563458,4.11382954733217,11.3501802776367));
#47688=CARTESIAN_POINT('Ctrl Pts',(0.951315435152466,5.20249366075065,11.4295521676901));
#47689=CARTESIAN_POINT('Ctrl Pts',(-1.6528625396318,5.02384183393465,11.5089240577436));
#47690=CARTESIAN_POINT('Ctrl Pts',(-3.85440685831092,3.62139325645746,11.5882959477969));
#47691=CARTESIAN_POINT('Ctrl Pts',(-5.11702619789041,1.33678129752526,11.6676678378503));
#47692=CARTESIAN_POINT('Ctrl Pts',(-5.13314928200913,-1.27346762656892,
11.7470397279037));
#47693=CARTESIAN_POINT('Ctrl Pts',(-3.89884856306365,-3.57350265560368,
11.8264116179572));
#47694=CARTESIAN_POINT('Ctrl Pts',(-1.71479696411077,-5.00304034754732,
11.9057835080105));
#47695=CARTESIAN_POINT('Ctrl Pts',(0.886975379660772,-5.21384848487043,
11.985155398064));
#47696=CARTESIAN_POINT('Ctrl Pts',(3.27268248423369,-4.15457467193696,12.0645272881174));
#47697=CARTESIAN_POINT('Ctrl Pts',(4.86117137960707,-2.08325566491467,12.1438991781708));
#47698=CARTESIAN_POINT('Ctrl Pts',(5.26548968692849,0.495539810872594,12.2232710682242));
#47699=CARTESIAN_POINT('Ctrl Pts',(4.38714636147788,2.95362288559007,12.3026429582776));
#47700=CARTESIAN_POINT('Ctrl Pts',(2.44010389315499,4.69220996311119,12.382014848331));
#47701=CARTESIAN_POINT('Ctrl Pts',(-0.101342482462103,5.28778507964898,
12.4613867383844));
#47702=CARTESIAN_POINT('Ctrl Pts',(-2.61810205366918,4.59526745509803,12.5407586284378));
#47703=CARTESIAN_POINT('Ctrl Pts',(-4.49709775967304,2.78335284993721,12.6201305184912));
#47704=CARTESIAN_POINT('Ctrl Pts',(-5.28061040557763,0.293419651378745,
12.6995024085446));
#47705=CARTESIAN_POINT('Ctrl Pts',(-4.7777780451164,-2.26798992478223,12.778874298598));
#47706=CARTESIAN_POINT('Ctrl Pts',(-3.11108952829712,-4.27692217537683,
12.8582461886514));
#47707=CARTESIAN_POINT('Ctrl Pts',(-0.686546488664521,-5.24400565085626,
12.9376180787048));
#47708=CARTESIAN_POINT('Ctrl Pts',(1.90523775596186,-4.93366095719673,13.0169899687582));
#47709=CARTESIAN_POINT('Ctrl Pts',(4.03291030040817,-3.42148737483739,13.0963618588116));
#47710=CARTESIAN_POINT('Ctrl Pts',(5.17817482237061,-1.07584704130148,13.175733748865));
#47711=CARTESIAN_POINT('Ctrl Pts',(5.06204741929909,1.53186725014844,13.2551056389184));
#47712=CARTESIAN_POINT('Ctrl Pts',(3.71281646953824,3.76642207019282,13.3344775289718));
#47713=CARTESIAN_POINT('Ctrl Pts',(1.45915164597774,5.08348481077208,13.4138494190252));
#47714=CARTESIAN_POINT('Ctrl Pts',(-1.14995928876559,5.16222190355004,13.4932213090786));
#47715=CARTESIAN_POINT('Ctrl Pts',(-3.47894268615732,3.98345316700755,13.572593199132));
#47716=CARTESIAN_POINT('Ctrl Pts',(-4.96046334571011,1.83432405620607,13.6519650891854));
#47717=CARTESIAN_POINT('Ctrl Pts',(-5.23362611404733,-0.761642334479749,
13.7313369792388));
#47718=CARTESIAN_POINT('Ctrl Pts',(-4.23188914543755,-3.17207433835303,
13.8107088692922));
#47719=CARTESIAN_POINT('Ctrl Pts',(-2.19927334812693,-4.80979605467098,
13.8900807593456));
#47720=CARTESIAN_POINT('Ctrl Pts',(0.369080568778457,-5.27586209837409,
13.9694526493991));
#47721=CARTESIAN_POINT('Ctrl Pts',(2.84752727607539,-4.45673981283591,14.0488245394524));
#47722=CARTESIAN_POINT('Ctrl Pts',(4.63232264181505,-2.55196557371717,14.1281964295059));
#47723=CARTESIAN_POINT('Ctrl Pts',(5.28869446548083,-0.0255381695209159,
14.2075683195592));
#47724=CARTESIAN_POINT('Ctrl Pts',(4.65675202368211,2.50711027624288,14.2869402096127));
#47725=CARTESIAN_POINT('Ctrl Pts',(2.89043509646017,4.42903220810837,14.3663120996661));
#47726=CARTESIAN_POINT('Ctrl Pts',(0.420014577610126,5.27205169757513,14.4456839897195));
#47727=CARTESIAN_POINT('Ctrl Pts',(-2.15272056265924,4.83081106300113,14.5250558797729));
#47728=CARTESIAN_POINT('Ctrl Pts',(-4.201057738831,3.21279554629894,14.6044277698263));
#47729=CARTESIAN_POINT('Ctrl Pts',(-5.22602654870706,0.81215014592063,14.6837996598797));
#47730=CARTESIAN_POINT('Ctrl Pts',(-4.97794685893165,-1.78633323234006,
14.7631715499331));
#47731=CARTESIAN_POINT('Ctrl Pts',(-3.51725033281897,-3.94966978918425,
14.8425434399865));
#47732=CARTESIAN_POINT('Ctrl Pts',(-1.19975941093315,-5.15087552782897,
14.9219153300399));
#47733=CARTESIAN_POINT('Ctrl Pts',(1.40999024783357,-5.09733938916413,15.0012872200933));
#47734=CARTESIAN_POINT('Ctrl Pts',(3.67626940318851,-3.8021026580683,15.0806591101467));
#47735=CARTESIAN_POINT('Ctrl Pts',(5.04701746921103,-1.5806821352785,15.1600310002001));
#47736=CARTESIAN_POINT('Ctrl Pts',(5.18832325111744,1.02578905688456,15.2394028902535));
#47737=CARTESIAN_POINT('Ctrl Pts',(4.06576497321036,3.38238030533612,15.3187747803069));
#47738=CARTESIAN_POINT('Ctrl Pts',(1.95279534724736,4.91503119817963,15.3981466703603));
#47739=CARTESIAN_POINT('Ctrl Pts',(-0.635870902865948,5.2503913703836,15.4775185604137));
#47740=CARTESIAN_POINT('Ctrl Pts',(-3.06964040851742,4.30676782630626,15.5568904504671));
#47741=CARTESIAN_POINT('Ctrl Pts',(-4.75565230518791,2.31402517260967,15.6362623405205));
#47742=CARTESIAN_POINT('Ctrl Pts',(-5.28319782677237,-0.24240889112691,
15.7156342305739));
#47743=CARTESIAN_POINT('Ctrl Pts',(-4.52376805191524,-2.73979268554778,
15.7950061206273));
#47744=CARTESIAN_POINT('Ctrl Pts',(-2.66235839280204,-4.56976904619777,
15.8743780106807));
#47745=CARTESIAN_POINT('Ctrl Pts',(-0.15240412223312,-5.28655978220556,
15.9537499007341));
#47746=CARTESIAN_POINT('Ctrl Pts',(2.39467545517194,-4.71555625687092,16.0331217907875));
#47747=CARTESIAN_POINT('Ctrl Pts',(4.35841739221953,-2.99585366506689,16.112493680841));
#47748=CARTESIAN_POINT('Ctrl Pts',(5.26045849971912,-0.546367751666672,
16.1918655708943));
#47749=CARTESIAN_POINT('Ctrl Pts',(4.88106356050808,2.03621213668353,16.2712374609478));
#47750=CARTESIAN_POINT('Ctrl Pts',(3.31265234202039,4.12277525560071,16.3506093510011));
#47751=CARTESIAN_POINT('Ctrl Pts',(0.937286345425132,5.20503944789207,16.4299812410546));
#47752=CARTESIAN_POINT('Ctrl Pts',(-1.66640053022416,5.01936755177917,16.509353131108));
#47753=CARTESIAN_POINT('Ctrl Pts',(-3.86415592530783,3.6109888303424,16.5887250211614));
#47754=CARTESIAN_POINT('Ctrl Pts',(-5.12061148999576,1.32298122241861,16.6680969112148));
#47755=CARTESIAN_POINT('Ctrl Pts',(-5.1296974302943,-1.28730168253218,16.7474688012682));
#47756=CARTESIAN_POINT('Ctrl Pts',(-3.88920043041393,-3.58400074773889,
16.8268406913216));
#47757=CARTESIAN_POINT('Ctrl Pts',(-1.70130281532588,-5.00764516247516,
16.906212581375));
#47758=CARTESIAN_POINT('Ctrl Pts',(0.90102840177319,-5.21143830245825,16.9855844714284));
#47759=CARTESIAN_POINT('Ctrl Pts',(3.28387109087768,-4.1457366023928,17.0649563614818));
#47760=CARTESIAN_POINT('Ctrl Pts',(4.86677005798476,-2.07014265165526,17.1443282515352));
#47761=CARTESIAN_POINT('Ctrl Pts',(5.26413459813378,0.50973348428664,17.2237001415886));
#47762=CARTESIAN_POINT('Ctrl Pts',(4.37916762715237,2.96543963879408,17.303072031642));
#47763=CARTESIAN_POINT('Ctrl Pts',(2.42744506809458,4.69877132337447,17.3824439216954));
#47764=CARTESIAN_POINT('Ctrl Pts',(-0.115597647321682,5.28749259670007,
17.4618158117488));
#47765=CARTESIAN_POINT('Ctrl Pts',(-2.63048120009413,4.58819259887652,17.5411877018022));
#47766=CARTESIAN_POINT('Ctrl Pts',(-4.5045850370732,2.7712186210673,17.6205595918556));
#47767=CARTESIAN_POINT('Ctrl Pts',(-5.28138253005218,0.27918271172893,17.699931481909));
#47768=CARTESIAN_POINT('Ctrl Pts',(-4.77164579536179,-2.28086298099153,
17.7793033719624));
#47769=CARTESIAN_POINT('Ctrl Pts',(-3.09954884704088,-4.28529268150238,
17.8586752620158));
#47770=CARTESIAN_POINT('Ctrl Pts',(-0.672404619068171,-5.24583989230806,
17.9380471520692));
#47771=CARTESIAN_POINT('Ctrl Pts',(1.91852825506979,-4.9285020674696,18.0174190421226));
#47772=CARTESIAN_POINT('Ctrl Pts',(4.04212630117149,-3.41061102326166,18.096790932176));
#47773=CARTESIAN_POINT('Ctrl Pts',(5.18104412158612,-1.06186685398811,18.1761628222294));
#47774=CARTESIAN_POINT('Ctrl Pts',(5.05792243214194,1.54547807796858,18.2555347122829));
#47775=CARTESIAN_POINT('Ctrl Pts',(3.70260503654169,3.77647571272922,18.3349066023362));
#47776=CARTESIAN_POINT('Ctrl Pts',(1.44552439996779,5.08729102078633,18.4142784923897));
#47777=CARTESIAN_POINT('Ctrl Pts',(-1.16402860508455,5.15930893371508,18.4936503824431));
#47778=CARTESIAN_POINT('Ctrl Pts',(-3.48937383888192,3.97367066688439,18.5730222724965));
#47779=CARTESIAN_POINT('Ctrl Pts',(-4.96594823061187,1.82167865277138,18.6523941625499));
#47780=CARTESIAN_POINT('Ctrl Pts',(-5.23050112077116,-0.77713504302674,
18.7317660526033));
#47781=CARTESIAN_POINT('Ctrl Pts',(-4.22530652207786,-3.18086119603167,
18.8111379426567));
#47782=CARTESIAN_POINT('Ctrl Pts',(-2.18257651229225,-4.82058518621618,
18.8905098327101));
#47783=CARTESIAN_POINT('Ctrl Pts',(0.37648005341871,-5.26605971579227,18.9698817227635));
#47784=CARTESIAN_POINT('Ctrl Pts',(3.70230252414111,-4.19446206534953,19.0757109095013));
#47785=CARTESIAN_POINT('Ctrl Pts',(5.99600976813328,-0.0197068834824163,
19.2079973929237));
#47786=CARTESIAN_POINT('Ctrl Pts',(3.26379011618947,5.03400372054209,19.3667411730305));
#47787=CARTESIAN_POINT('Ctrl Pts',(-2.45559119020206,5.46873373673905,19.5254849531373));
#47788=CARTESIAN_POINT('Ctrl Pts',(-5.92771323046149,0.905806267444168,
19.6842287332441));
#47789=CARTESIAN_POINT('Ctrl Pts',(-3.97578039972873,-4.48936692070992,
19.8429725133509));
#47790=CARTESIAN_POINT('Ctrl Pts',(1.61419617037569,-5.77483540889728,20.0017162934577));
#47791=CARTESIAN_POINT('Ctrl Pts',(5.72720375155094,-1.77677009197941,20.1604600735645));
#47792=CARTESIAN_POINT('Ctrl Pts',(4.59927593805412,3.84720861430021,20.3192038536713));
#47793=CARTESIAN_POINT('Ctrl Pts',(-0.73672307947618,5.95134306184733,20.4779476337782));
#47794=CARTESIAN_POINT('Ctrl Pts',(-5.3995463563661,2.60828838171381,20.6366914138849));
#47795=CARTESIAN_POINT('Ctrl Pts',(-5.1196790448508,-3.11863163173554,20.7954351939918));
#47796=CARTESIAN_POINT('Ctrl Pts',(-0.158509478954971,-5.99736559883163,
20.9541789740985));
#47797=CARTESIAN_POINT('Ctrl Pts',(4.95432466322423,-3.37745298000941,21.1129227542054));
#47798=CARTESIAN_POINT('Ctrl Pts',(5.4262515554071,1.3624793779577,21.2452092376277));
#47799=CARTESIAN_POINT('Ctrl Pts',(3.29092685490723,4.12830747359771,21.3510384243656));
#47800=CARTESIAN_POINT('Ctrl Pts',(0.929079443196039,5.20946188754723,21.430410314419));
#47801=CARTESIAN_POINT('Ctrl Pts',(-1.68303999757346,5.01382783115869,21.5097822044724));
#47802=CARTESIAN_POINT('Ctrl Pts',(-3.8722246926078,3.60110493868854,21.5891540945258));
#47803=CARTESIAN_POINT('Ctrl Pts',(-5.12503498129818,1.30888173016128,21.6685259845792));
#47804=CARTESIAN_POINT('Ctrl Pts',(-5.12574462250326,-1.300972874894,21.7478978746326));
#47805=CARTESIAN_POINT('Ctrl Pts',(-3.87976959979778,-3.59455409188016,
21.827269764686));
#47806=CARTESIAN_POINT('Ctrl Pts',(-1.68766624540451,-5.01217052435348,
21.9066416547394));
#47807=CARTESIAN_POINT('Ctrl Pts',(0.915005995631755,-5.2090130440819,21.9860135447928));
#47808=CARTESIAN_POINT('Ctrl Pts',(3.29507231119182,-4.13685632854986,22.0653854348462));
#47809=CARTESIAN_POINT('Ctrl Pts',(4.87231403886192,-2.05702097999265,22.1447573248996));
#47810=CARTESIAN_POINT('Ctrl Pts',(5.26275149225388,0.523926824466718,22.2241292149531));
#47811=CARTESIAN_POINT('Ctrl Pts',(4.37115162329097,2.97723307464397,22.3035011050064));
#47812=CARTESIAN_POINT('Ctrl Pts',(2.4147715124657,4.70529942618521,22.3828729950599));
#47813=CARTESIAN_POINT('Ctrl Pts',(-0.129853572474074,5.28716128664959,
22.4622448851132));
#47814=CARTESIAN_POINT('Ctrl Pts',(-2.64284027062663,4.58108446095525,22.5416167751666));
#47815=CARTESIAN_POINT('Ctrl Pts',(-4.51204028846786,2.7590644882843,22.62098866522));
#47816=CARTESIAN_POINT('Ctrl Pts',(-5.28211549991429,0.264943102456049,
22.7003605552734));
#47817=CARTESIAN_POINT('Ctrl Pts',(-4.76548000969985,-2.2937181486802,22.7797324453269));
#47818=CARTESIAN_POINT('Ctrl Pts',(-3.08798363825926,-4.29363457062517,
22.8591043353802));
#47819=CARTESIAN_POINT('Ctrl Pts',(-0.658261551986295,-5.24763120247219,
22.9384762254337));
#47820=CARTESIAN_POINT('Ctrl Pts',(1.93181173129385,-4.92331644248731,23.017848115487));
#47821=CARTESIAN_POINT('Ctrl Pts',(4.05129987868926,-3.39969271923279,23.0972200055405));
#47822=CARTESIAN_POINT('Ctrl Pts',(5.18390038229797,-1.0479113616667,23.1765918955939));
#47823=CARTESIAN_POINT('Ctrl Pts',(5.05371420635457,1.55913887720483,23.2559637856473));
#47824=CARTESIAN_POINT('Ctrl Pts',(3.69245444696201,3.78638634033052,23.3353356757007));
#47825=CARTESIAN_POINT('Ctrl Pts',(1.43172095156667,5.09127847004479,23.4147075657541));
#47826=CARTESIAN_POINT('Ctrl Pts',(-1.17777659548102,5.1559464348325,23.4940794558075));
#47827=CARTESIAN_POINT('Ctrl Pts',(-3.50037037246962,3.96463726004727,23.5734513458609));
#47828=CARTESIAN_POINT('Ctrl Pts',(-4.97028167379665,1.80755122457705,23.6528232359143));
#47829=CARTESIAN_POINT('Ctrl Pts',(-5.22944336137752,-0.789850288405212,
23.7321951259677));
#47830=CARTESIAN_POINT('Ctrl Pts',(-4.21472422106041,-3.19484601935549,
23.8115670160211));
#47831=CARTESIAN_POINT('Ctrl Pts',(-2.17330758975551,-4.82158433170509,
23.8909389060745));
#47832=CARTESIAN_POINT('Ctrl Pts',(0.397521959947206,-5.27379537322471,
23.9703107961279));
#47833=CARTESIAN_POINT('Ctrl Pts',(2.87151604007067,-4.4413215351868,24.0496826861813));
#47834=CARTESIAN_POINT('Ctrl Pts',(4.64601516884499,-2.5269516018695,24.1290545762347));
#47835=CARTESIAN_POINT('Ctrl Pts',(5.28875528625864,0.00297814834736192,
24.2084264662881));
#47836=CARTESIAN_POINT('Ctrl Pts',(4.64316632240633,2.53218242822061,24.2877983563415));
#47837=CARTESIAN_POINT('Ctrl Pts',(2.86651231988729,4.4445526734691,24.3671702463949));
#47838=CARTESIAN_POINT('Ctrl Pts',(0.391582261162602,5.27423972531146,24.4465421364484));
#47839=CARTESIAN_POINT('Ctrl Pts',(-2.1787363696294,4.81913365439931,24.5259140265017));
#47840=CARTESIAN_POINT('Ctrl Pts',(-4.21831964333045,3.19009729224708,24.6052859165552));
#47841=CARTESIAN_POINT('Ctrl Pts',(-5.23032958900859,0.783960290863936,
24.6846578066085));
#47842=CARTESIAN_POINT('Ctrl Pts',(-4.9682428239423,-1.81314770210696,24.764029696662));
#47843=CARTESIAN_POINT('Ctrl Pts',(-3.49590310398264,-3.96857692817898,
24.8434015867153));
#47844=CARTESIAN_POINT('Ctrl Pts',(-1.17196912594307,-5.15726959884261,
24.9227734767688));
#47845=CARTESIAN_POINT('Ctrl Pts',(1.43745393706658,-5.08966281065081,25.0021453668222));
#47846=CARTESIAN_POINT('Ctrl Pts',(3.69671640275713,-3.78222542756197,25.0815172568756));
#47847=CARTESIAN_POINT('Ctrl Pts',(5.05546693527898,-1.55344630213307,25.160889146929));
#47848=CARTESIAN_POINT('Ctrl Pts',(5.18271691245315,1.05374890400037,25.2402610369824));
#47849=CARTESIAN_POINT('Ctrl Pts',(4.04746852150308,3.40425320955296,25.3196329270358));
#47850=CARTESIAN_POINT('Ctrl Pts',(1.92626575763449,4.92548896844514,25.3990048170892));
#47851=CARTESIAN_POINT('Ctrl Pts',(-0.664171081076968,5.24688651700902,
25.4783767071426));
#47852=CARTESIAN_POINT('Ctrl Pts',(-3.09281731455583,4.2901541238158,25.5577485971959));
#47853=CARTESIAN_POINT('Ctrl Pts',(-4.76806009604388,2.2883496821561,25.6371204872494));
#47854=CARTESIAN_POINT('Ctrl Pts',(-5.28181399205765,-0.2708916769007,25.7164923773028));
#47855=CARTESIAN_POINT('Ctrl Pts',(-4.50892969070311,-2.76414442307307,
25.7958642673562));
#47856=CARTESIAN_POINT('Ctrl Pts',(-2.63768009703987,-4.58405770611471,
25.8752361574096));
#47857=CARTESIAN_POINT('Ctrl Pts',(-0.123897470143628,-5.28730467858643,
25.9546080474629));
#47858=CARTESIAN_POINT('Ctrl Pts',(2.42006630623721,-4.70257593460492,26.0339799375165));
#47859=CARTESIAN_POINT('Ctrl Pts',(4.37450728714461,-2.97231010192892,26.1133518275698));
#47860=CARTESIAN_POINT('Ctrl Pts',(5.26332797571122,-0.517996107519831,
26.1927237176232));
#47861=CARTESIAN_POINT('Ctrl Pts',(4.8700136195734,2.06250059211614,26.2720956076766));
#47862=CARTESIAN_POINT('Ctrl Pts',(3.29037472529985,4.14057671278022,26.35146749773));
#47863=CARTESIAN_POINT('Ctrl Pts',(0.909207831064193,5.21001751122215,26.4308393877834));
#47864=CARTESIAN_POINT('Ctrl Pts',(-1.69344007832135,5.01030957610855,26.5102112778369));
#47865=CARTESIAN_POINT('Ctrl Pts',(-3.88356973299385,3.59010131838702,26.5895831678902));
#47866=CARTESIAN_POINT('Ctrl Pts',(-5.12767039684481,1.29535232606086,26.6689550579437));
#47867=CARTESIAN_POINT('Ctrl Pts',(-5.12268190193029,-1.31494162567991,
26.748326947997));
#47868=CARTESIAN_POINT('Ctrl Pts',(-3.86981943456965,-3.604918707979,26.8276988380504));
#47869=CARTESIAN_POINT('Ctrl Pts',(-1.67427751864785,-5.01674557236666,
26.9070707281038));
#47870=CARTESIAN_POINT('Ctrl Pts',(0.929114694866165,-5.20650431970375,
26.9864426181573));
#47871=CARTESIAN_POINT('Ctrl Pts',(3.30617662527125,-4.12797013916282,27.0658145082107));
#47872=CARTESIAN_POINT('Ctrl Pts',(4.8778612478581,-2.04387156982875,27.145186398264));
#47873=CARTESIAN_POINT('Ctrl Pts',(5.26130966742943,0.538109589882639,27.2245582883175));
#47874=CARTESIAN_POINT('Ctrl Pts',(4.36311469772634,2.98900844458398,27.3039301783709));
#47875=CARTESIAN_POINT('Ctrl Pts',(2.40207464524773,4.7117914582426,27.3833020684242));
#47876=CARTESIAN_POINT('Ctrl Pts',(-0.144105473911181,5.28679250204684,
27.4626739584777));
#47877=CARTESIAN_POINT('Ctrl Pts',(-2.65518181859737,4.57394259446923,27.542045848531));
#47878=CARTESIAN_POINT('Ctrl Pts',(-4.51946174941854,2.74689039512913,27.6214177385845));
#47879=CARTESIAN_POINT('Ctrl Pts',(-5.28281080174027,0.25070177567431,27.7007896286378));
#47880=CARTESIAN_POINT('Ctrl Pts',(-4.75927883606144,-2.30655724141581,
27.7801615186913));
#47881=CARTESIAN_POINT('Ctrl Pts',(-3.07639708040302,-4.30194401997489,
27.8595334087447));
#47882=CARTESIAN_POINT('Ctrl Pts',(-0.644111805447875,-5.24938675745965,
27.9389052987981));
#47883=CARTESIAN_POINT('Ctrl Pts',(1.94507767959709,-4.91809050014772,28.0182771888515));
#47884=CARTESIAN_POINT('Ctrl Pts',(4.06045054724861,-3.38875828300845,28.0976490789049));
#47885=CARTESIAN_POINT('Ctrl Pts',(5.18670664924518,-1.03393204901761,28.1770209689583));
#47886=CARTESIAN_POINT('Ctrl Pts',(5.0494924920661,1.57275774354414,28.2563928590118));
#47887=CARTESIAN_POINT('Ctrl Pts',(3.68223314068176,3.79632723101881,28.3357647490651));
#47888=CARTESIAN_POINT('Ctrl Pts',(1.41798994671214,5.09511980804509,28.4151366391186));
#47889=CARTESIAN_POINT('Ctrl Pts',(-1.19167245960906,5.15275247768794,28.4945085291719));
#47890=CARTESIAN_POINT('Ctrl Pts',(-3.51104609249168,3.9551860491902,28.5738804192253));
#47891=CARTESIAN_POINT('Ctrl Pts',(-4.97513666881207,1.79414505376557,28.6532523092787));
#47892=CARTESIAN_POINT('Ctrl Pts',(-5.22729496488809,-0.803945705483672,
28.7326241993322));
#47893=CARTESIAN_POINT('Ctrl Pts',(-4.2060957779385,-3.20619707038074,28.8119960893855));
#47894=CARTESIAN_POINT('Ctrl Pts',(-2.16030096951815,-4.82742592572986,
28.891367979439));
#47895=CARTESIAN_POINT('Ctrl Pts',(0.41173837333167,-5.27270451089724,28.9707398694923));
#47896=CARTESIAN_POINT('Ctrl Pts',(2.88347915980534,-4.43356394814356,29.0501117595458));
#47897=CARTESIAN_POINT('Ctrl Pts',(4.65281080542333,-2.51441702114943,29.1294836495991));
#47898=CARTESIAN_POINT('Ctrl Pts',(5.28872803766221,0.0172363266290461,
29.2088555396526));
#47899=CARTESIAN_POINT('Ctrl Pts',(4.6363228263275,2.54469094339263,29.2882274297059));
#47900=CARTESIAN_POINT('Ctrl Pts',(2.85451963682592,4.45226447892365,29.3675993197594));
#47901=CARTESIAN_POINT('Ctrl Pts',(0.377361782165573,5.2752762423091,29.4469712098127));
#47902=CARTESIAN_POINT('Ctrl Pts',(-2.19172056735417,4.81324238969394,29.5263430998662));
#47903=CARTESIAN_POINT('Ctrl Pts',(-4.22690463795758,3.17871334488069,29.6057149899195));
#47904=CARTESIAN_POINT('Ctrl Pts',(-5.23242409484928,0.769856765217166,
29.6850868799731));
#47905=CARTESIAN_POINT('Ctrl Pts',(-4.96333662400999,-1.82653521840426,
29.7644587700263));
#47906=CARTESIAN_POINT('Ctrl Pts',(-3.48519133772112,-3.97798726578954,
29.8438306600798));
#47907=CARTESIAN_POINT('Ctrl Pts',(-1.15806115590354,-5.16041042035391,
29.9232025501331));
#47908=CARTESIAN_POINT('Ctrl Pts',(1.45117016016719,-5.08576901889481,30.0025744401866));
#47909=CARTESIAN_POINT('Ctrl Pts',(3.70689963733188,-3.77224554159173,30.08194633024));
#47910=CARTESIAN_POINT('Ctrl Pts',(5.05963656792573,-1.53981140008078,30.1613182202934));
#47911=CARTESIAN_POINT('Ctrl Pts',(5.17985722988845,1.06771739017516,30.2406901103468));
#47912=CARTESIAN_POINT('Ctrl Pts',(4.0382761360698,3.41515258753676,30.3200620004003));
#47913=CARTESIAN_POINT('Ctrl Pts',(1.91297991407722,4.93066417388641,30.3994338904535));
#47914=CARTESIAN_POINT('Ctrl Pts',(-0.678313980675348,5.24507688131741,
30.4788057805071));
#47915=CARTESIAN_POINT('Ctrl Pts',(-3.10437209115798,4.28180047024023,30.5581776705604));
#47916=CARTESIAN_POINT('Ctrl Pts',(-4.77421203164559,2.2754869422171,30.6375495606138));
#47917=CARTESIAN_POINT('Ctrl Pts',(-5.28106448876339,-0.285130168225216,
30.7169214506672));
#47918=CARTESIAN_POINT('Ctrl Pts',(-4.50146132585641,-2.77629020081278,
30.7962933407206));
#47919=CARTESIAN_POINT('Ctrl Pts',(-2.62531214778642,-4.59115208569648,
30.8756652307741));
#47920=CARTESIAN_POINT('Ctrl Pts',(-0.109642741545517,-5.28761948484725,
30.9550371208274));
#47921=CARTESIAN_POINT('Ctrl Pts',(2.43273539384572,-4.69603448143646,31.0344090108809));
#47922=CARTESIAN_POINT('Ctrl Pts',(4.38250457206463,-2.96050587284378,31.1137809009342));
#47923=CARTESIAN_POINT('Ctrl Pts',(5.26470533703794,-0.503804586594991,
31.1931527909877));
#47924=CARTESIAN_POINT('Ctrl Pts',(4.86443553513645,2.07562238179582,31.272524681041));
#47925=CARTESIAN_POINT('Ctrl Pts',(3.27920000412114,4.14943233229341,31.3518965710945));
#47926=CARTESIAN_POINT('Ctrl Pts',(0.895158610487983,5.21244975125701,31.4312684611478));
#47927=CARTESIAN_POINT('Ctrl Pts',(-1.70694143926006,5.00572594837619,31.5106403512013));
#47928=CARTESIAN_POINT('Ctrl Pts',(-3.89323433265515,3.57961838445739,31.5900122412546));
#47929=CARTESIAN_POINT('Ctrl Pts',(-5.13114396014345,1.28152370543563,31.6693841313081));
#47930=CARTESIAN_POINT('Ctrl Pts',(-5.11911827653528,-1.32874731162563,
31.7487560213615));
#47931=CARTESIAN_POINT('Ctrl Pts',(-3.86008671173927,-3.61533842470713,
31.8281279114149));
#47932=CARTESIAN_POINT('Ctrl Pts',(-1.6607465681206,-5.02124109994587,31.9074998014683));
#47933=CARTESIAN_POINT('Ctrl Pts',(0.943147763492109,-5.20398055756647,
31.9868716915216));
#47934=CARTESIAN_POINT('Ctrl Pts',(3.31729338754031,-4.11904187017945,32.0662435815751));
#47935=CARTESIAN_POINT('Ctrl Pts',(4.88335368508803,-2.03071370056122,32.1456154716285));
#47936=CARTESIAN_POINT('Ctrl Pts',(5.25983983406835,0.552291831605133,32.2249873616819));
#47937=CARTESIAN_POINT('Ctrl Pts',(4.35504064192764,3.00076029606972,32.3043592517354));
#47938=CARTESIAN_POINT('Ctrl Pts',(2.3893631891323,4.71825019448202,32.3837311417886));
#47939=CARTESIAN_POINT('Ctrl Pts',(-0.158357847769981,5.28638478918814,
32.4631030318421));
#47940=CARTESIAN_POINT('Ctrl Pts',(-2.66750326347463,4.56676775046226,32.5424749218955));
#47941=CARTESIAN_POINT('Ctrl Pts',(-4.52685078861515,2.73469619609277,32.6218468119489));
#47942=CARTESIAN_POINT('Ctrl Pts',(-5.28346748166331,0.23645870150246,32.7012187020024));
#47943=CARTESIAN_POINT('Ctrl Pts',(-4.75304319093522,-2.31937960938145,
32.7805905920557));
#47944=CARTESIAN_POINT('Ctrl Pts',(-3.06478809957792,-4.3102221812797,32.8599624821091));
#47945=CARTESIAN_POINT('Ctrl Pts',(-0.629957410956834,-5.25110417033318,
32.9393343721625));
#47946=CARTESIAN_POINT('Ctrl Pts',(1.95832950858626,-4.91282880661543,33.0187062622159));
#47947=CARTESIAN_POINT('Ctrl Pts',(4.06957169452659,-3.37779921996823,33.0980781522693));
#47948=CARTESIAN_POINT('Ctrl Pts',(5.18947522352436,-1.01994521996853,33.1774500423228));
#47949=CARTESIAN_POINT('Ctrl Pts',(5.04523407478018,1.586365178005,33.2568219323761));
#47950=CARTESIAN_POINT('Ctrl Pts',(3.67198507285579,3.80624052997629,33.3361938224296));
#47951=CARTESIAN_POINT('Ctrl Pts',(1.40424863498483,5.09892411381589,33.4155657124829));
#47952=CARTESIAN_POINT('Ctrl Pts',(-1.20555966211678,5.14952106980705,33.4949376025364));
#47953=CARTESIAN_POINT('Ctrl Pts',(-3.52169629398785,3.94570609146478,33.5743094925897));
#47954=CARTESIAN_POINT('Ctrl Pts',(-4.979955503786,1.78072584291395,33.6536813826432));
#47955=CARTESIAN_POINT('Ctrl Pts',(-5.22510857580638,-0.818035279400921,
33.7330532726965));
#47956=CARTESIAN_POINT('Ctrl Pts',(-4.19743676434199,-3.2175248183441,33.81242516275));
#47957=CARTESIAN_POINT('Ctrl Pts',(-2.14727864795256,-4.83323243340904,
33.8917970528034));
#47958=CARTESIAN_POINT('Ctrl Pts',(0.425951794157462,-5.27157532587404,
33.9711689428568));
#47959=CARTESIAN_POINT('Ctrl Pts',(2.89542132203897,-4.4257741373902,34.0505408329101));
#47960=CARTESIAN_POINT('Ctrl Pts',(4.6595726247782,-2.50186416532303,34.1299127229636));
#47961=CARTESIAN_POINT('Ctrl Pts',(5.28866234991056,0.0314943796344648,
34.209284613017));
#47962=CARTESIAN_POINT('Ctrl Pts',(4.62944563286023,2.55718096342464,34.2886565030704));
#47963=CARTESIAN_POINT('Ctrl Pts',(2.84250620674923,4.45994392474861,34.3680283931238));
#47964=CARTESIAN_POINT('Ctrl Pts',(0.363138560454883,5.27627441792225,34.4474002831772));
#47965=CARTESIAN_POINT('Ctrl Pts',(-2.20468883537271,4.80731614172534,34.5267721732306));
#47966=CARTESIAN_POINT('Ctrl Pts',(-4.23545891089946,3.1673062942179,34.606144063284));
#47967=CARTESIAN_POINT('Ctrl Pts',(-5.23448057076036,0.755747644152594,
34.6855159533374));
#47968=CARTESIAN_POINT('Ctrl Pts',(-4.95839434991029,-1.83990945920924,
34.7648878433908));
#47969=CARTESIAN_POINT('Ctrl Pts',(-3.47445424064183,-3.98736869087822,
34.8442597334442));
#47970=CARTESIAN_POINT('Ctrl Pts',(-1.14414476892706,-5.16351373534018,
34.9236316234976));
#47971=CARTESIAN_POINT('Ctrl Pts',(1.4648758359769,-5.0818382631171,35.003003513551));
#47972=CARTESIAN_POINT('Ctrl Pts',(3.71705592968454,-3.76223823845686,35.0823754036044));
#47973=CARTESIAN_POINT('Ctrl Pts',(5.06376942648477,-1.52616530648161,35.1617472936578));
#47974=CARTESIAN_POINT('Ctrl Pts',(5.1769598994568,1.08167811604296,35.2411191837112));
#47975=CARTESIAN_POINT('Ctrl Pts',(4.02905439992751,3.42602714375337,35.3204910737646));
#47976=CARTESIAN_POINT('Ctrl Pts',(1.8996801667365,4.93580354262787,35.3998629638181));
#47977=CARTESIAN_POINT('Ctrl Pts',(-0.69245195020073,5.24322912373406,35.4792348538714));
#47978=CARTESIAN_POINT('Ctrl Pts',(-3.11590430478548,4.27341569598948,35.5586067439249));
#47979=CARTESIAN_POINT('Ctrl Pts',(-4.78032926766171,2.26260766374704,35.6379786339782));
#47980=CARTESIAN_POINT('Ctrl Pts',(-5.28027660201491,-0.299366587187078,
35.7173505240316));
#47981=CARTESIAN_POINT('Ctrl Pts',(-4.49396024381123,-2.78841580011912,
35.7967224140851));
#47982=CARTESIAN_POINT('Ctrl Pts',(-2.61292511742748,-4.59821309619579,
35.8760943041384));
#47983=CARTESIAN_POINT('Ctrl Pts',(-0.0953872160500441,-5.28789586001125,
35.9554661941919));
#47984=CARTESIAN_POINT('Ctrl Pts',(2.4453868000212,-4.68945889688694,36.0348380842453));
#47985=CARTESIAN_POINT('Ctrl Pts',(4.39047000437915,-2.94868012642215,36.1142099742987));
#47986=CARTESIAN_POINT('Ctrl Pts',(5.26604443381084,-0.489609403953667,
36.1935818643521));
#47987=CARTESIAN_POINT('Ctrl Pts',(4.85882209535785,2.08872908558584,36.2729537544055));
#47988=CARTESIAN_POINT('Ctrl Pts',(3.26800144929601,4.15825779320007,36.3523256444589));
#47989=CARTESIAN_POINT('Ctrl Pts',(0.881102883784141,5.2148441065383,36.4316975345123));
#47990=CARTESIAN_POINT('Ctrl Pts',(-1.72043039392939,5.00110593838543,36.5110694245656));
#47991=CARTESIAN_POINT('Ctrl Pts',(-3.90287063578981,3.56910943340206,36.5904413146191));
#47992=CARTESIAN_POINT('Ctrl Pts',(-5.13458022962944,1.26768577053169,36.6698132046725));
#47993=CARTESIAN_POINT('Ctrl Pts',(-5.11551744473188,-1.34254334006536,
36.7491850947259));
#47994=CARTESIAN_POINT('Ctrl Pts',(-3.85032593330342,-3.62573186469175,
36.8285569847793));
#47995=CARTESIAN_POINT('Ctrl Pts',(-1.64720354707418,-5.02570013250056,
36.9079288748327));
#47996=CARTESIAN_POINT('Ctrl Pts',(0.957173977199105,-5.20141897223083,
36.9873007648861));
#47997=CARTESIAN_POINT('Ctrl Pts',(3.32838603929536,-4.11008366347129,37.0666726549395));
#47998=CARTESIAN_POINT('Ctrl Pts',(4.88881062947681,-2.01754107180608,37.1460445449929));
#47999=CARTESIAN_POINT('Ctrl Pts',(5.25833177151655,0.566470059199757,37.2254164350463));
#48000=CARTESIAN_POINT('Ctrl Pts',(4.34693493313475,3.01249033764469,37.3047883250998));
#48001=CARTESIAN_POINT('Ctrl Pts',(2.37663436681862,4.72467463787371,37.3841602151531));
#48002=CARTESIAN_POINT('Ctrl Pts',(-0.17260907066365,5.28593865420645,37.4635321052065));
#48003=CARTESIAN_POINT('Ctrl Pts',(-2.67980532059584,4.55955971460153,37.54290399526));
#48004=CARTESIAN_POINT('Ctrl Pts',(-4.53420692607955,2.72248212093334,37.6222758853133));
#48005=CARTESIAN_POINT('Ctrl Pts',(-5.28408576066665,0.222213908718847,
37.7016477753668));
#48006=CARTESIAN_POINT('Ctrl Pts',(-4.74677300008161,-2.33218511979937,
37.7810196654201));
#48007=CARTESIAN_POINT('Ctrl Pts',(-3.05315684347904,-4.31846901533503,
37.8603915554736));
#48008=CARTESIAN_POINT('Ctrl Pts',(-0.615798437855754,-5.25278341751105,
37.9397634455269));
#48009=CARTESIAN_POINT('Ctrl Pts',(1.97156710418767,-4.90753140600709,38.0191353355804));
#48010=CARTESIAN_POINT('Ctrl Pts',(4.07866326363087,-3.36681560666115,38.0985072256337));
#48011=CARTESIAN_POINT('Ctrl Pts',(5.19220608004019,-1.00595097780572,38.1778791156872));
#48012=CARTESIAN_POINT('Ctrl Pts',(5.04093898806991,1.59996108252017,38.2572510057405));
#48013=CARTESIAN_POINT('Ctrl Pts',(3.66171031660113,3.81612616476472,38.336622895794));
#48014=CARTESIAN_POINT('Ctrl Pts',(1.39049711694169,5.10269135980963,38.4159947858473));
#48015=CARTESIAN_POINT('Ctrl Pts',(-1.21943810235573,5.14625223481529,38.4953666759008));
#48016=CARTESIAN_POINT('Ctrl Pts',(-3.53232089954511,3.93619745533324,38.5747385659542));
#48017=CARTESIAN_POINT('Ctrl Pts',(-4.98473814342406,1.76729369047725,38.6541104560076));
#48018=CARTESIAN_POINT('Ctrl Pts',(-5.22288421068334,-0.832118909543577,
38.733482346061));
#48019=CARTESIAN_POINT('Ctrl Pts',(-4.18874724188046,-3.22882917750522,
38.8128542361144));
#48020=CARTESIAN_POINT('Ctrl Pts',(-2.13424072225093,-4.83900381899058,
38.8922261261678));
#48021=CARTESIAN_POINT('Ctrl Pts',(0.440162123945958,-5.27040781417516,
38.9715980162212));
#48022=CARTESIAN_POINT('Ctrl Pts',(2.90734243084964,-4.41795218255951,39.0509699062746));
#48023=CARTESIAN_POINT('Ctrl Pts',(4.66630059499982,-2.48929308216594,39.130341796328));
#48024=CARTESIAN_POINT('Ctrl Pts',(5.288558190933,0.0457521216721363,39.2097136863814));
#48025=CARTESIAN_POINT('Ctrl Pts',(4.62253485344793,2.56965255248844,39.2890855764349));
#48026=CARTESIAN_POINT('Ctrl Pts',(2.83047200092405,4.46759066254981,39.3684574664882));
#48027=CARTESIAN_POINT('Ctrl Pts',(0.34891291852996,5.27723479734496,39.4478293565417));
#48028=CARTESIAN_POINT('Ctrl Pts',(-2.21764149317963,4.80135391043001,39.527201246595));
#48029=CARTESIAN_POINT('Ctrl Pts',(-4.24398161873814,3.15587819282133,39.6065731366485));
#48030=CARTESIAN_POINT('Ctrl Pts',(-5.23650047694821,0.74162931109825,39.6859450267018));
#48031=CARTESIAN_POINT('Ctrl Pts',(-4.9534132521342,-1.85326330477585,39.7653169167553));
#48032=CARTESIAN_POINT('Ctrl Pts',(-3.46369715057683,-3.99673439595749,
39.8446888068086));
#48033=CARTESIAN_POINT('Ctrl Pts',(-1.13021013185916,-5.16655447652188,
39.9240606968621));
#48034=CARTESIAN_POINT('Ctrl Pts',(1.47855208450035,-5.0779179090888,40.0034325869154));
#48035=CARTESIAN_POINT('Ctrl Pts',(3.72722085031374,-3.75211381890458,40.0828044769689));
#48036=CARTESIAN_POINT('Ctrl Pts',(5.06779668194711,-1.51268081279862,40.1621763670222));
#48037=CARTESIAN_POINT('Ctrl Pts',(5.17416686787614,1.09598291074358,40.2415482570757));
#48038=CARTESIAN_POINT('Ctrl Pts',(4.40436067122798,2.65600709442752,40.2944628504446));
#48039=CARTESIAN_POINT('Ctrl Pts',(3.85627053850219,3.29705846079199,40.3209201471291));
#48040=CARTESIAN_POINT('Ctrl Pts',(1.26508527942741,-4.72177922709091,-0.106973382376351));
#48041=CARTESIAN_POINT('Ctrl Pts',(2.05001543279104,-4.51147638686031,-0.0805160856918833));
#48042=CARTESIAN_POINT('Ctrl Pts',(3.5121928105948,-3.69213734276823,-0.0276014923229477));
#48043=CARTESIAN_POINT('Ctrl Pts',(4.85026808817394,-1.56206090154413,0.0517703977304561));
#48044=CARTESIAN_POINT('Ctrl Pts',(5.00665954563268,0.947775616877177,0.13114228778386));
#48045=CARTESIAN_POINT('Ctrl Pts',(3.94352649879584,3.22711800485082,0.210514177837264));
#48046=CARTESIAN_POINT('Ctrl Pts',(1.91971357759781,4.72014150668349,0.289886067890667));
#48047=CARTESIAN_POINT('Ctrl Pts',(-0.571713243107534,5.06345468357225,
0.369257957944071));
#48048=CARTESIAN_POINT('Ctrl Pts',(-2.92388473013463,4.17326556172555,0.448629847997474));
#48049=CARTESIAN_POINT('Ctrl Pts',(-4.56379761866667,2.26650781142313,0.528001738050878));
#48050=CARTESIAN_POINT('Ctrl Pts',(-5.091983083909,-0.192381913949067,0.607373628104282));
#48051=CARTESIAN_POINT('Ctrl Pts',(-4.37977084759389,-2.6043995219968,0.686745518157685));
#48052=CARTESIAN_POINT('Ctrl Pts',(-2.60065712992448,-4.3819955716546,0.766117408211089));
#48053=CARTESIAN_POINT('Ctrl Pts',(-0.188028560849166,-5.09214486895681,
0.845489298264494));
#48054=CARTESIAN_POINT('Ctrl Pts',(2.27040306822816,-4.56186018168567,0.924861188317896));
#48055=CARTESIAN_POINT('Ctrl Pts',(4.17576968427582,-2.92031579800744,1.0042330783713));
#48056=CARTESIAN_POINT('Ctrl Pts',(5.06392796926476,-0.567389296122094,
1.0836049684247));
#48057=CARTESIAN_POINT('Ctrl Pts',(4.71852465152963,1.92375216574099,1.16297685847811));
#48058=CARTESIAN_POINT('Ctrl Pts',(3.22369915083516,3.94627176108661,1.24234874853151));
#48059=CARTESIAN_POINT('Ctrl Pts',(0.943587684251177,5.00748834177841,1.32172063858492));
#48060=CARTESIAN_POINT('Ctrl Pts',(-1.5663796598258,4.84889181906687,1.40109252863832));
#48061=CARTESIAN_POINT('Ctrl Pts',(-3.69478038260539,3.50911599649364,1.48046441869172));
#48062=CARTESIAN_POINT('Ctrl Pts',(-4.92314078418047,1.3145272768326,1.55983630874512));
#48063=CARTESIAN_POINT('Ctrl Pts',(-4.9522349869947,-1.20027737376273,1.63920819879853));
#48064=CARTESIAN_POINT('Ctrl Pts',(-3.77497570905141,-3.4226971150208,1.71858008885193));
#48065=CARTESIAN_POINT('Ctrl Pts',(-1.67814070389166,-4.81135541393673,
1.79795197890534));
#48066=CARTESIAN_POINT('Ctrl Pts',(0.827485662097738,-5.02797818437314,
1.87732386895874));
#48067=CARTESIAN_POINT('Ctrl Pts',(3.13153835248109,-4.01979659801894,1.95669575901214));
#48068=CARTESIAN_POINT('Ctrl Pts',(4.6727552317042,-2.03240145822472,2.03606764906555));
#48069=CARTESIAN_POINT('Ctrl Pts',(5.07569927947279,0.450082178237972,2.11543953911895));
#48070=CARTESIAN_POINT('Ctrl Pts',(4.24221421762082,2.82292679227462,2.19481142917235));
#48071=CARTESIAN_POINT('Ctrl Pts',(2.37533516234403,4.50811268818069,2.27418331922576));
#48072=CARTESIAN_POINT('Ctrl Pts',(-0.0701702807675918,5.09513231177087,
2.35355520927916));
#48073=CARTESIAN_POINT('Ctrl Pts',(-2.49858239880191,4.44098898210475,2.43292709933257));
#48074=CARTESIAN_POINT('Ctrl Pts',(-4.31834537500726,2.70503056635658,2.51229898938597));
#48075=CARTESIAN_POINT('Ctrl Pts',(-5.08616897635574,0.310132692129504,
2.59167087943937));
#48076=CARTESIAN_POINT('Ctrl Pts',(-4.61501307310829,-2.16031281943427,
2.67104276949278));
#48077=CARTESIAN_POINT('Ctrl Pts',(-3.01965020040969,-4.10451090995464,
2.75041465954618));
#48078=CARTESIAN_POINT('Ctrl Pts',(-0.688707222773715,-5.04885922799114,
2.82978654959958));
#48079=CARTESIAN_POINT('Ctrl Pts',(1.8100033099024,-4.7633166135492,2.90915843965299));
#48080=CARTESIAN_POINT('Ctrl Pts',(3.86780104266064,-3.31744061546923,2.98853032970639));
#48081=CARTESIAN_POINT('Ctrl Pts',(4.98341100265916,-1.06344342649117,3.0679022197598));
#48082=CARTESIAN_POINT('Ctrl Pts',(4.88507307300304,1.44960622728803,3.1472741098132));
#48083=CARTESIAN_POINT('Ctrl Pts',(3.59674215568923,3.60953501274882,3.2266459998666));
#48084=CARTESIAN_POINT('Ctrl Pts',(1.43225281050325,4.89018905867422,3.30601788992001));
#48085=CARTESIAN_POINT('Ctrl Pts',(-1.0811301490835,4.97960387415649,3.38538977997341));
#48086=CARTESIAN_POINT('Ctrl Pts',(-3.3311521973945,3.85599820806045,3.46476167002682));
#48087=CARTESIAN_POINT('Ctrl Pts',(-4.76971294380054,1.79307991358813,3.54413356008021));
#48088=CARTESIAN_POINT('Ctrl Pts',(-5.04638217467727,-0.706628678919173,
3.62350545013362));
#48089=CARTESIAN_POINT('Ctrl Pts',(-4.09376387778011,-3.03420408933784,
3.70287734018702));
#48090=CARTESIAN_POINT('Ctrl Pts',(-2.14391376164834,-4.62265409969061,
3.78224923024043));
#48091=CARTESIAN_POINT('Ctrl Pts',(0.328189001348338,-5.08503580343006,
3.86162112029383));
#48092=CARTESIAN_POINT('Ctrl Pts',(2.72034565005059,-4.30871404098977,3.94099301034724));
#48093=CARTESIAN_POINT('Ctrl Pts',(4.44983211978348,-2.48279907534115,4.02036490040064));
#48094=CARTESIAN_POINT('Ctrl Pts',(5.09534933467345,-0.0520797505219637,
4.09973679045404));
#48095=CARTESIAN_POINT('Ctrl Pts',(4.49965073000142,2.39132608624781,4.17910868050745));
#48096=CARTESIAN_POINT('Ctrl Pts',(2.80784716730899,4.25221018151813,4.25848057056085));
#48097=CARTESIAN_POINT('Ctrl Pts',(0.432058249724383,5.07726528867822,4.33785246061425));
#48098=CARTESIAN_POINT('Ctrl Pts',(-2.04897910114838,4.66550980985238,4.41722435066766));
#48099=CARTESIAN_POINT('Ctrl Pts',(-4.03088967831969,3.1172464682773,4.49659624072106));
#48100=CARTESIAN_POINT('Ctrl Pts',(-5.0308844520753,0.809628786937908,4.57596813077447));
#48101=CARTESIAN_POINT('Ctrl Pts',(-4.80536690897923,-1.69521267481664,
4.65534002082787));
#48102=CARTESIAN_POINT('Ctrl Pts',(-3.40927262335505,-3.78710408127548,
4.73471191088127));
#48103=CARTESIAN_POINT('Ctrl Pts',(-1.18268707297853,-4.9564653161483,4.81408380093467));
#48104=CARTESIAN_POINT('Ctrl Pts',(1.33199843054213,-4.91844257095729,4.89345569098808));
#48105=CARTESIAN_POINT('Ctrl Pts',(3.52221206471124,-3.68229810226904,4.97282758104148));
#48106=CARTESIAN_POINT('Ctrl Pts',(4.85442263620086,-1.54915396649666,5.05219947109489));
#48107=CARTESIAN_POINT('Ctrl Pts',(5.00410659859419,0.961360646520152,5.13157136114829));
#48108=CARTESIAN_POINT('Ctrl Pts',(3.93480126997208,3.23768993398037,5.21094325120169));
#48109=CARTESIAN_POINT('Ctrl Pts',(1.90698706151963,4.72532512002807,5.2903151412551));
#48110=CARTESIAN_POINT('Ctrl Pts',(-0.585364974074726,5.06188156616668,
5.3696870313085));
#48111=CARTESIAN_POINT('Ctrl Pts',(-2.93512339766788,4.1653748670719,5.44905892136191));
#48112=CARTESIAN_POINT('Ctrl Pts',(-4.56989225837456,2.25419207025927,5.52843081141531));
#48113=CARTESIAN_POINT('Ctrl Pts',(-5.09144548022617,-0.206106925298976,
5.60780270146872));
#48114=CARTESIAN_POINT('Ctrl Pts',(-4.37273385281808,-2.61619873006436,
5.68717459152211));
#48115=CARTESIAN_POINT('Ctrl Pts',(-2.58883393774572,-4.38899031504372,
5.76654648157553));
#48116=CARTESIAN_POINT('Ctrl Pts',(-0.174299805725225,-5.09263357414371,
5.84591837162892));
#48117=CARTESIAN_POINT('Ctrl Pts',(2.28269337316386,-4.5557225669355,5.92529026168233));
#48118=CARTESIAN_POINT('Ctrl Pts',(4.18362749900631,-2.90904762634266,6.00466215173574));
#48119=CARTESIAN_POINT('Ctrl Pts',(5.0654392263932,-0.553735123040447,6.08403404178913));
#48120=CARTESIAN_POINT('Ctrl Pts',(4.71332117039027,1.9364660305625,6.16340593184254));
#48121=CARTESIAN_POINT('Ctrl Pts',(3.21304851003972,3.95494834541529,6.24277782189595));
#48122=CARTESIAN_POINT('Ctrl Pts',(0.93008434460575,5.01001399745458,6.32214971194934));
#48123=CARTESIAN_POINT('Ctrl Pts',(-1.57944630846742,4.84465132919185,6.40152160200275));
#48124=CARTESIAN_POINT('Ctrl Pts',(-3.70422733684302,3.49914232059178,6.48089349205615));
#48125=CARTESIAN_POINT('Ctrl Pts',(-4.92666678513181,1.30124998791572,6.56026538210956));
#48126=CARTESIAN_POINT('Ctrl Pts',(-4.94898110955443,-1.21362396154863,
6.63963727216295));
#48127=CARTESIAN_POINT('Ctrl Pts',(-3.76573459007348,-3.43286180029078,
6.71900916221637));
#48128=CARTESIAN_POINT('Ctrl Pts',(-1.66516345976277,-4.81586210299283,
6.79838105226976));
#48129=CARTESIAN_POINT('Ctrl Pts',(0.841037803569352,-5.02572905713577,
6.87775294232318));
#48130=CARTESIAN_POINT('Ctrl Pts',(3.14236411955759,-4.01133953722303,6.95712483237658));
#48131=CARTESIAN_POINT('Ctrl Pts',(4.6782174915266,-2.0197965849922,7.03649672242998));
#48132=CARTESIAN_POINT('Ctrl Pts',(5.0744674376185,0.463764344598802,7.11586861248339));
#48133=CARTESIAN_POINT('Ctrl Pts',(4.23458834804968,2.83435330637052,7.19524050253678));
#48134=CARTESIAN_POINT('Ctrl Pts',(2.36317290999828,4.51450007644499,7.2746123925902));
#48135=CARTESIAN_POINT('Ctrl Pts',(-0.0839062181341898,5.09492462057389,
7.35398428264359));
#48136=CARTESIAN_POINT('Ctrl Pts',(-2.51054597725242,4.43423680455535,7.433356172697));
#48137=CARTESIAN_POINT('Ctrl Pts',(-4.32562229331123,2.69337871796382,7.5127280627504));
#48138=CARTESIAN_POINT('Ctrl Pts',(-5.08698659332198,0.296419537368979,
7.5920999528038));
#48139=CARTESIAN_POINT('Ctrl Pts',(-4.60917221905333,-2.17274678641544,
7.67147184285721));
#48140=CARTESIAN_POINT('Ctrl Pts',(-3.00857369445294,-4.11263680232249,
7.75084373291061));
#48141=CARTESIAN_POINT('Ctrl Pts',(-0.675093277248738,-5.05069759635094,
7.83021562296402));
#48142=CARTESIAN_POINT('Ctrl Pts',(1.82283836799964,-4.7584196354378,7.90958751301742));
#48143=CARTESIAN_POINT('Ctrl Pts',(3.8767306215876,-3.30700118391521,7.98895940307083));
#48144=CARTESIAN_POINT('Ctrl Pts',(4.9862598767545,-1.05000456391383,8.06833129312422));
#48145=CARTESIAN_POINT('Ctrl Pts',(4.881147262843,1.46277084371127,8.14770318317763));
#48146=CARTESIAN_POINT('Ctrl Pts',(3.58699797993919,3.61921851159664,8.22707507323104));
#48147=CARTESIAN_POINT('Ctrl Pts',(1.41906392880751,4.89403256106139,8.30644696328444));
#48148=CARTESIAN_POINT('Ctrl Pts',(-1.09455095433695,4.97667111140887,8.38581885333784));
#48149=CARTESIAN_POINT('Ctrl Pts',(-3.34153564775234,3.84700359469183,8.46519074339125));
#48150=CARTESIAN_POINT('Ctrl Pts',(-4.77452965373897,1.7802145175059,8.54456263344465));
#48151=CARTESIAN_POINT('Ctrl Pts',(-5.04445880431694,-0.720230875706447,
8.62393452349805));
#48152=CARTESIAN_POINT('Ctrl Pts',(-4.08556895588349,-3.04522962180074,
8.70330641355146));
#48153=CARTESIAN_POINT('Ctrl Pts',(-2.1314435530503,-4.62841717252583,8.78267830360486));
#48154=CARTESIAN_POINT('Ctrl Pts',(0.341896781435676,-5.08413254485124,
8.86205019365827));
#48155=CARTESIAN_POINT('Ctrl Pts',(2.73195181673958,-4.30136448278739,8.94142208371167));
#48156=CARTESIAN_POINT('Ctrl Pts',(4.45650943655852,-2.47079355362535,9.02079397376506));
#48157=CARTESIAN_POINT('Ctrl Pts',(5.09547122194811,-0.0383427838088964,
9.10016586381848));
#48158=CARTESIAN_POINT('Ctrl Pts',(4.49318749630538,2.40344820327308,9.17953775387187));
#48159=CARTESIAN_POINT('Ctrl Pts',(2.79637324206448,4.25976452798008,9.25890964392529));
#48160=CARTESIAN_POINT('Ctrl Pts',(0.418368655723882,5.07841164249998,9.33828153397869));
#48161=CARTESIAN_POINT('Ctrl Pts',(-2.06154960910779,4.65996892178041,9.41765342403209));
#48162=CARTESIAN_POINT('Ctrl Pts',(-4.03927895232343,3.10636808638134,9.49702531408549));
#48163=CARTESIAN_POINT('Ctrl Pts',(-5.03304888354539,0.79606286096894,9.5763972041389));
#48164=CARTESIAN_POINT('Ctrl Pts',(-4.80077924720044,-1.70816151532024,
9.6557690941923));
#48165=CARTESIAN_POINT('Ctrl Pts',(-3.39905041258209,-3.7962815274288,9.7351409842457));
#48166=CARTESIAN_POINT('Ctrl Pts',(-1.16932042112922,-4.95963576238233,
9.81451287429911));
#48167=CARTESIAN_POINT('Ctrl Pts',(1.34525343666388,-4.91483370358709,9.89388476435251));
#48168=CARTESIAN_POINT('Ctrl Pts',(3.53212653495364,-3.67278903339792,9.97325665440591));
#48169=CARTESIAN_POINT('Ctrl Pts',(4.85858142755815,-1.53606108425365,10.0526285444593));
#48170=CARTESIAN_POINT('Ctrl Pts',(5.00149663869711,0.974847945001263,10.1320004345127));
#48171=CARTESIAN_POINT('Ctrl Pts',(3.92605833927446,3.24828617264322,10.2113723245661));
#48172=CARTESIAN_POINT('Ctrl Pts',(1.89424091858727,4.73044907858876,10.2907442146195));
#48173=CARTESIAN_POINT('Ctrl Pts',(-0.599009397036607,5.0602850596615,10.3701161046729));
#48174=CARTESIAN_POINT('Ctrl Pts',(-2.94634234942717,4.15744680095171,10.4494879947264));
#48175=CARTESIAN_POINT('Ctrl Pts',(-4.57595282711548,2.24186370388246,10.5288598847797));
#48176=CARTESIAN_POINT('Ctrl Pts',(-5.09087132481819,-0.219832429171425,
10.6082317748331));
#48177=CARTESIAN_POINT('Ctrl Pts',(-4.36566483624775,-2.62797786906995,
10.6876036648866));
#48178=CARTESIAN_POINT('Ctrl Pts',(-2.57699205680257,-4.39595371699339,
10.7669755549399));
#48179=CARTESIAN_POINT('Ctrl Pts',(-0.160569716395434,-5.09308496973576,
10.8463474449934));
#48180=CARTESIAN_POINT('Ctrl Pts',(2.2949670515106,-4.54955199720284,10.9257193350468));
#48181=CARTESIAN_POINT('Ctrl Pts',(4.19145492549203,-2.89775822841384,11.0050912251002));
#48182=CARTESIAN_POINT('Ctrl Pts',(5.06691365725173,-0.540076969262297,
11.0844631151535));
#48183=CARTESIAN_POINT('Ctrl Pts',(4.70808343752805,1.94916584416147,11.163835005207));
#48184=CARTESIAN_POINT('Ctrl Pts',(3.20237451358847,3.96359617235289,11.2432068952604));
#48185=CARTESIAN_POINT('Ctrl Pts',(0.916574246474504,5.01250324623051,11.3225787853138));
#48186=CARTESIAN_POINT('Ctrl Pts',(-1.59250147827797,4.84037562431409,11.4019506753672));
#48187=CARTESIAN_POINT('Ctrl Pts',(-3.71364736786416,3.4891432143045,11.4813225654206));
#48188=CARTESIAN_POINT('Ctrl Pts',(-4.93015697865768,1.28796324037784,11.560694455474));
#48189=CARTESIAN_POINT('Ctrl Pts',(-4.94569126216756,-1.22696172804661,
11.6400663455274));
#48190=CARTESIAN_POINT('Ctrl Pts',(-3.75646610131532,-3.44300153535262,
11.7194382355808));
#48191=CARTESIAN_POINT('Ctrl Pts',(-1.65217411297936,-4.82033378960134,
11.7988101256342));
#48192=CARTESIAN_POINT('Ctrl Pts',(0.854583832252985,-5.02344340233105,
11.8781820156876));
#48193=CARTESIAN_POINT('Ctrl Pts',(3.15316704753777,-4.00285332145629,11.957553905741));
#48194=CARTESIAN_POINT('Ctrl Pts',(4.6836457494592,-2.00717703164028,12.0369257957944));
#48195=CARTESIAN_POINT('Ctrl Pts',(5.07319871388639,0.477443140272258,12.1162976858478));
#48196=CARTESIAN_POINT('Ctrl Pts',(4.22693170094574,2.84575922001696,12.1956695759012));
#48197=CARTESIAN_POINT('Ctrl Pts',(2.35099348180933,4.52085465274672,12.2750414659546));
#48198=CARTESIAN_POINT('Ctrl Pts',(-0.0976415456600611,5.09467989880942,
12.354413356008));
#48199=CARTESIAN_POINT('Ctrl Pts',(-2.52249130873252,4.4274523984048,12.4337852460614));
#48200=CARTESIAN_POINT('Ctrl Pts',(-4.33286777243754,2.68170729374847,12.5131571361148));
#48201=CARTESIAN_POINT('Ctrl Pts',(-5.08776723741693,0.282704228193439,
12.5925290261682));
#48202=CARTESIAN_POINT('Ctrl Pts',(-4.60329786494335,-2.18516496159434,
12.6719009162216));
#48203=CARTESIAN_POINT('Ctrl Pts',(-2.99747532179655,-4.12073280351837,
12.751272806275));
#48204=CARTESIAN_POINT('Ctrl Pts',(-0.661474425059184,-5.05249925559264,
12.8306446963284));
#48205=CARTESIAN_POINT('Ctrl Pts',(1.83566017747378,-4.75348807252195,12.9100165863819));
#48206=CARTESIAN_POINT('Ctrl Pts',(3.885632023939,-3.29653771665232,12.9893884764353));
#48207=CARTESIAN_POINT('Ctrl Pts',(4.98907251007332,-1.03655806976862,13.0687603664887));
#48208=CARTESIAN_POINT('Ctrl Pts',(4.87718597587842,1.47592482852836,13.1481322565421));
#48209=CARTESIAN_POINT('Ctrl Pts',(3.5772277334276,3.62887570549998,13.2275041465955));
#48210=CARTESIAN_POINT('Ctrl Pts',(1.4058647331731,4.89784049299196,13.3068760366489));
#48211=CARTESIAN_POINT('Ctrl Pts',(-1.10796380425358,4.97370217757714,13.3862479267023));
#48212=CARTESIAN_POINT('Ctrl Pts',(-3.35189481140037,3.83798102080754,13.4656198167557));
#48213=CARTESIAN_POINT('Ctrl Pts',(-4.77931166178332,1.76733618259613,13.5449917068091));
#48214=CARTESIAN_POINT('Ctrl Pts',(-5.0424987701828,-0.733827837763376,
13.6243635968625));
#48215=CARTESIAN_POINT('Ctrl Pts',(-4.07734433954749,-3.0562330211441,13.7037354869159));
#48216=CARTESIAN_POINT('Ctrl Pts',(-2.11895785284703,-4.6341466054312,13.7831073769693));
#48217=CARTESIAN_POINT('Ctrl Pts',(0.355602076573349,-5.08319233414479,
13.8624792670227));
#48218=CARTESIAN_POINT('Ctrl Pts',(2.74353812725229,-4.29398366171607,13.9418511570761));
#48219=CARTESIAN_POINT('Ctrl Pts',(4.4631543628512,-2.45877007386494,14.0212230471295));
#48220=CARTESIAN_POINT('Ctrl Pts',(5.09555607468418,-0.024605538415575,
14.1005949371829));
#48221=CARTESIAN_POINT('Ctrl Pts',(4.48669160554615,2.41555285172843,14.1799668272363));
#48222=CARTESIAN_POINT('Ctrl Pts',(2.78487899242048,4.26728791392691,14.2593387172897));
#48223=CARTESIAN_POINT('Ctrl Pts',(0.404676020966283,5.07952108577437,14.3387106073431));
#48224=CARTESIAN_POINT('Ctrl Pts',(-2.07410513346011,4.65439416445642,14.4180824973965));
#48225=CARTESIAN_POINT('Ctrl Pts',(-4.0476388683295,3.09546712700361,14.4974543874499));
#48226=CARTESIAN_POINT('Ctrl Pts',(-5.03517673417046,0.782491149112972,
14.5768262775033));
#48227=CARTESIAN_POINT('Ctrl Pts',(-4.79615669274215,-1.72109794068678,
14.6561981675567));
#48228=CARTESIAN_POINT('Ctrl Pts',(-3.38880349707463,-3.80543138172091,
14.7355700576101));
#48229=CARTESIAN_POINT('Ctrl Pts',(-1.15594527050905,-4.96277016134733,
14.8149419476636));
#48230=CARTESIAN_POINT('Ctrl Pts',(1.35849866531108,-4.91118911457496,14.8943138377169));
#48231=CARTESIAN_POINT('Ctrl Pts',(3.54201533324722,-3.66325327022487,14.9736857277704));
#48232=CARTESIAN_POINT('Ctrl Pts',(4.86270490612231,-1.52295703772157,15.0530576178238));
#48233=CARTESIAN_POINT('Ctrl Pts',(4.99885032728073,0.988328158162469,15.1324295078772));
#48234=CARTESIAN_POINT('Ctrl Pts',(3.91728687348112,3.25885880234541,15.2118013979306));
#48235=CARTESIAN_POINT('Ctrl Pts',(1.8814810080689,4.73553865563863,15.291173287984));
#48236=CARTESIAN_POINT('Ctrl Pts',(-0.612649466321345,5.05865177435528,
15.3705451780374));
#48237=CARTESIAN_POINT('Ctrl Pts',(-2.95753988679226,4.14948851797474,15.4499170680908));
#48238=CARTESIAN_POINT('Ctrl Pts',(-4.58198013724412,2.22951904335266,15.5292889581442));
#48239=CARTESIAN_POINT('Ctrl Pts',(-5.09026016830427,-0.233556335273548,
15.6086608481976));
#48240=CARTESIAN_POINT('Ctrl Pts',(-4.35856408946536,-2.63973790759512,
15.688032738251));
#48241=CARTESIAN_POINT('Ctrl Pts',(-2.56513144595043,-4.40288516858759,
15.7674046283044));
#48242=CARTESIAN_POINT('Ctrl Pts',(-0.146838460024607,-5.09349934813251,
15.8467765183578));
#48243=CARTESIAN_POINT('Ctrl Pts',(2.3072240497427,-4.54334836074314,15.9261484084112));
#48244=CARTESIAN_POINT('Ctrl Pts',(4.19925188794477,-2.88644776920547,16.0055202984646));
#48245=CARTESIAN_POINT('Ctrl Pts',(5.06835126113318,-0.526414890137456,
16.084892188518));
#48246=CARTESIAN_POINT('Ctrl Pts',(4.70281148570858,1.96185149097663,16.1642640785714));
#48247=CARTESIAN_POINT('Ctrl Pts',(3.19167724187374,3.97221519135797,16.2436359686248));
#48248=CARTESIAN_POINT('Ctrl Pts',(0.90305748655408,5.01495606350291,16.3230078586782));
#48249=CARTESIAN_POINT('Ctrl Pts',(-1.60554507356452,4.83606473894038,16.4023797487316));
#48250=CARTESIAN_POINT('Ctrl Pts',(-3.72304040765551,3.47911874852373,16.481751638785));
#48251=CARTESIAN_POINT('Ctrl Pts',(-4.93361133910263,1.27466713166901,16.5611235288384));
#48252=CARTESIAN_POINT('Ctrl Pts',(-4.94236546898943,-1.24029057666156,
16.6404954188918));
#48253=CARTESIAN_POINT('Ctrl Pts',(-3.74717030983909,-3.45311624655429,
16.7198673089452));
#48254=CARTESIAN_POINT('Ctrl Pts',(-1.6391727584367,-4.82477044080732,16.7992391989986));
#48255=CARTESIAN_POINT('Ctrl Pts',(0.868123650569205,-5.02112123762451,
16.8786110890521));
#48256=CARTESIAN_POINT('Ctrl Pts',(3.16394705627606,-3.99433801030565,16.9579829791054));
#48257=CARTESIAN_POINT('Ctrl Pts',(4.68903996911093,-1.99454289389466,17.0373548691589));
#48258=CARTESIAN_POINT('Ctrl Pts',(5.07189311172224,0.491118473430398,17.1167267592122));
#48259=CARTESIAN_POINT('Ctrl Pts',(4.21924434286031,2.85714443596481,17.1960986492657));
#48260=CARTESIAN_POINT('Ctrl Pts',(2.33879694571596,4.52717639800277,17.275470539319));
#48261=CARTESIAN_POINT('Ctrl Pts',(-0.11137612465114,5.09439809707615,17.3548424293725));
#48262=CARTESIAN_POINT('Ctrl Pts',(-2.53441837980398,4.42063590960358,17.4342143194259));
#48263=CARTESIAN_POINT('Ctrl Pts',(-4.34008162116489,2.67001619606203,17.5135862094793));
#48264=CARTESIAN_POINT('Ctrl Pts',(-5.08851116459639,0.268987208843763,
17.5929580995327));
#48265=CARTESIAN_POINT('Ctrl Pts',(-4.59738955946409,-2.19756790530666,
17.6723299895861));
#48266=CARTESIAN_POINT('Ctrl Pts',(-2.98635609589589,-4.12879762624818,
17.7517018796395));
#48267=CARTESIAN_POINT('Ctrl Pts',(-0.647849003889666,-5.05426651218747,
17.8310737696929));
#48268=CARTESIAN_POINT('Ctrl Pts',(1.84846531944351,-4.7485175808327,17.9104456597463));
#48269=CARTESIAN_POINT('Ctrl Pts',(3.89451146459875,-3.28605855970652,17.9898175497997));
#48270=CARTESIAN_POINT('Ctrl Pts',(4.99183702504825,-1.02308842638974,18.0691894398531));
#48271=CARTESIAN_POINT('Ctrl Pts',(4.87321162956217,1.48903860109228,18.1485613299065));
#48272=CARTESIAN_POINT('Ctrl Pts',(3.5673892128293,3.63856219800459,18.2279332199599));
#48273=CARTESIAN_POINT('Ctrl Pts',(1.39273514199697,4.90150770362139,18.3073051100133));
#48274=CARTESIAN_POINT('Ctrl Pts',(-1.12151932172649,4.97089558679471,18.3866770000667));
#48275=CARTESIAN_POINT('Ctrl Pts',(-3.36194502775882,3.82855576883779,18.4660488901201));
#48276=CARTESIAN_POINT('Ctrl Pts',(-4.78459624359504,1.75515257798274,18.5454207801735));
#48277=CARTESIAN_POINT('Ctrl Pts',(-5.03948789886558,-0.748754766453475,
18.6247926702269));
#48278=CARTESIAN_POINT('Ctrl Pts',(-4.0710021077043,-3.06469899064074,18.7041645602803));
#48279=CARTESIAN_POINT('Ctrl Pts',(-2.10287077052062,-4.64454172754396,
18.7835364503337));
#48280=CARTESIAN_POINT('Ctrl Pts',(0.36273133865386,-5.07374792580598,18.8629083403871));
#48281=CARTESIAN_POINT('Ctrl Pts',(3.56709774791096,-4.04128406294332,18.968737527125));
#48282=CARTESIAN_POINT('Ctrl Pts',(5.77704085522352,-0.0189872057267309,
19.1010240105473));
#48283=CARTESIAN_POINT('Ctrl Pts',(3.14459942081972,4.8501664079131,19.2597677906541));
#48284=CARTESIAN_POINT('Ctrl Pts',(-2.36591519662263,5.26902047281295,19.418511570761));
#48285=CARTESIAN_POINT('Ctrl Pts',(-5.71123844601178,0.872727032859995,
19.5772553508678));
#48286=CARTESIAN_POINT('Ctrl Pts',(-3.83058845612596,-4.3254192567976,19.7359991309746));
#48287=CARTESIAN_POINT('Ctrl Pts',(1.55524717023751,-5.5639435857319,19.8947429110814));
#48288=CARTESIAN_POINT('Ctrl Pts',(5.51805139390222,-1.71188403765725,20.0534866911882));
#48289=CARTESIAN_POINT('Ctrl Pts',(4.43131449514919,3.70671199728542,20.212230471295));
#48290=CARTESIAN_POINT('Ctrl Pts',(-0.709818611660639,5.73400533709385,
20.3709742514018));
#48291=CARTESIAN_POINT('Ctrl Pts',(-5.20235975367858,2.51303602329798,20.5297180315086));
#48292=CARTESIAN_POINT('Ctrl Pts',(-4.93271294602024,-3.0047419943643,20.6884618116154));
#48293=CARTESIAN_POINT('Ctrl Pts',(-0.152720854580618,-5.77834717219765,
20.8472055917222));
#48294=CARTESIAN_POINT('Ctrl Pts',(4.77339715849037,-3.25411141853181,21.005949371829));
#48295=CARTESIAN_POINT('Ctrl Pts',(5.22808970274015,1.3127228499015,21.1382358552514));
#48296=CARTESIAN_POINT('Ctrl Pts',(3.1707451501151,3.97754537770267,21.2440650419892));
#48297=CARTESIAN_POINT('Ctrl Pts',(0.895150293052777,5.019216999618,21.3234369320426));
#48298=CARTESIAN_POINT('Ctrl Pts',(-1.62157688245131,4.83072732396133,21.402808822096));
#48299=CARTESIAN_POINT('Ctrl Pts',(-3.73081451079173,3.46959580775127,21.4821807121495));
#48300=CARTESIAN_POINT('Ctrl Pts',(-4.93787328845979,1.26108254025601,21.5615526022028));
#48301=CARTESIAN_POINT('Ctrl Pts',(-4.93855701420288,-1.25346250930809,
21.6409244922563));
#48302=CARTESIAN_POINT('Ctrl Pts',(-3.73808388472054,-3.46328419200818,
21.7202963823096));
#48303=CARTESIAN_POINT('Ctrl Pts',(-1.62603418385006,-4.82913054051807,
21.7996682723631));
#48304=CARTESIAN_POINT('Ctrl Pts',(0.881590795203928,-5.01878454751451,
21.8790401624164));
#48305=CARTESIAN_POINT('Ctrl Pts',(3.17473921804455,-3.98578203611947,21.9584120524699));
#48306=CARTESIAN_POINT('Ctrl Pts',(4.69438148876591,-1.98190041394297,22.0377839425233));
#48307=CARTESIAN_POINT('Ctrl Pts',(5.0705605156318,0.504793485523968,22.1171558325767));
#48308=CARTESIAN_POINT('Ctrl Pts',(4.21152107628908,2.86850718608746,22.1965277226301));
#48309=CARTESIAN_POINT('Ctrl Pts',(2.32658621700133,4.53346610033867,22.2758996126835));
#48310=CARTESIAN_POINT('Ctrl Pts',(-0.125111436169825,5.09407888617233,
22.3552715027369));
#48311=CARTESIAN_POINT('Ctrl Pts',(-2.54632610813663,4.41378735452051,22.4346433927903));
#48312=CARTESIAN_POINT('Ctrl Pts',(-4.34726461344783,2.6583059213356,22.5140152828437));
#48313=CARTESIAN_POINT('Ctrl Pts',(-5.08921736705482,0.255267617363269,
22.5933871728972));
#48314=CARTESIAN_POINT('Ctrl Pts',(-4.59144894277882,-2.20995361377114,
22.6727590629504));
#48315=CARTESIAN_POINT('Ctrl Pts',(-2.97521323819314,-4.13683487704257,
22.7521309530039));
#48316=CARTESIAN_POINT('Ctrl Pts',(-0.634222428965717,-5.05599240530685,
22.8315028430573));
#48317=CARTESIAN_POINT('Ctrl Pts',(1.8612636949988,-4.74352133023588,22.9108747331107));
#48318=CARTESIAN_POINT('Ctrl Pts',(3.90335003127195,-3.27553898237365,22.9902466231641));
#48319=CARTESIAN_POINT('Ctrl Pts',(4.99458897767401,-1.00964257616381,23.0696185132175));
#48320=CARTESIAN_POINT('Ctrl Pts',(4.86915708441603,1.5022005201609,23.1489904032709));
#48321=CARTESIAN_POINT('Ctrl Pts',(3.55760931370069,3.6481108983516,23.2283622933243));
#48322=CARTESIAN_POINT('Ctrl Pts',(1.37943578318338,4.90534953479997,23.3077341833777));
#48323=CARTESIAN_POINT('Ctrl Pts',(-1.13476524781216,4.96765588336336,23.3871060734311));
#48324=CARTESIAN_POINT('Ctrl Pts',(-3.37253997777701,3.81985225393738,23.4664779634845));
#48325=CARTESIAN_POINT('Ctrl Pts',(-4.78877143331127,1.74154107082816,23.545849853538));
#48326=CARTESIAN_POINT('Ctrl Pts',(-5.03846876789875,-0.76100566244534,
23.6252217435914));
#48327=CARTESIAN_POINT('Ctrl Pts',(-4.06080626285345,-3.07817310072711,
23.7045936336447));
#48328=CARTESIAN_POINT('Ctrl Pts',(-2.09394034074327,-4.64550438513341,
23.7839655236982));
#48329=CARTESIAN_POINT('Ctrl Pts',(0.383004813579298,-5.08120108394905,
23.8633374137515));
#48330=CARTESIAN_POINT('Ctrl Pts',(2.76665084304599,-4.27912844577405,23.942709303805));
#48331=CARTESIAN_POINT('Ctrl Pts',(4.47634685104287,-2.43466958989253,24.0220811938583));
#48332=CARTESIAN_POINT('Ctrl Pts',(5.0956146743416,0.00286938903386649,
24.1014530839118));
#48333=CARTESIAN_POINT('Ctrl Pts',(4.47360204192767,2.4397093911446,24.1808249739652));
#48334=CARTESIAN_POINT('Ctrl Pts',(2.76182985424755,4.28224158577674,24.2601968640186));
#48335=CARTESIAN_POINT('Ctrl Pts',(0.377282027280861,5.08162920869509,24.339568754072));
#48336=CARTESIAN_POINT('Ctrl Pts',(-2.09917086643256,4.64314320437055,24.4189406441253));
#48337=CARTESIAN_POINT('Ctrl Pts',(-4.06427038351852,3.07359779288466,24.4983125341788));
#48338=CARTESIAN_POINT('Ctrl Pts',(-5.03932263128953,0.755330762345285,
24.5776844242322));
#48339=CARTESIAN_POINT('Ctrl Pts',(-4.78680704042971,-1.74693317000509,
24.6570563142856));
#48340=CARTESIAN_POINT('Ctrl Pts',(-3.36823584993892,-3.82364804891321,
24.736428204339));
#48341=CARTESIAN_POINT('Ctrl Pts',(-1.12916986186658,-4.96893072660747,
24.8158000943924));
#48342=CARTESIAN_POINT('Ctrl Pts',(1.38495940518137,-4.90379287784174,24.8951719844458));
#48343=CARTESIAN_POINT('Ctrl Pts',(3.56171562668277,-3.64410193839515,24.9745438744992));
#48344=CARTESIAN_POINT('Ctrl Pts',(4.87084580524804,-1.49671583283838,25.0539157645526));
#48345=CARTESIAN_POINT('Ctrl Pts',(4.99344872708924,1.01526693667351,25.133287654606));
#48346=CARTESIAN_POINT('Ctrl Pts',(3.8996585918228,3.27993292766699,25.2126595446594));
#48347=CARTESIAN_POINT('Ctrl Pts',(1.85592025533624,4.7456145174892,25.2920314347128));
#48348=CARTESIAN_POINT('Ctrl Pts',(-0.639916147340462,5.05527491509063,
25.3714033247662));
#48349=CARTESIAN_POINT('Ctrl Pts',(-2.9798703929554,4.13348153303719,25.4507752148196));
#48350=CARTESIAN_POINT('Ctrl Pts',(-4.59393480667762,2.20478119884206,25.5301471048731));
#48351=CARTESIAN_POINT('Ctrl Pts',(-5.08892686999539,-0.260998955190596,
25.6095189949264));
#48352=CARTESIAN_POINT('Ctrl Pts',(-4.34426761193083,-2.66320034145021,
25.6888908849798));
#48353=CARTESIAN_POINT('Ctrl Pts',(-2.54135437947314,-4.41665201942651,
25.7682627750333));
#48354=CARTESIAN_POINT('Ctrl Pts',(-0.119372845368366,-5.09421704156391,
25.8476346650866));
#48355=CARTESIAN_POINT('Ctrl Pts',(2.33168764964084,-4.53084206823456,25.9270065551401));
#48356=CARTESIAN_POINT('Ctrl Pts',(4.21475419430065,-2.86376399593205,26.0063784451934));
#48357=CARTESIAN_POINT('Ctrl Pts',(5.07111594642898,-0.49907935305457,26.0857503352469));
#48358=CARTESIAN_POINT('Ctrl Pts',(4.69216507873193,1.98717991553359,26.1651222253003));
#48359=CARTESIAN_POINT('Ctrl Pts',(3.17021318378706,3.98936655524586,26.2444941153537));
#48360=CARTESIAN_POINT('Ctrl Pts',(0.876004374419533,5.01975233241337,26.3238660054071));
#48361=CARTESIAN_POINT('Ctrl Pts',(-1.63159716155383,4.82733755243831,26.4032378954604));
#48362=CARTESIAN_POINT('Ctrl Pts',(-3.74174524045176,3.4589940298197,26.4826097855139));
#48363=CARTESIAN_POINT('Ctrl Pts',(-4.94041246098821,1.2480472178904,26.5619816755672));
#48364=CARTESIAN_POINT('Ctrl Pts',(-4.93560614144543,-1.26692113381128,
26.6413535656207));
#48365=CARTESIAN_POINT('Ctrl Pts',(-3.72849709062547,-3.4732703015989,26.7207254556741));
#48366=CARTESIAN_POINT('Ctrl Pts',(-1.61313440141745,-4.8335385118705,26.8000973457275));
#48367=CARTESIAN_POINT('Ctrl Pts',(0.895184257363441,-5.01636743950643,
26.8794692357809));
#48368=CARTESIAN_POINT('Ctrl Pts',(3.18543801250735,-3.97722036241957,26.9588411258343));
#48369=CARTESIAN_POINT('Ctrl Pts',(4.69972611865188,-1.96923120847525,27.0382130158877));
#48370=CARTESIAN_POINT('Ctrl Pts',(5.06917134496014,0.51845830903431,27.1175849059411));
#48371=CARTESIAN_POINT('Ctrl Pts',(4.20377765205651,2.8798525300511,27.1969567959945));
#48372=CARTESIAN_POINT('Ctrl Pts',(2.31435302801598,4.53972104919287,27.2763286860479));
#48373=CARTESIAN_POINT('Ctrl Pts',(-0.138842870915707,5.09372356925338,
27.3557005761014));
#48374=CARTESIAN_POINT('Ctrl Pts',(-2.5582169538158,4.40690630260968,27.4350724661547));
#48375=CARTESIAN_POINT('Ctrl Pts',(-4.35441504928357,2.64657641517193,27.5144443562082));
#48376=CARTESIAN_POINT('Ctrl Pts',(-5.08988727708012,0.241546371095803,
27.5938162462615));
#48377=CARTESIAN_POINT('Ctrl Pts',(-4.58547423045432,-2.22232383432546,
27.6731881363149));
#48378=CARTESIAN_POINT('Ctrl Pts',(-2.96404981106488,-4.14484087273538,
27.7525600263683));
#48379=CARTESIAN_POINT('Ctrl Pts',(-0.620589418513009,-5.05768384899663,
27.8319319164217));
#48380=CARTESIAN_POINT('Ctrl Pts',(1.87404518273727,-4.73848623463559,27.9113038064751));
#48381=CARTESIAN_POINT('Ctrl Pts',(3.91216652560138,-3.26500386197866,27.9906756965286));
#48382=CARTESIAN_POINT('Ctrl Pts',(4.9972927622627,-0.99617377550726,28.0700475865819));
#48383=CARTESIAN_POINT('Ctrl Pts',(4.86508954335677,1.51532203768447,28.1494194766354));
#48384=CARTESIAN_POINT('Ctrl Pts',(3.54776128038217,3.65768875660473,28.2287913666887));
#48385=CARTESIAN_POINT('Ctrl Pts',(1.36620622234286,4.90905059057282,28.3081632567422));
#48386=CARTESIAN_POINT('Ctrl Pts',(-1.148153647413,4.96457856667651,28.3875351467955));
#48387=CARTESIAN_POINT('Ctrl Pts',(-3.382825830054,3.81074619284609,28.466907036849));
#48388=CARTESIAN_POINT('Ctrl Pts',(-4.79344912825184,1.72862448138202,28.5462789269024));
#48389=CARTESIAN_POINT('Ctrl Pts',(-5.03639882892723,-0.774586327501372,
28.6256508169557));
#48390=CARTESIAN_POINT('Ctrl Pts',(-4.05249292275565,-3.08910962152317,
28.7050227070092));
#48391=CARTESIAN_POINT('Ctrl Pts',(-2.0814087106417,-4.65113264937009,28.7843945970626));
#48392=CARTESIAN_POINT('Ctrl Pts',(0.39670205626447,-5.08015005893792,28.863766487116));
#48393=CARTESIAN_POINT('Ctrl Pts',(2.77817708034974,-4.27165415886996,28.9431383771694));
#48394=CARTESIAN_POINT('Ctrl Pts',(4.48289431705251,-2.42259276084734,29.0225102672228));
#48395=CARTESIAN_POINT('Ctrl Pts',(5.09558842083954,0.016606871399571,29.1018821572762));
#48396=CARTESIAN_POINT('Ctrl Pts',(4.46700846420369,2.45176110653224,29.1812540473296));
#48397=CARTESIAN_POINT('Ctrl Pts',(2.75027513324334,4.28967176299481,29.260625937383));
#48398=CARTESIAN_POINT('Ctrl Pts',(0.363580867455653,5.08262787301922,29.3399978274364));
#48399=CARTESIAN_POINT('Ctrl Pts',(-2.11168089287163,4.6374670833821,29.4193697174898));
#48400=CARTESIAN_POINT('Ctrl Pts',(-4.07254186182172,3.0626295770924,29.4987416075432));
#48401=CARTESIAN_POINT('Ctrl Pts',(-5.04134064765058,0.741742284838609,
29.5781134975966));
#48402=CARTESIAN_POINT('Ctrl Pts',(-4.78208001053002,-1.75983178618322,
29.6574853876501));
#48403=CARTESIAN_POINT('Ctrl Pts',(-3.35791526779889,-3.8327147294124,29.7368572777034));
#48404=CARTESIAN_POINT('Ctrl Pts',(-1.11576979845131,-4.97195684812685,
29.8162291677569));
#48405=CARTESIAN_POINT('Ctrl Pts',(1.3981747240844,-4.90004128387741,29.8956010578102));
#48406=CARTESIAN_POINT('Ctrl Pts',(3.57152697864042,-3.63448650893289,29.9749729478637));
#48407=CARTESIAN_POINT('Ctrl Pts',(4.87486316664055,-1.48357886521172,30.054344837917));
#48408=CARTESIAN_POINT('Ctrl Pts',(4.99069347757362,1.02872530622892,30.1337167279705));
#48409=CARTESIAN_POINT('Ctrl Pts',(3.89080190408237,3.29043427011703,30.2130886180238));
#48410=CARTESIAN_POINT('Ctrl Pts',(1.84311959890063,4.75060072905731,30.2924605080773));
#48411=CARTESIAN_POINT('Ctrl Pts',(-0.653542560897256,5.05353136567563,
30.3718323981307));
#48412=CARTESIAN_POINT('Ctrl Pts',(-2.99100319945254,4.12543294741732,30.4512042881841));
#48413=CARTESIAN_POINT('Ctrl Pts',(-4.59986207909447,2.19238819465906,30.5305761782375));
#48414=CARTESIAN_POINT('Ctrl Pts',(-5.08820473789096,-0.274717469549192,
30.6099480682909));
#48415=CARTESIAN_POINT('Ctrl Pts',(-4.33707198508738,-2.67490256625206,
30.6893199583443));
#48416=CARTESIAN_POINT('Ctrl Pts',(-2.52943809666249,-4.42348731861233,
30.7686918483976));
#48417=CARTESIAN_POINT('Ctrl Pts',(-0.10563868670687,-5.09452035138171,
30.8480637384511));
#48418=CARTESIAN_POINT('Ctrl Pts',(2.34389407350322,-4.52453950308404,30.9274356285044));
#48419=CARTESIAN_POINT('Ctrl Pts',(4.22245942552948,-2.85239084673345,31.006807518558));
#48420=CARTESIAN_POINT('Ctrl Pts',(5.07244300775219,-0.485406093778655,
31.0861794086112));
#48421=CARTESIAN_POINT('Ctrl Pts',(4.68679070094865,1.99982250919246,31.1655512986648));
#48422=CARTESIAN_POINT('Ctrl Pts',(3.15944655342927,3.99789877545637,31.2449231887181));
#48423=CARTESIAN_POINT('Ctrl Pts',(0.862468218810821,5.02209574921795,31.3242950787715));
#48424=CARTESIAN_POINT('Ctrl Pts',(-1.64460546486892,4.82292131469039,31.4036669688249));
#48425=CARTESIAN_POINT('Ctrl Pts',(-3.75105689757904,3.44889392325951,31.4830388588783));
#48426=CARTESIAN_POINT('Ctrl Pts',(-4.94375917286251,1.23472360611981,31.5624107489317));
#48427=CARTESIAN_POINT('Ctrl Pts',(-4.93217265646195,-1.28022264845634,
31.6417826389851));
#48428=CARTESIAN_POINT('Ctrl Pts',(-3.7191197981263,-3.48330949959324,31.7211545290385));
#48429=CARTESIAN_POINT('Ctrl Pts',(-1.60009758909914,-4.83786986680406,
31.8005264190919));
#48430=CARTESIAN_POINT('Ctrl Pts',(0.908704850876668,-5.01393584290474,
31.8798983091453));
#48431=CARTESIAN_POINT('Ctrl Pts',(3.196148800563,-3.96861814583255,31.9592701991988));
#48432=CARTESIAN_POINT('Ctrl Pts',(4.70501797698753,-1.9565538528228,32.0386420892521));
#48433=CARTESIAN_POINT('Ctrl Pts',(5.06775518859854,0.532122627976042,32.1180139793055));
#48434=CARTESIAN_POINT('Ctrl Pts',(4.19599845355282,2.89117521443338,32.1973858693589));
#48435=CARTESIAN_POINT('Ctrl Pts',(2.30210578290666,4.54594391816259,32.2767577594124));
#48436=CARTESIAN_POINT('Ctrl Pts',(-0.152574760830862,5.09333074570355,
32.3561296494657));
#48437=CARTESIAN_POINT('Ctrl Pts',(-2.57008843054848,4.39999347748749,32.4355015395192));
#48438=CARTESIAN_POINT('Ctrl Pts',(-4.3615342473787,2.63482753737587,32.5148734295725));
#48439=CARTESIAN_POINT('Ctrl Pts',(-5.09051997563981,0.227823441251348,
32.594245319626));
#48440=CARTESIAN_POINT('Ctrl Pts',(-4.57946630550992,-2.23467794088343,
32.6736172096794));
#48441=CARTESIAN_POINT('Ctrl Pts',(-2.95286477983452,-4.1528167229947,32.7529890997328));
#48442=CARTESIAN_POINT('Ctrl Pts',(-0.60695192984675,-5.05933854348835,
32.8323609897862));
#48443=CARTESIAN_POINT('Ctrl Pts',(1.88681306678638,-4.73341669344416,32.9117328798396));
#48444=CARTESIAN_POINT('Ctrl Pts',(3.92095457674023,-3.25444501411708,32.991104769893));
#48445=CARTESIAN_POINT('Ctrl Pts',(4.99996023068588,-0.982697732942914,
33.0704766599464));
#48446=CARTESIAN_POINT('Ctrl Pts',(4.8609866396607,1.52843254081155,33.1498485499997));
#48447=CARTESIAN_POINT('Ctrl Pts',(3.53788746282564,3.66724003075238,33.2292204400532));
#48448=CARTESIAN_POINT('Ctrl Pts',(1.35296673102733,4.91271596650007,33.3085923301066));
#48449=CARTESIAN_POINT('Ctrl Pts',(-1.16153370170815,4.96146516692072,33.38796422016));
#48450=CARTESIAN_POINT('Ctrl Pts',(-3.39308709571883,3.80161243469636,33.4673361102134));
#48451=CARTESIAN_POINT('Ctrl Pts',(-4.79809198368328,1.71569532810634,33.5467080002668));
#48452=CARTESIAN_POINT('Ctrl Pts',(-5.03429228481892,-0.788161362783202,
33.6260798903202));
#48453=CARTESIAN_POINT('Ctrl Pts',(-4.04415012858963,-3.10002369026433,
33.7054517803737));
#48454=CARTESIAN_POINT('Ctrl Pts',(-2.06886195261037,-4.65672710858312,
33.784823670427));
#48455=CARTESIAN_POINT('Ctrl Pts',(0.41039641567654,-5.07906211074165,33.8641955604805));
#48456=CARTESIAN_POINT('Ctrl Pts',(2.78968312550164,-4.26414882503682,33.9435674505338));
#48457=CARTESIAN_POINT('Ctrl Pts',(4.48940920081343,-2.41049832408638,34.0229393405872));
#48458=CARTESIAN_POINT('Ctrl Pts',(5.09552513194581,0.0303442330639926,
34.1023112306406));
#48459=CARTESIAN_POINT('Ctrl Pts',(4.46038241968974,2.46379500220581,34.181683120694));
#48460=CARTESIAN_POINT('Ctrl Pts',(2.73870042288625,4.29707076232801,34.2610550107475));
#48461=CARTESIAN_POINT('Ctrl Pts',(0.349877065078239,5.0835895961519,34.3404269008008));
#48462=CARTESIAN_POINT('Ctrl Pts',(-2.1241755713431,4.63175725668789,34.4197987908543));
#48463=CARTESIAN_POINT('Ctrl Pts',(-4.08078374036812,3.05163910171546,34.4991706809076));
#48464=CARTESIAN_POINT('Ctrl Pts',(-5.04332202290104,0.728148416253786,
34.5785425709611));
#48465=CARTESIAN_POINT('Ctrl Pts',(-4.77731822385925,-1.77271761167814,
34.6579144610144));
#48466=CARTESIAN_POINT('Ctrl Pts',(-3.3475702798999,-3.84175355324914,34.7372863510679));
#48467=CARTESIAN_POINT('Ctrl Pts',(-1.10236162547809,-4.97494683282594,
34.8166582411212));
#48468=CARTESIAN_POINT('Ctrl Pts',(1.41137988087415,-4.8962540757844,34.8960301311747));
#48469=CARTESIAN_POINT('Ctrl Pts',(3.58131237228184,-3.62484466355631,34.9754020212281));
#48470=CARTESIAN_POINT('Ctrl Pts',(4.87884509690211,-1.47043111474347,35.0547739112815));
#48471=CARTESIAN_POINT('Ctrl Pts',(4.98790195505749,1.04217619887681,35.1341458013349));
#48472=CARTESIAN_POINT('Ctrl Pts',(3.88191693749454,3.3009116972686,35.2135176913883));
#48473=CARTESIAN_POINT('Ctrl Pts',(1.8303055464353,4.75555241264984,35.2928895814417));
#48474=CARTESIAN_POINT('Ctrl Pts',(-0.667164224422912,5.05175108654629,
35.3722614714951));
#48475=CARTESIAN_POINT('Ctrl Pts',(-3.00211426695468,4.11735437762148,35.4516333615485));
#48476=CARTESIAN_POINT('Ctrl Pts',(-4.60575591912355,2.17997925591738,35.5310052516019));
#48477=CARTESIAN_POINT('Ctrl Pts',(-5.08744562406171,-0.288433987225976,
35.6103771416553));
#48478=CARTESIAN_POINT('Ctrl Pts',(-4.32984483584829,-2.68658534951887,
35.6897490317088));
#48479=CARTESIAN_POINT('Ctrl Pts',(-2.51750342957125,-4.43029046732475,
35.7691209217621));
#48480=CARTESIAN_POINT('Ctrl Pts',(-0.0919037602499935,-5.09478663357195,
35.8484928118156));
#48481=CARTESIAN_POINT('Ctrl Pts',(2.35608346164268,-4.51820405299999,35.9278647018689));
#48482=CARTESIAN_POINT('Ctrl Pts',(4.23013396738149,-2.84099696599223,36.0072365919223));
#48483=CARTESIAN_POINT('Ctrl Pts',(5.07373320190884,-0.471729306508876,
36.0866084819757));
#48484=CARTESIAN_POINT('Ctrl Pts',(4.68138225896918,2.01245056788487,36.1659803720291));
#48485=CARTESIAN_POINT('Ctrl Pts',(3.14865695980852,4.00640193842567,36.2453522620825));
#48486=CARTESIAN_POINT('Ctrl Pts',(0.84892579467244,5.02440266478627,36.3247241521359));
#48487=CARTESIAN_POINT('Ctrl Pts',(-1.65760181498048,4.81847002333159,36.4040960421893));
#48488=CARTESIAN_POINT('Ctrl Pts',(-3.76034129154353,3.43876874969578,36.4834679322427));
#48489=CARTESIAN_POINT('Ctrl Pts',(-4.94706995286084,1.22139102021962,36.5628398222961));
#48490=CARTESIAN_POINT('Ctrl Pts',(-4.92870332381484,-1.2935148582789,36.6422117123495));
#48491=CARTESIAN_POINT('Ctrl Pts',(-3.70971547458727,-3.49332338044723,
36.721583602403));
#48492=CARTESIAN_POINT('Ctrl Pts',(-1.58704914706622,-4.84216605947875,
36.8009554924563));
#48493=CARTESIAN_POINT('Ctrl Pts',(0.922218839806455,-5.01146780437405,
36.8803273825098));
#48494=CARTESIAN_POINT('Ctrl Pts',(3.20683635859905,-3.95998708481968,36.9596992725631));
#48495=CARTESIAN_POINT('Ctrl Pts',(4.71027563864883,-1.94386227668601,37.0390711626166));
#48496=CARTESIAN_POINT('Ctrl Pts',(5.06630219914206,0.545783079382256,37.1184430526699));
#48497=CARTESIAN_POINT('Ctrl Pts',(4.18818875799396,2.90247688538333,37.1978149427234));
#48498=CARTESIAN_POINT('Ctrl Pts',(2.28984180579711,4.55213374662869,37.2771868327768));
#48499=CARTESIAN_POINT('Ctrl Pts',(-0.1663055418131,5.0929009031723,37.3565587228302));
#48500=CARTESIAN_POINT('Ctrl Pts',(-2.58194122754862,4.39304867264833,37.4359306128836));
#48501=CARTESIAN_POINT('Ctrl Pts',(-4.36862174528344,2.62305950931498,37.515302502937));
#48502=CARTESIAN_POINT('Ctrl Pts',(-5.09111567564704,0.214098855557291,
37.5946743929904));
#48503=CARTESIAN_POINT('Ctrl Pts',(-4.57342509641719,-2.24701580551625,
37.6740462830439));
#48504=CARTESIAN_POINT('Ctrl Pts',(-2.94165828680345,-4.16076239004767,
37.7534181730971));
#48505=CARTESIAN_POINT('Ctrl Pts',(-0.593310029777194,-5.06095646606148,
37.8327900631507));
#48506=CARTESIAN_POINT('Ctrl Pts',(1.89956723723832,-4.72831274916718,37.912161953204));
#48507=CARTESIAN_POINT('Ctrl Pts',(3.92971412987383,-3.2438625125424,37.9915338432574));
#48508=CARTESIAN_POINT('Ctrl Pts',(5.00259135876467,-0.969214547985126,
38.0709057333108));
#48509=CARTESIAN_POINT('Ctrl Pts',(4.85684840567486,1.54153193505625,38.1502776233642));
#48510=CARTESIAN_POINT('Ctrl Pts',(3.52798793147795,3.67676465100168,38.2296495134176));
#48511=CARTESIAN_POINT('Ctrl Pts',(1.3397174061215,4.91634563604017,38.309021403471));
#48512=CARTESIAN_POINT('Ctrl Pts',(-1.17490531372475,4.95831570685867,38.3883932935245));
#48513=CARTESIAN_POINT('Ctrl Pts',(-3.40332370018554,3.79245104545026,38.4677651835778));
#48514=CARTESIAN_POINT('Ctrl Pts',(-4.80269996560014,1.70275370586069,38.5471370736313));
#48515=CARTESIAN_POINT('Ctrl Pts',(-5.03214915152033,-0.801730671351773,
38.6265089636846));
#48516=CARTESIAN_POINT('Ctrl Pts',(-4.03577793971505,-3.11091522434137,
38.705880853738));
#48517=CARTESIAN_POINT('Ctrl Pts',(-2.05630016029208,-4.6622877283261,38.7852527437914));
#48518=CARTESIAN_POINT('Ctrl Pts',(0.424087796933226,-5.0779372355256,38.8646246338449));
#48519=CARTESIAN_POINT('Ctrl Pts',(2.80116888608276,-4.2566125209993,38.9439965238982));
#48520=CARTESIAN_POINT('Ctrl Pts',(4.49589147158116,-2.39838632564053,39.0233684139517));
#48521=CARTESIAN_POINT('Ctrl Pts',(5.09542477676094,0.0440812951169324,
39.1027403040051));
#48522=CARTESIAN_POINT('Ctrl Pts',(4.45372401575944,2.47581113999364,39.1821121940585));
#48523=CARTESIAN_POINT('Ctrl Pts',(2.72710569549243,4.30443824810521,39.2614840841118));
#48524=CARTESIAN_POINT('Ctrl Pts',(0.336170930870647,5.08451490337722,39.3408559741653));
#48525=CARTESIAN_POINT('Ctrl Pts',(-2.1366552096739,4.62601276074587,39.4202278642187));
#48526=CARTESIAN_POINT('Ctrl Pts',(-4.08899520654064,3.04062834435872,39.4995997542721));
#48527=CARTESIAN_POINT('Ctrl Pts',(-5.04526816392185,0.714545672092809,
39.5789716443255));
#48528=CARTESIAN_POINT('Ctrl Pts',(-4.77251903131803,-1.78558378675053,
39.6583435343789));
#48529=CARTESIAN_POINT('Ctrl Pts',(-3.33720602914116,-3.85077723115716,
39.7377154244323));
#48530=CARTESIAN_POINT('Ctrl Pts',(-1.08893586889047,-4.97787652885981,
39.8170873144857));
#48531=CARTESIAN_POINT('Ctrl Pts',(1.42455668503583,-4.8924768895782,39.8964592045391));
#48532=CARTESIAN_POINT('Ctrl Pts',(3.59110607910284,-3.61508997874913,39.9758310945925));
#48533=CARTESIAN_POINT('Ctrl Pts',(4.88272528059762,-1.45743906270703,40.0552029846459));
#48534=CARTESIAN_POINT('Ctrl Pts',(4.98521092249161,1.05595859527154,40.1345748746994));
#48535=CARTESIAN_POINT('Ctrl Pts',(4.2435173595031,2.5590120913109,40.1874894680683));
#48536=CARTESIAN_POINT('Ctrl Pts',(3.71544298812202,3.17665283523806,40.2139467647527));
#48537=CARTESIAN_POINT('Ctrl Pts',(1.21713437249832,-4.5428082122986,-0.213946764752702));
#48538=CARTESIAN_POINT('Ctrl Pts',(1.97231308274437,-4.34047654372165,-0.187489468068234));
#48539=CARTESIAN_POINT('Ctrl Pts',(3.37906911267772,-3.55219315325666,-0.134574874699299));
#48540=CARTESIAN_POINT('Ctrl Pts',(4.66642692152752,-1.5028536385038,-0.055202984645895));
#48541=CARTESIAN_POINT('Ctrl Pts',(4.81689062664967,0.911851793295018,0.0241689054075086));
#48542=CARTESIAN_POINT('Ctrl Pts',(3.79405383067521,3.10479958283122,0.103540795460912));
#48543=CARTESIAN_POINT('Ctrl Pts',(1.84695009786499,4.54123256689918,0.182912685514316));
#48544=CARTESIAN_POINT('Ctrl Pts',(-0.550043424514128,4.8715330414348,0.26228457556772));
#48545=CARTESIAN_POINT('Ctrl Pts',(-2.81305984991034,4.01508502497055,0.341656465621123));
#48546=CARTESIAN_POINT('Ctrl Pts',(-4.39081462818011,2.18059968579164,0.421028355674527));
#48547=CARTESIAN_POINT('Ctrl Pts',(-4.89898012125377,-0.18509000454136,
0.500400245727931));
#48548=CARTESIAN_POINT('Ctrl Pts',(-4.21376307902768,-2.5056841854766,0.579772135781334));
#48549=CARTESIAN_POINT('Ctrl Pts',(-2.50208364241389,-4.21590347870479,
0.659144025834738));
#48550=CARTESIAN_POINT('Ctrl Pts',(-0.180901657890204,-4.89913577411436,
0.738515915888141));
#48551=CARTESIAN_POINT('Ctrl Pts',(2.18434729950923,-4.38895062645432,0.817887805941546));
#48552=CARTESIAN_POINT('Ctrl Pts',(4.01749423301245,-2.8096261920884,0.897259695994948));
#48553=CARTESIAN_POINT('Ctrl Pts',(4.87198838803769,-0.545883369388664,
0.976631586048353));
#48554=CARTESIAN_POINT('Ctrl Pts',(4.53967699589134,1.85083561019003,1.05600347610176));
#48555=CARTESIAN_POINT('Ctrl Pts',(3.10151031466513,3.79669503846566,1.13537536615516));
#48556=CARTESIAN_POINT('Ctrl Pts',(0.907822597135906,4.81768800868641,1.21474725620856));
#48557=CARTESIAN_POINT('Ctrl Pts',(-1.50700870159448,4.66510281756135,1.29411914626197));
#48558=CARTESIAN_POINT('Ctrl Pts',(-3.55473601316185,3.37610891998462,1.37349103631537));
#48559=CARTESIAN_POINT('Ctrl Pts',(-4.73653750187219,1.26470235504102,1.45286292636877));
#48560=CARTESIAN_POINT('Ctrl Pts',(-4.76452893838759,-1.15478290032736,
1.53223481642218));
#48561=CARTESIAN_POINT('Ctrl Pts',(-3.63189167208734,-3.29296559930584,
1.61160670647558));
#48562=CARTESIAN_POINT('Ctrl Pts',(-1.61453363327375,-4.62898916605748,
1.69097859652899));
#48563=CARTESIAN_POINT('Ctrl Pts',(0.796121224764031,-4.8374012186294,1.77035048658239));
#48564=CARTESIAN_POINT('Ctrl Pts',(3.01284271470348,-3.86743304144296,1.8497223766358));
#48565=CARTESIAN_POINT('Ctrl Pts',(4.49564238811846,-1.95536673594104,1.92909426668919));
#48566=CARTESIAN_POINT('Ctrl Pts',(4.88331352674298,0.433022578391154,2.0084661567426));
#48567=CARTESIAN_POINT('Ctrl Pts',(4.08142029927371,2.71592855106099,2.087838046796));
#48568=CARTESIAN_POINT('Ctrl Pts',(2.28530212097744,4.33724034032234,2.16720993684941));
#48569=CARTESIAN_POINT('Ctrl Pts',(-0.067510595561391,4.90200998298708,
2.24658182690281));
#48570=CARTESIAN_POINT('Ctrl Pts',(-2.4038778804521,4.27266084421796,2.32595371695622));
#48571=CARTESIAN_POINT('Ctrl Pts',(-4.15466583455893,2.60250098116813,2.40532560700962));
#48572=CARTESIAN_POINT('Ctrl Pts',(-4.8933863875636,0.298377639645852,2.48469749706302));
#48573=CARTESIAN_POINT('Ctrl Pts',(-4.44008884788507,-2.07842983444745,
2.56406938711643));
#48574=CARTESIAN_POINT('Ctrl Pts',(-2.90519549283157,-3.94893640139523,
2.64344127716983));
#48575=CARTESIAN_POINT('Ctrl Pts',(-0.662602946265526,-4.85749080178588,
2.72281316722323));
#48576=CARTESIAN_POINT('Ctrl Pts',(1.7413982113641,-4.58277119473486,2.80218505727664));
#48577=CARTESIAN_POINT('Ctrl Pts',(3.72119861922498,-3.19169866843848,2.88155694733003));
#48578=CARTESIAN_POINT('Ctrl Pts',(4.79452328017608,-1.02313541121562,2.96092883738345));
#48579=CARTESIAN_POINT('Ctrl Pts',(4.69991268257356,1.39466136750753,3.04030072743684));
#48580=CARTESIAN_POINT('Ctrl Pts',(3.46041375857639,3.47272172413642,3.11967261749026));
#48581=CARTESIAN_POINT('Ctrl Pts',(1.37796570248595,4.70483475550482,3.19904450754365));
#48582=CARTESIAN_POINT('Ctrl Pts',(-1.04015174865471,4.79086045440737,3.27841639759706));
#48583=CARTESIAN_POINT('Ctrl Pts',(-3.20489053615995,3.70984315100601,3.35778828765046));
#48584=CARTESIAN_POINT('Ctrl Pts',(-4.5889250829615,1.72511626761812,3.43716017770387));
#48585=CARTESIAN_POINT('Ctrl Pts',(-4.85510763696699,-0.679845120081458,
3.51653206775727));
#48586=CARTESIAN_POINT('Ctrl Pts',(-3.9385967172058,-2.91919774134084,3.59590395781068));
#48587=CARTESIAN_POINT('Ctrl Pts',(-2.06265235506924,-4.44744025434419,
3.67527584786408));
#48588=CARTESIAN_POINT('Ctrl Pts',(0.315749555158651,-4.89229616563132,
3.75464773791748));
#48589=CARTESIAN_POINT('Ctrl Pts',(2.61723557264967,-4.14539955988454,3.83401962797088));
#48590=CARTESIAN_POINT('Ctrl Pts',(4.2811687977959,-2.38869279703619,3.91339151802429));
#48591=CARTESIAN_POINT('Ctrl Pts',(4.90221878000547,-0.0501057561116431,
3.99276340807769));
#48592=CARTESIAN_POINT('Ctrl Pts',(4.32909911828292,2.3006869360945,4.0721352981311));
#48593=CARTESIAN_POINT('Ctrl Pts',(2.701420493645,4.09103738315217,4.1515071881845));
#48594=CARTESIAN_POINT('Ctrl Pts',(0.415681816248014,4.88482017903163,4.2308790782379));
#48595=CARTESIAN_POINT('Ctrl Pts',(-1.97131603149091,4.48867159166503,4.31025096829131));
#48596=CARTESIAN_POINT('Ctrl Pts',(-3.87810565739265,2.9990925400749,4.38962285834471));
#48597=CARTESIAN_POINT('Ctrl Pts',(-4.84019732919483,0.778941184101248,
4.46899474839812));
#48598=CARTESIAN_POINT('Ctrl Pts',(-4.62322764520021,-1.63095852016239,
4.54836663845152));
#48599=CARTESIAN_POINT('Ctrl Pts',(-3.28004994017564,-3.64356033897994,
4.62773852850492));
#48600=CARTESIAN_POINT('Ctrl Pts',(-1.13785932999167,-4.76859892410598,
4.70711041855833));
#48601=CARTESIAN_POINT('Ctrl Pts',(1.28151129436936,-4.73201736643448,4.78648230861172));
#48602=CARTESIAN_POINT('Ctrl Pts',(3.38870860399915,-3.54272685244233,4.86585419866514));
#48603=CARTESIAN_POINT('Ctrl Pts',(4.67042399847401,-1.4904359188881,4.94522608871853));
#48604=CARTESIAN_POINT('Ctrl Pts',(4.81443444472878,0.924921905483315,5.02459797877194));
#48605=CARTESIAN_POINT('Ctrl Pts',(3.78565931681752,3.1149708009589,5.10396986882535));
#48606=CARTESIAN_POINT('Ctrl Pts',(1.83470595874426,4.54621970419184,5.18334175887875));
#48607=CARTESIAN_POINT('Ctrl Pts',(-0.563177709826337,4.87001955037026,
5.26271364893215));
#48608=CARTESIAN_POINT('Ctrl Pts',(-2.82387253485596,4.00749341368393,5.34208553898556));
#48609=CARTESIAN_POINT('Ctrl Pts',(-4.39667826093048,2.1687507518604,5.42145742903895));
#48610=CARTESIAN_POINT('Ctrl Pts',(-4.89846289452463,-0.198294792667946,
5.50082931909237));
#48611=CARTESIAN_POINT('Ctrl Pts',(-4.20699280957627,-2.51703616462048,
5.58020120914576));
#48612=CARTESIAN_POINT('Ctrl Pts',(-2.49070858823577,-4.2226330982365,5.65957309919917));
#48613=CARTESIAN_POINT('Ctrl Pts',(-0.16769326789098,-4.89960595576194,
5.73894498925257));
#48614=CARTESIAN_POINT('Ctrl Pts',(2.19617176132931,-4.38304564755759,5.81831687930597));
#48615=CARTESIAN_POINT('Ctrl Pts',(4.0250542106335,-2.7987851213152,5.89768876935939));
#48616=CARTESIAN_POINT('Ctrl Pts',(4.87344236353376,-0.532746734526196,
5.97706065941277));
#48617=CARTESIAN_POINT('Ctrl Pts',(4.53467074385888,1.86306757757847,6.05643254946619));
#48618=CARTESIAN_POINT('Ctrl Pts',(3.09126336830344,3.80504275161517,6.13580443951959));
#48619=CARTESIAN_POINT('Ctrl Pts',(0.894831078624676,4.82011793367768,6.215176329573));
#48620=CARTESIAN_POINT('Ctrl Pts',(-1.51958008113206,4.6610230562464,6.2945482196264));
#48621=CARTESIAN_POINT('Ctrl Pts',(-3.56382489665849,3.36651327931302,6.3739201096798));
#48622=CARTESIAN_POINT('Ctrl Pts',(-4.73992985575151,1.25192831918974,6.45329199973321));
#48623=CARTESIAN_POINT('Ctrl Pts',(-4.76139839364024,-1.16762360839183,
6.53266388978661));
#48624=CARTESIAN_POINT('Ctrl Pts',(-3.62300082201479,-3.30274500946015,
6.61203577984002));
#48625=CARTESIAN_POINT('Ctrl Pts',(-1.60204826952283,-4.63332503672608,
6.69140766989341));
#48626=CARTESIAN_POINT('Ctrl Pts',(0.809159695351183,-4.83523734073654,
6.77077955994682));
#48627=CARTESIAN_POINT('Ctrl Pts',(3.02325814948227,-3.8592965311599,6.85015145000022));
#48628=CARTESIAN_POINT('Ctrl Pts',(4.50089761026788,-1.94323962900068,6.92952334005363));
#48629=CARTESIAN_POINT('Ctrl Pts',(4.8821283757601,0.446186145495144,7.00889523010703));
#48630=CARTESIAN_POINT('Ctrl Pts',(4.07408347532503,2.72692196256463,7.08826712016044));
#48631=CARTESIAN_POINT('Ctrl Pts',(2.27360085813158,4.34338562549276,7.16763901021384));
#48632=CARTESIAN_POINT('Ctrl Pts',(-0.0807258955725768,4.90181016397186,
7.24701090026724));
#48633=CARTESIAN_POINT('Ctrl Pts',(-2.41538799979899,4.26616459648018,7.32638279032065));
#48634=CARTESIAN_POINT('Ctrl Pts',(-4.16166693364502,2.59129077628108,7.40575468037405));
#48635=CARTESIAN_POINT('Ctrl Pts',(-4.89417301414864,0.285184258704783,
7.48512657042745));
#48636=CARTESIAN_POINT('Ctrl Pts',(-4.43446938147388,-2.09039251304738,
7.56449846048085));
#48637=CARTESIAN_POINT('Ctrl Pts',(-2.89453882300355,-3.95675429562653,
7.64387035053426));
#48638=CARTESIAN_POINT('Ctrl Pts',(-0.649505014202585,-4.85925948991814,
7.72324224058766));
#48639=CARTESIAN_POINT('Ctrl Pts',(1.75374677840318,-4.57805982825413,7.80261413064107));
#48640=CARTESIAN_POINT('Ctrl Pts',(3.72978973764259,-3.18165492579096,7.88198602069447));
#48641=CARTESIAN_POINT('Ctrl Pts',(4.79726417254181,-1.01020592587881,7.96135791074788));
#48642=CARTESIAN_POINT('Ctrl Pts',(4.69613567357394,1.40732700152449,8.04072980080128));
#48643=CARTESIAN_POINT('Ctrl Pts',(3.45103891924351,3.48203818642192,8.12010169085468));
#48644=CARTESIAN_POINT('Ctrl Pts',(1.36527672293039,4.70853257646778,8.19947358090808));
#48645=CARTESIAN_POINT('Ctrl Pts',(-1.05306386109979,4.78803885304614,8.2788454709615));
#48646=CARTESIAN_POINT('Ctrl Pts',(-3.21488041948337,3.7011894631667,8.35821736101489));
#48647=CARTESIAN_POINT('Ctrl Pts',(-4.5935592236979,1.7127385125038,8.4375892510683));
#48648=CARTESIAN_POINT('Ctrl Pts',(-4.85325716869052,-0.692931748722623,
8.51696114112171));
#48649=CARTESIAN_POINT('Ctrl Pts',(-3.93071240989269,-2.92980536973865,
8.59633303117509));
#48650=CARTESIAN_POINT('Ctrl Pts',(-2.05065480852931,-4.45298488770055,
8.67570492122852));
#48651=CARTESIAN_POINT('Ctrl Pts',(0.328937765144378,-4.89142714353344,
8.7550768112819));
#48652=CARTESIAN_POINT('Ctrl Pts',(2.62840182732027,-4.1383285741919,8.83444870133532));
#48653=CARTESIAN_POINT('Ctrl Pts',(4.28759302222971,-2.37714232421218,8.91382059138872));
#48654=CARTESIAN_POINT('Ctrl Pts',(4.90233604735019,-0.0368894657696129,
8.99319248144213));
#48655=CARTESIAN_POINT('Ctrl Pts',(4.32288086247292,2.31234958488097,9.07256437149553));
#48656=CARTESIAN_POINT('Ctrl Pts',(2.69038146803174,4.09830539495352,9.15193626154892));
#48657=CARTESIAN_POINT('Ctrl Pts',(0.402511103036409,4.88592308226053,9.23130815160233));
#48658=CARTESIAN_POINT('Ctrl Pts',(-1.9834100757154,4.48334072153617,9.31068004165575));
#48659=CARTESIAN_POINT('Ctrl Pts',(-3.88617695022667,2.98862648475194,9.39005193170914));
#48660=CARTESIAN_POINT('Ctrl Pts',(-4.84227972156947,0.765889451494674,
9.46942382176256));
#48661=CARTESIAN_POINT('Ctrl Pts',(-4.61881387094234,-1.64341655687914,
9.54879571181594));
#48662=CARTESIAN_POINT('Ctrl Pts',(-3.27021518492473,-3.65238992963806,
9.62816760186936));
#48663=CARTESIAN_POINT('Ctrl Pts',(-1.124999318358,-4.77164919996512,9.70753949192275));
#48664=CARTESIAN_POINT('Ctrl Pts',(1.29426389201697,-4.72854528704705,9.78691138197616));
#48665=CARTESIAN_POINT('Ctrl Pts',(3.39824728310117,-3.53357820866179,9.86628327202957));
#48666=CARTESIAN_POINT('Ctrl Pts',(4.67442515791466,-1.4778393000892,9.94565516208296));
#48667=CARTESIAN_POINT('Ctrl Pts',(4.81192341092478,0.937897990843289,10.0250270521364));
#48668=CARTESIAN_POINT('Ctrl Pts',(3.7772477720454,3.12516540720838,10.1043989421898));
#48669=CARTESIAN_POINT('Ctrl Pts',(1.82244293669188,4.55114944781378,10.1837708322432));
#48670=CARTESIAN_POINT('Ctrl Pts',(-0.576304964130747,4.86848355673017,
10.2631427222966));
#48671=CARTESIAN_POINT('Ctrl Pts',(-2.83466625132052,3.99986584743267,10.34251461235));
#48672=CARTESIAN_POINT('Ctrl Pts',(-4.40250911411597,2.15688967125344,10.4218865024034));
#48673=CARTESIAN_POINT('Ctrl Pts',(-4.89791050150136,-0.211500054648842,
10.5012583924568));
#48674=CARTESIAN_POINT('Ctrl Pts',(-4.20019173206204,-2.52836883538606,
10.5806302825102));
#48675=CARTESIAN_POINT('Ctrl Pts',(-2.47931555365911,-4.22933256427274,
10.6600021725636));
#48676=CARTESIAN_POINT('Ctrl Pts',(-0.154483594256702,-4.90004024197143,
10.739374062617));
#48677=CARTESIAN_POINT('Ctrl Pts',(2.20798022676301,-4.37710896278096,10.8187459526704));
#48678=CARTESIAN_POINT('Ctrl Pts',(4.03258495182456,-2.7879236288234,10.8981178427238));
#48679=CARTESIAN_POINT('Ctrl Pts',(4.87486090859705,-0.519606269848766,
10.9774897327772));
#48680=CARTESIAN_POINT('Ctrl Pts',(4.52963153835691,1.87528602633207,11.0568616228306));
#48681=CARTESIAN_POINT('Ctrl Pts',(3.08099395154235,3.81336279737362,11.136233512884));
#48682=CARTESIAN_POINT('Ctrl Pts',(0.881833057796546,4.82251283171035,11.2156054029374));
#48683=CARTESIAN_POINT('Ctrl Pts',(-1.53214041692415,4.65690941469354,11.2949772929908));
#48684=CARTESIAN_POINT('Ctrl Pts',(-3.5728878774174,3.35689317215153,11.3743491830443));
#48685=CARTESIAN_POINT('Ctrl Pts',(-4.74328775942496,1.23914518323042,11.4537210730976));
#48686=CARTESIAN_POINT('Ctrl Pts',(-4.75823324232597,-1.1804558295243,11.533092963151));
#48687=CARTESIAN_POINT('Ctrl Pts',(-3.614083639567,-3.31250041510156,11.6124648532044));
#48688=CARTESIAN_POINT('Ctrl Pts',(-1.58955126184795,-4.63762723165536,
11.6918367432579));
#48689=CARTESIAN_POINT('Ctrl Pts',(0.822192284845203,-4.83303831979168,
11.7712086333112));
#48690=CARTESIAN_POINT('Ctrl Pts',(3.03365161084184,-3.85113197097562,11.8505805233647));
#48691=CARTESIAN_POINT('Ctrl Pts',(4.50612011931135,-1.9310983983659,11.9299524134181));
#48692=CARTESIAN_POINT('Ctrl Pts',(4.88090774084429,0.459346469671929,12.0093243034715));
#48693=CARTESIAN_POINT('Ctrl Pts',(4.06671704041361,2.73789555444384,12.0886961935249));
#48694=CARTESIAN_POINT('Ctrl Pts',(2.26188307046365,4.34949934238227,12.1680680835783));
#48695=CARTESIAN_POINT('Ctrl Pts',(-0.0939406088580155,4.90157471796985,
12.2474399736317));
#48696=CARTESIAN_POINT('Ctrl Pts',(-2.42688056379585,4.25963734171157,12.3268118636851));
#48697=CARTESIAN_POINT('Ctrl Pts',(-4.16863778520202,2.58006173755973,12.4061837537385));
#48698=CARTESIAN_POINT('Ctrl Pts',(-4.89492406925624,0.271988805008134,
12.4855556437919));
#48699=CARTESIAN_POINT('Ctrl Pts',(-4.4288176847703,-2.10233999840645,12.5649275338453));
#48700=CARTESIAN_POINT('Ctrl Pts',(-2.88386111529598,-3.96454343165991,
12.6442994238987));
#48701=CARTESIAN_POINT('Ctrl Pts',(-0.636402361453836,-4.86099286032903,
12.7236713139521));
#48702=CARTESIAN_POINT('Ctrl Pts',(1.76608259898569,-4.57331518784718,12.8030432040055));
#48703=CARTESIAN_POINT('Ctrl Pts',(3.73835374746984,-3.17158805846724,12.8824150940589));
#48704=CARTESIAN_POINT('Ctrl Pts',(4.79997019777602,-0.997269098235751,
12.9617869841123));
#48705=CARTESIAN_POINT('Ctrl Pts',(4.69232453245774,1.41998240690827,13.0411588741657));
#48706=CARTESIAN_POINT('Ctrl Pts',(3.44163899731696,3.49132934080715,13.1205307642191));
#48707=CARTESIAN_POINT('Ctrl Pts',(1.35257782036847,4.71219617521183,13.1999026542725));
#48708=CARTESIAN_POINT('Ctrl Pts',(-1.06596831974157,4.78518245160425,13.2792745443259));
#48709=CARTESIAN_POINT('Ctrl Pts',(-3.22484693664342,3.69250887460753,13.3586464343793));
#48710=CARTESIAN_POINT('Ctrl Pts',(-4.59815997785652,1.70034830898619,13.4380183244327));
#48711=CARTESIAN_POINT('Ctrl Pts',(-4.85137142631828,-0.706013341047003,
13.5173902144861));
#48712=CARTESIAN_POINT('Ctrl Pts',(-3.92279953365742,-2.94039170393519,
13.5967621045396));
#48713=CARTESIAN_POINT('Ctrl Pts',(-2.03864235756713,-4.45849715619141,
13.6761339945929));
#48714=CARTESIAN_POINT('Ctrl Pts',(0.342123584368241,-4.8905225699155,13.7555058846463));
#48715=CARTESIAN_POINT('Ctrl Pts',(2.63954897842921,-4.13122751059623,13.8348777746997));
#48716=CARTESIAN_POINT('Ctrl Pts',(4.29398608388735,-2.36557457401273,13.9142496647532));
#48717=CARTESIAN_POINT('Ctrl Pts',(4.90241768388754,-0.0236729073102294,
13.9936215548065));
#48718=CARTESIAN_POINT('Ctrl Pts',(4.31663118741021,2.32399542721397,14.07299344486));
#48719=CARTESIAN_POINT('Ctrl Pts',(2.67932288838078,4.10554361974547,14.1523653349134));
#48720=CARTESIAN_POINT('Ctrl Pts',(0.389337464322444,4.8869904739736,14.2317372249668));
#48721=CARTESIAN_POINT('Ctrl Pts',(-1.99548970426098,4.47797726591172,14.3111091150202));
#48722=CARTESIAN_POINT('Ctrl Pts',(-3.894219997828,2.97813870770829,14.3904810050736));
#48723=CARTESIAN_POINT('Ctrl Pts',(-4.84432691963384,0.752832152305313,
14.469852895127));
#48724=CARTESIAN_POINT('Ctrl Pts',(-4.61436652655265,-1.6558626490335,14.5492247851804));
#48725=CARTESIAN_POINT('Ctrl Pts',(-3.26035666133029,-3.66119297425757,
14.6285966752338));
#48726=CARTESIAN_POINT('Ctrl Pts',(-1.11213113008494,-4.77466479486569,
14.7079685652872));
#48727=CARTESIAN_POINT('Ctrl Pts',(1.30700708278859,-4.72503883998578,14.7873404553406));
#48728=CARTESIAN_POINT('Ctrl Pts',(3.40776126330594,-3.52440388238144,14.866712345394));
#48729=CARTESIAN_POINT('Ctrl Pts',(4.67839234303357,-1.46523194016464,14.9460842354474));
#48730=CARTESIAN_POINT('Ctrl Pts',(4.80937740344404,0.95086725944037,15.0254561255008));
#48731=CARTESIAN_POINT('Ctrl Pts',(3.76880877375186,3.13533729935469,15.1048280155542));
#48732=CARTESIAN_POINT('Ctrl Pts',(1.81016666889045,4.55604611309762,15.1841999056076));
#48733=CARTESIAN_POINT('Ctrl Pts',(-0.58942802977675,4.86691217832697,15.263571795661));
#48734=CARTESIAN_POINT('Ctrl Pts',(-2.84543936506709,3.99220920964323,15.3429436857144));
#48735=CARTESIAN_POINT('Ctrl Pts',(-4.40830796930035,2.14501291409566,15.4223155757678));
#48736=CARTESIAN_POINT('Ctrl Pts',(-4.89732250983615,-0.224703779420184,
15.5016874658212));
#48737=CARTESIAN_POINT('Ctrl Pts',(-4.19336012701549,-2.53968312964247,
15.5810593558746));
#48738=CARTESIAN_POINT('Ctrl Pts',(-2.46790449909881,-4.23600129097741,
15.6604312459281));
#48739=CARTESIAN_POINT('Ctrl Pts',(-0.141272797816101,-4.90043891405947,
15.7398031359814));
#48740=CARTESIAN_POINT('Ctrl Pts',(2.21977264431347,-4.37114046461536,15.8191750260349));
#48741=CARTESIAN_POINT('Ctrl Pts',(4.04008638367001,-2.77704187334405,15.8985469160882));
#48742=CARTESIAN_POINT('Ctrl Pts',(4.87624402254724,-0.50646202860824,15.9779188061417));
#48743=CARTESIAN_POINT('Ctrl Pts',(4.52455941090906,1.88749084526974,16.057290696195));
#48744=CARTESIAN_POINT('Ctrl Pts',(3.0707021417271,3.82165512711525,16.1366625862485));
#48745=CARTESIAN_POINT('Ctrl Pts',(0.868828627683026,4.82487267911372,16.2160344763019));
#48746=CARTESIAN_POINT('Ctrl Pts',(-1.54468961690488,4.65276192610161,16.2954063663553));
#48747=CARTESIAN_POINT('Ctrl Pts',(-3.58192489000319,3.34724866670505,16.3747782564087));
#48748=CARTESIAN_POINT('Ctrl Pts',(-4.74661118820951,1.22635304091943,16.4541501464621));
#48749=CARTESIAN_POINT('Ctrl Pts',(-4.75503350768456,-1.19327947079094,
16.5335220365155));
#48750=CARTESIAN_POINT('Ctrl Pts',(-3.60514018926425,-3.32223174536968,
16.6128939265689));
#48751=CARTESIAN_POINT('Ctrl Pts',(-1.57704270154751,-4.64189571913949,
16.6922658166223));
#48752=CARTESIAN_POINT('Ctrl Pts',(0.835218899365215,-4.83080417279076,
16.7716377066757));
#48753=CARTESIAN_POINT('Ctrl Pts',(3.04402302167444,-3.84293941821851,16.8510095967291));
#48754=CARTESIAN_POINT('Ctrl Pts',(4.5113098802371,-1.91894313613405,16.9303814867825));
#48755=CARTESIAN_POINT('Ctrl Pts',(4.87965162531072,0.47250346257415,17.0097533768359));
#48756=CARTESIAN_POINT('Ctrl Pts',(4.05932105856824,2.74884923313555,17.0891252668893));
#48757=CARTESIAN_POINT('Ctrl Pts',(2.25014882333735,4.35558147263106,17.1684971569427));
#48758=CARTESIAN_POINT('Ctrl Pts',(-0.107154601980602,4.90130359745223,
17.2478690469961));
#48759=CARTESIAN_POINT('Ctrl Pts',(-2.43835555951383,4.25307922033065,17.3272409370495));
#48760=CARTESIAN_POINT('Ctrl Pts',(-4.17557820525659,2.56881377105676,17.4066128271029));
#48761=CARTESIAN_POINT('Ctrl Pts',(-4.8956397991406,0.258791705958601,17.4859847171563));
#48762=CARTESIAN_POINT('Ctrl Pts',(-4.42313332356637,-2.11427282962181,
17.5653566072097));
#48763=CARTESIAN_POINT('Ctrl Pts',(-2.8731633447509,-3.97230257099397,17.6447284972631));
#48764=CARTESIAN_POINT('Ctrl Pts',(-0.623293388711154,-4.8626931320669,
17.7241003873165));
#48765=CARTESIAN_POINT('Ctrl Pts',(1.77840238381723,-4.56853309419578,17.8034722773699));
#48766=CARTESIAN_POINT('Ctrl Pts',(3.74689662802603,-3.1615060961514,17.8828441674233));
#48767=CARTESIAN_POINT('Ctrl Pts',(4.80262992851038,-0.984309998791364,
17.9622160574768));
#48768=CARTESIAN_POINT('Ctrl Pts',(4.6885008269824,1.43259912421597,18.0415879475301));
#48769=CARTESIAN_POINT('Ctrl Pts',(3.43217338911689,3.50064868327997,18.1209598375836));
#48770=CARTESIAN_POINT('Ctrl Pts',(1.33994588402617,4.71572438645645,18.2003317276369));
#48771=CARTESIAN_POINT('Ctrl Pts',(-1.07901003836845,4.78248223987434,18.2797036176904));
#48772=CARTESIAN_POINT('Ctrl Pts',(-3.23451621663571,3.68344087079119,18.3590755077438));
#48773=CARTESIAN_POINT('Ctrl Pts',(-4.60324425657823,1.68862650319409,18.4384473977972));
#48774=CARTESIAN_POINT('Ctrl Pts',(-4.84847467695998,-0.720374489880202,
18.5178192878506));
#48775=CARTESIAN_POINT('Ctrl Pts',(-3.91669769333075,-2.94853678524982,
18.597191177904));
#48776=CARTESIAN_POINT('Ctrl Pts',(-2.02316502874899,-4.46849826887172,
18.6765630679574));
#48777=CARTESIAN_POINT('Ctrl Pts',(0.348982623889014,-4.88143613581971,
18.7559349580108));
#48778=CARTESIAN_POINT('Ctrl Pts',(3.43189297168081,-3.8881060605371,18.8617641447486));
#48779=CARTESIAN_POINT('Ctrl Pts',(5.55807194231376,-0.0182675279710476,
18.994050628171));
#48780=CARTESIAN_POINT('Ctrl Pts',(3.02540872544997,4.66632909528411,19.1527944082778));
#48781=CARTESIAN_POINT('Ctrl Pts',(-2.2762392030432,5.06930720888685,19.3115381883846));
#48782=CARTESIAN_POINT('Ctrl Pts',(-5.49476366156208,0.839647798275813,
19.4702819684914));
#48783=CARTESIAN_POINT('Ctrl Pts',(-3.68539651252317,-4.16147159288528,
19.6290257485982));
#48784=CARTESIAN_POINT('Ctrl Pts',(1.49629817009931,-5.35305176256653,19.787769528705));
#48785=CARTESIAN_POINT('Ctrl Pts',(5.30889903625351,-1.64699798333508,19.9465133088118));
#48786=CARTESIAN_POINT('Ctrl Pts',(4.26335305224425,3.56621538027062,20.1052570889186));
#48787=CARTESIAN_POINT('Ctrl Pts',(-0.682914143845088,5.51666761234037,
20.2640008690254));
#48788=CARTESIAN_POINT('Ctrl Pts',(-5.00517315099108,2.41778366488215,20.4227446491323));
#48789=CARTESIAN_POINT('Ctrl Pts',(-4.74574684718966,-2.89085235699305,
20.581488429239));
#48790=CARTESIAN_POINT('Ctrl Pts',(-0.146932230206273,-5.55932874556366,
20.7402322093459));
#48791=CARTESIAN_POINT('Ctrl Pts',(4.59246965375652,-3.13076985705421,20.8989759894527));
#48792=CARTESIAN_POINT('Ctrl Pts',(5.0299278500732,1.2629663218453,21.031262472875));
#48793=CARTESIAN_POINT('Ctrl Pts',(3.05056344532296,3.82678328180762,21.1370916596129));
#48794=CARTESIAN_POINT('Ctrl Pts',(0.861221142909519,4.82897211168878,21.2164635496663));
#48795=CARTESIAN_POINT('Ctrl Pts',(-1.56011376732917,4.64762681676397,21.2958354397197));
#48796=CARTESIAN_POINT('Ctrl Pts',(-3.58940432897566,3.338086676814,21.3752073297731));
#48797=CARTESIAN_POINT('Ctrl Pts',(-4.75071159562141,1.21328335035074,21.4545792198265));
#48798=CARTESIAN_POINT('Ctrl Pts',(-4.75136940590249,-1.2059521437222,21.5339511098799));
#48799=CARTESIAN_POINT('Ctrl Pts',(-3.59639816964331,-3.33201429213618,
21.6133229999333));
#48800=CARTESIAN_POINT('Ctrl Pts',(-1.56440212229559,-4.64609055668268,
21.6926948899867));
#48801=CARTESIAN_POINT('Ctrl Pts',(0.848175594776096,-4.82855605094712,
21.7720667800401));
#48802=CARTESIAN_POINT('Ctrl Pts',(3.05440612489727,-3.83470774368908,21.8514386700935));
#48803=CARTESIAN_POINT('Ctrl Pts',(4.5164489386699,-1.90677984789329,21.9308105601469));
#48804=CARTESIAN_POINT('Ctrl Pts',(4.87836953900972,0.485660146581216,22.0101824502003));
#48805=CARTESIAN_POINT('Ctrl Pts',(4.0518905292872,2.75978129753096,22.0895543402537));
#48806=CARTESIAN_POINT('Ctrl Pts',(2.23840092153696,4.36163277449212,22.1689262303071));
#48807=CARTESIAN_POINT('Ctrl Pts',(-0.120369299865574,4.90099648569508,
22.2482981203605));
#48808=CARTESIAN_POINT('Ctrl Pts',(-2.44981194564663,4.24649024808576,22.327670010414));
#48809=CARTESIAN_POINT('Ctrl Pts',(-4.18248893842781,2.55754735438689,22.4070419004673));
#48810=CARTESIAN_POINT('Ctrl Pts',(-4.89631923419535,0.245592132270486,
22.4864137905208));
#48811=CARTESIAN_POINT('Ctrl Pts',(-4.41741787585779,-2.12618907886207,
22.5657856805741));
#48812=CARTESIAN_POINT('Ctrl Pts',(-2.86244283812702,-3.98003518345998,
22.6451575706276));
#48813=CARTESIAN_POINT('Ctrl Pts',(-0.610183305945143,-4.86435360814152,
22.724529460681));
#48814=CARTESIAN_POINT('Ctrl Pts',(1.79071565870375,-4.56372621798445,22.8039013507344));
#48815=CARTESIAN_POINT('Ctrl Pts',(3.75540018385464,-3.15138524551451,22.8832732407878));
#48816=CARTESIAN_POINT('Ctrl Pts',(4.80527757305005,-0.971373790660912,
22.9626451308412));
#48817=CARTESIAN_POINT('Ctrl Pts',(4.68459996247748,1.44526216311697,23.0420170208946));
#48818=CARTESIAN_POINT('Ctrl Pts',(3.42276418043937,3.50983545637268,23.121388910948));
#48819=CARTESIAN_POINT('Ctrl Pts',(1.3271506148001,4.71942059955514,23.2007608010014));
#48820=CARTESIAN_POINT('Ctrl Pts',(-1.09175390014331,4.7793653318942,23.2801326910548));
#48821=CARTESIAN_POINT('Ctrl Pts',(-3.2447095830844,3.67506724782751,23.3595045811082));
#48822=CARTESIAN_POINT('Ctrl Pts',(-4.60726119282589,1.67553091707926,23.4388764711616));
#48823=CARTESIAN_POINT('Ctrl Pts',(-4.84749417441997,-0.732161036485464,
23.518248361215));
#48824=CARTESIAN_POINT('Ctrl Pts',(-3.90688830464649,-2.96150018209874,
23.5976202512684));
#48825=CARTESIAN_POINT('Ctrl Pts',(-2.01457309173102,-4.46942443856173,
23.6769921413218));
#48826=CARTESIAN_POINT('Ctrl Pts',(0.368487667211392,-4.88860679467339,
23.7563640313752));
#48827=CARTESIAN_POINT('Ctrl Pts',(2.66178564602131,-4.1169353563613,23.8357359214286));
#48828=CARTESIAN_POINT('Ctrl Pts',(4.30667853324075,-2.34238757791555,23.915107811482));
#48829=CARTESIAN_POINT('Ctrl Pts',(4.90247406242456,0.00276062972037378,
23.9944797015354));
#48830=CARTESIAN_POINT('Ctrl Pts',(4.30403776144901,2.34723635406859,24.0738515915888));
#48831=CARTESIAN_POINT('Ctrl Pts',(2.65714738860781,4.1199304980844,24.1532234816422));
#48832=CARTESIAN_POINT('Ctrl Pts',(0.362981793399119,4.88901869207872,24.2325953716956));
#48833=CARTESIAN_POINT('Ctrl Pts',(-2.01960536323572,4.46715275434179,24.311967261749));
#48834=CARTESIAN_POINT('Ctrl Pts',(-3.9102211237066,2.95709829352223,24.3913391518025));
#48835=CARTESIAN_POINT('Ctrl Pts',(-4.84831567357046,0.726701233826634,
24.4707110418558));
#48836=CARTESIAN_POINT('Ctrl Pts',(-4.60537125691712,-1.68071863790322,
24.5500829319093));
#48837=CARTESIAN_POINT('Ctrl Pts',(-3.2405685958952,-3.67871916964745,24.6294548219626));
#48838=CARTESIAN_POINT('Ctrl Pts',(-1.08637059779009,-4.78059185437233,
24.7088267120161));
#48839=CARTESIAN_POINT('Ctrl Pts',(1.33246487329615,-4.71792294503267,24.7881986020694));
#48840=CARTESIAN_POINT('Ctrl Pts',(3.42671485060842,-3.50597844922833,24.8675704921229));
#48841=CARTESIAN_POINT('Ctrl Pts',(4.68622467521711,-1.43998536354369,24.9469423821763));
#48842=CARTESIAN_POINT('Ctrl Pts',(4.80418054172532,0.976784969346655,25.0263142722297));
#48843=CARTESIAN_POINT('Ctrl Pts',(3.75184866214253,3.15561264578101,25.105686162283));
#48844=CARTESIAN_POINT('Ctrl Pts',(1.785574753038,4.56574006653325,25.1850580523365));
#48845=CARTESIAN_POINT('Ctrl Pts',(-0.615661213603954,4.86366331317224,
25.2644299423898));
#48846=CARTESIAN_POINT('Ctrl Pts',(-2.86692347135497,3.97680894225859,25.3438018324433));
#48847=CARTESIAN_POINT('Ctrl Pts',(-4.41980951731136,2.12121271552801,25.4231737224967));
#48848=CARTESIAN_POINT('Ctrl Pts',(-4.89603974793313,-0.25110623348048,
25.5025456125501));
#48849=CARTESIAN_POINT('Ctrl Pts',(-4.17960553315853,-2.56225625982736,
25.5819175026035));
#48850=CARTESIAN_POINT('Ctrl Pts',(-2.44502866190641,-4.24924633273829,
25.6612893926569));
#48851=CARTESIAN_POINT('Ctrl Pts',(-0.114848220593104,-4.9011294045414,
25.7406612827103));
#48852=CARTESIAN_POINT('Ctrl Pts',(2.24330899304448,-4.35910820186418,25.8200331727637));
#48853=CARTESIAN_POINT('Ctrl Pts',(4.05500110145669,-2.75521788993518,25.8994050628171));
#48854=CARTESIAN_POINT('Ctrl Pts',(4.87890391714675,-0.480162598589303,
25.9787769528705));
#48855=CARTESIAN_POINT('Ctrl Pts',(4.51431653789045,1.91185923895103,26.0581488429239));
#48856=CARTESIAN_POINT('Ctrl Pts',(3.05005164227427,3.83815639771151,26.1375207329773));
#48857=CARTESIAN_POINT('Ctrl Pts',(0.842800917774871,4.82948715360457,26.2168926230307));
#48858=CARTESIAN_POINT('Ctrl Pts',(-1.56975424478632,4.64436552876808,26.2962645130841));
#48859=CARTESIAN_POINT('Ctrl Pts',(-3.59992074790968,3.32788674125238,26.3756364031376));
#48860=CARTESIAN_POINT('Ctrl Pts',(-4.7531545251316,1.20074210971995,26.4550082931909));
#48861=CARTESIAN_POINT('Ctrl Pts',(-4.74853038096058,-1.21890064194263,
26.5343801832443));
#48862=CARTESIAN_POINT('Ctrl Pts',(-3.58717474668129,-3.34162189521881,
26.6137520732977));
#48863=CARTESIAN_POINT('Ctrl Pts',(-1.55199128418706,-4.65033145137433,
26.6931239633511));
#48864=CARTESIAN_POINT('Ctrl Pts',(0.861253819860729,-4.82623055930912,
26.7724958534045));
#48865=CARTESIAN_POINT('Ctrl Pts',(3.06469939974342,-3.82647058567632,26.851867743458));
#48866=CARTESIAN_POINT('Ctrl Pts',(4.52159098944567,-1.89459084712176,26.9312396335114));
#48867=CARTESIAN_POINT('Ctrl Pts',(4.87703302249084,0.49880702818598,27.0106115235648));
#48868=CARTESIAN_POINT('Ctrl Pts',(4.0444406063867,2.77069661551822,27.0899834136182));
#48869=CARTESIAN_POINT('Ctrl Pts',(2.22663141078423,4.36765064014314,27.1693553036716));
#48870=CARTESIAN_POINT('Ctrl Pts',(-0.133580267920228,4.90065463645992,
27.248727193725));
#48871=CARTESIAN_POINT('Ctrl Pts',(-2.46125208903423,4.23987001075014,27.3280990837784));
#48872=CARTESIAN_POINT('Ctrl Pts',(-4.1893683491486,2.54626243521474,27.4074709738318));
#48873=CARTESIAN_POINT('Ctrl Pts',(-4.89696375241997,0.232390966517291,
27.4868428638852));
#48874=CARTESIAN_POINT('Ctrl Pts',(-4.41166962484721,-2.13809042723509,
27.5662147539386));
#48875=CARTESIAN_POINT('Ctrl Pts',(-2.85170254172674,-3.98773772549588,
27.645586643992));
#48876=CARTESIAN_POINT('Ctrl Pts',(-0.597067031578144,-4.8659809405336,
27.7249585340454));
#48877=CARTESIAN_POINT('Ctrl Pts',(1.80301268587744,-4.55888196912345,27.8043304240988));
#48878=CARTESIAN_POINT('Ctrl Pts',(3.76388250395415,-3.14124944094887,27.8837023141522));
#48879=CARTESIAN_POINT('Ctrl Pts',(4.80787887528022,-0.958415501996903,
27.9630742042056));
#48880=CARTESIAN_POINT('Ctrl Pts',(4.68068659464744,1.45788633182479,28.042446094259));
#48881=CARTESIAN_POINT('Ctrl Pts',(3.41328942008259,3.51905028219065,28.1218179843124));
#48882=CARTESIAN_POINT('Ctrl Pts',(1.31442249797358,4.72298137310056,28.2011898743658));
#48883=CARTESIAN_POINT('Ctrl Pts',(-1.10463483521695,4.77640465566507,28.2805617644192));
#48884=CARTESIAN_POINT('Ctrl Pts',(-3.25460556761632,3.66630633650198,28.3599336544726));
#48885=CARTESIAN_POINT('Ctrl Pts',(-4.6117615876916,1.66310390899846,28.439305544526));
#48886=CARTESIAN_POINT('Ctrl Pts',(-4.84550269296638,-0.745226949519058,
28.5186774345794));
#48887=CARTESIAN_POINT('Ctrl Pts',(-3.89889006757279,-2.97202217266562,
28.5980493246329));
#48888=CARTESIAN_POINT('Ctrl Pts',(-2.00251645176526,-4.4748393730103,28.6774212146862));
#48889=CARTESIAN_POINT('Ctrl Pts',(0.381665739197275,-4.88759560697863,
28.7567931047396));
#48890=CARTESIAN_POINT('Ctrl Pts',(2.67287500089413,-4.10974436959635,28.8361649947931));
#48891=CARTESIAN_POINT('Ctrl Pts',(4.31297782868169,-2.33076850054527,28.9155368848464));
#48892=CARTESIAN_POINT('Ctrl Pts',(4.90244880401687,0.015977416170102,28.9949087748999));
#48893=CARTESIAN_POINT('Ctrl Pts',(4.29769410207987,2.35883126967183,29.0742806649532));
#48894=CARTESIAN_POINT('Ctrl Pts',(2.64603062966077,4.12707904706596,29.1536525550067));
#48895=CARTESIAN_POINT('Ctrl Pts',(0.349799952745733,4.88997950372933,29.23302444506));
#48896=CARTESIAN_POINT('Ctrl Pts',(-2.03164121838909,4.46169177707024,29.3123963351135));
#48897=CARTESIAN_POINT('Ctrl Pts',(-3.91817908568586,2.94654580930412,29.3917682251669));
#48898=CARTESIAN_POINT('Ctrl Pts',(-4.85025720045188,0.71362780446005,29.4711401152203));
#48899=CARTESIAN_POINT('Ctrl Pts',(-4.60082339705005,-1.69312835396218,
29.5505120052737));
#48900=CARTESIAN_POINT('Ctrl Pts',(-3.23063919787666,-3.68744219303526,
29.6298838953271));
#48901=CARTESIAN_POINT('Ctrl Pts',(-1.07347844099907,-4.78350327589979,
29.7092557853805));
#48902=CARTESIAN_POINT('Ctrl Pts',(1.34517928800161,-4.71431354886002,29.7886276754339));
#48903=CARTESIAN_POINT('Ctrl Pts',(3.43615431994896,-3.49672747627405,29.8679995654873));
#48904=CARTESIAN_POINT('Ctrl Pts',(4.69008976535537,-1.42734633034267,29.9473714555407));
#48905=CARTESIAN_POINT('Ctrl Pts',(4.8015297252588,0.989733222282683,30.0267433455941));
#48906=CARTESIAN_POINT('Ctrl Pts',(3.74332767209493,3.16571595269729,30.1061152356475));
#48907=CARTESIAN_POINT('Ctrl Pts',(1.77325928372404,4.57053728422822,30.1854871257009));
#48908=CARTESIAN_POINT('Ctrl Pts',(-0.628771141119161,4.86198585003386,
30.2648590157543));
#48909=CARTESIAN_POINT('Ctrl Pts',(-2.8776343077471,3.9690654245944,30.3442309058078));
#48910=CARTESIAN_POINT('Ctrl Pts',(-4.42551212654334,2.10928944710103,30.4236027958611));
#48911=CARTESIAN_POINT('Ctrl Pts',(-4.89534498701853,-0.264304770873174,
30.5029746859146));
#48912=CARTESIAN_POINT('Ctrl Pts',(-4.17268264431835,-2.57351493169134,
30.5823465759679));
#48913=CARTESIAN_POINT('Ctrl Pts',(-2.43356404553856,-4.25582255152819,
30.6617184660214));
#48914=CARTESIAN_POINT('Ctrl Pts',(-0.101634631868219,-4.90142121791616,
30.7410903560747));
#48915=CARTESIAN_POINT('Ctrl Pts',(2.25505275316072,-4.35304452473163,30.8204622461282));
#48916=CARTESIAN_POINT('Ctrl Pts',(4.06241427899435,-2.74427582062311,30.8998341361815));
#48917=CARTESIAN_POINT('Ctrl Pts',(4.88018067846643,-0.467007600962325,
30.979206026235));
#48918=CARTESIAN_POINT('Ctrl Pts',(4.50914586676086,1.9240226365891,31.0585779162884));
#48919=CARTESIAN_POINT('Ctrl Pts',(3.0396931027374,3.84636521861933,31.1379498063418));
#48920=CARTESIAN_POINT('Ctrl Pts',(0.829777827133663,4.83174174717888,31.2173216963951));
#48921=CARTESIAN_POINT('Ctrl Pts',(-1.58226949047778,4.64011668100458,31.2966935864486));
#48922=CARTESIAN_POINT('Ctrl Pts',(-3.60887946250293,3.31816946206164,31.376065476502));
#48923=CARTESIAN_POINT('Ctrl Pts',(-4.75637438558157,1.18792350680397,31.4554373665554));
#48924=CARTESIAN_POINT('Ctrl Pts',(-4.74522703638862,-1.23169798528705,
31.5348092566087));
#48925=CARTESIAN_POINT('Ctrl Pts',(-3.57815288451333,-3.35128057447936,
31.6141811466622));
#48926=CARTESIAN_POINT('Ctrl Pts',(-1.53944861007768,-4.65449863366224,
31.6935530367156));
#48927=CARTESIAN_POINT('Ctrl Pts',(0.874261938261232,-4.823891128243,31.772924926769));
#48928=CARTESIAN_POINT('Ctrl Pts',(3.07500421358568,-3.81819442148565,31.8522968168224));
#48929=CARTESIAN_POINT('Ctrl Pts',(4.52668226888703,-1.88239400508438,31.9316687068758));
#48930=CARTESIAN_POINT('Ctrl Pts',(4.87567054312872,0.511953424346944,32.0110405969291));
#48931=CARTESIAN_POINT('Ctrl Pts',(4.036956265178,2.78159013279705,32.0904124869827));
#48932=CARTESIAN_POINT('Ctrl Pts',(2.21484837668102,4.37363764184315,32.169784377036));
#48933=CARTESIAN_POINT('Ctrl Pts',(-0.146791673891742,4.90027670221896,
32.2491562670894));
#48934=CARTESIAN_POINT('Ctrl Pts',(-2.47267359762233,4.23321920451271,32.3285281571428));
#48935=CARTESIAN_POINT('Ctrl Pts',(-4.19621770614226,2.53495887865897,32.4079000471962));
#48936=CARTESIAN_POINT('Ctrl Pts',(-4.89757246961631,0.219188181000233,
32.4872719372496));
#48937=CARTESIAN_POINT('Ctrl Pts',(-4.40588942008463,-2.1499762723854,32.566643827303));
#48938=CARTESIAN_POINT('Ctrl Pts',(-2.84094146009112,-3.99541126470971,
32.6460157173564));
#48939=CARTESIAN_POINT('Ctrl Pts',(-0.583946448736662,-4.86757291664353,
32.7253876074098));
#48940=CARTESIAN_POINT('Ctrl Pts',(1.81529662498649,-4.55400458027289,32.8047594974633));
#48941=CARTESIAN_POINT('Ctrl Pts',(3.77233745895388,-3.13109080826592,32.8841313875166));
#48942=CARTESIAN_POINT('Ctrl Pts',(4.81044523784739,-0.945450245917296,
32.96350327757));
#48943=CARTESIAN_POINT('Ctrl Pts',(4.67673920454123,1.4704999036181,33.0428751676234));
#48944=CARTESIAN_POINT('Ctrl Pts',(3.40378985279549,3.52823953152847,33.1222470576768));
#48945=CARTESIAN_POINT('Ctrl Pts',(1.30168482706983,4.72650781918426,33.2016189477302));
#48946=CARTESIAN_POINT('Ctrl Pts',(-1.11750774129953,4.7734092640344,33.2809908377837));
#48947=CARTESIAN_POINT('Ctrl Pts',(-3.2644778974498,3.65751877792795,33.360362727837));
#48948=CARTESIAN_POINT('Ctrl Pts',(-4.61622846358057,1.65066481329873,33.4397346178904));
#48949=CARTESIAN_POINT('Ctrl Pts',(-4.84347599383145,-0.75828744616548,
33.5191065079439));
#48950=CARTESIAN_POINT('Ctrl Pts',(-3.89086349283728,-2.98252256218456,
33.5984783979973));
#48951=CARTESIAN_POINT('Ctrl Pts',(-1.99044525726817,-4.4802217837572,33.6778502880507));
#48952=CARTESIAN_POINT('Ctrl Pts',(0.394841037195618,-4.88654889560926,
33.7572221781041));
#48953=CARTESIAN_POINT('Ctrl Pts',(2.68394492896431,-4.10252351268344,33.8365940681574));
#48954=CARTESIAN_POINT('Ctrl Pts',(4.31924577684866,-2.31913248284973,33.9159659582109));
#48955=CARTESIAN_POINT('Ctrl Pts',(4.90238791398107,0.029194086493524,33.9953378482642));
#48956=CARTESIAN_POINT('Ctrl Pts',(4.29131920651926,2.37040904098698,34.0747097383177));
#48957=CARTESIAN_POINT('Ctrl Pts',(2.63489463902328,4.13419759990741,34.1540816283711));
#48958=CARTESIAN_POINT('Ctrl Pts',(0.336615569701593,4.89090477438156,34.2334535184245));
#48959=CARTESIAN_POINT('Ctrl Pts',(-2.04366230731349,4.45619837165044,34.3128254084779));
#48960=CARTESIAN_POINT('Ctrl Pts',(-3.92610856983677,2.93597190921303,34.3921972985313));
#48961=CARTESIAN_POINT('Ctrl Pts',(-4.85216347504172,0.700549188354975,
34.4715691885847));
#48962=CARTESIAN_POINT('Ctrl Pts',(-4.59624209780822,-1.70552576414703,
34.5509410786381));
#48963=CARTESIAN_POINT('Ctrl Pts',(-3.22068631915797,-3.69613841562006,
34.6303129686915));
#48964=CARTESIAN_POINT('Ctrl Pts',(-1.06057848202912,-4.7863799303117,34.709684858745));
#48965=CARTESIAN_POINT('Ctrl Pts',(1.35788392577142,-4.71066988845169,34.7890567487982));
#48966=CARTESIAN_POINT('Ctrl Pts',(3.44556881487913,-3.48745108865577,34.8684286388518));
#48967=CARTESIAN_POINT('Ctrl Pts',(4.69392076731947,-1.41469692300534,34.9478005289051));
#48968=CARTESIAN_POINT('Ctrl Pts',(4.79884401065818,1.00267428171067,35.0271724189586));
#48969=CARTESIAN_POINT('Ctrl Pts',(3.73477947506157,3.17579625078383,35.1065443090119));
#48970=CARTESIAN_POINT('Ctrl Pts',(1.76093092613411,4.57530128267181,35.1859161990653));
#48971=CARTESIAN_POINT('Ctrl Pts',(-0.64187649864509,4.86027304935852,35.2652880891187));
#48972=CARTESIAN_POINT('Ctrl Pts',(-2.88832422912388,3.96129305925348,35.3446599791721));
#48973=CARTESIAN_POINT('Ctrl Pts',(-4.43118257058537,2.09735084808771,35.4240318692256));
#48974=CARTESIAN_POINT('Ctrl Pts',(-4.89461464610851,-0.277501387264873,
35.5034037592789));
#48975=CARTESIAN_POINT('Ctrl Pts',(-4.16572942788534,-2.58475489891863,
35.5827756493324));
#48976=CARTESIAN_POINT('Ctrl Pts',(-2.42208174171502,-4.2623678384537,35.6621475393857));
#48977=CARTESIAN_POINT('Ctrl Pts',(-0.0884203044499451,-4.90167740713266,
35.7415194294392));
#48978=CARTESIAN_POINT('Ctrl Pts',(2.26678012326416,-4.34694920911302,35.8208913194925));
#48979=CARTESIAN_POINT('Ctrl Pts',(4.06979793038381,-2.73331380556231,35.900263209546));
#48980=CARTESIAN_POINT('Ctrl Pts',(4.88142197000686,-0.453849209064084,
35.9796350995994));
#48981=CARTESIAN_POINT('Ctrl Pts',(4.50394242258051,1.9361720501839,36.0590069896528));
#48982=CARTESIAN_POINT('Ctrl Pts',(3.02931247032103,3.85454608365127,36.1383788797062));
#48983=CARTESIAN_POINT('Ctrl Pts',(0.816748705560739,4.83396122303424,36.2177507697595));
#48984=CARTESIAN_POINT('Ctrl Pts',(-1.59477323603157,4.63583410827775,36.297122659813));
#48985=CARTESIAN_POINT('Ctrl Pts',(-3.61781194729725,3.3084280659895,36.3764945498664));
#48986=CARTESIAN_POINT('Ctrl Pts',(-4.75955967609224,1.17509626990754,36.4558664399198));
#48987=CARTESIAN_POINT('Ctrl Pts',(-4.74188920289779,-1.24448637649244,
36.5352383299732));
#48988=CARTESIAN_POINT('Ctrl Pts',(-3.56910501587113,-3.36091489620272,
36.6146102200266));
#48989=CARTESIAN_POINT('Ctrl Pts',(-1.52689474705826,-4.65863198645693,
36.69398211008));
#48990=CARTESIAN_POINT('Ctrl Pts',(0.887263702413796,-4.82151663651726,
36.7733540001334));
#48991=CARTESIAN_POINT('Ctrl Pts',(3.08528667790275,-3.80989050616806,36.8527258901868));
#48992=CARTESIAN_POINT('Ctrl Pts',(4.53174064782084,-1.87018348156595,36.9320977802402));
#48993=CARTESIAN_POINT('Ctrl Pts',(4.87427262676759,0.525096099564754,37.0114696702936));
#48994=CARTESIAN_POINT('Ctrl Pts',(4.02944258285317,2.79246343312197,37.090841560347));
#48995=CARTESIAN_POINT('Ctrl Pts',(2.20304924477561,4.37959285538367,37.1702134504005));
#48996=CARTESIAN_POINT('Ctrl Pts',(-0.160002012962556,4.89986315213815,
37.2495853404538));
#48997=CARTESIAN_POINT('Ctrl Pts',(-2.48407713450139,4.22653763069513,37.3289572305073));
#48998=CARTESIAN_POINT('Ctrl Pts',(-4.20303656448734,2.52363689769662,37.4083291205606));
#48999=CARTESIAN_POINT('Ctrl Pts',(-4.89814559062741,0.20598380239574,37.4877010106141));
#49000=CARTESIAN_POINT('Ctrl Pts',(-4.40007719275278,-2.16184649123314,
37.5670729006674));
#49001=CARTESIAN_POINT('Ctrl Pts',(-2.83015973012786,-4.0030557647603,37.6464447907209));
#49002=CARTESIAN_POINT('Ctrl Pts',(-0.570821621698638,-4.86912951461192,
37.7258166807742));
#49003=CARTESIAN_POINT('Ctrl Pts',(1.82756737028896,-4.54909409232726,37.8051885708277));
#49004=CARTESIAN_POINT('Ctrl Pts',(3.78076499611679,-3.12090941842365,37.884560460881));
#49005=CARTESIAN_POINT('Ctrl Pts',(4.81297663748916,-0.932478118164531,
37.9639323509345));
#49006=CARTESIAN_POINT('Ctrl Pts',(4.6727578232798,1.48310278759233,38.0433042409879));
#49007=CARTESIAN_POINT('Ctrl Pts',(3.39426554635479,3.53740313723864,38.1226761310413));
#49008=CARTESIAN_POINT('Ctrl Pts',(1.2889376953013,4.72999991227071,38.2020480210947));
#49009=CARTESIAN_POINT('Ctrl Pts',(-1.13037252509376,4.77037917890205,38.2814199111481));
#49010=CARTESIAN_POINT('Ctrl Pts',(-3.27432650082598,3.64870463556727,38.3607918012015));
#49011=CARTESIAN_POINT('Ctrl Pts',(-4.62066178777622,1.63821372124413,38.4401636912549));
#49012=CARTESIAN_POINT('Ctrl Pts',(-4.84141409235733,-0.771342433159972,
38.5195355813083));
#49013=CARTESIAN_POINT('Ctrl Pts',(-3.88280863754963,-2.99300127117752,
38.5989074713617));
#49014=CARTESIAN_POINT('Ctrl Pts',(-1.97835959833324,-4.48557163766163,
38.6782793614151));
#49015=CARTESIAN_POINT('Ctrl Pts',(0.4080134699205,-4.88546665687603,38.7576512514685));
#49016=CARTESIAN_POINT('Ctrl Pts',(2.69499534131588,-4.09527285943909,38.8370231415219));
#49017=CARTESIAN_POINT('Ctrl Pts',(4.32548234816251,-2.30747956911512,38.9163950315754));
#49018=CARTESIAN_POINT('Ctrl Pts',(4.90229136258888,0.0424104685617285,
38.9957669216287));
#49019=CARTESIAN_POINT('Ctrl Pts',(4.28491317807095,2.38196972749885,39.0751388116822));
#49020=CARTESIAN_POINT('Ctrl Pts',(2.62373939006081,4.14128583366062,39.1545107017355));
#49021=CARTESIAN_POINT('Ctrl Pts',(0.323428943211332,4.89179500940948,39.233882591789));
#49022=CARTESIAN_POINT('Ctrl Pts',(-2.05566892616818,4.45067161106171,39.3132544818423));
#49023=CARTESIAN_POINT('Ctrl Pts',(-3.93400879434316,2.92537849589611,39.3926263718958));
#49024=CARTESIAN_POINT('Ctrl Pts',(-4.85403585089548,0.68746203308737,39.4719982619491));
#49025=CARTESIAN_POINT('Ctrl Pts',(-4.59162481050186,-1.71790426872522,
39.5513701520026));
#49026=CARTESIAN_POINT('Ctrl Pts',(-3.21071490770548,-3.70482006635682,
39.6307420420559));
#49027=CARTESIAN_POINT('Ctrl Pts',(-1.04766160592177,-4.78919858119775,
39.7101139321094));
#49028=CARTESIAN_POINT('Ctrl Pts',(1.37056128557131,-4.7070358700676,39.7894858221627));
#49029=CARTESIAN_POINT('Ctrl Pts',(3.45499130789194,-3.47806613859367,39.8688577122162));
#49030=CARTESIAN_POINT('Ctrl Pts',(4.69765387924814,-1.40219731261544,39.9482296022695));
#49031=CARTESIAN_POINT('Ctrl Pts',(4.79625497710706,1.0159342797995,40.027601492323));
#49032=CARTESIAN_POINT('Ctrl Pts',(4.08267404777822,2.46201708819427,40.0805160856919));
#49033=CARTESIAN_POINT('Ctrl Pts',(3.57461543774186,3.05624720968413,40.1069733823764));
#49034=CARTESIAN_POINT('Ctrl Pts',(1.16918346556923,-4.36383719750629,-0.320920147129053));
#49035=CARTESIAN_POINT('Ctrl Pts',(1.8946107326977,-4.16947670058299,-0.294462850444586));
#49036=CARTESIAN_POINT('Ctrl Pts',(3.24594541476064,-3.41224896374509,-0.24154825707565));
#49037=CARTESIAN_POINT('Ctrl Pts',(4.48258575488109,-1.44364637546346,-0.162176367022246));
#49038=CARTESIAN_POINT('Ctrl Pts',(4.62712170766666,0.875927969712858,-0.0828044769688426));
#49039=CARTESIAN_POINT('Ctrl Pts',(3.64458116255458,2.98248116081162,-0.00343258691543892));
#49040=CARTESIAN_POINT('Ctrl Pts',(1.77418661813218,4.36232362711486,0.0759393031379646));
#49041=CARTESIAN_POINT('Ctrl Pts',(-0.52837360592073,4.67961139929734,0.155311193191369));
#49042=CARTESIAN_POINT('Ctrl Pts',(-2.70223496968603,3.85690448821556,0.234683083244771));
#49043=CARTESIAN_POINT('Ctrl Pts',(-4.21783163769356,2.09469156016015,0.314054973298176));
#49044=CARTESIAN_POINT('Ctrl Pts',(-4.70597715859854,-0.177798095133649,
0.393426863351579));
#49045=CARTESIAN_POINT('Ctrl Pts',(-4.04775531046147,-2.4069688489564,0.472798753404983));
#49046=CARTESIAN_POINT('Ctrl Pts',(-2.40351015490329,-4.04981138575499,
0.552170643458387));
#49047=CARTESIAN_POINT('Ctrl Pts',(-0.173774754931243,-4.70612667927193,
0.631542533511791));
#49048=CARTESIAN_POINT('Ctrl Pts',(2.0982915307903,-4.21604107122297,0.710914423565194));
#49049=CARTESIAN_POINT('Ctrl Pts',(3.85921878174909,-2.69893658616936,0.790286313618597));
#49050=CARTESIAN_POINT('Ctrl Pts',(4.68004880681062,-0.524377442655228,
0.869658203672002));
#49051=CARTESIAN_POINT('Ctrl Pts',(4.36082934025305,1.77791905463906,0.949030093725404));
#49052=CARTESIAN_POINT('Ctrl Pts',(2.97932147849509,3.64711831584472,1.02840198377881));
#49053=CARTESIAN_POINT('Ctrl Pts',(0.872057510020645,4.62788767559441,1.10777387383221));
#49054=CARTESIAN_POINT('Ctrl Pts',(-1.44763774336318,4.48131381605584,1.18714576388562));
#49055=CARTESIAN_POINT('Ctrl Pts',(-3.4146916437183,3.2431018434756,1.26651765393902));
#49056=CARTESIAN_POINT('Ctrl Pts',(-4.54993421956391,1.21487743324944,1.34588954399242));
#49057=CARTESIAN_POINT('Ctrl Pts',(-4.57682288978047,-1.10928842689199,
1.42526143404583));
#49058=CARTESIAN_POINT('Ctrl Pts',(-3.48880763512327,-3.16323408359086,
1.50463332409923));
#49059=CARTESIAN_POINT('Ctrl Pts',(-1.55092656265583,-4.44662291817823,
1.58400521415264));
#49060=CARTESIAN_POINT('Ctrl Pts',(0.764756787430318,-4.64682425288564,
1.66337710420604));
#49061=CARTESIAN_POINT('Ctrl Pts',(2.89414707692588,-3.71506948486699,1.74274899425944));
#49062=CARTESIAN_POINT('Ctrl Pts',(4.31852954453272,-1.87833201365734,1.82212088431284));
#49063=CARTESIAN_POINT('Ctrl Pts',(4.69092777401317,0.415962978544339,1.90149277436625));
#49064=CARTESIAN_POINT('Ctrl Pts',(3.92062638092659,2.60893030984735,1.98086466441965));
#49065=CARTESIAN_POINT('Ctrl Pts',(2.19526907961086,4.166367992464,2.06023655447306));
#49066=CARTESIAN_POINT('Ctrl Pts',(-0.0648509103551908,4.70888765420329,
2.13960844452646));
#49067=CARTESIAN_POINT('Ctrl Pts',(-2.30917336210229,4.10433270633116,2.21898033457986));
#49068=CARTESIAN_POINT('Ctrl Pts',(-3.99098629411059,2.49997139597969,2.29835222463327));
#49069=CARTESIAN_POINT('Ctrl Pts',(-4.70060379877146,0.286622587162194,
2.37772411468667));
#49070=CARTESIAN_POINT('Ctrl Pts',(-4.26516462266185,-1.99654684946062,
2.45709600474007));
#49071=CARTESIAN_POINT('Ctrl Pts',(-2.79074078525346,-3.79336189283582,
2.53646789479348));
#49072=CARTESIAN_POINT('Ctrl Pts',(-0.636498669757338,-4.66612237558061,
2.61583978484688));
#49073=CARTESIAN_POINT('Ctrl Pts',(1.6727931128258,-4.40222577592052,2.69521167490029));
#49074=CARTESIAN_POINT('Ctrl Pts',(3.5745961957893,-3.06595672140773,2.77458356495369));
#49075=CARTESIAN_POINT('Ctrl Pts',(4.60563555769302,-0.982827395940078,
2.85395545500709));
#49076=CARTESIAN_POINT('Ctrl Pts',(4.51475229214408,1.33971650772703,2.9333273450605));
#49077=CARTESIAN_POINT('Ctrl Pts',(3.32408536146356,3.33590843552402,3.0126992351139));
#49078=CARTESIAN_POINT('Ctrl Pts',(1.32367859446866,4.51948045233543,3.0920711251673));
#49079=CARTESIAN_POINT('Ctrl Pts',(-0.99917334822593,4.60211703465825,3.17144301522071));
#49080=CARTESIAN_POINT('Ctrl Pts',(-3.07862887492539,3.56368809395157,3.25081490527411));
#49081=CARTESIAN_POINT('Ctrl Pts',(-4.40813722212245,1.65715262164811,3.33018679532752));
#49082=CARTESIAN_POINT('Ctrl Pts',(-4.66383309925671,-0.653061561243739,
3.40955868538092));
#49083=CARTESIAN_POINT('Ctrl Pts',(-3.7834295566315,-2.80419139334385,3.48893057543432));
#49084=CARTESIAN_POINT('Ctrl Pts',(-1.98139094849014,-4.27222640899777,
3.56830246548773));
#49085=CARTESIAN_POINT('Ctrl Pts',(0.303310108968963,-4.69955652783259,
3.64767435554113));
#49086=CARTESIAN_POINT('Ctrl Pts',(2.51412549524875,-3.98208507877931,3.72704624559453));
#49087=CARTESIAN_POINT('Ctrl Pts',(4.11250547580833,-2.29458651873122,3.80641813564794));
#49088=CARTESIAN_POINT('Ctrl Pts',(4.70908822533748,-0.0481317617013215,
3.88579002570134));
#49089=CARTESIAN_POINT('Ctrl Pts',(4.15854750656441,2.21004778594118,3.96516191575474));
#49090=CARTESIAN_POINT('Ctrl Pts',(2.59499381998102,3.92986458478622,4.04453380580815));
#49091=CARTESIAN_POINT('Ctrl Pts',(0.399305382771643,4.69237506938503,4.12390569586155));
#49092=CARTESIAN_POINT('Ctrl Pts',(-1.89365296183344,4.3118333734777,4.20327758591496));
#49093=CARTESIAN_POINT('Ctrl Pts',(-3.72532163646561,2.88093861187248,4.28264947596836));
#49094=CARTESIAN_POINT('Ctrl Pts',(-4.64951020631435,0.748253581264596,
4.36202136602176));
#49095=CARTESIAN_POINT('Ctrl Pts',(-4.44108838142119,-1.56670436550815,
4.44139325607517));
#49096=CARTESIAN_POINT('Ctrl Pts',(-3.15082725699623,-3.5000165966844,4.52076514612857));
#49097=CARTESIAN_POINT('Ctrl Pts',(-1.09303158700481,-4.58073253206366,
4.60013703618198));
#49098=CARTESIAN_POINT('Ctrl Pts',(1.23102415819659,-4.54559216191169,4.67950892623538));
#49099=CARTESIAN_POINT('Ctrl Pts',(3.25520514328707,-3.40315560261561,4.75888081628878));
#49100=CARTESIAN_POINT('Ctrl Pts',(4.48642536074717,-1.43171787127954,4.83825270634219));
#49101=CARTESIAN_POINT('Ctrl Pts',(4.62476229086337,0.888483164446475,4.91762459639559));
#49102=CARTESIAN_POINT('Ctrl Pts',(3.63651736366295,2.99225166793745,4.99699648644899));
#49103=CARTESIAN_POINT('Ctrl Pts',(1.76242485596889,4.36711428835561,5.0763683765024));
#49104=CARTESIAN_POINT('Ctrl Pts',(-0.540990445577951,4.67815753457383,
5.15574026655579));
#49105=CARTESIAN_POINT('Ctrl Pts',(-2.71262167204403,3.84961196029596,5.23511215660921));
#49106=CARTESIAN_POINT('Ctrl Pts',(-4.22346426348642,2.08330943346152,5.3144840466626));
#49107=CARTESIAN_POINT('Ctrl Pts',(-4.70548030882309,-0.190482660036918,
5.39385593671601));
#49108=CARTESIAN_POINT('Ctrl Pts',(-4.04125176633447,-2.41787359917659,
5.47322782676941));
#49109=CARTESIAN_POINT('Ctrl Pts',(-2.39258323872581,-4.05627588142928,
5.55259971682282));
#49110=CARTESIAN_POINT('Ctrl Pts',(-0.161086730056731,-4.70657833738016,
5.63197160687622));
#49111=CARTESIAN_POINT('Ctrl Pts',(2.10965014949475,-4.21036872817968,5.71134349692963));
#49112=CARTESIAN_POINT('Ctrl Pts',(3.86648092226071,-2.68852261628773,5.79071538698303));
#49113=CARTESIAN_POINT('Ctrl Pts',(4.68144550067431,-0.511758346011949,
5.87008727703643));
#49114=CARTESIAN_POINT('Ctrl Pts',(4.3560203173275,1.78966912459444,5.94945916708984));
#49115=CARTESIAN_POINT('Ctrl Pts',(2.96947822656715,3.65513715781504,6.02883105714324));
#49116=CARTESIAN_POINT('Ctrl Pts',(0.859577812643608,4.63022186990077,6.10820294719665));
#49117=CARTESIAN_POINT('Ctrl Pts',(-1.45971385379671,4.47739478330096,6.18757483725004));
#49118=CARTESIAN_POINT('Ctrl Pts',(-3.42342245647396,3.23388423803426,6.26694672730346));
#49119=CARTESIAN_POINT('Ctrl Pts',(-4.55319292637122,1.20260665046377,6.34631861735685));
#49120=CARTESIAN_POINT('Ctrl Pts',(-4.57381567772605,-1.12162325523503,
6.42569050741026));
#49121=CARTESIAN_POINT('Ctrl Pts',(-3.48026705395609,-3.17262821862952,
6.50506239746367));
#49122=CARTESIAN_POINT('Ctrl Pts',(-1.5389330792829,-4.45078797045933,6.58443428751706));
#49123=CARTESIAN_POINT('Ctrl Pts',(0.777281587133017,-4.64474562433731,
6.66380617757047));
#49124=CARTESIAN_POINT('Ctrl Pts',(2.90415217940695,-3.70725352509678,6.74317806762387));
#49125=CARTESIAN_POINT('Ctrl Pts',(4.32357772900916,-1.86668267300916,6.82254995767728));
#49126=CARTESIAN_POINT('Ctrl Pts',(4.68978931390171,0.428607946391479,6.90192184773068));
#49127=CARTESIAN_POINT('Ctrl Pts',(3.91357860260037,2.61949061875875,6.98129373778408));
#49128=CARTESIAN_POINT('Ctrl Pts',(2.18402880626489,4.17227117454053,7.06066562783749));
#49129=CARTESIAN_POINT('Ctrl Pts',(-0.0775455730109682,4.70869570736982,
7.14003751789088));
#49130=CARTESIAN_POINT('Ctrl Pts',(-2.32023002234555,4.09809238840499,7.2194094079443));
#49131=CARTESIAN_POINT('Ctrl Pts',(-3.9977115739788,2.48920283459836,7.29878129799769));
#49132=CARTESIAN_POINT('Ctrl Pts',(-4.70135943497531,0.273948980040579,
7.37815318805111));
#49133=CARTESIAN_POINT('Ctrl Pts',(-4.25976654389442,-2.00803823967931,
7.4575250781045));
#49134=CARTESIAN_POINT('Ctrl Pts',(-2.78050395155417,-3.80087178893057,
7.53689696815791));
#49135=CARTESIAN_POINT('Ctrl Pts',(-0.623916751156424,-4.66782138348534,
7.61626885821132));
#49136=CARTESIAN_POINT('Ctrl Pts',(1.68465518880672,-4.39770002107047,7.69564074826471));
#49137=CARTESIAN_POINT('Ctrl Pts',(3.58284885369757,-3.05630866766671,7.77501263831812));
#49138=CARTESIAN_POINT('Ctrl Pts',(4.6082684683291,-0.970407287843808,7.85438452837152));
#49139=CARTESIAN_POINT('Ctrl Pts',(4.51112408430488,1.35188315933773,7.93375641842493));
#49140=CARTESIAN_POINT('Ctrl Pts',(3.31507985854782,3.3448578612472,8.01312830847833));
#49141=CARTESIAN_POINT('Ctrl Pts',(1.31148951705327,4.52303259187419,8.09250019853174));
#49142=CARTESIAN_POINT('Ctrl Pts',(-1.01157676786264,4.5994065946834,8.17187208858514));
#49143=CARTESIAN_POINT('Ctrl Pts',(-3.08822519121439,3.55537533164157,8.25124397863854));
#49144=CARTESIAN_POINT('Ctrl Pts',(-4.41258879365683,1.64526250750169,8.33061586869195));
#49145=CARTESIAN_POINT('Ctrl Pts',(-4.66205553306411,-0.665632621738795,
8.40998775874535));
#49146=CARTESIAN_POINT('Ctrl Pts',(-3.77585586390188,-2.81438111767656,
8.48935964879875));
#49147=CARTESIAN_POINT('Ctrl Pts',(-1.96986606400833,-4.27755260287526,
8.56873153885216));
#49148=CARTESIAN_POINT('Ctrl Pts',(0.315978748853086,-4.69872174221563,
8.64810342890556));
#49149=CARTESIAN_POINT('Ctrl Pts',(2.52485183790096,-3.97529266559641,8.72747531895897));
#49150=CARTESIAN_POINT('Ctrl Pts',(4.11867660790092,-2.28349109479901,8.80684720901236));
#49151=CARTESIAN_POINT('Ctrl Pts',(4.70920087275226,-0.0354361477303297,
8.88621909906579));
#49152=CARTESIAN_POINT('Ctrl Pts',(4.15257422864046,2.22125096648886,8.96559098911916));
#49153=CARTESIAN_POINT('Ctrl Pts',(2.58438969399899,3.93684626192698,9.04496287917259));
#49154=CARTESIAN_POINT('Ctrl Pts',(0.386653550348944,4.69343452202107,9.12433476922598));
#49155=CARTESIAN_POINT('Ctrl Pts',(-1.90527054232303,4.30671252129195,9.20370665927939));
#49156=CARTESIAN_POINT('Ctrl Pts',(-3.7330749481299,2.87088488312254,9.28307854933279));
#49157=CARTESIAN_POINT('Ctrl Pts',(-4.65151055959357,0.735716042020416,
9.3624504393862));
#49158=CARTESIAN_POINT('Ctrl Pts',(-4.43684849468422,-1.57867159843805,
9.4418223294396));
#49159=CARTESIAN_POINT('Ctrl Pts',(-3.14137995726738,-3.50849833184732,
9.52119421949301));
#49160=CARTESIAN_POINT('Ctrl Pts',(-1.08067821558679,-4.58366263754791,
9.6005661095464));
#49161=CARTESIAN_POINT('Ctrl Pts',(1.24327434737007,-4.54225687050701,9.67993799959982));
#49162=CARTESIAN_POINT('Ctrl Pts',(3.26436803124868,-3.39436738392564,9.75930988965321));
#49163=CARTESIAN_POINT('Ctrl Pts',(4.49026888827119,-1.41961751592476,9.83868177970662));
#49164=CARTESIAN_POINT('Ctrl Pts',(4.62235018315245,0.900948036685318,9.91805366976003));
#49165=CARTESIAN_POINT('Ctrl Pts',(3.62843720481635,3.00204464177353,9.99742555981342));
#49166=CARTESIAN_POINT('Ctrl Pts',(1.7506449547965,4.37184981703879,10.0767974498668));
#49167=CARTESIAN_POINT('Ctrl Pts',(-0.553600531224886,4.67668205379884,
10.1561693399202));
#49168=CARTESIAN_POINT('Ctrl Pts',(-2.72299015321387,3.84228489391363,10.2355412299736));
#49169=CARTESIAN_POINT('Ctrl Pts',(-4.22906540111646,2.07191563862441,10.314913120027));
#49170=CARTESIAN_POINT('Ctrl Pts',(-4.70494967818453,-0.203167680126261,
10.3942850100804));
#49171=CARTESIAN_POINT('Ctrl Pts',(-4.03471862787632,-2.42875980170217,
10.4736569001339));
#49172=CARTESIAN_POINT('Ctrl Pts',(-2.38163905051565,-4.06271141155209,
10.5530287901872));
#49173=CARTESIAN_POINT('Ctrl Pts',(-0.148397472117971,-4.70699551420709,
10.6324006802407));
#49174=CARTESIAN_POINT('Ctrl Pts',(2.12099340201542,-4.20466592835908,10.7117725702941));
#49175=CARTESIAN_POINT('Ctrl Pts',(3.87371497815709,-2.67808902923296,10.7911444603475));
#49176=CARTESIAN_POINT('Ctrl Pts',(4.68280815994238,-0.499135570435235,
10.8705163504009));
#49177=CARTESIAN_POINT('Ctrl Pts',(4.35117963918574,1.80140620850268,10.9498882404543));
#49178=CARTESIAN_POINT('Ctrl Pts',(2.95961338949625,3.66312942239435,11.0292601305077));
#49179=CARTESIAN_POINT('Ctrl Pts',(0.847091869118581,4.6325224171902,11.1086320205611));
#49180=CARTESIAN_POINT('Ctrl Pts',(-1.47177935557031,4.47344320507298,11.1880039106145));
#49181=CARTESIAN_POINT('Ctrl Pts',(-3.43212838697064,3.22464312999856,11.2673758006679));
#49182=CARTESIAN_POINT('Ctrl Pts',(-4.55641854019224,1.19032712608301,11.3467476907213));
#49183=CARTESIAN_POINT('Ctrl Pts',(-4.5707752224844,-1.13394993100199,11.4261195807747));
#49184=CARTESIAN_POINT('Ctrl Pts',(-3.47170117781866,-3.1819992948505,11.5054914708281));
#49185=CARTESIAN_POINT('Ctrl Pts',(-1.52692841071655,-4.45492067370938,
11.5848633608815));
#49186=CARTESIAN_POINT('Ctrl Pts',(0.789800737437414,-4.64263323725232,
11.6642352509349));
#49187=CARTESIAN_POINT('Ctrl Pts',(2.91413617414593,-3.69941062049495,11.7436071409883));
#49188=CARTESIAN_POINT('Ctrl Pts',(4.32859448916348,-1.85501976509151,11.8229790310417));
#49189=CARTESIAN_POINT('Ctrl Pts',(4.68861676780219,0.441249799071602,11.9023509210951));
#49190=CARTESIAN_POINT('Ctrl Pts',(3.90650237988148,2.63003188887072,11.9817228111485));
#49191=CARTESIAN_POINT('Ctrl Pts',(2.17277265911798,4.17814403201782,12.0610947012019));
#49192=CARTESIAN_POINT('Ctrl Pts',(-0.0902396720559702,4.70846953713027,
12.1404665912553));
#49193=CARTESIAN_POINT('Ctrl Pts',(-2.33126981885919,4.09182228501836,12.2198384813087));
#49194=CARTESIAN_POINT('Ctrl Pts',(-4.00440779796651,2.47841618137099,12.2992103713621));
#49195=CARTESIAN_POINT('Ctrl Pts',(-4.70208090109554,0.261273381822832,
12.3785822614155));
#49196=CARTESIAN_POINT('Ctrl Pts',(-4.25433750459725,-2.01951503521857,
12.4579541514689));
#49197=CARTESIAN_POINT('Ctrl Pts',(-2.7702469087954,-3.80835405980145,12.5373260415224));
#49198=CARTESIAN_POINT('Ctrl Pts',(-0.611330297848498,-4.66948646506541,
12.6166979315757));
#49199=CARTESIAN_POINT('Ctrl Pts',(1.69650502049761,-4.3931423031724,12.6960698216292));
#49200=CARTESIAN_POINT('Ctrl Pts',(3.59107547100067,-3.04663840028217,12.7754417116826));
#49201=CARTESIAN_POINT('Ctrl Pts',(4.61086788547872,-0.957980126702884,
12.854813601736));
#49202=CARTESIAN_POINT('Ctrl Pts',(4.50746308903707,1.36403998528818,12.9341854917894));
#49203=CARTESIAN_POINT('Ctrl Pts',(3.30605026120632,3.35378297611432,13.0135573818428));
#49204=CARTESIAN_POINT('Ctrl Pts',(1.29929090756384,4.52655185743172,13.0929292718962));
#49205=CARTESIAN_POINT('Ctrl Pts',(-1.02397283522957,4.59666272563134,13.1723011619496));
#49206=CARTESIAN_POINT('Ctrl Pts',(-3.09779906188647,3.54703672840752,13.251673052003));
#49207=CARTESIAN_POINT('Ctrl Pts',(-4.41700829392973,1.63336043537625,13.3310449420564));
#49208=CARTESIAN_POINT('Ctrl Pts',(-4.66024408245374,-0.67819884433063,
13.4104168321098));
#49209=CARTESIAN_POINT('Ctrl Pts',(-3.76825472776737,-2.82455038672626,
13.4897887221632));
#49210=CARTESIAN_POINT('Ctrl Pts',(-1.95832686228722,-4.28284770695163,
13.5691606122166));
#49211=CARTESIAN_POINT('Ctrl Pts',(0.328645092163131,-4.69785280568621,
13.64853250227));
#49212=CARTESIAN_POINT('Ctrl Pts',(2.53555982960612,-3.96847135947639,13.7279043923234));
#49213=CARTESIAN_POINT('Ctrl Pts',(4.12481780492351,-2.2723790741605,13.8072762823768));
#49214=CARTESIAN_POINT('Ctrl Pts',(4.7092792930909,-0.0227402762048894,
13.8866481724302));
#49215=CARTESIAN_POINT('Ctrl Pts',(4.14657076927425,2.23243800269952,13.9660200624836));
#49216=CARTESIAN_POINT('Ctrl Pts',(2.57376678434109,3.94379932556401,14.045391952537));
#49217=CARTESIAN_POINT('Ctrl Pts',(0.373998907678603,4.69445986217284,14.1247638425904));
#49218=CARTESIAN_POINT('Ctrl Pts',(-1.91687427506185,4.30156036736702,14.2041357326438));
#49219=CARTESIAN_POINT('Ctrl Pts',(-3.7408011273265,2.86081028841297,14.2835076226972));
#49220=CARTESIAN_POINT('Ctrl Pts',(-4.65347710509724,0.723173155497658,
14.3628795127506));
#49221=CARTESIAN_POINT('Ctrl Pts',(-4.43257636036315,-1.59062735738022,
14.442251402804));
#49222=CARTESIAN_POINT('Ctrl Pts',(-3.13190982558595,-3.51695456679423,
14.5216232928574));
#49223=CARTESIAN_POINT('Ctrl Pts',(-1.06831698966085,-4.58655942838405,
14.6009951829108));
#49224=CARTESIAN_POINT('Ctrl Pts',(1.25551550026611,-4.53888856539661,14.6803670729642));
#49225=CARTESIAN_POINT('Ctrl Pts',(3.27350719336465,-3.38555449453801,14.7597389630177));
#49226=CARTESIAN_POINT('Ctrl Pts',(4.49407977994485,-1.40750684260771,14.839110853071));
#49227=CARTESIAN_POINT('Ctrl Pts',(4.61990447960734,0.913406360718275,14.9184827431245));
#49228=CARTESIAN_POINT('Ctrl Pts',(3.62033067402261,3.01181579636398,14.9978546331779));
#49229=CARTESIAN_POINT('Ctrl Pts',(1.73885232971199,4.37655357055661,15.0772265232313));
#49230=CARTESIAN_POINT('Ctrl Pts',(-0.566206593232149,4.67517258229866,
15.1565984132847));
#49231=CARTESIAN_POINT('Ctrl Pts',(-2.73333884334193,3.83492990131171,15.2359703033381));
#49232=CARTESIAN_POINT('Ctrl Pts',(-4.23463580135657,2.06050678483865,15.3153421933915));
#49233=CARTESIAN_POINT('Ctrl Pts',(-4.70438485136804,-0.21585122356682,
15.3947140834449));
#49234=CARTESIAN_POINT('Ctrl Pts',(-4.02815616456562,-2.43962835168982,
15.4740859734983));
#49235=CARTESIAN_POINT('Ctrl Pts',(-2.3706775522472,-4.06911741336723,15.5534578635517));
#49236=CARTESIAN_POINT('Ctrl Pts',(-0.135707135607595,-4.70737847998642,
15.6328297536051));
#49237=CARTESIAN_POINT('Ctrl Pts',(2.13232123888424,-4.19893256848759,15.7122016436585));
#49238=CARTESIAN_POINT('Ctrl Pts',(3.88092087939525,-2.66763597748263,15.7915735337119));
#49239=CARTESIAN_POINT('Ctrl Pts',(4.6841367839613,-0.486509167079024,15.8709454237653));
#49240=CARTESIAN_POINT('Ctrl Pts',(4.34630733610955,1.81313019956284,15.9503173138187));
#49241=CARTESIAN_POINT('Ctrl Pts',(2.94972704158046,3.67109506287253,16.0296892038721));
#49242=CARTESIAN_POINT('Ctrl Pts',(0.834599768811967,4.63478929472454,16.1090610939255));
#49243=CARTESIAN_POINT('Ctrl Pts',(-1.48383416024523,4.46945911326284,16.1884329839789));
#49244=CARTESIAN_POINT('Ctrl Pts',(-3.44080937235088,3.21537858488636,16.2678048740323));
#49245=CARTESIAN_POINT('Ctrl Pts',(-4.55961103731638,1.17803895016983,16.3471767640857));
#49246=CARTESIAN_POINT('Ctrl Pts',(-4.5677015463797,-1.14626836492032,16.4265486541391));
#49247=CARTESIAN_POINT('Ctrl Pts',(-3.4631100686894,-3.19134724418507,16.5059205441925));
#49248=CARTESIAN_POINT('Ctrl Pts',(-1.51491264465833,-4.45902099747165,
16.5852924342459));
#49249=CARTESIAN_POINT('Ctrl Pts',(0.802314148161232,-4.64048710795702,
16.6646643242993));
#49250=CARTESIAN_POINT('Ctrl Pts',(2.92409898707282,-3.69154082613136,16.7440362143527));
#49251=CARTESIAN_POINT('Ctrl Pts',(4.33357979136326,-1.84334337837345,16.8234081044061));
#49252=CARTESIAN_POINT('Ctrl Pts',(4.68741013889918,0.453888451717908,16.9027799944596));
#49253=CARTESIAN_POINT('Ctrl Pts',(3.89939777427618,2.64055403030628,16.9821518845129));
#49254=CARTESIAN_POINT('Ctrl Pts',(2.16150070095874,4.18398654725935,17.0615237745663));
#49255=CARTESIAN_POINT('Ctrl Pts',(-0.102933079310061,4.70820909782832,
17.1408956646198));
#49256=CARTESIAN_POINT('Ctrl Pts',(-2.34229273922368,4.08552253105771,17.2202675546731));
#49257=CARTESIAN_POINT('Ctrl Pts',(-4.01107478934828,2.46761134605149,17.2996394447266));
#49258=CARTESIAN_POINT('Ctrl Pts',(-4.70276843368481,0.248596203073432,
17.37901133478));
#49259=CARTESIAN_POINT('Ctrl Pts',(-4.24887708766866,-2.03097775393694,
17.4583832248334));
#49260=CARTESIAN_POINT('Ctrl Pts',(-2.75997059360591,-3.81580751573978,
17.5377551148868));
#49261=CARTESIAN_POINT('Ctrl Pts',(-0.598737773532647,-4.6711197519463,
17.6171270049402));
#49262=CARTESIAN_POINT('Ctrl Pts',(1.70833944819094,-4.38854860755889,17.6964988949936));
#49263=CARTESIAN_POINT('Ctrl Pts',(3.5992817914533,-3.03695363259626,17.775870785047));
#49264=CARTESIAN_POINT('Ctrl Pts',(4.61342283197251,-0.945531571192997,
17.8552426751004));
#49265=CARTESIAN_POINT('Ctrl Pts',(4.50379002440264,1.37615964733967,17.9346145651538));
#49266=CARTESIAN_POINT('Ctrl Pts',(3.29695756540449,3.36273516855535,18.0139864552072));
#49267=CARTESIAN_POINT('Ctrl Pts',(1.28715662605536,4.52994106929151,18.0933583452606));
#49268=CARTESIAN_POINT('Ctrl Pts',(-1.03650075501039,4.59406889295398,18.172730235314));
#49269=CARTESIAN_POINT('Ctrl Pts',(-3.10708740551261,3.53832597274458,18.2521021253674));
#49270=CARTESIAN_POINT('Ctrl Pts',(-4.42189226956141,1.62210042840545,18.3314740154208));
#49271=CARTESIAN_POINT('Ctrl Pts',(-4.65746145505438,-0.691994213306935,
18.4108459054742));
#49272=CARTESIAN_POINT('Ctrl Pts',(-3.7623932789572,-2.83237457985889,18.4902177955276));
#49273=CARTESIAN_POINT('Ctrl Pts',(-1.94345928697736,-4.29245481019949,
18.569589685581));
#49274=CARTESIAN_POINT('Ctrl Pts',(0.335233909124166,-4.68912434583344,
18.6489615756345));
#49275=CARTESIAN_POINT('Ctrl Pts',(3.29668819545067,-3.73492805813089,18.7547907623723));
#49276=CARTESIAN_POINT('Ctrl Pts',(5.339103029404,-0.0175478502153651,18.8870772457947));
#49277=CARTESIAN_POINT('Ctrl Pts',(2.90621803008022,4.48249178265512,19.0458210259014));
#49278=CARTESIAN_POINT('Ctrl Pts',(-2.18656320946377,4.86959394496076,19.2045648060083));
#49279=CARTESIAN_POINT('Ctrl Pts',(-5.27828887711238,0.806568563691633,
19.363308586115));
#49280=CARTESIAN_POINT('Ctrl Pts',(-3.54020456892039,-3.99752392897296,
19.5220523662219));
#49281=CARTESIAN_POINT('Ctrl Pts',(1.43734916996113,-5.14215993940115,19.6807961463287));
#49282=CARTESIAN_POINT('Ctrl Pts',(5.09974667860479,-1.58211192901293,19.8395399264355));
#49283=CARTESIAN_POINT('Ctrl Pts',(4.09539160933933,3.42571876325583,19.9982837065423));
#49284=CARTESIAN_POINT('Ctrl Pts',(-0.656009676029552,5.29932988758688,
20.1570274866491));
#49285=CARTESIAN_POINT('Ctrl Pts',(-4.80798654830356,2.32253130646633,20.3157712667559));
#49286=CARTESIAN_POINT('Ctrl Pts',(-4.5587807483591,-2.77696271962182,20.4745150468627));
#49287=CARTESIAN_POINT('Ctrl Pts',(-0.141143605831918,-5.34031031892967,
20.6332588269695));
#49288=CARTESIAN_POINT('Ctrl Pts',(4.41154214902265,-3.00742829557661,20.7920026070763));
#49289=CARTESIAN_POINT('Ctrl Pts',(4.83176599740626,1.2132097937891,20.9242890904987));
#49290=CARTESIAN_POINT('Ctrl Pts',(2.93038174053082,3.67602118591258,21.0301182772365));
#49291=CARTESIAN_POINT('Ctrl Pts',(0.82729199276626,4.63872722375956,21.1094901672899));
#49292=CARTESIAN_POINT('Ctrl Pts',(-1.49865065220701,4.46452630956661,21.1888620573433));
#49293=CARTESIAN_POINT('Ctrl Pts',(-3.44799414715959,3.20657754587673,21.2682339473967));
#49294=CARTESIAN_POINT('Ctrl Pts',(-4.56354990278301,1.16548416044547,21.3476058374502));
#49295=CARTESIAN_POINT('Ctrl Pts',(-4.56418179760212,-1.1584417781363,21.4269777275035));
#49296=CARTESIAN_POINT('Ctrl Pts',(-3.45471245456607,-3.20074439226419,
21.506349617557));
#49297=CARTESIAN_POINT('Ctrl Pts',(-1.50277006074114,-4.46305057284728,
21.5857215076104));
#49298=CARTESIAN_POINT('Ctrl Pts',(0.814760394348267,-4.63832755437973,
21.6650933976638));
#49299=CARTESIAN_POINT('Ctrl Pts',(2.93407303175,-3.6836334512587,21.7444652877172));
#49300=CARTESIAN_POINT('Ctrl Pts',(4.33851638857388,-1.83165928184362,21.8238371777706));
#49301=CARTESIAN_POINT('Ctrl Pts',(4.68617856238765,0.466526807638465,21.903209067824));
#49302=CARTESIAN_POINT('Ctrl Pts',(3.89225998228531,2.65105540897445,21.9825809578774));
#49303=CARTESIAN_POINT('Ctrl Pts',(2.1502156260726,4.18979944864558,22.0619528479308));
#49304=CARTESIAN_POINT('Ctrl Pts',(-0.115627163561327,4.70791408521783,
22.1413247379842));
#49305=CARTESIAN_POINT('Ctrl Pts',(-2.35329778315663,4.07919314165102,22.2206966280376));
#49306=CARTESIAN_POINT('Ctrl Pts',(-4.01771326340777,2.45678878743819,22.300068518091));
#49307=CARTESIAN_POINT('Ctrl Pts',(-4.7034211013359,0.235916647177708,22.3794404081444));
#49308=CARTESIAN_POINT('Ctrl Pts',(-4.24338680893675,-2.04242454395301,
22.4588122981978));
#49309=CARTESIAN_POINT('Ctrl Pts',(-2.74967243806091,-3.82323548987737,
22.5381841882512));
#49310=CARTESIAN_POINT('Ctrl Pts',(-0.586144182924564,-4.67271481097619,
22.6175560783046));
#49311=CARTESIAN_POINT('Ctrl Pts',(1.7201676224087,-4.38393110573301,22.696927968358));
#49312=CARTESIAN_POINT('Ctrl Pts',(3.60745033643733,-3.02723150865538,22.7762998584114));
#49313=CARTESIAN_POINT('Ctrl Pts',(4.61596616842609,-0.933105005158016,
22.8556717484649));
#49314=CARTESIAN_POINT('Ctrl Pts',(4.50004284053894,1.38832380607303,22.9350436385182));
#49315=CARTESIAN_POINT('Ctrl Pts',(3.28791904717806,3.37156001439376,23.0144155285717));
#49316=CARTESIAN_POINT('Ctrl Pts',(1.27486544641681,4.53349166431032,23.093787418625));
#49317=CARTESIAN_POINT('Ctrl Pts',(-1.04874255247445,4.59107478042505,23.1731593086785));
#49318=CARTESIAN_POINT('Ctrl Pts',(-3.11687918839179,3.53028224171763,23.2525311987318));
#49319=CARTESIAN_POINT('Ctrl Pts',(-4.42575095234051,1.60952076333037,23.3319030887853));
#49320=CARTESIAN_POINT('Ctrl Pts',(-4.6565195809412,-0.703316410525592,
23.4112749788386));
#49321=CARTESIAN_POINT('Ctrl Pts',(-3.75297034643954,-2.84482726347037,
23.4906468688921));
#49322=CARTESIAN_POINT('Ctrl Pts',(-1.93520584271877,-4.29334449199004,
23.5700187589454));
#49323=CARTESIAN_POINT('Ctrl Pts',(0.353970520843478,-4.69601250539774,
23.6493906489989));
#49324=CARTESIAN_POINT('Ctrl Pts',(2.55692044899663,-3.95474226694855,23.7287625390522));
#49325=CARTESIAN_POINT('Ctrl Pts',(4.13701021543862,-2.25010556593857,23.8081344291057));
#49326=CARTESIAN_POINT('Ctrl Pts',(4.70933345050753,0.00265187040687223,
23.887506319159));
#49327=CARTESIAN_POINT('Ctrl Pts',(4.13447348097035,2.25476331699259,23.9668782092125));
#49328=CARTESIAN_POINT('Ctrl Pts',(2.55246492296808,3.95761941039203,24.0462500992659));
#49329=CARTESIAN_POINT('Ctrl Pts',(0.348681559517371,4.69640817546236,24.1256219893193));
#49330=CARTESIAN_POINT('Ctrl Pts',(-1.94003986003887,4.29116230431301,24.2049938793727));
#49331=CARTESIAN_POINT('Ctrl Pts',(-3.75617186389469,2.84059879415982,24.2843657694261));
#49332=CARTESIAN_POINT('Ctrl Pts',(-4.65730871585138,0.698071705307978,
24.3637376594795));
#49333=CARTESIAN_POINT('Ctrl Pts',(-4.42393547340455,-1.61450410580135,
24.4431095495329));
#49334=CARTESIAN_POINT('Ctrl Pts',(-3.11290134185147,-3.5337902903817,24.5224814395863));
#49335=CARTESIAN_POINT('Ctrl Pts',(-1.0435713337136,-4.59225298213718,24.6018533296397));
#49336=CARTESIAN_POINT('Ctrl Pts',(1.27997034141094,-4.5320530122236,24.6812252196931));
#49337=CARTESIAN_POINT('Ctrl Pts',(3.29171407453406,-3.36785496006151,24.7605971097465));
#49338=CARTESIAN_POINT('Ctrl Pts',(4.50160354518617,-1.38325489424899,24.8399689997999));
#49339=CARTESIAN_POINT('Ctrl Pts',(4.61491235636141,0.938303002019797,24.9193408898533));
#49340=CARTESIAN_POINT('Ctrl Pts',(3.60403873246226,3.03129236389504,24.9987127799067));
#49341=CARTESIAN_POINT('Ctrl Pts',(1.71522925073975,4.3858656155773,25.0780846699601));
#49342=CARTESIAN_POINT('Ctrl Pts',(-0.591406279867446,4.67205171125385,
25.1574565600135));
#49343=CARTESIAN_POINT('Ctrl Pts',(-2.75397654975454,3.82013635147998,25.2368284500669));
#49344=CARTESIAN_POINT('Ctrl Pts',(-4.2456842279451,2.03764423221396,25.3162003401203));
#49345=CARTESIAN_POINT('Ctrl Pts',(-4.70315262587087,-0.24121351177037,
25.3955722301737));
#49346=CARTESIAN_POINT('Ctrl Pts',(-4.01494345438624,-2.4613121782045,25.4749441202271));
#49347=CARTESIAN_POINT('Ctrl Pts',(-2.34870294433969,-4.08184064605008,
25.5543160102806));
#49348=CARTESIAN_POINT('Ctrl Pts',(-0.110323595817837,-4.70804176751889,
25.6336879003339));
#49349=CARTESIAN_POINT('Ctrl Pts',(2.15493033644811,-4.1873743354938,25.7130597903874));
#49350=CARTESIAN_POINT('Ctrl Pts',(3.89524800861274,-2.64667178393831,25.7924316804407));
#49351=CARTESIAN_POINT('Ctrl Pts',(4.68669188786451,-0.461245844124039,
25.8718035704942));
#49352=CARTESIAN_POINT('Ctrl Pts',(4.33646799704899,1.83653856236848,25.9511754605475));
#49353=CARTESIAN_POINT('Ctrl Pts',(2.92989010076147,3.68694624017715,26.030547350601));
#49354=CARTESIAN_POINT('Ctrl Pts',(0.809597461130217,4.63922197479579,26.1099192406544));
#49355=CARTESIAN_POINT('Ctrl Pts',(-1.50791132801882,4.46139350509784,26.1892911307078));
#49356=CARTESIAN_POINT('Ctrl Pts',(-3.45809625536759,3.19677945268506,26.2686630207611));
#49357=CARTESIAN_POINT('Ctrl Pts',(-4.56589658927499,1.15343700154949,26.3480349108146));
#49358=CARTESIAN_POINT('Ctrl Pts',(-4.56145462047572,-1.170880150074,26.427406800868));
#49359=CARTESIAN_POINT('Ctrl Pts',(-3.44585240273711,-3.20997348883872,
26.5067786909214));
#49360=CARTESIAN_POINT('Ctrl Pts',(-1.49084816695666,-4.46712439087817,
26.5861505809748));
#49361=CARTESIAN_POINT('Ctrl Pts',(0.827323382358012,-4.6360936791118,26.6655224710282));
#49362=CARTESIAN_POINT('Ctrl Pts',(2.9439607869795,-3.67572080893307,26.7448943610816));
#49363=CARTESIAN_POINT('Ctrl Pts',(4.34345586023946,-1.81995048576826,26.824266251135));
#49364=CARTESIAN_POINT('Ctrl Pts',(4.68489470002155,0.479155747337646,26.9036381411885));
#49365=CARTESIAN_POINT('Ctrl Pts',(3.88510356071688,2.66154070098535,26.9830100312418));
#49366=CARTESIAN_POINT('Ctrl Pts',(2.13890979355249,4.1955802310934,27.0623819212952));
#49367=CARTESIAN_POINT('Ctrl Pts',(-0.128317664924755,4.70758570366646,
27.1417538113486));
#49368=CARTESIAN_POINT('Ctrl Pts',(-2.36428722425266,4.07283371889059,27.221125701402));
#49369=CARTESIAN_POINT('Ctrl Pts',(-4.02432164901364,2.44594845525754,27.3004975914554));
#49370=CARTESIAN_POINT('Ctrl Pts',(-4.70404022775981,0.223235561938782,
27.3798694815088));
#49371=CARTESIAN_POINT('Ctrl Pts',(-4.2378650192401,-2.05385702014473,27.4592413715622));
#49372=CARTESIAN_POINT('Ctrl Pts',(-2.73935527238859,-3.83063457825638,
27.5386132616157));
#49373=CARTESIAN_POINT('Ctrl Pts',(-0.573544644643281,-4.67427803207058,
27.617985151669));
#49374=CARTESIAN_POINT('Ctrl Pts',(1.73198018901762,-4.37927770361132,27.6973570417225));
#49375=CARTESIAN_POINT('Ctrl Pts',(3.61559848230692,-3.01749501991908,27.7767289317758));
#49376=CARTESIAN_POINT('Ctrl Pts',(4.61846498829774,-0.920657228486544,
27.8561008218292));
#49377=CARTESIAN_POINT('Ctrl Pts',(4.49628364593812,1.4004506259651,27.9354727118827));
#49378=CARTESIAN_POINT('Ctrl Pts',(3.278817559783,3.38041180777658,28.014844601936));
#49379=CARTESIAN_POINT('Ctrl Pts',(1.2626387736043,4.53691215562828,28.0942164919895));
#49380=CARTESIAN_POINT('Ctrl Pts',(-1.0611160230209,4.58823074465364,28.1735883820429));
#49381=CARTESIAN_POINT('Ctrl Pts',(-3.12638530517863,3.52186648015787,28.2529602720962));
#49382=CARTESIAN_POINT('Ctrl Pts',(-4.43007404713138,1.59758333661492,28.3323321621497));
#49383=CARTESIAN_POINT('Ctrl Pts',(-4.65460655700551,-0.715867571536754,
28.4117040522031));
#49384=CARTESIAN_POINT('Ctrl Pts',(-3.74528721238995,-2.85493472380806,
28.4910759422565));
#49385=CARTESIAN_POINT('Ctrl Pts',(-1.9236241928888,-4.29854609665053,28.5704478323099));
#49386=CARTESIAN_POINT('Ctrl Pts',(0.366629422130075,-4.69504115501931,
28.6498197223633));
#49387=CARTESIAN_POINT('Ctrl Pts',(2.56757292143854,-3.94783458032276,28.7291916124167));
#49388=CARTESIAN_POINT('Ctrl Pts',(4.14306134031087,-2.23894424024318,28.8085635024701));
#49389=CARTESIAN_POINT('Ctrl Pts',(4.70930918719419,0.0153479609406268,
28.8879353925235));
#49390=CARTESIAN_POINT('Ctrl Pts',(4.12837973995606,2.26590143281143,28.9673072825769));
#49391=CARTESIAN_POINT('Ctrl Pts',(2.54178612607819,3.96448633113712,29.0466791726303));
#49392=CARTESIAN_POINT('Ctrl Pts',(0.336019038035816,4.69733113443944,29.1260510626837));
#49393=CARTESIAN_POINT('Ctrl Pts',(-1.95160154390656,4.2859164707584,29.2054229527371));
#49394=CARTESIAN_POINT('Ctrl Pts',(-3.76381630954999,2.83046204151583,29.2847948427905));
#49395=CARTESIAN_POINT('Ctrl Pts',(-4.65917375325318,0.68551332408149,29.364166732844));
#49396=CARTESIAN_POINT('Ctrl Pts',(-4.41956678357008,-1.62642492174114,
29.4435386228973));
#49397=CARTESIAN_POINT('Ctrl Pts',(-3.10336312795443,-3.54216965665813,
29.5229105129507));
#49398=CARTESIAN_POINT('Ctrl Pts',(-1.03118708354684,-4.59504970367272,
29.6022824030041));
#49399=CARTESIAN_POINT('Ctrl Pts',(1.29218385191882,-4.52858581384264,29.6816542930575));
#49400=CARTESIAN_POINT('Ctrl Pts',(3.30078166125751,-3.3589684436152,29.761026183111));
#49401=CARTESIAN_POINT('Ctrl Pts',(4.50531636407018,-1.37111379547362,29.8403980731643));
#49402=CARTESIAN_POINT('Ctrl Pts',(4.61236597294397,0.950741138336453,29.9197699632178));
#49403=CARTESIAN_POINT('Ctrl Pts',(3.59585344010749,3.04099763527755,29.9991418532711));
#49404=CARTESIAN_POINT('Ctrl Pts',(1.70339896854746,4.39047383939912,30.0785137433246));
#49405=CARTESIAN_POINT('Ctrl Pts',(-0.603999721341074,4.67044033439209,
30.157885633378));
#49406=CARTESIAN_POINT('Ctrl Pts',(-2.76426541604165,3.81269790177148,30.2372575234314));
#49407=CARTESIAN_POINT('Ctrl Pts',(-4.25116217399222,2.02619069954299,30.3166294134847));
#49408=CARTESIAN_POINT('Ctrl Pts',(-4.70248523614609,-0.253892072197153,
30.3960013035382));
#49409=CARTESIAN_POINT('Ctrl Pts',(-4.00829330354932,-2.47212729713062,
30.4753731935915));
#49410=CARTESIAN_POINT('Ctrl Pts',(-2.33768999441463,-4.08815778444404,
30.554745083645));
#49411=CARTESIAN_POINT('Ctrl Pts',(-0.0976305770295779,-4.70832208445062,
30.6341169736984));
#49412=CARTESIAN_POINT('Ctrl Pts',(2.16621143281822,-4.18154954637921,30.7134888637517));
#49413=CARTESIAN_POINT('Ctrl Pts',(3.90236913245919,-2.63616079451278,30.7928607538052));
#49414=CARTESIAN_POINT('Ctrl Pts',(4.68791834918069,-0.448609108145992,
30.8722326438586));
#49415=CARTESIAN_POINT('Ctrl Pts',(4.33150103257305,1.84822276398574,30.951604533912));
#49416=CARTESIAN_POINT('Ctrl Pts',(2.91993965204555,3.69483166178228,31.0309764239654));
#49417=CARTESIAN_POINT('Ctrl Pts',(0.797087435456495,4.64138774513982,31.1103483140188));
#49418=CARTESIAN_POINT('Ctrl Pts',(-1.51993351608663,4.45731204731877,31.1897202040722));
#49419=CARTESIAN_POINT('Ctrl Pts',(-3.46670202742684,3.18744500086376,31.2690920941256));
#49420=CARTESIAN_POINT('Ctrl Pts',(-4.56898959830062,1.14112340748814,31.348463984179));
#49421=CARTESIAN_POINT('Ctrl Pts',(-4.5582814163153,-1.18317332211776,31.4278358742324));
#49422=CARTESIAN_POINT('Ctrl Pts',(-3.43718597090036,-3.21925164936547,
31.5072077642858));
#49423=CARTESIAN_POINT('Ctrl Pts',(-1.47879963105622,-4.47112740052042,
31.5865796543392));
#49424=CARTESIAN_POINT('Ctrl Pts',(0.839819025645787,-4.63384641358128,
31.6659515443926));
#49425=CARTESIAN_POINT('Ctrl Pts',(2.95385962660838,-3.66777069713875,31.745323434446));
#49426=CARTESIAN_POINT('Ctrl Pts',(4.34834656078651,-1.80823415734596,31.8246953244994));
#49427=CARTESIAN_POINT('Ctrl Pts',(4.68358589765892,0.491784220717852,31.9040672145528));
#49428=CARTESIAN_POINT('Ctrl Pts',(3.87791407680318,2.67200505116071,31.9834391046062));
#49429=CARTESIAN_POINT('Ctrl Pts',(2.12759097045539,4.20133136552371,32.0628109946597));
#49430=CARTESIAN_POINT('Ctrl Pts',(-0.141008586952624,4.70722265873437,
32.142182884713));
#49431=CARTESIAN_POINT('Ctrl Pts',(-2.37525876469618,4.06644493153793,32.2215547747665));
#49432=CARTESIAN_POINT('Ctrl Pts',(-4.03090116490581,2.43509021994207,32.3009266648198));
#49433=CARTESIAN_POINT('Ctrl Pts',(-4.7046249635928,0.21055292074912,32.3802985548733));
#49434=CARTESIAN_POINT('Ctrl Pts',(-4.23231253465933,-2.06527460388738,
32.4596704449267));
#49435=CARTESIAN_POINT('Ctrl Pts',(-2.72901814034772,-3.83800580642471,
32.5390423349801));
#49436=CARTESIAN_POINT('Ctrl Pts',(-0.560940967626579,-4.67580728979871,
32.6184142250335));
#49437=CARTESIAN_POINT('Ctrl Pts',(1.74378018318661,-4.37459246710163,32.6977861150869));
#49438=CARTESIAN_POINT('Ctrl Pts',(3.62372034116752,-3.00773660241476,32.7771580051403));
#49439=CARTESIAN_POINT('Ctrl Pts',(4.62093024500891,-0.90820275889168,32.8565298951936));
#49440=CARTESIAN_POINT('Ctrl Pts',(4.49249176942175,1.41256726642465,32.9359017852471));
#49441=CARTESIAN_POINT('Ctrl Pts',(3.26969224276534,3.38923903230456,33.0152736753005));
#49442=CARTESIAN_POINT('Ctrl Pts',(1.25040292311233,4.54029967186844,33.0946455653539));
#49443=CARTESIAN_POINT('Ctrl Pts',(-1.0734817808909,4.58535336114807,33.1740174554073));
#49444=CARTESIAN_POINT('Ctrl Pts',(-3.13586869918079,3.51342512115953,33.2533893454607));
#49445=CARTESIAN_POINT('Ctrl Pts',(-4.43436494347784,1.58563429849111,33.3327612355141));
#49446=CARTESIAN_POINT('Ctrl Pts',(-4.65265970284399,-0.728413529547759,
33.4121331255675));
#49447=CARTESIAN_POINT('Ctrl Pts',(-3.73757685708491,-2.8650214341048,33.4915050156209));
#49448=CARTESIAN_POINT('Ctrl Pts',(-1.91202856192598,-4.30371645893127,
33.5708769056743));
#49449=CARTESIAN_POINT('Ctrl Pts',(0.379285658714694,-4.69403568047687,
33.6502487957277));
#49450=CARTESIAN_POINT('Ctrl Pts',(2.57820673242699,-3.94089820033005,33.7296206857811));
#49451=CARTESIAN_POINT('Ctrl Pts',(4.14908235288389,-2.22776664161308,33.8089925758346));
#49452=CARTESIAN_POINT('Ctrl Pts',(4.70925069601633,0.0280439399230538,
33.8883644658879));
#49453=CARTESIAN_POINT('Ctrl Pts',(4.12225599334877,2.27702307976815,33.9677363559414));
#49454=CARTESIAN_POINT('Ctrl Pts',(2.53108885516031,3.9713244374868,34.0471082459947));
#49455=CARTESIAN_POINT('Ctrl Pts',(0.323354074324944,4.69821995261122,34.1264801360482));
#49456=CARTESIAN_POINT('Ctrl Pts',(-1.96314904328387,4.28063948661298,34.2058520261016));
#49457=CARTESIAN_POINT('Ctrl Pts',(-3.77143339930544,2.8203047167106,34.2852239161549));
#49458=CARTESIAN_POINT('Ctrl Pts',(-4.66100492718239,0.672949960456159,
34.3645958062084));
#49459=CARTESIAN_POINT('Ctrl Pts',(-4.41516597175719,-1.63833391661592,
34.4439676962618));
#49460=CARTESIAN_POINT('Ctrl Pts',(-3.09380235841604,-3.55052327799099,
34.5233395863151));
#49461=CARTESIAN_POINT('Ctrl Pts',(-1.01879533858015,-4.59781302779744,
34.6027114763686));
#49462=CARTESIAN_POINT('Ctrl Pts',(1.30438797066869,-4.52508570111899,34.6820833664219));
#49463=CARTESIAN_POINT('Ctrl Pts',(3.30982525747642,-3.35005751375522,34.7614552564754));
#49464=CARTESIAN_POINT('Ctrl Pts',(4.50899643773683,-1.3589627312672,34.8408271465288));
#49465=CARTESIAN_POINT('Ctrl Pts',(4.60978606625886,0.963172364544519,34.9201990365822));
#49466=CARTESIAN_POINT('Ctrl Pts',(3.58764201262861,3.05068080429907,34.9995709266356));
#49467=CARTESIAN_POINT('Ctrl Pts',(1.69155630583291,4.39505015269376,35.078942816689));
#49468=CARTESIAN_POINT('Ctrl Pts',(-0.616588772867267,4.66879501217076,
35.1583147067424));
#49469=CARTESIAN_POINT('Ctrl Pts',(-2.77453419129308,3.80523174088547,35.2376865967958));
#49470=CARTESIAN_POINT('Ctrl Pts',(-4.2566092220472,2.01472244025804,35.3170584868492));
#49471=CARTESIAN_POINT('Ctrl Pts',(-4.70178366815532,-0.266568787303772,
35.3964303769026));
#49472=CARTESIAN_POINT('Ctrl Pts',(-4.00161401992238,-2.48292444831838,
35.475802266956));
#49473=CARTESIAN_POINT('Ctrl Pts',(-2.3266600538588,-4.09444520958265,35.5551741570094));
#49474=CARTESIAN_POINT('Ctrl Pts',(-0.0849368486498902,-4.70856818069336,
35.6345460470628));
#49475=CARTESIAN_POINT('Ctrl Pts',(2.17747678488564,-4.17569436522607,35.7139179371162));
#49476=CARTESIAN_POINT('Ctrl Pts',(3.90946189338614,-2.62563064513239,35.7932898271696));
#49477=CARTESIAN_POINT('Ctrl Pts',(4.68911073810487,-0.435969111619298,
35.872661717223));
#49478=CARTESIAN_POINT('Ctrl Pts',(4.32650258619184,1.85989353248294,35.9520336072764));
#49479=CARTESIAN_POINT('Ctrl Pts',(2.90996798083354,3.70269022887686,36.0314054973299));
#49480=CARTESIAN_POINT('Ctrl Pts',(0.784571616449035,4.64351978128221,36.1107773873832));
#49481=CARTESIAN_POINT('Ctrl Pts',(-1.53194465708265,4.4531981932239,36.1901492774366));
#49482=CARTESIAN_POINT('Ctrl Pts',(-3.47528260305097,3.17808738228323,36.2695211674901));
#49483=CARTESIAN_POINT('Ctrl Pts',(-4.57204939932363,1.12880151959547,36.3488930575434));
#49484=CARTESIAN_POINT('Ctrl Pts',(-4.55507508198074,-1.19545789470598,
36.4282649475969));
#49485=CARTESIAN_POINT('Ctrl Pts',(-3.42849455715498,-3.2285064119582,36.5076368376502));
#49486=CARTESIAN_POINT('Ctrl Pts',(-1.4667403470503,-4.47509791343512,36.5870087277037));
#49487=CARTESIAN_POINT('Ctrl Pts',(0.852308565021146,-4.63156546866048,
36.6663806177571));
#49488=CARTESIAN_POINT('Ctrl Pts',(2.96373699720644,-3.65979392751645,36.7457525078104));
#49489=CARTESIAN_POINT('Ctrl Pts',(4.35320565699285,-1.79650468644589,36.8251243978639));
#49490=CARTESIAN_POINT('Ctrl Pts',(4.68224305439311,0.504409119747259,36.9044962879172));
#49491=CARTESIAN_POINT('Ctrl Pts',(3.87069640771237,2.68244998086059,36.9838681779707));
#49492=CARTESIAN_POINT('Ctrl Pts',(2.1162566837541,4.20705196413867,37.0632400680241));
#49493=CARTESIAN_POINT('Ctrl Pts',(-0.153698484112011,4.70682540110399,
37.1426119580775));
#49494=CARTESIAN_POINT('Ctrl Pts',(-2.38621304145417,4.06002658874194,37.2219838481309));
#49495=CARTESIAN_POINT('Ctrl Pts',(-4.03745138369124,2.42421428607825,37.3013557381843));
#49496=CARTESIAN_POINT('Ctrl Pts',(-4.7051755056078,0.197868749234187,37.3807276282377));
#49497=CARTESIAN_POINT('Ctrl Pts',(-4.22672928908836,-2.07667717695002,
37.4600995182911));
#49498=CARTESIAN_POINT('Ctrl Pts',(-2.71866117345227,-3.84534913947293,
37.5394714083445));
#49499=CARTESIAN_POINT('Ctrl Pts',(-0.548333213620079,-4.67730256316236,
37.6188432983979));
#49500=CARTESIAN_POINT('Ctrl Pts',(1.75556750333961,-4.36987543548734,37.6982151884513));
#49501=CARTESIAN_POINT('Ctrl Pts',(3.63181586235974,-2.99795632430491,37.7775870785047));
#49502=CARTESIAN_POINT('Ctrl Pts',(4.62336191621364,-0.895741688343936,
37.8569589685581));
#49503=CARTESIAN_POINT('Ctrl Pts',(4.48866724088475,1.42467364012841,37.9363308586115));
#49504=CARTESIAN_POINT('Ctrl Pts',(3.26054316123161,3.3980416234756,38.0157027486649));
#49505=CARTESIAN_POINT('Ctrl Pts',(1.23815798448111,4.54365418850126,38.0950746387183));
#49506=CARTESIAN_POINT('Ctrl Pts',(-1.08583973646279,4.58244265094544,38.1744465287717));
#49507=CARTESIAN_POINT('Ctrl Pts',(-3.1453293014664,3.50495822568428,38.2538184188251));
#49508=CARTESIAN_POINT('Ctrl Pts',(-4.43862360995231,1.57367373662757,38.3331903088785));
#49509=CARTESIAN_POINT('Ctrl Pts',(-4.65067903319431,-0.740954194968168,
38.412562198932));
#49510=CARTESIAN_POINT('Ctrl Pts',(-3.72983933538423,-2.87508731801368,
38.4919340889853));
#49511=CARTESIAN_POINT('Ctrl Pts',(-1.9004190363744,-4.30885554699714,38.5713059790388));
#49512=CARTESIAN_POINT('Ctrl Pts',(0.391939142907767,-4.69299607822647,
38.6506778690921));
#49513=CARTESIAN_POINT('Ctrl Pts',(2.588821796549,-3.93393319787887,38.7300497591456));
#49514=CARTESIAN_POINT('Ctrl Pts',(4.15507322474385,-2.21657281258971,38.8094216491989));
#49515=CARTESIAN_POINT('Ctrl Pts',(4.70915794841682,0.040739642006525,38.8887935392524));
#49516=CARTESIAN_POINT('Ctrl Pts',(4.11610234038245,2.28812831500406,38.9681654293058));
#49517=CARTESIAN_POINT('Ctrl Pts',(2.52037308462918,3.97813341921603,39.0475373193591));
#49518=CARTESIAN_POINT('Ctrl Pts',(0.310686955552019,4.69907511544173,39.1269092094126));
#49519=CARTESIAN_POINT('Ctrl Pts',(-1.97468264266246,4.27533046137757,39.2062810994659));
#49520=CARTESIAN_POINT('Ctrl Pts',(-3.77902238214566,2.81012864743349,39.2856529895194));
#49521=CARTESIAN_POINT('Ctrl Pts',(-4.66280353786911,0.660378394081937,
39.3650248795728));
#49522=CARTESIAN_POINT('Ctrl Pts',(-4.41073058968569,-1.65022475069991,
39.4443967696262));
#49523=CARTESIAN_POINT('Ctrl Pts',(-3.0842237862698,-3.55886290155649,39.5237686596796));
#49524=CARTESIAN_POINT('Ctrl Pts',(-1.00638734295308,-4.60052063353569,
39.603140549733));
#49525=CARTESIAN_POINT('Ctrl Pts',(1.3165658861068,-4.521594850557,39.6825124397864));
#49526=CARTESIAN_POINT('Ctrl Pts',(3.31887653668104,-3.34104229843822,39.7618843298398));
#49527=CARTESIAN_POINT('Ctrl Pts',(4.51258247789865,-1.34695556252384,39.8412562198932));
#49528=CARTESIAN_POINT('Ctrl Pts',(4.60729903172253,0.975909964327458,39.9206281099466));
#49529=CARTESIAN_POINT('Ctrl Pts',(3.92183073605334,2.36502208507764,39.9735427033156));
#49530=CARTESIAN_POINT('Ctrl Pts',(3.43378788736169,2.9358415841302,40.));
#49531=CARTESIAN_POINT('Ctrl Pts',(4.5177656910975,-0.000116631996953637,
0.887416697508071));
#49532=CARTESIAN_POINT('Ctrl Pts',(4.51716522512143,0.582848551743655,0.907954496247182));
#49533=CARTESIAN_POINT('Ctrl Pts',(4.40381632429852,1.16604045169665,0.928492294986294));
#49534=CARTESIAN_POINT('Ctrl Pts',(4.18378127438632,1.70573618195762,0.949030093725405));
#49535=CARTESIAN_POINT('Ctrl Pts',(3.90032671966707,2.40098547504095,0.975487390409873));
#49536=CARTESIAN_POINT('Ctrl Pts',(3.43982409908107,3.02405189544283,1.00194468709434));
#49537=CARTESIAN_POINT('Ctrl Pts',(2.85836212737567,3.49904666560206,1.02840198377881));
#49538=CARTESIAN_POINT('Ctrl Pts',(2.27690015567027,3.97404143576128,1.05485928046328));
#49539=CARTESIAN_POINT('Ctrl Pts',(1.57447883284546,4.30096455567785,1.08131657714775));
#49540=CARTESIAN_POINT('Ctrl Pts',(0.83665229586908,4.43999713904637,1.10777387383221));
#49541=CARTESIAN_POINT('Ctrl Pts',(0.0988257588927,4.57902972241489,1.13423117051668));
#49542=CARTESIAN_POINT('Ctrl Pts',(-0.674405992235245,4.53017176923536,
1.16068846720115));
#49543=CARTESIAN_POINT('Ctrl Pts',(-1.38886418452507,4.29937413054889,1.18714576388562));
#49544=CARTESIAN_POINT('Ctrl Pts',(-2.1033223768149,4.06857649186242,1.21360306057009));
#49545=CARTESIAN_POINT('Ctrl Pts',(-2.7590070102666,3.65583916766901,1.24006035725455));
#49546=CARTESIAN_POINT('Ctrl Pts',(-3.27605642296673,3.11143310386793,1.26651765393902));
#49547=CARTESIAN_POINT('Ctrl Pts',(-3.79310583566684,2.56702704006687,1.29297495062349));
#49548=CARTESIAN_POINT('Ctrl Pts',(-4.17152002761538,1.89095223665816,1.31943224730795));
#49549=CARTESIAN_POINT('Ctrl Pts',(-4.36520856862574,1.16555385826357,1.34588954399242));
#49550=CARTESIAN_POINT('Ctrl Pts',(-4.5588971096361,0.440155479868968,1.37234684067689));
#49551=CARTESIAN_POINT('Ctrl Pts',(-4.56785999970828,-0.334566473511511,
1.39880413736136));
#49552=CARTESIAN_POINT('Ctrl Pts',(-4.39100556896818,-1.06425172631823,
1.42526143404583));
#49553=CARTESIAN_POINT('Ctrl Pts',(-4.21415113822807,-1.79393697912495,
1.4517187307303));
#49554=CARTESIAN_POINT('Ctrl Pts',(-3.85147938667567,-2.4785855313579,1.47817602741476));
#49555=CARTESIAN_POINT('Ctrl Pts',(-3.3471633321549,-3.03480794657228,1.50463332409923));
#49556=CARTESIAN_POINT('Ctrl Pts',(-2.84284727763412,-3.59103036178665,
1.5310906207837));
#49557=CARTESIAN_POINT('Ctrl Pts',(-2.19688692014498,-4.01882663998244,
1.55754791746817));
#49558=CARTESIAN_POINT('Ctrl Pts',(-1.48795951638605,-4.26609166819824,
1.58400521415264));
#49559=CARTESIAN_POINT('Ctrl Pts',(-0.779032112627116,-4.51335669641404,
1.6104625108371));
#49560=CARTESIAN_POINT('Ctrl Pts',(-0.0071376625983989,-4.58009047464984,
1.63691980752157));
#49561=CARTESIAN_POINT('Ctrl Pts',(0.733707943998554,-4.4581649024313,1.66337710420604));
#49562=CARTESIAN_POINT('Ctrl Pts',(1.47455355059551,-4.33623933021276,1.68983440089051));
#49563=CARTESIAN_POINT('Ctrl Pts',(2.18435031376069,-4.02565440753988,1.71629169757498));
#49564=CARTESIAN_POINT('Ctrl Pts',(2.77664577327776,-3.56423903433516,1.74274899425944));
#49565=CARTESIAN_POINT('Ctrl Pts',(3.36894123279483,-3.10282366113044,1.76920629094391));
#49566=CARTESIAN_POINT('Ctrl Pts',(3.84373538866378,-2.49057783739389,1.79566358762838));
#49567=CARTESIAN_POINT('Ctrl Pts',(4.14319883817832,-1.80207242682533,1.82212088431285));
#49568=CARTESIAN_POINT('Ctrl Pts',(4.38955443642782,-1.23566887208905,1.84388615537792));
#49569=CARTESIAN_POINT('Ctrl Pts',(4.51725253079926,-0.617655577060232,
1.865651426443));
#49570=CARTESIAN_POINT('Ctrl Pts',(4.51787557461174,0.000108094638884985,
1.88741669750807));
#49571=CARTESIAN_POINT('Ctrl Pts',(1.3130361863565,-4.90075024188322,0.));
#49572=CARTESIAN_POINT('Ctrl Pts',(1.45293783176837,-4.85499972547219,-2.12441198790355E-17));
#49573=CARTESIAN_POINT('Ctrl Pts',(1.59048961161953,-4.80314405262584,1.00940613638452E-17));
#49574=CARTESIAN_POINT('Ctrl Pts',(1.72536214292615,-4.74546564178603,1.90819582357449E-17));
#49575=CARTESIAN_POINT('Ctrl Pts',(1.86158804346972,-4.68720846085782,2.81600435471549E-17));
#49576=CARTESIAN_POINT('Ctrl Pts',(1.9950813260058,-4.62301070705921,2.02661125299078E-16));
#49577=CARTESIAN_POINT('Ctrl Pts',(2.12548189098024,-4.5531145507957,1.45716771982052E-16));
#49578=CARTESIAN_POINT('Ctrl Pts',(2.25528319940241,-4.4835396027235,8.90341067708004E-17));
#49579=CARTESIAN_POINT('Ctrl Pts',(2.38202075670042,-4.40831802172382,2.31151513749735E-16));
#49580=CARTESIAN_POINT('Ctrl Pts',(2.50530950004123,-4.32764726500609,1.45716771982052E-16));
#49581=CARTESIAN_POINT('Ctrl Pts',(2.62711997854446,-4.24794377212644,6.13064155008212E-17));
#49582=CARTESIAN_POINT('Ctrl Pts',(2.74556437761014,-4.16292050991704,2.71959880884896E-17));
#49583=CARTESIAN_POINT('Ctrl Pts',(2.86023373369319,-4.07273466802712,-6.93889390390723E-17));
#49584=CARTESIAN_POINT('Ctrl Pts',(2.90383704830196,-4.03844127202745,-1.06115603492979E-16));
#49585=CARTESIAN_POINT('Ctrl Pts',(2.94689409015111,-4.00340109988822,-3.37664978924697E-16));
#49586=CARTESIAN_POINT('Ctrl Pts',(2.98938067979849,-3.96762172921426,-3.7470027081099E-16));
#49587=CARTESIAN_POINT('Ctrl Pts',(3.0045493035191,-3.95484772651792,-3.87922664316067E-16));
#49588=CARTESIAN_POINT('Ctrl Pts',(3.0196457209465,-3.94197897848992,-6.77418652234536E-17));
#49589=CARTESIAN_POINT('Ctrl Pts',(3.03465663588118,-3.92902653262601,-5.55111512312578E-17));
#49590=CARTESIAN_POINT('Ctrl Pts',(3.14512636784121,-3.83370567916447,3.44982654016709E-17));
#49591=CARTESIAN_POINT('Ctrl Pts',(3.25112830521826,-3.73372148501147,-5.43481287766778E-16));
#49592=CARTESIAN_POINT('Ctrl Pts',(3.35231677944077,-3.62929621080565,-5.13478148889135E-16));
#49593=CARTESIAN_POINT('Ctrl Pts',(3.36921809466263,-3.61185425914028,-5.08466782607427E-16));
#49594=CARTESIAN_POINT('Ctrl Pts',(3.38598504383309,-3.59428832049142,-2.69772873285687E-16));
#49595=CARTESIAN_POINT('Ctrl Pts',(3.40261591802407,-3.57659932769537,-2.63677968348475E-16));
#49596=CARTESIAN_POINT('Ctrl Pts',(3.50230123740107,-3.4705716543402,-2.26333319460949E-16));
#49597=CARTESIAN_POINT('Ctrl Pts',(3.59710111637371,-3.36012540834712,3.61502860778476E-17));
#49598=CARTESIAN_POINT('Ctrl Pts',(3.68681562587056,-3.2456540248488,-6.93889390390723E-17));
#49599=CARTESIAN_POINT('Ctrl Pts',(3.77658274630639,-3.13111551233192,-1.74990055122844E-16));
#49600=CARTESIAN_POINT('Ctrl Pts',(3.86125888590103,-3.01254641429341,-2.14930374901985E-16));
#49601=CARTESIAN_POINT('Ctrl Pts',(3.94059800782458,-2.89031628889591,-9.71445146547012E-17));
#49602=CARTESIAN_POINT('Ctrl Pts',(4.01127293754548,-2.78143424794555,7.77859507059291E-18));
#49603=CARTESIAN_POINT('Ctrl Pts',(4.07771240145114,-2.66964644715424,3.21618427330635E-16));
#49604=CARTESIAN_POINT('Ctrl Pts',(4.13970845878657,-2.55520469810914,3.46944695195361E-16));
#49605=CARTESIAN_POINT('Ctrl Pts',(4.1548365715119,-2.52727892743195,3.53124743599032E-16));
#49606=CARTESIAN_POINT('Ctrl Pts',(4.16969994577116,-2.49919510449128,-5.38761705143296E-16));
#49607=CARTESIAN_POINT('Ctrl Pts',(4.18429524804614,-2.47095685207318,-5.41233724504764E-16));
#49608=CARTESIAN_POINT('Ctrl Pts',(4.1935591046312,-2.45303361104087,-5.42802752155488E-16));
#49609=CARTESIAN_POINT('Ctrl Pts',(4.20271084368267,-2.4350560800449,-1.54877819716967E-16));
#49610=CARTESIAN_POINT('Ctrl Pts',(4.21174771778014,-2.41702978670704,-1.66533453693773E-16));
#49611=CARTESIAN_POINT('Ctrl Pts',(4.27617843190164,-2.28850670005169,-2.49635288749205E-16));
#49612=CARTESIAN_POINT('Ctrl Pts',(4.33481139244535,-2.15743447779131,-2.0244448216388E-16));
#49613=CARTESIAN_POINT('Ctrl Pts',(4.38745860743762,-2.0241905870822,-2.77555756156289E-16));
#49614=CARTESIAN_POINT('Ctrl Pts',(4.43978289169495,-1.89176399596928,-3.52206307982929E-16));
#49615=CARTESIAN_POINT('Ctrl Pts',(4.48619490051256,-1.75719157307499,-5.94819252645897E-16));
#49616=CARTESIAN_POINT('Ctrl Pts',(4.52646203441684,-1.6208264292839,-5.55111512312578E-16));
#49617=CARTESIAN_POINT('Ctrl Pts',(4.54111387023209,-1.5712078072459,-5.40663220727154E-16));
#49618=CARTESIAN_POINT('Ctrl Pts',(4.55495165294679,-1.52135171714656,-2.34210881400015E-17));
#49619=CARTESIAN_POINT('Ctrl Pts',(4.56796247846719,-1.47127487515823,-2.77555756156289E-17));
#49620=CARTESIAN_POINT('Ctrl Pts',(4.60395075905375,-1.33276103239401,-1.11900177134892E-17));
#49621=CARTESIAN_POINT('Ctrl Pts',(4.63361579821919,-1.19255796729143,2.91143634808383E-16));
#49622=CARTESIAN_POINT('Ctrl Pts',(4.65692008513065,-1.05110298842804,2.77555756156289E-16));
#49623=CARTESIAN_POINT('Ctrl Pts',(4.67001847025983,-0.971596938805809,
2.69918566125548E-16));
#49624=CARTESIAN_POINT('Ctrl Pts',(4.68110649292123,-0.891695424459561,
-5.05694400348962E-17));
#49625=CARTESIAN_POINT('Ctrl Pts',(4.69017032387523,-0.811477248591749,
-5.55111512312578E-17));
#49626=CARTESIAN_POINT('Ctrl Pts',(4.69376322527145,-0.779678774244579,
-5.74700448985431E-17));
#49627=CARTESIAN_POINT('Ctrl Pts',(4.69703800287417,-0.74783055663592,9.2602246089847E-18));
#49628=CARTESIAN_POINT('Ctrl Pts',(4.69999357182281,-0.715937571621207,
0.));
#49629=CARTESIAN_POINT('Ctrl Pts',(4.7021844555123,-0.692296160477742,-6.86435519161465E-18));
#49630=CARTESIAN_POINT('Ctrl Pts',(4.70420012738525,-0.668626688781088,
-5.81512878434173E-17));
#49631=CARTESIAN_POINT('Ctrl Pts',(4.70603832259692,-0.644957088113592,
-5.55111512312578E-17));
#49632=CARTESIAN_POINT('Ctrl Pts',(4.7169850543804,-0.50400101974599,-3.97887365597508E-17));
#49633=CARTESIAN_POINT('Ctrl Pts',(4.72166050160268,-0.362862391559157,
3.85433575684503E-16));
#49634=CARTESIAN_POINT('Ctrl Pts',(4.72009704228143,-0.221963242879035,
3.88578058618805E-16));
#49635=CARTESIAN_POINT('Ctrl Pts',(4.71853510529174,-0.0812012869083159,
3.91719479787741E-16));
#49636=CARTESIAN_POINT('Ctrl Pts',(4.71074633224057,0.0593224521016401,
3.13145818824179E-16));
#49637=CARTESIAN_POINT('Ctrl Pts',(4.69671116060458,0.199185274316974,2.22044604925031E-16));
#49638=CARTESIAN_POINT('Ctrl Pts',(4.68289306772495,0.336884870581422,1.3235243244906E-16));
#49639=CARTESIAN_POINT('Ctrl Pts',(4.6630201315191,0.473944543714825,-1.38004669694731E-16));
#49640=CARTESIAN_POINT('Ctrl Pts',(4.63702542177262,0.609947964574148,-1.38777878078145E-16));
#49641=CARTESIAN_POINT('Ctrl Pts',(4.62055356019607,0.696128173708246,-1.39267830902609E-16));
#49642=CARTESIAN_POINT('Ctrl Pts',(4.60162268181677,0.781883974967431,8.79945197126988E-17));
#49643=CARTESIAN_POINT('Ctrl Pts',(4.58020591978812,0.867104757427645,1.11022302462516E-16));
#49644=CARTESIAN_POINT('Ctrl Pts',(4.56733705680351,0.918312058113609,6.78760316859931E-17));
#49645=CARTESIAN_POINT('Ctrl Pts',(4.55357049340461,0.96932610659445,-4.99175148350681E-16));
#49646=CARTESIAN_POINT('Ctrl Pts',(4.53891402393445,1.0201248132638,-5.55111512312578E-16));
#49647=CARTESIAN_POINT('Ctrl Pts',(4.5307224586103,1.04851643410481,-5.86374592437204E-16));
#49648=CARTESIAN_POINT('Ctrl Pts',(4.52225289509851,1.0768407763045,9.91752405205522E-17));
#49649=CARTESIAN_POINT('Ctrl Pts',(4.51350658698018,1.10509389044702,1.11022302462516E-16));
#49650=CARTESIAN_POINT('Ctrl Pts',(4.50742875670279,1.12472704654475,1.19254853933931E-16));
#49651=CARTESIAN_POINT('Ctrl Pts',(4.50121763562789,1.14432449467847,-5.35474147175706E-16));
#49652=CARTESIAN_POINT('Ctrl Pts',(4.49487767268156,1.16387312026907,-5.27355936696949E-16));
#49653=CARTESIAN_POINT('Ctrl Pts',(4.45189774593679,1.2963973168547,-4.72320900273343E-16));
#49654=CARTESIAN_POINT('Ctrl Pts',(4.40295499932666,1.42682794112182,5.0484926233065E-16));
#49655=CARTESIAN_POINT('Ctrl Pts',(4.34826585417728,1.55478882374,3.88578058618805E-16));
#49656=CARTESIAN_POINT('Ctrl Pts',(4.29692960608226,1.67490464560194,2.79435241634665E-16));
#49657=CARTESIAN_POINT('Ctrl Pts',(4.24052923074577,1.79284458992044,2.95867102710926E-16));
#49658=CARTESIAN_POINT('Ctrl Pts',(4.17920839057011,1.90827559700852,4.9960036108132E-16));
#49659=CARTESIAN_POINT('Ctrl Pts',(4.15338816346376,1.95687986938296,5.85385862147007E-16));
#49660=CARTESIAN_POINT('Ctrl Pts',(4.12669516016291,2.0050390084677,-2.10958088174218E-16));
#49661=CARTESIAN_POINT('Ctrl Pts',(4.09913850024111,2.05272668507128,-1.66533453693773E-16));
#49662=CARTESIAN_POINT('Ctrl Pts',(4.08221130669435,2.08201973197734,-1.3924479141655E-16));
#49663=CARTESIAN_POINT('Ctrl Pts',(4.06495515473503,2.11113968242291,3.92725569055683E-16));
#49664=CARTESIAN_POINT('Ctrl Pts',(4.04738928099658,2.14005245629164,3.33066907387547E-16));
#49665=CARTESIAN_POINT('Ctrl Pts',(3.97588097586157,2.2577524629574,9.02045342409376E-17));
#49666=CARTESIAN_POINT('Ctrl Pts',(3.89920169633387,2.37209762967783,1.73844745989399E-16));
#49667=CARTESIAN_POINT('Ctrl Pts',(3.81753428055142,2.4827050770719,1.11022302462516E-16));
#49668=CARTESIAN_POINT('Ctrl Pts',(3.73700167373633,2.59177557950503,4.90728077314622E-17));
#49669=CARTESIAN_POINT('Ctrl Pts',(3.65161810526706,2.69721206501942,-2.17511715066662E-16));
#49670=CARTESIAN_POINT('Ctrl Pts',(3.56152350731999,2.79861134980753,-2.22044604925031E-16));
#49671=CARTESIAN_POINT('Ctrl Pts',(3.54164701408898,2.82098186084422,-2.23044642181868E-16));
#49672=CARTESIAN_POINT('Ctrl Pts',(3.52154110171521,2.8431557130462,3.77586732270394E-16));
#49673=CARTESIAN_POINT('Ctrl Pts',(3.50120707213069,2.86512829543052,4.44089209850063E-16));
#49674=CARTESIAN_POINT('Ctrl Pts',(3.47910313325541,2.88901340959032,5.16017817963063E-16));
#49675=CARTESIAN_POINT('Ctrl Pts',(3.45672963690434,2.91266069254474,2.77193395410128E-16));
#49676=CARTESIAN_POINT('Ctrl Pts',(3.43409108914483,2.93606647242265,2.77555756156289E-16));
#49677=CARTESIAN_POINT('Origin',(0.,0.,20.5));
#49678=CARTESIAN_POINT('Origin',(0.,0.,41.));
#49679=CARTESIAN_POINT('',(-4.,4.89858719658941E-16,41.));
#49680=CARTESIAN_POINT('Origin',(0.,0.,41.));
#49681=CARTESIAN_POINT('Origin',(-4.45462538595717E-16,-1.65775395963113E-16,
375.));
#49682=CARTESIAN_POINT('Ctrl Pts',(-3.43378788736335,2.93584158412826,375.));
#49683=CARTESIAN_POINT('Ctrl Pts',(-3.52812472271588,2.83822707478694,375.));
#49684=CARTESIAN_POINT('Ctrl Pts',(-3.61783741229297,2.73641228828402,375.));
#49685=CARTESIAN_POINT('Ctrl Pts',(-3.70278930559469,2.6308098016192,375.));
#49686=CARTESIAN_POINT('Ctrl Pts',(-3.78883118430305,2.52385236964479,375.));
#49687=CARTESIAN_POINT('Ctrl Pts',(-3.86998980756465,2.41300886934011,375.));
#49688=CARTESIAN_POINT('Ctrl Pts',(-3.94608965952372,2.29866645157891,375.));
#49689=CARTESIAN_POINT('Ctrl Pts',(-3.98412572654406,2.24151606621978,375.));
#49690=CARTESIAN_POINT('Ctrl Pts',(-4.02089745503991,2.18349099620346,375.));
#49691=CARTESIAN_POINT('Ctrl Pts',(-4.0563792513302,2.12463643972661,375.));
#49692=CARTESIAN_POINT('Ctrl Pts',(-4.0706431485814,2.10097655116059,375.));
#49693=CARTESIAN_POINT('Ctrl Pts',(-4.08469915763129,2.07718134398868,375.));
#49694=CARTESIAN_POINT('Ctrl Pts',(-4.09853534340515,2.05327180953563,375.));
#49695=CARTESIAN_POINT('Ctrl Pts',(-4.16827482663706,1.93275893089092,375.));
#49696=CARTESIAN_POINT('Ctrl Pts',(-4.23249571495574,1.80924176863962,375.));
#49697=CARTESIAN_POINT('Ctrl Pts',(-4.29102780012401,1.68312480250504,375.));
#49698=CARTESIAN_POINT('Ctrl Pts',(-4.34427585815273,1.56839313846413,375.));
#49699=CARTESIAN_POINT('Ctrl Pts',(-4.3928156984662,1.45150902581472,375.));
#49700=CARTESIAN_POINT('Ctrl Pts',(-4.4364893782082,1.33275463175064,375.));
#49701=CARTESIAN_POINT('Ctrl Pts',(-4.46204208504677,1.2632735109649,375.));
#49702=CARTESIAN_POINT('Ctrl Pts',(-4.48592844490179,1.19315178813539,375.));
#49703=CARTESIAN_POINT('Ctrl Pts',(-4.50811171504532,1.12244350259313,375.));
#49704=CARTESIAN_POINT('Ctrl Pts',(-4.5141904988611,1.10306762252609,375.));
#49705=CARTESIAN_POINT('Ctrl Pts',(-4.52013855791141,1.08365664730297,375.));
#49706=CARTESIAN_POINT('Ctrl Pts',(-4.52595509671778,1.06421299497352,375.));
#49707=CARTESIAN_POINT('Ctrl Pts',(-4.53519138586709,1.0333377268782,375.));
#49708=CARTESIAN_POINT('Ctrl Pts',(-4.54409635013865,1.00237910104441,375.));
#49709=CARTESIAN_POINT('Ctrl Pts',(-4.55266817723945,0.971342071123453,
375.));
#49710=CARTESIAN_POINT('Ctrl Pts',(-4.58939773349738,0.838351015289689,
375.));
#49711=CARTESIAN_POINT('Ctrl Pts',(-4.62001434120323,0.703922655316075,
375.));
#49712=CARTESIAN_POINT('Ctrl Pts',(-4.6446125449424,0.568489655194437,375.));
#49713=CARTESIAN_POINT('Ctrl Pts',(-4.6695978975114,0.43092508774079,375.));
#49714=CARTESIAN_POINT('Ctrl Pts',(-4.68837408722962,0.292323323451818,
375.));
#49715=CARTESIAN_POINT('Ctrl Pts',(-4.7009917947161,0.153114389433896,375.));
#49716=CARTESIAN_POINT('Ctrl Pts',(-4.71369611133585,0.0129499121739395,
375.));
#49717=CARTESIAN_POINT('Ctrl Pts',(-4.72015723771216,-0.127830868720726,
375.));
#49718=CARTESIAN_POINT('Ctrl Pts',(-4.72037601386282,-0.2688014592115,375.));
#49719=CARTESIAN_POINT('Ctrl Pts',(-4.72051776383518,-0.360139464952745,
375.));
#49720=CARTESIAN_POINT('Ctrl Pts',(-4.71803791594725,-0.451557379168488,
375.));
#49721=CARTESIAN_POINT('Ctrl Pts',(-4.7129250253839,-0.542939603201634,
375.));
#49722=CARTESIAN_POINT('Ctrl Pts',(-4.71050429468246,-0.586205100974703,
375.));
#49723=CARTESIAN_POINT('Ctrl Pts',(-4.70749320436126,-0.629462591214061,
375.));
#49724=CARTESIAN_POINT('Ctrl Pts',(-4.70388981020381,-0.672699721412066,
375.));
#49725=CARTESIAN_POINT('Ctrl Pts',(-4.70250698353675,-0.689292260011098,
375.));
#49726=CARTESIAN_POINT('Ctrl Pts',(-4.7010370790231,-0.705879562100339,
375.));
#49727=CARTESIAN_POINT('Ctrl Pts',(-4.69948096449077,-0.722452069367425,
375.));
#49728=CARTESIAN_POINT('Ctrl Pts',(-4.68606574819498,-0.865323153038659,
375.));
#49729=CARTESIAN_POINT('Ctrl Pts',(-4.66623214709618,-1.0072815713457,375.));
#49730=CARTESIAN_POINT('Ctrl Pts',(-4.64004375541204,-1.14788248706686,
375.));
#49731=CARTESIAN_POINT('Ctrl Pts',(-4.6270279916287,-1.21776185685865,375.));
#49732=CARTESIAN_POINT('Ctrl Pts',(-4.61244171628795,-1.28730612660771,
375.));
#49733=CARTESIAN_POINT('Ctrl Pts',(-4.59628803251995,-1.35646150527604,
375.));
#49734=CARTESIAN_POINT('Ctrl Pts',(-4.56399682193468,-1.4947030932479,375.));
#49735=CARTESIAN_POINT('Ctrl Pts',(-4.52544561415923,-1.63139110841489,
375.));
#49736=CARTESIAN_POINT('Ctrl Pts',(-4.48088607305284,-1.76617553752727,
375.));
#49737=CARTESIAN_POINT('Ctrl Pts',(-4.43597574851398,-1.90202102210641,
375.));
#49738=CARTESIAN_POINT('Ctrl Pts',(-4.38496188398045,-2.03593355195248,
375.));
#49739=CARTESIAN_POINT('Ctrl Pts',(-4.32805045687434,-2.16754392308446,
375.));
#49740=CARTESIAN_POINT('Ctrl Pts',(-4.30216783694698,-2.22739870775111,
375.));
#49741=CARTESIAN_POINT('Ctrl Pts',(-4.27506473176287,-2.28677711825493,
375.));
#49742=CARTESIAN_POINT('Ctrl Pts',(-4.24675722722924,-2.34564306219817,
375.));
#49743=CARTESIAN_POINT('Ctrl Pts',(-4.22863084786129,-2.38333718074896,
375.));
#49744=CARTESIAN_POINT('Ctrl Pts',(-4.21001058428347,-2.42082115169986,
375.));
#49745=CARTESIAN_POINT('Ctrl Pts',(-4.190900240747,-2.45808525714998,375.));
#49746=CARTESIAN_POINT('Ctrl Pts',(-4.18310501328873,-2.47328551649951,
375.));
#49747=CARTESIAN_POINT('Ctrl Pts',(-4.17522954608524,-2.48844657780472,
375.));
#49748=CARTESIAN_POINT('Ctrl Pts',(-4.16727814768109,-2.50356042854303,
375.));
#49749=CARTESIAN_POINT('Ctrl Pts',(-4.09969026676857,-2.63203005010014,
375.));
#49750=CARTESIAN_POINT('Ctrl Pts',(-4.02654009074559,-2.75724655837471,
375.));
#49751=CARTESIAN_POINT('Ctrl Pts',(-3.94810710693448,-2.87885707775794,
375.));
#49752=CARTESIAN_POINT('Ctrl Pts',(-3.86905485941559,-3.00142776692534,
375.));
#49753=CARTESIAN_POINT('Ctrl Pts',(-3.78463578072622,-3.12033603731368,
375.));
#49754=CARTESIAN_POINT('Ctrl Pts',(-3.69508499761951,-3.23520722691392,
375.));
#49755=CARTESIAN_POINT('Ctrl Pts',(-3.62943480927899,-3.31941994924341,
375.));
#49756=CARTESIAN_POINT('Ctrl Pts',(-3.56102553573526,-3.40146273807253,
375.));
#49757=CARTESIAN_POINT('Ctrl Pts',(-3.48993392179959,-3.48117995730746,
375.));
#49758=CARTESIAN_POINT('Ctrl Pts',(-3.39320786765338,-3.58964186493951,
375.));
#49759=CARTESIAN_POINT('Ctrl Pts',(-3.29151757709749,-3.69380035593463,
375.));
#49760=CARTESIAN_POINT('Ctrl Pts',(-3.18521993250538,-3.79343311373674,
375.));
#49761=CARTESIAN_POINT('Ctrl Pts',(-3.1484894856507,-3.82786055311678,375.));
#49762=CARTESIAN_POINT('Ctrl Pts',(-3.1112085895158,-3.86174730075506,375.));
#49763=CARTESIAN_POINT('Ctrl Pts',(-3.07339099123149,-3.89508311993719,
375.));
#49764=CARTESIAN_POINT('Ctrl Pts',(-3.05466088259105,-3.91159351571128,
375.));
#49765=CARTESIAN_POINT('Ctrl Pts',(-3.03579911530405,-3.92796876126283,
375.));
#49766=CARTESIAN_POINT('Ctrl Pts',(-3.01680731961894,-3.94420755857869,
375.));
#49767=CARTESIAN_POINT('Ctrl Pts',(-3.00397674416022,-3.95517824917451,
375.));
#49768=CARTESIAN_POINT('Ctrl Pts',(-2.99108750647465,-3.96608603020355,
375.));
#49769=CARTESIAN_POINT('Ctrl Pts',(-2.97814807270005,-3.97692398964623,
375.));
#49770=CARTESIAN_POINT('Ctrl Pts',(-2.86441519405387,-4.07218567941864,
375.));
#49771=CARTESIAN_POINT('Ctrl Pts',(-2.74664729621727,-4.16219378118691,
375.));
#49772=CARTESIAN_POINT('Ctrl Pts',(-2.62528201158405,-4.24677543677276,
375.));
#49773=CARTESIAN_POINT('Ctrl Pts',(-2.50379141827822,-4.33144442223239,
375.));
#49774=CARTESIAN_POINT('Ctrl Pts',(-2.3786953776454,-4.41067622052404,375.));
#49775=CARTESIAN_POINT('Ctrl Pts',(-2.25039003171722,-4.4842647871821,375.));
#49776=CARTESIAN_POINT('Ctrl Pts',(-2.12228319217728,-4.5577395019934,375.));
#49777=CARTESIAN_POINT('Ctrl Pts',(-1.9909763337868,-4.62558889864692,375.));
#49778=CARTESIAN_POINT('Ctrl Pts',(-1.85683056691249,-4.68756837108862,
375.));
#49779=CARTESIAN_POINT('Ctrl Pts',(-1.72268480003817,-4.74954784353032,
375.));
#49780=CARTESIAN_POINT('Ctrl Pts',(-1.58569949586696,-4.80565788540407,
375.));
#49781=CARTESIAN_POINT('Ctrl Pts',(-1.44621200484621,-4.85560714827263,
375.));
#49782=CARTESIAN_POINT('Ctrl Pts',(-1.40211572701684,-4.87139764358304,
375.));
#49783=CARTESIAN_POINT('Ctrl Pts',(-1.35776924324391,-4.88657205481219,
375.));
#49784=CARTESIAN_POINT('Ctrl Pts',(-1.31318542874385,-4.90112866933901,
375.));
#49785=CARTESIAN_POINT('Ctrl Pts',(1.31303618635831,-4.90075024188273,375.));
#49786=CARTESIAN_POINT('Ctrl Pts',(1.45436548505342,-4.85453285551617,375.));
#49787=CARTESIAN_POINT('Ctrl Pts',(1.5934293761686,-4.80203848222433,375.));
#49788=CARTESIAN_POINT('Ctrl Pts',(1.72987023226972,-4.74352674861442,375.));
#49789=CARTESIAN_POINT('Ctrl Pts',(1.86675271207831,-4.68482562767973,375.));
#49790=CARTESIAN_POINT('Ctrl Pts',(2.00099581082903,-4.620067688427,375.));
#49791=CARTESIAN_POINT('Ctrl Pts',(2.13221219437754,-4.54946990611926,375.));
#49792=CARTESIAN_POINT('Ctrl Pts',(2.19270449791029,-4.5169234941499,375.));
#49793=CARTESIAN_POINT('Ctrl Pts',(2.25255310159603,-4.48313534130926,375.));
#49794=CARTESIAN_POINT('Ctrl Pts',(2.31171758991926,-4.44812388272337,375.));
#49795=CARTESIAN_POINT('Ctrl Pts',(2.3344624112488,-4.43466429923687,375.));
#49796=CARTESIAN_POINT('Ctrl Pts',(2.35710754237018,-4.42102302699321,375.));
#49797=CARTESIAN_POINT('Ctrl Pts',(2.37964612843956,-4.40720380568676,375.));
#49798=CARTESIAN_POINT('Ctrl Pts',(2.50549113115601,-4.33004368847728,375.));
#49799=CARTESIAN_POINT('Ctrl Pts',(2.62778788875034,-4.24748071485227,375.));
#49800=CARTESIAN_POINT('Ctrl Pts',(2.74616817727066,-4.15974114711123,375.));
#49801=CARTESIAN_POINT('Ctrl Pts',(2.86286389724632,-4.07325012604791,375.));
#49802=CARTESIAN_POINT('Ctrl Pts',(2.97575433427861,-3.98172826743118,375.));
#49803=CARTESIAN_POINT('Ctrl Pts',(3.08445220151971,-3.8853563473526,375.));
#49804=CARTESIAN_POINT('Ctrl Pts',(3.13995990370008,-3.83614301894012,375.));
#49805=CARTESIAN_POINT('Ctrl Pts',(3.19437368596074,-3.78566438686541,375.));
#49806=CARTESIAN_POINT('Ctrl Pts',(3.24763776430821,-3.73394147802337,375.));
#49807=CARTESIAN_POINT('Ctrl Pts',(3.2699643084639,-3.71226094127233,375.));
#49808=CARTESIAN_POINT('Ctrl Pts',(3.29209335275734,-3.69035703897681,375.));
#49809=CARTESIAN_POINT('Ctrl Pts',(3.31399620763943,-3.66825627851417,375.));
#49810=CARTESIAN_POINT('Ctrl Pts',(3.34216498231236,-3.63983298187436,375.));
#49811=CARTESIAN_POINT('Ctrl Pts',(3.36996576521876,-3.6110784436862,375.));
#49812=CARTESIAN_POINT('Ctrl Pts',(3.39739154337912,-3.58199736557932,375.));
#49813=CARTESIAN_POINT('Ctrl Pts',(3.49658091940006,-3.47682135290355,375.));
#49814=CARTESIAN_POINT('Ctrl Pts',(3.59086820857194,-3.3673769231021,375.));
#49815=CARTESIAN_POINT('Ctrl Pts',(3.6800850008747,-3.25406730243395,375.));
#49816=CARTESIAN_POINT('Ctrl Pts',(3.76996985501536,-3.13990921107455,375.));
#49817=CARTESIAN_POINT('Ctrl Pts',(3.85470838531078,-3.02182713075438,375.));
#49818=CARTESIAN_POINT('Ctrl Pts',(3.93408537345353,-2.90020291820586,375.));
#49819=CARTESIAN_POINT('Ctrl Pts',(4.01274556585136,-2.77967700530409,375.));
#49820=CARTESIAN_POINT('Ctrl Pts',(4.08614088023802,-2.65567191437214,375.));
#49821=CARTESIAN_POINT('Ctrl Pts',(4.15401504305787,-2.52854018053819,375.));
#49822=CARTESIAN_POINT('Ctrl Pts',(4.19807507197777,-2.44601352184147,375.));
#49823=CARTESIAN_POINT('Ctrl Pts',(4.23980760353704,-2.36216897889331,375.));
#49824=CARTESIAN_POINT('Ctrl Pts',(4.27913099033935,-2.27710078886137,375.));
#49825=CARTESIAN_POINT('Ctrl Pts',(4.29645860907187,-2.23961599207746,375.));
#49826=CARTESIAN_POINT('Ctrl Pts',(4.31331832747089,-2.20189359019125,375.));
#49827=CARTESIAN_POINT('Ctrl Pts',(4.32970256286081,-2.16394161183312,375.));
#49828=CARTESIAN_POINT('Ctrl Pts',(4.33919451441291,-2.14195472435813,375.));
#49829=CARTESIAN_POINT('Ctrl Pts',(4.34852813367479,-2.11988754210219,375.));
#49830=CARTESIAN_POINT('Ctrl Pts',(4.35769217797944,-2.0977656675703,375.));
#49831=CARTESIAN_POINT('Ctrl Pts',(4.41245445040556,-1.96557030933995,375.));
#49832=CARTESIAN_POINT('Ctrl Pts',(4.46123822222855,-1.83125898605536,375.));
#49833=CARTESIAN_POINT('Ctrl Pts',(4.50384926204605,-1.6951979775962,375.));
#49834=CARTESIAN_POINT('Ctrl Pts',(4.52559692351824,-1.62575567428212,375.));
#49835=CARTESIAN_POINT('Ctrl Pts',(4.54573592530189,-1.55585726815914,375.));
#49836=CARTESIAN_POINT('Ctrl Pts',(4.56423545664257,-1.48554983900212,375.));
#49837=CARTESIAN_POINT('Ctrl Pts',(4.60056463169787,-1.34748088717324,375.));
#49838=CARTESIAN_POINT('Ctrl Pts',(4.63057447100037,-1.20783464517222,375.));
#49839=CARTESIAN_POINT('Ctrl Pts',(4.65426082259252,-1.06704756524395,375.));
#49840=CARTESIAN_POINT('Ctrl Pts',(4.67788678995459,-0.926619397467839,
375.));
#49841=CARTESIAN_POINT('Ctrl Pts',(4.69522141344644,-0.785055397710089,
375.));
#49842=CARTESIAN_POINT('Ctrl Pts',(4.7062090782541,-0.642791899249072,375.));
#49843=CARTESIAN_POINT('Ctrl Pts',(4.71102657060836,-0.58041710641334,375.));
#49844=CARTESIAN_POINT('Ctrl Pts',(4.71462329627092,-0.5179079594038,375.));
#49845=CARTESIAN_POINT('Ctrl Pts',(4.71699147233722,-0.455302034234564,
375.));
#49846=CARTESIAN_POINT('Ctrl Pts',(4.71854674616479,-0.414186275042497,
375.));
#49847=CARTESIAN_POINT('Ctrl Pts',(4.71957210036622,-0.373028786701393,
375.));
#49848=CARTESIAN_POINT('Ctrl Pts',(4.72006488912048,-0.331840385723362,
375.));
#49849=CARTESIAN_POINT('Ctrl Pts',(4.72028902811531,-0.313106340528846,
375.));
#49850=CARTESIAN_POINT('Ctrl Pts',(4.72040288834379,-0.294371677101196,
375.));
#49851=CARTESIAN_POINT('Ctrl Pts',(4.72040648677608,-0.275644826658347,
375.));
#49852=CARTESIAN_POINT('Ctrl Pts',(4.72043355701338,-0.134766732053278,
375.));
#49853=CARTESIAN_POINT('Ctrl Pts',(4.71422662120245,0.0057990813089247,
375.));
#49854=CARTESIAN_POINT('Ctrl Pts',(4.70180390274057,0.145635587850549,375.));
#49855=CARTESIAN_POINT('Ctrl Pts',(4.68946458626375,0.284533278764535,375.));
#49856=CARTESIAN_POINT('Ctrl Pts',(4.67099254981089,0.422712188593173,375.));
#49857=CARTESIAN_POINT('Ctrl Pts',(4.6463550982981,0.559757549565289,375.));
#49858=CARTESIAN_POINT('Ctrl Pts',(4.62907635772754,0.655870219230258,375.));
#49859=CARTESIAN_POINT('Ctrl Pts',(4.60876410990094,0.751425238603689,375.));
#49860=CARTESIAN_POINT('Ctrl Pts',(4.58539251247819,0.846274706840598,375.));
#49861=CARTESIAN_POINT('Ctrl Pts',(4.55189132819966,0.982233300369681,375.));
#49862=CARTESIAN_POINT('Ctrl Pts',(4.51210568697928,1.11674373042915,375.));
#49863=CARTESIAN_POINT('Ctrl Pts',(4.46619637471526,1.24939846486887,375.));
#49864=CARTESIAN_POINT('Ctrl Pts',(4.4514821415469,1.29191517002461,375.));
#49865=CARTESIAN_POINT('Ctrl Pts',(4.43613853638538,1.33424101402745,375.));
#49866=CARTESIAN_POINT('Ctrl Pts',(4.42016997732094,1.37636185265469,375.));
#49867=CARTESIAN_POINT('Ctrl Pts',(4.41229563070378,1.39713229799154,375.));
#49868=CARTESIAN_POINT('Ctrl Pts',(4.40426931219602,1.41785288761014,375.));
#49869=CARTESIAN_POINT('Ctrl Pts',(4.39609151624634,1.43852188916379,375.));
#49870=CARTESIAN_POINT('Ctrl Pts',(4.38944561986513,1.45531908531226,375.));
#49871=CARTESIAN_POINT('Ctrl Pts',(4.38270019096179,1.4720807922257,375.));
#49872=CARTESIAN_POINT('Ctrl Pts',(4.37586028060643,1.48879486186589,375.));
#49873=CARTESIAN_POINT('Ctrl Pts',(4.32342038722716,1.61693748133431,375.));
#49874=CARTESIAN_POINT('Ctrl Pts',(4.26535943234438,1.74246391819237,375.));
#49875=CARTESIAN_POINT('Ctrl Pts',(4.20190818178381,1.86501937630542,375.));
#49876=CARTESIAN_POINT('Ctrl Pts',(4.13850743678452,1.98747728343019,375.));
#49877=CARTESIAN_POINT('Ctrl Pts',(4.06972452623307,2.10696961603591,375.));
#49878=CARTESIAN_POINT('Ctrl Pts',(3.99574428312086,2.22311713285455,375.));
#49879=CARTESIAN_POINT('Ctrl Pts',(3.9230204444275,2.3372921196134,375.));
#49880=CARTESIAN_POINT('Ctrl Pts',(3.84527380385539,2.44823547455532,375.));
#49881=CARTESIAN_POINT('Ctrl Pts',(3.7626432675861,2.55555363817714,375.));
#49882=CARTESIAN_POINT('Ctrl Pts',(3.68595020843944,2.65516037730487,375.));
#49883=CARTESIAN_POINT('Ctrl Pts',(3.60504931330013,2.75164424921775,375.));
#49884=CARTESIAN_POINT('Ctrl Pts',(3.52002795172102,2.84465807652531,375.));
#49885=CARTESIAN_POINT('Ctrl Pts',(3.49183173897392,2.87550488507407,375.));
#49886=CARTESIAN_POINT('Ctrl Pts',(3.46318217104164,2.90596975880766,375.));
#49887=CARTESIAN_POINT('Ctrl Pts',(3.43408816985932,2.93604417002309,375.));
#49888=CARTESIAN_POINT('Origin',(0.,0.,402.208336844637));
#49889=CARTESIAN_POINT('Ctrl Pts',(-5.07353386009457,0.000128968315485402,
399.708336844637));
#49890=CARTESIAN_POINT('Ctrl Pts',(-5.07374798994712,0.217328374468673,
399.701523610908));
#49891=CARTESIAN_POINT('Ctrl Pts',(-5.00706367321595,1.27523772951867,399.668334418693));
#49892=CARTESIAN_POINT('Ctrl Pts',(-4.28603436807985,3.09622957226831,399.608769267991));
#49893=CARTESIAN_POINT('Ctrl Pts',(-2.29040909926245,4.7655795591539,399.529641392531));
#49894=CARTESIAN_POINT('Ctrl Pts',(0.259800278618912,5.28102545063066,399.450513517072));
#49895=CARTESIAN_POINT('Ctrl Pts',(2.7471033957984,4.51775909222651,399.371385641611));
#49896=CARTESIAN_POINT('Ctrl Pts',(4.56924148852249,2.66059337678593,399.292257766152));
#49897=CARTESIAN_POINT('Ctrl Pts',(5.2850143906551,0.159209483399153,399.213129890692));
#49898=CARTESIAN_POINT('Ctrl Pts',(4.7211096918349,-2.38072426286758,399.134002015232));
#49899=CARTESIAN_POINT('Ctrl Pts',(3.01406746059458,-4.34420558161996,399.054874139772));
#49900=CARTESIAN_POINT('Ctrl Pts',(0.577219342712345,-5.25581036421826,
398.975746264313));
#49901=CARTESIAN_POINT('Ctrl Pts',(-1.99939275815206,-4.89480881878609,
398.896618388853));
#49902=CARTESIAN_POINT('Ctrl Pts',(-4.09188543486623,-3.34861140683646,
398.817490513394));
#49903=CARTESIAN_POINT('Ctrl Pts',(-4.96571105424643,-1.479143747598,398.754729998654));
#49904=CARTESIAN_POINT('Ctrl Pts',(-5.07346848196321,-0.319197162169717,
398.718345442402));
#49905=CARTESIAN_POINT('Ctrl Pts',(-5.07327504304777,-8.56681209025073E-5,
398.708336844637));
#49906=CARTESIAN_POINT('Ctrl Pts',(-5.07330191118131,0.000105688062508012,
399.791663155363));
#49907=CARTESIAN_POINT('Ctrl Pts',(-5.07350034043644,0.308800908665525,
399.781980894782));
#49908=CARTESIAN_POINT('Ctrl Pts',(-4.97021252404761,1.45829359598981,399.745922675715));
#49909=CARTESIAN_POINT('Ctrl Pts',(-4.11241943286933,3.32339561801255,399.683488498161));
#49910=CARTESIAN_POINT('Ctrl Pts',(-2.02945797892606,4.8824090247121,399.604360622701));
#49911=CARTESIAN_POINT('Ctrl Pts',(0.54487554882432,5.2592655238007,399.525232747241));
#49912=CARTESIAN_POINT('Ctrl Pts',(2.98728943775363,4.36266186092565,399.446104871781));
#49913=CARTESIAN_POINT('Ctrl Pts',(4.70637522433117,2.40972094089285,399.366976996322));
#49914=CARTESIAN_POINT('Ctrl Pts',(5.28589404837916,-0.126697339701679,
399.287849120862));
#49915=CARTESIAN_POINT('Ctrl Pts',(4.58552092441564,-2.6324361653814,399.208721245402));
#49916=CARTESIAN_POINT('Ctrl Pts',(2.77484145336967,-4.50077558224301,399.129593369943));
#49917=CARTESIAN_POINT('Ctrl Pts',(0.292280359106768,-5.27932726882375,
399.050465494482));
#49918=CARTESIAN_POINT('Ctrl Pts',(-2.26105137922953,-4.77957858969287,
398.971337619023));
#49919=CARTESIAN_POINT('Ctrl Pts',(-4.26690751412045,-3.12253502339944,
398.892209743563));
#49920=CARTESIAN_POINT('Ctrl Pts',(-5.00313619365009,-1.29606201606178,
398.832318255676));
#49921=CARTESIAN_POINT('Ctrl Pts',(-5.07372209014652,-0.227734309753026,
398.798802726276));
#49922=CARTESIAN_POINT('Ctrl Pts',(-5.07350261625086,-0.000127405426567848,
398.791663155363));
#49923=CARTESIAN_POINT('Ctrl Pts',(3.43378788736214,2.93584158412968,400.));
#49924=CARTESIAN_POINT('Ctrl Pts',(3.92033033613488,2.36677696691239,399.973624041513));
#49925=CARTESIAN_POINT('Ctrl Pts',(4.60446627899797,0.982571495138102,399.92087212454));
#49926=CARTESIAN_POINT('Ctrl Pts',(4.51560363134058,-1.33271150407048,399.84174424908));
#49927=CARTESIAN_POINT('Ctrl Pts',(3.3333277577492,-3.32493526877752,399.762616373621));
#49928=CARTESIAN_POINT('Ctrl Pts',(1.34394627169084,-4.51226606526834,399.683488498161));
#49929=CARTESIAN_POINT('Ctrl Pts',(-0.97085300939813,-4.60694214684371,
399.604360622701));
#49930=CARTESIAN_POINT('Ctrl Pts',(-3.05057500858779,-3.58616495104857,
399.525232747241));
#49931=CARTESIAN_POINT('Ctrl Pts',(-4.391652180308,-1.69703895278099,399.446104871782));
#49932=CARTESIAN_POINT('Ctrl Pts',(-4.66936408063869,0.602987533589634,
399.366976996322));
#49933=CARTESIAN_POINT('Ctrl Pts',(-3.81646794512629,2.7570149696695,399.287849120862));
#49934=CARTESIAN_POINT('Ctrl Pts',(-2.03947802510898,4.24347545201977,399.208721245402));
#49935=CARTESIAN_POINT('Ctrl Pts',(0.231337257318392,4.70245047492642,399.129593369942));
#49936=CARTESIAN_POINT('Ctrl Pts',(2.44613812014511,4.02280553037415,399.050465494483));
#49937=CARTESIAN_POINT('Ctrl Pts',(4.06864765349505,2.36910590664905,398.971337619023));
#49938=CARTESIAN_POINT('Ctrl Pts',(4.70600239738688,0.141766919667795,398.892209743563));
#49939=CARTESIAN_POINT('Ctrl Pts',(4.20387758402063,-2.11989850176798,398.813081868103));
#49940=CARTESIAN_POINT('Ctrl Pts',(2.68385431845262,-3.86826607662479,398.733953992643));
#49941=CARTESIAN_POINT('Ctrl Pts',(0.513980740606018,-4.67999788571173,
398.654826117184));
#49942=CARTESIAN_POINT('Ctrl Pts',(-1.78034465333125,-4.35854670077871,
398.575698241724));
#49943=CARTESIAN_POINT('Ctrl Pts',(-3.64358944799884,-2.98174652775848,
398.496570366264));
#49944=CARTESIAN_POINT('Ctrl Pts',(-4.62460016500653,-0.88296644150622,
398.417442490804));
#49945=CARTESIAN_POINT('Ctrl Pts',(-4.48584151198124,1.42960916071621,398.338314615345));
#49946=CARTESIAN_POINT('Ctrl Pts',(-3.2609115695794,3.39602888062287,398.259186739885));
#49947=CARTESIAN_POINT('Ctrl Pts',(-1.24640657987359,4.54015716254393,398.180058864425));
#49948=CARTESIAN_POINT('Ctrl Pts',(1.06989485946835,4.5849625311949,398.100930988966));
#49949=CARTESIAN_POINT('Ctrl Pts',(3.12713920196537,3.51959611807719,398.021803113505));
#49950=CARTESIAN_POINT('Ctrl Pts',(4.42719923245446,1.6020185326593,397.942675238046));
#49951=CARTESIAN_POINT('Ctrl Pts',(4.65528721806493,-0.70346097272927,397.863547362586));
#49952=CARTESIAN_POINT('Ctrl Pts',(3.75617547838133,-2.83860920142977,397.784419487126));
#49953=CARTESIAN_POINT('Ctrl Pts',(1.94756884202228,-4.28643581876784,397.705291611666));
#49954=CARTESIAN_POINT('Ctrl Pts',(-0.332608926446521,-4.69637389108681,
397.626163736207));
#49955=CARTESIAN_POINT('Ctrl Pts',(-2.53225102161336,-3.96916378931016,
397.547035860747));
#49956=CARTESIAN_POINT('Ctrl Pts',(-4.11875100068,-2.28088724342758,397.467907985287));
#49957=CARTESIAN_POINT('Ctrl Pts',(-4.70796450115822,-0.0403321046706491,
397.388780109827));
#49958=CARTESIAN_POINT('Ctrl Pts',(-4.15722335570028,2.20998877681613,397.309652234368));
#49959=CARTESIAN_POINT('Ctrl Pts',(-2.59988029611171,3.92519794006916,397.230524358908));
#49960=CARTESIAN_POINT('Ctrl Pts',(-0.413019825824474,4.6899862522516,397.151396483448));
#49961=CARTESIAN_POINT('Ctrl Pts',(1.87384646846516,4.31917304995456,397.072268607988));
#49962=CARTESIAN_POINT('Ctrl Pts',(3.70699226699225,2.90254453114723,396.993140732528));
#49963=CARTESIAN_POINT('Ctrl Pts',(4.6425520586224,0.783113533157272,396.914012857069));
#49964=CARTESIAN_POINT('Ctrl Pts',(4.45399573023398,-1.52593527316547,396.834884981609));
#49965=CARTESIAN_POINT('Ctrl Pts',(3.18697903443818,-3.46550444479366,396.755757106149));
#49966=CARTESIAN_POINT('Ctrl Pts',(1.14828881478399,-4.56595983563972,396.676629230689));
#49967=CARTESIAN_POINT('Ctrl Pts',(-1.16844028323631,-4.56084462872216,
396.597501355229));
#49968=CARTESIAN_POINT('Ctrl Pts',(-3.20225116276825,-3.45139738560812,
396.51837347977));
#49969=CARTESIAN_POINT('Ctrl Pts',(-4.46069062869795,-1.50625214950199,
396.43924560431));
#49970=CARTESIAN_POINT('Ctrl Pts',(-4.63904866983842,0.803606783012363,
396.36011772885));
#49971=CARTESIAN_POINT('Ctrl Pts',(-3.69413887779848,2.91888581043708,396.28098985339));
#49972=CARTESIAN_POINT('Ctrl Pts',(-1.85475531148862,4.32740559196129,396.201861977931));
#49973=CARTESIAN_POINT('Ctrl Pts',(0.433726147102728,4.68811668499756,396.122734102471));
#49974=CARTESIAN_POINT('Ctrl Pts',(2.61718809326315,3.9136789479101,396.043606227011));
#49975=CARTESIAN_POINT('Ctrl Pts',(4.16694183591648,2.19160949051653,395.964478351551));
#49976=CARTESIAN_POINT('Ctrl Pts',(4.70774049744502,-0.0611214491752849,
395.885350476092));
#49977=CARTESIAN_POINT('Ctrl Pts',(4.10863875177974,-2.29905285502682,395.806222600631));
#49978=CARTESIAN_POINT('Ctrl Pts',(2.5146990390031,-3.98030716981366,395.727094725172));
#49979=CARTESIAN_POINT('Ctrl Pts',(0.311867128348267,-4.69779685779291,
395.647966849712));
#49980=CARTESIAN_POINT('Ctrl Pts',(-1.96647817706303,-4.27779382415375,
395.568838974252));
#49981=CARTESIAN_POINT('Ctrl Pts',(-3.7686737720159,-2.82199475955442,395.489711098792));
#49982=CARTESIAN_POINT('Ctrl Pts',(-4.65834821810063,-0.682896992050643,
395.410583223333));
#49983=CARTESIAN_POINT('Ctrl Pts',(-4.42008176906904,1.62155282910444,395.331455347873));
#49984=CARTESIAN_POINT('Ctrl Pts',(-3.11156664954973,3.53337082801154,395.252327472413));
#49985=CARTESIAN_POINT('Ctrl Pts',(-1.0496378504197,4.58964233963818,395.173199596953));
#49986=CARTESIAN_POINT('Ctrl Pts',(1.2664431505466,4.53460893234099,395.094071721494));
#49987=CARTESIAN_POINT('Ctrl Pts',(3.27587618232697,3.381596022723,395.014943846034));
#49988=CARTESIAN_POINT('Ctrl Pts',(4.49211073679585,1.40978634948583,394.935815970574));
#49989=CARTESIAN_POINT('Ctrl Pts',(4.6206560142512,-0.903379444528889,394.856688095114));
#49990=CARTESIAN_POINT('Ctrl Pts',(3.63038693161045,-2.99780705677087,394.777560219655));
#49991=CARTESIAN_POINT('Ctrl Pts',(1.7610805392752,-4.36636596691336,394.698432344195));
#49992=CARTESIAN_POINT('Ctrl Pts',(-0.534641970284508,-4.6776825871839,
394.619304468735));
#49993=CARTESIAN_POINT('Ctrl Pts',(-2.7009098933051,-3.85637681912437,394.540176593275));
#49994=CARTESIAN_POINT('Ctrl Pts',(-4.21319778305003,-2.1013140802211,394.461048717815));
#49995=CARTESIAN_POINT('Ctrl Pts',(-4.7053304898376,0.162546621736014,394.381920842356));
#49996=CARTESIAN_POINT('Ctrl Pts',(-4.05814633235487,2.38704938533492,394.302792966896));
#49997=CARTESIAN_POINT('Ctrl Pts',(-2.42835010030815,4.03356817385879,394.223665091436));
#49998=CARTESIAN_POINT('Ctrl Pts',(-0.210569617716467,4.70342607669429,
394.144537215976));
#49999=CARTESIAN_POINT('Ctrl Pts',(2.05819676630879,4.23442823696295,394.065409340517));
#50000=CARTESIAN_POINT('Ctrl Pts',(3.82860532171676,2.74013461591856,393.986281465057));
#50001=CARTESIAN_POINT('Ctrl Pts',(4.67198130861809,0.582363352861709,393.907153589597));
#50002=CARTESIAN_POINT('Ctrl Pts',(4.38411537617703,-1.71641742918247,393.828025714137));
#50003=CARTESIAN_POINT('Ctrl Pts',(3.03470943208895,-3.59959651705903,393.748897838677));
#50004=CARTESIAN_POINT('Ctrl Pts',(0.950499494613711,-4.61119367773381,
393.669769963218));
#50005=CARTESIAN_POINT('Ctrl Pts',(-1.36385795450447,-4.50626762440581,
393.590642087758));
#50006=CARTESIAN_POINT('Ctrl Pts',(-3.34798007341745,-3.31022444115695,
393.511514212298));
#50007=CARTESIAN_POINT('Ctrl Pts',(-4.52144496705717,-1.31266592578101,
393.432386336838));
#50008=CARTESIAN_POINT('Ctrl Pts',(-4.60011779179461,1.00273262859438,393.353258461379));
#50009=CARTESIAN_POINT('Ctrl Pts',(-3.56494924255402,3.07533629394358,393.274130585919));
#50010=CARTESIAN_POINT('Ctrl Pts',(-1.6665880225581,4.40329885266706,393.195002710459));
#50011=CARTESIAN_POINT('Ctrl Pts',(0.635309536488234,4.6650764426406,393.115874834999));
#50012=CARTESIAN_POINT('Ctrl Pts',(2.78337754615093,3.79728401076558,393.03674695954));
#50013=CARTESIAN_POINT('Ctrl Pts',(4.25749736347943,2.01004294053605,392.957619084079));
#50014=CARTESIAN_POINT('Ctrl Pts',(4.70073559740488,-0.263896316995348,
392.87849120862));
#50015=CARTESIAN_POINT('Ctrl Pts',(4.00576954320095,-2.47393750721331,392.79936333316));
#50016=CARTESIAN_POINT('Ctrl Pts',(2.3408735755072,-4.08495622085785,392.7202354577));
#50017=CARTESIAN_POINT('Ctrl Pts',(0.109174330666369,-4.70687129507029,
392.64110758224));
#50018=CARTESIAN_POINT('Ctrl Pts',(-2.14895964736531,-4.18909642486643,
392.561979706781));
#50019=CARTESIAN_POINT('Ctrl Pts',(-3.88675908733054,-2.65700211138166,
392.482851831321));
#50020=CARTESIAN_POINT('Ctrl Pts',(-4.68344499975174,-0.481559297629621,
392.403723955861));
#50021=CARTESIAN_POINT('Ctrl Pts',(-4.34611325228191,1.81048502373608,392.324596080401));
#50022=CARTESIAN_POINT('Ctrl Pts',(-2.95644307012664,3.66415076053556,392.245468204942));
#50023=CARTESIAN_POINT('Ctrl Pts',(-0.850919781515802,4.63060384272486,
392.166340329482));
#50024=CARTESIAN_POINT('Ctrl Pts',(1.46063946127848,4.47583386498977,392.087212454022));
#50025=CARTESIAN_POINT('Ctrl Pts',(3.41852935514023,3.23731578176699,392.008084578562));
#50026=CARTESIAN_POINT('Ctrl Pts',(4.54867969835275,1.21493597552573,391.928956703102));
#50027=CARTESIAN_POINT('Ctrl Pts',(4.57744353923776,-1.10162020130516,391.849828827643));
#50028=CARTESIAN_POINT('Ctrl Pts',(3.4978561961279,-3.1514375218371,391.770700952183));
#50029=CARTESIAN_POINT('Ctrl Pts',(1.57132163822667,-4.43818709971468,391.691573076723));
#50030=CARTESIAN_POINT('Ctrl Pts',(-0.735682101486766,-4.65030410493606,
391.612445201263));
#50031=CARTESIAN_POINT('Ctrl Pts',(-2.86455275856638,-3.73642796213481,
391.533317325804));
#50032=CARTESIAN_POINT('Ctrl Pts',(-4.29982000702773,-1.91783845252855,
391.454189450344));
#50033=CARTESIAN_POINT('Ctrl Pts',(-4.6939579537506,0.36512347398464,391.375061574884));
#50034=CARTESIAN_POINT('Ctrl Pts',(-3.95153270508603,2.55967687481616,391.295933699424));
#50035=CARTESIAN_POINT('Ctrl Pts',(-2.25231008366655,4.13444744915776,391.216805823965));
#50036=CARTESIAN_POINT('Ctrl Pts',(-0.00772834933684394,4.70813091315965,
391.137677948505));
#50037=CARTESIAN_POINT('Ctrl Pts',(2.2387246751714,4.14181943735019,391.058550073045));
#50038=CARTESIAN_POINT('Ctrl Pts',(3.94310806559349,2.572635847897,390.979422197585));
#50039=CARTESIAN_POINT('Ctrl Pts',(4.69273396842282,0.380531633959359,390.900294322126));
#50040=CARTESIAN_POINT('Ctrl Pts',(4.30609304338418,-1.90371193318514,390.821166446665));
#50041=CARTESIAN_POINT('Ctrl Pts',(2.87680390605944,-3.72700358316359,390.742038571206));
#50042=CARTESIAN_POINT('Ctrl Pts',(0.750944950216976,-4.64786382164717,
390.662910695746));
#50043=CARTESIAN_POINT('Ctrl Pts',(-1.55674273110369,-4.4433217857802,390.583782820286));
#50044=CARTESIAN_POINT('Ctrl Pts',(-3.48749126846685,-3.16290389914089,
390.504654944827));
#50045=CARTESIAN_POINT('Ctrl Pts',(-4.57380228443991,-1.11664187888751,
390.425527069367));
#50046=CARTESIAN_POINT('Ctrl Pts',(-4.55264378519931,1.19999624496042,390.346399193907));
#50047=CARTESIAN_POINT('Ctrl Pts',(-3.42913894648368,3.22607540341852,390.267271318447));
#50048=CARTESIAN_POINT('Ctrl Pts',(-1.4753256225101,4.47101450796107,390.188143442987));
#50049=CARTESIAN_POINT('Ctrl Pts',(0.835713058034306,4.63337243349421,390.109015567528));
#50050=CARTESIAN_POINT('Ctrl Pts',(2.94439783745191,3.67383693128064,390.029887692068));
#50051=CARTESIAN_POINT('Ctrl Pts',(4.34014606149365,1.8247434306593,389.950759816608));
#50052=CARTESIAN_POINT('Ctrl Pts',(4.68500070602262,-0.466181088634749,
389.871631941148));
#50053=CARTESIAN_POINT('Ctrl Pts',(3.89546100247805,-2.64422767571286,389.792504065689));
#50054=CARTESIAN_POINT('Ctrl Pts',(2.16270074857769,-4.18201887787879,389.713376190229));
#50055=CARTESIAN_POINT('Ctrl Pts',(-0.0937212205934936,-4.70720434606822,
389.634248314769));
#50056=CARTESIAN_POINT('Ctrl Pts',(-2.32745016801145,-4.09261922712786,
389.555120439309));
#50057=CARTESIAN_POINT('Ctrl Pts',(-3.99762609128131,-2.48707500030459,
389.475992563849));
#50058=CARTESIAN_POINT('Ctrl Pts',(-4.69984390136856,-0.279327273286843,
389.39686468839));
#50059=CARTESIAN_POINT('Ctrl Pts',(-4.26407333256687,1.99605486831531,389.31773681293));
#50060=CARTESIAN_POINT('Ctrl Pts',(-2.79582891973421,3.78812579970769,389.23860893747));
#50061=CARTESIAN_POINT('Ctrl Pts',(-0.650621423278113,4.6629655999594,389.159481062011));
#50062=CARTESIAN_POINT('Ctrl Pts',(1.65212313914968,4.40874648351652,389.08035318655));
#50063=CARTESIAN_POINT('Ctrl Pts',(3.55483379145156,3.08702334587661,389.001225311091));
#50064=CARTESIAN_POINT('Ctrl Pts',(4.59680105983476,1.01782927799078,388.922097435631));
#50065=CARTESIAN_POINT('Ctrl Pts',(4.52573004525854,-1.29781507938429,388.842969560171));
#50066=CARTESIAN_POINT('Ctrl Pts',(3.35882940195932,-3.29921528114894,388.763841684711));
#50067=CARTESIAN_POINT('Ctrl Pts',(1.37864455043625,-4.50176583424611,388.684713809252));
#50068=CARTESIAN_POINT('Ctrl Pts',(-0.935355957508586,-4.61428929040934,
388.605585933792));
#50069=CARTESIAN_POINT('Ctrl Pts',(-3.02287570734582,-3.60953998187742,
388.526458058332));
#50070=CARTESIAN_POINT('Ctrl Pts',(-4.37845680177713,-1.73080110290138,
388.447330182872));
#50071=CARTESIAN_POINT('Ctrl Pts',(-4.67386801345155,0.567022235602428,
388.368202307413));
#50072=CARTESIAN_POINT('Ctrl Pts',(-3.83758047185038,2.72755064937495,388.289074431953));
#50073=CARTESIAN_POINT('Ctrl Pts',(-2.07208717966135,4.22764841758585,388.209946556493));
#50074=CARTESIAN_POINT('Ctrl Pts',(0.19512727177995,4.70409202404044,388.130818681033));
#50075=CARTESIAN_POINT('Ctrl Pts',(2.41509492687017,4.04151863994701,388.051690805573));
#50076=CARTESIAN_POINT('Ctrl Pts',(4.0502878493588,2.40035929814049,387.972562930114));
#50077=CARTESIAN_POINT('Ctrl Pts',(4.7047714971451,0.17799320909573,387.893435054654));
#50078=CARTESIAN_POINT('Ctrl Pts',(4.22007363136663,-2.08747095037925,387.814307179194));
#50079=CARTESIAN_POINT('Ctrl Pts',(2.71355571127686,-3.84748902852625,387.735179303735));
#50080=CARTESIAN_POINT('Ctrl Pts',(0.549995785174607,-4.67590216526428,
387.656051428274));
#50081=CARTESIAN_POINT('Ctrl Pts',(-1.74673639624114,-4.37212401298038,
387.576923552815));
#50082=CARTESIAN_POINT('Ctrl Pts',(-3.62052565410023,-3.00970935653847,
387.497795677355));
#50083=CARTESIAN_POINT('Ctrl Pts',(-4.61766534522889,-0.918544055723703,
387.418667801895));
#50084=CARTESIAN_POINT('Ctrl Pts',(-4.49671481660818,1.39503128313651,387.339539926435));
#50085=CARTESIAN_POINT('Ctrl Pts',(-3.28696021026318,3.37082319307611,387.260412050976));
#50086=CARTESIAN_POINT('Ctrl Pts',(-1.28132331513389,4.53042679942271,387.181284175516));
#50087=CARTESIAN_POINT('Ctrl Pts',(1.03456453147854,4.59306353679543,387.102156300057));
#50088=CARTESIAN_POINT('Ctrl Pts',(3.09994992763925,3.54356696973015,387.023028424596));
#50089=CARTESIAN_POINT('Ctrl Pts',(4.414734438574,1.63605509066836,386.943900549137));
#50090=CARTESIAN_POINT('Ctrl Pts',(4.66056504541948,-0.667600090059401,
386.864772673676));
#50091=CARTESIAN_POINT('Ctrl Pts',(3.77791798959212,-2.80960710540626,386.785644798217));
#50092=CARTESIAN_POINT('Ctrl Pts',(1.9805114526468,-4.27131488054533,386.706516922757));
#50093=CARTESIAN_POINT('Ctrl Pts',(-0.29644271708526,-4.69879539225962,
386.627389047298));
#50094=CARTESIAN_POINT('Ctrl Pts',(-2.50161825456297,-3.98854140398097,
386.548261171838));
#50095=CARTESIAN_POINT('Ctrl Pts',(-4.10106888673475,-2.31252900718875,
386.469133296378));
#50096=CARTESIAN_POINT('Ctrl Pts',(-4.70751446766038,-0.0765764950965269,
386.390005420918));
#50097=CARTESIAN_POINT('Ctrl Pts',(-4.1741143707138,2.17791773100677,386.310877545459));
#50098=CARTESIAN_POINT('Ctrl Pts',(-2.63002248363295,3.90506570475047,386.231749669998));
#50099=CARTESIAN_POINT('Ctrl Pts',(-0.449114760664552,4.68666751056509,
386.152621794539));
#50100=CARTESIAN_POINT('Ctrl Pts',(1.84053856942387,4.33347137954045,386.073493919079));
#50101=CARTESIAN_POINT('Ctrl Pts',(3.68453635289055,2.93099783129588,385.994366043619));
#50102=CARTESIAN_POINT('Ctrl Pts',(4.63638545244831,0.818832314432457,385.915238168159));
#50103=CARTESIAN_POINT('Ctrl Pts',(4.46561157225142,-1.49159971460418,385.8361102927));
#50104=CARTESIAN_POINT('Ctrl Pts',(3.21356474331376,-3.44086588860477,385.75698241724));
#50105=CARTESIAN_POINT('Ctrl Pts',(1.18340710698663,-4.55698409498724,385.67785454178));
#50106=CARTESIAN_POINT('Ctrl Pts',(-1.13329271318905,-4.56970502867152,
385.59872666632));
#50107=CARTESIAN_POINT('Ctrl Pts',(-3.17558470949784,-3.47594852891073,
385.519598790861));
#50108=CARTESIAN_POINT('Ctrl Pts',(-4.44896212663648,-1.54054938855827,
385.440470915401));
#50109=CARTESIAN_POINT('Ctrl Pts',(-4.64509797905953,0.767867949435454,
385.361343039941));
#50110=CARTESIAN_POINT('Ctrl Pts',(-3.71650125952819,2.89035894150857,385.282215164481));
#50111=CARTESIAN_POINT('Ctrl Pts',(-1.88801609003413,4.31299799056357,385.203087289022));
#50112=CARTESIAN_POINT('Ctrl Pts',(0.397620511444409,4.69131691017691,385.123959413562));
#50113=CARTESIAN_POINT('Ctrl Pts',(2.58697997463334,3.93371211881083,385.044831538102));
#50114=CARTESIAN_POINT('Ctrl Pts',(4.14994562361626,2.22362491078451,384.965703662642));
#50115=CARTESIAN_POINT('Ctrl Pts',(4.70807153923669,-0.0248757766222604,
384.886575787182));
#50116=CARTESIAN_POINT('Ctrl Pts',(4.12621689144541,-2.26735321191552,384.807447911723));
#50117=CARTESIAN_POINT('Ctrl Pts',(2.54526802482854,-3.96082909308373,384.728320036263));
#50118=CARTESIAN_POINT('Ctrl Pts',(0.348025193093154,-4.69525663705463,
384.649192160803));
#50119=CARTESIAN_POINT('Ctrl Pts',(-1.93348610236405,-4.29280653125647,
384.570064285343));
#50120=CARTESIAN_POINT('Ctrl Pts',(-3.74683616493588,-2.85092531925369,
384.490936409884));
#50121=CARTESIAN_POINT('Ctrl Pts',(-4.65295268895202,-0.718740354514286,
384.411808534423));
#50122=CARTESIAN_POINT('Ctrl Pts',(-4.43243475474589,1.58747553296225,384.332680658964));
#50123=CARTESIAN_POINT('Ctrl Pts',(-3.1386770817443,3.50931084393592,384.253552783504));
#50124=CARTESIAN_POINT('Ctrl Pts',(-1.08494139264941,4.58142538925924,384.174424908044));
#50125=CARTESIAN_POINT('Ctrl Pts',(1.23149465895138,4.54422461238519,384.095297032584));
#50126=CARTESIAN_POINT('Ctrl Pts',(3.24974493247929,3.40671605753374,384.016169157125));
#50127=CARTESIAN_POINT('Ctrl Pts',(4.48112397259501,1.44432834392579,383.937041281665));
#50128=CARTESIAN_POINT('Ctrl Pts',(4.62747399638768,-0.867779255104094,
383.857913406205));
#50129=CARTESIAN_POINT('Ctrl Pts',(3.65335880005533,-2.96976866117404,383.778785530746));
#50130=CARTESIAN_POINT('Ctrl Pts',(1.79464404134943,-4.35267839240186,383.699657655285));
#50131=CARTESIAN_POINT('Ctrl Pts',(-0.498613673709388,-4.68166005036923,
383.620529779826));
#50132=CARTESIAN_POINT('Ctrl Pts',(-2.6711404500085,-3.87705624400286,383.541401904366));
#50133=CARTESIAN_POINT('Ctrl Pts',(-4.19689536445816,-2.13368829087633,
383.462274028906));
#50134=CARTESIAN_POINT('Ctrl Pts',(-4.70644245320202,0.126316497461169,
383.383146153446));
#50135=CARTESIAN_POINT('Ctrl Pts',(-4.07640343439582,2.35573586441245,383.304018277987));
#50136=CARTESIAN_POINT('Ctrl Pts',(-2.45933168995915,4.01475330021607,383.224890402527));
#50137=CARTESIAN_POINT('Ctrl Pts',(-0.246774022640667,4.70166555643666,
383.145762527067));
#50138=CARTESIAN_POINT('Ctrl Pts',(2.02553583557396,4.25014835054481,383.066634651607));
#50139=CARTESIAN_POINT('Ctrl Pts',(3.80739616178709,2.76952900148059,382.987506776148));
#50140=CARTESIAN_POINT('Ctrl Pts',(4.66735936186835,0.618314652917929,382.908378900688));
#50141=CARTESIAN_POINT('Ctrl Pts',(4.39719976949725,-1.68261421899571,382.829251025228));
#50142=CARTESIAN_POINT('Ctrl Pts',(3.06233199907708,-3.57612627716942,382.750123149768));
#50143=CARTESIAN_POINT('Ctrl Pts',(0.985971893936046,-4.60373933310752,
382.670995274309));
#50144=CARTESIAN_POINT('Ctrl Pts',(-1.32912476943063,-4.51663411957612,
382.591867398849));
#50145=CARTESIAN_POINT('Ctrl Pts',(-3.32239616084197,-3.33590170317647,
382.512739523389));
#50146=CARTESIAN_POINT('Ctrl Pts',(-4.51120504233833,-1.34743663628917,
382.433611647929));
#50147=CARTESIAN_POINT('Ctrl Pts',(-4.6077012809677,0.967287614002028,382.354483772469));
#50148=CARTESIAN_POINT('Ctrl Pts',(-3.58851993089967,3.04779939109664,382.27535589701));
#50149=CARTESIAN_POINT('Ctrl Pts',(-1.70043866320114,4.39033766076413,382.19622802155));
#50150=CARTESIAN_POINT('Ctrl Pts',(0.599375308465022,4.66982929692676,382.11710014609));
#50151=CARTESIAN_POINT('Ctrl Pts',(2.75406060140474,3.81860008728635,382.03797227063));
#50152=CARTESIAN_POINT('Ctrl Pts',(4.24189630850143,2.0427609088572,381.95884439517));
#50153=CARTESIAN_POINT('Ctrl Pts',(4.70262796601022,-0.227698564184567,
381.879716519711));
#50154=CARTESIAN_POINT('Ctrl Pts',(4.02469713006905,-2.44302464867774,381.800588644251));
#50155=CARTESIAN_POINT('Ctrl Pts',(2.37225338291554,-4.06681328684744,381.721460768791));
#50156=CARTESIAN_POINT('Ctrl Pts',(0.145408264526719,-4.70589129277765,
381.642332893331));
#50157=CARTESIAN_POINT('Ctrl Pts',(-2.11664502645219,-4.20551664541093,
381.563205017872));
#50158=CARTESIAN_POINT('Ctrl Pts',(-3.86618822286509,-2.68684667374458,
381.484077142412));
#50159=CARTESIAN_POINT('Ctrl Pts',(-4.67959878156707,-0.517601841562701,
381.404949266952));
#50160=CARTESIAN_POINT('Ctrl Pts',(-4.35992297760592,1.77697159577105,381.325821391492));
#50161=CARTESIAN_POINT('Ctrl Pts',(-2.98456494557718,3.6412811630613,381.246693516033));
#50162=CARTESIAN_POINT('Ctrl Pts',(-0.886544566588966,4.62391556522009,
381.167565640573));
#50163=CARTESIAN_POINT('Ctrl Pts',(1.4261377108192,4.48694636168212,381.088437765113));
#50164=CARTESIAN_POINT('Ctrl Pts',(3.39350465953423,3.26353834795189,381.009309889653));
#50165=CARTESIAN_POINT('Ctrl Pts',(4.53919136794792,1.2499192565843,380.930182014193));
#50166=CARTESIAN_POINT('Ctrl Pts',(4.58578901411133,-1.06634682017112,380.851054138734));
#50167=CARTESIAN_POINT('Ctrl Pts',(3.52201475950248,-3.12441489829372,380.771926263274));
#50168=CARTESIAN_POINT('Ctrl Pts',(1.60544369914822,-4.42595830885227,380.692798387814));
#50169=CARTESIAN_POINT('Ctrl Pts',(-0.699858627803908,-4.65583014337095,
380.613670512354));
#50170=CARTESIAN_POINT('Ctrl Pts',(-2.83570192547335,-3.75837079233806,
380.534542636895));
#50171=CARTESIAN_POINT('Ctrl Pts',(-4.28492755989611,-1.95088498617316,
380.455414761435));
#50172=CARTESIAN_POINT('Ctrl Pts',(-4.69662984888973,0.32897490079206,380.376286885975));
#50173=CARTESIAN_POINT('Ctrl Pts',(-3.97112198789876,2.52917903282076,380.297159010515));
#50174=CARTESIAN_POINT('Ctrl Pts',(-2.28407353785474,4.11698487931458,380.218031135056));
#50175=CARTESIAN_POINT('Ctrl Pts',(-0.0439749871787381,4.70793188388869,
380.138903259595));
#50176=CARTESIAN_POINT('Ctrl Pts',(2.20677136913111,4.15893214025144,380.059775384136));
#50177=CARTESIAN_POINT('Ctrl Pts',(3.92318504851847,2.60291672896277,379.980647508676));
#50178=CARTESIAN_POINT('Ctrl Pts',(4.68966526476571,0.416648685685039,379.901519633216));
#50179=CARTESIAN_POINT('Ctrl Pts',(4.32062168826984,-1.8705038491501,379.822391757756));
#50180=CARTESIAN_POINT('Ctrl Pts',(2.90541203179102,-3.70474524743025,379.743263882297));
#50181=CARTESIAN_POINT('Ctrl Pts',(0.786705578939987,-4.64194471691529,
379.664136006837));
#50182=CARTESIAN_POINT('Ctrl Pts',(-1.52248843588733,-4.45517512399035,
379.585008131377));
#50183=CARTESIAN_POINT('Ctrl Pts',(-3.46303740985959,-3.18965959323972,
379.505880255917));
#50184=CARTESIAN_POINT('Ctrl Pts',(-4.56506995418396,-1.15182148627296,
379.426752380458));
#50185=CARTESIAN_POINT('Ctrl Pts',(-4.56174737061485,1.16491087621397,379.347624504998));
#50186=CARTESIAN_POINT('Ctrl Pts',(-3.45387416703998,3.19957960693074,379.268496629538));
#50187=CARTESIAN_POINT('Ctrl Pts',(-1.50970325938777,4.45952379648624,379.189368754078));
#50188=CARTESIAN_POINT('Ctrl Pts',(0.800016973052387,4.63966909010343,379.110240878619));
#50189=CARTESIAN_POINT('Ctrl Pts',(2.91602651267941,3.69639632617822,379.031113003159));
#50190=CARTESIAN_POINT('Ctrl Pts',(4.32596913740423,1.85810318471799,378.951985127699));
#50191=CARTESIAN_POINT('Ctrl Pts',(4.68845088702114,-0.430098480378534,
378.872857252239));
#50192=CARTESIAN_POINT('Ctrl Pts',(3.91570288509923,-2.61415901170123,378.79372937678));
#50193=CARTESIAN_POINT('Ctrl Pts',(2.19483310042462,-4.16524478081583,378.714601501319));
#50194=CARTESIAN_POINT('Ctrl Pts',(-0.0574787096237898,-4.70778638223669,
378.63547362586));
#50195=CARTESIAN_POINT('Ctrl Pts',(-2.29587301412136,-4.11041646623094,
378.5563457504));
#50196=CARTESIAN_POINT('Ctrl Pts',(-3.97836017269986,-2.5177781393738,378.47721787494));
#50197=CARTESIAN_POINT('Ctrl Pts',(-4.69755413716848,-0.315502062123824,
378.398089999481));
#50198=CARTESIAN_POINT('Ctrl Pts',(-4.27931415074721,1.96316754813432,378.318962124021));
#50199=CARTESIAN_POINT('Ctrl Pts',(-2.82491001177881,3.76648906120608,378.239834248561));
#50200=CARTESIAN_POINT('Ctrl Pts',(-0.686501290471962,4.65781841649216,
378.160706373101));
#50201=CARTESIAN_POINT('Ctrl Pts',(1.61813220490064,4.421335159236,378.081578497641));
#50202=CARTESIAN_POINT('Ctrl Pts',(3.5309621248084,3.11429974408401,378.002450622182));
#50203=CARTESIAN_POINT('Ctrl Pts',(4.58882878451957,1.05318887631696,377.923322746722));
#50204=CARTESIAN_POINT('Ctrl Pts',(4.53558751403461,-1.26293401465255,377.844194871262));
#50205=CARTESIAN_POINT('Ctrl Pts',(3.38412979408371,-3.27325861484057,377.765066995802));
#50206=CARTESIAN_POINT('Ctrl Pts',(1.41326180027294,-4.49101853778431,377.685939120342));
#50207=CARTESIAN_POINT('Ctrl Pts',(-0.899803836436171,-4.62135364138776,
377.606811244883));
#50208=CARTESIAN_POINT('Ctrl Pts',(-2.99499706490511,-3.63270546618397,
377.527683369423));
#50209=CARTESIAN_POINT('Ctrl Pts',(-4.36500198367802,-1.76445858702323,
377.448555493963));
#50210=CARTESIAN_POINT('Ctrl Pts',(-4.67809487824384,0.531022346970404,
377.369427618503));
#50211=CARTESIAN_POINT('Ctrl Pts',(-3.858465555114,2.69792512550514,377.290299743043));
#50212=CARTESIAN_POINT('Ctrl Pts',(-2.10457350875104,4.21157058222897,377.211171867584));
#50213=CARTESIAN_POINT('Ctrl Pts',(0.158905716619817,4.70545485538416,377.132043992124));
#50214=CARTESIAN_POINT('Ctrl Pts',(2.38390858774424,4.05999215123785,377.052916116664));
#50215=CARTESIAN_POINT('Ctrl Pts',(4.03168797525527,2.43147043844132,376.973788241204));
#50216=CARTESIAN_POINT('Ctrl Pts',(4.70326173563702,0.21420893755303,376.894660365745));
#50217=CARTESIAN_POINT('Ctrl Pts',(4.23601954588194,-2.0549196650327,376.815532490285));
#50218=CARTESIAN_POINT('Ctrl Pts',(2.74309626604883,-3.82648393411214,376.736404614825));
#50219=CARTESIAN_POINT('Ctrl Pts',(0.585978230290955,-4.67152929311995,
376.657276739365));
#50220=CARTESIAN_POINT('Ctrl Pts',(-1.71302460639056,-4.38544218074737,
376.578148863906));
#50221=CARTESIAN_POINT('Ctrl Pts',(-3.59724726405772,-3.03749379327437,
376.499020988446));
#50222=CARTESIAN_POINT('Ctrl Pts',(-4.61045682670426,-0.954067226005277,
376.419893112986));
#50223=CARTESIAN_POINT('Ctrl Pts',(-4.50732159153776,1.36037071913331,376.340765237526));
#50224=CARTESIAN_POINT('Ctrl Pts',(-3.31281402583599,3.34541770982772,376.261637362067));
#50225=CARTESIAN_POINT('Ctrl Pts',(-1.31616410382415,4.52042790819332,376.182509486607));
#50226=CARTESIAN_POINT('Ctrl Pts',(0.999172883001983,4.60089230230265,376.103381611147));
#50227=CARTESIAN_POINT('Ctrl Pts',(3.07257691207793,3.5673277858007,376.024253735687));
#50228=CARTESIAN_POINT('Ctrl Pts',(4.40200797556968,1.66999467821426,375.945125860228));
#50229=CARTESIAN_POINT('Ctrl Pts',(4.66556662820138,-0.631699641477607,
375.865997984767));
#50230=CARTESIAN_POINT('Ctrl Pts',(3.79943658220811,-2.78043846928895,375.786870109308));
#50231=CARTESIAN_POINT('Ctrl Pts',(2.01333666035538,-4.25594079109181,375.707742233848));
#50232=CARTESIAN_POINT('Ctrl Pts',(-0.260258907652536,-4.70093834665202,
375.628614358388));
#50233=CARTESIAN_POINT('Ctrl Pts',(-2.47083727331916,-4.00768269259632,
375.549486482929));
#50234=CARTESIAN_POINT('Ctrl Pts',(-4.08314356267804,-2.34403352650038,
375.470358607469));
#50235=CARTESIAN_POINT('Ctrl Pts',(-4.70678568739368,-0.112816719080636,
375.391230732009));
#50236=CARTESIAN_POINT('Ctrl Pts',(-4.19075739000426,2.14571838351356,375.312102856549));
#50237=CARTESIAN_POINT('Ctrl Pts',(-2.66001002678919,3.8847003407523,375.232974981089));
#50238=CARTESIAN_POINT('Ctrl Pts',(-0.48518044668226,4.68307451075752,375.153847105629));
#50239=CARTESIAN_POINT('Ctrl Pts',(1.80711601134657,4.34750540330396,375.07471923017));
#50240=CARTESIAN_POINT('Ctrl Pts',(3.66187380043387,2.9592933100083,374.99559135471));
#50241=CARTESIAN_POINT('Ctrl Pts',(4.62991897355734,0.854469882696709,374.91646347925));
#50242=CARTESIAN_POINT('Ctrl Pts',(4.477014386818,-1.45709927207541,374.837335603791));
#50243=CARTESIAN_POINT('Ctrl Pts',(3.23983968516725,-3.41613747848395,374.758207728331));
#50244=CARTESIAN_POINT('Ctrl Pts',(1.8923805371004,-4.17007422695688,374.705455811358));
#50245=CARTESIAN_POINT('Ctrl Pts',(1.16918346556986,-4.36383719750612,374.679079852871));
#50246=CARTESIAN_POINT('Ctrl Pts',(3.57461543774233,3.05624720968358,400.106973382376));
#50247=CARTESIAN_POINT('Ctrl Pts',(4.0811121130032,2.46384394177512,400.08059742389));
#50248=CARTESIAN_POINT('Ctrl Pts',(4.79330604666853,1.02286901533234,400.027845506917));
#50249=CARTESIAN_POINT('Ctrl Pts',(4.70079893715141,-1.38736907251624,399.948717631457));
#50250=CARTESIAN_POINT('Ctrl Pts',(3.47003520682193,-3.46129852254691,399.869589755997));
#50251=CARTESIAN_POINT('Ctrl Pts',(1.39906460383401,-4.69732448980706,399.790461880537));
#50252=CARTESIAN_POINT('Ctrl Pts',(-1.01066992750072,-4.79588345555735,
399.711334005077));
#50253=CARTESIAN_POINT('Ctrl Pts',(-3.17568611614676,-3.73324183578399,
399.632206129617));
#50254=CARTESIAN_POINT('Ctrl Pts',(-4.57176395161188,-1.76663842906183,
399.553078254158));
#50255=CARTESIAN_POINT('Ctrl Pts',(-4.86086545663507,0.627717441216646,
399.473950378698));
#50256=CARTESIAN_POINT('Ctrl Pts',(-3.97299008611081,2.8700865038691,399.394822503238));
#50257=CARTESIAN_POINT('Ctrl Pts',(-2.12312171649347,4.41751015439781,399.315694627778));
#50258=CARTESIAN_POINT('Ctrl Pts',(0.240824931085231,4.89530880016116,399.236566752319));
#50259=CARTESIAN_POINT('Ctrl Pts',(2.54645987869621,4.18779005099161,399.157438876859));
#50260=CARTESIAN_POINT('Ctrl Pts',(4.23551226517086,2.46626839669468,399.078311001399));
#50261=CARTESIAN_POINT('Ctrl Pts',(4.89900639514296,0.147581107578247,398.999183125939));
#50262=CARTESIAN_POINT('Ctrl Pts',(4.37628828662539,-2.20684042213451,398.920055250479));
#50263=CARTESIAN_POINT('Ctrl Pts',(2.79392536583327,-4.02691257828985,398.84092737502));
#50264=CARTESIAN_POINT('Ctrl Pts',(0.53506027464146,-4.87193537854724,398.76179949956));
#50265=CARTESIAN_POINT('Ctrl Pts',(-1.85336068827152,-4.53730074011451,
398.6826716241));
#50266=CARTESIAN_POINT('Ctrl Pts',(-3.7930214436213,-3.10403482078447,398.60354374864));
#50267=CARTESIAN_POINT('Ctrl Pts',(-4.81426566971713,-0.919178929028494,
398.524415873181));
#50268=CARTESIAN_POINT('Ctrl Pts',(-4.6698162047254,1.48824072524753,398.445287997721));
#50269=CARTESIAN_POINT('Ctrl Pts',(-3.39464906397748,3.53530784716552,398.366160122261));
#50270=CARTESIAN_POINT('Ctrl Pts',(-1.29752458459001,4.7263594652241,398.287032246801));
#50271=CARTESIAN_POINT('Ctrl Pts',(1.1137737119676,4.77300240524464,398.207904371341));
#50272=CARTESIAN_POINT('Ctrl Pts',(3.25539038344674,3.66394286164299,398.128776495882));
#50273=CARTESIAN_POINT('Ctrl Pts',(4.60876887024317,1.66772100264832,398.049648620422));
#50274=CARTESIAN_POINT('Ctrl Pts',(4.84621126950363,-0.732311527518088,
397.970520744962));
#50275=CARTESIAN_POINT('Ctrl Pts',(3.91022488643166,-2.95502710301166,397.891392869503));
#50276=CARTESIAN_POINT('Ctrl Pts',(2.02744312611193,-4.46223242473778,397.812264994043));
#50277=CARTESIAN_POINT('Ctrl Pts',(-0.346249984625578,-4.88898300162196,
397.733137118583));
#50278=CARTESIAN_POINT('Ctrl Pts',(-2.63610446859942,-4.13194833857237,
397.654009243123));
#50279=CARTESIAN_POINT('Ctrl Pts',(-4.28767046602801,-2.3744316828985,397.574881367663));
#50280=CARTESIAN_POINT('Ctrl Pts',(-4.90104896930931,-0.0419862171810207,
397.495753492204));
#50281=CARTESIAN_POINT('Ctrl Pts',(-4.3277206609419,2.30062550686931,397.416625616744));
#50282=CARTESIAN_POINT('Ctrl Pts',(-2.70650737541695,4.08617934858649,397.337497741284));
#50283=CARTESIAN_POINT('Ctrl Pts',(-0.429958720199221,4.88233339100534,
397.258369865824));
#50284=CARTESIAN_POINT('Ctrl Pts',(1.95069722820886,4.49631228517985,397.179241990364));
#50285=CARTESIAN_POINT('Ctrl Pts',(3.85902455825875,3.0215845678645,397.100114114904));
#50286=CARTESIAN_POINT('Ctrl Pts',(4.83295381183918,0.815230822914742,397.020986239445));
#50287=CARTESIAN_POINT('Ctrl Pts',(4.63666435411759,-1.58851739343839,396.941858363985));
#50288=CARTESIAN_POINT('Ctrl Pts',(3.31768438527967,-3.60763276424756,396.862730488525));
#50289=CARTESIAN_POINT('Ctrl Pts',(1.19538278395727,-4.75322036537541,396.783602613066));
#50290=CARTESIAN_POINT('Ctrl Pts',(-1.21636071054614,-4.7478953720402,396.704474737606));
#50291=CARTESIAN_POINT('Ctrl Pts',(-3.33358285876919,-3.59294714207171,
396.625346862146));
#50292=CARTESIAN_POINT('Ctrl Pts',(-4.64363382578808,-1.5680270195369,396.546218986686));
#50293=CARTESIAN_POINT('Ctrl Pts',(-4.82930674101173,0.836564548148951,
396.467091111227));
#50294=CARTESIAN_POINT('Ctrl Pts',(-3.84564402196864,3.03859604065724,396.387963235766));
#50295=CARTESIAN_POINT('Ctrl Pts',(-1.93082309891163,4.50488246269648,396.308835360307));
#50296=CARTESIAN_POINT('Ctrl Pts',(0.451514255406424,4.88038714849199,396.229707484847));
#50297=CARTESIAN_POINT('Ctrl Pts',(2.724525005195,4.07418793602703,396.150579609387));
#50298=CARTESIAN_POINT('Ctrl Pts',(4.33783771841656,2.28149244370514,396.071451733927));
#50299=CARTESIAN_POINT('Ctrl Pts',(4.90081577868788,-0.063628180588346,
395.992323858468));
#50300=CARTESIAN_POINT('Ctrl Pts',(4.27714349050859,-2.39334230807068,395.913195983008));
#50301=CARTESIAN_POINT('Ctrl Pts',(2.61783263875445,-4.14354873477711,395.834068107548));
#50302=CARTESIAN_POINT('Ctrl Pts',(0.324657517612272,-4.89046432747023,
395.754940232088));
#50303=CARTESIAN_POINT('Ctrl Pts',(-2.04712797653699,-4.45323600201927,
395.675812356629));
#50304=CARTESIAN_POINT('Ctrl Pts',(-3.92323576387579,-2.93773126460658,
395.596684481169));
#50305=CARTESIAN_POINT('Ctrl Pts',(-4.84939780820125,-0.710904170626361,
395.517556605709));
#50306=CARTESIAN_POINT('Ctrl Pts',(-4.6013595032905,1.68805644558445,395.438428730249));
#50307=CARTESIAN_POINT('Ctrl Pts',(-3.23917916478794,3.67828250415935,395.35930085479));
#50308=CARTESIAN_POINT('Ctrl Pts',(-1.09268591631945,4.77787414341129,395.28017297933));
#50309=CARTESIAN_POINT('Ctrl Pts',(1.31838290117699,4.72058368932118,395.20104510387));
#50310=CARTESIAN_POINT('Ctrl Pts',(3.41022740996214,3.52028306451966,395.12191722841));
#50311=CARTESIAN_POINT('Ctrl Pts',(4.6763425448897,1.46760493487027,395.04278935295));
#50312=CARTESIAN_POINT('Ctrl Pts',(4.81015976025467,-0.940429116322842,
394.963661477491));
#50313=CARTESIAN_POINT('Ctrl Pts',(3.77927746162617,-3.12075402908423,394.884533602031));
#50314=CARTESIAN_POINT('Ctrl Pts',(1.83330650852657,-4.54544069236363,394.805405726571));
#50315=CARTESIAN_POINT('Ctrl Pts',(-0.556568868938532,-4.8695251242939,
394.726277851111));
#50316=CARTESIAN_POINT('Ctrl Pts',(-2.81168042909494,-4.01453571495453,
394.647149975651));
#50317=CARTESIAN_POINT('Ctrl Pts',(-4.3859907284844,-2.18749381065409,394.568022100192));
#50318=CARTESIAN_POINT('Ctrl Pts',(-4.89830693111745,0.169213033090633,
394.488894224732));
#50319=CARTESIAN_POINT('Ctrl Pts',(-4.2245802606628,2.48494777877106,394.409766349272));
#50320=CARTESIAN_POINT('Ctrl Pts',(-2.52794233119419,4.19899409527539,394.330638473813));
#50321=CARTESIAN_POINT('Ctrl Pts',(-0.219205562748669,4.89632441360466,
394.251510598353));
#50322=CARTESIAN_POINT('Ctrl Pts',(2.14260815638517,4.40809189221286,394.172382722893));
#50323=CARTESIAN_POINT('Ctrl Pts',(3.98562524447155,2.85251384792995,394.093254847433));
#50324=CARTESIAN_POINT('Ctrl Pts',(4.86359002316223,0.606247415332937,394.014126971973));
#50325=CARTESIAN_POINT('Ctrl Pts',(4.56391804578379,-1.78681166141541,393.934999096514));
#50326=CARTESIAN_POINT('Ctrl Pts',(3.15916985581216,-3.74722426125376,393.855871221054));
#50327=CARTESIAN_POINT('Ctrl Pts',(0.989481668194294,-4.80030935152189,
393.776743345594));
#50328=CARTESIAN_POINT('Ctrl Pts',(-1.41979291062284,-4.69108003906842,
393.697615470134));
#50329=CARTESIAN_POINT('Ctrl Pts',(-3.48528844770473,-3.44598437000184,
393.618487594675));
#50330=CARTESIAN_POINT('Ctrl Pts',(-4.70687983950021,-1.3665013788897,393.539359719215));
#50331=CARTESIAN_POINT('Ctrl Pts',(-4.788779217989,1.04385700330924,393.460231843755));
#50332=CARTESIAN_POINT('Ctrl Pts',(-3.71115602221747,3.2014629188482,393.381103968295));
#50333=CARTESIAN_POINT('Ctrl Pts',(-1.7349386360522,4.58388828083041,393.301976092836));
#50334=CARTESIAN_POINT('Ctrl Pts',(0.661365043902099,4.85640197272687,393.222848217375));
#50335=CARTESIAN_POINT('Ctrl Pts',(2.89753027033354,3.95301937441519,393.143720341916));
#50336=CARTESIAN_POINT('Ctrl Pts',(4.43210713674341,2.09247943130372,393.064592466456));
#50337=CARTESIAN_POINT('Ctrl Pts',(4.89352359156256,-0.27471931279354,392.985464590996));
#50338=CARTESIAN_POINT('Ctrl Pts',(4.17005537874506,-2.57539938265902,392.906336715536));
#50339=CARTESIAN_POINT('Ctrl Pts',(2.43687819262455,-4.2524896844451,392.827208840076));
#50340=CARTESIAN_POINT('Ctrl Pts',(0.113651821430644,-4.89991092832171,
392.748080964617));
#50341=CARTESIAN_POINT('Ctrl Pts',(-2.23709343224997,-4.3609009180885,392.668953089157));
#50342=CARTESIAN_POINT('Ctrl Pts',(-4.04616402995999,-2.76597188790106,
392.589825213697));
#50343=CARTESIAN_POINT('Ctrl Pts',(-4.87552386667384,-0.501309153611575,
392.510697338238));
#50344=CARTESIAN_POINT('Ctrl Pts',(-4.52435736725662,1.88473718468963,392.431569462777));
#50345=CARTESIAN_POINT('Ctrl Pts',(-3.07769361007314,3.81442602294447,392.352441587318));
#50346=CARTESIAN_POINT('Ctrl Pts',(-0.885817961698088,4.82051557208708,
392.273313711858));
#50347=CARTESIAN_POINT('Ctrl Pts',(1.52054364990864,4.65939812107997,392.194185836399));
#50348=CARTESIAN_POINT('Ctrl Pts',(3.55873111796869,3.37008555855818,392.115057960939));
#50349=CARTESIAN_POINT('Ctrl Pts',(4.73523152985659,1.2647632982709,392.035930085479));
#50350=CARTESIAN_POINT('Ctrl Pts',(4.76517504210868,-1.14680018314682,391.956802210019));
#50351=CARTESIAN_POINT('Ctrl Pts',(3.64131133542052,-3.28068523338327,391.877674334559));
#50352=CARTESIAN_POINT('Ctrl Pts',(1.63576515787017,-4.62020737524832,391.7985464591));
#50353=CARTESIAN_POINT('Ctrl Pts',(-0.765854118981568,-4.84102378742762,
391.71941858364));
#50354=CARTESIAN_POINT('Ctrl Pts',(-2.98203466518281,-3.88966747905899,
391.64029070818));
#50355=CARTESIAN_POINT('Ctrl Pts',(-4.47616552938631,-1.99649342486641,
391.56116283272));
#50356=CARTESIAN_POINT('Ctrl Pts',(-4.88646798113091,0.380098028649711,
391.482034957261));
#50357=CARTESIAN_POINT('Ctrl Pts',(-4.11359416297415,2.66465511921264,391.402907081801));
#50358=CARTESIAN_POINT('Ctrl Pts',(-2.34468250799326,4.30401066201183,391.323779206341));
#50359=CARTESIAN_POINT('Ctrl Pts',(-0.00804530674402572,4.90122220625023,
391.244651330881));
#50360=CARTESIAN_POINT('Ctrl Pts',(2.33053993060416,4.31168499242009,391.165523455421));
#50361=CARTESIAN_POINT('Ctrl Pts',(4.10482400961136,2.67814556962822,391.086395579962));
#50362=CARTESIAN_POINT('Ctrl Pts',(4.88519379734561,0.396138112754947,391.007267704502));
#50363=CARTESIAN_POINT('Ctrl Pts',(4.48269583741255,-1.98178754442679,390.928139829042));
#50364=CARTESIAN_POINT('Ctrl Pts',(2.99478826045289,-3.87985658459878,390.849011953582));
#50365=CARTESIAN_POINT('Ctrl Pts',(0.781742932293461,-4.8384834225003,390.769884078122));
#50366=CARTESIAN_POINT('Ctrl Pts',(-1.62058833618616,-4.62555264661623,
390.690756202663));
#50367=CARTESIAN_POINT('Ctrl Pts',(-3.63052131820232,-3.29262187323105,
390.611628327203));
#50368=CARTESIAN_POINT('Ctrl Pts',(-4.76138445106458,-1.16243793432658,
390.532500451743));
#50369=CARTESIAN_POINT('Ctrl Pts',(-4.7393581930353,1.24921085494409,390.453372576283));
#50370=CARTESIAN_POINT('Ctrl Pts',(-3.56977583309043,3.35838418640342,390.374244700824));
#50371=CARTESIAN_POINT('Ctrl Pts',(-1.53583212443933,4.65438111111899,390.295116825364));
#50372=CARTESIAN_POINT('Ctrl Pts',(0.869987575460632,4.82339770914085,390.215988949904));
#50373=CARTESIAN_POINT('Ctrl Pts',(3.06515437466237,3.82450944586218,390.136861074444));
#50374=CARTESIAN_POINT('Ctrl Pts',(4.51814544822977,1.89958036172247,390.057733198985));
#50375=CARTESIAN_POINT('Ctrl Pts',(4.87714337604219,-0.485300248844855,
389.978605323525));
#50376=CARTESIAN_POINT('Ctrl Pts',(4.05522283069102,-2.75267354320184,389.899477448065));
#50377=CARTESIAN_POINT('Ctrl Pts',(2.25139808767325,-4.35353310459702,389.820349572605));
#50378=CARTESIAN_POINT('Ctrl Pts',(-0.0975649437201896,-4.9002576385082,
389.741221697145));
#50379=CARTESIAN_POINT('Ctrl Pts',(-2.42290426026896,-4.26046696825261,
389.662093821685));
#50380=CARTESIAN_POINT('Ctrl Pts',(-4.16157794510521,-2.58907567460185,
389.582965946226));
#50381=CARTESIAN_POINT('Ctrl Pts',(-4.89259532501792,-0.290783128145012,
389.503838070766));
#50382=CARTESIAN_POINT('Ctrl Pts',(-4.43895280146969,2.07791767602217,389.424710195306));
#50383=CARTESIAN_POINT('Ctrl Pts',(-2.91049230342699,3.9434855640275,389.345582319846));
#50384=CARTESIAN_POINT('Ctrl Pts',(-0.67730490643744,4.85420455952536,389.266454444387));
#50385=CARTESIAN_POINT('Ctrl Pts',(1.71988051445791,4.58955933156866,389.187326568927));
#50386=CARTESIAN_POINT('Ctrl Pts',(3.70062571316616,3.21362928370005,389.108198693467));
#50387=CARTESIAN_POINT('Ctrl Pts',(4.78532645921196,1.05957280106983,389.029070818007));
#50388=CARTESIAN_POINT('Ctrl Pts',(4.71134065862855,-1.35104146507597,388.949942942548));
#50389=CARTESIAN_POINT('Ctrl Pts',(3.49658273219959,-3.43452369898426,388.870815067087));
#50390=CARTESIAN_POINT('Ctrl Pts',(1.43518593891208,-4.68639362012519,388.791687191628));
#50391=CARTESIAN_POINT('Ctrl Pts',(-0.973717059752046,-4.80353192240344,
388.712559316168));
#50392=CARTESIAN_POINT('Ctrl Pts',(-3.14685080276043,-3.75757553046736,
388.633431440709));
#50393=CARTESIAN_POINT('Ctrl Pts',(-4.55802740021425,-1.80178524272377,
388.554303565248));
#50394=CARTESIAN_POINT('Ctrl Pts',(-4.8655541061066,0.590277123519319,388.475175689789));
#50395=CARTESIAN_POINT('Ctrl Pts',(-3.9949684861848,2.83941378393346,388.396047814329));
#50396=CARTESIAN_POINT('Ctrl Pts',(-2.15706824758342,4.401034016827,388.316919938869));
#50397=CARTESIAN_POINT('Ctrl Pts',(0.2031298906366,4.89701767298537,388.237792063409));
#50398=CARTESIAN_POINT('Ctrl Pts',(2.51414353256258,4.20727062829036,388.15866418795));
#50399=CARTESIAN_POINT('Ctrl Pts',(4.21639948317845,2.49880356175781,388.07953631249));
#50400=CARTESIAN_POINT('Ctrl Pts',(4.8977250128471,0.185293120576435,388.00040843703));
#50401=CARTESIAN_POINT('Ctrl Pts',(4.39314857117775,-2.17308294217223,387.92128056157));
#50402=CARTESIAN_POINT('Ctrl Pts',(2.82484488118912,-4.00528341559255,387.842152686111));
#50403=CARTESIAN_POINT('Ctrl Pts',(0.572552379142054,-4.86767168317048,
387.763024810651));
#50404=CARTESIAN_POINT('Ctrl Pts',(-1.8183740791475,-4.55143488916249,387.683896935191));
#50405=CARTESIAN_POINT('Ctrl Pts',(-3.76901175041157,-3.13314446958014,
387.604769059731));
#50406=CARTESIAN_POINT('Ctrl Pts',(-4.80704643700727,-0.956215663151738,
387.525641184272));
#50407=CARTESIAN_POINT('Ctrl Pts',(-4.68113544861982,1.45224472926429,387.446513308812));
#50408=CARTESIAN_POINT('Ctrl Pts',(-3.4217660194141,3.50906841631565,387.367385433352));
#50409=CARTESIAN_POINT('Ctrl Pts',(-1.33387333558782,4.71623003749912,387.288257557892));
#50410=CARTESIAN_POINT('Ctrl Pts',(1.07699440584981,4.78143565174407,387.209129682432));
#50411=CARTESIAN_POINT('Ctrl Pts',(3.22708601435485,3.68889681313483,387.130001806972));
#50412=CARTESIAN_POINT('Ctrl Pts',(4.59579286645524,1.70315347829848,387.050873931513));
#50413=CARTESIAN_POINT('Ctrl Pts',(4.85170555271451,-0.694979907450764,
386.971746056053));
#50414=CARTESIAN_POINT('Ctrl Pts',(3.93285910810722,-2.92483556422906,386.892618180594));
#50415=CARTESIAN_POINT('Ctrl Pts',(2.06173678907561,-4.44649134201037,386.813490305133));
#50416=CARTESIAN_POINT('Ctrl Pts',(-0.308600515715983,-4.89150381413537,
386.734362429674));
#50417=CARTESIAN_POINT('Ctrl Pts',(-2.60421538121517,-4.15212067385372,
386.655234554214));
#50418=CARTESIAN_POINT('Ctrl Pts',(-4.26926316786226,-2.40737114827269,
386.576106678754));
#50419=CARTESIAN_POINT('Ctrl Pts',(-4.90058047890116,-0.0797170735407659,
386.496978803294));
#50420=CARTESIAN_POINT('Ctrl Pts',(-4.34530441538657,2.26723915360136,386.417850927834));
#50421=CARTESIAN_POINT('Ctrl Pts',(-2.7378857634756,4.06522144392636,386.338723052375));
#50422=CARTESIAN_POINT('Ctrl Pts',(-0.46753399145535,4.87887854007813,386.259595176915));
#50423=CARTESIAN_POINT('Ctrl Pts',(1.91602329550907,4.51119702219572,386.180467301455));
#50424=CARTESIAN_POINT('Ctrl Pts',(3.83564767539653,3.05120480338935,386.101339425996));
#50425=CARTESIAN_POINT('Ctrl Pts',(4.82653429894221,0.852414513681883,386.022211550536));
#50426=CARTESIAN_POINT('Ctrl Pts',(4.6487565885712,-1.55277365453466,385.943083675076));
#50427=CARTESIAN_POINT('Ctrl Pts',(3.34536043531169,-3.58198372411883,385.863955799616));
#50428=CARTESIAN_POINT('Ctrl Pts',(1.23194135821188,-4.74387650892475,385.784827924157));
#50429=CARTESIAN_POINT('Ctrl Pts',(-1.17977165769507,-4.75711915739983,
385.705700048696));
#50430=CARTESIAN_POINT('Ctrl Pts',(-3.30582275282872,-3.61850518431036,
385.626572173237));
#50431=CARTESIAN_POINT('Ctrl Pts',(-4.63142431084255,-1.60373086736447,
385.547444297777));
#50432=CARTESIAN_POINT('Ctrl Pts',(-4.8356041463375,0.799359982689007,385.468316422318));
#50433=CARTESIAN_POINT('Ctrl Pts',(-3.86892353648086,3.00889921912741,385.389188546857));
#50434=CARTESIAN_POINT('Ctrl Pts',(-1.96544797859558,4.48988397238009,385.310060671398));
#50435=CARTESIAN_POINT('Ctrl Pts',(0.413927844466849,4.88371862227708,385.230932795938));
#50436=CARTESIAN_POINT('Ctrl Pts',(2.69307798204115,4.09504271340925,385.151804920478));
#50437=CARTESIAN_POINT('Ctrl Pts',(4.32014445230215,2.31482089010014,385.072677045018));
#50438=CARTESIAN_POINT('Ctrl Pts',(4.90116039726593,-0.0258959895184648,
384.993549169559));
#50439=CARTESIAN_POINT('Ctrl Pts',(4.29544255017007,-2.3603425895809,384.914421294099));
#50440=CARTESIAN_POINT('Ctrl Pts',(2.6496553290988,-4.12327181725621,384.835293418639));
#50441=CARTESIAN_POINT('Ctrl Pts',(0.362298507876016,-4.88781992642853,
384.756165543179));
#50442=CARTESIAN_POINT('Ctrl Pts',(-2.01278282086323,-4.46886441481938,
384.67703766772));
#50443=CARTESIAN_POINT('Ctrl Pts',(-3.90050254623037,-2.96784833319553,
384.59790979226));
#50444=CARTESIAN_POINT('Ctrl Pts',(-4.84378099597461,-0.748217551943446,
384.5187819168));
#50445=CARTESIAN_POINT('Ctrl Pts',(-4.61421911336287,1.65258156103648,384.43965404134));
#50446=CARTESIAN_POINT('Ctrl Pts',(-3.26740145825086,3.65323576471889,384.36052616588));
#50447=CARTESIAN_POINT('Ctrl Pts',(-1.12943733813143,4.76932019697102,384.281398290421));
#50448=CARTESIAN_POINT('Ctrl Pts',(1.28200109144381,4.730593730552,384.202270414961));
#50449=CARTESIAN_POINT('Ctrl Pts',(3.38302445736953,3.54643332981752,384.123142539501));
#50450=CARTESIAN_POINT('Ctrl Pts',(4.66490518818293,1.50356357606356,384.044014664042));
#50451=CARTESIAN_POINT('Ctrl Pts',(4.81725736354257,-0.903368881131035,
383.964886788581));
#50452=CARTESIAN_POINT('Ctrl Pts',(3.80319145930759,-3.09156571430251,383.885758913122));
#50453=CARTESIAN_POINT('Ctrl Pts',(1.86824652712842,-4.53119175889452,383.806631037662));
#50454=CARTESIAN_POINT('Ctrl Pts',(-0.519062968936094,-4.87366571240583,
383.727503162202));
#50455=CARTESIAN_POINT('Ctrl Pts',(-2.78069007236013,-4.03606325067867,
383.648375286742));
#50456=CARTESIAN_POINT('Ctrl Pts',(-4.36901971015636,-2.22119576225652,
383.569247411283));
#50457=CARTESIAN_POINT('Ctrl Pts',(-4.89946449866066,0.131497027969629,
383.490119535823));
#50458=CARTESIAN_POINT('Ctrl Pts',(-4.24358612851044,2.45235001823044,383.410991660363));
#50459=CARTESIAN_POINT('Ctrl Pts',(-2.56019454719736,4.17940758032786,383.331863784903));
#50460=CARTESIAN_POINT('Ctrl Pts',(-0.256894793709217,4.89449169035623,
383.252735909444));
#50461=CARTESIAN_POINT('Ctrl Pts',(2.10860772565226,4.4244567238612,383.173608033984));
#50462=CARTESIAN_POINT('Ctrl Pts',(3.96354624804163,2.88311376494861,383.094480158524));
#50463=CARTESIAN_POINT('Ctrl Pts',(4.85877851973045,0.643673161011885,383.015352283064));
#50464=CARTESIAN_POINT('Ctrl Pts',(4.57753906021165,-1.7516221037192,382.936224407605));
#50465=CARTESIAN_POINT('Ctrl Pts',(3.18792528789615,-3.72279145276676,382.857096532144));
#50466=CARTESIAN_POINT('Ctrl Pts',(1.0264088723172,-4.79254928705272,382.777968656685));
#50467=CARTESIAN_POINT('Ctrl Pts',(-1.38363523762741,-4.70187168808304,
382.698840781225));
#50468=CARTESIAN_POINT('Ctrl Pts',(-3.45865527994654,-3.47271471567979,
382.619712905766));
#50469=CARTESIAN_POINT('Ctrl Pts',(-4.69621995188282,-1.40269811632394,
382.540585030305));
#50470=CARTESIAN_POINT('Ctrl Pts',(-4.79667372352029,1.00695830702717,382.461457154846));
#50471=CARTESIAN_POINT('Ctrl Pts',(-3.73569339878306,3.17279666418915,382.382329279386));
#50472=CARTESIAN_POINT('Ctrl Pts',(-1.77017756943694,4.57039552059375,382.303201403927));
#50473=CARTESIAN_POINT('Ctrl Pts',(0.623957070419554,4.86134975251467,382.224073528466));
#50474=CARTESIAN_POINT('Ctrl Pts',(2.86701097015694,3.97520967233186,382.144945653007));
#50475=CARTESIAN_POINT('Ctrl Pts',(4.41586624656651,2.12653923886574,382.065817777547));
#50476=CARTESIAN_POINT('Ctrl Pts',(4.89549357056314,-0.237037006764906,
381.986689902087));
#50477=CARTESIAN_POINT('Ctrl Pts',(4.18975922954695,-2.54321871659263,381.907562026627));
#50478=CARTESIAN_POINT('Ctrl Pts',(2.46954495821251,-4.2336026669219,381.828434151167));
#50479=CARTESIAN_POINT('Ctrl Pts',(0.151371792377024,-4.89889073387779,
381.749306275708));
#50480=CARTESIAN_POINT('Ctrl Pts',(-2.20345351430222,-4.37799456969858,
381.670178400248));
#50481=CARTESIAN_POINT('Ctrl Pts',(-4.0247495069615,-2.79704044450812,381.591050524788));
#50482=CARTESIAN_POINT('Ctrl Pts',(-4.87151990622233,-0.53882988528894,
381.511922649328));
#50483=CARTESIAN_POINT('Ctrl Pts',(-4.53873346122441,1.84984929385154,381.432794773869));
#50484=CARTESIAN_POINT('Ctrl Pts',(-3.10696882840965,3.79061849060175,381.353666898409));
#50485=CARTESIAN_POINT('Ctrl Pts',(-0.922903801262455,4.8135529929166,381.274539022949));
#50486=CARTESIAN_POINT('Ctrl Pts',(1.48462690319438,4.67096636685734,381.195411147489));
#50487=CARTESIAN_POINT('Ctrl Pts',(3.53268010195595,3.39738357258133,381.11628327203));
#50488=CARTESIAN_POINT('Ctrl Pts',(4.72535406116718,1.30118132426344,381.03715539657));
#50489=CARTESIAN_POINT('Ctrl Pts',(4.77386278412913,-1.11008015940651,380.95802752111));
#50490=CARTESIAN_POINT('Ctrl Pts',(3.66646069712405,-3.25255434980657,380.87889964565));
#50491=CARTESIAN_POINT('Ctrl Pts',(1.67128664310421,-4.60747705350581,380.799771770191));
#50492=CARTESIAN_POINT('Ctrl Pts',(-0.728561442129978,-4.84677646142697,
380.72064389473));
#50493=CARTESIAN_POINT('Ctrl Pts',(-2.95200059297187,-3.91251023527028,
380.641516019271));
#50494=CARTESIAN_POINT('Ctrl Pts',(-4.46066230869571,-2.03089527297259,
380.562388143811));
#50495=CARTESIAN_POINT('Ctrl Pts',(-4.88924945684393,0.342466919208695,
380.483260268352));
#50496=CARTESIAN_POINT('Ctrl Pts',(-4.13398684739545,2.63290649047066,380.404132392891));
#50497=CARTESIAN_POINT('Ctrl Pts',(-2.37774865459918,4.28583191195745,380.325004517432));
#50498=CARTESIAN_POINT('Ctrl Pts',(-0.045778502691498,4.90101501433043,
380.245876641972));
#50499=CARTESIAN_POINT('Ctrl Pts',(2.29727614588441,4.32949952668338,380.166748766512));
#50500=CARTESIAN_POINT('Ctrl Pts',(4.08408390371697,2.70966833937311,380.087620891052));
#50501=CARTESIAN_POINT('Ctrl Pts',(4.88199923908331,0.433736407961101,380.008493015593));
#50502=CARTESIAN_POINT('Ctrl Pts',(4.49782033548913,-1.94721752037656,379.929365140133));
#50503=CARTESIAN_POINT('Ctrl Pts',(3.02456967131446,-3.8566853832489,379.850237264673));
#50504=CARTESIAN_POINT('Ctrl Pts',(0.818970186768649,-4.83232156164975,
379.771109389213));
#50505=CARTESIAN_POINT('Ctrl Pts',(-1.5849291934243,-4.63789211752843,379.691981513754));
#50506=CARTESIAN_POINT('Ctrl Pts',(-3.60506455052847,-3.32047487997185,
379.612853638294));
#50507=CARTESIAN_POINT('Ctrl Pts',(-4.75229398783147,-1.19906033844088,
379.533725762834));
#50508=CARTESIAN_POINT('Ctrl Pts',(-4.74883513745721,1.21268655441244,379.454597887374));
#50509=CARTESIAN_POINT('Ctrl Pts',(-3.59552550201493,3.33080173627333,379.375470011914));
#50510=CARTESIAN_POINT('Ctrl Pts',(-1.57161966738812,4.64241913909978,379.296342136455));
#50511=CARTESIAN_POINT('Ctrl Pts',(0.832827511814025,4.82995260614083,379.217214260995));
#50512=CARTESIAN_POINT('Ctrl Pts',(3.03561947651265,3.84799405350607,379.138086385535));
#50513=CARTESIAN_POINT('Ctrl Pts',(4.50338709582942,1.93430827613337,379.058958510075));
#50514=CARTESIAN_POINT('Ctrl Pts',(4.88073505691033,-0.447737809714184,
378.979830634616));
#50515=CARTESIAN_POINT('Ctrl Pts',(4.07629487954206,-2.72137169402128,378.900702759156));
#50516=CARTESIAN_POINT('Ctrl Pts',(2.28484826128058,-4.33607106317736,378.821574883696));
#50517=CARTESIAN_POINT('Ctrl Pts',(-0.0598360438974424,-4.90086354532054,
378.742447008237));
#50518=CARTESIAN_POINT('Ctrl Pts',(-2.39003205456549,-4.27899411312408,
378.663319132776));
#50519=CARTESIAN_POINT('Ctrl Pts',(-4.14152188682712,-2.62103802012351,
378.584191257317));
#50520=CARTESIAN_POINT('Ctrl Pts',(-4.89021165231393,-0.328441528394388,
378.505063381857));
#50521=CARTESIAN_POINT('Ctrl Pts',(-4.45481868070814,2.04368157109047,378.425935506397));
#50522=CARTESIAN_POINT('Ctrl Pts',(-2.94076607803947,3.92096145304356,378.346807630937));
#50523=CARTESIAN_POINT('Ctrl Pts',(-0.714656289627798,4.84884627820851,
378.267679755477));
#50524=CARTESIAN_POINT('Ctrl Pts',(1.68449553370326,4.60266429787517,378.188551880018));
#50525=CARTESIAN_POINT('Ctrl Pts',(3.67577501448982,3.24202434982427,378.109424004558));
#50526=CARTESIAN_POINT('Ctrl Pts',(4.77702722252339,1.09638257796792,378.030296129098));
#50527=CARTESIAN_POINT('Ctrl Pts',(4.72160240490404,-1.31472984753725,377.951168253638));
#50528=CARTESIAN_POINT('Ctrl Pts',(3.52292075167996,-3.40750249000403,377.872040378179));
#50529=CARTESIAN_POINT('Ctrl Pts',(1.47122292189925,-4.67520555228101,377.792912502719));
#50530=CARTESIAN_POINT('Ctrl Pts',(-0.936706864306466,-4.81088599868696,
377.713784627259));
#50531=CARTESIAN_POINT('Ctrl Pts',(-3.11782879297974,-3.78169108464289,
377.634656751799));
#50532=CARTESIAN_POINT('Ctrl Pts',(-4.54402076903412,-1.83682309779347,
377.555528876339));
#50533=CARTESIAN_POINT('Ctrl Pts',(-4.86995432435985,0.552800796535157,
377.47640100088));
#50534=CARTESIAN_POINT('Ctrl Pts',(-4.01671011481814,2.80857324909262,377.39727312542));
#50535=CARTESIAN_POINT('Ctrl Pts',(-2.19088691585556,4.3842967924097,377.31814524996));
#50536=CARTESIAN_POINT('Ctrl Pts',(0.165422806069439,4.89843639718154,377.2390173745));
#50537=CARTESIAN_POINT('Ctrl Pts',(2.48167816983692,4.22650178082969,377.159889499041));
#50538=CARTESIAN_POINT('Ctrl Pts',(4.19703678539643,2.53119064158134,377.080761623581));
#50539=CARTESIAN_POINT('Ctrl Pts',(4.89615333254211,0.222994139474255,377.001633748121));
#50540=CARTESIAN_POINT('Ctrl Pts',(4.40974846437591,-2.13919665363753,376.922505872661));
#50541=CARTESIAN_POINT('Ctrl Pts',(2.85559696215369,-3.98341685387501,376.843377997201));
#50542=CARTESIAN_POINT('Ctrl Pts',(0.610010547211784,-4.86311946946737,
376.764250121742));
#50543=CARTESIAN_POINT('Ctrl Pts',(-1.78327969114604,-4.56529926566563,
376.685122246282));
#50544=CARTESIAN_POINT('Ctrl Pts',(-3.74477865997579,-3.16206841006309,
376.605994370822));
#50545=CARTESIAN_POINT('Ctrl Pts',(-4.79954228053442,-0.99319572046786,
376.526866495362));
#50546=CARTESIAN_POINT('Ctrl Pts',(-4.69217723182007,1.41616265569688,376.447738619902));
#50547=CARTESIAN_POINT('Ctrl Pts',(-3.44868015951322,3.48262099568224,376.368610744443));
#50548=CARTESIAN_POINT('Ctrl Pts',(-1.37014302527182,4.70582106870975,376.289482868983));
#50549=CARTESIAN_POINT('Ctrl Pts',(1.04015126435086,4.78958549295691,376.210354993523));
#50550=CARTESIAN_POINT('Ctrl Pts',(3.1985903683765,3.71363211500125,376.131227118063));
#50551=CARTESIAN_POINT('Ctrl Pts',(4.58254446188996,1.73848500650345,376.052099242604));
#50552=CARTESIAN_POINT('Ctrl Pts',(4.85691226192656,-0.657607098782336,
375.972971367144));
#50553=CARTESIAN_POINT('Ctrl Pts',(3.95526022777064,-2.89447065515981,375.893843491684));
#50554=CARTESIAN_POINT('Ctrl Pts',(2.09590823415934,-4.43048672573689,375.814715616224));
#50555=CARTESIAN_POINT('Ctrl Pts',(-0.270932724915457,-4.89373465602332,
375.735587740765));
#50556=CARTESIAN_POINT('Ctrl Pts',(-2.57217200103202,-4.17204699080374,
375.656459865305));
#50557=CARTESIAN_POINT('Ctrl Pts',(-4.25060268497819,-2.44016774048634,
375.577331989845));
#50558=CARTESIAN_POINT('Ctrl Pts',(-4.8998218096771,-0.117443592583374,
375.498204114385));
#50559=CARTESIAN_POINT('Ctrl Pts',(-4.36263000323237,2.23371923670199,375.419076238926));
#50560=CARTESIAN_POINT('Ctrl Pts',(-2.76910316484765,4.04402084944263,375.339948363465));
#50561=CARTESIAN_POINT('Ctrl Pts',(-0.505078814327535,4.87513818307261,
375.260820488006));
#50562=CARTESIAN_POINT('Ctrl Pts',(1.88123000134211,4.52580661359865,375.181692612546));
#50563=CARTESIAN_POINT('Ctrl Pts',(3.81205567946445,3.08066074485737,375.102564737086));
#50564=CARTESIAN_POINT('Ctrl Pts',(4.81980261485754,0.889513660705449,375.023436861627));
#50565=CARTESIAN_POINT('Ctrl Pts',(4.6606270588275,-1.51685826939215,374.944308986167));
#50566=CARTESIAN_POINT('Ctrl Pts',(3.37271297305025,-3.55624114494146,374.865181110707));
#50567=CARTESIAN_POINT('Ctrl Pts',(1.96999142168877,-4.34109857602843,374.812429193734));
#50568=CARTESIAN_POINT('Ctrl Pts',(1.21713437249897,-4.54280821229842,374.786053235247));
#50569=CARTESIAN_POINT('Ctrl Pts',(3.71544298812251,3.17665283523749,400.213946764753));
#50570=CARTESIAN_POINT('Ctrl Pts',(4.24189388987153,2.56091091663784,400.187570806266));
#50571=CARTESIAN_POINT('Ctrl Pts',(4.98214581433909,1.06316653552657,400.134818889293));
#50572=CARTESIAN_POINT('Ctrl Pts',(4.88599424296224,-1.44202664096201,400.055691013833));
#50573=CARTESIAN_POINT('Ctrl Pts',(3.60674265589465,-3.5976617763163,399.976563138373));
#50574=CARTESIAN_POINT('Ctrl Pts',(1.45418293597717,-4.88238291434578,399.897435262914));
#50575=CARTESIAN_POINT('Ctrl Pts',(-1.05048684560331,-4.98482476427098,
399.818307387454));
#50576=CARTESIAN_POINT('Ctrl Pts',(-3.30079722370572,-3.88031872051941,
399.739179511994));
#50577=CARTESIAN_POINT('Ctrl Pts',(-4.75187572291575,-1.83623790534267,
399.660051636534));
#50578=CARTESIAN_POINT('Ctrl Pts',(-5.05236683263146,0.652447348843657,
399.580923761074));
#50579=CARTESIAN_POINT('Ctrl Pts',(-4.12951222709533,2.98315803806871,399.501795885615));
#50580=CARTESIAN_POINT('Ctrl Pts',(-2.20676540787796,4.59154485677586,399.422668010155));
#50581=CARTESIAN_POINT('Ctrl Pts',(0.250312604852073,5.08816712539591,399.343540134695));
#50582=CARTESIAN_POINT('Ctrl Pts',(2.64678163724731,4.35277457160906,399.264412259235));
#50583=CARTESIAN_POINT('Ctrl Pts',(4.40237687684668,2.5634308867403,399.185284383776));
#50584=CARTESIAN_POINT('Ctrl Pts',(5.09201039289903,0.153395295488701,399.106156508315));
#50585=CARTESIAN_POINT('Ctrl Pts',(4.54869898923014,-2.29378234250105,399.027028632856));
#50586=CARTESIAN_POINT('Ctrl Pts',(2.90399641321393,-4.1855590799549,398.947900757396));
#50587=CARTESIAN_POINT('Ctrl Pts',(0.556139808676901,-5.06387287138275,
398.868772881936));
#50588=CARTESIAN_POINT('Ctrl Pts',(-1.92637672321179,-4.7160547794503,398.789645006477));
#50589=CARTESIAN_POINT('Ctrl Pts',(-3.94245343924376,-3.22632311381047,
398.710517131017));
#50590=CARTESIAN_POINT('Ctrl Pts',(-5.00393117442772,-0.955391416550765,
398.631389255557));
#50591=CARTESIAN_POINT('Ctrl Pts',(-4.85379089746955,1.54687228977885,398.552261380098));
#50592=CARTESIAN_POINT('Ctrl Pts',(-3.52838655837555,3.67458681370817,398.473133504638));
#50593=CARTESIAN_POINT('Ctrl Pts',(-1.34864258930642,4.91256176790427,398.394005629178));
#50594=CARTESIAN_POINT('Ctrl Pts',(1.15765256446685,4.96104227929438,398.314877753718));
#50595=CARTESIAN_POINT('Ctrl Pts',(3.38364156492812,3.80828960520879,398.235749878258));
#50596=CARTESIAN_POINT('Ctrl Pts',(4.79033850803188,1.73342347263734,398.156622002798));
#50597=CARTESIAN_POINT('Ctrl Pts',(5.03713532094231,-0.761162082306909,
398.077494127339));
#50598=CARTESIAN_POINT('Ctrl Pts',(4.064274294482,-3.07144500459355,397.998366251879));
#50599=CARTESIAN_POINT('Ctrl Pts',(2.10731741020158,-4.63802903070772,397.919238376419));
#50600=CARTESIAN_POINT('Ctrl Pts',(-0.359891042804634,-5.08159211215712,
397.840110500959));
#50601=CARTESIAN_POINT('Ctrl Pts',(-2.73995791558548,-4.29473288783458,
397.7609826255));
#50602=CARTESIAN_POINT('Ctrl Pts',(-4.45658993137603,-2.46797612236942,
397.68185475004));
#50603=CARTESIAN_POINT('Ctrl Pts',(-5.0941334374604,-0.0436403296913884,
397.60272687458));
#50604=CARTESIAN_POINT('Ctrl Pts',(-4.49821796618352,2.39126223692249,397.52359899912));
#50605=CARTESIAN_POINT('Ctrl Pts',(-2.81313445472219,4.24716075710381,397.44447112366));
#50606=CARTESIAN_POINT('Ctrl Pts',(-0.446897614573966,5.07468052975907,
397.365343248201));
#50607=CARTESIAN_POINT('Ctrl Pts',(2.02754798795257,4.67345152040515,397.286215372741));
#50608=CARTESIAN_POINT('Ctrl Pts',(4.01105684952524,3.14062460458175,397.207087497281));
#50609=CARTESIAN_POINT('Ctrl Pts',(5.02335556505595,0.847348112672217,397.127959621822));
#50610=CARTESIAN_POINT('Ctrl Pts',(4.8193329780012,-1.65109951371132,397.048831746361));
#50611=CARTESIAN_POINT('Ctrl Pts',(3.44838973612117,-3.74976108370145,396.969703870902));
#50612=CARTESIAN_POINT('Ctrl Pts',(1.24247675313054,-4.94048089511111,396.890575995442));
#50613=CARTESIAN_POINT('Ctrl Pts',(-1.26428113785597,-4.93494611535824,
396.811448119982));
#50614=CARTESIAN_POINT('Ctrl Pts',(-3.46491455477013,-3.73449689853531,
396.732320244522));
#50615=CARTESIAN_POINT('Ctrl Pts',(-4.82657702287821,-1.62980188957181,
396.653192369063));
#50616=CARTESIAN_POINT('Ctrl Pts',(-5.01956481218505,0.869522313285533,
396.574064493603));
#50617=CARTESIAN_POINT('Ctrl Pts',(-3.99714916613881,3.15830627087741,396.494936618143));
#50618=CARTESIAN_POINT('Ctrl Pts',(-2.00689088633465,4.68235933343167,396.415808742683));
#50619=CARTESIAN_POINT('Ctrl Pts',(0.469302363710116,5.07265761198643,396.336680867223));
#50620=CARTESIAN_POINT('Ctrl Pts',(2.83186191712685,4.23469692414397,396.257552991764));
#50621=CARTESIAN_POINT('Ctrl Pts',(4.50873360091663,2.37137539689376,396.178425116304));
#50622=CARTESIAN_POINT('Ctrl Pts',(5.09389105993074,-0.066134912001412,
396.099297240844));
#50623=CARTESIAN_POINT('Ctrl Pts',(4.44564822923743,-2.48763176111453,396.020169365385));
#50624=CARTESIAN_POINT('Ctrl Pts',(2.72096623850579,-4.30679029974057,395.941041489925));
#50625=CARTESIAN_POINT('Ctrl Pts',(0.337447906876279,-5.08313179714755,
395.861913614465));
#50626=CARTESIAN_POINT('Ctrl Pts',(-2.12777777601096,-4.6286781798848,395.782785739005));
#50627=CARTESIAN_POINT('Ctrl Pts',(-4.07779775573568,-3.05346776965875,
395.703657863545));
#50628=CARTESIAN_POINT('Ctrl Pts',(-5.04044739830187,-0.738911349202079,
395.624529988086));
#50629=CARTESIAN_POINT('Ctrl Pts',(-4.78263723751197,1.75456006206446,395.545402112625));
#50630=CARTESIAN_POINT('Ctrl Pts',(-3.36679168002614,3.82319418030715,395.466274237166));
#50631=CARTESIAN_POINT('Ctrl Pts',(-1.13573398221921,4.9661059471844,395.387146361706));
#50632=CARTESIAN_POINT('Ctrl Pts',(1.37032265180738,4.90655844630137,395.308018486247));
#50633=CARTESIAN_POINT('Ctrl Pts',(3.54457863759732,3.65897010631632,395.228890610786));
#50634=CARTESIAN_POINT('Ctrl Pts',(4.86057435298355,1.52542352025471,395.149762735327));
#50635=CARTESIAN_POINT('Ctrl Pts',(4.99966350625814,-0.977478788116796,
395.070634859867));
#50636=CARTESIAN_POINT('Ctrl Pts',(3.9281679916419,-3.24370100139759,394.991506984407));
#50637=CARTESIAN_POINT('Ctrl Pts',(1.90553247777794,-4.72451541781389,394.912379108947));
#50638=CARTESIAN_POINT('Ctrl Pts',(-0.578495767592555,-5.0613676614039,
394.833251233488));
#50639=CARTESIAN_POINT('Ctrl Pts',(-2.92245096488478,-4.17269461078471,
394.754123358028));
#50640=CARTESIAN_POINT('Ctrl Pts',(-4.55878367391877,-2.27367354108707,
394.674995482568));
#50641=CARTESIAN_POINT('Ctrl Pts',(-5.09128337239731,0.175879444445247,
394.595867607109));
#50642=CARTESIAN_POINT('Ctrl Pts',(-4.39101418897073,2.58284617220721,394.516739731648));
#50643=CARTESIAN_POINT('Ctrl Pts',(-2.62753456208024,4.36442001669197,394.437611856189));
#50644=CARTESIAN_POINT('Ctrl Pts',(-0.227841507780872,5.08922275051504,
394.358483980729));
#50645=CARTESIAN_POINT('Ctrl Pts',(2.22701954646155,4.58175554746277,394.279356105269));
#50646=CARTESIAN_POINT('Ctrl Pts',(4.14264516722633,2.96489307994134,394.200228229809));
#50647=CARTESIAN_POINT('Ctrl Pts',(5.05519873770637,0.630131477804167,394.12110035435));
#50648=CARTESIAN_POINT('Ctrl Pts',(4.74372071539057,-1.85720589364835,394.04197247889));
#50649=CARTESIAN_POINT('Ctrl Pts',(3.28363027953537,-3.89485200544849,393.96284460343));
#50650=CARTESIAN_POINT('Ctrl Pts',(1.02846384177488,-4.98942502530997,393.883716727971));
#50651=CARTESIAN_POINT('Ctrl Pts',(-1.47572786674121,-4.87589245373102,
393.80458885251));
#50652=CARTESIAN_POINT('Ctrl Pts',(-3.62259682199201,-3.58174429884674,
393.725460977051));
#50653=CARTESIAN_POINT('Ctrl Pts',(-4.89231471194326,-1.42033683199839,
393.646333101591));
#50654=CARTESIAN_POINT('Ctrl Pts',(-4.97744064418338,1.0849813780241,393.567205226131));
#50655=CARTESIAN_POINT('Ctrl Pts',(-3.85736280188092,3.32758954375282,393.488077350671));
#50656=CARTESIAN_POINT('Ctrl Pts',(-1.8032892495463,4.76447770899377,393.408949475212));
#50657=CARTESIAN_POINT('Ctrl Pts',(0.687420551315965,5.04772750281314,393.329821599752));
#50658=CARTESIAN_POINT('Ctrl Pts',(3.01168299451616,4.1087547380648,393.250693724292));
#50659=CARTESIAN_POINT('Ctrl Pts',(4.60671691000739,2.1749159220714,393.171565848832));
#50660=CARTESIAN_POINT('Ctrl Pts',(5.08631158572023,-0.285542308591735,
393.092437973373));
#50661=CARTESIAN_POINT('Ctrl Pts',(4.33434121428917,-2.67686125810472,393.013310097913));
#50662=CARTESIAN_POINT('Ctrl Pts',(2.5328828097419,-4.42002314803234,392.934182222453));
#50663=CARTESIAN_POINT('Ctrl Pts',(0.118129312194917,-5.09295056157313,
392.855054346993));
#50664=CARTESIAN_POINT('Ctrl Pts',(-2.32522721713463,-4.53270541131057,
392.775926471534));
#50665=CARTESIAN_POINT('Ctrl Pts',(-4.20556897258945,-2.87494166442045,
392.696798596073));
#50666=CARTESIAN_POINT('Ctrl Pts',(-5.06760273359595,-0.521059009593531,
392.617670720614));
#50667=CARTESIAN_POINT('Ctrl Pts',(-4.70260148223132,1.95898934564318,392.538542845154));
#50668=CARTESIAN_POINT('Ctrl Pts',(-3.19894415001964,3.96470128535339,392.459414969695));
#50669=CARTESIAN_POINT('Ctrl Pts',(-0.920716141880372,5.01042730144931,
392.380287094234));
#50670=CARTESIAN_POINT('Ctrl Pts',(1.58044783853879,4.84296237717018,392.301159218775));
#50671=CARTESIAN_POINT('Ctrl Pts',(3.69893288079714,3.50285533534937,392.222031343315));
#50672=CARTESIAN_POINT('Ctrl Pts',(4.92178336136043,1.31459062101607,392.142903467856));
#50673=CARTESIAN_POINT('Ctrl Pts',(4.9529065449796,-1.19198016498848,392.063775592395));
#50674=CARTESIAN_POINT('Ctrl Pts',(3.78476647471314,-3.40993294492945,391.984647716936));
#50675=CARTESIAN_POINT('Ctrl Pts',(1.70020867751367,-4.80222765078197,391.905519841476));
#50676=CARTESIAN_POINT('Ctrl Pts',(-0.796026136476369,-5.03174346991918,
391.826391966016));
#50677=CARTESIAN_POINT('Ctrl Pts',(-3.09951657179924,-4.04290699598317,
391.747264090556));
#50678=CARTESIAN_POINT('Ctrl Pts',(-4.65251105174488,-2.07514839720426,
391.668136215097));
#50679=CARTESIAN_POINT('Ctrl Pts',(-5.07897800851123,0.395072583314779,
391.589008339637));
#50680=CARTESIAN_POINT('Ctrl Pts',(-4.27565562086226,2.76963336360912,391.509880464177));
#50681=CARTESIAN_POINT('Ctrl Pts',(-2.43705493231998,4.47357387486589,391.430752588717));
#50682=CARTESIAN_POINT('Ctrl Pts',(-0.00836226415120685,5.0943134993408,
391.351624713257));
#50683=CARTESIAN_POINT('Ctrl Pts',(2.42235518603692,4.48155054748998,391.272496837798));
#50684=CARTESIAN_POINT('Ctrl Pts',(4.26653995362923,2.78365529135943,391.193368962338));
#50685=CARTESIAN_POINT('Ctrl Pts',(5.0776536262684,0.411744591550536,391.114241086878));
#50686=CARTESIAN_POINT('Ctrl Pts',(4.65929863144093,-2.05986315566845,391.035113211418));
#50687=CARTESIAN_POINT('Ctrl Pts',(3.11277261484635,-4.03270958603397,390.955985335959));
#50688=CARTESIAN_POINT('Ctrl Pts',(0.812540914369942,-5.02910302335342,
390.876857460499));
#50689=CARTESIAN_POINT('Ctrl Pts',(-1.68443394126863,-4.80778350745226,
390.797729585039));
#50690=CARTESIAN_POINT('Ctrl Pts',(-3.7735513679378,-3.42233984732121,390.718601709579));
#50691=CARTESIAN_POINT('Ctrl Pts',(-4.94896661768926,-1.20823398976565,
390.639473834119));
#50692=CARTESIAN_POINT('Ctrl Pts',(-4.92607260087128,1.29842546492777,390.56034595866));
#50693=CARTESIAN_POINT('Ctrl Pts',(-3.71041271969718,3.49069296938833,390.4812180832));
#50694=CARTESIAN_POINT('Ctrl Pts',(-1.59633862636855,4.83774771427692,390.40209020774));
#50695=CARTESIAN_POINT('Ctrl Pts',(0.904262092886961,5.01342298478748,390.32296233228));
#50696=CARTESIAN_POINT('Ctrl Pts',(3.18591091187283,3.97518196044373,390.243834456821));
#50697=CARTESIAN_POINT('Ctrl Pts',(4.69614483496588,1.97441729278565,390.164706581361));
#50698=CARTESIAN_POINT('Ctrl Pts',(5.06928604606176,-0.504419409054961,
390.085578705901));
#50699=CARTESIAN_POINT('Ctrl Pts',(4.21498465890399,-2.86111941069082,390.006450830441));
#50700=CARTESIAN_POINT('Ctrl Pts',(2.34009542676882,-4.52504733131526,389.927322954981));
#50701=CARTESIAN_POINT('Ctrl Pts',(-0.101408666846889,-5.09331093094817,
389.848195079522));
#50702=CARTESIAN_POINT('Ctrl Pts',(-2.51835835252648,-4.42831470937736,
389.769067204062));
#50703=CARTESIAN_POINT('Ctrl Pts',(-4.3255297989291,-2.6910763488991,389.689939328602));
#50704=CARTESIAN_POINT('Ctrl Pts',(-5.08534674866728,-0.302238983003182,
389.610811453142));
#50705=CARTESIAN_POINT('Ctrl Pts',(-4.61383227037253,2.15978048372904,389.531683577683));
#50706=CARTESIAN_POINT('Ctrl Pts',(-3.02515568711978,4.09884532834732,389.452555702223));
#50707=CARTESIAN_POINT('Ctrl Pts',(-0.703988389596766,5.04544351909133,
389.373427826763));
#50708=CARTESIAN_POINT('Ctrl Pts',(1.78763788976615,4.7703721796208,389.294299951303));
#50709=CARTESIAN_POINT('Ctrl Pts',(3.84641763488075,3.34023522152349,389.215172075843));
#50710=CARTESIAN_POINT('Ctrl Pts',(4.97385185858917,1.10131632414888,389.136044200384));
#50711=CARTESIAN_POINT('Ctrl Pts',(4.89695127199855,-1.40426785076764,389.056916324924));
#50712=CARTESIAN_POINT('Ctrl Pts',(3.63433606243988,-3.56983211681959,388.977788449464));
#50713=CARTESIAN_POINT('Ctrl Pts',(1.4917273273879,-4.87102140600428,388.898660574004));
#50714=CARTESIAN_POINT('Ctrl Pts',(-1.0120781619955,-4.99277455439754,388.819532698545));
#50715=CARTESIAN_POINT('Ctrl Pts',(-3.27082589817505,-3.9056110790573,388.740404823085));
#50716=CARTESIAN_POINT('Ctrl Pts',(-4.73759799865136,-1.87276938254615,
388.661276947625));
#50717=CARTESIAN_POINT('Ctrl Pts',(-5.05724019876165,0.613532011436209,
388.582149072166));
#50718=CARTESIAN_POINT('Ctrl Pts',(-4.15235650051922,2.95127691849197,388.503021196705));
#50719=CARTESIAN_POINT('Ctrl Pts',(-2.24204931550549,4.57441961606814,388.423893321246));
#50720=CARTESIAN_POINT('Ctrl Pts',(0.211132509493252,5.0899433219303,388.344765445786));
#50721=CARTESIAN_POINT('Ctrl Pts',(2.613192138255,4.37302261663371,388.265637570326));
#50722=CARTESIAN_POINT('Ctrl Pts',(4.3825111169981,2.59724782537512,388.186509694867));
#50723=CARTESIAN_POINT('Ctrl Pts',(5.09067852854909,0.192593032057139,388.107381819407));
#50724=CARTESIAN_POINT('Ctrl Pts',(4.56622351098889,-2.25869493396522,388.028253943947));
#50725=CARTESIAN_POINT('Ctrl Pts',(2.93613405110136,-4.16307780265885,387.949126068487));
#50726=CARTESIAN_POINT('Ctrl Pts',(0.595108973109503,-5.05944120107668,
387.869998193027));
#50727=CARTESIAN_POINT('Ctrl Pts',(-1.89001176205386,-4.73074576534459,
387.790870317568));
#50728=CARTESIAN_POINT('Ctrl Pts',(-3.91749784672291,-3.2565795826218,387.711742442108));
#50729=CARTESIAN_POINT('Ctrl Pts',(-4.99642752878567,-0.993887270579772,
387.632614566648));
#50730=CARTESIAN_POINT('Ctrl Pts',(-4.86555608063145,1.50945817539208,387.553486691188));
#50731=CARTESIAN_POINT('Ctrl Pts',(-3.55657182856503,3.6473136395552,387.474358815728));
#50732=CARTESIAN_POINT('Ctrl Pts',(-1.38642335604174,4.90203327557553,387.395230940269));
#50733=CARTESIAN_POINT('Ctrl Pts',(1.11942428022107,4.96980776669272,387.316103064809));
#50734=CARTESIAN_POINT('Ctrl Pts',(3.35422210107046,3.83422665653951,387.236975189349));
#50735=CARTESIAN_POINT('Ctrl Pts',(4.77685129433647,1.77025186592861,387.157847313889));
#50736=CARTESIAN_POINT('Ctrl Pts',(5.04284606000954,-0.72235972484213,387.07871943843));
#50737=CARTESIAN_POINT('Ctrl Pts',(4.08780022662232,-3.04006402305186,386.99959156297));
#50738=CARTESIAN_POINT('Ctrl Pts',(2.14296212550442,-4.62166780347541,386.92046368751));
#50739=CARTESIAN_POINT('Ctrl Pts',(-0.320758314346703,-5.08421223601112,
386.84133581205));
#50740=CARTESIAN_POINT('Ctrl Pts',(-2.70681250786736,-4.31569994372646,
386.76220793659));
#50741=CARTESIAN_POINT('Ctrl Pts',(-4.43745744898977,-2.50221328935662,
386.683080061131));
#50742=CARTESIAN_POINT('Ctrl Pts',(-5.09364649014193,-0.082857651985011,
386.603952185671));
#50743=CARTESIAN_POINT('Ctrl Pts',(-4.51649446005934,2.35656057619595,386.524824310211));
#50744=CARTESIAN_POINT('Ctrl Pts',(-2.84574904331825,4.22537718310224,386.445696434751));
#50745=CARTESIAN_POINT('Ctrl Pts',(-0.485953222246148,5.07108956959117,
386.366568559292));
#50746=CARTESIAN_POINT('Ctrl Pts',(1.99150802159427,4.68892266485099,386.287440683832));
#50747=CARTESIAN_POINT('Ctrl Pts',(3.98675899790251,3.17141177548282,386.208312808372));
#50748=CARTESIAN_POINT('Ctrl Pts',(5.01668314543611,0.885996712931309,386.129184932912));
#50749=CARTESIAN_POINT('Ctrl Pts',(4.83190160489097,-1.61394759446514,386.050057057452));
#50750=CARTESIAN_POINT('Ctrl Pts',(3.47715612730962,-3.72310155963289,385.970929181992));
#50751=CARTESIAN_POINT('Ctrl Pts',(1.28047560943712,-4.93076892286227,385.891801306533));
#50752=CARTESIAN_POINT('Ctrl Pts',(-1.22625060220108,-4.94453328612815,
385.812673431073));
#50753=CARTESIAN_POINT('Ctrl Pts',(-3.43606079615961,-3.76106183970999,
385.733545555613));
#50754=CARTESIAN_POINT('Ctrl Pts',(-4.81388649504862,-1.66691234617067,
385.654417680153));
#50755=CARTESIAN_POINT('Ctrl Pts',(-5.02611031361548,0.830852015942555,
385.575289804694));
#50756=CARTESIAN_POINT('Ctrl Pts',(-4.02134581343353,3.12743949674625,385.496161929234));
#50757=CARTESIAN_POINT('Ctrl Pts',(-2.04287986715703,4.66676995419661,385.417034053774));
#50758=CARTESIAN_POINT('Ctrl Pts',(0.430235177489289,5.07612033437727,385.337906178314));
#50759=CARTESIAN_POINT('Ctrl Pts',(2.79917598944896,4.25637330800767,385.258778302855));
#50760=CARTESIAN_POINT('Ctrl Pts',(4.49034328098805,2.40601686941577,385.179650427394));
#50761=CARTESIAN_POINT('Ctrl Pts',(5.09424925529516,-0.0269162024146704,
385.100522551935));
#50762=CARTESIAN_POINT('Ctrl Pts',(4.46466820889472,-2.45333196724627,385.021394676475));
#50763=CARTESIAN_POINT('Ctrl Pts',(2.75404263336906,-4.28571454142868,384.942266801016));
#50764=CARTESIAN_POINT('Ctrl Pts',(0.376571822658881,-5.08038321580243,
384.863138925555));
#50765=CARTESIAN_POINT('Ctrl Pts',(-2.09207953936242,-4.64492229838228,
384.784011050096));
#50766=CARTESIAN_POINT('Ctrl Pts',(-4.05416892752487,-3.08477134713736,
384.704883174636));
#50767=CARTESIAN_POINT('Ctrl Pts',(-5.03460930299721,-0.777694749372607,
384.625755299176));
#50768=CARTESIAN_POINT('Ctrl Pts',(-4.79600347197984,1.71768758911072,384.546627423717));
#50769=CARTESIAN_POINT('Ctrl Pts',(-3.39612583475742,3.79716068550186,384.467499548257));
#50770=CARTESIAN_POINT('Ctrl Pts',(-1.17393328361345,4.9572150046828,384.388371672797));
#50771=CARTESIAN_POINT('Ctrl Pts',(1.33250752393625,4.91696284871881,384.309243797337));
#50772=CARTESIAN_POINT('Ctrl Pts',(3.51630398225976,3.6861506021013,384.230115921877));
#50773=CARTESIAN_POINT('Ctrl Pts',(4.84868640377085,1.56279880820132,384.150988046418));
#50774=CARTESIAN_POINT('Ctrl Pts',(5.00704073069747,-0.938958507157973,
384.071860170958));
#50775=CARTESIAN_POINT('Ctrl Pts',(3.95302411855986,-3.213362767431,383.992732295498));
#50776=CARTESIAN_POINT('Ctrl Pts',(1.94184901290741,-4.70970512538717,383.913604420038));
#50777=CARTESIAN_POINT('Ctrl Pts',(-0.539512264162803,-5.06567137444245,
383.834476544579));
#50778=CARTESIAN_POINT('Ctrl Pts',(-2.89023969471176,-4.19507025735449,
383.755348669118));
#50779=CARTESIAN_POINT('Ctrl Pts',(-4.54114405585455,-2.30870323363671,
383.676220793659));
#50780=CARTESIAN_POINT('Ctrl Pts',(-5.0924865441193,0.136677558478088,383.597092918199));
#50781=CARTESIAN_POINT('Ctrl Pts',(-4.41076882262505,2.54896417204843,383.51796504274));
#50782=CARTESIAN_POINT('Ctrl Pts',(-2.66105740443557,4.34406186043965,383.43883716728));
#50783=CARTESIAN_POINT('Ctrl Pts',(-0.267015564777766,5.08731782427579,
383.35970929182));
#50784=CARTESIAN_POINT('Ctrl Pts',(2.19167961573057,4.59876509717759,383.28058141636));
#50785=CARTESIAN_POINT('Ctrl Pts',(4.11969633429617,2.99669852841663,383.201453540901));
#50786=CARTESIAN_POINT('Ctrl Pts',(5.05019767759256,0.669031669105843,383.12232566544));
#50787=CARTESIAN_POINT('Ctrl Pts',(4.75787835092606,-1.8206299884427,383.043197789981));
#50788=CARTESIAN_POINT('Ctrl Pts',(3.31351857671521,-3.8694566283641,382.964069914521));
#50789=CARTESIAN_POINT('Ctrl Pts',(1.06684585069835,-4.98135924099793,382.884942039061));
#50790=CARTESIAN_POINT('Ctrl Pts',(-1.43814570582419,-4.88710925658996,
382.805814163602));
#50791=CARTESIAN_POINT('Ctrl Pts',(-3.59491439905111,-3.60952772818311,
382.726686288142));
#50792=CARTESIAN_POINT('Ctrl Pts',(-4.8812348614273,-1.45795959635872,382.647558412682));
#50793=CARTESIAN_POINT('Ctrl Pts',(-4.98564616607288,1.04662900005231,382.568430537222));
#50794=CARTESIAN_POINT('Ctrl Pts',(-3.88286686666645,3.29779393728166,382.489302661762));
#50795=CARTESIAN_POINT('Ctrl Pts',(-1.83991647567274,4.75045338042336,382.410174786303));
#50796=CARTESIAN_POINT('Ctrl Pts',(0.648538832374088,5.05287020810257,382.331046910843));
#50797=CARTESIAN_POINT('Ctrl Pts',(2.97996133890915,4.13181925737738,382.251919035383));
#50798=CARTESIAN_POINT('Ctrl Pts',(4.58983618463159,2.21031756887428,382.172791159923));
#50799=CARTESIAN_POINT('Ctrl Pts',(5.08835917511605,-0.246375449345246,
382.093663284464));
#50800=CARTESIAN_POINT('Ctrl Pts',(4.35482132902486,-2.64341278450753,382.014535409004));
#50801=CARTESIAN_POINT('Ctrl Pts',(2.56683653350947,-4.40039204699635,381.935407533544));
#50802=CARTESIAN_POINT('Ctrl Pts',(0.157335320227334,-5.09189017497793,
381.856279658084));
#50803=CARTESIAN_POINT('Ctrl Pts',(-2.29026200215225,-4.55047249398623,
381.777151782624));
#50804=CARTESIAN_POINT('Ctrl Pts',(-4.1833107910579,-2.90723421527166,381.698023907165));
#50805=CARTESIAN_POINT('Ctrl Pts',(-5.06344103087761,-0.560057929015174,
381.618896031705));
#50806=CARTESIAN_POINT('Ctrl Pts',(-4.71754394484289,1.92272699193202,381.539768156245));
#50807=CARTESIAN_POINT('Ctrl Pts',(-3.22937271124211,3.9399558181422,381.460640280785));
#50808=CARTESIAN_POINT('Ctrl Pts',(-0.959263035935946,5.0031904206131,381.381512405325));
#50809=CARTESIAN_POINT('Ctrl Pts',(1.54311609556955,4.85498637203256,381.302384529866));
#50810=CARTESIAN_POINT('Ctrl Pts',(3.67185554437766,3.53122879721078,381.223256654406));
#50811=CARTESIAN_POINT('Ctrl Pts',(4.91151675438643,1.35244339194259,381.144128778947));
#50812=CARTESIAN_POINT('Ctrl Pts',(4.96193655414693,-1.15381349864191,381.065000903486));
#50813=CARTESIAN_POINT('Ctrl Pts',(3.81090663474561,-3.38069380131942,380.985873028027));
#50814=CARTESIAN_POINT('Ctrl Pts',(1.73712958706021,-4.78899579815935,380.906745152567));
#50815=CARTESIAN_POINT('Ctrl Pts',(-0.757264256456047,-5.03772277948299,
380.827617277107));
#50816=CARTESIAN_POINT('Ctrl Pts',(-3.06829926047039,-4.0666496782025,380.748489401647));
#50817=CARTESIAN_POINT('Ctrl Pts',(-4.63639705749532,-2.11090555977201,
380.669361526187));
#50818=CARTESIAN_POINT('Ctrl Pts',(-5.08186906479814,0.355958937625331,
380.590233650728));
#50819=CARTESIAN_POINT('Ctrl Pts',(-4.29685170689215,2.73663394812055,380.511105775268));
#50820=CARTESIAN_POINT('Ctrl Pts',(-2.47142377134362,4.45467894460033,380.431977899808));
#50821=CARTESIAN_POINT('Ctrl Pts',(-0.0475820182042561,5.09409814477217,
380.352850024348));
#50822=CARTESIAN_POINT('Ctrl Pts',(2.38778092263769,4.50006691311533,380.273722148889));
#50823=CARTESIAN_POINT('Ctrl Pts',(4.24498275891546,2.81641994978345,380.194594273428));
#50824=CARTESIAN_POINT('Ctrl Pts',(5.07433321340091,0.450824130237162,380.115466397969));
#50825=CARTESIAN_POINT('Ctrl Pts',(4.67501898270842,-2.02393119160303,380.036338522509));
#50826=CARTESIAN_POINT('Ctrl Pts',(3.14372731083789,-4.00862551906755,379.957210647049));
#50827=CARTESIAN_POINT('Ctrl Pts',(0.851234794597309,-5.02269840638422,
379.87808277159));
#50828=CARTESIAN_POINT('Ctrl Pts',(-1.64736995096127,-4.82060911106652,
379.79895489613));
#50829=CARTESIAN_POINT('Ctrl Pts',(-3.74709169119734,-3.45129016670399,
379.71982702067));
#50830=CARTESIAN_POINT('Ctrl Pts',(-4.93951802147898,-1.2462991906088,379.64069914521));
#50831=CARTESIAN_POINT('Ctrl Pts',(-4.93592290429957,1.26046223261093,379.56157126975));
#50832=CARTESIAN_POINT('Ctrl Pts',(-3.73717683698987,3.46202386561592,379.482443394291));
#50833=CARTESIAN_POINT('Ctrl Pts',(-1.63353607538846,4.82531448171332,379.403315518831));
#50834=CARTESIAN_POINT('Ctrl Pts',(0.865638050575662,5.02023612217824,379.324187643371));
#50835=CARTESIAN_POINT('Ctrl Pts',(3.15521244034589,3.99959178083392,379.245059767911));
#50836=CARTESIAN_POINT('Ctrl Pts',(4.6808050542546,2.01051336754875,379.165931892452));
#50837=CARTESIAN_POINT('Ctrl Pts',(5.07301922679952,-0.465377139049836,
379.086804016992));
#50838=CARTESIAN_POINT('Ctrl Pts',(4.23688687398491,-2.82858437634132,379.007676141532));
#50839=CARTESIAN_POINT('Ctrl Pts',(2.37486342213654,-4.5068973455389,378.928548266072));
#50840=CARTESIAN_POINT('Ctrl Pts',(-0.0621933781710937,-5.0939407084044,
378.849420390613));
#50841=CARTESIAN_POINT('Ctrl Pts',(-2.48419109500962,-4.44757176001722,
378.770292515152));
#50842=CARTESIAN_POINT('Ctrl Pts',(-4.30468360095437,-2.72429790087321,
378.691164639693));
#50843=CARTESIAN_POINT('Ctrl Pts',(-5.08286916745938,-0.341380994664952,
378.612036764233));
#50844=CARTESIAN_POINT('Ctrl Pts',(-4.63032321066906,2.12419559404662,378.532908888774));
#50845=CARTESIAN_POINT('Ctrl Pts',(-3.05662214430013,4.07543384488105,378.453781013314));
#50846=CARTESIAN_POINT('Ctrl Pts',(-0.742811288783636,5.03987413992486,
378.374653137854));
#50847=CARTESIAN_POINT('Ctrl Pts',(1.75085886250587,4.78399343651434,378.295525262394));
#50848=CARTESIAN_POINT('Ctrl Pts',(3.82058790417125,3.36974895556452,378.216397386935));
#50849=CARTESIAN_POINT('Ctrl Pts',(4.9652256605272,1.13957627961887,378.137269511474));
#50850=CARTESIAN_POINT('Ctrl Pts',(4.90761729577347,-1.36652568042196,378.058141636015));
#50851=CARTESIAN_POINT('Ctrl Pts',(3.66171170927622,-3.54174636516749,377.979013760555));
#50852=CARTESIAN_POINT('Ctrl Pts',(1.52918404352555,-4.85939256677772,377.899885885095));
#50853=CARTESIAN_POINT('Ctrl Pts',(-0.973609892176757,-5.00041835598616,
377.820758009635));
#50854=CARTESIAN_POINT('Ctrl Pts',(-3.24066052105438,-3.93067670310182,
377.741630134176));
#50855=CARTESIAN_POINT('Ctrl Pts',(-4.72303955439021,-1.90918760856372,
377.662502258716));
#50856=CARTESIAN_POINT('Ctrl Pts',(-5.06181377047586,0.574579246099912,
377.583374383256));
#50857=CARTESIAN_POINT('Ctrl Pts',(-4.17495467452228,2.91922137268011,377.504246507796));
#50858=CARTESIAN_POINT('Ctrl Pts',(-2.27720032296007,4.55702300259043,377.425118632336));
#50859=CARTESIAN_POINT('Ctrl Pts',(0.171939895519064,5.09141793897891,377.345990756877));
#50860=CARTESIAN_POINT('Ctrl Pts',(2.5794477519296,4.39301141042152,377.266862881417));
#50861=CARTESIAN_POINT('Ctrl Pts',(4.36238559553759,2.63091084472138,377.187735005957));
#50862=CARTESIAN_POINT('Ctrl Pts',(5.08904492944719,0.231779341395482,377.108607130498));
#50863=CARTESIAN_POINT('Ctrl Pts',(4.58347738286989,-2.22347364224237,377.029479255037));
#50864=CARTESIAN_POINT('Ctrl Pts',(2.96809765825856,-4.14034977363789,376.950351379578));
#50865=CARTESIAN_POINT('Ctrl Pts',(0.634042864132613,-5.0547096458148,376.871223504118));
#50866=CARTESIAN_POINT('Ctrl Pts',(-1.85353477590152,-4.7451563505839,376.792095628658));
#50867=CARTESIAN_POINT('Ctrl Pts',(-3.89231005589385,-3.28664302685179,
376.712967753199));
#50868=CARTESIAN_POINT('Ctrl Pts',(-4.98862773436458,-1.03232421493045,
376.633839877739));
#50869=CARTESIAN_POINT('Ctrl Pts',(-4.87703287210239,1.47195459226046,376.554712002279));
#50870=CARTESIAN_POINT('Ctrl Pts',(-3.58454629319045,3.61982428153675,376.475584126819));
#50871=CARTESIAN_POINT('Ctrl Pts',(-1.42412194671949,4.89121422922617,376.39645625136));
#50872=CARTESIAN_POINT('Ctrl Pts',(1.08112964569973,4.97827868361118,376.3173283759));
#50873=CARTESIAN_POINT('Ctrl Pts',(3.32460382467506,3.85993644420179,376.23820050044));
#50874=CARTESIAN_POINT('Ctrl Pts',(4.76308094821025,1.80697533479263,376.15907262498));
#50875=CARTESIAN_POINT('Ctrl Pts',(5.04825789565173,-0.683514556087066,
376.07994474952));
#50876=CARTESIAN_POINT('Ctrl Pts',(4.11108387333318,-3.00850284103068,376.000816874061));
#50877=CARTESIAN_POINT('Ctrl Pts',(2.1784798079633,-4.60503266038196,375.921688998601));
#50878=CARTESIAN_POINT('Ctrl Pts',(-0.281606542178375,-5.08653096539461,
375.842561123141));
#50879=CARTESIAN_POINT('Ctrl Pts',(-2.67350672874489,-4.33641128901115,
375.763433247681));
#50880=CARTESIAN_POINT('Ctrl Pts',(-4.41806180727835,-2.5363019544723,375.684305372222));
#50881=CARTESIAN_POINT('Ctrl Pts',(-5.09285793196053,-0.12207046608611,
375.605177496761));
#50882=CARTESIAN_POINT('Ctrl Pts',(-4.53450261646048,2.32172008989041,375.526049621302));
#50883=CARTESIAN_POINT('Ctrl Pts',(-2.8781963029061,4.20334135813296,375.446921745842));
#50884=CARTESIAN_POINT('Ctrl Pts',(-0.524977181972811,5.06720185538771,
375.367793870382));
#50885=CARTESIAN_POINT('Ctrl Pts',(1.95534399133764,4.70410782389334,375.288665994923));
#50886=CARTESIAN_POINT('Ctrl Pts',(3.96223755849503,3.20202817970643,375.209538119463));
#50887=CARTESIAN_POINT('Ctrl Pts',(5.00968625615773,0.924557438714191,375.130410244003));
#50888=CARTESIAN_POINT('Ctrl Pts',(4.84423973083701,-1.5766172667089,375.051282368543));
#50889=CARTESIAN_POINT('Ctrl Pts',(3.50558626093324,-3.69634481139898,374.972154493084));
#50890=CARTESIAN_POINT('Ctrl Pts',(2.04760230627713,-4.51212292509998,374.91940257611));
#50891=CARTESIAN_POINT('Ctrl Pts',(1.26508527942809,-4.72177922709072,374.893026617624));
#50892=CARTESIAN_POINT('Ctrl Pts',(3.8562705385027,3.2970584607914,400.320920147129));
#50893=CARTESIAN_POINT('Ctrl Pts',(4.40267566673985,2.65797789150057,400.294544188642));
#50894=CARTESIAN_POINT('Ctrl Pts',(5.17098558200965,1.10346405572081,400.241792271669));
#50895=CARTESIAN_POINT('Ctrl Pts',(5.07118954877308,-1.49668420940778,400.162664396209));
#50896=CARTESIAN_POINT('Ctrl Pts',(3.74345010496737,-3.73402503008569,400.08353652075));
#50897=CARTESIAN_POINT('Ctrl Pts',(1.50930126812034,-5.0674413388845,400.00440864529));
#50898=CARTESIAN_POINT('Ctrl Pts',(-1.09030376370591,-5.17376607298461,
399.925280769831));
#50899=CARTESIAN_POINT('Ctrl Pts',(-3.42590833126468,-4.02739560525483,
399.84615289437));
#50900=CARTESIAN_POINT('Ctrl Pts',(-4.93198749421962,-1.90583738162352,
399.767025018911));
#50901=CARTESIAN_POINT('Ctrl Pts',(-5.24386820862784,0.677177256470671,
399.68789714345));
#50902=CARTESIAN_POINT('Ctrl Pts',(-4.28603436807985,3.09622957226831,399.608769267991));
#50903=CARTESIAN_POINT('Ctrl Pts',(-2.29040909926245,4.7655795591539,399.529641392531));
#50904=CARTESIAN_POINT('Ctrl Pts',(0.259800278618912,5.28102545063066,399.450513517072));
#50905=CARTESIAN_POINT('Ctrl Pts',(2.7471033957984,4.51775909222651,399.371385641611));
#50906=CARTESIAN_POINT('Ctrl Pts',(4.56924148852249,2.66059337678593,399.292257766152));
#50907=CARTESIAN_POINT('Ctrl Pts',(5.2850143906551,0.159209483399153,399.213129890692));
#50908=CARTESIAN_POINT('Ctrl Pts',(4.7211096918349,-2.38072426286758,399.134002015232));
#50909=CARTESIAN_POINT('Ctrl Pts',(3.01406746059458,-4.34420558161996,399.054874139772));
#50910=CARTESIAN_POINT('Ctrl Pts',(0.577219342712345,-5.25581036421826,
398.975746264313));
#50911=CARTESIAN_POINT('Ctrl Pts',(-1.99939275815206,-4.89480881878609,
398.896618388853));
#50912=CARTESIAN_POINT('Ctrl Pts',(-4.09188543486623,-3.34861140683646,
398.817490513394));
#50913=CARTESIAN_POINT('Ctrl Pts',(-5.19359667913832,-0.991603904073038,
398.738362637933));
#50914=CARTESIAN_POINT('Ctrl Pts',(-5.03776559021372,1.60550385431017,398.659234762474));
#50915=CARTESIAN_POINT('Ctrl Pts',(-3.66212405277363,3.81386578025083,398.580106887014));
#50916=CARTESIAN_POINT('Ctrl Pts',(-1.39976059402284,5.09876407058445,398.500979011554));
#50917=CARTESIAN_POINT('Ctrl Pts',(1.2015314169661,5.14908215334412,398.421851136094));
#50918=CARTESIAN_POINT('Ctrl Pts',(3.51189274640949,3.9526363487746,398.342723260634));
#50919=CARTESIAN_POINT('Ctrl Pts',(4.97190814582059,1.79912594262636,398.263595385175));
#50920=CARTESIAN_POINT('Ctrl Pts',(5.22805937238099,-0.790012637095727,
398.184467509715));
#50921=CARTESIAN_POINT('Ctrl Pts',(4.21832370253235,-3.18786290617544,398.105339634255));
#50922=CARTESIAN_POINT('Ctrl Pts',(2.18719169429123,-4.81382563667766,398.026211758795));
#50923=CARTESIAN_POINT('Ctrl Pts',(-0.37353210098369,-5.27420122269227,
397.947083883336));
#50924=CARTESIAN_POINT('Ctrl Pts',(-2.84381136257153,-4.45751743709679,
397.867956007876));
#50925=CARTESIAN_POINT('Ctrl Pts',(-4.62550939672404,-2.56152056184034,
397.788828132416));
#50926=CARTESIAN_POINT('Ctrl Pts',(-5.2872179056115,-0.0452944422017613,
397.709700256956));
#50927=CARTESIAN_POINT('Ctrl Pts',(-4.66871527142514,2.48189896697567,397.630572381496));
#50928=CARTESIAN_POINT('Ctrl Pts',(-2.91976153402742,4.40814216562114,397.551444506037));
#50929=CARTESIAN_POINT('Ctrl Pts',(-0.463836508948714,5.26702766851281,
397.472316630577));
#50930=CARTESIAN_POINT('Ctrl Pts',(2.10439874769627,4.85059075563045,397.393188755117));
#50931=CARTESIAN_POINT('Ctrl Pts',(4.16308914079174,3.25966464129901,397.314060879657));
#50932=CARTESIAN_POINT('Ctrl Pts',(5.21375731827273,0.87946540242969,397.234933004198));
#50933=CARTESIAN_POINT('Ctrl Pts',(5.00200160188481,-1.71368163398425,397.155805128738));
#50934=CARTESIAN_POINT('Ctrl Pts',(3.57909508696266,-3.89188940315535,397.076677253278));
#50935=CARTESIAN_POINT('Ctrl Pts',(1.28957072230382,-5.12774142484681,396.997549377819));
#50936=CARTESIAN_POINT('Ctrl Pts',(-1.31220156516579,-5.12199685867627,
396.918421502358));
#50937=CARTESIAN_POINT('Ctrl Pts',(-3.59624625077107,-3.87604665499891,
396.839293626899));
#50938=CARTESIAN_POINT('Ctrl Pts',(-5.00952021996834,-1.69157675960673,
396.760165751439));
#50939=CARTESIAN_POINT('Ctrl Pts',(-5.20982288335836,0.90248007842212,396.681037875979));
#50940=CARTESIAN_POINT('Ctrl Pts',(-4.14865431030898,3.27801650109757,396.601910000519));
#50941=CARTESIAN_POINT('Ctrl Pts',(-2.08295867375766,4.85983620416686,396.52278212506));
#50942=CARTESIAN_POINT('Ctrl Pts',(0.487090472013812,5.26492807548086,396.4436542496));
#50943=CARTESIAN_POINT('Ctrl Pts',(2.93919882905869,4.3952059122609,396.36452637414));
#50944=CARTESIAN_POINT('Ctrl Pts',(4.67962948341671,2.46125835008237,396.28539849868));
#50945=CARTESIAN_POINT('Ctrl Pts',(5.2869663411736,-0.0686416434144708,
396.206270623221));
#50946=CARTESIAN_POINT('Ctrl Pts',(4.61415296796628,-2.58192121415839,396.127142747761));
#50947=CARTESIAN_POINT('Ctrl Pts',(2.82409983825713,-4.47003186470401,396.048014872301));
#50948=CARTESIAN_POINT('Ctrl Pts',(0.350238296140284,-5.27579926682488,
395.968886996841));
#50949=CARTESIAN_POINT('Ctrl Pts',(-2.20842757548492,-4.80412035775031,
395.889759121382));
#50950=CARTESIAN_POINT('Ctrl Pts',(-4.23235974759556,-3.16920427471092,
395.810631245921));
#50951=CARTESIAN_POINT('Ctrl Pts',(-5.23149698840249,-0.766918527777797,
395.731503370462));
#50952=CARTESIAN_POINT('Ctrl Pts',(-4.96391497173342,1.82106367854447,395.652375495002));
#50953=CARTESIAN_POINT('Ctrl Pts',(-3.49440419526435,3.96810585645496,395.573247619542));
#50954=CARTESIAN_POINT('Ctrl Pts',(-1.17878204811896,5.1543377509575,395.494119744082));
#50955=CARTESIAN_POINT('Ctrl Pts',(1.42226240243777,5.09253320328156,395.414991868623));
#50956=CARTESIAN_POINT('Ctrl Pts',(3.67892986523249,3.79765714811298,395.335863993163));
#50957=CARTESIAN_POINT('Ctrl Pts',(5.0448061610774,1.58324210563915,395.256736117703));
#50958=CARTESIAN_POINT('Ctrl Pts',(5.18916725226161,-1.01452845991075,395.177608242243));
#50959=CARTESIAN_POINT('Ctrl Pts',(4.07705852165763,-3.36664797371096,395.098480366784));
#50960=CARTESIAN_POINT('Ctrl Pts',(1.97775844702931,-4.90359014326416,395.019352491324));
#50961=CARTESIAN_POINT('Ctrl Pts',(-0.60042266624658,-5.25321019851391,
394.940224615864));
#50962=CARTESIAN_POINT('Ctrl Pts',(-3.03322150067462,-4.33085350661488,
394.861096740404));
#50963=CARTESIAN_POINT('Ctrl Pts',(-4.73157661935314,-2.35985327152006,
394.781968864945));
#50964=CARTESIAN_POINT('Ctrl Pts',(-5.28425981367717,0.182545855799866,
394.702840989484));
#50965=CARTESIAN_POINT('Ctrl Pts',(-4.55744811727866,2.68074456564335,394.623713114025));
#50966=CARTESIAN_POINT('Ctrl Pts',(-2.72712679296628,4.52984593810856,394.544585238565));
#50967=CARTESIAN_POINT('Ctrl Pts',(-0.236477452813074,5.28212108742541,
394.465457363106));
#50968=CARTESIAN_POINT('Ctrl Pts',(2.31143093653793,4.75541920271268,394.386329487645));
#50969=CARTESIAN_POINT('Ctrl Pts',(4.29966508998112,3.07727231195273,394.307201612186));
#50970=CARTESIAN_POINT('Ctrl Pts',(5.2468074522505,0.654015540275394,394.228073736726));
#50971=CARTESIAN_POINT('Ctrl Pts',(4.92352338499734,-1.92760012588128,394.148945861266));
#50972=CARTESIAN_POINT('Ctrl Pts',(3.40809070325859,-4.04247974964323,394.069817985806));
#50973=CARTESIAN_POINT('Ctrl Pts',(1.06744601535546,-5.17854069909805,393.990690110347));
#50974=CARTESIAN_POINT('Ctrl Pts',(-1.53166282285958,-5.06070486839363,
393.911562234887));
#50975=CARTESIAN_POINT('Ctrl Pts',(-3.75990519627929,-3.71750422769163,
393.832434359427));
#50976=CARTESIAN_POINT('Ctrl Pts',(-5.07774958438631,-1.47417228510708,
393.753306483967));
#50977=CARTESIAN_POINT('Ctrl Pts',(-5.16610207037776,1.12610575273896,393.674178608508));
#50978=CARTESIAN_POINT('Ctrl Pts',(-4.00356958154437,3.45371616865744,393.595050733048));
#50979=CARTESIAN_POINT('Ctrl Pts',(-1.8716398630404,4.94506713715712,393.515922857588));
#50980=CARTESIAN_POINT('Ctrl Pts',(0.713476058729831,5.23905303289941,393.436794982128));
#50981=CARTESIAN_POINT('Ctrl Pts',(3.12583571869877,4.26449010171441,393.357667106669));
#50982=CARTESIAN_POINT('Ctrl Pts',(4.78132668327137,2.25735241283907,393.278539231209));
#50983=CARTESIAN_POINT('Ctrl Pts',(5.2790995798779,-0.296365304389928,393.199411355749));
#50984=CARTESIAN_POINT('Ctrl Pts',(4.49862704983328,-2.77832313355043,393.120283480289));
#50985=CARTESIAN_POINT('Ctrl Pts',(2.62888742685924,-4.58755661161959,393.041155604829));
#50986=CARTESIAN_POINT('Ctrl Pts',(0.122606802959192,-5.28599019482455,
392.96202772937));
#50987=CARTESIAN_POINT('Ctrl Pts',(-2.41336100201929,-4.70450990453263,
392.88289985391));
#50988=CARTESIAN_POINT('Ctrl Pts',(-4.3649739152189,-2.98391144093985,392.80377197845));
#50989=CARTESIAN_POINT('Ctrl Pts',(-5.25968160051806,-0.540808865575483,
392.724644102991));
#50990=CARTESIAN_POINT('Ctrl Pts',(-4.88084559720602,2.03324150659673,392.64551622753));
#50991=CARTESIAN_POINT('Ctrl Pts',(-3.32019468996614,4.11497654776232,392.566388352071));
#50992=CARTESIAN_POINT('Ctrl Pts',(-0.955614322062658,5.20033903081154,
392.487260476611));
#50993=CARTESIAN_POINT('Ctrl Pts',(1.64035202716895,5.02652663326038,392.408132601151));
#50994=CARTESIAN_POINT('Ctrl Pts',(3.83913464362559,3.63562511214056,392.329004725691));
#50995=CARTESIAN_POINT('Ctrl Pts',(5.10833519286426,1.36441794376124,392.249876850232));
#50996=CARTESIAN_POINT('Ctrl Pts',(5.14063804785052,-1.23716014683014,392.170748974772));
#50997=CARTESIAN_POINT('Ctrl Pts',(3.92822161400576,-3.53918065647562,392.091621099312));
#50998=CARTESIAN_POINT('Ctrl Pts',(1.76465219715718,-4.98424792631562,392.012493223852));
#50999=CARTESIAN_POINT('Ctrl Pts',(-0.826198153971171,-5.22246315241074,
391.933365348392));
#51000=CARTESIAN_POINT('Ctrl Pts',(-3.21699847841567,-4.19614651290735,
391.854237472933));
#51001=CARTESIAN_POINT('Ctrl Pts',(-4.82885657410346,-2.15380336954211,
391.775109597473));
#51002=CARTESIAN_POINT('Ctrl Pts',(-5.27148803589155,0.41004713797985,391.695981722013));
#51003=CARTESIAN_POINT('Ctrl Pts',(-4.43771707875037,2.8746116080056,391.616853846554));
#51004=CARTESIAN_POINT('Ctrl Pts',(-2.52942735664669,4.64313708771996,391.537725971094));
#51005=CARTESIAN_POINT('Ctrl Pts',(-0.00867922155838994,5.28740479243137,
391.458598095634));
#51006=CARTESIAN_POINT('Ctrl Pts',(2.51417044146968,4.65141610255989,391.379470220174));
#51007=CARTESIAN_POINT('Ctrl Pts',(4.42825589764708,2.88916501309064,391.300342344714));
#51008=CARTESIAN_POINT('Ctrl Pts',(5.27011345519119,0.427351070346123,391.221214469255));
#51009=CARTESIAN_POINT('Ctrl Pts',(4.8359014254693,-2.1379387669101,391.142086593795));
#51010=CARTESIAN_POINT('Ctrl Pts',(3.23075696923981,-4.18556258746916,391.062958718335));
#51011=CARTESIAN_POINT('Ctrl Pts',(0.843338896446427,-5.21972262420654,
390.983830842875));
#51012=CARTESIAN_POINT('Ctrl Pts',(-1.7482795463511,-4.99001436828829,390.904702967415));
#51013=CARTESIAN_POINT('Ctrl Pts',(-3.91658141767327,-3.55205782141137,
390.825575091956));
#51014=CARTESIAN_POINT('Ctrl Pts',(-5.13654878431394,-1.25403004520473,
390.746447216496));
#51015=CARTESIAN_POINT('Ctrl Pts',(-5.11278700870727,1.34764007491144,390.667319341036));
#51016=CARTESIAN_POINT('Ctrl Pts',(-3.85104960630393,3.62300175237324,390.588191465576));
#51017=CARTESIAN_POINT('Ctrl Pts',(-1.65684512829777,5.02111431743484,390.509063590116));
#51018=CARTESIAN_POINT('Ctrl Pts',(0.938536610313288,5.20344826043412,390.429935714657));
#51019=CARTESIAN_POINT('Ctrl Pts',(3.30666744908329,4.12585447502528,390.350807839197));
#51020=CARTESIAN_POINT('Ctrl Pts',(4.874144221702,2.04925422384882,390.271679963737));
#51021=CARTESIAN_POINT('Ctrl Pts',(5.26142871608132,-0.523538569265068,
390.192552088277));
#51022=CARTESIAN_POINT('Ctrl Pts',(4.37474648711696,-2.96956527817979,390.113424212818));
#51023=CARTESIAN_POINT('Ctrl Pts',(2.42879276586438,-4.69656155803349,390.034296337358));
#51024=CARTESIAN_POINT('Ctrl Pts',(-0.105252389973582,-5.28636422338813,
389.955168461898));
#51025=CARTESIAN_POINT('Ctrl Pts',(-2.61381244478399,-4.59616245050211,
389.876040586438));
#51026=CARTESIAN_POINT('Ctrl Pts',(-4.48948165275299,-2.79307702319636,
389.796912710979));
#51027=CARTESIAN_POINT('Ctrl Pts',(-5.27809817231664,-0.313694837861352,
389.717784835519));
#51028=CARTESIAN_POINT('Ctrl Pts',(-4.78871173927535,2.2416432914359,389.638656960059));
#51029=CARTESIAN_POINT('Ctrl Pts',(-3.13981907081257,4.25420509266713,389.559529084599));
#51030=CARTESIAN_POINT('Ctrl Pts',(-0.730671872756092,5.23668247865729,
389.48040120914));
#51031=CARTESIAN_POINT('Ctrl Pts',(1.85539526507438,4.95118502767294,389.401273333679));
#51032=CARTESIAN_POINT('Ctrl Pts',(3.99220955659535,3.46684115934693,389.32214545822));
#51033=CARTESIAN_POINT('Ctrl Pts',(5.16237725796638,1.14305984722794,389.24301758276));
#51034=CARTESIAN_POINT('Ctrl Pts',(5.08256188536855,-1.45749423645932,389.1638897073));
#51035=CARTESIAN_POINT('Ctrl Pts',(3.77208939268016,-3.70514053465492,389.08476183184));
#51036=CARTESIAN_POINT('Ctrl Pts',(1.54826871586373,-5.05564919188336,389.005633956381));
#51037=CARTESIAN_POINT('Ctrl Pts',(-1.05043926423896,-5.18201718639165,
388.926506080921));
#51038=CARTESIAN_POINT('Ctrl Pts',(-3.39480099358967,-4.05364662764723,
388.847378205461));
#51039=CARTESIAN_POINT('Ctrl Pts',(-4.91716859708847,-1.94375352236854,
388.768250330001));
#51040=CARTESIAN_POINT('Ctrl Pts',(-5.2489262914167,0.636786899353102,388.689122454542));
#51041=CARTESIAN_POINT('Ctrl Pts',(-4.30974451485365,3.06314005305047,388.609994579082));
#51042=CARTESIAN_POINT('Ctrl Pts',(-2.32703038342756,4.74780521530929,388.530866703622));
#51043=CARTESIAN_POINT('Ctrl Pts',(0.2191351283499,5.28286897087523,388.451738828163));
#51044=CARTESIAN_POINT('Ctrl Pts',(2.71224074394742,4.53877460497707,388.372610952702));
#51045=CARTESIAN_POINT('Ctrl Pts',(4.54862275081774,2.69569208899244,388.293483077243));
#51046=CARTESIAN_POINT('Ctrl Pts',(5.28363204425109,0.199892943537846,388.214355201783));
#51047=CARTESIAN_POINT('Ctrl Pts',(4.73929845080001,-2.34430692575821,388.135227326323));
#51048=CARTESIAN_POINT('Ctrl Pts',(3.04742322101362,-4.32087218972514,388.056099450863));
#51049=CARTESIAN_POINT('Ctrl Pts',(0.617665567076949,-5.25121071898288,
387.976971575404));
#51050=CARTESIAN_POINT('Ctrl Pts',(-1.96164944496022,-4.9100566415267,387.897843699944));
#51051=CARTESIAN_POINT('Ctrl Pts',(-4.06598394303424,-3.38001469566346,
387.818715824484));
#51052=CARTESIAN_POINT('Ctrl Pts',(-5.18580862056406,-1.03155887800781,
387.739587949024));
#51053=CARTESIAN_POINT('Ctrl Pts',(-5.04997671264308,1.56667162151986,387.660460073564));
#51054=CARTESIAN_POINT('Ctrl Pts',(-3.69137763771595,3.78555886279474,387.581332198105));
#51055=CARTESIAN_POINT('Ctrl Pts',(-1.43897337649567,5.08783651365194,387.502204322645));
#51056=CARTESIAN_POINT('Ctrl Pts',(1.16185415459233,5.15817988164137,387.423076447186));
#51057=CARTESIAN_POINT('Ctrl Pts',(3.48135818778607,3.97955649994419,387.343948571725));
#51058=CARTESIAN_POINT('Ctrl Pts',(4.95790972221771,1.83735025355874,387.264820696266));
#51059=CARTESIAN_POINT('Ctrl Pts',(5.23398656730458,-0.749739542233496,
387.185692820806));
#51060=CARTESIAN_POINT('Ctrl Pts',(4.24274134513742,-3.15529248187465,387.106564945346));
#51061=CARTESIAN_POINT('Ctrl Pts',(2.22418746193322,-4.79684426494046,387.027437069886));
#51062=CARTESIAN_POINT('Ctrl Pts',(-0.332916112977428,-5.27692065788687,
386.948309194427));
#51063=CARTESIAN_POINT('Ctrl Pts',(-2.80940963451955,-4.47927921359921,
386.869181318967));
#51064=CARTESIAN_POINT('Ctrl Pts',(-4.6056517301173,-2.59705543044056,386.790053443507));
#51065=CARTESIAN_POINT('Ctrl Pts',(-5.2867125013827,-0.0859982304292488,
386.710925568047));
#51066=CARTESIAN_POINT('Ctrl Pts',(-4.68768450473212,2.44588199879054,386.631797692588));
#51067=CARTESIAN_POINT('Ctrl Pts',(-2.95361232316089,4.38553292227813,386.552669817127));
#51068=CARTESIAN_POINT('Ctrl Pts',(-0.504372453036948,5.26330059910421,
386.473541941668));
#51069=CARTESIAN_POINT('Ctrl Pts',(2.06699274767947,4.86664830750627,386.394414066208));
#51070=CARTESIAN_POINT('Ctrl Pts',(4.1378703204085,3.29161874757629,386.315286190749));
#51071=CARTESIAN_POINT('Ctrl Pts',(5.20683199193,0.919578912180737,386.236158315288));
#51072=CARTESIAN_POINT('Ctrl Pts',(5.01504662121074,-1.67512153439562,386.157030439829));
#51073=CARTESIAN_POINT('Ctrl Pts',(3.60895181930755,-3.86421939514695,386.077902564369));
#51074=CARTESIAN_POINT('Ctrl Pts',(1.32900986066236,-5.11766133679979,385.998774688909));
#51075=CARTESIAN_POINT('Ctrl Pts',(-1.2727295467071,-5.13194741485647,385.91964681345));
#51076=CARTESIAN_POINT('Ctrl Pts',(-3.5662988394905,-3.90361849510962,385.84051893799));
#51077=CARTESIAN_POINT('Ctrl Pts',(-4.99634867925468,-1.73009382497687,
385.76139106253));
#51078=CARTESIAN_POINT('Ctrl Pts',(-5.21661648089346,0.862344049196109,
385.68226318707));
#51079=CARTESIAN_POINT('Ctrl Pts',(-4.1737680903862,3.24597977436508,385.60313531161));
#51080=CARTESIAN_POINT('Ctrl Pts',(-2.12031175571847,4.84365593601313,385.524007436151));
#51081=CARTESIAN_POINT('Ctrl Pts',(0.446542510511727,5.26852204647746,385.44487956069));
#51082=CARTESIAN_POINT('Ctrl Pts',(2.90527399685678,4.41770390260608,385.365751685231));
#51083=CARTESIAN_POINT('Ctrl Pts',(4.66054210967394,2.4972128487314,385.286623809771));
#51084=CARTESIAN_POINT('Ctrl Pts',(5.2873381133244,-0.0279364153108744,
385.207495934311));
#51085=CARTESIAN_POINT('Ctrl Pts',(4.63389386761938,-2.54632134491165,385.128368058852));
#51086=CARTESIAN_POINT('Ctrl Pts',(2.85842993763932,-4.44815726560116,385.049240183392));
#51087=CARTESIAN_POINT('Ctrl Pts',(0.390845137441743,-5.27294650517633,
384.970112307932));
#51088=CARTESIAN_POINT('Ctrl Pts',(-2.1713762578616,-4.82098018194518,384.890984432472));
#51089=CARTESIAN_POINT('Ctrl Pts',(-4.20783530881936,-3.2016943610792,384.811856557012));
#51090=CARTESIAN_POINT('Ctrl Pts',(-5.2254376100198,-0.807171946801767,
384.732728681553));
#51091=CARTESIAN_POINT('Ctrl Pts',(-4.97778783059681,1.78279361718495,384.653600806093));
#51092=CARTESIAN_POINT('Ctrl Pts',(-3.52485021126398,3.94108560628483,384.574472930633));
#51093=CARTESIAN_POINT('Ctrl Pts',(-1.21842922909547,5.14510981239459,384.495345055173));
#51094=CARTESIAN_POINT('Ctrl Pts',(1.38301395642869,5.10333196688562,384.416217179714));
#51095=CARTESIAN_POINT('Ctrl Pts',(3.64958350715001,3.82586787438508,384.337089304254));
#51096=CARTESIAN_POINT('Ctrl Pts',(5.03246761935876,1.62203404033908,384.257961428794));
#51097=CARTESIAN_POINT('Ctrl Pts',(5.19682409785237,-0.974548133184912,
384.178833553334));
#51098=CARTESIAN_POINT('Ctrl Pts',(4.10285677781212,-3.33515982055948,384.099705677875));
#51099=CARTESIAN_POINT('Ctrl Pts',(2.0154514986864,-4.88821849187982,384.020577802414));
#51100=CARTESIAN_POINT('Ctrl Pts',(-0.559961559389509,-5.25767703647906,
383.941449926955));
#51101=CARTESIAN_POINT('Ctrl Pts',(-2.99978931706339,-4.3540772640303,383.862322051495));
#51102=CARTESIAN_POINT('Ctrl Pts',(-4.71326840155275,-2.39621070501691,
383.783194176035));
#51103=CARTESIAN_POINT('Ctrl Pts',(-5.28550858957794,0.14185808898655,383.704066300575));
#51104=CARTESIAN_POINT('Ctrl Pts',(-4.57795151673967,2.64557832586642,383.624938425116));
#51105=CARTESIAN_POINT('Ctrl Pts',(-2.76192026167378,4.50871614055144,383.545810549656));
#51106=CARTESIAN_POINT('Ctrl Pts',(-0.277136335846315,5.28014395819535,
383.466682674197));
#51107=CARTESIAN_POINT('Ctrl Pts',(2.27475150580887,4.77307347049397,383.387554798736));
#51108=CARTESIAN_POINT('Ctrl Pts',(4.27584642055071,3.11028329188466,383.308426923277));
#51109=CARTESIAN_POINT('Ctrl Pts',(5.24161683545466,0.6943901771998,383.229299047817));
#51110=CARTESIAN_POINT('Ctrl Pts',(4.93821764164047,-1.8896378731662,383.150171172357));
#51111=CARTESIAN_POINT('Ctrl Pts',(3.43911186553428,-4.01612180396144,383.071043296897));
#51112=CARTESIAN_POINT('Ctrl Pts',(1.1072828290795,-5.17016919494313,382.991915421438));
#51113=CARTESIAN_POINT('Ctrl Pts',(-1.49265617402097,-5.07234682509687,
382.912787545978));
#51114=CARTESIAN_POINT('Ctrl Pts',(-3.73117351815568,-3.74634074068643,
382.833659670518));
#51115=CARTESIAN_POINT('Ctrl Pts',(-5.06624977097178,-1.5132210763935,382.754531795058));
#51116=CARTESIAN_POINT('Ctrl Pts',(-5.17461860862547,1.08629969307746,382.675403919598));
#51117=CARTESIAN_POINT('Ctrl Pts',(-4.03004033454984,3.42279121037416,382.596276044139));
#51118=CARTESIAN_POINT('Ctrl Pts',(-1.90965538190854,4.93051124025298,382.517148168679));
#51119=CARTESIAN_POINT('Ctrl Pts',(0.673120594328623,5.24439066369047,382.438020293219));
#51120=CARTESIAN_POINT('Ctrl Pts',(3.09291170766135,4.28842884242289,382.35889241776));
#51121=CARTESIAN_POINT('Ctrl Pts',(4.76380612269667,2.29409589888282,382.2797645423));
#51122=CARTESIAN_POINT('Ctrl Pts',(5.28122477966896,-0.255713891925586,
382.20063666684));
#51123=CARTESIAN_POINT('Ctrl Pts',(4.51988342850276,-2.74360685242242,382.12150879138));
#51124=CARTESIAN_POINT('Ctrl Pts',(2.66412810880644,-4.56718142707082,382.04238091592));
#51125=CARTESIAN_POINT('Ctrl Pts',(0.16329884807764,-5.28488961607806,381.96325304046));
#51126=CARTESIAN_POINT('Ctrl Pts',(-2.37707049000228,-4.72295041827389,
381.884125165001));
#51127=CARTESIAN_POINT('Ctrl Pts',(-4.3418720751543,-3.0174279860352,381.804997289541));
#51128=CARTESIAN_POINT('Ctrl Pts',(-5.25536215553288,-0.581285972741413,
381.725869414081));
#51129=CARTESIAN_POINT('Ctrl Pts',(-4.89635442846138,1.99560469001251,381.646741538622));
#51130=CARTESIAN_POINT('Ctrl Pts',(-3.35177659407457,4.08929314568265,381.567613663161));
#51131=CARTESIAN_POINT('Ctrl Pts',(-0.995622270609436,5.1928278483096,381.488485787702));
#51132=CARTESIAN_POINT('Ctrl Pts',(1.60160528794473,5.03900637720777,381.409357912242));
#51133=CARTESIAN_POINT('Ctrl Pts',(3.81103098679937,3.66507402184023,381.330230036782));
#51134=CARTESIAN_POINT('Ctrl Pts',(5.09767944760569,1.40370545962173,381.251102161322));
#51135=CARTESIAN_POINT('Ctrl Pts',(5.15001032416474,-1.1975468378773,381.171974285863));
#51136=CARTESIAN_POINT('Ctrl Pts',(3.95535257236717,-3.50883325283227,381.092846410403));
#51137=CARTESIAN_POINT('Ctrl Pts',(1.8029725310162,-4.97051454281288,381.013718534943));
#51138=CARTESIAN_POINT('Ctrl Pts',(-0.785967070782117,-5.22866909753901,
380.934590659483));
#51139=CARTESIAN_POINT('Ctrl Pts',(-3.18459792796892,-4.22078912113472,
380.855462784024));
#51140=CARTESIAN_POINT('Ctrl Pts',(-4.81213180629493,-2.19091584657144,
380.776334908564));
#51141=CARTESIAN_POINT('Ctrl Pts',(-5.27448867275235,0.369450956041967,
380.697207033104));
#51142=CARTESIAN_POINT('Ctrl Pts',(-4.45971656638884,2.84036140577044,380.618079157644));
#51143=CARTESIAN_POINT('Ctrl Pts',(-2.56509888808806,4.6235259772432,380.538951282184));
#51144=CARTESIAN_POINT('Ctrl Pts',(-0.0493855337170155,5.28718127521391,
380.459823406725));
#51145=CARTESIAN_POINT('Ctrl Pts',(2.47828569939099,4.67063429954727,380.380695531265));
#51146=CARTESIAN_POINT('Ctrl Pts',(4.40588161411396,2.92317156019379,380.301567655805));
#51147=CARTESIAN_POINT('Ctrl Pts',(5.26666718771851,0.467911852513223,380.222439780345));
#51148=CARTESIAN_POINT('Ctrl Pts',(4.8522176299277,-2.10064486282949,380.143311904886));
#51149=CARTESIAN_POINT('Ctrl Pts',(3.26288495036134,-4.1605656548862,380.064184029426));
#51150=CARTESIAN_POINT('Ctrl Pts',(0.883499402425967,-5.21307525111868,
379.985056153966));
#51151=CARTESIAN_POINT('Ctrl Pts',(-1.70981070849824,-5.0033261046046,379.905928278506));
#51152=CARTESIAN_POINT('Ctrl Pts',(-3.88911883186622,-3.58210545343612,
379.826800403046));
#51153=CARTESIAN_POINT('Ctrl Pts',(-5.1267420551265,-1.29353804277671,379.747672527587));
#51154=CARTESIAN_POINT('Ctrl Pts',(-5.12301067114194,1.3082379108094,379.668544652126));
#51155=CARTESIAN_POINT('Ctrl Pts',(-3.87882817196482,3.59324599495851,379.589416776668));
#51156=CARTESIAN_POINT('Ctrl Pts',(-1.69545248338881,5.00820982432685,379.510288901207));
#51157=CARTESIAN_POINT('Ctrl Pts',(0.898448589337301,5.21051963821565,379.431161025747));
#51158=CARTESIAN_POINT('Ctrl Pts',(3.27480540417913,4.15118950816177,379.352033150288));
#51159=CARTESIAN_POINT('Ctrl Pts',(4.85822301267979,2.08671845896413,379.272905274828));
#51160=CARTESIAN_POINT('Ctrl Pts',(5.26530339668872,-0.483016468385486,
379.193777399368));
#51161=CARTESIAN_POINT('Ctrl Pts',(4.39747886842774,-2.93579705866137,379.114649523908));
#51162=CARTESIAN_POINT('Ctrl Pts',(2.4648785829925,-4.67772362790043,379.035521648449));
#51163=CARTESIAN_POINT('Ctrl Pts',(-0.0645507124447473,-5.28701787148826,
378.956393772989));
#51164=CARTESIAN_POINT('Ctrl Pts',(-2.57835013545374,-4.61614940691036,
378.877265897529));
#51165=CARTESIAN_POINT('Ctrl Pts',(-4.46784531508162,-2.82755778162292,
378.798138022069));
#51166=CARTESIAN_POINT('Ctrl Pts',(-5.27552668260484,-0.354320460935515,
378.719010146609));
#51167=CARTESIAN_POINT('Ctrl Pts',(-4.80582774062997,2.20470961700277,378.63988227115));
#51168=CARTESIAN_POINT('Ctrl Pts',(-3.17247821056078,4.22990623671853,378.56075439569));
#51169=CARTESIAN_POINT('Ctrl Pts',(-0.770966287939471,5.23090200164121,
378.48162652023));
#51170=CARTESIAN_POINT('Ctrl Pts',(1.81722219130848,4.96532257515351,378.40249864477));
#51171=CARTESIAN_POINT('Ctrl Pts',(3.96540079385267,3.49747356130477,378.323370769311));
#51172=CARTESIAN_POINT('Ctrl Pts',(5.15342409853101,1.18276998126983,378.244242893851));
#51173=CARTESIAN_POINT('Ctrl Pts',(5.09363218664291,-1.41832151330666,378.165115018391));
#51174=CARTESIAN_POINT('Ctrl Pts',(3.80050266687247,-3.67599024033094,378.085987142931));
#51175=CARTESIAN_POINT('Ctrl Pts',(1.58714516515185,-5.04357958127442,378.006859267472));
#51176=CARTESIAN_POINT('Ctrl Pts',(-1.01051292004705,-5.18995071328536,
377.927731392012));
#51177=CARTESIAN_POINT('Ctrl Pts',(-3.36349224912901,-4.07966232156074,
377.848603516552));
#51178=CARTESIAN_POINT('Ctrl Pts',(-4.90205833974629,-1.98155211933397,
377.769475641092));
#51179=CARTESIAN_POINT('Ctrl Pts',(-5.25367321659188,0.596357695664665,
377.690347765633));
#51180=CARTESIAN_POINT('Ctrl Pts',(-4.33319923422642,3.02986949626759,377.611219890172));
#51181=CARTESIAN_POINT('Ctrl Pts',(-2.36351373006459,4.72974921277116,377.532092014713));
#51182=CARTESIAN_POINT('Ctrl Pts',(0.178456984968689,5.28439948077629,377.452964139253));
#51183=CARTESIAN_POINT('Ctrl Pts',(2.67721733402229,4.55952104001336,377.373836263793));
#51184=CARTESIAN_POINT('Ctrl Pts',(4.52773440567874,2.73063104786141,377.294708388334));
#51185=CARTESIAN_POINT('Ctrl Pts',(5.28193652635228,0.240564543316707,377.215580512874));
#51186=CARTESIAN_POINT('Ctrl Pts',(4.75720630136386,-2.3077506308472,377.136452637414));
#51187=CARTESIAN_POINT('Ctrl Pts',(3.08059835436342,-4.29728269340077,377.057324761954));
#51188=CARTESIAN_POINT('Ctrl Pts',(0.658075181053442,-5.24629982216222,
376.978196886494));
#51189=CARTESIAN_POINT('Ctrl Pts',(-1.923789860657,-4.92501343550216,376.899069011035));
#51190=CARTESIAN_POINT('Ctrl Pts',(-4.03984145181191,-3.4112176436405,376.819941135575));
#51191=CARTESIAN_POINT('Ctrl Pts',(-5.17771318819473,-1.07145270939303,
376.740813260115));
#51192=CARTESIAN_POINT('Ctrl Pts',(-5.0618885123847,1.52774652882403,376.661685384655));
#51193=CARTESIAN_POINT('Ctrl Pts',(-3.72041242686768,3.75702756739127,376.582557509196));
#51194=CARTESIAN_POINT('Ctrl Pts',(-1.47810086816716,5.0766073897426,376.503429633736));
#51195=CARTESIAN_POINT('Ctrl Pts',(1.12210802704861,5.16697187426544,376.424301758276));
#51196=CARTESIAN_POINT('Ctrl Pts',(3.45061728097363,4.00624077340234,376.345173882816));
#51197=CARTESIAN_POINT('Ctrl Pts',(4.94361743453053,1.87546566308182,376.266046007357));
#51198=CARTESIAN_POINT('Ctrl Pts',(5.23960352937691,-0.709422013391795,
376.186918131896));
#51199=CARTESIAN_POINT('Ctrl Pts',(4.2669075188957,-3.12253502690154,376.107790256437));
#51200=CARTESIAN_POINT('Ctrl Pts',(2.26105138176727,-4.77957859502704,376.028662380977));
#51201=CARTESIAN_POINT('Ctrl Pts',(-0.292280359441297,-5.27932727476591,
375.949534505517));
#51202=CARTESIAN_POINT('Ctrl Pts',(-2.77484145645776,-4.50077558721857,
375.870406630058));
#51203=CARTESIAN_POINT('Ctrl Pts',(-4.58552092957851,-2.63243616845826,
375.791278754598));
#51204=CARTESIAN_POINT('Ctrl Pts',(-5.28589405424394,-0.126697339588848,
375.712150879138));
#51205=CARTESIAN_POINT('Ctrl Pts',(-4.70637522968859,2.40972094307884,375.633023003678));
#51206=CARTESIAN_POINT('Ctrl Pts',(-2.98728944096456,4.36266186682328,375.553895128218));
#51207=CARTESIAN_POINT('Ctrl Pts',(-0.544875549618088,5.2592655277028,375.474767252759));
#51208=CARTESIAN_POINT('Ctrl Pts',(2.02945798133318,4.88240903418803,375.395639377299));
#51209=CARTESIAN_POINT('Ctrl Pts',(4.1124194375256,3.3233956145555,375.316511501839));
#51210=CARTESIAN_POINT('Ctrl Pts',(5.19956989745793,0.959601216722932,375.237383626379));
#51211=CARTESIAN_POINT('Ctrl Pts',(5.02785240284651,-1.63637626402564,375.15825575092));
#51212=CARTESIAN_POINT('Ctrl Pts',(3.63845954881624,-3.83644847785649,375.07912787546));
#51213=CARTESIAN_POINT('Ctrl Pts',(2.1252131908655,-4.68314727417153,375.026375958487));
#51214=CARTESIAN_POINT('Ctrl Pts',(1.3130361863572,-4.90075024188303,375.));
#51215=CARTESIAN_POINT('Ctrl Pts',(3.43378788736214,2.93584158412968,400.));
#51216=CARTESIAN_POINT('Ctrl Pts',(3.5274081047691,2.83896859117363,400.));
#51217=CARTESIAN_POINT('Ctrl Pts',(3.61639766139016,2.73803801067182,400.));
#51218=CARTESIAN_POINT('Ctrl Pts',(3.70064392711817,2.63347462098305,400.));
#51219=CARTESIAN_POINT('Ctrl Pts',(3.7863602040819,2.52708670700993,400.));
#51220=CARTESIAN_POINT('Ctrl Pts',(3.86716669541736,2.4169376104458,400.));
#51221=CARTESIAN_POINT('Ctrl Pts',(3.94291532865978,2.30342952486372,400.));
#51222=CARTESIAN_POINT('Ctrl Pts',(4.0194785589048,2.18870077902246,400.));
#51223=CARTESIAN_POINT('Ctrl Pts',(4.09087506217895,2.07053982333204,400.));
#51224=CARTESIAN_POINT('Ctrl Pts',(4.15691470252894,1.94932444936402,400.));
#51225=CARTESIAN_POINT('Ctrl Pts',(4.22265038067262,1.82866699624951,400.));
#51226=CARTESIAN_POINT('Ctrl Pts',(4.28307881326963,1.70498249960347,400.));
#51227=CARTESIAN_POINT('Ctrl Pts',(4.33796903578875,1.57861622186133,400.));
#51228=CARTESIAN_POINT('Ctrl Pts',(4.35514545623615,1.53907329021963,400.));
#51229=CARTESIAN_POINT('Ctrl Pts',(4.37177922400871,1.4992675947038,400.));
#51230=CARTESIAN_POINT('Ctrl Pts',(4.38786228046478,1.45920932342454,400.));
#51231=CARTESIAN_POINT('Ctrl Pts',(4.39466658849891,1.44226174770453,400.));
#51232=CARTESIAN_POINT('Ctrl Pts',(4.40137035215038,1.4252737748662,400.));
#51233=CARTESIAN_POINT('Ctrl Pts',(4.40797035684919,1.40825358562441,400.));
#51234=CARTESIAN_POINT('Ctrl Pts',(4.45876403554847,1.27726609952389,400.));
#51235=CARTESIAN_POINT('Ctrl Pts',(4.50346815482664,1.14424239282724,400.));
#51236=CARTESIAN_POINT('Ctrl Pts',(4.54192438339399,1.0095915875114,400.));
#51237=CARTESIAN_POINT('Ctrl Pts',(4.54556160496616,0.996856204140475,400.));
#51238=CARTESIAN_POINT('Ctrl Pts',(4.54914290628383,0.984106240915922,400.));
#51239=CARTESIAN_POINT('Ctrl Pts',(4.55266813447105,0.971342029205324,400.));
#51240=CARTESIAN_POINT('Ctrl Pts',(4.58957020263633,0.837726335240427,400.));
#51241=CARTESIAN_POINT('Ctrl Pts',(4.62033177525015,0.702551284224113,400.));
#51242=CARTESIAN_POINT('Ctrl Pts',(4.64501953741251,0.566245432199611,400.));
#51243=CARTESIAN_POINT('Ctrl Pts',(4.66997011124341,0.428488546737278,400.));
#51244=CARTESIAN_POINT('Ctrl Pts',(4.68871702492031,0.289575922051531,400.));
#51245=CARTESIAN_POINT('Ctrl Pts',(4.70127911966368,0.149931994443125,400.));
#51246=CARTESIAN_POINT('Ctrl Pts',(4.71259060845871,0.0241901691579915,
400.));
#51247=CARTESIAN_POINT('Ctrl Pts',(4.71888682786237,-0.102145233205809,
400.));
#51248=CARTESIAN_POINT('Ctrl Pts',(4.72014590598849,-0.228768981279396,
400.));
#51249=CARTESIAN_POINT('Ctrl Pts',(4.72038025896983,-0.252337536919386,
400.));
#51250=CARTESIAN_POINT('Ctrl Pts',(4.72044000678068,-0.275916082362071,
400.));
#51251=CARTESIAN_POINT('Ctrl Pts',(4.72032487691908,-0.299502644881673,
400.));
#51252=CARTESIAN_POINT('Ctrl Pts',(4.7202295663887,-0.319028836890583,400.));
#51253=CARTESIAN_POINT('Ctrl Pts',(4.72001432373552,-0.338562445738198,
400.));
#51254=CARTESIAN_POINT('Ctrl Pts',(4.71967941555818,-0.358084898519809,
400.));
#51255=CARTESIAN_POINT('Ctrl Pts',(4.71723826258667,-0.50038448044343,400.));
#51256=CARTESIAN_POINT('Ctrl Pts',(4.70844382065583,-0.642283037525432,
400.));
#51257=CARTESIAN_POINT('Ctrl Pts',(4.69336920270997,-0.783339178745919,
400.));
#51258=CARTESIAN_POINT('Ctrl Pts',(4.6781762779915,-0.925502339519639,400.));
#51259=CARTESIAN_POINT('Ctrl Pts',(4.65660432919034,-1.06681060067863,400.));
#51260=CARTESIAN_POINT('Ctrl Pts',(4.62867689090467,-1.20682343753469,400.));
#51261=CARTESIAN_POINT('Ctrl Pts',(4.61869343839589,-1.25687498515869,400.));
#51262=CARTESIAN_POINT('Ctrl Pts',(4.6078973313099,-1.30676103650428,400.));
#51263=CARTESIAN_POINT('Ctrl Pts',(4.59628802798414,-1.35646151489045,400.));
#51264=CARTESIAN_POINT('Ctrl Pts',(4.56393613692852,-1.49496288892161,400.));
#51265=CARTESIAN_POINT('Ctrl Pts',(4.5252728763513,-1.63202392528166,400.));
#51266=CARTESIAN_POINT('Ctrl Pts',(4.48051876179014,-1.76728613860278,400.));
#51267=CARTESIAN_POINT('Ctrl Pts',(4.45444111221125,-1.84610169857621,400.));
#51268=CARTESIAN_POINT('Ctrl Pts',(4.42629449108343,-1.92430635496666,400.));
#51269=CARTESIAN_POINT('Ctrl Pts',(4.3961147432142,-2.00182684735068,400.));
#51270=CARTESIAN_POINT('Ctrl Pts',(4.37905752655991,-2.04564046168142,400.));
#51271=CARTESIAN_POINT('Ctrl Pts',(4.36135075314648,-2.08923549081769,400.));
#51272=CARTESIAN_POINT('Ctrl Pts',(4.34300012999985,-2.13259835388101,400.));
#51273=CARTESIAN_POINT('Ctrl Pts',(4.33569114983399,-2.14986960965973,400.));
#51274=CARTESIAN_POINT('Ctrl Pts',(4.32828379731778,-2.1670950989908,400.));
#51275=CARTESIAN_POINT('Ctrl Pts',(4.32077934892109,-2.18427268326289,400.));
#51276=CARTESIAN_POINT('Ctrl Pts',(4.26291559960507,-2.31672204897711,400.));
#51277=CARTESIAN_POINT('Ctrl Pts',(4.19927220468674,-2.44635051906979,400.));
#51278=CARTESIAN_POINT('Ctrl Pts',(4.13013682131626,-2.57280699644751,400.));
#51279=CARTESIAN_POINT('Ctrl Pts',(4.06045781537672,-2.70025782131784,400.));
#51280=CARTESIAN_POINT('Ctrl Pts',(3.98519984558575,-2.82448729912954,400.));
#51281=CARTESIAN_POINT('Ctrl Pts',(3.90460511771477,-2.94512595263581,400.));
#51282=CARTESIAN_POINT('Ctrl Pts',(3.82424500701874,-3.06541341815719,400.));
#51283=CARTESIAN_POINT('Ctrl Pts',(3.73857881602801,-3.18213164834041,400.));
#51284=CARTESIAN_POINT('Ctrl Pts',(3.6477996177404,-3.29489368172134,400.));
#51285=CARTESIAN_POINT('Ctrl Pts',(3.5967838663573,-3.35826326383848,400.));
#51286=CARTESIAN_POINT('Ctrl Pts',(3.54415252096129,-3.42038297838046,400.));
#51287=CARTESIAN_POINT('Ctrl Pts',(3.48993392052895,-3.48117996717138,400.));
#51288=CARTESIAN_POINT('Ctrl Pts',(3.44896085489101,-3.52712432929906,400.));
#51289=CARTESIAN_POINT('Ctrl Pts',(3.40708123835602,-3.57231323683387,400.));
#51290=CARTESIAN_POINT('Ctrl Pts',(3.36432098798037,-3.61672891625407,400.));
#51291=CARTESIAN_POINT('Ctrl Pts',(3.33855500174508,-3.64349241212974,400.));
#51292=CARTESIAN_POINT('Ctrl Pts',(3.31246924398559,-3.66997513430726,400.));
#51293=CARTESIAN_POINT('Ctrl Pts',(3.28606918882681,-3.69617297251379,400.));
#51294=CARTESIAN_POINT('Ctrl Pts',(3.27036247014898,-3.71175938217099,400.));
#51295=CARTESIAN_POINT('Ctrl Pts',(3.25455092639766,-3.72723854435311,400.));
#51296=CARTESIAN_POINT('Ctrl Pts',(3.23863897351742,-3.74260697959096,400.));
#51297=CARTESIAN_POINT('Ctrl Pts',(3.1336340986207,-3.84402511673945,400.));
#51298=CARTESIAN_POINT('Ctrl Pts',(3.02421929001433,-3.94066423251855,400.));
#51299=CARTESIAN_POINT('Ctrl Pts',(2.9108005879282,-4.03233943093569,400.));
#51300=CARTESIAN_POINT('Ctrl Pts',(2.80145832608402,-4.12071968362393,400.));
#51301=CARTESIAN_POINT('Ctrl Pts',(2.6883940765038,-4.20448664484191,400.));
#51302=CARTESIAN_POINT('Ctrl Pts',(2.57193725133249,-4.28344581179871,400.));
#51303=CARTESIAN_POINT('Ctrl Pts',(2.52394060920348,-4.31598812843542,400.));
#51304=CARTESIAN_POINT('Ctrl Pts',(2.47536734937678,-4.34771342641671,400.));
#51305=CARTESIAN_POINT('Ctrl Pts',(2.4262391678432,-4.37860645542617,400.));
#51306=CARTESIAN_POINT('Ctrl Pts',(2.4057205129273,-4.39150909871084,400.));
#51307=CARTESIAN_POINT('Ctrl Pts',(2.38510290902907,-4.40426785187222,400.));
#51308=CARTESIAN_POINT('Ctrl Pts',(2.36439500508045,-4.41687723791363,400.));
#51309=CARTESIAN_POINT('Ctrl Pts',(2.23718127032588,-4.49433979014823,400.));
#51310=CARTESIAN_POINT('Ctrl Pts',(2.10670807231056,-4.56608151115334,400.));
#51311=CARTESIAN_POINT('Ctrl Pts',(1.97337536799814,-4.63189274468176,400.));
#51312=CARTESIAN_POINT('Ctrl Pts',(1.84010399988323,-4.69767370348621,400.));
#51313=CARTESIAN_POINT('Ctrl Pts',(1.70397511685538,-4.75753010362705,400.));
#51314=CARTESIAN_POINT('Ctrl Pts',(1.56535633801641,-4.81121182598771,400.));
#51315=CARTESIAN_POINT('Ctrl Pts',(1.52584133805609,-4.82651446589492,400.));
#51316=CARTESIAN_POINT('Ctrl Pts',(1.48612384295406,-4.84131506971587,400.));
#51317=CARTESIAN_POINT('Ctrl Pts',(1.44621200692229,-4.85560715259022,400.));
#51318=CARTESIAN_POINT('Ctrl Pts',(1.4021027224054,-4.87140230542011,400.));
#51319=CARTESIAN_POINT('Ctrl Pts',(1.35775607141996,-4.88657636029028,400.));
#51320=CARTESIAN_POINT('Ctrl Pts',(1.31318543090145,-4.90112867346808,400.));
#51321=CARTESIAN_POINT('Ctrl Pts',(-4.51746064445937,-7.62825515632226E-5,
398.387416697508));
#51322=CARTESIAN_POINT('Ctrl Pts',(-4.51763289072636,-0.284226777710601,
398.397425295273));
#51323=CARTESIAN_POINT('Ctrl Pts',(-4.49123863994107,-0.568345670691312,
398.407433893039));
#51324=CARTESIAN_POINT('Ctrl Pts',(-4.4379719366677,-0.847333855511198,
398.417442490804));
#51325=CARTESIAN_POINT('Ctrl Pts',(-4.29759659267063,-1.58255980359031,
398.443818449291));
#51326=CARTESIAN_POINT('Ctrl Pts',(-3.97059302033473,-2.2821531656744,398.470194407778));
#51327=CARTESIAN_POINT('Ctrl Pts',(-3.49655043505552,-2.86141654221982,
398.496570366264));
#51328=CARTESIAN_POINT('Ctrl Pts',(-3.0225078497763,-3.44067991876523,398.522946324751));
#51329=CARTESIAN_POINT('Ctrl Pts',(-2.40142625155378,-3.89961330977197,
398.549322283237));
#51330=CARTESIAN_POINT('Ctrl Pts',(-1.70849788678631,-4.18265520276417,
398.575698241724));
#51331=CARTESIAN_POINT('Ctrl Pts',(-1.01556952201883,-4.46569709575638,
398.60207420021));
#51332=CARTESIAN_POINT('Ctrl Pts',(-0.250794390706405,-4.57284749073406,
398.628450158697));
#51333=CARTESIAN_POINT('Ctrl Pts',(0.493238771257572,-4.49113405337507,
398.654826117184));
#51334=CARTESIAN_POINT('Ctrl Pts',(1.23727193322155,-4.40942061601609,398.68120207567));
#51335=CARTESIAN_POINT('Ctrl Pts',(1.96056312583708,-4.13884334632044,398.707578034157));
#51336=CARTESIAN_POINT('Ctrl Pts',(2.57554593307285,-3.71216011566315,398.733953992643));
#51337=CARTESIAN_POINT('Ctrl Pts',(3.19052874030862,-3.28547688500585,398.76032995113));
#51338=CARTESIAN_POINT('Ctrl Pts',(3.69720316216463,-2.70268769338692,398.786705909617));
#51339=CARTESIAN_POINT('Ctrl Pts',(4.03422784198701,-2.03434886067149,398.813081868103));
#51340=CARTESIAN_POINT('Ctrl Pts',(4.37125252180939,-1.36601002795605,398.83945782659));
#51341=CARTESIAN_POINT('Ctrl Pts',(4.53862745959814,-0.612121554144129,
398.865833785076));
#51342=CARTESIAN_POINT('Ctrl Pts',(4.51608913784387,0.136045847258709,398.892209743563));
#51343=CARTESIAN_POINT('Ctrl Pts',(4.49355081608961,0.884213248661547,398.91858570205));
#51344=CARTESIAN_POINT('Ctrl Pts',(4.28109923479233,1.6266595776553,398.944961660536));
#51345=CARTESIAN_POINT('Ctrl Pts',(3.90445518858537,2.27349934610636,398.971337619023));
#51346=CARTESIAN_POINT('Ctrl Pts',(3.5278111423784,2.92033911455742,398.997713577509));
#51347=CARTESIAN_POINT('Ctrl Pts',(2.98697463126176,3.47157232246578,399.024089535996));
#51348=CARTESIAN_POINT('Ctrl Pts',(2.34742289856565,3.86046308384535,399.050465494483));
#51349=CARTESIAN_POINT('Ctrl Pts',(1.70787116586954,4.24935384522491,399.076841452969));
#51350=CARTESIAN_POINT('Ctrl Pts',(0.969604211593966,4.47590216007566,399.103217411456));
#51351=CARTESIAN_POINT('Ctrl Pts',(0.222001520718283,4.51268048034993,399.129593369942));
#51352=CARTESIAN_POINT('Ctrl Pts',(-0.525601170157399,4.5494588006242,399.155969328429));
#51353=CARTESIAN_POINT('Ctrl Pts',(-1.28253959763319,4.39646712632199,399.182345286915));
#51354=CARTESIAN_POINT('Ctrl Pts',(-1.95717379804064,4.07222787544583,399.208721245402));
#51355=CARTESIAN_POINT('Ctrl Pts',(-2.63180799844808,3.74798862456968,399.235097203889));
#51356=CARTESIAN_POINT('Ctrl Pts',(-3.22413797178719,3.25250179711959,399.261473162375));
#51357=CARTESIAN_POINT('Ctrl Pts',(-3.66245231437547,2.64575381071457,399.287849120862));
#51358=CARTESIAN_POINT('Ctrl Pts',(-4.10076665696376,2.03900582430954,399.314225079348));
#51359=CARTESIAN_POINT('Ctrl Pts',(-4.38506536880122,1.32099667894959,399.340601037835));
#51360=CARTESIAN_POINT('Ctrl Pts',(-4.48092940799817,0.578654358541173,
399.366976996322));
#51361=CARTESIAN_POINT('Ctrl Pts',(-4.50569226564232,0.386898228114258,
399.37379023005));
#51362=CARTESIAN_POINT('Ctrl Pts',(-4.51788177656568,0.193518461005119,
399.380603463779));
#51363=CARTESIAN_POINT('Ctrl Pts',(-4.51769110620511,0.00011483889287206,
399.387416697508));
#51364=CARTESIAN_POINT('Ctrl Pts',(-1.31303618635555,-4.90075024188347,
400.));
#51365=CARTESIAN_POINT('Ctrl Pts',(-2.12521319086393,-4.68314727417224,
399.973624041513));
#51366=CARTESIAN_POINT('Ctrl Pts',(-3.63845957255092,-3.83644859241818,
399.92087212454));
#51367=CARTESIAN_POINT('Ctrl Pts',(-5.02785239518849,-1.63637624738159,
399.84174424908));
#51368=CARTESIAN_POINT('Ctrl Pts',(-5.19956989353463,0.959601198026513,
399.76261637362));
#51369=CARTESIAN_POINT('Ctrl Pts',(-4.11241943286933,3.32339561801255,399.683488498161));
#51370=CARTESIAN_POINT('Ctrl Pts',(-2.02945797892606,4.8824090247121,399.604360622701));
#51371=CARTESIAN_POINT('Ctrl Pts',(0.54487554882432,5.2592655238007,399.525232747241));
#51372=CARTESIAN_POINT('Ctrl Pts',(2.98728943775363,4.36266186092565,399.446104871781));
#51373=CARTESIAN_POINT('Ctrl Pts',(4.70637522433117,2.40972094089285,399.366976996322));
#51374=CARTESIAN_POINT('Ctrl Pts',(5.28589404837916,-0.126697339701679,
399.287849120862));
#51375=CARTESIAN_POINT('Ctrl Pts',(4.58552092441564,-2.6324361653814,399.208721245402));
#51376=CARTESIAN_POINT('Ctrl Pts',(2.77484145336967,-4.50077558224301,399.129593369943));
#51377=CARTESIAN_POINT('Ctrl Pts',(0.292280359106768,-5.27932726882375,
399.050465494482));
#51378=CARTESIAN_POINT('Ctrl Pts',(-2.26105137922953,-4.77957858969287,
398.971337619023));
#51379=CARTESIAN_POINT('Ctrl Pts',(-4.26690751412045,-3.12253502339944,
398.892209743563));
#51380=CARTESIAN_POINT('Ctrl Pts',(-5.23960352350959,-0.709422012603199,
398.813081868103));
#51381=CARTESIAN_POINT('Ctrl Pts',(-4.94361742899746,1.87546566098248,398.733953992643));
#51382=CARTESIAN_POINT('Ctrl Pts',(-3.45061727711166,4.00624076891526,398.654826117184));
#51383=CARTESIAN_POINT('Ctrl Pts',(-1.12210802579434,5.16697186848109,398.575698241724));
#51384=CARTESIAN_POINT('Ctrl Pts',(1.47810086651078,5.07660738405961,398.496570366264));
#51385=CARTESIAN_POINT('Ctrl Pts',(3.72041242270134,3.75702756318667,398.417442490805));
#51386=CARTESIAN_POINT('Ctrl Pts',(5.06188850671742,1.52774652711538,398.338314615344));
#51387=CARTESIAN_POINT('Ctrl Pts',(5.17771318239863,-1.0714527081918,398.259186739885));
#51388=CARTESIAN_POINT('Ctrl Pts',(4.03984144729043,-3.41121763982034,398.180058864425));
#51389=CARTESIAN_POINT('Ctrl Pts',(1.92378985850489,-4.92501342998799,398.100930988965));
#51390=CARTESIAN_POINT('Ctrl Pts',(-0.658075180315041,-5.24629981628919,
398.021803113506));
#51391=CARTESIAN_POINT('Ctrl Pts',(-3.08059835091328,-4.29728268859095,
397.942675238046));
#51392=CARTESIAN_POINT('Ctrl Pts',(-4.75720629603741,-2.30775062826524,
397.863547362586));
#51393=CARTESIAN_POINT('Ctrl Pts',(-5.28193652043922,0.240564543045645,
397.784419487126));
#51394=CARTESIAN_POINT('Ctrl Pts',(-4.52773440061085,2.73063104480294,397.705291611666));
#51395=CARTESIAN_POINT('Ctrl Pts',(-2.67721733102668,4.55952103490808,397.626163736206));
#51396=CARTESIAN_POINT('Ctrl Pts',(-0.178456984770649,5.28439947486034,
397.547035860747));
#51397=CARTESIAN_POINT('Ctrl Pts',(2.36351372741711,4.72974920747697,397.467907985287));
#51398=CARTESIAN_POINT('Ctrl Pts',(4.33319922937441,3.02986949287705,397.388780109827));
#51399=CARTESIAN_POINT('Ctrl Pts',(5.25367321071018,0.596357694998765,397.309652234368));
#51400=CARTESIAN_POINT('Ctrl Pts',(4.90205833425909,-1.98155211711401,397.230524358907));
#51401=CARTESIAN_POINT('Ctrl Pts',(3.36349224536493,-4.07966231699243,397.151396483448));
#51402=CARTESIAN_POINT('Ctrl Pts',(1.01051291891753,-5.18995070747486,397.072268607988));
#51403=CARTESIAN_POINT('Ctrl Pts',(-1.58714516337332,-5.04357957562867,
396.993140732529));
#51404=CARTESIAN_POINT('Ctrl Pts',(-3.80050266261658,-3.67599023621695,
396.914012857068));
#51405=CARTESIAN_POINT('Ctrl Pts',(-5.09363218094012,-1.41832151172053,
396.834884981609));
#51406=CARTESIAN_POINT('Ctrl Pts',(-5.15342409276215,1.182769979944,396.755757106149));
#51407=CARTESIAN_POINT('Ctrl Pts',(-3.96540078941456,3.49747355738801,396.676629230689));
#51408=CARTESIAN_POINT('Ctrl Pts',(-1.81722218927578,4.96532256959422,396.597501355229));
#51409=CARTESIAN_POINT('Ctrl Pts',(0.770966287074601,5.23090199578547,396.51837347977));
#51410=CARTESIAN_POINT('Ctrl Pts',(3.17247820700774,4.22990623198423,396.43924560431));
#51411=CARTESIAN_POINT('Ctrl Pts',(4.8058277352491,2.20470961453625,396.36011772885));
#51412=CARTESIAN_POINT('Ctrl Pts',(5.275526676699,-0.354320460537079,396.28098985339));
#51413=CARTESIAN_POINT('Ctrl Pts',(4.46784531008081,-2.82755777845599,396.201861977931));
#51414=CARTESIAN_POINT('Ctrl Pts',(2.57835013256881,-4.61614940174172,396.122734102471));
#51415=CARTESIAN_POINT('Ctrl Pts',(0.0645507123742531,-5.2870178655694,
396.043606227011));
#51416=CARTESIAN_POINT('Ctrl Pts',(-2.46487858023149,-4.67772362266456,
395.964478351551));
#51417=CARTESIAN_POINT('Ctrl Pts',(-4.39747886350376,-2.93579705537622,
395.885350476092));
#51418=CARTESIAN_POINT('Ctrl Pts',(-5.26530339079403,-0.48301646784655,
395.806222600631));
#51419=CARTESIAN_POINT('Ctrl Pts',(-4.85822300724173,2.08671845662638,395.727094725172));
#51420=CARTESIAN_POINT('Ctrl Pts',(-3.27480540051438,4.15118950351341,395.647966849712));
#51421=CARTESIAN_POINT('Ctrl Pts',(-0.898448588333209,5.21051963238218,
395.568838974252));
#51422=CARTESIAN_POINT('Ctrl Pts',(1.69545248148909,5.00820981872071,395.489711098793));
#51423=CARTESIAN_POINT('Ctrl Pts',(3.87882816762124,3.59324599093717,395.410583223333));
#51424=CARTESIAN_POINT('Ctrl Pts',(5.12301066540628,1.30823790934658,395.331455347873));
#51425=CARTESIAN_POINT('Ctrl Pts',(5.12674204938754,-1.29353804132683,395.252327472413));
#51426=CARTESIAN_POINT('Ctrl Pts',(3.88911882751359,-3.58210544942458,395.173199596953));
#51427=CARTESIAN_POINT('Ctrl Pts',(1.70981070658587,-5.00332609900278,395.094071721494));
#51428=CARTESIAN_POINT('Ctrl Pts',(-0.883499401435098,-5.21307524528295,
395.014943846034));
#51429=CARTESIAN_POINT('Ctrl Pts',(-3.26288494670713,-4.16056565022955,
394.935815970574));
#51430=CARTESIAN_POINT('Ctrl Pts',(-4.85221762449495,-2.10064486047942,
394.856688095114));
#51431=CARTESIAN_POINT('Ctrl Pts',(-5.26666718182262,0.467911851987696,
394.777560219655));
#51432=CARTESIAN_POINT('Ctrl Pts',(-4.40588160918252,2.92317155691987,394.698432344195));
#51433=CARTESIAN_POINT('Ctrl Pts',(-2.47828569661807,4.67063429431767,394.619304468735));
#51434=CARTESIAN_POINT('Ctrl Pts',(0.0493855336599835,5.28718126929493,
394.540176593275));
#51435=CARTESIAN_POINT('Ctrl Pts',(2.56509888521489,4.623525972068,394.461048717816));
#51436=CARTESIAN_POINT('Ctrl Pts',(4.45971656139522,2.84036140259214,394.381920842355));
#51437=CARTESIAN_POINT('Ctrl Pts',(5.27448866684743,0.369450955630144,394.302792966896));
#51438=CARTESIAN_POINT('Ctrl Pts',(4.81213180090847,-2.19091584411711,394.223665091436));
#51439=CARTESIAN_POINT('Ctrl Pts',(3.18459792440514,-4.2207891164085,394.144537215977));
#51440=CARTESIAN_POINT('Ctrl Pts',(0.785967069903959,-5.22866909168525,
394.065409340517));
#51441=CARTESIAN_POINT('Ctrl Pts',(-1.8029725289961,-4.97051453724898,393.986281465057));
#51442=CARTESIAN_POINT('Ctrl Pts',(-3.95535256793798,-3.50883324890547,
393.907153589597));
#51443=CARTESIAN_POINT('Ctrl Pts',(-5.15001031839888,-1.19754683653839,
393.828025714137));
#51444=CARTESIAN_POINT('Ctrl Pts',(-5.0976794418993,1.40370545804854,393.748897838677));
#51445=CARTESIAN_POINT('Ctrl Pts',(-3.81103098253419,3.66507401773587,393.669769963218));
#51446=CARTESIAN_POINT('Ctrl Pts',(-1.60160528615343,5.03900637156607,393.590642087758));
#51447=CARTESIAN_POINT('Ctrl Pts',(0.995622269493122,5.19282784249655,393.511514212298));
#51448=CARTESIAN_POINT('Ctrl Pts',(3.3517765903209,4.08929314110579,393.432386336838));
#51449=CARTESIAN_POINT('Ctrl Pts',(4.89635442297923,1.99560468778007,393.353258461378));
#51450=CARTESIAN_POINT('Ctrl Pts',(5.2553621496497,-0.581285972088894,393.274130585919));
#51451=CARTESIAN_POINT('Ctrl Pts',(4.34187207029457,-3.01742798265574,393.195002710459));
#51452=CARTESIAN_POINT('Ctrl Pts',(2.37707048734272,-4.72295041298575,393.115874834999));
#51453=CARTESIAN_POINT('Ctrl Pts',(-0.163298847893048,-5.28488961016167,
393.03674695954));
#51454=CARTESIAN_POINT('Ctrl Pts',(-2.66412810582239,-4.56718142195876,
392.957619084079));
#51455=CARTESIAN_POINT('Ctrl Pts',(-4.51988342344183,-2.74360684935247,
392.87849120862));
#51456=CARTESIAN_POINT('Ctrl Pts',(-5.28122477375654,-0.255713891641081,
392.79936333316));
#51457=CARTESIAN_POINT('Ctrl Pts',(-4.76380611736435,2.29409589631297,392.7202354577));
#51458=CARTESIAN_POINT('Ctrl Pts',(-3.09291170420029,4.28842883762094,392.64110758224));
#51459=CARTESIAN_POINT('Ctrl Pts',(-0.67312059357683,5.24439065781915,392.561979706781));
#51460=CARTESIAN_POINT('Ctrl Pts',(1.90965537976903,4.9305112347339,392.482851831321));
#51461=CARTESIAN_POINT('Ctrl Pts',(4.03004033003705,3.4227912065437,392.403723955861));
#51462=CARTESIAN_POINT('Ctrl Pts',(5.17461860283211,1.0862996918631,392.324596080401));
#51463=CARTESIAN_POINT('Ctrl Pts',(5.06624976530063,-1.51322107469774,392.245468204942));
#51464=CARTESIAN_POINT('Ctrl Pts',(3.73117351397988,-3.74634073649114,392.166340329482));
#51465=CARTESIAN_POINT('Ctrl Pts',(1.49265617235166,-5.07234681941786,392.087212454022));
#51466=CARTESIAN_POINT('Ctrl Pts',(-1.10728282783815,-5.1701691891555,392.008084578562));
#51467=CARTESIAN_POINT('Ctrl Pts',(-3.43911186168285,-4.01612179946654,
391.928956703103));
#51468=CARTESIAN_POINT('Ctrl Pts',(-4.93821763611149,-1.8896378710524,391.849828827643));
#51469=CARTESIAN_POINT('Ctrl Pts',(-5.24161682958689,0.694390176420624,
391.770700952183));
#51470=CARTESIAN_POINT('Ctrl Pts',(-4.27584641576499,3.1102832884012,391.691573076723));
#51471=CARTESIAN_POINT('Ctrl Pts',(-2.27475150326393,4.77307346514974,391.612445201264));
#51472=CARTESIAN_POINT('Ctrl Pts',(0.277136335534271,5.28014395228432,391.533317325804));
#51473=CARTESIAN_POINT('Ctrl Pts',(2.76192025858026,4.50871613550486,391.454189450344));
#51474=CARTESIAN_POINT('Ctrl Pts',(4.57795151161372,2.64557832290629,391.375061574885));
#51475=CARTESIAN_POINT('Ctrl Pts',(5.28550858366077,0.141858088829558,391.295933699424));
#51476=CARTESIAN_POINT('Ctrl Pts',(4.71326839627705,-2.39621070233275,391.216805823965));
#51477=CARTESIAN_POINT('Ctrl Pts',(2.99978931370662,-4.35407725915487,391.137677948505));
#51478=CARTESIAN_POINT('Ctrl Pts',(0.559961558764467,-5.2576770305929,391.058550073045));
#51479=CARTESIAN_POINT('Ctrl Pts',(-2.01545149642842,-4.88821848640817,
390.979422197585));
#51480=CARTESIAN_POINT('Ctrl Pts',(-4.10285677321784,-3.33515981682715,
390.900294322126));
#51481=CARTESIAN_POINT('Ctrl Pts',(-5.19682409203417,-0.974548132095691,
390.821166446665));
#51482=CARTESIAN_POINT('Ctrl Pts',(-5.03246761372548,1.62203403852146,390.742038571206));
#51483=CARTESIAN_POINT('Ctrl Pts',(-3.64958350306562,3.82586787010077,390.662910695746));
#51484=CARTESIAN_POINT('Ctrl Pts',(-1.38301395488213,5.10333196117197,390.583782820286));
#51485=CARTESIAN_POINT('Ctrl Pts',(1.21842922772966,5.14510980663504,390.504654944826));
#51486=CARTESIAN_POINT('Ctrl Pts',(3.52485020731651,3.94108560187402,390.425527069367));
#51487=CARTESIAN_POINT('Ctrl Pts',(4.97778782502355,1.78279361519087,390.346399193907));
#51488=CARTESIAN_POINT('Ctrl Pts',(5.2254376041702,-0.807171945896316,390.267271318447));
#51489=CARTESIAN_POINT('Ctrl Pts',(4.2078353041098,-3.20169435749343,390.188143442988));
#51490=CARTESIAN_POINT('Ctrl Pts',(2.17137625543244,-4.82098017654731,390.109015567527));
#51491=CARTESIAN_POINT('Ctrl Pts',(-0.390845137002325,-5.27294649927341,
390.029887692068));
#51492=CARTESIAN_POINT('Ctrl Pts',(-2.85842993443779,-4.44815726062243,
389.950759816608));
#51493=CARTESIAN_POINT('Ctrl Pts',(-4.63389386243089,-2.54632134206259,
389.871631941148));
#51494=CARTESIAN_POINT('Ctrl Pts',(-5.2873381074052,-0.0279364152813674,
389.792504065688));
#51495=CARTESIAN_POINT('Ctrl Pts',(-4.66054210445731,2.49721284593419,389.713376190229));
#51496=CARTESIAN_POINT('Ctrl Pts',(-2.90527399360582,4.41770389765948,389.634248314769));
#51497=CARTESIAN_POINT('Ctrl Pts',(-0.446542510013585,5.2685220405792,389.55512043931));
#51498=CARTESIAN_POINT('Ctrl Pts',(2.12031175334316,4.84365593059135,389.475992563849));
#51499=CARTESIAN_POINT('Ctrl Pts',(4.17376808571255,3.24597977073262,389.39686468839));
#51500=CARTESIAN_POINT('Ctrl Pts',(5.21661647505316,0.862344048232485,389.31773681293));
#51501=CARTESIAN_POINT('Ctrl Pts',(4.99634867366186,-1.73009382303836,389.23860893747));
#51502=CARTESIAN_POINT('Ctrl Pts',(3.56629883549932,-3.90361849073832,389.15948106201));
#51503=CARTESIAN_POINT('Ctrl Pts',(1.27272954528402,-5.13194740911081,389.08035318655));
#51504=CARTESIAN_POINT('Ctrl Pts',(-1.3290098591728,-5.11766133107102,389.001225311091));
#51505=CARTESIAN_POINT('Ctrl Pts',(-3.60895181526604,-3.86421939082217,
388.922097435631));
#51506=CARTESIAN_POINT('Ctrl Pts',(-5.01504661559582,-1.67512153252199,
388.842969560171));
#51507=CARTESIAN_POINT('Ctrl Pts',(-5.20683198610126,0.919578911149497,
388.763841684712));
#51508=CARTESIAN_POINT('Ctrl Pts',(-4.13787031577727,3.29161874388992,388.684713809251));
#51509=CARTESIAN_POINT('Ctrl Pts',(-2.0669927453671,4.86664830205737,388.605585933792));
#51510=CARTESIAN_POINT('Ctrl Pts',(0.504372452470541,5.2633005932121,388.526458058332));
#51511=CARTESIAN_POINT('Ctrl Pts',(2.95361231985281,4.38553291736953,388.447330182872));
#51512=CARTESIAN_POINT('Ctrl Pts',(4.68768449948338,2.44588199605403,388.368202307412));
#51513=CARTESIAN_POINT('Ctrl Pts',(5.28671249546426,-0.0859982303311033,
388.289074431953));
#51514=CARTESIAN_POINT('Ctrl Pts',(4.60565172496217,-2.59705542753155,388.209946556493));
#51515=CARTESIAN_POINT('Ctrl Pts',(2.80940963137597,-4.47927920858367,388.130818681033));
#51516=CARTESIAN_POINT('Ctrl Pts',(0.332916112606594,-5.27692065197923,
388.051690805573));
#51517=CARTESIAN_POINT('Ctrl Pts',(-2.22418745944155,-4.79684425957118,
387.972562930114));
#51518=CARTESIAN_POINT('Ctrl Pts',(-4.24274134038657,-3.15529247834378,
387.893435054654));
#51519=CARTESIAN_POINT('Ctrl Pts',(-5.23398656144486,-0.749739541395986,
387.814307179194));
#51520=CARTESIAN_POINT('Ctrl Pts',(-4.95790971666796,1.83735025150007,387.735179303734));
#51521=CARTESIAN_POINT('Ctrl Pts',(-3.48135818389009,3.97955649548785,387.656051428275));
#51522=CARTESIAN_POINT('Ctrl Pts',(-1.16185415329344,5.15817987586638,387.576923552815));
#51523=CARTESIAN_POINT('Ctrl Pts',(1.43897337488296,5.0878365079566,387.497795677355));
#51524=CARTESIAN_POINT('Ctrl Pts',(3.69137763358211,3.7855588585581,387.418667801895));
#51525=CARTESIAN_POINT('Ctrl Pts',(5.04997670698908,1.56667161976776,387.339539926436));
#51526=CARTESIAN_POINT('Ctrl Pts',(5.1858086147589,-1.03155887685117,387.260412050976));
#51527=CARTESIAN_POINT('Ctrl Pts',(4.06598393848355,-3.38001469187811,387.181284175516));
#51528=CARTESIAN_POINT('Ctrl Pts',(1.96164944276588,-4.91005663602919,387.102156300056));
#51529=CARTESIAN_POINT('Ctrl Pts',(-0.617665566383616,-5.25121071310437,
387.023028424596));
#51530=CARTESIAN_POINT('Ctrl Pts',(-3.04742321760052,-4.32087218488899,
386.943900549136));
#51531=CARTESIAN_POINT('Ctrl Pts',(-4.73929844549354,-2.34430692313541,
386.864772673677));
#51532=CARTESIAN_POINT('Ctrl Pts',(-5.28363203833613,0.199892943312196,
386.785644798217));
#51533=CARTESIAN_POINT('Ctrl Pts',(-4.54862274572651,2.695692085973,386.706516922757));
#51534=CARTESIAN_POINT('Ctrl Pts',(-2.71224074091265,4.53877459989496,386.627389047297));
#51535=CARTESIAN_POINT('Ctrl Pts',(-0.219135128106394,5.28286896496098,
386.548261171838));
#51536=CARTESIAN_POINT('Ctrl Pts',(2.32703038082081,4.74780520999492,386.469133296378));
#51537=CARTESIAN_POINT('Ctrl Pts',(4.30974451002784,3.06314004962277,386.390005420918));
#51538=CARTESIAN_POINT('Ctrl Pts',(5.24892628554031,0.636786898642001,386.310877545458));
#51539=CARTESIAN_POINT('Ctrl Pts',(4.91716859158436,-1.94375352019086,386.231749669999));
#51540=CARTESIAN_POINT('Ctrl Pts',(3.39480098979053,-4.05364662310803,386.152621794539));
#51541=CARTESIAN_POINT('Ctrl Pts',(1.05043926306477,-5.18201718059,386.073493919079));
#51542=CARTESIAN_POINT('Ctrl Pts',(-1.54826871412865,-5.0556491862241,385.994366043619));
#51543=CARTESIAN_POINT('Ctrl Pts',(-3.772089388456,-3.70514053050835,385.91523816816));
#51544=CARTESIAN_POINT('Ctrl Pts',(-5.08256187967811,-1.45749423482943,
385.836110292699));
#51545=CARTESIAN_POINT('Ctrl Pts',(-5.16237725218749,1.14305984594648,385.75698241724));
#51546=CARTESIAN_POINT('Ctrl Pts',(-3.99220955212729,3.46684115546438,385.67785454178));
#51547=CARTESIAN_POINT('Ctrl Pts',(-1.85539526299902,4.95118502212943,385.59872666632));
#51548=CARTESIAN_POINT('Ctrl Pts',(0.73067187193628,5.23668247279509,385.51959879086));
#51549=CARTESIAN_POINT('Ctrl Pts',(3.13981906729605,4.25420508790564,385.440470915401));
#51550=CARTESIAN_POINT('Ctrl Pts',(4.78871173391359,2.24164328892807,385.361343039941));
#51551=CARTESIAN_POINT('Ctrl Pts',(5.27809816640793,-0.313694837508304,
385.282215164481));
#51552=CARTESIAN_POINT('Ctrl Pts',(4.48948164772799,-2.79307702006795,385.203087289022));
#51553=CARTESIAN_POINT('Ctrl Pts',(2.61381244185943,-4.59616244535579,385.123959413562));
#51554=CARTESIAN_POINT('Ctrl Pts',(0.105252389857621,-5.28636421747,385.044831538102));
#51555=CARTESIAN_POINT('Ctrl Pts',(-2.42879276314368,-4.69656155277656,
384.965703662642));
#51556=CARTESIAN_POINT('Ctrl Pts',(-4.3747464822184,-2.96956527485689,384.886575787182));
#51557=CARTESIAN_POINT('Ctrl Pts',(-5.26142871019096,-0.5235385686808,384.807447911723));
#51558=CARTESIAN_POINT('Ctrl Pts',(-4.87414421624611,2.04925422155296,384.728320036263));
#51559=CARTESIAN_POINT('Ctrl Pts',(-3.30666744538294,4.12585447040522,384.649192160803));
#51560=CARTESIAN_POINT('Ctrl Pts',(-0.93853660926441,5.20344825460853,384.570064285343));
#51561=CARTESIAN_POINT('Ctrl Pts',(1.65684512644118,5.02111431181428,384.490936409884));
#51562=CARTESIAN_POINT('Ctrl Pts',(3.85104960199139,3.62300174831864,384.411808534424));
#51563=CARTESIAN_POINT('Ctrl Pts',(5.11278700298303,1.34764007340457,384.332680658964));
#51564=CARTESIAN_POINT('Ctrl Pts',(5.13654877856401,-1.25403004379905,384.253552783504));
#51565=CARTESIAN_POINT('Ctrl Pts',(3.91658141328989,-3.55205781743347,384.174424908044));
#51566=CARTESIAN_POINT('Ctrl Pts',(1.74827954439566,-4.99001436270134,384.095297032584));
#51567=CARTESIAN_POINT('Ctrl Pts',(-0.843338895500463,-5.21972261836337,
384.016169157125));
#51568=CARTESIAN_POINT('Ctrl Pts',(-3.23075696562154,-4.18556258278454,
383.937041281665));
#51569=CARTESIAN_POINT('Ctrl Pts',(-4.8359014200548,-2.1379387645183,383.857913406205));
#51570=CARTESIAN_POINT('Ctrl Pts',(-5.27011344929143,0.427351069865941,
383.778785530745));
#51571=CARTESIAN_POINT('Ctrl Pts',(-4.42825589269063,2.88916500985471,383.699657655286));
#51572=CARTESIAN_POINT('Ctrl Pts',(-2.51417043865664,4.65141609735177,383.620529779826));
#51573=CARTESIAN_POINT('Ctrl Pts',(0.00867922154690349,5.28740478651213,
383.541401904366));
#51574=CARTESIAN_POINT('Ctrl Pts',(2.52942735381344,4.6431370825228,383.462274028906));
#51575=CARTESIAN_POINT('Ctrl Pts',(4.43771707378134,2.87461160478899,383.383146153446));
#51576=CARTESIAN_POINT('Ctrl Pts',(5.27148802998996,0.410047137522666,383.304018277987));
#51577=CARTESIAN_POINT('Ctrl Pts',(4.82885656869832,-2.15380336712922,383.224890402527));
#51578=CARTESIAN_POINT('Ctrl Pts',(3.2169984748157,-4.19614650820864,383.145762527067));
#51579=CARTESIAN_POINT('Ctrl Pts',(0.82619815304806,-5.22246314656389,383.066634651607));
#51580=CARTESIAN_POINT('Ctrl Pts',(-1.76465219517988,-4.98424792073636,
382.987506776148));
#51581=CARTESIAN_POINT('Ctrl Pts',(-3.92822160960685,-3.5391806525149,382.908378900688));
#51582=CARTESIAN_POINT('Ctrl Pts',(-5.14063804209515,-1.23716014544694,
382.829251025228));
#51583=CARTESIAN_POINT('Ctrl Pts',(-5.10833518714595,1.36441794223199,382.750123149768));
#51584=CARTESIAN_POINT('Ctrl Pts',(-3.83913463932894,3.63562510806912,382.670995274309));
#51585=CARTESIAN_POINT('Ctrl Pts',(-1.64035202533435,5.0265266276326,382.591867398849));
#51586=CARTESIAN_POINT('Ctrl Pts',(0.955614320991023,5.2003390249901,382.512739523389));
#51587=CARTESIAN_POINT('Ctrl Pts',(3.32019468624774,4.11497654315675,382.433611647929));
#51588=CARTESIAN_POINT('Ctrl Pts',(4.8808455917412,2.03324150432223,382.354483772469));
#51589=CARTESIAN_POINT('Ctrl Pts',(5.25968159463003,-0.540808864968189,
382.27535589701));
#51590=CARTESIAN_POINT('Ctrl Pts',(4.36497391033337,-2.98391143759783,382.19622802155));
#51591=CARTESIAN_POINT('Ctrl Pts',(2.41336099931917,-4.70450989926509,382.11710014609));
#51592=CARTESIAN_POINT('Ctrl Pts',(-0.122606802820077,-5.28599018890692,
382.03797227063));
#51593=CARTESIAN_POINT('Ctrl Pts',(-2.6288874239146,-4.58755660648474,381.958844395171));
#51594=CARTESIAN_POINT('Ctrl Pts',(-4.49862704479611,-2.77832313044165,
381.879716519711));
#51595=CARTESIAN_POINT('Ctrl Pts',(-5.27909957396784,-0.296365304059962,
381.800588644251));
#51596=CARTESIAN_POINT('Ctrl Pts',(-4.78132667791946,2.25735241031028,381.721460768791));
#51597=CARTESIAN_POINT('Ctrl Pts',(-3.12583571520092,4.26449009693918,381.642332893332));
#51598=CARTESIAN_POINT('Ctrl Pts',(-0.713476057932961,5.23905302703404,
381.563205017871));
#51599=CARTESIAN_POINT('Ctrl Pts',(1.87163986094335,4.94506713162178,381.484077142412));
#51600=CARTESIAN_POINT('Ctrl Pts',(4.00356957706116,3.45371616479241,381.404949266952));
#51601=CARTESIAN_POINT('Ctrl Pts',(5.16610206459392,1.12610575148009,381.325821391492));
#51602=CARTESIAN_POINT('Ctrl Pts',(5.07774957870228,-1.47417228345499,381.246693516033));
#51603=CARTESIAN_POINT('Ctrl Pts',(3.75990519207135,-3.71750422352859,381.167565640573));
#51604=CARTESIAN_POINT('Ctrl Pts',(1.53166282114666,-5.06070486272762,381.088437765113));
#51605=CARTESIAN_POINT('Ctrl Pts',(-1.0674460141586,-5.17854069330105,381.009309889653));
#51606=CARTESIAN_POINT('Ctrl Pts',(-3.40809069944175,-4.04247974511891,
380.930182014193));
#51607=CARTESIAN_POINT('Ctrl Pts',(-4.92352337948473,-1.92760012372517,
380.851054138734));
#51608=CARTESIAN_POINT('Ctrl Pts',(-5.24680744637695,0.654015539541282,
380.771926263274));
#51609=CARTESIAN_POINT('Ctrl Pts',(-4.29966508516876,3.07727230850615,380.692798387814));
#51610=CARTESIAN_POINT('Ctrl Pts',(-2.31143093395199,4.75541919738815,380.613670512354));
#51611=CARTESIAN_POINT('Ctrl Pts',(0.236477452546483,5.28212108151216,380.534542636895));
#51612=CARTESIAN_POINT('Ctrl Pts',(2.7271267899117,4.52984593303835,380.455414761435));
#51613=CARTESIAN_POINT('Ctrl Pts',(4.55744811217567,2.68074456264382,380.376286885975));
#51614=CARTESIAN_POINT('Ctrl Pts',(5.28425980776137,0.182545855597361,380.297159010515));
#51615=CARTESIAN_POINT('Ctrl Pts',(4.73157661405697,-2.35985326887651,380.218031135055));
#51616=CARTESIAN_POINT('Ctrl Pts',(3.03322149728047,-4.33085350176541,380.138903259596));
#51617=CARTESIAN_POINT('Ctrl Pts',(0.600422665576261,-5.25321019263273,
380.059775384136));
#51618=CARTESIAN_POINT('Ctrl Pts',(-1.97775844481349,-4.90359013777528,
379.980647508676));
#51619=CARTESIAN_POINT('Ctrl Pts',(-4.07705851709219,-3.36664796994342,
379.901519633216));
#51620=CARTESIAN_POINT('Ctrl Pts',(-5.18916724645199,-1.01452845877678,
379.822391757756));
#51621=CARTESIAN_POINT('Ctrl Pts',(-5.04480615543027,1.58324210386498,379.743263882297));
#51622=CARTESIAN_POINT('Ctrl Pts',(-3.67892986111526,3.7976571438602,379.664136006837));
#51623=CARTESIAN_POINT('Ctrl Pts',(-1.42226240084736,5.09253319757995,379.585008131377));
#51624=CARTESIAN_POINT('Ctrl Pts',(1.17878204679748,5.15433774518764,379.505880255918));
#51625=CARTESIAN_POINT('Ctrl Pts',(3.49440419135096,3.9681058520139,379.426752380457));
#51626=CARTESIAN_POINT('Ctrl Pts',(4.96391496617568,1.82106367650753,379.347624504998));
#51627=CARTESIAN_POINT('Ctrl Pts',(5.2314969825461,-0.766918526917405,379.268496629538));
#51628=CARTESIAN_POINT('Ctrl Pts',(4.23235974285854,-3.16920427116154,379.189368754078));
#51629=CARTESIAN_POINT('Ctrl Pts',(2.20842757301423,-4.80412035237133,379.110240878619));
#51630=CARTESIAN_POINT('Ctrl Pts',(-0.350238295746339,-5.27579926091873,
379.031113003158));
#51631=CARTESIAN_POINT('Ctrl Pts',(-2.82409983509395,-4.47003185970082,
378.951985127699));
#51632=CARTESIAN_POINT('Ctrl Pts',(-4.61415296279982,-2.58192121126957,
378.872857252239));
#51633=CARTESIAN_POINT('Ctrl Pts',(-5.28696633525482,-0.0686416433394937,
378.793729376779));
#51634=CARTESIAN_POINT('Ctrl Pts',(-4.67962947817872,2.46125834732535,378.71460150132));
#51635=CARTESIAN_POINT('Ctrl Pts',(-2.9391988257698,4.39520590733944,378.63547362586));
#51636=CARTESIAN_POINT('Ctrl Pts',(-0.487090471470337,5.2649280695866,378.5563457504));
#51637=CARTESIAN_POINT('Ctrl Pts',(2.08295867142411,4.85983619872698,378.47721787494));
#51638=CARTESIAN_POINT('Ctrl Pts',(4.1486543056634,3.27801649742928,378.398089999481));
#51639=CARTESIAN_POINT('Ctrl Pts',(5.20982287752563,0.902480077413658,378.318962124021));
#51640=CARTESIAN_POINT('Ctrl Pts',(5.00952021436078,-1.69157675771122,378.239834248561));
#51641=CARTESIAN_POINT('Ctrl Pts',(3.59624624674644,-3.8760466506584,378.160706373101));
#51642=CARTESIAN_POINT('Ctrl Pts',(1.31220156369858,-5.12199685294173,378.081578497641));
#51643=CARTESIAN_POINT('Ctrl Pts',(-1.28957072085835,-5.12774141910675,
378.002450622182));
#51644=CARTESIAN_POINT('Ctrl Pts',(-3.57909508295452,-3.89188939879962,
377.923322746722));
#51645=CARTESIAN_POINT('Ctrl Pts',(-5.00200159628448,-1.71368163206748,
377.844194871262));
#51646=CARTESIAN_POINT('Ctrl Pts',(-5.21375731243622,0.879465401443313,
377.765066995802));
#51647=CARTESIAN_POINT('Ctrl Pts',(-4.16308913613231,3.25966463764834,377.685939120343));
#51648=CARTESIAN_POINT('Ctrl Pts',(-2.1043987453421,4.85059075019948,377.606811244883));
#51649=CARTESIAN_POINT('Ctrl Pts',(0.463836508427624,5.26702766261653,377.527683369423));
#51650=CARTESIAN_POINT('Ctrl Pts',(2.91976153075723,4.40814216068722,377.448555493963));
#51651=CARTESIAN_POINT('Ctrl Pts',(4.66871526619766,2.48189896419878,377.369427618503));
#51652=CARTESIAN_POINT('Ctrl Pts',(5.28721789969248,-0.0452944421492617,
377.290299743044));
#51653=CARTESIAN_POINT('Ctrl Pts',(4.62550939154664,-2.56152055897115,377.211171867584));
#51654=CARTESIAN_POINT('Ctrl Pts',(2.84381135938942,-4.45751743210561,377.132043992124));
#51655=CARTESIAN_POINT('Ctrl Pts',(0.373532100567371,-5.27420121678766,
377.052916116664));
#51656=CARTESIAN_POINT('Ctrl Pts',(-2.18719169184094,-4.81382563128935,
376.973788241204));
#51657=CARTESIAN_POINT('Ctrl Pts',(-4.21832369780876,-3.18786290260816,
376.894660365745));
#51658=CARTESIAN_POINT('Ctrl Pts',(-5.2280593665279,-0.790012636213206,
376.815532490285));
#51659=CARTESIAN_POINT('Ctrl Pts',(-4.97190814025518,1.79912594061044,376.736404614825));
#51660=CARTESIAN_POINT('Ctrl Pts',(-3.51189274247934,3.95263634434836,376.657276739365));
#51661=CARTESIAN_POINT('Ctrl Pts',(-1.20153141562281,5.1490821475793,376.578148863906));
#51662=CARTESIAN_POINT('Ctrl Pts',(1.39976059245402,5.09876406487689,376.499020988446));
#51663=CARTESIAN_POINT('Ctrl Pts',(3.66212404867255,3.81386577598244,376.419893112986));
#51664=CARTESIAN_POINT('Ctrl Pts',(5.03776558457334,1.60550385251465,376.340765237526));
#51665=CARTESIAN_POINT('Ctrl Pts',(5.19359667332446,-0.99160390296118,376.261637362067));
#51666=CARTESIAN_POINT('Ctrl Pts',(4.09188543028651,-3.34861140308599,376.182509486607));
#51667=CARTESIAN_POINT('Ctrl Pts',(1.99939275591558,-4.89480881330613,376.103381611147));
#51668=CARTESIAN_POINT('Ctrl Pts',(-0.577219342064538,-5.2558103583336,
376.024253735687));
#51669=CARTESIAN_POINT('Ctrl Pts',(-3.01406745721832,-4.34420557675964,
375.945125860227));
#51670=CARTESIAN_POINT('Ctrl Pts',(-4.72110968654987,-2.38072426020005,
375.865997984768));
#51671=CARTESIAN_POINT('Ctrl Pts',(-5.28501438473626,0.159209483211192,
375.786870109308));
#51672=CARTESIAN_POINT('Ctrl Pts',(-4.56924148341307,2.66059337382158,375.707742233848));
#51673=CARTESIAN_POINT('Ctrl Pts',(-2.74710339271414,4.51775908713646,375.628614358388));
#51674=CARTESIAN_POINT('Ctrl Pts',(-0.25980027835232,5.28102544478076,375.549486482929));
#51675=CARTESIAN_POINT('Ctrl Pts',(2.29040909674433,4.76557955369675,375.470358607468));
#51676=CARTESIAN_POINT('Ctrl Pts',(4.28603436317887,3.09622956904483,375.391230732009));
#51677=CARTESIAN_POINT('Ctrl Pts',(5.24386820297344,0.677177255244125,375.312102856549));
#51678=CARTESIAN_POINT('Ctrl Pts',(4.93198748823577,-1.90583737857549,375.232974981089));
#51679=CARTESIAN_POINT('Ctrl Pts',(3.42590832840442,-4.02739560248487,375.153847105629));
#51680=CARTESIAN_POINT('Ctrl Pts',(1.09030376033057,-5.1737660638094,375.07471923017));
#51681=CARTESIAN_POINT('Ctrl Pts',(-1.50930126232148,-5.06744133910014,
374.99559135471));
#51682=CARTESIAN_POINT('Ctrl Pts',(-3.74345011231245,-3.7340250124542,374.91646347925));
#51683=CARTESIAN_POINT('Ctrl Pts',(-5.07118953303831,-1.49668421879837,
374.83733560379));
#51684=CARTESIAN_POINT('Ctrl Pts',(-5.17098566641861,1.10346413672945,374.758207728331));
#51685=CARTESIAN_POINT('Ctrl Pts',(-4.40267566674078,2.65797789149901,374.705455811358));
#51686=CARTESIAN_POINT('Ctrl Pts',(-3.85627053850387,3.29705846079003,374.679079852871));
#51687=CARTESIAN_POINT('Ctrl Pts',(-1.2650852794265,-4.72177922709115,400.106973382376));
#51688=CARTESIAN_POINT('Ctrl Pts',(-2.04760230627562,-4.51212292510067,
400.08059742389));
#51689=CARTESIAN_POINT('Ctrl Pts',(-3.50558628380115,-3.69634492177698,
400.027845506916));
#51690=CARTESIAN_POINT('Ctrl Pts',(-4.84423972345866,-1.57661725067267,
399.948717631457));
#51691=CARTESIAN_POINT('Ctrl Pts',(-5.0096862523777,0.92455742070055,399.869589755997));
#51692=CARTESIAN_POINT('Ctrl Pts',(-3.9622375540088,3.20202818303723,399.790461880537));
#51693=CARTESIAN_POINT('Ctrl Pts',(-1.95534398901843,4.70410781476347,399.711334005077));
#51694=CARTESIAN_POINT('Ctrl Pts',(0.524977181208032,5.06720185162811,399.632206129618));
#51695=CARTESIAN_POINT('Ctrl Pts',(2.87819629981243,4.2033413524507,399.553078254158));
#51696=CARTESIAN_POINT('Ctrl Pts',(4.53450261129871,2.32172008778426,399.473950378698));
#51697=CARTESIAN_POINT('Ctrl Pts',(5.09285792630992,-0.122070466194823,
399.394822503238));
#51698=CARTESIAN_POINT('Ctrl Pts',(4.41806180230403,-2.5363019515078,399.315694627778));
#51699=CARTESIAN_POINT('Ctrl Pts',(2.67350672576957,-4.3364112842173,399.236566752319));
#51700=CARTESIAN_POINT('Ctrl Pts',(0.281606541856066,-5.08653095966945,
399.157438876859));
#51701=CARTESIAN_POINT('Ctrl Pts',(-2.17847980551824,-4.60503265524259,
399.078311001399));
#51702=CARTESIAN_POINT('Ctrl Pts',(-4.1110838687323,-3.00850283765647,398.999183125939));
#51703=CARTESIAN_POINT('Ctrl Pts',(-5.04825788999868,-0.683514555327269,
398.920055250479));
#51704=CARTESIAN_POINT('Ctrl Pts',(-4.76308094287924,1.80697533276996,398.84092737502));
#51705=CARTESIAN_POINT('Ctrl Pts',(-3.32460382095413,3.85993643987858,398.76179949956));
#51706=CARTESIAN_POINT('Ctrl Pts',(-1.08112964449127,4.97827867803806,398.6826716241));
#51707=CARTESIAN_POINT('Ctrl Pts',(1.4241219451236,4.89121422375072,398.603543748641));
#51708=CARTESIAN_POINT('Ctrl Pts',(3.58454628917626,3.6198242774857,398.52441587318));
#51709=CARTESIAN_POINT('Ctrl Pts',(4.87703286664207,1.4719545906142,398.445287997721));
#51710=CARTESIAN_POINT('Ctrl Pts',(4.98862772878014,-1.03232421377308,398.366160122261));
#51711=CARTESIAN_POINT('Ctrl Pts',(3.89231005153748,-3.28664302317114,398.287032246801));
#51712=CARTESIAN_POINT('Ctrl Pts',(1.853534773828,-4.7451563452711,398.207904371342));
#51713=CARTESIAN_POINT('Ctrl Pts',(-0.634042863421179,-5.05470964015625,
398.128776495882));
#51714=CARTESIAN_POINT('Ctrl Pts',(-2.96809765493441,-4.14034976900372,
398.049648620422));
#51715=CARTESIAN_POINT('Ctrl Pts',(-4.58347737773795,-2.22347363975469,
397.970520744962));
#51716=CARTESIAN_POINT('Ctrl Pts',(-5.08904492375008,0.231779341134317,
397.891392869503));
#51717=CARTESIAN_POINT('Ctrl Pts',(-4.36238559065476,2.6309108417746,397.812264994043));
#51718=CARTESIAN_POINT('Ctrl Pts',(-2.57944774904339,4.39301140550268,397.733137118583));
#51719=CARTESIAN_POINT('Ctrl Pts',(-0.171939895328258,5.09141793327901,
397.654009243123));
#51720=CARTESIAN_POINT('Ctrl Pts',(2.27720032040928,4.55702299748958,397.574881367663));
#51721=CARTESIAN_POINT('Ctrl Pts',(4.17495466984747,2.91922136941339,397.495753492203));
#51722=CARTESIAN_POINT('Ctrl Pts',(5.06181376480896,0.574579245458329,397.416625616744));
#51723=CARTESIAN_POINT('Ctrl Pts',(4.72303954910339,-1.90918760642483,397.337497741284));
#51724=CARTESIAN_POINT('Ctrl Pts',(3.24066051742776,-3.93067669870034,397.258369865824));
#51725=CARTESIAN_POINT('Ctrl Pts',(0.973609891088484,-5.00041835038785,
397.179241990364));
#51726=CARTESIAN_POINT('Ctrl Pts',(-1.52918404181197,-4.85939256133815,
397.100114114905));
#51727=CARTESIAN_POINT('Ctrl Pts',(-3.66171170517574,-3.54174636120374,
397.020986239445));
#51728=CARTESIAN_POINT('Ctrl Pts',(-4.90761729027895,-1.36652567889375,
396.941858363985));
#51729=CARTESIAN_POINT('Ctrl Pts',(-4.965225654969,1.13957627834147,396.862730488525));
#51730=CARTESIAN_POINT('Ctrl Pts',(-3.82058789989522,3.3697489517908,396.783602613066));
#51731=CARTESIAN_POINT('Ctrl Pts',(-1.7508588605474,4.78399343115808,396.704474737606));
#51732=CARTESIAN_POINT('Ctrl Pts',(0.742811287950349,5.03987413428296,396.625346862146));
#51733=CARTESIAN_POINT('Ctrl Pts',(3.05662214087683,4.07543384031964,396.546218986686));
#51734=CARTESIAN_POINT('Ctrl Pts',(4.63032320548468,2.12419559167018,396.467091111227));
#51735=CARTESIAN_POINT('Ctrl Pts',(5.08286916176923,-0.341380994281065,
396.387963235767));
#51736=CARTESIAN_POINT('Ctrl Pts',(4.30468359613617,-2.72429789782194,396.308835360307));
#51737=CARTESIAN_POINT('Ctrl Pts',(2.48419109223004,-4.44757175503734,396.229707484847));
#51738=CARTESIAN_POINT('Ctrl Pts',(0.0621933781031742,-5.09394070270169,
396.150579609387));
#51739=CARTESIAN_POINT('Ctrl Pts',(-2.37486341947636,-4.50689734049423,
396.071451733928));
#51740=CARTESIAN_POINT('Ctrl Pts',(-4.23688686924074,-2.82858437317615,
395.992323858468));
#51741=CARTESIAN_POINT('Ctrl Pts',(-5.07301922112011,-0.46537713853058,
395.913195983008));
#51742=CARTESIAN_POINT('Ctrl Pts',(-4.68080504901513,2.01051336529637,395.834068107548));
#51743=CARTESIAN_POINT('Ctrl Pts',(-3.15521243681498,3.99959177635531,395.754940232089));
#51744=CARTESIAN_POINT('Ctrl Pts',(-0.865638049608238,5.0202361165578,395.675812356629));
#51745=CARTESIAN_POINT('Ctrl Pts',(1.63353607355812,4.82531447631191,395.596684481169));
#51746=CARTESIAN_POINT('Ctrl Pts',(3.73717683280492,3.46202386174144,395.517556605709));
#51747=CARTESIAN_POINT('Ctrl Pts',(4.93592289877338,1.26046223120153,395.43842873025));
#51748=CARTESIAN_POINT('Ctrl Pts',(4.93951801594962,-1.24629918921186,395.35930085479));
#51749=CARTESIAN_POINT('Ctrl Pts',(3.74709168700367,-3.45129016283895,395.28017297933));
#51750=CARTESIAN_POINT('Ctrl Pts',(1.64736994911874,-4.82060910566927,395.20104510387));
#51751=CARTESIAN_POINT('Ctrl Pts',(-0.851234793642623,-5.0226984007616,
395.12191722841));
#51752=CARTESIAN_POINT('Ctrl Pts',(-3.14372730731715,-4.00862551458096,
395.04278935295));
#51753=CARTESIAN_POINT('Ctrl Pts',(-4.67501897747406,-2.02393118933878,
394.963661477491));
#51754=CARTESIAN_POINT('Ctrl Pts',(-5.07433320772034,0.450824129730827,
394.884533602031));
#51755=CARTESIAN_POINT('Ctrl Pts',(-4.24498275416411,2.81641994662909,394.805405726571));
#51756=CARTESIAN_POINT('Ctrl Pts',(-2.38778091996604,4.50006690807671,394.726277851111));
#51757=CARTESIAN_POINT('Ctrl Pts',(0.0475820181493076,5.09409813906934,
394.647149975652));
#51758=CARTESIAN_POINT('Ctrl Pts',(2.47142376857538,4.45467893961412,394.568022100192));
#51759=CARTESIAN_POINT('Ctrl Pts',(4.29685170208089,2.73663394505832,394.488894224732));
#51760=CARTESIAN_POINT('Ctrl Pts',(5.08186905910887,0.355958937228547,394.409766349272));
#51761=CARTESIAN_POINT('Ctrl Pts',(4.63639705230557,-2.11090555740732,394.330638473812));
#51762=CARTESIAN_POINT('Ctrl Pts',(3.06829925703676,-4.06664967364888,394.251510598353));
#51763=CARTESIAN_POINT('Ctrl Pts',(0.757264255609957,-5.037722773843,394.172382722893));
#51764=CARTESIAN_POINT('Ctrl Pts',(-1.73712958511388,-4.78899579279863,
394.093254847433));
#51765=CARTESIAN_POINT('Ctrl Pts',(-3.81090663047816,-3.38069379753602,
394.014126971973));
#51766=CARTESIAN_POINT('Ctrl Pts',(-4.96193654859164,-1.15381349735189,
393.934999096513));
#51767=CARTESIAN_POINT('Ctrl Pts',(-4.91151674888844,1.35244339042685,393.855871221054));
#51768=CARTESIAN_POINT('Ctrl Pts',(-3.67185554026823,3.53122879325631,393.776743345594));
#51769=CARTESIAN_POINT('Ctrl Pts',(-1.54311609384367,4.85498636659688,393.697615470134));
#51770=CARTESIAN_POINT('Ctrl Pts',(0.959263034860399,5.00319041501234,393.618487594674));
#51771=CARTESIAN_POINT('Ctrl Pts',(3.22937270762551,3.93995581373248,393.539359719215));
#51772=CARTESIAN_POINT('Ctrl Pts',(4.71754393956094,1.92272698978111,393.460231843755));
#51773=CARTESIAN_POINT('Ctrl Pts',(5.06344102520928,-0.560057928386485,
393.381103968295));
#51774=CARTESIAN_POINT('Ctrl Pts',(4.18331078637565,-2.90723421201562,393.301976092835));
#51775=CARTESIAN_POINT('Ctrl Pts',(2.29026199958981,-4.55047248889121,393.222848217376));
#51776=CARTESIAN_POINT('Ctrl Pts',(-0.157335320049481,-5.0918901692776,
393.143720341916));
#51777=CARTESIAN_POINT('Ctrl Pts',(-2.5668365306344,-4.40039204207098,393.064592466456));
#51778=CARTESIAN_POINT('Ctrl Pts',(-4.35482132414875,-2.6434127815497,392.985464590996));
#51779=CARTESIAN_POINT('Ctrl Pts',(-5.08835916941954,-0.24637544907113,
392.906336715536));
#51780=CARTESIAN_POINT('Ctrl Pts',(-4.58983617949401,2.21031756639828,392.827208840077));
#51781=CARTESIAN_POINT('Ctrl Pts',(-2.97996133557448,4.13181925275079,392.748080964617));
#51782=CARTESIAN_POINT('Ctrl Pts',(-0.648538831649752,5.05287020244567,
392.668953089157));
#51783=CARTESIAN_POINT('Ctrl Pts',(1.83991647361136,4.75045337510584,392.589825213697));
#51784=CARTESIAN_POINT('Ctrl Pts',(3.88286686231846,3.29779393359108,392.510697338238));
#51785=CARTESIAN_POINT('Ctrl Pts',(4.98564616049109,1.04662899888231,392.431569462778));
#51786=CARTESIAN_POINT('Ctrl Pts',(4.88123485596325,-1.45795959472489,392.352441587318));
#51787=CARTESIAN_POINT('Ctrl Pts',(3.59491439502781,-3.60952772414103,392.273313711858));
#51788=CARTESIAN_POINT('Ctrl Pts',(1.43814570421584,-4.88710925111834,392.194185836399));
#51789=CARTESIAN_POINT('Ctrl Pts',(-1.06684584950233,-4.98135923542166,
392.115057960939));
#51790=CARTESIAN_POINT('Ctrl Pts',(-3.31351857300444,-3.86945662403335,
392.035930085479));
#51791=CARTESIAN_POINT('Ctrl Pts',(-4.75787834559899,-1.82062998640609,
391.956802210019));
#51792=CARTESIAN_POINT('Ctrl Pts',(-5.05019767193907,0.669031668355122,
391.877674334559));
#51793=CARTESIAN_POINT('Ctrl Pts',(-4.11969632968522,2.99669852506039,391.7985464591));
#51794=CARTESIAN_POINT('Ctrl Pts',(-2.19167961327856,4.59876509202852,391.71941858364));
#51795=CARTESIAN_POINT('Ctrl Pts',(0.267015564477117,5.08731781858062,391.64029070818));
#51796=CARTESIAN_POINT('Ctrl Pts',(2.66105740145502,4.34406185557737,391.56116283272));
#51797=CARTESIAN_POINT('Ctrl Pts',(4.4107688176863,2.54896416919641,391.48203495726));
#51798=CARTESIAN_POINT('Ctrl Pts',(5.09248653841822,0.136677558326831,391.402907081801));
#51799=CARTESIAN_POINT('Ctrl Pts',(4.54114405077152,-2.30870323105058,391.323779206341));
#51800=CARTESIAN_POINT('Ctrl Pts',(2.89023969147757,-4.1950702526571,391.244651330881));
#51801=CARTESIAN_POINT('Ctrl Pts',(0.539512263560586,-5.06567136877124,
391.165523455421));
#51802=CARTESIAN_POINT('Ctrl Pts',(-1.94184901073189,-4.70970512011533,
391.086395579962));
#51803=CARTESIAN_POINT('Ctrl Pts',(-3.95302411413336,-3.21336276383497,
391.007267704502));
#51804=CARTESIAN_POINT('Ctrl Pts',(-5.00704072509175,-0.93895850610853,
390.928139829042));
#51805=CARTESIAN_POINT('Ctrl Pts',(-4.84868639834328,1.56279880645007,390.849011953582));
#51806=CARTESIAN_POINT('Ctrl Pts',(-3.51630397832454,3.68615059797345,390.769884078122));
#51807=CARTESIAN_POINT('Ctrl Pts',(-1.33250752244617,4.91696284321382,390.690756202663));
#51808=CARTESIAN_POINT('Ctrl Pts',(1.17393328229752,4.95721499913359,390.611628327203));
#51809=CARTESIAN_POINT('Ctrl Pts',(3.39612583095411,3.79716068125213,390.532500451743));
#51810=CARTESIAN_POINT('Ctrl Pts',(4.79600346661011,1.71768758718946,390.453372576283));
#51811=CARTESIAN_POINT('Ctrl Pts',(5.03460929736123,-0.777694748500222,
390.374244700824));
#51812=CARTESIAN_POINT('Ctrl Pts',(4.05416892298729,-3.08477134368254,390.295116825364));
#51813=CARTESIAN_POINT('Ctrl Pts',(2.09207953702197,-4.64492229318153,390.215988949904));
#51814=CARTESIAN_POINT('Ctrl Pts',(-0.376571822235509,-5.08038321011508,
390.136861074444));
#51815=CARTESIAN_POINT('Ctrl Pts',(-2.75404263028444,-4.28571453663178,
390.057733198984));
#51816=CARTESIAN_POINT('Ctrl Pts',(-4.46466820389571,-2.45333196450126,
389.978605323525));
#51817=CARTESIAN_POINT('Ctrl Pts',(-5.09424924959213,-0.0269162023862396,
389.899477448065));
#51818=CARTESIAN_POINT('Ctrl Pts',(-4.49034327596192,2.40601686672071,389.820349572605));
#51819=CARTESIAN_POINT('Ctrl Pts',(-2.79917598631673,4.25637330324171,389.741221697145));
#51820=CARTESIAN_POINT('Ctrl Pts',(-0.430235177009337,5.07612032869441,
389.662093821686));
#51821=CARTESIAN_POINT('Ctrl Pts',(2.04287986486846,4.66676994897283,389.582965946226));
#51822=CARTESIAN_POINT('Ctrl Pts',(4.02134580893056,3.12743949324644,389.503838070766));
#51823=CARTESIAN_POINT('Ctrl Pts',(5.02611030798847,0.830852015014124,389.424710195306));
#51824=CARTESIAN_POINT('Ctrl Pts',(4.81388648966003,-1.66691234430295,389.345582319847));
#51825=CARTESIAN_POINT('Ctrl Pts',(3.43606079231419,-3.76106183549833,389.266454444386));
#51826=CARTESIAN_POINT('Ctrl Pts',(1.22625060082997,-4.94453328059232,389.187326568927));
#51827=CARTESIAN_POINT('Ctrl Pts',(-1.28047560800195,-4.93076891734271,
389.108198693467));
#51828=CARTESIAN_POINT('Ctrl Pts',(-3.4771561234157,-3.72310155546604,389.029070818007));
#51829=CARTESIAN_POINT('Ctrl Pts',(-4.8319015994811,-1.61394759265993,388.949942942547));
#51830=CARTESIAN_POINT('Ctrl Pts',(-5.01668313982022,0.88599671193773,388.870815067088));
#51831=CARTESIAN_POINT('Ctrl Pts',(-3.98675899344041,3.17141177193107,388.791687191628));
#51832=CARTESIAN_POINT('Ctrl Pts',(-1.99150801936634,4.68892265960108,388.712559316169));
#51833=CARTESIAN_POINT('Ctrl Pts',(0.485953221700427,5.07108956391423,388.633431440708));
#51834=CARTESIAN_POINT('Ctrl Pts',(2.84574904013097,4.2253771783729,388.554303565249));
#51835=CARTESIAN_POINT('Ctrl Pts',(4.51649445500228,2.35656057355938,388.475175689789));
#51836=CARTESIAN_POINT('Ctrl Pts',(5.09364648443963,-0.0828576518904476,
388.396047814329));
#51837=CARTESIAN_POINT('Ctrl Pts',(4.43745744402291,-2.50221328655385,388.316919938869));
#51838=CARTESIAN_POINT('Ctrl Pts',(2.70681250483858,-4.31569993889408,388.23779206341));
#51839=CARTESIAN_POINT('Ctrl Pts',(0.320758313989414,-5.08421223031922,
388.15866418795));
#51840=CARTESIAN_POINT('Ctrl Pts',(-2.14296212310374,-4.62166779830222,
388.07953631249));
#51841=CARTESIAN_POINT('Ctrl Pts',(-4.08780022204497,-3.04006401964993,
388.00040843703));
#51842=CARTESIAN_POINT('Ctrl Pts',(-5.04284605436382,-0.722359724035205,
387.921280561571));
#51843=CARTESIAN_POINT('Ctrl Pts',(-4.7768512889894,1.77025186394512,387.842152686111));
#51844=CARTESIAN_POINT('Ctrl Pts',(-3.35422209731677,3.83422665224591,387.763024810651));
#51845=CARTESIAN_POINT('Ctrl Pts',(-1.11942427896961,4.96980776112863,387.683896935191));
#51846=CARTESIAN_POINT('Ctrl Pts',(1.38642335448793,4.90203327008818,387.604769059731));
#51847=CARTESIAN_POINT('Ctrl Pts',(3.55657182458215,3.64731363547327,387.525641184271));
#51848=CARTESIAN_POINT('Ctrl Pts',(4.86555607518393,1.50945817370396,387.446513308812));
#51849=CARTESIAN_POINT('Ctrl Pts',(4.99642752319251,-0.993887269465375,
387.367385433352));
#51850=CARTESIAN_POINT('Ctrl Pts',(3.9174978423384,-3.25657957897469,387.288257557892));
#51851=CARTESIAN_POINT('Ctrl Pts',(1.89001175993966,-4.73074576004784,387.209129682432));
#51852=CARTESIAN_POINT('Ctrl Pts',(-0.595108972441489,-5.05944119541285,
387.130001806973));
#51853=CARTESIAN_POINT('Ctrl Pts',(-2.93613404781291,-4.1630777979993,387.050873931513));
#51854=CARTESIAN_POINT('Ctrl Pts',(-4.5662235058762,-2.2586949314382,386.971746056053));
#51855=CARTESIAN_POINT('Ctrl Pts',(-5.09067852285014,0.192593031839733,
386.892618180593));
#51856=CARTESIAN_POINT('Ctrl Pts',(-4.38251111209279,2.59724782246595,386.813490305134));
#51857=CARTESIAN_POINT('Ctrl Pts',(-2.61319213533106,4.37302261173721,386.734362429674));
#51858=CARTESIAN_POINT('Ctrl Pts',(-0.211132509258637,5.08994331623203,
386.655234554214));
#51859=CARTESIAN_POINT('Ctrl Pts',(2.24204931299394,4.57441961094785,386.576106678754));
#51860=CARTESIAN_POINT('Ctrl Pts',(4.15235649586965,2.95127691518944,386.496978803295));
#51861=CARTESIAN_POINT('Ctrl Pts',(5.05724019309986,0.613532010751077,386.417850927834));
#51862=CARTESIAN_POINT('Ctrl Pts',(4.73759799334825,-1.872769380448,386.338723052375));
#51863=CARTESIAN_POINT('Ctrl Pts',(3.27082589451466,-3.90561107468386,386.259595176915));
#51864=CARTESIAN_POINT('Ctrl Pts',(1.01207816086419,-4.99277454880777,386.180467301455));
#51865=CARTESIAN_POINT('Ctrl Pts',(-1.49172732571618,-4.87102140055169,
386.101339425996));
#51866=CARTESIAN_POINT('Ctrl Pts',(-3.63433605836998,-3.56983211282445,
386.022211550536));
#51867=CARTESIAN_POINT('Ctrl Pts',(-4.89695126651592,-1.40426784919727,
385.943083675076));
#51868=CARTESIAN_POINT('Ctrl Pts',(-4.97385185302132,1.10131632291422,385.863955799616));
#51869=CARTESIAN_POINT('Ctrl Pts',(-3.84641763057586,3.34023521778273,385.784827924157));
#51870=CARTESIAN_POINT('Ctrl Pts',(-1.78763788776658,4.77037217427974,385.705700048697));
#51871=CARTESIAN_POINT('Ctrl Pts',(0.703988388806892,5.0454435134432,385.626572173237));
#51872=CARTESIAN_POINT('Ctrl Pts',(3.02515568373168,4.09884532375971,385.547444297777));
#51873=CARTESIAN_POINT('Ctrl Pts',(4.61383226520657,2.15978048131279,385.468316422317));
#51874=CARTESIAN_POINT('Ctrl Pts',(5.08534674297434,-0.302238982663029,
385.389188546858));
#51875=CARTESIAN_POINT('Ctrl Pts',(4.32552979408761,-2.69107634588493,385.310060671397));
#51876=CARTESIAN_POINT('Ctrl Pts',(2.51835834970871,-4.42831470441898,385.230932795938));
#51877=CARTESIAN_POINT('Ctrl Pts',(0.10140866673516,-5.09331092524616,385.151804920478));
#51878=CARTESIAN_POINT('Ctrl Pts',(-2.34009542414748,-4.5250473262503,385.072677045019));
#51879=CARTESIAN_POINT('Ctrl Pts',(-4.21498465418432,-2.86111940748926,
384.993549169558));
#51880=CARTESIAN_POINT('Ctrl Pts',(-5.06928604038651,-0.504419408492031,
384.914421294099));
#51881=CARTESIAN_POINT('Ctrl Pts',(-4.69614482970923,1.97441729057362,384.835293418639));
#51882=CARTESIAN_POINT('Ctrl Pts',(-3.18591090830761,3.97518195599239,384.756165543179));
#51883=CARTESIAN_POINT('Ctrl Pts',(-0.904262091876385,5.01342297917464,
384.677037667719));
#51884=CARTESIAN_POINT('Ctrl Pts',(1.59633862457976,4.83774770886161,384.59790979226));
#51885=CARTESIAN_POINT('Ctrl Pts',(3.71041271554213,3.4906929654818,384.5187819168));
#51886=CARTESIAN_POINT('Ctrl Pts',(4.92607259535609,1.29842546347592,384.43965404134));
#51887=CARTESIAN_POINT('Ctrl Pts',(4.94896661214932,-1.20823398841131,384.360526165881));
#51888=CARTESIAN_POINT('Ctrl Pts',(3.77355136371449,-3.42233984348858,384.281398290421));
#51889=CARTESIAN_POINT('Ctrl Pts',(1.6844339393846,-4.80778350206934,384.202270414961));
#51890=CARTESIAN_POINT('Ctrl Pts',(-0.812540913458525,-5.02910301772363,
384.123142539501));
#51891=CARTESIAN_POINT('Ctrl Pts',(-3.11277261136022,-4.03270958152043,
384.044014664041));
#51892=CARTESIAN_POINT('Ctrl Pts',(-4.65929862622416,-2.05986315336399,
383.964886788582));
#51893=CARTESIAN_POINT('Ctrl Pts',(-5.07765362058409,0.411744591087888,
383.885758913121));
#51894=CARTESIAN_POINT('Ctrl Pts',(-4.26653994885377,2.78365528824167,383.806631037662));
#51895=CARTESIAN_POINT('Ctrl Pts',(-2.42235518332661,4.48155054247207,383.727503162202));
#51896=CARTESIAN_POINT('Ctrl Pts',(0.00836226414014005,5.09431349363773,
383.648375286742));
#51897=CARTESIAN_POINT('Ctrl Pts',(2.43705492959019,4.47357386985853,383.569247411283));
#51898=CARTESIAN_POINT('Ctrl Pts',(4.27565561607469,2.76963336050998,383.490119535823));
#51899=CARTESIAN_POINT('Ctrl Pts',(5.07897800282517,0.39507258287429,383.410991660363));
#51900=CARTESIAN_POINT('Ctrl Pts',(4.65251104653713,-2.07514839487948,383.331863784903));
#51901=CARTESIAN_POINT('Ctrl Pts',(3.09951656833074,-4.04290699145606,383.252735909444));
#51902=CARTESIAN_POINT('Ctrl Pts',(0.79602613558697,-5.03174346428585,383.173608033984));
#51903=CARTESIAN_POINT('Ctrl Pts',(-1.70020867560859,-4.80222764540647,
383.094480158524));
#51904=CARTESIAN_POINT('Ctrl Pts',(-3.78476647047488,-3.40993294111337,
383.015352283064));
#51905=CARTESIAN_POINT('Ctrl Pts',(-4.9529065394344,-1.1919801636558,382.936224407604));
#51906=CARTESIAN_POINT('Ctrl Pts',(-4.92178335585094,1.31459061954267,382.857096532145));
#51907=CARTESIAN_POINT('Ctrl Pts',(-3.6989328766574,3.50285533142662,382.777968656685));
#51908=CARTESIAN_POINT('Ctrl Pts',(-1.58044783677119,4.84296237174792,382.698840781225));
#51909=CARTESIAN_POINT('Ctrl Pts',(0.920716140847871,5.01042729584046,382.619712905765));
#51910=CARTESIAN_POINT('Ctrl Pts',(3.19894414643704,3.96470128091602,382.540585030306));
#51911=CARTESIAN_POINT('Ctrl Pts',(4.70260147696606,1.95898934345174,382.461457154846));
#51912=CARTESIAN_POINT('Ctrl Pts',(5.06760272792295,-0.521059009008414,
382.382329279386));
#51913=CARTESIAN_POINT('Ctrl Pts',(4.20556896788232,-2.87494166120048,382.303201403926));
#51914=CARTESIAN_POINT('Ctrl Pts',(2.32522721453312,-4.53270540623539,382.224073528466));
#51915=CARTESIAN_POINT('Ctrl Pts',(-0.118129312060885,-5.0929505558716,
382.144945653006));
#51916=CARTESIAN_POINT('Ctrl Pts',(-2.53288280690479,-4.42002314308501,
382.065817777547));
#51917=CARTESIAN_POINT('Ctrl Pts',(-4.33434120943595,-2.67686125510947,
381.986689902087));
#51918=CARTESIAN_POINT('Ctrl Pts',(-5.08631158002599,-0.285542308273818,
381.907562026627));
#51919=CARTESIAN_POINT('Ctrl Pts',(-4.60671690485093,2.17491591963496,381.828434151168));
#51920=CARTESIAN_POINT('Ctrl Pts',(-3.01168299114604,4.10875473346396,381.749306275708));
#51921=CARTESIAN_POINT('Ctrl Pts',(-0.687420550548197,5.04772749716196,
381.670178400248));
#51922=CARTESIAN_POINT('Ctrl Pts',(1.80328924752583,4.76447770366057,381.591050524788));
#51923=CARTESIAN_POINT('Ctrl Pts',(3.85736279756143,3.32758954002893,381.511922649328));
#51924=CARTESIAN_POINT('Ctrl Pts',(4.97744063861076,1.0849813768112,381.432794773869));
#51925=CARTESIAN_POINT('Ctrl Pts',(4.89231470646681,-1.42033683040663,381.353666898409));
#51926=CARTESIAN_POINT('Ctrl Pts',(3.62259681793774,-3.58174429483572,381.274539022949));
#51927=CARTESIAN_POINT('Ctrl Pts',(1.47572786509085,-4.87589244827193,381.195411147489));
#51928=CARTESIAN_POINT('Ctrl Pts',(-1.02846384062172,-4.98942501972467,
381.11628327203));
#51929=CARTESIAN_POINT('Ctrl Pts',(-3.28363027585792,-3.89485200108939,
381.03715539657));
#51930=CARTESIAN_POINT('Ctrl Pts',(-4.74372071007927,-1.85720589157097,
380.95802752111));
#51931=CARTESIAN_POINT('Ctrl Pts',(-5.05519873204731,0.630131477096863,
380.87889964565));
#51932=CARTESIAN_POINT('Ctrl Pts',(-4.14264516258972,2.96489307662063,380.79977177019));
#51933=CARTESIAN_POINT('Ctrl Pts',(-2.22701954397005,4.58175554233269,380.720643894731));
#51934=CARTESIAN_POINT('Ctrl Pts',(0.227841507524015,5.08922274481773,380.641516019271));
#51935=CARTESIAN_POINT('Ctrl Pts',(2.6275345591372,4.36442001180692,380.562388143811));
#51936=CARTESIAN_POINT('Ctrl Pts',(4.39101418405409,2.58284616931722,380.483260268351));
#51937=CARTESIAN_POINT('Ctrl Pts',(5.09128336669755,0.175879444250141,380.404132392892));
#51938=CARTESIAN_POINT('Ctrl Pts',(4.55878366881602,-2.27367353854006,380.325004517432));
#51939=CARTESIAN_POINT('Ctrl Pts',(2.92245096161458,-4.17269460611234,380.245876641972));
#51940=CARTESIAN_POINT('Ctrl Pts',(0.578495766946718,-5.0613676557375,380.166748766512));
#51941=CARTESIAN_POINT('Ctrl Pts',(-1.90553247564304,-4.72451541252546,
380.087620891052));
#51942=CARTESIAN_POINT('Ctrl Pts',(-3.92816798724318,-3.24370099776764,
380.008493015593));
#51943=CARTESIAN_POINT('Ctrl Pts',(-4.99966350066068,-0.977478787024238,
379.929365140133));
#51944=CARTESIAN_POINT('Ctrl Pts',(-4.86057434754265,1.52542351854533,379.850237264673));
#51945=CARTESIAN_POINT('Ctrl Pts',(-3.54457863363044,3.65897010221885,379.771109389213));
#51946=CARTESIAN_POINT('Ctrl Pts',(-1.37032265027505,4.90655844080798,379.691981513754));
#51947=CARTESIAN_POINT('Ctrl Pts',(1.13573398094598,4.96610594162524,379.612853638294));
#51948=CARTESIAN_POINT('Ctrl Pts',(3.36679167625567,3.82319417602828,379.533725762834));
#51949=CARTESIAN_POINT('Ctrl Pts',(4.78263723215717,1.75456006010191,379.454597887374));
#51950=CARTESIAN_POINT('Ctrl Pts',(5.04044739265935,-0.738911348373108,
379.375470011914));
#51951=CARTESIAN_POINT('Ctrl Pts',(4.07779775117163,-3.05346776623899,379.296342136454));
#51952=CARTESIAN_POINT('Ctrl Pts',(2.1277777736305,-4.62867817470224,379.217214260995));
#51953=CARTESIAN_POINT('Ctrl Pts',(-0.337447906496721,-5.0831317914571,
379.138086385535));
#51954=CARTESIAN_POINT('Ctrl Pts',(-2.72096623545812,-4.30679029492008,
379.058958510076));
#51955=CARTESIAN_POINT('Ctrl Pts',(-4.44564822425965,-2.48763175833121,
378.979830634615));
#51956=CARTESIAN_POINT('Ctrl Pts',(-5.09389105422811,-0.0661349119291711,
378.900702759156));
#51957=CARTESIAN_POINT('Ctrl Pts',(-4.50873359586993,2.37137539423742,378.821574883696));
#51958=CARTESIAN_POINT('Ctrl Pts',(-2.83186191395806,4.23469691940223,378.742447008236));
#51959=CARTESIAN_POINT('Ctrl Pts',(-0.469302363186489,5.07265760630743,
378.663319132776));
#51960=CARTESIAN_POINT('Ctrl Pts',(2.00689088408632,4.68235932819045,378.584191257317));
#51961=CARTESIAN_POINT('Ctrl Pts',(3.99714916166288,3.15830626734308,378.505063381856));
#51962=CARTESIAN_POINT('Ctrl Pts',(5.01956480656533,0.869522312313901,378.425935506397));
#51963=CARTESIAN_POINT('Ctrl Pts',(4.82657701747544,-1.62980188774553,378.346807630937));
#51964=CARTESIAN_POINT('Ctrl Pts',(3.46491455089248,-3.73449689435332,378.267679755478));
#51965=CARTESIAN_POINT('Ctrl Pts',(1.26428113644233,-4.93494610983311,378.188551880018));
#51966=CARTESIAN_POINT('Ctrl Pts',(-1.24247675173787,-4.94048088958068,
378.109424004558));
#51967=CARTESIAN_POINT('Ctrl Pts',(-3.4483897322594,-3.74976107950479,378.030296129098));
#51968=CARTESIAN_POINT('Ctrl Pts',(-4.81933297260539,-1.65109951186456,
377.951168253638));
#51969=CARTESIAN_POINT('Ctrl Pts',(-5.02335555943258,0.847348111721862,
377.872040378178));
#51970=CARTESIAN_POINT('Ctrl Pts',(-4.01105684503597,3.1406246010644,377.792912502719));
#51971=CARTESIAN_POINT('Ctrl Pts',(-2.02754798568437,4.67345151517251,377.713784627259));
#51972=CARTESIAN_POINT('Ctrl Pts',(0.44689761407191,5.07468052407812,377.634656751799));
#51973=CARTESIAN_POINT('Ctrl Pts',(2.81313445157142,4.24716075235008,377.555528876339));
#51974=CARTESIAN_POINT('Ctrl Pts',(4.49821796114695,2.39126223424701,377.47640100088));
#51975=CARTESIAN_POINT('Ctrl Pts',(5.09413343175754,-0.043640329640808,
377.39727312542));
#51976=CARTESIAN_POINT('Ctrl Pts',(4.4565899263877,-2.46797611960502,377.31814524996));
#51977=CARTESIAN_POINT('Ctrl Pts',(2.73995791251956,-4.29473288302567,377.2390173745));
#51978=CARTESIAN_POINT('Ctrl Pts',(0.35989104240352,-5.08159210646814,377.159889499041));
#51979=CARTESIAN_POINT('Ctrl Pts',(-2.10731740784078,-4.63802902551619,
377.080761623581));
#51980=CARTESIAN_POINT('Ctrl Pts',(-4.06427428993092,-3.07144500115654,
377.001633748121));
#51981=CARTESIAN_POINT('Ctrl Pts',(-5.03713531530297,-0.761162081456616,
376.922505872661));
#51982=CARTESIAN_POINT('Ctrl Pts',(-4.79033850266972,1.73342347069504,376.843377997201));
#51983=CARTESIAN_POINT('Ctrl Pts',(-3.38364156114149,3.8082896009442,376.764250121742));
#51984=CARTESIAN_POINT('Ctrl Pts',(-1.15765256317261,4.96104227374008,376.685122246282));
#51985=CARTESIAN_POINT('Ctrl Pts',(1.3486425877949,4.91256176240515,376.605994370822));
#51986=CARTESIAN_POINT('Ctrl Pts',(3.52838655442424,3.67458680959566,376.526866495362));
#51987=CARTESIAN_POINT('Ctrl Pts',(4.85379089203517,1.5468722880489,376.447738619903));
#51988=CARTESIAN_POINT('Ctrl Pts',(5.00393116882618,-0.955391415479512,
376.368610744443));
#51989=CARTESIAN_POINT('Ctrl Pts',(3.94245343483129,-3.22632311019696,376.289482868983));
#51990=CARTESIAN_POINT('Ctrl Pts',(1.92637672105698,-4.71605477417046,376.210354993523));
#51991=CARTESIAN_POINT('Ctrl Pts',(-0.556139808052753,-5.06387286571299,
376.131227118063));
#51992=CARTESIAN_POINT('Ctrl Pts',(-2.90399640996096,-4.18555907527208,
376.052099242604));
#51993=CARTESIAN_POINT('Ctrl Pts',(-4.54869898413812,-2.29378233993093,
375.972971367144));
#51994=CARTESIAN_POINT('Ctrl Pts',(-5.09201038719634,0.153395295307603,
375.893843491684));
#51995=CARTESIAN_POINT('Ctrl Pts',(-4.40237687192385,2.56343088388421,375.814715616224));
#51996=CARTESIAN_POINT('Ctrl Pts',(-2.64678163427568,4.35277456670489,375.735587740765));
#51997=CARTESIAN_POINT('Ctrl Pts',(-0.250312604595216,5.08816711975964,
375.656459865305));
#51998=CARTESIAN_POINT('Ctrl Pts',(2.2067654054518,4.59154485151799,375.577331989845));
#51999=CARTESIAN_POINT('Ctrl Pts',(4.12951222237333,2.98315803496294,375.498204114385));
#52000=CARTESIAN_POINT('Ctrl Pts',(5.05236682718355,0.652447347661906,375.419076238925));
#52001=CARTESIAN_POINT('Ctrl Pts',(4.75187571715042,-1.83623790240596,375.339948363465));
#52002=CARTESIAN_POINT('Ctrl Pts',(3.30079722094991,-3.88031871785061,375.260820488006));
#52003=CARTESIAN_POINT('Ctrl Pts',(1.05048684235124,-4.98482475543083,375.181692612546));
#52004=CARTESIAN_POINT('Ctrl Pts',(-1.45418293039009,-4.88238291455355,
375.102564737087));
#52005=CARTESIAN_POINT('Ctrl Pts',(-3.60674266297149,-3.59766175932869,
375.023436861626));
#52006=CARTESIAN_POINT('Ctrl Pts',(-4.8859942278021,-1.44202665000967,374.944308986167));
#52007=CARTESIAN_POINT('Ctrl Pts',(-4.98214589566551,1.06316661357685,374.865181110707));
#52008=CARTESIAN_POINT('Ctrl Pts',(-4.24189388987242,2.56091091663634,374.812429193734));
#52009=CARTESIAN_POINT('Ctrl Pts',(-3.71544298812364,3.17665283523617,374.786053235247));
#52010=CARTESIAN_POINT('Ctrl Pts',(-1.21713437249744,-4.54280821229883,
400.213946764753));
#52011=CARTESIAN_POINT('Ctrl Pts',(-1.96999142168732,-4.34109857602909,
400.187570806266));
#52012=CARTESIAN_POINT('Ctrl Pts',(-3.37271299505139,-3.55624125113577,
400.134818889293));
#52013=CARTESIAN_POINT('Ctrl Pts',(-4.66062705172882,-1.51685825396376,
400.055691013833));
#52014=CARTESIAN_POINT('Ctrl Pts',(-4.81980261122079,0.889513643374588,
399.976563138373));
#52015=CARTESIAN_POINT('Ctrl Pts',(-3.81205567514826,3.08066074806192,399.897435262913));
#52016=CARTESIAN_POINT('Ctrl Pts',(-1.8812299991108,4.52580660481483,399.818307387454));
#52017=CARTESIAN_POINT('Ctrl Pts',(0.505078813591743,4.87513817945551,399.739179511994));
#52018=CARTESIAN_POINT('Ctrl Pts',(2.76910316187124,4.04402084397575,399.660051636534));
#52019=CARTESIAN_POINT('Ctrl Pts',(4.36262999826625,2.23371923467566,399.580923761074));
#52020=CARTESIAN_POINT('Ctrl Pts',(4.89982180424067,-0.117443592687962,
399.501795885615));
#52021=CARTESIAN_POINT('Ctrl Pts',(4.25060268019241,-2.44016773763421,399.422668010155));
#52022=CARTESIAN_POINT('Ctrl Pts',(2.57217199816948,-4.17204698619159,399.343540134695));
#52023=CARTESIAN_POINT('Ctrl Pts',(0.270932724605363,-4.89373465051516,
399.264412259235));
#52024=CARTESIAN_POINT('Ctrl Pts',(-2.09590823180696,-4.43048672079232,
399.185284383776));
#52025=CARTESIAN_POINT('Ctrl Pts',(-3.95526022334416,-2.89447065191351,
399.106156508316));
#52026=CARTESIAN_POINT('Ctrl Pts',(-4.85691225648777,-0.657607098051338,
399.027028632856));
#52027=CARTESIAN_POINT('Ctrl Pts',(-4.58254445676102,1.73848500455744,398.947900757396));
#52028=CARTESIAN_POINT('Ctrl Pts',(-3.1985903647966,3.71363211084189,398.868772881936));
#52029=CARTESIAN_POINT('Ctrl Pts',(-1.0401512631882,4.78958548759503,398.789645006477));
#52030=CARTESIAN_POINT('Ctrl Pts',(1.37014302373642,4.70582106344184,398.710517131017));
#52031=CARTESIAN_POINT('Ctrl Pts',(3.44868015565118,3.48262099178473,398.631389255557));
#52032=CARTESIAN_POINT('Ctrl Pts',(4.69217722656672,1.41616265411303,398.552261380097));
#52033=CARTESIAN_POINT('Ctrl Pts',(4.79954227516165,-0.993195719354361,
398.473133504638));
#52034=CARTESIAN_POINT('Ctrl Pts',(3.74477865578454,-3.16206840652194,398.394005629178));
#52035=CARTESIAN_POINT('Ctrl Pts',(1.78327968915111,-4.56529926055421,398.314877753718));
#52036=CARTESIAN_POINT('Ctrl Pts',(-0.610010546527312,-4.8631194640233,
398.235749878258));
#52037=CARTESIAN_POINT('Ctrl Pts',(-2.85559695895555,-3.9834168494165,398.156622002799));
#52038=CARTESIAN_POINT('Ctrl Pts',(-4.40974845943849,-2.13919665124415,
398.077494127339));
#52039=CARTESIAN_POINT('Ctrl Pts',(-4.89615332706093,0.22299413922299,397.998366251879));
#52040=CARTESIAN_POINT('Ctrl Pts',(-4.19703678069868,2.53119063874627,397.919238376419));
#52041=CARTESIAN_POINT('Ctrl Pts',(-2.48167816706011,4.22650177609728,397.840110500959));
#52042=CARTESIAN_POINT('Ctrl Pts',(-0.165422805885864,4.89843639169769,
397.7609826255));
#52043=CARTESIAN_POINT('Ctrl Pts',(2.19088691340144,4.38429678750219,397.68185475004));
#52044=CARTESIAN_POINT('Ctrl Pts',(4.01671011032052,2.80857324594973,397.60272687458));
#52045=CARTESIAN_POINT('Ctrl Pts',(4.86995431890775,0.55280079591789,397.52359899912));
#52046=CARTESIAN_POINT('Ctrl Pts',(4.54402076394769,-1.83682309573565,397.444471123661));
#52047=CARTESIAN_POINT('Ctrl Pts',(3.11782878949058,-3.78169108040825,397.365343248201));
#52048=CARTESIAN_POINT('Ctrl Pts',(0.93670686325944,-4.81088599330085,397.286215372741));
#52049=CARTESIAN_POINT('Ctrl Pts',(-1.47122292025061,-4.67520554704762,
397.207087497281));
#52050=CARTESIAN_POINT('Ctrl Pts',(-3.52292074773491,-3.40750248619052,
397.127959621821));
#52051=CARTESIAN_POINT('Ctrl Pts',(-4.72160239961778,-1.31472984606697,
397.048831746362));
#52052=CARTESIAN_POINT('Ctrl Pts',(-4.77702721717586,1.09638257673893,396.969703870902));
#52053=CARTESIAN_POINT('Ctrl Pts',(-3.67577501037587,3.24202434619358,396.890575995442));
#52054=CARTESIAN_POINT('Ctrl Pts',(-1.68449553181902,4.60266429272193,396.811448119982));
#52055=CARTESIAN_POINT('Ctrl Pts',(0.714656288826095,4.84884627278046,396.732320244522));
#52056=CARTESIAN_POINT('Ctrl Pts',(2.94076607474594,3.92096144865504,396.653192369063));
#52057=CARTESIAN_POINT('Ctrl Pts',(4.45481867572026,2.0436815688041,396.574064493603));
#52058=CARTESIAN_POINT('Ctrl Pts',(4.89021164683945,-0.328441528025053,
396.494936618143));
#52059=CARTESIAN_POINT('Ctrl Pts',(4.14152188219155,-2.62103801718789,396.415808742683));
#52060=CARTESIAN_POINT('Ctrl Pts',(2.39003205189126,-4.27899410833295,396.336680867224));
#52061=CARTESIAN_POINT('Ctrl Pts',(0.0598360438320979,-4.90086353983399,
396.257552991764));
#52062=CARTESIAN_POINT('Ctrl Pts',(-2.28484825872123,-4.33607105832391,
396.178425116304));
#52063=CARTESIAN_POINT('Ctrl Pts',(-4.07629487497772,-2.72137169097608,
396.099297240844));
#52064=CARTESIAN_POINT('Ctrl Pts',(-4.88073505144618,-0.447737809214611,
396.020169365385));
#52065=CARTESIAN_POINT('Ctrl Pts',(-4.50338709078854,1.93430827396637,395.941041489924));
#52066=CARTESIAN_POINT('Ctrl Pts',(-3.03561947311557,3.84799404919722,395.861913614465));
#52067=CARTESIAN_POINT('Ctrl Pts',(-0.832827510883269,4.82995260073343,
395.782785739005));
#52068=CARTESIAN_POINT('Ctrl Pts',(1.57161966562715,4.64241913390311,395.703657863545));
#52069=CARTESIAN_POINT('Ctrl Pts',(3.5955254979886,3.3308017325457,395.624529988085));
#52070=CARTESIAN_POINT('Ctrl Pts',(4.74883513214048,1.21268655305647,395.545402112626));
#52071=CARTESIAN_POINT('Ctrl Pts',(4.75229398251168,-1.19906033709689,395.466274237166));
#52072=CARTESIAN_POINT('Ctrl Pts',(3.60506454649375,-3.32047487625331,395.387146361706));
#52073=CARTESIAN_POINT('Ctrl Pts',(1.5849291916516,-4.63789211233576,395.308018486247));
#52074=CARTESIAN_POINT('Ctrl Pts',(-0.818970185850148,-4.83232155624025,
395.228890610786));
#52075=CARTESIAN_POINT('Ctrl Pts',(-3.02456966792716,-3.85668537893236,
395.149762735327));
#52076=CARTESIAN_POINT('Ctrl Pts',(-4.49782033045318,-1.94721751819814,
395.070634859867));
#52077=CARTESIAN_POINT('Ctrl Pts',(-4.88199923361805,0.433736407473957,
394.991506984407));
#52078=CARTESIAN_POINT('Ctrl Pts',(-4.08408389914571,2.70966833633831,394.912379108948));
#52079=CARTESIAN_POINT('Ctrl Pts',(-2.29727614331402,4.32949952183574,394.833251233488));
#52080=CARTESIAN_POINT('Ctrl Pts',(0.04577850263863,4.90101500884376,394.754123358028));
#52081=CARTESIAN_POINT('Ctrl Pts',(2.37774865193587,4.28583190716024,394.674995482568));
#52082=CARTESIAN_POINT('Ctrl Pts',(4.13398684276656,2.63290648752449,394.595867607109));
#52083=CARTESIAN_POINT('Ctrl Pts',(4.8892494513703,0.34246691882695,394.516739731649));
#52084=CARTESIAN_POINT('Ctrl Pts',(4.46066230370267,-2.03089527069752,394.437611856189));
#52085=CARTESIAN_POINT('Ctrl Pts',(2.95200058966839,-3.91251023088926,394.358483980729));
#52086=CARTESIAN_POINT('Ctrl Pts',(0.728561441315958,-4.84677645600076,
394.279356105269));
#52087=CARTESIAN_POINT('Ctrl Pts',(-1.67128664123166,-4.60747704834829,
394.200228229809));
#52088=CARTESIAN_POINT('Ctrl Pts',(-3.66646069301835,-3.25255434616657,
394.12110035435));
#52089=CARTESIAN_POINT('Ctrl Pts',(-4.7738627787844,-1.11008015816539,394.04197247889));
#52090=CARTESIAN_POINT('Ctrl Pts',(-4.72535405587758,1.30118132280515,393.96284460343));
#52091=CARTESIAN_POINT('Ctrl Pts',(-3.53268009800228,3.39738356877675,393.88371672797));
#52092=CARTESIAN_POINT('Ctrl Pts',(-1.48462690153391,4.6709663616277,393.804588852511));
#52093=CARTESIAN_POINT('Ctrl Pts',(0.922903800227676,4.81355298752812,393.725460977051));
#52094=CARTESIAN_POINT('Ctrl Pts',(3.10696882493013,3.79061848635918,393.646333101591));
#52095=CARTESIAN_POINT('Ctrl Pts',(4.53873345614266,1.84984929178215,393.567205226131));
#52096=CARTESIAN_POINT('Ctrl Pts',(4.87151990076886,-0.538829884684078,
393.488077350672));
#52097=CARTESIAN_POINT('Ctrl Pts',(4.02474950245672,-2.79704044137549,393.408949475212));
#52098=CARTESIAN_POINT('Ctrl Pts',(2.2034535118369,-4.37799456479668,393.329821599752));
#52099=CARTESIAN_POINT('Ctrl Pts',(-0.151371792205916,-4.89889072839352,
393.250693724292));
#52100=CARTESIAN_POINT('Ctrl Pts',(-2.46954495544641,-4.23360266218321,
393.171565848832));
#52101=CARTESIAN_POINT('Ctrl Pts',(-4.18975922485567,-2.54321871374691,
393.092437973373));
#52102=CARTESIAN_POINT('Ctrl Pts',(-4.89549356508254,-0.23703700650118,
393.013310097913));
#52103=CARTESIAN_POINT('Ctrl Pts',(-4.41586624162366,2.12653923648359,392.934182222453));
#52104=CARTESIAN_POINT('Ctrl Pts',(-2.86701096694867,3.97520966788064,392.855054346993));
#52105=CARTESIAN_POINT('Ctrl Pts',(-0.623957069722673,4.86134974707218,
392.775926471534));
#52106=CARTESIAN_POINT('Ctrl Pts',(1.7701775674537,4.57039551547777,392.696798596074));
#52107=CARTESIAN_POINT('Ctrl Pts',(3.73569339459987,3.17279666063845,392.617670720614));
#52108=CARTESIAN_POINT('Ctrl Pts',(4.79667371815007,1.00695830590151,392.538542845154));
#52109=CARTESIAN_POINT('Ctrl Pts',(4.69621994662587,-1.40269811475204,392.459414969694));
#52110=CARTESIAN_POINT('Ctrl Pts',(3.45865527607574,-3.47271471179091,392.380287094234));
#52111=CARTESIAN_POINT('Ctrl Pts',(1.38363523608003,-4.70187168281881,392.301159218775));
#52112=CARTESIAN_POINT('Ctrl Pts',(-1.02640887116651,-4.79254928168782,
392.222031343315));
#52113=CARTESIAN_POINT('Ctrl Pts',(-3.18792528432602,-3.72279144860016,
392.142903467855));
#52114=CARTESIAN_POINT('Ctrl Pts',(-4.5775390550865,-1.75162210175979,392.063775592395));
#52115=CARTESIAN_POINT('Ctrl Pts',(-4.85877851429126,0.64367316028962,391.984647716936));
#52116=CARTESIAN_POINT('Ctrl Pts',(-3.96354624360545,2.88311376171958,391.905519841476));
#52117=CARTESIAN_POINT('Ctrl Pts',(-2.1086077232932,4.4244567189073,391.826391966016));
#52118=CARTESIAN_POINT('Ctrl Pts',(0.256894793419963,4.89449168487693,391.747264090557));
#52119=CARTESIAN_POINT('Ctrl Pts',(2.56019454432978,4.17940757564988,391.668136215096));
#52120=CARTESIAN_POINT('Ctrl Pts',(4.24358612375888,2.45235001548652,391.589008339637));
#52121=CARTESIAN_POINT('Ctrl Pts',(4.89946449317567,0.131497027824103,391.509880464177));
#52122=CARTESIAN_POINT('Ctrl Pts',(4.36901970526599,-2.22119575976841,391.430752588718));
#52123=CARTESIAN_POINT('Ctrl Pts',(2.78069006924853,-4.03606324615933,391.351624713257));
#52124=CARTESIAN_POINT('Ctrl Pts',(0.519062968356706,-4.87366570694958,
391.272496837798));
#52125=CARTESIAN_POINT('Ctrl Pts',(-1.86824652503536,-4.5311917538225,391.193368962338));
#52126=CARTESIAN_POINT('Ctrl Pts',(-3.80319145504887,-3.09156571084279,
391.114241086878));
#52127=CARTESIAN_POINT('Ctrl Pts',(-4.81725735814933,-0.903368880121367,
391.035113211418));
#52128=CARTESIAN_POINT('Ctrl Pts',(-4.66490518296109,1.50356357437869,390.955985335959));
#52129=CARTESIAN_POINT('Ctrl Pts',(-3.38302445358346,3.54643332584613,390.876857460499));
#52130=CARTESIAN_POINT('Ctrl Pts',(-1.28200109001022,4.73059372525567,390.797729585039));
#52131=CARTESIAN_POINT('Ctrl Pts',(1.12943733686538,4.76932019163214,390.718601709579));
#52132=CARTESIAN_POINT('Ctrl Pts',(3.2674014545917,3.65323576063024,390.639473834119));
#52133=CARTESIAN_POINT('Ctrl Pts',(4.61421910819667,1.65258155918805,390.56034595866));
#52134=CARTESIAN_POINT('Ctrl Pts',(4.84378099055226,-0.74821755110413,390.4812180832));
#52135=CARTESIAN_POINT('Ctrl Pts',(3.90050254186479,-2.96784832987165,390.40209020774));
#52136=CARTESIAN_POINT('Ctrl Pts',(2.01278281861149,-4.46886440981576,390.32296233228));
#52137=CARTESIAN_POINT('Ctrl Pts',(-0.362298507468694,-4.88781992095675,
390.243834456821));
#52138=CARTESIAN_POINT('Ctrl Pts',(-2.6496553261311,-4.12327181264112,390.164706581361));
#52139=CARTESIAN_POINT('Ctrl Pts',(-4.29544254536053,-2.36034258693993,
390.085578705901));
#52140=CARTESIAN_POINT('Ctrl Pts',(-4.90116039177906,-0.0258959894911138,
390.006450830441));
#52141=CARTESIAN_POINT('Ctrl Pts',(-4.32014444746653,2.31482088750723,389.927322954982));
#52142=CARTESIAN_POINT('Ctrl Pts',(-2.69307797902764,4.09504270882394,389.848195079522));
#52143=CARTESIAN_POINT('Ctrl Pts',(-0.41392784400509,4.88371861680963,389.769067204062));
#52144=CARTESIAN_POINT('Ctrl Pts',(1.96544797639375,4.48988396735431,389.689939328602));
#52145=CARTESIAN_POINT('Ctrl Pts',(3.86892353214857,3.00889921576025,389.610811453142));
#52146=CARTESIAN_POINT('Ctrl Pts',(4.83560414092378,0.799359981795764,389.531683577683));
#52147=CARTESIAN_POINT('Ctrl Pts',(4.63142430565821,-1.60373086556754,389.452555702223));
#52148=CARTESIAN_POINT('Ctrl Pts',(3.30582274912905,-3.61850518025834,389.373427826763));
#52149=CARTESIAN_POINT('Ctrl Pts',(1.17977165637593,-4.75711915207383,389.294299951303));
#52150=CARTESIAN_POINT('Ctrl Pts',(-1.23194135683111,-4.74387650361441,
389.215172075843));
#52151=CARTESIAN_POINT('Ctrl Pts',(-3.34536043156536,-3.58198372010992,
389.136044200384));
#52152=CARTESIAN_POINT('Ctrl Pts',(-4.64875658336638,-1.55277365279788,
389.056916324924));
#52153=CARTESIAN_POINT('Ctrl Pts',(-4.82653429353919,0.852414512725966,
388.977788449464));
#52154=CARTESIAN_POINT('Ctrl Pts',(-3.83564767110356,3.05120479997222,388.898660574004));
#52155=CARTESIAN_POINT('Ctrl Pts',(-1.91602329336559,4.5111970171448,388.819532698545));
#52156=CARTESIAN_POINT('Ctrl Pts',(0.467533990930312,4.87887853461636,388.740404823085));
#52157=CARTESIAN_POINT('Ctrl Pts',(2.73788576040913,4.06522143937628,388.661276947625));
#52158=CARTESIAN_POINT('Ctrl Pts',(4.34530441052119,2.26723915106472,388.582149072165));
#52159=CARTESIAN_POINT('Ctrl Pts',(4.90058047341499,-0.0797170734497908,
388.503021196706));
#52160=CARTESIAN_POINT('Ctrl Pts',(4.26926316308366,-2.40737114557615,388.423893321245));
#52161=CARTESIAN_POINT('Ctrl Pts',(2.60421537830119,-4.1521206692045,388.344765445786));
#52162=CARTESIAN_POINT('Ctrl Pts',(0.308600515372232,-4.89150380865921,
388.265637570326));
#52163=CARTESIAN_POINT('Ctrl Pts',(-2.06173678676592,-4.44649133703325,
388.186509694866));
#52164=CARTESIAN_POINT('Ctrl Pts',(-3.93285910370337,-2.92483556095608,
388.107381819407));
#52165=CARTESIAN_POINT('Ctrl Pts',(-4.85170554728278,-0.694979906674425,
388.028253943947));
#52166=CARTESIAN_POINT('Ctrl Pts',(-4.59579286131083,1.70315347639018,387.949126068487));
#52167=CARTESIAN_POINT('Ctrl Pts',(-3.22708601074344,3.68889680900396,387.869998193027));
#52168=CARTESIAN_POINT('Ctrl Pts',(-1.07699440464578,4.78143564639088,387.790870317567));
#52169=CARTESIAN_POINT('Ctrl Pts',(1.3338733340929,4.71623003221975,387.711742442108));
#52170=CARTESIAN_POINT('Ctrl Pts',(3.42176601558219,3.50906841238845,387.632614566648));
#52171=CARTESIAN_POINT('Ctrl Pts',(4.68113544337878,1.45224472764016,387.553486691188));
#52172=CARTESIAN_POINT('Ctrl Pts',(4.80704643162612,-0.956215662079578,
387.474358815728));
#52173=CARTESIAN_POINT('Ctrl Pts',(3.76901174619325,-3.13314446607126,387.395230940269));
#52174=CARTESIAN_POINT('Ctrl Pts',(1.81837407711343,-4.5514348840665,387.316103064809));
#52175=CARTESIAN_POINT('Ctrl Pts',(-0.572552378499359,-4.86767167772133,
387.236975189349));
#52176=CARTESIAN_POINT('Ctrl Pts',(-2.82484487802531,-4.00528341110962,
387.157847313889));
#52177=CARTESIAN_POINT('Ctrl Pts',(-4.39314856625886,-2.173082939741,387.07871943843));
#52178=CARTESIAN_POINT('Ctrl Pts',(-4.89772500736415,0.185293120367267,
386.99959156297));
#52179=CARTESIAN_POINT('Ctrl Pts',(-4.21639947845907,2.4988035589589,386.92046368751));
#52180=CARTESIAN_POINT('Ctrl Pts',(-2.51414352974947,4.20727062357945,386.84133581205));
#52181=CARTESIAN_POINT('Ctrl Pts',(-0.203129890410879,4.89701766750308,
386.762207936591));
#52182=CARTESIAN_POINT('Ctrl Pts',(2.15706824516707,4.40103401190078,386.68308006113));
#52183=CARTESIAN_POINT('Ctrl Pts',(3.99496848171146,2.83941378075611,386.603952185671));
#52184=CARTESIAN_POINT('Ctrl Pts',(4.86555410065941,0.590277122860157,386.524824310211));
#52185=CARTESIAN_POINT('Ctrl Pts',(4.55802739511214,-1.80178524070515,386.445696434751));
#52186=CARTESIAN_POINT('Ctrl Pts',(3.14685079923878,-3.75757552625969,386.366568559291));
#52187=CARTESIAN_POINT('Ctrl Pts',(0.973717058663619,-4.80353191702554,
386.287440683832));
#52188=CARTESIAN_POINT('Ctrl Pts',(-1.43518593730373,-4.68639361487927,
386.208312808372));
#52189=CARTESIAN_POINT('Ctrl Pts',(-3.49658272828396,-3.43452369514056,
386.129184932912));
#52190=CARTESIAN_POINT('Ctrl Pts',(-4.71134065335373,-1.35104146356512,
386.050057057452));
#52191=CARTESIAN_POINT('Ctrl Pts',(-4.78532645385515,1.05957279988197,385.970929181993));
#52192=CARTESIAN_POINT('Ctrl Pts',(-3.70062570902444,3.21362928010108,385.891801306533));
#52193=CARTESIAN_POINT('Ctrl Pts',(-1.71988051253413,4.58955932643004,385.812673431073));
#52194=CARTESIAN_POINT('Ctrl Pts',(0.677304905677504,4.85420455409132,385.733545555613));
#52195=CARTESIAN_POINT('Ctrl Pts',(2.91049230016732,3.94348555961378,385.654417680154));
#52196=CARTESIAN_POINT('Ctrl Pts',(4.43895279649954,2.07791767369751,385.575289804694));
#52197=CARTESIAN_POINT('Ctrl Pts',(4.89259531954076,-0.29078312781775,385.496161929234));
#52198=CARTESIAN_POINT('Ctrl Pts',(4.16157794044722,-2.58907567170192,385.417034053774));
#52199=CARTESIAN_POINT('Ctrl Pts',(2.42290425755801,-4.26046696348217,385.337906178315));
#52200=CARTESIAN_POINT('Ctrl Pts',(0.0975649436126985,-4.90025763302231,
385.258778302854));
#52201=CARTESIAN_POINT('Ctrl Pts',(-2.25139808515128,-4.35353309972404,
385.179650427395));
#52202=CARTESIAN_POINT('Ctrl Pts',(-4.05522282615024,-2.75267354012164,
385.100522551935));
#52203=CARTESIAN_POINT('Ctrl Pts',(-4.87714337058205,-0.485300248303261,
385.021394676475));
#52204=CARTESIAN_POINT('Ctrl Pts',(-4.51814544317236,1.89958035959429,384.942266801015));
#52205=CARTESIAN_POINT('Ctrl Pts',(-3.06515437123229,3.82450944157957,384.863138925556));
#52206=CARTESIAN_POINT('Ctrl Pts',(-0.869987574488363,4.82339770374075,
384.784011050096));
#52207=CARTESIAN_POINT('Ctrl Pts',(1.53583212271834,4.65438110590894,384.704883174636));
#52208=CARTESIAN_POINT('Ctrl Pts',(3.56977582909287,3.35838418264497,384.625755299176));
#52209=CARTESIAN_POINT('Ctrl Pts',(4.73935818772915,1.24921085354728,384.546627423716));
#52210=CARTESIAN_POINT('Ctrl Pts',(4.76138444573462,-1.16243793302357,384.467499548257));
#52211=CARTESIAN_POINT('Ctrl Pts',(3.6305213141391,-3.29262186954369,384.388371672797));
#52212=CARTESIAN_POINT('Ctrl Pts',(1.62058833437354,-4.62555264143734,384.309243797337));
#52213=CARTESIAN_POINT('Ctrl Pts',(-0.781742931416587,-4.83848341708389,
384.230115921878));
#52214=CARTESIAN_POINT('Ctrl Pts',(-2.9947882570989,-3.87985658025632,384.150988046417));
#52215=CARTESIAN_POINT('Ctrl Pts',(-4.48269583239351,-1.98178754220968,
384.071860170958));
#52216=CARTESIAN_POINT('Ctrl Pts',(-4.88519379187676,0.396138112309837,
383.992732295498));
#52217=CARTESIAN_POINT('Ctrl Pts',(-4.10482400501691,2.67814556662863,383.913604420039));
#52218=CARTESIAN_POINT('Ctrl Pts',(-2.33053992799659,4.31168498759236,383.834476544578));
#52219=CARTESIAN_POINT('Ctrl Pts',(0.00804530673338092,4.90122220076332,
383.755348669119));
#52220=CARTESIAN_POINT('Ctrl Pts',(2.34468250536694,4.30401065719426,383.676220793659));
#52221=CARTESIAN_POINT('Ctrl Pts',(4.11359415836805,2.66465511623097,383.5970929182));
#52222=CARTESIAN_POINT('Ctrl Pts',(4.88646797566037,0.380098028225917,383.517965042739));
#52223=CARTESIAN_POINT('Ctrl Pts',(4.47616552437595,-1.99649342262975,383.43883716728));
#52224=CARTESIAN_POINT('Ctrl Pts',(2.98203466184577,-3.88966747470347,383.35970929182));
#52225=CARTESIAN_POINT('Ctrl Pts',(0.765854118125881,-4.84102378200782,
383.28058141636));
#52226=CARTESIAN_POINT('Ctrl Pts',(-1.6357651560373,-4.62020737007657,383.2014535409));
#52227=CARTESIAN_POINT('Ctrl Pts',(-3.6413113313429,-3.28068522971184,383.122325665441));
#52228=CARTESIAN_POINT('Ctrl Pts',(-4.76517503677366,-1.14680018186465,
383.043197789981));
#52229=CARTESIAN_POINT('Ctrl Pts',(-4.73523152455593,1.26476329685335,382.964069914521));
#52230=CARTESIAN_POINT('Ctrl Pts',(-3.55873111398586,3.37008555478411,382.884942039061));
#52231=CARTESIAN_POINT('Ctrl Pts',(-1.52054364820804,4.65939811586324,382.805814163601));
#52232=CARTESIAN_POINT('Ctrl Pts',(0.885817960704724,4.82051556669083,382.726686288142));
#52233=CARTESIAN_POINT('Ctrl Pts',(3.07769360662633,3.8144260186753,382.647558412682));
#52234=CARTESIAN_POINT('Ctrl Pts',(4.52435736219093,1.88473718258125,382.568430537222));
#52235=CARTESIAN_POINT('Ctrl Pts',(4.87552386121587,-0.501309153048634,
382.489302661763));
#52236=CARTESIAN_POINT('Ctrl Pts',(4.04616402543129,-2.76597188480314,382.410174786302));
#52237=CARTESIAN_POINT('Ctrl Pts',(2.23709342974706,-4.36090091320568,382.331046910843));
#52238=CARTESIAN_POINT('Ctrl Pts',(-0.113651821301689,-4.89991092283629,
382.251919035383));
#52239=CARTESIAN_POINT('Ctrl Pts',(-2.43687818989498,-4.25248967968529,
382.172791159923));
#52240=CARTESIAN_POINT('Ctrl Pts',(-4.17005537407579,-2.5753993797773,382.093663284464));
#52241=CARTESIAN_POINT('Ctrl Pts',(-4.89352358608415,-0.274719312487676,
382.014535409004));
#52242=CARTESIAN_POINT('Ctrl Pts',(-4.43210713178239,2.09247942895964,381.935407533544));
#52243=CARTESIAN_POINT('Ctrl Pts',(-2.89753026709117,3.95301936998874,381.856279658084));
#52244=CARTESIAN_POINT('Ctrl Pts',(-0.661365043163431,4.85640196728989,
381.777151782624));
#52245=CARTESIAN_POINT('Ctrl Pts',(1.73493863410831,4.58388827569936,381.698023907165));
#52246=CARTESIAN_POINT('Ctrl Pts',(3.7111560180617,3.20146291526546,381.618896031705));
#52247=CARTESIAN_POINT('Ctrl Pts',(4.78877921262759,1.04385700214232,381.539768156245));
#52248=CARTESIAN_POINT('Ctrl Pts',(4.70687983423134,-1.36650137735827,381.460640280785));
#52249=CARTESIAN_POINT('Ctrl Pts',(3.48528844380413,-3.44598436614286,381.381512405325));
#52250=CARTESIAN_POINT('Ctrl Pts',(1.41979290903503,-4.69108003381625,381.302384529866));
#52251=CARTESIAN_POINT('Ctrl Pts',(-0.989481667084847,-4.80030934614829,
381.223256654406));
#52252=CARTESIAN_POINT('Ctrl Pts',(-3.1591698522741,-3.74722425705989,381.144128778946));
#52253=CARTESIAN_POINT('Ctrl Pts',(-4.56391804067381,-1.78681165941677,
381.065000903487));
#52254=CARTESIAN_POINT('Ctrl Pts',(-4.86359001771767,0.606247414652442,
380.985873028026));
#52255=CARTESIAN_POINT('Ctrl Pts',(-3.98562524001068,2.85251384473511,380.906745152567));
#52256=CARTESIAN_POINT('Ctrl Pts',(-2.1426081539881,4.40809188727722,380.827617277107));
#52257=CARTESIAN_POINT('Ctrl Pts',(0.219205562501549,4.89632440812331,380.748489401647));
#52258=CARTESIAN_POINT('Ctrl Pts',(2.52794232836271,4.19899409057548,380.669361526187));
#52259=CARTESIAN_POINT('Ctrl Pts',(4.22458025593252,2.48494777599062,380.590233650728));
#52260=CARTESIAN_POINT('Ctrl Pts',(4.89830692563373,0.169213032902914,380.511105775268));
#52261=CARTESIAN_POINT('Ctrl Pts',(4.38599072357506,-2.18749380820361,380.431977899808));
#52262=CARTESIAN_POINT('Ctrl Pts',(2.81168042594869,-4.01453571045926,380.352850024348));
#52263=CARTESIAN_POINT('Ctrl Pts',(0.556568868317172,-4.86952511884227,
380.273722148889));
#52264=CARTESIAN_POINT('Ctrl Pts',(-1.83330650647258,-4.54544068727564,
380.194594273429));
#52265=CARTESIAN_POINT('Ctrl Pts',(-3.77927745739419,-3.12075402559187,
380.115466397969));
#52266=CARTESIAN_POINT('Ctrl Pts',(-4.81015975486937,-0.940429115271696,
380.036338522509));
#52267=CARTESIAN_POINT('Ctrl Pts',(-4.67634253965503,1.46760493322567,379.95721064705));
#52268=CARTESIAN_POINT('Ctrl Pts',(-3.41022740614562,3.5202830605775,379.878082771589));
#52269=CARTESIAN_POINT('Ctrl Pts',(-1.31838289970275,4.72058368403601,379.79895489613));
#52270=CARTESIAN_POINT('Ctrl Pts',(1.09268591509449,4.77787413806285,379.71982702067));
#52271=CARTESIAN_POINT('Ctrl Pts',(3.23917916116038,3.67828250004266,379.64069914521));
#52272=CARTESIAN_POINT('Ctrl Pts',(4.60135949813868,1.68805644369628,379.56157126975));
#52273=CARTESIAN_POINT('Ctrl Pts',(4.8493978027726,-0.71090416982881,379.482443394291));
#52274=CARTESIAN_POINT('Ctrl Pts',(3.92323575948474,-2.93773126131644,379.403315518831));
#52275=CARTESIAN_POINT('Ctrl Pts',(2.04712797424676,-4.45323599703316,379.324187643371));
#52276=CARTESIAN_POINT('Ctrl Pts',(-0.324657517247101,-4.89046432199546,
379.245059767911));
#52277=CARTESIAN_POINT('Ctrl Pts',(-2.61783263582229,-4.14354873013934,
379.165931892452));
#52278=CARTESIAN_POINT('Ctrl Pts',(-4.27714348571947,-2.39334230539285,
379.086804016992));
#52279=CARTESIAN_POINT('Ctrl Pts',(-4.90081577320139,-0.0636281805188475,
379.007676141532));
#52280=CARTESIAN_POINT('Ctrl Pts',(-4.33783771356114,2.28149244114949,378.928548266072));
#52281=CARTESIAN_POINT('Ctrl Pts',(-2.72452500214632,4.07418793146503,378.849420390613));
#52282=CARTESIAN_POINT('Ctrl Pts',(-0.451514254902642,4.88038714302825,
378.770292515153));
#52283=CARTESIAN_POINT('Ctrl Pts',(1.93082309674852,4.50488245765392,378.691164639693));
#52284=CARTESIAN_POINT('Ctrl Pts',(3.84564401766237,3.03859603725688,378.612036764233));
#52285=CARTESIAN_POINT('Ctrl Pts',(4.82930673560502,0.836564547214143,378.532908888774));
#52286=CARTESIAN_POINT('Ctrl Pts',(4.64363382059009,-1.56802701777984,378.453781013314));
#52287=CARTESIAN_POINT('Ctrl Pts',(3.33358285503851,-3.59294713804823,378.374653137854));
#52288=CARTESIAN_POINT('Ctrl Pts',(1.21636070918609,-4.74789536672449,378.295525262394));
#52289=CARTESIAN_POINT('Ctrl Pts',(-1.19538278261738,-4.7532203600546,378.216397386934));
#52290=CARTESIAN_POINT('Ctrl Pts',(-3.31768438156428,-3.60763276020996,
378.137269511475));
#52291=CARTESIAN_POINT('Ctrl Pts',(-4.6366643489263,-1.58851739166163,378.058141636015));
#52292=CARTESIAN_POINT('Ctrl Pts',(-4.83295380642895,0.815230822000412,
377.979013760555));
#52293=CARTESIAN_POINT('Ctrl Pts',(-3.85902455393964,3.02158456448046,377.899885885095));
#52294=CARTESIAN_POINT('Ctrl Pts',(-1.95069722602663,4.49631228014555,377.820758009635));
#52295=CARTESIAN_POINT('Ctrl Pts',(0.429958719716191,4.88233338553971,377.741630134176));
#52296=CARTESIAN_POINT('Ctrl Pts',(2.70650737238561,4.08617934401293,377.662502258716));
#52297=CARTESIAN_POINT('Ctrl Pts',(4.32772065609622,2.30062550429524,377.583374383256));
#52298=CARTESIAN_POINT('Ctrl Pts',(4.9010489638226,-0.0419862171323538,
377.504246507796));
#52299=CARTESIAN_POINT('Ctrl Pts',(4.28767046122876,-2.37443168023888,377.425118632336));
#52300=CARTESIAN_POINT('Ctrl Pts',(2.63610446564972,-4.13194833394574,377.345990756877));
#52301=CARTESIAN_POINT('Ctrl Pts',(0.346249984239667,-4.88898299614862,
377.266862881417));
#52302=CARTESIAN_POINT('Ctrl Pts',(-2.0274431238406,-4.46223241974302,377.187735005957));
#52303=CARTESIAN_POINT('Ctrl Pts',(-3.91022488205308,-2.95502709970493,
377.108607130498));
#52304=CARTESIAN_POINT('Ctrl Pts',(-4.84621126407803,-0.732311526700024,
377.029479255038));
#52305=CARTESIAN_POINT('Ctrl Pts',(-4.60876886508425,1.66772100077964,376.950351379578));
#52306=CARTESIAN_POINT('Ctrl Pts',(-3.25539037980364,3.66394285754004,376.871223504118));
#52307=CARTESIAN_POINT('Ctrl Pts',(-1.11377371072242,4.77300239990086,376.792095628659));
#52308=CARTESIAN_POINT('Ctrl Pts',(1.29752458313577,4.72635945993341,376.712967753198));
#52309=CARTESIAN_POINT('Ctrl Pts',(3.39464906017594,3.53530784320889,376.633839877739));
#52310=CARTESIAN_POINT('Ctrl Pts',(4.66981619949699,1.48824072358315,376.554712002279));
#52311=CARTESIAN_POINT('Ctrl Pts',(4.8142656643279,-0.919178927997845,376.475584126819));
#52312=CARTESIAN_POINT('Ctrl Pts',(3.79302143937608,-3.10403481730793,376.396456251359));
#52313=CARTESIAN_POINT('Ctrl Pts',(1.85336068619839,-4.53730073503479,376.3173283759));
#52314=CARTESIAN_POINT('Ctrl Pts',(-0.535060274040971,-4.87193537309239,
376.23820050044));
#52315=CARTESIAN_POINT('Ctrl Pts',(-2.7939253627036,-4.02691257378452,376.15907262498));
#52316=CARTESIAN_POINT('Ctrl Pts',(-4.37628828172638,-2.20684041966181,
376.07994474952));
#52317=CARTESIAN_POINT('Ctrl Pts',(-4.89900638965642,0.147581107404016,
376.000816874061));
#52318=CARTESIAN_POINT('Ctrl Pts',(-4.23551226043463,2.46626839394683,375.921688998601));
#52319=CARTESIAN_POINT('Ctrl Pts',(-2.54645987583722,4.18779004627332,375.842561123141));
#52320=CARTESIAN_POINT('Ctrl Pts',(-0.24082493083811,4.89530879473852,375.763433247681));
#52321=CARTESIAN_POINT('Ctrl Pts',(2.12312171415927,4.41751014933925,375.684305372222));
#52322=CARTESIAN_POINT('Ctrl Pts',(3.97299008156779,2.87008650088106,375.605177496762));
#52323=CARTESIAN_POINT('Ctrl Pts',(4.86086545139366,0.627717440079687,375.526049621302));
#52324=CARTESIAN_POINT('Ctrl Pts',(4.57176394606508,-1.76663842623643,375.446921745842));
#52325=CARTESIAN_POINT('Ctrl Pts',(3.1756861134954,-3.73324183321634,375.367793870382));
#52326=CARTESIAN_POINT('Ctrl Pts',(1.01066992437191,-4.79588344705227,375.288665994922));
#52327=CARTESIAN_POINT('Ctrl Pts',(-1.39906459845869,-4.69732449000695,
375.209538119463));
#52328=CARTESIAN_POINT('Ctrl Pts',(-3.47003521363053,-3.46129850620319,
375.130410244003));
#52329=CARTESIAN_POINT('Ctrl Pts',(-4.70079892256589,-1.38736908122097,
375.051282368543));
#52330=CARTESIAN_POINT('Ctrl Pts',(-4.79330612491241,1.02286909042425,374.972154493083));
#52331=CARTESIAN_POINT('Ctrl Pts',(-4.08111211300407,2.46384394177367,374.91940257611));
#52332=CARTESIAN_POINT('Ctrl Pts',(-3.57461543774341,3.05624720968232,374.893026617624));
#52333=CARTESIAN_POINT('Ctrl Pts',(-1.16918346556839,-4.36383719750651,
400.320920147129));
#52334=CARTESIAN_POINT('Ctrl Pts',(-1.89238053709901,-4.17007422695751,
400.294544188642));
#52335=CARTESIAN_POINT('Ctrl Pts',(-3.23983970630162,-3.41613758049457,
400.241792271669));
#52336=CARTESIAN_POINT('Ctrl Pts',(-4.47701437999898,-1.45709925725484,
400.162664396209));
#52337=CARTESIAN_POINT('Ctrl Pts',(-4.62991897006387,0.854469866048622,
400.08353652075));
#52338=CARTESIAN_POINT('Ctrl Pts',(-3.66187379628773,2.9592933130866,400.00440864529));
#52339=CARTESIAN_POINT('Ctrl Pts',(-1.80711600920317,4.34750539486619,399.92528076983));
#52340=CARTESIAN_POINT('Ctrl Pts',(0.485180445975455,4.68307450728292,399.84615289437));
#52341=CARTESIAN_POINT('Ctrl Pts',(2.66001002393004,3.8847003355008,399.767025018911));
#52342=CARTESIAN_POINT('Ctrl Pts',(4.19075738523379,2.14571838156707,399.687897143451));
#52343=CARTESIAN_POINT('Ctrl Pts',(4.70678568217143,-0.112816719181106,
399.608769267991));
#52344=CARTESIAN_POINT('Ctrl Pts',(4.0831435580808,-2.34403352376061,399.529641392531));
#52345=CARTESIAN_POINT('Ctrl Pts',(2.47083727056938,-4.00768268816587,399.450513517072));
#52346=CARTESIAN_POINT('Ctrl Pts',(0.26025890735466,-4.70093834136087,399.371385641611));
#52347=CARTESIAN_POINT('Ctrl Pts',(-2.01333665809567,-4.25594078634204,
399.292257766152));
#52348=CARTESIAN_POINT('Ctrl Pts',(-3.79943657795602,-2.78043846617054,
399.213129890692));
#52349=CARTESIAN_POINT('Ctrl Pts',(-4.66556662297687,-0.631699640775407,
399.134002015232));
#52350=CARTESIAN_POINT('Ctrl Pts',(-4.40200797064279,1.66999467634492,399.054874139773));
#52351=CARTESIAN_POINT('Ctrl Pts',(-3.07257690863908,3.56732778180521,398.975746264313));
#52352=CARTESIAN_POINT('Ctrl Pts',(-0.999172881885126,4.60089229715201,
398.896618388853));
#52353=CARTESIAN_POINT('Ctrl Pts',(1.31616410234924,4.52042790313295,398.817490513393));
#52354=CARTESIAN_POINT('Ctrl Pts',(3.3128140221261,3.34541770608376,398.738362637933));
#52355=CARTESIAN_POINT('Ctrl Pts',(4.50732158649137,1.36037071761185,398.659234762474));
#52356=CARTESIAN_POINT('Ctrl Pts',(4.61045682154316,-0.954067224935643,
398.580106887014));
#52357=CARTESIAN_POINT('Ctrl Pts',(3.5972472600316,-3.03749378987274,398.500979011554));
#52358=CARTESIAN_POINT('Ctrl Pts',(1.71302460447423,-4.38544217583732,398.421851136094));
#52359=CARTESIAN_POINT('Ctrl Pts',(-0.58597822963345,-4.67152928789035,
398.342723260635));
#52360=CARTESIAN_POINT('Ctrl Pts',(-2.74309626297668,-3.82648392982927,
398.263595385175));
#52361=CARTESIAN_POINT('Ctrl Pts',(-4.23601954113904,-2.05491966273361,
398.184467509715));
#52362=CARTESIAN_POINT('Ctrl Pts',(-4.70326173037178,0.214208937311664,
398.105339634255));
#52363=CARTESIAN_POINT('Ctrl Pts',(-4.0316879707426,2.43147043571793,398.026211758796));
#52364=CARTESIAN_POINT('Ctrl Pts',(-2.38390858507682,4.05999214669189,397.947083883336));
#52365=CARTESIAN_POINT('Ctrl Pts',(-0.158905716443472,4.70545485011635,
397.867956007876));
#52366=CARTESIAN_POINT('Ctrl Pts',(2.10457350639361,4.2115705775148,397.788828132416));
#52367=CARTESIAN_POINT('Ctrl Pts',(3.85846555079357,2.69792512248606,397.709700256956));
#52368=CARTESIAN_POINT('Ctrl Pts',(4.67809487300653,0.531022346377457,397.630572381497));
#52369=CARTESIAN_POINT('Ctrl Pts',(4.36500197879199,-1.76445858504648,397.551444506037));
#52370=CARTESIAN_POINT('Ctrl Pts',(2.99499706155341,-3.63270546211616,397.472316630577));
#52371=CARTESIAN_POINT('Ctrl Pts',(0.899803835430396,-4.62135363621384,
397.393188755117));
#52372=CARTESIAN_POINT('Ctrl Pts',(-1.41326179868926,-4.4910185327571,397.314060879658));
#52373=CARTESIAN_POINT('Ctrl Pts',(-3.38412979029408,-3.2732586111773,397.234933004198));
#52374=CARTESIAN_POINT('Ctrl Pts',(-4.53558750895661,-1.26293401324019,
397.155805128738));
#52375=CARTESIAN_POINT('Ctrl Pts',(-4.58882877938272,1.0531888751364,397.076677253278));
#52376=CARTESIAN_POINT('Ctrl Pts',(-3.53096212085652,3.11429974059636,396.997549377818));
#52377=CARTESIAN_POINT('Ctrl Pts',(-1.61813220309064,4.42133515428577,396.918421502359));
#52378=CARTESIAN_POINT('Ctrl Pts',(0.686501289701844,4.65781841127795,396.839293626899));
#52379=CARTESIAN_POINT('Ctrl Pts',(2.82491000861503,3.76648905699045,396.760165751439));
#52380=CARTESIAN_POINT('Ctrl Pts',(4.27931414595585,1.96316754593802,396.681037875979));
#52381=CARTESIAN_POINT('Ctrl Pts',(4.69755413190968,-0.315502061769038,
396.601910000519));
#52382=CARTESIAN_POINT('Ctrl Pts',(3.97836016824692,-2.51777813655384,396.52278212506));
#52383=CARTESIAN_POINT('Ctrl Pts',(2.29587301155249,-4.11041646162856,396.4436542496));
#52384=CARTESIAN_POINT('Ctrl Pts',(0.0574787095610184,-4.70778637696628,
396.36452637414));
#52385=CARTESIAN_POINT('Ctrl Pts',(-2.1948330979661,-4.16524477615358,396.28539849868));
#52386=CARTESIAN_POINT('Ctrl Pts',(-3.9157028807147,-2.614159008776,396.206270623221));
#52387=CARTESIAN_POINT('Ctrl Pts',(-4.68845088177226,-0.430098479898641,
396.127142747761));
#52388=CARTESIAN_POINT('Ctrl Pts',(-4.32596913256195,1.85810318263636,396.048014872301));
#52389=CARTESIAN_POINT('Ctrl Pts',(-2.91602650941616,3.69639632203913,395.968886996841));
#52390=CARTESIAN_POINT('Ctrl Pts',(-0.8000169721583,4.63966908490906,395.889759121381));
#52391=CARTESIAN_POINT('Ctrl Pts',(1.50970325769618,4.4595237914943,395.810631245922));
#52392=CARTESIAN_POINT('Ctrl Pts',(3.45387416317228,3.19957960334997,395.731503370462));
#52393=CARTESIAN_POINT('Ctrl Pts',(4.56174736550757,1.16491087491141,395.652375495002));
#52394=CARTESIAN_POINT('Ctrl Pts',(4.56506994907375,-1.15182148498192,395.573247619542));
#52395=CARTESIAN_POINT('Ctrl Pts',(3.46303740598383,-3.18965958966768,395.494119744083));
#52396=CARTESIAN_POINT('Ctrl Pts',(1.52248843418447,-4.45517511900225,395.414991868623));
#52397=CARTESIAN_POINT('Ctrl Pts',(-0.786705578057672,-4.64194471171891,
395.335863993163));
#52398=CARTESIAN_POINT('Ctrl Pts',(-2.90541202853717,-3.70474524328377,
395.256736117703));
#52399=CARTESIAN_POINT('Ctrl Pts',(-4.32062168343229,-1.87050384705749,
395.177608242243));
#52400=CARTESIAN_POINT('Ctrl Pts',(-4.68966525951576,0.416648685217087,
395.098480366784));
#52401=CARTESIAN_POINT('Ctrl Pts',(-3.92318504412731,2.60291672604753,395.019352491324));
#52402=CARTESIAN_POINT('Ctrl Pts',(-2.20677136666199,4.15893213559478,394.940224615864));
#52403=CARTESIAN_POINT('Ctrl Pts',(0.0439749871279553,4.70793187861818,
394.861096740404));
#52404=CARTESIAN_POINT('Ctrl Pts',(2.28407353529635,4.11698487470637,394.781968864944));
#52405=CARTESIAN_POINT('Ctrl Pts',(3.97112198345224,2.52917902999067,394.702840989485));
#52406=CARTESIAN_POINT('Ctrl Pts',(4.69662984363174,0.328974900425354,394.623713114025));
#52407=CARTESIAN_POINT('Ctrl Pts',(4.28492755509978,-1.95088498398772,394.544585238566));
#52408=CARTESIAN_POINT('Ctrl Pts',(2.83570192230001,-3.75837078812964,394.465457363105));
#52409=CARTESIAN_POINT('Ctrl Pts',(0.699858627021958,-4.65583013815851,
394.386329487646));
#52410=CARTESIAN_POINT('Ctrl Pts',(-1.60544369734944,-4.42595830389794,
394.307201612186));
#52411=CARTESIAN_POINT('Ctrl Pts',(-3.52201475555854,-3.12441489479712,
394.228073736726));
#52412=CARTESIAN_POINT('Ctrl Pts',(-4.58578900897716,-1.06634681897889,
394.148945861266));
#52413=CARTESIAN_POINT('Ctrl Pts',(-4.53919136286672,1.24991925518346,394.069817985807));
#52414=CARTESIAN_POINT('Ctrl Pts',(-3.39350465573632,3.26353834429719,393.990690110347));
#52415=CARTESIAN_POINT('Ctrl Pts',(-1.42613770922415,4.48694635665851,393.911562234887));
#52416=CARTESIAN_POINT('Ctrl Pts',(0.886544565594953,4.62391556004391,393.832434359427));
#52417=CARTESIAN_POINT('Ctrl Pts',(2.98456494223475,3.64128115898587,393.753306483967));
#52418=CARTESIAN_POINT('Ctrl Pts',(4.35992297272438,1.77697159378319,393.674178608508));
#52419=CARTESIAN_POINT('Ctrl Pts',(4.67959877632843,-0.51760184098167,393.595050733048));
#52420=CARTESIAN_POINT('Ctrl Pts',(3.86618821853779,-2.68684667073537,393.515922857588));
#52421=CARTESIAN_POINT('Ctrl Pts',(2.116645024084,-4.20551664070214,393.436794982129));
#52422=CARTESIAN_POINT('Ctrl Pts',(-0.14540826436235,-4.70589128750945,
393.357667106668));
#52423=CARTESIAN_POINT('Ctrl Pts',(-2.37225338025842,-4.06681328229544,
393.278539231209));
#52424=CARTESIAN_POINT('Ctrl Pts',(-4.02469712556258,-2.44302464594413,
393.199411355749));
#52425=CARTESIAN_POINT('Ctrl Pts',(-4.70262796074555,-0.227698563931231,
393.120283480289));
#52426=CARTESIAN_POINT('Ctrl Pts',(-4.24189630375331,2.04276090656889,393.04115560483));
#52427=CARTESIAN_POINT('Ctrl Pts',(-2.75406059832286,3.81860008301049,392.962027729369));
#52428=CARTESIAN_POINT('Ctrl Pts',(-0.599375307795595,4.66982929169869,
392.88289985391));
#52429=CARTESIAN_POINT('Ctrl Pts',(1.70043866129603,4.39033765584971,392.80377197845));
#52430=CARTESIAN_POINT('Ctrl Pts',(3.58851992688128,3.04779938768583,392.72464410299));
#52431=CARTESIAN_POINT('Ctrl Pts',(4.60770127580904,0.967287612920714,392.64551622753));
#52432=CARTESIAN_POINT('Ctrl Pts',(4.51120503728849,-1.34743663477919,392.566388352071));
#52433=CARTESIAN_POINT('Ctrl Pts',(3.32239615712367,-3.3359016994408,392.487260476611));
#52434=CARTESIAN_POINT('Ctrl Pts',(1.32912476794421,-4.51663411451929,392.408132601151));
#52435=CARTESIAN_POINT('Ctrl Pts',(-0.985971892830688,-4.60373932795397,
392.329004725692));
#52436=CARTESIAN_POINT('Ctrl Pts',(-3.06233199564761,-3.57612627316698,
392.249876850231));
#52437=CARTESIAN_POINT('Ctrl Pts',(-4.397199764574,-1.68261421711348,392.170748974772));
#52438=CARTESIAN_POINT('Ctrl Pts',(-4.66735935664344,0.618314652224117,
392.091621099312));
#52439=CARTESIAN_POINT('Ctrl Pts',(-3.80739615752567,2.76952899837877,392.012493223852));
#52440=CARTESIAN_POINT('Ctrl Pts',(-2.02553583330784,4.25014834578608,391.933365348393));
#52441=CARTESIAN_POINT('Ctrl Pts',(0.24677402236281,4.70166555117323,391.854237472933));
#52442=CARTESIAN_POINT('Ctrl Pts',(2.45933168720454,4.01475329572239,391.775109597473));
#52443=CARTESIAN_POINT('Ctrl Pts',(4.07640342983146,2.35573586177663,391.695981722014));
#52444=CARTESIAN_POINT('Ctrl Pts',(4.70644244793312,0.126316497321376,391.616853846553));
#52445=CARTESIAN_POINT('Ctrl Pts',(4.19689535976046,-2.13368828848624,391.537725971094));
#52446=CARTESIAN_POINT('Ctrl Pts',(2.67114044701949,-3.87705623966156,391.458598095634));
#52447=CARTESIAN_POINT('Ctrl Pts',(0.498613673152825,-4.68166004512793,
391.379470220174));
#52448=CARTESIAN_POINT('Ctrl Pts',(-1.79464403933883,-4.35267838752966,
391.300342344714));
#52449=CARTESIAN_POINT('Ctrl Pts',(-3.65335879596438,-2.96976865785062,
391.221214469255));
#52450=CARTESIAN_POINT('Ctrl Pts',(-4.62747399120691,-0.867779254134205,
391.142086593794));
#52451=CARTESIAN_POINT('Ctrl Pts',(-4.4811239675789,1.4443283423073,391.062958718335));
#52452=CARTESIAN_POINT('Ctrl Pts',(-3.24974492884238,3.40671605371881,390.983830842875));
#52453=CARTESIAN_POINT('Ctrl Pts',(-1.23149465757426,4.54422460729751,390.904702967416));
#52454=CARTESIAN_POINT('Ctrl Pts',(1.08494139143324,4.58142538413069,390.825575091955));
#52455=CARTESIAN_POINT('Ctrl Pts',(3.1386770782293,3.50931084000835,390.746447216496));
#52456=CARTESIAN_POINT('Ctrl Pts',(4.43243474978322,1.58747553118664,390.667319341036));
#52457=CARTESIAN_POINT('Ctrl Pts',(4.65295268374329,-0.718740353708034,
390.588191465577));
#52458=CARTESIAN_POINT('Ctrl Pts',(3.74683616074228,-2.85092531606077,390.509063590117));
#52459=CARTESIAN_POINT('Ctrl Pts',(1.93348610020102,-4.29280652644998,390.429935714657));
#52460=CARTESIAN_POINT('Ctrl Pts',(-0.348025192701879,-4.69525663179842,
390.350807839197));
#52461=CARTESIAN_POINT('Ctrl Pts',(-2.54526802197775,-3.96082908865047,
390.271679963737));
#52462=CARTESIAN_POINT('Ctrl Pts',(-4.12621688682536,-2.2673532093786,390.192552088278));
#52463=CARTESIAN_POINT('Ctrl Pts',(-4.70807153396599,-0.0248757765959869,
390.113424212818));
#52464=CARTESIAN_POINT('Ctrl Pts',(-4.14994561897114,2.22362490829375,390.034296337358));
#52465=CARTESIAN_POINT('Ctrl Pts',(-2.58697997173855,3.93371211440616,389.955168461898));
#52466=CARTESIAN_POINT('Ctrl Pts',(-0.397620511000842,4.69131690492484,
389.876040586439));
#52467=CARTESIAN_POINT('Ctrl Pts',(1.88801608791904,4.31299798573579,389.796912710978));
#52468=CARTESIAN_POINT('Ctrl Pts',(3.71650125536658,2.89035893827407,389.717784835519));
#52469=CARTESIAN_POINT('Ctrl Pts',(4.64509797385908,0.767867948577403,389.638656960059));
#52470=CARTESIAN_POINT('Ctrl Pts',(4.44896212165639,-1.54054938683214,389.559529084599));
#52471=CARTESIAN_POINT('Ctrl Pts',(3.17558470594392,-3.47594852501834,389.480401209139));
#52472=CARTESIAN_POINT('Ctrl Pts',(1.13329271192188,-4.56970502355534,389.40127333368));
#52473=CARTESIAN_POINT('Ctrl Pts',(-1.18340710566026,-4.55698408988609,
389.32214545822));
#52474=CARTESIAN_POINT('Ctrl Pts',(-3.21356473971502,-3.44086588475379,
389.24301758276));
#52475=CARTESIAN_POINT('Ctrl Pts',(-4.46561156725167,-1.49159971293583,
389.1638897073));
#52476=CARTESIAN_POINT('Ctrl Pts',(-4.63638544725815,0.818832313514199,
389.084761831841));
#52477=CARTESIAN_POINT('Ctrl Pts',(-3.6845363487667,2.93099782801338,389.00563395638));
#52478=CARTESIAN_POINT('Ctrl Pts',(-1.84053856736483,4.33347137468852,388.926506080921));
#52479=CARTESIAN_POINT('Ctrl Pts',(0.449114760160199,4.6866675053185,388.847378205461));
#52480=CARTESIAN_POINT('Ctrl Pts',(2.63002248068729,3.90506570037965,388.768250330001));
#52481=CARTESIAN_POINT('Ctrl Pts',(4.1741143660401,2.17791772857007,388.689122454542));
#52482=CARTESIAN_POINT('Ctrl Pts',(4.70751446239035,-0.0765764950091339,
388.609994579082));
#52483=CARTESIAN_POINT('Ctrl Pts',(4.10106888214441,-2.31252900459844,388.530866703622));
#52484=CARTESIAN_POINT('Ctrl Pts',(2.5016182517638,-3.98854139951492,388.451738828162));
#52485=CARTESIAN_POINT('Ctrl Pts',(0.296442716755053,-4.6987953869992,388.372610952703));
#52486=CARTESIAN_POINT('Ctrl Pts',(-1.98051145042811,-4.27131487576429,
388.293483077243));
#52487=CARTESIAN_POINT('Ctrl Pts',(-3.77791798536176,-2.80960710226223,
388.214355201783));
#52488=CARTESIAN_POINT('Ctrl Pts',(-4.66056504020173,-0.667600089313645,
388.135227326323));
#52489=CARTESIAN_POINT('Ctrl Pts',(-4.41473443363227,1.63605508883523,388.056099450863));
#52490=CARTESIAN_POINT('Ctrl Pts',(-3.09994992417011,3.54356696576203,387.976971575404));
#52491=CARTESIAN_POINT('Ctrl Pts',(-1.03456453032195,4.59306353165313,387.897843699944));
#52492=CARTESIAN_POINT('Ctrl Pts',(1.28132331369787,4.53042679435133,387.818715824484));
#52493=CARTESIAN_POINT('Ctrl Pts',(3.28696020658222,3.37082318930362,387.739587949024));
#52494=CARTESIAN_POINT('Ctrl Pts',(4.49671481157362,1.39503128157636,387.660460073565));
#52495=CARTESIAN_POINT('Ctrl Pts',(4.61766534005973,-0.918544054693783,
387.581332198105));
#52496=CARTESIAN_POINT('Ctrl Pts',(3.6205256500481,-3.00970935316784,387.502204322645));
#52497=CARTESIAN_POINT('Ctrl Pts',(1.74673639428721,-4.37212400808516,387.423076447185));
#52498=CARTESIAN_POINT('Ctrl Pts',(-0.549995784557234,-4.67590216002981,
387.343948571725));
#52499=CARTESIAN_POINT('Ctrl Pts',(-2.71355570823769,-3.84748902421993,
387.264820696266));
#52500=CARTESIAN_POINT('Ctrl Pts',(-4.22007362664152,-2.08747094804379,
387.185692820806));
#52501=CARTESIAN_POINT('Ctrl Pts',(-4.70477149187816,0.177993208894804,
387.106564945346));
#52502=CARTESIAN_POINT('Ctrl Pts',(-4.05028784482536,2.40035929545185,387.027437069887));
#52503=CARTESIAN_POINT('Ctrl Pts',(-2.41509492416788,4.04151863542169,386.948309194426));
#52504=CARTESIAN_POINT('Ctrl Pts',(-0.195127271563123,4.70409201877413,
386.869181318967));
#52505=CARTESIAN_POINT('Ctrl Pts',(2.0720871773402,4.22764841285371,386.790053443507));
#52506=CARTESIAN_POINT('Ctrl Pts',(3.83758046755327,2.72755064632278,386.710925568048));
#52507=CARTESIAN_POINT('Ctrl Pts',(4.67386800821896,0.567022234969233,386.631797692587));
#52508=CARTESIAN_POINT('Ctrl Pts',(4.37845679687603,-1.73080110096229,386.552669817128));
#52509=CARTESIAN_POINT('Ctrl Pts',(3.02287570396291,-3.60953997783552,386.473541941668));
#52510=CARTESIAN_POINT('Ctrl Pts',(0.935355956463039,-4.61428928524331,
386.394414066208));
#52511=CARTESIAN_POINT('Ctrl Pts',(-1.37864454889126,-4.50176582920686,
386.315286190748));
#52512=CARTESIAN_POINT('Ctrl Pts',(-3.35882939819794,-3.29921527745666,
386.236158315289));
#52513=CARTESIAN_POINT('Ctrl Pts',(-4.52573004019154,-1.29781507793296,
386.157030439828));
#52514=CARTESIAN_POINT('Ctrl Pts',(-4.59680105468898,1.01782927684972,386.077902564369));
#52515=CARTESIAN_POINT('Ctrl Pts',(-3.55483378747301,3.08702334241943,385.998774688909));
#52516=CARTESIAN_POINT('Ctrl Pts',(-1.65212313730168,4.40874647858035,385.91964681345));
#52517=CARTESIAN_POINT('Ctrl Pts',(0.650621422548117,4.66296559473944,385.84051893799));
#52518=CARTESIAN_POINT('Ctrl Pts',(2.79582891660295,3.78812579546785,385.76139106253));
#52519=CARTESIAN_POINT('Ctrl Pts',(4.26407332779252,1.99605486608223,385.68226318707));
#52520=CARTESIAN_POINT('Ctrl Pts',(4.69984389610718,-0.279327272972474,
385.603135311611));
#52521=CARTESIAN_POINT('Ctrl Pts',(3.99762608680683,-2.48707499751891,385.52400743615));
#52522=CARTESIAN_POINT('Ctrl Pts',(2.32745016540729,-4.09261922254535,385.444879560691));
#52523=CARTESIAN_POINT('Ctrl Pts',(0.0937212204902381,-4.70720434079847,
385.365751685231));
#52524=CARTESIAN_POINT('Ctrl Pts',(-2.16270074615507,-4.18201887319778,
385.286623809771));
#52525=CARTESIAN_POINT('Ctrl Pts',(-3.89546099811616,-2.64422767275401,
385.207495934311));
#52526=CARTESIAN_POINT('Ctrl Pts',(-4.6850007007776,-0.466181088114491,
385.128368058852));
#52527=CARTESIAN_POINT('Ctrl Pts',(-4.34014605663549,1.82474342861496,385.049240183392));
#52528=CARTESIAN_POINT('Ctrl Pts',(-2.94439783415696,3.67383692716674,384.970112307932));
#52529=CARTESIAN_POINT('Ctrl Pts',(-0.83571305710034,4.63337242830686,384.890984432472));
#52530=CARTESIAN_POINT('Ctrl Pts',(1.47532562085691,4.47101450295627,384.811856557013));
#52531=CARTESIAN_POINT('Ctrl Pts',(3.42913894264361,3.22607539980813,384.732728681553));
#52532=CARTESIAN_POINT('Ctrl Pts',(4.55264378010221,1.19999624361863,384.653600806093));
#52533=CARTESIAN_POINT('Ctrl Pts',(4.57380227931992,-1.11664187763583,384.574472930633));
#52534=CARTESIAN_POINT('Ctrl Pts',(3.4874912645637,-3.1629038955988,384.495345055174));
#52535=CARTESIAN_POINT('Ctrl Pts',(1.55674272936248,-4.44332178080534,384.416217179713));
#52536=CARTESIAN_POINT('Ctrl Pts',(-0.750944949374648,-4.64786381644416,
384.337089304254));
#52537=CARTESIAN_POINT('Ctrl Pts',(-2.87680390283758,-3.72700357899221,
384.257961428794));
#52538=CARTESIAN_POINT('Ctrl Pts',(-4.30609303856287,-1.90371193105537,
384.178833553335));
#52539=CARTESIAN_POINT('Ctrl Pts',(-4.69273396316942,0.380531633531783,
384.099705677874));
#52540=CARTESIAN_POINT('Ctrl Pts',(-3.94310806118005,2.5726358450156,384.020577802415));
#52541=CARTESIAN_POINT('Ctrl Pts',(-2.23872467266656,4.14181943271266,383.941449926955));
#52542=CARTESIAN_POINT('Ctrl Pts',(0.00772834932661786,4.70813090788891,
383.862322051495));
#52543=CARTESIAN_POINT('Ctrl Pts',(2.2523100811437,4.13444744452999,383.783194176035));
#52544=CARTESIAN_POINT('Ctrl Pts',(3.9515327006614,2.55967687195196,383.704066300576));
#52545=CARTESIAN_POINT('Ctrl Pts',(4.69395794849557,0.365123473577542,383.624938425116));
#52546=CARTESIAN_POINT('Ctrl Pts',(4.29982000221476,-1.91783845038001,383.545810549656));
#52547=CARTESIAN_POINT('Ctrl Pts',(2.86455275536081,-3.73642795795088,383.466682674196));
#52548=CARTESIAN_POINT('Ctrl Pts',(0.735682100664791,-4.65030409972978,
383.387554798737));
#52549=CARTESIAN_POINT('Ctrl Pts',(-1.571321636466,-4.43818709474668,383.308426923276));
#52550=CARTESIAN_POINT('Ctrl Pts',(-3.49785619221092,-3.15143751831031,
383.229299047817));
#52551=CARTESIAN_POINT('Ctrl Pts',(-4.57744353411293,-1.10162020007351,
383.150171172357));
#52552=CARTESIAN_POINT('Ctrl Pts',(-4.54867969326092,1.21493597416402,383.071043296898));
#52553=CARTESIAN_POINT('Ctrl Pts',(-3.41852935131432,3.23731577814161,382.991915421438));
#52554=CARTESIAN_POINT('Ctrl Pts',(-1.46063945964488,4.47583385997855,382.912787545978));
#52555=CARTESIAN_POINT('Ctrl Pts',(0.850919780561573,4.6306038375412,382.833659670518));
#52556=CARTESIAN_POINT('Ctrl Pts',(2.95644306681562,3.66415075643457,382.754531795058));
#52557=CARTESIAN_POINT('Ctrl Pts',(4.3461132474158,1.81048502171076,382.675403919598));
#52558=CARTESIAN_POINT('Ctrl Pts',(4.68344499450879,-0.481559297088858,
382.596276044139));
#52559=CARTESIAN_POINT('Ctrl Pts',(3.88675908298024,-2.65700210840579,382.517148168679));
#52560=CARTESIAN_POINT('Ctrl Pts',(2.14895964496101,-4.18909642017598,382.438020293219));
#52561=CARTESIAN_POINT('Ctrl Pts',(-0.109174330542496,-4.70687128980098,
382.358892417759));
#52562=CARTESIAN_POINT('Ctrl Pts',(-2.34087357288517,-4.08495621628556,
382.2797645423));
#52563=CARTESIAN_POINT('Ctrl Pts',(-4.00576953871563,-2.47393750444512,
382.20063666684));
#52564=CARTESIAN_POINT('Ctrl Pts',(-4.7007355921423,-0.263896316701532,
382.12150879138));
#52565=CARTESIAN_POINT('Ctrl Pts',(-4.25749735871386,2.01004293828431,382.04238091592));
#52566=CARTESIAN_POINT('Ctrl Pts',(-2.78337754303629,3.79728400651352,381.963253040461));
#52567=CARTESIAN_POINT('Ctrl Pts',(-0.635309535778666,4.66507643741782,
381.884125165001));
#52568=CARTESIAN_POINT('Ctrl Pts',(1.6665880206908,4.40329884773815,381.804997289541));
#52569=CARTESIAN_POINT('Ctrl Pts',(3.56494923856197,3.07533629050199,381.725869414081));
#52570=CARTESIAN_POINT('Ctrl Pts',(4.60011778664443,1.00273262747343,381.646741538621));
#52571=CARTESIAN_POINT('Ctrl Pts',(4.52144496199587,-1.31266592430991,381.567613663161));
#52572=CARTESIAN_POINT('Ctrl Pts',(3.34798006967052,-3.31022443744999,381.488485787702));
#52573=CARTESIAN_POINT('Ctrl Pts',(1.36385795297921,-4.50626761936056,381.409357912242));
#52574=CARTESIAN_POINT('Ctrl Pts',(-0.950499493547971,-4.6111936725719,
381.330230036783));
#52575=CARTESIAN_POINT('Ctrl Pts',(-3.03470942869027,-3.59959651303038,
381.251102161322));
#52576=CARTESIAN_POINT('Ctrl Pts',(-4.38411537126835,-1.71641742726257,
381.171974285863));
#52577=CARTESIAN_POINT('Ctrl Pts',(-4.67198130338802,0.582363352208024,
381.092846410403));
#52578=CARTESIAN_POINT('Ctrl Pts',(-3.82860531743164,2.74013461284959,381.013718534943));
#52579=CARTESIAN_POINT('Ctrl Pts',(-2.05819676400615,4.23442823222176,380.934590659483));
#52580=CARTESIAN_POINT('Ctrl Pts',(0.210569617479083,4.70342607142888,380.855462784024));
#52581=CARTESIAN_POINT('Ctrl Pts',(2.42835009758821,4.03356816934405,380.776334908564));
#52582=CARTESIAN_POINT('Ctrl Pts',(4.05814632781095,2.38704938266401,380.697207033104));
#52583=CARTESIAN_POINT('Ctrl Pts',(4.70533048456991,0.162546621555695,380.618079157644));
#52584=CARTESIAN_POINT('Ctrl Pts',(4.2131977783341,-2.10131407786716,380.538951282185));
#52585=CARTESIAN_POINT('Ctrl Pts',(2.7009098902828,-3.85637681480619,380.459823406725));
#52586=CARTESIAN_POINT('Ctrl Pts',(0.53464196968763,-4.67768258194704,380.380695531265));
#52587=CARTESIAN_POINT('Ctrl Pts',(-1.76108053730214,-4.36636596202583,
380.301567655805));
#52588=CARTESIAN_POINT('Ctrl Pts',(-3.63038692754518,-2.99780705341609,
380.222439780345));
#52589=CARTESIAN_POINT('Ctrl Pts',(-4.62065600907807,-0.903379443519156,
380.143311904886));
#52590=CARTESIAN_POINT('Ctrl Pts',(-4.49211073176741,1.40978634790602,380.064184029426));
#52591=CARTESIAN_POINT('Ctrl Pts',(-3.27587617866081,3.38159601893615,379.985056153966));
#52592=CARTESIAN_POINT('Ctrl Pts',(-1.26644314913044,4.53460892726404,379.905928278506));
#52593=CARTESIAN_POINT('Ctrl Pts',(1.049637849243,4.58964233450045,379.826800403046));
#52594=CARTESIAN_POINT('Ctrl Pts',(3.11156664606508,3.53337082405704,379.747672527587));
#52595=CARTESIAN_POINT('Ctrl Pts',(4.42008176412018,1.62155282729066,379.668544652127));
#52596=CARTESIAN_POINT('Ctrl Pts',(4.65834821288585,-0.682896991284513,
379.589416776667));
#52597=CARTESIAN_POINT('Ctrl Pts',(3.76867376779785,-2.82199475639389,379.510288901207));
#52598=CARTESIAN_POINT('Ctrl Pts',(1.96647817486303,-4.27779381936408,379.431161025748));
#52599=CARTESIAN_POINT('Ctrl Pts',(-0.311867127997482,-4.69779685253383,
379.352033150288));
#52600=CARTESIAN_POINT('Ctrl Pts',(-2.51469903618647,-3.9803071653586,379.272905274828));
#52601=CARTESIAN_POINT('Ctrl Pts',(-4.1086387471793,-2.29905285245449,379.193777399368));
#52602=CARTESIAN_POINT('Ctrl Pts',(-4.70774049217468,-0.0611214491085228,
379.114649523908));
#52603=CARTESIAN_POINT('Ctrl Pts',(-4.16694183125235,2.19160948806155,379.035521648449));
#52604=CARTESIAN_POINT('Ctrl Pts',(-2.61718809033458,3.91367894352783,378.956393772989));
#52605=CARTESIAN_POINT('Ctrl Pts',(-0.433726146618794,4.68811667974907,
378.877265897529));
#52606=CARTESIAN_POINT('Ctrl Pts',(1.85475530941073,4.32740558711739,378.798138022069));
#52607=CARTESIAN_POINT('Ctrl Pts',(3.69413887366186,2.91888580717067,378.71901014661));
#52608=CARTESIAN_POINT('Ctrl Pts',(4.63904866464471,0.803606782114387,378.63988227115));
#52609=CARTESIAN_POINT('Ctrl Pts',(4.46069062370475,-1.50625214781415,378.56075439569));
#52610=CARTESIAN_POINT('Ctrl Pts',(3.20225115918455,-3.45139738174314,378.48162652023));
#52611=CARTESIAN_POINT('Ctrl Pts',(1.16844028192984,-4.56084462361588,378.40249864477));
#52612=CARTESIAN_POINT('Ctrl Pts',(-1.14828881349689,-4.56595983052853,
378.323370769311));
#52613=CARTESIAN_POINT('Ctrl Pts',(-3.18697903086916,-3.46550444091513,
378.244242893851));
#52614=CARTESIAN_POINT('Ctrl Pts',(-4.45399572524721,-1.5259352714587,378.165115018391));
#52615=CARTESIAN_POINT('Ctrl Pts',(-4.64255205342532,0.783113532278959,
378.085987142931));
#52616=CARTESIAN_POINT('Ctrl Pts',(-3.7069922628433,2.90254452789652,378.006859267472));
#52617=CARTESIAN_POINT('Ctrl Pts',(-1.8738464663689,4.31917304511859,377.927731392012));
#52618=CARTESIAN_POINT('Ctrl Pts',(0.413019825360475,4.68998624700131,377.848603516552));
#52619=CARTESIAN_POINT('Ctrl Pts',(2.59988029319979,3.92519793567579,377.769475641092));
#52620=CARTESIAN_POINT('Ctrl Pts',(4.15722335104551,2.20998877434347,377.690347765632));
#52621=CARTESIAN_POINT('Ctrl Pts',(4.70796449588766,-0.0403321046239016,
377.611219890173));
#52622=CARTESIAN_POINT('Ctrl Pts',(4.11875099606982,-2.28088724087274,377.532092014713));
#52623=CARTESIAN_POINT('Ctrl Pts',(2.53225101877986,-3.9691637848658,377.452964139253));
#52624=CARTESIAN_POINT('Ctrl Pts',(0.332608926075814,-4.69637388582909,
377.373836263793));
#52625=CARTESIAN_POINT('Ctrl Pts',(-1.94756883984043,-4.28643581396986,
377.294708388333));
#52626=CARTESIAN_POINT('Ctrl Pts',(-3.75617547417524,-2.83860919825332,
377.215580512874));
#52627=CARTESIAN_POINT('Ctrl Pts',(-4.65528721285309,-0.703460971943434,
377.136452637414));
#52628=CARTESIAN_POINT('Ctrl Pts',(-4.42719922749879,1.60201853086424,377.057324761954));
#52629=CARTESIAN_POINT('Ctrl Pts',(-3.12713919846579,3.51959611413589,376.978196886494));
#52630=CARTESIAN_POINT('Ctrl Pts',(-1.06989485827222,4.58496252606164,376.899069011035));
#52631=CARTESIAN_POINT('Ctrl Pts',(1.24640657847665,4.54015715746168,376.819941135575));
#52632=CARTESIAN_POINT('Ctrl Pts',(3.26091156592763,3.39602887682211,376.740813260115));
#52633=CARTESIAN_POINT('Ctrl Pts',(4.48584150695881,1.4296091591174,376.661685384655));
#52634=CARTESIAN_POINT('Ctrl Pts',(4.62460015982963,-0.882966440516176,
376.582557509196));
#52635=CARTESIAN_POINT('Ctrl Pts',(3.64358944392086,-2.9817465244189,376.503429633736));
#52636=CARTESIAN_POINT('Ctrl Pts',(1.7803446513398,-4.35854669589912,376.424301758276));
#52637=CARTESIAN_POINT('Ctrl Pts',(-0.513980740029185,-4.67999788047178,
376.345173882816));
#52638=CARTESIAN_POINT('Ctrl Pts',(-2.68385431544624,-3.86826607229696,
376.266046007356));
#52639=CARTESIAN_POINT('Ctrl Pts',(-4.20387757931463,-2.11989849939269,
376.186918131897));
#52640=CARTESIAN_POINT('Ctrl Pts',(-4.7060023921165,0.141766919500427,376.107790256437));
#52641=CARTESIAN_POINT('Ctrl Pts',(-4.0686476489454,2.36910590400946,376.028662380977));
#52642=CARTESIAN_POINT('Ctrl Pts',(-2.44613811739875,4.02280552584175,375.949534505517));
#52643=CARTESIAN_POINT('Ctrl Pts',(-0.231337257081005,4.70245046971741,
375.870406630058));
#52644=CARTESIAN_POINT('Ctrl Pts',(2.03947802286674,4.24347544716049,375.791278754597));
#52645=CARTESIAN_POINT('Ctrl Pts',(3.81646794076225,2.75701496679917,375.712150879138));
#52646=CARTESIAN_POINT('Ctrl Pts',(4.66936407560377,0.602987532497468,375.633023003678));
#52647=CARTESIAN_POINT('Ctrl Pts',(4.39165217497973,-1.6970389500669,375.553895128218));
#52648=CARTESIAN_POINT('Ctrl Pts',(3.05057500604089,-3.58616494858208,375.474767252759));
#52649=CARTESIAN_POINT('Ctrl Pts',(0.970853006392586,-4.60694213867371,
375.395639377299));
#52650=CARTESIAN_POINT('Ctrl Pts',(-1.34394626652729,-4.51226606546036,
375.316511501839));
#52651=CARTESIAN_POINT('Ctrl Pts',(-3.33332776428957,-3.32493525307769,
375.23738362638));
#52652=CARTESIAN_POINT('Ctrl Pts',(-4.51560361732968,-1.33271151243227,
375.158255750919));
#52653=CARTESIAN_POINT('Ctrl Pts',(-4.60446635415931,0.982571567271653,
375.07912787546));
#52654=CARTESIAN_POINT('Ctrl Pts',(-3.92033033613572,2.36677696691101,375.026375958487));
#52655=CARTESIAN_POINT('Ctrl Pts',(-3.43378788736318,2.93584158412846,375.));
#52656=CARTESIAN_POINT('Ctrl Pts',(-4.51766328535307,-0.00011344722995056,
399.112583302492));
#52657=CARTESIAN_POINT('Ctrl Pts',(-4.51713673458649,0.545949625983492,
399.093346914919));
#52658=CARTESIAN_POINT('Ctrl Pts',(-4.41799450573444,1.09219871675483,399.074110527346));
#52659=CARTESIAN_POINT('Ctrl Pts',(-4.22436256903118,1.60260114106826,399.054874139773));
#52660=CARTESIAN_POINT('Ctrl Pts',(-3.95886428330821,2.3024390448317,399.028498181286));
#52661=CARTESIAN_POINT('Ctrl Pts',(-3.51572059597365,2.93488341331845,399.002122222799));
#52662=CARTESIAN_POINT('Ctrl Pts',(-2.94858141451404,3.42336635011963,398.975746264313));
#52663=CARTESIAN_POINT('Ctrl Pts',(-2.38144223305443,3.91184928692081,398.949370305826));
#52664=CARTESIAN_POINT('Ctrl Pts',(-1.69030755746978,4.25637079203641,398.92299434734));
#52665=CARTESIAN_POINT('Ctrl Pts',(-0.958850722305057,4.4152208122577,398.896618388853));
#52666=CARTESIAN_POINT('Ctrl Pts',(-0.227393887140339,4.57407083247899,
398.870242430366));
#52667=CARTESIAN_POINT('Ctrl Pts',(0.544385107604448,4.54724936780597,398.84386647188));
#52668=CARTESIAN_POINT('Ctrl Pts',(1.26304959160632,4.33800360262792,398.817490513393));
#52669=CARTESIAN_POINT('Ctrl Pts',(1.98171407560819,4.12875783744988,398.791114554907));
#52670=CARTESIAN_POINT('Ctrl Pts',(2.64726404886714,3.73708777176682,398.76473859642));
#52671=CARTESIAN_POINT('Ctrl Pts',(3.1791236295575,3.21041157417997,398.738362637933));
#52672=CARTESIAN_POINT('Ctrl Pts',(3.71098321024786,2.68373537659312,398.711986679447));
#52673=CARTESIAN_POINT('Ctrl Pts',(4.10915239836962,2.02205304710248,398.68561072096));
#52674=CARTESIAN_POINT('Ctrl Pts',(4.32542619827246,1.30547222526591,398.659234762474));
#52675=CARTESIAN_POINT('Ctrl Pts',(4.5416999981753,0.588891403429356,398.632858803987));
#52676=CARTESIAN_POINT('Ctrl Pts',(4.57607840985923,-0.182587910753133,
398.6064828455));
#52677=CARTESIAN_POINT('Ctrl Pts',(4.42439935544928,-0.915565328667223,
398.580106887014));
#52678=CARTESIAN_POINT('Ctrl Pts',(4.27272030103931,-1.64854274658133,398.553730928527));
#52679=CARTESIAN_POINT('Ctrl Pts',(3.93498378053545,-2.34301826822704,398.527354970041));
#52680=CARTESIAN_POINT('Ctrl Pts',(3.45207841102396,-2.91491409337733,398.500979011554));
#52681=CARTESIAN_POINT('Ctrl Pts',(2.96917304151247,-3.48680991852761,398.474603053068));
#52682=CARTESIAN_POINT('Ctrl Pts',(2.34109882299336,-3.93612604718246,398.448227094581));
#52683=CARTESIAN_POINT('Ctrl Pts',(1.64389457471586,-4.20846529685206,398.421851136094));
#52684=CARTESIAN_POINT('Ctrl Pts',(0.946690326438348,-4.48080454652167,
398.395475177608));
#52685=CARTESIAN_POINT('Ctrl Pts',(0.180356048402448,-4.57616691720601,
398.369099219121));
#52686=CARTESIAN_POINT('Ctrl Pts',(-0.562330762839376,-4.483007209538,398.342723260635));
#52687=CARTESIAN_POINT('Ctrl Pts',(-1.3050175740812,-4.38984750186999,398.316347302148));
#52688=CARTESIAN_POINT('Ctrl Pts',(-2.02405691852894,-4.10816571584963,
398.289971343661));
#52689=CARTESIAN_POINT('Ctrl Pts',(-2.63239713711321,-3.67206411165684,
398.263595385175));
#52690=CARTESIAN_POINT('Ctrl Pts',(-3.24073735569747,-3.23596250746405,
398.237219426688));
#52691=CARTESIAN_POINT('Ctrl Pts',(-3.73837844841825,-2.64544108509883,
398.210843468202));
#52692=CARTESIAN_POINT('Ctrl Pts',(-4.0650726929841,-1.97199227390868,398.184467509715));
#52693=CARTESIAN_POINT('Ctrl Pts',(-4.36186009740405,-1.36019354158502,
398.160506107307));
#52694=CARTESIAN_POINT('Ctrl Pts',(-4.51756632872819,-0.679955446831048,
398.1365447049));
#52695=CARTESIAN_POINT('Ctrl Pts',(-4.51805439081064,6.66898104614677E-5,
398.112583302492));
#52696=CARTESIAN_POINT('Ctrl Pts',(-1.31303618635555,-4.90075024188347,
400.));
#52697=CARTESIAN_POINT('Ctrl Pts',(-1.45291589482402,-4.85500689927294,
400.));
#52698=CARTESIAN_POINT('Ctrl Pts',(-1.59044602699472,-4.80315746369625,
400.));
#52699=CARTESIAN_POINT('Ctrl Pts',(-1.72529743087534,-4.74548509357023,
400.));
#52700=CARTESIAN_POINT('Ctrl Pts',(-1.86151474898354,-4.68722855814354,
400.));
#52701=CARTESIAN_POINT('Ctrl Pts',(-1.99499946782598,-4.62303013629637,
400.));
#52702=CARTESIAN_POINT('Ctrl Pts',(-2.12539163452376,-4.55313283560557,
400.));
#52703=CARTESIAN_POINT('Ctrl Pts',(-2.25520494367751,-4.48354583407488,
400.));
#52704=CARTESIAN_POINT('Ctrl Pts',(-2.38195370500541,-4.40830995570903,
400.));
#52705=CARTESIAN_POINT('Ctrl Pts',(-2.50525282411489,-4.32762357969483,
400.));
#52706=CARTESIAN_POINT('Ctrl Pts',(-2.6270809920476,-4.24789978736008,400.));
#52707=CARTESIAN_POINT('Ctrl Pts',(-2.74554186145885,-4.1628542844716,400.));
#52708=CARTESIAN_POINT('Ctrl Pts',(-2.86022634881304,-4.07264517835143,
400.));
#52709=CARTESIAN_POINT('Ctrl Pts',(-2.90206457395326,-4.03973585487948,
400.));
#52710=CARTESIAN_POINT('Ctrl Pts',(-2.94339980617641,-4.00613903342865,
400.));
#52711=CARTESIAN_POINT('Ctrl Pts',(-2.98421070502804,-3.97186145992605,
400.));
#52712=CARTESIAN_POINT('Ctrl Pts',(-3.00176471409307,-3.95711763283762,
400.));
#52713=CARTESIAN_POINT('Ctrl Pts',(-3.01922333710064,-3.94224634426854,
400.));
#52714=CARTESIAN_POINT('Ctrl Pts',(-3.0365678292172,-3.92726308267954,400.));
#52715=CARTESIAN_POINT('Ctrl Pts',(-3.14698675201001,-3.83187628245151,
400.));
#52716=CARTESIAN_POINT('Ctrl Pts',(-3.25293553514171,-3.73182827889012,
400.));
#52717=CARTESIAN_POINT('Ctrl Pts',(-3.35406834590596,-3.62734196551097,
400.));
#52718=CARTESIAN_POINT('Ctrl Pts',(-3.36860939901959,-3.61231873990287,
400.));
#52719=CARTESIAN_POINT('Ctrl Pts',(-3.3830508320319,-3.59720369462607,400.));
#52720=CARTESIAN_POINT('Ctrl Pts',(-3.3973915556082,-3.58199742790278,400.));
#52721=CARTESIAN_POINT('Ctrl Pts',(-3.49724054898418,-3.4761219874308,400.));
#52722=CARTESIAN_POINT('Ctrl Pts',(-3.59221081092533,-3.36582685075802,
400.));
#52723=CARTESIAN_POINT('Ctrl Pts',(-3.68210185106465,-3.25150412359693,
400.));
#52724=CARTESIAN_POINT('Ctrl Pts',(-3.77205159485829,-3.13710673758391,
400.));
#52725=CARTESIAN_POINT('Ctrl Pts',(-3.85691583765602,-3.01867577562728,
400.));
#52726=CARTESIAN_POINT('Ctrl Pts',(-3.93644802914845,-2.89657936297904,
400.));
#52727=CARTESIAN_POINT('Ctrl Pts',(-4.00696577927717,-2.78832176115549,
400.));
#52728=CARTESIAN_POINT('Ctrl Pts',(-4.07329120966267,-2.67718185514111,
400.));
#52729=CARTESIAN_POINT('Ctrl Pts',(-4.13521902572865,-2.56340683612714,
400.));
#52730=CARTESIAN_POINT('Ctrl Pts',(-4.14927174249539,-2.53758890455934,
400.));
#52731=CARTESIAN_POINT('Ctrl Pts',(-4.16309787710306,-2.511635261477,400.));
#52732=CARTESIAN_POINT('Ctrl Pts',(-4.17669478808166,-2.48554876582588,
400.));
#52733=CARTESIAN_POINT('Ctrl Pts',(-4.18567658693009,-2.46831664178184,
400.));
#52734=CARTESIAN_POINT('Ctrl Pts',(-4.19455855900594,-2.45102602806576,
400.));
#52735=CARTESIAN_POINT('Ctrl Pts',(-4.20333295387386,-2.43369188245622,
400.));
#52736=CARTESIAN_POINT('Ctrl Pts',(-4.26826574456287,-2.30541472311025,
400.));
#52737=CARTESIAN_POINT('Ctrl Pts',(-4.32740788322074,-2.17457173953832,
400.));
#52738=CARTESIAN_POINT('Ctrl Pts',(-4.38057216155237,-2.04153956135574,
400.));
#52739=CARTESIAN_POINT('Ctrl Pts',(-4.43343069026291,-1.90927245587513,
400.));
#52740=CARTESIAN_POINT('Ctrl Pts',(-4.48038018757078,-1.77484054207341,
400.));
#52741=CARTESIAN_POINT('Ctrl Pts',(-4.52118875294636,-1.63859604986007,
400.));
#52742=CARTESIAN_POINT('Ctrl Pts',(-4.53639547739945,-1.58782650105892,
400.));
#52743=CARTESIAN_POINT('Ctrl Pts',(-4.55074898869301,-1.53680513764063,
400.));
#52744=CARTESIAN_POINT('Ctrl Pts',(-4.56423545493657,-1.48554984951531,
400.));
#52745=CARTESIAN_POINT('Ctrl Pts',(-4.60065397684761,-1.34714132945246,
400.));
#52746=CARTESIAN_POINT('Ctrl Pts',(-4.63075368245775,-1.20702677925683,
400.));
#52747=CARTESIAN_POINT('Ctrl Pts',(-4.65449674508562,-1.06564398750406,
400.));
#52748=CARTESIAN_POINT('Ctrl Pts',(-4.6677938749007,-0.986463581630512,
400.));
#52749=CARTESIAN_POINT('Ctrl Pts',(-4.67909632529634,-0.906885415400295,
400.));
#52750=CARTESIAN_POINT('Ctrl Pts',(-4.68839036132626,-0.826987472477294,
400.));
#52751=CARTESIAN_POINT('Ctrl Pts',(-4.69350021378828,-0.783059656936131,
400.));
#52752=CARTESIAN_POINT('Ctrl Pts',(-4.69800287543295,-0.73903519996531,
400.));
#52753=CARTESIAN_POINT('Ctrl Pts',(-4.70189541038099,-0.69492725727482,
400.));
#52754=CARTESIAN_POINT('Ctrl Pts',(-4.70335699391325,-0.678365442534775,
400.));
#52755=CARTESIAN_POINT('Ctrl Pts',(-4.70473233460286,-0.661793969471143,
400.));
#52756=CARTESIAN_POINT('Ctrl Pts',(-4.70602072340745,-0.645222510455179,
400.));
#52757=CARTESIAN_POINT('Ctrl Pts',(-4.71697947907218,-0.504269275129255,
400.));
#52758=CARTESIAN_POINT('Ctrl Pts',(-4.72166837458957,-0.363132695636631,
400.));
#52759=CARTESIAN_POINT('Ctrl Pts',(-4.7201177742283,-0.222235244668839,
400.));
#52760=CARTESIAN_POINT('Ctrl Pts',(-4.71856870881553,-0.0814772689241232,
400.));
#52761=CARTESIAN_POINT('Ctrl Pts',(-4.71079242396856,0.0590428483946887,
400.));
#52762=CARTESIAN_POINT('Ctrl Pts',(-4.69676735600276,0.19890200600945,400.));
#52763=CARTESIAN_POINT('Ctrl Pts',(-4.68295624998761,0.33662751705272,400.));
#52764=CARTESIAN_POINT('Ctrl Pts',(-4.66308539592085,0.473712790055481,
400.));
#52765=CARTESIAN_POINT('Ctrl Pts',(-4.63708587274883,0.609740845579473,
400.));
#52766=CARTESIAN_POINT('Ctrl Pts',(-4.62194193613231,0.6889730775437,400.));
#52767=CARTESIAN_POINT('Ctrl Pts',(-4.60471782759541,0.767846329349665,
400.));
#52768=CARTESIAN_POINT('Ctrl Pts',(-4.58539250818854,0.846274698465189,
400.));
#52769=CARTESIAN_POINT('Ctrl Pts',(-4.57105296447468,0.904469184344614,
400.));
#52770=CARTESIAN_POINT('Ctrl Pts',(-4.55555640760633,0.962418671522469,
400.));
#52771=CARTESIAN_POINT('Ctrl Pts',(-4.53891410477628,1.02009082935325,400.));
#52772=CARTESIAN_POINT('Ctrl Pts',(-4.53055828962656,1.04904703181158,400.));
#52773=CARTESIAN_POINT('Ctrl Pts',(-4.52191362534324,1.07793330641511,400.));
#52774=CARTESIAN_POINT('Ctrl Pts',(-4.51298141319226,1.1067454537709,400.));
#52775=CARTESIAN_POINT('Ctrl Pts',(-4.50751626468392,1.12437408388872,400.));
#52776=CARTESIAN_POINT('Ctrl Pts',(-4.50194375351087,1.14197390912326,400.));
#52777=CARTESIAN_POINT('Ctrl Pts',(-4.49626740324529,1.15953444897625,400.));
#52778=CARTESIAN_POINT('Ctrl Pts',(-4.45341464273149,1.29210512795207,400.));
#52779=CARTESIAN_POINT('Ctrl Pts',(-4.4046021744809,1.42258699257377,400.));
#52780=CARTESIAN_POINT('Ctrl Pts',(-4.35004408840361,1.55060321390413,400.));
#52781=CARTESIAN_POINT('Ctrl Pts',(-4.29958883856276,1.66899245545036,400.));
#52782=CARTESIAN_POINT('Ctrl Pts',(-4.24421884943669,1.7852731960868,400.));
#52783=CARTESIAN_POINT('Ctrl Pts',(-4.18406982393872,1.89912668839153,400.));
#52784=CARTESIAN_POINT('Ctrl Pts',(-4.15968128005935,1.94529070966877,400.));
#52785=CARTESIAN_POINT('Ctrl Pts',(-4.13450669520302,1.99105541062324,400.));
#52786=CARTESIAN_POINT('Ctrl Pts',(-4.10855377241811,2.03639833327113,400.));
#52787=CARTESIAN_POINT('Ctrl Pts',(-4.09598731345164,2.05835347033207,400.));
#52788=CARTESIAN_POINT('Ctrl Pts',(-4.08323760980602,2.0802109712186,400.));
#52789=CARTESIAN_POINT('Ctrl Pts',(-4.07030781226104,2.10196429342508,400.));
#52790=CARTESIAN_POINT('Ctrl Pts',(-3.9998914613058,2.22043401931249,400.));
#52791=CARTESIAN_POINT('Ctrl Pts',(-3.92427608656828,2.33558378339706,400.));
#52792=CARTESIAN_POINT('Ctrl Pts',(-3.84364635340467,2.44703278518893,400.));
#52793=CARTESIAN_POINT('Ctrl Pts',(-3.76407407271829,2.55702014226977,400.));
#52794=CARTESIAN_POINT('Ctrl Pts',(-3.67961761227173,2.66340373121656,400.));
#52795=CARTESIAN_POINT('Ctrl Pts',(-3.59041821150276,2.76578232711007,400.));
#52796=CARTESIAN_POINT('Ctrl Pts',(-3.56727357293573,2.79234658178586,400.));
#52797=CARTESIAN_POINT('Ctrl Pts',(-3.5438094445685,2.81864098904491,400.));
#52798=CARTESIAN_POINT('Ctrl Pts',(-3.52002794801113,2.84465807439287,400.));
#52799=CARTESIAN_POINT('Ctrl Pts',(-3.49182454546321,2.87551274871592,400.));
#52800=CARTESIAN_POINT('Ctrl Pts',(-3.46317478144493,2.90597739162215,400.));
#52801=CARTESIAN_POINT('Ctrl Pts',(-3.43408816619831,2.93604416807489,400.));
#52802=CARTESIAN_POINT('Origin',(0.,0.,387.));
#52803=CARTESIAN_POINT('Origin',(0.,0.,374.));
#52804=CARTESIAN_POINT('',(-4.,-4.89858719658941E-16,374.));
#52805=CARTESIAN_POINT('Origin',(0.,0.,374.));
#52806=CARTESIAN_POINT('Origin',(-17.,5.,0.));
#52807=CARTESIAN_POINT('',(-16.,5.,400.));
#52808=CARTESIAN_POINT('',(-17.,4.,400.));
#52809=CARTESIAN_POINT('Origin',(-17.,5.,400.));
#52810=CARTESIAN_POINT('',(-17.,4.,0.));
#52811=CARTESIAN_POINT('',(-17.,4.,0.));
#52812=CARTESIAN_POINT('',(-16.,5.,0.));
#52813=CARTESIAN_POINT('Origin',(-17.,5.,0.));
#52814=CARTESIAN_POINT('',(-16.,5.,0.));
#52815=CARTESIAN_POINT('Origin',(-20.,4.,0.));
#52816=CARTESIAN_POINT('',(-19.,4.,400.));
#52817=CARTESIAN_POINT('',(-16.,4.,400.));
#52818=CARTESIAN_POINT('',(-19.,4.,0.));
#52819=CARTESIAN_POINT('',(-19.,4.,0.));
#52820=CARTESIAN_POINT('',(-16.,4.,0.));
#52821=CARTESIAN_POINT('Origin',(0.,0.,400.));
#52822=CARTESIAN_POINT('',(-16.,6.,400.));
#52823=CARTESIAN_POINT('',(-16.,7.,400.));
#52824=CARTESIAN_POINT('',(-15.,7.,400.));
#52825=CARTESIAN_POINT('Origin',(-15.,6.,400.));
#52826=CARTESIAN_POINT('',(-9.,7.,400.));
#52827=CARTESIAN_POINT('',(-8.,7.,400.));
#52828=CARTESIAN_POINT('',(-8.,6.,400.));
#52829=CARTESIAN_POINT('Origin',(-9.,6.,400.));
#52830=CARTESIAN_POINT('',(-8.,-6.,400.));
#52831=CARTESIAN_POINT('',(-8.,-7.,400.));
#52832=CARTESIAN_POINT('',(-9.,-7.,400.));
#52833=CARTESIAN_POINT('Origin',(-9.,-6.,400.));
#52834=CARTESIAN_POINT('',(-15.,-7.,400.));
#52835=CARTESIAN_POINT('',(-16.,-7.,400.));
#52836=CARTESIAN_POINT('',(-16.,-6.,400.));
#52837=CARTESIAN_POINT('Origin',(-15.,-6.,400.));
#52838=CARTESIAN_POINT('',(-16.,-5.,400.));
#52839=CARTESIAN_POINT('',(-16.,-4.,400.));
#52840=CARTESIAN_POINT('',(-17.,-4.,400.));
#52841=CARTESIAN_POINT('Origin',(-17.,-5.,400.));
#52842=CARTESIAN_POINT('',(-19.,-4.,400.));
#52843=CARTESIAN_POINT('',(-20.,-4.,400.));
#52844=CARTESIAN_POINT('',(-20.,-5.,400.));
#52845=CARTESIAN_POINT('Origin',(-19.,-5.,400.));
#52846=CARTESIAN_POINT('',(-20.,-19.,400.));
#52847=CARTESIAN_POINT('',(-20.,-20.,400.));
#52848=CARTESIAN_POINT('',(-19.,-20.,400.));
#52849=CARTESIAN_POINT('Origin',(-19.,-19.,400.));
#52850=CARTESIAN_POINT('',(-5.,-20.,400.));
#52851=CARTESIAN_POINT('',(-4.,-20.,400.));
#52852=CARTESIAN_POINT('',(-4.,-19.,400.));
#52853=CARTESIAN_POINT('Origin',(-5.,-19.,400.));
#52854=CARTESIAN_POINT('',(-4.,-17.,400.));
#52855=CARTESIAN_POINT('',(-4.,-16.,400.));
#52856=CARTESIAN_POINT('',(-5.,-16.,400.));
#52857=CARTESIAN_POINT('Origin',(-5.,-17.,400.));
#52858=CARTESIAN_POINT('',(-6.,-16.,400.));
#52859=CARTESIAN_POINT('',(-7.,-16.,400.));
#52860=CARTESIAN_POINT('',(-7.,-15.,400.));
#52861=CARTESIAN_POINT('Origin',(-6.,-15.,400.));
#52862=CARTESIAN_POINT('',(-7.,-9.,400.));
#52863=CARTESIAN_POINT('',(-7.,-8.,400.));
#52864=CARTESIAN_POINT('',(-6.,-8.,400.));
#52865=CARTESIAN_POINT('Origin',(-6.,-9.,400.));
#52866=CARTESIAN_POINT('',(6.,-8.,400.));
#52867=CARTESIAN_POINT('',(7.,-8.,400.));
#52868=CARTESIAN_POINT('',(7.,-9.,400.));
#52869=CARTESIAN_POINT('Origin',(6.,-9.,400.));
#52870=CARTESIAN_POINT('',(7.,-15.,400.));
#52871=CARTESIAN_POINT('',(7.,-16.,400.));
#52872=CARTESIAN_POINT('',(6.,-16.,400.));
#52873=CARTESIAN_POINT('Origin',(6.,-15.,400.));
#52874=CARTESIAN_POINT('',(5.,-16.,400.));
#52875=CARTESIAN_POINT('',(4.,-16.,400.));
#52876=CARTESIAN_POINT('',(4.,-17.,400.));
#52877=CARTESIAN_POINT('Origin',(5.,-17.,400.));
#52878=CARTESIAN_POINT('',(4.,-19.,400.));
#52879=CARTESIAN_POINT('',(4.,-20.,400.));
#52880=CARTESIAN_POINT('',(5.,-20.,400.));
#52881=CARTESIAN_POINT('Origin',(5.,-19.,400.));
#52882=CARTESIAN_POINT('',(19.,-20.,400.));
#52883=CARTESIAN_POINT('',(20.,-20.,400.));
#52884=CARTESIAN_POINT('',(20.,-19.,400.));
#52885=CARTESIAN_POINT('Origin',(19.,-19.,400.));
#52886=CARTESIAN_POINT('',(20.,-5.,400.));
#52887=CARTESIAN_POINT('',(20.,-4.,400.));
#52888=CARTESIAN_POINT('',(19.,-4.,400.));
#52889=CARTESIAN_POINT('Origin',(19.,-5.,400.));
#52890=CARTESIAN_POINT('',(17.,-4.,400.));
#52891=CARTESIAN_POINT('',(16.,-4.,400.));
#52892=CARTESIAN_POINT('',(16.,-5.,400.));
#52893=CARTESIAN_POINT('Origin',(17.,-5.,400.));
#52894=CARTESIAN_POINT('',(16.,-6.,400.));
#52895=CARTESIAN_POINT('',(16.,-7.,400.));
#52896=CARTESIAN_POINT('',(15.,-7.,400.));
#52897=CARTESIAN_POINT('Origin',(15.,-6.,400.));
#52898=CARTESIAN_POINT('',(9.,-7.,400.));
#52899=CARTESIAN_POINT('',(8.,-7.,400.));
#52900=CARTESIAN_POINT('',(8.,-6.,400.));
#52901=CARTESIAN_POINT('Origin',(9.,-6.,400.));
#52902=CARTESIAN_POINT('',(8.,6.,400.));
#52903=CARTESIAN_POINT('',(8.,7.,400.));
#52904=CARTESIAN_POINT('',(9.,7.,400.));
#52905=CARTESIAN_POINT('Origin',(9.,6.,400.));
#52906=CARTESIAN_POINT('',(15.,7.,400.));
#52907=CARTESIAN_POINT('',(16.,7.,400.));
#52908=CARTESIAN_POINT('',(16.,6.,400.));
#52909=CARTESIAN_POINT('Origin',(15.,6.,400.));
#52910=CARTESIAN_POINT('',(16.,5.,400.));
#52911=CARTESIAN_POINT('',(16.,4.,400.));
#52912=CARTESIAN_POINT('',(17.,4.,400.));
#52913=CARTESIAN_POINT('Origin',(17.,5.,400.));
#52914=CARTESIAN_POINT('',(19.,4.,400.));
#52915=CARTESIAN_POINT('',(20.,4.,400.));
#52916=CARTESIAN_POINT('',(20.,5.,400.));
#52917=CARTESIAN_POINT('Origin',(19.,5.,400.));
#52918=CARTESIAN_POINT('',(20.,19.,400.));
#52919=CARTESIAN_POINT('',(20.,20.,400.));
#52920=CARTESIAN_POINT('',(19.,20.,400.));
#52921=CARTESIAN_POINT('Origin',(19.,19.,400.));
#52922=CARTESIAN_POINT('',(5.,20.,400.));
#52923=CARTESIAN_POINT('',(4.,20.,400.));
#52924=CARTESIAN_POINT('',(4.,19.,400.));
#52925=CARTESIAN_POINT('Origin',(5.,19.,400.));
#52926=CARTESIAN_POINT('',(4.,17.,400.));
#52927=CARTESIAN_POINT('',(4.,16.,400.));
#52928=CARTESIAN_POINT('',(5.,16.,400.));
#52929=CARTESIAN_POINT('Origin',(5.,17.,400.));
#52930=CARTESIAN_POINT('',(6.,16.,400.));
#52931=CARTESIAN_POINT('',(7.,16.,400.));
#52932=CARTESIAN_POINT('',(7.,15.,400.));
#52933=CARTESIAN_POINT('Origin',(6.,15.,400.));
#52934=CARTESIAN_POINT('',(7.,9.,400.));
#52935=CARTESIAN_POINT('',(7.,8.,400.));
#52936=CARTESIAN_POINT('',(6.,8.,400.));
#52937=CARTESIAN_POINT('Origin',(6.,9.,400.));
#52938=CARTESIAN_POINT('',(-6.,8.,400.));
#52939=CARTESIAN_POINT('',(-7.,8.,400.));
#52940=CARTESIAN_POINT('',(-7.,9.,400.));
#52941=CARTESIAN_POINT('Origin',(-6.,9.,400.));
#52942=CARTESIAN_POINT('',(-7.,15.,400.));
#52943=CARTESIAN_POINT('',(-7.,16.,400.));
#52944=CARTESIAN_POINT('',(-6.,16.,400.));
#52945=CARTESIAN_POINT('Origin',(-6.,15.,400.));
#52946=CARTESIAN_POINT('',(-5.,16.,400.));
#52947=CARTESIAN_POINT('',(-4.,16.,400.));
#52948=CARTESIAN_POINT('',(-4.,17.,400.));
#52949=CARTESIAN_POINT('Origin',(-5.,17.,400.));
#52950=CARTESIAN_POINT('',(-4.,19.,400.));
#52951=CARTESIAN_POINT('',(-4.,20.,400.));
#52952=CARTESIAN_POINT('',(-5.,20.,400.));
#52953=CARTESIAN_POINT('Origin',(-5.,19.,400.));
#52954=CARTESIAN_POINT('',(-19.,20.,400.));
#52955=CARTESIAN_POINT('',(-20.,20.,400.));
#52956=CARTESIAN_POINT('',(-20.,19.,400.));
#52957=CARTESIAN_POINT('Origin',(-19.,19.,400.));
#52958=CARTESIAN_POINT('',(-20.,5.,400.));
#52959=CARTESIAN_POINT('',(-20.,4.,400.));
#52960=CARTESIAN_POINT('Origin',(-19.,5.,400.));
#52961=CARTESIAN_POINT('',(-15.,-12.,400.));
#52962=CARTESIAN_POINT('Origin',(-12.,-12.,400.));
#52963=CARTESIAN_POINT('',(-15.,12.,400.));
#52964=CARTESIAN_POINT('Origin',(-12.,12.,400.));
#52965=CARTESIAN_POINT('',(9.,12.,400.));
#52966=CARTESIAN_POINT('Origin',(12.,12.,400.));
#52967=CARTESIAN_POINT('',(9.,-12.,400.));
#52968=CARTESIAN_POINT('Origin',(12.,-12.,400.));
#52969=CARTESIAN_POINT('Origin',(-15.,6.,0.));
#52970=CARTESIAN_POINT('',(-16.,6.,0.));
#52971=CARTESIAN_POINT('',(-15.,7.,0.));
#52972=CARTESIAN_POINT('Origin',(-15.,6.,0.));
#52973=CARTESIAN_POINT('',(-15.,7.,0.));
#52974=CARTESIAN_POINT('',(-16.,6.,0.));
#52975=CARTESIAN_POINT('Origin',(-16.,7.,0.));
#52976=CARTESIAN_POINT('',(-9.,7.,0.));
#52977=CARTESIAN_POINT('',(-8.,7.,0.));
#52978=CARTESIAN_POINT('',(-9.,7.,0.));
#52979=CARTESIAN_POINT('Origin',(-9.,6.,0.));
#52980=CARTESIAN_POINT('',(-8.,6.,0.));
#52981=CARTESIAN_POINT('Origin',(-9.,6.,0.));
#52982=CARTESIAN_POINT('',(-8.,6.,0.));
#52983=CARTESIAN_POINT('Origin',(-8.,7.,0.));
#52984=CARTESIAN_POINT('',(-8.,-6.,0.));
#52985=CARTESIAN_POINT('',(-8.,-7.,0.));
#52986=CARTESIAN_POINT('',(-8.,-6.,0.));
#52987=CARTESIAN_POINT('Origin',(-9.,-6.,0.));
#52988=CARTESIAN_POINT('',(-9.,-7.,0.));
#52989=CARTESIAN_POINT('Origin',(-9.,-6.,0.));
#52990=CARTESIAN_POINT('',(-9.,-7.,0.));
#52991=CARTESIAN_POINT('Origin',(-8.,-7.,0.));
#52992=CARTESIAN_POINT('',(-15.,-7.,0.));
#52993=CARTESIAN_POINT('',(-16.,-7.,0.));
#52994=CARTESIAN_POINT('',(-15.,-7.,0.));
#52995=CARTESIAN_POINT('Origin',(-15.,-6.,0.));
#52996=CARTESIAN_POINT('',(-16.,-6.,0.));
#52997=CARTESIAN_POINT('Origin',(-15.,-6.,0.));
#52998=CARTESIAN_POINT('',(-16.,-6.,0.));
#52999=CARTESIAN_POINT('Origin',(-16.,-7.,0.));
#53000=CARTESIAN_POINT('',(-16.,-5.,0.));
#53001=CARTESIAN_POINT('',(-16.,-4.,0.));
#53002=CARTESIAN_POINT('',(-16.,-5.,0.));
#53003=CARTESIAN_POINT('Origin',(-17.,-5.,0.));
#53004=CARTESIAN_POINT('',(-17.,-4.,0.));
#53005=CARTESIAN_POINT('Origin',(-17.,-5.,0.));
#53006=CARTESIAN_POINT('',(-17.,-4.,0.));
#53007=CARTESIAN_POINT('Origin',(-19.,-5.,0.));
#53008=CARTESIAN_POINT('',(-19.,-4.,0.));
#53009=CARTESIAN_POINT('',(-19.,-4.,0.));
#53010=CARTESIAN_POINT('',(-20.,-5.,0.));
#53011=CARTESIAN_POINT('Origin',(-19.,-5.,0.));
#53012=CARTESIAN_POINT('',(-20.,-5.,0.));
#53013=CARTESIAN_POINT('Origin',(-20.,-4.,0.));
#53014=CARTESIAN_POINT('',(-20.,-19.,0.));
#53015=CARTESIAN_POINT('',(-20.,-20.,0.));
#53016=CARTESIAN_POINT('',(-20.,-19.,0.));
#53017=CARTESIAN_POINT('Origin',(-19.,-19.,0.));
#53018=CARTESIAN_POINT('',(-19.,-20.,0.));
#53019=CARTESIAN_POINT('Origin',(-19.,-19.,0.));
#53020=CARTESIAN_POINT('',(-19.,-20.,0.));
#53021=CARTESIAN_POINT('Origin',(-5.,-19.,0.));
#53022=CARTESIAN_POINT('',(-5.,-20.,0.));
#53023=CARTESIAN_POINT('',(-5.,-20.,0.));
#53024=CARTESIAN_POINT('',(-4.,-19.,0.));
#53025=CARTESIAN_POINT('Origin',(-5.,-19.,0.));
#53026=CARTESIAN_POINT('',(-4.,-19.,0.));
#53027=CARTESIAN_POINT('Origin',(-4.,-20.,0.));
#53028=CARTESIAN_POINT('',(-4.,-17.,0.));
#53029=CARTESIAN_POINT('',(-4.,-16.,0.));
#53030=CARTESIAN_POINT('',(-4.,-17.,0.));
#53031=CARTESIAN_POINT('Origin',(-5.,-17.,0.));
#53032=CARTESIAN_POINT('',(-5.,-16.,0.));
#53033=CARTESIAN_POINT('Origin',(-5.,-17.,0.));
#53034=CARTESIAN_POINT('',(-5.,-16.,0.));
#53035=CARTESIAN_POINT('Origin',(-6.,-15.,0.));
#53036=CARTESIAN_POINT('',(-6.,-16.,0.));
#53037=CARTESIAN_POINT('',(-7.,-15.,0.));
#53038=CARTESIAN_POINT('Origin',(-6.,-15.,0.));
#53039=CARTESIAN_POINT('',(-7.,-15.,0.));
#53040=CARTESIAN_POINT('',(-6.,-16.,0.));
#53041=CARTESIAN_POINT('Origin',(-7.,-16.,0.));
#53042=CARTESIAN_POINT('',(-7.,-9.,0.));
#53043=CARTESIAN_POINT('',(-7.,-8.,0.));
#53044=CARTESIAN_POINT('',(-7.,-9.,0.));
#53045=CARTESIAN_POINT('Origin',(-6.,-9.,0.));
#53046=CARTESIAN_POINT('',(-6.,-8.,0.));
#53047=CARTESIAN_POINT('Origin',(-6.,-9.,0.));
#53048=CARTESIAN_POINT('',(-6.,-8.,0.));
#53049=CARTESIAN_POINT('Origin',(-7.,-8.,0.));
#53050=CARTESIAN_POINT('',(6.,-8.,0.));
#53051=CARTESIAN_POINT('',(7.,-8.,0.));
#53052=CARTESIAN_POINT('',(6.,-8.,0.));
#53053=CARTESIAN_POINT('Origin',(6.,-9.,0.));
#53054=CARTESIAN_POINT('',(7.,-9.,0.));
#53055=CARTESIAN_POINT('Origin',(6.,-9.,0.));
#53056=CARTESIAN_POINT('',(7.,-9.,0.));
#53057=CARTESIAN_POINT('Origin',(7.,-8.,0.));
#53058=CARTESIAN_POINT('',(7.,-15.,0.));
#53059=CARTESIAN_POINT('',(7.,-16.,0.));
#53060=CARTESIAN_POINT('',(7.,-15.,0.));
#53061=CARTESIAN_POINT('Origin',(6.,-15.,0.));
#53062=CARTESIAN_POINT('',(6.,-16.,0.));
#53063=CARTESIAN_POINT('Origin',(6.,-15.,0.));
#53064=CARTESIAN_POINT('',(6.,-16.,0.));
#53065=CARTESIAN_POINT('Origin',(7.,-16.,0.));
#53066=CARTESIAN_POINT('',(5.,-16.,0.));
#53067=CARTESIAN_POINT('',(4.,-16.,0.));
#53068=CARTESIAN_POINT('',(5.,-16.,0.));
#53069=CARTESIAN_POINT('Origin',(5.,-17.,0.));
#53070=CARTESIAN_POINT('',(4.,-17.,0.));
#53071=CARTESIAN_POINT('Origin',(5.,-17.,0.));
#53072=CARTESIAN_POINT('',(4.,-17.,0.));
#53073=CARTESIAN_POINT('Origin',(5.,-19.,0.));
#53074=CARTESIAN_POINT('',(4.,-19.,0.));
#53075=CARTESIAN_POINT('',(4.,-19.,0.));
#53076=CARTESIAN_POINT('',(5.,-20.,0.));
#53077=CARTESIAN_POINT('Origin',(5.,-19.,0.));
#53078=CARTESIAN_POINT('',(5.,-20.,0.));
#53079=CARTESIAN_POINT('Origin',(4.,-20.,0.));
#53080=CARTESIAN_POINT('',(19.,-20.,0.));
#53081=CARTESIAN_POINT('',(20.,-20.,0.));
#53082=CARTESIAN_POINT('',(19.,-20.,0.));
#53083=CARTESIAN_POINT('Origin',(19.,-19.,0.));
#53084=CARTESIAN_POINT('',(20.,-19.,0.));
#53085=CARTESIAN_POINT('Origin',(19.,-19.,0.));
#53086=CARTESIAN_POINT('',(20.,-19.,0.));
#53087=CARTESIAN_POINT('Origin',(19.,-5.,0.));
#53088=CARTESIAN_POINT('',(20.,-5.,0.));
#53089=CARTESIAN_POINT('',(20.,-5.,0.));
#53090=CARTESIAN_POINT('',(19.,-4.,0.));
#53091=CARTESIAN_POINT('Origin',(19.,-5.,0.));
#53092=CARTESIAN_POINT('',(19.,-4.,0.));
#53093=CARTESIAN_POINT('Origin',(20.,-4.,0.));
#53094=CARTESIAN_POINT('',(17.,-4.,0.));
#53095=CARTESIAN_POINT('',(16.,-4.,0.));
#53096=CARTESIAN_POINT('',(17.,-4.,0.));
#53097=CARTESIAN_POINT('Origin',(17.,-5.,0.));
#53098=CARTESIAN_POINT('',(16.,-5.,0.));
#53099=CARTESIAN_POINT('Origin',(17.,-5.,0.));
#53100=CARTESIAN_POINT('',(16.,-5.,0.));
#53101=CARTESIAN_POINT('Origin',(15.,-6.,0.));
#53102=CARTESIAN_POINT('',(16.,-6.,0.));
#53103=CARTESIAN_POINT('',(15.,-7.,0.));
#53104=CARTESIAN_POINT('Origin',(15.,-6.,0.));
#53105=CARTESIAN_POINT('',(15.,-7.,0.));
#53106=CARTESIAN_POINT('',(16.,-6.,0.));
#53107=CARTESIAN_POINT('Origin',(16.,-7.,0.));
#53108=CARTESIAN_POINT('',(9.,-7.,0.));
#53109=CARTESIAN_POINT('',(8.,-7.,0.));
#53110=CARTESIAN_POINT('',(9.,-7.,0.));
#53111=CARTESIAN_POINT('Origin',(9.,-6.,0.));
#53112=CARTESIAN_POINT('',(8.,-6.,0.));
#53113=CARTESIAN_POINT('Origin',(9.,-6.,0.));
#53114=CARTESIAN_POINT('',(8.,-6.,0.));
#53115=CARTESIAN_POINT('Origin',(8.,-7.,0.));
#53116=CARTESIAN_POINT('',(8.,6.,0.));
#53117=CARTESIAN_POINT('',(8.,7.,0.));
#53118=CARTESIAN_POINT('',(8.,6.,0.));
#53119=CARTESIAN_POINT('Origin',(9.,6.,0.));
#53120=CARTESIAN_POINT('',(9.,7.,0.));
#53121=CARTESIAN_POINT('Origin',(9.,6.,0.));
#53122=CARTESIAN_POINT('',(9.,7.,0.));
#53123=CARTESIAN_POINT('Origin',(8.,7.,0.));
#53124=CARTESIAN_POINT('',(15.,7.,0.));
#53125=CARTESIAN_POINT('',(16.,7.,0.));
#53126=CARTESIAN_POINT('',(15.,7.,0.));
#53127=CARTESIAN_POINT('Origin',(15.,6.,0.));
#53128=CARTESIAN_POINT('',(16.,6.,0.));
#53129=CARTESIAN_POINT('Origin',(15.,6.,0.));
#53130=CARTESIAN_POINT('',(16.,6.,0.));
#53131=CARTESIAN_POINT('Origin',(16.,7.,0.));
#53132=CARTESIAN_POINT('',(16.,5.,0.));
#53133=CARTESIAN_POINT('',(16.,4.,0.));
#53134=CARTESIAN_POINT('',(16.,5.,0.));
#53135=CARTESIAN_POINT('Origin',(17.,5.,0.));
#53136=CARTESIAN_POINT('',(17.,4.,0.));
#53137=CARTESIAN_POINT('Origin',(17.,5.,0.));
#53138=CARTESIAN_POINT('',(17.,4.,0.));
#53139=CARTESIAN_POINT('Origin',(19.,5.,0.));
#53140=CARTESIAN_POINT('',(19.,4.,0.));
#53141=CARTESIAN_POINT('',(19.,4.,0.));
#53142=CARTESIAN_POINT('',(20.,5.,0.));
#53143=CARTESIAN_POINT('Origin',(19.,5.,0.));
#53144=CARTESIAN_POINT('',(20.,5.,0.));
#53145=CARTESIAN_POINT('Origin',(20.,4.,0.));
#53146=CARTESIAN_POINT('',(20.,19.,0.));
#53147=CARTESIAN_POINT('',(20.,20.,0.));
#53148=CARTESIAN_POINT('',(20.,19.,0.));
#53149=CARTESIAN_POINT('Origin',(19.,19.,0.));
#53150=CARTESIAN_POINT('',(19.,20.,0.));
#53151=CARTESIAN_POINT('Origin',(19.,19.,0.));
#53152=CARTESIAN_POINT('',(19.,20.,0.));
#53153=CARTESIAN_POINT('Origin',(5.,19.,0.));
#53154=CARTESIAN_POINT('',(5.,20.,0.));
#53155=CARTESIAN_POINT('',(5.,20.,0.));
#53156=CARTESIAN_POINT('',(4.,19.,0.));
#53157=CARTESIAN_POINT('Origin',(5.,19.,0.));
#53158=CARTESIAN_POINT('',(4.,19.,0.));
#53159=CARTESIAN_POINT('Origin',(4.,20.,0.));
#53160=CARTESIAN_POINT('',(4.,17.,0.));
#53161=CARTESIAN_POINT('',(4.,16.,0.));
#53162=CARTESIAN_POINT('',(4.,17.,0.));
#53163=CARTESIAN_POINT('Origin',(5.,17.,0.));
#53164=CARTESIAN_POINT('',(5.,16.,0.));
#53165=CARTESIAN_POINT('Origin',(5.,17.,0.));
#53166=CARTESIAN_POINT('',(5.,16.,0.));
#53167=CARTESIAN_POINT('Origin',(6.,15.,0.));
#53168=CARTESIAN_POINT('',(6.,16.,0.));
#53169=CARTESIAN_POINT('',(7.,15.,0.));
#53170=CARTESIAN_POINT('Origin',(6.,15.,0.));
#53171=CARTESIAN_POINT('',(7.,15.,0.));
#53172=CARTESIAN_POINT('',(6.,16.,0.));
#53173=CARTESIAN_POINT('Origin',(7.,16.,0.));
#53174=CARTESIAN_POINT('',(7.,9.,0.));
#53175=CARTESIAN_POINT('',(7.,8.,0.));
#53176=CARTESIAN_POINT('',(7.,9.,0.));
#53177=CARTESIAN_POINT('Origin',(6.,9.,0.));
#53178=CARTESIAN_POINT('',(6.,8.,0.));
#53179=CARTESIAN_POINT('Origin',(6.,9.,0.));
#53180=CARTESIAN_POINT('',(6.,8.,0.));
#53181=CARTESIAN_POINT('Origin',(7.,8.,0.));
#53182=CARTESIAN_POINT('',(-6.,8.,0.));
#53183=CARTESIAN_POINT('',(-7.,8.,0.));
#53184=CARTESIAN_POINT('',(-6.,8.,0.));
#53185=CARTESIAN_POINT('Origin',(-6.,9.,0.));
#53186=CARTESIAN_POINT('',(-7.,9.,0.));
#53187=CARTESIAN_POINT('Origin',(-6.,9.,0.));
#53188=CARTESIAN_POINT('',(-7.,9.,0.));
#53189=CARTESIAN_POINT('Origin',(-7.,8.,0.));
#53190=CARTESIAN_POINT('',(-7.,15.,0.));
#53191=CARTESIAN_POINT('',(-7.,16.,0.));
#53192=CARTESIAN_POINT('',(-7.,15.,0.));
#53193=CARTESIAN_POINT('Origin',(-6.,15.,0.));
#53194=CARTESIAN_POINT('',(-6.,16.,0.));
#53195=CARTESIAN_POINT('Origin',(-6.,15.,0.));
#53196=CARTESIAN_POINT('',(-6.,16.,0.));
#53197=CARTESIAN_POINT('Origin',(-7.,16.,0.));
#53198=CARTESIAN_POINT('',(-5.,16.,0.));
#53199=CARTESIAN_POINT('',(-4.,16.,0.));
#53200=CARTESIAN_POINT('',(-5.,16.,0.));
#53201=CARTESIAN_POINT('Origin',(-5.,17.,0.));
#53202=CARTESIAN_POINT('',(-4.,17.,0.));
#53203=CARTESIAN_POINT('Origin',(-5.,17.,0.));
#53204=CARTESIAN_POINT('',(-4.,17.,0.));
#53205=CARTESIAN_POINT('Origin',(-5.,19.,0.));
#53206=CARTESIAN_POINT('',(-4.,19.,0.));
#53207=CARTESIAN_POINT('',(-4.,19.,0.));
#53208=CARTESIAN_POINT('',(-5.,20.,0.));
#53209=CARTESIAN_POINT('Origin',(-5.,19.,0.));
#53210=CARTESIAN_POINT('',(-5.,20.,0.));
#53211=CARTESIAN_POINT('Origin',(-4.,20.,0.));
#53212=CARTESIAN_POINT('',(-19.,20.,0.));
#53213=CARTESIAN_POINT('',(-20.,20.,0.));
#53214=CARTESIAN_POINT('',(-19.,20.,0.));
#53215=CARTESIAN_POINT('Origin',(-19.,19.,0.));
#53216=CARTESIAN_POINT('',(-20.,19.,0.));
#53217=CARTESIAN_POINT('Origin',(-19.,19.,0.));
#53218=CARTESIAN_POINT('',(-20.,19.,0.));
#53219=CARTESIAN_POINT('Origin',(-19.,5.,0.));
#53220=CARTESIAN_POINT('',(-20.,5.,0.));
#53221=CARTESIAN_POINT('',(-20.,5.,0.));
#53222=CARTESIAN_POINT('Origin',(-19.,5.,0.));
#53223=CARTESIAN_POINT('Origin',(12.,-12.,0.));
#53224=CARTESIAN_POINT('',(9.,-12.,0.));
#53225=CARTESIAN_POINT('',(9.,-12.,0.));
#53226=CARTESIAN_POINT('Origin',(12.,-12.,0.));
#53227=CARTESIAN_POINT('Origin',(12.,12.,0.));
#53228=CARTESIAN_POINT('',(9.,12.,0.));
#53229=CARTESIAN_POINT('',(9.,12.,0.));
#53230=CARTESIAN_POINT('Origin',(12.,12.,0.));
#53231=CARTESIAN_POINT('Origin',(0.,0.,0.));
#53232=CARTESIAN_POINT('',(-4.,-4.89858719658941E-16,0.));
#53233=CARTESIAN_POINT('Origin',(-12.,12.,0.));
#53234=CARTESIAN_POINT('',(-15.,12.,0.));
#53235=CARTESIAN_POINT('',(-15.,12.,0.));
#53236=CARTESIAN_POINT('Origin',(-12.,12.,0.));
#53237=CARTESIAN_POINT('Origin',(-12.,-12.,0.));
#53238=CARTESIAN_POINT('',(-15.,-12.,0.));
#53239=CARTESIAN_POINT('',(-15.,-12.,0.));
#53240=CARTESIAN_POINT('Origin',(-12.,-12.,0.));
#53241=CARTESIAN_POINT('Origin',(-20.,20.,0.));
#53242=CARTESIAN_POINT('',(-20.,4.,0.));
#53243=CARTESIAN_POINT('Origin',(-4.,16.,0.));
#53244=CARTESIAN_POINT('',(-4.,20.,0.));
#53245=CARTESIAN_POINT('Origin',(4.,16.,0.));
#53246=CARTESIAN_POINT('',(7.,16.,0.));
#53247=CARTESIAN_POINT('Origin',(20.,20.,0.));
#53248=CARTESIAN_POINT('',(4.,20.,0.));
#53249=CARTESIAN_POINT('Origin',(16.,4.,0.));
#53250=CARTESIAN_POINT('',(20.,4.,0.));
#53251=CARTESIAN_POINT('Origin',(16.,-4.,0.));
#53252=CARTESIAN_POINT('',(16.,-7.,0.));
#53253=CARTESIAN_POINT('Origin',(20.,-20.,0.));
#53254=CARTESIAN_POINT('',(20.,-4.,0.));
#53255=CARTESIAN_POINT('Origin',(4.,-16.,0.));
#53256=CARTESIAN_POINT('',(4.,-20.,0.));
#53257=CARTESIAN_POINT('Origin',(-4.,-16.,0.));
#53258=CARTESIAN_POINT('',(-7.,-16.,0.));
#53259=CARTESIAN_POINT('Origin',(-20.,-20.,0.));
#53260=CARTESIAN_POINT('',(-4.,-20.,0.));
#53261=CARTESIAN_POINT('Origin',(-16.,-4.,0.));
#53262=CARTESIAN_POINT('',(-20.,-4.,0.));
#53263=CARTESIAN_POINT('Origin',(-16.,4.,0.));
#53264=CARTESIAN_POINT('',(-16.,7.,0.));
#53265=CARTESIAN_POINT('Origin',(0.,0.,0.));
#53266=CARTESIAN_POINT('',(0.,0.,0.));
#53267=CARTESIAN_POINT('Origin',(0.,0.,6.));
#53268=CARTESIAN_POINT('',(-8.5,1.04094977927525E-15,6.));
#53269=CARTESIAN_POINT('Origin',(0.,0.,6.));
#53270=CARTESIAN_POINT('',(-5.5,6.73555739531044E-16,6.));
#53271=CARTESIAN_POINT('Origin',(0.,0.,6.));
#53272=CARTESIAN_POINT('Origin',(0.,0.,11.));
#53273=CARTESIAN_POINT('',(-8.5,1.04094977927525E-15,16.));
#53274=CARTESIAN_POINT('Origin',(0.,0.,16.));
#53275=CARTESIAN_POINT('',(-8.5,1.04094977927525E-15,11.));
#53276=CARTESIAN_POINT('Origin',(0.,0.,8.));
#53277=CARTESIAN_POINT('',(-5.5,6.73555739531044E-16,0.));
#53278=CARTESIAN_POINT('',(-5.5,6.73555739531044E-16,8.));
#53279=CARTESIAN_POINT('Origin',(0.,0.,0.));
#53280=CARTESIAN_POINT('Origin',(35.,-35.,8.));
#53281=CARTESIAN_POINT('',(30.5,-35.,16.));
#53282=CARTESIAN_POINT('Origin',(35.,-35.,16.));
#53283=CARTESIAN_POINT('',(30.5,-35.,0.));
#53284=CARTESIAN_POINT('',(30.5,-35.,8.));
#53285=CARTESIAN_POINT('Origin',(35.,-35.,0.));
#53286=CARTESIAN_POINT('Origin',(-35.,-35.,8.));
#53287=CARTESIAN_POINT('',(-39.5,-35.,16.));
#53288=CARTESIAN_POINT('Origin',(-35.,-35.,16.));
#53289=CARTESIAN_POINT('',(-39.5,-35.,0.));
#53290=CARTESIAN_POINT('',(-39.5,-35.,8.));
#53291=CARTESIAN_POINT('Origin',(-35.,-35.,0.));
#53292=CARTESIAN_POINT('Origin',(-35.,35.,8.));
#53293=CARTESIAN_POINT('',(-39.5,35.,16.));
#53294=CARTESIAN_POINT('Origin',(-35.,35.,16.));
#53295=CARTESIAN_POINT('',(-39.5,35.,0.));
#53296=CARTESIAN_POINT('',(-39.5,35.,8.));
#53297=CARTESIAN_POINT('Origin',(-35.,35.,0.));
#53298=CARTESIAN_POINT('Origin',(35.,35.,8.));
#53299=CARTESIAN_POINT('',(30.5,35.,16.));
#53300=CARTESIAN_POINT('Origin',(35.,35.,16.));
#53301=CARTESIAN_POINT('',(30.5,35.,0.));
#53302=CARTESIAN_POINT('',(30.5,35.,8.));
#53303=CARTESIAN_POINT('Origin',(35.,35.,0.));
#53304=CARTESIAN_POINT('Origin',(50.,50.,0.));
#53305=CARTESIAN_POINT('',(50.,50.,0.));
#53306=CARTESIAN_POINT('',(-50.,50.,0.));
#53307=CARTESIAN_POINT('',(50.,50.,0.));
#53308=CARTESIAN_POINT('',(-50.,50.,16.));
#53309=CARTESIAN_POINT('',(-50.,50.,0.));
#53310=CARTESIAN_POINT('',(50.,50.,16.));
#53311=CARTESIAN_POINT('',(50.,50.,16.));
#53312=CARTESIAN_POINT('',(50.,50.,0.));
#53313=CARTESIAN_POINT('Origin',(50.,-50.,0.));
#53314=CARTESIAN_POINT('',(50.,-50.,0.));
#53315=CARTESIAN_POINT('',(50.,-50.,0.));
#53316=CARTESIAN_POINT('',(50.,-50.,16.));
#53317=CARTESIAN_POINT('',(50.,-50.,16.));
#53318=CARTESIAN_POINT('',(50.,-50.,0.));
#53319=CARTESIAN_POINT('Origin',(-50.,-50.,0.));
#53320=CARTESIAN_POINT('',(-50.,-50.,0.));
#53321=CARTESIAN_POINT('',(-50.,-50.,0.));
#53322=CARTESIAN_POINT('',(-50.,-50.,16.));
#53323=CARTESIAN_POINT('',(-50.,-50.,16.));
#53324=CARTESIAN_POINT('',(-50.,-50.,0.));
#53325=CARTESIAN_POINT('Origin',(-50.,50.,0.));
#53326=CARTESIAN_POINT('',(-50.,50.,0.));
#53327=CARTESIAN_POINT('',(-50.,50.,16.));
#53328=CARTESIAN_POINT('Origin',(0.,0.,16.));
#53329=CARTESIAN_POINT('Origin',(0.,0.,0.));
#53330=CARTESIAN_POINT('',(0.,0.,0.));
#53331=CARTESIAN_POINT('Origin',(0.,0.,0.));
#53332=CARTESIAN_POINT('',(-4.94697864382552,0.00278476180115707,0.322320454656892));
#53333=CARTESIAN_POINT('',(-4.94423617559418,0.00148231834052548,0.177679545343088));
#53334=CARTESIAN_POINT('',(-4.942,-6.05220448138622E-16,0.));
#53335=CARTESIAN_POINT('',(2.16917135428609,4.440502182833,0.));
#53336=CARTESIAN_POINT('Ctrl Pts',(-4.94697864382552,0.00278476180115707,
0.322320454656892));
#53337=CARTESIAN_POINT('Ctrl Pts',(-4.94837427497074,0.191084575140575,
0.316237515399425));
#53338=CARTESIAN_POINT('Ctrl Pts',(-4.93857638297692,0.379246871981659,
0.310154576141959));
#53339=CARTESIAN_POINT('Ctrl Pts',(-4.91710439111276,0.566072733558586,
0.304071636884492));
#53340=CARTESIAN_POINT('Ctrl Pts',(-4.73085624282078,2.18660104746097,0.251308196024277));
#53341=CARTESIAN_POINT('Ctrl Pts',(-3.66626808942587,3.70657817799375,0.198544755164062));
#53342=CARTESIAN_POINT('Ctrl Pts',(-2.20523483873771,4.43248249176653,0.145781314303847));
#53343=CARTESIAN_POINT('Ctrl Pts',(-0.85966080708188,5.10102168731156,0.097187542869231));
#53344=CARTESIAN_POINT('Ctrl Pts',(0.822175421307706,5.09603339682298,0.0485937714346156));
#53345=CARTESIAN_POINT('Ctrl Pts',(2.17571852337094,4.44456444733847,3.90312782094782E-17));
#53346=CARTESIAN_POINT('',(-2.16917135428615,4.44050218283297,0.));
#53347=CARTESIAN_POINT('Origin',(0.,0.,0.));
#53348=CARTESIAN_POINT('Ctrl Pts',(-2.16917135428615,4.44050218283297,1.94289029309402E-15));
#53349=CARTESIAN_POINT('Ctrl Pts',(-2.90569614448719,4.08071213863431,0.0263982667373533));
#53350=CARTESIAN_POINT('Ctrl Pts',(-3.54537901519776,3.53418981917855,0.0527965334747045));
#53351=CARTESIAN_POINT('Ctrl Pts',(-4.02261725675323,2.86672087533204,0.0791948002120558));
#53352=CARTESIAN_POINT('Ctrl Pts',(-4.49985549830871,2.1992519314855,0.105593066949408));
#53353=CARTESIAN_POINT('Ctrl Pts',(-4.81464911070909,1.41083636324821,0.13199133368676));
#53354=CARTESIAN_POINT('Ctrl Pts',(-4.91161341297729,0.598206782831744,
0.158389600424112));
#53355=CARTESIAN_POINT('Ctrl Pts',(-4.93523158039298,0.400269799547603,
0.164819582063771));
#53356=CARTESIAN_POINT('Ctrl Pts',(-4.94592610470609,0.200896217803435,
0.171249563703429));
#53357=CARTESIAN_POINT('Ctrl Pts',(-4.94423617559418,0.00148231834052548,
0.177679545343088));
#53358=CARTESIAN_POINT('Origin',(0.,0.,0.));
#53359=CARTESIAN_POINT('',(-4.93459216488855,0.00173983556611496,1.32232045465689));
#53360=CARTESIAN_POINT('',(-4.93449003509191,0.0016461999684793,1.17767954534309));
#53361=CARTESIAN_POINT('',(-4.942,-6.05220448138622E-16,0.));
#53362=CARTESIAN_POINT('Ctrl Pts',(-4.93459216488855,0.00173983556611496,
1.32232045465689));
#53363=CARTESIAN_POINT('Ctrl Pts',(-4.93685941200801,0.71330292763056,1.29948482722738));
#53364=CARTESIAN_POINT('Ctrl Pts',(-4.79300629668486,1.42399221307712,1.27664919979787));
#53365=CARTESIAN_POINT('Ctrl Pts',(-4.49846232996172,2.06549179869028,1.25381357236836));
#53366=CARTESIAN_POINT('Ctrl Pts',(-3.81789626200921,3.5477250130758,1.20105013150815));
#53367=CARTESIAN_POINT('Ctrl Pts',(-2.33282804601649,4.66057109067704,1.14828669064793));
#53368=CARTESIAN_POINT('Ctrl Pts',(-0.719110050159326,4.89750101325702,
1.09552324978772));
#53369=CARTESIAN_POINT('Ctrl Pts',(0.89460794569784,5.13443093583701,1.0427598089275));
#53370=CARTESIAN_POINT('Ctrl Pts',(2.63697572141945,4.49544470339575,0.989996368067287));
#53371=CARTESIAN_POINT('Ctrl Pts',(3.71488022775187,3.27143294682148,0.937232927207072));
#53372=CARTESIAN_POINT('Ctrl Pts',(4.79278473408429,2.04742119024721,0.884469486346857));
#53373=CARTESIAN_POINT('Ctrl Pts',(5.20622597102753,0.238383909539938,0.831706045486642));
#53374=CARTESIAN_POINT('Ctrl Pts',(4.76722694025552,-1.33245018266074,0.778942604626427));
#53375=CARTESIAN_POINT('Ctrl Pts',(4.32822790948351,-2.90328427486142,0.726179163766212));
#53376=CARTESIAN_POINT('Ctrl Pts',(3.03678861099627,-4.2359151785555,0.673415722905997));
#53377=CARTESIAN_POINT('Ctrl Pts',(1.48031593870399,-4.72357537917557,0.620652282045782));
#53378=CARTESIAN_POINT('Ctrl Pts',(-0.0761567335882804,-5.21123557979564,
0.567888841185567));
#53379=CARTESIAN_POINT('Ctrl Pts',(-1.89766277968558,-4.8539250773417,0.515125400325352));
#53380=CARTESIAN_POINT('Ctrl Pts',(-3.1544617311397,-3.81473007747874,0.462361959465137));
#53381=CARTESIAN_POINT('Ctrl Pts',(-4.26636809113457,-2.89534076044788,
0.415681457862388));
#53382=CARTESIAN_POINT('Ctrl Pts',(-4.93626856451128,-1.44222880258692,
0.36900095625964));
#53383=CARTESIAN_POINT('Ctrl Pts',(-4.94697864382552,0.00278476180115707,
0.322320454656892));
#53384=CARTESIAN_POINT('Ctrl Pts',(-4.94423617559418,0.00148231834052548,
0.177679545343088));
#53385=CARTESIAN_POINT('Ctrl Pts',(-4.93205010879707,-1.4364898912607,0.224046097178133));
#53386=CARTESIAN_POINT('Ctrl Pts',(-4.27589205183812,-2.87655855846778,
0.270412649013179));
#53387=CARTESIAN_POINT('Ctrl Pts',(-3.17793668728658,-3.7951739429827,0.316779200848224));
#53388=CARTESIAN_POINT('Ctrl Pts',(-1.92771999305178,-4.8411802984146,0.369575734322928));
#53389=CARTESIAN_POINT('Ctrl Pts',(-0.104675240574504,-5.21107779972881,
0.422372267797632));
#53390=CARTESIAN_POINT('Ctrl Pts',(1.45583984202071,-4.73188592100135,0.475168801272336));
#53391=CARTESIAN_POINT('Ctrl Pts',(3.01635492461593,-4.25269404227389,0.527965334747039));
#53392=CARTESIAN_POINT('Ctrl Pts',(4.31434033732908,-2.92441278350478,0.580761868221743));
#53393=CARTESIAN_POINT('Ctrl Pts',(4.76068268187915,-1.35442587380419,0.633558401696447));
#53394=CARTESIAN_POINT('Ctrl Pts',(5.20702502642923,0.215561035896397,0.686354935171151));
#53395=CARTESIAN_POINT('Ctrl Pts',(4.80172430281623,2.02725359652845,0.739151468645856));
#53396=CARTESIAN_POINT('Ctrl Pts',(3.72825744985575,3.25624139915875,0.791948002120559));
#53397=CARTESIAN_POINT('Ctrl Pts',(2.65479059689527,4.48522920178905,0.844744535595263));
#53398=CARTESIAN_POINT('Ctrl Pts',(0.9131576145873,5.13151224641759,0.897541069069967));
#53399=CARTESIAN_POINT('Ctrl Pts',(-0.702426516917608,4.90003317713487,
0.950337602544671));
#53400=CARTESIAN_POINT('Ctrl Pts',(-2.31801064842252,4.66855410785214,1.00313413601937));
#53401=CARTESIAN_POINT('Ctrl Pts',(-3.80754592912437,3.55931292465815,1.05593066949408));
#53402=CARTESIAN_POINT('Ctrl Pts',(-4.49264215512641,2.07804350324001,1.10872720296878));
#53403=CARTESIAN_POINT('Ctrl Pts',(-4.79088768013657,1.43319689701884,1.13171131709355));
#53404=CARTESIAN_POINT('Ctrl Pts',(-4.93667954029292,0.71784517544428,1.15469543121832));
#53405=CARTESIAN_POINT('Ctrl Pts',(-4.93449003509191,0.0016461999684793,
1.17767954534309));
#53406=CARTESIAN_POINT('Origin',(0.,0.,0.));
#53407=CARTESIAN_POINT('',(-4.9411817412373,-0.00444225127051057,2.32232045465689));
#53408=CARTESIAN_POINT('',(-4.94111085608669,-0.00445469630641156,2.17767954534309));
#53409=CARTESIAN_POINT('',(-4.942,-6.05220448138622E-16,0.));
#53410=CARTESIAN_POINT('Ctrl Pts',(-4.9411817412373,-0.00444225127051057,
2.32232045465689));
#53411=CARTESIAN_POINT('Ctrl Pts',(-4.93017412883888,1.22499555075574,2.28273213905534));
#53412=CARTESIAN_POINT('Ctrl Pts',(-4.46534239547945,2.46186324317617,2.24314382345379));
#53413=CARTESIAN_POINT('Ctrl Pts',(-3.63458175569093,3.36040592443024,2.20355550785224));
#53414=CARTESIAN_POINT('Ctrl Pts',(-2.52734116663296,4.55798664748753,2.15079206699202));
#53415=CARTESIAN_POINT('Ctrl Pts',(-0.770077330248272,5.15457871251208,
2.0980286261318));
#53416=CARTESIAN_POINT('Ctrl Pts',(0.837419729043101,4.87865187630481,2.04526518527159));
#53417=CARTESIAN_POINT('Ctrl Pts',(2.44491678833447,4.60272504009754,1.99250174441137));
#53418=CARTESIAN_POINT('Ctrl Pts',(3.90264707053253,3.45427930265847,1.93973830355116));
#53419=CARTESIAN_POINT('Ctrl Pts',(4.54714538443732,1.95601310903264,1.88697486269094));
#53420=CARTESIAN_POINT('Ctrl Pts',(5.19164369834212,0.45774691540682,1.83421142183073));
#53421=CARTESIAN_POINT('Ctrl Pts',(5.02291004395365,-1.39033973440576,1.78144798097051));
#53422=CARTESIAN_POINT('Ctrl Pts',(4.11774488359116,-2.74712173291455,1.7286845401103));
#53423=CARTESIAN_POINT('Ctrl Pts',(3.21257972322867,-4.10390373142335,1.67592109925008));
#53424=CARTESIAN_POINT('Ctrl Pts',(1.57098305689217,-4.96938107862837,1.62315765838987));
#53425=CARTESIAN_POINT('Ctrl Pts',(-0.0599057143251611,-4.94964036759779,
1.57039421752965));
#53426=CARTESIAN_POINT('Ctrl Pts',(-1.69079448554249,-4.92989965656721,
1.51763077666944));
#53427=CARTESIAN_POINT('Ctrl Pts',(-3.31097536164064,-4.02494088730103,
1.46486733580922));
#53428=CARTESIAN_POINT('Ctrl Pts',(-4.18303383973357,-2.64665132708304,
1.41210389494901));
#53429=CARTESIAN_POINT('Ctrl Pts',(-4.67767185058986,-1.86487530680844,
1.3821760815183));
#53430=CARTESIAN_POINT('Ctrl Pts',(-4.9316207664016,-0.930817306961143,
1.3522482680876));
#53431=CARTESIAN_POINT('Ctrl Pts',(-4.93459216488855,0.00173983556611496,
1.32232045465689));
#53432=CARTESIAN_POINT('Ctrl Pts',(-4.93449003509191,0.0016461999684793,
1.17767954534309));
#53433=CARTESIAN_POINT('Ctrl Pts',(-4.9316500541004,-0.927326919420464,
1.20749196469302));
#53434=CARTESIAN_POINT('Ctrl Pts',(-4.67984069516382,-1.85772549042789,
1.23730438404296));
#53435=CARTESIAN_POINT('Ctrl Pts',(-4.18882172046978,-2.63753729589231,
1.26711680339289));
#53436=CARTESIAN_POINT('Ctrl Pts',(-3.31924788850886,-4.01855101396421,
1.3199133368676));
#53437=CARTESIAN_POINT('Ctrl Pts',(-1.69944305328478,-4.92728079046571,
1.3727098703423));
#53438=CARTESIAN_POINT('Ctrl Pts',(-0.0675730918879967,-4.94957507244757,
1.42550640381701));
#53439=CARTESIAN_POINT('Ctrl Pts',(1.56429686950879,-4.97186935442943,1.47830293729171));
#53440=CARTESIAN_POINT('Ctrl Pts',(3.20823195707828,-4.10772814189165,1.53109947076641));
#53441=CARTESIAN_POINT('Ctrl Pts',(4.11520771620268,-2.7509467593832,1.58389600424112));
#53442=CARTESIAN_POINT('Ctrl Pts',(5.02218347532707,-1.39416537687474,1.63669253771582));
#53443=CARTESIAN_POINT('Ctrl Pts',(5.19219990600637,0.455256175604397,1.68948907119053));
#53444=CARTESIAN_POINT('Ctrl Pts',(4.54776321553941,1.95463753781542,1.74228560466523));
#53445=CARTESIAN_POINT('Ctrl Pts',(3.90332652507246,3.45401890002643,1.79508213813993));
#53446=CARTESIAN_POINT('Ctrl Pts',(2.44443671345924,4.60336007196933,1.84787867161464));
#53447=CARTESIAN_POINT('Ctrl Pts',(0.835860696338233,4.878943390804,1.90067520508934));
#53448=CARTESIAN_POINT('Ctrl Pts',(-0.772715320782773,5.15452670963867,
1.95347173856405));
#53449=CARTESIAN_POINT('Ctrl Pts',(-2.53097754341157,4.55635217536511,2.00626827203875));
#53450=CARTESIAN_POINT('Ctrl Pts',(-3.63776731536415,3.3569886406566,2.05906480551345));
#53451=CARTESIAN_POINT('Ctrl Pts',(-4.4666195916167,2.45880976243686,2.09860305212333));
#53452=CARTESIAN_POINT('Ctrl Pts',(-4.93011266597958,1.22347167947137,2.13814129873321));
#53453=CARTESIAN_POINT('Ctrl Pts',(-4.94111085608669,-0.00445469630641156,
2.17767954534309));
#53454=CARTESIAN_POINT('Origin',(0.,0.,0.));
#53455=CARTESIAN_POINT('',(-4.94903399601206,0.00195803074323202,3.32232045465689));
#53456=CARTESIAN_POINT('',(-4.94919334226918,0.00181972978148383,3.17767954534309));
#53457=CARTESIAN_POINT('',(-4.942,-6.05220448138622E-16,0.));
#53458=CARTESIAN_POINT('Ctrl Pts',(-4.94903399601206,0.00195803074323202,
3.32232045465689));
#53459=CARTESIAN_POINT('Ctrl Pts',(-4.949593728633,0.112604296590692,3.31874289174351));
#53460=CARTESIAN_POINT('Ctrl Pts',(-4.94620248790589,0.223215646212416,
3.31516532883013));
#53461=CARTESIAN_POINT('Ctrl Pts',(-4.93875055399973,0.333552745210412,
3.31158776591675));
#53462=CARTESIAN_POINT('Ctrl Pts',(-4.82884621871006,1.96085186995656,3.25882432505653));
#53463=CARTESIAN_POINT('Ctrl Pts',(-3.83567522857514,3.52849703407851,3.20606088419632));
#53464=CARTESIAN_POINT('Ctrl Pts',(-2.41126381713223,4.32299910001284,3.15329744333611));
#53465=CARTESIAN_POINT('Ctrl Pts',(-0.986852405689299,5.11750116594718,
3.10053400247589));
#53466=CARTESIAN_POINT('Ctrl Pts',(0.868799427061646,5.13886013369387,3.04777056161567));
#53467=CARTESIAN_POINT('Ctrl Pts',(2.31112083361857,4.37735478907724,2.99500712075546));
#53468=CARTESIAN_POINT('Ctrl Pts',(3.75344224017549,3.61584944446061,2.94224367989524));
#53469=CARTESIAN_POINT('Ctrl Pts',(4.78243322053839,2.07147978748068,2.88948023903503));
#53470=CARTESIAN_POINT('Ctrl Pts',(4.92976460259391,0.447141508486386,2.83671679817481));
#53471=CARTESIAN_POINT('Ctrl Pts',(5.07709598464943,-1.17719677050791,2.7839533573146));
#53472=CARTESIAN_POINT('Ctrl Pts',(4.34276776839756,-2.88150367151656,2.73118991645438));
#53473=CARTESIAN_POINT('Ctrl Pts',(3.06099802257449,-3.89009065317052,2.67842647559417));
#53474=CARTESIAN_POINT('Ctrl Pts',(1.77922827675142,-4.89867763482448,2.62566303473395));
#53475=CARTESIAN_POINT('Ctrl Pts',(-0.0499829986428499,-5.21154469712375,
2.57289959387374));
#53476=CARTESIAN_POINT('Ctrl Pts',(-1.59409909536903,-4.68629519517074,
2.52013615301352));
#53477=CARTESIAN_POINT('Ctrl Pts',(-3.13821519209522,-4.16104569321773,
2.46737271215331));
#53478=CARTESIAN_POINT('Ctrl Pts',(-4.39723611015331,-2.79767962701243,
2.41460927129309));
#53479=CARTESIAN_POINT('Ctrl Pts',(-4.79813789831673,-1.21671190336476,
2.36184583043288));
#53480=CARTESIAN_POINT('Ctrl Pts',(-4.89824378961878,-0.821941443944892,
2.34867070517422));
#53481=CARTESIAN_POINT('Ctrl Pts',(-4.94484511185421,-0.413603307842339,
2.33549557991555));
#53482=CARTESIAN_POINT('Ctrl Pts',(-4.9411817412373,-0.00444225127051057,
2.32232045465689));
#53483=CARTESIAN_POINT('Ctrl Pts',(-4.94111085608669,-0.00445469630641156,
2.17767954534309));
#53484=CARTESIAN_POINT('Ctrl Pts',(-4.94479885876604,-0.416212969241057,
2.19093783220791));
#53485=CARTESIAN_POINT('Ctrl Pts',(-4.89760609031032,-0.8271378330251,2.20419611907274));
#53486=CARTESIAN_POINT('Ctrl Pts',(-4.79624701605789,-1.22423691020985,
2.21745440593756));
#53487=CARTESIAN_POINT('Ctrl Pts',(-4.39261962352267,-2.80554639122433,
2.27025093941227));
#53488=CARTESIAN_POINT('Ctrl Pts',(-3.13004751717586,-4.16761281810985,
2.32304747288697));
#53489=CARTESIAN_POINT('Ctrl Pts',(-1.58383298272376,-4.68979872834667,
2.37584400636168));
#53490=CARTESIAN_POINT('Ctrl Pts',(-0.0376184482716604,-5.21198463858349,
2.42864053983638));
#53491=CARTESIAN_POINT('Ctrl Pts',(1.79223851428572,-4.89429003217164,2.48143707331108));
#53492=CARTESIAN_POINT('Ctrl Pts',(3.07195081718679,-3.88147571791622,2.53423360678579));
#53493=CARTESIAN_POINT('Ctrl Pts',(4.35166312008787,-2.86866140366079,2.58703014026049));
#53494=CARTESIAN_POINT('Ctrl Pts',(5.08123076333263,-1.1607273815618,2.6398266737352));
#53495=CARTESIAN_POINT('Ctrl Pts',(4.92822027622649,0.464093861851888,2.6926232072099));
#53496=CARTESIAN_POINT('Ctrl Pts',(4.77520978912036,2.08891510526557,2.7454197406846));
#53497=CARTESIAN_POINT('Ctrl Pts',(3.73962117166333,3.63062356999396,2.79821627415931));
#53498=CARTESIAN_POINT('Ctrl Pts',(2.29332840687238,4.38672799125455,2.85101280763401));
#53499=CARTESIAN_POINT('Ctrl Pts',(0.847035642081437,5.14283241251514,2.90380934110872));
#53500=CARTESIAN_POINT('Ctrl Pts',(-1.00996127004341,5.11333279030795,2.95660587458342));
#53501=CARTESIAN_POINT('Ctrl Pts',(-2.4315078970232,4.31167097450304,3.00940240805812));
#53502=CARTESIAN_POINT('Ctrl Pts',(-3.853054524003,3.51000915869812,3.06219894153283));
#53503=CARTESIAN_POINT('Ctrl Pts',(-4.83915086583772,1.93618514929547,3.11499547500753));
#53504=CARTESIAN_POINT('Ctrl Pts',(-4.94047465700387,0.307323593631802,
3.16779200848224));
#53505=CARTESIAN_POINT('Ctrl Pts',(-4.94679983692322,0.205641231723391,
3.17108785410252));
#53506=CARTESIAN_POINT('Ctrl Pts',(-4.94967711776464,0.103744392201655,
3.17438369972281));
#53507=CARTESIAN_POINT('Ctrl Pts',(-4.94919334226918,0.00181972978148383,
3.17767954534309));
#53508=CARTESIAN_POINT('Origin',(0.,0.,0.));
#53509=CARTESIAN_POINT('',(-4.93570031758673,0.00282778719561921,4.32232045465689));
#53510=CARTESIAN_POINT('',(-4.93596067211196,0.00302686994969232,4.17767954534309));
#53511=CARTESIAN_POINT('',(-4.942,-6.05220448138622E-16,0.));
#53512=CARTESIAN_POINT('Ctrl Pts',(-4.93570031758673,0.00282778719561921,
4.32232045465689));
#53513=CARTESIAN_POINT('Ctrl Pts',(-4.93901975399819,0.635970529567334,
4.30199020357146));
#53514=CARTESIAN_POINT('Ctrl Pts',(-4.82594024125747,1.26797266957629,4.28165995248604));
#53515=CARTESIAN_POINT('Ctrl Pts',(-4.59096240198504,1.85083188703807,4.26132970140062));
#53516=CARTESIAN_POINT('Ctrl Pts',(-3.98112048346584,3.36353616802088,4.2085662605404));
#53517=CARTESIAN_POINT('Ctrl Pts',(-2.55021179152983,4.54522999135323,4.15580281968019));
#53518=CARTESIAN_POINT('Ctrl Pts',(-0.94949200772219,4.85808392031181,4.10303937881998));
#53519=CARTESIAN_POINT('Ctrl Pts',(0.651227776085471,5.17093784927039,4.05027593795976));
#53520=CARTESIAN_POINT('Ctrl Pts',(2.42175865176475,4.61495188385518,3.99751249709954));
#53521=CARTESIAN_POINT('Ctrl Pts',(3.55627122044722,3.44317432848828,3.94474905623933));
#53522=CARTESIAN_POINT('Ctrl Pts',(4.69078378912967,2.27139677312141,3.89198561537911));
#53523=CARTESIAN_POINT('Ctrl Pts',(5.18927805081532,0.483827627802874,3.8392221745189));
#53524=CARTESIAN_POINT('Ctrl Pts',(4.82487214846976,-1.10594900598695,3.78645873365868));
#53525=CARTESIAN_POINT('Ctrl Pts',(4.46046624612419,-2.6957256397768,3.73369529279847));
#53526=CARTESIAN_POINT('Ctrl Pts',(3.23316017974738,-4.08770976203793,3.68093185193825));
#53527=CARTESIAN_POINT('Ctrl Pts',(1.7015430859675,-4.6483616008314,3.62816841107804));
#53528=CARTESIAN_POINT('Ctrl Pts',(0.169925992187646,-5.20901343962485,
3.57540497021783));
#53529=CARTESIAN_POINT('Ctrl Pts',(-1.66600212899526,-4.93833299495065,
3.52264152935761));
#53530=CARTESIAN_POINT('Ctrl Pts',(-2.97064734936451,-3.95951622992839,
3.4698780884974));
#53531=CARTESIAN_POINT('Ctrl Pts',(-4.18683263839842,-3.04706698189228,
3.42069221055056));
#53532=CARTESIAN_POINT('Ctrl Pts',(-4.94133855052495,-1.51925455419597,
3.37150633260372));
#53533=CARTESIAN_POINT('Ctrl Pts',(-4.94903399601206,0.00195803074323202,
3.32232045465689));
#53534=CARTESIAN_POINT('Ctrl Pts',(-4.94919334226918,0.00181972978148383,
3.17767954534309));
#53535=CARTESIAN_POINT('Ctrl Pts',(-4.94192746196068,-1.52899860347891,
3.22718023319751));
#53536=CARTESIAN_POINT('Ctrl Pts',(-4.17649517400323,-3.06609305497157,
3.27668092105193));
#53537=CARTESIAN_POINT('Ctrl Pts',(-2.94711271903068,-3.97709242316291,
3.32618160890635));
#53538=CARTESIAN_POINT('Ctrl Pts',(-1.63587574939375,-4.94874778236929,
3.37897814238105));
#53539=CARTESIAN_POINT('Ctrl Pts',(0.203149430377691,-5.20815939885737,
3.43177467585576));
#53540=CARTESIAN_POINT('Ctrl Pts',(1.73199722462222,-4.63712444206039,3.48457120933046));
#53541=CARTESIAN_POINT('Ctrl Pts',(3.26084501886676,-4.06608948526341,3.53736774280516));
#53542=CARTESIAN_POINT('Ctrl Pts',(4.47951542758438,-2.66460795518137,3.59016427627987));
#53543=CARTESIAN_POINT('Ctrl Pts',(4.83271212906113,-1.07127541230128,3.64296080975457));
#53544=CARTESIAN_POINT('Ctrl Pts',(5.18590883053788,0.522057130578818,3.69575734322927));
#53545=CARTESIAN_POINT('Ctrl Pts',(4.67363182477377,2.30724068625696,3.74855387670398));
#53546=CARTESIAN_POINT('Ctrl Pts',(3.52930397676422,3.47084297428374,3.80135041017868));
#53547=CARTESIAN_POINT('Ctrl Pts',(2.38497612875467,4.63444526231052,3.85414694365339));
#53548=CARTESIAN_POINT('Ctrl Pts',(0.6085974384997,5.17646628268592,3.90694347712809));
#53549=CARTESIAN_POINT('Ctrl Pts',(-0.990411824257063,4.84993009504558,
3.95974001060279));
#53550=CARTESIAN_POINT('Ctrl Pts',(-2.58942108701383,4.52339390740524,4.0125365440775));
#53551=CARTESIAN_POINT('Ctrl Pts',(-4.01106092227238,3.32830051174915,4.0653330775522));
#53552=CARTESIAN_POINT('Ctrl Pts',(-4.60755047572122,1.80920317532792,4.11812961102691));
#53553=CARTESIAN_POINT('Ctrl Pts',(-4.831813392182,1.23806626759189,4.1379795891323));
#53554=CARTESIAN_POINT('Ctrl Pts',(-4.93943770829377,0.621129986103563,
4.1578295672377));
#53555=CARTESIAN_POINT('Ctrl Pts',(-4.93596067211196,0.00302686994969232,
4.17767954534309));
#53556=CARTESIAN_POINT('Origin',(0.,0.,0.));
#53557=CARTESIAN_POINT('',(-4.93897027655035,-0.00418490057281118,5.32232045465689));
#53558=CARTESIAN_POINT('',(-4.93838471541483,-0.00406162586984615,5.17767954534309));
#53559=CARTESIAN_POINT('',(-4.942,-6.05220448138622E-16,0.));
#53560=CARTESIAN_POINT('Ctrl Pts',(-4.93897027655035,-0.00418490057281118,
5.32232045465689));
#53561=CARTESIAN_POINT('Ctrl Pts',(-4.92960049919577,1.1487585810669,5.28523751539942));
#53562=CARTESIAN_POINT('Ctrl Pts',(-4.5267508630109,2.30760372029857,5.24815457614196));
#53563=CARTESIAN_POINT('Ctrl Pts',(-3.78916668346253,3.18507932319436,5.21107163688449));
#53564=CARTESIAN_POINT('Ctrl Pts',(-2.73969541672107,4.43359502898083,5.15830819602428));
#53565=CARTESIAN_POINT('Ctrl Pts',(-1.01255385125843,5.11247792715855,5.10554475516406));
#53566=CARTESIAN_POINT('Ctrl Pts',(0.606176578608286,4.91274509878472,5.05278131430385));
#53567=CARTESIAN_POINT('Ctrl Pts',(2.224907008475,4.71301227041089,5.00001787344363));
#53568=CARTESIAN_POINT('Ctrl Pts',(3.73522630274578,3.63466371548551,4.94725443258342));
#53569=CARTESIAN_POINT('Ctrl Pts',(4.44973628814144,2.16849289048282,4.8944909917232));
#53570=CARTESIAN_POINT('Ctrl Pts',(5.1642462735371,0.702322065480126,4.84172755086299));
#53571=CARTESIAN_POINT('Ctrl Pts',(5.08294695005765,-1.15167102959988,4.78896411000277));
#53572=CARTESIAN_POINT('Ctrl Pts',(4.24284043151724,-2.54967047338244,4.73620066914256));
#53573=CARTESIAN_POINT('Ctrl Pts',(3.40273391297681,-3.94766991716502,4.68343722828234));
#53574=CARTESIAN_POINT('Ctrl Pts',(1.80382019937538,-4.88967570965013,4.63067378742212));
#53575=CARTESIAN_POINT('Ctrl Pts',(0.173819826494171,-4.94694866740537,
4.57791034656191));
#53576=CARTESIAN_POINT('Ctrl Pts',(-1.45618054638702,-5.0042216251606,4.5251469057017));
#53577=CARTESIAN_POINT('Ctrl Pts',(-3.11726757854798,-4.17676174818597,
4.47238346484148));
#53578=CARTESIAN_POINT('Ctrl Pts',(-4.05342352207729,-2.84117444038203,
4.41962002398127));
#53579=CARTESIAN_POINT('Ctrl Pts',(-4.62886975682389,-2.02020151085742,
4.38718683420648));
#53580=CARTESIAN_POINT('Ctrl Pts',(-4.93040476513016,-1.00723542508793,
4.35475364443168));
#53581=CARTESIAN_POINT('Ctrl Pts',(-4.93570031758673,0.00282778719561921,
4.32232045465689));
#53582=CARTESIAN_POINT('Ctrl Pts',(-4.93596067211196,0.00302686994969232,
4.17767954534309));
#53583=CARTESIAN_POINT('Ctrl Pts',(-4.9301895642308,-1.0228870344476,4.2106261007124));
#53584=CARTESIAN_POINT('Ctrl Pts',(-4.61834948018582,-2.05201540819261,
4.24357265608171));
#53585=CARTESIAN_POINT('Ctrl Pts',(-4.02575926717865,-2.88027773583012,
4.27651921145102));
#53586=CARTESIAN_POINT('Ctrl Pts',(-3.07613923354808,-4.20756003338059,
4.32931574492572));
#53587=CARTESIAN_POINT('Ctrl Pts',(-1.40555989464781,-5.01902335129515,
4.38211227840043));
#53588=CARTESIAN_POINT('Ctrl Pts',(0.224766745275694,-4.94491834338594,
4.43490881187513));
#53589=CARTESIAN_POINT('Ctrl Pts',(1.85509338519918,-4.87081333547673,4.48770534534984));
#53590=CARTESIAN_POINT('Ctrl Pts',(3.44516732614589,-3.91114000174376,4.54050187882454));
#53591=CARTESIAN_POINT('Ctrl Pts',(4.270459451601,-2.50318069379225,4.59329841229924));
#53592=CARTESIAN_POINT('Ctrl Pts',(5.09575157705613,-1.09522138584072,4.64609494577394));
#53593=CARTESIAN_POINT('Ctrl Pts',(5.15626188701963,0.761023896329388,4.69889147924865));
#53594=CARTESIAN_POINT('Ctrl Pts',(4.42441840505647,2.21974306847382,4.75168801272335));
#53595=CARTESIAN_POINT('Ctrl Pts',(3.69257492309331,3.67846224061823,4.80448454619806));
#53596=CARTESIAN_POINT('Ctrl Pts',(2.16837764920352,4.73965530273698,4.85728107967276));
#53597=CARTESIAN_POINT('Ctrl Pts',(0.54633850223222,4.91978167747611,4.91007761314747));
#53598=CARTESIAN_POINT('Ctrl Pts',(-1.0757006447391,5.09990805221523,4.96287414662217));
#53599=CARTESIAN_POINT('Ctrl Pts',(-2.79558166479192,4.39896773957469,5.01567068009687));
#53600=CARTESIAN_POINT('Ctrl Pts',(-3.82962787248045,3.13634944983863,5.06846721357158));
#53601=CARTESIAN_POINT('Ctrl Pts',(-4.54262037450559,2.26575259758193,5.10487132416208));
#53602=CARTESIAN_POINT('Ctrl Pts',(-4.92954384104421,1.12811506301544,5.14127543475258));
#53603=CARTESIAN_POINT('Ctrl Pts',(-4.93838471541483,-0.00406162586984614,
5.17767954534309));
#53604=CARTESIAN_POINT('Origin',(0.,0.,0.));
#53605=CARTESIAN_POINT('',(-4.94990673126105,0.000609106175146774,6.32232045465689));
#53606=CARTESIAN_POINT('',(-4.95002176789587,9.24615926348992E-5,6.1776795453431));
#53607=CARTESIAN_POINT('',(-4.942,-6.05220448138622E-16,0.));
#53608=CARTESIAN_POINT('Ctrl Pts',(-4.94990673126105,0.000609106175146774,
6.32232045465689));
#53609=CARTESIAN_POINT('Ctrl Pts',(-4.94996465668772,0.0337538979231002,
6.3212482680876));
#53610=CARTESIAN_POINT('Ctrl Pts',(-4.94966035453883,0.0668975980773335,
6.3201760815183));
#53611=CARTESIAN_POINT('Ctrl Pts',(-4.94899057048952,0.100033910748547,
6.31910389494901));
#53612=CARTESIAN_POINT('Ctrl Pts',(-4.91602978541085,1.73070708277234,6.26634045408879));
#53613=CARTESIAN_POINT('Ctrl Pts',(-3.99797098316147,3.34348977495136,6.21357701322858));
#53614=CARTESIAN_POINT('Ctrl Pts',(-2.61265424963019,4.20434920314469,6.16081357236836));
#53615=CARTESIAN_POINT('Ctrl Pts',(-1.22733751609891,5.06520863133802,6.10805013150815));
#53616=CARTESIAN_POINT('Ctrl Pts',(0.625237148714281,5.17414479554567,6.05528669064793));
#53617=CARTESIAN_POINT('Ctrl Pts',(2.10189939976769,4.48157710670587,6.00252324978771));
#53618=CARTESIAN_POINT('Ctrl Pts',(3.57856165082109,3.78900941786606,5.9497598089275));
#53619=CARTESIAN_POINT('Ctrl Pts',(4.67931148811471,2.29493787597879,5.89699636806729));
#53620=CARTESIAN_POINT('Ctrl Pts',(4.90315986233076,0.679365744295384,5.84423292720707));
#53621=CARTESIAN_POINT('Ctrl Pts',(5.12700823654681,-0.936206387388013,
5.79146948634686));
#53622=CARTESIAN_POINT('Ctrl Pts',(4.4739551476853,-2.67327910886755,5.73870604548664));
#53623=CARTESIAN_POINT('Ctrl Pts',(3.24122748150885,-3.74125097570411,5.68594260462643));
#53624=CARTESIAN_POINT('Ctrl Pts',(2.00849981533238,-4.80922284254067,5.63317916376621));
#53625=CARTESIAN_POINT('Ctrl Pts',(0.196097571840956,-5.20809385473422,
5.580415722906));
#53626=CARTESIAN_POINT('Ctrl Pts',(-1.37109275233711,-4.7563241179068,5.52765228204578));
#53627=CARTESIAN_POINT('Ctrl Pts',(-2.93828307651517,-4.30455438107937,
5.47488884118557));
#53628=CARTESIAN_POINT('Ctrl Pts',(-4.26026148137987,-3.00214389523098,
5.42212540032535));
#53629=CARTESIAN_POINT('Ctrl Pts',(-4.73535019980207,-1.44186439560917,
5.36936195946513));
#53630=CARTESIAN_POINT('Ctrl Pts',(-4.87653942645625,-0.978172778920024,
5.35368145786239));
#53631=CARTESIAN_POINT('Ctrl Pts',(-4.94293228203772,-0.49170645290201,
5.33800095625964));
#53632=CARTESIAN_POINT('Ctrl Pts',(-4.93897027655035,-0.00418490057281118,
5.32232045465689));
#53633=CARTESIAN_POINT('Ctrl Pts',(-4.93838471541483,-0.00406162586984614,
5.17767954534309));
#53634=CARTESIAN_POINT('Ctrl Pts',(-4.94236567660296,-0.513869962422989,
5.19407196822729));
#53635=CARTESIAN_POINT('Ctrl Pts',(-4.86968605256145,-1.02257104983416,
5.21046439111149));
#53636=CARTESIAN_POINT('Ctrl Pts',(-4.71559692470099,-1.50528507494596,
5.22685681399569));
#53637=CARTESIAN_POINT('Ctrl Pts',(-4.21930837390877,-3.06000504316299,
5.27965334747039));
#53638=CARTESIAN_POINT('Ctrl Pts',(-2.8785198770001,-4.34514871276549,5.3324498809451));
#53639=CARTESIAN_POINT('Ctrl Pts',(-1.30417176812337,-4.7751307324871,5.3852464144198));
#53640=CARTESIAN_POINT('Ctrl Pts',(0.270176340753341,-5.2051127522087,5.4380429478945));
#53641=CARTESIAN_POINT('Ctrl Pts',(2.07808406159809,-4.77993312204945,5.49083948136921));
#53642=CARTESIAN_POINT('Ctrl Pts',(3.29576468259939,-3.69332812921623,5.54363601484391));
#53643=CARTESIAN_POINT('Ctrl Pts',(4.51344530360071,-2.606723136383,5.59643254831862));
#53644=CARTESIAN_POINT('Ctrl Pts',(5.14089882475856,-0.858692780875764,
5.64922908179332));
#53645=CARTESIAN_POINT('Ctrl Pts',(4.892221343433,0.754259796075777,5.70202561526803));
#53646=CARTESIAN_POINT('Ctrl Pts',(4.64354386210744,2.36721237302732,5.75482214874273));
#53647=CARTESIAN_POINT('Ctrl Pts',(3.51873537829851,3.84508717142316,5.80761868221743));
#53648=CARTESIAN_POINT('Ctrl Pts',(2.03032331340283,4.51447945572607,5.86041521569213));
#53649=CARTESIAN_POINT('Ctrl Pts',(0.54191124850715,5.18387174002898,5.91321174916684));
#53650=CARTESIAN_POINT('Ctrl Pts',(-1.31010439747531,5.04478151023892,5.96600828264154));
#53651=CARTESIAN_POINT('Ctrl Pts',(-2.68183880585053,4.16058627269715,6.01880481611625));
#53652=CARTESIAN_POINT('Ctrl Pts',(-4.05357321422575,3.27639103515538,6.07160134959095));
#53653=CARTESIAN_POINT('Ctrl Pts',(-4.94502638499377,1.6470907898619,6.12439788306566));
#53654=CARTESIAN_POINT('Ctrl Pts',(-4.95000099524402,0.0150884128829395,
6.17719441654037));
#53655=CARTESIAN_POINT('Ctrl Pts',(-4.95001623189281,0.0100897806679753,
6.17735612614128));
#53656=CARTESIAN_POINT('Ctrl Pts',(-4.950023152263,0.00509112310363388,
6.17751783574219));
#53657=CARTESIAN_POINT('Ctrl Pts',(-4.95002176789587,9.24615926348992E-5,
6.1776795453431));
#53658=CARTESIAN_POINT('Origin',(0.,0.,0.));
#53659=CARTESIAN_POINT('',(-4.93729272679059,0.00368592931905526,7.32232045465689));
#53660=CARTESIAN_POINT('',(-4.93812703863464,0.00398950918922817,7.17767954534309));
#53661=CARTESIAN_POINT('',(-4.942,-6.05220448138622E-16,0.));
#53662=CARTESIAN_POINT('Ctrl Pts',(-4.93729272679059,0.00368592931905526,
7.32232045465689));
#53663=CARTESIAN_POINT('Ctrl Pts',(-4.94116559210242,0.558353954818944,
7.30449557991555));
#53664=CARTESIAN_POINT('Ctrl Pts',(-4.85488370936681,1.1118525040865,7.28667070517422));
#53665=CARTESIAN_POINT('Ctrl Pts',(-4.67321739836765,1.63203970469098,7.26884583043288));
#53666=CARTESIAN_POINT('Ctrl Pts',(-4.13546665420853,3.17184668755196,7.21608238957266));
#53667=CARTESIAN_POINT('Ctrl Pts',(-2.76193831173125,4.41977291493536,7.16331894871245));
#53668=CARTESIAN_POINT('Ctrl Pts',(-1.17777228483381,4.80784430854112,7.11055550785224));
#53669=CARTESIAN_POINT('Ctrl Pts',(0.406393742063621,5.19591570214688,7.05779206699202));
#53670=CARTESIAN_POINT('Ctrl Pts',(2.2011974533812,4.72413226197502,7.0050286261318));
#53671=CARTESIAN_POINT('Ctrl Pts',(3.38976204879511,3.60721883209798,6.95226518527158));
#53672=CARTESIAN_POINT('Ctrl Pts',(4.57832664420902,2.49030540222094,6.89950174441137));
#53673=CARTESIAN_POINT('Ctrl Pts',(5.16065212371926,0.728261982638741,6.84673830355116));
#53674=CARTESIAN_POINT('Ctrl Pts',(4.8717021652758,-0.876944960040814,6.79397486269094));
#53675=CARTESIAN_POINT('Ctrl Pts',(4.58275220683234,-2.48215190272036,6.74121142183073));
#53676=CARTESIAN_POINT('Ctrl Pts',(3.4225268104352,-3.93052236849726,6.68844798097051));
#53677=CARTESIAN_POINT('Ctrl Pts',(1.91908439466629,-4.56285322317541,6.63568454011029));
#53678=CARTESIAN_POINT('Ctrl Pts',(0.415641978897348,-5.19518407785358,
6.58292109925008));
#53679=CARTESIAN_POINT('Ctrl Pts',(-1.43101745624338,-5.01147532143298,
6.53015765838987));
#53680=CARTESIAN_POINT('Ctrl Pts',(-2.78041578985976,-4.09533911728839,
6.47739421752966));
#53681=CARTESIAN_POINT('Ctrl Pts',(-4.10239349384425,-3.1978193816249,6.42570296323874));
#53682=CARTESIAN_POINT('Ctrl Pts',(-4.94711408486409,-1.59733653848074,
6.37401170894781));
#53683=CARTESIAN_POINT('Ctrl Pts',(-4.94990673126105,0.000609106175146774,
6.32232045465689));
#53684=CARTESIAN_POINT('Ctrl Pts',(-4.95002176789587,9.24615926348992E-5,
6.1776795453431));
#53685=CARTESIAN_POINT('Ctrl Pts',(-4.94957117052949,-1.62692081873173,
6.23031436921689));
#53686=CARTESIAN_POINT('Ctrl Pts',(-4.06928678123987,-3.25435222218023,
6.28294919309067));
#53687=CARTESIAN_POINT('Ctrl Pts',(-2.70715303041471,-4.14415974390912,
6.33558401696446));
#53688=CARTESIAN_POINT('Ctrl Pts',(-1.34083440560272,-5.03670101505779,
6.38838055043917));
#53689=CARTESIAN_POINT('Ctrl Pts',(0.510298893753757,-5.18707904869072,
6.44117708391388));
#53690=CARTESIAN_POINT('Ctrl Pts',(2.00276409681877,-4.52677296598962,6.49397361738859));
#53691=CARTESIAN_POINT('Ctrl Pts',(3.49522929988377,-3.86646688328851,6.54677015086329));
#53692=CARTESIAN_POINT('Ctrl Pts',(4.62902640665733,-2.39547668425338,6.59956668433799));
#53693=CARTESIAN_POINT('Ctrl Pts',(4.88753226227565,-0.784070085091338,
6.65236321781269));
#53694=CARTESIAN_POINT('Ctrl Pts',(5.14603811789397,0.827336514070738,6.7051597512874));
#53695=CARTESIAN_POINT('Ctrl Pts',(4.52925272235704,2.57915951335971,6.7579562847621));
#53696=CARTESIAN_POINT('Ctrl Pts',(3.31821896685987,3.67316762496513,6.81075281823681));
#53697=CARTESIAN_POINT('Ctrl Pts',(2.10718521136272,4.76717573657052,6.86354935171151));
#53698=CARTESIAN_POINT('Ctrl Pts',(0.301903095905328,5.20336896049236,6.91634588518622));
#53699=CARTESIAN_POINT('Ctrl Pts',(-1.27503704449112,4.78299258292295,6.96914241866092));
#53700=CARTESIAN_POINT('Ctrl Pts',(-2.85197718488759,4.36261620535354,7.02193895213562));
#53701=CARTESIAN_POINT('Ctrl Pts',(-4.20057535022311,3.0856702262929,7.07473548561032));
#53702=CARTESIAN_POINT('Ctrl Pts',(-4.70633267235205,1.53400465783913,7.12753201908503));
#53703=CARTESIAN_POINT('Ctrl Pts',(-4.86645984309908,1.04273383179117,7.14424786117105));
#53704=CARTESIAN_POINT('Ctrl Pts',(-4.94209974418837,0.523924819599999,
7.16096370325707));
#53705=CARTESIAN_POINT('Ctrl Pts',(-4.93812703863464,0.00398950918922817,
7.17767954534309));
#53706=CARTESIAN_POINT('Origin',(0.,0.,0.));
#53707=CARTESIAN_POINT('',(-4.9370364718937,-0.00357917755902493,8.32232045465689));
#53708=CARTESIAN_POINT('',(-4.93615302863258,-0.00314627141571121,8.17767954534309));
#53709=CARTESIAN_POINT('',(-4.942,-6.05220448138622E-16,0.));
#53710=CARTESIAN_POINT('Ctrl Pts',(-4.9370364718937,-0.00357917755902493,
8.32232045465689));
#53711=CARTESIAN_POINT('Ctrl Pts',(-4.92976643593387,1.07253365977557,8.28774289174351));
#53712=CARTESIAN_POINT('Ctrl Pts',(-4.58366254169201,2.15290343310709,8.25316532883013));
#53713=CARTESIAN_POINT('Ctrl Pts',(-3.93530233070663,3.00265049848112,8.21858776591675));
#53714=CARTESIAN_POINT('Ctrl Pts',(-2.94594065318929,4.29931733247173,8.16582432505654));
#53715=CARTESIAN_POINT('Ctrl Pts',(-1.25277317118212,5.05897768713911,8.11306088419632));
#53716=CARTESIAN_POINT('Ctrl Pts',(0.373581453010537,4.93588404929253,8.06029744333611));
#53717=CARTESIAN_POINT('Ctrl Pts',(1.99993607720318,4.81279041144596,8.00753400247589));
#53718=CARTESIAN_POINT('Ctrl Pts',(3.55947784358134,3.80694278108544,7.95477056161567));
#53719=CARTESIAN_POINT('Ctrl Pts',(4.34240574156256,2.37613695433122,7.90200712075546));
#53720=CARTESIAN_POINT('Ctrl Pts',(5.12533363954378,0.945331127576992,7.84924367989524));
#53721=CARTESIAN_POINT('Ctrl Pts',(5.13164766912806,-0.910432895570919,
7.79648023903503));
#53722=CARTESIAN_POINT('Ctrl Pts',(4.35847409863575,-2.34653318357428,7.74371679817482));
#53723=CARTESIAN_POINT('Ctrl Pts',(3.58530052814345,-3.78263347157761,7.6909533573146));
#53724=CARTESIAN_POINT('Ctrl Pts',(2.03263935757455,-4.7990700244364,7.63818991645438));
#53725=CARTESIAN_POINT('Ctrl Pts',(0.407160002087725,-4.93322766379111,
7.58542647559417));
#53726=CARTESIAN_POINT('Ctrl Pts',(-1.21831935339912,-5.06738530314582,
7.53266303473395));
#53727=CARTESIAN_POINT('Ctrl Pts',(-2.91661689380388,-4.31926402899647,
7.47989959387374));
#53728=CARTESIAN_POINT('Ctrl Pts',(-3.9147790910858,-3.02935952275251,7.42713615301352));
#53729=CARTESIAN_POINT('Ctrl Pts',(-4.57573590812677,-2.1752186035157,7.39219758689465));
#53730=CARTESIAN_POINT('Ctrl Pts',(-4.92970151716189,-1.08351977418085,
7.35725902077577));
#53731=CARTESIAN_POINT('Ctrl Pts',(-4.93729272679059,0.00368592931905526,
7.32232045465689));
#53732=CARTESIAN_POINT('Ctrl Pts',(-4.93812703863464,0.00398950918922817,
7.17767954534309));
#53733=CARTESIAN_POINT('Ctrl Pts',(-4.9295520615366,-1.11827674461206,7.21376023673177));
#53734=CARTESIAN_POINT('Ctrl Pts',(-4.55006154683992,-2.24579042752333,
7.24984092812046));
#53735=CARTESIAN_POINT('Ctrl Pts',(-3.84867674353058,-3.11294472114867,
7.28592161950915));
#53736=CARTESIAN_POINT('Ctrl Pts',(-2.82234701365785,-4.38184337383585,
7.33871815298385));
#53737=CARTESIAN_POINT('Ctrl Pts',(-1.10677107499002,-5.09325552136332,
7.39151468645855));
#53738=CARTESIAN_POINT('Ctrl Pts',(0.516336029677229,-4.92302088331724,
7.44431121993325));
#53739=CARTESIAN_POINT('Ctrl Pts',(2.13944313434447,-4.75278624527117,7.49710775340795));
#53740=CARTESIAN_POINT('Ctrl Pts',(3.67008140501115,-3.70090482165158,7.54990428688267));
#53741=CARTESIAN_POINT('Ctrl Pts',(4.41080403428737,-2.24667427194838,7.60270082035737));
#53742=CARTESIAN_POINT('Ctrl Pts',(5.15152666356361,-0.792443722245162,
7.65549735383208));
#53743=CARTESIAN_POINT('Ctrl Pts',(5.10233365144936,1.06413595354166,7.70829388730677));
#53744=CARTESIAN_POINT('Ctrl Pts',(4.28564016284837,2.47710030230944,7.76109042078147));
#53745=CARTESIAN_POINT('Ctrl Pts',(3.46894667424739,3.89006465107721,7.81388695425618));
#53746=CARTESIAN_POINT('Ctrl Pts',(1.88475270915971,4.85941367282593,7.86668348773089));
#53747=CARTESIAN_POINT('Ctrl Pts',(0.254908128790928,4.94345621594819,7.91948002120559));
#53748=CARTESIAN_POINT('Ctrl Pts',(-1.37493645157786,5.02749875907046,7.9722765546803));
#53749=CARTESIAN_POINT('Ctrl Pts',(-3.05043164722777,4.22623482356622,8.02507308815499));
#53750=CARTESIAN_POINT('Ctrl Pts',(-4.00812550651364,2.90476633090432,8.0778696216297));
#53751=CARTESIAN_POINT('Ctrl Pts',(-4.61162062728013,2.07203697816232,8.11113959620083));
#53752=CARTESIAN_POINT('Ctrl Pts',(-4.93008062183261,1.03273713844183,8.14440957077196));
#53753=CARTESIAN_POINT('Ctrl Pts',(-4.93615302863258,-0.00314627141571121,
8.17767954534309));
#53754=CARTESIAN_POINT('Origin',(0.,0.,0.));
#53755=CARTESIAN_POINT('',(-4.94983422880388,-0.000811751590238941,9.32232045465689));
#53756=CARTESIAN_POINT('',(-4.94934061074693,-0.00165165342605634,9.1776795453431));
#53757=CARTESIAN_POINT('',(-4.942,-6.05220448138622E-16,0.));
#53758=CARTESIAN_POINT('Ctrl Pts',(-4.94983422880388,-0.000811751590238941,
9.32232045465689));
#53759=CARTESIAN_POINT('Ctrl Pts',(-4.94619904315733,1.58603660082692,9.27099020357146));
#53760=CARTESIAN_POINT('Ctrl Pts',(-4.11486910012118,3.17616060693066,9.21965995248604));
#53761=CARTESIAN_POINT('Ctrl Pts',(-2.80821896129528,4.07632441244751,9.16832970140062));
#53762=CARTESIAN_POINT('Ctrl Pts',(-1.46508589907443,5.00162165359779,9.1155662605404));
#53763=CARTESIAN_POINT('Ctrl Pts',(0.38028069926283,5.19789211576897,9.06280281968019));
#53764=CARTESIAN_POINT('Ctrl Pts',(1.88799112724405,4.575806371946,9.01003937881998));
#53765=CARTESIAN_POINT('Ctrl Pts',(3.39570155522527,3.95372062812305,8.95727593795976));
#53766=CARTESIAN_POINT('Ctrl Pts',(4.56575581285046,2.51327867830594,8.90451249709954));
#53767=CARTESIAN_POINT('Ctrl Pts',(4.86562202928207,0.910075116822231,8.85174905623933));
#53768=CARTESIAN_POINT('Ctrl Pts',(5.16548824571368,-0.693128444661515,
8.79898561537912));
#53769=CARTESIAN_POINT('Ctrl Pts',(4.5951664209517,-2.45909361781186,8.7462221745189));
#53770=CARTESIAN_POINT('Ctrl Pts',(3.4142296015798,-3.58406901130408,8.69345873365869));
#53771=CARTESIAN_POINT('Ctrl Pts',(2.23329278220791,-4.70904440479628,8.64069529279847));
#53772=CARTESIAN_POINT('Ctrl Pts',(0.441740968226092,-5.19303001863033,
8.58793185193825));
#53773=CARTESIAN_POINT('Ctrl Pts',(-1.14502909018537,-4.81574738049279,
8.53516841107804));
#53774=CARTESIAN_POINT('Ctrl Pts',(-2.73179914859682,-4.43846474235526,
8.48240497021782));
#53775=CARTESIAN_POINT('Ctrl Pts',(-4.11378745143793,-3.19991385224615,
8.42964152935761));
#53776=CARTESIAN_POINT('Ctrl Pts',(-4.66200366634471,-1.66380175053471,
8.3768780884974));
#53777=CARTESIAN_POINT('Ctrl Pts',(-4.85095633907095,-1.1343528226608,8.35869221055056));
#53778=CARTESIAN_POINT('Ctrl Pts',(-4.94086010709221,-0.569554771785043,
8.34050633260373));
#53779=CARTESIAN_POINT('Ctrl Pts',(-4.9370364718937,-0.00357917755902493,
8.32232045465689));
#53780=CARTESIAN_POINT('Ctrl Pts',(-4.93615302863258,-0.00314627141571121,
8.17767954534309));
#53781=CARTESIAN_POINT('Ctrl Pts',(-4.93971699916741,-0.611119036064889,
8.19720610424667));
#53782=CARTESIAN_POINT('Ctrl Pts',(-4.83567403422615,-1.21791495642756,
8.21673266315024));
#53783=CARTESIAN_POINT('Ctrl Pts',(-4.61849424808279,-1.78108068136924,
8.23625922205381));
#53784=CARTESIAN_POINT('Ctrl Pts',(-4.03127660744421,-3.30378615116137,
8.28905575552852));
#53785=CARTESIAN_POINT('Ctrl Pts',(-2.61694880324517,-4.50752404092604,
8.34185228900322));
#53786=CARTESIAN_POINT('Ctrl Pts',(-1.01995990653351,-4.84380215349313,
8.39464882247793));
#53787=CARTESIAN_POINT('Ctrl Pts',(0.57702899017813,-5.18008026606022,8.44744535595263));
#53788=CARTESIAN_POINT('Ctrl Pts',(2.35667897940238,-4.64889860142975,8.50024188942734));
#53789=CARTESIAN_POINT('Ctrl Pts',(3.50807919667006,-3.4922940688051,8.55303842290204));
#53790=CARTESIAN_POINT('Ctrl Pts',(4.65947941393775,-2.33568953618045,8.60583495637674));
#53791=CARTESIAN_POINT('Ctrl Pts',(5.18262985924886,-0.553662135561577,
8.65863148985144));
#53792=CARTESIAN_POINT('Ctrl Pts',(4.83915310871477,1.04179398325038,8.71142802332615));
#53793=CARTESIAN_POINT('Ctrl Pts',(4.49567635818068,2.63725010206233,8.76422455680085));
#53794=CARTESIAN_POINT('Ctrl Pts',(3.28557241180142,4.04613493906739,8.81702109027556));
#53795=CARTESIAN_POINT('Ctrl Pts',(1.76023420818717,4.62647955204043,8.86981762375026));
#53796=CARTESIAN_POINT('Ctrl Pts',(0.234896004572933,5.20682416501346,8.92261415722497));
#53797=CARTESIAN_POINT('Ctrl Pts',(-1.60567645627628,4.95862855395447,8.97541069069966));
#53798=CARTESIAN_POINT('Ctrl Pts',(-2.9228125287938,3.99498491044041,9.02820722417436));
#53799=CARTESIAN_POINT('Ctrl Pts',(-4.16579429986394,3.0855940679239,9.07803133123061));
#53800=CARTESIAN_POINT('Ctrl Pts',(-4.9426191442377,1.53904642191653,9.12785543828685));
#53801=CARTESIAN_POINT('Ctrl Pts',(-4.94934061074693,-0.00165165342605634,
9.1776795453431));
#53802=CARTESIAN_POINT('Origin',(0.,0.,0.));
#53803=CARTESIAN_POINT('',(-4.93927523449924,0.00424456982664218,10.3223204546569));
#53804=CARTESIAN_POINT('',(-4.94081497674544,0.00444099958366976,10.1776795453431));
#53805=CARTESIAN_POINT('',(-4.942,-6.05220448138622E-16,0.));
#53806=CARTESIAN_POINT('Ctrl Pts',(-4.93927523449924,0.00424456982664218,
10.3223204546569));
#53807=CARTESIAN_POINT('Ctrl Pts',(-4.94321947186548,0.480467662900444,
10.3070009562597));
#53808=CARTESIAN_POINT('Ctrl Pts',(-4.8799048924926,0.955663934034991,10.2916814578624));
#53809=CARTESIAN_POINT('Ctrl Pts',(-4.7450520171049,1.40960838712838,10.2763619594652));
#53810=CARTESIAN_POINT('Ctrl Pts',(-4.28059152820107,2.97308459787111,10.2235985186049));
#53811=CARTESIAN_POINT('Ctrl Pts',(-2.96750623957443,4.28446059329433,10.1708350777447));
#53812=CARTESIAN_POINT('Ctrl Pts',(-1.40342635577711,4.74688412687777,10.1180716368845));
#53813=CARTESIAN_POINT('Ctrl Pts',(0.160653528020168,5.2093076604612,10.0653081960243));
#53814=CARTESIAN_POINT('Ctrl Pts',(1.9757280069881,4.82277873220489,10.0125447551641));
#53815=CARTESIAN_POINT('Ctrl Pts',(3.21569435837255,3.76321993027579,9.95978131430385));
#53816=CARTESIAN_POINT('Ctrl Pts',(4.455660709757,2.70366112834667,9.90701787344364));
#53817=CARTESIAN_POINT('Ctrl Pts',(5.12051893355795,0.971072452744719,9.85425443258342));
#53818=CARTESIAN_POINT('Ctrl Pts',(4.90766922172796,-0.64598549534651,9.8014909917232));
#53819=CARTESIAN_POINT('Ctrl Pts',(4.69481950989796,-2.26304344343773,9.74872755086298));
#53820=CARTESIAN_POINT('Ctrl Pts',(3.60426186243706,-3.76457066401824,9.69596411000277));
#53821=CARTESIAN_POINT('Ctrl Pts',(2.13234651308336,-4.4671705584447,9.64320066914255));
#53822=CARTESIAN_POINT('Ctrl Pts',(0.660431163729675,-5.16977045287116,
9.59043722828234));
#53823=CARTESIAN_POINT('Ctrl Pts',(-1.19284188751682,-5.07344302114356,
9.53767378742213));
#53824=CARTESIAN_POINT('Ctrl Pts',(-2.58398443596702,-4.22203018520405,
9.48491034656191));
#53825=CARTESIAN_POINT('Ctrl Pts',(-3.97512698441724,-3.37061734926452,
9.43214690570169));
#53826=CARTESIAN_POINT('Ctrl Pts',(-4.90413903007116,-1.76411910911306,
9.37938346484148));
#53827=CARTESIAN_POINT('Ctrl Pts',(-4.94819528984589,-0.133707978972622,
9.32662002398126));
#53828=CARTESIAN_POINT('Ctrl Pts',(-4.94939197035033,-0.089421849745139,
9.32518683420647));
#53829=CARTESIAN_POINT('Ctrl Pts',(-4.94993572666894,-0.0451180774845514,
9.32375364443168));
#53830=CARTESIAN_POINT('Ctrl Pts',(-4.94983422880388,-0.000811751590238941,
9.32232045465689));
#53831=CARTESIAN_POINT('Ctrl Pts',(-4.94934061074693,-0.00165165342605634,
9.1776795453431));
#53832=CARTESIAN_POINT('Ctrl Pts',(-4.94974160267239,-0.0935672327028531,
9.18065197176156));
#53833=CARTESIAN_POINT('Ctrl Pts',(-4.94740170081727,-0.185461992629528,
9.18362439818002));
#53834=CARTESIAN_POINT('Ctrl Pts',(-4.9422563677255,-0.277199402591944,
9.18659682459849));
#53835=CARTESIAN_POINT('Ctrl Pts',(-4.85086444995379,-1.90664839614095,
9.23939335807319));
#53836=CARTESIAN_POINT('Ctrl Pts',(-3.87438093022463,-3.48645470726985,
9.29218989154789));
#53837=CARTESIAN_POINT('Ctrl Pts',(-2.45774784765697,-4.29676774220554,
9.34498642502259));
#53838=CARTESIAN_POINT('Ctrl Pts',(-1.04111476508925,-5.10708077714125,
9.3977829584973));
#53839=CARTESIAN_POINT('Ctrl Pts',(0.815667880316977,-5.14790053588371,
9.450579491972));
#53840=CARTESIAN_POINT('Ctrl Pts',(2.2665431508298,-4.40062718922509,9.50337602544671));
#53841=CARTESIAN_POINT('Ctrl Pts',(3.71741842134259,-3.65335384256648,9.55617255892141));
#53842=CARTESIAN_POINT('Ctrl Pts',(4.76238631696197,-2.11798739050681,9.60896909239612));
#53843=CARTESIAN_POINT('Ctrl Pts',(4.92529937908085,-0.494129071747753,
9.66176562587082));
#53844=CARTESIAN_POINT('Ctrl Pts',(5.08821244119973,1.12972924701132,9.71456215934552));
#53845=CARTESIAN_POINT('Ctrl Pts',(4.36907066981809,2.8420794324698,9.76735869282023));
#53846=CARTESIAN_POINT('Ctrl Pts',(3.09555640642893,3.86267628047412,9.82015522629493));
#53847=CARTESIAN_POINT('Ctrl Pts',(1.82204214303977,4.88327312847843,9.87295175976963));
#53848=CARTESIAN_POINT('Ctrl Pts',(-0.00584461235687284,5.21211663902861,
9.92574829324434));
#53849=CARTESIAN_POINT('Ctrl Pts',(-1.55521355102309,4.69936680030775,9.97854482671904));
#53850=CARTESIAN_POINT('Ctrl Pts',(-3.10458248968932,4.18661696158688,10.0313413601937));
#53851=CARTESIAN_POINT('Ctrl Pts',(-4.37543361162511,2.83227377359494,10.0841378936684));
#53852=CARTESIAN_POINT('Ctrl Pts',(-4.78869407209101,1.25345386713711,10.1369344271432));
#53853=CARTESIAN_POINT('Ctrl Pts',(-4.89500374307923,0.847308491854974,
10.1505161332098));
#53854=CARTESIAN_POINT('Ctrl Pts',(-4.9445618440258,0.426308236753005,10.1640978392764));
#53855=CARTESIAN_POINT('Ctrl Pts',(-4.94081497674544,0.00444099958366976,
10.1776795453431));
#53856=CARTESIAN_POINT('Origin',(0.,0.,0.));
#53857=CARTESIAN_POINT('',(-4.93550942083981,-0.00268364051190351,11.3223204546569));
#53858=CARTESIAN_POINT('',(-4.93464332849729,-0.00183839903596135,11.1776795453431));
#53859=CARTESIAN_POINT('',(-4.942,-6.05220448138622E-16,0.));
#53860=CARTESIAN_POINT('Ctrl Pts',(-4.93550942083981,-0.00268364051190351,
11.3223204546569));
#53861=CARTESIAN_POINT('Ctrl Pts',(-4.93055147786098,0.996233778963576,
11.2902482680876));
#53862=CARTESIAN_POINT('Ctrl Pts',(-4.63616667462007,1.99783803363001,11.2581760815183));
#53863=CARTESIAN_POINT('Ctrl Pts',(-4.07266300921302,2.81352633957493,11.226103894949));
#53864=CARTESIAN_POINT('Ctrl Pts',(-3.14561700753245,4.15545298365024,11.1733404540888));
#53865=CARTESIAN_POINT('Ctrl Pts',(-1.49019904742592,4.99419689804637,11.1205770132286));
#53866=CARTESIAN_POINT('Ctrl Pts',(0.140153312490383,4.94801692591001,11.0678135723684));
#53867=CARTESIAN_POINT('Ctrl Pts',(1.77050567240668,4.90183695377364,11.0150501315081));
#53868=CARTESIAN_POINT('Ctrl Pts',(3.37579243213274,3.97073309510478,10.9622866906479));
#53869=CARTESIAN_POINT('Ctrl Pts',(4.22539246378791,2.57848268891964,10.9095232497877));
#53870=CARTESIAN_POINT('Ctrl Pts',(5.07499249544306,1.18623228273452,10.8567598089275));
#53871=CARTESIAN_POINT('Ctrl Pts',(5.16890579902736,-0.667164670966868,
10.8039963680673));
#53872=CARTESIAN_POINT('Ctrl Pts',(4.46438920521479,-2.13816357523356,10.7512329272071));
#53873=CARTESIAN_POINT('Ctrl Pts',(3.75987261140222,-3.60916247950026,10.6984694863469));
#53874=CARTESIAN_POINT('Ctrl Pts',(2.25692612019279,-4.69776333433226,10.6457060454866));
#53875=CARTESIAN_POINT('Ctrl Pts',(0.639592289029041,-4.90850650951066,
10.5929426046264));
#53876=CARTESIAN_POINT('Ctrl Pts',(-0.977741542134707,-5.11924968468906,
10.5401791637662));
#53877=CARTESIAN_POINT('Ctrl Pts',(-2.70946271325277,-4.45213518021386,
10.487415722906));
#53878=CARTESIAN_POINT('Ctrl Pts',(-3.76740545422127,-3.21078971494518,
10.4346522820458));
#53879=CARTESIAN_POINT('Ctrl Pts',(-4.51818187206105,-2.32986027932856,
10.3972083395828));
#53880=CARTESIAN_POINT('Ctrl Pts',(-4.92963472322582,-1.15974067526383,
10.3597643971199));
#53881=CARTESIAN_POINT('Ctrl Pts',(-4.93927523449924,0.00424456982664218,
10.3223204546569));
#53882=CARTESIAN_POINT('Ctrl Pts',(-4.94081497674544,0.00444099958366976,
10.1776795453431));
#53883=CARTESIAN_POINT('Ctrl Pts',(-4.92999654546744,-1.21362768880717,
10.2168943727512));
#53884=CARTESIAN_POINT('Ctrl Pts',(-4.47479284917987,-2.43892410978247,
10.2561092001592));
#53885=CARTESIAN_POINT('Ctrl Pts',(-3.65816585751927,-3.33475037626519,
10.2953240275673));
#53886=CARTESIAN_POINT('Ctrl Pts',(-2.5587073834856,-4.54083808828599,10.348120561042));
#53887=CARTESIAN_POINT('Ctrl Pts',(-0.804120636422241,-5.14971688740386,
10.4009170945167));
#53888=CARTESIAN_POINT('Ctrl Pts',(0.806103773459557,-4.88394658237934,
10.4537136279914));
#53889=CARTESIAN_POINT('Ctrl Pts',(2.41632818334133,-4.61817627735482,10.5065101614661));
#53890=CARTESIAN_POINT('Ctrl Pts',(3.88219025604155,-3.47775686818796,10.5593066949408));
#53891=CARTESIAN_POINT('Ctrl Pts',(4.53575894457716,-1.9823290114935,10.6121032284155));
#53892=CARTESIAN_POINT('Ctrl Pts',(5.18932763311279,-0.486901154799003,
10.6648997618902));
#53893=CARTESIAN_POINT('Ctrl Pts',(5.03060293748377,1.3635351494231,10.7176962953649));
#53894=CARTESIAN_POINT('Ctrl Pts',(4.13190895564446,2.72581472139719,10.7704928288396));
#53895=CARTESIAN_POINT('Ctrl Pts',(3.23321497380518,4.08809429337122,10.8232893623143));
#53896=CARTESIAN_POINT('Ctrl Pts',(1.5945517057557,4.96221713309726,10.876085895789));
#53897=CARTESIAN_POINT('Ctrl Pts',(-0.0374116408992591,4.94988261297637,
10.9288824292637));
#53898=CARTESIAN_POINT('Ctrl Pts',(-1.66937498755429,4.93754809285548,10.9816789627384));
#53899=CARTESIAN_POINT('Ctrl Pts',(-3.29463841281478,4.03875621288757,11.0344754962131));
#53900=CARTESIAN_POINT('Ctrl Pts',(-4.17263844793783,2.66304823386876,11.0872720296878));
#53901=CARTESIAN_POINT('Ctrl Pts',(-4.67379383761091,1.87780513509723,11.1174078682396));
#53902=CARTESIAN_POINT('Ctrl Pts',(-4.93148820012105,0.937181102537252,
11.1475437067913));
#53903=CARTESIAN_POINT('Ctrl Pts',(-4.93464332849729,-0.00183839903596135,
11.1776795453431));
#53904=CARTESIAN_POINT('Origin',(0.,0.,0.));
#53905=CARTESIAN_POINT('',(-4.9488440041135,-0.00213750530709822,12.3223204546569));
#53906=CARTESIAN_POINT('',(-4.94745353480859,-0.00311052193284108,12.1776795453431));
#53907=CARTESIAN_POINT('',(-4.942,-6.05220448138622E-16,0.));
#53908=CARTESIAN_POINT('Ctrl Pts',(-4.9488440041135,-0.00213750530709822,
12.3223204546569));
#53909=CARTESIAN_POINT('Ctrl Pts',(-4.94061448411462,1.50806390763245,12.2734955799156));
#53910=CARTESIAN_POINT('Ctrl Pts',(-4.19858957372796,3.0252638763299,12.2246707051742));
#53911=CARTESIAN_POINT('Ctrl Pts',(-2.99752188376984,3.93921020084163,12.1758458304329));
#53912=CARTESIAN_POINT('Ctrl Pts',(-1.69956742174719,4.92688201973019,12.1230823895727));
#53913=CARTESIAN_POINT('Ctrl Pts',(0.13447629685455,5.21004913441221,12.0703189487124));
#53914=CARTESIAN_POINT('Ctrl Pts',(1.669872996944,4.65983246739314,12.0175555078522));
#53915=CARTESIAN_POINT('Ctrl Pts',(3.20526969703341,4.10961580037408,11.964792066992));
#53916=CARTESIAN_POINT('Ctrl Pts',(4.44201937861055,2.72601535165399,11.9120286261318));
#53917=CARTESIAN_POINT('Ctrl Pts',(4.81723479316035,1.13875519654544,11.8592651852716));
#53918=CARTESIAN_POINT('Ctrl Pts',(5.19245020771016,-0.44850495856316,11.8065017444114));
#53919=CARTESIAN_POINT('Ctrl Pts',(4.70613135523258,-2.23942482006024,11.7537383035512));
#53920=CARTESIAN_POINT('Ctrl Pts',(3.57961864506819,-3.4188952610418,11.7009748626909));
#53921=CARTESIAN_POINT('Ctrl Pts',(2.45310593490382,-4.59836570202334,11.6482114218307));
#53922=CARTESIAN_POINT('Ctrl Pts',(0.686399367052665,-5.16638672248939,
11.5954479809705));
#53923=CARTESIAN_POINT('Ctrl Pts',(-0.916412232973623,-4.86443245089807,
11.5426845401103));
#53924=CARTESIAN_POINT('Ctrl Pts',(-2.51922383299994,-4.56247817930674,
11.4899210992501));
#53925=CARTESIAN_POINT('Ctrl Pts',(-3.95814046520138,-3.39054861565802,
11.4371576583899));
#53926=CARTESIAN_POINT('Ctrl Pts',(-4.57826175967478,-1.88202914695641,
11.3843942175297));
#53927=CARTESIAN_POINT('Ctrl Pts',(-4.82144315925703,-1.29046120861066,
11.3637029632387));
#53928=CARTESIAN_POINT('Ctrl Pts',(-4.93870801968536,-0.647131573531266,
11.3430117089478));
#53929=CARTESIAN_POINT('Ctrl Pts',(-4.93550942083981,-0.00268364051190351,
11.3223204546569));
#53930=CARTESIAN_POINT('Ctrl Pts',(-4.93464332849729,-0.00183839903596135,
11.1776795453431));
#53931=CARTESIAN_POINT('Ctrl Pts',(-4.93701583263233,-0.707935706243941,
11.200340240266));
#53932=CARTESIAN_POINT('Ctrl Pts',(-4.79546387301719,-1.41312576132387,
11.223000935189));
#53933=CARTESIAN_POINT('Ctrl Pts',(-4.50527725011862,-2.05066194500317,
11.2456616301119));
#53934=CARTESIAN_POINT('Ctrl Pts',(-3.82917937219074,-3.53604006678678,
11.2984581635866));
#53935=CARTESIAN_POINT('Ctrl Pts',(-2.34624697134931,-4.65417223228435,
11.3512546970613));
#53936=CARTESIAN_POINT('Ctrl Pts',(-0.732189317617651,-4.89557313460714,
11.404051230536));
#53937=CARTESIAN_POINT('Ctrl Pts',(0.881868336113988,-5.13697403692992,
11.4568477640108));
#53938=CARTESIAN_POINT('Ctrl Pts',(2.62705124273586,-4.50164367607793,11.5096442974855));
#53939=CARTESIAN_POINT('Ctrl Pts',(3.70815372246008,-3.27907509577412,11.5624408309602));
#53940=CARTESIAN_POINT('Ctrl Pts',(4.78925620218431,-2.05650651547028,11.6152373644349));
#53941=CARTESIAN_POINT('Ctrl Pts',(5.20627825501086,-0.246699715714593,
11.6680338979096));
#53942=CARTESIAN_POINT('Ctrl Pts',(4.76920065502008,1.32569326213742,11.7208304313843));
#53943=CARTESIAN_POINT('Ctrl Pts',(4.33212305502932,2.89808623998941,11.773626964859));
#53944=CARTESIAN_POINT('Ctrl Pts',(3.04094580222125,4.23306539593773,11.8264234983337));
#53945=CARTESIAN_POINT('Ctrl Pts',(1.48400349530759,4.72233746560275,11.8792200318084));
#53946=CARTESIAN_POINT('Ctrl Pts',(-0.0729388116060994,5.21160953526778,
11.9320165652831));
#53947=CARTESIAN_POINT('Ctrl Pts',(-1.89564617262539,4.85517451864949,11.9848130987578));
#53948=CARTESIAN_POINT('Ctrl Pts',(-3.15358830890438,3.81544470423333,12.0376096322325));
#53949=CARTESIAN_POINT('Ctrl Pts',(-4.26603410872305,2.89597231227191,12.0842996032694));
#53950=CARTESIAN_POINT('Ctrl Pts',(-4.93680336098554,1.44212692063929,12.1309895743062));
#53951=CARTESIAN_POINT('Ctrl Pts',(-4.94745353480859,-0.00311052193284108,
12.1776795453431));
#53952=CARTESIAN_POINT('Origin',(0.,0.,0.));
#53953=CARTESIAN_POINT('',(-4.94151427280004,0.00444821020356132,13.3223204546569));
#53954=CARTESIAN_POINT('',(-4.94372929093918,0.00429917225691094,13.1776795453431));
#53955=CARTESIAN_POINT('',(-4.942,-6.05220448138622E-16,0.));
#53956=CARTESIAN_POINT('Ctrl Pts',(-4.94151427280004,0.00444821020356132,
13.3223204546569));
#53957=CARTESIAN_POINT('Ctrl Pts',(-4.94510334294322,0.402329751972593,
13.3095063326037));
#53958=CARTESIAN_POINT('Ctrl Pts',(-4.90105411066494,0.799426659282486,
13.2966922105506));
#53959=CARTESIAN_POINT('Ctrl Pts',(-4.80630608075059,1.18403391346491,13.2838780884974));
#53960=CARTESIAN_POINT('Ctrl Pts',(-4.41617150483,2.76769310027955,13.2311146476372));
#53961=CARTESIAN_POINT('Ctrl Pts',(-3.16645719817481,4.13959474701713,13.178351206777));
#53962=CARTESIAN_POINT('Ctrl Pts',(-1.62595105536246,4.67533930486966,13.1255877659167));
#53963=CARTESIAN_POINT('Ctrl Pts',(-0.0854449125500667,5.21108386272221,
13.0728243250565));
#53964=CARTESIAN_POINT('Ctrl Pts',(1.74585306641946,4.91067133168968,13.0200608841963));
#53965=CARTESIAN_POINT('Ctrl Pts',(3.03445628684691,3.91082977043353,12.9672974433361));
#53966=CARTESIAN_POINT('Ctrl Pts',(4.3230595072743,2.91098820917742,12.9145340024759));
#53967=CARTESIAN_POINT('Ctrl Pts',(5.06896796915959,1.21171761769772,12.8617705616157));
#53968=CARTESIAN_POINT('Ctrl Pts',(4.9326931179398,-0.41358560700714,12.8090071207555));
#53969=CARTESIAN_POINT('Ctrl Pts',(4.79641826672,-2.03888883171205,12.7562436798952));
#53970=CARTESIAN_POINT('Ctrl Pts',(3.77796010239502,-3.59022468964221,12.703480239035));
#53971=CARTESIAN_POINT('Ctrl Pts',(2.34085390812233,-4.36152696093034,12.6507167981748));
#53972=CARTESIAN_POINT('Ctrl Pts',(0.903747713849633,-5.13282923221848,
12.5979533573146));
#53973=CARTESIAN_POINT('Ctrl Pts',(-0.952006510370724,-5.12409791686467,
12.5451899164544));
#53974=CARTESIAN_POINT('Ctrl Pts',(-2.38179129282902,-4.33930693630882,
12.4924264755942));
#53975=CARTESIAN_POINT('Ctrl Pts',(-3.81157607528729,-3.55451595575297,
12.4396630347339));
#53976=CARTESIAN_POINT('Ctrl Pts',(-4.81539141598345,-1.99366530999509,
12.3868995938737));
#53977=CARTESIAN_POINT('Ctrl Pts',(-4.93636648360977,-0.367151725568608,
12.3341361530135));
#53978=CARTESIAN_POINT('Ctrl Pts',(-4.94539675712518,-0.245739414485935,
12.3301975868946));
#53979=CARTESIAN_POINT('Ctrl Pts',(-4.94950785648002,-0.123961230389695,
12.3262590207758));
#53980=CARTESIAN_POINT('Ctrl Pts',(-4.9488440041135,-0.00213750530709822,
12.3223204546569));
#53981=CARTESIAN_POINT('Ctrl Pts',(-4.94745353480859,-0.00311052193284108,
12.1776795453431));
#53982=CARTESIAN_POINT('Ctrl Pts',(-4.94884646673765,-0.192132542820318,
12.1837861077809));
#53983=CARTESIAN_POINT('Ctrl Pts',(-4.93894745560412,-0.381007316833933,
12.1898926702188));
#53984=CARTESIAN_POINT('Ctrl Pts',(-4.91726778514412,-0.568520045648731,
12.1959992326566));
#53985=CARTESIAN_POINT('Ctrl Pts',(-4.72982821356618,-2.18973036890068,
12.2487957661313));
#53986=CARTESIAN_POINT('Ctrl Pts',(-3.6617721588716,-3.70912640319057,12.301592299606));
#53987=CARTESIAN_POINT('Ctrl Pts',(-2.19976737250484,-4.4343839504472,12.3543888330807));
#53988=CARTESIAN_POINT('Ctrl Pts',(-0.737762586138102,-5.15964149770382,
12.4071853665554));
#53989=CARTESIAN_POINT('Ctrl Pts',(1.1181909319008,-5.09076055792721,12.4599819000301));
#53990=CARTESIAN_POINT('Ctrl Pts',(2.52241404198307,-4.25912724791444,12.5127784335048));
#53991=CARTESIAN_POINT('Ctrl Pts',(3.92663715206537,-3.42749393790165,12.5655749669795));
#53992=CARTESIAN_POINT('Ctrl Pts',(4.87912985419102,-1.83310825765268,12.6183715004542));
#53993=CARTESIAN_POINT('Ctrl Pts',(4.94588170520655,-0.202463999821435,
12.6711680339289));
#53994=CARTESIAN_POINT('Ctrl Pts',(5.01263355622208,1.42818025800979,12.7239645674036));
#53995=CARTESIAN_POINT('Ctrl Pts',(4.1936445561275,3.09508309342328,12.7767611008784));
#53996=CARTESIAN_POINT('Ctrl Pts',(2.86209318500527,4.03870772815599,12.8295576343531));
#53997=CARTESIAN_POINT('Ctrl Pts',(1.53054181388302,4.98233236288871,12.8823541678278));
#53998=CARTESIAN_POINT('Ctrl Pts',(-0.313571928266912,5.20267879694063,
12.9351507013025));
#53999=CARTESIAN_POINT('Ctrl Pts',(-1.82996378449454,4.59934452509909,12.9879472347772));
#54000=CARTESIAN_POINT('Ctrl Pts',(-3.34635564072214,3.99601025325757,13.0407437682519));
#54001=CARTESIAN_POINT('Ctrl Pts',(-4.53502561102745,2.56899527552262,13.0935403017266));
#54002=CARTESIAN_POINT('Ctrl Pts',(-4.85434730874721,0.968529668713999,
13.1463368352013));
#54003=CARTESIAN_POINT('Ctrl Pts',(-4.917535847558,0.651823714081653,13.1567844052486));
#54004=CARTESIAN_POINT('Ctrl Pts',(-4.94668250438369,0.328325791222804,
13.1672319752958));
#54005=CARTESIAN_POINT('Ctrl Pts',(-4.94372929093918,0.00429917225691095,
13.1776795453431));
#54006=CARTESIAN_POINT('Origin',(0.,0.,0.));
#54007=CARTESIAN_POINT('',(-4.93448587773112,-0.00157506815688546,14.3223204546569));
#54008=CARTESIAN_POINT('',(-4.93400159721632,-0.000305393655117946,14.1776795453431));
#54009=CARTESIAN_POINT('',(-4.942,-6.05220448138622E-16,0.));
#54010=CARTESIAN_POINT('Ctrl Pts',(-4.93448587773112,-0.00157506815688546,
14.3223204546569));
#54011=CARTESIAN_POINT('Ctrl Pts',(-4.9318360603942,0.919788438910237,14.2927536444317));
#54012=CARTESIAN_POINT('Ctrl Pts',(-4.68434909382344,1.84247391790569,14.2631868342065));
#54013=CARTESIAN_POINT('Ctrl Pts',(-4.20094243104244,2.61812855704659,14.2336200239813));
#54014=CARTESIAN_POINT('Ctrl Pts',(-3.3382792398224,4.00232277240241,14.180856583121));
#54015=CARTESIAN_POINT('Ctrl Pts',(-1.72430206586684,4.91828000860559,14.1280931422608));
#54016=CARTESIAN_POINT('Ctrl Pts',(-0.0935873430086671,4.94911667465072,
14.0753297014006));
#54017=CARTESIAN_POINT('Ctrl Pts',(1.53712737984951,4.97995334069586,14.0225662605404));
#54018=CARTESIAN_POINT('Ctrl Pts',(3.18457965161027,4.12566943658293,13.9698028196802));
#54019=CARTESIAN_POINT('Ctrl Pts',(4.09895737196505,2.77507890210349,13.91703937882));
#54020=CARTESIAN_POINT('Ctrl Pts',(5.01333509231982,1.42448836762405,13.8642759379598));
#54021=CARTESIAN_POINT('Ctrl Pts',(5.19463826126858,-0.422408797221965,
13.8115124970995));
#54022=CARTESIAN_POINT('Ctrl Pts',(4.56034958089476,-1.92502627258323,13.7587490562393));
#54023=CARTESIAN_POINT('Ctrl Pts',(3.92606090052093,-3.42764374794451,13.7059856153791));
#54024=CARTESIAN_POINT('Ctrl Pts',(2.47618037082453,-4.58598153382108,13.6532221745189));
#54025=CARTESIAN_POINT('Ctrl Pts',(0.870598407947765,-4.87284032799863,
13.6004587336587));
#54026=CARTESIAN_POINT('Ctrl Pts',(-0.734983554928979,-5.15969912217617,
13.5476952927985));
#54027=CARTESIAN_POINT('Ctrl Pts',(-2.49626695098606,-4.57507892465472,
13.4949318519383));
#54028=CARTESIAN_POINT('Ctrl Pts',(-3.61163122642161,-3.38506046244813,
13.442168411078));
#54029=CARTESIAN_POINT('Ctrl Pts',(-4.45611828600162,-2.48404972171741,
13.402219092271));
#54030=CARTESIAN_POINT('Ctrl Pts',(-4.93032498439027,-1.23598765372993,
13.3622697734639));
#54031=CARTESIAN_POINT('Ctrl Pts',(-4.94151427280004,0.00444821020356132,
13.3223204546569));
#54032=CARTESIAN_POINT('Ctrl Pts',(-4.94372929093918,0.00429917225691095,
13.1776795453431));
#54033=CARTESIAN_POINT('Ctrl Pts',(-4.93175851423331,-1.30913460937943,
13.2200285087705));
#54034=CARTESIAN_POINT('Ctrl Pts',(-4.39236571089229,-2.63125521653574,
13.262377472198));
#54035=CARTESIAN_POINT('Ctrl Pts',(-3.45489131803353,-3.54492080217556,
13.3047264356254));
#54036=CARTESIAN_POINT('Ctrl Pts',(-2.28614020446586,-4.68398943037421,
13.3575229691001));
#54037=CARTESIAN_POINT('Ctrl Pts',(-0.498664552196314,-5.18821045088918,
13.4103195025748));
#54038=CARTESIAN_POINT('Ctrl Pts',(1.09305895224904,-4.82783177420557,13.4631160360495));
#54039=CARTESIAN_POINT('Ctrl Pts',(2.68478245669437,-4.46745309752197,13.5159125695242));
#54040=CARTESIAN_POINT('Ctrl Pts',(4.08075381331552,-3.2424747236398,13.5687091029989));
#54041=CARTESIAN_POINT('Ctrl Pts',(4.64488820407174,-1.71106723561516,13.6215056364736));
#54042=CARTESIAN_POINT('Ctrl Pts',(5.20902259482797,-0.179659747590474,
13.6743021699483));
#54043=CARTESIAN_POINT('Ctrl Pts',(4.94132001971923,1.6581768545767,13.727098703423));
#54044=CARTESIAN_POINT('Ctrl Pts',(3.9637611647886,2.96501853984655,13.7798952368977));
#54045=CARTESIAN_POINT('Ctrl Pts',(2.98620230985801,4.27186022511634,13.8326917703724));
#54046=CARTESIAN_POINT('Ctrl Pts',(1.29878717510559,5.04770699348884,13.8854883038471));
#54047=CARTESIAN_POINT('Ctrl Pts',(-0.32960087817538,4.93903844632007,13.9382848373218));
#54048=CARTESIAN_POINT('Ctrl Pts',(-1.95798893145639,4.8303698991513,13.9910813707965));
#54049=CARTESIAN_POINT('Ctrl Pts',(-3.52734990326595,3.8371860364412,14.0438779042712));
#54050=CARTESIAN_POINT('Ctrl Pts',(-4.32259269702876,2.41203853383676,14.0966744377459));
#54051=CARTESIAN_POINT('Ctrl Pts',(-4.72930328852039,1.68317611811527,14.1236761402783));
#54052=CARTESIAN_POINT('Ctrl Pts',(-4.93353545879958,0.841329253368597,
14.1506778428107));
#54053=CARTESIAN_POINT('Ctrl Pts',(-4.93400159721632,-0.000305393655117946,
14.1776795453431));
#54054=CARTESIAN_POINT('Origin',(0.,0.,0.));
#54055=CARTESIAN_POINT('',(-4.94718090754756,-0.00323194414963146,15.3223204546569));
#54056=CARTESIAN_POINT('',(-4.9448369857261,-0.0040807615555026,15.1776795453431));
#54057=CARTESIAN_POINT('',(-4.942,-6.05220448138622E-16,0.));
#54058=CARTESIAN_POINT('Ctrl Pts',(-4.94718090754756,-0.00323194414963146,
15.3223204546569));
#54059=CARTESIAN_POINT('Ctrl Pts',(-4.93629962156844,1.4307451373895,15.2760009562597));
#54060=CARTESIAN_POINT('Ctrl Pts',(-4.27737587184649,2.87344030248637,15.2296814578624));
#54061=CARTESIAN_POINT('Ctrl Pts',(-3.18014090814091,3.79331230684891,15.1833619594651));
#54062=CARTESIAN_POINT('Ctrl Pts',(-1.93025923583274,4.84115638505733,15.1305985186049));
#54063=CARTESIAN_POINT('Ctrl Pts',(-0.111627961864901,5.21058874364864,
15.0778350777447));
#54064=CARTESIAN_POINT('Ctrl Pts',(1.44803137056367,4.73346803090561,15.0250716368845));
#54065=CARTESIAN_POINT('Ctrl Pts',(3.00769070299228,4.25634731816257,14.9723081960243));
#54066=CARTESIAN_POINT('Ctrl Pts',(4.30837809388161,2.93267353408514,14.9195447551641));
#54067=CARTESIAN_POINT('Ctrl Pts',(4.75810604814116,1.36489607082845,14.8667813143038));
#54068=CARTESIAN_POINT('Ctrl Pts',(5.20783400240071,-0.202881392428214,
14.8140178734436));
#54069=CARTESIAN_POINT('Ctrl Pts',(4.80660252003052,-2.01476253486414,14.7612544325834));
#54070=CARTESIAN_POINT('Ctrl Pts',(3.73702582619445,-3.2460980306936,14.7084909917232));
#54071=CARTESIAN_POINT('Ctrl Pts',(2.66744913235836,-4.47743352652308,14.655727550863));
#54072=CARTESIAN_POINT('Ctrl Pts',(0.929527227056376,-5.12822337574609,
14.6029641100028));
#54073=CARTESIAN_POINT('Ctrl Pts',(-0.685751952425607,-4.90227077075043,
14.5502006691425));
#54074=CARTESIAN_POINT('Ctrl Pts',(-2.30103113190757,-4.67631816575478,
14.4974372282823));
#54075=CARTESIAN_POINT('Ctrl Pts',(-3.79366758556953,-3.57362310654048,
14.4446737874221));
#54076=CARTESIAN_POINT('Ctrl Pts',(-4.48431120815826,-2.09605997967911,
14.3919103465619));
#54077=CARTESIAN_POINT('Ctrl Pts',(-4.78794199402862,-1.44647220574097,
14.3687137159269));
#54078=CARTESIAN_POINT('Ctrl Pts',(-4.93656479099726,-0.724430485809702,
14.3455170852919));
#54079=CARTESIAN_POINT('Ctrl Pts',(-4.93448587773112,-0.00157506815688546,
14.3223204546569));
#54080=CARTESIAN_POINT('Ctrl Pts',(-4.93400159721632,-0.000305393655117946,
14.1776795453431));
#54081=CARTESIAN_POINT('Ctrl Pts',(-4.93444690105008,-0.804322229598714,
14.2034743762854));
#54082=CARTESIAN_POINT('Ctrl Pts',(-4.74893420650715,-1.60814539448429,
14.2292692072277));
#54083=CARTESIAN_POINT('Ctrl Pts',(-4.37634095459745,-2.31308827376533,
14.2550640381701));
#54084=CARTESIAN_POINT('Ctrl Pts',(-3.61372180268731,-3.75595643626419,
14.3078605716448));
#54085=CARTESIAN_POINT('Ctrl Pts',(-2.06735888315097,-4.78458161876317,
14.3606571051195));
#54086=CARTESIAN_POINT('Ctrl Pts',(-0.44186405756573,-4.93026304245127,
14.4134536385942));
#54087=CARTESIAN_POINT('Ctrl Pts',(1.18363076801951,-5.07594446613938,14.4662501720689));
#54088=CARTESIAN_POINT('Ctrl Pts',(2.88825749965368,-4.33868213101661,14.5190467055436));
#54089=CARTESIAN_POINT('Ctrl Pts',(3.89529018284092,-3.05441514934954,14.5718432390183));
#54090=CARTESIAN_POINT('Ctrl Pts',(4.90232286602818,-1.77014816768244,14.624639772493));
#54091=CARTESIAN_POINT('Ctrl Pts',(5.21176150076849,0.0611234605289337,
14.6774363059677));
#54092=CARTESIAN_POINT('Ctrl Pts',(4.682608052441,1.60496708387405,14.7302328394424));
#54093=CARTESIAN_POINT('Ctrl Pts',(4.15345460411353,3.1488107072191,14.7830293729171));
#54094=CARTESIAN_POINT('Ctrl Pts',(2.78570907271829,4.40522632569788,14.8358259063918));
#54095=CARTESIAN_POINT('Ctrl Pts',(1.20259496734194,4.80171873996239,14.8886224398665));
#54096=CARTESIAN_POINT('Ctrl Pts',(-0.380519138034476,5.19821115422692,
14.9414189733412));
#54097=CARTESIAN_POINT('Ctrl Pts',(-2.17900181739205,4.73478036427711,14.9942155068159));
#54098=CARTESIAN_POINT('Ctrl Pts',(-3.3733609497546,3.62259208519558,15.0470120402906));
#54099=CARTESIAN_POINT('Ctrl Pts',(-4.35867771010103,2.70506424759102,15.0905678753081));
#54100=CARTESIAN_POINT('Ctrl Pts',(-4.93283752130763,1.34600230443831,15.1341237103256));
#54101=CARTESIAN_POINT('Ctrl Pts',(-4.9448369857261,-0.0040807615555026,
15.1776795453431));
#54102=CARTESIAN_POINT('Origin',(0.,0.,0.));
#54103=CARTESIAN_POINT('',(-4.94384666289092,0.00426556420662083,16.3223204546569));
#54104=CARTESIAN_POINT('',(-4.94650740111161,0.00354971811832453,16.1776795453431));
#54105=CARTESIAN_POINT('',(-4.942,-6.05220448138622E-16,0.));
#54106=CARTESIAN_POINT('Ctrl Pts',(-4.94384666289092,0.00426556420662083,
16.3223204546569));
#54107=CARTESIAN_POINT('Ctrl Pts',(-4.94674943417405,0.323967179430384,
16.3120117089478));
#54108=CARTESIAN_POINT('Ctrl Pts',(-4.91837466800284,0.643155833620532,
16.3017029632387));
#54109=CARTESIAN_POINT('Ctrl Pts',(-4.85684297990262,0.955819257318147,
16.2913942175296));
#54110=CARTESIAN_POINT('Ctrl Pts',(-4.5419042203555,2.55613015167716,16.2386307766694));
#54111=CARTESIAN_POINT('Ctrl Pts',(-3.35834756654112,3.98549839996768,16.1858673358092));
#54112=CARTESIAN_POINT('Ctrl Pts',(-1.84485020909617,4.59336938114029,16.133103894949));
#54113=CARTESIAN_POINT('Ctrl Pts',(-0.331352851651252,5.20124036231289,
16.0803404540888));
#54114=CARTESIAN_POINT('Ctrl Pts',(1.51208520942422,4.98761407636759,16.0275770132286));
#54115=CARTESIAN_POINT('Ctrl Pts',(2.84645196705723,4.04971920709069,15.9748135723683));
#54116=CARTESIAN_POINT('Ctrl Pts',(4.18081872469025,3.11182433781378,15.9220501315081));
#54117=CARTESIAN_POINT('Ctrl Pts',(5.00611417888079,1.44966088520527,15.8692866906479));
#54118=CARTESIAN_POINT('Ctrl Pts',(4.94671805190497,-0.180263500133812,
15.8165232497877));
#54119=CARTESIAN_POINT('Ctrl Pts',(4.88732192492914,-1.81018788547292,15.7637598089275));
#54120=CARTESIAN_POINT('Ctrl Pts',(3.94323421678691,-3.40787320354259,15.7109963680673));
#54121=CARTESIAN_POINT('Ctrl Pts',(2.54414165016166,-4.24615799663446,15.6582329272071));
#54122=CARTESIAN_POINT('Ctrl Pts',(1.14504908353641,-5.08444278972633,15.6054694863468));
#54123=CARTESIAN_POINT('Ctrl Pts',(-0.709048341571857,-5.16332705784039,
15.5527060454866));
#54124=CARTESIAN_POINT('Ctrl Pts',(-2.17428721330366,-4.44690786540681,
15.4999426046264));
#54125=CARTESIAN_POINT('Ctrl Pts',(-3.63952608503543,-3.73048867297323,
15.4471791637662));
#54126=CARTESIAN_POINT('Ctrl Pts',(-4.71590640339076,-2.21876601999203,
15.394415722906));
#54127=CARTESIAN_POINT('Ctrl Pts',(-4.91353052724419,-0.59977679458864,
15.3416522820458));
#54128=CARTESIAN_POINT('Ctrl Pts',(-4.93766614961155,-0.402051376257967,
15.3352083395828));
#54129=CARTESIAN_POINT('Ctrl Pts',(-4.94869470590891,-0.202726026045579,
15.3287643971199));
#54130=CARTESIAN_POINT('Ctrl Pts',(-4.94718090754756,-0.00323194414963146,
15.3223204546569));
#54131=CARTESIAN_POINT('Ctrl Pts',(-4.9448369857261,-0.0040807615555026,
15.1776795453431));
#54132=CARTESIAN_POINT('Ctrl Pts',(-4.94738276248126,-0.290511052698514,
15.1869202438003));
#54133=CARTESIAN_POINT('Ctrl Pts',(-4.92462524198781,-0.576537197232804,
15.1961609422575));
#54134=CARTESIAN_POINT('Ctrl Pts',(-4.8751224347969,-0.857857073631679,
15.2054016407147));
#54135=CARTESIAN_POINT('Ctrl Pts',(-4.59228920210912,-2.46517218516427,
15.2581981741894));
#54136=CARTESIAN_POINT('Ctrl Pts',(-3.436387151366,-3.91885664001626,15.3109947076642));
#54137=CARTESIAN_POINT('Ctrl Pts',(-1.93411172090367,-4.55652821395913,
15.3637912411389));
#54138=CARTESIAN_POINT('Ctrl Pts',(-0.431836290441309,-5.19419978790203,
15.4165877746136));
#54139=CARTESIAN_POINT('Ctrl Pts',(1.41681251974025,-5.01585848093576,15.4693843080882));
#54140=CARTESIAN_POINT('Ctrl Pts',(2.76948401487652,-4.1027668473702,15.522180841563));
#54141=CARTESIAN_POINT('Ctrl Pts',(4.12215551001273,-3.18967521380468,15.5749773750377));
#54142=CARTESIAN_POINT('Ctrl Pts',(4.97884969010367,-1.54183325363995,15.6277739085124));
#54143=CARTESIAN_POINT('Ctrl Pts',(4.94920742712676,0.0899074861556964,
15.6805704419871));
#54144=CARTESIAN_POINT('Ctrl Pts',(4.91956516414985,1.72164822595137,15.7333669754618));
#54145=CARTESIAN_POINT('Ctrl Pts',(4.00358645810502,3.33728774537801,15.7861635089365));
#54146=CARTESIAN_POINT('Ctrl Pts',(2.61864387578884,4.200647779537,15.8389600424112));
#54147=CARTESIAN_POINT('Ctrl Pts',(1.23370129347265,5.06400781369599,15.8917565758859));
#54148=CARTESIAN_POINT('Ctrl Pts',(-0.620205165114908,5.17508836258739,
15.9445531093606));
#54149=CARTESIAN_POINT('Ctrl Pts',(-2.09832911795802,4.48327474299608,15.9973496428353));
#54150=CARTESIAN_POINT('Ctrl Pts',(-3.57645307080114,3.79146112340477,16.05014617631));
#54151=CARTESIAN_POINT('Ctrl Pts',(-4.67879451789979,2.29675333533074,16.1029427097847));
#54152=CARTESIAN_POINT('Ctrl Pts',(-4.90306331235317,0.680226188554136,
16.1557392432594));
#54153=CARTESIAN_POINT('Ctrl Pts',(-4.93412927302912,0.456303065875542,
16.1630526772873));
#54154=CARTESIAN_POINT('Ctrl Pts',(-4.94834669148062,0.23004246166547,16.1703661113152));
#54155=CARTESIAN_POINT('Ctrl Pts',(-4.94650740111161,0.00354971811832453,
16.1776795453431));
#54156=CARTESIAN_POINT('Origin',(0.,0.,0.));
#54157=CARTESIAN_POINT('',(-4.93403031428168,-0.000341981052076612,17.3223204546569));
#54158=CARTESIAN_POINT('',(-4.93428824426153,0.00126466874552048,17.1776795453431));
#54159=CARTESIAN_POINT('',(-4.942,-6.05220448138622E-16,0.));
#54160=CARTESIAN_POINT('Ctrl Pts',(-4.93403031428168,-0.000341981052076612,
17.3223204546569));
#54161=CARTESIAN_POINT('Ctrl Pts',(-4.93350394108414,0.843143514252388,
17.2952590207758));
#54162=CARTESIAN_POINT('Ctrl Pts',(-4.72829119907115,1.68686850434222,17.2681975868947));
#54163=CARTESIAN_POINT('Ctrl Pts',(-4.31985335744029,2.41689215977968,17.2411361530135));
#54164=CARTESIAN_POINT('Ctrl Pts',(-3.52349548532491,3.84026684640702,17.1883727121533));
#54165=CARTESIAN_POINT('Ctrl Pts',(-1.9545602926493,4.83139633972401,17.1356092712931));
#54166=CARTESIAN_POINT('Ctrl Pts',(-0.327119944589159,4.9391812045894,17.0828458304329));
#54167=CARTESIAN_POINT('Ctrl Pts',(1.30032040347096,5.04696606945479,17.0300823895727));
#54168=CARTESIAN_POINT('Ctrl Pts',(2.98626590691563,4.2714063058686,16.9773189487124));
#54169=CARTESIAN_POINT('Ctrl Pts',(3.96338272054503,2.96548703306019,16.9245555078522));
#54170=CARTESIAN_POINT('Ctrl Pts',(4.94049953417446,1.65956776025175,16.871792066992));
#54171=CARTESIAN_POINT('Ctrl Pts',(5.20878765798859,-0.176711021778891,
16.8190286261318));
#54172=CARTESIAN_POINT('Ctrl Pts',(4.64614108062899,-1.70759643201752,16.7662651852716));
#54173=CARTESIAN_POINT('Ctrl Pts',(4.0834945032694,-3.2384818422561,16.7135017444114));
#54174=CARTESIAN_POINT('Ctrl Pts',(2.68991322473609,-4.46397388070265,16.6607383035511));
#54175=CARTESIAN_POINT('Ctrl Pts',(1.09966334943406,-4.82630869971703,16.6079748626909));
#54176=CARTESIAN_POINT('Ctrl Pts',(-0.490586525867957,-5.18864351873141,
16.5552114218307));
#54177=CARTESIAN_POINT('Ctrl Pts',(-2.27750499793871,-4.68782111831362,
16.5024479809705));
#54178=CARTESIAN_POINT('Ctrl Pts',(-3.44780380133416,-3.551783147891,16.4496845401103));
#54179=CARTESIAN_POINT('Ctrl Pts',(-4.38945351416312,-2.63770050035899,
16.4072298449592));
#54180=CARTESIAN_POINT('Ctrl Pts',(-4.93189212706316,-1.31236741876541,
16.364775149808));
#54181=CARTESIAN_POINT('Ctrl Pts',(-4.94384666289092,0.00426556420662083,
16.3223204546569));
#54182=CARTESIAN_POINT('Ctrl Pts',(-4.94650740111161,0.00354971811832453,
16.1776795453431));
#54183=CARTESIAN_POINT('Ctrl Pts',(-4.93506863972457,-1.40503507794796,
16.2231626447899));
#54184=CARTESIAN_POINT('Ctrl Pts',(-4.30259793428105,-2.82259842281934,
16.2686457442367));
#54185=CARTESIAN_POINT('Ctrl Pts',(-3.23956236772638,-3.74272269838241,
16.3141288436835));
#54186=CARTESIAN_POINT('Ctrl Pts',(-2.00559648683807,-4.81079793306321,
16.3669253771582));
#54187=CARTESIAN_POINT('Ctrl Pts',(-0.191468583253334,-5.20860189694556,
16.4197219106329));
#54188=CARTESIAN_POINT('Ctrl Pts',(1.37620035566145,-4.75487224416495,16.4725184441076));
#54189=CARTESIAN_POINT('Ctrl Pts',(2.94386929457619,-4.30114259138436,16.5253149775823));
#54190=CARTESIAN_POINT('Ctrl Pts',(4.265079268821,-2.99587932194087,16.578111511057));
#54191=CARTESIAN_POINT('Ctrl Pts',(4.73781104997921,-1.43383540748133,16.6309080445317));
#54192=CARTESIAN_POINT('Ctrl Pts',(5.21054283113743,0.128208506978224,16.6837045780064));
#54193=CARTESIAN_POINT('Ctrl Pts',(4.83479641920902,1.94703306645383,16.7365011114811));
#54194=CARTESIAN_POINT('Ctrl Pts',(3.78178347511922,3.19387716968194,16.7892976449558));
#54195=CARTESIAN_POINT('Ctrl Pts',(2.72877053102942,4.44072127291004,16.8420941784306));
#54196=CARTESIAN_POINT('Ctrl Pts',(0.998491054778278,5.11558491989063,16.8948907119053));
#54197=CARTESIAN_POINT('Ctrl Pts',(-0.620640115192454,4.91096152429156,
16.94768724538));
#54198=CARTESIAN_POINT('Ctrl Pts',(-2.23977128516316,4.70633812869249,17.0004837788547));
#54199=CARTESIAN_POINT('Ctrl Pts',(-3.74775414885348,3.62222769051368,17.0532803123294));
#54200=CARTESIAN_POINT('Ctrl Pts',(-4.45746504028889,2.1526130784761,17.1060768458041));
#54201=CARTESIAN_POINT('Ctrl Pts',(-4.77830186027552,1.48824892058866,17.1299444123171));
#54202=CARTESIAN_POINT('Ctrl Pts',(-4.93600022440261,0.745101393327629,
17.1538119788301));
#54203=CARTESIAN_POINT('Ctrl Pts',(-4.93428824426153,0.00126466874552048,
17.1776795453431));
#54204=CARTESIAN_POINT('Origin',(0.,0.,0.));
#54205=CARTESIAN_POINT('',(-4.94522242777803,-0.0039236424385497,18.3223204546569));
#54206=CARTESIAN_POINT('',(-4.94192999916445,-0.00446510791632448,18.1776795453431));
#54207=CARTESIAN_POINT('',(-4.942,-6.05220448138622E-16,0.));
#54208=CARTESIAN_POINT('Ctrl Pts',(-4.94522242777803,-0.0039236424385497,
18.3223204546569));
#54209=CARTESIAN_POINT('Ctrl Pts',(-4.93329330491003,1.35399213993734,18.2785063326037));
#54210=CARTESIAN_POINT('Ctrl Pts',(-4.3513066594067,2.72080403156538,18.2346922105506));
#54211=CARTESIAN_POINT('Ctrl Pts',(-3.35561026819536,3.63892235657103,18.1908780884974));
#54212=CARTESIAN_POINT('Ctrl Pts',(-2.15653642646331,4.74457230855067,18.1381146476372));
#54213=CARTESIAN_POINT('Ctrl Pts',(-0.35748677154393,5.19951173147208,18.085351206777));
#54214=CARTESIAN_POINT('Ctrl Pts',(1.22293027595834,4.79656649826054,18.0325877659168));
#54215=CARTESIAN_POINT('Ctrl Pts',(2.80334732346066,4.39362126504898,17.9798243250565));
#54216=CARTESIAN_POINT('Ctrl Pts',(4.16513176354582,3.13279137570437,17.9270608841963));
#54217=CARTESIAN_POINT('Ctrl Pts',(4.68838366687364,1.58798426669984,17.8742974433361));
#54218=CARTESIAN_POINT('Ctrl Pts',(5.21163557020145,0.0431771576953521,
17.8215340024759));
#54219=CARTESIAN_POINT('Ctrl Pts',(4.89635493677199,-1.78560717096906,17.7687705616157));
#54220=CARTESIAN_POINT('Ctrl Pts',(3.88609177304056,-3.06605780050668,17.7160071207555));
#54221=CARTESIAN_POINT('Ctrl Pts',(2.87582860930912,-4.34650843004432,17.6632436798953));
#54222=CARTESIAN_POINT('Ctrl Pts',(1.17058291527568,-5.07862536045516,17.610480239035));
#54223=CARTESIAN_POINT('Ctrl Pts',(-0.453558190725748,-4.92918049163674,
17.5577167981748));
#54224=CARTESIAN_POINT('Ctrl Pts',(-2.0776992967272,-4.77973562281832,17.5049533573146));
#54225=CARTESIAN_POINT('Ctrl Pts',(-3.62073581469659,-3.74872895477065,
17.4521899164544));
#54226=CARTESIAN_POINT('Ctrl Pts',(-4.38036379790372,-2.30541568077795,
17.3994264755942));
#54227=CARTESIAN_POINT('Ctrl Pts',(-4.75039204866972,-1.6023522103828,17.3737244686151));
#54228=CARTESIAN_POINT('Ctrl Pts',(-4.93453024520391,-0.801455114314277,
17.348022461636));
#54229=CARTESIAN_POINT('Ctrl Pts',(-4.93403031428168,-0.000341981052076612,
17.3223204546569));
#54230=CARTESIAN_POINT('Ctrl Pts',(-4.93428824426153,0.00126466874552048,
17.1776795453431));
#54231=CARTESIAN_POINT('Ctrl Pts',(-4.93221321843459,-0.900311452079429,
17.2066085123048));
#54232=CARTESIAN_POINT('Ctrl Pts',(-4.69594942149747,-1.80290006851385,
17.2355374792665));
#54233=CARTESIAN_POINT('Ctrl Pts',(-4.23213525097133,-2.56744414176908,
17.2644664462282));
#54234=CARTESIAN_POINT('Ctrl Pts',(-3.38565565103777,-3.96276796408032,
17.3172629797029));
#54235=CARTESIAN_POINT('Ctrl Pts',(-1.78125753199004,-4.89829682280636,
17.3700595131776));
#54236=CARTESIAN_POINT('Ctrl Pts',(-0.149997058388728,-4.94775064594635,
17.4228560466523));
#54237=CARTESIAN_POINT('Ctrl Pts',(1.48126341521252,-4.99720446908635,17.475652580127));
#54238=CARTESIAN_POINT('Ctrl Pts',(3.13938624336737,-4.16058325664038,17.5284491136017));
#54239=CARTESIAN_POINT('Ctrl Pts',(4.06883557073125,-2.81909846013186,17.5812456470764));
#54240=CARTESIAN_POINT('Ctrl Pts',(4.99828489809513,-1.47761366362332,17.6340421805511));
#54241=CARTESIAN_POINT('Ctrl Pts',(5.19906072466804,0.368734716947733,17.6868387140258));
#54242=CARTESIAN_POINT('Ctrl Pts',(4.57967756755998,1.87864175098721,17.7396352475005));
#54243=CARTESIAN_POINT('Ctrl Pts',(3.9602944104519,3.38854878502672,17.7924317809752));
#54244=CARTESIAN_POINT('Ctrl Pts',(2.52075226966277,4.56201447253459,17.8452283144499));
#54245=CARTESIAN_POINT('Ctrl Pts',(0.916990219673444,4.86434504442812,17.8980248479246));
#54246=CARTESIAN_POINT('Ctrl Pts',(-0.68677183031584,5.16667561632164,17.9508213813993));
#54247=CARTESIAN_POINT('Ctrl Pts',(-2.45475378950534,4.59787107260088,18.003617914874));
#54248=CARTESIAN_POINT('Ctrl Pts',(-3.58136314295608,3.4171025376229,18.0564144483487));
#54249=CARTESIAN_POINT('Ctrl Pts',(-4.44390962426003,2.51309109660283,18.0968361473469));
#54250=CARTESIAN_POINT('Ctrl Pts',(-4.93050729338922,1.25036908149785,18.137257846345));
#54251=CARTESIAN_POINT('Ctrl Pts',(-4.94192999916445,-0.00446510791632448,
18.1776795453431));
#54252=CARTESIAN_POINT('Origin',(0.,0.,-1.84858989190501));
#54253=CARTESIAN_POINT('',(-4.37485075966118,-0.00347109768167049,18.651410108095));
#54254=CARTESIAN_POINT('',(-4.37798451307649,0.0018411544964702,18.848589891905));
#54255=CARTESIAN_POINT('',(-4.372,-4.40683631492666E-13,-1.84858989190501));
#54256=CARTESIAN_POINT('',(-4.32479004603203,0.640761311052912,19.628));
#54257=CARTESIAN_POINT('Ctrl Pts',(-4.37485075966118,-0.00347109768167011,
18.651410108095));
#54258=CARTESIAN_POINT('Ctrl Pts',(-4.37700632796887,-0.248843725443851,
18.660359426902));
#54259=CARTESIAN_POINT('Ctrl Pts',(-4.24678226663423,-1.93862138449445,
18.7220721865693));
#54260=CARTESIAN_POINT('Ctrl Pts',(-2.04533412033072,-4.73987705500777,
18.8365483870968));
#54261=CARTESIAN_POINT('Ctrl Pts',(2.85792925831606,-4.29723869811459,18.9948387096774));
#54262=CARTESIAN_POINT('Ctrl Pts',(5.16462833680317,0.0542185969503185,
19.1531290322581));
#54263=CARTESIAN_POINT('Ctrl Pts',(2.76051461044002,4.36178489183685,19.3114193548387));
#54264=CARTESIAN_POINT('Ctrl Pts',(-1.32005059452733,4.63359119197125,19.4433279569892));
#54265=CARTESIAN_POINT('Ctrl Pts',(-3.63987183575178,2.72812739966123,19.5488548387097));
#54266=CARTESIAN_POINT('Ctrl Pts',(-4.21857665773145,1.35764386397051,19.6016182795699));
#54267=CARTESIAN_POINT('Ctrl Pts',(-4.32479004603219,0.640761311051878,
19.628));
#54268=CARTESIAN_POINT('',(-0.803308159453264,4.29756675351946,19.628));
#54269=CARTESIAN_POINT('Origin',(0.,0.,19.628));
#54270=CARTESIAN_POINT('Ctrl Pts',(-4.37798451307649,0.00184115449647014,
18.848589891905));
#54271=CARTESIAN_POINT('Ctrl Pts',(-4.37034287302321,-1.32832166361097,
18.8972071273712));
#54272=CARTESIAN_POINT('Ctrl Pts',(-3.01402217294637,-4.11556359956004,
18.9986208963121));
#54273=CARTESIAN_POINT('Ctrl Pts',(1.72525842040716,-4.86940713488401,19.1528311987277));
#54274=CARTESIAN_POINT('Ctrl Pts',(5.02276837180745,-1.19521866677756,19.3112207991518));
#54275=CARTESIAN_POINT('Ctrl Pts',(3.95306672650205,2.75529758855723,19.4432121328385));
#54276=CARTESIAN_POINT('Ctrl Pts',(1.3947178009747,4.32991044428859,19.548805199788));
#54277=CARTESIAN_POINT('Ctrl Pts',(-0.0904913830656236,4.43080762341373,
19.6016017332627));
#54278=CARTESIAN_POINT('Ctrl Pts',(-0.803308159453631,4.29756675351939,
19.628));
#54279=CARTESIAN_POINT('Origin',(0.,0.,-1.84858989190501));
#54280=CARTESIAN_POINT('',(-4.36494952125445,-0.000302537669007011,17.651410108095));
#54281=CARTESIAN_POINT('',(-4.37193807291522,-0.0039501116577445,17.848589891905));
#54282=CARTESIAN_POINT('',(-4.372,-4.40683631492666E-13,-1.84858989190501));
#54283=CARTESIAN_POINT('Ctrl Pts',(-4.36494952125446,-0.000302537669007175,
17.651410108095));
#54284=CARTESIAN_POINT('Ctrl Pts',(-4.36539179118401,-0.709016948559791,
17.6771121150741));
#54285=CARTESIAN_POINT('Ctrl Pts',(-3.86807546336294,-2.87206193474975,
17.7555775629134));
#54286=CARTESIAN_POINT('Ctrl Pts',(-0.472995886023615,-5.14054336213398,
17.8868064516129));
#54287=CARTESIAN_POINT('Ctrl Pts',(4.05270272242283,-3.19751510246813,18.0450967741935));
#54288=CARTESIAN_POINT('Ctrl Pts',(4.88945318540557,1.65605334244537,18.2033870967742));
#54289=CARTESIAN_POINT('Ctrl Pts',(1.27529601904452,5.00227852023644,18.3616774193548));
#54290=CARTESIAN_POINT('Ctrl Pts',(-3.22941067771149,3.86313894204385,18.5110184231284));
#54291=CARTESIAN_POINT('Ctrl Pts',(-4.36429751701074,1.19782550299575,18.6075959860418));
#54292=CARTESIAN_POINT('Ctrl Pts',(-4.37485075966118,-0.00347109768167011,
18.651410108095));
#54293=CARTESIAN_POINT('Ctrl Pts',(-4.37193807291522,-0.00395011165774454,
17.848589891905));
#54294=CARTESIAN_POINT('Ctrl Pts',(-4.37503172333717,-0.34380114135277,
17.8609647263816));
#54295=CARTESIAN_POINT('Ctrl Pts',(-4.18383382909851,-2.13016311819971,
17.9261360943329));
#54296=CARTESIAN_POINT('Ctrl Pts',(-1.7333097832156,-4.86367572142824,18.0441039957589));
#54297=CARTESIAN_POINT('Ctrl Pts',(3.13645552043595,-4.10159948955856,18.202493596183));
#54298=CARTESIAN_POINT('Ctrl Pts',(5.14796384574126,0.398543369117654,18.3608831966071));
#54299=CARTESIAN_POINT('Ctrl Pts',(2.46797524199195,4.53507188733415,18.5192727970312));
#54300=CARTESIAN_POINT('Ctrl Pts',(-2.46096278237594,4.53951629179981,18.6776623974553));
#54301=CARTESIAN_POINT('Ctrl Pts',(-4.32286248336998,1.67443240118537,18.7874347624133));
#54302=CARTESIAN_POINT('Ctrl Pts',(-4.37864141367461,0.116186340178791,
18.8444105938965));
#54303=CARTESIAN_POINT('Ctrl Pts',(-4.37798451307649,0.00184115449647014,
18.848589891905));
#54304=CARTESIAN_POINT('Origin',(0.,0.,-1.84858989190501));
#54305=CARTESIAN_POINT('',(-4.37363367263438,0.00377358290378073,16.651410108095));
#54306=CARTESIAN_POINT('',(-4.36517770212695,0.0011188044825361,16.848589891905));
#54307=CARTESIAN_POINT('',(-4.372,-4.40683631492666E-13,-1.84858989190501));
#54308=CARTESIAN_POINT('Ctrl Pts',(-4.37363367263438,0.00377358290378063,
16.651410108095));
#54309=CARTESIAN_POINT('Ctrl Pts',(-4.36305794810196,-1.16100169057931,
16.6938648032461));
#54310=CARTESIAN_POINT('Ctrl Pts',(-3.28678615689719,-3.7906423093463,16.7890829392575));
#54311=CARTESIAN_POINT('Ctrl Pts',(1.14681571606612,-5.03325475486043,16.937064516129));
#54312=CARTESIAN_POINT('Ctrl Pts',(4.84536125415653,-1.78081574711759,17.0953548387097));
#54313=CARTESIAN_POINT('Ctrl Pts',(4.13332826509411,3.09264287390914,17.2536451612903));
#54314=CARTESIAN_POINT('Ctrl Pts',(-0.341147903092961,5.15096781506579,
17.411935483871));
#54315=CARTESIAN_POINT('Ctrl Pts',(-3.82897189620604,2.94763574423766,17.5445237994725));
#54316=CARTESIAN_POINT('Ctrl Pts',(-4.36448385884661,0.745897095166127,
17.6243486742139));
#54317=CARTESIAN_POINT('Ctrl Pts',(-4.36494952125446,-0.000302537669007175,
17.651410108095));
#54318=CARTESIAN_POINT('Ctrl Pts',(-4.36517770212695,0.0011188044825361,
16.848589891905));
#54319=CARTESIAN_POINT('Ctrl Pts',(-4.36334200546248,-0.796471401961387,
16.8775188588667));
#54320=CARTESIAN_POINT('Ctrl Pts',(-3.77287007871479,-3.05222639411641,
16.9592443593031));
#54321=CARTESIAN_POINT('Ctrl Pts',(-0.156460816144074,-5.16096436253732,
17.0937663932142));
#54322=CARTESIAN_POINT('Ctrl Pts',(4.24417435465306,-2.94058317628852,17.2521559936383));
#54323=CARTESIAN_POINT('Ctrl Pts',(4.7770306357801,1.95960002071087,17.4105455940624));
#54324=CARTESIAN_POINT('Ctrl Pts',(0.956505601666415,5.07396180892462,17.5689351944865));
#54325=CARTESIAN_POINT('Ctrl Pts',(-3.36909691713057,3.68230599805327,17.7149499604341));
#54326=CARTESIAN_POINT('Ctrl Pts',(-4.36183283826352,1.10615411256716,17.8081681929069));
#54327=CARTESIAN_POINT('Ctrl Pts',(-4.37193807291522,-0.00395011165774454,
17.848589891905));
#54328=CARTESIAN_POINT('Origin',(0.,0.,-1.84858989190501));
#54329=CARTESIAN_POINT('',(-4.37658335244799,-0.00285917843438755,15.651410108095));
#54330=CARTESIAN_POINT('',(-4.37598752684337,0.00314030101388529,15.848589891905));
#54331=CARTESIAN_POINT('',(-4.372,-4.40683631492666E-13,-1.84858989190501));
#54332=CARTESIAN_POINT('Ctrl Pts',(-4.37658335244799,-0.00285917843438723,
15.651410108095));
#54333=CARTESIAN_POINT('Ctrl Pts',(-4.37792255245523,-0.179344027897961,
15.657854050558));
#54334=CARTESIAN_POINT('Ctrl Pts',(-4.28827874574891,-1.79952736688815,
15.7170614338811));
#54335=CARTESIAN_POINT('Ctrl Pts',(-2.26751786562628,-4.63758557609733,
15.8290322580645));
#54336=CARTESIAN_POINT('Ctrl Pts',(2.65323118895075,-4.42822781393943,15.9873225806452));
#54337=CARTESIAN_POINT('Ctrl Pts',(5.15882697608013,-0.187992963311806,
16.1456129032258));
#54338=CARTESIAN_POINT('Ctrl Pts',(2.96850419640318,4.22336596918787,16.3039032258064));
#54339=CARTESIAN_POINT('Ctrl Pts',(-1.92395505269964,4.79032719267193,16.4621935483871));
#54340=CARTESIAN_POINT('Ctrl Pts',(-4.22261913325801,2.01425606870238,16.5780291758166));
#54341=CARTESIAN_POINT('Ctrl Pts',(-4.37620164431587,0.286601478848438,
16.6411013623859));
#54342=CARTESIAN_POINT('Ctrl Pts',(-4.37363367263438,0.00377358290378063,
16.651410108095));
#54343=CARTESIAN_POINT('Ctrl Pts',(-4.37598752684337,0.00314030101388495,
15.848589891905));
#54344=CARTESIAN_POINT('Ctrl Pts',(-4.36586808840044,-1.24298125471277,
15.8940729913518));
#54345=CARTESIAN_POINT('Ctrl Pts',(-3.15685416964687,-3.95275705920985,
15.9923526242733));
#54346=CARTESIAN_POINT('Ctrl Pts',(1.43550516966593,-4.9597746708902,16.1434287906695));
#54347=CARTESIAN_POINT('Ctrl Pts',(4.94197826197569,-1.49562391370258,16.3018183910937));
#54348=CARTESIAN_POINT('Ctrl Pts',(3.94475245484231,3.3315114408263,16.4602079915177));
#54349=CARTESIAN_POINT('Ctrl Pts',(-0.647385467154988,5.12259027405121,
16.6185975919419));
#54350=CARTESIAN_POINT('Ctrl Pts',(-3.91857823830144,2.77088302731469,16.7480582254043));
#54351=CARTESIAN_POINT('Ctrl Pts',(-4.36669222603978,0.659162948528226,
16.824722325392));
#54352=CARTESIAN_POINT('Ctrl Pts',(-4.36517770212695,0.0011188044825361,
16.848589891905));
#54353=CARTESIAN_POINT('Origin',(0.,0.,-1.84858989190501));
#54354=CARTESIAN_POINT('',(-4.36535254096326,-0.00139340307212889,14.651410108095));
#54355=CARTESIAN_POINT('',(-4.37450977369375,-0.00361009500681242,14.848589891905));
#54356=CARTESIAN_POINT('',(-4.372,-4.40683631492666E-13,-1.84858989190501));
#54357=CARTESIAN_POINT('Ctrl Pts',(-4.36535254096326,-0.00139340307212868,
14.651410108095));
#54358=CARTESIAN_POINT('Ctrl Pts',(-4.36719167669768,-0.640876180485729,
14.67460673873));
#54359=CARTESIAN_POINT('Ctrl Pts',(-3.93664196772952,-2.73257986740296,
14.7505668102252));
#54360=CARTESIAN_POINT('Ctrl Pts',(-0.715156117622299,-5.11247386069707,
14.8792903225806));
#54361=CARTESIAN_POINT('Ctrl Pts',(3.89726470591888,-3.38528655547465,15.0375806451613));
#54362=CARTESIAN_POINT('Ctrl Pts',(4.96212753934002,1.42342106576975,15.1958709677419));
#54363=CARTESIAN_POINT('Ctrl Pts',(1.5101211008729,4.93643307547415,15.3541612903226));
#54364=CARTESIAN_POINT('Ctrl Pts',(-3.1200112045152,3.99587919704142,15.5060076704403));
#54365=CARTESIAN_POINT('Ctrl Pts',(-4.36695709135924,1.26572596937806,15.6050906096977));
#54366=CARTESIAN_POINT('Ctrl Pts',(-4.37658335244799,-0.00285917843438723,
15.651410108095));
#54367=CARTESIAN_POINT('Ctrl Pts',(-4.37450977369375,-0.00361009500681263,
14.848589891905));
#54368=CARTESIAN_POINT('Ctrl Pts',(-4.37676192585348,-0.2570041121813,14.8578305903622));
#54369=CARTESIAN_POINT('Ctrl Pts',(-4.24160137044629,-1.95575914866763,
14.9198678222941));
#54370=CARTESIAN_POINT('Ctrl Pts',(-2.01745869282129,-4.75288338056742,
15.0347015877008));
#54371=CARTESIAN_POINT('Ctrl Pts',(2.88882981271105,-4.27956800578602,15.1930911881249));
#54372=CARTESIAN_POINT('Ctrl Pts',(5.16248437889336,0.0937818828261288,
15.351480788549));
#54373=CARTESIAN_POINT('Ctrl Pts',(2.73148949656154,4.38166693681219,15.5098703889731));
#54374=CARTESIAN_POINT('Ctrl Pts',(-2.18875273549729,4.67647318514471,15.6682599893972));
#54375=CARTESIAN_POINT('Ctrl Pts',(-4.27423782525496,1.84868256384714,15.7811664903745));
#54376=CARTESIAN_POINT('Ctrl Pts',(-4.37761467728721,0.203509842654685,
15.8412764578771));
#54377=CARTESIAN_POINT('Ctrl Pts',(-4.37598752684337,0.00314030101388495,
15.848589891905));
#54378=CARTESIAN_POINT('Origin',(0.,0.,-1.84858989190501));
#54379=CARTESIAN_POINT('',(-4.3715702955649,0.00393516289142377,13.651410108095));
#54380=CARTESIAN_POINT('',(-4.36492411635568,-0.000270170186619789,13.848589891905));
#54381=CARTESIAN_POINT('',(-4.372,-4.40683631492666E-13,-1.84858989190501));
#54382=CARTESIAN_POINT('Ctrl Pts',(-4.3715702955649,0.00393516289142415,
13.651410108095));
#54383=CARTESIAN_POINT('Ctrl Pts',(-4.36167155640512,-1.09343140876319,
13.691359426902));
#54384=CARTESIAN_POINT('Ctrl Pts',(-3.38808352462445,-3.65581253168041,
13.7840721865693));
#54385=CARTESIAN_POINT('Ctrl Pts',(0.907928552289056,-5.08178147829179,
13.9295483870968));
#54386=CARTESIAN_POINT('Ctrl Pts',(4.75589152831045,-2.00756893285326,14.0878387096774));
#54387=CARTESIAN_POINT('Ctrl Pts',(4.2747154125816,2.89407073006048,14.2461290322581));
#54388=CARTESIAN_POINT('Ctrl Pts',(-0.0976002483683332,5.16132845696157,
14.4044193548387));
#54389=CARTESIAN_POINT('Ctrl Pts',(-3.75335254656528,3.08663197095523,14.5395130467844));
#54390=CARTESIAN_POINT('Ctrl Pts',(-4.36300834804604,0.813701953645304,
14.6218432978698));
#54391=CARTESIAN_POINT('Ctrl Pts',(-4.36535254096326,-0.00139340307212868,
14.651410108095));
#54392=CARTESIAN_POINT('Ctrl Pts',(-4.36492411635568,-0.000270170186619789,
13.848589891905));
#54393=CARTESIAN_POINT('Ctrl Pts',(-4.36531805977148,-0.711553376731479,
13.8743847228474));
#54394=CARTESIAN_POINT('Ctrl Pts',(-3.86529136737144,-2.8781600308068,13.9529760872644));
#54395=CARTESIAN_POINT('Ctrl Pts',(-0.460905372910369,-5.14272362102755,
14.0843639851561));
#54396=CARTESIAN_POINT('Ctrl Pts',(4.06315051784514,-3.18603952805496,14.2427535855802));
#54397=CARTESIAN_POINT('Ctrl Pts',(4.88439639669049,1.67413017563193,14.4011431860043));
#54398=CARTESIAN_POINT('Ctrl Pts',(1.25441857601452,5.00863993928383,14.5595327864284));
#54399=CARTESIAN_POINT('Ctrl Pts',(-3.24025672884045,3.85045757200017,14.7086816883953));
#54400=CARTESIAN_POINT('Ctrl Pts',(-4.36389430254103,1.19075719850307,14.8050340568875));
#54401=CARTESIAN_POINT('Ctrl Pts',(-4.37450977369375,-0.00361009500681263,
14.848589891905));
#54402=CARTESIAN_POINT('Origin',(0.,0.,-1.84858989190501));
#54403=CARTESIAN_POINT('',(-4.37805463091546,-0.00189096989131645,12.651410108095));
#54404=CARTESIAN_POINT('',(-4.3735298381194,0.00380331467108683,12.848589891905));
#54405=CARTESIAN_POINT('',(-4.372,-4.40683631492666E-13,-1.84858989190501));
#54406=CARTESIAN_POINT('Ctrl Pts',(-4.37805463091546,-0.00189096989131629,
12.651410108095));
#54407=CARTESIAN_POINT('Ctrl Pts',(-4.37864191593093,-0.109663799931991,
12.6553486742139));
#54408=CARTESIAN_POINT('Ctrl Pts',(-4.32628239365674,-1.66064736718339,
12.7120506811929));
#54409=CARTESIAN_POINT('Ctrl Pts',(-2.4839194519693,-4.5253708583176,12.8215161290323));
#54410=CARTESIAN_POINT('Ctrl Pts',(2.44122672465452,-4.54854364912704,12.9798064516129));
#54411=CARTESIAN_POINT('Ctrl Pts',(5.14420067918421,-0.431319627959304,
13.1380967741936));
#54412=CARTESIAN_POINT('Ctrl Pts',(3.16456988475122,4.07852114052473,13.2963870967742));
#54413=CARTESIAN_POINT('Ctrl Pts',(-1.69566975348524,4.87581186432528,13.4546774193548));
#54414=CARTESIAN_POINT('Ctrl Pts',(-4.17531922896613,2.15372155886245,13.5730184231284));
#54415=CARTESIAN_POINT('Ctrl Pts',(-4.37474540982351,0.355925875277971,
13.6385959860418));
#54416=CARTESIAN_POINT('Ctrl Pts',(-4.3715702955649,0.00393516289142415,
13.651410108095));
#54417=CARTESIAN_POINT('Ctrl Pts',(-4.3735298381194,0.00380331467108686,
12.848589891905));
#54418=CARTESIAN_POINT('Ctrl Pts',(-4.36293974589787,-1.15814174670351,
12.8909388553325));
#54419=CARTESIAN_POINT('Ctrl Pts',(-3.29085772231164,-3.78595162322649,
12.9860843522346));
#54420=CARTESIAN_POINT('Ctrl Pts',(1.14016230868481,-5.03587826648703,13.1340263826114));
#54421=CARTESIAN_POINT('Ctrl Pts',(4.84505108113381,-1.78480251743019,13.2924159830355));
#54422=CARTESIAN_POINT('Ctrl Pts',(4.13457213027864,3.09279053680373,13.4508055834596));
#54423=CARTESIAN_POINT('Ctrl Pts',(-0.343804419177731,5.15187718471428,
13.6091951838838));
#54424=CARTESIAN_POINT('Ctrl Pts',(-3.8305579098897,2.94525464061577,13.7417899533655));
#54425=CARTESIAN_POINT('Ctrl Pts',(-4.36451174137436,0.744292087358565,
13.8215881893726));
#54426=CARTESIAN_POINT('Ctrl Pts',(-4.36492411635568,-0.000270170186619789,
13.848589891905));
#54427=CARTESIAN_POINT('Origin',(0.,0.,-1.84858989190501));
#54428=CARTESIAN_POINT('',(-4.3662580307389,-0.00237411499775451,11.651410108095));
#54429=CARTESIAN_POINT('',(-4.37682453544783,-0.00275176080394124,11.848589891905));
#54430=CARTESIAN_POINT('',(-4.372,-4.40683631492666E-13,-1.84858989190501));
#54431=CARTESIAN_POINT('Ctrl Pts',(-4.3662580307389,-0.00237411499775443,
11.651410108095));
#54432=CARTESIAN_POINT('Ctrl Pts',(-4.36908770984708,-0.57249276395778,
11.6721013623859));
#54433=CARTESIAN_POINT('Ctrl Pts',(-4.00080778508103,-2.59292231754593,
11.745556057537));
#54434=CARTESIAN_POINT('Ctrl Pts',(-0.955706815437237,-5.07301308219371,
11.8717741935484));
#54435=CARTESIAN_POINT('Ctrl Pts',(3.73310810644377,-3.5654931096253,12.030064516129));
#54436=CARTESIAN_POINT('Ctrl Pts',(5.02379164936073,1.1875835604264,12.1883548387097));
#54437=CARTESIAN_POINT('Ctrl Pts',(1.74147501164997,4.85964011352491,12.3466451612903));
#54438=CARTESIAN_POINT('Ctrl Pts',(-3.00493840101716,4.12681778354368,12.5009969177521));
#54439=CARTESIAN_POINT('Ctrl Pts',(-4.3707742866348,1.33412695349428,12.6025852333536));
#54440=CARTESIAN_POINT('Ctrl Pts',(-4.37805463091546,-0.00189096989131629,
12.651410108095));
#54441=CARTESIAN_POINT('Ctrl Pts',(-4.37682453544783,-0.0027517608039412,
11.848589891905));
#54442=CARTESIAN_POINT('Ctrl Pts',(-4.37805680950565,-0.169972374992373,
11.8546964543429));
#54443=CARTESIAN_POINT('Ctrl Pts',(-4.29358524369388,-1.7817038588778,11.9135995502554));
#54444=CARTESIAN_POINT('Ctrl Pts',(-2.29456228398659,-4.62547553554524,
12.0252991796426));
#54445=CARTESIAN_POINT('Ctrl Pts',(2.63111281568934,-4.44266646915302,12.1836887800668));
#54446=CARTESIAN_POINT('Ctrl Pts',(5.15901534120123,-0.211188811899807,
12.3420783804909));
#54447=CARTESIAN_POINT('Ctrl Pts',(2.98542980392062,4.2127483773522,12.500467980915));
#54448=CARTESIAN_POINT('Ctrl Pts',(-1.90882269345658,4.79754478144462,12.6588575813391));
#54449=CARTESIAN_POINT('Ctrl Pts',(-4.22005393336117,2.0228792487521,12.7748982183358));
#54450=CARTESIAN_POINT('Ctrl Pts',(-4.37614243406833,0.290457377422949,
12.8381423218578));
#54451=CARTESIAN_POINT('Ctrl Pts',(-4.3735298381194,0.00380331467108686,
12.848589891905));
#54452=CARTESIAN_POINT('Origin',(0.,0.,-1.84858989190501));
#54453=CARTESIAN_POINT('',(-4.36958950328423,0.00375500997191766,10.651410108095));
#54454=CARTESIAN_POINT('',(-4.36549183168559,-0.00162636191587406,10.848589891905));
#54455=CARTESIAN_POINT('',(-4.372,-4.40683631492666E-13,-1.84858989190501));
#54456=CARTESIAN_POINT('Ctrl Pts',(-4.36958950328423,0.00375500997191747,
10.651410108095));
#54457=CARTESIAN_POINT('Ctrl Pts',(-4.36106090852754,-1.0259785981898,10.688854050558));
#54458=CARTESIAN_POINT('Ctrl Pts',(-3.48414488794968,-3.51981628552574,
10.7790614338811));
#54459=CARTESIAN_POINT('Ctrl Pts',(0.667017186951725,-5.11897697997292,
10.9220322580645));
#54460=CARTESIAN_POINT('Ctrl Pts',(4.65581649466175,-2.22984528997355,11.0803225806452));
#54461=CARTESIAN_POINT('Ctrl Pts',(4.40657187915952,2.68904472312794,11.2386129032258));
#54462=CARTESIAN_POINT('Ctrl Pts',(0.14616290696869,5.16018155240764,11.3969032258064));
#54463=CARTESIAN_POINT('Ctrl Pts',(-3.67299362448513,3.22514497791193,11.5345022940962));
#54464=CARTESIAN_POINT('Ctrl Pts',(-4.36187192659012,0.881330247193059,
11.6193379215257));
#54465=CARTESIAN_POINT('Ctrl Pts',(-4.3662580307389,-0.00237411499775443,
11.651410108095));
#54466=CARTESIAN_POINT('Ctrl Pts',(-4.36549183168559,-0.00162636191587386,
10.848589891905));
#54467=CARTESIAN_POINT('Ctrl Pts',(-4.36759069612872,-0.626283874484138,
10.871250586828));
#54468=CARTESIAN_POINT('Ctrl Pts',(-3.95060522485931,-2.70364125089475,
10.9467078152256));
#54469=CARTESIAN_POINT('Ctrl Pts',(-0.763741663751577,-5.10653881568242,
11.074961577098));
#54470=CARTESIAN_POINT('Ctrl Pts',(3.86794975738412,-3.42038077988013,11.2333511775221));
#54471=CARTESIAN_POINT('Ctrl Pts',(4.97472054752429,1.38282156443299,11.3917407779462));
#54472=CARTESIAN_POINT('Ctrl Pts',(1.54795388466898,4.92583787552529,11.5501303783703));
#54473=CARTESIAN_POINT('Ctrl Pts',(-3.10298340129681,4.01633537157594,11.7024134163566));
#54474=CARTESIAN_POINT('Ctrl Pts',(-4.36740273051995,1.27579500142313,11.8018999208682));
#54475=CARTESIAN_POINT('Ctrl Pts',(-4.37682453544783,-0.0027517608039412,
11.848589891905));
#54476=CARTESIAN_POINT('Origin',(0.,0.,-1.84858989190501));
#54477=CARTESIAN_POINT('',(-4.37893064514985,-0.000718125850480163,9.65141010809499));
#54478=CARTESIAN_POINT('',(-4.37095165486262,0.00392878392899476,9.84858989190502));
#54479=CARTESIAN_POINT('',(-4.372,-4.40683631492666E-13,-1.84858989190501));
#54480=CARTESIAN_POINT('Ctrl Pts',(-4.37893064514985,-0.000718125850479884,
9.65141010809498));
#54481=CARTESIAN_POINT('Ctrl Pts',(-4.37902043646228,-0.0399142522790172,
9.65284329786977));
#54482=CARTESIAN_POINT('Ctrl Pts',(-4.36082969860212,-1.52204564057694,
9.70703992850478));
#54483=CARTESIAN_POINT('Ctrl Pts',(-2.69478237803987,-4.40306543037773,
9.81399999999999));
#54484=CARTESIAN_POINT('Ctrl Pts',(2.22377879965116,-4.65871710875468,9.97229032258064));
#54485=CARTESIAN_POINT('Ctrl Pts',(5.11810379036282,-0.67368452576514,10.1305806451613));
#54486=CARTESIAN_POINT('Ctrl Pts',(3.35357921258595,3.92458197953528,10.2888709677419));
#54487=CARTESIAN_POINT('Ctrl Pts',(-1.46360347987537,4.95042443663959,10.4471612903226));
#54488=CARTESIAN_POINT('Ctrl Pts',(-4.12415016732119,2.29334108429437,10.5680076704403));
#54489=CARTESIAN_POINT('Ctrl Pts',(-4.37307882051719,0.425051522096353,
10.6360906096977));
#54490=CARTESIAN_POINT('Ctrl Pts',(-4.36958950328423,0.00375500997191747,
10.651410108095));
#54491=CARTESIAN_POINT('Ctrl Pts',(-4.37095165486262,0.00392878392899445,
9.84858989190502));
#54492=CARTESIAN_POINT('Ctrl Pts',(-4.36138099894435,-1.0736503956833,9.88780471931308));
#54493=CARTESIAN_POINT('Ctrl Pts',(-3.41650604254828,-3.61702144425598,
9.97981608019584));
#54494=CARTESIAN_POINT('Ctrl Pts',(0.840841326532404,-5.09441123866306,
10.1246239745533));
#54495=CARTESIAN_POINT('Ctrl Pts',(4.73121909778617,-2.06775381846214,10.2830135749774));
#54496=CARTESIAN_POINT('Ctrl Pts',(4.30996593957687,2.84327867165857,10.4414031754015));
#54497=CARTESIAN_POINT('Ctrl Pts',(-0.0390238264566685,5.16318866070086,
10.5997927758256));
#54498=CARTESIAN_POINT('Ctrl Pts',(-3.7353314916358,3.11908229388608,10.7355216813268));
#54499=CARTESIAN_POINT('Ctrl Pts',(-4.36270060925329,0.829088583628261,
10.8184540533533));
#54500=CARTESIAN_POINT('Ctrl Pts',(-4.36549183168559,-0.00162636191587386,
10.848589891905));
#54501=CARTESIAN_POINT('Origin',(0.,0.,-1.84858989190501));
#54502=CARTESIAN_POINT('',(-4.3676089549007,-0.00316636266463396,8.65141010809498));
#54503=CARTESIAN_POINT('',(-4.3784939599728,-0.00146115515596901,8.84858989190502));
#54504=CARTESIAN_POINT('',(-4.372,-4.40683631492666E-13,-1.84858989190501));
#54505=CARTESIAN_POINT('Ctrl Pts',(-4.3676089549007,-0.0031663626646336,
8.65141010809498));
#54506=CARTESIAN_POINT('Ctrl Pts',(-4.37099157996906,-0.503863509155134,
8.66959598604181));
#54507=CARTESIAN_POINT('Ctrl Pts',(-4.0607005189635,-2.45318988687306,8.74054530484886));
#54508=CARTESIAN_POINT('Ctrl Pts',(-1.19412647058753,-5.02224045834365,
8.86425806451613));
#54509=CARTESIAN_POINT('Ctrl Pts',(3.56062739266322,-3.73774929868204,9.02254838709676));
#54510=CARTESIAN_POINT('Ctrl Pts',(5.07425366817473,0.949097971864315,9.18083870967742));
#54511=CARTESIAN_POINT('Ctrl Pts',(1.96894576792944,4.77201108675727,9.33912903225805));
#54512=CARTESIAN_POINT('Ctrl Pts',(-2.88428822201713,4.2558282973375,9.49598616506391));
#54513=CARTESIAN_POINT('Ctrl Pts',(-4.37571473425415,1.40310643844898,9.60007985700956));
#54514=CARTESIAN_POINT('Ctrl Pts',(-4.37893064514985,-0.000718125850479884,
9.65141010809498));
#54515=CARTESIAN_POINT('Ctrl Pts',(-4.3784939599728,-0.00146115515596968,
8.84858989190502));
#54516=CARTESIAN_POINT('Ctrl Pts',(-4.37884870232368,-0.0827753827151446,
8.85156231832348));
#54517=CARTESIAN_POINT('Ctrl Pts',(-4.34001073551865,-1.6080554399903,8.90733127821665));
#54518=CARTESIAN_POINT('Ctrl Pts',(-2.56365995117077,-4.48192901101572,
9.01589677158451));
#54519=CARTESIAN_POINT('Ctrl Pts',(2.36421564112952,-4.59026408905411,9.17428637200862));
#54520=CARTESIAN_POINT('Ctrl Pts',(5.13754605775107,-0.515422651333577,
9.33267597243274));
#54521=CARTESIAN_POINT('Ctrl Pts',(3.22895369161553,4.02913117959985,9.49106557285684));
#54522=CARTESIAN_POINT('Ctrl Pts',(-1.62223260619563,4.90187733184103,9.64945517328097));
#54523=CARTESIAN_POINT('Ctrl Pts',(-4.15999532952882,2.19738929405191,9.76862994629701));
#54524=CARTESIAN_POINT('Ctrl Pts',(-4.37426636626487,0.377138731501872,
9.83500818583837));
#54525=CARTESIAN_POINT('Ctrl Pts',(-4.37095165486262,0.00392878392899445,
9.84858989190502));
#54526=CARTESIAN_POINT('Origin',(0.,0.,-1.84858989190501));
#54527=CARTESIAN_POINT('',(-4.36783565389082,0.00326080189849165,7.65141010809498));
#54528=CARTESIAN_POINT('',(-4.36682740614764,-0.00278338701585445,7.84858989190503));
#54529=CARTESIAN_POINT('',(-4.372,-4.40683631492666E-13,-1.84858989190501));
#54530=CARTESIAN_POINT('Ctrl Pts',(-4.36783565389082,0.0032608018984915,
7.65141010809498));
#54531=CARTESIAN_POINT('Ctrl Pts',(-4.36111999858997,-0.958548857288375,
7.68634867421386));
#54532=CARTESIAN_POINT('Ctrl Pts',(-3.57508309710888,-3.38283964502905,
7.77405068119295));
#54533=CARTESIAN_POINT('Ctrl Pts',(0.424618501333285,-5.14475814567673,
7.91451612903225));
#54534=CARTESIAN_POINT('Ctrl Pts',(4.54535988400859,-2.44714952016159,8.0728064516129));
#54535=CARTESIAN_POINT('Ctrl Pts',(4.52860253637045,2.47802266268103,8.23109677419354));
#54536=CARTESIAN_POINT('Ctrl Pts',(0.389600147091602,5.14752843358518,8.38938709677419));
#54537=CARTESIAN_POINT('Ctrl Pts',(-3.58777114537366,3.36303202741965,8.52949154140801));
#54538=CARTESIAN_POINT('Ctrl Pts',(-4.36117742976588,0.948829858465871,
8.6168325451816));
#54539=CARTESIAN_POINT('Ctrl Pts',(-4.3676089549007,-0.0031663626646336,
8.65141010809498));
#54540=CARTESIAN_POINT('Ctrl Pts',(-4.36682740614764,-0.00278338701585466,
7.84858989190503));
#54541=CARTESIAN_POINT('Ctrl Pts',(-4.36998031573444,-0.540633837652302,
7.8681164508086));
#54542=CARTESIAN_POINT('Ctrl Pts',(-4.02906901036793,-2.52888541639766,
7.94043954318687));
#54543=CARTESIAN_POINT('Ctrl Pts',(-1.06391319462353,-5.05253685976928,
8.06555916903983));
#54544=CARTESIAN_POINT('Ctrl Pts',(3.65925338948522,-3.64278803069328,8.22394876946396));
#54545=CARTESIAN_POINT('Ctrl Pts',(5.04768747299395,1.08668817054443,8.38233836988805));
#54546=CARTESIAN_POINT('Ctrl Pts',(1.83608824986349,4.82584914224785,8.54072797031219));
#54547=CARTESIAN_POINT('Ctrl Pts',(-2.95709387717496,4.17950307750852,8.69614514431782));
#54548=CARTESIAN_POINT('Ctrl Pts',(-4.37254773342937,1.36153600902825,8.79876578484878));
#54549=CARTESIAN_POINT('Ctrl Pts',(-4.3784939599728,-0.00146115515596968,
8.84858989190502));
#54550=CARTESIAN_POINT('Origin',(0.,0.,-1.84858989190501));
#54551=CARTESIAN_POINT('',(-4.37899478532443,0.000538853135781114,6.65141010809498));
#54552=CARTESIAN_POINT('',(-4.36857373794226,0.00352936749739713,6.84858989190502));
#54553=CARTESIAN_POINT('',(-4.372,-4.40683631492666E-13,-1.84858989190501));
#54554=CARTESIAN_POINT('Ctrl Pts',(-4.37899478532443,0.00053885313578114,
6.65141010809498));
#54555=CARTESIAN_POINT('Ctrl Pts',(-4.37652423695377,-1.41310306479934,
6.7031013623859));
#54556=CARTESIAN_POINT('Ctrl Pts',(-2.86643925520047,-4.27424452468468,
6.80755605753705));
#54557=CARTESIAN_POINT('Ctrl Pts',(2.00137227482285,-4.75850252356265,6.96477419354837));
#54558=CARTESIAN_POINT('Ctrl Pts',(5.08059451261016,-0.914547236405604,
7.12306451612904));
#54559=CARTESIAN_POINT('Ctrl Pts',(3.53511070256229,3.76189175413264,7.28135483870967));
#54560=CARTESIAN_POINT('Ctrl Pts',(-1.22827365147281,5.01399851279189,7.43964516129032));
#54561=CARTESIAN_POINT('Ctrl Pts',(-4.06898604612617,2.43305468214084,7.56299691775209));
#54562=CARTESIAN_POINT('Ctrl Pts',(-4.37126183097366,0.493954571118568,
7.63358523335364));
#54563=CARTESIAN_POINT('Ctrl Pts',(-4.36783565389082,0.0032608018984915,
7.65141010809498));
#54564=CARTESIAN_POINT('Ctrl Pts',(-4.36857373794226,0.00352936749739713,
6.84858989190502));
#54565=CARTESIAN_POINT('Ctrl Pts',(-4.3609877808655,-0.989297031049394,
6.8846705832937));
#54566=CARTESIAN_POINT('Ctrl Pts',(-3.53400975081915,-3.4463519724339,6.97354780815709));
#54567=CARTESIAN_POINT('Ctrl Pts',(0.538586577094185,-5.13516937442138,
7.11522156649516));
#54568=CARTESIAN_POINT('Ctrl Pts',(4.60087948645563,-2.34349054961462,7.27361116691928));
#54569=CARTESIAN_POINT('Ctrl Pts',(4.47032190918109,2.58384636410851,7.43200076734339));
#54570=CARTESIAN_POINT('Ctrl Pts',(0.26589292373178,5.15648532996368,7.59039036776751));
#54571=CARTESIAN_POINT('Ctrl Pts',(-3.63264590427038,3.29210602756316,7.72925340928804));
#54572=CARTESIAN_POINT('Ctrl Pts',(-4.3614553781167,0.913623385120531,7.81531991733389));
#54573=CARTESIAN_POINT('Ctrl Pts',(-4.36682740614764,-0.00278338701585466,
7.84858989190503));
#54574=CARTESIAN_POINT('Origin',(0.,0.,-1.84858989190501));
#54575=CARTESIAN_POINT('',(-4.36931971855082,-0.00370222284602327,5.65141010809498));
#54576=CARTESIAN_POINT('',(-4.37909655387308,8.17972643269707E-5,5.84858989190502));
#54577=CARTESIAN_POINT('',(-4.372,-4.40683631492666E-13,-1.84858989190501));
#54578=CARTESIAN_POINT('Ctrl Pts',(-4.36931971855082,-0.00370222284602335,
5.65141010809498));
#54579=CARTESIAN_POINT('Ctrl Pts',(-4.37282475456675,-0.434994053437505,
5.66709060969773));
#54580=CARTESIAN_POINT('Ctrl Pts',(-4.11645084466375,-2.3134683703663,5.73553455216068));
#54581=CARTESIAN_POINT('Ctrl Pts',(-1.42988345294528,-4.96026920238937,
5.85674193548387));
#54582=CARTESIAN_POINT('Ctrl Pts',(3.38020716333018,-3.90167102433782,6.01503225806451));
#54583=CARTESIAN_POINT('Ctrl Pts',(5.11340107541181,0.708496077023162,6.17332258064516));
#54584=CARTESIAN_POINT('Ctrl Pts',(2.19202615312461,4.67374139134797,6.3316129032258));
#54585=CARTESIAN_POINT('Ctrl Pts',(-2.72468151658193,4.38462631046011,6.48990322580645));
#54586=CARTESIAN_POINT('Ctrl Pts',(-4.36552898201431,1.50209810391025,6.59650229409617));
#54587=CARTESIAN_POINT('Ctrl Pts',(-4.37904602975287,0.0298607935490157,
6.65033792152568));
#54588=CARTESIAN_POINT('Ctrl Pts',(-4.37899478532443,0.00053885313578114,
6.65141010809498));
#54589=CARTESIAN_POINT('Ctrl Pts',(-4.37909655387308,8.17972643267733E-5,
5.84858989190502));
#54590=CARTESIAN_POINT('Ctrl Pts',(-4.37869792746944,-1.43927515570558,
5.90122471577881));
#54591=CARTESIAN_POINT('Ctrl Pts',(-2.8187969284654,-4.3231521197151,6.0066560731273));
#54592=CARTESIAN_POINT('Ctrl Pts',(2.08906951604171,-4.72184588505036,6.16488396395049));
#54593=CARTESIAN_POINT('Ctrl Pts',(5.098151436811,-0.817858137064712,6.32327356437462));
#54594=CARTESIAN_POINT('Ctrl Pts',(3.46121148378334,3.83145599864432,6.48166316479871));
#54595=CARTESIAN_POINT('Ctrl Pts',(-1.32998241066,4.98910681308353,6.64005276522284));
#54596=CARTESIAN_POINT('Ctrl Pts',(-4.09382090065572,2.37211345116906,6.76236167425826));
#54597=CARTESIAN_POINT('Ctrl Pts',(-4.37208823990123,0.463496420738366,
6.831874049819));
#54598=CARTESIAN_POINT('Ctrl Pts',(-4.36857373794226,0.00352936749739713,
6.84858989190502));
#54599=CARTESIAN_POINT('Origin',(0.,0.,-1.84858989190501));
#54600=CARTESIAN_POINT('',(-4.36642690985212,0.00250163610255838,4.65141010809498));
#54601=CARTESIAN_POINT('',(-4.36880169481863,-0.00359316639133633,4.84858989190502));
#54602=CARTESIAN_POINT('',(-4.372,-4.40683631492666E-13,-1.84858989190501));
#54603=CARTESIAN_POINT('Ctrl Pts',(-4.36642690985212,0.00250163610255878,
4.65141010809498));
#54604=CARTESIAN_POINT('Ctrl Pts',(-4.36174213540044,-0.891062986338486,
4.68384329786977));
#54605=CARTESIAN_POINT('Ctrl Pts',(-3.66101665548786,-3.24505548151499,
4.76903992850477));
#54606=CARTESIAN_POINT('Ctrl Pts',(0.181272997936893,-5.15906748833169,
4.907));
#54607=CARTESIAN_POINT('Ctrl Pts',(4.4247679934035,-2.65899707670991,5.06529032258064));
#54608=CARTESIAN_POINT('Ctrl Pts',(4.64053527927078,2.26147508740778,5.22358064516129));
#54609=CARTESIAN_POINT('Ctrl Pts',(0.63216865368283,5.12339731452249,5.38187096774192));
#54610=CARTESIAN_POINT('Ctrl Pts',(-3.49756148837773,3.50013537491244,5.52448078871984));
#54611=CARTESIAN_POINT('Ctrl Pts',(-4.361030631826,1.01626315589314,5.61432716883751));
#54612=CARTESIAN_POINT('Ctrl Pts',(-4.36931971855082,-0.00370222284602335,
5.65141010809498));
#54613=CARTESIAN_POINT('Ctrl Pts',(-4.36880169481863,-0.00359316639133644,
4.84858989190502));
#54614=CARTESIAN_POINT('Ctrl Pts',(-4.37232350022417,-0.454601269873613,
4.86498231478922));
#54615=CARTESIAN_POINT('Ctrl Pts',(-4.10093982798236,-2.35407682434418,
4.93417127114812));
#54616=CARTESIAN_POINT('Ctrl Pts',(-1.36037264139205,-4.98090617072295,
5.05615676098171));
#54617=CARTESIAN_POINT('Ctrl Pts',(3.43778957362211,-3.85248528258675,5.21454636140584));
#54618=CARTESIAN_POINT('Ctrl Pts',(5.10304258525828,0.786763228710822,5.37293596182993));
#54619=CARTESIAN_POINT('Ctrl Pts',(2.11781634615703,4.70902260867037,5.53132556225406));
#54620=CARTESIAN_POINT('Ctrl Pts',(-2.79740769526454,4.33987905263503,5.68971516267816));
#54621=CARTESIAN_POINT('Ctrl Pts',(-4.37709282415761,1.45270398568835,5.79546993922849));
#54622=CARTESIAN_POINT('Ctrl Pts',(-4.37909777857019,0.00450392355468565,
5.84842818230411));
#54623=CARTESIAN_POINT('Ctrl Pts',(-4.37909655387308,8.17972643267733E-5,
5.84858989190502));
#54624=CARTESIAN_POINT('Origin',(0.,0.,-1.84858989190501));
#54625=CARTESIAN_POINT('',(-4.37822270954365,0.00173219555018226,3.65141010809498));
#54626=CARTESIAN_POINT('',(-4.36665723562798,0.00267775706545931,3.84858989190502));
#54627=CARTESIAN_POINT('',(-4.372,-4.40683631492666E-13,-1.84858989190501));
#54628=CARTESIAN_POINT('Ctrl Pts',(-4.37822270954365,0.00173219555018251,
3.65141010809498));
#54629=CARTESIAN_POINT('Ctrl Pts',(-4.37141484073147,-1.3440268941613,3.70059598604181));
#54630=CARTESIAN_POINT('Ctrl Pts',(-2.98789956101879,-4.1455315666631,3.80254530484886));
#54631=CARTESIAN_POINT('Ctrl Pts',(1.77450307237079,-4.84767739015689,3.95725806451612));
#54632=CARTESIAN_POINT('Ctrl Pts',(5.03175648528012,-1.15337068283656,4.11554838709677));
#54633=CARTESIAN_POINT('Ctrl Pts',(3.7087595738537,3.5908132325819,4.27383870967742));
#54634=CARTESIAN_POINT('Ctrl Pts',(-0.990205008382098,5.06639233464293,
4.43212903225806));
#54635=CARTESIAN_POINT('Ctrl Pts',(-4.00969822487022,2.57279053906618,4.55798616506392));
#54636=CARTESIAN_POINT('Ctrl Pts',(-4.36936348937275,0.562619011588028,
4.63107985700956));
#54637=CARTESIAN_POINT('Ctrl Pts',(-4.36642690985212,0.00250163610255878,
4.65141010809498));
#54638=CARTESIAN_POINT('Ctrl Pts',(-4.36665723562798,0.00267775706545938,
3.84858989190502));
#54639=CARTESIAN_POINT('Ctrl Pts',(-4.36155175532508,-0.904909371632279,
3.88153644727432));
#54640=CARTESIAN_POINT('Ctrl Pts',(-3.64359471136329,-3.27429676880991,
3.96727953611833));
#54641=CARTESIAN_POINT('Ctrl Pts',(0.234452652827207,-5.15801046495039,
4.10581915843705));
#54642=CARTESIAN_POINT('Ctrl Pts',(4.4544870133001,-2.61105064195526,4.26420875886115));
#54643=CARTESIAN_POINT('Ctrl Pts',(4.61508054334482,2.31539879571022,4.42259835928526));
#54644=CARTESIAN_POINT('Ctrl Pts',(0.56988195080356,5.13179058096912,4.58098795970938));
#54645=CARTESIAN_POINT('Ctrl Pts',(-3.52225462180705,3.46403365178023,4.72298513724929));
#54646=CARTESIAN_POINT('Ctrl Pts',(-4.36098050850789,0.998000618272236,
4.81218578131451));
#54647=CARTESIAN_POINT('Ctrl Pts',(-4.36880169481863,-0.00359316639133644,
4.84858989190502));
#54648=CARTESIAN_POINT('Origin',(0.,0.,-1.84858989190501));
#54649=CARTESIAN_POINT('',(-4.3712761175009,-0.0039298912494793,2.65141010809498));
#54650=CARTESIAN_POINT('',(-4.37836367713493,0.00160984593324705,2.84858989190502));
#54651=CARTESIAN_POINT('',(-4.372,-4.40683631492666E-13,-1.84858989190501));
#54652=CARTESIAN_POINT('Ctrl Pts',(-4.3712761175009,-0.00392989124947909,
2.65141010809498));
#54653=CARTESIAN_POINT('Ctrl Pts',(-4.37451696257115,-0.365899162664298,
2.66458523335364));
#54654=CARTESIAN_POINT('Ctrl Pts',(-4.16818790357475,-2.17383119834201,
2.73052379947252));
#54655=CARTESIAN_POINT('Ctrl Pts',(-1.66245191543707,-4.88723759858308,
2.84922580645161));
#54656=CARTESIAN_POINT('Ctrl Pts',(3.19224964022283,-4.05689272016998,3.00751612903226));
#54657=CARTESIAN_POINT('Ctrl Pts',(5.14114662208426,0.466314344506177,3.1658064516129));
#54658=CARTESIAN_POINT('Ctrl Pts',(2.41021871871718,4.56505016420442,3.32409677419355));
#54659=CARTESIAN_POINT('Ctrl Pts',(-2.5146557123555,4.50836375769575,3.48238709677419));
#54660=CARTESIAN_POINT('Ctrl Pts',(-4.33147098232467,1.64065849811777,3.591491541408));
#54661=CARTESIAN_POINT('Ctrl Pts',(-4.37871788376841,0.0996167512533684,
3.6478325451816));
#54662=CARTESIAN_POINT('Ctrl Pts',(-4.37822270954365,0.00173219555018251,
3.65141010809498));
#54663=CARTESIAN_POINT('Ctrl Pts',(-4.37836367713493,0.00160984593324717,
2.84858989190502));
#54664=CARTESIAN_POINT('Ctrl Pts',(-4.37193582834707,-1.35264708506912,
2.89809057975943));
#54665=CARTESIAN_POINT('Ctrl Pts',(-2.9725521843832,-4.16280399703585,3.00038780108855));
#54666=CARTESIAN_POINT('Ctrl Pts',(1.80663443860224,-4.83695274769126,3.15548155589238));
#54667=CARTESIAN_POINT('Ctrl Pts',(5.04096893490742,-1.11744005069485,3.31387115631648));
#54668=CARTESIAN_POINT('Ctrl Pts',(3.68139281034196,3.62041254264275,3.4722607567406));
#54669=CARTESIAN_POINT('Ctrl Pts',(-1.03309179131411,5.05892887272037,3.63065035716471));
#54670=CARTESIAN_POINT('Ctrl Pts',(-4.0212815682019,2.54692422938098,3.75609340221952));
#54671=CARTESIAN_POINT('Ctrl Pts',(-4.36973323768933,0.549490145536826,
3.82873991379962));
#54672=CARTESIAN_POINT('Ctrl Pts',(-4.36665723562798,0.00267775706545938,
3.84858989190502));
#54673=CARTESIAN_POINT('Origin',(0.,0.,-1.84858989190501));
#54674=CARTESIAN_POINT('',(-4.36544656918105,0.00153916655095219,1.65141010809498));
#54675=CARTESIAN_POINT('',(-4.37121340809612,-0.00394090090135357,1.84858989190502));
#54676=CARTESIAN_POINT('',(-4.372,-4.40683631492666E-13,-1.84858989190501));
#54677=CARTESIAN_POINT('Ctrl Pts',(-4.36544656918105,0.00153916655095176,
1.65141010809498));
#54678=CARTESIAN_POINT('Ctrl Pts',(-4.36281788561468,-0.823458774996837,
1.68133792152568));
#54679=CARTESIAN_POINT('Ctrl Pts',(-3.74207983653693,-3.10661615213039,
1.76402917581661));
#54680=CARTESIAN_POINT('Ctrl Pts',(-0.0624691826164238,-5.16187799225891,
1.89948387096774));
#54681=CARTESIAN_POINT('Ctrl Pts',(4.29430578210828,-2.8649130214088,2.05777419354839));
#54682=CARTESIAN_POINT('Ctrl Pts',(4.74212257914569,2.03988351823947,2.21606451612903));
#54683=CARTESIAN_POINT('Ctrl Pts',(0.873326467994359,5.08784270323556,2.37435483870968));
#54684=CARTESIAN_POINT('Ctrl Pts',(-3.40224500791429,3.63628377215307,2.51947003603166));
#54685=CARTESIAN_POINT('Ctrl Pts',(-4.36153810021927,1.08370711208091,2.61182179249343));
#54686=CARTESIAN_POINT('Ctrl Pts',(-4.3712761175009,-0.00392989124947909,
2.65141010809498));
#54687=CARTESIAN_POINT('Ctrl Pts',(-4.37121340809612,-0.00394090090135399,
1.84858989190502));
#54688=CARTESIAN_POINT('Ctrl Pts',(-4.37447604421791,-0.368207831146071,
1.86184817876984));
#54689=CARTESIAN_POINT('Ctrl Pts',(-4.16647286574876,-2.17936832407669,
1.92790299910937));
#54690=CARTESIAN_POINT('Ctrl Pts',(-1.65208468153467,-4.89189754332655,
2.04675435292359));
#54691=CARTESIAN_POINT('Ctrl Pts',(3.20433051897175,-4.04874042926377,2.20514395334771));
#54692=CARTESIAN_POINT('Ctrl Pts',(5.14059300557593,0.484092964878372,2.36353355377181));
#54693=CARTESIAN_POINT('Ctrl Pts',(2.392155064142,4.57576601695794,2.52192315419593));
#54694=CARTESIAN_POINT('Ctrl Pts',(-2.53628918908134,4.49747442552335,2.68031275462004));
#54695=CARTESIAN_POINT('Ctrl Pts',(-4.33547083524805,1.62595452236117,2.78920166718974));
#54696=CARTESIAN_POINT('Ctrl Pts',(-4.37879165497107,0.0917787298065273,
2.84529404628473));
#54697=CARTESIAN_POINT('Ctrl Pts',(-4.37836367713493,0.00160984593324717,
2.84858989190502));
#54698=CARTESIAN_POINT('Origin',(0.,0.,-1.84858989190501));
#54699=CARTESIAN_POINT('',(-4.37640441740291,0.00246357316762604,0.651410108094979));
#54700=CARTESIAN_POINT('',(-4.36535621882271,0.00145633068789036,0.848589891905021));
#54701=CARTESIAN_POINT('',(-4.372,-4.40683631492666E-13,-1.84858989190501));
#54702=CARTESIAN_POINT('Ctrl Pts',(-4.37640441740291,0.00246357316762608,
0.651410108094978));
#54703=CARTESIAN_POINT('Ctrl Pts',(-4.3669296163584,-1.27588513251927,0.698090609697727));
#54704=CARTESIAN_POINT('Ctrl Pts',(-3.10443214653608,-4.01442651751147,
0.79753455216069));
#54705=CARTESIAN_POINT('Ctrl Pts',(1.54404435335689,-4.92628156041988,0.949741935483869));
#54706=CARTESIAN_POINT('Ctrl Pts',(4.97150648183897,-1.38949747849925,1.10803225806451));
#54707=CARTESIAN_POINT('Ctrl Pts',(3.87423912778238,3.41166257284768,1.26632258064516));
#54708=CARTESIAN_POINT('Ctrl Pts',(-0.749980974679123,5.10752324154442,
1.42461290322581));
#54709=CARTESIAN_POINT('Ctrl Pts',(-3.94614385852298,2.71245661069425,1.55297541237574));
#54710=CARTESIAN_POINT('Ctrl Pts',(-4.36745231673392,0.631032051720065,
1.62857448066547));
#54711=CARTESIAN_POINT('Ctrl Pts',(-4.36544656918105,0.00153916655095176,
1.65141010809498));
#54712=CARTESIAN_POINT('Ctrl Pts',(-4.36535621882271,0.0014563306878905,
0.848589891905021));
#54713=CARTESIAN_POINT('Ctrl Pts',(-4.36284379533113,-0.820370961494963,
0.87840231125495));
#54714=CARTESIAN_POINT('Ctrl Pts',(-3.74556810328531,-3.1011139180804,0.961011264079584));
#54715=CARTESIAN_POINT('Ctrl Pts',(-0.0704529116473286,-5.16289724783097,
1.09641675037892));
#54716=CARTESIAN_POINT('Ctrl Pts',(4.29252819085395,-2.86947836000301,1.25480635080303));
#54717=CARTESIAN_POINT('Ctrl Pts',(4.74374945851672,2.03886099295457,1.41319595122714));
#54718=CARTESIAN_POINT('Ctrl Pts',(0.87187597225223,5.08919664880298,1.57158555165126));
#54719=CARTESIAN_POINT('Ctrl Pts',(-3.4039180408651,3.63453814591924,1.71671686521054));
#54720=CARTESIAN_POINT('Ctrl Pts',(-4.36148372635845,1.08235900094027,1.80905164529514));
#54721=CARTESIAN_POINT('Ctrl Pts',(-4.37121340809612,-0.00394090090135399,
1.84858989190502));
#54722=CARTESIAN_POINT('Origin',(0.,0.,19.5));
#54723=CARTESIAN_POINT('',(-4.87237116524908,0.00192128708900893,19.1338737912933));
#54724=CARTESIAN_POINT('Ctrl Pts',(-0.803308159453631,4.29756675351939,
19.628));
#54725=CARTESIAN_POINT('Ctrl Pts',(-0.673853669232168,4.32487002581643,
19.6249474412138));
#54726=CARTESIAN_POINT('Ctrl Pts',(-0.543485635434045,4.34604385579072,
19.621903094994));
#54727=CARTESIAN_POINT('Ctrl Pts',(-0.412569255997991,4.3612238307311,19.6188638308603));
#54728=CARTESIAN_POINT('Ctrl Pts',(-0.27984336996821,4.37661362101213,19.6157825584728));
#54729=CARTESIAN_POINT('Ctrl Pts',(-0.146553204834455,4.38584275860783,
19.6127065096298));
#54730=CARTESIAN_POINT('Ctrl Pts',(-0.0130667331008604,4.38900056457998,
19.6096324222416));
#54731=CARTESIAN_POINT('Ctrl Pts',(0.102479072721167,4.39173395943972,19.6069714941353));
#54732=CARTESIAN_POINT('Ctrl Pts',(0.218172435996331,4.38991749290017,19.6043120356729));
#54733=CARTESIAN_POINT('Ctrl Pts',(0.333776183320261,4.38357806344137,19.6016519311904));
#54734=CARTESIAN_POINT('Ctrl Pts',(0.379031782704649,4.38109635600062,19.6006105754768));
#54735=CARTESIAN_POINT('Ctrl Pts',(0.424273632554427,4.37792119522461,19.5995691207606));
#54736=CARTESIAN_POINT('Ctrl Pts',(0.469487373095433,4.37405300814147,19.5985274401165));
#54737=CARTESIAN_POINT('Ctrl Pts',(0.491900142232015,4.37213552060263,19.598011071696));
#54738=CARTESIAN_POINT('Ctrl Pts',(0.514298864495916,4.37004829843513,19.5974948121273));
#54739=CARTESIAN_POINT('Ctrl Pts',(0.536673783628106,4.36779258854753,19.5969788310225));
#54740=CARTESIAN_POINT('Ctrl Pts',(0.67587029099505,4.35375960205351,19.5937688633242));
#54741=CARTESIAN_POINT('Ctrl Pts',(0.814241659431173,4.33320254529649,19.5905674515573));
#54742=CARTESIAN_POINT('Ctrl Pts',(0.951373424482021,4.30622334317185,19.5873709472848));
#54743=CARTESIAN_POINT('Ctrl Pts',(1.08850518953287,4.2792441410472,19.5841744430122));
#54744=CARTESIAN_POINT('Ctrl Pts',(1.22439822554137,4.24584269855803,19.580982846234));
#54745=CARTESIAN_POINT('Ctrl Pts',(1.35863436321977,4.20606161338018,19.5777925085132));
#54746=CARTESIAN_POINT('Ctrl Pts',(1.44718365537814,4.1798198949077,19.57568799216));
#54747=CARTESIAN_POINT('Ctrl Pts',(1.53501187237287,4.15080088353343,19.573584023676));
#54748=CARTESIAN_POINT('Ctrl Pts',(1.62197697724057,4.11905814350536,19.5714795558027));
#54749=CARTESIAN_POINT('Ctrl Pts',(1.66029004733011,4.10507366288661,19.5705524181278));
#54750=CARTESIAN_POINT('Ctrl Pts',(1.69843554242665,4.09056039562537,19.5696251835263));
#54751=CARTESIAN_POINT('Ctrl Pts',(1.73640102301099,4.07552228846135,19.5686977624494));
#54752=CARTESIAN_POINT('Ctrl Pts',(1.75436952443725,4.06840497436797,19.5682588277464));
#54753=CARTESIAN_POINT('Ctrl Pts',(1.77228816141992,4.061173866115,19.5678200842298));
#54754=CARTESIAN_POINT('Ctrl Pts',(1.79015508413385,4.05383000141309,19.5673815385189));
#54755=CARTESIAN_POINT('Ctrl Pts',(1.91574464850677,4.00220875787305,19.5642989279495));
#54756=CARTESIAN_POINT('Ctrl Pts',(2.03879019285953,3.94501636210332,19.561225830935));
#54757=CARTESIAN_POINT('Ctrl Pts',(2.15887237555029,3.88249361470115,19.5581590360687));
#54758=CARTESIAN_POINT('Ctrl Pts',(2.27969637656572,3.81958462748645,19.5550732958053));
#54759=CARTESIAN_POINT('Ctrl Pts',(2.39752111769151,3.75127894449634,19.5519939357949));
#54760=CARTESIAN_POINT('Ctrl Pts',(2.51190593036526,3.67777150955579,19.5489176847461));
#54761=CARTESIAN_POINT('Ctrl Pts',(2.62522809247125,3.60494696874821,19.5458700124906));
#54762=CARTESIAN_POINT('Ctrl Pts',(2.73517470696147,3.52701649641376,19.5428253916997));
#54763=CARTESIAN_POINT('Ctrl Pts',(2.84129224832913,3.44412553804493,19.5397806414099));
#54764=CARTESIAN_POINT('Ctrl Pts',(2.91209516263097,3.38881968242346,19.5377491469835));
#54765=CARTESIAN_POINT('Ctrl Pts',(2.98119295340959,3.33130466078434,19.5357175949077));
#54766=CARTESIAN_POINT('Ctrl Pts',(3.04844206982076,3.27161381566964,19.5336850403595));
#54767=CARTESIAN_POINT('Ctrl Pts',(3.08425226424725,3.23982840519718,19.5326027038555));
#54768=CARTESIAN_POINT('Ctrl Pts',(3.1195381208217,3.20742589648737,19.5315200830935));
#54769=CARTESIAN_POINT('Ctrl Pts',(3.15427695670459,3.17441047942531,19.5304370354107));
#54770=CARTESIAN_POINT('Ctrl Pts',(3.16725486117647,3.16207641819842,19.5300324251523));
#54771=CARTESIAN_POINT('Ctrl Pts',(3.18015812731145,3.14965513440157,19.5296277011351));
#54772=CARTESIAN_POINT('Ctrl Pts',(3.19297991753168,3.13715232569191,19.5292230337074));
#54773=CARTESIAN_POINT('Ctrl Pts',(3.21028959746143,3.12027327734767,19.5286767243753));
#54774=CARTESIAN_POINT('Ctrl Pts',(3.22744427955767,3.10325207454711,19.5281307247594));
#54775=CARTESIAN_POINT('Ctrl Pts',(3.24444163127926,3.08608990264034,19.5275850170264));
#54776=CARTESIAN_POINT('Ctrl Pts',(3.33717764080849,2.99245464912803,19.5246076851246));
#54777=CARTESIAN_POINT('Ctrl Pts',(3.42523294755332,2.89462674101026,19.5216390416869));
#54778=CARTESIAN_POINT('Ctrl Pts',(3.50859096128539,2.79305369138356,19.5186761904996));
#54779=CARTESIAN_POINT('Ctrl Pts',(3.59397640033088,2.68901019215335,19.5156412771407));
#54780=CARTESIAN_POINT('Ctrl Pts',(3.67443362705331,2.58103662340854,19.5126124412155));
#54781=CARTESIAN_POINT('Ctrl Pts',(3.74990902226373,2.46957232453757,19.5095865700048));
#54782=CARTESIAN_POINT('Ctrl Pts',(3.82667993619766,2.35619476524857,19.5065087603736));
#54783=CARTESIAN_POINT('Ctrl Pts',(3.89829689144343,2.23920494837555,19.5034340181076));
#54784=CARTESIAN_POINT('Ctrl Pts',(3.96466142958627,2.11903192999767,19.5003590674328));
#54785=CARTESIAN_POINT('Ctrl Pts',(4.0309620923612,1.99897457724446,19.4972870763748));
#54786=CARTESIAN_POINT('Ctrl Pts',(4.09202070623594,1.87573937136613,19.4942148773091));
#54787=CARTESIAN_POINT('Ctrl Pts',(4.14769296331372,1.74973219296001,19.4911392039111));
#54788=CARTESIAN_POINT('Ctrl Pts',(4.15491534612853,1.73338523439156,19.4907401956463));
#54789=CARTESIAN_POINT('Ctrl Pts',(4.16204794028702,1.71698942368025,19.490341076027));
#54790=CARTESIAN_POINT('Ctrl Pts',(4.1690873140012,1.70055278577387,19.4899420115644));
#54791=CARTESIAN_POINT('Ctrl Pts',(4.2235955422653,1.57327839358026,19.4868519217777));
#54792=CARTESIAN_POINT('Ctrl Pts',(4.27240340036226,1.44383040880503,19.4837717143479));
#54793=CARTESIAN_POINT('Ctrl Pts',(4.31545919855678,1.31266698606642,19.4806981622917));
#54794=CARTESIAN_POINT('Ctrl Pts',(4.35892069590576,1.18026765801579,19.4775956492703));
#54795=CARTESIAN_POINT('Ctrl Pts',(4.39652153701043,1.04611964222381,19.4744999176358));
#54796=CARTESIAN_POINT('Ctrl Pts',(4.42816288898243,0.910666566444117,19.4714076483225));
#54797=CARTESIAN_POINT('Ctrl Pts',(4.45971763719553,0.775584231634271,19.4683238426851));
#54798=CARTESIAN_POINT('Ctrl Pts',(4.48534571134421,0.639203155572113,19.4652434804418));
#54799=CARTESIAN_POINT('Ctrl Pts',(4.50489988856683,0.501947997482608,19.4621632697058));
#54800=CARTESIAN_POINT('Ctrl Pts',(4.5234656283834,0.371630903362032,19.4592387594872));
#54801=CARTESIAN_POINT('Ctrl Pts',(4.53655584516878,0.240525160569636,19.456314385846));
#54802=CARTESIAN_POINT('Ctrl Pts',(4.5440002395032,0.108991400598333,19.453387331288));
#54803=CARTESIAN_POINT('Ctrl Pts',(4.54553145652646,0.0819365827912304,
19.4527852734757));
#54804=CARTESIAN_POINT('Ctrl Pts',(4.54682366211308,0.0548636663001908,
19.4521831022411));
#54805=CARTESIAN_POINT('Ctrl Pts',(4.54787513450369,0.0277758132908992,
19.4515807930663));
#54806=CARTESIAN_POINT('Ctrl Pts',(4.54880630338109,0.00378719894119923,
19.4510473966946));
#54807=CARTESIAN_POINT('Ctrl Pts',(4.54954867988174,-0.0202170615304457,
19.450513804788));
#54808=CARTESIAN_POINT('Ctrl Pts',(4.5501006277934,-0.0442070954676754,
19.4499806150988));
#54809=CARTESIAN_POINT('Ctrl Pts',(4.55331420062987,-0.183882814458235,
19.4468762571225));
#54810=CARTESIAN_POINT('Ctrl Pts',(4.55008558494902,-0.323251293541528,
19.443781616557));
#54811=CARTESIAN_POINT('Ctrl Pts',(4.54031186270851,-0.461877411739,19.4406934171861));
#54812=CARTESIAN_POINT('Ctrl Pts',(4.53067866021077,-0.598510460562132,
19.4376496177859));
#54813=CARTESIAN_POINT('Ctrl Pts',(4.51468731171393,-0.734423134579881,
19.4346120756979));
#54814=CARTESIAN_POINT('Ctrl Pts',(4.49218947310497,-0.869204596926774,
19.4315776539935));
#54815=CARTESIAN_POINT('Ctrl Pts',(4.48129191999887,-0.934490341445224,
19.430107834059));
#54816=CARTESIAN_POINT('Ctrl Pts',(4.46886701290829,-0.999510687886201,
19.4286387462481));
#54817=CARTESIAN_POINT('Ctrl Pts',(4.45489347098868,-1.06421861098155,19.4271700340528));
#54818=CARTESIAN_POINT('Ctrl Pts',(4.42601008140308,-1.19797025124501,19.4241341977007));
#54819=CARTESIAN_POINT('Ctrl Pts',(4.39051333916906,-1.33038812058978,19.421099966171));
#54820=CARTESIAN_POINT('Ctrl Pts',(4.34872071354063,-1.46115895479143,19.4180641910325));
#54821=CARTESIAN_POINT('Ctrl Pts',(4.32227027711835,-1.54392345173146,19.416142857398));
#54822=CARTESIAN_POINT('Ctrl Pts',(4.29329690956391,-1.62602796166861,19.4142209054574));
#54823=CARTESIAN_POINT('Ctrl Pts',(4.26187123440312,-1.70738903830258,19.4122975370436));
#54824=CARTESIAN_POINT('Ctrl Pts',(4.25321767430855,-1.72979310639049,19.4117679069221));
#54825=CARTESIAN_POINT('Ctrl Pts',(4.24437655206198,-1.75214443843245,19.4112380817814));
#54826=CARTESIAN_POINT('Ctrl Pts',(4.23535981723739,-1.7744158038722,19.4107086515302));
#54827=CARTESIAN_POINT('Ctrl Pts',(4.18439432237877,-1.90030074813356,19.4077161409069));
#54828=CARTESIAN_POINT('Ctrl Pts',(4.12776551664013,-2.02378469411099,19.4047326389142));
#54829=CARTESIAN_POINT('Ctrl Pts',(4.06584469055636,-2.14458841387499,19.4017552111055));
#54830=CARTESIAN_POINT('Ctrl Pts',(4.00036068062891,-2.2723436859638,19.3986064496223));
#54831=CARTESIAN_POINT('Ctrl Pts',(3.92895803265593,-2.39710220266129,19.3954644815049));
#54832=CARTESIAN_POINT('Ctrl Pts',(3.85201703329039,-2.51851897272141,19.392325836016));
#54833=CARTESIAN_POINT('Ctrl Pts',(3.77655716323104,-2.63759844617919,19.3892476100675));
#54834=CARTESIAN_POINT('Ctrl Pts',(3.69576939240684,-2.75346420580146,19.3861725800561));
#54835=CARTESIAN_POINT('Ctrl Pts',(3.60996439826952,-2.86576656284731,19.3830974718481));
#54836=CARTESIAN_POINT('Ctrl Pts',(3.54413699183306,-2.95192207133902,19.3807383271401));
#54837=CARTESIAN_POINT('Ctrl Pts',(3.47535563877055,-3.03597991726489,19.3783791364089));
#54838=CARTESIAN_POINT('Ctrl Pts',(3.40374469167589,-3.11776882943693,19.3760184212987));
#54839=CARTESIAN_POINT('Ctrl Pts',(3.38306291872267,-3.14139007423622,19.3753366292557));
#54840=CARTESIAN_POINT('Ctrl Pts',(3.36214505086869,-3.16482198260282,19.3746547100648));
#54841=CARTESIAN_POINT('Ctrl Pts',(3.34099389843024,-3.18806021076517,19.3739726281131));
#54842=CARTESIAN_POINT('Ctrl Pts',(3.32373515295353,-3.20702195132993,19.3734160684253));
#54843=CARTESIAN_POINT('Ctrl Pts',(3.30632108269655,-3.22585473586077,19.3728594003699));
#54844=CARTESIAN_POINT('Ctrl Pts',(3.28875317708965,-3.24455615157313,19.372302604599));
#54845=CARTESIAN_POINT('Ctrl Pts',(3.27637002727884,-3.25773828253526,19.3719101340564));
#54846=CARTESIAN_POINT('Ctrl Pts',(3.26391669904378,-3.27084847479794,19.3715177984306));
#54847=CARTESIAN_POINT('Ctrl Pts',(3.25139510554647,-3.28388487669204,19.3711256274074));
#54848=CARTESIAN_POINT('Ctrl Pts',(3.15282448543269,-3.38650809465787,19.3680384371903));
#54849=CARTESIAN_POINT('Ctrl Pts',(3.05000398947139,-3.48458548857025,19.3649607083322));
#54850=CARTESIAN_POINT('Ctrl Pts',(2.94328170324704,-3.57779502158214,19.3618892172301));
#54851=CARTESIAN_POINT('Ctrl Pts',(2.83673480189425,-3.67085137626031,19.3588227737435));
#54852=CARTESIAN_POINT('Ctrl Pts',(2.72629835158367,-3.75905650319765,19.3557625475278));
#54853=CARTESIAN_POINT('Ctrl Pts',(2.61227793614804,-3.84205888933313,19.3527053308466));
#54854=CARTESIAN_POINT('Ctrl Pts',(2.49975879118773,-3.92396840950061,19.3496883675631));
#54855=CARTESIAN_POINT('Ctrl Pts',(2.38374884571102,-4.0008118415243,19.3466743350847));
#54856=CARTESIAN_POINT('Ctrl Pts',(2.26451075890163,-4.07221233820177,19.3436601507197));
#54857=CARTESIAN_POINT('Ctrl Pts',(2.15307182587664,-4.13894265382576,19.3408431188587));
#54858=CARTESIAN_POINT('Ctrl Pts',(2.03881261846325,-4.20091883876065,19.3380259543306));
#54859=CARTESIAN_POINT('Ctrl Pts',(1.92192917555825,-4.2577952663979,19.3352061406412));
#54860=CARTESIAN_POINT('Ctrl Pts',(1.89885610409831,-4.26902280938128,19.334649502668));
#54861=CARTESIAN_POINT('Ctrl Pts',(1.87568072700257,-4.28005149894805,19.3340927614631));
#54862=CARTESIAN_POINT('Ctrl Pts',(1.85240449004643,-4.29087848232892,19.3335358976687));
#54863=CARTESIAN_POINT('Ctrl Pts',(1.83464431921192,-4.29913965765674,19.3331110009753));
#54864=CARTESIAN_POINT('Ctrl Pts',(1.81682357432143,-4.30728417370212,19.3326859893584));
#54865=CARTESIAN_POINT('Ctrl Pts',(1.79895912167073,-4.315303623104,19.3322612385723));
#54866=CARTESIAN_POINT('Ctrl Pts',(1.72163150021165,-4.35001641054753,19.3304226729781));
#54867=CARTESIAN_POINT('Ctrl Pts',(1.64342321773675,-4.38241577414544,19.3285875039126));
#54868=CARTESIAN_POINT('Ctrl Pts',(1.56440032675076,-4.41242911636972,19.3267550510791));
#54869=CARTESIAN_POINT('Ctrl Pts',(1.43711047143297,-4.46077452542352,19.3238033410982));
#54870=CARTESIAN_POINT('Ctrl Pts',(1.30770822291801,-4.50293181836922,19.3208586788369));
#54871=CARTESIAN_POINT('Ctrl Pts',(1.17662145504096,-4.53906398417229,19.3179182210069));
#54872=CARTESIAN_POINT('Ctrl Pts',(1.04250946942332,-4.57603000735673,19.3149099033514));
#54873=CARTESIAN_POINT('Ctrl Pts',(0.906633655370345,-4.60668969161992,
19.3119059864259));
#54874=CARTESIAN_POINT('Ctrl Pts',(0.769431097467203,-4.63116704578967,
19.308903425512));
#54875=CARTESIAN_POINT('Ctrl Pts',(0.630182204159468,-4.65600947242755,
19.3058560822937));
#54876=CARTESIAN_POINT('Ctrl Pts',(0.489565915681568,-4.67448381748104,
19.3028101358377));
#54877=CARTESIAN_POINT('Ctrl Pts',(0.348028745832047,-4.68666735853543,
19.2997624031501));
#54878=CARTESIAN_POINT('Ctrl Pts',(0.276401735269172,-4.69283302247179,
19.2982200522494));
#54879=CARTESIAN_POINT('Ctrl Pts',(0.204538794597775,-4.69738677129886,
19.2966772438915));
#54880=CARTESIAN_POINT('Ctrl Pts',(0.132497794988,-4.70033357743951,19.2951335655473));
#54881=CARTESIAN_POINT('Ctrl Pts',(0.112510249077041,-4.70115115941847,
19.2947052769069));
#54882=CARTESIAN_POINT('Ctrl Pts',(0.092508998863809,-4.70184502431764,
19.2942769212978));
#54883=CARTESIAN_POINT('Ctrl Pts',(0.0724952864131179,-4.70241523264229,
19.2938484899096));
#54884=CARTESIAN_POINT('Ctrl Pts',(0.0524053747538238,-4.70298761194961,
19.2934184273332));
#54885=CARTESIAN_POINT('Ctrl Pts',(0.0323102430098365,-4.70343515128597,
19.2929884454936));
#54886=CARTESIAN_POINT('Ctrl Pts',(0.0122186816347883,-4.70375813703399,
19.2925586960882));
#54887=CARTESIAN_POINT('Ctrl Pts',(-0.130279647047385,-4.70604889624492,
19.2895107213251));
#54888=CARTESIAN_POINT('Ctrl Pts',(-0.272714799094277,-4.70208198168319,
19.2864719199788));
#54889=CARTESIAN_POINT('Ctrl Pts',(-0.414633190928799,-4.69200784465072,
19.2834391901245));
#54890=CARTESIAN_POINT('Ctrl Pts',(-0.558078433367512,-4.68182532348272,
19.2803738321848));
#54891=CARTESIAN_POINT('Ctrl Pts',(-0.70099656213896,-4.66540343587715,
19.277314677082));
#54892=CARTESIAN_POINT('Ctrl Pts',(-0.842927293052888,-4.64284438111864,
19.2742585216926));
#54893=CARTESIAN_POINT('Ctrl Pts',(-0.984668741071393,-4.62031541176288,
19.2712064420796));
#54894=CARTESIAN_POINT('Ctrl Pts',(-1.12542627120009,-4.59166551790643,
19.2681573541844));
#54895=CARTESIAN_POINT('Ctrl Pts',(-1.26473685825812,-4.5569449834536,19.2651080676816));
#54896=CARTESIAN_POINT('Ctrl Pts',(-1.40219852797764,-4.52268525675062,
19.2620992510297));
#54897=CARTESIAN_POINT('Ctrl Pts',(-1.53825218997399,-4.48251476703442,
19.259090241007));
#54898=CARTESIAN_POINT('Ctrl Pts',(-1.6724364842164,-4.43643407027143,19.2560779726351));
#54899=CARTESIAN_POINT('Ctrl Pts',(-1.69577574030498,-4.42841905488856,
19.2555540357366));
#54900=CARTESIAN_POINT('Ctrl Pts',(-1.71905838453956,-4.42022512285657,
19.2550300002629));
#54901=CARTESIAN_POINT('Ctrl Pts',(-1.74228191014027,-4.41185213332152,
19.2545058500857));
#54902=CARTESIAN_POINT('Ctrl Pts',(-1.76035515482698,-4.40533602154642,
19.2540979406852));
#54903=CARTESIAN_POINT('Ctrl Pts',(-1.77838477372036,-4.39871426481839,
19.2536901381687));
#54904=CARTESIAN_POINT('Ctrl Pts',(-1.79636551936284,-4.3919886694264,19.2532825296376));
#54905=CARTESIAN_POINT('Ctrl Pts',(-1.93187451941972,-4.34130230054732,
19.2502106534458));
#54906=CARTESIAN_POINT('Ctrl Pts',(-2.06468449537211,-4.28469503542289,
19.2471480732848));
#54907=CARTESIAN_POINT('Ctrl Pts',(-2.19433977491624,-4.22226508755719,
19.2440916139197));
#54908=CARTESIAN_POINT('Ctrl Pts',(-2.32196725551768,-4.1608115394395,19.2410829573521));
#54909=CARTESIAN_POINT('Ctrl Pts',(-2.44653872111971,-4.09371577322205,
19.23808023162));
#54910=CARTESIAN_POINT('Ctrl Pts',(-2.56760656005401,-4.02102358517923,
19.235080408152));
#54911=CARTESIAN_POINT('Ctrl Pts',(-2.68526160349352,-3.95038052574101,
19.2321651470591));
#54912=CARTESIAN_POINT('Ctrl Pts',(-2.79960837675168,-3.87445182317372,
19.229252626912));
#54913=CARTESIAN_POINT('Ctrl Pts',(-2.91021369160128,-3.79323796763903,
19.2263400681055));
#54914=CARTESIAN_POINT('Ctrl Pts',(-2.98399388261748,-3.73906359290253,
19.2243972216394));
#54915=CARTESIAN_POINT('Ctrl Pts',(-3.05610871619606,-3.68253657740801,
19.2224543579711));
#54916=CARTESIAN_POINT('Ctrl Pts',(-3.12651483591522,-3.62376762555295,
19.2205106520618));
#54917=CARTESIAN_POINT('Ctrl Pts',(-3.16741234664924,-3.58962991353437,
19.2193815920652));
#54918=CARTESIAN_POINT('Ctrl Pts',(-3.20773318569702,-3.55473559432281,
19.2182522478782));
#54919=CARTESIAN_POINT('Ctrl Pts',(-3.24746784403176,-3.51910539807467,
19.217122457792));
#54920=CARTESIAN_POINT('Ctrl Pts',(-3.26700401396051,-3.50158725150764,
19.2165669787208));
#54921=CARTESIAN_POINT('Ctrl Pts',(-3.28639847163628,-3.48389120743249,
19.21601139186));
#54922=CARTESIAN_POINT('Ctrl Pts',(-3.30565001708697,-3.46601967389373,
19.2154556779901));
#54923=CARTESIAN_POINT('Ctrl Pts',(-3.31923733798883,-3.45340633530117,
19.2150634672609));
#54924=CARTESIAN_POINT('Ctrl Pts',(-3.33275239972697,-3.44070650564925,
19.2146712232022));
#54925=CARTESIAN_POINT('Ctrl Pts',(-3.34618584616149,-3.42792978435657,
19.2142792032619));
#54926=CARTESIAN_POINT('Ctrl Pts',(-3.44713342315095,-3.33191726347047,
19.2113333126973));
#54927=CARTESIAN_POINT('Ctrl Pts',(-3.54361479719668,-3.23143681477532,
19.2083960349772));
#54928=CARTESIAN_POINT('Ctrl Pts',(-3.63553433126932,-3.126940879262,19.2054645714511));
#54929=CARTESIAN_POINT('Ctrl Pts',(-3.73049026986206,-3.01899309932707,
19.2024362720435));
#54930=CARTESIAN_POINT('Ctrl Pts',(-3.82057851236323,-2.90675969406161,
19.1994141772984));
#54931=CARTESIAN_POINT('Ctrl Pts',(-3.90566064499467,-2.79069444962541,
19.1963952019566));
#54932=CARTESIAN_POINT('Ctrl Pts',(-3.99147592842286,-2.67362907362455,
19.1933502121733));
#54933=CARTESIAN_POINT('Ctrl Pts',(-4.07219888206677,-2.55266483623709,
19.1903083957846));
#54934=CARTESIAN_POINT('Ctrl Pts',(-4.14764752468129,-2.42823151976782,
19.1872665870857));
#54935=CARTESIAN_POINT('Ctrl Pts',(-4.20306739838779,-2.33683055555379,
19.1850322638681));
#54936=CARTESIAN_POINT('Ctrl Pts',(-4.25564073821494,-2.24355706942676,
19.1827979447995));
#54937=CARTESIAN_POINT('Ctrl Pts',(-4.30527982057198,-2.14857260904585,
19.1805623752584));
#54938=CARTESIAN_POINT('Ctrl Pts',(-4.32699691910319,-2.10701690762921,
19.1795843135842));
#54939=CARTESIAN_POINT('Ctrl Pts',(-4.3481522027174,-2.06513363702578,19.1786060125617));
#54940=CARTESIAN_POINT('Ctrl Pts',(-4.36873745807105,-2.02293601505909,
19.1776273671286));
#54941=CARTESIAN_POINT('Ctrl Pts',(-4.38086243818899,-1.99808107308335,
19.1770509323837));
#54942=CARTESIAN_POINT('Ctrl Pts',(-4.39278964467502,-1.97311706816874,
19.1764743781503));
#54943=CARTESIAN_POINT('Ctrl Pts',(-4.40451730909724,-1.9480466787424,19.175897682959));
#54944=CARTESIAN_POINT('Ctrl Pts',(-4.4127985002692,-1.93034386255322,19.1754904643556));
#54945=CARTESIAN_POINT('Ctrl Pts',(-4.42097601800018,-1.91259691029446,
19.1750833804788));
#54946=CARTESIAN_POINT('Ctrl Pts',(-4.42904852534276,-1.89480918199437,
19.1746764755087));
#54947=CARTESIAN_POINT('Ctrl Pts',(-4.48950921559979,-1.76158436280397,
19.1716288777402));
#54948=CARTESIAN_POINT('Ctrl Pts',(-4.54410184606152,-1.62603381239176,
19.1685903704127));
#54949=CARTESIAN_POINT('Ctrl Pts',(-4.59268280744846,-1.48860776987399,
19.1655578531078));
#54950=CARTESIAN_POINT('Ctrl Pts',(-4.64144650306992,-1.35066480793007,
19.1625139291796));
#54951=CARTESIAN_POINT('Ctrl Pts',(-4.68415360775462,-1.21083146528599,
19.1594760404209));
#54952=CARTESIAN_POINT('Ctrl Pts',(-4.72061445405524,-1.06953622768658,
19.1564410512956));
#54953=CARTESIAN_POINT('Ctrl Pts',(-4.75671346962216,-0.929643178041525,
19.1534361808442));
#54954=CARTESIAN_POINT('Ctrl Pts',(-4.78668986944038,-0.78831633896503,
19.1504341527609));
#54955=CARTESIAN_POINT('Ctrl Pts',(-4.81031125214298,-0.645956691618861,
19.1474319239356));
#54956=CARTESIAN_POINT('Ctrl Pts',(-4.82807965738957,-0.538871347096197,
19.1451735964244));
#54957=CARTESIAN_POINT('Ctrl Pts',(-4.84225125518576,-0.431201234879474,
19.1429151553273));
#54958=CARTESIAN_POINT('Ctrl Pts',(-4.85270728658022,-0.32311529964396,
19.1406553054137));
#54959=CARTESIAN_POINT('Ctrl Pts',(-4.85885127437678,-0.259603758599947,
19.1393274124716));
#54960=CARTESIAN_POINT('Ctrl Pts',(-4.86371203457958,-0.195948633814534,
19.1379990330984));
#54961=CARTESIAN_POINT('Ctrl Pts',(-4.86726251019289,-0.132184380886881,
19.136669904511));
#54962=CARTESIAN_POINT('Ctrl Pts',(-4.86838059639054,-0.112104273637358,
19.1362513464105));
#54963=CARTESIAN_POINT('Ctrl Pts',(-4.86936819801155,-0.0920224658990377,
19.1358329041084));
#54964=CARTESIAN_POINT('Ctrl Pts',(-4.87022464687506,-0.0719445408679467,
19.1354146627671));
#54965=CARTESIAN_POINT('Ctrl Pts',(-4.87127693233824,-0.0472755739962392,
19.1349007858712));
#54966=CARTESIAN_POINT('Ctrl Pts',(-4.87213135174695,-0.0226102934020704,
19.134387167001));
#54967=CARTESIAN_POINT('Ctrl Pts',(-4.8727870952798,0.00204924970852941,
19.1338737912933));
#54968=CARTESIAN_POINT('',(0.446113671359645,4.91412736825422,19.058));
#54969=CARTESIAN_POINT('Ctrl Pts',(0.44649414690178,4.91265885279919,19.058));
#54970=CARTESIAN_POINT('Ctrl Pts',(0.299727560449543,4.91447193481392,19.0691244126311));
#54971=CARTESIAN_POINT('Ctrl Pts',(0.153167317909177,4.91005959431981,19.0802626720314));
#54972=CARTESIAN_POINT('Ctrl Pts',(0.00725046426545532,4.89944030839442,
19.0914270753353));
#54973=CARTESIAN_POINT('Ctrl Pts',(-0.137909608980915,4.88887609813179,
19.10253357579));
#54974=CARTESIAN_POINT('Ctrl Pts',(-0.282433758712205,4.87216902002991,
19.1136659496671));
#54975=CARTESIAN_POINT('Ctrl Pts',(-0.425882683147369,4.84928678485378,
19.1248363037588));
#54976=CARTESIAN_POINT('Ctrl Pts',(-0.565675808016648,4.82698770403557,
19.1357219810862));
#54977=CARTESIAN_POINT('Ctrl Pts',(-0.704448457143253,4.79882393308609,
19.1466437274425));
#54978=CARTESIAN_POINT('Ctrl Pts',(-0.841774914873059,4.76472078486696,
19.1576127473831));
#54979=CARTESIAN_POINT('Ctrl Pts',(-0.940805834192305,4.74012781002693,
19.1655228919155));
#54980=CARTESIAN_POINT('Ctrl Pts',(-1.0390843184423,4.71244522520194,19.1734576204009));
#54981=CARTESIAN_POINT('Ctrl Pts',(-1.13644149966956,4.68163105513636,19.181421134727));
#54982=CARTESIAN_POINT('Ctrl Pts',(-1.16730557623662,4.6718623776514,19.1839457201022));
#54983=CARTESIAN_POINT('Ctrl Pts',(-1.198076992637,4.66177888532038,19.1864731984846));
#54984=CARTESIAN_POINT('Ctrl Pts',(-1.22875016771071,4.65137899873876,19.1890037037495));
#54985=CARTESIAN_POINT('Ctrl Pts',(-1.24841289336978,4.644712257645,19.190625858309));
#54986=CARTESIAN_POINT('Ctrl Pts',(-1.26802854233492,4.6379177328912,19.1922487049096));
#54987=CARTESIAN_POINT('Ctrl Pts',(-1.28758810772402,4.63099805128267,19.1938716419773));
#54988=CARTESIAN_POINT('Ctrl Pts',(-1.41973360557623,4.58424830235176,19.204836293928));
#54989=CARTESIAN_POINT('Ctrl Pts',(-1.54943066798541,4.53175252800649,19.2158141351685));
#54990=CARTESIAN_POINT('Ctrl Pts',(-1.67628513679076,4.47348474855613,19.2268170475339));
#54991=CARTESIAN_POINT('Ctrl Pts',(-1.77854477370016,4.42651405823497,19.2356866903145));
#54992=CARTESIAN_POINT('Ctrl Pts',(-1.87895707987582,4.37579165399884,19.2445726249588));
#54993=CARTESIAN_POINT('Ctrl Pts',(-1.97730366067652,4.32128226154577,19.2534810756009));
#54994=CARTESIAN_POINT('Ctrl Pts',(-2.10058309475894,4.25295363233385,19.2646479991967));
#54995=CARTESIAN_POINT('Ctrl Pts',(-2.22061803115919,4.17867506623871,19.275850302475));
#54996=CARTESIAN_POINT('Ctrl Pts',(-2.3371003873209,4.09882401061829,19.2871002449437));
#54997=CARTESIAN_POINT('Ctrl Pts',(-2.45349352336119,4.01903411722977,19.2983415704744));
#54998=CARTESIAN_POINT('Ctrl Pts',(-2.56634003134295,3.93367951832198,19.3096304622446));
#54999=CARTESIAN_POINT('Ctrl Pts',(-2.67529062823455,3.84310647943015,19.3209791516131));
#55000=CARTESIAN_POINT('Ctrl Pts',(-2.71693531724479,3.80848632915125,19.3253170134781));
#55001=CARTESIAN_POINT('Ctrl Pts',(-2.75801032451888,3.77310349110297,19.3296636119694));
#55002=CARTESIAN_POINT('Ctrl Pts',(-2.79849428295858,3.73697648238141,19.3340196301562));
#55003=CARTESIAN_POINT('Ctrl Pts',(-2.81294818526249,3.72407813264686,19.335574850143));
#55004=CARTESIAN_POINT('Ctrl Pts',(-2.82732736116309,3.71108427106867,19.3371313434063));
#55005=CARTESIAN_POINT('Ctrl Pts',(-2.84161861583708,3.69800711896962,19.3386877998622));
#55006=CARTESIAN_POINT('Ctrl Pts',(-2.94391515755751,3.60440110145739,19.34982888694));
#55007=CARTESIAN_POINT('Ctrl Pts',(-3.04186033803071,3.50639786607989,19.3609841912936));
#55008=CARTESIAN_POINT('Ctrl Pts',(-3.13519298587128,3.40438402939327,19.3721662582028));
#55009=CARTESIAN_POINT('Ctrl Pts',(-3.22998005288867,3.30078049302696,19.3835225772406));
#55010=CARTESIAN_POINT('Ctrl Pts',(-3.32001032606879,3.19303967930977,19.3949064994243));
#55011=CARTESIAN_POINT('Ctrl Pts',(-3.4049668301135,3.08153340439932,19.4063311657064));
#55012=CARTESIAN_POINT('Ctrl Pts',(-3.48992333415822,2.97002712948888,19.4177558319884));
#55013=CARTESIAN_POINT('Ctrl Pts',(-3.56980658085615,2.85475460919877,19.4292212423689));
#55014=CARTESIAN_POINT('Ctrl Pts',(-3.64424819284547,2.73606613269444,19.4407405378004));
#55015=CARTESIAN_POINT('Ctrl Pts',(-3.69362849951562,2.65733498741996,19.4483817793834));
#55016=CARTESIAN_POINT('Ctrl Pts',(-3.74061319511361,2.57710031760525,19.4560467316635));
#55017=CARTESIAN_POINT('Ctrl Pts',(-3.78513614038734,2.49546231597417,19.463739230308));
#55018=CARTESIAN_POINT('Ctrl Pts',(-3.80567440292713,2.4578030214146,19.4672877501953));
#55019=CARTESIAN_POINT('Ctrl Pts',(-3.82568866999261,2.41984508871949,19.470842131787));
#55020=CARTESIAN_POINT('Ctrl Pts',(-3.84517166765662,2.38159830576804,19.4744027515965));
#55021=CARTESIAN_POINT('Ctrl Pts',(-3.85722034167954,2.35794573298872,19.4766047098446));
#55022=CARTESIAN_POINT('Ctrl Pts',(-3.86906582550741,2.33418269113951,19.4788090538567));
#55023=CARTESIAN_POINT('Ctrl Pts',(-3.88070630194933,2.310311496771,19.4810158726822));
#55024=CARTESIAN_POINT('Ctrl Pts',(-3.8885082527386,2.29431198982011,19.4824949781091));
#55025=CARTESIAN_POINT('Ctrl Pts',(-3.8962165975453,2.27826690602767,19.4839749160027));
#55026=CARTESIAN_POINT('Ctrl Pts',(-3.90382674774023,2.26218599112426,19.4854548878754));
#55027=CARTESIAN_POINT('Ctrl Pts',(-3.96414789534232,2.13472211503535,19.4971857472531));
#55028=CARTESIAN_POINT('Ctrl Pts',(-4.01838481417725,2.00484470453858,19.5089339279855));
#55029=CARTESIAN_POINT('Ctrl Pts',(-4.06640211675339,1.87293521419554,19.5207141703003));
#55030=CARTESIAN_POINT('Ctrl Pts',(-4.11224826252183,1.74699016109889,19.5319617555951));
#55031=CARTESIAN_POINT('Ctrl Pts',(-4.15242432683241,1.61919178653392,19.5432385686204));
#55032=CARTESIAN_POINT('Ctrl Pts',(-4.18676153681696,1.4898597689249,19.554557439162));
#55033=CARTESIAN_POINT('Ctrl Pts',(-4.2207524598163,1.36183205048544,19.5657621601394));
#55034=CARTESIAN_POINT('Ctrl Pts',(-4.24902179998014,1.23230080216518,19.5770080946197));
#55035=CARTESIAN_POINT('Ctrl Pts',(-4.27135507448881,1.1015746586975,19.588307688129));
#55036=CARTESIAN_POINT('Ctrl Pts',(-4.29323252438759,0.973516650317833,
19.5993766556815));
#55037=CARTESIAN_POINT('Ctrl Pts',(-4.30941374767392,0.844311453337346,
19.6104971142425));
#55038=CARTESIAN_POINT('Ctrl Pts',(-4.31964759244882,0.714256825545012,
19.621680762742));
#55039=CARTESIAN_POINT('Ctrl Pts',(-4.32157304106312,0.689787673591424,
19.6237849123534));
#55040=CARTESIAN_POINT('Ctrl Pts',(-4.32328781702124,0.665288489028016,
19.6258912988008));
#55041=CARTESIAN_POINT('Ctrl Pts',(-4.32479004603219,0.640761311051878,
19.628));
#55042=CARTESIAN_POINT('',(-3.60367707498796,3.37571982724537,19.058));
#55043=CARTESIAN_POINT('Origin',(0.,0.,19.058));
#55044=CARTESIAN_POINT('Ctrl Pts',(-4.8727870952798,0.00204924970852941,
19.1338737912933));
#55045=CARTESIAN_POINT('Ctrl Pts',(-4.87617886814195,0.129598459003725,
19.1312184028586));
#55046=CARTESIAN_POINT('Ctrl Pts',(-4.87425769241846,0.256993603559053,
19.1285695196845));
#55047=CARTESIAN_POINT('Ctrl Pts',(-4.86689403436298,0.383955746440246,
19.1259250851319));
#55048=CARTESIAN_POINT('Ctrl Pts',(-4.85865401760772,0.526027822131655,
19.1229659329201));
#55049=CARTESIAN_POINT('Ctrl Pts',(-4.84360044272571,0.667558209996482,
19.1200123512114));
#55050=CARTESIAN_POINT('Ctrl Pts',(-4.82205180462592,0.808202442374607,
19.117061458221));
#55051=CARTESIAN_POINT('Ctrl Pts',(-4.80012826355871,0.951293601552751,
19.1140592256271));
#55052=CARTESIAN_POINT('Ctrl Pts',(-4.77148144982624,1.09346818380839,19.1110597761218));
#55053=CARTESIAN_POINT('Ctrl Pts',(-4.73639180273002,1.23435901743,19.1080600748768));
#55054=CARTESIAN_POINT('Ctrl Pts',(-4.71189105823817,1.33273362650888,19.1059655849107));
#55055=CARTESIAN_POINT('Ctrl Pts',(-4.68424808585656,1.43048229055225,19.1038709722142));
#55056=CARTESIAN_POINT('Ctrl Pts',(-4.6535439006576,1.52747603119476,19.1017752037047));
#55057=CARTESIAN_POINT('Ctrl Pts',(-4.64011081963306,1.56991079272586,19.1008583049818));
#55058=CARTESIAN_POINT('Ctrl Pts',(-4.62609165763282,1.61220100164168,19.099941185029));
#55059=CARTESIAN_POINT('Ctrl Pts',(-4.61149254035212,1.65433555918283,19.0990237573359));
#55060=CARTESIAN_POINT('Ctrl Pts',(-4.60425406248102,1.6752265525563,19.098568881885));
#55061=CARTESIAN_POINT('Ctrl Pts',(-4.59687300609065,1.69607927843875,19.0981139307812));
#55062=CARTESIAN_POINT('Ctrl Pts',(-4.58935008303519,1.71689236429986,19.0976588934799));
#55063=CARTESIAN_POINT('Ctrl Pts',(-4.58288926961042,1.73476699408821,19.0972680997573));
#55064=CARTESIAN_POINT('Ctrl Pts',(-4.57632388063936,1.75261206193917,19.0968772491973));
#55065=CARTESIAN_POINT('Ctrl Pts',(-4.56965942251531,1.77041363655401,19.0964866227106));
#55066=CARTESIAN_POINT('Ctrl Pts',(-4.51879838731399,1.90626962008207,19.0935054849917));
#55067=CARTESIAN_POINT('Ctrl Pts',(-4.4621015938381,2.03978869153619,19.090533120728));
#55068=CARTESIAN_POINT('Ctrl Pts',(-4.39988991481362,2.17062521779186,19.0875666304161));
#55069=CARTESIAN_POINT('Ctrl Pts',(-4.33631291127845,2.304333139242,19.0845350362203));
#55070=CARTESIAN_POINT('Ctrl Pts',(-4.26697605411688,2.4352402172723,19.08150957663));
#55071=CARTESIAN_POINT('Ctrl Pts',(-4.19216902199247,2.5629660482269,19.0784871570202));
#55072=CARTESIAN_POINT('Ctrl Pts',(-4.11721282278043,2.69094656767373,19.0754587106304));
#55073=CARTESIAN_POINT('Ctrl Pts',(-4.03676418963347,2.81573387820879,19.0724333163567));
#55074=CARTESIAN_POINT('Ctrl Pts',(-3.95106744680097,2.93692273562437,19.0694078610249));
#55075=CARTESIAN_POINT('Ctrl Pts',(-3.86644065662709,3.05659850939287,19.0664201795206));
#55076=CARTESIAN_POINT('Ctrl Pts',(-3.77669549591118,3.17276577294219,19.0634324384734));
#55077=CARTESIAN_POINT('Ctrl Pts',(-3.68202832948565,3.28500209019142,19.0604416398662));
#55078=CARTESIAN_POINT('Ctrl Pts',(-3.65627454507218,3.31553548447098,19.0596280063176));
#55079=CARTESIAN_POINT('Ctrl Pts',(-3.63015628737134,3.34577773744076,19.0588141464826));
#55080=CARTESIAN_POINT('Ctrl Pts',(-3.60367707498796,3.37571982724537,19.058));
#55081=CARTESIAN_POINT('',(-4.,-4.89858719658941E-16,20.));
#55082=CARTESIAN_POINT('',(-4.5,-5.51091059616309E-16,19.5));
#55083=CARTESIAN_POINT('Origin',(0.,0.,20.));
#55084=CARTESIAN_POINT('Ctrl Pts',(2.86929757049748,-4.02374147429196,-0.329089653438089));
#55085=CARTESIAN_POINT('Ctrl Pts',(3.53627793941073,-3.54812315628632,-0.302707933007981));
#55086=CARTESIAN_POINT('Ctrl Pts',(4.61815699384527,-2.26074102389229,-0.249944492147766));
#55087=CARTESIAN_POINT('Ctrl Pts',(5.34305681190694,1.0543831002385,-0.144417610427336));
#55088=CARTESIAN_POINT('Ctrl Pts',(2.97075510791326,5.02204979956487,-0.0125090082767979));
#55089=CARTESIAN_POINT('Ctrl Pts',(-2.60167993603097,5.22655530852652,0.145781314303847));
#55090=CARTESIAN_POINT('Ctrl Pts',(-5.79544439621568,0.666623916928201,
0.304071636884492));
#55091=CARTESIAN_POINT('Ctrl Pts',(-3.71916882578288,-4.49661457488776,
0.462361959465137));
#55092=CARTESIAN_POINT('Ctrl Pts',(1.74534931250902,-5.56854608224957,0.620652282045782));
#55093=CARTESIAN_POINT('Ctrl Pts',(5.61966720797076,-1.57065337116734,0.778942604626428));
#55094=CARTESIAN_POINT('Ctrl Pts',(4.37934349714106,3.85645847095449,0.937232927207072));
#55095=CARTESIAN_POINT('Ctrl Pts',(-0.84775983002377,5.77341716827827,1.09552324978772));
#55096=CARTESIAN_POINT('Ctrl Pts',(-5.30296447800194,2.43487893547456,1.25381357236836));
#55097=CARTESIAN_POINT('Ctrl Pts',(-4.93115623773879,-3.11998211803485,
1.41210389494901));
#55098=CARTESIAN_POINT('Ctrl Pts',(-0.0706136094443395,-5.83485842583339,
1.57039421752965));
#55099=CARTESIAN_POINT('Ctrl Pts',(4.85417638956518,-3.23842638421833,1.7286845401103));
#55100=CARTESIAN_POINT('Ctrl Pts',(5.36037735273058,2.3058335652194,1.88697486269095));
#55101=CARTESIAN_POINT('Ctrl Pts',(0.98718650613642,5.75117077753662,2.04526518527159));
#55102=CARTESIAN_POINT('Ctrl Pts',(-4.28460500301765,3.96139458246299,2.20355550785224));
#55103=CARTESIAN_POINT('Ctrl Pts',(-5.65625702821141,-1.43431356080714,
2.36184583043288));
#55104=CARTESIAN_POINT('Ctrl Pts',(-1.87919427403712,-5.52441175942303,
2.52013615301353));
#55105=CARTESIAN_POINT('Ctrl Pts',(3.60843955214569,-4.58581057252521,2.67842647559417));
#55106=CARTESIAN_POINT('Ctrl Pts',(5.81142420090129,0.527110130500736,2.83671679817481));
#55107=CARTESIAN_POINT('Ctrl Pts',(2.72445125981257,5.16021910144056,2.99500712075546));
#55108=CARTESIAN_POINT('Ctrl Pts',(-2.84250423844022,5.09614219820049,3.15329744333611));
#55109=CARTESIAN_POINT('Ctrl Pts',(-5.82201720884499,0.393206705834578,
3.31158776591675));
#55110=CARTESIAN_POINT('Ctrl Pts',(-3.50193025017819,-4.66765255027645,
3.4698780884974));
#55111=CARTESIAN_POINT('Ctrl Pts',(2.00585411337058,-5.47969388429905,3.62816841107804));
#55112=CARTESIAN_POINT('Ctrl Pts',(5.68777231250098,-1.30374151751568,3.78645873365868));
#55113=CARTESIAN_POINT('Ctrl Pts',(4.19228952744401,4.05896591843996,3.94474905623933));
#55114=CARTESIAN_POINT('Ctrl Pts',(-1.11930309959379,5.72692381468561,4.10303937881998));
#55115=CARTESIAN_POINT('Ctrl Pts',(-5.41202917540188,2.18184234468851,4.26132970140061));
#55116=CARTESIAN_POINT('Ctrl Pts',(-4.77835461070898,-3.34930187121133,
4.41962002398127));
#55117=CARTESIAN_POINT('Ctrl Pts',(0.204906485773977,-5.83168150213524,
4.57791034656191));
#55118=CARTESIAN_POINT('Ctrl Pts',(5.00164762657821,-3.00566412467992,4.73620066914256));
#55119=CARTESIAN_POINT('Ctrl Pts',(5.24554559701654,2.55631516056015,4.8944909917232));
#55120=CARTESIAN_POINT('Ctrl Pts',(0.714587714204218,5.79136082533626,5.05278131430385));
#55121=CARTESIAN_POINT('Ctrl Pts',(-4.46683698218372,3.75471213080312,5.21107163688449));
#55122=CARTESIAN_POINT('Ctrl Pts',(-5.58223988624457,-1.69973340938259,
5.36936195946513));
#55123=CARTESIAN_POINT('Ctrl Pts',(-1.61630467165047,-5.60696486692776,
5.52765228204579));
#55124=CARTESIAN_POINT('Ctrl Pts',(3.82090205882377,-4.41035183034713,5.68594260462642));
#55125=CARTESIAN_POINT('Ctrl Pts',(5.78006132540833,0.800866334091529,5.84423292720708));
#55126=CARTESIAN_POINT('Ctrl Pts',(2.47781181352747,5.28308095975332,6.00252324978771));
#55127=CARTESIAN_POINT('Ctrl Pts',(-3.07991218091209,4.95627246713037,6.16081357236837));
#55128=CARTESIAN_POINT('Ctrl Pts',(-5.83408858766023,0.117924390593317,
6.319103894949));
#55129=CARTESIAN_POINT('Ctrl Pts',(-3.27767689138409,-4.82776656501236,
6.47739421752966));
#55130=CARTESIAN_POINT('Ctrl Pts',(2.26230141403803,-5.37889283427418,6.63568454011029));
#55131=CARTESIAN_POINT('Ctrl Pts',(5.7429776032295,-1.03378143694346,6.79397486269095));
#55132=CARTESIAN_POINT('Ctrl Pts',(3.99600116469878,4.25234882180315,6.95226518527158));
#55133=CARTESIAN_POINT('Ctrl Pts',(-1.38840996925396,5.66769914231875,7.11055550785224));
#55134=CARTESIAN_POINT('Ctrl Pts',(-5.50899499668582,1.92392046016856,7.26884583043288));
#55135=CARTESIAN_POINT('Ctrl Pts',(-4.61491443420867,-3.57114275484712,
7.42713615301353));
#55136=CARTESIAN_POINT('Ctrl Pts',(0.47997818700567,-5.81550657729517,7.58542647559416));
#55137=CARTESIAN_POINT('Ctrl Pts',(5.13796169871233,-2.76619691871885,7.74371679817482));
#55138=CARTESIAN_POINT('Ctrl Pts',(5.1190196099595,2.80109515072493,7.90200712075546));
#55139=CARTESIAN_POINT('Ctrl Pts',(0.440394310825021,5.81863804180648,8.06029744333611));
#55140=CARTESIAN_POINT('Ctrl Pts',(-4.63910813519642,3.53965697780435,8.21858776591675));
#55141=CARTESIAN_POINT('Ctrl Pts',(-5.49577575427904,-1.96136296213705,
8.3768780884974));
#55142=CARTESIAN_POINT('Ctrl Pts',(-1.34981084575569,-5.67701563246438,
8.53516841107803));
#55143=CARTESIAN_POINT('Ctrl Pts',(4.02484459618971,-4.22505879096223,8.69345873365869));
#55144=CARTESIAN_POINT('Ctrl Pts',(5.73581007047566,1.07283672848883,8.85174905623933));
#55145=CARTESIAN_POINT('Ctrl Pts',(2.22564729760008,5.39416257794014,9.01003937881998));
#55146=CARTESIAN_POINT('Ctrl Pts',(-3.31045249741171,4.80535119142661,9.16832970140062));
#55147=CARTESIAN_POINT('Ctrl Pts',(-5.83315107572507,-0.157620868961595,
9.32662002398126));
#55148=CARTESIAN_POINT('Ctrl Pts',(-3.04611493876333,-4.97711558941596,
9.48491034656191));
#55149=CARTESIAN_POINT('Ctrl Pts',(2.51370421497615,-5.26609788459876,9.64320066914256));
#55150=CARTESIAN_POINT('Ctrl Pts',(5.78537715735888,-0.761516222857186,
9.8014909917232));
#55151=CARTESIAN_POINT('Ctrl Pts',(3.79080248595607,4.43624980394858,9.95978131430386));
#55152=CARTESIAN_POINT('Ctrl Pts',(-1.6544209509478,5.59583658871751,10.1180716368845));
#55153=CARTESIAN_POINT('Ctrl Pts',(-5.59367681682763,1.66170860244797,10.2763619594652));
#55154=CARTESIAN_POINT('Ctrl Pts',(-4.44118388437089,-3.78502067573863,
10.4346522820458));
#55155=CARTESIAN_POINT('Ctrl Pts',(0.753979628983335,-5.78636418916428,
10.5929426046264));
#55156=CARTESIAN_POINT('Ctrl Pts',(5.26281910261167,-2.52056162466824,10.7512329272071));
#55157=CARTESIAN_POINT('Ctrl Pts',(4.98107919185876,3.03962923643596,10.9095232497877));
#55158=CARTESIAN_POINT('Ctrl Pts',(0.165218912680596,5.83294081244249,11.0678135723684));
#55159=CARTESIAN_POINT('Ctrl Pts',(-4.80103496763896,3.31670906925412,11.226103894949));
#55160=CARTESIAN_POINT('Ctrl Pts',(-5.3970570974028,-2.21861905200931,11.3843942175297));
#55161=CARTESIAN_POINT('Ctrl Pts',(-1.08030720079852,-5.73440774295545,
11.5426845401103));
#55162=CARTESIAN_POINT('Ctrl Pts',(4.219812502755,-4.03034468155729,11.7009748626909));
#55163=CARTESIAN_POINT('Ctrl Pts',(5.67876906018774,1.34241490293389,11.8592651852716));
#55164=CARTESIAN_POINT('Ctrl Pts',(1.96852001545618,5.49321624909424,12.0175555078522));
#55165=CARTESIAN_POINT('Ctrl Pts',(-3.53361114034896,4.64371490504813,12.1758458304329));
#55166=CARTESIAN_POINT('Ctrl Pts',(-5.81920675667964,-0.432814664237157,
12.3341361530135));
#55167=CARTESIAN_POINT('Ctrl Pts',(-2.80776073459116,-5.11536660151085,
12.4924264755942));
#55168=CARTESIAN_POINT('Ctrl Pts',(2.75950193807008,-5.14156054757227,12.6507167981748));
#55169=CARTESIAN_POINT('Ctrl Pts',(5.81487643104491,-0.487552973782061,
12.8090071207555));
#55170=CARTESIAN_POINT('Ctrl Pts',(3.57715104538901,4.61025880065714,12.9672974433361));
#55171=CARTESIAN_POINT('Ctrl Pts',(-1.91674289151962,5.51149639375472,13.1255877659167));
#55172=CARTESIAN_POINT('Ctrl Pts',(-5.66588581148519,1.39579145354196,13.2838780884974));
#55173=CARTESIAN_POINT('Ctrl Pts',(-4.25755034704318,-3.99045872713326,
13.442168411078));
#55174=CARTESIAN_POINT('Ctrl Pts',(1.02629984112814,-5.74431931969763,13.6004587336587));
#55175=CARTESIAN_POINT('Ctrl Pts',(5.37594143021732,-2.26930596206795,13.7587490562393));
#55176=CARTESIAN_POINT('Ctrl Pts',(4.8320319233711,3.27138553246996,13.91703937882));
#55177=CARTESIAN_POINT('Ctrl Pts',(-0.110324891911251,5.8342372448088,14.0753297014006));
#55178=CARTESIAN_POINT('Ctrl Pts',(-4.95225641377798,3.0863655361992,14.2336200239813));
#55179=CARTESIAN_POINT('Ctrl Pts',(-5.28630403923151,-2.47092804732617,
14.3919103465619));
#55180=CARTESIAN_POINT('Ctrl Pts',(-0.808394678245584,-5.77901322496909,
14.5502006691425));
#55181=CARTESIAN_POINT('Ctrl Pts',(4.40537103766032,-3.82664367730009,14.7084909917232));
#55182=CARTESIAN_POINT('Ctrl Pts',(5.60906548477092,1.60899975000773,14.8667813143038));
#55183=CARTESIAN_POINT('Ctrl Pts',(1.70700331210297,5.58002110223998,15.0250716368845));
#55184=CARTESIAN_POINT('Ctrl Pts',(-3.74889050980069,4.47172402646598,15.1833619594651));
#55185=CARTESIAN_POINT('Ctrl Pts',(-5.7922867217461,-0.707043367010812,
15.3416522820458));
#55186=CARTESIAN_POINT('Ctrl Pts',(-2.56314576668009,-5.24221132595445,
15.4999426046264));
#55187=CARTESIAN_POINT('Ctrl Pts',(2.99914650864464,-5.00555852161226,15.658232927207));
#55188=CARTESIAN_POINT('Ctrl Pts',(5.83140963307135,-0.2125025674033,15.8165232497877));
#55189=CARTESIAN_POINT('Ctrl Pts',(3.35552327049972,4.77398779042229,15.9748135723683));
#55190=CARTESIAN_POINT('Ctrl Pts',(-2.17479091272675,5.41486664825819,16.133103894949));
#55191=CARTESIAN_POINT('Ctrl Pts',(-5.72546087416986,1.12676190338666,16.2913942175296));
#55192=CARTESIAN_POINT('Ctrl Pts',(-4.06442347000951,-4.18699871789581,
16.4496845401103));
#55193=CARTESIAN_POINT('Ctrl Pts',(1.29633194620277,-5.68946591914921,16.6079748626909));
#55194=CARTESIAN_POINT('Ctrl Pts',(5.47707578180272,-2.01298980380955,16.7662651852716));
#55195=CARTESIAN_POINT('Ctrl Pts',(4.67221141036031,3.49584654228241,16.9245555078522));
#55196=CARTESIAN_POINT('Ctrl Pts',(-0.385625099973721,5.82252583304098,
17.0828458304329));
#55197=CARTESIAN_POINT('Ctrl Pts',(-5.09243067800049,2.84913735309004,17.2411361530135));
#55198=CARTESIAN_POINT('Ctrl Pts',(-5.163772332666,-2.71772228672297,17.3994264755942));
#55199=CARTESIAN_POINT('Ctrl Pts',(-0.534662778757779,-5.81074229086598,
17.5577167981748));
#55200=CARTESIAN_POINT('Ctrl Pts',(4.58107430334251,-3.61439149963352,17.7160071207555));
#55201=CARTESIAN_POINT('Ctrl Pts',(5.52691620363093,1.87196148635973,17.8742974433361));
#55202=CARTESIAN_POINT('Ctrl Pts',(1.44156288337564,5.6544511543935,18.0325877659168));
#55203=CARTESIAN_POINT('Ctrl Pts',(-3.95558608138272,4.2896328856293,18.1908780884974));
#55204=CARTESIAN_POINT('Ctrl Pts',(-5.75288016701676,-0.979448557484372,
18.349168411078));
#55205=CARTESIAN_POINT('Ctrl Pts',(-2.31199479018177,-5.35783906812632,
18.5074587336587));
#55206=CARTESIAN_POINT('Ctrl Pts',(3.23053211221357,-4.8574916848313,18.6657490562393));
#55207=CARTESIAN_POINT('Ctrl Pts',(5.83796734686214,0.0612873527283092,
18.82403937882));
#55208=CARTESIAN_POINT('Ctrl Pts',(3.12041701848007,4.9304530959418,18.9823297014006));
#55209=CARTESIAN_POINT('Ctrl Pts',(-1.49215234175522,5.23769617354117,19.1142383035512));
#55210=CARTESIAN_POINT('Ctrl Pts',(-4.11442054260868,3.08380732139205,19.2197651852716));
#55211=CARTESIAN_POINT('Ctrl Pts',(-4.76857407193705,1.53464683800148,19.2725286261318));
#55212=CARTESIAN_POINT('Ctrl Pts',(-4.8886350428845,0.724300640260437,19.2989103465619));
#55213=CARTESIAN_POINT('Ctrl Pts',(2.75898463274061,-3.86904481704479,-0.21939310229206));
#55214=CARTESIAN_POINT('Ctrl Pts',(3.40032229220555,-3.4117121081895,-0.193011381861952));
#55215=CARTESIAN_POINT('Ctrl Pts',(4.44060745341011,-2.17382463487172,-0.140247941001737));
#55216=CARTESIAN_POINT('Ctrl Pts',(5.13763779242852,1.01384631572915,-0.0347210592813072));
#55217=CARTESIAN_POINT('Ctrl Pts',(2.85654153638278,4.82897220710893,0.0971875428692309));
#55218=CARTESIAN_POINT('Ctrl Pts',(-2.50165581870078,5.02561530273532,0.255477865449875));
#55219=CARTESIAN_POINT('Ctrl Pts',(-5.57263289575413,0.640994911623377,
0.413768188030522));
#55220=CARTESIAN_POINT('Ctrl Pts',(-3.5761817604452,-4.32373785104547,0.572058510611166));
#55221=CARTESIAN_POINT('Ctrl Pts',(1.67824765945831,-5.35445790830635,0.730348833191812));
#55222=CARTESIAN_POINT('Ctrl Pts',(5.4036136325935,-1.51026807361131,0.888639155772457));
#55223=CARTESIAN_POINT('Ctrl Pts',(4.2109753740215,3.70819317158555,1.0469294783531));
#55224=CARTESIAN_POINT('Ctrl Pts',(-0.815166878242221,5.55145252603366,
1.20521980093375));
#55225=CARTESIAN_POINT('Ctrl Pts',(-5.09908684732198,2.3412676449565,1.36351012351439));
#55226=CARTESIAN_POINT('Ctrl Pts',(-4.74157313673304,-3.0000313688591,1.52180044609504));
#55227=CARTESIAN_POINT('Ctrl Pts',(-0.0678988005016982,-5.6105316146419,
1.68009076867568));
#55228=CARTESIAN_POINT('Ctrl Pts',(4.66755285374621,-3.11392192994849,1.83838109125633));
#55229=CARTESIAN_POINT('Ctrl Pts',(5.15429242820228,2.21718354955942,1.99667141383697));
#55230=CARTESIAN_POINT('Ctrl Pts',(0.94923316008907,5.53006141943627,2.15496173641762));
#55231=CARTESIAN_POINT('Ctrl Pts',(-4.11987919351274,3.8090949121538,2.31325205899827));
#55232=CARTESIAN_POINT('Ctrl Pts',(-5.43879672158246,-1.37916997995865,
2.47154238157891));
#55233=CARTESIAN_POINT('Ctrl Pts',(-1.80694682117044,-5.31202037247638,
2.62983270415955));
#55234=CARTESIAN_POINT('Ctrl Pts',(3.46970958150474,-4.40950462174014,2.7881230267402));
#55235=CARTESIAN_POINT('Ctrl Pts',(5.58799834129561,0.506844868502552,2.94641334932084));
#55236=CARTESIAN_POINT('Ctrl Pts',(2.61970707944744,4.96182945569518,3.10470367190149));
#55237=CARTESIAN_POINT('Ctrl Pts',(-2.73322139641198,4.90021605136558,3.26299399448213));
#55238=CARTESIAN_POINT('Ctrl Pts',(-5.59818409073885,0.378089491324522,
3.42128431706278));
#55239=CARTESIAN_POINT('Ctrl Pts',(-3.3672951333158,-4.48820010500075,3.57957463964342));
#55240=CARTESIAN_POINT('Ctrl Pts',(1.92873709970399,-5.269021719585,3.73786496222407));
#55241=CARTESIAN_POINT('Ctrl Pts',(5.46910037009403,-1.25361790595597,3.89615528480471));
#55242=CARTESIAN_POINT('Ctrl Pts',(4.03111287624724,3.90291502315395,4.05444560738536));
#55243=CARTESIAN_POINT('Ctrl Pts',(-1.07627040252322,5.50674665467138,4.21273592996601));
#55244=CARTESIAN_POINT('Ctrl Pts',(-5.20395844627879,2.09795929218125,4.37102625254665));
#55245=CARTESIAN_POINT('Ctrl Pts',(-4.5946461169747,-3.22053470093006,4.5293165751273));
#55246=CARTESIAN_POINT('Ctrl Pts',(0.197028656494944,-5.60747683086738,
4.68760689770794));
#55247=CARTESIAN_POINT('Ctrl Pts',(4.80935441551997,-2.89010844202325,4.84589722028858));
#55248=CARTESIAN_POINT('Ctrl Pts',(5.04387549110129,2.45803513617603,5.00418754286923));
#55249=CARTESIAN_POINT('Ctrl Pts',(0.687114694030425,5.56870632173167,5.16247786544987));
#55250=CARTESIAN_POINT('Ctrl Pts',(-4.29510508687517,3.61035856850998,5.32076818803052));
#55251=CARTESIAN_POINT('Ctrl Pts',(-5.3676252406787,-1.63438550412508,5.47905851061116));
#55252=CARTESIAN_POINT('Ctrl Pts',(-1.55416426541541,-5.39139964541496,
5.63734883319181));
#55253=CARTESIAN_POINT('Ctrl Pts',(3.67400376032591,-4.24079156167736,5.79563915577246));
#55254=CARTESIAN_POINT('Ctrl Pts',(5.55784124207616,0.770076248402076,5.95392947835309));
#55255=CARTESIAN_POINT('Ctrl Pts',(2.38254992672651,5.07996777028487,6.11221980093375));
#55256=CARTESIAN_POINT('Ctrl Pts',(-2.9615019594687,4.76572374824029,6.27051012351439));
#55257=CARTESIAN_POINT('Ctrl Pts',(-5.60979137364659,0.113390672622288,
6.42880044609503));
#55258=CARTESIAN_POINT('Ctrl Pts',(-3.15166341316413,-4.64215838060276,
6.58709076867568));
#55259=CARTESIAN_POINT('Ctrl Pts',(2.17532503429963,-5.17209606403701,6.74538109125632));
#55260=CARTESIAN_POINT('Ctrl Pts',(5.52218323968972,-0.994036703430842,
6.90367141383697));
#55261=CARTESIAN_POINT('Ctrl Pts',(3.84237101065328,4.08886313257964,7.06196173641762));
#55262=CARTESIAN_POINT('Ctrl Pts',(-1.33503119666024,5.44979893247647,7.22025205899827));
#55263=CARTESIAN_POINT('Ctrl Pts',(-5.29719632218758,1.84995346554449,7.3785423815789));
#55264=CARTESIAN_POINT('Ctrl Pts',(-4.43748955713467,-3.43384669587891,
7.53683270415955));
#55265=CARTESIAN_POINT('Ctrl Pts',(0.461524958448211,-5.59192376675569,
7.6951230267402));
#55266=CARTESIAN_POINT('Ctrl Pts',(4.94042776047775,-2.65984778586643,7.85341334932084));
#55267=CARTESIAN_POINT('Ctrl Pts',(4.92221391876315,2.69340432137696,8.01170367190149));
#55268=CARTESIAN_POINT('Ctrl Pts',(0.42346292291388,5.59493483906605,8.16999399448214));
#55269=CARTESIAN_POINT('Ctrl Pts',(-4.46075310774047,3.40357142017932,8.32828431706278));
#55270=CARTESIAN_POINT('Ctrl Pts',(-5.28448530642128,-1.88595645408243,
8.48657463964342));
#55271=CARTESIAN_POINT('Ctrl Pts',(-1.29791605403297,-5.4587572410908,8.64486496222408));
#55272=CARTESIAN_POINT('Ctrl Pts',(3.87010552834755,-4.0626222935355,8.8031552848047));
#55273=CARTESIAN_POINT('Ctrl Pts',(5.51529126970868,1.03159047628066,8.96144560738537));
#55274=CARTESIAN_POINT('Ctrl Pts',(2.1400801210432,5.18677874754585,9.11973592996599));
#55275=CARTESIAN_POINT('Ctrl Pts',(-3.18317892911787,4.62060478787114,9.27802625254666));
#55276=CARTESIAN_POINT('Ctrl Pts',(-5.60888990527024,-0.151560981243543,
9.43631657512728));
#55277=CARTESIAN_POINT('Ctrl Pts',(-2.92900408518884,-4.78576553640322,
9.59460689770795));
#55278=CARTESIAN_POINT('Ctrl Pts',(2.41706240986782,-5.06363762598407,9.75289722028857));
#55279=CARTESIAN_POINT('Ctrl Pts',(5.56295270169353,-0.732238990493172,
9.91118754286925));
#55280=CARTESIAN_POINT('Ctrl Pts',(3.6450613948327,4.26569386247748,10.0694778654499));
#55281=CARTESIAN_POINT('Ctrl Pts',(-1.59081512725699,5.38069920469153,10.2277681880305));
#55282=CARTESIAN_POINT('Ctrl Pts',(-5.37862246733407,1.5978225979022,10.3860585106112));
#55283=CARTESIAN_POINT('Ctrl Pts',(-4.27043824737563,-3.63950187193647,
10.5443488331918));
#55284=CARTESIAN_POINT('Ctrl Pts',(0.724992148306133,-5.56390178610049,
10.7026391557725));
#55285=CARTESIAN_POINT('Ctrl Pts',(5.0604848999617,-2.42365617977001,10.8609294783531));
#55286=CARTESIAN_POINT('Ctrl Pts',(4.78957675429235,2.92276773199996,11.0192198009338));
#55287=CARTESIAN_POINT('Ctrl Pts',(0.158866910776627,5.60868772576421,11.1775101235144));
#55288=CARTESIAN_POINT('Ctrl Pts',(-4.61645450550797,3.18919496096631,11.335800446095));
#55289=CARTESIAN_POINT('Ctrl Pts',(-5.18956198439054,-2.13332208319472,
11.4940907686757));
#55290=CARTESIAN_POINT('Ctrl Pts',(-1.03877373901142,-5.51394285603487,
11.6523810912563));
#55291=CARTESIAN_POINT('Ctrl Pts',(4.05757770398459,-3.87539415757996,11.810671413837));
#55292=CARTESIAN_POINT('Ctrl Pts',(5.46044325657874,1.29080445543139,11.9689617364176));
#55293=CARTESIAN_POINT('Ctrl Pts',(1.89283834752078,5.28202420390446,12.1272520589983));
#55294=CARTESIAN_POINT('Ctrl Pts',(-3.39775802082929,4.4651827658415,12.2855423815789));
#55295=CARTESIAN_POINT('Ctrl Pts',(-5.59548168914238,-0.416174683216324,
12.4438327041595));
#55296=CARTESIAN_POINT('Ctrl Pts',(-2.69981364038388,-4.91870135377977,
12.6021230267402));
#55297=CARTESIAN_POINT('Ctrl Pts',(2.65341020026489,-4.94388824809053,12.7604133493208));
#55298=CARTESIAN_POINT('Ctrl Pts',(5.59131784709134,-0.468808525174477,
12.9187036719015));
#55299=CARTESIAN_POINT('Ctrl Pts',(3.43962399184309,4.43301291394634,13.0769939944821));
#55300=CARTESIAN_POINT('Ctrl Pts',(-1.84305184550816,5.29960155061157,13.2352843170628));
#55301=CARTESIAN_POINT('Ctrl Pts',(-5.44805531691171,1.34212889260043,13.3935746396434));
#55302=CARTESIAN_POINT('Ctrl Pts',(-4.0938646801192,-3.8370416574944,13.5518649622241));
#55303=CARTESIAN_POINT('Ctrl Pts',(0.986842744848443,-5.52347337256235,
13.7101552848047));
#55304=CARTESIAN_POINT('Ctrl Pts',(5.1692581295817,-2.18206028566305,13.8684456073854));
#55305=CARTESIAN_POINT('Ctrl Pts',(4.64625975310793,3.1456139316668,14.026735929966));
#55306=CARTESIAN_POINT('Ctrl Pts',(-0.106083344063608,5.60993431552639,
14.1850262525467));
#55307=CARTESIAN_POINT('Ctrl Pts',(-4.76186209596784,2.96770720923078,14.3433165751273));
#55308=CARTESIAN_POINT('Ctrl Pts',(-5.08306693533551,-2.37593081361676,
14.5016068977079));
#55309=CARTESIAN_POINT('Ctrl Pts',(-0.777315158037826,-5.55683343687841,
14.6598972202886));
#55310=CARTESIAN_POINT('Ctrl Pts',(4.23600226041317,-3.67952463669161,14.8181875428692));
#55311=CARTESIAN_POINT('Ctrl Pts',(5.39341950296062,1.54714018859507,14.9764778654499));
#55312=CARTESIAN_POINT('Ctrl Pts',(1.64137590835962,5.3654917599847,15.1347681880305));
#55313=CARTESIAN_POINT('Ctrl Pts',(-3.60476076539315,4.29980424398346,15.2930585106112));
#55314=CARTESIAN_POINT('Ctrl Pts',(-5.56959662115286,-0.679860396607744,
15.4513488331918));
#55315=CARTESIAN_POINT('Ctrl Pts',(-2.46460313299549,-5.04066940933542,
15.6096391557725));
#55316=CARTESIAN_POINT('Ctrl Pts',(2.88384140208001,-4.81311495238798,15.7679294783531));
#55317=CARTESIAN_POINT('Ctrl Pts',(5.60721541407427,-0.204332699372805,
15.9262198009337));
#55318=CARTESIAN_POINT('Ctrl Pts',(3.22651691246755,4.59044718334415,16.0845101235144));
#55319=CARTESIAN_POINT('Ctrl Pts',(-2.09117895938438,5.20668682972943,16.242800446095));
#55320=CARTESIAN_POINT('Ctrl Pts',(-5.50533995832764,1.08344244534466,16.4010907686757));
#55321=CARTESIAN_POINT('Ctrl Pts',(-3.90816275384159,-4.02602547702165,
16.5593810912563));
#55322=CARTESIAN_POINT('Ctrl Pts',(1.24649320282389,-5.47072886438628,16.717671413837));
#55323=CARTESIAN_POINT('Ctrl Pts',(5.26650427258732,-1.9355984515789,16.8759617364176));
#55324=CARTESIAN_POINT('Ctrl Pts',(4.49258369527158,3.36144531949132,17.0342520589983));
#55325=CARTESIAN_POINT('Ctrl Pts',(-0.370799367680139,5.59867316038258,
17.1925423815789));
#55326=CARTESIAN_POINT('Ctrl Pts',(-4.89664722417207,2.73959949451312,17.3508327041595));
#55327=CARTESIAN_POINT('Ctrl Pts',(-4.96524607948782,-2.61323680827755,
17.5091230267402));
#55328=CARTESIAN_POINT('Ctrl Pts',(-0.51410714784639,-5.58734264795531,
17.6674133493208));
#55329=CARTESIAN_POINT('Ctrl Pts',(4.40495044303595,-3.47543270057839,17.8257036719015));
#55330=CARTESIAN_POINT('Ctrl Pts',(5.31442853088914,1.79999210505495,17.9839939944821));
#55331=CARTESIAN_POINT('Ctrl Pts',(1.38614059526527,5.43706027634114,18.1422843170628));
#55332=CARTESIAN_POINT('Ctrl Pts',(-3.80350972455094,4.12471377428376,18.3005746396434));
#55333=CARTESIAN_POINT('Ctrl Pts',(-5.53170508977411,-0.941792704404255,
18.4588649622241));
#55334=CARTESIAN_POINT('Ctrl Pts',(-2.22310790023142,-5.15185173042014,
18.6171552848047));
#55335=CARTESIAN_POINT('Ctrl Pts',(3.1063311609144,-4.67074068925906,18.7754456073854));
#55336=CARTESIAN_POINT('Ctrl Pts',(5.61352101017582,0.0589311008023047,
18.933735929966));
#55337=CARTESIAN_POINT('Ctrl Pts',(3.00044954913339,4.74089702790683,19.0920262525466));
#55338=CARTESIAN_POINT('Ctrl Pts',(-1.43478509267926,5.03632784635119,19.2239348546972));
#55339=CARTESIAN_POINT('Ctrl Pts',(-3.95623764032305,2.96524734748178,19.3294617364176));
#55340=CARTESIAN_POINT('Ctrl Pts',(-4.58524160053518,1.47564584665783,19.3822251772778));
#55341=CARTESIAN_POINT('Ctrl Pts',(-4.70068671060039,0.696454197190917,
19.4086068977079));
#55342=CARTESIAN_POINT('Ctrl Pts',(2.64867169498374,-3.71434815979762,-0.109696551146031));
#55343=CARTESIAN_POINT('Ctrl Pts',(3.26436664500038,-3.27530106009269,-0.0833148307159233));
#55344=CARTESIAN_POINT('Ctrl Pts',(4.26305791297495,-2.08690824585116,-0.0305513898557082));
#55345=CARTESIAN_POINT('Ctrl Pts',(4.93221877295011,0.973309531219794,0.0749754918647217));
#55346=CARTESIAN_POINT('Ctrl Pts',(2.74232796485231,4.63589461465298,0.20688409401526));
#55347=CARTESIAN_POINT('Ctrl Pts',(-2.40163170137059,4.82467529694413,0.365174416595904));
#55348=CARTESIAN_POINT('Ctrl Pts',(-5.34982139529258,0.615365906318545,
0.52346473917655));
#55349=CARTESIAN_POINT('Ctrl Pts',(-3.43319469510752,-4.15086112720317,
0.681755061757195));
#55350=CARTESIAN_POINT('Ctrl Pts',(1.6111460064076,-5.14036973436311,0.84004538433784));
#55351=CARTESIAN_POINT('Ctrl Pts',(5.18756005721624,-1.44988277605528,0.998335706918485));
#55352=CARTESIAN_POINT('Ctrl Pts',(4.04260725090194,3.55992787221662,1.15662602949913));
#55353=CARTESIAN_POINT('Ctrl Pts',(-0.782573926460673,5.32948788378904,
1.31491635207978));
#55354=CARTESIAN_POINT('Ctrl Pts',(-4.89520921664203,2.24765635443844,1.47320667466042));
#55355=CARTESIAN_POINT('Ctrl Pts',(-4.55199003572729,-2.88008061968337,
1.63149699724107));
#55356=CARTESIAN_POINT('Ctrl Pts',(-0.065183991559061,-5.3862048034504,
1.78978731982171));
#55357=CARTESIAN_POINT('Ctrl Pts',(4.48092931792725,-2.98941747567865,1.94807764240236));
#55358=CARTESIAN_POINT('Ctrl Pts',(4.94820750367398,2.12853353389945,2.106367964983));
#55359=CARTESIAN_POINT('Ctrl Pts',(0.911279814041717,5.30895206133591,2.26465828756365));
#55360=CARTESIAN_POINT('Ctrl Pts',(-3.95515338400782,3.6567952418446,2.42294861014429));
#55361=CARTESIAN_POINT('Ctrl Pts',(-5.22133641495353,-1.32402639911015,
2.58123893272494));
#55362=CARTESIAN_POINT('Ctrl Pts',(-1.73469936830376,-5.09962898552972,
2.73952925530558));
#55363=CARTESIAN_POINT('Ctrl Pts',(3.33097961086378,-4.23319867095506,2.89781957788623));
#55364=CARTESIAN_POINT('Ctrl Pts',(5.36457248168994,0.486579606504366,3.05610990046687));
#55365=CARTESIAN_POINT('Ctrl Pts',(2.51496289908231,4.7634398099498,3.21440022304752));
#55366=CARTESIAN_POINT('Ctrl Pts',(-2.62393855438374,4.70428990453067,3.37269054562815));
#55367=CARTESIAN_POINT('Ctrl Pts',(-5.37435097263271,0.362972276814471,
3.53098086820881));
#55368=CARTESIAN_POINT('Ctrl Pts',(-3.23266001645341,-4.30874765972506,
3.68927119078945));
#55369=CARTESIAN_POINT('Ctrl Pts',(1.85162008603739,-5.05834955487095,3.8475615133701));
#55370=CARTESIAN_POINT('Ctrl Pts',(5.25042842768707,-1.20349429439626,4.00585183595074));
#55371=CARTESIAN_POINT('Ctrl Pts',(3.86993622505047,3.74686412786792,4.16414215853139));
#55372=CARTESIAN_POINT('Ctrl Pts',(-1.03323770545266,5.28656949465716,4.32243248111203));
#55373=CARTESIAN_POINT('Ctrl Pts',(-4.9958877171557,2.01407623967397,4.48072280369268));
#55374=CARTESIAN_POINT('Ctrl Pts',(-4.41093762324043,-3.09176753064878,
4.63901312627333));
#55375=CARTESIAN_POINT('Ctrl Pts',(0.18915082721592,-5.38327215959954,4.79730344885396));
#55376=CARTESIAN_POINT('Ctrl Pts',(4.61706120446174,-2.77455275936658,4.95559377143462));
#55377=CARTESIAN_POINT('Ctrl Pts',(4.84220538518603,2.3597551117919,5.11388409401526));
#55378=CARTESIAN_POINT('Ctrl Pts',(0.65964167385663,5.34605181812708,5.2721744165959));
#55379=CARTESIAN_POINT('Ctrl Pts',(-4.12337319156663,3.46600500621685,5.43046473917655));
#55380=CARTESIAN_POINT('Ctrl Pts',(-5.15301059511283,-1.56903759886758,
5.58875506175719));
#55381=CARTESIAN_POINT('Ctrl Pts',(-1.49202385918035,-5.17583442390216,
5.74704538433784));
#55382=CARTESIAN_POINT('Ctrl Pts',(3.52710546182805,-4.07123129300759,5.90533570691848));
#55383=CARTESIAN_POINT('Ctrl Pts',(5.33562115874398,0.739286162712621,6.06362602949913));
#55384=CARTESIAN_POINT('Ctrl Pts',(2.28728803992556,4.87685458081641,6.22191635207978));
#55385=CARTESIAN_POINT('Ctrl Pts',(-2.84309173802532,4.5751750293502,6.38020667466042));
#55386=CARTESIAN_POINT('Ctrl Pts',(-5.38549415963294,0.108856954651256,
6.53849699724107));
#55387=CARTESIAN_POINT('Ctrl Pts',(-3.02564993494416,-4.45655019619314,
6.6967873198217));
#55388=CARTESIAN_POINT('Ctrl Pts',(2.08834865456124,-4.96529929379983,6.85507764240235));
#55389=CARTESIAN_POINT('Ctrl Pts',(5.30138887614994,-0.954291969918219,
7.013367964983));
#55390=CARTESIAN_POINT('Ctrl Pts',(3.68874085660779,3.92537744335614,7.17165828756364));
#55391=CARTESIAN_POINT('Ctrl Pts',(-1.28165242406652,5.23189872263419,7.32994861014429));
#55392=CARTESIAN_POINT('Ctrl Pts',(-5.08539764768935,1.77598647092042,7.48823893272493));
#55393=CARTESIAN_POINT('Ctrl Pts',(-4.26006468006067,-3.2965506369107,7.64652925530558));
#55394=CARTESIAN_POINT('Ctrl Pts',(0.443071729890745,-5.36834095621621,
7.80481957788623));
#55395=CARTESIAN_POINT('Ctrl Pts',(4.74289382224317,-2.55349865301401,7.96310990046686));
#55396=CARTESIAN_POINT('Ctrl Pts',(4.7254082275668,2.58571349202899,8.12140022304752));
#55397=CARTESIAN_POINT('Ctrl Pts',(0.406531535002743,5.37123163632562,8.27969054562816));
#55398=CARTESIAN_POINT('Ctrl Pts',(-4.28239808028453,3.26748586255429,8.43798086820882));
#55399=CARTESIAN_POINT('Ctrl Pts',(-5.07319485856352,-1.81054994602781,
8.59627119078944));
#55400=CARTESIAN_POINT('Ctrl Pts',(-1.24602126231025,-5.24049884971722,
8.7545615133701));
#55401=CARTESIAN_POINT('Ctrl Pts',(3.71536646050538,-3.90018579610877,8.91285183595074));
#55402=CARTESIAN_POINT('Ctrl Pts',(5.29477246894171,0.99034422407249,9.07114215853139));
#55403=CARTESIAN_POINT('Ctrl Pts',(2.05451294448632,4.97939491715156,9.22943248111203));
#55404=CARTESIAN_POINT('Ctrl Pts',(-3.05590536082404,4.43585838431568,9.38772280369268));
#55405=CARTESIAN_POINT('Ctrl Pts',(-5.38462873481541,-0.145501093525492,
9.54601312627332));
#55406=CARTESIAN_POINT('Ctrl Pts',(-2.81189323161436,-4.59441548339048,
9.70430344885398));
#55407=CARTESIAN_POINT('Ctrl Pts',(2.32042060475949,-4.86117736736937,9.8625937714346));
#55408=CARTESIAN_POINT('Ctrl Pts',(5.34052824602817,-0.702961758129157,
10.0208840940153));
#55409=CARTESIAN_POINT('Ctrl Pts',(3.49932030370932,4.09513792100639,10.1791744165959));
#55410=CARTESIAN_POINT('Ctrl Pts',(-1.52720930356618,5.16556182066556,10.3374647391766));
#55411=CARTESIAN_POINT('Ctrl Pts',(-5.16356811784049,1.53393659335643,10.4957550617572));
#55412=CARTESIAN_POINT('Ctrl Pts',(-4.09969261038038,-3.49398306813431,
10.6540453843378));
#55413=CARTESIAN_POINT('Ctrl Pts',(0.69600466762893,-5.34143938303671,10.8123357069185));
#55414=CARTESIAN_POINT('Ctrl Pts',(4.85815069731172,-2.32675073487178,10.9706260294991));
#55415=CARTESIAN_POINT('Ctrl Pts',(4.59807431672593,2.80590622756395,11.1289163520798));
#55416=CARTESIAN_POINT('Ctrl Pts',(0.152514908872657,5.38443463908592,11.2872066746604));
#55417=CARTESIAN_POINT('Ctrl Pts',(-4.43187404337698,3.0616808526785,11.4454969972411));
#55418=CARTESIAN_POINT('Ctrl Pts',(-4.98206687137828,-2.04802511438014,
11.6037873198217));
#55419=CARTESIAN_POINT('Ctrl Pts',(-0.997240277224328,-5.29347796911429,
11.7620776424023));
#55420=CARTESIAN_POINT('Ctrl Pts',(3.89534290521418,-3.72044363360263,11.920367964983));
#55421=CARTESIAN_POINT('Ctrl Pts',(5.24211745296974,1.2391940079289,12.0786582875636));
#55422=CARTESIAN_POINT('Ctrl Pts',(1.81715667958537,5.07083215871469,12.2369486101443));
#55423=CARTESIAN_POINT('Ctrl Pts',(-3.26190490130962,4.28665062663486,12.3952389327249));
#55424=CARTESIAN_POINT('Ctrl Pts',(-5.37175662160512,-0.399534702195488,
12.5535292553056));
#55425=CARTESIAN_POINT('Ctrl Pts',(-2.59186654617659,-4.72203610604869,
12.7118195778862));
#55426=CARTESIAN_POINT('Ctrl Pts',(2.5473184624597,-4.74621594860878,12.8701099004669));
#55427=CARTESIAN_POINT('Ctrl Pts',(5.36775926313778,-0.450064076566892,
13.0284002230475));
#55428=CARTESIAN_POINT('Ctrl Pts',(3.30209693829715,4.25576702723554,13.1866905456282));
#55429=CARTESIAN_POINT('Ctrl Pts',(-1.76936079949669,5.08770670746843,13.3449808682088));
#55430=CARTESIAN_POINT('Ctrl Pts',(-5.23022482233823,1.28846633165889,13.5032711907894));
#55431=CARTESIAN_POINT('Ctrl Pts',(-3.93017901319522,-3.68362458785553,
13.6615615133701));
#55432=CARTESIAN_POINT('Ctrl Pts',(0.947385648568746,-5.30262742542707,
13.8198518359507));
#55433=CARTESIAN_POINT('Ctrl Pts',(4.96257482894607,-2.09481460925815,13.9781421585314));
#55434=CARTESIAN_POINT('Ctrl Pts',(4.46048758284477,3.01984233086364,14.136432481112));
#55435=CARTESIAN_POINT('Ctrl Pts',(-0.101841796215968,5.38563138624398,
14.2947228036927));
#55436=CARTESIAN_POINT('Ctrl Pts',(-4.57146777815769,2.84904888226236,14.4530131262733));
#55437=CARTESIAN_POINT('Ctrl Pts',(-4.87982983143951,-2.28093357990735,
14.611303448854));
#55438=CARTESIAN_POINT('Ctrl Pts',(-0.746235637830062,-5.33465364878775,
14.7695937714346));
#55439=CARTESIAN_POINT('Ctrl Pts',(4.06663348316603,-3.53240559608313,14.9278840940153));
#55440=CARTESIAN_POINT('Ctrl Pts',(5.17777352115031,1.48528062718241,15.0861744165959));
#55441=CARTESIAN_POINT('Ctrl Pts',(1.57574850461626,5.15096241772943,15.2444647391765));
#55442=CARTESIAN_POINT('Ctrl Pts',(-3.46063102098561,4.12788446150094,15.4027550617572));
#55443=CARTESIAN_POINT('Ctrl Pts',(-5.34690652055963,-0.652677426204677,
15.5610453843378));
#55444=CARTESIAN_POINT('Ctrl Pts',(-2.36606049931089,-4.83912749271637,
15.7193357069185));
#55445=CARTESIAN_POINT('Ctrl Pts',(2.76853629551539,-4.62067138316371,15.8776260294991));
#55446=CARTESIAN_POINT('Ctrl Pts',(5.3830211950772,-0.196162831342301,16.0359163520798));
#55447=CARTESIAN_POINT('Ctrl Pts',(3.09751055443537,4.406906576266,16.1942066746604));
#55448=CARTESIAN_POINT('Ctrl Pts',(-2.00756700604201,4.99850701120068,16.3524969972411));
#55449=CARTESIAN_POINT('Ctrl Pts',(-5.28521904248542,1.04012298730266,16.5107873198217));
#55450=CARTESIAN_POINT('Ctrl Pts',(-3.75190203767367,-3.86505223614748,
16.6690776424023));
#55451=CARTESIAN_POINT('Ctrl Pts',(1.19665445944501,-5.25199180962336,16.827367964983));
#55452=CARTESIAN_POINT('Ctrl Pts',(5.05593276337192,-1.85820709934824,16.9856582875636));
#55453=CARTESIAN_POINT('Ctrl Pts',(4.31295598018285,3.22704409670023,17.1439486101443));
#55454=CARTESIAN_POINT('Ctrl Pts',(-0.355973635386551,5.37482048772419,
17.3022389327249));
#55455=CARTESIAN_POINT('Ctrl Pts',(-4.70086377034365,2.63006163593618,17.4605292553056));
#55456=CARTESIAN_POINT('Ctrl Pts',(-4.76671982630963,-2.50875132983212,
17.6188195778862));
#55457=CARTESIAN_POINT('Ctrl Pts',(-0.493551516935001,-5.36394300504465,
17.7771099004669));
#55458=CARTESIAN_POINT('Ctrl Pts',(4.22882658272939,-3.33647390152326,17.9354002230475));
#55459=CARTESIAN_POINT('Ctrl Pts',(5.10194085814736,1.72802272375016,18.0936905456282));
#55460=CARTESIAN_POINT('Ctrl Pts',(1.3307183071549,5.21966939828879,18.2519808682088));
#55461=CARTESIAN_POINT('Ctrl Pts',(-3.65143336771916,3.95979466293823,18.4102711907895));
#55462=CARTESIAN_POINT('Ctrl Pts',(-5.31053001253145,-0.904136851324141,
18.5685615133701));
#55463=CARTESIAN_POINT('Ctrl Pts',(-2.13422101028107,-4.94586439271395,
18.7268518359507));
#55464=CARTESIAN_POINT('Ctrl Pts',(2.98213020961523,-4.48398969368682,18.8851421585314));
#55465=CARTESIAN_POINT('Ctrl Pts',(5.3890746734895,0.056574848876316,19.043432481112));
#55466=CARTESIAN_POINT('Ctrl Pts',(2.88048207978671,4.55134095987183,19.2017228036927));
#55467=CARTESIAN_POINT('Ctrl Pts',(-1.3774178436033,4.83495951916122,19.3336314058432));
#55468=CARTESIAN_POINT('Ctrl Pts',(-3.79805473803742,2.8466873735715,19.4391582875636));
#55469=CARTESIAN_POINT('Ctrl Pts',(-4.40190912913332,1.41664485531417,19.4919217284239));
#55470=CARTESIAN_POINT('Ctrl Pts',(-4.51273837831629,0.668607754121397,
19.518303448854));
#55471=CARTESIAN_POINT('Ctrl Pts',(2.53835875722687,-3.55965150255045,-1.94289029309402E-15));
#55472=CARTESIAN_POINT('Ctrl Pts',(3.1284109977952,-3.13889001199587,0.0263817204301056));
#55473=CARTESIAN_POINT('Ctrl Pts',(4.08550837253979,-1.9999918568306,0.0791451612903207));
#55474=CARTESIAN_POINT('Ctrl Pts',(4.72679975347169,0.932772746710439,0.184672043010751));
#55475=CARTESIAN_POINT('Ctrl Pts',(2.62811439332184,4.44281702219704,0.316580645161289));
#55476=CARTESIAN_POINT('Ctrl Pts',(-2.3016075840404,4.62373529115294,0.474870967741933));
#55477=CARTESIAN_POINT('Ctrl Pts',(-5.12700989483103,0.589736901013719,
0.633161290322578));
#55478=CARTESIAN_POINT('Ctrl Pts',(-3.29020762976984,-3.97798440336088,
0.791451612903224));
#55479=CARTESIAN_POINT('Ctrl Pts',(1.54404435335689,-4.92628156041988,0.949741935483869));
#55480=CARTESIAN_POINT('Ctrl Pts',(4.97150648183897,-1.38949747849925,1.10803225806451));
#55481=CARTESIAN_POINT('Ctrl Pts',(3.87423912778238,3.41166257284768,1.26632258064516));
#55482=CARTESIAN_POINT('Ctrl Pts',(-0.749980974679123,5.10752324154442,
1.42461290322581));
#55483=CARTESIAN_POINT('Ctrl Pts',(-4.69133158596208,2.15404506392038,1.58290322580645));
#55484=CARTESIAN_POINT('Ctrl Pts',(-4.36240693472153,-2.76012987050762,
1.7411935483871));
#55485=CARTESIAN_POINT('Ctrl Pts',(-0.0624691826164238,-5.16187799225891,
1.89948387096774));
#55486=CARTESIAN_POINT('Ctrl Pts',(4.29430578210828,-2.8649130214088,2.05777419354839));
#55487=CARTESIAN_POINT('Ctrl Pts',(4.74212257914569,2.03988351823947,2.21606451612903));
#55488=CARTESIAN_POINT('Ctrl Pts',(0.873326467994359,5.08784270323556,2.37435483870968));
#55489=CARTESIAN_POINT('Ctrl Pts',(-3.7904275745029,3.50449557153541,2.53264516129032));
#55490=CARTESIAN_POINT('Ctrl Pts',(-5.00387610832461,-1.26888281826166,
2.69093548387097));
#55491=CARTESIAN_POINT('Ctrl Pts',(-1.66245191543707,-4.88723759858308,
2.84922580645161));
#55492=CARTESIAN_POINT('Ctrl Pts',(3.19224964022283,-4.05689272016998,3.00751612903226));
#55493=CARTESIAN_POINT('Ctrl Pts',(5.14114662208426,0.466314344506177,3.1658064516129));
#55494=CARTESIAN_POINT('Ctrl Pts',(2.41021871871718,4.56505016420442,3.32409677419355));
#55495=CARTESIAN_POINT('Ctrl Pts',(-2.5146557123555,4.50836375769575,3.48238709677419));
#55496=CARTESIAN_POINT('Ctrl Pts',(-5.15051785452657,0.347855062304423,
3.64067741935484));
#55497=CARTESIAN_POINT('Ctrl Pts',(-3.09802489959102,-4.12929521444937,
3.79896774193548));
#55498=CARTESIAN_POINT('Ctrl Pts',(1.77450307237079,-4.84767739015689,3.95725806451612));
#55499=CARTESIAN_POINT('Ctrl Pts',(5.03175648528012,-1.15337068283656,4.11554838709677));
#55500=CARTESIAN_POINT('Ctrl Pts',(3.7087595738537,3.5908132325819,4.27383870967742));
#55501=CARTESIAN_POINT('Ctrl Pts',(-0.990205008382098,5.06639233464293,
4.43212903225806));
#55502=CARTESIAN_POINT('Ctrl Pts',(-4.7878169880326,1.93019318716672,4.59041935483871));
#55503=CARTESIAN_POINT('Ctrl Pts',(-4.22722912950617,-2.96300036036751,
4.74870967741935));
#55504=CARTESIAN_POINT('Ctrl Pts',(0.181272997936893,-5.15906748833169,
4.907));
#55505=CARTESIAN_POINT('Ctrl Pts',(4.4247679934035,-2.65899707670991,5.06529032258064));
#55506=CARTESIAN_POINT('Ctrl Pts',(4.64053527927078,2.26147508740778,5.22358064516129));
#55507=CARTESIAN_POINT('Ctrl Pts',(0.63216865368283,5.12339731452249,5.38187096774192));
#55508=CARTESIAN_POINT('Ctrl Pts',(-3.95164129625807,3.32165144392371,5.54016129032259));
#55509=CARTESIAN_POINT('Ctrl Pts',(-4.93839594954698,-1.50368969361007,
5.69845161290321));
#55510=CARTESIAN_POINT('Ctrl Pts',(-1.42988345294528,-4.96026920238937,
5.85674193548387));
#55511=CARTESIAN_POINT('Ctrl Pts',(3.38020716333018,-3.90167102433782,6.01503225806451));
#55512=CARTESIAN_POINT('Ctrl Pts',(5.11340107541181,0.708496077023162,6.17332258064516));
#55513=CARTESIAN_POINT('Ctrl Pts',(2.19202615312461,4.67374139134797,6.3316129032258));
#55514=CARTESIAN_POINT('Ctrl Pts',(-2.72468151658193,4.38462631046011,6.48990322580645));
#55515=CARTESIAN_POINT('Ctrl Pts',(-5.16119694561929,0.104323236680228,
6.64819354838708));
#55516=CARTESIAN_POINT('Ctrl Pts',(-2.8996364567242,-4.27094201178353,6.80648387096775));
#55517=CARTESIAN_POINT('Ctrl Pts',(2.00137227482285,-4.75850252356265,6.96477419354837));
#55518=CARTESIAN_POINT('Ctrl Pts',(5.08059451261016,-0.914547236405604,
7.12306451612904));
#55519=CARTESIAN_POINT('Ctrl Pts',(3.53511070256229,3.76189175413264,7.28135483870967));
#55520=CARTESIAN_POINT('Ctrl Pts',(-1.22827365147281,5.01399851279189,7.43964516129032));
#55521=CARTESIAN_POINT('Ctrl Pts',(-4.87359897319111,1.70201947629637,7.59793548387097));
#55522=CARTESIAN_POINT('Ctrl Pts',(-4.08263980298667,-3.1592545779425,7.75622580645161));
#55523=CARTESIAN_POINT('Ctrl Pts',(0.424618501333285,-5.14475814567673,
7.91451612903225));
#55524=CARTESIAN_POINT('Ctrl Pts',(4.54535988400859,-2.44714952016159,8.0728064516129));
#55525=CARTESIAN_POINT('Ctrl Pts',(4.52860253637045,2.47802266268103,8.23109677419354));
#55526=CARTESIAN_POINT('Ctrl Pts',(0.389600147091602,5.14752843358518,8.38938709677419));
#55527=CARTESIAN_POINT('Ctrl Pts',(-4.10404305282859,3.13140030492926,8.54767741935484));
#55528=CARTESIAN_POINT('Ctrl Pts',(-4.86190441070575,-1.73514343797319,
8.70596774193548));
#55529=CARTESIAN_POINT('Ctrl Pts',(-1.19412647058753,-5.02224045834365,
8.86425806451613));
#55530=CARTESIAN_POINT('Ctrl Pts',(3.56062739266322,-3.73774929868204,9.02254838709676));
#55531=CARTESIAN_POINT('Ctrl Pts',(5.07425366817473,0.949097971864315,9.18083870967742));
#55532=CARTESIAN_POINT('Ctrl Pts',(1.96894576792944,4.77201108675727,9.33912903225805));
#55533=CARTESIAN_POINT('Ctrl Pts',(-2.9286317925302,4.25111198076021,9.4974193548387));
#55534=CARTESIAN_POINT('Ctrl Pts',(-5.16036756436058,-0.139441205807441,
9.65570967741936));
#55535=CARTESIAN_POINT('Ctrl Pts',(-2.69478237803987,-4.40306543037773,
9.81399999999999));
#55536=CARTESIAN_POINT('Ctrl Pts',(2.22377879965116,-4.65871710875468,9.97229032258064));
#55537=CARTESIAN_POINT('Ctrl Pts',(5.11810379036282,-0.67368452576514,10.1305806451613));
#55538=CARTESIAN_POINT('Ctrl Pts',(3.35357921258595,3.92458197953528,10.2888709677419));
#55539=CARTESIAN_POINT('Ctrl Pts',(-1.46360347987537,4.95042443663959,10.4471612903226));
#55540=CARTESIAN_POINT('Ctrl Pts',(-4.94851376834693,1.47005058881065,10.6054516129032));
#55541=CARTESIAN_POINT('Ctrl Pts',(-3.92894697338513,-3.34846426433215,
10.7637419354839));
#55542=CARTESIAN_POINT('Ctrl Pts',(0.667017186951725,-5.11897697997292,
10.9220322580645));
#55543=CARTESIAN_POINT('Ctrl Pts',(4.65581649466175,-2.22984528997355,11.0803225806452));
#55544=CARTESIAN_POINT('Ctrl Pts',(4.40657187915952,2.68904472312794,11.2386129032258));
#55545=CARTESIAN_POINT('Ctrl Pts',(0.14616290696869,5.16018155240764,11.3969032258064));
#55546=CARTESIAN_POINT('Ctrl Pts',(-4.24729358124599,2.93416674439068,11.5551935483871));
#55547=CARTESIAN_POINT('Ctrl Pts',(-4.77457175836603,-1.96272814556555,
11.7134838709677));
#55548=CARTESIAN_POINT('Ctrl Pts',(-0.955706815437237,-5.07301308219371,
11.8717741935484));
#55549=CARTESIAN_POINT('Ctrl Pts',(3.73310810644377,-3.5654931096253,12.030064516129));
#55550=CARTESIAN_POINT('Ctrl Pts',(5.02379164936073,1.1875835604264,12.1883548387097));
#55551=CARTESIAN_POINT('Ctrl Pts',(1.74147501164997,4.85964011352491,12.3466451612903));
#55552=CARTESIAN_POINT('Ctrl Pts',(-3.12605178178994,4.10811848742822,12.504935483871));
#55553=CARTESIAN_POINT('Ctrl Pts',(-5.14803155406786,-0.382894721174656,
12.6632258064516));
#55554=CARTESIAN_POINT('Ctrl Pts',(-2.4839194519693,-4.5253708583176,12.8215161290323));
#55555=CARTESIAN_POINT('Ctrl Pts',(2.44122672465452,-4.54854364912704,12.9798064516129));
#55556=CARTESIAN_POINT('Ctrl Pts',(5.14420067918421,-0.431319627959304,
13.1380967741936));
#55557=CARTESIAN_POINT('Ctrl Pts',(3.16456988475122,4.07852114052473,13.2963870967742));
#55558=CARTESIAN_POINT('Ctrl Pts',(-1.69566975348524,4.87581186432528,13.4546774193548));
#55559=CARTESIAN_POINT('Ctrl Pts',(-5.01239432776474,1.23480377071736,13.6129677419355));
#55560=CARTESIAN_POINT('Ctrl Pts',(-3.76649334627126,-3.53020751821668,
13.7712580645161));
#55561=CARTESIAN_POINT('Ctrl Pts',(0.907928552289056,-5.08178147829179,
13.9295483870968));
#55562=CARTESIAN_POINT('Ctrl Pts',(4.75589152831045,-2.00756893285326,14.0878387096774));
#55563=CARTESIAN_POINT('Ctrl Pts',(4.2747154125816,2.89407073006048,14.2461290322581));
#55564=CARTESIAN_POINT('Ctrl Pts',(-0.0976002483683332,5.16132845696157,
14.4044193548387));
#55565=CARTESIAN_POINT('Ctrl Pts',(-4.38107346034753,2.73039055529394,14.5627096774194));
#55566=CARTESIAN_POINT('Ctrl Pts',(-4.67659272754351,-2.18593634619795,
14.721));
#55567=CARTESIAN_POINT('Ctrl Pts',(-0.715156117622299,-5.11247386069707,
14.8792903225806));
#55568=CARTESIAN_POINT('Ctrl Pts',(3.89726470591888,-3.38528655547465,15.0375806451613));
#55569=CARTESIAN_POINT('Ctrl Pts',(4.96212753934002,1.42342106576975,15.1958709677419));
#55570=CARTESIAN_POINT('Ctrl Pts',(1.5101211008729,4.93643307547415,15.3541612903226));
#55571=CARTESIAN_POINT('Ctrl Pts',(-3.31650127657807,3.95596467901843,15.5124516129032));
#55572=CARTESIAN_POINT('Ctrl Pts',(-5.1242164199664,-0.62549445580161,15.6707419354839));
#55573=CARTESIAN_POINT('Ctrl Pts',(-2.26751786562628,-4.63758557609733,
15.8290322580645));
#55574=CARTESIAN_POINT('Ctrl Pts',(2.65323118895075,-4.42822781393943,15.9873225806452));
#55575=CARTESIAN_POINT('Ctrl Pts',(5.15882697608013,-0.187992963311806,
16.1456129032258));
#55576=CARTESIAN_POINT('Ctrl Pts',(2.96850419640318,4.22336596918787,16.3039032258064));
#55577=CARTESIAN_POINT('Ctrl Pts',(-1.92395505269964,4.79032719267193,16.4621935483871));
#55578=CARTESIAN_POINT('Ctrl Pts',(-5.06509812664321,0.99680352926066,16.6204838709677));
#55579=CARTESIAN_POINT('Ctrl Pts',(-3.59564132150574,-3.70407899527331,
16.7787741935484));
#55580=CARTESIAN_POINT('Ctrl Pts',(1.14681571606612,-5.03325475486043,16.937064516129));
#55581=CARTESIAN_POINT('Ctrl Pts',(4.84536125415653,-1.78081574711759,17.0953548387097));
#55582=CARTESIAN_POINT('Ctrl Pts',(4.13332826509411,3.09264287390914,17.2536451612903));
#55583=CARTESIAN_POINT('Ctrl Pts',(-0.341147903092961,5.15096781506579,
17.411935483871));
#55584=CARTESIAN_POINT('Ctrl Pts',(-4.50508031651524,2.52052377735926,17.5702258064516));
#55585=CARTESIAN_POINT('Ctrl Pts',(-4.56819357313145,-2.40426585138671,
17.7285161290323));
#55586=CARTESIAN_POINT('Ctrl Pts',(-0.472995886023615,-5.14054336213398,
17.8868064516129));
#55587=CARTESIAN_POINT('Ctrl Pts',(4.05270272242283,-3.19751510246813,18.0450967741935));
#55588=CARTESIAN_POINT('Ctrl Pts',(4.88945318540557,1.65605334244537,18.2033870967742));
#55589=CARTESIAN_POINT('Ctrl Pts',(1.27529601904452,5.00227852023644,18.3616774193548));
#55590=CARTESIAN_POINT('Ctrl Pts',(-3.49935701088739,3.79487555159269,18.5199677419355));
#55591=CARTESIAN_POINT('Ctrl Pts',(-5.0893549352888,-0.866480998244023,
18.6782580645161));
#55592=CARTESIAN_POINT('Ctrl Pts',(-2.04533412033072,-4.73987705500777,
18.8365483870968));
#55593=CARTESIAN_POINT('Ctrl Pts',(2.85792925831606,-4.29723869811459,18.9948387096774));
#55594=CARTESIAN_POINT('Ctrl Pts',(5.16462833680317,0.0542185969503185,
19.1531290322581));
#55595=CARTESIAN_POINT('Ctrl Pts',(2.76051461044002,4.36178489183685,19.3114193548387));
#55596=CARTESIAN_POINT('Ctrl Pts',(-1.32005059452733,4.63359119197125,19.4433279569892));
#55597=CARTESIAN_POINT('Ctrl Pts',(-3.63987183575178,2.72812739966123,19.5488548387097));
#55598=CARTESIAN_POINT('Ctrl Pts',(-4.21857665773145,1.35764386397051,19.6016182795699));
#55599=CARTESIAN_POINT('Ctrl Pts',(-4.32479004603219,0.640761311051878,
19.628));
#55600=CARTESIAN_POINT('',(2.53835875722687,-3.55965150255045,0.));
#55601=CARTESIAN_POINT('Ctrl Pts',(2.53835875722687,-3.55965150255045,-1.94289029309402E-15));
#55602=CARTESIAN_POINT('Ctrl Pts',(3.1284109977952,-3.13889001199587,0.0263817204301056));
#55603=CARTESIAN_POINT('Ctrl Pts',(4.08550837253979,-1.9999918568306,0.0791451612903207));
#55604=CARTESIAN_POINT('Ctrl Pts',(4.72679975347169,0.932772746710439,0.184672043010751));
#55605=CARTESIAN_POINT('Ctrl Pts',(2.62811439332184,4.44281702219704,0.316580645161289));
#55606=CARTESIAN_POINT('Ctrl Pts',(-2.3016075840404,4.62373529115294,0.474870967741933));
#55607=CARTESIAN_POINT('Ctrl Pts',(-4.29378651801925,1.77938049543143,0.58648078871983));
#55608=CARTESIAN_POINT('Ctrl Pts',(-4.37763907935493,0.169045277724475,
0.645327168837512));
#55609=CARTESIAN_POINT('Ctrl Pts',(-4.37640441740291,0.00246357316762608,
0.651410108094978));
#55610=CARTESIAN_POINT('Ctrl Pts',(2.17571852337094,4.44456444733847,4.16333634234434E-17));
#55611=CARTESIAN_POINT('Ctrl Pts',(2.288553758881,4.38223977042994,4.80899030934479E-17));
#55612=CARTESIAN_POINT('Ctrl Pts',(2.39856816217823,4.31535914976362,1.26999648448827E-16));
#55613=CARTESIAN_POINT('Ctrl Pts',(2.50544378309707,4.24391302988421,1.37043154602168E-16));
#55614=CARTESIAN_POINT('Ctrl Pts',(2.62554044419194,4.16362867343386,1.45788230031228E-16));
#55615=CARTESIAN_POINT('Ctrl Pts',(2.7416747038151,4.07757963945051,2.86902645733316E-16));
#55616=CARTESIAN_POINT('Ctrl Pts',(2.85366454038282,3.98618686426695,3.64291929955129E-16));
#55617=CARTESIAN_POINT('Ctrl Pts',(2.9232629976869,3.92938888726778,4.12387140724083E-16));
#55618=CARTESIAN_POINT('Ctrl Pts',(2.99126006746036,3.87052620415169,6.62527936102846E-16));
#55619=CARTESIAN_POINT('Ctrl Pts',(3.05760444128136,3.80969336998723,7.21644966006352E-16));
#55620=CARTESIAN_POINT('Ctrl Pts',(3.09753791324214,3.7730773596537,7.57228213237312E-16));
#55621=CARTESIAN_POINT('Ctrl Pts',(3.13687250045182,3.73574748028041,-2.48343235400226E-16));
#55622=CARTESIAN_POINT('Ctrl Pts',(3.17559590361344,3.69772367591327,-3.60822483003176E-16));
#55623=CARTESIAN_POINT('Ctrl Pts',(3.19355313598542,3.68009086900739,-4.12982567637309E-16));
#55624=CARTESIAN_POINT('Ctrl Pts',(3.21137384475144,3.66231375739153,2.85386760819859E-16));
#55625=CARTESIAN_POINT('Ctrl Pts',(3.22905135321198,3.64440041383412,2.77555756156289E-16));
#55626=CARTESIAN_POINT('Ctrl Pts',(3.33032953777236,3.54177108012739,2.32690274271181E-16));
#55627=CARTESIAN_POINT('Ctrl Pts',(3.42697009782031,3.4346145361773,1.17947475774344E-16));
#55628=CARTESIAN_POINT('Ctrl Pts',(3.51879473621821,3.32334962039163,1.38777878078145E-16));
#55629=CARTESIAN_POINT('Ctrl Pts',(3.60865605635445,3.21446367875555,1.59162901995989E-16));
#55630=CARTESIAN_POINT('Ctrl Pts',(3.69390536375717,3.10164237133953,1.64416256607793E-16));
#55631=CARTESIAN_POINT('Ctrl Pts',(3.77433601631748,2.9852523894932,1.52655665885959E-16));
#55632=CARTESIAN_POINT('Ctrl Pts',(3.80952442681261,2.93433177243543,1.47510407445157E-16));
#55633=CARTESIAN_POINT('Ctrl Pts',(3.84378998451378,2.88272782098782,-1.03604202083645E-16));
#55634=CARTESIAN_POINT('Ctrl Pts',(3.87711279910771,2.83047021492504,-1.52655665885959E-16));
#55635=CARTESIAN_POINT('Ctrl Pts',(3.90167945166607,2.79194422402902,-1.88817985407716E-16));
#55636=CARTESIAN_POINT('Ctrl Pts',(3.92573367987553,2.75306295204808,1.37038491228682E-16));
#55637=CARTESIAN_POINT('Ctrl Pts',(3.94926693181774,2.71383814709955,1.2490009027033E-16));
#55638=CARTESIAN_POINT('Ctrl Pts',(3.95979885299727,2.69628372856808,1.19467747878689E-16));
#55639=CARTESIAN_POINT('Ctrl Pts',(3.97022193097802,2.67866796640904,3.81603872600368E-16));
#55640=CARTESIAN_POINT('Ctrl Pts',(3.98053410416003,2.66099477842828,3.7470027081099E-16));
#55641=CARTESIAN_POINT('Ctrl Pts',(4.05311436653015,2.53660541859884,3.26110587499023E-16));
#55642=CARTESIAN_POINT('Ctrl Pts',(4.12023044721824,2.40933003202768,5.80264781591426E-16));
#55643=CARTESIAN_POINT('Ctrl Pts',(4.1817056161975,2.27957303631144,5.41233724504764E-16));
#55644=CARTESIAN_POINT('Ctrl Pts',(4.24306352883745,2.15006353613803,5.02277114368784E-16));
#55645=CARTESIAN_POINT('Ctrl Pts',(4.29880233786649,2.01808110524174,-2.01806554237873E-16));
#55646=CARTESIAN_POINT('Ctrl Pts',(4.34869895497134,1.88400727320529,-2.08166817117217E-16));
#55647=CARTESIAN_POINT('Ctrl Pts',(4.3987130094648,1.74961788308838,-2.14542049601851E-16));
#55648=CARTESIAN_POINT('Ctrl Pts',(4.44285769397013,1.61312648052743,2.07700331834603E-16));
#55649=CARTESIAN_POINT('Ctrl Pts',(4.48085566800584,1.47490808725521,2.22044604925031E-16));
#55650=CARTESIAN_POINT('Ctrl Pts',(4.50935414853263,1.37124429230104,2.32802809742852E-16));
#55651=CARTESIAN_POINT('Ctrl Pts',(4.53439405643066,1.26660880723853,3.27090126933202E-16));
#55652=CARTESIAN_POINT('Ctrl Pts',(4.55583718119808,1.16116031586893,3.33066907387547E-16));
#55653=CARTESIAN_POINT('Ctrl Pts',(4.5647459632839,1.1173505800641,3.35550026579367E-16));
#55654=CARTESIAN_POINT('Ctrl Pts',(4.57303368750873,1.073400536371,3.93488937669688E-16));
#55655=CARTESIAN_POINT('Ctrl Pts',(4.58068946156208,1.02932171064127,4.16333634234434E-16));
#55656=CARTESIAN_POINT('Ctrl Pts',(4.58528213032192,1.00287899635937,4.3003807790138E-16));
#55657=CARTESIAN_POINT('Ctrl Pts',(4.58964820129846,0.976383975558462,1.1911498064296E-16));
#55658=CARTESIAN_POINT('Ctrl Pts',(4.59378028021791,0.949872636571533,1.38777878078145E-16));
#55659=CARTESIAN_POINT('Ctrl Pts',(4.61514939077547,0.812768833647209,2.40464858739661E-16));
#55660=CARTESIAN_POINT('Ctrl Pts',(4.63029132458926,0.675091193156248,-6.4053354410212E-17));
#55661=CARTESIAN_POINT('Ctrl Pts',(4.63900152451931,0.537186451104229,-1.38777878078145E-16));
#55662=CARTESIAN_POINT('Ctrl Pts',(4.64607280433788,0.42523000611001,-1.99442159083017E-16));
#55663=CARTESIAN_POINT('Ctrl Pts',(4.64890419840177,0.313123505052828,4.93108554065338E-16));
#55664=CARTESIAN_POINT('Ctrl Pts',(4.64736094433393,0.20105139156818,4.71844785465692E-16));
#55665=CARTESIAN_POINT('Ctrl Pts',(4.64544832051237,0.0621554064876461,
4.17736069944506E-16));
#55666=CARTESIAN_POINT('Ctrl Pts',(4.63681759992347,-0.0766885915146454,
3.72153370275118E-16));
#55667=CARTESIAN_POINT('Ctrl Pts',(4.62166663169142,-0.215038242011895,
4.16333634234434E-16));
#55668=CARTESIAN_POINT('Ctrl Pts',(4.60648817669052,-0.353638885370275,
4.605940496854E-16));
#55669=CARTESIAN_POINT('Ctrl Pts',(4.58476541728463,-0.491744202092864,
1.3585326957315E-16));
#55670=CARTESIAN_POINT('Ctrl Pts',(4.55664910490708,-0.628889846984247,
2.22044604925031E-16));
#55671=CARTESIAN_POINT('Ctrl Pts',(4.54627797904168,-0.679478086507271,
2.53837578891091E-16));
#55672=CARTESIAN_POINT('Ctrl Pts',(4.53503649423606,-0.729935498537829,
-4.17628381648536E-17));
#55673=CARTESIAN_POINT('Ctrl Pts',(4.52293072203927,-0.780237766000663,
-5.55111512312578E-17));
#55674=CARTESIAN_POINT('Ctrl Pts',(4.51852089045776,-0.798561630358381,
-6.05193195799785E-17));
#55675=CARTESIAN_POINT('Ctrl Pts',(4.51399616118864,-0.816865466942453,
-2.76721061431502E-16));
#55676=CARTESIAN_POINT('Ctrl Pts',(4.50936083932464,-0.835132869996713,
-2.77555756156289E-16));
#55677=CARTESIAN_POINT('Ctrl Pts',(4.47555258032973,-0.968368298245966,
-2.83643699187054E-16));
#55678=CARTESIAN_POINT('Ctrl Pts',(4.43581935723855,-1.09986196998026,4.56182438062644E-17));
#55679=CARTESIAN_POINT('Ctrl Pts',(4.39038959840621,-1.229200829575,5.55111512312578E-17));
#55680=CARTESIAN_POINT('Ctrl Pts',(4.34480983538931,-1.35896675219327,6.54367239740816E-17));
#55681=CARTESIAN_POINT('Ctrl Pts',(4.29349546516567,-1.48656440482432,-4.64120495657098E-16));
#55682=CARTESIAN_POINT('Ctrl Pts',(4.23662839209755,-1.61155805192221,-3.05311331771918E-16));
#55683=CARTESIAN_POINT('Ctrl Pts',(4.17976131902944,-1.7365516990201,-1.46502167886738E-16));
#55684=CARTESIAN_POINT('Ctrl Pts',(4.11734114389621,-1.85894212089202,1.98375931461375E-16));
#55685=CARTESIAN_POINT('Ctrl Pts',(4.04950702451708,-1.97826322671605,2.22044604925031E-16));
#55686=CARTESIAN_POINT('Ctrl Pts',(4.0039219578893,-2.05844795689127,2.37950141352824E-16));
#55687=CARTESIAN_POINT('Ctrl Pts',(3.95589106826036,-2.13724588577774,1.34209299017938E-16));
#55688=CARTESIAN_POINT('Ctrl Pts',(3.90547300064698,-2.21455451296583,1.66533453693773E-16));
#55689=CARTESIAN_POINT('Ctrl Pts',(3.88226355505238,-2.25014275467462,1.81413550152313E-16));
#55690=CARTESIAN_POINT('Ctrl Pts',(3.85854814303777,-2.28541527809141,-1.96535868138964E-16));
#55691=CARTESIAN_POINT('Ctrl Pts',(3.8343320388377,-2.32036145673223,-2.22044604925031E-16));
#55692=CARTESIAN_POINT('Ctrl Pts',(3.81846869581275,-2.34325379377416,-2.38754718097135E-16));
#55693=CARTESIAN_POINT('Ctrl Pts',(3.80239048915502,-2.36600608076709,-1.28420314193019E-17));
#55694=CARTESIAN_POINT('Ctrl Pts',(3.78609884210449,-2.38861523157554,0.));
#55695=CARTESIAN_POINT('Ctrl Pts',(3.77490538198125,-2.40414924279059,8.82334156561408E-18));
#55696=CARTESIAN_POINT('Ctrl Pts',(3.76361599384939,-2.41960894071961,1.65364095173029E-16));
#55697=CARTESIAN_POINT('Ctrl Pts',(3.7522346949218,-2.43498912758705,1.66533453693773E-16));
#55698=CARTESIAN_POINT('Ctrl Pts',(3.66941253061457,-2.54691135824948,1.75042922090602E-16));
#55699=CARTESIAN_POINT('Ctrl Pts',(3.58167249725696,-2.65470179052059,3.28026165867355E-16));
#55700=CARTESIAN_POINT('Ctrl Pts',(3.48928766288614,-2.75807107487432,2.22044604925031E-16));
#55701=CARTESIAN_POINT('Ctrl Pts',(3.39991887248819,-2.85806571111424,1.19522973854221E-16));
#55702=CARTESIAN_POINT('Ctrl Pts',(3.30620285470906,-2.9539234934181,-1.0442180859248E-16));
#55703=CARTESIAN_POINT('Ctrl Pts',(3.20834980062004,-3.04534562649001,-1.66533453693773E-16));
#55704=CARTESIAN_POINT('Ctrl Pts',(3.11144260907094,-3.13588405928502,-2.28044718163707E-16));
#55705=CARTESIAN_POINT('Ctrl Pts',(3.01047744826623,-3.22207261031851,3.41219002678743E-16));
#55706=CARTESIAN_POINT('Ctrl Pts',(2.90563068007557,-3.30357847782834,3.33066907387547E-16));
#55707=CARTESIAN_POINT('Ctrl Pts',(2.80291415997029,-3.38342833131688,3.25080444148589E-16));
#55708=CARTESIAN_POINT('Ctrl Pts',(2.69647166403099,-3.45878415557578,1.92670969748543E-16));
#55709=CARTESIAN_POINT('Ctrl Pts',(2.58644978075874,-3.52928668450907,1.66533453693773E-16));
#55710=CARTESIAN_POINT('Ctrl Pts',(2.57049460076127,-3.53951083724989,1.62743037088118E-16));
#55711=CARTESIAN_POINT('Ctrl Pts',(2.5544641189252,-3.54963283815124,3.31276988434876E-16));
#55712=CARTESIAN_POINT('Ctrl Pts',(2.53835875722692,-3.55965150255041,3.33066907387547E-16));
#55713=CARTESIAN_POINT('Ctrl Pts',(0.446494146901359,4.91265885279923,19.058));
#55714=CARTESIAN_POINT('Ctrl Pts',(1.22846295052447,4.84360722676543,19.0327765671335));
#55715=CARTESIAN_POINT('Ctrl Pts',(1.9933030120195,4.59769822736177,19.0075531342671));
#55716=CARTESIAN_POINT('Ctrl Pts',(2.65082820116331,4.18037408759279,18.9823297014006));
#55717=CARTESIAN_POINT('Ctrl Pts',(4.02626712794074,3.307397848204,18.9295662605404));
#55718=CARTESIAN_POINT('Ctrl Pts',(4.93211723740144,1.68434260046616,18.8768028196802));
#55719=CARTESIAN_POINT('Ctrl Pts',(4.95046975302369,0.05301847033729,18.82403937882));
#55720=CARTESIAN_POINT('Ctrl Pts',(4.96882226864594,-1.57830565979157,18.7712759379598));
#55721=CARTESIAN_POINT('Ctrl Pts',(4.09967719042974,-3.21789867231146,18.7185124970995));
#55722=CARTESIAN_POINT('Ctrl Pts',(2.74135016758908,-4.12108640912056,18.6657490562393));
#55723=CARTESIAN_POINT('Ctrl Pts',(1.38302314474846,-5.02427414592964,18.6129856153791));
#55724=CARTESIAN_POINT('Ctrl Pts',(-0.464485822716606,-5.19105660702797,
18.5602221745189));
#55725=CARTESIAN_POINT('Ctrl Pts',(-1.9617212025883,-4.54471608580352,18.5074587336587));
#55726=CARTESIAN_POINT('Ctrl Pts',(-3.45895658246008,-3.89837556457903,
18.4546952927985));
#55727=CARTESIAN_POINT('Ctrl Pts',(-4.60591837473846,-2.43891206103166,
18.4019318519383));
#55728=CARTESIAN_POINT('Ctrl Pts',(-4.87985025660527,-0.831000068739,18.349168411078));
#55729=CARTESIAN_POINT('Ctrl Pts',(-4.92631242249651,-0.558278714746532,
18.340219092271));
#55730=CARTESIAN_POINT('Ctrl Pts',(-4.94765902855038,-0.28128675460715,
18.3312697734639));
#55731=CARTESIAN_POINT('Ctrl Pts',(-4.94522242777803,-0.0039236424385497,
18.3223204546569));
#55732=CARTESIAN_POINT('Origin',(0.,0.,-1.84858989190501));
#55733=CARTESIAN_POINT('',(-2.53835875722683,-3.55965150255047,0.));
#55734=CARTESIAN_POINT('Ctrl Pts',(-2.54467524200888,-3.56229978442276,
-3.12521276218947E-15));
#55735=CARTESIAN_POINT('Ctrl Pts',(-1.45608504857279,-4.32913804450291,
0.0486930492780809));
#55736=CARTESIAN_POINT('Ctrl Pts',(1.60942354292801,-4.84594693373762,0.150182632030869));
#55737=CARTESIAN_POINT('Ctrl Pts',(4.96501177239675,-1.41203703483287,0.304468748258361));
#55738=CARTESIAN_POINT('Ctrl Pts',(3.88934922870828,3.39617009289883,0.462858348682473));
#55739=CARTESIAN_POINT('Ctrl Pts',(-0.732920742143878,5.1113964007393,0.621247949106584));
#55740=CARTESIAN_POINT('Ctrl Pts',(-3.9420462167219,2.72159457156631,0.749825130180767));
#55741=CARTESIAN_POINT('Ctrl Pts',(-4.36729319104836,0.635050406119092,
0.825605777780246));
#55742=CARTESIAN_POINT('Ctrl Pts',(-4.36535621882271,0.0014563306878905,
0.848589891905021));
#55743=CARTESIAN_POINT('Origin',(0.,0.,0.));
#55744=CARTESIAN_POINT('Ctrl Pts',(-1.91898364244012,3.92834389788461,-0.329089653438086));
#55745=CARTESIAN_POINT('Ctrl Pts',(-2.57055919540632,3.61005128897394,-0.302691386700734));
#55746=CARTESIAN_POINT('Ctrl Pts',(-3.7023655534584,2.64307614504004,-0.24989485322603));
#55747=CARTESIAN_POINT('Ctrl Pts',(-4.81630944128875,-0.146849281373132,
-0.144301786276623));
#55748=CARTESIAN_POINT('Ctrl Pts',(-3.3181593418561,-3.95557434013013,-0.0123104525898624));
#55749=CARTESIAN_POINT('Ctrl Pts',(1.52017634683108,-4.93727721897207,0.146079147834249));
#55750=CARTESIAN_POINT('Ctrl Pts',(4.96501177239675,-1.41203703483287,0.304468748258361));
#55751=CARTESIAN_POINT('Ctrl Pts',(3.88934922870828,3.39617009289883,0.462858348682473));
#55752=CARTESIAN_POINT('Ctrl Pts',(-0.732920742143878,5.1113964007393,0.621247949106584));
#55753=CARTESIAN_POINT('Ctrl Pts',(-4.68612688169979,2.16748556327014,0.779637549530696));
#55754=CARTESIAN_POINT('Ctrl Pts',(-4.36939265644683,-2.75114092476471,
0.938027149954809));
#55755=CARTESIAN_POINT('Ctrl Pts',(-0.0704529116473286,-5.16289724783097,
1.09641675037892));
#55756=CARTESIAN_POINT('Ctrl Pts',(4.29252819085395,-2.86947836000301,1.25480635080303));
#55757=CARTESIAN_POINT('Ctrl Pts',(4.74374945851672,2.03886099295457,1.41319595122714));
#55758=CARTESIAN_POINT('Ctrl Pts',(0.87187597225223,5.08919664880298,1.57158555165126));
#55759=CARTESIAN_POINT('Ctrl Pts',(-3.79452777359949,3.50164966549009,1.72997515207536));
#55760=CARTESIAN_POINT('Ctrl Pts',(-5.00293367927747,-1.2769919878773,1.88836475249948));
#55761=CARTESIAN_POINT('Ctrl Pts',(-1.65208468153467,-4.89189754332655,
2.04675435292359));
#55762=CARTESIAN_POINT('Ctrl Pts',(3.20433051897175,-4.04874042926377,2.20514395334771));
#55763=CARTESIAN_POINT('Ctrl Pts',(5.14059300557593,0.484092964878372,2.36353355377181));
#55764=CARTESIAN_POINT('Ctrl Pts',(2.392155064142,4.57576601695794,2.52192315419593));
#55765=CARTESIAN_POINT('Ctrl Pts',(-2.53628918908134,4.49747442552335,2.68031275462004));
#55766=CARTESIAN_POINT('Ctrl Pts',(-5.15337531200808,0.320567159775624,
2.83870235504415));
#55767=CARTESIAN_POINT('Ctrl Pts',(-3.07411308423917,-4.14847788693502,
2.99709195546826));
#55768=CARTESIAN_POINT('Ctrl Pts',(1.80663443860224,-4.83695274769126,3.15548155589238));
#55769=CARTESIAN_POINT('Ctrl Pts',(5.04096893490742,-1.11744005069485,3.31387115631648));
#55770=CARTESIAN_POINT('Ctrl Pts',(3.68139281034196,3.62041254264275,3.4722607567406));
#55771=CARTESIAN_POINT('Ctrl Pts',(-1.03309179131411,5.05892887272037,3.63065035716471));
#55772=CARTESIAN_POINT('Ctrl Pts',(-4.80610435287845,1.88716744466989,3.78903995758882));
#55773=CARTESIAN_POINT('Ctrl Pts',(-4.19924192609147,-3.00439798462519,
3.94742955801293));
#55774=CARTESIAN_POINT('Ctrl Pts',(0.234452652827207,-5.15801046495039,
4.10581915843705));
#55775=CARTESIAN_POINT('Ctrl Pts',(4.4544870133001,-2.61105064195526,4.26420875886115));
#55776=CARTESIAN_POINT('Ctrl Pts',(4.61508054334482,2.31539879571022,4.42259835928526));
#55777=CARTESIAN_POINT('Ctrl Pts',(0.56988195080356,5.13179058096912,4.58098795970938));
#55778=CARTESIAN_POINT('Ctrl Pts',(-3.99465861152192,3.27150463588748,4.73937756013348));
#55779=CARTESIAN_POINT('Ctrl Pts',(-4.91880686345887,-1.5701525546756,4.89776716055761));
#55780=CARTESIAN_POINT('Ctrl Pts',(-1.36037264139205,-4.98090617072295,
5.05615676098171));
#55781=CARTESIAN_POINT('Ctrl Pts',(3.43778957362211,-3.85248528258675,5.21454636140584));
#55782=CARTESIAN_POINT('Ctrl Pts',(5.10304258525828,0.786763228710822,5.37293596182993));
#55783=CARTESIAN_POINT('Ctrl Pts',(2.11781634615703,4.70902260867037,5.53132556225406));
#55784=CARTESIAN_POINT('Ctrl Pts',(-2.79740769526454,4.33987905263503,5.68971516267816));
#55785=CARTESIAN_POINT('Ctrl Pts',(-5.16331214443354,0.0157386201644824,
5.84810476310228));
#55786=CARTESIAN_POINT('Ctrl Pts',(-2.82381278957536,-4.32274465293194,
6.00649436352639));
#55787=CARTESIAN_POINT('Ctrl Pts',(2.08906951604171,-4.72184588505036,6.16488396395049));
#55788=CARTESIAN_POINT('Ctrl Pts',(5.098151436811,-0.817858137064712,6.32327356437462));
#55789=CARTESIAN_POINT('Ctrl Pts',(3.46121148378334,3.83145599864432,6.48166316479871));
#55790=CARTESIAN_POINT('Ctrl Pts',(-1.32998241066,4.98910681308353,6.64005276522284));
#55791=CARTESIAN_POINT('Ctrl Pts',(-4.90914338527368,1.60010975493711,6.79844236564693));
#55792=CARTESIAN_POINT('Ctrl Pts',(-4.01452835847177,-3.24709132363831,
6.95683196607106));
#55793=CARTESIAN_POINT('Ctrl Pts',(0.538586577094185,-5.13516937442138,
7.11522156649516));
#55794=CARTESIAN_POINT('Ctrl Pts',(4.60087948645563,-2.34349054961462,7.27361116691928));
#55795=CARTESIAN_POINT('Ctrl Pts',(4.47032190918109,2.58384636410851,7.43200076734339));
#55796=CARTESIAN_POINT('Ctrl Pts',(0.26589292373178,5.15648532996368,7.59039036776751));
#55797=CARTESIAN_POINT('Ctrl Pts',(-4.18084827136001,3.02994187021587,7.74877996819161));
#55798=CARTESIAN_POINT('Ctrl Pts',(-4.81751972636668,-1.85783306329961,
7.90716956861574));
#55799=CARTESIAN_POINT('Ctrl Pts',(-1.06391319462353,-5.05253685976928,
8.06555916903983));
#55800=CARTESIAN_POINT('Ctrl Pts',(3.65925338948522,-3.64278803069328,8.22394876946396));
#55801=CARTESIAN_POINT('Ctrl Pts',(5.04768747299395,1.08668817054443,8.38233836988805));
#55802=CARTESIAN_POINT('Ctrl Pts',(1.83608824986349,4.82584914224785,8.54072797031219));
#55803=CARTESIAN_POINT('Ctrl Pts',(-3.04876573566835,4.1671414055724,8.69911757073628));
#55804=CARTESIAN_POINT('Ctrl Pts',(-5.15523377649819,-0.289144798800594,
8.8575071711604));
#55805=CARTESIAN_POINT('Ctrl Pts',(-2.56365995117077,-4.48192901101572,
9.01589677158451));
#55806=CARTESIAN_POINT('Ctrl Pts',(2.36421564112952,-4.59026408905411,9.17428637200862));
#55807=CARTESIAN_POINT('Ctrl Pts',(5.13754605775107,-0.515422651333577,
9.33267597243274));
#55808=CARTESIAN_POINT('Ctrl Pts',(3.22895369161553,4.02913117959985,9.49106557285684));
#55809=CARTESIAN_POINT('Ctrl Pts',(-1.62223260619563,4.90187733184103,9.64945517328097));
#55810=CARTESIAN_POINT('Ctrl Pts',(-4.99505399739544,1.30746914614654,9.80784477370506));
#55811=CARTESIAN_POINT('Ctrl Pts',(-3.81580775774175,-3.47845528374006,
9.96623437412919));
#55812=CARTESIAN_POINT('Ctrl Pts',(0.840841326532404,-5.09441123866306,
10.1246239745533));
#55813=CARTESIAN_POINT('Ctrl Pts',(4.73121909778617,-2.06775381846214,10.2830135749774));
#55814=CARTESIAN_POINT('Ctrl Pts',(4.30996593957687,2.84327867165857,10.4414031754015));
#55815=CARTESIAN_POINT('Ctrl Pts',(-0.0390238264566685,5.16318866070086,
10.5997927758256));
#55816=CARTESIAN_POINT('Ctrl Pts',(-4.35245059410458,2.77780737829316,10.7581823762498));
#55817=CARTESIAN_POINT('Ctrl Pts',(-4.69942385101101,-2.13903143351615,
10.9165719766738));
#55818=CARTESIAN_POINT('Ctrl Pts',(-0.763741663751577,-5.10653881568242,
11.074961577098));
#55819=CARTESIAN_POINT('Ctrl Pts',(3.86794975738412,-3.42038077988013,11.2333511775221));
#55820=CARTESIAN_POINT('Ctrl Pts',(4.97472054752429,1.38282156443299,11.3917407779462));
#55821=CARTESIAN_POINT('Ctrl Pts',(1.54795388466898,4.92583787552529,11.5501303783703));
#55822=CARTESIAN_POINT('Ctrl Pts',(-3.28948637173101,3.97986424582764,11.7085199787944));
#55823=CARTESIAN_POINT('Ctrl Pts',(-5.12916835710966,-0.593019366839089,
11.8669095792185));
#55824=CARTESIAN_POINT('Ctrl Pts',(-2.29456228398659,-4.62547553554524,
12.0252991796426));
#55825=CARTESIAN_POINT('Ctrl Pts',(2.63111281568934,-4.44266646915302,12.1836887800668));
#55826=CARTESIAN_POINT('Ctrl Pts',(5.15901534120123,-0.211188811899807,
12.3420783804909));
#55827=CARTESIAN_POINT('Ctrl Pts',(2.98542980392062,4.2127483773522,12.500467980915));
#55828=CARTESIAN_POINT('Ctrl Pts',(-1.90882269345658,4.79754478144462,12.6588575813391));
#55829=CARTESIAN_POINT('Ctrl Pts',(-5.0635364390099,1.01026666570772,12.8172471817632));
#55830=CARTESIAN_POINT('Ctrl Pts',(-3.60377347746801,-3.6976826159257,12.9756367821873));
#55831=CARTESIAN_POINT('Ctrl Pts',(1.14016230868481,-5.03587826648703,13.1340263826114));
#55832=CARTESIAN_POINT('Ctrl Pts',(4.84505108113381,-1.78480251743019,13.2924159830355));
#55833=CARTESIAN_POINT('Ctrl Pts',(4.13457213027864,3.09279053680373,13.4508055834596));
#55834=CARTESIAN_POINT('Ctrl Pts',(-0.343804419177731,5.15187718471428,
13.6091951838838));
#55835=CARTESIAN_POINT('Ctrl Pts',(-4.50886684456297,2.51598087890574,13.7675847843078));
#55836=CARTESIAN_POINT('Ctrl Pts',(-4.56493128400683,-2.41276654015816,
13.925974384732));
#55837=CARTESIAN_POINT('Ctrl Pts',(-0.460905372910369,-5.14272362102755,
14.0843639851561));
#55838=CARTESIAN_POINT('Ctrl Pts',(4.06315051784514,-3.18603952805496,14.2427535855802));
#55839=CARTESIAN_POINT('Ctrl Pts',(4.88439639669049,1.67413017563193,14.4011431860043));
#55840=CARTESIAN_POINT('Ctrl Pts',(1.25441857601452,5.00863993928383,14.5595327864284));
#55841=CARTESIAN_POINT('Ctrl Pts',(-3.51872970857736,3.7787009993846,14.7179223868525));
#55842=CARTESIAN_POINT('Ctrl Pts',(-5.08520683073047,-0.894824839523584,
14.8763119872766));
#55843=CARTESIAN_POINT('Ctrl Pts',(-2.01745869282129,-4.75288338056742,
15.0347015877008));
#55844=CARTESIAN_POINT('Ctrl Pts',(2.88882981271105,-4.27956800578602,15.1930911881249));
#55845=CARTESIAN_POINT('Ctrl Pts',(5.16248437889336,0.0937818828261288,
15.351480788549));
#55846=CARTESIAN_POINT('Ctrl Pts',(2.73148949656154,4.38166693681219,15.5098703889731));
#55847=CARTESIAN_POINT('Ctrl Pts',(-2.18875273549729,4.67647318514471,15.6682599893972));
#55848=CARTESIAN_POINT('Ctrl Pts',(-5.11435176830703,0.709539282194621,
15.8266495898213));
#55849=CARTESIAN_POINT('Ctrl Pts',(-3.37916532475269,-3.90400842437456,
15.9850391902454));
#55850=CARTESIAN_POINT('Ctrl Pts',(1.43550516966593,-4.9597746708902,16.1434287906695));
#55851=CARTESIAN_POINT('Ctrl Pts',(4.94197826197569,-1.49562391370258,16.3018183910937));
#55852=CARTESIAN_POINT('Ctrl Pts',(3.94475245484231,3.3315114408263,16.4602079915177));
#55853=CARTESIAN_POINT('Ctrl Pts',(-0.647385467154988,5.12259027405121,
16.6185975919419));
#55854=CARTESIAN_POINT('Ctrl Pts',(-4.64955123813058,2.24537608806315,16.776987192366));
#55855=CARTESIAN_POINT('Ctrl Pts',(-4.41451134820182,-2.67808364399215,
16.9353767927901));
#55856=CARTESIAN_POINT('Ctrl Pts',(-0.156460816144074,-5.16096436253732,
17.0937663932142));
#55857=CARTESIAN_POINT('Ctrl Pts',(4.24417435465306,-2.94058317628852,17.2521559936383));
#55858=CARTESIAN_POINT('Ctrl Pts',(4.7770306357801,1.95960002071087,17.4105455940624));
#55859=CARTESIAN_POINT('Ctrl Pts',(0.956505601666415,5.07396180892462,17.5689351944865));
#55860=CARTESIAN_POINT('Ctrl Pts',(-3.73569419127765,3.5643623764192,17.7273247949107));
#55861=CARTESIAN_POINT('Ctrl Pts',(-5.02350584303606,-1.19352508090609,
17.8857143953348));
#55862=CARTESIAN_POINT('Ctrl Pts',(-1.7333097832156,-4.86367572142824,18.0441039957589));
#55863=CARTESIAN_POINT('Ctrl Pts',(3.13645552043595,-4.10159948955856,18.202493596183));
#55864=CARTESIAN_POINT('Ctrl Pts',(5.14796384574126,0.398543369117654,18.3608831966071));
#55865=CARTESIAN_POINT('Ctrl Pts',(2.46797524199195,4.53507188733415,18.5192727970312));
#55866=CARTESIAN_POINT('Ctrl Pts',(-2.46096278237594,4.53951629179981,18.6776623974553));
#55867=CARTESIAN_POINT('Ctrl Pts',(-5.14748183280556,0.405511410062441,
18.8360519978794));
#55868=CARTESIAN_POINT('Ctrl Pts',(-3.14246278706502,-4.0951334678725,18.9944415983036));
#55869=CARTESIAN_POINT('Ctrl Pts',(1.72525842040716,-4.86940713488401,19.1528311987277));
#55870=CARTESIAN_POINT('Ctrl Pts',(5.02276837180745,-1.19521866677756,19.3112207991518));
#55871=CARTESIAN_POINT('Ctrl Pts',(3.95306672650205,2.75529758855723,19.4432121328385));
#55872=CARTESIAN_POINT('Ctrl Pts',(1.3947178009747,4.32991044428859,19.548805199788));
#55873=CARTESIAN_POINT('Ctrl Pts',(-0.0904913830656236,4.43080762341373,
19.6016017332627));
#55874=CARTESIAN_POINT('Ctrl Pts',(-0.803308159453631,4.29756675351939,
19.628));
#55875=CARTESIAN_POINT('Ctrl Pts',(-2.00237954638878,4.09906332620074,-0.219393102292058));
#55876=CARTESIAN_POINT('Ctrl Pts',(-2.6822715117666,3.76693823886074,-0.192994835554706));
#55877=CARTESIAN_POINT('Ctrl Pts',(-3.86326433094171,2.75793992993429,-0.140198302080001));
#55878=CARTESIAN_POINT('Ctrl Pts',(-5.02561840602911,-0.153231111990883,
-0.0346052351305939));
#55879=CARTESIAN_POINT('Ctrl Pts',(-3.46236114308042,-4.12747715912022,
0.0973860985561662));
#55880=CARTESIAN_POINT('Ctrl Pts',(1.58624073518831,-5.15184324632905,0.255775698980278));
#55881=CARTESIAN_POINT('Ctrl Pts',(5.18078309827857,-1.47340186480046,0.414165299404389));
#55882=CARTESIAN_POINT('Ctrl Pts',(4.0583740122066,3.54376211431939,0.572554899828502));
#55883=CARTESIAN_POINT('Ctrl Pts',(-0.764772284002811,5.33352936417491,
0.730944500252612));
#55884=CARTESIAN_POINT('Ctrl Pts',(-4.88977832440859,2.26168095600148,0.889334100676726));
#55885=CARTESIAN_POINT('Ctrl Pts',(-4.55927934554221,-2.87070102899737,
1.04772370110084));
#55886=CARTESIAN_POINT('Ctrl Pts',(-0.0735146804517841,-5.38726835420972,
1.20611330152495));
#55887=CARTESIAN_POINT('Ctrl Pts',(4.47907447545189,-2.9941812164533,1.36450290194906));
#55888=CARTESIAN_POINT('Ctrl Pts',(4.94990508457304,2.12746657133089,1.52289250237317));
#55889=CARTESIAN_POINT('Ctrl Pts',(0.909766282116828,5.31036484717274,1.68128210279728));
#55890=CARTESIAN_POINT('Ctrl Pts',(-3.95943177107978,3.65382565735724,1.8396717032214));
#55891=CARTESIAN_POINT('Ctrl Pts',(-5.2203530294748,-1.33248798003114,1.99806130364551));
#55892=CARTESIAN_POINT('Ctrl Pts',(-1.72388159129946,-5.10449144388282,
2.15645090406962));
#55893=CARTESIAN_POINT('Ctrl Pts',(3.34358550492888,-4.22469209476243,2.31484050449373));
#55894=CARTESIAN_POINT('Ctrl Pts',(5.36399480590974,0.505130856764646,2.47323010491784));
#55895=CARTESIAN_POINT('Ctrl Pts',(2.49611422749678,4.77462135621273,2.63161970534196));
#55896=CARTESIAN_POINT('Ctrl Pts',(-2.64651218677699,4.69292733971583,2.79000930576607));
#55897=CARTESIAN_POINT('Ctrl Pts',(-5.37733261056287,0.334498486481351,
2.94839890619018));
#55898=CARTESIAN_POINT('Ctrl Pts',(-3.20770903254784,-4.32876397991708,
3.10678850661429));
#55899=CARTESIAN_POINT('Ctrl Pts',(1.88514782911787,-5.04715883690933,3.2651781070384));
#55900=CARTESIAN_POINT('Ctrl Pts',(5.26004123537227,-1.16600217549634,3.42356770746252));
#55901=CARTESIAN_POINT('Ctrl Pts',(3.84138014656453,3.77774977574021,3.58195730788662));
#55902=CARTESIAN_POINT('Ctrl Pts',(-1.07798827812784,5.27878168283402,3.74034690831074));
#55903=CARTESIAN_POINT('Ctrl Pts',(-5.01496982109594,1.96918066847761,3.89873650873484));
#55904=CARTESIAN_POINT('Ctrl Pts',(-4.38173414154377,-3.1349642282388,4.05712610915897));
#55905=CARTESIAN_POINT('Ctrl Pts',(0.244641583302294,-5.38216919970349,
4.21551570958307));
#55906=CARTESIAN_POINT('Ctrl Pts',(4.64807176456428,-2.72452265064043,4.37390531000719));
#55907=CARTESIAN_POINT('Ctrl Pts',(4.81564442789093,2.41602225663996,4.53229491043129));
#55908=CARTESIAN_POINT('Ctrl Pts',(0.594648092306935,5.35480984226466,4.69068451085541));
#55909=CARTESIAN_POINT('Ctrl Pts',(-4.16825996929618,3.41367889956971,4.84907411127951));
#55910=CARTESIAN_POINT('Ctrl Pts',(-5.13257019924506,-1.63838882763724,
5.00746371170364));
#55911=CARTESIAN_POINT('Ctrl Pts',(-1.41949222095851,-5.19736824127129,
5.16585331212774));
#55912=CARTESIAN_POINT('Ctrl Pts',(3.58719030989569,-4.01990801902123,5.32424291255186));
#55913=CARTESIAN_POINT('Ctrl Pts',(5.32481250547765,0.820954677351021,5.48263251297596));
#55914=CARTESIAN_POINT('Ctrl Pts',(2.2098531956012,4.91366906238659,5.64102211340008));
#55915=CARTESIAN_POINT('Ctrl Pts',(-2.9189784779956,4.52848312857297,5.79941171382418));
#55916=CARTESIAN_POINT('Ctrl Pts',(-5.38770128154296,0.0164225949658002,
5.9578013142483));
#55917=CARTESIAN_POINT('Ctrl Pts',(-2.9465310947033,-4.51060409576292,6.11619091467242));
#55918=CARTESIAN_POINT('Ctrl Pts',(2.17985707506455,-4.92704961747478,6.27458051509652));
#55919=CARTESIAN_POINT('Ctrl Pts',(5.3197087956843,-0.853400919782555,6.43297011552065));
#55920=CARTESIAN_POINT('Ctrl Pts',(3.61163009812893,3.99796483664578,6.59135971594474));
#55921=CARTESIAN_POINT('Ctrl Pts',(-1.38778128029068,5.20592527019374,6.74974931636887));
#55922=CARTESIAN_POINT('Ctrl Pts',(-5.12248676203533,1.6696479190355,6.90813891679296));
#55923=CARTESIAN_POINT('Ctrl Pts',(-4.18899322308973,-3.38820462452834,
7.0665285172171));
#55924=CARTESIAN_POINT('Ctrl Pts',(0.561992672622043,-5.35833547257784,
7.22491811764118));
#55925=CARTESIAN_POINT('Ctrl Pts',(4.80082621619637,-2.44533483242041,7.38330771806533));
#55926=CARTESIAN_POINT('Ctrl Pts',(4.66459481923242,2.69613611918183,7.5416973184894));
#55927=CARTESIAN_POINT('Ctrl Pts',(0.27744819717852,5.38057778483401,7.70008691891355));
#55928=CARTESIAN_POINT('Ctrl Pts',(-4.36254112853255,3.16161820949792,7.85847651933763));
#55929=CARTESIAN_POINT('Ctrl Pts',(-5.02688128812553,-1.93857146266532,
8.01686611976177));
#55930=CARTESIAN_POINT('Ctrl Pts',(-1.11014912943107,-5.27211188340975,
8.17525572018585));
#55931=CARTESIAN_POINT('Ctrl Pts',(3.81827858253237,-3.80109766606194,8.33364532061));
#55932=CARTESIAN_POINT('Ctrl Pts',(5.26705175018262,1.13391386871537,8.49203492103408));
#55933=CARTESIAN_POINT('Ctrl Pts',(1.91588165504971,5.03557268685605,8.65042452145821));
#55934=CARTESIAN_POINT('Ctrl Pts',(-3.18126012948741,4.34823858468009,8.80881412188231));
#55935=CARTESIAN_POINT('Ctrl Pts',(-5.37927184089313,-0.301710560871043,
8.96720372230643));
#55936=CARTESIAN_POINT('Ctrl Pts',(-2.67507243761234,-4.67670634681008,
9.12559332273054));
#55937=CARTESIAN_POINT('Ctrl Pts',(2.46696060266074,-4.78974949091146,9.28398292315464));
#55938=CARTESIAN_POINT('Ctrl Pts',(5.36081544269451,-0.537822080371423,
9.44237252357877));
#55939=CARTESIAN_POINT('Ctrl Pts',(3.36927876055584,4.20423065904265,9.60076212400287));
#55940=CARTESIAN_POINT('Ctrl Pts',(-1.69273219338161,5.11490493775362,9.75915172442699));
#55941=CARTESIAN_POINT('Ctrl Pts',(-5.21213090945059,1.36428962596537,9.91754132485109));
#55942=CARTESIAN_POINT('Ctrl Pts',(-3.98163654867748,-3.62962328554942,
10.0759309252752));
#55943=CARTESIAN_POINT('Ctrl Pts',(0.877382921235304,-5.31580605461594,
10.2343205256993));
#55944=CARTESIAN_POINT('Ctrl Pts',(4.93683017477137,-2.15761503198178,10.3927101261234));
#55945=CARTESIAN_POINT('Ctrl Pts',(4.49727004033617,2.96684293232075,10.5510997265475));
#55946=CARTESIAN_POINT('Ctrl Pts',(-0.0407197384023858,5.38757243140836,
10.7094893269717));
#55947=CARTESIAN_POINT('Ctrl Pts',(-4.54160100876145,2.89852636316868,10.8678789273958));
#55948=CARTESIAN_POINT('Ctrl Pts',(-4.90365315835139,-2.23199025610718,
11.0262685278199));
#55949=CARTESIAN_POINT('Ctrl Pts',(-0.796932632670351,-5.32846067638225,
11.184658128244));
#55950=CARTESIAN_POINT('Ctrl Pts',(4.03604455470867,-3.56902495832874,11.3430477286681));
#55951=CARTESIAN_POINT('Ctrl Pts',(5.19091380096199,1.44291673763568,11.5014373290922));
#55952=CARTESIAN_POINT('Ctrl Pts',(1.6152254395837,5.13990676764554,11.6598269295163));
#55953=CARTESIAN_POINT('Ctrl Pts',(-3.43244209236889,4.15282266456216,11.8182165299404));
#55954=CARTESIAN_POINT('Ctrl Pts',(-5.3520736608267,-0.618791022762998,
11.9766061303646));
#55955=CARTESIAN_POINT('Ctrl Pts',(-2.39428022405006,-4.82649116952364,
12.1349957307887));
#55956=CARTESIAN_POINT('Ctrl Pts',(2.7454566937728,-4.63573751881888,12.2933853312128));
#55957=CARTESIAN_POINT('Ctrl Pts',(5.38321774623971,-0.22036673373445,12.4517749316369));
#55958=CARTESIAN_POINT('Ctrl Pts',(3.11517172129139,4.39582756118039,12.610164532061));
#55959=CARTESIAN_POINT('Ctrl Pts',(-1.99177701910997,5.00603826462726,12.7685541324851));
#55960=CARTESIAN_POINT('Ctrl Pts',(-5.28358948645086,1.05417120973438,12.9269437329092));
#55961=CARTESIAN_POINT('Ctrl Pts',(-3.76038760389046,-3.85837788057022,
13.0853333333334));
#55962=CARTESIAN_POINT('Ctrl Pts',(1.18971190581428,-5.25472933479274,13.2437229337574));
#55963=CARTESIAN_POINT('Ctrl Pts',(5.05560911073477,-1.862367128206,13.4021125341816));
#55964=CARTESIAN_POINT('Ctrl Pts',(4.3142539017226,3.22719817678374,13.5605021346057));
#55965=CARTESIAN_POINT('Ctrl Pts',(-0.358745599334103,5.37576937709664,
13.7188917350298));
#55966=CARTESIAN_POINT('Ctrl Pts',(-4.70481485473382,2.6253213105142,13.8772813354539));
#55967=CARTESIAN_POINT('Ctrl Pts',(-4.76331576341244,-2.51762144469383,
14.035670935878));
#55968=CARTESIAN_POINT('Ctrl Pts',(-0.480935569811807,-5.36621801443908,
14.1940605363021));
#55969=CARTESIAN_POINT('Ctrl Pts',(4.23972842232605,-3.32449961733459,14.3524501367262));
#55970=CARTESIAN_POINT('Ctrl Pts',(5.09666430962992,1.74688514666806,14.5108397371504));
#55971=CARTESIAN_POINT('Ctrl Pts',(1.30893356445067,5.22630727424813,14.6692293375744));
#55972=CARTESIAN_POINT('Ctrl Pts',(-3.67164797130143,3.94291719103216,14.8276189379986));
#55973=CARTESIAN_POINT('Ctrl Pts',(-5.30620163810439,-0.933712469786478,
14.9860085384227));
#55974=CARTESIAN_POINT('Ctrl Pts',(-2.10513416208848,-4.95943595200104,
15.1443981388468));
#55975=CARTESIAN_POINT('Ctrl Pts',(3.01437365178127,-4.46555106184718,15.3027877392709));
#55976=CARTESIAN_POINT('Ctrl Pts',(5.38683754266046,0.0978574907256861,
15.461177339695));
#55977=CARTESIAN_POINT('Ctrl Pts',(2.85019558172777,4.57208704614299,15.6195669401191));
#55978=CARTESIAN_POINT('Ctrl Pts',(-2.28387236489903,4.87970509392274,15.7779565405432));
#55979=CARTESIAN_POINT('Ctrl Pts',(-5.33661316720418,0.740374703881965,
15.9363461409674));
#55980=CARTESIAN_POINT('Ctrl Pts',(-3.5260183466427,-4.07367027264334,16.0947357413914));
#55981=CARTESIAN_POINT('Ctrl Pts',(1.49788988655441,-5.17531840086943,16.2531253418156));
#55982=CARTESIAN_POINT('Ctrl Pts',(5.15674858900573,-1.56062129330084,16.4115149422397));
#55983=CARTESIAN_POINT('Ctrl Pts',(4.11618497232175,3.47629350252734,16.5699045426638));
#55984=CARTESIAN_POINT('Ctrl Pts',(-0.675519785260975,5.34520970499122,
16.7282941430879));
#55985=CARTESIAN_POINT('Ctrl Pts',(-4.85161316293496,2.34295647615374,16.886683743512));
#55986=CARTESIAN_POINT('Ctrl Pts',(-4.60635882216303,-2.79446879777952,
17.0450733439361));
#55987=CARTESIAN_POINT('Ctrl Pts',(-0.16326034841019,-5.385251468869,17.2034629443603));
#55988=CARTESIAN_POINT('Ctrl Pts',(4.42861926027611,-3.06837613225715,17.3618525447843));
#55989=CARTESIAN_POINT('Ctrl Pts',(4.98463260760038,2.04476104631356,17.5202421452085));
#55990=CARTESIAN_POINT('Ctrl Pts',(0.998073777402168,5.29446792596388,17.6786317456326));
#55991=CARTESIAN_POINT('Ctrl Pts',(-3.89804137708339,3.71926376057284,17.8370213460567));
#55992=CARTESIAN_POINT('Ctrl Pts',(-5.24181922596764,-1.24539373721259,
17.9954109464808));
#55993=CARTESIAN_POINT('Ctrl Pts',(-1.8086366036207,-5.07504314756533,18.1538005469049));
#55994=CARTESIAN_POINT('Ctrl Pts',(3.27276076949422,-4.27984832373426,18.312190147329));
#55995=CARTESIAN_POINT('Ctrl Pts',(5.37168597078491,0.415863414893554,18.4705797477531));
#55996=CARTESIAN_POINT('Ctrl Pts',(2.57522942679949,4.73215872598774,18.6289693481773));
#55997=CARTESIAN_POINT('Ctrl Pts',(-2.56791221710864,4.73679627703356,18.7873589486013));
#55998=CARTESIAN_POINT('Ctrl Pts',(-5.371183010352,0.423134275550087,18.9457485490255));
#55999=CARTESIAN_POINT('Ctrl Pts',(-3.27902910214792,-4.27310129927592,
19.1041381494496));
#56000=CARTESIAN_POINT('Ctrl Pts',(1.80023534169657,-5.08102363891602,19.2625277498737));
#56001=CARTESIAN_POINT('Ctrl Pts',(5.24104970544042,-1.24716092356801,19.4209173502978));
#56002=CARTESIAN_POINT('Ctrl Pts',(4.12486056868766,2.87503833462901,19.5529086839846));
#56003=CARTESIAN_POINT('Ctrl Pts',(1.45532996524397,4.51808130074211,19.658501750934));
#56004=CARTESIAN_POINT('Ctrl Pts',(-0.0944239912043199,4.62336330695642,
19.7112982844087));
#56005=CARTESIAN_POINT('Ctrl Pts',(-0.838218623839749,4.48433200584526,
19.737696551146));
#56006=CARTESIAN_POINT('Ctrl Pts',(-2.08577545033744,4.26978275451687,-0.109696551146029));
#56007=CARTESIAN_POINT('Ctrl Pts',(-2.79398382812688,3.92382518874754,-0.0832982844086765));
#56008=CARTESIAN_POINT('Ctrl Pts',(-4.02416310842503,2.87280371482855,-0.0305017509339729));
#56009=CARTESIAN_POINT('Ctrl Pts',(-5.23492737076948,-0.159612942608633,
0.0750913160154349));
#56010=CARTESIAN_POINT('Ctrl Pts',(-3.60656294430474,-4.29937997811031,
0.207082649702195));
#56011=CARTESIAN_POINT('Ctrl Pts',(1.65230512354554,-5.36640927368603,0.365472250126306));
#56012=CARTESIAN_POINT('Ctrl Pts',(5.39655442416041,-1.53476669476806,0.523861850550419));
#56013=CARTESIAN_POINT('Ctrl Pts',(4.22739879570491,3.69135413573996,0.68225145097453));
#56014=CARTESIAN_POINT('Ctrl Pts',(-0.796623825861737,5.55566232761052,
0.840641051398642));
#56015=CARTESIAN_POINT('Ctrl Pts',(-5.09342976711741,2.35587634873282,0.999030651822753));
#56016=CARTESIAN_POINT('Ctrl Pts',(-4.74916603463757,-2.99026113323004,
1.15742025224687));
#56017=CARTESIAN_POINT('Ctrl Pts',(-0.0765764492562429,-5.61163946058846,
1.31580985267098));
#56018=CARTESIAN_POINT('Ctrl Pts',(4.66562076004983,-3.11888407290359,1.47419945309509));
#56019=CARTESIAN_POINT('Ctrl Pts',(5.15606071062936,2.21607214970721,1.6325890535192));
#56020=CARTESIAN_POINT('Ctrl Pts',(0.947656591981422,5.53153304554248,1.79097865394331));
#56021=CARTESIAN_POINT('Ctrl Pts',(-4.12433576856007,3.80600164922439,1.94936825436742));
#56022=CARTESIAN_POINT('Ctrl Pts',(-5.43777237967215,-1.38798397218498,
2.10775785479154));
#56023=CARTESIAN_POINT('Ctrl Pts',(-1.79567850106425,-5.31708534443909,
2.26614745521565));
#56024=CARTESIAN_POINT('Ctrl Pts',(3.482840490886,-4.4006437602611,2.42453705563976));
#56025=CARTESIAN_POINT('Ctrl Pts',(5.58739660624356,0.526168748650917,2.58292665606387));
#56026=CARTESIAN_POINT('Ctrl Pts',(2.60007339085155,4.97347669546753,2.74131625648798));
#56027=CARTESIAN_POINT('Ctrl Pts',(-2.75673518447264,4.88838025390829,2.8997058569121));
#56028=CARTESIAN_POINT('Ctrl Pts',(-5.60128990911765,0.348429813187091,
3.05809545733621));
#56029=CARTESIAN_POINT('Ctrl Pts',(-3.34130498085651,-4.50905007289915,
3.21648505776032));
#56030=CARTESIAN_POINT('Ctrl Pts',(1.9636612196335,-5.25736492612739,3.37487465818443));
#56031=CARTESIAN_POINT('Ctrl Pts',(5.47911353583714,-1.21456430029784,3.53326425860854));
#56032=CARTESIAN_POINT('Ctrl Pts',(4.00136748278709,3.93508700883766,3.69165385903265));
#56033=CARTESIAN_POINT('Ctrl Pts',(-1.12288476494156,5.49863449294768,3.85004345945677));
#56034=CARTESIAN_POINT('Ctrl Pts',(-5.22383528931343,2.05119389228533,4.00843305988088));
#56035=CARTESIAN_POINT('Ctrl Pts',(-4.56422635699607,-3.26553047185241,
4.16682266030499));
#56036=CARTESIAN_POINT('Ctrl Pts',(0.254830513777376,-5.6063279344566,4.3252122607291));
#56037=CARTESIAN_POINT('Ctrl Pts',(4.84165651582845,-2.8379946593256,4.48360186115322));
#56038=CARTESIAN_POINT('Ctrl Pts',(5.01620831243703,2.51664571756971,4.64199146157732));
#56039=CARTESIAN_POINT('Ctrl Pts',(0.619414233810315,5.57782910356021,4.80038106200144));
#56040=CARTESIAN_POINT('Ctrl Pts',(-4.34186132707045,3.55585316325194,4.95877066242554));
#56041=CARTESIAN_POINT('Ctrl Pts',(-5.34633353503125,-1.70662510059887,
5.11716026284966));
#56042=CARTESIAN_POINT('Ctrl Pts',(-1.47861180052498,-5.41383031181963,
5.27554986327377));
#56043=CARTESIAN_POINT('Ctrl Pts',(3.73659104616929,-4.18733075545571,5.43393946369789));
#56044=CARTESIAN_POINT('Ctrl Pts',(5.54658242569702,0.855146125991221,5.59232906412199));
#56045=CARTESIAN_POINT('Ctrl Pts',(2.30189004504538,5.11831551610282,5.75071866454611));
#56046=CARTESIAN_POINT('Ctrl Pts',(-3.04054926072666,4.71708720451092,5.90910826497022));
#56047=CARTESIAN_POINT('Ctrl Pts',(-5.61209041865238,0.0171065697671163,
6.06749786539433));
#56048=CARTESIAN_POINT('Ctrl Pts',(-3.06924939983126,-4.69846353859389,
6.22588746581845));
#56049=CARTESIAN_POINT('Ctrl Pts',(2.27064463408739,-5.13225334989921,6.38427706624255));
#56050=CARTESIAN_POINT('Ctrl Pts',(5.5412661545576,-0.888943702500394,6.54266666666667));
#56051=CARTESIAN_POINT('Ctrl Pts',(3.76204871247451,4.16447367464723,6.70105626709077));
#56052=CARTESIAN_POINT('Ctrl Pts',(-1.44558014992134,5.42274372730397,6.85944586751489));
#56053=CARTESIAN_POINT('Ctrl Pts',(-5.33583013879699,1.73918608313389,7.017835467939));
#56054=CARTESIAN_POINT('Ctrl Pts',(-4.36345808770768,-3.52931792541838,
7.17622506836312));
#56055=CARTESIAN_POINT('Ctrl Pts',(0.585398768149902,-5.58150157073431,
7.33461466878722));
#56056=CARTESIAN_POINT('Ctrl Pts',(5.00077294593711,-2.54717911522619,7.49300426921134));
#56057=CARTESIAN_POINT('Ctrl Pts',(4.85886772928377,2.80842587425515,7.65139386963545));
#56058=CARTESIAN_POINT('Ctrl Pts',(0.289003470625252,5.60467023970434,7.80978347005956));
#56059=CARTESIAN_POINT('Ctrl Pts',(-4.54423398570509,3.29329454877997,7.96817307048368));
#56060=CARTESIAN_POINT('Ctrl Pts',(-5.23624284988438,-2.01930986203101,
8.12656267090778));
#56061=CARTESIAN_POINT('Ctrl Pts',(-1.15638506423861,-5.49168690705022,
8.2849522713319));
#56062=CARTESIAN_POINT('Ctrl Pts',(3.97730377557951,-3.9594073014306,8.44334187175601));
#56063=CARTESIAN_POINT('Ctrl Pts',(5.48641602737129,1.1811395668863,8.60173147218012));
#56064=CARTESIAN_POINT('Ctrl Pts',(1.99567506023593,5.24529623146426,8.76012107260423));
#56065=CARTESIAN_POINT('Ctrl Pts',(-3.31375452330647,4.52933576378778,8.91851067302835));
#56066=CARTESIAN_POINT('Ctrl Pts',(-5.60330990528806,-0.314276322941499,
9.07690027345245));
#56067=CARTESIAN_POINT('Ctrl Pts',(-2.78648492405391,-4.87148368260443,
9.23528987387657));
#56068=CARTESIAN_POINT('Ctrl Pts',(2.56970556419197,-4.98923489276881,9.39367947430067));
#56069=CARTESIAN_POINT('Ctrl Pts',(5.58408482763794,-0.560221509409272,
9.5520690747248));
#56070=CARTESIAN_POINT('Ctrl Pts',(3.50960382949614,4.37933013848544,9.7104586751489));
#56071=CARTESIAN_POINT('Ctrl Pts',(-1.76323178056758,5.32793254366621,9.86884827557301));
#56072=CARTESIAN_POINT('Ctrl Pts',(-5.42920782150573,1.4211101057842,10.0272378759971));
#56073=CARTESIAN_POINT('Ctrl Pts',(-4.14746533961321,-3.78079128735878,
10.1856274764213));
#56074=CARTESIAN_POINT('Ctrl Pts',(0.913924515938199,-5.53720087056882,
10.3440170768453));
#56075=CARTESIAN_POINT('Ctrl Pts',(5.14244125175658,-2.24747624550143,10.5024066772695));
#56076=CARTESIAN_POINT('Ctrl Pts',(4.68457414109547,3.09040719298293,10.6607962776936));
#56077=CARTESIAN_POINT('Ctrl Pts',(-0.0424156503481004,5.61195620211585,
10.8191858781177));
#56078=CARTESIAN_POINT('Ctrl Pts',(-4.73075142341831,3.01924534804421,10.9775754785418));
#56079=CARTESIAN_POINT('Ctrl Pts',(-5.10788246569177,-2.32494907869821,
11.1359650789659));
#56080=CARTESIAN_POINT('Ctrl Pts',(-0.83012360158913,-5.55038253708208,
11.29435467939));
#56081=CARTESIAN_POINT('Ctrl Pts',(4.20413935203321,-3.71766913677734,11.4527442798141));
#56082=CARTESIAN_POINT('Ctrl Pts',(5.4071070543997,1.50301191083837,11.6111338802383));
#56083=CARTESIAN_POINT('Ctrl Pts',(1.68249699449844,5.35397565976581,11.7695234806624));
#56084=CARTESIAN_POINT('Ctrl Pts',(-3.57539781300678,4.32578108329668,11.9279130810865));
#56085=CARTESIAN_POINT('Ctrl Pts',(-5.57497896454372,-0.644562678686908,
12.0863026815106));
#56086=CARTESIAN_POINT('Ctrl Pts',(-2.49399816411355,-5.02750680350203,
12.2446922819347));
#56087=CARTESIAN_POINT('Ctrl Pts',(2.85980057185626,-4.82880856848474,12.4030818823588));
#56088=CARTESIAN_POINT('Ctrl Pts',(5.60742015127818,-0.229544655569092,
12.5614714827829));
#56089=CARTESIAN_POINT('Ctrl Pts',(3.24491363866216,4.57890674500859,12.719861083207));
#56090=CARTESIAN_POINT('Ctrl Pts',(-2.07473134476337,5.2145317478099,12.8782506836311));
#56091=CARTESIAN_POINT('Ctrl Pts',(-5.50364253389182,1.09807575376104,13.0366402840552));
#56092=CARTESIAN_POINT('Ctrl Pts',(-3.91700173031292,-4.01907314521474,
13.1950298844794));
#56093=CARTESIAN_POINT('Ctrl Pts',(1.23926150294374,-5.47358040309844,13.3534194849035));
#56094=CARTESIAN_POINT('Ctrl Pts',(5.26616714033573,-1.93993173898181,13.5118090853276));
#56095=CARTESIAN_POINT('Ctrl Pts',(4.49393567316656,3.36160581676376,13.6701986857517));
#56096=CARTESIAN_POINT('Ctrl Pts',(-0.37368677949048,5.59966156947901,13.8285882861758));
#56097=CARTESIAN_POINT('Ctrl Pts',(-4.90076286490465,2.73466174212266,13.9869778865999));
#56098=CARTESIAN_POINT('Ctrl Pts',(-4.96170024281806,-2.6224763492295,14.1453674870241));
#56099=CARTESIAN_POINT('Ctrl Pts',(-0.500965766713239,-5.58971240785062,
14.3037570874481));
#56100=CARTESIAN_POINT('Ctrl Pts',(4.41630632680696,-3.46295970661421,14.4621466878723));
#56101=CARTESIAN_POINT('Ctrl Pts',(5.30893222256936,1.81964011770419,14.6205362882964));
#56102=CARTESIAN_POINT('Ctrl Pts',(1.36344855288682,5.44397460921243,14.7789258887205));
#56103=CARTESIAN_POINT('Ctrl Pts',(-3.8245662340255,4.10713338267972,14.9373154891446));
#56104=CARTESIAN_POINT('Ctrl Pts',(-5.52719644547832,-0.972600100049373,
15.0957050895687));
#56105=CARTESIAN_POINT('Ctrl Pts',(-2.19280963135567,-5.16598852343466,
15.2540946899928));
#56106=CARTESIAN_POINT('Ctrl Pts',(3.1399174908515,-4.65153411790834,15.4124842904169));
#56107=CARTESIAN_POINT('Ctrl Pts',(5.61119070642755,0.101933098625243,15.570873890841));
#56108=CARTESIAN_POINT('Ctrl Pts',(2.96890166689401,4.76250715547379,15.7292634912652));
#56109=CARTESIAN_POINT('Ctrl Pts',(-2.37899199430077,5.08293700270077,15.8876530916893));
#56110=CARTESIAN_POINT('Ctrl Pts',(-5.55887456610132,0.77121012556931,16.0460426921134));
#56111=CARTESIAN_POINT('Ctrl Pts',(-3.6728713685327,-4.24333212091212,16.2044322925375));
#56112=CARTESIAN_POINT('Ctrl Pts',(1.56027460344289,-5.39086213084865,16.3628218929616));
#56113=CARTESIAN_POINT('Ctrl Pts',(5.37151891603578,-1.6256186728991,16.5212114933857));
#56114=CARTESIAN_POINT('Ctrl Pts',(4.28761748980119,3.62107556422837,16.6796010938098));
#56115=CARTESIAN_POINT('Ctrl Pts',(-0.703654103366955,5.56782913593124,
16.837990694234));
#56116=CARTESIAN_POINT('Ctrl Pts',(-5.05367508773934,2.44053686424434,16.996380294658));
#56117=CARTESIAN_POINT('Ctrl Pts',(-4.79820629612424,-2.91085395156691,
17.1547698950822));
#56118=CARTESIAN_POINT('Ctrl Pts',(-0.170059880676311,-5.60953857520067,
17.3131594955063));
#56119=CARTESIAN_POINT('Ctrl Pts',(4.61306416589918,-3.1961690882258,17.4715490959304));
#56120=CARTESIAN_POINT('Ctrl Pts',(5.19223457942065,2.12992207191625,17.6299386963545));
#56121=CARTESIAN_POINT('Ctrl Pts',(1.03964195313792,5.51497404300314,17.7883282967786));
#56122=CARTESIAN_POINT('Ctrl Pts',(-4.06038856288912,3.87416514472648,17.9467178972027));
#56123=CARTESIAN_POINT('Ctrl Pts',(-5.46013260889923,-1.2972623935191,18.1051074976268));
#56124=CARTESIAN_POINT('Ctrl Pts',(-1.88396342402579,-5.28641057370242,
18.263497098051));
#56125=CARTESIAN_POINT('Ctrl Pts',(3.40906601855249,-4.45809715790996,18.421886698475));
#56126=CARTESIAN_POINT('Ctrl Pts',(5.59540809582856,0.433183460669457,18.5802762988992));
#56127=CARTESIAN_POINT('Ctrl Pts',(2.68248361160703,4.92924556464132,18.7386658993233));
#56128=CARTESIAN_POINT('Ctrl Pts',(-2.67486165184133,4.93407626226733,18.8970554997474));
#56129=CARTESIAN_POINT('Ctrl Pts',(-5.59488418789844,0.440757141037727,
19.0554451001715));
#56130=CARTESIAN_POINT('Ctrl Pts',(-3.41559541723082,-4.45106913067933,
19.2138347005956));
#56131=CARTESIAN_POINT('Ctrl Pts',(1.87521226298597,-5.29264014294805,19.3722243010197));
#56132=CARTESIAN_POINT('Ctrl Pts',(5.4593310390734,-1.29910318035845,19.5306139014438));
#56133=CARTESIAN_POINT('Ctrl Pts',(4.29665441087326,2.99477908070078,19.6626052351306));
#56134=CARTESIAN_POINT('Ctrl Pts',(1.51594212951325,4.70625215719564,19.76819830208));
#56135=CARTESIAN_POINT('Ctrl Pts',(-0.098356599343019,4.8159189904991,19.8209948355547));
#56136=CARTESIAN_POINT('Ctrl Pts',(-0.873129088225867,4.67109725817113,
19.8473931022921));
#56137=CARTESIAN_POINT('Ctrl Pts',(-2.1691713542861,4.440502182833,2.77555756156289E-16));
#56138=CARTESIAN_POINT('Ctrl Pts',(-2.90569614448715,4.08071213863434,0.0263982667373523));
#56139=CARTESIAN_POINT('Ctrl Pts',(-4.18506188590834,2.9876674997228,0.079194800212056));
#56140=CARTESIAN_POINT('Ctrl Pts',(-5.44423633550983,-0.165994773226382,
0.184787867161464));
#56141=CARTESIAN_POINT('Ctrl Pts',(-3.75076474552906,-4.4712827971004,0.316779200848224));
#56142=CARTESIAN_POINT('Ctrl Pts',(1.71836951190277,-5.58097530104301,0.475168801272335));
#56143=CARTESIAN_POINT('Ctrl Pts',(5.61232575004223,-1.59613152473566,0.633558401696447));
#56144=CARTESIAN_POINT('Ctrl Pts',(4.39642357920323,3.83894615716052,0.79194800212056));
#56145=CARTESIAN_POINT('Ctrl Pts',(-0.828475367720669,5.77779529104613,
0.95033760254467));
#56146=CARTESIAN_POINT('Ctrl Pts',(-5.29708120982622,2.45007174146416,1.10872720296878));
#56147=CARTESIAN_POINT('Ctrl Pts',(-4.93905272373294,-3.10982123746271,
1.26711680339289));
#56148=CARTESIAN_POINT('Ctrl Pts',(-0.0796382180607007,-5.83601056696721,
1.42550640381701));
#56149=CARTESIAN_POINT('Ctrl Pts',(4.85216704464777,-3.24358692935388,1.58389600424112));
#56150=CARTESIAN_POINT('Ctrl Pts',(5.36221633668567,2.30467772808354,1.74228560466523));
#56151=CARTESIAN_POINT('Ctrl Pts',(0.985546901846022,5.75270124391223,1.90067520508934));
#56152=CARTESIAN_POINT('Ctrl Pts',(-4.28923976604036,3.95817764109155,2.05906480551345));
#56153=CARTESIAN_POINT('Ctrl Pts',(-5.65519172986948,-1.44347996433883,
2.21745440593756));
#56154=CARTESIAN_POINT('Ctrl Pts',(-1.86747541082905,-5.52967924499536,
2.37584400636168));
#56155=CARTESIAN_POINT('Ctrl Pts',(3.62209547684312,-4.57659542575977,2.53423360678579));
#56156=CARTESIAN_POINT('Ctrl Pts',(5.81079840657738,0.547206640537195,2.6926232072099));
#56157=CARTESIAN_POINT('Ctrl Pts',(2.70403255420632,5.17233203472232,2.85101280763401));
#56158=CARTESIAN_POINT('Ctrl Pts',(-2.86695818216828,5.08383316810077,3.00940240805812));
#56159=CARTESIAN_POINT('Ctrl Pts',(-5.82524720767244,0.362361139892822,
3.16779200848224));
#56160=CARTESIAN_POINT('Ctrl Pts',(-3.47490092916519,-4.68933616588121,
3.32618160890635));
#56161=CARTESIAN_POINT('Ctrl Pts',(2.04217461014913,-5.46757101534546,3.48457120933046));
#56162=CARTESIAN_POINT('Ctrl Pts',(5.698185836302,-1.26312642509933,3.64296080975457));
#56163=CARTESIAN_POINT('Ctrl Pts',(4.16135481900965,4.09242424193511,3.80135041017868));
#56164=CARTESIAN_POINT('Ctrl Pts',(-1.16778125175528,5.71848730306133,3.95974001060279));
#56165=CARTESIAN_POINT('Ctrl Pts',(-5.43270075753092,2.13320711609306,4.11812961102691));
#56166=CARTESIAN_POINT('Ctrl Pts',(-4.74671857244836,-3.39609671546603,
4.27651921145102));
#56167=CARTESIAN_POINT('Ctrl Pts',(0.265019444252462,-5.8304866692097,4.43490881187513));
#56168=CARTESIAN_POINT('Ctrl Pts',(5.03524126709262,-2.95146666801078,4.59329841229924));
#56169=CARTESIAN_POINT('Ctrl Pts',(5.21677219698313,2.61726917849946,4.75168801272335));
#56170=CARTESIAN_POINT('Ctrl Pts',(0.644180375313696,5.80084836485576,4.91007761314747));
#56171=CARTESIAN_POINT('Ctrl Pts',(-4.51546268484472,3.69802742693416,5.06846721357158));
#56172=CARTESIAN_POINT('Ctrl Pts',(-5.56009687081743,-1.77486137356051,
5.22685681399569));
#56173=CARTESIAN_POINT('Ctrl Pts',(-1.53773138009144,-5.63029238236797,
5.3852464144198));
#56174=CARTESIAN_POINT('Ctrl Pts',(3.88599178244287,-4.35475349189019,5.54363601484391));
#56175=CARTESIAN_POINT('Ctrl Pts',(5.7683523459164,0.889337574631424,5.70202561526803));
#56176=CARTESIAN_POINT('Ctrl Pts',(2.39392689448955,5.32296196981904,5.86041521569214));
#56177=CARTESIAN_POINT('Ctrl Pts',(-3.16212004345771,4.90569128044887,6.01880481611624));
#56178=CARTESIAN_POINT('Ctrl Pts',(-5.8364795557618,0.0177905445684291,
6.17719441654037));
#56179=CARTESIAN_POINT('Ctrl Pts',(-3.19196770495921,-4.88632298142486,
6.33558401696446));
#56180=CARTESIAN_POINT('Ctrl Pts',(2.36143219311022,-5.33745708232365,6.49397361738859));
#56181=CARTESIAN_POINT('Ctrl Pts',(5.7628235134309,-0.924486485218232,6.65236321781269));
#56182=CARTESIAN_POINT('Ctrl Pts',(3.9124673268201,4.33098251264868,6.81075281823681));
#56183=CARTESIAN_POINT('Ctrl Pts',(-1.50337901955202,5.63956218441419,6.96914241866092));
#56184=CARTESIAN_POINT('Ctrl Pts',(-5.54917351555865,1.80872424723227,7.12753201908502));
#56185=CARTESIAN_POINT('Ctrl Pts',(-4.53792295232564,-3.6704312263084,7.28592161950915));
#56186=CARTESIAN_POINT('Ctrl Pts',(0.60880486367776,-5.80466766889078,7.44431121993324));
#56187=CARTESIAN_POINT('Ctrl Pts',(5.20071967567786,-2.64902339803196,7.60270082035738));
#56188=CARTESIAN_POINT('Ctrl Pts',(5.0531406393351,2.92071562932846,7.76109042078146));
#56189=CARTESIAN_POINT('Ctrl Pts',(0.300558744071995,5.82876269457468,7.9194800212056));
#56190=CARTESIAN_POINT('Ctrl Pts',(-4.72592684287763,3.42497088806201,8.07786962162969));
#56191=CARTESIAN_POINT('Ctrl Pts',(-5.44560441164323,-2.10004826139671,
8.23625922205382));
#56192=CARTESIAN_POINT('Ctrl Pts',(-1.20262099904615,-5.7112619306907,8.39464882247792));
#56193=CARTESIAN_POINT('Ctrl Pts',(4.13632896862666,-4.11771693679927,8.55303842290205));
#56194=CARTESIAN_POINT('Ctrl Pts',(5.70578030455996,1.22836526505724,8.71142802332614));
#56195=CARTESIAN_POINT('Ctrl Pts',(2.07546846542215,5.45501977607246,8.86981762375027));
#56196=CARTESIAN_POINT('Ctrl Pts',(-3.44624891712552,4.71043294289546,9.02820722417436));
#56197=CARTESIAN_POINT('Ctrl Pts',(-5.827347969683,-0.32684208501195,9.18659682459849));
#56198=CARTESIAN_POINT('Ctrl Pts',(-2.89789741049547,-5.06626101839879,
9.3449864250226));
#56199=CARTESIAN_POINT('Ctrl Pts',(2.6724505257232,-5.18872029462616,9.50337602544671));
#56200=CARTESIAN_POINT('Ctrl Pts',(5.80735421258137,-0.582620938447121,
9.66176562587082));
#56201=CARTESIAN_POINT('Ctrl Pts',(3.64992889843646,4.55442961792825,9.82015522629493));
#56202=CARTESIAN_POINT('Ctrl Pts',(-1.83373136775356,5.54096014957879,9.97854482671904));
#56203=CARTESIAN_POINT('Ctrl Pts',(-5.64628473356088,1.47793058560304,10.1369344271431));
#56204=CARTESIAN_POINT('Ctrl Pts',(-4.31329413054894,-3.93195928916814,
10.2953240275673));
#56205=CARTESIAN_POINT('Ctrl Pts',(0.950466110641093,-5.7585956865217,10.4537136279914));
#56206=CARTESIAN_POINT('Ctrl Pts',(5.34805232874179,-2.33733745902108,10.6121032284155));
#56207=CARTESIAN_POINT('Ctrl Pts',(4.87187824185477,3.2139714536451,10.7704928288396));
#56208=CARTESIAN_POINT('Ctrl Pts',(-0.0441115622938141,5.83633997282335,
10.9288824292637));
#56209=CARTESIAN_POINT('Ctrl Pts',(-4.91990183807518,3.13996433291973,11.0872720296878));
#56210=CARTESIAN_POINT('Ctrl Pts',(-5.31211177303214,-2.41790790128923,
11.2456616301119));
#56211=CARTESIAN_POINT('Ctrl Pts',(-0.863314570507911,-5.77230439778191,
11.404051230536));
#56212=CARTESIAN_POINT('Ctrl Pts',(4.37223414935776,-3.86631331522594,11.5624408309602));
#56213=CARTESIAN_POINT('Ctrl Pts',(5.6233003078374,1.56310708404107,11.7208304313843));
#56214=CARTESIAN_POINT('Ctrl Pts',(1.74976854941316,5.56804455188607,11.8792200318084));
#56215=CARTESIAN_POINT('Ctrl Pts',(-3.71835353364465,4.4987395020312,12.0376096322325));
#56216=CARTESIAN_POINT('Ctrl Pts',(-5.79788426826075,-0.670334334610817,
12.1959992326566));
#56217=CARTESIAN_POINT('Ctrl Pts',(-2.59371610417703,-5.22852243748043,
12.3543888330807));
#56218=CARTESIAN_POINT('Ctrl Pts',(2.97414444993972,-5.0218796181506,12.5127784335049));
#56219=CARTESIAN_POINT('Ctrl Pts',(5.83162255631666,-0.238722577403733,
12.6711680339289));
#56220=CARTESIAN_POINT('Ctrl Pts',(3.37465555603293,4.76198592883678,12.8295576343531));
#56221=CARTESIAN_POINT('Ctrl Pts',(-2.15768567041678,5.42302523099255,12.9879472347772));
#56222=CARTESIAN_POINT('Ctrl Pts',(-5.72369558133277,1.1419802977877,13.1463368352013));
#56223=CARTESIAN_POINT('Ctrl Pts',(-4.07361585673539,-4.17976840985925,
13.3047264356254));
#56224=CARTESIAN_POINT('Ctrl Pts',(1.28881110007321,-5.69243147140415,13.4631160360495));
#56225=CARTESIAN_POINT('Ctrl Pts',(5.47672516993668,-2.01749634975762,13.6215056364736));
#56226=CARTESIAN_POINT('Ctrl Pts',(4.67361744461052,3.49601345674377,13.7798952368977));
#56227=CARTESIAN_POINT('Ctrl Pts',(-0.388627959646856,5.82355376186139,
13.9382848373218));
#56228=CARTESIAN_POINT('Ctrl Pts',(-5.09671087507549,2.84400217373111,14.096674437746));
#56229=CARTESIAN_POINT('Ctrl Pts',(-5.16008472222368,-2.72733125376517,
14.2550640381701));
#56230=CARTESIAN_POINT('Ctrl Pts',(-0.520995963614669,-5.81320680126216,
14.4134536385942));
#56231=CARTESIAN_POINT('Ctrl Pts',(4.59288423128786,-3.60141979589384,14.5718432390183));
#56232=CARTESIAN_POINT('Ctrl Pts',(5.5212001355088,1.89239508874033,14.7302328394424));
#56233=CARTESIAN_POINT('Ctrl Pts',(1.41796354132297,5.66164194417672,14.8886224398665));
#56234=CARTESIAN_POINT('Ctrl Pts',(-3.97748449674956,4.27134957432729,15.0470120402906));
#56235=CARTESIAN_POINT('Ctrl Pts',(-5.74819125285225,-1.01148773031227,
15.2054016407147));
#56236=CARTESIAN_POINT('Ctrl Pts',(-2.28048510062285,-5.37254109486827,
15.3637912411389));
#56237=CARTESIAN_POINT('Ctrl Pts',(3.26546132992172,-4.8375171739695,15.5221808415629));
#56238=CARTESIAN_POINT('Ctrl Pts',(5.83554387019465,0.106008706524804,15.6805704419871));
#56239=CARTESIAN_POINT('Ctrl Pts',(3.08760775206024,4.95292726480458,15.8389600424112));
#56240=CARTESIAN_POINT('Ctrl Pts',(-2.4741116237025,5.2861689114788,15.9973496428353));
#56241=CARTESIAN_POINT('Ctrl Pts',(-5.78113596499847,0.802045547256652,
16.1557392432594));
#56242=CARTESIAN_POINT('Ctrl Pts',(-3.81972439042269,-4.4129939691809,16.3141288436835));
#56243=CARTESIAN_POINT('Ctrl Pts',(1.62265932033137,-5.60640586082788,16.4725184441076));
#56244=CARTESIAN_POINT('Ctrl Pts',(5.58628924306583,-1.69061605249735,16.6309080445317));
#56245=CARTESIAN_POINT('Ctrl Pts',(4.45905000728063,3.76585762592941,16.7892976449558));
#56246=CARTESIAN_POINT('Ctrl Pts',(-0.731788421472935,5.79044856687125,
16.94768724538));
#56247=CARTESIAN_POINT('Ctrl Pts',(-5.25573701254373,2.53811725233494,17.106076845804));
#56248=CARTESIAN_POINT('Ctrl Pts',(-4.99005377008544,-3.02723910535429,
17.2644664462282));
#56249=CARTESIAN_POINT('Ctrl Pts',(-0.176859412942431,-5.83382568153235,
17.4228560466523));
#56250=CARTESIAN_POINT('Ctrl Pts',(4.79750907152224,-3.32396204419444,17.5812456470764));
#56251=CARTESIAN_POINT('Ctrl Pts',(5.39983655124094,2.21508309751895,17.7396352475005));
#56252=CARTESIAN_POINT('Ctrl Pts',(1.08121012887367,5.73548016004241,17.8980248479246));
#56253=CARTESIAN_POINT('Ctrl Pts',(-4.22273574869486,4.02906652888012,18.0564144483487));
#56254=CARTESIAN_POINT('Ctrl Pts',(-5.67844599183081,-1.34913104982561,
18.2148040487729));
#56255=CARTESIAN_POINT('Ctrl Pts',(-1.95929024443088,-5.4977779998395,18.373193649197));
#56256=CARTESIAN_POINT('Ctrl Pts',(3.54537126761076,-4.63634599208567,18.5315832496211));
#56257=CARTESIAN_POINT('Ctrl Pts',(5.81913022087222,0.450503506445362,18.6899728500452));
#56258=CARTESIAN_POINT('Ctrl Pts',(2.78973779641457,5.12633240329489,18.8483624504693));
#56259=CARTESIAN_POINT('Ctrl Pts',(-2.78181108657403,5.13135624750109,19.0067520508934));
#56260=CARTESIAN_POINT('Ctrl Pts',(-5.81858536544488,0.458380006525366,
19.1651416513175));
#56261=CARTESIAN_POINT('Ctrl Pts',(-3.55216173231372,-4.62903696208274,
19.3235312517416));
#56262=CARTESIAN_POINT('Ctrl Pts',(1.95018918427537,-5.50425664698007,19.4819208521657));
#56263=CARTESIAN_POINT('Ctrl Pts',(5.67761237270639,-1.3510454371489,19.6403104525899));
#56264=CARTESIAN_POINT('Ctrl Pts',(4.46844825305886,3.11451982677256,19.7723017862766));
#56265=CARTESIAN_POINT('Ctrl Pts',(1.57655429378253,4.89442301364916,19.877894853226));
#56266=CARTESIAN_POINT('Ctrl Pts',(-0.102289207481715,5.00847467404178,
19.9306913867007));
#56267=CARTESIAN_POINT('Ctrl Pts',(-0.908039552611985,4.857862510497,19.9570896534381));
#56268=CARTESIAN_POINT('Ctrl Pts',(-4.94192999916445,-0.00446510791632448,
18.1776795453431));
#56269=CARTESIAN_POINT('Ctrl Pts',(-4.94542698461402,-0.388624254474772,
18.1900543798197));
#56270=CARTESIAN_POINT('Ctrl Pts',(-4.90438878928145,-0.772044124408378,
18.2024292142963));
#56271=CARTESIAN_POINT('Ctrl Pts',(-4.81596832674149,-1.14420594504366,
18.2148040487729));
#56272=CARTESIAN_POINT('Ctrl Pts',(-4.43872740936416,-2.73201336649694,
18.2676005822476));
#56273=CARTESIAN_POINT('Ctrl Pts',(-3.19900882689749,-4.11489568316824,
18.3203971157223));
#56274=CARTESIAN_POINT('Ctrl Pts',(-1.66170595032388,-4.66276484021157,
18.373193649197));
#56275=CARTESIAN_POINT('Ctrl Pts',(-0.124403073750308,-5.21063399725488,
18.4259901826717));
#56276=CARTESIAN_POINT('Ctrl Pts',(1.71048409693019,-4.92348999467027,18.4787867161464));
#56277=CARTESIAN_POINT('Ctrl Pts',(3.00688750781402,-3.93210974362283,18.5315832496211));
#56278=CARTESIAN_POINT('Ctrl Pts',(4.3032909186979,-2.94072949257537,18.5843797830958));
#56279=CARTESIAN_POINT('Ctrl Pts',(5.06121056978506,-1.24511299306501,18.6371763165705));
#56280=CARTESIAN_POINT('Ctrl Pts',(4.93527165791903,0.38200007283176,18.6899728500452));
#56281=CARTESIAN_POINT('Ctrl Pts',(4.80933274605301,2.00911313872853,18.7427693835199));
#56282=CARTESIAN_POINT('Ctrl Pts',(3.79953527123378,3.56772277101172,18.7955659169946));
#56283=CARTESIAN_POINT('Ctrl Pts',(2.36604505332606,4.34786489452101,18.8483624504693));
#56284=CARTESIAN_POINT('Ctrl Pts',(0.932554835418334,5.1280070180303,18.901158983944));
#56285=CARTESIAN_POINT('Ctrl Pts',(-0.92462812557789,5.12968163276569,18.9539555174187));
#56286=CARTESIAN_POINT('Ctrl Pts',(-2.35934865255447,4.3516895666374,19.0067520508934));
#56287=CARTESIAN_POINT('Ctrl Pts',(-2.82356148188028,4.09996535176783,19.0238347005956));
#56288=CARTESIAN_POINT('Ctrl Pts',(-3.24354728379133,3.7666188744385,19.0409173502978));
#56289=CARTESIAN_POINT('Ctrl Pts',(-3.60367707498796,3.37571982724537,19.058));
#56290=CARTESIAN_POINT('Ctrl Pts',(-2.54467524200881,-3.56229978442281,
-6.93889390390723E-18));
#56291=CARTESIAN_POINT('Ctrl Pts',(-2.64087676169121,-3.50326719695733,
3.78010404015323E-18));
#56292=CARTESIAN_POINT('Ctrl Pts',(-2.73444512499906,-3.44042480726573,
1.70774935809012E-16));
#56293=CARTESIAN_POINT('Ctrl Pts',(-2.82511133337028,-3.37382080685403,
1.33573707650214E-16));
#56294=CARTESIAN_POINT('Ctrl Pts',(-2.93010592262241,-3.29669108243516,
6.34680042936623E-17));
#56295=CARTESIAN_POINT('Ctrl Pts',(-3.0312098993845,-3.21451805045997,-1.1579302301566E-16));
#56296=CARTESIAN_POINT('Ctrl Pts',(-3.12833116102487,-3.1277186925041,-1.87350135405495E-16));
#56297=CARTESIAN_POINT('Ctrl Pts',(-3.19203631412683,-3.07078402861756,
-2.34286889761188E-16));
#56298=CARTESIAN_POINT('Ctrl Pts',(-3.25402740755314,-3.01185787186213,
2.54730009275007E-16));
#56299=CARTESIAN_POINT('Ctrl Pts',(-3.3142718238098,-2.95104792020956,3.67761376907083E-16));
#56300=CARTESIAN_POINT('Ctrl Pts',(-3.34056115234898,-2.92451180455305,
4.17085761531429E-16));
#56301=CARTESIAN_POINT('Ctrl Pts',(-3.36651779652415,-2.8976168731598,-1.29958168485043E-16));
#56302=CARTESIAN_POINT('Ctrl Pts',(-3.39213869657566,-2.87037166754254,
-1.66533453693773E-16));
#56303=CARTESIAN_POINT('Ctrl Pts',(-3.4107075535189,-2.85062558819017,-1.9304154815313E-16));
#56304=CARTESIAN_POINT('Ctrl Pts',(-3.42910165503002,-2.83069359301782,
5.20445990861309E-16));
#56305=CARTESIAN_POINT('Ctrl Pts',(-3.44730402197008,-2.81059669044114,
5.13478148889135E-16));
#56306=CARTESIAN_POINT('Ctrl Pts',(-3.53659117665104,-2.71201636542733,
4.79299144256909E-16));
#56307=CARTESIAN_POINT('Ctrl Pts',(-3.62135066124632,-2.60938482813861,
1.69265913904123E-16));
#56308=CARTESIAN_POINT('Ctrl Pts',(-3.70148784592851,-2.50313357384095,
1.80411241501588E-16));
#56309=CARTESIAN_POINT('Ctrl Pts',(-3.78346559823418,-2.39444197154017,
1.91812551751929E-16));
#56310=CARTESIAN_POINT('Ctrl Pts',(-3.86060678067413,-2.28196193869908,
-1.60403205534396E-16));
#56311=CARTESIAN_POINT('Ctrl Pts',(-3.93277586934314,-2.16611326123794,
-5.55111512312578E-17));
#56312=CARTESIAN_POINT('Ctrl Pts',(-3.96434984563583,-2.1154294648487,-9.62087747363501E-18));
#56313=CARTESIAN_POINT('Ctrl Pts',(-3.99497165206884,-2.06410040223293,
2.30246512287273E-16));
#56314=CARTESIAN_POINT('Ctrl Pts',(-4.02462756948077,-2.01215919201488,
2.91433543964104E-16));
#56315=CARTESIAN_POINT('Ctrl Pts',(-4.03961656660672,-1.98590653424469,
3.22359319390632E-16));
#56316=CARTESIAN_POINT('Ctrl Pts',(-4.05435879396083,-1.95949747991113,
2.06007824657555E-17));
#56317=CARTESIAN_POINT('Ctrl Pts',(-4.06885232846184,-1.93293620549746,
1.38777878078145E-17));
#56318=CARTESIAN_POINT('Ctrl Pts',(-4.08041475408644,-1.91174656677398,
8.51442211522865E-18));
#56319=CARTESIAN_POINT('Ctrl Pts',(-4.09181979945551,-1.89045816584063,
2.1634594979841E-16));
#56320=CARTESIAN_POINT('Ctrl Pts',(-4.10305617212226,-1.86909315496197,
2.08166817117217E-16));
#56321=CARTESIAN_POINT('Ctrl Pts',(-4.16736596175704,-1.74681353716178,
1.61354708109947E-16));
#56322=CARTESIAN_POINT('Ctrl Pts',(-4.22623125974132,-1.62188769970873,
-1.58091925840003E-16));
#56323=CARTESIAN_POINT('Ctrl Pts',(-4.27954887166761,-1.49476314498018,
-1.66533453693773E-16));
#56324=CARTESIAN_POINT('Ctrl Pts',(-4.33347479304113,-1.36618820519452,
-1.75071292334113E-16));
#56325=CARTESIAN_POINT('Ctrl Pts',(-4.38172617240059,-1.23536340764327,
-1.43714543602008E-16));
#56326=CARTESIAN_POINT('Ctrl Pts',(-4.42415678995003,-1.10271583109255,
-9.71445146547012E-17));
#56327=CARTESIAN_POINT('Ctrl Pts',(-4.46710218965978,-0.968458930662989,
-5.00094828511621E-17));
#56328=CARTESIAN_POINT('Ctrl Pts',(-4.50408524649974,-0.832334009558243,
-1.01069852635313E-16));
#56329=CARTESIAN_POINT('Ctrl Pts',(-4.53490679318661,-0.694758137572736,
-1.38777878078145E-16));
#56330=CARTESIAN_POINT('Ctrl Pts',(-4.55802295320176,-0.591576233583606,
-1.67058897160268E-16));
#56331=CARTESIAN_POINT('Ctrl Pts',(-4.5776723273625,-0.487577560717138,
-2.48733805589575E-17));
#56332=CARTESIAN_POINT('Ctrl Pts',(-4.59375100179198,-0.38293266212137,
-5.55111512312578E-17));
#56333=CARTESIAN_POINT('Ctrl Pts',(-4.60074932415958,-0.337385453754768,
-6.88463920640666E-17));
#56334=CARTESIAN_POINT('Ctrl Pts',(-4.60707095895173,-0.291715781756126,
-3.50051711561292E-16));
#56335=CARTESIAN_POINT('Ctrl Pts',(-4.61270623945594,-0.245937595982269,
-3.60822483003176E-16));
#56336=CARTESIAN_POINT('Ctrl Pts',(-4.61510536794149,-0.226448282287078,
-3.65407962742523E-16));
#56337=CARTESIAN_POINT('Ctrl Pts',(-4.61738026973089,-0.206937176747096,
-2.11235974110856E-16));
#56338=CARTESIAN_POINT('Ctrl Pts',(-4.61952832377542,-0.187423425576886,
-2.22044604925031E-16));
#56339=CARTESIAN_POINT('Ctrl Pts',(-4.63503826526744,-0.0465251368621273,
-3.00087907403534E-16));
#56340=CARTESIAN_POINT('Ctrl Pts',(-4.64396392467283,0.0947008669712182,
-1.99183435512137E-16));
#56341=CARTESIAN_POINT('Ctrl Pts',(-4.64615947496329,0.235825173850752,
-2.22044604925031E-16));
#56342=CARTESIAN_POINT('Ctrl Pts',(-4.64786848339456,0.345675825581053,
-2.39839656782873E-16));
#56343=CARTESIAN_POINT('Ctrl Pts',(-4.64549890174975,0.455465549450203,
-1.5964104232527E-16));
#56344=CARTESIAN_POINT('Ctrl Pts',(-4.63896138884064,0.56499930567962,-1.38777878078145E-16));
#56345=CARTESIAN_POINT('Ctrl Pts',(-4.63077575597687,0.702146738831947,
-1.08813479195783E-16));
#56346=CARTESIAN_POINT('Ctrl Pts',(-4.61605776615402,0.838893185885087,
-2.45094142526848E-16));
#56347=CARTESIAN_POINT('Ctrl Pts',(-4.59507497843275,0.974861012835041,
-2.22044604925031E-16));
#56348=CARTESIAN_POINT('Ctrl Pts',(-4.57379787866946,1.11273597287572,-1.98671766312435E-16));
#56349=CARTESIAN_POINT('Ctrl Pts',(-4.54607882402517,1.24981106593623,-1.79874459778951E-16));
#56350=CARTESIAN_POINT('Ctrl Pts',(-4.51214338117474,1.38568894112939,-8.32667268468867E-17));
#56351=CARTESIAN_POINT('Ctrl Pts',(-4.50044605637916,1.43252515439685,-4.99666743073618E-17));
#56352=CARTESIAN_POINT('Ctrl Pts',(-4.48800969217396,1.47921903836149,8.24656052999656E-18));
#56353=CARTESIAN_POINT('Ctrl Pts',(-4.47484214689978,1.52575396812219,5.55111512312578E-17));
#56354=CARTESIAN_POINT('Ctrl Pts',(-4.46954654891505,1.54446894309507,7.45195742938095E-17));
#56355=CARTESIAN_POINT('Ctrl Pts',(-4.4641321445575,1.56316001192783,2.98076212871544E-17));
#56356=CARTESIAN_POINT('Ctrl Pts',(-4.45860111065483,1.58182037106622,2.77555756156289E-17));
#56357=CARTESIAN_POINT('Ctrl Pts',(-4.41871853179728,1.7163744631118,1.29589074421813E-17));
#56358=CARTESIAN_POINT('Ctrl Pts',(-4.37289155988743,1.84894716867807,-3.65495115057949E-16));
#56359=CARTESIAN_POINT('Ctrl Pts',(-4.32143318995775,1.97915634222774,-3.60822483003176E-16));
#56360=CARTESIAN_POINT('Ctrl Pts',(-4.26919198995651,2.11134637247354,-3.56078766751783E-16));
#56361=CARTESIAN_POINT('Ctrl Pts',(-4.21114654432903,2.24110115829447,1.76811505571791E-16));
#56362=CARTESIAN_POINT('Ctrl Pts',(-4.147570486657,2.36801906886784,1.66533453693773E-16));
#56363=CARTESIAN_POINT('Ctrl Pts',(-4.08343929176894,2.49604520883007,1.56165655308743E-16));
#56364=CARTESIAN_POINT('Ctrl Pts',(-4.01368020422711,2.62118552486071,-5.6466401912637E-17));
#56365=CARTESIAN_POINT('Ctrl Pts',(-3.93852341174026,2.7430141593252,-2.77555756156289E-17));
#56366=CARTESIAN_POINT('Ctrl Pts',(-3.9294168218154,2.75777587784009,-2.4276745388323E-17));
#56367=CARTESIAN_POINT('Ctrl Pts',(-3.9202309270139,2.77248895031151,-1.25624424874937E-18));
#56368=CARTESIAN_POINT('Ctrl Pts',(-3.91096608990011,2.78715259668566,0.));
#56369=CARTESIAN_POINT('Ctrl Pts',(-3.85692740501027,2.87268072373382,-4.76202655277902E-17));
#56370=CARTESIAN_POINT('Ctrl Pts',(-3.80020397437343,2.95652797095731,1.2876992925575E-16));
#56371=CARTESIAN_POINT('Ctrl Pts',(-3.74088150109056,3.03859647479229,1.66533453693773E-16));
#56372=CARTESIAN_POINT('Ctrl Pts',(-3.7149279190293,3.0745014452201,1.83054995635409E-16));
#56373=CARTESIAN_POINT('Ctrl Pts',(-3.68847672600951,3.11006585723381,-1.71465257258441E-16));
#56374=CARTESIAN_POINT('Ctrl Pts',(-3.66153447975748,3.14528103385681,-1.66533453693773E-16));
#56375=CARTESIAN_POINT('Ctrl Pts',(-3.64469680263863,3.16728891575776,-1.6345130103068E-16));
#56376=CARTESIAN_POINT('Ctrl Pts',(-3.62766732852701,3.18916039136048,2.64610714971295E-16));
#56377=CARTESIAN_POINT('Ctrl Pts',(-3.6104475878738,3.21089327815198,2.77555756156289E-16));
#56378=CARTESIAN_POINT('Ctrl Pts',(-3.59895112257703,3.22540286826887,2.86198291473495E-16));
#56379=CARTESIAN_POINT('Ctrl Pts',(-3.58737284218715,3.23984685581822,3.27202329850872E-16));
#56380=CARTESIAN_POINT('Ctrl Pts',(-3.57571845845413,3.25421848714644,3.33066907387547E-16));
#56381=CARTESIAN_POINT('Ctrl Pts',(-3.4847651283665,3.36637780487935,3.78835338283328E-16));
#56382=CARTESIAN_POINT('Ctrl Pts',(-3.38908875605728,3.4742480319481,-5.71170610872501E-17));
#56383=CARTESIAN_POINT('Ctrl Pts',(-3.28901395033307,3.5775964314093,-5.55111512312578E-17));
#56384=CARTESIAN_POINT('Ctrl Pts',(-3.1878935796381,3.68202459780562,-5.38884630954632E-17));
#56385=CARTESIAN_POINT('Ctrl Pts',(-3.08228201196636,3.78183656326097,2.20761671403476E-16));
#56386=CARTESIAN_POINT('Ctrl Pts',(-2.97246730240431,3.87676781486652,2.77555756156289E-16));
#56387=CARTESIAN_POINT('Ctrl Pts',(-2.86296602007246,3.97142811880605,3.34187742290929E-16));
#56388=CARTESIAN_POINT('Ctrl Pts',(-2.74928508452755,4.0612360937228,2.13145292818159E-16));
#56389=CARTESIAN_POINT('Ctrl Pts',(-2.63167026985783,4.14589663192155,2.22044604925031E-16));
#56390=CARTESIAN_POINT('Ctrl Pts',(-2.51583556938655,4.22927582281283,2.3080922488549E-16));
#56391=CARTESIAN_POINT('Ctrl Pts',(-2.39618466430397,4.30766267709754,-5.76377990669945E-17));
#56392=CARTESIAN_POINT('Ctrl Pts',(-2.27292097783335,4.38073587186789,-1.11022302462516E-16));
#56393=CARTESIAN_POINT('Ctrl Pts',(-2.23861641107446,4.40107230963037,-1.25879332241991E-16));
#56394=CARTESIAN_POINT('Ctrl Pts',(-2.2040318620339,4.42099693210222,2.77555756156289E-16));
#56395=CARTESIAN_POINT('Ctrl Pts',(-2.1691713542861,4.440502182833,2.77555756156289E-16));
#56396=CARTESIAN_POINT('Origin',(0.,0.,0.));
#56397=CARTESIAN_POINT('Origin',(-2.30940107675851,-4.,-10.));
#56398=CARTESIAN_POINT('',(-2.30940107675851,-4.,-10.));
#56399=CARTESIAN_POINT('',(2.3094010767585,-4.,-10.));
#56400=CARTESIAN_POINT('',(-1.15470053837925,-4.,-10.));
#56401=CARTESIAN_POINT('',(-2.30940107675851,-4.,-4.));
#56402=CARTESIAN_POINT('',(-2.30940107675851,-4.,-10.));
#56403=CARTESIAN_POINT('',(2.3094010767585,-4.,-4.));
#56404=CARTESIAN_POINT('',(-2.30940107675851,-4.,-4.));
#56405=CARTESIAN_POINT('',(2.3094010767585,-4.,-10.));
#56406=CARTESIAN_POINT('Origin',(-4.61880215351701,5.6564012731995E-16,
-10.));
#56407=CARTESIAN_POINT('',(-4.61880215351701,5.6564012731995E-16,-10.));
#56408=CARTESIAN_POINT('',(-4.04145188432738,-0.999999999999999,-10.));
#56409=CARTESIAN_POINT('',(-4.61880215351701,5.55111512312578E-16,-4.));
#56410=CARTESIAN_POINT('',(-4.61880215351701,5.6564012731995E-16,-10.));
#56411=CARTESIAN_POINT('',(-4.61880215351701,5.6564012731995E-16,-4.));
#56412=CARTESIAN_POINT('Origin',(-2.3094010767585,4.,-10.));
#56413=CARTESIAN_POINT('',(-2.3094010767585,4.,-10.));
#56414=CARTESIAN_POINT('',(-2.88675134594813,3.,-10.));
#56415=CARTESIAN_POINT('',(-2.3094010767585,4.,-4.));
#56416=CARTESIAN_POINT('',(-2.3094010767585,4.,-10.));
#56417=CARTESIAN_POINT('',(-2.3094010767585,4.,-4.));
#56418=CARTESIAN_POINT('Origin',(2.3094010767585,4.,-10.));
#56419=CARTESIAN_POINT('',(2.3094010767585,4.,-10.));
#56420=CARTESIAN_POINT('',(1.15470053837925,4.,-10.));
#56421=CARTESIAN_POINT('',(2.3094010767585,4.,-4.));
#56422=CARTESIAN_POINT('',(2.3094010767585,4.,-10.));
#56423=CARTESIAN_POINT('',(2.3094010767585,4.,-4.));
#56424=CARTESIAN_POINT('Origin',(4.61880215351701,0.,-10.));
#56425=CARTESIAN_POINT('',(4.61880215351701,0.,-10.));
#56426=CARTESIAN_POINT('',(4.04145188432738,1.,-10.));
#56427=CARTESIAN_POINT('',(4.61880215351701,0.,-4.));
#56428=CARTESIAN_POINT('',(4.61880215351701,0.,-10.));
#56429=CARTESIAN_POINT('',(4.61880215351701,0.,-4.));
#56430=CARTESIAN_POINT('Origin',(2.3094010767585,-4.,-10.));
#56431=CARTESIAN_POINT('',(2.88675134594813,-3.,-10.));
#56432=CARTESIAN_POINT('',(2.3094010767585,-4.,-4.));
#56433=CARTESIAN_POINT('Origin',(0.,0.,-4.));
#56434=CARTESIAN_POINT('Origin',(0.,0.,0.));
#56435=CARTESIAN_POINT('',(-8.,-9.79717439317883E-16,0.));
#56436=CARTESIAN_POINT('Origin',(0.,0.,0.));
#56437=CARTESIAN_POINT('Origin',(0.,0.,-10.));
#56438=CARTESIAN_POINT('',(-8.,-9.79717439317883E-16,-10.));
#56439=CARTESIAN_POINT('',(-8.,-9.79717439317883E-16,-10.));
#56440=CARTESIAN_POINT('Origin',(0.,0.,-10.));
#56441=CARTESIAN_POINT('Origin',(0.,0.,-10.));
#56442=CARTESIAN_POINT('Origin',(0.,0.,20.));
#56443=CARTESIAN_POINT('',(0.,0.,0.));
#56444=CARTESIAN_POINT('Origin',(0.,0.,0.));
#56445=CARTESIAN_POINT('',(-30.,-3.67394039744206E-15,4.));
#56446=CARTESIAN_POINT('Origin',(0.,0.,4.));
#56447=CARTESIAN_POINT('',(-30.,-3.67394039744206E-15,0.));
#56448=CARTESIAN_POINT('',(-30.,-3.67394039744206E-15,0.));
#56449=CARTESIAN_POINT('Origin',(0.,0.,0.));
#56450=CARTESIAN_POINT('Origin',(0.,0.,4.));
#56451=CARTESIAN_POINT('Origin',(0.,0.,0.));
#56452=CARTESIAN_POINT('',(0.,0.,0.));
#56453=CARTESIAN_POINT('Origin',(15.,0.,7.5));
#56454=CARTESIAN_POINT('',(12.4864520394788,-8.37379766882585E-5,4.38741669750802));
#56455=CARTESIAN_POINT('',(12.4839933051997,-0.00316412607611227,4.11258330249198));
#56456=CARTESIAN_POINT('',(12.4825,3.08304831685346E-16,7.5));
#56457=CARTESIAN_POINT('',(13.086534003335,1.63598720337497,4.));
#56458=CARTESIAN_POINT('Ctrl Pts',(12.4839933051997,-0.00316412607611227,
4.11258330249198));
#56459=CARTESIAN_POINT('Ctrl Pts',(12.4891843965477,0.589325119423629,4.07505553499466));
#56460=CARTESIAN_POINT('Ctrl Pts',(12.700778171916,1.18480356030443,4.03752776749733));
#56461=CARTESIAN_POINT('Ctrl Pts',(13.086534003335,1.63598720337497,4.));
#56462=CARTESIAN_POINT('',(12.4825,3.08304831685346E-16,4.));
#56463=CARTESIAN_POINT('Origin',(15.,0.,4.));
#56464=CARTESIAN_POINT('',(12.4825,-3.08304831685346E-16,3.));
#56465=CARTESIAN_POINT('',(12.4825,3.08304831685346E-16,7.5));
#56466=CARTESIAN_POINT('Origin',(15.,0.,3.));
#56467=CARTESIAN_POINT('',(16.9169900003259,1.63831767401966,4.));
#56468=CARTESIAN_POINT('Origin',(15.,0.,4.));
#56469=CARTESIAN_POINT('Ctrl Pts',(16.9170033607455,1.63832650944338,4.));
#56470=CARTESIAN_POINT('Ctrl Pts',(16.4032792982694,2.23546892087832,4.04999787746244));
#56471=CARTESIAN_POINT('Ctrl Pts',(15.5859097998096,2.57572249729409,4.09999575492489));
#56472=CARTESIAN_POINT('Ctrl Pts',(14.8008208232653,2.51338129467797,4.14999363238733));
#56473=CARTESIAN_POINT('Ctrl Pts',(13.9790588101819,2.44812801296032,4.20232700817141));
#56474=CARTESIAN_POINT('Ctrl Pts',(13.1926635275253,1.94178951401471,4.2546603839555));
#56475=CARTESIAN_POINT('Ctrl Pts',(12.7937453701095,1.22068434196769,4.30699375973958));
#56476=CARTESIAN_POINT('Ctrl Pts',(12.5894005030727,0.851299951304611,4.3338014056624));
#56477=CARTESIAN_POINT('Ctrl Pts',(12.4867287035022,0.425561301199251,4.36060905158521));
#56478=CARTESIAN_POINT('Ctrl Pts',(12.4864520394788,-8.37379766882585E-5,
4.38741669750802));
#56479=CARTESIAN_POINT('Origin',(15.,0.,7.5));
#56480=CARTESIAN_POINT('',(12.4798657694311,-0.00154038945686864,5.38741669750803));
#56481=CARTESIAN_POINT('',(12.4793021139561,0.00120904389216911,5.11258330249198));
#56482=CARTESIAN_POINT('',(12.4825,3.08304831685346E-16,7.5));
#56483=CARTESIAN_POINT('Ctrl Pts',(12.4793021139561,0.00120904389216911,
5.11258330249198));
#56484=CARTESIAN_POINT('Ctrl Pts',(12.478879906904,0.0725686704440801,5.10805583214991));
#56485=CARTESIAN_POINT('Ctrl Pts',(12.4816538040259,0.14389470397244,5.10352836180784));
#56486=CARTESIAN_POINT('Ctrl Pts',(12.4877315613661,0.214937734438189,5.09900089146578));
#56487=CARTESIAN_POINT('Ctrl Pts',(12.5579848230722,1.0361295544392,5.04666751568169));
#56488=CARTESIAN_POINT('Ctrl Pts',(13.0696742764471,1.81950869898314,4.99433413989761));
#56489=CARTESIAN_POINT('Ctrl Pts',(13.7933805800141,2.21395750784665,4.94200076411352));
#56490=CARTESIAN_POINT('Ctrl Pts',(14.5170868835811,2.60840631671017,4.88966738832944));
#56491=CARTESIAN_POINT('Ctrl Pts',(15.4528100373402,2.61392478989326,4.83733401254535));
#56492=CARTESIAN_POINT('Ctrl Pts',(16.1810158838377,2.22781637405164,4.78500063676127));
#56493=CARTESIAN_POINT('Ctrl Pts',(16.9092217303351,1.84170795821001,4.73266726097718));
#56494=CARTESIAN_POINT('Ctrl Pts',(17.4299102695709,1.06397265334366,4.6803338851931));
#56495=CARTESIAN_POINT('Ctrl Pts',(17.5096246317311,0.243745210316159,4.62800050940901));
#56496=CARTESIAN_POINT('Ctrl Pts',(17.5893389938914,-0.576482232711353,
4.57566713362493));
#56497=CARTESIAN_POINT('Ctrl Pts',(17.2280791789763,-1.43920181390003,4.52333375784085));
#56498=CARTESIAN_POINT('Ctrl Pts',(16.5878264117224,-1.95845762325597,4.47100038205676));
#56499=CARTESIAN_POINT('Ctrl Pts',(15.9475736444685,-2.47771343261192,4.41866700627268));
#56500=CARTESIAN_POINT('Ctrl Pts',(15.0283279248759,-2.65350547013512,4.36633363048859));
#56501=CARTESIAN_POINT('Ctrl Pts',(14.2422049662735,-2.40531717421469,4.3140002547045));
#56502=CARTESIAN_POINT('Ctrl Pts',(13.4560820076711,-2.15712887829427,4.26166687892042));
#56503=CARTESIAN_POINT('Ctrl Pts',(12.8030818100589,-1.48496024893023,4.20933350313634));
#56504=CARTESIAN_POINT('Ctrl Pts',(12.5762083591215,-0.69397784322712,4.15700012735226));
#56505=CARTESIAN_POINT('Ctrl Pts',(12.5120237084102,-0.470201419766977,
4.1421945190655));
#56506=CARTESIAN_POINT('Ctrl Pts',(12.4819452946144,-0.236915405941376,
4.12738891077874));
#56507=CARTESIAN_POINT('Ctrl Pts',(12.4839933051997,-0.00316412607611227,
4.11258330249198));
#56508=CARTESIAN_POINT('Ctrl Pts',(12.4864520394788,-8.37379766882585E-5,
4.38741669750802));
#56509=CARTESIAN_POINT('Ctrl Pts',(12.4861886052651,-0.405374837317443,
4.41294242736929));
#56510=CARTESIAN_POINT('Ctrl Pts',(12.5787615741259,-0.810581064443052,
4.43846815723057));
#56511=CARTESIAN_POINT('Ctrl Pts',(12.7647943027407,-1.16697133984538,4.46399388709184));
#56512=CARTESIAN_POINT('Ctrl Pts',(13.146202424963,-1.897650004463,4.51632726287592));
#56513=CARTESIAN_POINT('Ctrl Pts',(13.9204597015827,-2.42313548854983,4.56866063866001));
#56514=CARTESIAN_POINT('Ctrl Pts',(14.7402998673034,-2.50800691661078,4.62099401444409));
#56515=CARTESIAN_POINT('Ctrl Pts',(15.560140033024,-2.59287834467174,4.67332739022818));
#56516=CARTESIAN_POINT('Ctrl Pts',(16.4255630878457,-2.23713571670682,4.72566076601226));
#56517=CARTESIAN_POINT('Ctrl Pts',(16.9486162247073,-1.60018404184685,4.77799414179635));
#56518=CARTESIAN_POINT('Ctrl Pts',(17.471669361569,-0.963232366986897,4.83032751758043));
#56519=CARTESIAN_POINT('Ctrl Pts',(17.6523525804706,-0.0450716452319087,
4.88266089336451));
#56520=CARTESIAN_POINT('Ctrl Pts',(17.4096229743894,0.742588180844264,4.9349942691486));
#56521=CARTESIAN_POINT('Ctrl Pts',(17.1668933683082,1.53024800692044,4.98732764493268));
#56522=CARTESIAN_POINT('Ctrl Pts',(16.5007509372442,2.1874069373178,5.03966102071677));
#56523=CARTESIAN_POINT('Ctrl Pts',(15.7098806230762,2.41944933284425,5.09199439650085));
#56524=CARTESIAN_POINT('Ctrl Pts',(14.9190103089082,2.6514917283707,5.14432777228493));
#56525=CARTESIAN_POINT('Ctrl Pts',(14.0034121116361,2.45841758902623,5.19666114806902));
#56526=CARTESIAN_POINT('Ctrl Pts',(13.3735902615222,1.92677994818613,5.2489945238531));
#56527=CARTESIAN_POINT('Ctrl Pts',(12.8182957469354,1.45805142494902,5.29513524840474));
#56528=CARTESIAN_POINT('Ctrl Pts',(12.4851467735748,0.72614376520494,5.34127597295639));
#56529=CARTESIAN_POINT('Ctrl Pts',(12.4798657694311,-0.00154038945686864,
5.38741669750803));
#56530=CARTESIAN_POINT('Origin',(15.,0.,7.5));
#56531=CARTESIAN_POINT('',(12.482920633805,0.00216662177004473,6.38741669750803));
#56532=CARTESIAN_POINT('',(12.4862854318642,0.000566909999415368,6.11258330249198));
#56533=CARTESIAN_POINT('',(12.4825,3.08304831685346E-16,7.5));
#56534=CARTESIAN_POINT('Ctrl Pts',(12.4862854318642,0.000566909999415368,
6.11258330249198));
#56535=CARTESIAN_POINT('Ctrl Pts',(12.4855058897774,0.379333771915191,6.08872275352109));
#56536=CARTESIAN_POINT('Ctrl Pts',(12.5659381445238,0.757786273313489,6.06486220455019));
#56537=CARTESIAN_POINT('Ctrl Pts',(12.7293101493446,1.09619859491376,6.04100165557929));
#56538=CARTESIAN_POINT('Ctrl Pts',(13.08763419844,1.83843881821599,5.98866827979521));
#56539=CARTESIAN_POINT('Ctrl Pts',(13.8449458114837,2.38806291012985,5.93633490401113));
#56540=CARTESIAN_POINT('Ctrl Pts',(14.6617006772638,2.49864636478707,5.88400152822704));
#56541=CARTESIAN_POINT('Ctrl Pts',(15.4784555430439,2.60922981944428,5.83166815244296));
#56542=CARTESIAN_POINT('Ctrl Pts',(16.3546536615603,2.28077263684485,5.77933477665887));
#56543=CARTESIAN_POINT('Ctrl Pts',(16.8974474362482,1.66053609593171,5.72700140087479));
#56544=CARTESIAN_POINT('Ctrl Pts',(17.4402412109362,1.04029955501857,5.6746680250907));
#56545=CARTESIAN_POINT('Ctrl Pts',(17.6496306417956,0.128283655791723,5.62233464930662));
#56546=CARTESIAN_POINT('Ctrl Pts',(17.4317349092204,-0.66659696383412,5.57000127352254));
#56547=CARTESIAN_POINT('Ctrl Pts',(17.2138391766452,-1.46147758345996,5.51766789773845));
#56548=CARTESIAN_POINT('Ctrl Pts',(16.5686582806354,-2.13922292348481,5.46533452195437));
#56549=CARTESIAN_POINT('Ctrl Pts',(15.7854622951236,-2.39597806232545,5.41300114617028));
#56550=CARTESIAN_POINT('Ctrl Pts',(15.0022663096119,-2.65273320116609,5.3606677703862));
#56551=CARTESIAN_POINT('Ctrl Pts',(14.0810552345983,-2.48849813882253,5.30833439460211));
#56552=CARTESIAN_POINT('Ctrl Pts',(13.4348582321103,-1.9768783599217,5.25600101881803));
#56553=CARTESIAN_POINT('Ctrl Pts',(12.8445650905918,-1.50951988350108,5.20819511337601));
#56554=CARTESIAN_POINT('Ctrl Pts',(12.4837602304949,-0.752282707918894,
5.160389207934));
#56555=CARTESIAN_POINT('Ctrl Pts',(12.4793021139561,0.00120904389216911,
5.11258330249198));
#56556=CARTESIAN_POINT('Ctrl Pts',(12.4798657694311,-0.00154038945686864,
5.38741669750803));
#56557=CARTESIAN_POINT('Ctrl Pts',(12.4791569938941,-0.0992045293459824,
5.39360934874047));
#56558=CARTESIAN_POINT('Ctrl Pts',(12.4843540819724,-0.196792591522919,
5.39980199997291));
#56559=CARTESIAN_POINT('Ctrl Pts',(12.4957126236098,-0.293658114991017,
5.40599465120536));
#56560=CARTESIAN_POINT('Ctrl Pts',(12.5917023387672,-1.11225739499233,5.45832802698944));
#56561=CARTESIAN_POINT('Ctrl Pts',(13.1277272720379,-1.87925481265923,5.51066140277353));
#56562=CARTESIAN_POINT('Ctrl Pts',(13.8634558058795,-2.25076673554666,5.56299477855761));
#56563=CARTESIAN_POINT('Ctrl Pts',(14.5991843397211,-2.62227865843409,5.61532815434169));
#56564=CARTESIAN_POINT('Ctrl Pts',(15.5346164741336,-2.59830508654206,5.66766153012578));
#56565=CARTESIAN_POINT('Ctrl Pts',(16.2503478880118,-2.18959297269902,5.71999490590987));
#56566=CARTESIAN_POINT('Ctrl Pts',(16.96607930189,-1.78088085885597,5.77232828169395));
#56567=CARTESIAN_POINT('Ctrl Pts',(17.4621099952338,-0.98743020306191,5.82466165747803));
#56568=CARTESIAN_POINT('Ctrl Pts',(17.5160416303984,-0.16498929182795,5.87699503326212));
#56569=CARTESIAN_POINT('Ctrl Pts',(17.5699732655631,0.657451619406004,5.9293284090462));
#56570=CARTESIAN_POINT('Ctrl Pts',(17.1818058425485,1.50888278607985,5.98166178483029));
#56571=CARTESIAN_POINT('Ctrl Pts',(16.5255763936941,2.00756141147231,6.03399516061437));
#56572=CARTESIAN_POINT('Ctrl Pts',(15.8693469448397,2.50624003686478,6.08632853639846));
#56573=CARTESIAN_POINT('Ctrl Pts',(14.9450554701454,2.65216612097585,6.13866191218254));
#56574=CARTESIAN_POINT('Ctrl Pts',(14.1671123287709,2.37991277262463,6.19099528796662));
#56575=CARTESIAN_POINT('Ctrl Pts',(13.3891691873965,2.10765942427341,6.24332866375071));
#56576=CARTESIAN_POINT('Ctrl Pts',(12.7575743793418,1.41722664345988,6.2956620395348));
#56577=CARTESIAN_POINT('Ctrl Pts',(12.5555065470498,0.618173398042358,6.34799541531888));
#56578=CARTESIAN_POINT('Ctrl Pts',(12.5047691803197,0.417538506829285,6.36113584271526));
#56579=CARTESIAN_POINT('Ctrl Pts',(12.4811120172555,0.210055467607507,6.37427627011165));
#56580=CARTESIAN_POINT('Ctrl Pts',(12.482920633805,0.00216662177004473,
6.38741669750803));
#56581=CARTESIAN_POINT('Origin',(15.,0.,7.5));
#56582=CARTESIAN_POINT('',(12.4854953774899,-0.00143787083715985,7.38741669750803));
#56583=CARTESIAN_POINT('',(12.4810882026093,-0.00198272270578489,7.11258330249199));
#56584=CARTESIAN_POINT('',(12.4825,3.08304831685346E-16,7.5));
#56585=CARTESIAN_POINT('Ctrl Pts',(12.4810882026093,-0.00198272270578489,
7.11258330249199));
#56586=CARTESIAN_POINT('Ctrl Pts',(12.4869739395021,0.680084118616307,7.06938967489226));
#56587=CARTESIAN_POINT('Ctrl Pts',(12.7744552727444,1.36652561897882,7.02619604729254));
#56588=CARTESIAN_POINT('Ctrl Pts',(13.269118044078,1.83350231786092,6.98300241969281));
#56589=CARTESIAN_POINT('Ctrl Pts',(13.8684511896637,2.39929103307328,6.93066904390873));
#56590=CARTESIAN_POINT('Ctrl Pts',(14.7719211435091,2.64291129119537,6.87833566812465));
#56591=CARTESIAN_POINT('Ctrl Pts',(15.5744528177492,2.45513481925728,6.82600229234056));
#56592=CARTESIAN_POINT('Ctrl Pts',(16.3769844919893,2.26735834731918,6.77366891655648));
#56593=CARTESIAN_POINT('Ctrl Pts',(17.0785778866242,1.64818514532091,6.72133554077239));
#56594=CARTESIAN_POINT('Ctrl Pts',(17.3646702383797,0.875224413728682,6.66900216498831));
#56595=CARTESIAN_POINT('Ctrl Pts',(17.6507625901351,0.102263682136454,6.61666878920422));
#56596=CARTESIAN_POINT('Ctrl Pts',(17.5213538990113,-0.82448457904973,6.56433541342014));
#56597=CARTESIAN_POINT('Ctrl Pts',(17.0344651712476,-1.48950819606356,6.51200203763606));
#56598=CARTESIAN_POINT('Ctrl Pts',(16.547576443484,-2.15453181307739,6.45966866185197));
#56599=CARTESIAN_POINT('Ctrl Pts',(15.7032076790805,-2.55783078591888,6.40733528606789));
#56600=CARTESIAN_POINT('Ctrl Pts',(14.8799356660918,-2.51858436884117,6.3550019102838));
#56601=CARTESIAN_POINT('Ctrl Pts',(14.0566636531032,-2.47933795176346,6.30266853449972));
#56602=CARTESIAN_POINT('Ctrl Pts',(13.2544883915292,-1.99754614476656,6.25033515871564));
#56603=CARTESIAN_POINT('Ctrl Pts',(12.8330690033158,-1.28922206392281,6.19800178293155));
#56604=CARTESIAN_POINT('Ctrl Pts',(12.6037889105156,-0.903846792801687,
6.16952895611836));
#56605=CARTESIAN_POINT('Ctrl Pts',(12.4872156605381,-0.451416121701059,
6.14105612930517));
#56606=CARTESIAN_POINT('Ctrl Pts',(12.4862854318642,0.000566909999415368,
6.11258330249198));
#56607=CARTESIAN_POINT('Ctrl Pts',(12.482920633805,0.00216662177004473,
6.38741669750803));
#56608=CARTESIAN_POINT('Ctrl Pts',(12.488315056143,-0.617887548426095,6.42660964589573));
#56609=CARTESIAN_POINT('Ctrl Pts',(12.7202541571503,-1.24155179185567,6.46580259428343));
#56610=CARTESIAN_POINT('Ctrl Pts',(13.1359015380453,-1.69788793113621,6.50499554267113));
#56611=CARTESIAN_POINT('Ctrl Pts',(13.6909052178623,-2.30722230487577,6.55732891845522));
#56612=CARTESIAN_POINT('Ctrl Pts',(14.5734534340258,-2.61821734233337,6.6096622942393));
#56613=CARTESIAN_POINT('Ctrl Pts',(15.3878514816524,-2.49143689543374,6.66199567002338));
#56614=CARTESIAN_POINT('Ctrl Pts',(16.2022495292791,-2.36465644853411,6.71432904580747));
#56615=CARTESIAN_POINT('Ctrl Pts',(16.9484974083689,-1.80010051727723,6.76666242159155));
#56616=CARTESIAN_POINT('Ctrl Pts',(17.2920112918525,-1.05089047753226,6.81899579737564));
#56617=CARTESIAN_POINT('Ctrl Pts',(17.635525175336,-0.301680437787271,6.87132917315973));
#56618=CARTESIAN_POINT('Ctrl Pts',(17.5763050632133,0.632183710445827,6.92366254894381));
#56619=CARTESIAN_POINT('Ctrl Pts',(17.1409025824082,1.33199950499447,6.97599592472789));
#56620=CARTESIAN_POINT('Ctrl Pts',(16.7055001016032,2.03181529954311,7.02832930051198));
#56621=CARTESIAN_POINT('Ctrl Pts',(15.8939152521159,2.49758274040729,7.08066267629606));
#56622=CARTESIAN_POINT('Ctrl Pts',(15.0700259913432,2.52047275706227,7.13299605208015));
#56623=CARTESIAN_POINT('Ctrl Pts',(14.2461367305706,2.54336277371724,7.18532942786423));
#56624=CARTESIAN_POINT('Ctrl Pts',(13.4099430585124,2.12337536616301,7.23766280364831));
#56625=CARTESIAN_POINT('Ctrl Pts',(12.9363564205467,1.44881390534349,7.2899961794324));
#56626=CARTESIAN_POINT('Ctrl Pts',(12.6424900625863,1.03024018763275,7.32246968545761));
#56627=CARTESIAN_POINT('Ctrl Pts',(12.4882403133338,0.513646402355209,7.35494319148282));
#56628=CARTESIAN_POINT('Ctrl Pts',(12.4854953774899,-0.00143787083715985,
7.38741669750803));
#56629=CARTESIAN_POINT('Origin',(15.,0.,7.5));
#56630=CARTESIAN_POINT('',(12.4785663033905,-0.000147683907944251,8.38741669750803));
#56631=CARTESIAN_POINT('',(12.4815651121962,0.00207920831391662,8.11258330249198));
#56632=CARTESIAN_POINT('',(12.4825,3.08304831685346E-16,7.5));
#56633=CARTESIAN_POINT('Ctrl Pts',(12.4815651121962,0.00207920831391661,
8.11258330249198));
#56634=CARTESIAN_POINT('Ctrl Pts',(12.4801423769425,0.163120151964822,8.10238997204752));
#56635=CARTESIAN_POINT('Ctrl Pts',(12.4942993050251,0.323912101526709,8.09219664160305));
#56636=CARTESIAN_POINT('Ctrl Pts',(12.524955296352,0.48149432911561,8.08200331115859));
#56637=CARTESIAN_POINT('Ctrl Pts',(12.6823456137647,1.29053412020584,8.0296699353745));
#56638=CARTESIAN_POINT('Ctrl Pts',(13.27463109749,2.01496955827445,7.97733655959042));
#56639=CARTESIAN_POINT('Ctrl Pts',(14.036257709891,2.32999653926404,7.92500318380634));
#56640=CARTESIAN_POINT('Ctrl Pts',(14.797884322292,2.64502352025364,7.87266980802225));
#56641=CARTESIAN_POINT('Ctrl Pts',(15.7288520633688,2.55064204416424,7.82033643223817));
#56642=CARTESIAN_POINT('Ctrl Pts',(16.4117570807264,2.08916849927148,7.76800305645408));
#56643=CARTESIAN_POINT('Ctrl Pts',(17.0946620980841,1.62769495437873,7.71566968067));
#56644=CARTESIAN_POINT('Ctrl Pts',(17.5295043917226,0.799129340682624,7.66333630488591));
#56645=CARTESIAN_POINT('Ctrl Pts',(17.5213203334702,-0.0250369758568184,
7.61100292910183));
#56646=CARTESIAN_POINT('Ctrl Pts',(17.5131362752179,-0.849203292396252,
7.55866955331774));
#56647=CARTESIAN_POINT('Ctrl Pts',(17.0619258650746,-1.66897031177902,7.50633617753366));
#56648=CARTESIAN_POINT('Ctrl Pts',(16.3699914547578,-2.11679155594354,7.45400280174958));
#56649=CARTESIAN_POINT('Ctrl Pts',(15.678057044441,-2.56461280010805,7.4016694259655));
#56650=CARTESIAN_POINT('Ctrl Pts',(14.7453986339507,-2.6404882690543,7.34933605018141));
#56651=CARTESIAN_POINT('Ctrl Pts',(13.9901780954356,-2.31039883752012,7.29700267439732));
#56652=CARTESIAN_POINT('Ctrl Pts',(13.2349575569204,-1.98030940598595,7.24466929861324));
#56653=CARTESIAN_POINT('Ctrl Pts',(12.6571748903804,-1.24425507397135,7.19233592282916));
#56654=CARTESIAN_POINT('Ctrl Pts',(12.5158817257734,-0.43224932181273,7.14000254704507));
#56655=CARTESIAN_POINT('Ctrl Pts',(12.4912056194582,-0.29043679801142,7.13086279886071));
#56656=CARTESIAN_POINT('Ctrl Pts',(12.4798427838735,-0.146307696573625,
7.12172305067635));
#56657=CARTESIAN_POINT('Ctrl Pts',(12.4810882026093,-0.00198272270578489,
7.11258330249199));
#56658=CARTESIAN_POINT('Ctrl Pts',(12.4854953774899,-0.00143787083715985,
7.38741669750803));
#56659=CARTESIAN_POINT('Ctrl Pts',(12.4838166530455,-0.316448716062932,
7.4072765672669));
#56660=CARTESIAN_POINT('Ctrl Pts',(12.5388037075173,-0.630894974090679,
7.42713643702578));
#56661=CARTESIAN_POINT('Ctrl Pts',(12.6531758459131,-0.922010273445696,
7.44699630678465));
#56662=CARTESIAN_POINT('Ctrl Pts',(12.9545615131189,-1.68913747733048,7.49932968256874));
#56663=CARTESIAN_POINT('Ctrl Pts',(13.6683124514037,-2.29425637101525,7.55166305835282));
#56664=CARTESIAN_POINT('Ctrl Pts',(14.474415004267,-2.46605899527454,7.6039964341369));
#56665=CARTESIAN_POINT('Ctrl Pts',(15.2805175571303,-2.63786161953383,7.65632980992099));
#56666=CARTESIAN_POINT('Ctrl Pts',(16.1789717245721,-2.37634797436764,7.70866318570507));
#56667=CARTESIAN_POINT('Ctrl Pts',(16.766951270731,-1.79876895739606,7.76099656148916));
#56668=CARTESIAN_POINT('Ctrl Pts',(17.35493081689,-1.22118994042448,7.81332993727324));
#56669=CARTESIAN_POINT('Ctrl Pts',(17.6324357417662,-0.327545551647488,
7.86566331305733));
#56670=CARTESIAN_POINT('Ctrl Pts',(17.4750453812635,0.48149446094025,7.91799668884141));
#56671=CARTESIAN_POINT('Ctrl Pts',(17.3176550207607,1.290534473528,7.97033006462549));
#56672=CARTESIAN_POINT('Ctrl Pts',(16.7253693748791,2.01497010992651,8.02266344040958));
#56673=CARTESIAN_POINT('Ctrl Pts',(15.9637425539609,2.32999717716545,8.07499681619367));
#56674=CARTESIAN_POINT('Ctrl Pts',(15.2021157330427,2.64502424440439,8.12733019197775));
#56675=CARTESIAN_POINT('Ctrl Pts',(14.271147737088,2.55064274248376,8.17966356776183));
#56676=CARTESIAN_POINT('Ctrl Pts',(13.5882425327649,2.08916907124602,8.23199694354592));
#56677=CARTESIAN_POINT('Ctrl Pts',(12.9122114961964,1.63234062369425,8.28380352819995));
#56678=CARTESIAN_POINT('Ctrl Pts',(12.4792743543203,0.815773157793952,8.33561011285399));
#56679=CARTESIAN_POINT('Ctrl Pts',(12.4785663033905,-0.000147683907944251,
8.38741669750803));
#56680=CARTESIAN_POINT('Origin',(15.,0.,7.5));
#56681=CARTESIAN_POINT('',(12.4851788739807,0.00162480267774629,9.38741669750802));
#56682=CARTESIAN_POINT('',(12.486145438329,-0.000815058042068406,9.11258330249198));
#56683=CARTESIAN_POINT('',(12.4825,3.08304831685346E-16,7.5));
#56684=CARTESIAN_POINT('Ctrl Pts',(12.486145438329,-0.000815058042068406,
9.11258330249198));
#56685=CARTESIAN_POINT('Ctrl Pts',(12.4875376300823,0.467827170949961,9.08305689341869));
#56686=CARTESIAN_POINT('Ctrl Pts',(12.6134446697461,0.937164267550756,9.0535304843454));
#56687=CARTESIAN_POINT('Ctrl Pts',(12.8590980037376,1.33199914029708,9.02400407527211));
#56688=CARTESIAN_POINT('Ctrl Pts',(13.2945003653482,2.03181474323085,8.97167069948803));
#56689=CARTESIAN_POINT('Ctrl Pts',(14.1060849926179,2.49758205662421,8.91933732370394));
#56690=CARTESIAN_POINT('Ctrl Pts',(14.9299740278219,2.52047206702312,8.86700394791986));
#56691=CARTESIAN_POINT('Ctrl Pts',(15.753863063026,2.54336207742203,8.81467057213577));
#56692=CARTESIAN_POINT('Ctrl Pts',(16.5900565061644,2.12337478482649,8.76233719635169));
#56693=CARTESIAN_POINT('Ctrl Pts',(17.063643014475,1.44881350868189,8.7100038205676));
#56694=CARTESIAN_POINT('Ctrl Pts',(17.5372295227856,0.774252232537298,8.65767044478352));
#56695=CARTESIAN_POINT('Ctrl Pts',(17.6482090962684,-0.154883027156347,
8.60533706899943));
#56696=CARTESIAN_POINT('Ctrl Pts',(17.3468235115742,-0.922010021015011,
8.55300369321535));
#56697=CARTESIAN_POINT('Ctrl Pts',(17.0454379268799,-1.68913701487367,8.50067031743127));
#56698=CARTESIAN_POINT('Ctrl Pts',(16.3316871840086,-2.29425574289735,8.44833694164718));
#56699=CARTESIAN_POINT('Ctrl Pts',(15.5255848518399,-2.46605832012208,8.3960035658631));
#56700=CARTESIAN_POINT('Ctrl Pts',(14.7194825196712,-2.6378608973468,8.34367019007902));
#56701=CARTESIAN_POINT('Ctrl Pts',(13.8210285982051,-2.37634732377256,8.29133681429493));
#56702=CARTESIAN_POINT('Ctrl Pts',(13.2330492130222,-1.79876846492951,8.23900343851085));
#56703=CARTESIAN_POINT('Ctrl Pts',(12.7595946043877,-1.33368860080475,8.19686339317123));
#56704=CARTESIAN_POINT('Ctrl Pts',(12.4874468138073,-0.663676964701131,
8.1547233478316));
#56705=CARTESIAN_POINT('Ctrl Pts',(12.4815651121962,0.00207920831391661,
8.11258330249198));
#56706=CARTESIAN_POINT('Ctrl Pts',(12.4785663033905,-0.000147683907944251,
8.38741669750803));
#56707=CARTESIAN_POINT('Ctrl Pts',(12.478559103631,-0.0084443100048087,
8.38794348863808));
#56708=CARTESIAN_POINT('Ctrl Pts',(12.4785965949646,-0.016740869242818,
8.38847027976812));
#56709=CARTESIAN_POINT('Ctrl Pts',(12.4786789762444,-0.0250369827190495,
8.38899707089817));
#56710=CARTESIAN_POINT('Ctrl Pts',(12.4868630367383,-0.84920352489154,8.44133044668226));
#56711=CARTESIAN_POINT('Ctrl Pts',(12.9380735704173,-1.66897076868167,8.49366382246634));
#56712=CARTESIAN_POINT('Ctrl Pts',(13.6300081701693,-2.11679213546203,8.54599719825043));
#56713=CARTESIAN_POINT('Ctrl Pts',(14.3219427699214,-2.5646135022424,8.59833057403451));
#56714=CARTESIAN_POINT('Ctrl Pts',(15.2546014357464,-2.64048899201301,8.65066394981859));
#56715=CARTESIAN_POINT('Ctrl Pts',(16.0098221810285,-2.31039947008532,8.70299732560268));
#56716=CARTESIAN_POINT('Ctrl Pts',(16.7650429263106,-1.98030994815763,8.75533070138676));
#56717=CARTESIAN_POINT('Ctrl Pts',(17.3428257510498,-1.24425541453165,8.80766407717086));
#56718=CARTESIAN_POINT('Ctrl Pts',(17.4841189543331,-0.432249440103775,
8.85999745295494));
#56719=CARTESIAN_POINT('Ctrl Pts',(17.6254121576165,0.379756534324098,8.91233082873902));
#56720=CARTESIAN_POINT('Ctrl Pts',(17.3302157394439,1.26771394955386,8.9646642045231));
#56721=CARTESIAN_POINT('Ctrl Pts',(16.7308824297867,1.83350281974262,9.01699758030718));
#56722=CARTESIAN_POINT('Ctrl Pts',(16.1315491201295,2.39929168993138,9.06933095609127));
#56723=CARTESIAN_POINT('Ctrl Pts',(15.2280789189876,2.64291201507916,9.12166433187536));
#56724=CARTESIAN_POINT('Ctrl Pts',(14.4255470250055,2.45513549159302,9.17399770765945));
#56725=CARTESIAN_POINT('Ctrl Pts',(13.6230151310234,2.26735896810689,9.22633108344353));
#56726=CARTESIAN_POINT('Ctrl Pts',(12.9214215442012,1.64818559598687,9.2786644592276));
#56727=CARTESIAN_POINT('Ctrl Pts',(12.6353291141696,0.875224653029136,9.33099783501169));
#56728=CARTESIAN_POINT('Ctrl Pts',(12.5325202200407,0.597456870981902,9.34980412251047));
#56729=CARTESIAN_POINT('Ctrl Pts',(12.4833676454127,0.29982951718309,9.36861041000924));
#56730=CARTESIAN_POINT('Ctrl Pts',(12.4851788739807,0.00162480267774629,
9.38741669750802));
#56731=CARTESIAN_POINT('Origin',(15.,0.,7.5));
#56732=CARTESIAN_POINT('',(12.4833920687165,-0.00213593309729046,10.387416697508));
#56733=CARTESIAN_POINT('',(12.4790122776664,-0.000936909191352325,10.112583302492));
#56734=CARTESIAN_POINT('',(12.4825,3.08304831685346E-16,7.5));
#56735=CARTESIAN_POINT('Ctrl Pts',(12.4790122776664,-0.000936909191352325,
10.112583302492));
#56736=CARTESIAN_POINT('Ctrl Pts',(12.4827416706421,0.768933033990792,10.0637238147899));
#56737=CARTESIAN_POINT('Ctrl Pts',(12.8617552362247,1.54198463745441,10.0148643270877));
#56738=CARTESIAN_POINT('Ctrl Pts',(13.4744240244193,2.00756086084053,9.96600483938563));
#56739=CARTESIAN_POINT('Ctrl Pts',(14.1306532939369,2.50623934889895,9.91367146360154));
#56740=CARTESIAN_POINT('Ctrl Pts',(15.0549445147503,2.65216539497217,9.86133808781746));
#56741=CARTESIAN_POINT('Ctrl Pts',(15.8328874429565,2.37991212159725,9.80900471203338));
#56742=CARTESIAN_POINT('Ctrl Pts',(16.6108303711627,2.10765884822232,9.75667133624929));
#56743=CARTESIAN_POINT('Ctrl Pts',(17.2424250067619,1.41722625539925,9.70433796046521));
#56744=CARTESIAN_POINT('Ctrl Pts',(17.4444927838351,0.618173228507267,9.65200458468112));
#56745=CARTESIAN_POINT('Ctrl Pts',(17.6465605609084,-0.18087979838472,9.59967120889704));
#56746=CARTESIAN_POINT('Ctrl Pts',(17.4191014794558,-1.08855325934562,9.54733783311295));
#56747=CARTESIAN_POINT('Ctrl Pts',(16.8640979515296,-1.69788746613335,9.49500445732887));
#56748=CARTESIAN_POINT('Ctrl Pts',(16.3090944236034,-2.30722167292107,9.44267108154478));
#56749=CARTESIAN_POINT('Ctrl Pts',(15.4265464492036,-2.61821662553562,9.3903377057607));
#56750=CARTESIAN_POINT('Ctrl Pts',(14.6121486245737,-2.49143621341537,9.33800432997662));
#56751=CARTESIAN_POINT('Ctrl Pts',(13.7977507999438,-2.36465580129513,9.28567095419253));
#56752=CARTESIAN_POINT('Ctrl Pts',(13.0515031250838,-1.80010002444009,9.23333757840845));
#56753=CARTESIAN_POINT('Ctrl Pts',(12.7079893356296,-1.05089018977548,9.18100420262436));
#56754=CARTESIAN_POINT('Ctrl Pts',(12.5582854909339,-0.724383376435316,
9.15819723591357));
#56755=CARTESIAN_POINT('Ctrl Pts',(12.4850700731909,-0.362806510824638,
9.13539026920278));
#56756=CARTESIAN_POINT('Ctrl Pts',(12.486145438329,-0.000815058042068406,
9.11258330249198));
#56757=CARTESIAN_POINT('Ctrl Pts',(12.4851788739807,0.00162480267774629,
9.38741669750802));
#56758=CARTESIAN_POINT('Ctrl Pts',(12.4884078589736,-0.530002494361348,
9.42094378579333));
#56759=CARTESIAN_POINT('Ctrl Pts',(12.6536116109961,-1.06346477741145,9.45447087407864));
#56760=CARTESIAN_POINT('Ctrl Pts',(12.9655342718635,-1.48950860327335,9.48799796236395));
#56761=CARTESIAN_POINT('Ctrl Pts',(13.4524231328298,-2.15453240282264,9.54033133814804));
#56762=CARTESIAN_POINT('Ctrl Pts',(14.2967921280032,-2.55783148812579,9.59266471393212));
#56763=CARTESIAN_POINT('Ctrl Pts',(15.1200643665754,-2.51858505945467,9.6449980897162));
#56764=CARTESIAN_POINT('Ctrl Pts',(15.9433366051476,-2.47933863078355,9.69733146550028));
#56765=CARTESIAN_POINT('Ctrl Pts',(16.7455120871185,-1.99754668813814,9.74966484128436));
#56766=CARTESIAN_POINT('Ctrl Pts',(17.1669315903404,-1.28922241490791,9.80199821706845));
#56767=CARTESIAN_POINT('Ctrl Pts',(17.5883510935622,-0.580898141677671,
9.85433159285254));
#56768=CARTESIAN_POINT('Ctrl Pts',(17.6290146180349,0.353958462137397,9.90666496863663));
#56769=CARTESIAN_POINT('Ctrl Pts',(17.2706904715522,1.09619889141998,9.95899834442071));
#56770=CARTESIAN_POINT('Ctrl Pts',(16.9123663250695,1.83843932070257,10.0113317202048));
#56771=CARTESIAN_POINT('Ctrl Pts',(16.1550545076315,2.38806357545267,10.0636650959889));
#56772=CARTESIAN_POINT('Ctrl Pts',(15.3382994168527,2.49864705542611,10.115998471773));
#56773=CARTESIAN_POINT('Ctrl Pts',(14.5215443260739,2.60923053539955,10.168331847557));
#56774=CARTESIAN_POINT('Ctrl Pts',(13.6453459619542,2.28077324059635,10.2206652233411));
#56775=CARTESIAN_POINT('Ctrl Pts',(13.1025520413601,1.66053653868267,10.2729985991252));
#56776=CARTESIAN_POINT('Ctrl Pts',(12.7069762589991,1.20852223030592,10.3111379652528));
#56777=CARTESIAN_POINT('Ctrl Pts',(12.4884769342622,0.601539190041919,10.3492773313804));
#56778=CARTESIAN_POINT('Ctrl Pts',(12.4833920687165,-0.00213593309729046,
10.387416697508));
#56779=CARTESIAN_POINT('Origin',(15.,0.,7.5));
#56780=CARTESIAN_POINT('',(12.4794948718273,0.00124609658704006,11.387416697508));
#56781=CARTESIAN_POINT('',(12.4841021658346,0.00201143405015815,11.112583302492));
#56782=CARTESIAN_POINT('',(12.4825,3.08304831685346E-16,7.5));
#56783=CARTESIAN_POINT('',(16.9134659966651,1.63598720337492,12.));
#56784=CARTESIAN_POINT('Ctrl Pts',(12.4794948718273,0.00124609658704006,
11.387416697508));
#56785=CARTESIAN_POINT('Ctrl Pts',(12.4843009282632,-0.742606326482963,
11.4346110043198));
#56786=CARTESIAN_POINT('Ctrl Pts',(12.8347911135691,-1.49019380442116,11.4818053111315));
#56787=CARTESIAN_POINT('Ctrl Pts',(13.4121725655462,-1.95845906653105,11.5289996179432));
#56788=CARTESIAN_POINT('Ctrl Pts',(14.0524260736147,-2.47771453576351,11.5813329937273));
#56789=CARTESIAN_POINT('Ctrl Pts',(14.971674348053,-2.65350400257885,11.6336663695114));
#56790=CARTESIAN_POINT('Ctrl Pts',(15.7577964008607,-2.4053165320775,11.6859997452955));
#56791=CARTESIAN_POINT('Ctrl Pts',(16.5439184536685,-2.15712906157615,11.7383331210796));
#56792=CARTESIAN_POINT('Ctrl Pts',(17.1969142848456,-1.4849646537581,11.7906664968637));
#56793=CARTESIAN_POINT('Ctrl Pts',(17.4237876204482,-0.693982202234524,
11.8429998726477));
#56794=CARTESIAN_POINT('Ctrl Pts',(17.6506609560507,0.0970002492890512,
11.8953332484318));
#56795=CARTESIAN_POINT('Ctrl Pts',(17.4514117960785,1.00680074451815,11.9476666242159));
#56796=CARTESIAN_POINT('Ctrl Pts',(16.9134659966651,1.63598720337493,12.));
#56797=CARTESIAN_POINT('',(13.0830107080184,1.63831915944298,12.));
#56798=CARTESIAN_POINT('Origin',(15.,0.,12.));
#56799=CARTESIAN_POINT('Ctrl Pts',(13.0829974340784,1.63832794503776,12.));
#56800=CARTESIAN_POINT('Ctrl Pts',(13.5967216860793,2.23547110522819,11.9500021225376));
#56801=CARTESIAN_POINT('Ctrl Pts',(14.4140905740858,2.57572139725963,11.9000042450751));
#56802=CARTESIAN_POINT('Ctrl Pts',(15.1991791514308,2.51337952595466,11.8500063676127));
#56803=CARTESIAN_POINT('Ctrl Pts',(16.0209407466675,2.44812554431239,11.7976729918286));
#56804=CARTESIAN_POINT('Ctrl Pts',(16.8073358429282,1.94178921121356,11.7453396160445));
#56805=CARTESIAN_POINT('Ctrl Pts',(17.2062539503585,1.22068465472099,11.6930062402604));
#56806=CARTESIAN_POINT('Ctrl Pts',(17.6051720577887,0.499580098228415,11.6406728644763));
#56807=CARTESIAN_POINT('Ctrl Pts',(17.6166131763885,-0.436292681657898,
11.5883394886922));
#56808=CARTESIAN_POINT('Ctrl Pts',(17.2352051529428,-1.16697139580525,11.5360061129082));
#56809=CARTESIAN_POINT('Ctrl Pts',(16.853797129497,-1.8976501099526,11.4836727371241));
#56810=CARTESIAN_POINT('Ctrl Pts',(16.0795399640059,-2.42313475836099,11.43133936134));
#56811=CARTESIAN_POINT('Ctrl Pts',(15.259700012361,-2.508006015706,11.3790059855559));
#56812=CARTESIAN_POINT('Ctrl Pts',(14.439860060716,-2.59287727305101,11.3266726097718));
#56813=CARTESIAN_POINT('Ctrl Pts',(13.5744373229174,-2.23713513933264,11.2743392339877));
#56814=CARTESIAN_POINT('Ctrl Pts',(13.0513843414681,-1.60018372469102,11.2220058582037));
#56815=CARTESIAN_POINT('Ctrl Pts',(12.6868381785572,-1.15625509336019,11.1855316729664));
#56816=CARTESIAN_POINT('Ctrl Pts',(12.488598465426,-0.575728774038117,11.1490574877292));
#56817=CARTESIAN_POINT('Ctrl Pts',(12.4841021658346,0.00201143405015815,
11.112583302492));
#56818=CARTESIAN_POINT('Origin',(15.,0.,14.2084234471775));
#56819=CARTESIAN_POINT('',(11.9225958479619,0.00147606609843115,4.79157655282255));
#56820=CARTESIAN_POINT('',(11.9313248632922,-0.000102231845577353,4.70842344717745));
#56821=CARTESIAN_POINT('',(11.9265,6.70613782525944E-14,14.2084234471775));
#56822=CARTESIAN_POINT('',(15.7937992825329,-2.9692229537457,4.));
#56823=CARTESIAN_POINT('Ctrl Pts',(11.9313248632922,-0.000102231845577234,
4.70842344717745));
#56824=CARTESIAN_POINT('Ctrl Pts',(11.9316626296779,0.519548226111607,4.68161580125464));
#56825=CARTESIAN_POINT('Ctrl Pts',(12.3017104806267,2.0539878015009,4.60247477954774));
#56826=CARTESIAN_POINT('Ctrl Pts',(14.713653685934,3.60697232347283,4.47100038205677));
#56827=CARTESIAN_POINT('Ctrl Pts',(17.8529409071999,2.23046453345384,4.3140002547045));
#56828=CARTESIAN_POINT('Ctrl Pts',(18.4294036968932,-1.15306868324745,4.15700012735226));
#56829=CARTESIAN_POINT('Ctrl Pts',(16.7701400584231,-2.7082056372685,4.05233337578409));
#56830=CARTESIAN_POINT('Ctrl Pts',(15.7937992825329,-2.9692229537457,4.));
#56831=CARTESIAN_POINT('',(14.2042685477155,-2.9740056618826,4.));
#56832=CARTESIAN_POINT('Origin',(15.,0.,4.));
#56833=CARTESIAN_POINT('Ctrl Pts',(11.9225958479619,0.00147606609843164,
4.79157655282255));
#56834=CARTESIAN_POINT('Ctrl Pts',(11.9220803947843,0.0885957531718082,
4.78704908248048));
#56835=CARTESIAN_POINT('Ctrl Pts',(11.9646120017673,1.18222348786824,4.73018823635433));
#56836=CARTESIAN_POINT('Ctrl Pts',(13.2680522040149,3.17774609218688,4.62099401444409));
#56837=CARTESIAN_POINT('Ctrl Pts',(16.6951963308219,3.19795784272698,4.46399388709183));
#56838=CARTESIAN_POINT('Ctrl Pts',(18.6022504225887,0.349454018091392,4.30699375973959));
#56839=CARTESIAN_POINT('Ctrl Pts',(17.2987966073653,-2.76330605967289,4.15232913070897));
#56840=CARTESIAN_POINT('Ctrl Pts',(15.1340732479013,-3.21955219912907,4.04999787746244));
#56841=CARTESIAN_POINT('Ctrl Pts',(14.2042612683071,-2.97402368063355,4.));
#56842=CARTESIAN_POINT('Origin',(15.,0.,14.2084234471775));
#56843=CARTESIAN_POINT('',(11.9311214597158,0.000692114352876805,5.79157655282255));
#56844=CARTESIAN_POINT('',(11.9232839890155,-0.001880590663607,5.70842344717745));
#56845=CARTESIAN_POINT('',(11.9265,6.70613782525944E-14,14.2084234471775));
#56846=CARTESIAN_POINT('Ctrl Pts',(11.9232839890155,-0.00188059066360697,
5.70842344717745));
#56847=CARTESIAN_POINT('Ctrl Pts',(11.9297313241637,0.88651553618964,5.66228272262581));
#56848=CARTESIAN_POINT('Ctrl Pts',(12.7977715060129,2.79354605065376,5.56380862229009));
#56849=CARTESIAN_POINT('Ctrl Pts',(16.0189351514379,3.47279968000896,5.41300114617029));
#56850=CARTESIAN_POINT('Ctrl Pts',(18.4587231497003,1.06591431050395,5.25600101881802));
#56851=CARTESIAN_POINT('Ctrl Pts',(17.7969596462713,-2.29690631906584,5.09900089146578));
#56852=CARTESIAN_POINT('Ctrl Pts',(14.6272939950368,-3.59983577334609,4.94200076411352));
#56853=CARTESIAN_POINT('Ctrl Pts',(12.2757333222409,-2.00384044231271,4.81180828268409));
#56854=CARTESIAN_POINT('Ctrl Pts',(11.9310032485729,-0.494903500494573,
4.73394917703873));
#56855=CARTESIAN_POINT('Ctrl Pts',(11.9313248632922,-0.000102231845577234,
4.70842344717745));
#56856=CARTESIAN_POINT('Ctrl Pts',(11.9311214597158,0.000692114352877186,
5.79157655282255));
#56857=CARTESIAN_POINT('Ctrl Pts',(11.930169752624,0.463111161065124,5.76771600385165));
#56858=CARTESIAN_POINT('Ctrl Pts',(12.2437393113606,1.9385290048203,5.69152207909668));
#56859=CARTESIAN_POINT('Ctrl Pts',(14.5144143770745,3.58648699137295,5.56299477855761));
#56860=CARTESIAN_POINT('Ctrl Pts',(17.7235443678513,2.3834921742297,5.40599465120536));
#56861=CARTESIAN_POINT('Ctrl Pts',(18.4904461542425,-0.956822661448993,
5.2489945238531));
#56862=CARTESIAN_POINT('Ctrl Pts',(16.1274310791049,-3.43910703392132,5.09199439650085));
#56863=CARTESIAN_POINT('Ctrl Pts',(12.8507354093227,-2.85493220992714,4.93952173949066));
#56864=CARTESIAN_POINT('Ctrl Pts',(11.9280385574681,-0.918427369528735,
4.83938245826456));
#56865=CARTESIAN_POINT('Ctrl Pts',(11.9225958479619,0.00147606609843164,
4.79157655282255));
#56866=CARTESIAN_POINT('Origin',(15.,0.,14.2084234471775));
#56867=CARTESIAN_POINT('',(11.9247764014775,-0.00242061498952145,6.79157655282255));
#56868=CARTESIAN_POINT('',(11.9270135324726,0.00264512890178066,6.70842344717746));
#56869=CARTESIAN_POINT('',(11.9265,6.70613782525944E-14,14.2084234471775));
#56870=CARTESIAN_POINT('Ctrl Pts',(11.9270135324726,0.00264512890178106,
6.70842344717746));
#56871=CARTESIAN_POINT('Ctrl Pts',(11.9248054756842,0.256447062439599,6.69528301978107));
#56872=CARTESIAN_POINT('Ctrl Pts',(12.0687133238052,1.518578012587,6.62980921660061));
#56873=CARTESIAN_POINT('Ctrl Pts',(13.8044957855091,3.41606212207931,6.51200203763605));
#56874=CARTESIAN_POINT('Ctrl Pts',(17.1897706782275,2.88159878204111,6.35500191028381));
#56875=CARTESIAN_POINT('Ctrl Pts',(18.6114579568395,-0.236820710438023,
6.19800178293155));
#56876=CARTESIAN_POINT('Ctrl Pts',(16.7947147560542,-3.14288298322814,6.04100165557929));
#56877=CARTESIAN_POINT('Ctrl Pts',(13.3686365056666,-3.23068767821543,5.88400152822705));
#56878=CARTESIAN_POINT('Ctrl Pts',(11.9823834565481,-1.24709989542488,5.77314212542643));
#56879=CARTESIAN_POINT('Ctrl Pts',(11.9224186775506,-0.121114248637474,
5.7146160984099));
#56880=CARTESIAN_POINT('Ctrl Pts',(11.9232839890155,-0.00188059066360697,
5.70842344717745));
#56881=CARTESIAN_POINT('Ctrl Pts',(11.9247764014775,-0.00242061498952133,
6.79157655282255));
#56882=CARTESIAN_POINT('Ctrl Pts',(11.9319620270346,0.830283431407061,6.74838292522283));
#56883=CARTESIAN_POINT('Ctrl Pts',(12.7081731527432,2.68370300380156,6.65285592183902));
#56884=CARTESIAN_POINT('Ctrl Pts',(15.824553937525,3.52403365117268,6.50499554267113));
#56885=CARTESIAN_POINT('Ctrl Pts',(18.3941832901488,1.25627336953411,6.34799541531888));
#56886=CARTESIAN_POINT('Ctrl Pts',(17.9202159270872,-2.13799965619268,6.19099528796662));
#56887=CARTESIAN_POINT('Ctrl Pts',(14.8276629212552,-3.61510717519363,6.03399516061437));
#56888=CARTESIAN_POINT('Ctrl Pts',(12.3361598311427,-2.11869381838128,5.90085558223301));
#56889=CARTESIAN_POINT('Ctrl Pts',(11.9322571331336,-0.551113187705301,
5.82004937963574));
#56890=CARTESIAN_POINT('Ctrl Pts',(11.9311214597158,0.000692114352877186,
5.79157655282255));
#56891=CARTESIAN_POINT('Origin',(15.,0.,14.2084234471775));
#56892=CARTESIAN_POINT('',(11.9253586384648,0.00253840983232584,7.79157655282255));
#56893=CARTESIAN_POINT('',(11.9301569186554,-0.00175543039446494,7.70842344717746));
#56894=CARTESIAN_POINT('',(11.9265,6.70613782525944E-14,14.2084234471775));
#56895=CARTESIAN_POINT('Ctrl Pts',(11.9301569186554,-0.00175543039446478,
7.70842344717746));
#56896=CARTESIAN_POINT('Ctrl Pts',(11.9335080846202,0.627087276122613,7.67594994115225));
#56897=CARTESIAN_POINT('Ctrl Pts',(12.425309891706,2.27416779560488,7.59114305934296));
#56898=CARTESIAN_POINT('Ctrl Pts',(15.1005134031695,3.61781798694653,7.45400280174957));
#56899=CARTESIAN_POINT('Ctrl Pts',(18.0729932858696,1.91191582667314,7.29700267439733));
#56900=CARTESIAN_POINT('Ctrl Pts',(18.2898906220475,-1.50841957701434,7.14000254704506));
#56901=CARTESIAN_POINT('Ctrl Pts',(15.5567114486024,-3.57614071471203,6.98300241969282));
#56902=CARTESIAN_POINT('Ctrl Pts',(12.5948647250275,-2.532436114927,6.83914271973694));
#56903=CARTESIAN_POINT('Ctrl Pts',(11.9335993346794,-0.754350498545223,
6.74761639556516));
#56904=CARTESIAN_POINT('Ctrl Pts',(11.9270135324726,0.00264512890178106,
6.70842344717746));
#56905=CARTESIAN_POINT('Ctrl Pts',(11.9253586384648,0.00253840983232619,
7.79157655282255));
#56906=CARTESIAN_POINT('Ctrl Pts',(11.9236216864083,0.199145893570575,7.78138322237808));
#56907=CARTESIAN_POINT('Ctrl Pts',(12.0296403223963,1.40328729141077,7.71885651614953));
#56908=CARTESIAN_POINT('Ctrl Pts',(13.6166705510885,3.34441360725337,7.60399643413689));
#56909=CARTESIAN_POINT('Ctrl Pts',(17.0263976837988,2.99873559323853,7.44699630678466));
#56910=CARTESIAN_POINT('Ctrl Pts',(18.6190345729722,-0.0359373922966709,
7.2899961794324));
#56911=CARTESIAN_POINT('Ctrl Pts',(16.9664484412042,-3.03838498006983,7.13299605208014));
#56912=CARTESIAN_POINT('Ctrl Pts',(13.5505291268344,-3.3162835943375,6.97599592472789));
#56913=CARTESIAN_POINT('Ctrl Pts',(12.0165601959407,-1.36211545786235,6.86218942497536));
#56914=CARTESIAN_POINT('Ctrl Pts',(11.923255927005,-0.178620339789062,6.80071630100691));
#56915=CARTESIAN_POINT('Ctrl Pts',(11.9247764014775,-0.00242061498952133,
6.79157655282255));
#56916=CARTESIAN_POINT('Origin',(15.,0.,14.2084234471775));
#56917=CARTESIAN_POINT('',(11.9309505480454,-0.000995066888654084,8.79157655282255));
#56918=CARTESIAN_POINT('',(11.9216975306736,-0.000180300492997754,8.70842344717746));
#56919=CARTESIAN_POINT('',(11.9265,6.70613782525944E-14,14.2084234471775));
#56920=CARTESIAN_POINT('Ctrl Pts',(11.9216975306736,-0.000180300492997622,
8.70842344717746));
#56921=CARTESIAN_POINT('Ctrl Pts',(11.9225619574989,0.995939940607609,8.65661686252342));
#56922=CARTESIAN_POINT('Ctrl Pts',(12.9850426088341,2.99989628694768,8.5524769020853));
#56923=CARTESIAN_POINT('Ctrl Pts',(16.383329827636,3.34441452287188,8.39600356586309));
#56924=CARTESIAN_POINT('Ctrl Pts',(18.5526127662067,0.691124042072478,8.23900343851084));
#56925=CARTESIAN_POINT('Ctrl Pts',(17.5362337553543,-2.58190399634584,8.08200331115859));
#56926=CARTESIAN_POINT('Ctrl Pts',(14.2455896040548,-3.53971395275292,7.92500318380633));
#56927=CARTESIAN_POINT('Ctrl Pts',(12.1721380845128,-1.78183929043833,7.8004765624793));
#56928=CARTESIAN_POINT('Ctrl Pts',(11.928107441166,-0.386337687713779,7.72828331693634));
#56929=CARTESIAN_POINT('Ctrl Pts',(11.9301569186554,-0.00175543039446478,
7.70842344717746));
#56930=CARTESIAN_POINT('Ctrl Pts',(11.9309505480454,-0.000995066888653875,
8.79157655282255));
#56931=CARTESIAN_POINT('Ctrl Pts',(11.9326502109465,0.571148683183627,8.76205014374926));
#56932=CARTESIAN_POINT('Ctrl Pts',(12.3588112254404,2.15972684180816,8.68019035889189));
#56933=CARTESIAN_POINT('Ctrl Pts',(14.8994866243195,3.61781699652394,8.54599719825042));
#56934=CARTESIAN_POINT('Ctrl Pts',(17.9620970086125,2.07958747065415,8.38899707089818));
#56935=CARTESIAN_POINT('Ctrl Pts',(18.3685665845007,-1.32342808525659,8.23199694354591));
#56936=CARTESIAN_POINT('Ctrl Pts',(15.7544101894084,-3.53971298366467,8.07499681619367));
#56937=CARTESIAN_POINT('Ctrl Pts',(12.6774139888043,-2.64408967670503,7.92819001928588));
#56938=CARTESIAN_POINT('Ctrl Pts',(11.932539337532,-0.810252691562618,7.83371659816217));
#56939=CARTESIAN_POINT('Ctrl Pts',(11.9253586384648,0.00253840983232619,
7.79157655282255));
#56940=CARTESIAN_POINT('Origin',(15.,0.,14.2084234471775));
#56941=CARTESIAN_POINT('',(11.9222420001619,-0.00114382935434674,9.79157655282255));
#56942=CARTESIAN_POINT('',(11.9297705140734,0.00198364688382296,9.70842344717746));
#56943=CARTESIAN_POINT('',(11.9265,6.70613782525944E-14,14.2084234471775));
#56944=CARTESIAN_POINT('Ctrl Pts',(11.9297705140734,0.00198364688382347,
9.70842344717746));
#56945=CARTESIAN_POINT('Ctrl Pts',(11.9275592683916,0.36604807192143,9.68961715967868));
#56946=CARTESIAN_POINT('Ctrl Pts',(12.1545555502906,1.7405498801195,9.61847749639582));
#56947=CARTESIAN_POINT('Ctrl Pts',(14.1754458368614,3.52403461675767,9.49500445732887));
#56948=CARTESIAN_POINT('Ctrl Pts',(17.4844615229107,2.63176005547664,9.33800432997661));
#56949=CARTESIAN_POINT('Ctrl Pts',(18.565636725993,-0.620439089359897,9.18100420262437));
#56950=CARTESIAN_POINT('Ctrl Pts',(16.4494712699821,-3.31628450238807,9.0240040752721));
#56951=CARTESIAN_POINT('Ctrl Pts',(13.033551020433,-3.03838581184986,8.86700394791986));
#56952=CARTESIAN_POINT('Ctrl Pts',(11.9262816166307,-1.02667925906391,8.76181040522164));
#56953=CARTESIAN_POINT('Ctrl Pts',(11.9216887408183,-0.0103092698311159,
8.70895023830751));
#56954=CARTESIAN_POINT('Ctrl Pts',(11.9216975306736,-0.000180300492997622,
8.70842344717746));
#56955=CARTESIAN_POINT('Ctrl Pts',(11.9222420001619,-0.00114382935434687,
9.79157655282255));
#56956=CARTESIAN_POINT('Ctrl Pts',(11.9267950445754,0.938754987078744,9.74271706512043));
#56957=CARTESIAN_POINT('Ctrl Pts',(12.8851347215443,2.89342387288723,9.64152420163423));
#56958=CARTESIAN_POINT('Ctrl Pts',(16.1955038860992,3.41606118929613,9.48799796236394));
#56959=CARTESIAN_POINT('Ctrl Pts',(18.5087584392439,0.887308966009096,9.3309978350117));
#56960=CARTESIAN_POINT('Ctrl Pts',(17.6756754360527,-2.43710142000481,9.17399770765943));
#56961=CARTESIAN_POINT('Ctrl Pts',(14.4432887039958,-3.57613973602564,9.0169975803072));
#56962=CARTESIAN_POINT('Ctrl Pts',(12.2241286148511,-1.89728740549368,8.88952386202822));
#56963=CARTESIAN_POINT('Ctrl Pts',(11.9296376841916,-0.442933787892533,
8.81438351953334));
#56964=CARTESIAN_POINT('Ctrl Pts',(11.9309505480454,-0.000995066888653875,
8.79157655282255));
#56965=CARTESIAN_POINT('Origin',(15.,0.,14.2084234471775));
#56966=CARTESIAN_POINT('',(11.9284560106028,0.00245566734982605,10.7915765528225));
#56967=CARTESIAN_POINT('',(11.9275890856804,-0.00260766251225693,10.7084234471775));
#56968=CARTESIAN_POINT('',(11.9265,6.70613782525944E-14,14.2084234471775));
#56969=CARTESIAN_POINT('Ctrl Pts',(11.9275890856804,-0.00260766251225678,
10.7084234471775));
#56970=CARTESIAN_POINT('Ctrl Pts',(11.9337969642323,0.734391539461283,10.6702840810499));
#56971=CARTESIAN_POINT('Ctrl Pts',(12.5665847955819,2.49225272359552,10.5798113391382));
#56972=CARTESIAN_POINT('Ctrl Pts',(15.4855857629831,3.58648800243424,10.4370052214424));
#56973=CARTESIAN_POINT('Ctrl Pts',(18.2592872973176,1.57345505668517,10.2800050940901));
#56974=CARTESIAN_POINT('Ctrl Pts',(18.1103546151327,-1.85051527716861,10.1230049667379));
#56975=CARTESIAN_POINT('Ctrl Pts',(15.1723371249586,-3.61510816978504,9.96600483938563));
#56976=CARTESIAN_POINT('Ctrl Pts',(12.4502253736084,-2.31493586870828,9.82781099953215));
#56977=CARTESIAN_POINT('Ctrl Pts',(11.9337126333884,-0.647055676830039,
9.74195053546276));
#56978=CARTESIAN_POINT('Ctrl Pts',(11.9297705140734,0.00198364688382347,
9.70842344717746));
#56979=CARTESIAN_POINT('Ctrl Pts',(11.9284560106028,0.0024556673498264,
10.7915765528226));
#56980=CARTESIAN_POINT('Ctrl Pts',(11.9260692195737,0.309140112596412,10.7757173622757));
#56981=CARTESIAN_POINT('Ctrl Pts',(12.1080878285752,1.62508037117336,10.7075247959448));
#56982=CARTESIAN_POINT('Ctrl Pts',(13.9810651784412,3.47279856287599,10.5869988538297));
#56983=CARTESIAN_POINT('Ctrl Pts',(17.3344994031312,2.76565299665532,10.4299987264775));
#56984=CARTESIAN_POINT('Ctrl Pts',(18.5945871152999,-0.421511967551375,
10.2729985991252));
#56985=CARTESIAN_POINT('Ctrl Pts',(16.6313630370479,-3.23068676566348,10.115998471773));
#56986=CARTESIAN_POINT('Ctrl Pts',(13.205285741413,-3.14288213812672,9.9589983444207));
#56987=CARTESIAN_POINT('Ctrl Pts',(11.9539254885605,-1.14120637601563,9.85085770477057));
#56988=CARTESIAN_POINT('Ctrl Pts',(11.921918280707,-0.0679702217342443,
9.79505044090452));
#56989=CARTESIAN_POINT('Ctrl Pts',(11.9222420001619,-0.00114382935434687,
9.79157655282255));
#56990=CARTESIAN_POINT('Origin',(15.,0.,14.2084234471775));
#56991=CARTESIAN_POINT('',(11.9297760945785,-0.00333806817183438,11.7915765528226));
#56992=CARTESIAN_POINT('',(11.9228311771842,0.00152130202986591,11.7084234471775));
#56993=CARTESIAN_POINT('',(11.9265,6.70613782525944E-14,14.2084234471775));
#56994=CARTESIAN_POINT('',(14.2062007174671,-2.96922295374568,12.));
#56995=CARTESIAN_POINT('Ctrl Pts',(14.2062007174671,-2.96922295374568,12.));
#56996=CARTESIAN_POINT('Ctrl Pts',(13.2298599415769,-2.70820563726846,11.9476666242159));
#56997=CARTESIAN_POINT('Ctrl Pts',(12.1284916041782,-1.6759644246982,11.8781921418234));
#56998=CARTESIAN_POINT('Ctrl Pts',(11.9274999800733,-0.33505537898738,11.8087176594309));
#56999=CARTESIAN_POINT('Ctrl Pts',(11.9297760945785,-0.00333806817183434,
11.7915765528225));
#57000=CARTESIAN_POINT('',(15.7957331921886,-2.97400465723624,12.));
#57001=CARTESIAN_POINT('Origin',(15.,0.,12.));
#57002=CARTESIAN_POINT('Ctrl Pts',(15.7957405241459,-2.97402278592475,12.));
#57003=CARTESIAN_POINT('Ctrl Pts',(14.8659292530302,-3.21955068215558,11.9500021225376));
#57004=CARTESIAN_POINT('Ctrl Pts',(12.809912552641,-2.78622279751186,11.8528099382634));
#57005=CARTESIAN_POINT('Ctrl Pts',(11.9286986705132,-0.906613920335824,
11.7556177539892));
#57006=CARTESIAN_POINT('Ctrl Pts',(11.9228311771842,0.00152130202986659,
11.7084234471775));
#57007=CARTESIAN_POINT('Origin',(-7.5,12.9903810567666,7.5));
#57008=CARTESIAN_POINT('',(-10.0135512354019,12.9902955808623,4.38741669750803));
#57009=CARTESIAN_POINT('',(-10.0159871075715,12.98719611739,4.11258330249198));
#57010=CARTESIAN_POINT('',(-10.0175,12.9903810567666,7.5));
#57011=CARTESIAN_POINT('',(-9.41346599666504,14.6263682601415,4.));
#57012=CARTESIAN_POINT('Ctrl Pts',(-10.0159871075715,12.98719611739,4.11258330249198));
#57013=CARTESIAN_POINT('Ctrl Pts',(-10.0108029441705,13.5796929638899,4.07505553499465));
#57014=CARTESIAN_POINT('Ctrl Pts',(-9.79922182808404,14.175184617071,4.03752776749733));
#57015=CARTESIAN_POINT('Ctrl Pts',(-9.41346599666504,14.6263682601416,4.));
#57016=CARTESIAN_POINT('',(-10.0175,12.9903810567666,4.));
#57017=CARTESIAN_POINT('Origin',(-7.5,12.9903810567666,4.));
#57018=CARTESIAN_POINT('',(-10.0175,12.9903810567666,3.));
#57019=CARTESIAN_POINT('',(-10.0175,12.9903810567666,7.5));
#57020=CARTESIAN_POINT('Origin',(-7.5,12.9903810567666,3.));
#57021=CARTESIAN_POINT('',(-5.58300657818904,14.6286918237334,4.));
#57022=CARTESIAN_POINT('Origin',(-7.5,12.9903810567666,4.));
#57023=CARTESIAN_POINT('Ctrl Pts',(-5.58299280741585,14.6287008947316,4.));
#57024=CARTESIAN_POINT('Ctrl Pts',(-6.09671594976083,15.225839628633,4.04999787746244));
#57025=CARTESIAN_POINT('Ctrl Pts',(-6.91408837638834,15.566108849254,4.09999575492489));
#57026=CARTESIAN_POINT('Ctrl Pts',(-7.69917928811933,15.5037708430362,4.14999363238733));
#57027=CARTESIAN_POINT('Ctrl Pts',(-8.52094332678579,15.4385209070269,4.20232700817142));
#57028=CARTESIAN_POINT('Ctrl Pts',(-9.30733954710939,14.9321721158988,4.2546603839555));
#57029=CARTESIAN_POINT('Ctrl Pts',(-9.7062579619942,14.2110639837978,4.30699375973958));
#57030=CARTESIAN_POINT('Ctrl Pts',(-9.91060296091885,13.8416780768541,4.3338014056624));
#57031=CARTESIAN_POINT('Ctrl Pts',(-10.0132747138948,13.4159398344011,4.36060905158521));
#57032=CARTESIAN_POINT('Ctrl Pts',(-10.0135512354019,12.9902955808623,4.38741669750803));
#57033=CARTESIAN_POINT('Origin',(-7.5,12.9903810567666,7.5));
#57034=CARTESIAN_POINT('',(-10.0201376030965,12.9888406983805,5.38741669750803));
#57035=CARTESIAN_POINT('',(-10.0207017684327,12.9915893349038,5.11258330249198));
#57036=CARTESIAN_POINT('',(-10.0175,12.9903810567666,7.5));
#57037=CARTESIAN_POINT('Ctrl Pts',(-10.0207017684327,12.9915893349038,5.11258330249198));
#57038=CARTESIAN_POINT('Ctrl Pts',(-10.021123985829,13.062949094674,5.10805583214991));
#57039=CARTESIAN_POINT('Ctrl Pts',(-10.0183500982852,13.1342752724561,5.10352836180784));
#57040=CARTESIAN_POINT('Ctrl Pts',(-10.0122723502588,13.2053184595532,5.09900089146578));
#57041=CARTESIAN_POINT('Ctrl Pts',(-9.94201919621031,14.0265120900682,5.04666751568169));
#57042=CARTESIAN_POINT('Ctrl Pts',(-9.43032981516091,14.8098946989374,4.99433413989761));
#57043=CARTESIAN_POINT('Ctrl Pts',(-8.7066218792309,15.204343412931,4.94200076411352));
#57044=CARTESIAN_POINT('Ctrl Pts',(-7.98291394330089,15.5987921269246,4.88966738832944));
#57045=CARTESIAN_POINT('Ctrl Pts',(-7.04718745249026,15.6043069460425,4.83733401254535));
#57046=CARTESIAN_POINT('Ctrl Pts',(-6.31898125676283,15.2181990815764,4.78500063676127));
#57047=CARTESIAN_POINT('Ctrl Pts',(-5.59077506103539,14.8320912171102,4.73266726097718));
#57048=CARTESIAN_POINT('Ctrl Pts',(-5.07008916039116,14.0543606690598,4.6803338851931));
#57049=CARTESIAN_POINT('Ctrl Pts',(-4.99037298951262,13.2341300396427,4.62800050940902));
#57050=CARTESIAN_POINT('Ctrl Pts',(-4.91065681863409,12.4138994102257,4.57566713362493));
#57051=CARTESIAN_POINT('Ctrl Pts',(-5.27191037752124,11.5511686994419,4.52333375784085));
#57052=CARTESIAN_POINT('Ctrl Pts',(-5.91216754016691,11.0319148801645,4.47100038205676));
#57053=CARTESIAN_POINT('Ctrl Pts',(-6.55242470281257,10.5126610608871,4.41866700627268));
#57054=CARTESIAN_POINT('Ctrl Pts',(-7.47168546921673,10.336884133116,4.36633363048859));
#57055=CARTESIAN_POINT('Ctrl Pts',(-8.25780300491658,10.5850674765643,4.31400025470451));
#57056=CARTESIAN_POINT('Ctrl Pts',(-9.04392054061644,10.8332508200125,4.26166687892042));
#57057=CARTESIAN_POINT('Ctrl Pts',(-9.696894845612,11.50539443468,4.20933350313634));
#57058=CARTESIAN_POINT('Ctrl Pts',(-9.92376765947752,12.2963771799981,4.15700012735225));
#57059=CARTESIAN_POINT('Ctrl Pts',(-9.98795212995513,12.5201536995385,4.1421945190655));
#57060=CARTESIAN_POINT('Ctrl Pts',(-10.0180323849149,12.7534418387471,4.12738891077874));
#57061=CARTESIAN_POINT('Ctrl Pts',(-10.0159871075715,12.98719611739,4.11258330249198));
#57062=CARTESIAN_POINT('Ctrl Pts',(-10.0135512354019,12.9902955808623,4.38741669750803));
#57063=CARTESIAN_POINT('Ctrl Pts',(-10.0138145339143,12.5850052295903,4.4129424273693));
#57064=CARTESIAN_POINT('Ctrl Pts',(-9.92124134238478,12.1798000932329,4.43846815723057));
#57065=CARTESIAN_POINT('Ctrl Pts',(-9.73520837540778,11.8234099166911,4.46399388709184));
#57066=CARTESIAN_POINT('Ctrl Pts',(-9.35379976449056,11.0927314547595,4.51632726287592));
#57067=CARTESIAN_POINT('Ctrl Pts',(-8.57954193321014,10.5672420039701,4.56866063866001));
#57068=CARTESIAN_POINT('Ctrl Pts',(-7.75970071708304,10.482369764132,4.62099401444409));
#57069=CARTESIAN_POINT('Ctrl Pts',(-6.93985950095593,10.3974975242939,4.67332739022817));
#57070=CARTESIAN_POINT('Ctrl Pts',(-6.07443489998217,10.7532424954071,4.72566076601226));
#57071=CARTESIAN_POINT('Ctrl Pts',(-5.55138100127894,11.3901954309976,4.77799414179634));
#57072=CARTESIAN_POINT('Ctrl Pts',(-5.02832710257572,12.0271483665881,4.83032751758043));
#57073=CARTESIAN_POINT('Ctrl Pts',(-4.84764390614303,12.945309266656,4.88266089336452));
#57074=CARTESIAN_POINT('Ctrl Pts',(-5.09037388542358,13.7329699193423,4.9349942691486));
#57075=CARTESIAN_POINT('Ctrl Pts',(-5.33310386470412,14.5206305720287,4.98732764493268));
#57076=CARTESIAN_POINT('Ctrl Pts',(-5.9992470196979,15.1777909773334,5.03966102071676));
#57077=CARTESIAN_POINT('Ctrl Pts',(-6.79011836385736,15.4098338158843,5.09199439650085));
#57078=CARTESIAN_POINT('Ctrl Pts',(-7.58098970801682,15.6418766544352,5.14432777228493));
#57079=CARTESIAN_POINT('Ctrl Pts',(-8.49658924134195,15.4488019262325,5.19666114806902));
#57080=CARTESIAN_POINT('Ctrl Pts',(-9.12641195891838,14.9171634974037,5.24899452385311));
#57081=CARTESIAN_POINT('Ctrl Pts',(-9.68170723832013,14.4484342794212,5.29513524840475));
#57082=CARTESIAN_POINT('Ctrl Pts',(-10.0148566122412,13.7165257701398,5.34127597295639));
#57083=CARTESIAN_POINT('Ctrl Pts',(-10.0201376030965,12.9888406983805,5.38741669750803));
#57084=CARTESIAN_POINT('Origin',(-7.5,12.9903810567666,7.5));
#57085=CARTESIAN_POINT('',(-10.0170827477036,12.9925476830062,6.38741669750803));
#57086=CARTESIAN_POINT('',(-10.0137187170915,12.9909479514162,6.11258330249198));
#57087=CARTESIAN_POINT('',(-10.0175,12.9903810567666,7.5));
#57088=CARTESIAN_POINT('Ctrl Pts',(-10.0137187170915,12.9909479514162,6.11258330249198));
#57089=CARTESIAN_POINT('Ctrl Pts',(-10.0144982588899,13.3697154315319,6.08872275352109));
#57090=CARTESIAN_POINT('Ctrl Pts',(-9.93406587049998,13.7481685539756,6.06486220455019));
#57091=CARTESIAN_POINT('Ctrl Pts',(-9.77069359762705,14.0865814419388,6.0410016555793));
#57092=CARTESIAN_POINT('Ctrl Pts',(-9.41236896061271,14.8288229074456,5.98866827979521));
#57093=CARTESIAN_POINT('Ctrl Pts',(-8.65505611306826,15.3784479785104,5.93633490401113));
#57094=CARTESIAN_POINT('Ctrl Pts',(-7.83829989006264,15.4890315871854,5.88400152822704));
#57095=CARTESIAN_POINT('Ctrl Pts',(-7.02154366705702,15.5996151958603,5.83166815244296));
#57096=CARTESIAN_POINT('Ctrl Pts',(-6.14534406859022,15.2711573421455,5.77933477665887));
#57097=CARTESIAN_POINT('Ctrl Pts',(-5.60254941260429,14.6509198275943,5.72700140087479));
#57098=CARTESIAN_POINT('Ctrl Pts',(-5.05975475661836,14.0306823130431,5.6746680250907));
#57099=CARTESIAN_POINT('Ctrl Pts',(-4.8503650431133,13.1186651376555,5.62233464930662));
#57100=CARTESIAN_POINT('Ctrl Pts',(-5.06826110556232,12.3237831148942,5.57000127352254));
#57101=CARTESIAN_POINT('Ctrl Pts',(-5.28615716801134,11.5289010921329,5.51766789773845));
#57102=CARTESIAN_POINT('Ctrl Pts',(-5.93133900641445,10.8511542219977,5.46533452195436));
#57103=CARTESIAN_POINT('Ctrl Pts',(-6.71453634454677,10.5943988157391,5.41300114617028));
#57104=CARTESIAN_POINT('Ctrl Pts',(-7.49773368267909,10.3376434094805,5.3606677703862));
#57105=CARTESIAN_POINT('Ctrl Pts',(-8.41894652054063,10.5018794670985,5.30833439460211));
#57106=CARTESIAN_POINT('Ctrl Pts',(-9.06514447594766,11.0134998219879,5.25600101881803));
#57107=CARTESIAN_POINT('Ctrl Pts',(-9.65543848794614,11.4808588245671,5.20819511337601));
#57108=CARTESIAN_POINT('Ctrl Pts',(-10.0162435426697,12.2380961764306,5.160389207934));
#57109=CARTESIAN_POINT('Ctrl Pts',(-10.0207017684327,12.9915893349038,5.11258330249198));
#57110=CARTESIAN_POINT('Ctrl Pts',(-10.0201376030965,12.9888406983805,5.38741669750803));
#57111=CARTESIAN_POINT('Ctrl Pts',(-10.02084637685,12.8911764354056,5.39360934874047));
#57112=CARTESIAN_POINT('Ctrl Pts',(-10.0156492795336,12.793588248926,5.39980199997291));
#57113=CARTESIAN_POINT('Ctrl Pts',(-10.0042907210835,12.6967226001492,5.40599465120536));
#57114=CARTESIAN_POINT('Ctrl Pts',(-9.90830086384453,11.8781222611782,5.45832802698944));
#57115=CARTESIAN_POINT('Ctrl Pts',(-9.37227524753879,11.1111237126909,5.51066140277353));
#57116=CARTESIAN_POINT('Ctrl Pts',(-8.63654573295752,10.739611267924,5.56299477855761));
#57117=CARTESIAN_POINT('Ctrl Pts',(-7.90081621837627,10.368098823157,5.6153281543417));
#57118=CARTESIAN_POINT('Ctrl Pts',(-6.96538280551948,10.3920724821103,5.66766153012578));
#57119=CARTESIAN_POINT('Ctrl Pts',(-6.24965042528476,10.8007851576184,5.71999490590986));
#57120=CARTESIAN_POINT('Ctrl Pts',(-5.53391804505003,11.2094978331266,5.77232828169395));
#57121=CARTESIAN_POINT('Ctrl Pts',(-5.03788669743737,12.0029495251895,5.82466165747803));
#57122=CARTESIAN_POINT('Ctrl Pts',(-4.98395499247446,12.8253915347154,5.87699503326212));
#57123=CARTESIAN_POINT('Ctrl Pts',(-4.93002328751154,13.6478335442413,5.9293284090462));
#57124=CARTESIAN_POINT('Ctrl Pts',(-5.31819122519835,14.4992658712303,5.98166178483029));
#57125=CARTESIAN_POINT('Ctrl Pts',(-5.97442155431181,14.997945170426,6.03399516061437));
#57126=CARTESIAN_POINT('Ctrl Pts',(-6.63065188342527,15.4966244696218,6.08632853639846));
#57127=CARTESIAN_POINT('Ctrl Pts',(-7.55494460396538,15.6425507410243,6.13866191218253));
#57128=CARTESIAN_POINT('Ctrl Pts',(-8.33288879152928,15.3702970248207,6.19099528796662));
#57129=CARTESIAN_POINT('Ctrl Pts',(-9.11083297909318,15.0980433086171,6.2433286637507));
#57130=CARTESIAN_POINT('Ctrl Pts',(-9.74242863368087,14.4076096048073,6.2956620395348));
#57131=CARTESIAN_POINT('Ctrl Pts',(-9.94449673701248,13.6085552867894,6.34799541531888));
#57132=CARTESIAN_POINT('Ctrl Pts',(-9.99523417179805,13.4079201262562,6.36113584271526));
#57133=CARTESIAN_POINT('Ctrl Pts',(-10.0188913666349,13.2004368082823,6.37427627011165));
#57134=CARTESIAN_POINT('Ctrl Pts',(-10.0170827477036,12.9925476830062,6.38741669750803));
#57135=CARTESIAN_POINT('Origin',(-7.5,12.9903810567666,7.5));
#57136=CARTESIAN_POINT('',(-10.0145080012689,12.9889431840086,7.38741669750803));
#57137=CARTESIAN_POINT('',(-10.0189159587739,12.9883983308864,7.11258330249199));
#57138=CARTESIAN_POINT('',(-10.0175,12.9903810567666,7.5));
#57139=CARTESIAN_POINT('Ctrl Pts',(-10.0189159587739,12.9883983308864,7.11258330249199));
#57140=CARTESIAN_POINT('Ctrl Pts',(-10.0130302121016,13.6704662986594,7.06938967489226));
#57141=CARTESIAN_POINT('Ctrl Pts',(-9.72554840383075,14.3569089324365,7.02619604729254));
#57142=CARTESIAN_POINT('Ctrl Pts',(-9.2308848153494,14.8238864031427,6.98300241969281));
#57143=CARTESIAN_POINT('Ctrl Pts',(-8.63155067970796,15.3896760534967,6.93066904390873));
#57144=CARTESIAN_POINT('Ctrl Pts',(-7.72807923358486,15.6332967159553,6.87833566812465));
#57145=CARTESIAN_POINT('Ctrl Pts',(-6.9255462333781,15.4455199330078,6.82600229234057));
#57146=CARTESIAN_POINT('Ctrl Pts',(-6.12301323317133,15.2577431500604,6.77366891655648));
#57147=CARTESIAN_POINT('Ctrl Pts',(-5.4214186788809,14.638568921707,6.72133554077239));
#57148=CARTESIAN_POINT('Ctrl Pts',(-5.13532585476554,13.8656069146025,6.66900216498831));
#57149=CARTESIAN_POINT('Ctrl Pts',(-4.84923303065017,13.092644907498,6.61666878920422));
#57150=CARTESIAN_POINT('Ctrl Pts',(-4.97864193670987,12.1658951216425,6.56433541342014));
#57151=CARTESIAN_POINT('Ctrl Pts',(-5.46553146829354,11.5008704033029,6.51200203763605));
#57152=CARTESIAN_POINT('Ctrl Pts',(-5.95242099987721,10.8358456849633,6.45966866185197));
#57153=CARTESIAN_POINT('Ctrl Pts',(-6.79679115698486,10.4325460341398,6.40733528606789));
#57154=CARTESIAN_POINT('Ctrl Pts',(-7.62006453112491,10.471792520931,6.35500191028381));
#57155=CARTESIAN_POINT('Ctrl Pts',(-8.44333790526497,10.5110390077222,6.30266853449972));
#57156=CARTESIAN_POINT('Ctrl Pts',(-9.24551449643742,10.9928316321281,6.25033515871563));
#57157=CARTESIAN_POINT('Ctrl Pts',(-9.66693457878153,11.7011568743055,6.19800178293155));
#57158=CARTESIAN_POINT('Ctrl Pts',(-9.89621504923482,12.0865327772692,6.16952895611836));
#57159=CARTESIAN_POINT('Ctrl Pts',(-10.0127884887617,12.5389641820168,6.14105612930517));
#57160=CARTESIAN_POINT('Ctrl Pts',(-10.0137187170915,12.9909479514162,6.11258330249198));
#57161=CARTESIAN_POINT('Ctrl Pts',(-10.0170827477036,12.9925476830062,6.38741669750803));
#57162=CARTESIAN_POINT('Ctrl Pts',(-10.0116883182615,12.3724926793498,6.42660964589573));
#57163=CARTESIAN_POINT('Ctrl Pts',(-9.77974890631033,11.7488275963524,6.46580259428343));
#57164=CARTESIAN_POINT('Ctrl Pts',(-9.36410096710587,11.2924908434457,6.50499554267113));
#57165=CARTESIAN_POINT('Ctrl Pts',(-8.80909654179214,10.6831556503463,6.55732891845521));
#57166=CARTESIAN_POINT('Ctrl Pts',(-7.92654713908917,10.3721601963736,6.6096622942393));
#57167=CARTESIAN_POINT('Ctrl Pts',(-7.11214799700031,10.4989408139477,6.66199567002338));
#57168=CARTESIAN_POINT('Ctrl Pts',(-6.29774885491145,10.6257214315218,6.71432904580747));
#57169=CARTESIAN_POINT('Ctrl Pts',(-5.55149997343671,11.1902781206427,6.76666242159156));
#57170=CARTESIAN_POINT('Ctrl Pts',(-5.20798562845119,11.9394891669376,6.81899579737564));
#57171=CARTESIAN_POINT('Ctrl Pts',(-4.86447128346568,12.6887002132326,6.87132917315972));
#57172=CARTESIAN_POINT('Ctrl Pts',(-4.92369147496937,13.6225656167016,6.92366254894381));
#57173=CARTESIAN_POINT('Ctrl Pts',(-5.35909454078469,14.3223823516912,6.97599592472789));
#57174=CARTESIAN_POINT('Ctrl Pts',(-5.79449760660002,15.0221990866808,7.02832930051197));
#57175=CARTESIAN_POINT('Ctrl Pts',(-6.60608354672698,15.4879671531909,7.08066267629606));
#57176=CARTESIAN_POINT('Ctrl Pts',(-7.42997391459192,15.5108572005546,7.13299605208014));
#57177=CARTESIAN_POINT('Ctrl Pts',(-8.25386428245684,15.5337472479183,7.18532942786423));
#57178=CARTESIAN_POINT('Ctrl Pts',(-9.09005907805975,15.1137592761355,7.23766280364831));
#57179=CARTESIAN_POINT('Ctrl Pts',(-9.56364635237551,14.4391969089269,7.2899961794324));
#57180=CARTESIAN_POINT('Ctrl Pts',(-9.85751310519891,14.0206226287906,7.32246968545761));
#57181=CARTESIAN_POINT('Ctrl Pts',(-10.0117630617271,13.5040281493434,7.35494319148282));
#57182=CARTESIAN_POINT('Ctrl Pts',(-10.0145080012689,12.9889431840086,7.38741669750803));
#57183=CARTESIAN_POINT('Origin',(-7.5,12.9903810567666,7.5));
#57184=CARTESIAN_POINT('',(-10.0214370846894,12.9902333726245,8.38741669750803));
#57185=CARTESIAN_POINT('',(-10.0184390483887,12.992460268524,8.11258330249199));
#57186=CARTESIAN_POINT('',(-10.0175,12.9903810567666,7.5));
#57187=CARTESIAN_POINT('Ctrl Pts',(-10.0184390483887,12.992460268524,8.11258330249199));
#57188=CARTESIAN_POINT('Ctrl Pts',(-10.0198617859934,13.1535014782239,8.10238997204752));
#57189=CARTESIAN_POINT('Ctrl Pts',(-10.0057048345233,13.3142936934228,8.09219664160306));
#57190=CARTESIAN_POINT('Ctrl Pts',(-9.9750487925512,13.4718761813451,8.08200331115859));
#57191=CARTESIAN_POINT('Ctrl Pts',(-9.8176582151223,14.2809173090076,8.02966993537451));
#57192=CARTESIAN_POINT('Ctrl Pts',(-9.22537175290504,15.0053539438514,7.97733655959042));
#57193=CARTESIAN_POINT('Ctrl Pts',(-8.46374388225838,15.3203814452906,7.92500318380634));
#57194=CARTESIAN_POINT('Ctrl Pts',(-7.70211601161172,15.6354089467299,7.87266980802225));
#57195=CARTESIAN_POINT('Ctrl Pts',(-6.77114673253565,15.5410273147647,7.82033643223817));
#57196=CARTESIAN_POINT('Ctrl Pts',(-6.08824058698168,15.0795530074754,7.76800305645409));
#57197=CARTESIAN_POINT('Ctrl Pts',(-5.40533444142772,14.6180787001861,7.71566968067));
#57198=CARTESIAN_POINT('Ctrl Pts',(-4.97049142939586,13.7895117175727,7.66333630488591));
#57199=CARTESIAN_POINT('Ctrl Pts',(-4.97867550117357,12.9653440395039,7.61100292910182));
#57200=CARTESIAN_POINT('Ctrl Pts',(-4.98685957295128,12.1411763614351,7.55866955331774));
#57201=CARTESIAN_POINT('Ctrl Pts',(-5.43807072853852,11.3214079879109,7.50633617753367));
#57202=CARTESIAN_POINT('Ctrl Pts',(-6.13000628195668,10.8735860038557,7.45400280174958));
#57203=CARTESIAN_POINT('Ctrl Pts',(-6.82194183537485,10.4257640198005,7.4016694259655));
#57204=CARTESIAN_POINT('Ctrl Pts',(-7.75460178662392,10.3498884252143,7.3493360501814));
#57205=CARTESIAN_POINT('Ctrl Pts',(-8.50982357282137,10.6799784021981,7.29700267439732));
#57206=CARTESIAN_POINT('Ctrl Pts',(-9.2650453590188,11.0100683791819,7.24466929861323));
#57207=CARTESIAN_POINT('Ctrl Pts',(-9.84282898016461,11.7461239277358,7.19233592282916));
#57208=CARTESIAN_POINT('Ctrl Pts',(-9.98412237815762,12.5581310211375,7.14000254704507));
#57209=CARTESIAN_POINT('Ctrl Pts',(-10.0087985252324,12.6999437791798,7.13086279886071));
#57210=CARTESIAN_POINT('Ctrl Pts',(-10.020161379579,12.8440731186622,7.12172305067635));
#57211=CARTESIAN_POINT('Ctrl Pts',(-10.0189159587739,12.9883983308864,7.11258330249199));
#57212=CARTESIAN_POINT('Ctrl Pts',(-10.0145080012689,12.9889431840086,7.38741669750803));
#57213=CARTESIAN_POINT('Ctrl Pts',(-10.0161867279748,12.6739319154882,7.4072765672669));
#57214=CARTESIAN_POINT('Ctrl Pts',(-9.96119959962244,12.359485234924,7.42713643702578));
#57215=CARTESIAN_POINT('Ctrl Pts',(-9.84682730754632,12.0683695443894,7.44699630678465));
#57216=CARTESIAN_POINT('Ctrl Pts',(-9.54544123537271,11.3012413096949,7.49932968256874));
#57217=CARTESIAN_POINT('Ctrl Pts',(-8.83168933799688,10.6961216029404,7.55166305835282));
#57218=CARTESIAN_POINT('Ctrl Pts',(-8.02558570196195,10.5243187478344,7.60399643413691));
#57219=CARTESIAN_POINT('Ctrl Pts',(-7.21948206592701,10.3525158927284,7.65632980992099));
#57220=CARTESIAN_POINT('Ctrl Pts',(-6.32102669123297,10.6140298892709,7.70866318570508));
#57221=CARTESIAN_POINT('Ctrl Pts',(-5.73304635500187,11.1916096823396,7.76099656148916));
#57222=CARTESIAN_POINT('Ctrl Pts',(-5.14506601877077,11.7691894754082,7.81332993727325));
#57223=CARTESIAN_POINT('Ctrl Pts',(-4.8675607210026,12.6628350650029,7.86566331305733));
#57224=CARTESIAN_POINT('Ctrl Pts',(-5.02495129299175,13.4718761647033,7.91799668884141));
#57225=CARTESIAN_POINT('Ctrl Pts',(-5.18234186498089,14.2809172644038,7.9703300646255));
#57226=CARTESIAN_POINT('Ctrl Pts',(-5.77462830672734,15.0053538742101,8.02266344040958));
#57227=CARTESIAN_POINT('Ctrl Pts',(-6.53625615105054,15.3203813647611,8.07499681619367));
#57228=CARTESIAN_POINT('Ctrl Pts',(-7.29788399537374,15.6354088553122,8.12733019197775));
#57229=CARTESIAN_POINT('Ctrl Pts',(-8.22885324227368,15.5410272266082,8.17966356776184));
#57230=CARTESIAN_POINT('Ctrl Pts',(-8.91175936422494,15.0795529352688,8.23199694354592));
#57231=CARTESIAN_POINT('Ctrl Pts',(-9.58779130918474,14.6227238738573,8.28380352819996));
#57232=CARTESIAN_POINT('Ctrl Pts',(-10.0207290328118,13.8061553106607,8.33561011285399));
#57233=CARTESIAN_POINT('Ctrl Pts',(-10.0214370846894,12.9902333726245,8.38741669750803));
#57234=CARTESIAN_POINT('Origin',(-7.5,12.9903810567666,7.5));
#57235=CARTESIAN_POINT('',(-10.0148245050326,12.9920058624485,9.38741669750802));
#57236=CARTESIAN_POINT('',(-10.0138587145805,12.9895659971561,9.11258330249198));
#57237=CARTESIAN_POINT('',(-10.0175,12.9903810567666,7.5));
#57238=CARTESIAN_POINT('Ctrl Pts',(-10.0138587145805,12.9895659971561,9.11258330249198));
#57239=CARTESIAN_POINT('Ctrl Pts',(-10.0124665205819,13.458209000479,9.08305689341869));
#57240=CARTESIAN_POINT('Ctrl Pts',(-9.88655927300326,13.9275468726326,9.0535304843454));
#57241=CARTESIAN_POINT('Ctrl Pts',(-9.64090553321082,14.3223823977307,9.02400407527211));
#57242=CARTESIAN_POINT('Ctrl Pts',(-9.20550245234811,15.0221991569096,8.97167069948803));
#57243=CARTESIAN_POINT('Ctrl Pts',(-8.39391648416845,15.4879672395126,8.91933732370394));
#57244=CARTESIAN_POINT('Ctrl Pts',(-7.57002608782754,15.5108572876662,8.86700394791986));
#57245=CARTESIAN_POINT('Ctrl Pts',(-6.74613569148664,15.5337473358198,8.81467057213577));
#57246=CARTESIAN_POINT('Ctrl Pts',(-5.90994086698447,15.113759349524,8.76233719635169));
#57247=CARTESIAN_POINT('Ctrl Pts',(-5.43635357630086,14.4391969590017,8.71000382056761));
#57248=CARTESIAN_POINT('Ctrl Pts',(-4.96276628561725,13.7646345684795,8.65767044478352));
#57249=CARTESIAN_POINT('Ctrl Pts',(-4.85178652875219,12.8354977737306,8.60533706899943));
#57250=CARTESIAN_POINT('Ctrl Pts',(-5.15317261134217,12.0683695125223,8.55300369321535));
#57251=CARTESIAN_POINT('Ctrl Pts',(-5.45455869393216,11.3012412513139,8.50067031743126));
#57252=CARTESIAN_POINT('Ctrl Pts',(-6.16831061597719,10.696121523646,8.44833694164718));
#57253=CARTESIAN_POINT('Ctrl Pts',(-6.97441427987286,10.5243186626023,8.3960035658631));
#57254=CARTESIAN_POINT('Ctrl Pts',(-7.78051794376854,10.3525158015586,8.34367019007901));
#57255=CARTESIAN_POINT('Ctrl Pts',(-8.67897334951486,10.6140298071391,8.29133681429493));
#57256=CARTESIAN_POINT('Ctrl Pts',(-9.26695370606775,11.1916096201701,8.23900343851084));
#57257=CARTESIAN_POINT('Ctrl Pts',(-9.74040909687172,11.656690252629,8.19686339317122));
#57258=CARTESIAN_POINT('Ctrl Pts',(-10.0125573370586,12.3267029956413,8.15472334783161));
#57259=CARTESIAN_POINT('Ctrl Pts',(-10.0184390483887,12.992460268524,8.11258330249199));
#57260=CARTESIAN_POINT('Ctrl Pts',(-10.0214370846894,12.9902333726245,8.38741669750803));
#57261=CARTESIAN_POINT('Ctrl Pts',(-10.0214442844586,12.9819367353796,8.38794348863807));
#57262=CARTESIAN_POINT('Ctrl Pts',(-10.0214067930746,12.9736401649937,8.38847027976812));
#57263=CARTESIAN_POINT('Ctrl Pts',(-10.021324411684,12.9653440403702,8.38899707089817));
#57264=CARTESIAN_POINT('Ctrl Pts',(-10.0131403401893,12.1411763907856,8.44133044668226));
#57265=CARTESIAN_POINT('Ctrl Pts',(-9.56192920019726,11.3214080455913,8.49366382246634));
#57266=CARTESIAN_POINT('Ctrl Pts',(-8.86999367069368,10.873586077015,8.54599719825042));
#57267=CARTESIAN_POINT('Ctrl Pts',(-8.1780581411901,10.4257641084388,8.59833057403451));
#57268=CARTESIAN_POINT('Ctrl Pts',(-7.24539822217496,10.3498885164806,8.65066394981859));
#57269=CARTESIAN_POINT('Ctrl Pts',(-6.49017646207993,10.6799784820534,8.70299732560268));
#57270=CARTESIAN_POINT('Ctrl Pts',(-5.7349547019849,11.0100684476262,8.75533070138676));
#57271=CARTESIAN_POINT('Ctrl Pts',(-5.15717110080998,11.7461239707299,8.80766407717085));
#57272=CARTESIAN_POINT('Ctrl Pts',(-5.01587770769964,12.5581310360714,8.85999745295494));
#57273=CARTESIAN_POINT('Ctrl Pts',(-4.8745843145893,13.3701381014129,8.91233082873902));
#57274=CARTESIAN_POINT('Ctrl Pts',(-5.16978112954355,14.2580967089923,8.96466420452309));
#57275=CARTESIAN_POINT('Ctrl Pts',(-5.76911524447212,14.823886339783,9.01699758030718));
#57276=CARTESIAN_POINT('Ctrl Pts',(-6.36844935940068,15.3896759705738,9.06933095609126));
#57277=CARTESIAN_POINT('Ctrl Pts',(-7.27192077430355,15.633296624576,9.12166433187536));
#57278=CARTESIAN_POINT('Ctrl Pts',(-8.07445374677037,15.4455198481341,9.17399770765944));
#57279=CARTESIAN_POINT('Ctrl Pts',(-8.87698671923719,15.2577430716922,9.22633108344353));
#57280=CARTESIAN_POINT('Ctrl Pts',(-9.57858124926796,14.6385688648061,9.2786644592276));
#57281=CARTESIAN_POINT('Ctrl Pts',(-9.8646740635007,13.8656068843882,9.33099783501169));
#57282=CARTESIAN_POINT('Ctrl Pts',(-9.96748309569448,13.5878387295239,9.34980412251046));
#57283=CARTESIAN_POINT('Ctrl Pts',(-10.0166357361991,13.2902109767329,9.36861041000924));
#57284=CARTESIAN_POINT('Ctrl Pts',(-10.0148245050326,12.9920058624485,9.38741669750802));
#57285=CARTESIAN_POINT('Origin',(-7.5,12.9903810567666,7.5));
#57286=CARTESIAN_POINT('',(-10.0166112816083,12.988245230306,10.387416697508));
#57287=CARTESIAN_POINT('',(-10.0209918820407,12.9894441341194,10.112583302492));
#57288=CARTESIAN_POINT('',(-10.0175,12.9903810567666,7.5));
#57289=CARTESIAN_POINT('Ctrl Pts',(-10.0209918820407,12.9894441341194,10.112583302492));
#57290=CARTESIAN_POINT('Ctrl Pts',(-10.0172624812131,13.7593153446234,10.0637238147899));
#57291=CARTESIAN_POINT('Ctrl Pts',(-9.63824829706051,14.5323682430672,10.0148643270877));
#57292=CARTESIAN_POINT('Ctrl Pts',(-9.02557849846605,14.9979452399236,9.96600483938563));
#57293=CARTESIAN_POINT('Ctrl Pts',(-8.36934814670953,15.4966245564456,9.91367146360154));
#57294=CARTESIAN_POINT('Ctrl Pts',(-7.44505539412875,15.642550832678,9.86133808781746));
#57295=CARTESIAN_POINT('Ctrl Pts',(-6.66711117965626,15.3702971070154,9.80900471203338));
#57296=CARTESIAN_POINT('Ctrl Pts',(-5.88916696518377,15.0980433813528,9.75667133624929));
#57297=CARTESIAN_POINT('Ctrl Pts',(-5.25757128881956,14.4076096537953,9.70433796046521));
#57298=CARTESIAN_POINT('Ctrl Pts',(-5.05550317851592,13.608555308187,9.65200458468112));
#57299=CARTESIAN_POINT('Ctrl Pts',(-4.85343506821227,12.8095009625786,9.59967120889704));
#57300=CARTESIAN_POINT('Ctrl Pts',(-5.08089452396919,11.9018259989194,9.54733783311296));
#57301=CARTESIAN_POINT('Ctrl Pts',(-5.6358989684585,11.2924907847457,9.49500445732887));
#57302=CARTESIAN_POINT('Ctrl Pts',(-6.19090341294781,10.683155570572,9.44267108154479));
#57303=CARTESIAN_POINT('Ctrl Pts',(-7.0734528461695,10.3721601058839,9.3903377057607));
#57304=CARTESIAN_POINT('Ctrl Pts',(-7.88785201640932,10.4989407278476,9.33800432997662));
#57305=CARTESIAN_POINT('Ctrl Pts',(-8.70225118664915,10.6257213498112,9.28567095419253));
#57306=CARTESIAN_POINT('Ctrl Pts',(-9.44850009390711,11.1902780584266,9.23333757840845));
#57307=CARTESIAN_POINT('Ctrl Pts',(-9.79201445076321,11.9394891306117,9.18100420262436));
#57308=CARTESIAN_POINT('Ctrl Pts',(-9.9417185427335,12.2659964832652,9.15819723591357));
#57309=CARTESIAN_POINT('Ctrl Pts',(-10.014934081453,12.6275739462602,9.13539026920278));
#57310=CARTESIAN_POINT('Ctrl Pts',(-10.0138587145805,12.9895659971561,9.11258330249198));
#57311=CARTESIAN_POINT('Ctrl Pts',(-10.0148245050326,12.9920058624485,9.38741669750802));
#57312=CARTESIAN_POINT('Ctrl Pts',(-10.0115955154073,12.4603778526996,9.42094378579333));
#57313=CARTESIAN_POINT('Ctrl Pts',(-9.84639154112273,11.9269148544392,9.45447087407864));
#57314=CARTESIAN_POINT('Ctrl Pts',(-9.53446846140197,11.5008704547181,9.48799796236395));
#57315=CARTESIAN_POINT('Ctrl Pts',(-9.0475789466358,10.8358457594159,9.54033133814803));
#57316=CARTESIAN_POINT('Ctrl Pts',(-8.20320881866876,10.4325461227612,9.59266471393211));
#57317=CARTESIAN_POINT('Ctrl Pts',(-7.37993547300324,10.4717926080996,9.64499808971619));
#57318=CARTESIAN_POINT('Ctrl Pts',(-6.55666212733773,10.5110390934381,9.69733146550028));
#57319=CARTESIAN_POINT('Ctrl Pts',(-5.75448556397372,10.9928317007697,9.74966484128437));
#57320=CARTESIAN_POINT('Ctrl Pts',(-5.33306549615464,11.7011569186411,9.80199821706845));
#57321=CARTESIAN_POINT('Ctrl Pts',(-4.91164542833556,12.4094821365125,9.85433159285254));
#57322=CARTESIAN_POINT('Ctrl Pts',(-4.87098185606138,13.3443399649238,9.90666496863662));
#57323=CARTESIAN_POINT('Ctrl Pts',(-5.22930648076992,14.0865814044601,9.9589983444207));
#57324=CARTESIAN_POINT('Ctrl Pts',(-5.58763110547847,14.8288228439964,10.0113317202048));
#57325=CARTESIAN_POINT('Ctrl Pts',(-6.34494392716974,15.3784478946578,10.0636650959889));
#57326=CARTESIAN_POINT('Ctrl Pts',(-7.1617001217923,15.489031500081,10.115998471773));
#57327=CARTESIAN_POINT('Ctrl Pts',(-7.97845631641486,15.5996151055041,10.168331847557));
#57328=CARTESIAN_POINT('Ctrl Pts',(-8.8546558839687,15.2711572656891,10.2206652233411));
#57329=CARTESIAN_POINT('Ctrl Pts',(-9.39745052149691,14.6509197715574,10.2729985991252));
#57330=CARTESIAN_POINT('Ctrl Pts',(-9.79302682634298,14.1989048858303,10.3111379652528));
#57331=CARTESIAN_POINT('Ctrl Pts',(-10.0115264151771,13.5919211369207,10.3492773313804));
#57332=CARTESIAN_POINT('Ctrl Pts',(-10.0166112816083,12.988245230306,10.387416697508));
#57333=CARTESIAN_POINT('Origin',(-7.5,12.9903810567666,7.5));
#57334=CARTESIAN_POINT('',(-10.020507596494,12.9916292754481,11.387416697508));
#57335=CARTESIAN_POINT('',(-10.0159019782719,12.9923925656114,11.112583302492));
#57336=CARTESIAN_POINT('',(-10.0175,12.9903810567666,7.5));
#57337=CARTESIAN_POINT('',(-5.58653400333491,14.6263682601415,12.));
#57338=CARTESIAN_POINT('Ctrl Pts',(-10.020507596494,12.9916292754481,11.387416697508));
#57339=CARTESIAN_POINT('Ctrl Pts',(-10.0157033908479,12.2477735308672,11.4346110043198));
#57340=CARTESIAN_POINT('Ctrl Pts',(-9.66521700262529,11.5001788657538,11.4818053111315));
#57341=CARTESIAN_POINT('Ctrl Pts',(-9.08783233623607,11.0319150553912,11.5289996179432));
#57342=CARTESIAN_POINT('Ctrl Pts',(-8.44757526373259,10.5126611959891,11.5813329937273));
#57343=CARTESIAN_POINT('Ctrl Pts',(-7.52831480323821,10.3368839617759,11.6336663695114));
#57344=CARTESIAN_POINT('Ctrl Pts',(-6.74219715513642,10.5850674081367,11.6859997452955));
#57345=CARTESIAN_POINT('Ctrl Pts',(-5.95607950703463,10.8332508544976,11.7383331210796));
#57346=CARTESIAN_POINT('Ctrl Pts',(-5.30310467132541,11.5053949814325,11.7906664968637));
#57347=CARTESIAN_POINT('Ctrl Pts',(-5.07623184554712,12.2963777181293,11.8429998726477));
#57348=CARTESIAN_POINT('Ctrl Pts',(-4.84935901976883,13.0873604548261,11.8953332484318));
#57349=CARTESIAN_POINT('Ctrl Pts',(-5.04858820392146,13.9971818012847,11.9476666242159));
#57350=CARTESIAN_POINT('Ctrl Pts',(-5.58653400333491,14.6263682601415,12.));
#57351=CARTESIAN_POINT('',(-9.41699350863879,14.6286916542883,12.));
#57352=CARTESIAN_POINT('Origin',(-7.5,12.9903810567666,12.));
#57353=CARTESIAN_POINT('Ctrl Pts',(-9.41700728965905,14.6287007311509,12.));
#57354=CARTESIAN_POINT('Ctrl Pts',(-8.90328417076102,15.2258393704274,11.9500021225376));
#57355=CARTESIAN_POINT('Ctrl Pts',(-8.08591167026785,15.5661089832965,11.9000042450751));
#57356=CARTESIAN_POINT('Ctrl Pts',(-7.30082070927967,15.5037710574514,11.8500063676127));
#57357=CARTESIAN_POINT('Ctrl Pts',(-6.47905661905513,15.438521205569,11.7976729918286));
#57358=CARTESIAN_POINT('Ctrl Pts',(-5.6926603741346,14.9321721568753,11.7453396160445));
#57359=CARTESIAN_POINT('Ctrl Pts',(-5.29374195236929,14.2110639499398,11.6930062402604));
#57360=CARTESIAN_POINT('Ctrl Pts',(-4.89482353060398,13.4899557430043,11.6406728644763));
#57361=CARTESIAN_POINT('Ctrl Pts',(-4.88338293199389,12.554088377827,11.5883394886922));
#57362=CARTESIAN_POINT('Ctrl Pts',(-5.26479155556264,11.8234099202509,11.5360061129082));
#57363=CARTESIAN_POINT('Ctrl Pts',(-5.64620017913138,11.0927314626748,11.4836727371241));
#57364=CARTESIAN_POINT('Ctrl Pts',(-6.42045802487898,10.5672419126997,11.43133936134));
#57365=CARTESIAN_POINT('Ctrl Pts',(-7.24029926801916,10.482369652534,11.3790059855559));
#57366=CARTESIAN_POINT('Ctrl Pts',(-8.06014051115934,10.3974973923684,11.3266726097718));
#57367=CARTESIAN_POINT('Ctrl Pts',(-8.92556515169212,10.753242422012,11.2743392339877));
#57368=CARTESIAN_POINT('Ctrl Pts',(-9.44861906997071,11.3901953896836,11.2220058582037));
#57369=CARTESIAN_POINT('Ctrl Pts',(-9.81316588581269,11.8341251034117,11.1855316729664));
#57370=CARTESIAN_POINT('Ctrl Pts',(-10.0114057826858,12.4146518528183,11.1490574877292));
#57371=CARTESIAN_POINT('Ctrl Pts',(-10.0159019782719,12.9923925656114,11.112583302492));
#57372=CARTESIAN_POINT('Origin',(-7.5,12.9903810567666,14.2084234471775));
#57373=CARTESIAN_POINT('',(-10.5774088918681,12.99185618799,4.79157655282255));
#57374=CARTESIAN_POINT('',(-10.5686791348591,12.9902767031652,4.70842344717746));
#57375=CARTESIAN_POINT('',(-10.5735,12.9903810567666,14.2084234471775));
#57376=CARTESIAN_POINT('',(-6.70620071746715,10.0211581030209,4.));
#57377=CARTESIAN_POINT('Ctrl Pts',(-10.5686791348591,12.9902767031652,4.70842344717746));
#57378=CARTESIAN_POINT('Ctrl Pts',(-10.568341542465,13.509926201974,4.68161580125464));
#57379=CARTESIAN_POINT('Ctrl Pts',(-10.1982938594512,15.0443643081101,4.60247477954774));
#57380=CARTESIAN_POINT('Ctrl Pts',(-7.78634777823694,16.5973803971072,4.47100038205676));
#57381=CARTESIAN_POINT('Ctrl Pts',(-4.64704915358778,15.2208104036021,4.31400025470451));
#57382=CARTESIAN_POINT('Ctrl Pts',(-4.07060765975928,11.8373819589561,4.15700012735225));
#57383=CARTESIAN_POINT('Ctrl Pts',(-5.72985994157694,10.2821754194981,4.05233337578409));
#57384=CARTESIAN_POINT('Ctrl Pts',(-6.70620071746715,10.0211581030209,4.));
#57385=CARTESIAN_POINT('',(-8.29574161562937,10.0163810931058,4.00000000000001));
#57386=CARTESIAN_POINT('Origin',(-7.5,12.9903810567666,4.));
#57387=CARTESIAN_POINT('Ctrl Pts',(-10.5774088918681,12.99185618799,4.79157655282254));
#57388=CARTESIAN_POINT('Ctrl Pts',(-10.5779243576744,13.0789760377035,4.78704908248048));
#57389=CARTESIAN_POINT('Ctrl Pts',(-10.535392897551,14.1726059842126,4.73018823635432));
#57390=CARTESIAN_POINT('Ctrl Pts',(-9.2319528795399,16.1681374132995,4.62099401444409));
#57391=CARTESIAN_POINT('Ctrl Pts',(-5.80479653057489,16.1883357805992,4.46399388709183));
#57392=CARTESIAN_POINT('Ctrl Pts',(-3.89775210281319,13.3398493780975,4.30699375973959));
#57393=CARTESIAN_POINT('Ctrl Pts',(-5.2011833457958,10.227049143879,4.15232913070897));
#57394=CARTESIAN_POINT('Ctrl Pts',(-7.36594149062469,9.77083767708475,4.04999787746245));
#57395=CARTESIAN_POINT('Ctrl Pts',(-8.29574920379123,10.0163624306404,4.00000000000001));
#57396=CARTESIAN_POINT('Origin',(-7.5,12.9903810567666,14.2084234471775));
#57397=CARTESIAN_POINT('',(-10.5688836055535,12.9910731523796,5.79157655282255));
#57398=CARTESIAN_POINT('',(-10.5767201283484,12.9885005040359,5.70842344717746));
#57399=CARTESIAN_POINT('',(-10.5735,12.9903810567666,14.2084234471775));
#57400=CARTESIAN_POINT('Ctrl Pts',(-10.5767201283484,12.9885005040358,5.70842344717746));
#57401=CARTESIAN_POINT('Ctrl Pts',(-10.5702728094234,13.8768977505312,5.66228272262582));
#57402=CARTESIAN_POINT('Ctrl Pts',(-9.70223158388916,15.7839304785174,5.56380862229009));
#57403=CARTESIAN_POINT('Ctrl Pts',(-6.48106323809927,16.4631861795336,5.41300114617029));
#57404=CARTESIAN_POINT('Ctrl Pts',(-4.04127258839909,14.0562954080889,5.25600101881802));
#57405=CARTESIAN_POINT('Ctrl Pts',(-4.70303600953422,10.693474125437,5.09900089146578));
#57406=CARTESIAN_POINT('Ctrl Pts',(-7.87270732364685,9.390536089231,4.94200076411351));
#57407=CARTESIAN_POINT('Ctrl Pts',(-10.2242696810485,10.9865434678639,4.81180828268408));
#57408=CARTESIAN_POINT('Ctrl Pts',(-10.5690005839068,12.4954763477989,4.73394917703873));
#57409=CARTESIAN_POINT('Ctrl Pts',(-10.5686791348591,12.9902767031652,4.70842344717746));
#57410=CARTESIAN_POINT('Ctrl Pts',(-10.5688836055535,12.9910731523796,5.79157655282255));
#57411=CARTESIAN_POINT('Ctrl Pts',(-10.5698353122932,13.4534929538237,5.76771600385165));
#57412=CARTESIAN_POINT('Ctrl Pts',(-10.2562652325398,14.9289132187583,5.69152207909668));
#57413=CARTESIAN_POINT('Ctrl Pts',(-7.98558646537732,16.576874141135,5.56299477855761));
#57414=CARTESIAN_POINT('Ctrl Pts',(-4.77645105419042,15.3738768659897,5.40599465120536));
#57415=CARTESIAN_POINT('Ctrl Pts',(-4.00954823259222,12.0335573562934,5.24899452385311));
#57416=CARTESIAN_POINT('Ctrl Pts',(-6.37256675930357,9.55126737969704,5.09199439650085));
#57417=CARTESIAN_POINT('Ctrl Pts',(-9.64926869943611,10.135445743826,4.93952173949067));
#57418=CARTESIAN_POINT('Ctrl Pts',(-10.571966049015,12.0719510350338,4.83938245826456));
#57419=CARTESIAN_POINT('Ctrl Pts',(-10.5774088918681,12.99185618799,4.79157655282254));
#57420=CARTESIAN_POINT('Origin',(-7.5,12.9903810567666,14.2084234471775));
#57421=CARTESIAN_POINT('',(-10.5752286789639,12.9879604379016,6.79157655282255));
#57422=CARTESIAN_POINT('',(-10.5729905958558,12.9930261911251,6.70842344717746));
#57423=CARTESIAN_POINT('',(-10.5735,12.9903810567666,14.2084234471775));
#57424=CARTESIAN_POINT('Ctrl Pts',(-10.5729905958558,12.9930261911251,6.70842344717746));
#57425=CARTESIAN_POINT('Ctrl Pts',(-10.5751986555521,13.2468284658167,6.69528301978108));
#57426=CARTESIAN_POINT('Ctrl Pts',(-10.4312906141563,14.5089611116288,6.62980921660061));
#57427=CARTESIAN_POINT('Ctrl Pts',(-8.69550582596531,16.4064477577484,6.51200203763606));
#57428=CARTESIAN_POINT('Ctrl Pts',(-5.31022637025923,15.8719837317436,6.3550019102838));
#57429=CARTESIAN_POINT('Ctrl Pts',(-3.88853720662811,12.7535599895385,6.19800178293155));
#57430=CARTESIAN_POINT('Ctrl Pts',(-5.70528280371351,9.84749392134933,6.04100165557929));
#57431=CARTESIAN_POINT('Ctrl Pts',(-9.13136573648253,9.75968890749465,5.88400152822705));
#57432=CARTESIAN_POINT('Ctrl Pts',(-10.5176205520478,11.7432796147819,5.77314212542643));
#57433=CARTESIAN_POINT('Ctrl Pts',(-10.5775854376359,12.8692666957923,5.7146160984099));
#57434=CARTESIAN_POINT('Ctrl Pts',(-10.5767201283484,12.9885005040358,5.70842344717746));
#57435=CARTESIAN_POINT('Ctrl Pts',(-10.5752286789639,12.9879604379016,6.79157655282255));
#57436=CARTESIAN_POINT('Ctrl Pts',(-10.5680430414674,13.8206658595303,6.74838292522283));
#57437=CARTESIAN_POINT('Ctrl Pts',(-9.79183063316292,15.6740884921896,6.65285592183902));
#57438=CARTESIAN_POINT('Ctrl Pts',(-6.67544470099851,16.5144205342573,6.50499554267113));
#57439=CARTESIAN_POINT('Ctrl Pts',(-4.10581110106408,14.2466564935293,6.34799541531888));
#57440=CARTESIAN_POINT('Ctrl Pts',(-4.57977925134152,10.8523778836063,6.19099528796662));
#57441=CARTESIAN_POINT('Ctrl Pts',(-7.67233735803906,9.3752678814539,6.03399516061438));
#57442=CARTESIAN_POINT('Ctrl Pts',(-10.1638445777963,10.8716837770844,5.90085558223301));
#57443=CARTESIAN_POINT('Ctrl Pts',(-10.5677479325558,12.4392669496988,5.82004937963574));
#57444=CARTESIAN_POINT('Ctrl Pts',(-10.5688836055535,12.9910731523796,5.79157655282255));
#57445=CARTESIAN_POINT('Origin',(-7.5,12.9903810567666,14.2084234471775));
#57446=CARTESIAN_POINT('',(-10.5746464410021,12.992919470803,7.79157655282256));
#57447=CARTESIAN_POINT('',(-10.5698472063158,12.988625624027,7.70842344717746));
#57448=CARTESIAN_POINT('',(-10.5735,12.9903810567666,14.2084234471775));
#57449=CARTESIAN_POINT('Ctrl Pts',(-10.5698472063158,12.988625624027,7.70842344717746));
#57450=CARTESIAN_POINT('Ctrl Pts',(-10.5664960358364,13.6174691755491,7.67594994115225));
#57451=CARTESIAN_POINT('Ctrl Pts',(-10.0746935678837,15.2645519082853,7.59114305934296));
#57452=CARTESIAN_POINT('Ctrl Pts',(-7.39948646190492,16.6082039047423,7.45400280174958));
#57453=CARTESIAN_POINT('Ctrl Pts',(-4.42700258466931,14.902299453002,7.29700267439732));
#57454=CARTESIAN_POINT('Ctrl Pts',(-4.21010495775379,11.4819594519348,7.14000254704507));
#57455=CARTESIAN_POINT('Ctrl Pts',(-6.94328780249567,9.41423553851335,6.98300241969282));
#57456=CARTESIAN_POINT('Ctrl Pts',(-9.90513850811741,10.4579415361298,6.83914271973694));
#57457=CARTESIAN_POINT('Ctrl Pts',(-10.5664047849758,12.2360295461447,6.74761639556516));
#57458=CARTESIAN_POINT('Ctrl Pts',(-10.5729905958558,12.9930261911251,6.70842344717746));
#57459=CARTESIAN_POINT('Ctrl Pts',(-10.5746464410021,12.992919470803,7.79157655282255));
#57460=CARTESIAN_POINT('Ctrl Pts',(-10.5763833959288,13.1895272793482,7.78138322237809));
#57461=CARTESIAN_POINT('Ctrl Pts',(-10.4703645847954,14.393670666495,7.71885651614954));
#57462=CARTESIAN_POINT('Ctrl Pts',(-8.88333173423194,16.3348001890992,7.6039964341369));
#57463=CARTESIAN_POINT('Ctrl Pts',(-5.47359896850368,15.9891216041795,7.44699630678466));
#57464=CARTESIAN_POINT('Ctrl Pts',(-3.88095944817013,12.9544436048999,7.28999617943239));
#57465=CARTESIAN_POINT('Ctrl Pts',(-5.53354831017302,9.95199105749957,7.13299605208015));
#57466=CARTESIAN_POINT('Ctrl Pts',(-8.9494732676674,9.67409198306777,6.97599592472789));
#57467=CARTESIAN_POINT('Ctrl Pts',(-10.4834447329667,11.6282633493619,6.86218942497536));
#57468=CARTESIAN_POINT('Ctrl Pts',(-10.5767491559627,12.8117604221037,6.80071630100691));
#57469=CARTESIAN_POINT('Ctrl Pts',(-10.5752286789639,12.9879604379016,6.79157655282255));
#57470=CARTESIAN_POINT('Origin',(-7.5,12.9903810567666,14.2084234471775));
#57471=CARTESIAN_POINT('',(-10.5690545220509,12.9893859879631,8.79157655282255));
#57472=CARTESIAN_POINT('',(-10.5783066056774,12.9902007559877,8.70842344717746));
#57473=CARTESIAN_POINT('',(-10.5735,12.9903810567666,14.2084234471775));
#57474=CARTESIAN_POINT('Ctrl Pts',(-10.5783066056774,12.9902007559877,8.70842344717746));
#57475=CARTESIAN_POINT('Ctrl Pts',(-10.5774421776949,13.9863223355525,8.65661686252342));
#57476=CARTESIAN_POINT('Ctrl Pts',(-9.51496009867182,15.9902813747918,8.5524769020853));
#57477=CARTESIAN_POINT('Ctrl Pts',(-6.11666831357863,16.3348000735102,8.3960035658631));
#57478=CARTESIAN_POINT('Ctrl Pts',(-3.9473824601037,13.6815060275445,8.23900343851085));
#57479=CARTESIAN_POINT('Ctrl Pts',(-4.9637628366961,10.4084735910568,8.08200331115859));
#57480=CARTESIAN_POINT('Ctrl Pts',(-8.25441140963209,9.45066234771208,7.92500318380633));
#57481=CARTESIAN_POINT('Ctrl Pts',(-10.3278657153401,11.208539372,7.80047656247929));
#57482=CARTESIAN_POINT('Ctrl Pts',(-10.5718966865663,12.6040428499268,7.72828331693633));
#57483=CARTESIAN_POINT('Ctrl Pts',(-10.5698472063158,12.988625624027,7.70842344717746));
#57484=CARTESIAN_POINT('Ctrl Pts',(-10.5690545220509,12.9893859879631,8.79157655282255));
#57485=CARTESIAN_POINT('Ctrl Pts',(-10.5673548564085,13.5615306833804,8.76205014374926));
#57486=CARTESIAN_POINT('Ctrl Pts',(-10.1411931381796,15.1501114670399,8.6801903588919));
#57487=CARTESIAN_POINT('Ctrl Pts',(-7.60051354156566,16.6082040297755,8.54599719825042));
#57488=CARTESIAN_POINT('Ctrl Pts',(-4.53789809794217,15.0699719631857,8.38899707089818));
#57489=CARTESIAN_POINT('Ctrl Pts',(-4.1314278504052,11.6669507850401,8.23199694354592));
#57490=CARTESIAN_POINT('Ctrl Pts',(-6.74558856429446,9.45066222537301,8.07499681619367));
#57491=CARTESIAN_POINT('Ctrl Pts',(-9.82258984821385,10.3462870118539,7.92819001928587));
#57492=CARTESIAN_POINT('Ctrl Pts',(-10.5674657300694,12.1801270266301,7.83371659816217));
#57493=CARTESIAN_POINT('Ctrl Pts',(-10.5746464410021,12.992919470803,7.79157655282255));
#57494=CARTESIAN_POINT('Origin',(-7.5,12.9903810567666,14.2084234471775));
#57495=CARTESIAN_POINT('',(-10.5777630782332,12.9892372109846,9.79157655282255));
#57496=CARTESIAN_POINT('',(-10.5702336112086,12.9923647073181,9.70842344717745));
#57497=CARTESIAN_POINT('',(-10.5735,12.9903810567666,14.2084234471775));
#57498=CARTESIAN_POINT('Ctrl Pts',(-10.5702336112086,12.9923647073181,9.70842344717746));
#57499=CARTESIAN_POINT('Ctrl Pts',(-10.5724448600627,13.3564296204275,9.68961715967868));
#57500=CARTESIAN_POINT('Ctrl Pts',(-10.3454482739325,14.7309332712505,9.61847749639582));
#57501=CARTESIAN_POINT('Ctrl Pts',(-8.32455527051676,16.5144204123725,9.49500445732887));
#57502=CARTESIAN_POINT('Ctrl Pts',(-5.01553513899265,15.6221446466417,9.33800432997661));
#57503=CARTESIAN_POINT('Ctrl Pts',(-3.93435848267263,12.3699411347509,9.18100420262437));
#57504=CARTESIAN_POINT('Ctrl Pts',(-6.0505267824277,9.67409209769908,9.02400407527211));
#57505=CARTESIAN_POINT('Ctrl Pts',(-9.46645162186327,9.95199116250562,8.86700394791985));
#57506=CARTESIAN_POINT('Ctrl Pts',(-10.573722513556,11.9637004181345,8.76181040522164));
#57507=CARTESIAN_POINT('Ctrl Pts',(-10.5783153955445,12.9800717730395,8.70895023830751));
#57508=CARTESIAN_POINT('Ctrl Pts',(-10.5783066056774,12.9902007559877,8.70842344717746));
#57509=CARTESIAN_POINT('Ctrl Pts',(-10.5777630782332,12.9892372109846,9.79157655282255));
#57510=CARTESIAN_POINT('Ctrl Pts',(-10.5732100242337,13.9291375746327,9.74271706512043));
#57511=CARTESIAN_POINT('Ctrl Pts',(-9.61486878320428,15.8838097348119,9.64152420163422));
#57512=CARTESIAN_POINT('Ctrl Pts',(-6.30449413259093,16.4064478755407,9.48799796236394));
#57513=CARTESIAN_POINT('Ctrl Pts',(-3.99123576757957,13.8776914962184,9.3309978350117));
#57514=CARTESIAN_POINT('Ctrl Pts',(-4.82432014168349,10.5532756064786,9.17399770765943));
#57515=CARTESIAN_POINT('Ctrl Pts',(-8.05671221676616,9.41423541495656,9.0169975803072));
#57516=CARTESIAN_POINT('Ctrl Pts',(-10.2758759707643,11.0930905163184,8.88952386202821));
#57517=CARTESIAN_POINT('Ctrl Pts',(-10.5703673880222,12.5474465367502,8.81438351953334));
#57518=CARTESIAN_POINT('Ctrl Pts',(-10.5690545220509,12.9893859879631,8.79157655282255));
#57519=CARTESIAN_POINT('Origin',(-7.5,12.9903810567666,14.2084234471775));
#57520=CARTESIAN_POINT('',(-10.5715490487462,12.9928368154298,10.7915765528225));
#57521=CARTESIAN_POINT('',(-10.5724150045772,12.9877735244422,10.7084234471775));
#57522=CARTESIAN_POINT('',(-10.5735,12.9903810567666,14.2084234471775));
#57523=CARTESIAN_POINT('Ctrl Pts',(-10.5724150045772,12.9877735244422,10.7084234471775));
#57524=CARTESIAN_POINT('Ctrl Pts',(-10.5662071249442,13.7247736829249,10.6702840810499));
#57525=CARTESIAN_POINT('Ctrl Pts',(-9.93341852875246,15.4826369193415,10.5798113391382));
#57526=CARTESIAN_POINT('Ctrl Pts',(-7.01441355218445,16.5768740138536,10.4370052214424));
#57527=CARTESIAN_POINT('Ctrl Pts',(-4.24070833971001,14.56383815303,10.2800050940901));
#57528=CARTESIAN_POINT('Ctrl Pts',(-4.38964119697082,11.1398633340167,10.1230049667379));
#57529=CARTESIAN_POINT('Ctrl Pts',(-7.32766264781398,9.3752680069458,9.96600483938563));
#57530=CARTESIAN_POINT('Ctrl Pts',(-10.0497780511113,10.6754420854925,9.82781099953215));
#57531=CARTESIAN_POINT('Ctrl Pts',(-10.5662914862381,12.3433245134896,9.74195053546276));
#57532=CARTESIAN_POINT('Ctrl Pts',(-10.5702336112086,12.9923647073181,9.70842344717746));
#57533=CARTESIAN_POINT('Ctrl Pts',(-10.5715490487462,12.9928368154298,10.7915765528225));
#57534=CARTESIAN_POINT('Ctrl Pts',(-10.5739357845658,13.2995215285911,10.7757173622757));
#57535=CARTESIAN_POINT('Ctrl Pts',(-10.391916652594,14.6154630132259,10.7075247959447));
#57536=CARTESIAN_POINT('Ctrl Pts',(-8.5189368031419,16.4631863186891,10.5869988538297));
#57537=CARTESIAN_POINT('Ctrl Pts',(-5.16549655959477,15.7560380892136,10.4299987264775));
#57538=CARTESIAN_POINT('Ctrl Pts',(-3.90540705298465,12.5688686867556,10.2729985991252));
#57539=CARTESIAN_POINT('Ctrl Pts',(-5.86863420589283,9.75968879265402,10.115998471773));
#57540=CARTESIAN_POINT('Ctrl Pts',(-9.29471725902464,9.84749381445728,9.9589983444207));
#57541=CARTESIAN_POINT('Ctrl Pts',(-10.5460795409153,11.8491727898316,9.85085770477057));
#57542=CARTESIAN_POINT('Ctrl Pts',(-10.5780867983696,12.9224107085984,9.79505044090452));
#57543=CARTESIAN_POINT('Ctrl Pts',(-10.5777630782332,12.9892372109846,9.79157655282255));
#57544=CARTESIAN_POINT('Origin',(-7.5,12.9903810567666,14.2084234471775));
#57545=CARTESIAN_POINT('',(-10.5702206634037,12.9870745539208,11.7915765528226));
#57546=CARTESIAN_POINT('',(-10.5771718362758,12.9919049495641,11.7084234471775));
#57547=CARTESIAN_POINT('',(-10.5735,12.9903810567666,14.2084234471775));
#57548=CARTESIAN_POINT('',(-8.29379928253292,10.0211581030209,12.));
#57549=CARTESIAN_POINT('Ctrl Pts',(-8.29379928253292,10.0211581030209,12.));
#57550=CARTESIAN_POINT('Ctrl Pts',(-9.27014005842312,10.2821754194981,11.9476666242159));
#57551=CARTESIAN_POINT('Ctrl Pts',(-10.3714991025232,11.3144735509882,11.8781921418234));
#57552=CARTESIAN_POINT('Ctrl Pts',(-10.5724953140326,12.655363779409,11.808717659431));
#57553=CARTESIAN_POINT('Ctrl Pts',(-10.5702206634037,12.9870745539208,11.7915765528226));
#57554=CARTESIAN_POINT('',(-6.70425858890745,10.0163809826708,12.));
#57555=CARTESIAN_POINT('Origin',(-7.5,12.9903810567666,12.));
#57556=CARTESIAN_POINT('Ctrl Pts',(-6.70425100699972,10.0163623331919,12.));
#57557=CARTESIAN_POINT('Ctrl Pts',(-7.63405880919358,9.77083750064795,11.9500021225376));
#57558=CARTESIAN_POINT('Ctrl Pts',(-9.69010226711413,10.2041387247117,11.8528099382634));
#57559=CARTESIAN_POINT('Ctrl Pts',(-10.5713066024909,12.0837656721183,11.7556177539892));
#57560=CARTESIAN_POINT('Ctrl Pts',(-10.5771718362758,12.9919049495641,11.7084234471775));
#57561=CARTESIAN_POINT('Origin',(-7.50000000000001,-12.9903810567666,7.5));
#57562=CARTESIAN_POINT('',(-10.0135514395051,-12.9904666377399,4.38741669750803));
#57563=CARTESIAN_POINT('',(-10.0159862278212,-12.9935669321582,4.11258330249198));
#57564=CARTESIAN_POINT('',(-10.0175,-12.9903810567666,7.5));
#57565=CARTESIAN_POINT('',(-9.41346599666503,-11.3543938533916,4.));
#57566=CARTESIAN_POINT('Ctrl Pts',(-10.0159862278212,-12.9935669321582,
4.11258330249198));
#57567=CARTESIAN_POINT('Ctrl Pts',(-10.0108023762528,-12.4010697429433,
4.07505553499466));
#57568=CARTESIAN_POINT('Ctrl Pts',(-9.79922182808404,-11.8055774964621,
4.03752776749733));
#57569=CARTESIAN_POINT('Ctrl Pts',(-9.41346599666503,-11.3543938533916,
4.));
#57570=CARTESIAN_POINT('',(-10.0175,-12.9903810567666,4.));
#57571=CARTESIAN_POINT('Origin',(-7.50000000000001,-12.9903810567666,4.));
#57572=CARTESIAN_POINT('',(-10.0175,-12.9903810567666,3.));
#57573=CARTESIAN_POINT('',(-10.0175,-12.9903810567666,7.5));
#57574=CARTESIAN_POINT('Origin',(-7.50000000000001,-12.9903810567666,3.));
#57575=CARTESIAN_POINT('',(-5.58300636833058,-11.3520706988407,4.));
#57576=CARTESIAN_POINT('Origin',(-7.50000000000001,-12.9903810567666,4.));
#57577=CARTESIAN_POINT('Ctrl Pts',(-5.58299257280548,-11.3520616136783,
4.));
#57578=CARTESIAN_POINT('Ctrl Pts',(-6.09671565847252,-10.7549231085896,
4.04999787746244));
#57579=CARTESIAN_POINT('Ctrl Pts',(-6.91408826359173,-10.4146529403296,
4.09999575492489));
#57580=CARTESIAN_POINT('Ctrl Pts',(-7.6991792943871,-10.4769907523554,4.14999363238733));
#57581=CARTESIAN_POINT('Ctrl Pts',(-8.52094345767964,-10.5422404851016,
4.20232700817142));
#57582=CARTESIAN_POINT('Ctrl Pts',(-9.30733973752043,-11.0485898984475,
4.2546603839555));
#57583=CARTESIAN_POINT('Ctrl Pts',(-9.70625816906456,-11.7696982113955,
4.30699375973958));
#57584=CARTESIAN_POINT('Ctrl Pts',(-9.91060317652291,-12.1390842109776,
4.3338014056624));
#57585=CARTESIAN_POINT('Ctrl Pts',(-10.0132749267868,-12.5648224302545,
4.36060905158521));
#57586=CARTESIAN_POINT('Ctrl Pts',(-10.0135514395051,-12.9904666377399,
4.38741669750803));
#57587=CARTESIAN_POINT('Origin',(-7.50000000000001,-12.9903810567666,7.5));
#57588=CARTESIAN_POINT('',(-10.0201378128903,-12.991921413328,5.38741669750803));
#57589=CARTESIAN_POINT('',(-10.020701946345,-12.9891728119784,5.11258330249198));
#57590=CARTESIAN_POINT('',(-10.0175,-12.9903810567666,7.5));
#57591=CARTESIAN_POINT('Ctrl Pts',(-10.020701946345,-12.9891728119784,5.11258330249198));
#57592=CARTESIAN_POINT('Ctrl Pts',(-10.0211241641948,-12.9178130461518,
5.10805583214991));
#57593=CARTESIAN_POINT('Ctrl Pts',(-10.0183502770585,-12.846486861832,5.10352836180784));
#57594=CARTESIAN_POINT('Ctrl Pts',(-10.0122725294143,-12.775443667658,5.09900089146577));
#57595=CARTESIAN_POINT('Ctrl Pts',(-9.94201937978509,-11.9542499553417,
5.04666751568169));
#57596=CARTESIAN_POINT('Ctrl Pts',(-9.43032999980707,-11.170867192649,4.99433413989761));
#57597=CARTESIAN_POINT('Ctrl Pts',(-8.70662199025935,-10.7764184817432,
4.94200076411352));
#57598=CARTESIAN_POINT('Ctrl Pts',(-7.98291398071162,-10.3819697708373,
4.88966738832944));
#57599=CARTESIAN_POINT('Ctrl Pts',(-7.04718734159418,-10.3764551117184,
4.83733401254535));
#57600=CARTESIAN_POINT('Ctrl Pts',(-6.31898112841336,-10.7625629528365,
4.78500063676127));
#57601=CARTESIAN_POINT('Ctrl Pts',(-5.59077491523255,-11.1486707939545,
4.73266726097718));
#57602=CARTESIAN_POINT('Ctrl Pts',(-5.07008912798835,-11.9264011353096,
4.6803338851931));
#57603=CARTESIAN_POINT('Ctrl Pts',(-4.99037287718051,-12.7466319075856,
4.62800050940901));
#57604=CARTESIAN_POINT('Ctrl Pts',(-4.91065662637267,-13.5668626798615,
4.57566713362493));
#57605=CARTESIAN_POINT('Ctrl Pts',(-5.27190991200121,-14.4295938830583,
4.52333375784085));
#57606=CARTESIAN_POINT('Ctrl Pts',(-5.9121672709983,-14.948847615037,4.47100038205676));
#57607=CARTESIAN_POINT('Ctrl Pts',(-6.55242462999539,-15.4681013470158,
4.41866700627267));
#57608=CARTESIAN_POINT('Ctrl Pts',(-7.47168606236103,-15.6438776077765,
4.36633363048859));
#57609=CARTESIAN_POINT('Ctrl Pts',(-8.25780335304795,-15.3956944886946,
4.31400025470451));
#57610=CARTESIAN_POINT('Ctrl Pts',(-9.04392064373486,-15.1475113696128,
4.26166687892042));
#57611=CARTESIAN_POINT('Ctrl Pts',(-9.69689379274305,-14.4753688706883,
4.20933350313634));
#57612=CARTESIAN_POINT('Ctrl Pts',(-9.92376658082896,-13.6843861063472,
4.15700012735226));
#57613=CARTESIAN_POINT('Ctrl Pts',(-9.98795104401328,-13.460609581425,4.1421945190655));
#57614=CARTESIAN_POINT('Ctrl Pts',(-10.0180313821391,-13.2273213460105,
4.12738891077874));
#57615=CARTESIAN_POINT('Ctrl Pts',(-10.0159862278212,-12.9935669321582,
4.11258330249198));
#57616=CARTESIAN_POINT('Ctrl Pts',(-10.0135514395051,-12.9904666377399,
4.38741669750803));
#57617=CARTESIAN_POINT('Ctrl Pts',(-10.013814729649,-13.3957569451608,4.41294242736929));
#57618=CARTESIAN_POINT('Ctrl Pts',(-9.92124152424158,-13.8009620169255,
4.43846815723057));
#57619=CARTESIAN_POINT('Ctrl Pts',(-9.73520854233975,-14.1573521883653,
4.46399388709184));
#57620=CARTESIAN_POINT('Ctrl Pts',(-9.35379990082332,-14.8880306398367,
4.51632726287592));
#57621=CARTESIAN_POINT('Ctrl Pts',(-8.57954203454297,-15.4135203302294,
4.56866063866001));
#57622=CARTESIAN_POINT('Ctrl Pts',(-7.75970075309617,-15.4983926191754,
4.62099401444409));
#57623=CARTESIAN_POINT('Ctrl Pts',(-6.93985947164937,-15.5832649081213,
4.67332739022818));
#57624=CARTESIAN_POINT('Ctrl Pts',(-6.07443477503611,-15.2275197956205,
4.72566076601226));
#57625=CARTESIAN_POINT('Ctrl Pts',(-5.5513808289996,-14.5905667824841,4.77799414179634));
#57626=CARTESIAN_POINT('Ctrl Pts',(-5.02832688296309,-13.9536137693476,
4.83032751758043));
#57627=CARTESIAN_POINT('Ctrl Pts',(-4.84764368750334,-13.0354528555755,
4.88266089336451));
#57628=CARTESIAN_POINT('Ctrl Pts',(-5.09037368993613,-12.2477921509444,
4.93499426914859));
#57629=CARTESIAN_POINT('Ctrl Pts',(-5.33310369236891,-11.4601314463133,
4.98732764493268));
#57630=CARTESIAN_POINT('Ctrl Pts',(-5.99924689269421,-10.8029709508232,
5.03966102071677));
#57631=CARTESIAN_POINT('Ctrl Pts',(-6.79011830096555,-10.5709280850384,
5.09199439650085));
#57632=CARTESIAN_POINT('Ctrl Pts',(-7.58098970923688,-10.3388852192536,
5.14432777228494));
#57633=CARTESIAN_POINT('Ctrl Pts',(-8.49658932545427,-10.5319599831741,
5.19666114806902));
#57634=CARTESIAN_POINT('Ctrl Pts',(-9.1264120969476,-11.0635984608226,5.2489945238531));
#57635=CARTESIAN_POINT('Ctrl Pts',(-9.68170742388623,-11.532327721848,5.29513524840475));
#57636=CARTESIAN_POINT('Ctrl Pts',(-10.0148568228205,-12.2642362843572,
5.34127597295639));
#57637=CARTESIAN_POINT('Ctrl Pts',(-10.0201378128903,-12.991921413328,5.38741669750803));
#57638=CARTESIAN_POINT('Origin',(-7.50000000000001,-12.9903810567666,7.5));
#57639=CARTESIAN_POINT('',(-10.0170829580245,-12.9882144302548,6.38741669750803));
#57640=CARTESIAN_POINT('',(-10.0137189064297,-12.9898141627747,6.11258330249198));
#57641=CARTESIAN_POINT('',(-10.0175,-12.9903810567666,7.5));
#57642=CARTESIAN_POINT('Ctrl Pts',(-10.0137189064297,-12.9898141627747,
6.11258330249198));
#57643=CARTESIAN_POINT('Ctrl Pts',(-10.0144984482212,-12.6110466544282,
6.08872275352109));
#57644=CARTESIAN_POINT('Ctrl Pts',(-9.93406605373638,-12.2325935036327,
6.06486220455019));
#57645=CARTESIAN_POINT('Ctrl Pts',(-9.77069376862533,-11.8941805898436,
6.04100165557929));
#57646=CARTESIAN_POINT('Ctrl Pts',(-9.41236910476912,-11.151939067693,5.98866827979521));
#57647=CARTESIAN_POINT('Ctrl Pts',(-8.65505620083081,-10.6023139521363,
5.93633490401113));
#57648=CARTESIAN_POINT('Ctrl Pts',(-7.83829991591844,-10.4917303363644,
5.88400152822705));
#57649=CARTESIAN_POINT('Ctrl Pts',(-7.02154363100607,-10.3811467205925,
5.83166815244296));
#57650=CARTESIAN_POINT('Ctrl Pts',(-6.14534396511963,-10.7096046046056,
5.77933477665887));
#57651=CARTESIAN_POINT('Ctrl Pts',(-5.60254926887142,-11.3298421637022,
5.72700140087479));
#57652=CARTESIAN_POINT('Ctrl Pts',(-5.05975457262321,-11.9500797227988,
5.6746680250907));
#57653=CARTESIAN_POINT('Ctrl Pts',(-4.8503648460132,-12.862096956979,5.62233464930662));
#57654=CARTESIAN_POINT('Ctrl Pts',(-5.06826092360056,-13.6569790435728,
5.57000127352254));
#57655=CARTESIAN_POINT('Ctrl Pts',(-5.28615700118792,-14.4518611301666,
5.51766789773845));
#57656=CARTESIAN_POINT('Ctrl Pts',(-5.93133888297262,-15.129608069174,5.46533452195437));
#57657=CARTESIAN_POINT('Ctrl Pts',(-6.71453628267279,-15.3863634879565,
5.41300114617028));
#57658=CARTESIAN_POINT('Ctrl Pts',(-7.49773368237297,-15.6431189067389,
5.3606677703862));
#57659=CARTESIAN_POINT('Ctrl Pts',(-8.41894659998862,-15.4788828052965,
5.30833439460211));
#57660=CARTESIAN_POINT('Ctrl Pts',(-9.06514459915626,-14.9672624236053,
5.25600101881803));
#57661=CARTESIAN_POINT('Ctrl Pts',(-9.65543865112952,-14.4999033965431,
5.20819511337601));
#57662=CARTESIAN_POINT('Ctrl Pts',(-10.0162437157927,-13.7426660344013,
5.160389207934));
#57663=CARTESIAN_POINT('Ctrl Pts',(-10.020701946345,-12.9891728119784,5.11258330249198));
#57664=CARTESIAN_POINT('Ctrl Pts',(-10.0201378128903,-12.991921413328,5.38741669750803));
#57665=CARTESIAN_POINT('Ctrl Pts',(-10.0208465865384,-13.0895856839813,
5.39360934874047));
#57666=CARTESIAN_POINT('Ctrl Pts',(-10.0156494886519,-13.1871738782112,
5.39980199997292));
#57667=CARTESIAN_POINT('Ctrl Pts',(-10.004290929159,-13.2840395347951,5.40599465120536));
#57668=CARTESIAN_POINT('Ctrl Pts',(-9.90830106310784,-14.1026399397423,
5.45832802698944));
#57669=CARTESIAN_POINT('Ctrl Pts',(-9.37227540423617,-14.8696385582602,
5.51066140277353));
#57670=CARTESIAN_POINT('Ctrl Pts',(-8.63654582863995,-15.2411510354214,
5.56299477855761));
#57671=CARTESIAN_POINT('Ctrl Pts',(-7.90081625304375,-15.6126635125827,
5.61532815434169));
#57672=CARTESIAN_POINT('Ctrl Pts',(-6.96538276072302,-15.5886898483873,
5.66766153012578));
#57673=CARTESIAN_POINT('Ctrl Pts',(-6.24965032039424,-15.1799771379828,
5.71999490590986));
#57674=CARTESIAN_POINT('Ctrl Pts',(-5.53391788006544,-14.7712644275784,
5.77232828169395));
#57675=CARTESIAN_POINT('Ctrl Pts',(-5.03788649172861,-13.9778126709648,
5.82466165747803));
#57676=CARTESIAN_POINT('Ctrl Pts',(-4.9839547824182,-13.1553705931073,5.87699503326212));
#57677=CARTESIAN_POINT('Ctrl Pts',(-4.9300230731078,-12.3329285152499,5.9293284090462));
#57678=CARTESIAN_POINT('Ctrl Pts',(-5.31819104282381,-11.4814961161485,
5.98166178483029));
#57679=CARTESIAN_POINT('Ctrl Pts',(-5.97442142669028,-10.9828167750565,
6.03399516061437));
#57680=CARTESIAN_POINT('Ctrl Pts',(-6.63065181055676,-10.4841374339645,
6.08632853639846));
#57681=CARTESIAN_POINT('Ctrl Pts',(-7.5549446085737,-10.338211150882,6.13866191218254));
#57682=CARTESIAN_POINT('Ctrl Pts',(-8.33288886120492,-10.6104648899579,
6.19099528796662));
#57683=CARTESIAN_POINT('Ctrl Pts',(-9.11083311383614,-10.8827186290339,
6.24332866375071));
#57684=CARTESIAN_POINT('Ctrl Pts',(-9.74242882108165,-11.5731523902683,
6.29566203953479));
#57685=CARTESIAN_POINT('Ctrl Pts',(-9.94449694127237,-12.3722067750024,
6.34799541531888));
#57686=CARTESIAN_POINT('Ctrl Pts',(-9.9952343802911,-12.5728419522874,6.36113584271526));
#57687=CARTESIAN_POINT('Ctrl Pts',(-10.0188915771041,-12.7803252875989,
6.37427627011165));
#57688=CARTESIAN_POINT('Ctrl Pts',(-10.0170829580245,-12.9882144302548,
6.38741669750803));
#57689=CARTESIAN_POINT('Origin',(-7.50000000000001,-12.9903810567666,7.5));
#57690=CARTESIAN_POINT('',(-10.0145082114167,-12.9918189296441,7.38741669750803));
#57691=CARTESIAN_POINT('',(-10.018916148665,-12.992363782792,7.11258330249199));
#57692=CARTESIAN_POINT('',(-10.0175,-12.9903810567666,7.5));
#57693=CARTESIAN_POINT('Ctrl Pts',(-10.018916148665,-12.992363782792,7.11258330249199));
#57694=CARTESIAN_POINT('Ctrl Pts',(-10.0130304015467,-12.3102957636159,
7.06938967489226));
#57695=CARTESIAN_POINT('Ctrl Pts',(-9.72554857159998,-11.6238530781169,
7.02619604729253));
#57696=CARTESIAN_POINT('Ctrl Pts',(-9.23088494583046,-11.1568755721922,
6.98300241969281));
#57697=CARTESIAN_POINT('Ctrl Pts',(-8.63155076501069,-10.5910858791674,
6.93066904390873));
#57698=CARTESIAN_POINT('Ctrl Pts',(-7.72807925079087,-10.3474651982644,
6.87833566812465));
#57699=CARTESIAN_POINT('Ctrl Pts',(-6.92554619007859,-10.5352419954014,
6.82600229234057));
#57700=CARTESIAN_POINT('Ctrl Pts',(-6.12301312936631,-10.7230187925383,
6.77366891655648));
#57701=CARTESIAN_POINT('Ctrl Pts',(-5.42141852216156,-11.342193067715,6.72133554077239));
#57702=CARTESIAN_POINT('Ctrl Pts',(-5.13532567649039,-12.1151551330277,
6.6690021649883));
#57703=CARTESIAN_POINT('Ctrl Pts',(-4.84923283081922,-12.8881171983403,
6.61666878920422));
#57704=CARTESIAN_POINT('Ctrl Pts',(-4.97864174668163,-13.8148670537889,
6.56433541342015));
#57705=CARTESIAN_POINT('Ctrl Pts',(-5.46553131494727,-14.4798918223762,
6.51200203763606));
#57706=CARTESIAN_POINT('Ctrl Pts',(-5.95242088321289,-15.1449165909636,
6.45966866185198));
#57707=CARTESIAN_POINT('Ctrl Pts',(-6.79679110388174,-15.5482162726898,
6.40733528606788));
#57708=CARTESIAN_POINT('Ctrl Pts',(-7.62006454012935,-15.5089697827308,
6.3550019102838));
#57709=CARTESIAN_POINT('Ctrl Pts',(-8.44333797637697,-15.4697232927718,
6.30266853449971));
#57710=CARTESIAN_POINT('Ctrl Pts',(-9.24551462820336,-14.9879306311276,
6.25033515871564));
#57711=CARTESIAN_POINT('Ctrl Pts',(-9.6669347422295,-14.2796053359332,6.19800178293155));
#57712=CARTESIAN_POINT('Ctrl Pts',(-9.89621522991991,-13.8942294041248,
6.16952895611836));
#57713=CARTESIAN_POINT('Ctrl Pts',(-10.012788678108,-13.4417979658618,6.14105612930517));
#57714=CARTESIAN_POINT('Ctrl Pts',(-10.0137189064297,-12.9898141627747,
6.11258330249198));
#57715=CARTESIAN_POINT('Ctrl Pts',(-10.0170829580245,-12.9882144302548,
6.38741669750803));
#57716=CARTESIAN_POINT('Ctrl Pts',(-10.0116885281401,-13.6082694857485,
6.42660964589573));
#57717=CARTESIAN_POINT('Ctrl Pts',(-9.77974909684708,-14.2319346209584,
6.46580259428343));
#57718=CARTESIAN_POINT('Ctrl Pts',(-9.36410112291705,-14.688271412029,6.50499554267113));
#57719=CARTESIAN_POINT('Ctrl Pts',(-8.80909665123509,-15.2976066560878,
6.55732891845521));
#57720=CARTESIAN_POINT('Ctrl Pts',(-7.92654717473526,-15.6086021359717,
6.6096622942393));
#57721=CARTESIAN_POINT('Ctrl Pts',(-7.11214796457486,-15.4818215077834,
6.66199567002339));
#57722=CARTESIAN_POINT('Ctrl Pts',(-6.29774875441446,-15.3550408795951,
6.71432904580747));
#57723=CARTESIAN_POINT('Ctrl Pts',(-5.55149981059349,-14.7904841433347,
6.76666242159156));
#57724=CARTESIAN_POINT('Ctrl Pts',(-5.20798543690379,-14.041273034435,6.81899579737564));
#57725=CARTESIAN_POINT('Ctrl Pts',(-4.8644710632141,-13.2920619255352,6.87132917315972));
#57726=CARTESIAN_POINT('Ctrl Pts',(-4.92369125965567,-12.3581964439962,
6.92366254894381));
#57727=CARTESIAN_POINT('Ctrl Pts',(-5.35909436185687,-11.6583796505146,
6.97599592472789));
#57728=CARTESIAN_POINT('Ctrl Pts',(-5.79449746405807,-10.958562857033,7.02832930051198));
#57729=CARTESIAN_POINT('Ctrl Pts',(-6.60608347201889,-10.4927947516089,
7.08066267629606));
#57730=CARTESIAN_POINT('Ctrl Pts',(-7.42997390874126,-10.469904702335,7.13299605208014));
#57731=CARTESIAN_POINT('Ctrl Pts',(-8.25386434546363,-10.4470146530611,
7.18532942786423));
#57732=CARTESIAN_POINT('Ctrl Pts',(-9.09005921094755,-10.8670026599375,
7.23766280364831));
#57733=CARTESIAN_POINT('Ctrl Pts',(-9.56364652484227,-11.5415650835207,
7.2899961794324));
#57734=CARTESIAN_POINT('Ctrl Pts',(-9.8575133022249,-11.9601393986381,7.32246968545761));
#57735=CARTESIAN_POINT('Ctrl Pts',(-10.0117632716449,-12.4767339212603,
7.35494319148282));
#57736=CARTESIAN_POINT('Ctrl Pts',(-10.0145082114167,-12.9918189296441,
7.38741669750803));
#57737=CARTESIAN_POINT('Origin',(-7.50000000000001,-12.9903810567666,7.5));
#57738=CARTESIAN_POINT('',(-10.0214372954169,-12.9905287409231,8.38741669750803));
#57739=CARTESIAN_POINT('',(-10.0184392382435,-12.988301844852,8.11258330249199));
#57740=CARTESIAN_POINT('',(-10.0175,-12.9903810567666,7.5));
#57741=CARTESIAN_POINT('Ctrl Pts',(-10.0184392382435,-12.988301844852,8.11258330249199));
#57742=CARTESIAN_POINT('Ctrl Pts',(-10.0198619759554,-12.8272606230119,
8.10238997204752));
#57743=CARTESIAN_POINT('Ctrl Pts',(-10.0057050234181,-12.6664683956915,
8.09219664160306));
#57744=CARTESIAN_POINT('Ctrl Pts',(-9.97504897913497,-12.5088858958898,
8.08200331115859));
#57745=CARTESIAN_POINT('Ctrl Pts',(-9.81765838984107,-11.699844707237,8.02966993537451));
#57746=CARTESIAN_POINT('Ctrl Pts',(-9.22537188297354,-10.9754080177822,
7.97733655959042));
#57747=CARTESIAN_POINT('Ctrl Pts',(-8.46374395491092,-10.660380492594,7.92500318380633));
#57748=CARTESIAN_POINT('Ctrl Pts',(-7.70211602684831,-10.3453529674058,
7.87266980802225));
#57749=CARTESIAN_POINT('Ctrl Pts',(-6.77114667759061,-10.4397346064841,
7.82033643223817));
#57750=CARTESIAN_POINT('Ctrl Pts',(-6.0882404805551,-10.9012089485628,7.76800305645409));
#57751=CARTESIAN_POINT('Ctrl Pts',(-5.4053342835196,-11.3626832906415,7.71566968067));
#57752=CARTESIAN_POINT('Ctrl Pts',(-4.97049123870628,-12.1912503357206,
7.66333630488591));
#57753=CARTESIAN_POINT('Ctrl Pts',(-4.97867531110115,-13.0154180759185,
7.61100292910183));
#57754=CARTESIAN_POINT('Ctrl Pts',(-4.98685938349602,-13.8395858161164,
7.55866955331774));
#57755=CARTESIAN_POINT('Ctrl Pts',(-5.43807057309907,-14.6593542514331,
7.50633617753366));
#57756=CARTESIAN_POINT('Ctrl Pts',(-6.130006178679,-15.1071762692505,7.45400280174958));
#57757=CARTESIAN_POINT('Ctrl Pts',(-6.82194178425893,-15.554998287068,7.40166942596549));
#57758=CARTESIAN_POINT('Ctrl Pts',(-7.75460180581574,-15.6308738873863,
7.3493360501814));
#57759=CARTESIAN_POINT('Ctrl Pts',(-8.509823648947,-15.3007838855131,7.29700267439732));
#57760=CARTESIAN_POINT('Ctrl Pts',(-9.26504549207826,-14.9706938836398,
7.24466929861323));
#57761=CARTESIAN_POINT('Ctrl Pts',(-9.84282915678396,-14.2346382795751,
7.19233592282916));
#57762=CARTESIAN_POINT('Ctrl Pts',(-9.98412256542695,-13.4226311249693,
7.14000254704507));
#57763=CARTESIAN_POINT('Ctrl Pts',(-10.0087987143617,-13.2808183562381,
7.13086279886071));
#57764=CARTESIAN_POINT('Ctrl Pts',(-10.0201615695645,-13.1366890058931,
7.12172305067635));
#57765=CARTESIAN_POINT('Ctrl Pts',(-10.018916148665,-12.992363782792,7.11258330249199));
#57766=CARTESIAN_POINT('Ctrl Pts',(-10.0145082114167,-12.9918189296441,
7.38741669750803));
#57767=CARTESIAN_POINT('Ctrl Pts',(-10.0161869382632,-13.306830224492,7.4072765672669));
#57768=CARTESIAN_POINT('Ctrl Pts',(-9.96119980531574,-13.6212769313365,
7.42713643702578));
#57769=CARTESIAN_POINT('Ctrl Pts',(-9.84682750368121,-13.9123926462011,
7.44699630678465));
#57770=CARTESIAN_POINT('Ctrl Pts',(-9.54544140631991,-14.6795209450086,
7.49932968256874));
#57771=CARTESIAN_POINT('Ctrl Pts',(-8.83168944929182,-15.2846407023335,
7.55166305835282));
#57772=CARTESIAN_POINT('Ctrl Pts',(-8.02558574588715,-15.4564435717975,
7.60399643413691));
#57773=CARTESIAN_POINT('Ctrl Pts',(-7.21948204248248,-15.6282464412614,
7.65632980992099));
#57774=CARTESIAN_POINT('Ctrl Pts',(-6.32102659270125,-15.3667324228643,
7.70866318570508));
#57775=CARTESIAN_POINT('Ctrl Pts',(-5.73304620733022,-14.789152581525,7.76099656148916));
#57776=CARTESIAN_POINT('Ctrl Pts',(-5.1450658219592,-14.2115727401857,7.81332993727324));
#57777=CARTESIAN_POINT('Ctrl Pts',(-4.86756050099838,-13.3179270759042,
7.86566331305732));
#57778=CARTESIAN_POINT('Ctrl Pts',(-5.02495108614128,-12.5088859085888,
7.91799668884141));
#57779=CARTESIAN_POINT('Ctrl Pts',(-5.18234167128417,-11.6998447412735,
7.9703300646255));
#57780=CARTESIAN_POINT('Ctrl Pts',(-5.77462816253079,-10.9754080709243,
8.02266344040959));
#57781=CARTESIAN_POINT('Ctrl Pts',(-6.53625607050644,-10.6603805540446,
8.07499681619367));
#57782=CARTESIAN_POINT('Ctrl Pts',(-7.29788397848209,-10.3453530371649,
8.12733019197775));
#57783=CARTESIAN_POINT('Ctrl Pts',(-8.22885330318678,-10.4397346737546,
8.17966356776183));
#57784=CARTESIAN_POINT('Ctrl Pts',(-8.91175948221152,-10.9012090036623,
8.23199694354592));
#57785=CARTESIAN_POINT('Ctrl Pts',(-9.5877914836703,-11.3580381032537,8.28380352819995));
#57786=CARTESIAN_POINT('Ctrl Pts',(-10.0207292434803,-12.1746067346983,
8.33561011285399));
#57787=CARTESIAN_POINT('Ctrl Pts',(-10.0214372954169,-12.9905287409231,
8.38741669750803));
#57788=CARTESIAN_POINT('Origin',(-7.50000000000001,-12.9903810567666,7.5));
#57789=CARTESIAN_POINT('',(-10.014824715197,-12.9887562509003,9.38741669750802));
#57790=CARTESIAN_POINT('',(-10.0138589040853,-12.9911961164478,9.11258330249198));
#57791=CARTESIAN_POINT('',(-10.0175,-12.9903810567666,7.5));
#57792=CARTESIAN_POINT('Ctrl Pts',(-10.0138589040853,-12.9911961164478,
9.11258330249198));
#57793=CARTESIAN_POINT('Ctrl Pts',(-10.0124667099841,-12.5225530777913,
9.08305689341869));
#57794=CARTESIAN_POINT('Ctrl Pts',(-9.88655945291767,-12.0532151702485,
9.05353048434541));
#57795=CARTESIAN_POINT('Ctrl Pts',(-9.64090569460772,-11.6583796153827,
9.02400407527212));
#57796=CARTESIAN_POINT('Ctrl Pts',(-9.20550258092411,-10.9585628034427,
8.97167069948803));
#57797=CARTESIAN_POINT('Ctrl Pts',(-8.39391655155678,-10.4927946857384,
8.91933732370393));
#57798=CARTESIAN_POINT('Ctrl Pts',(-7.57002609310491,-10.4699046358618,
8.86700394791985));
#57799=CARTESIAN_POINT('Ctrl Pts',(-6.74613563465304,-10.4470145859851,
8.81467057213576));
#57800=CARTESIAN_POINT('Ctrl Pts',(-5.90994074711664,-10.8670026039362,
8.7623371963517));
#57801=CARTESIAN_POINT('Ctrl Pts',(-5.43635342073195,-11.5415650453096,
8.71000382056761));
#57802=CARTESIAN_POINT('Ctrl Pts',(-4.96276609434725,-12.216127486683,8.65767044478353));
#57803=CARTESIAN_POINT('Ctrl Pts',(-4.85178632911427,-13.1452643514787,
8.60533706899943));
#57804=CARTESIAN_POINT('Ctrl Pts',(-5.15317243442415,-13.9123926705184,
8.55300369321534));
#57805=CARTESIAN_POINT('Ctrl Pts',(-5.45455853973402,-14.6795209895581,
8.50067031743125));
#57806=CARTESIAN_POINT('Ctrl Pts',(-6.16831051558674,-15.2846407628417,
8.44833694164718));
#57807=CARTESIAN_POINT('Ctrl Pts',(-6.97441424025143,-15.4564436368365,
8.3960035658631));
#57808=CARTESIAN_POINT('Ctrl Pts',(-7.78051796491612,-15.6282465108314,
8.34367019007902));
#57809=CARTESIAN_POINT('Ctrl Pts',(-8.67897343839277,-15.3667324855376,
8.29133681429492));
#57810=CARTESIAN_POINT('Ctrl Pts',(-9.26695383927095,-14.7891526289653,
8.23900343851084));
#57811=CARTESIAN_POINT('Ctrl Pts',(-9.74040926576667,-14.324071961446,8.19686339317122));
#57812=CARTESIAN_POINT('Ctrl Pts',(-10.0125575264699,-13.6540591679237,
8.15472334783161));
#57813=CARTESIAN_POINT('Ctrl Pts',(-10.0184392382435,-12.988301844852,8.11258330249199));
#57814=CARTESIAN_POINT('Ctrl Pts',(-10.0214372954169,-12.9905287409231,
8.38741669750803));
#57815=CARTESIAN_POINT('Ctrl Pts',(-10.0214444951867,-12.9988253788613,
8.38794348863808));
#57816=CARTESIAN_POINT('Ctrl Pts',(-10.0214070037996,-13.0071219499406,
8.38847027976813));
#57817=CARTESIAN_POINT('Ctrl Pts',(-10.0213246224021,-13.0154180752574,
8.38899707089817));
#57818=CARTESIAN_POINT('Ctrl Pts',(-10.0131405502232,-13.8395857937195,
8.44133044668226));
#57819=CARTESIAN_POINT('Ctrl Pts',(-9.56192937252059,-14.6593542074181,
8.49366382246634));
#57820=CARTESIAN_POINT('Ctrl Pts',(-8.86999378518945,-15.1071762134239,
8.54599719825042));
#57821=CARTESIAN_POINT('Ctrl Pts',(-8.17805819785831,-15.5549982194297,
8.59833057403451));
#57822=CARTESIAN_POINT('Ctrl Pts',(-7.24539820089864,-15.6308738177427,
8.6506639498186));
#57823=CARTESIAN_POINT('Ctrl Pts',(-6.49017637768564,-15.300783824577,8.70299732560268));
#57824=CARTESIAN_POINT('Ctrl Pts',(-5.73495455447264,-14.9706938314114,
8.75533070138677));
#57825=CARTESIAN_POINT('Ctrl Pts',(-5.15717090500631,-14.2346382467671,
8.80766407717085));
#57826=CARTESIAN_POINT('Ctrl Pts',(-5.01587750008917,-13.4226311135736,
8.85999745295493));
#57827=CARTESIAN_POINT('Ctrl Pts',(-4.87458409517204,-12.6106239803801,
8.91233082873901));
#57828=CARTESIAN_POINT('Ctrl Pts',(-5.16978093480409,-11.7226652986374,
8.96466420452309));
#57829=CARTESIAN_POINT('Ctrl Pts',(-5.76911509981821,-11.1568756205409,
9.01699758030718));
#57830=CARTESIAN_POINT('Ctrl Pts',(-6.36844926483233,-10.5910859424444,
9.06933095609127));
#57831=CARTESIAN_POINT('Ctrl Pts',(-7.27192075522852,-10.3474652679941,
9.12166433187536));
#57832=CARTESIAN_POINT('Ctrl Pts',(-8.07445379477299,-10.5352420601668,
9.17399770765945));
#57833=CARTESIAN_POINT('Ctrl Pts',(-8.87698683431745,-10.7230188523395,
9.22633108344353));
#57834=CARTESIAN_POINT('Ctrl Pts',(-9.5785814230102,-11.3421931111353,9.27866445922761));
#57835=CARTESIAN_POINT('Ctrl Pts',(-9.86467426114011,-12.1151551560838,
9.33099783501169));
#57836=CARTESIAN_POINT('Ctrl Pts',(-9.96748330192147,-12.3929233341375,
9.34980412251047));
#57837=CARTESIAN_POINT('Ctrl Pts',(-10.0166359465243,-12.6905511117478,
9.36861041000925));
#57838=CARTESIAN_POINT('Ctrl Pts',(-10.014824715197,-12.9887562509003,9.38741669750802));
#57839=CARTESIAN_POINT('Origin',(-7.50000000000001,-12.9903810567666,7.5));
#57840=CARTESIAN_POINT('',(-10.0166114900998,-12.9925168768863,10.387416697508));
#57841=CARTESIAN_POINT('',(-10.0209920718673,-12.9913179799917,10.112583302492));
#57842=CARTESIAN_POINT('',(-10.0175,-12.9903810567666,7.5));
#57843=CARTESIAN_POINT('Ctrl Pts',(-10.0209920718673,-12.9913179799917,
10.112583302492));
#57844=CARTESIAN_POINT('Ctrl Pts',(-10.0172626706847,-12.2214467116455,
10.0637238147899));
#57845=CARTESIAN_POINT('Ctrl Pts',(-9.63824845828795,-11.4483937541634,
10.0148643270877));
#57846=CARTESIAN_POINT('Ctrl Pts',(-9.02557861358329,-10.9828167220247,
9.96600483938563));
#57847=CARTESIAN_POINT('Ctrl Pts',(-8.36934821243818,-10.4841373677117,
9.91367146360155));
#57848=CARTESIAN_POINT('Ctrl Pts',(-7.44505538997194,-10.3382110809426,
9.86133808781746));
#57849=CARTESIAN_POINT('Ctrl Pts',(-6.66711111680735,-10.6104648272364,
9.80900471203337));
#57850=CARTESIAN_POINT('Ctrl Pts',(-5.88916684364275,-10.8827185735301,
9.75667133624929));
#57851=CARTESIAN_POINT('Ctrl Pts',(-5.2575711197798,-11.5731523528866,9.70433796046521));
#57852=CARTESIAN_POINT('Ctrl Pts',(-5.05550299426883,-12.3722067586746,
9.65200458468113));
#57853=CARTESIAN_POINT('Ctrl Pts',(-4.85343486875787,-13.1712611644625,
9.59967120889704));
#57854=CARTESIAN_POINT('Ctrl Pts',(-5.08089434159889,-14.0789361966818,
9.54733783311295));
#57855=CARTESIAN_POINT('Ctrl Pts',(-5.63589882791342,-14.6882714568219,
9.49500445732887));
#57856=CARTESIAN_POINT('Ctrl Pts',(-6.19090331422795,-15.297606716962,9.44267108154478));
#57857=CARTESIAN_POINT('Ctrl Pts',(-7.07345281401599,-15.6086022050228,
9.3903377057607));
#57858=CARTESIAN_POINT('Ctrl Pts',(-7.88785204565785,-15.4818215734849,
9.33800432997662));
#57859=CARTESIAN_POINT('Ctrl Pts',(-8.70225127729972,-15.3550409419471,
9.28567095419253));
#57860=CARTESIAN_POINT('Ctrl Pts',(-9.44850024079541,-14.7904841908106,
9.23333757840844));
#57861=CARTESIAN_POINT('Ctrl Pts',(-9.79201462354332,-14.0412730621545,
9.18100420262436));
#57862=CARTESIAN_POINT('Ctrl Pts',(-9.94171872679729,-13.7147656848908,
9.15819723591356));
#57863=CARTESIAN_POINT('Ctrl Pts',(-10.0149342710371,-13.3531881946364,
9.13539026920277));
#57864=CARTESIAN_POINT('Ctrl Pts',(-10.0138589040853,-12.9911961164478,
9.11258330249198));
#57865=CARTESIAN_POINT('Ctrl Pts',(-10.014824715197,-12.9887562509003,9.38741669750802));
#57866=CARTESIAN_POINT('Ctrl Pts',(-10.0115957252851,-13.5203843049831,
9.42094378579333));
#57867=CARTESIAN_POINT('Ctrl Pts',(-9.84639173717802,-14.053847347733,9.45447087407864));
#57868=CARTESIAN_POINT('Ctrl Pts',(-9.53446863140466,-14.4798917831418,
9.48799796236395));
#57869=CARTESIAN_POINT('Ctrl Pts',(-9.04757907597225,-15.1449165341501,
9.54033133814803));
#57870=CARTESIAN_POINT('Ctrl Pts',(-8.20320887754036,-15.5482162050654,
9.59266471393211));
#57871=CARTESIAN_POINT('Ctrl Pts',(-7.37993546302102,-15.5089697162145,
9.6449980897162));
#57872=CARTESIAN_POINT('Ctrl Pts',(-6.55666204850167,-15.4697232273637,
9.69733146550028));
#57873=CARTESIAN_POINT('Ctrl Pts',(-5.75448541789485,-14.9879305787468,
9.74966484128437));
#57874=CARTESIAN_POINT('Ctrl Pts',(-5.3330653149527,-14.2796053021006,9.80199821706846));
#57875=CARTESIAN_POINT('Ctrl Pts',(-4.91164521201054,-13.5712800254544,
9.85433159285254));
#57876=CARTESIAN_POINT('Ctrl Pts',(-4.87098163673303,-12.636422120779,9.90666496863662));
#57877=CARTESIAN_POINT('Ctrl Pts',(-5.22930629119846,-11.8941806184447,
9.95899834442071));
#57878=CARTESIAN_POINT('Ctrl Pts',(-5.58763094566388,-11.1519391161105,
10.0113317202048));
#57879=CARTESIAN_POINT('Ctrl Pts',(-6.34494382987224,-10.6023140161175,
10.0636650959889));
#57880=CARTESIAN_POINT('Ctrl Pts',(-7.1617000931268,-10.4917304028291,10.115998471773));
#57881=CARTESIAN_POINT('Ctrl Pts',(-7.97845635638136,-10.3811467895407,
10.168331847557));
#57882=CARTESIAN_POINT('Ctrl Pts',(-8.85465599868212,-10.7096046629569,
10.2206652233411));
#57883=CARTESIAN_POINT('Ctrl Pts',(-9.39745068084417,-11.3298422064682,
10.2729985991252));
#57884=CARTESIAN_POINT('Ctrl Pts',(-9.79302701821837,-11.781857128182,10.3111379652528));
#57885=CARTESIAN_POINT('Ctrl Pts',(-10.0115266235871,-12.3888409214585,
10.3492773313804));
#57886=CARTESIAN_POINT('Ctrl Pts',(-10.0166114900998,-12.9925168768863,
10.387416697508));
#57887=CARTESIAN_POINT('Origin',(-7.50000000000001,-12.9903810567666,7.5));
#57888=CARTESIAN_POINT('',(-10.0205077525331,-12.989132710429,11.387416697508));
#57889=CARTESIAN_POINT('',(-10.0159021674261,-12.9883695445715,11.112583302492));
#57890=CARTESIAN_POINT('',(-10.0175,-12.9903810567666,7.5));
#57891=CARTESIAN_POINT('',(-5.5865340033349,-11.3543938533917,12.));
#57892=CARTESIAN_POINT('Ctrl Pts',(-10.0205077525331,-12.989132710429,11.387416697508));
#57893=CARTESIAN_POINT('Ctrl Pts',(-10.0157036585105,-13.732988657673,11.4346110043198));
#57894=CARTESIAN_POINT('Ctrl Pts',(-9.66521749773701,-14.4805837586295,
11.4818053111315));
#57895=CARTESIAN_POINT('Ctrl Pts',(-9.08783263489828,-14.9488474815931,
11.5289996179432));
#57896=CARTESIAN_POINT('Ctrl Pts',(-8.44757534455355,-15.468101244079,11.5813329937273));
#57897=CARTESIAN_POINT('Ctrl Pts',(-7.52831414497493,-15.6438777379762,
11.6336663695114));
#57898=CARTESIAN_POINT('Ctrl Pts',(-6.74219676859447,-15.395694540416,11.6859997452955));
#57899=CARTESIAN_POINT('Ctrl Pts',(-5.956079392214,-15.1475113428559,11.7383331210796));
#57900=CARTESIAN_POINT('Ctrl Pts',(-5.3031058390317,-14.4753684538384,11.7906664968637));
#57901=CARTESIAN_POINT('Ctrl Pts',(-5.07623304195856,-13.6843856961865,
11.8429998726477));
#57902=CARTESIAN_POINT('Ctrl Pts',(-4.84936024488542,-12.8934029385347,
11.8953332484318));
#57903=CARTESIAN_POINT('Ctrl Pts',(-5.04858820392145,-11.9835803122485,
11.9476666242159));
#57904=CARTESIAN_POINT('Ctrl Pts',(-5.5865340033349,-11.3543938533917,12.));
#57905=CARTESIAN_POINT('',(-9.41699369782473,-11.3520708274328,12.));
#57906=CARTESIAN_POINT('Origin',(-7.50000000000001,-12.9903810567666,12.));
#57907=CARTESIAN_POINT('Ctrl Pts',(-9.41700750114216,-11.3520617378123,
12.));
#57908=CARTESIAN_POINT('Ctrl Pts',(-8.90328443334769,-10.7549233049312,
11.9500021225376));
#57909=CARTESIAN_POINT('Ctrl Pts',(-8.08591177198773,-10.4146528382252,
11.9000042450751));
#57910=CARTESIAN_POINT('Ctrl Pts',(-7.30082070365003,-10.4769905890799,
11.8500063676127));
#57911=CARTESIAN_POINT('Ctrl Pts',(-6.47905650106146,-10.5422402577977,
11.7976729918286));
#57912=CARTESIAN_POINT('Ctrl Pts',(-5.69266020241076,-11.048589867075,11.7453396160445));
#57913=CARTESIAN_POINT('Ctrl Pts',(-5.29374176559417,-11.769698237016,11.6930062402604));
#57914=CARTESIAN_POINT('Ctrl Pts',(-4.89482332877758,-12.4908066069571,
11.6406728644763));
#57915=CARTESIAN_POINT('Ctrl Pts',(-4.88338275379511,-13.4266737375619,
11.5883394886922));
#57916=CARTESIAN_POINT('Ctrl Pts',(-5.2647914049726,-14.1573521857831,11.5360061129082));
#57917=CARTESIAN_POINT('Ctrl Pts',(-5.64620005615009,-14.8880306340043,
11.4836727371241));
#57918=CARTESIAN_POINT('Ctrl Pts',(-6.42045793348755,-15.413520399842,11.43133936134));
#57919=CARTESIAN_POINT('Ctrl Pts',(-7.24029923554721,-15.4983927042523,
11.3790059855559));
#57920=CARTESIAN_POINT('Ctrl Pts',(-8.06014053760687,-15.5832650086627,
11.3266726097718));
#57921=CARTESIAN_POINT('Ctrl Pts',(-8.92556526438873,-15.2275198516459,
11.2743392339877));
#57922=CARTESIAN_POINT('Ctrl Pts',(-9.44861922536103,-14.5905668140585,
11.2220058582037));
#57923=CARTESIAN_POINT('Ctrl Pts',(-9.81316607095874,-14.146637051602,11.1855316729664));
#57924=CARTESIAN_POINT('Ctrl Pts',(-10.0114059764305,-13.566110281377,11.1490574877292));
#57925=CARTESIAN_POINT('Ctrl Pts',(-10.0159021674261,-12.9883695445715,
11.112583302492));
#57926=CARTESIAN_POINT('Origin',(-7.50000000000001,-12.9903810567666,14.2084234471775));
#57927=CARTESIAN_POINT('',(-10.5774091090731,-12.9889059662574,4.79157655282255));
#57928=CARTESIAN_POINT('',(-10.5686793840393,-12.990485538642,4.70842344717746));
#57929=CARTESIAN_POINT('',(-10.5735,-12.9903810567665,14.2084234471775));
#57930=CARTESIAN_POINT('',(-6.7062007174672,-15.9596040105123,4.));
#57931=CARTESIAN_POINT('Ctrl Pts',(-10.5686793840393,-12.990485538642,4.70842344717746));
#57932=CARTESIAN_POINT('Ctrl Pts',(-10.568341802375,-12.4708360960575,4.68161580125464));
#57933=CARTESIAN_POINT('Ctrl Pts',(-10.1982941291361,-10.9363980734526,
4.60247477954775));
#57934=CARTESIAN_POINT('Ctrl Pts',(-7.78634786537746,-9.38338007605921,
4.47100038205676));
#57935=CARTESIAN_POINT('Ctrl Pts',(-4.64704854581202,-10.7599538374027,
4.31400025470451));
#57936=CARTESIAN_POINT('Ctrl Pts',(-4.0706083548489,-14.143375884847,4.15700012735225));
#57937=CARTESIAN_POINT('Ctrl Pts',(-5.72985994157699,-15.6985866940351,
4.05233337578409));
#57938=CARTESIAN_POINT('Ctrl Pts',(-6.7062007174672,-15.9596040105123,4.));
#57939=CARTESIAN_POINT('',(-8.29574206058843,-15.9643807808206,4.));
#57940=CARTESIAN_POINT('Origin',(-7.50000000000001,-12.9903810567666,4.));
#57941=CARTESIAN_POINT('Ctrl Pts',(-10.5774091090731,-12.9889059662574,
4.79157655282255));
#57942=CARTESIAN_POINT('Ctrl Pts',(-10.5779245754331,-12.90178610915,4.78704908248048));
#57943=CARTESIAN_POINT('Ctrl Pts',(-10.5353931215559,-11.8081560623987,
4.73018823635433));
#57944=CARTESIAN_POINT('Ctrl Pts',(-9.23195310627391,-9.81262424147309,
4.62099401444409));
#57945=CARTESIAN_POINT('Ctrl Pts',(-5.80479621412607,-9.79242646017958,
4.46399388709183));
#57946=CARTESIAN_POINT('Ctrl Pts',(-3.89775220169895,-12.6409121056472,
4.30699375973959));
#57947=CARTESIAN_POINT('Ctrl Pts',(-5.20118245874298,-15.7537141165304,
4.15232913070897));
#57948=CARTESIAN_POINT('Ctrl Pts',(-7.3659421433414,-16.2099240527811,4.04999787746244));
#57949=CARTESIAN_POINT('Ctrl Pts',(-8.2957496623611,-15.9643994715412,4.));
#57950=CARTESIAN_POINT('Origin',(-7.50000000000001,-12.9903810567666,14.2084234471775));
#57951=CARTESIAN_POINT('',(-10.5688838367077,-12.9896889619566,5.79157655282255));
#57952=CARTESIAN_POINT('',(-10.576720384476,-12.9922616072697,5.70842344717746));
#57953=CARTESIAN_POINT('',(-10.5735,-12.9903810567665,14.2084234471775));
#57954=CARTESIAN_POINT('Ctrl Pts',(-10.576720384476,-12.9922616072697,5.70842344717746));
#57955=CARTESIAN_POINT('Ctrl Pts',(-10.5702730665099,-12.1038642909273,
5.66228272262582));
#57956=CARTESIAN_POINT('Ctrl Pts',(-9.70223177580237,-10.196831424253,5.56380862229009));
#57957=CARTESIAN_POINT('Ctrl Pts',(-6.48106313838945,-9.51757559757857,
5.41300114617028));
#57958=CARTESIAN_POINT('Ctrl Pts',(-4.04127232265978,-11.9244666993329,
5.25600101881803));
#57959=CARTESIAN_POINT('Ctrl Pts',(-4.70303574023142,-15.2872880321773,
5.09900089146577));
#57960=CARTESIAN_POINT('Ctrl Pts',(-7.87270740462966,-16.5902265862243,
4.94200076411352));
#57961=CARTESIAN_POINT('Ctrl Pts',(-10.2242698683325,-14.9942184798723,
4.81180828268408));
#57962=CARTESIAN_POINT('Ctrl Pts',(-10.5690008228703,-13.4852858404724,
4.73394917703873));
#57963=CARTESIAN_POINT('Ctrl Pts',(-10.5686793840393,-12.990485538642,4.70842344717746));
#57964=CARTESIAN_POINT('Ctrl Pts',(-10.5688838367077,-12.9896889619566,
5.79157655282255));
#57965=CARTESIAN_POINT('Ctrl Pts',(-10.5698355434391,-12.5272691260468,
5.76771600385165));
#57966=CARTESIAN_POINT('Ctrl Pts',(-10.2562654399242,-11.0518487505808,
5.69152207909667));
#57967=CARTESIAN_POINT('Ctrl Pts',(-7.98558650367391,-9.40388769480238,
5.56299477855761));
#57968=CARTESIAN_POINT('Ctrl Pts',(-4.77645084555843,-10.6068850809164,
5.40599465120535));
#57969=CARTESIAN_POINT('Ctrl Pts',(-4.00954797596254,-13.9472048059447,
5.24899452385311));
#57970=CARTESIAN_POINT('Ctrl Pts',(-6.37256666156175,-16.4294950347898,
5.09199439650084));
#57971=CARTESIAN_POINT('Ctrl Pts',(-9.64926888537511,-15.8453165147797,
4.93952173949067));
#57972=CARTESIAN_POINT('Ctrl Pts',(-10.5719662603729,-13.908811197287,4.83938245826456));
#57973=CARTESIAN_POINT('Ctrl Pts',(-10.5774091090731,-12.9889059662574,
4.79157655282255));
#57974=CARTESIAN_POINT('Origin',(-7.50000000000001,-12.9903810567666,14.2084234471775));
#57975=CARTESIAN_POINT('',(-10.5752289107932,-12.9928016758089,6.79157655282255));
#57976=CARTESIAN_POINT('',(-10.5729908526269,-12.9877359220758,6.70842344717746));
#57977=CARTESIAN_POINT('',(-10.5735,-12.9903810567665,14.2084234471775));
#57978=CARTESIAN_POINT('Ctrl Pts',(-10.5729908526269,-12.9877359220758,
6.70842344717746));
#57979=CARTESIAN_POINT('Ctrl Pts',(-10.5751989125043,-12.733933626166,6.69528301978108));
#57980=CARTESIAN_POINT('Ctrl Pts',(-10.4312908590873,-11.4718008748884,
6.62980921660061));
#57981=CARTESIAN_POINT('Ctrl Pts',(-8.69550592617927,-9.57431407095109,
6.51200203763606));
#57982=CARTESIAN_POINT('Ctrl Pts',(-5.31022618670948,-10.1087781397346,
6.3550019102838));
#57983=CARTESIAN_POINT('Ctrl Pts',(-3.88853690576949,-13.2272021460562,
6.19800178293155));
#57984=CARTESIAN_POINT('Ctrl Pts',(-5.70528265200966,-16.133268450666,6.0410016555793));
#57985=CARTESIAN_POINT('Ctrl Pts',(-9.13136587582039,-16.22107348372,5.88400152822704));
#57986=CARTESIAN_POINT('Ctrl Pts',(-10.5176208014685,-14.2374825953214,
5.77314212542643));
#57987=CARTESIAN_POINT('Ctrl Pts',(-10.5775856936348,-13.1114954248875,
5.7146160984099));
#57988=CARTESIAN_POINT('Ctrl Pts',(-10.576720384476,-12.9922616072697,5.70842344717746));
#57989=CARTESIAN_POINT('Ctrl Pts',(-10.5752289107932,-12.9928016758089,
6.79157655282255));
#57990=CARTESIAN_POINT('Ctrl Pts',(-10.5680432727522,-12.1600961914245,
6.74838292522283));
#57991=CARTESIAN_POINT('Ctrl Pts',(-9.79183080592196,-10.3066734191141,
6.65285592183901));
#57992=CARTESIAN_POINT('Ctrl Pts',(-6.67544463886838,-9.46634131342536,
6.50499554267114));
#57993=CARTESIAN_POINT('Ctrl Pts',(-4.10581084513197,-11.7341055256468,
6.34799541531887));
#57994=CARTESIAN_POINT('Ctrl Pts',(-4.57977903131249,-15.1283843904584,
6.19099528796663));
#57995=CARTESIAN_POINT('Ctrl Pts',(-7.67233737080682,-16.6054945057935,
6.03399516061437));
#57996=CARTESIAN_POINT('Ctrl Pts',(-10.1638447789511,-15.1090784945035,
5.90085558223301));
#57997=CARTESIAN_POINT('Ctrl Pts',(-10.56774816372,-13.5414952057652,5.82004937963574));
#57998=CARTESIAN_POINT('Ctrl Pts',(-10.5688838367077,-12.9896889619566,
5.79157655282255));
#57999=CARTESIAN_POINT('Origin',(-7.50000000000001,-12.9903810567666,14.2084234471775));
#58000=CARTESIAN_POINT('',(-10.574646672787,-12.9878426425384,7.79157655282256));
#58001=CARTESIAN_POINT('',(-10.5698474628756,-12.992136489652,7.70842344717746));
#58002=CARTESIAN_POINT('',(-10.5735,-12.9903810567665,14.2084234471775));
#58003=CARTESIAN_POINT('Ctrl Pts',(-10.5698474628756,-12.9921364896521,
7.70842344717746));
#58004=CARTESIAN_POINT('Ctrl Pts',(-10.5664962921154,-12.3632928855735,
7.67594994115225));
#58005=CARTESIAN_POINT('Ctrl Pts',(-10.0746937830591,-10.7162100151804,
7.59114305934296));
#58006=CARTESIAN_POINT('Ctrl Pts',(-7.39948645351245,-9.37255790644949,
7.45400280174957));
#58007=CARTESIAN_POINT('Ctrl Pts',(-4.42700232783115,-11.078462500715,7.29700267439732));
#58008=CARTESIAN_POINT('Ctrl Pts',(-4.21010468283033,-14.4988027877182,
7.14000254704507));
#58009=CARTESIAN_POINT('Ctrl Pts',(-6.94328775591919,-16.5665268737914,
6.98300241969282));
#58010=CARTESIAN_POINT('Ctrl Pts',(-9.90513870920436,-15.5228207892163,
6.83914271973694));
#58011=CARTESIAN_POINT('Ctrl Pts',(-10.566405041207,-13.7447326303419,6.74761639556516));
#58012=CARTESIAN_POINT('Ctrl Pts',(-10.5729908526269,-12.9877359220758,
6.70842344717746));
#58013=CARTESIAN_POINT('Ctrl Pts',(-10.574646672787,-12.9878426425384,7.79157655282256));
#58014=CARTESIAN_POINT('Ctrl Pts',(-10.5763836278447,-12.7912348191717,
7.78138322237809));
#58015=CARTESIAN_POINT('Ctrl Pts',(-10.4703648087191,-11.5870913412493,
7.71885651614955));
#58016=CARTESIAN_POINT('Ctrl Pts',(-8.88333183851511,-9.64596167231467,
7.60399643413689));
#58017=CARTESIAN_POINT('Ctrl Pts',(-5.47359881574229,-9.99164028328652,
7.44699630678467));
#58018=CARTESIAN_POINT('Ctrl Pts',(-3.88095917534459,-13.0263185113509,
7.28999617943238));
#58019=CARTESIAN_POINT('Ctrl Pts',(-5.53354816193247,-16.0287712850697,
7.13299605208016));
#58020=CARTESIAN_POINT('Ctrl Pts',(-8.94947337693327,-16.3066703804957,
6.97599592472788));
#58021=CARTESIAN_POINT('Ctrl Pts',(-10.4834449578808,-14.3524988668243,
6.86218942497536));
#58022=CARTESIAN_POINT('Ctrl Pts',(-10.5767493879072,-13.1690017048858,
6.80071630100692));
#58023=CARTESIAN_POINT('Ctrl Pts',(-10.5752289107932,-12.9928016758089,
6.79157655282255));
#58024=CARTESIAN_POINT('Origin',(-7.50000000000001,-12.9903810567666,14.2084234471775));
#58025=CARTESIAN_POINT('',(-10.5690547534087,-12.9913761256565,8.79157655282255));
#58026=CARTESIAN_POINT('',(-10.5783068629449,-12.9905613575631,8.70842344717746));
#58027=CARTESIAN_POINT('',(-10.5735,-12.9903810567665,14.2084234471775));
#58028=CARTESIAN_POINT('Ctrl Pts',(-10.5783068629449,-12.9905613575631,
8.70842344717747));
#58029=CARTESIAN_POINT('Ctrl Pts',(-10.5774424348904,-11.99443969475,8.65661686252343));
#58030=CARTESIAN_POINT('Ctrl Pts',(-9.51496026706992,-9.99048048802178,
8.55247690208529));
#58031=CARTESIAN_POINT('Ctrl Pts',(-6.11666819796815,-9.64596176051859,
8.3960035658631));
#58032=CARTESIAN_POINT('Ctrl Pts',(-3.94738216319582,-12.2992560282264,
8.23900343851084));
#58033=CARTESIAN_POINT('Ctrl Pts',(-4.96376262473273,-15.5722887382593,
8.0820033111586));
#58034=CARTESIAN_POINT('Ctrl Pts',(-8.25441147268027,-16.5301000616477,
7.92500318380633));
#58035=CARTESIAN_POINT('Ctrl Pts',(-10.3278659516785,-14.7722228904523,
7.80047656247929));
#58036=CARTESIAN_POINT('Ctrl Pts',(-10.5718969432977,-13.3767192958943,
7.72828331693634));
#58037=CARTESIAN_POINT('Ctrl Pts',(-10.5698474628756,-12.9921364896521,
7.70842344717746));
#58038=CARTESIAN_POINT('Ctrl Pts',(-10.5690547534086,-12.9913761256565,
8.79157655282255));
#58039=CARTESIAN_POINT('Ctrl Pts',(-10.5673550876409,-12.4192313871019,
8.76205014374926));
#58040=CARTESIAN_POINT('Ctrl Pts',(-10.1411933372985,-10.8306504836598,
8.6801903588919));
#58041=CARTESIAN_POINT('Ctrl Pts',(-7.60051354913579,-9.37255781103892,
8.54599719825042));
#58042=CARTESIAN_POINT('Ctrl Pts',(-4.53789787464541,-10.9107899935683,
8.38899707089818));
#58043=CARTESIAN_POINT('Ctrl Pts',(-4.13142759646044,-14.3138114282651,
8.23199694354591));
#58044=CARTESIAN_POINT('Ctrl Pts',(-6.74558850742372,-16.5301001550025,
8.07499681619368));
#58045=CARTESIAN_POINT('Ctrl Pts',(-9.82259002330375,-15.634475301008,7.92819001928586));
#58046=CARTESIAN_POINT('Ctrl Pts',(-10.5674659613129,-13.8006351479846,
7.83371659816217));
#58047=CARTESIAN_POINT('Ctrl Pts',(-10.574646672787,-12.9878426425384,7.79157655282256));
#58048=CARTESIAN_POINT('Origin',(-7.50000000000001,-12.9903810567666,14.2084234471775));
#58049=CARTESIAN_POINT('',(-10.5777633099838,-12.991524903254,9.79157655282255));
#58050=CARTESIAN_POINT('',(-10.5702338677887,-12.98839740599,9.70842344717746));
#58051=CARTESIAN_POINT('',(-10.5735,-12.9903810567665,14.2084234471775));
#58052=CARTESIAN_POINT('Ctrl Pts',(-10.5702338677887,-12.98839740599,9.70842344717746));
#58053=CARTESIAN_POINT('Ctrl Pts',(-10.5724451168391,-12.6243324625202,
9.68961715967868));
#58054=CARTESIAN_POINT('Ctrl Pts',(-10.3454485117827,-11.2498286970771,
9.61847749639582));
#58055=CARTESIAN_POINT('Ctrl Pts',(-8.32455533939524,-9.46634140643289,
9.49500445732887));
#58056=CARTESIAN_POINT('Ctrl Pts',(-5.01553493137219,-10.3586172470561,
9.33800432997662));
#58057=CARTESIAN_POINT('Ctrl Pts',(-3.93435818466818,-13.6108210305748,
9.18100420262436));
#58058=CARTESIAN_POINT('Ctrl Pts',(-6.05052666129351,-16.3066702930228,
9.02400407527212));
#58059=CARTESIAN_POINT('Ctrl Pts',(-9.46645178620579,-16.0287712049414,
8.86700394791984));
#58060=CARTESIAN_POINT('Ctrl Pts',(-10.5737227704402,-14.0170617812033,
8.76181040522164));
#58061=CARTESIAN_POINT('Ctrl Pts',(-10.5783156528128,-13.0006903413578,
8.70895023830751));
#58062=CARTESIAN_POINT('Ctrl Pts',(-10.5783068629449,-12.9905613575631,
8.70842344717747));
#58063=CARTESIAN_POINT('Ctrl Pts',(-10.5777633099838,-12.991524903254,9.79157655282255));
#58064=CARTESIAN_POINT('Ctrl Pts',(-10.5732102555509,-12.0516244689892,
9.74271706512043));
#58065=CARTESIAN_POINT('Ctrl Pts',(-9.61486894310576,-10.0969521595311,
9.64152420163424));
#58066=CARTESIAN_POINT('Ctrl Pts',(-6.30449404219616,-9.57431398106461,
9.48799796236394));
#58067=CARTESIAN_POINT('Ctrl Pts',(-3.99123550321764,-12.1030705501041,
9.33099783501171));
#58068=CARTESIAN_POINT('Ctrl Pts',(-4.82431993989319,-15.4274866909495,
9.17399770765942));
#58069=CARTESIAN_POINT('Ctrl Pts',(-8.05671225877921,-16.5665269680756,
9.0169975803072));
#58070=CARTESIAN_POINT('Ctrl Pts',(-10.2758761800147,-14.8876717402662,
8.88952386202821));
#58071=CARTESIAN_POINT('Ctrl Pts',(-10.5703676194767,-13.4333156101897,
8.81438351953334));
#58072=CARTESIAN_POINT('Ctrl Pts',(-10.5690547534086,-12.9913761256565,
8.79157655282255));
#58073=CARTESIAN_POINT('Origin',(-7.50000000000001,-12.9903810567666,14.2084234471775));
#58074=CARTESIAN_POINT('',(-10.5715492796759,-12.9879252940133,10.7915765528226));
#58075=CARTESIAN_POINT('',(-10.5724152591149,-12.9929885813497,10.7084234471775));
#58076=CARTESIAN_POINT('',(-10.5735,-12.9903810567665,14.2084234471775));
#58077=CARTESIAN_POINT('Ctrl Pts',(-10.5724152591149,-12.9929885813497,
10.7084234471775));
#58078=CARTESIAN_POINT('Ctrl Pts',(-10.5662073793823,-12.2559883632733,
10.6702840810499));
#58079=CARTESIAN_POINT('Ctrl Pts',(-9.93341873530542,-10.4981249983676,
10.5798113391382));
#58080=CARTESIAN_POINT('Ctrl Pts',(-7.01441350972263,-9.40388779191504,
10.4370052214424));
#58081=CARTESIAN_POINT('Ctrl Pts',(-4.2407080682755,-11.4169238334189,10.2800050940901));
#58082=CARTESIAN_POINT('Ctrl Pts',(-4.38964093653616,-14.8408989317544,
10.1230049667379));
#58083=CARTESIAN_POINT('Ctrl Pts',(-7.32766263366035,-16.6054944100355,
9.96600483938563));
#58084=CARTESIAN_POINT('Ctrl Pts',(-10.049778264125,-15.305320221038,9.82781099953216));
#58085=CARTESIAN_POINT('Ctrl Pts',(-10.5662917424682,-13.6374376539438,
9.74195053546276));
#58086=CARTESIAN_POINT('Ctrl Pts',(-10.5702338677887,-12.98839740599,9.70842344717746));
#58087=CARTESIAN_POINT('Ctrl Pts',(-10.5715492796759,-12.9879252940133,
10.7915765528226));
#58088=CARTESIAN_POINT('Ctrl Pts',(-10.5739360130587,-12.6812405681054,
10.7757173622757));
#58089=CARTESIAN_POINT('Ctrl Pts',(-10.3919168575192,-11.3652990254922,
10.7075247959448));
#58090=CARTESIAN_POINT('Ctrl Pts',(-8.51893689306524,-9.51757549146244,
10.5869988538297));
#58091=CARTESIAN_POINT('Ctrl Pts',(-5.16549637569413,-10.2247238388162,
10.4299987264775));
#58092=CARTESIAN_POINT('Ctrl Pts',(-3.90540678666615,-13.4118934459175,
10.2729985991252));
#58093=CARTESIAN_POINT('Ctrl Pts',(-5.86863408021139,-16.2210735713392,
10.115998471773));
#58094=CARTESIAN_POINT('Ctrl Pts',(-9.29471739586239,-16.133268532241,9.9589983444207));
#58095=CARTESIAN_POINT('Ctrl Pts',(-10.5460797704268,-14.1315894099677,
9.85085770477056));
#58096=CARTESIAN_POINT('Ctrl Pts',(-10.5780870301511,-13.0583514106611,
9.79505044090451));
#58097=CARTESIAN_POINT('Ctrl Pts',(-10.5777633099838,-12.991524903254,9.79157655282255));
#58098=CARTESIAN_POINT('Origin',(-7.50000000000001,-12.9903810567666,14.2084234471775));
#58099=CARTESIAN_POINT('',(-10.5702205181091,-12.9936861301783,11.7915765528225));
#58100=CARTESIAN_POINT('',(-10.5771720267767,-12.9888570081198,11.7084234471775));
#58101=CARTESIAN_POINT('',(-10.5735,-12.9903810567665,14.2084234471775));
#58102=CARTESIAN_POINT('',(-8.29379928253297,-15.9596040105122,12.));
#58103=CARTESIAN_POINT('Ctrl Pts',(-8.29379928253297,-15.9596040105122,
12.));
#58104=CARTESIAN_POINT('Ctrl Pts',(-9.27014005842316,-15.698586694035,11.9476666242159));
#58105=CARTESIAN_POINT('Ctrl Pts',(-10.3714986866323,-14.6662860075735,
11.8781921418234));
#58106=CARTESIAN_POINT('Ctrl Pts',(-10.5724951032558,-13.3253966136884,
11.8087176594309));
#58107=CARTESIAN_POINT('Ctrl Pts',(-10.5702205181091,-12.9936861301783,
11.7915765528225));
#58108=CARTESIAN_POINT('',(-6.70425809489808,-15.964380864449,12.));
#58109=CARTESIAN_POINT('Origin',(-7.50000000000001,-12.9903810567666,12.));
#58110=CARTESIAN_POINT('Ctrl Pts',(-6.70425049788239,-15.9643995452956,
12.));
#58111=CARTESIAN_POINT('Ctrl Pts',(-7.63405808481853,-16.2099241868245,
11.9500021225376));
#58112=CARTESIAN_POINT('Ctrl Pts',(-9.69010316575102,-15.7766245762052,
11.8528099382634));
#58113=CARTESIAN_POINT('Ctrl Pts',(-10.571306929268,-13.8969965329875,11.7556177539892));
#58114=CARTESIAN_POINT('Ctrl Pts',(-10.5771720267767,-12.9888570081198,
11.7084234471775));
#58115=CARTESIAN_POINT('Origin',(-7.50000000000001,-12.9903810567666,4.));
#58116=CARTESIAN_POINT('Ctrl Pts',(-9.41346599666503,-11.3543938533916,
4.));
#58117=CARTESIAN_POINT('Ctrl Pts',(-9.47563125999352,-11.4128139360928,
4.));
#58118=CARTESIAN_POINT('Ctrl Pts',(-9.5344254182292,-11.4744857433087,4.));
#58119=CARTESIAN_POINT('Ctrl Pts',(-9.58983450470078,-11.5390333604437,
4.));
#58120=CARTESIAN_POINT('Ctrl Pts',(-9.64659408185619,-11.6051542024983,
4.));
#58121=CARTESIAN_POINT('Ctrl Pts',(-9.69980203857783,-11.6742932390243,
4.));
#58122=CARTESIAN_POINT('Ctrl Pts',(-9.74941453503823,-11.7460926626337,
4.));
#58123=CARTESIAN_POINT('Ctrl Pts',(-9.76241984954432,-11.7649140111248,
4.));
#58124=CARTESIAN_POINT('Ctrl Pts',(-9.77517792533989,-11.7839183899685,
4.));
#58125=CARTESIAN_POINT('Ctrl Pts',(-9.78768759195629,-11.8030997933617,
4.));
#58126=CARTESIAN_POINT('Ctrl Pts',(-9.79776752365911,-11.8185556198114,
4.));
#58127=CARTESIAN_POINT('Ctrl Pts',(-9.8076865335191,-11.8341271625133,4.));
#58128=CARTESIAN_POINT('Ctrl Pts',(-9.81743537915168,-11.8497970439193,
4.));
#58129=CARTESIAN_POINT('Ctrl Pts',(-9.86491247379083,-11.9261097142127,
4.));
#58130=CARTESIAN_POINT('Ctrl Pts',(-9.90840731623012,-12.0048277686438,
4.));
#58131=CARTESIAN_POINT('Ctrl Pts',(-9.94788306281372,-12.0855595944701,
4.));
#58132=CARTESIAN_POINT('Ctrl Pts',(-9.97942487229752,-12.150065730259,4.));
#58133=CARTESIAN_POINT('Ctrl Pts',(-10.0084002601673,-12.2158586031585,
4.));
#58134=CARTESIAN_POINT('Ctrl Pts',(-10.034773868227,-12.2827556582142,4.));
#58135=CARTESIAN_POINT('Ctrl Pts',(-10.0434527794708,-12.3047698476261,
4.));
#58136=CARTESIAN_POINT('Ctrl Pts',(-10.0518498142904,-12.326903713834,4.));
#58137=CARTESIAN_POINT('Ctrl Pts',(-10.0599633247681,-12.3491510331904,
4.));
#58138=CARTESIAN_POINT('Ctrl Pts',(-10.0673313519173,-12.369354230495,4.));
#58139=CARTESIAN_POINT('Ctrl Pts',(-10.0744669979504,-12.3896556179549,
4.));
#58140=CARTESIAN_POINT('Ctrl Pts',(-10.0813595780794,-12.4100219884372,
4.));
#58141=CARTESIAN_POINT('Ctrl Pts',(-10.110937259752,-12.4974188719965,4.));
#58142=CARTESIAN_POINT('Ctrl Pts',(-10.1360761396945,-12.5860974112731,
4.));
#58143=CARTESIAN_POINT('Ctrl Pts',(-10.1567415216565,-12.6756607739627,
4.));
#58144=CARTESIAN_POINT('Ctrl Pts',(-10.1777235800004,-12.7665966059193,
4.));
#58145=CARTESIAN_POINT('Ctrl Pts',(-10.194094489083,-12.8584453915162,4.));
#58146=CARTESIAN_POINT('Ctrl Pts',(-10.205776157801,-12.9508249271276,4.));
#58147=CARTESIAN_POINT('Ctrl Pts',(-10.2173669041142,-13.0424854413619,
4.));
#58148=CARTESIAN_POINT('Ctrl Pts',(-10.2243414700862,-13.1346694027891,
4.00000000000001));
#58149=CARTESIAN_POINT('Ctrl Pts',(-10.2265766240073,-13.2270226781325,
4.00000000000001));
#58150=CARTESIAN_POINT('Ctrl Pts',(-10.2276561070688,-13.2716253318781,
4.00000000000001));
#58151=CARTESIAN_POINT('Ctrl Pts',(-10.2276293996605,-13.3162676791034,
4.00000000000001));
#58152=CARTESIAN_POINT('Ctrl Pts',(-10.2264782755414,-13.360910468216,4.00000000000001));
#58153=CARTESIAN_POINT('Ctrl Pts',(-10.2261080116976,-13.3752700063553,
4.00000000000001));
#58154=CARTESIAN_POINT('Ctrl Pts',(-10.2256213911499,-13.3896295910271,
4.00000000000001));
#58155=CARTESIAN_POINT('Ctrl Pts',(-10.2250177409671,-13.40398791621,4.00000000000001));
#58156=CARTESIAN_POINT('Ctrl Pts',(-10.2243866916487,-13.4189979527825,
4.00000000000001));
#58157=CARTESIAN_POINT('Ctrl Pts',(-10.2236280724728,-13.4339981404011,
4.));
#58158=CARTESIAN_POINT('Ctrl Pts',(-10.2227419311859,-13.4489814918393,
4.));
#58159=CARTESIAN_POINT('Ctrl Pts',(-10.2170924746832,-13.5445055278686,
4.));
#58160=CARTESIAN_POINT('Ctrl Pts',(-10.2062608557766,-13.6394136430286,
4.));
#58161=CARTESIAN_POINT('Ctrl Pts',(-10.1901745261949,-13.7333115332678,
4.));
#58162=CARTESIAN_POINT('Ctrl Pts',(-10.1886860667379,-13.74199985474,4.));
#58163=CARTESIAN_POINT('Ctrl Pts',(-10.1871525835688,-13.7506795401449,
4.));
#58164=CARTESIAN_POINT('Ctrl Pts',(-10.1855739978038,-13.7593502843482,
4.));
#58165=CARTESIAN_POINT('Ctrl Pts',(-10.1691852106353,-13.8493694549782,
4.));
#58166=CARTESIAN_POINT('Ctrl Pts',(-10.1479394797701,-13.9384246529327,
4.));
#58167=CARTESIAN_POINT('Ctrl Pts',(-10.1221390901744,-14.0262810420052,
4.));
#58168=CARTESIAN_POINT('Ctrl Pts',(-10.0957476132678,-14.1161502222633,
4.));
#58169=CARTESIAN_POINT('Ctrl Pts',(-10.0645901923201,-14.2047657338476,
4.));
#58170=CARTESIAN_POINT('Ctrl Pts',(-10.0289360631668,-14.2918733204662,
4.));
#58171=CARTESIAN_POINT('Ctrl Pts',(-10.0090443370482,-14.3404713453517,
4.));
#58172=CARTESIAN_POINT('Ctrl Pts',(-9.98775201258348,-14.3885999003503,
4.));
#58173=CARTESIAN_POINT('Ctrl Pts',(-9.96509914777034,-14.4362131753606,
4.));
#58174=CARTESIAN_POINT('Ctrl Pts',(-9.95876399288502,-14.4495288188465,
4.));
#58175=CARTESIAN_POINT('Ctrl Pts',(-9.95232213153922,-14.4628045348086,
4.));
#58176=CARTESIAN_POINT('Ctrl Pts',(-9.94578145907892,-14.4760254702856,
4.));
#58177=CARTESIAN_POINT('Ctrl Pts',(-9.90302407067229,-14.562452772175,4.));
#58178=CARTESIAN_POINT('Ctrl Pts',(-9.85598091444247,-14.6466834011242,
4.));
#58179=CARTESIAN_POINT('Ctrl Pts',(-9.80499202080536,-14.7284640330205,
4.));
#58180=CARTESIAN_POINT('Ctrl Pts',(-9.75299794500559,-14.8118568676255,
4.));
#58181=CARTESIAN_POINT('Ctrl Pts',(-9.69690071688324,-14.8927029338428,
4.));
#58182=CARTESIAN_POINT('Ctrl Pts',(-9.63700597453379,-14.9707266774082,
4.));
#58183=CARTESIAN_POINT('Ctrl Pts',(-9.57663995749172,-15.049364341567,4.));
#58184=CARTESIAN_POINT('Ctrl Pts',(-9.51241597456512,-15.1251359367173,
4.));
#58185=CARTESIAN_POINT('Ctrl Pts',(-9.44459769690279,-15.1977400638646,
4.));
#58186=CARTESIAN_POINT('Ctrl Pts',(-9.40866340733751,-15.2362101904805,
4.));
#58187=CARTESIAN_POINT('Ctrl Pts',(-9.37171922385876,-15.2737906405076,
4.));
#58188=CARTESIAN_POINT('Ctrl Pts',(-9.33379951949355,-15.3104331478965,
4.));
#58189=CARTESIAN_POINT('Ctrl Pts',(-9.31851290781191,-15.3252048817713,
4.));
#58190=CARTESIAN_POINT('Ctrl Pts',(-9.30306772443973,-15.339824154646,4.));
#58191=CARTESIAN_POINT('Ctrl Pts',(-9.28746608368795,-15.3542876681649,
4.));
#58192=CARTESIAN_POINT('Ctrl Pts',(-9.27676581806402,-15.3642073579572,
4.));
#58193=CARTESIAN_POINT('Ctrl Pts',(-9.26599878272636,-15.3740474389504,
4.));
#58194=CARTESIAN_POINT('Ctrl Pts',(-9.25516737653956,-15.3838058321128,
4.));
#58195=CARTESIAN_POINT('Ctrl Pts',(-9.17938057199806,-15.452084818468,4.));
#58196=CARTESIAN_POINT('Ctrl Pts',(-9.10042438929677,-15.5163865482147,
4.));
#58197=CARTESIAN_POINT('Ctrl Pts',(-9.01862162231471,-15.5764248312756,
4.));
#58198=CARTESIAN_POINT('Ctrl Pts',(-8.93674927983158,-15.636514178546,4.));
#58199=CARTESIAN_POINT('Ctrl Pts',(-8.8520249381574,-15.6923336670045,4.));
#58200=CARTESIAN_POINT('Ctrl Pts',(-8.76472731465809,-15.7435701437727,
4.));
#58201=CARTESIAN_POINT('Ctrl Pts',(-8.67912044767158,-15.7938142864623,
4.));
#58202=CARTESIAN_POINT('Ctrl Pts',(-8.59103835537406,-15.8396519102272,
4.));
#58203=CARTESIAN_POINT('Ctrl Pts',(-8.50070999295064,-15.8807513482254,
4.));
#58204=CARTESIAN_POINT('Ctrl Pts',(-8.47449902628609,-15.8926773476613,
4.));
#58205=CARTESIAN_POINT('Ctrl Pts',(-8.44809873411205,-15.9042041128398,
4.));
#58206=CARTESIAN_POINT('Ctrl Pts',(-8.42151428132428,-15.9153228238725,
4.));
#58207=CARTESIAN_POINT('Ctrl Pts',(-8.38003054177093,-15.9326730291346,
4.));
#58208=CARTESIAN_POINT('Ctrl Pts',(-8.3380984052677,-15.9490297174903,4.));
#58209=CARTESIAN_POINT('Ctrl Pts',(-8.29574966236114,-15.9643994715412,
4.));
#58210=CARTESIAN_POINT('Ctrl Pts',(-6.7062007174672,-15.9596040105123,4.));
#58211=CARTESIAN_POINT('Ctrl Pts',(-6.61134542475377,-15.9249055207219,
4.));
#58212=CARTESIAN_POINT('Ctrl Pts',(-6.51853060534356,-15.8852234998271,
4.));
#58213=CARTESIAN_POINT('Ctrl Pts',(-6.42799851956089,-15.8408762347418,
4.));
#58214=CARTESIAN_POINT('Ctrl Pts',(-6.33621693362306,-15.7959169003098,
4.));
#58215=CARTESIAN_POINT('Ctrl Pts',(-6.24678085823289,-15.7461619565544,
4.));
#58216=CARTESIAN_POINT('Ctrl Pts',(-6.15997674190851,-15.691902411869,4.));
#58217=CARTESIAN_POINT('Ctrl Pts',(-6.13531568434349,-15.6764872701499,
4.));
#58218=CARTESIAN_POINT('Ctrl Pts',(-6.11086730231581,-15.6607083372246,
4.));
#58219=CARTESIAN_POINT('Ctrl Pts',(-6.08663877235659,-15.6445718215519,
4.));
#58220=CARTESIAN_POINT('Ctrl Pts',(-6.06744081682964,-15.6317857337964,
4.));
#58221=CARTESIAN_POINT('Ctrl Pts',(-6.0483789202221,-15.6187736030245,4.));
#58222=CARTESIAN_POINT('Ctrl Pts',(-6.02947561532874,-15.6055520498285,
4.));
#58223=CARTESIAN_POINT('Ctrl Pts',(-5.94677128184633,-15.5477060937462,
4.));
#58224=CARTESIAN_POINT('Ctrl Pts',(-5.86702045523495,-15.485803012119,4.));
#58225=CARTESIAN_POINT('Ctrl Pts',(-5.79049058680189,-15.4201377361794,
4.));
#58226=CARTESIAN_POINT('Ctrl Pts',(-5.73202513270763,-15.3699723529815,
4.));
#58227=CARTESIAN_POINT('Ctrl Pts',(-5.67544017028651,-15.3176103400047,
4.));
#58228=CARTESIAN_POINT('Ctrl Pts',(-5.62087197491949,-15.2631717733717,
4.));
#58229=CARTESIAN_POINT('Ctrl Pts',(-5.59237459351674,-15.2347420885356,
4.));
#58230=CARTESIAN_POINT('Ctrl Pts',(-5.56442750315923,-15.2057459282144,
4.));
#58231=CARTESIAN_POINT('Ctrl Pts',(-5.53705194133909,-15.1761996365986,
4.));
#58232=CARTESIAN_POINT('Ctrl Pts',(-5.52590419986363,-15.1641679412254,
4.));
#58233=CARTESIAN_POINT('Ctrl Pts',(-5.51485102559337,-15.1520446566585,
4.));
#58234=CARTESIAN_POINT('Ctrl Pts',(-5.50390395570898,-15.1398423958921,
4.));
#58235=CARTESIAN_POINT('Ctrl Pts',(-5.43813919199008,-15.0665370452716,
4.));
#58236=CARTESIAN_POINT('Ctrl Pts',(-5.37610812852687,-14.9902855415477,
4.));
#58237=CARTESIAN_POINT('Ctrl Pts',(-5.31805567958009,-14.9113640105217,
4.));
#58238=CARTESIAN_POINT('Ctrl Pts',(-5.26107088016972,-14.8338939348183,
4.));
#58239=CARTESIAN_POINT('Ctrl Pts',(-5.20791934818337,-14.7538503489036,
4.));
#58240=CARTESIAN_POINT('Ctrl Pts',(-5.15887699703074,-14.6714727381725,
4.));
#58241=CARTESIAN_POINT('Ctrl Pts',(-5.11076871641508,-14.5906641080731,
4.));
#58242=CARTESIAN_POINT('Ctrl Pts',(-5.0666142946296,-14.5076088453843,4.));
#58243=CARTESIAN_POINT('Ctrl Pts',(-5.02672179249125,-14.4225226052514,
4.));
#58244=CARTESIAN_POINT('Ctrl Pts',(-5.00642778712802,-14.3792377642152,
4.));
#58245=CARTESIAN_POINT('Ctrl Pts',(-4.98723753203067,-14.3354272137238,
4.));
#58246=CARTESIAN_POINT('Ctrl Pts',(-4.96919681035721,-14.2911191061582,
4.));
#58247=CARTESIAN_POINT('Ctrl Pts',(-4.96034382211253,-14.2693761203441,
4.));
#58248=CARTESIAN_POINT('Ctrl Pts',(-4.95176770738618,-14.2475133193776,
4.));
#58249=CARTESIAN_POINT('Ctrl Pts',(-4.94347420847157,-14.2255340469214,
4.));
#58250=CARTESIAN_POINT('Ctrl Pts',(-4.93874143956184,-14.2129913531307,
4.));
#58251=CARTESIAN_POINT('Ctrl Pts',(-4.93410201278753,-14.2004140677721,
4.));
#58252=CARTESIAN_POINT('Ctrl Pts',(-4.92955955708199,-14.1878106688628,
4.));
#58253=CARTESIAN_POINT('Ctrl Pts',(-4.89805327414987,-14.1003940207578,
4.));
#58254=CARTESIAN_POINT('Ctrl Pts',(-4.87116570943181,-14.0116107665047,
4.));
#58255=CARTESIAN_POINT('Ctrl Pts',(-4.8491500138814,-13.9216823090563,4.));
#58256=CARTESIAN_POINT('Ctrl Pts',(-4.84589778208928,-13.9083977781333,
4.));
#58257=CARTESIAN_POINT('Ctrl Pts',(-4.84275195632634,-13.8950882390595,
4.));
#58258=CARTESIAN_POINT('Ctrl Pts',(-4.8397134492654,-13.8817543903633,4.));
#58259=CARTESIAN_POINT('Ctrl Pts',(-4.81880165443801,-13.7899873802489,
4.));
#58260=CARTESIAN_POINT('Ctrl Pts',(-4.80296876416446,-13.6970686989268,
4.));
#58261=CARTESIAN_POINT('Ctrl Pts',(-4.7921064004091,-13.6033902081318,4.));
#58262=CARTESIAN_POINT('Ctrl Pts',(-4.78082403916422,-13.5060896023125,
4.));
#58263=CARTESIAN_POINT('Ctrl Pts',(-4.77490405625791,-13.4079680956598,
4.));
#58264=CARTESIAN_POINT('Ctrl Pts',(-4.77428165528829,-13.3094781487529,
4.));
#58265=CARTESIAN_POINT('Ctrl Pts',(-4.77410059584044,-13.2808269475559,
4.));
#58266=CARTESIAN_POINT('Ctrl Pts',(-4.77436819825548,-13.2521447164312,
4.));
#58267=CARTESIAN_POINT('Ctrl Pts',(-4.77508370765677,-13.2234430275403,
4.));
#58268=CARTESIAN_POINT('Ctrl Pts',(-4.77547928901581,-13.2075748180131,
4.));
#58269=CARTESIAN_POINT('Ctrl Pts',(-4.77601178481995,-13.19170066513,4.));
#58270=CARTESIAN_POINT('Ctrl Pts',(-4.77668111451686,-13.175822557735,4.));
#58271=CARTESIAN_POINT('Ctrl Pts',(-4.77726173830688,-13.1620487674244,
4.));
#58272=CARTESIAN_POINT('Ctrl Pts',(-4.77794533193815,-13.1482734031105,
4.));
#58273=CARTESIAN_POINT('Ctrl Pts',(-4.77873092865176,-13.1345098810533,
4.));
#58274=CARTESIAN_POINT('Ctrl Pts',(-4.78403323232826,-13.0416144140266,
4.));
#58275=CARTESIAN_POINT('Ctrl Pts',(-4.79398378921199,-12.9491067853577,
4.));
#58276=CARTESIAN_POINT('Ctrl Pts',(-4.8084638797429,-12.8573599583,4.));
#58277=CARTESIAN_POINT('Ctrl Pts',(-4.82290323568455,-12.7658712283383,
4.));
#58278=CARTESIAN_POINT('Ctrl Pts',(-4.84184708120934,-12.6751380809488,
4.));
#58279=CARTESIAN_POINT('Ctrl Pts',(-4.86522624014646,-12.5855474359577,
4.));
#58280=CARTESIAN_POINT('Ctrl Pts',(-4.88820176586815,-12.4975035429353,
4.));
#58281=CARTESIAN_POINT('Ctrl Pts',(-4.9154612393753,-12.4105622603287,4.));
#58282=CARTESIAN_POINT('Ctrl Pts',(-4.94697939694318,-12.3251200100783,
4.));
#58283=CARTESIAN_POINT('Ctrl Pts',(-4.96237184169077,-12.2833927894037,
4.));
#58284=CARTESIAN_POINT('Ctrl Pts',(-4.9787805689918,-12.2420236106898,4.));
#58285=CARTESIAN_POINT('Ctrl Pts',(-4.99620574112456,-12.2010620870672,
4.));
#58286=CARTESIAN_POINT('Ctrl Pts',(-5.00196784663073,-12.1875170489459,
4.));
#58287=CARTESIAN_POINT('Ctrl Pts',(-5.00784111328384,-12.1740166075363,
4.));
#58288=CARTESIAN_POINT('Ctrl Pts',(-5.01382559232837,-12.160562620369,4.));
#58289=CARTESIAN_POINT('Ctrl Pts',(-5.01951333079912,-12.1477757495608,
4.));
#58290=CARTESIAN_POINT('Ctrl Pts',(-5.02529810648898,-12.135038576554,4.));
#58291=CARTESIAN_POINT('Ctrl Pts',(-5.0311780316899,-12.1223558509962,4.));
#58292=CARTESIAN_POINT('Ctrl Pts',(-5.06862974733614,-12.0415742398394,
4.));
#58293=CARTESIAN_POINT('Ctrl Pts',(-5.10995835566621,-11.9629538753605,
4.));
#58294=CARTESIAN_POINT('Ctrl Pts',(-5.15509810659155,-11.8868432541903,
4.));
#58295=CARTESIAN_POINT('Ctrl Pts',(-5.19948167106006,-11.8120076471655,
4.));
#58296=CARTESIAN_POINT('Ctrl Pts',(-5.24755020547363,-11.739597730264,4.));
#58297=CARTESIAN_POINT('Ctrl Pts',(-5.29927754869182,-11.6699789932549,
4.));
#58298=CARTESIAN_POINT('Ctrl Pts',(-5.34947355289339,-11.6024212530347,
4.));
#58299=CARTESIAN_POINT('Ctrl Pts',(-5.40311537622297,-11.5374914288171,
4.));
#58300=CARTESIAN_POINT('Ctrl Pts',(-5.46020711675472,-11.4755639671884,
4.));
#58301=CARTESIAN_POINT('Ctrl Pts',(-5.47440621920022,-11.4601621881628,
4.));
#58302=CARTESIAN_POINT('Ctrl Pts',(-5.48881883821923,-11.4449463392586,
4.));
#58303=CARTESIAN_POINT('Ctrl Pts',(-5.50344527039708,-11.4299226339363,
4.));
#58304=CARTESIAN_POINT('Ctrl Pts',(-5.52930152881858,-11.4033640855126,
4.));
#58305=CARTESIAN_POINT('Ctrl Pts',(-5.55582596313967,-11.37740591447,4.));
#58306=CARTESIAN_POINT('Ctrl Pts',(-5.58299257280551,-11.3520616136783,
4.));
#58307=CARTESIAN_POINT('Origin',(-7.50000000000001,-12.9903810567666,14.2084234471775));
#58308=CARTESIAN_POINT('Ctrl Pts',(-10.5771720267767,-12.9888570081198,
11.7084234471775));
#58309=CARTESIAN_POINT('Ctrl Pts',(-10.5778106872988,-12.8899681384638,
11.7032843782051));
#58310=CARTESIAN_POINT('Ctrl Pts',(-10.5289895265855,-11.7846562178796,
11.6458119334487));
#58311=CARTESIAN_POINT('Ctrl Pts',(-9.19520367525283,-9.79242641580684,
11.5360061129082));
#58312=CARTESIAN_POINT('Ctrl Pts',(-5.76804697299906,-9.81262440187857,
11.3790059855559));
#58313=CARTESIAN_POINT('Ctrl Pts',(-3.89395285925593,-12.6818121943635,
11.2220058582037));
#58314=CARTESIAN_POINT('Ctrl Pts',(-5.25343392007517,-15.8279700706855,
11.0650057308514));
#58315=CARTESIAN_POINT('Ctrl Pts',(-8.62743330425189,-16.429494929522,10.9080056034992));
#58316=CARTESIAN_POINT('Ctrl Pts',(-10.4164139750736,-14.5502168635008,
10.7891448422745));
#58317=CARTESIAN_POINT('Ctrl Pts',(-10.5747255939164,-13.2672718029744,
10.7226174568339));
#58318=CARTESIAN_POINT('Ctrl Pts',(-10.5724152591149,-12.9929885813497,
10.7084234471775));
#58319=CARTESIAN_POINT('Ctrl Pts',(-10.5702205181091,-12.9936861301783,
11.7915765528225));
#58320=CARTESIAN_POINT('Ctrl Pts',(-10.5655505854978,-12.3126539838428,
11.7563842836469));
#58321=CARTESIAN_POINT('Ctrl Pts',(-10.0102062672903,-10.6096615213504,
11.6688586386871));
#58322=CARTESIAN_POINT('Ctrl Pts',(-7.21365210721562,-9.38337955935061,
11.5289996179432));
#58323=CARTESIAN_POINT('Ctrl Pts',(-4.33342685529555,-11.2379164301912,
11.371999490591));
#58324=CARTESIAN_POINT('Ctrl Pts',(-4.29152503935676,-14.6655878811314,
11.2149993632387));
#58325=CARTESIAN_POINT('Ctrl Pts',(-7.12729256983938,-16.5902267633183,
11.0579992358865));
#58326=CARTESIAN_POINT('Ctrl Pts',(-9.97678353025252,-15.4189029291823,
10.9168582990811));
#58327=CARTESIAN_POINT('Ctrl Pts',(-10.5660600868159,-13.6932623961271,
10.8280507380598));
#58328=CARTESIAN_POINT('Ctrl Pts',(-10.5715492796759,-12.9879252940133,
10.7915765528226));
#58329=CARTESIAN_POINT('Ctrl Pts',(-5.5865340033349,-11.3543938533917,12.));
#58330=CARTESIAN_POINT('Ctrl Pts',(-5.04858820392145,-11.9835803122485,
11.9476666242159));
#58331=CARTESIAN_POINT('Ctrl Pts',(-4.6501322858494,-13.8032255648209,11.8429998726477));
#58332=CARTESIAN_POINT('Ctrl Pts',(-6.60905294539631,-15.8196542318734,
11.6859997452955));
#58333=CARTESIAN_POINT('Ctrl Pts',(-9.36683654413216,-15.2923247501818,
11.5289996179432));
#58334=CARTESIAN_POINT('Ctrl Pts',(-10.4505966874647,-12.7041316569579,
11.371999490591));
#58335=CARTESIAN_POINT('Ctrl Pts',(-8.88853920691362,-10.3709404162538,
11.2149993632387));
#58336=CARTESIAN_POINT('Ctrl Pts',(-6.08135944510335,-10.3874845613442,
11.0579992358865));
#58337=CARTESIAN_POINT('Ctrl Pts',(-4.54629130410829,-12.737632688099,10.9009991085342));
#58338=CARTESIAN_POINT('Ctrl Pts',(-5.65984053808011,-15.31464666358,10.743998981182));
#58339=CARTESIAN_POINT('Ctrl Pts',(-8.42347920724065,-15.8073549219566,
10.5869988538297));
#58340=CARTESIAN_POINT('Ctrl Pts',(-10.3590248070529,-13.7741141771921,
10.4299987264775));
#58341=CARTESIAN_POINT('Ctrl Pts',(-9.73085564098287,-11.0380625363732,
10.2729985991252));
#58342=CARTESIAN_POINT('Ctrl Pts',(-7.1022567140806,-10.0526889161244,10.115998471773));
#58343=CARTESIAN_POINT('Ctrl Pts',(-4.83031806145553,-11.7015642161036,
9.9589983444207));
#58344=CARTESIAN_POINT('Ctrl Pts',(-4.95230878728804,-14.5061379301299,
9.80199821706846));
#58345=CARTESIAN_POINT('Ctrl Pts',(-7.35883867910848,-15.9515158759806,
9.64499808971619));
#58346=CARTESIAN_POINT('Ctrl Pts',(-9.89194927440413,-14.7416168632348,
9.48799796236395));
#58347=CARTESIAN_POINT('Ctrl Pts',(-10.2801760117029,-11.961367369931,9.33099783501168));
#58348=CARTESIAN_POINT('Ctrl Pts',(-8.17539224562471,-10.1038445935438,
9.17399770765945));
#58349=CARTESIAN_POINT('Ctrl Pts',(-5.46497777443614,-10.8347066168947,
9.01699758030717));
#58350=CARTESIAN_POINT('Ctrl Pts',(-4.57938725553999,-13.4985826621227,
8.85999745295493));
#58351=CARTESIAN_POINT('Ctrl Pts',(-6.31273820393898,-15.7067494160557,
8.70299732560268));
#58352=CARTESIAN_POINT('Ctrl Pts',(-9.11071819481798,-15.4791226211167,
8.54599719825042));
#58353=CARTESIAN_POINT('Ctrl Pts',(-10.4643517279258,-13.0198173800209,
8.38899707089818));
#58354=CARTESIAN_POINT('Ctrl Pts',(-9.15982262789147,-10.5341163103444,
8.23199694354591));
#58355=CARTESIAN_POINT('Ctrl Pts',(-6.3669146537774,-10.2509714005752,8.07499681619367));
#58356=CARTESIAN_POINT('Ctrl Pts',(-4.59005518003756,-12.4242814116226,
7.9179966888414));
#58357=CARTESIAN_POINT('Ctrl Pts',(-5.42257114292002,-15.1052184044673,
7.76099656148916));
#58358=CARTESIAN_POINT('Ctrl Pts',(-8.11793749226372,-15.8897604596585,
7.60399643413691));
#58359=CARTESIAN_POINT('Ctrl Pts',(-10.259193363348,-14.0744011876836,7.44699630678465));
#58360=CARTESIAN_POINT('Ctrl Pts',(-9.92625407643148,-11.286990666814,7.2899961794324));
#58361=CARTESIAN_POINT('Ctrl Pts',(-7.4176694799797,-10.0270266461848,7.13299605208014));
#58362=CARTESIAN_POINT('Ctrl Pts',(-4.98291145609725,-11.4243309624572,
6.97599592472789));
#58363=CARTESIAN_POINT('Ctrl Pts',(-4.80525086677252,-14.2259274070742,
6.81899579737564));
#58364=CARTESIAN_POINT('Ctrl Pts',(-7.04399769823543,-15.9195976158556,
6.66199567002339));
#58365=CARTESIAN_POINT('Ctrl Pts',(-9.69164612773492,-14.986611176204,6.50499554267113));
#58366=CARTESIAN_POINT('Ctrl Pts',(-10.3740245283272,-12.2635861515028,
6.34799541531888));
#58367=CARTESIAN_POINT('Ctrl Pts',(-8.47923740659063,-10.1922848677994,
6.19099528796662));
#58368=CARTESIAN_POINT('Ctrl Pts',(-5.70635901253982,-10.630063717047,6.03399516061437));
#58369=CARTESIAN_POINT('Ctrl Pts',(-4.54185510339179,-13.1843609143513,
5.87699503326211));
#58370=CARTESIAN_POINT('Ctrl Pts',(-6.02994926840226,-15.5647161841919,
5.71999490590987));
#58371=CARTESIAN_POINT('Ctrl Pts',(-8.83624974536451,-15.636637176778,5.5629947785576));
#58372=CARTESIAN_POINT('Ctrl Pts',(-10.4443267219795,-13.3356413212244,
5.40599465120536));
#58373=CARTESIAN_POINT('Ctrl Pts',(-9.41218894167164,-10.7250347470945,
5.2489945238531));
#58374=CARTESIAN_POINT('Ctrl Pts',(-6.66539009301951,-10.1458104553331,
5.09199439650085));
#58375=CARTESIAN_POINT('Ctrl Pts',(-4.66696049204361,-12.1172919418034,
4.93499426914859));
#58376=CARTESIAN_POINT('Ctrl Pts',(-5.20901007842283,-14.8717746831197,
4.77799414179635));
#58377=CARTESIAN_POINT('Ctrl Pts',(-7.80528416826264,-15.9390100206221,
4.62099401444409));
#58378=CARTESIAN_POINT('Ctrl Pts',(-10.1280577671037,-14.362540949444,4.46399388709183));
#58379=CARTESIAN_POINT('Ctrl Pts',(-10.0937360173612,-11.5549393117934,
4.30699375973958));
#58380=CARTESIAN_POINT('Ctrl Pts',(-7.73454717783886,-10.0358910717557,
4.14999363238733));
#58381=CARTESIAN_POINT('Ctrl Pts',(-5.16315103760592,-11.163440915316,3.99299350503507));
#58382=CARTESIAN_POINT('Ctrl Pts',(-4.69098959926211,-13.9347976761557,
3.83599337768283));
#58383=CARTESIAN_POINT('Ctrl Pts',(-6.05008049550027,-15.2086689018369,
3.73132662611465));
#58384=CARTESIAN_POINT('Ctrl Pts',(-6.84980000202495,-15.4224678588017,
3.67899325033057));
#58385=CARTESIAN_POINT('Ctrl Pts',(-5.44566844965787,-11.2339557355398,
12.1070022498898));
#58386=CARTESIAN_POINT('Ctrl Pts',(-4.86812015246569,-11.9094616477066,
12.0546688741057));
#58387=CARTESIAN_POINT('Ctrl Pts',(-4.44033070371531,-13.8630655577342,
11.9500021225376));
#58388=CARTESIAN_POINT('Ctrl Pts',(-6.54346319864229,-16.0279396850822,
11.7930019951853));
#58389=CARTESIAN_POINT('Ctrl Pts',(-9.50426933043305,-15.4617892577673,
11.6360018678331));
#58390=CARTESIAN_POINT('Ctrl Pts',(-10.6678137358898,-12.6830585465582,
11.4790017404808));
#58391=CARTESIAN_POINT('Ctrl Pts',(-8.99076069636001,-10.1781024161048,
11.3220016131285));
#58392=CARTESIAN_POINT('Ctrl Pts',(-5.97692195440192,-10.195864508189,11.1650014857763));
#58393=CARTESIAN_POINT('Ctrl Pts',(-4.32884515582416,-12.7190258568539,
11.008001358424));
#58394=CARTESIAN_POINT('Ctrl Pts',(-5.52437166541181,-15.4857544659485,
10.8510012310718));
#58395=CARTESIAN_POINT('Ctrl Pts',(-8.49146390624439,-16.0147349244784,
10.6940011037195));
#58396=CARTESIAN_POINT('Ctrl Pts',(-10.569500516119,-13.831811047759,10.5370009763673));
#58397=CARTESIAN_POINT('Ctrl Pts',(-9.89508678780663,-10.8943367373214,
10.380000849015));
#58398=CARTESIAN_POINT('Ctrl Pts',(-7.07297564596128,-9.83642187472128,
10.2230007216628));
#58399=CARTESIAN_POINT('Ctrl Pts',(-4.6337813970622,-11.606684088542,10.0660005943105));
#58400=CARTESIAN_POINT('Ctrl Pts',(-4.76475283703741,-14.6177249306714,
9.90900046695826));
#58401=CARTESIAN_POINT('Ctrl Pts',(-7.34844666395912,-16.1695087206656,
9.75200033960601));
#58402=CARTESIAN_POINT('Ctrl Pts',(-10.0680398135062,-14.8705393535885,
9.59500021225375));
#58403=CARTESIAN_POINT('Ctrl Pts',(-10.4848470295787,-11.8856134328399,
9.43800008490151));
#58404=CARTESIAN_POINT('Ctrl Pts',(-8.22511327688156,-9.89134353117351,
9.28099995754925));
#58405=CARTESIAN_POINT('Ctrl Pts',(-5.31516349341482,-10.6760101602818,
9.123999830197));
#58406=CARTESIAN_POINT('Ctrl Pts',(-4.36437756524938,-13.5359954516068,
8.96699970284473));
#58407=CARTESIAN_POINT('Ctrl Pts',(-6.22533435639049,-15.9067230417114,
8.80999957549251));
#58408=CARTESIAN_POINT('Ctrl Pts',(-9.22929605861391,-15.6623388157249,
8.65299944814021));
#58409=CARTESIAN_POINT('Ctrl Pts',(-10.6825813950197,-13.0219844234806,
8.495999320788));
#58410=CARTESIAN_POINT('Ctrl Pts',(-9.28201546219901,-10.3532909943549,
8.33899919343572));
#58411=CARTESIAN_POINT('Ctrl Pts',(-6.28349916850765,-10.0493015205563,
8.18199906608348));
#58412=CARTESIAN_POINT('Ctrl Pts',(-4.37583084109032,-12.3826062838239,
8.02499893873122));
#58413=CARTESIAN_POINT('Ctrl Pts',(-5.26963497019092,-15.2609085157313,
7.86799881137897));
#58414=CARTESIAN_POINT('Ctrl Pts',(-8.16342881906923,-16.1032069936549,
7.71099868402671));
#58415=CARTESIAN_POINT('Ctrl Pts',(-10.4623196804644,-14.1542045895756,
7.55399855667447));
#58416=CARTESIAN_POINT('Ctrl Pts',(-10.1048700666991,-11.1615904606817,
7.3969984293222));
#58417=CARTESIAN_POINT('Ctrl Pts',(-7.41160847115729,-9.80887039960631,
7.23999830196995));
#58418=CARTESIAN_POINT('Ctrl Pts',(-4.79760841334188,-11.3090414752098,
7.08299817461771));
#58419=CARTESIAN_POINT('Ctrl Pts',(-4.60686880545846,-14.3168858672889,
6.92599804726544));
#58420=CARTESIAN_POINT('Ctrl Pts',(-7.01042771746335,-16.1352407018342,
6.7689979199132));
#58421=CARTESIAN_POINT('Ctrl Pts',(-9.85299074832685,-15.133569659674,6.61199779256094));
#58422=CARTESIAN_POINT('Ctrl Pts',(-10.5856044869832,-12.2100809588743,
6.45499766520869));
#58423=CARTESIAN_POINT('Ctrl Pts',(-8.55132691312017,-9.98629460218332,
6.29799753785643));
#58424=CARTESIAN_POINT('Ctrl Pts',(-5.57431473726304,-10.4563018579429,
6.14099741050418));
#58425=CARTESIAN_POINT('Ctrl Pts',(-4.32408237085103,-13.1986413249196,
5.98399728315193));
#58426=CARTESIAN_POINT('Ctrl Pts',(-5.92172706293806,-15.75423360635,5.82699715579966));
#58427=CARTESIAN_POINT('Ctrl Pts',(-8.9346217888498,-15.831449279092,5.66999702844743));
#58428=CARTESIAN_POINT('Ctrl Pts',(-10.6610821880398,-13.3610586938876,
5.51299690109516));
#58429=CARTESIAN_POINT('Ctrl Pts',(-9.55296048110486,-10.558264465972,5.35599677374292));
#58430=CARTESIAN_POINT('Ctrl Pts',(-6.60394777480949,-9.93639883608159,
5.19899664639066));
#58431=CARTESIAN_POINT('Ctrl Pts',(-4.45839776891566,-12.0530168609799,
5.04199651903841));
#58432=CARTESIAN_POINT('Ctrl Pts',(-5.04035196569236,-15.0102791328056,
4.88499639168615));
#58433=CARTESIAN_POINT('Ctrl Pts',(-7.82775858038497,-16.1560822091562,
4.72799626433391));
#58434=CARTESIAN_POINT('Ctrl Pts',(-10.3215301429408,-14.4635566264157,
4.57099613698164));
#58435=CARTESIAN_POINT('Ctrl Pts',(-10.2846816943758,-11.4492649509585,
4.4139960096294));
#58436=CARTESIAN_POINT('Ctrl Pts',(-7.75181407368507,-9.81838740652354,
4.25699588227714));
#58437=CARTESIAN_POINT('Ctrl Pts',(-4.99111687367461,-11.0289452226782,
4.09999575492489));
#58438=CARTESIAN_POINT('Ctrl Pts',(-4.48419585112438,-14.0043237457194,
3.94299562757263));
#58439=CARTESIAN_POINT('Ctrl Pts',(-5.94334031085918,-15.3719748325696,
3.83832887600446));
#58440=CARTESIAN_POINT('Ctrl Pts',(-6.80193357383903,-15.6015132427052,
3.78599550022038));
#58441=CARTESIAN_POINT('Ctrl Pts',(-5.30480289598084,-11.1135176176879,
12.2140044997796));
#58442=CARTESIAN_POINT('Ctrl Pts',(-4.68765210100992,-11.8353429831648,
12.1616711239955));
#58443=CARTESIAN_POINT('Ctrl Pts',(-4.23052912158122,-13.9229055506476,
12.0570043724274));
#58444=CARTESIAN_POINT('Ctrl Pts',(-6.47787345188828,-16.2362251382909,
11.9000042450751));
#58445=CARTESIAN_POINT('Ctrl Pts',(-9.64170211673396,-15.6312537653527,
11.7430041177229));
#58446=CARTESIAN_POINT('Ctrl Pts',(-10.8850307843148,-12.6619854361585,
11.5860039903706));
#58447=CARTESIAN_POINT('Ctrl Pts',(-9.09298218580643,-9.98526441595581,
11.4290038630183));
#58448=CARTESIAN_POINT('Ctrl Pts',(-5.87248446370049,-10.0042444550338,
11.2720037356661));
#58449=CARTESIAN_POINT('Ctrl Pts',(-4.11139900754004,-12.7004190256087,
11.1150036083138));
#58450=CARTESIAN_POINT('Ctrl Pts',(-5.3889027927435,-15.656862268317,10.9580034809616));
#58451=CARTESIAN_POINT('Ctrl Pts',(-8.55944860524813,-16.2221149270002,
10.8010033536093));
#58452=CARTESIAN_POINT('Ctrl Pts',(-10.7799762251851,-13.889507918326,10.6440032262571));
#58453=CARTESIAN_POINT('Ctrl Pts',(-10.0593179346304,-10.7506109382696,
10.4870030989048));
#58454=CARTESIAN_POINT('Ctrl Pts',(-7.04369457784195,-9.62015483331818,
10.3300029715526));
#58455=CARTESIAN_POINT('Ctrl Pts',(-4.43724473266885,-11.5118039609805,
10.1730028442003));
#58456=CARTESIAN_POINT('Ctrl Pts',(-4.57719688678678,-14.7293119312129,
10.0160027168481));
#58457=CARTESIAN_POINT('Ctrl Pts',(-7.33805464880973,-16.3875015653505,
9.85900258949582));
#58458=CARTESIAN_POINT('Ctrl Pts',(-10.2441303526083,-14.9994618439422,
9.70200246214357));
#58459=CARTESIAN_POINT('Ctrl Pts',(-10.6895180474545,-11.8098594957488,
9.5450023347913));
#58460=CARTESIAN_POINT('Ctrl Pts',(-8.2748343081384,-9.6788424688032,9.38800220743907));
#58461=CARTESIAN_POINT('Ctrl Pts',(-5.1653492123935,-10.517313703669,9.2310020800868));
#58462=CARTESIAN_POINT('Ctrl Pts',(-4.14936787495879,-13.5734082410908,
9.07400195273456));
#58463=CARTESIAN_POINT('Ctrl Pts',(-6.137930508842,-16.1066966673671,8.9170018253823));
#58464=CARTESIAN_POINT('Ctrl Pts',(-9.34787392240984,-15.8455550103332,
8.76000169803005));
#58465=CARTESIAN_POINT('Ctrl Pts',(-10.9008110621136,-13.0241514669403,
8.60300157067779));
#58466=CARTESIAN_POINT('Ctrl Pts',(-9.40420829650654,-10.1724656783654,
8.44600144332554));
#58467=CARTESIAN_POINT('Ctrl Pts',(-6.20008368323791,-9.84763164053746,
8.28900131597328));
#58468=CARTESIAN_POINT('Ctrl Pts',(-4.16160650214306,-12.3409311560251,
8.13200118862103));
#58469=CARTESIAN_POINT('Ctrl Pts',(-5.11669879746183,-15.4165986269953,
7.97500106126878));
#58470=CARTESIAN_POINT('Ctrl Pts',(-8.20892014587475,-16.3166535276513,
7.81800093391653));
#58471=CARTESIAN_POINT('Ctrl Pts',(-10.6654459975808,-14.2340079914677,
7.66100080656427));
#58472=CARTESIAN_POINT('Ctrl Pts',(-10.2834860569666,-11.0361902545495,
7.50400067921202));
#58473=CARTESIAN_POINT('Ctrl Pts',(-7.40554746233487,-9.59071415302789,
7.34700055185976));
#58474=CARTESIAN_POINT('Ctrl Pts',(-4.61230537058651,-11.1937519879624,
7.19000042450751));
#58475=CARTESIAN_POINT('Ctrl Pts',(-4.40848674414439,-14.4078443275035,
7.03300029715526));
#58476=CARTESIAN_POINT('Ctrl Pts',(-6.97685773669127,-16.3508837878128,
6.876000169803));
#58477=CARTESIAN_POINT('Ctrl Pts',(-10.0143353689188,-15.280528143144,6.71900004245075));
#58478=CARTESIAN_POINT('Ctrl Pts',(-10.7971844456393,-12.1565757662458,
6.5619999150985));
#58479=CARTESIAN_POINT('Ctrl Pts',(-8.62341641964973,-9.78030433656719,
6.40499978774624));
#58480=CARTESIAN_POINT('Ctrl Pts',(-5.44227046198626,-10.2825399988388,
6.24799966039399));
#58481=CARTESIAN_POINT('Ctrl Pts',(-4.10630963831026,-13.2129217354879,
6.09099953304174));
#58482=CARTESIAN_POINT('Ctrl Pts',(-5.81350485747386,-15.943751028508,5.93399940568949));
#58483=CARTESIAN_POINT('Ctrl Pts',(-9.0329938323351,-16.026261381406,5.77699927833723));
#58484=CARTESIAN_POINT('Ctrl Pts',(-10.8778376541001,-13.3864760665508,
5.61999915098497));
#58485=CARTESIAN_POINT('Ctrl Pts',(-9.69373202053811,-10.3914941848495,
5.46299902363273));
#58486=CARTESIAN_POINT('Ctrl Pts',(-6.54250545659946,-9.72698721683007,
5.30599889628047));
#58487=CARTESIAN_POINT('Ctrl Pts',(-4.24983504578773,-11.9887417801564,
5.14899876892822));
#58488=CARTESIAN_POINT('Ctrl Pts',(-4.87169385296189,-15.1487835824914,
4.99199864157596));
#58489=CARTESIAN_POINT('Ctrl Pts',(-7.85023299250732,-16.3731543976903,
4.83499851422371));
#58490=CARTESIAN_POINT('Ctrl Pts',(-10.5150025187778,-14.5645723033874,
4.67799838687146));
#58491=CARTESIAN_POINT('Ctrl Pts',(-10.4756273713904,-11.3435905901237,
4.5209982595192));
#58492=CARTESIAN_POINT('Ctrl Pts',(-7.76908096953125,-9.60088374129137,
4.36399813216695));
#58493=CARTESIAN_POINT('Ctrl Pts',(-4.81908270974332,-10.8944495300405,
4.2069980048147));
#58494=CARTESIAN_POINT('Ctrl Pts',(-4.27740210298664,-14.0738498152832,
4.04999787746244));
#58495=CARTESIAN_POINT('Ctrl Pts',(-5.83660012621808,-15.5352807633023,
3.94533112589427));
#58496=CARTESIAN_POINT('Ctrl Pts',(-6.75406714565312,-15.7805586266087,
3.89299775011019));
#58497=CARTESIAN_POINT('Ctrl Pts',(-5.1639373423038,-10.993079499836,12.3210067496694));
#58498=CARTESIAN_POINT('Ctrl Pts',(-4.50718404955416,-11.761224318623,12.2686733738853));
#58499=CARTESIAN_POINT('Ctrl Pts',(-4.02072753944713,-13.9827455435609,
12.1640066223172));
#58500=CARTESIAN_POINT('Ctrl Pts',(-6.41228370513427,-16.4445105914997,
12.0070064949649));
#58501=CARTESIAN_POINT('Ctrl Pts',(-9.77913490303484,-15.8007182729381,
11.8500063676127));
#58502=CARTESIAN_POINT('Ctrl Pts',(-11.1022478327399,-12.6409123257588,
11.6930062402604));
#58503=CARTESIAN_POINT('Ctrl Pts',(-9.19520367525283,-9.79242641580684,
11.5360061129082));
#58504=CARTESIAN_POINT('Ctrl Pts',(-5.76804697299906,-9.81262440187857,
11.3790059855559));
#58505=CARTESIAN_POINT('Ctrl Pts',(-3.89395285925593,-12.6818121943635,
11.2220058582037));
#58506=CARTESIAN_POINT('Ctrl Pts',(-5.25343392007517,-15.8279700706855,
11.0650057308514));
#58507=CARTESIAN_POINT('Ctrl Pts',(-8.62743330425189,-16.429494929522,10.9080056034992));
#58508=CARTESIAN_POINT('Ctrl Pts',(-10.9904519342511,-13.9472047888929,
10.7510054761469));
#58509=CARTESIAN_POINT('Ctrl Pts',(-10.2235490814542,-10.6068851392178,
10.5940053487946));
#58510=CARTESIAN_POINT('Ctrl Pts',(-7.01441350972263,-9.40388779191504,
10.4370052214424));
#58511=CARTESIAN_POINT('Ctrl Pts',(-4.2407080682755,-11.4169238334189,10.2800050940901));
#58512=CARTESIAN_POINT('Ctrl Pts',(-4.38964093653616,-14.8408989317544,
10.1230049667379));
#58513=CARTESIAN_POINT('Ctrl Pts',(-7.32766263366035,-16.6054944100355,
9.96600483938563));
#58514=CARTESIAN_POINT('Ctrl Pts',(-10.4202208917104,-15.1283843342959,
9.80900471203338));
#58515=CARTESIAN_POINT('Ctrl Pts',(-10.8941890653303,-11.7341055586577,
9.65200458468112));
#58516=CARTESIAN_POINT('Ctrl Pts',(-8.32455533939524,-9.46634140643289,
9.49500445732887));
#58517=CARTESIAN_POINT('Ctrl Pts',(-5.01553493137219,-10.3586172470561,
9.33800432997662));
#58518=CARTESIAN_POINT('Ctrl Pts',(-3.93435818466818,-13.6108210305748,
9.18100420262436));
#58519=CARTESIAN_POINT('Ctrl Pts',(-6.05052666129351,-16.3066702930228,
9.02400407527212));
#58520=CARTESIAN_POINT('Ctrl Pts',(-9.46645178620579,-16.0287712049414,
8.86700394791984));
#58521=CARTESIAN_POINT('Ctrl Pts',(-11.1190407292075,-13.0263185104,8.71000382056762));
#58522=CARTESIAN_POINT('Ctrl Pts',(-9.52640113081409,-9.99164036237588,
8.55300369321534));
#58523=CARTESIAN_POINT('Ctrl Pts',(-6.11666819796815,-9.64596176051859,
8.3960035658631));
#58524=CARTESIAN_POINT('Ctrl Pts',(-3.94738216319582,-12.2992560282264,
8.23900343851084));
#58525=CARTESIAN_POINT('Ctrl Pts',(-4.96376262473273,-15.5722887382593,
8.0820033111586));
#58526=CARTESIAN_POINT('Ctrl Pts',(-8.25441147268027,-16.5301000616477,
7.92500318380633));
#58527=CARTESIAN_POINT('Ctrl Pts',(-10.8685723146971,-14.3138113933598,
7.76800305645408));
#58528=CARTESIAN_POINT('Ctrl Pts',(-10.4621020472342,-10.9107900484173,
7.61100292910183));
#58529=CARTESIAN_POINT('Ctrl Pts',(-7.39948645351245,-9.37255790644949,
7.45400280174957));
#58530=CARTESIAN_POINT('Ctrl Pts',(-4.42700232783115,-11.078462500715,7.29700267439732));
#58531=CARTESIAN_POINT('Ctrl Pts',(-4.21010468283033,-14.4988027877182,
7.14000254704507));
#58532=CARTESIAN_POINT('Ctrl Pts',(-6.94328775591919,-16.5665268737914,
6.98300241969282));
#58533=CARTESIAN_POINT('Ctrl Pts',(-10.1756799895107,-15.427486626614,6.82600229234056));
#58534=CARTESIAN_POINT('Ctrl Pts',(-11.0087644042953,-12.1030705736173,
6.66900216498831));
#58535=CARTESIAN_POINT('Ctrl Pts',(-8.69550592617927,-9.57431407095109,
6.51200203763606));
#58536=CARTESIAN_POINT('Ctrl Pts',(-5.31022618670948,-10.1087781397346,
6.3550019102838));
#58537=CARTESIAN_POINT('Ctrl Pts',(-3.88853690576949,-13.2272021460562,
6.19800178293155));
#58538=CARTESIAN_POINT('Ctrl Pts',(-5.70528265200966,-16.133268450666,6.0410016555793));
#58539=CARTESIAN_POINT('Ctrl Pts',(-9.13136587582039,-16.22107348372,5.88400152822704));
#58540=CARTESIAN_POINT('Ctrl Pts',(-11.0945931201605,-13.4118934392139,
5.72700140087479));
#58541=CARTESIAN_POINT('Ctrl Pts',(-9.83450355997132,-10.224723903727,5.57000127352253));
#58542=CARTESIAN_POINT('Ctrl Pts',(-6.48106313838945,-9.51757559757857,
5.41300114617028));
#58543=CARTESIAN_POINT('Ctrl Pts',(-4.04127232265978,-11.9244666993329,
5.25600101881803));
#58544=CARTESIAN_POINT('Ctrl Pts',(-4.70303574023142,-15.2872880321773,
5.09900089146577));
#58545=CARTESIAN_POINT('Ctrl Pts',(-7.87270740462966,-16.5902265862243,
4.94200076411352));
#58546=CARTESIAN_POINT('Ctrl Pts',(-10.7084748946149,-14.6655879803591,
4.78500063676127));
#58547=CARTESIAN_POINT('Ctrl Pts',(-10.666573048405,-11.2379162292888,4.62800050940902));
#58548=CARTESIAN_POINT('Ctrl Pts',(-7.78634786537746,-9.38338007605921,
4.47100038205676));
#58549=CARTESIAN_POINT('Ctrl Pts',(-4.64704854581202,-10.7599538374027,
4.31400025470451));
#58550=CARTESIAN_POINT('Ctrl Pts',(-4.0706083548489,-14.143375884847,4.15700012735225));
#58551=CARTESIAN_POINT('Ctrl Pts',(-5.72985994157699,-15.6985866940351,
4.05233337578409));
#58552=CARTESIAN_POINT('Ctrl Pts',(-6.7062007174672,-15.9596040105123,4.));
#58553=CARTESIAN_POINT('Ctrl Pts',(-5.5865340033349,-11.3543938533917,12.));
#58554=CARTESIAN_POINT('Ctrl Pts',(-5.52489675159201,-11.412317734857,12.));
#58555=CARTESIAN_POINT('Ctrl Pts',(-5.46662466733851,-11.4733903391465,
12.));
#58556=CARTESIAN_POINT('Ctrl Pts',(-5.41171731080853,-11.5372273647712,
12.));
#58557=CARTESIAN_POINT('Ctrl Pts',(-5.35535954826471,-11.6027506782036,
12.));
#58558=CARTESIAN_POINT('Ctrl Pts',(-5.30254618320446,-11.6711868211063,
12.));
#58559=CARTESIAN_POINT('Ctrl Pts',(-5.25330217107373,-11.7421687765855,
12.));
#58560=CARTESIAN_POINT('Ctrl Pts',(-5.20312956815832,-11.8144892336791,
12.));
#58561=CARTESIAN_POINT('Ctrl Pts',(-5.1566617252503,-11.8894530177238,12.));
#58562=CARTESIAN_POINT('Ctrl Pts',(-5.11395808422126,-11.9667137220828,
12.));
#58563=CARTESIAN_POINT('Ctrl Pts',(-5.09461562078295,-12.0017086853522,
12.));
#58564=CARTESIAN_POINT('Ctrl Pts',(-5.07604591099636,-12.0371753912937,
12.));
#58565=CARTESIAN_POINT('Ctrl Pts',(-5.05825705836343,-12.0730838611618,
12.));
#58566=CARTESIAN_POINT('Ctrl Pts',(-5.04815218455416,-12.093481498052,12.));
#58567=CARTESIAN_POINT('Ctrl Pts',(-5.03829930483427,-12.1140217037901,
12.));
#58568=CARTESIAN_POINT('Ctrl Pts',(-5.02870015601257,-12.1346991425122,
12.));
#58569=CARTESIAN_POINT('Ctrl Pts',(-5.02048318017586,-12.1523992550431,
12.));
#58570=CARTESIAN_POINT('Ctrl Pts',(-5.01244999988763,-12.1702050672847,
12.));
#58571=CARTESIAN_POINT('Ctrl Pts',(-5.00461448908043,-12.1880835326347,
12.));
#58572=CARTESIAN_POINT('Ctrl Pts',(-4.96800851502513,-12.2716082261557,
12.));
#58573=CARTESIAN_POINT('Ctrl Pts',(-4.93566438777708,-12.3568162975634,
12.));
#58574=CARTESIAN_POINT('Ctrl Pts',(-4.9076092477584,-12.4433098844385,12.));
#58575=CARTESIAN_POINT('Ctrl Pts',(-4.87909470826589,-12.531219793181,12.));
#58576=CARTESIAN_POINT('Ctrl Pts',(-4.85501027288513,-12.6204584164563,
12.));
#58577=CARTESIAN_POINT('Ctrl Pts',(-4.83542346103633,-12.7106451238744,
12.));
#58578=CARTESIAN_POINT('Ctrl Pts',(-4.81671890332471,-12.7967695266993,
12.));
#58579=CARTESIAN_POINT('Ctrl Pts',(-4.80211587003395,-12.8837594508039,
12.));
#58580=CARTESIAN_POINT('Ctrl Pts',(-4.79171175017421,-12.9713041908118,
12.));
#58581=CARTESIAN_POINT('Ctrl Pts',(-4.7871219669274,-13.0099246014234,12.));
#58582=CARTESIAN_POINT('Ctrl Pts',(-4.78334987321312,-13.0486531860177,
12.));
#58583=CARTESIAN_POINT('Ctrl Pts',(-4.78040642509842,-13.0874639619222,
12.));
#58584=CARTESIAN_POINT('Ctrl Pts',(-4.7790340847621,-13.1055589278201,12.));
#58585=CARTESIAN_POINT('Ctrl Pts',(-4.77784189531648,-13.1236717640034,
12.));
#58586=CARTESIAN_POINT('Ctrl Pts',(-4.77683109303951,-13.1417998520234,
12.));
#58587=CARTESIAN_POINT('Ctrl Pts',(-4.7758570840318,-13.1592680764492,12.));
#58588=CARTESIAN_POINT('Ctrl Pts',(-4.77505149943043,-13.1767532882224,
12.));
#58589=CARTESIAN_POINT('Ctrl Pts',(-4.77441609878784,-13.1942285673893,
12.));
#58590=CARTESIAN_POINT('Ctrl Pts',(-4.77095265346117,-13.2894829154418,
12.));
#58591=CARTESIAN_POINT('Ctrl Pts',(-4.77253183089421,-13.3845892743107,
12.));
#58592=CARTESIAN_POINT('Ctrl Pts',(-4.77921580433521,-13.4791489989792,
12.));
#58593=CARTESIAN_POINT('Ctrl Pts',(-4.78586481725455,-13.5732141290278,
12.));
#58594=CARTESIAN_POINT('Ctrl Pts',(-4.79756501411883,-13.6667392834721,
12.));
#58595=CARTESIAN_POINT('Ctrl Pts',(-4.81442558423848,-13.7593498298833,
12.));
#58596=CARTESIAN_POINT('Ctrl Pts',(-4.830924328857,-13.8499729667865,12.));
#58597=CARTESIAN_POINT('Ctrl Pts',(-4.85236399681968,-13.9397212614334,
12.));
#58598=CARTESIAN_POINT('Ctrl Pts',(-4.87847000308199,-14.0283529813775,
12.));
#58599=CARTESIAN_POINT('Ctrl Pts',(-4.89379441408366,-14.0803804301784,
12.));
#58600=CARTESIAN_POINT('Ctrl Pts',(-4.91072775850773,-14.1320231162836,
12.));
#58601=CARTESIAN_POINT('Ctrl Pts',(-4.92922261500886,-14.1832309956159,
12.));
#58602=CARTESIAN_POINT('Ctrl Pts',(-4.93398351814407,-14.1964128093404,
12.));
#58603=CARTESIAN_POINT('Ctrl Pts',(-4.93884875001307,-14.2095679810762,
12.));
#58604=CARTESIAN_POINT('Ctrl Pts',(-4.94381485137731,-14.2226885070165,
12.));
#58605=CARTESIAN_POINT('Ctrl Pts',(-4.97686325186981,-14.310002954335,12.));
#58606=CARTESIAN_POINT('Ctrl Pts',(-5.01429440116268,-14.3955759829307,
12.));
#58607=CARTESIAN_POINT('Ctrl Pts',(-5.05577732713123,-14.4791717978631,
12.));
#58608=CARTESIAN_POINT('Ctrl Pts',(-5.09882663969929,-14.5659241732654,
12.));
#58609=CARTESIAN_POINT('Ctrl Pts',(-5.1462396027634,-14.6505479156747,12.));
#58610=CARTESIAN_POINT('Ctrl Pts',(-5.19770241499811,-14.7327775666312,
12.));
#58611=CARTESIAN_POINT('Ctrl Pts',(-5.24979009521262,-14.8160056604173,
12.));
#58612=CARTESIAN_POINT('Ctrl Pts',(-5.30602696260126,-14.8967819927061,
12.));
#58613=CARTESIAN_POINT('Ctrl Pts',(-5.36613986514052,-14.9748175661494,
12.));
#58614=CARTESIAN_POINT('Ctrl Pts',(-5.40561376259492,-15.0260606120477,
12.));
#58615=CARTESIAN_POINT('Ctrl Pts',(-5.44676008901899,-15.076121523717,12.));
#58616=CARTESIAN_POINT('Ctrl Pts',(-5.48951221838806,-15.1249126475777,
12.));
#58617=CARTESIAN_POINT('Ctrl Pts',(-5.50097170290556,-15.1379908529612,
12.));
#58618=CARTESIAN_POINT('Ctrl Pts',(-5.51254660460158,-15.1509777948558,
12.));
#58619=CARTESIAN_POINT('Ctrl Pts',(-5.52423573327417,-15.1638717111488,
12.));
#58620=CARTESIAN_POINT('Ctrl Pts',(-5.5353884173992,-15.1761738920537,12.));
#58621=CARTESIAN_POINT('Ctrl Pts',(-5.54663940936984,-15.1883850930378,
12.));
#58622=CARTESIAN_POINT('Ctrl Pts',(-5.55798428070717,-15.2005008010861,
12.));
#58623=CARTESIAN_POINT('Ctrl Pts',(-5.62980603833238,-15.2772025477193,
12.));
#58624=CARTESIAN_POINT('Ctrl Pts',(-5.70542358612169,-15.3501207786779,
12.));
#58625=CARTESIAN_POINT('Ctrl Pts',(-5.7844933991545,-15.4189223872958,12.));
#58626=CARTESIAN_POINT('Ctrl Pts',(-5.8437957589291,-15.4705235937591,12.));
#58627=CARTESIAN_POINT('Ctrl Pts',(-5.90504133108183,-15.519808942512,12.));
#58628=CARTESIAN_POINT('Ctrl Pts',(-5.968104244788,-15.5666263507592,12.));
#58629=CARTESIAN_POINT('Ctrl Pts',(-5.99074690383604,-15.5834360817113,
12.));
#58630=CARTESIAN_POINT('Ctrl Pts',(-6.01362398614045,-15.5999275418789,
12.));
#58631=CARTESIAN_POINT('Ctrl Pts',(-6.03673011024537,-15.6160932756601,
12.));
#58632=CARTESIAN_POINT('Ctrl Pts',(-6.05604444624562,-15.6296061613575,
12.));
#58633=CARTESIAN_POINT('Ctrl Pts',(-6.07552135620629,-15.6428929845117,
12.));
#58634=CARTESIAN_POINT('Ctrl Pts',(-6.09513705214722,-15.655935902686,12.));
#58635=CARTESIAN_POINT('Ctrl Pts',(-6.1801078936968,-15.7124349296322,12.));
#58636=CARTESIAN_POINT('Ctrl Pts',(-6.26775546621735,-15.7644144018326,
12.));
#58637=CARTESIAN_POINT('Ctrl Pts',(-6.3577924589883,-15.8115622787044,12.));
#58638=CARTESIAN_POINT('Ctrl Pts',(-6.42986829724945,-15.8493047958986,
12.));
#58639=CARTESIAN_POINT('Ctrl Pts',(-6.50347629812978,-15.8839507974289,
12.));
#58640=CARTESIAN_POINT('Ctrl Pts',(-6.57848586659695,-15.9153228867674,
12.));
#58641=CARTESIAN_POINT('Ctrl Pts',(-6.61998922672564,-15.9326813004793,
12.));
#58642=CARTESIAN_POINT('Ctrl Pts',(-6.66192191928759,-15.9490371078547,
12.));
#58643=CARTESIAN_POINT('Ctrl Pts',(-6.70425049788235,-15.9643995452955,
12.));
#58644=CARTESIAN_POINT('Ctrl Pts',(-10.0166114900998,-12.9925168768863,
10.387416697508));
#58645=CARTESIAN_POINT('Ctrl Pts',(-10.0185038824417,-13.21718192014,10.4016107071645));
#58646=CARTESIAN_POINT('Ctrl Pts',(-9.99083741615502,-13.441388813634,10.415804716821));
#58647=CARTESIAN_POINT('Ctrl Pts',(-9.93173901273922,-13.6569790278497,
10.4299987264775));
#58648=CARTESIAN_POINT('Ctrl Pts',(-9.71384294044885,-14.4518610921136,
10.4823321022616));
#58649=CARTESIAN_POINT('Ctrl Pts',(-9.06866107384475,-15.1296080070351,
10.5346654780456));
#58650=CARTESIAN_POINT('Ctrl Pts',(-8.28546369568261,-15.3863634214331,
10.5869988538297));
#58651=CARTESIAN_POINT('Ctrl Pts',(-7.50226631752047,-15.6431188358311,
10.6393322296138));
#58652=CARTESIAN_POINT('Ctrl Pts',(-6.58105342780029,-15.4788827497055,
10.6916656053979));
#58653=CARTESIAN_POINT('Ctrl Pts',(-5.9348554439449,-14.9672623773959,10.743998981182));
#58654=CARTESIAN_POINT('Ctrl Pts',(-5.2886574600895,-14.4556420050863,10.7963323569661));
#58655=CARTESIAN_POINT('Ctrl Pts',(-4.91747438209889,-13.5966373465927,
10.8486657327501));
#58656=CARTESIAN_POINT('Ctrl Pts',(-4.98772753326943,-12.7754436628867,
10.9009991085342));
#58657=CARTESIAN_POINT('Ctrl Pts',(-5.05798068443997,-11.9542499791808,
10.9533324843183));
#58658=CARTESIAN_POINT('Ctrl Pts',(-5.56967006477166,-11.1708672702625,
11.0056658601024));
#58659=CARTESIAN_POINT('Ctrl Pts',(-6.29337804857255,-10.7764185582883,
11.0579992358865));
#58660=CARTESIAN_POINT('Ctrl Pts',(-7.01708603237344,-10.3819698463141,
11.1103326116706));
#58661=CARTESIAN_POINT('Ctrl Pts',(-7.95281261964353,-10.3764551312839,
11.1626659874547));
#58662=CARTESIAN_POINT('Ctrl Pts',(-8.68101882670376,-10.7625629805529,
11.2149993632387));
#58663=CARTESIAN_POINT('Ctrl Pts',(-9.40922503376398,-11.1486708298218,
11.2673327390228));
#58664=CARTESIAN_POINT('Ctrl Pts',(-9.92991086061434,-11.9264012433898,
11.3196661148069));
#58665=CARTESIAN_POINT('Ctrl Pts',(-10.0096270834841,-12.7466319657112,
11.371999490591));
#58666=CARTESIAN_POINT('Ctrl Pts',(-10.0174551121829,-12.8271775485652,
11.3771385595633));
#58667=CARTESIAN_POINT('Ctrl Pts',(-10.0210308785667,-12.9081329611663,
11.3822776285357));
#58668=CARTESIAN_POINT('Ctrl Pts',(-10.0205077525331,-12.989132710429,11.387416697508));
#58669=CARTESIAN_POINT('Ctrl Pts',(-8.29379928253297,-15.9596040105122,
12.));
#58670=CARTESIAN_POINT('Ctrl Pts',(-9.27014005842316,-15.698586694035,11.9476666242159));
#58671=CARTESIAN_POINT('Ctrl Pts',(-10.9293914260692,-14.1433745388278,
11.8429998726477));
#58672=CARTESIAN_POINT('Ctrl Pts',(-10.3529516457367,-10.7599545073216,
11.6859997452955));
#58673=CARTESIAN_POINT('Ctrl Pts',(-7.21365210721562,-9.38337955935061,
11.5289996179432));
#58674=CARTESIAN_POINT('Ctrl Pts',(-4.33342685529555,-11.2379164301912,
11.371999490591));
#58675=CARTESIAN_POINT('Ctrl Pts',(-4.29152503935676,-14.6655878811314,
11.2149993632387));
#58676=CARTESIAN_POINT('Ctrl Pts',(-7.12729256983938,-16.5902267633183,
11.0579992358865));
#58677=CARTESIAN_POINT('Ctrl Pts',(-10.296964344732,-15.2872880462285,10.9009991085342));
#58678=CARTESIAN_POINT('Ctrl Pts',(-10.9587277612158,-11.9244666973206,
10.743998981182));
#58679=CARTESIAN_POINT('Ctrl Pts',(-8.51893689306524,-9.51757549146244,
10.5869988538297));
#58680=CARTESIAN_POINT('Ctrl Pts',(-5.16549637569413,-10.2247238388162,
10.4299987264775));
#58681=CARTESIAN_POINT('Ctrl Pts',(-3.90540678666615,-13.4118934459175,
10.2729985991252));
#58682=CARTESIAN_POINT('Ctrl Pts',(-5.86863408021139,-16.2210735713392,
10.115998471773));
#58683=CARTESIAN_POINT('Ctrl Pts',(-9.29471739586239,-16.133268532241,9.9589983444207));
#58684=CARTESIAN_POINT('Ctrl Pts',(-11.1114631891741,-13.227202153015,9.80199821706844));
#58685=CARTESIAN_POINT('Ctrl Pts',(-9.68977387121298,-10.1087780633504,
9.64499808971621));
#58686=CARTESIAN_POINT('Ctrl Pts',(-6.30449404219616,-9.57431398106461,
9.48799796236394));
#58687=CARTESIAN_POINT('Ctrl Pts',(-3.99123550321764,-12.1030705501041,
9.33099783501171));
#58688=CARTESIAN_POINT('Ctrl Pts',(-4.82431993989319,-15.4274866909495,
9.17399770765942));
#58689=CARTESIAN_POINT('Ctrl Pts',(-8.05671225877921,-16.5665269680756,
9.0169975803072));
#58690=CARTESIAN_POINT('Ctrl Pts',(-10.789895403928,-14.4988028275178,8.85999745295491));
#58691=CARTESIAN_POINT('Ctrl Pts',(-10.5729977532197,-11.0784624502813,
8.70299732560269));
#58692=CARTESIAN_POINT('Ctrl Pts',(-7.60051354913579,-9.37255781103892,
8.54599719825042));
#58693=CARTESIAN_POINT('Ctrl Pts',(-4.53789787464541,-10.9107899935683,
8.38899707089818));
#58694=CARTESIAN_POINT('Ctrl Pts',(-4.13142759646044,-14.3138114282651,
8.23199694354591));
#58695=CARTESIAN_POINT('Ctrl Pts',(-6.74558850742372,-16.5301001550025,
8.07499681619368));
#58696=CARTESIAN_POINT('Ctrl Pts',(-10.0362374421571,-15.5722888063543,
7.9179966888414));
#58697=CARTESIAN_POINT('Ctrl Pts',(-11.0526179305001,-12.2992560099981,
7.76099656148917));
#58698=CARTESIAN_POINT('Ctrl Pts',(-8.88333183851511,-9.64596167231467,
7.60399643413689));
#58699=CARTESIAN_POINT('Ctrl Pts',(-5.47359881574229,-9.99164028328652,
7.44699630678467));
#58700=CARTESIAN_POINT('Ctrl Pts',(-3.88095917534459,-13.0263185113509,
7.28999617943238));
#58701=CARTESIAN_POINT('Ctrl Pts',(-5.53354816193247,-16.0287712850697,
7.13299605208016));
#58702=CARTESIAN_POINT('Ctrl Pts',(-8.94947337693327,-16.3066703804957,
6.97599592472788));
#58703=CARTESIAN_POINT('Ctrl Pts',(-11.0656419093738,-13.610821046919,6.81899579737565));
#58704=CARTESIAN_POINT('Ctrl Pts',(-9.98446513414696,-10.3586171776818,
6.66199567002337));
#58705=CARTESIAN_POINT('Ctrl Pts',(-6.67544463886838,-9.46634131342536,
6.50499554267114));
#58706=CARTESIAN_POINT('Ctrl Pts',(-4.10581084513197,-11.7341055256468,
6.34799541531887));
#58707=CARTESIAN_POINT('Ctrl Pts',(-4.57977903131249,-15.1283843904584,
6.19099528796663));
#58708=CARTESIAN_POINT('Ctrl Pts',(-7.67233737080682,-16.6054945057935,
6.03399516061437));
#58709=CARTESIAN_POINT('Ctrl Pts',(-10.610359145649,-14.8408989797994,5.87699503326212));
#58710=CARTESIAN_POINT('Ctrl Pts',(-10.7592920173832,-11.4169237933092,
5.71999490590986));
#58711=CARTESIAN_POINT('Ctrl Pts',(-7.98558650367391,-9.40388769480238,
5.56299477855761));
#58712=CARTESIAN_POINT('Ctrl Pts',(-4.77645084555843,-10.6068850809164,
5.40599465120535));
#58713=CARTESIAN_POINT('Ctrl Pts',(-4.00954797596254,-13.9472048059447,
5.24899452385311));
#58714=CARTESIAN_POINT('Ctrl Pts',(-6.37256666156175,-16.4294950347898,
5.09199439650084));
#58715=CARTESIAN_POINT('Ctrl Pts',(-9.74656614790733,-15.8279701198543,
4.9349942691486));
#58716=CARTESIAN_POINT('Ctrl Pts',(-11.1060472187217,-12.6818122309103,
4.77799414179634));
#58717=CARTESIAN_POINT('Ctrl Pts',(-9.23195310627391,-9.81262424147309,
4.62099401444409));
#58718=CARTESIAN_POINT('Ctrl Pts',(-5.80479621412607,-9.79242646017958,
4.46399388709183));
#58719=CARTESIAN_POINT('Ctrl Pts',(-3.89775220169895,-12.6409121056472,
4.30699375973959));
#58720=CARTESIAN_POINT('Ctrl Pts',(-5.22086478169416,-15.8007186832344,
4.14999363238732));
#58721=CARTESIAN_POINT('Ctrl Pts',(-8.58771683219162,-16.4445101479194,
3.99299350503508));
#58722=CARTESIAN_POINT('Ctrl Pts',(-10.979271517566,-13.9827465287205,3.83599337768283));
#58723=CARTESIAN_POINT('Ctrl Pts',(-10.4928159504458,-11.7612243186229,
3.73132662611465));
#58724=CARTESIAN_POINT('Ctrl Pts',(-9.83606265769611,-10.9930794998359,
3.67899325033057));
#58725=CARTESIAN_POINT('Ctrl Pts',(-8.24593285434704,-15.7805586266087,
12.1070022498898));
#58726=CARTESIAN_POINT('Ctrl Pts',(-9.16339987378206,-15.5352807633023,
12.0546688741057));
#58727=CARTESIAN_POINT('Ctrl Pts',(-10.7225976911422,-14.0738485504296,
11.9500021225376));
#58728=CARTESIAN_POINT('Ctrl Pts',(-10.180917470255,-10.8944501595629,11.7930019951853));
#58729=CARTESIAN_POINT('Ctrl Pts',(-7.23091900471447,-9.60088325574055,
11.6360018678331));
#58730=CARTESIAN_POINT('Ctrl Pts',(-4.52437253811706,-11.3435907789116,
11.4790017404808));
#58731=CARTESIAN_POINT('Ctrl Pts',(-4.48499741917537,-14.5645722101431,
11.3220016131286));
#58732=CARTESIAN_POINT('Ctrl Pts',(-7.14976698350127,-16.3731545641054,
11.1650014857763));
#58733=CARTESIAN_POINT('Ctrl Pts',(-10.1283062268782,-15.1487835956953,
11.008001358424));
#58734=CARTESIAN_POINT('Ctrl Pts',(-10.7501650330301,-11.9887417782655,
10.8510012310718));
#58735=CARTESIAN_POINT('Ctrl Pts',(-8.45749457295849,-9.72698711711278,
10.6940011037196));
#58736=CARTESIAN_POINT('Ctrl Pts',(-5.30626791900676,-10.3914941238528,
10.5370009763673));
#58737=CARTESIAN_POINT('Ctrl Pts',(-4.12216225834487,-13.3864760728501,
10.380000849015));
#58738=CARTESIAN_POINT('Ctrl Pts',(-5.96700612634799,-16.0262614637418,
10.2230007216628));
#58739=CARTESIAN_POINT('Ctrl Pts',(-9.18649518751149,-15.9437511051639,
10.0660005943105));
#58740=CARTESIAN_POINT('Ctrl Pts',(-10.8936904509082,-13.2129217420271,
9.90900046695826));
#58741=CARTESIAN_POINT('Ctrl Pts',(-9.55772959244346,-10.2825399270605,
9.75200033960601));
#58742=CARTESIAN_POINT('Ctrl Pts',(-6.37658355063268,-9.78030425210093,
9.59500021225375));
#58743=CARTESIAN_POINT('Ctrl Pts',(-4.20281546745071,-12.1565757441505,
9.43800008490151));
#58744=CARTESIAN_POINT('Ctrl Pts',(-4.9856645647421,-15.2805282036001,9.28099995754924));
#58745=CARTESIAN_POINT('Ctrl Pts',(-8.02314227712081,-16.3508838764116,
9.12399983019701));
#58746=CARTESIAN_POINT('Ctrl Pts',(-10.5915133373824,-14.4078443649032,
8.96699970284473));
#58747=CARTESIAN_POINT('Ctrl Pts',(-10.387694705577,-11.1937519405699,8.8099995754925));
#58748=CARTESIAN_POINT('Ctrl Pts',(-7.59445254015368,-9.59071406337065,
8.65299944814022));
#58749=CARTESIAN_POINT('Ctrl Pts',(-4.71651386962368,-11.0361902030079,
8.49599932078799));
#58750=CARTESIAN_POINT('Ctrl Pts',(-4.33455391893407,-14.2340080242683,
8.33899919343572));
#58751=CARTESIAN_POINT('Ctrl Pts',(-6.79107983542896,-16.3166536153767,
8.18199906608348));
#58752=CARTESIAN_POINT('Ctrl Pts',(-9.88330126539458,-15.4165986909841,
8.02499893873122));
#58753=CARTESIAN_POINT('Ctrl Pts',(-10.8383935859029,-12.340931138896,7.86799881137898));
#58754=CARTESIAN_POINT('Ctrl Pts',(-8.79991635104542,-9.84763155765228,
7.7109986840267));
#58755=CARTESIAN_POINT('Ctrl Pts',(-5.59579165327249,-10.1724656040451,
7.55399855667448));
#58756=CARTESIAN_POINT('Ctrl Pts',(-4.09918884819405,-13.0241514678338,
7.3969984293222));
#58757=CARTESIAN_POINT('Ctrl Pts',(-5.65212602885569,-15.8455550856297,
7.23999830196996));
#58758=CARTESIAN_POINT('Ctrl Pts',(-8.8620695270797,-16.1066967495653,7.0829981746177));
#58759=CARTESIAN_POINT('Ctrl Pts',(-10.8506322134124,-13.5734082564495,
6.92599804726545));
#58760=CARTESIAN_POINT('Ctrl Pts',(-9.83465084917482,-10.517313638478,6.76899791991319));
#58761=CARTESIAN_POINT('Ctrl Pts',(-6.72516567143593,-9.67884238140407,
6.61199779256095));
#58762=CARTESIAN_POINT('Ctrl Pts',(-4.31048186840692,-11.8098594647285,
6.45499766520868));
#58763=CARTESIAN_POINT('Ctrl Pts',(-4.75586957505634,-14.999461896718,6.29799753785644));
#58764=CARTESIAN_POINT('Ctrl Pts',(-7.66194535538809,-16.3875016553343,
6.14099741050417));
#58765=CARTESIAN_POINT('Ctrl Pts',(-10.4228031904426,-14.7293119763608,
5.98399728315194));
#58766=CARTESIAN_POINT('Ctrl Pts',(-10.5627553478246,-11.5118039232893,
5.82699715579966));
#58767=CARTESIAN_POINT('Ctrl Pts',(-7.95630543474677,-9.62015474206144,
5.66999702844743));
#58768=CARTESIAN_POINT('Ctrl Pts',(-4.94068199678335,-10.7506108834838,
5.51299690109516));
#58769=CARTESIAN_POINT('Ctrl Pts',(-4.22002369044277,-13.8895079343495,
5.35599677374291));
#58770=CARTESIAN_POINT('Ctrl Pts',(-6.44055136262695,-16.2221150259203,
5.19899664639066));
#58771=CARTESIAN_POINT('Ctrl Pts',(-9.61109727113964,-15.6568623145209,
5.04199651903841));
#58772=CARTESIAN_POINT('Ctrl Pts',(-10.8886010657355,-12.7004190599517,
4.88499639168614));
#58773=CARTESIAN_POINT('Ctrl Pts',(-9.12751561079228,-10.0042443043008,
4.72799626433391));
#58774=CARTESIAN_POINT('Ctrl Pts',(-5.90701771024297,-9.98526445765287,
4.57099613698164));
#58775=CARTESIAN_POINT('Ctrl Pts',(-4.11496924804734,-12.6619852293197,
4.4139960096294));
#58776=CARTESIAN_POINT('Ctrl Pts',(-5.35829758700603,-15.631254150908,4.25699588227714));
#58777=CARTESIAN_POINT('Ctrl Pts',(-8.52212705303664,-16.2362247214587,
4.09999575492489));
#58778=CARTESIAN_POINT('Ctrl Pts',(-10.7694699922944,-13.9229064764016,
3.94299562757263));
#58779=CARTESIAN_POINT('Ctrl Pts',(-10.31234789899,-11.8353429831647,3.83832887600446));
#58780=CARTESIAN_POINT('Ctrl Pts',(-9.69519710401908,-11.1135176176878,
3.78599550022038));
#58781=CARTESIAN_POINT('Ctrl Pts',(-8.19806642616111,-15.6015132427052,
12.2140044997796));
#58782=CARTESIAN_POINT('Ctrl Pts',(-9.05665968914096,-15.3719748325695,
12.1616711239955));
#58783=CARTESIAN_POINT('Ctrl Pts',(-10.5158039562152,-14.0043225620313,
12.0570043724274));
#58784=CARTESIAN_POINT('Ctrl Pts',(-10.0088832947732,-11.0289458118043,
11.9000042450751));
#58785=CARTESIAN_POINT('Ctrl Pts',(-7.24818590221332,-9.81838695213045,
11.7430041177229));
#58786=CARTESIAN_POINT('Ctrl Pts',(-4.71531822093855,-11.4492651276319,
11.5860039903706));
#58787=CARTESIAN_POINT('Ctrl Pts',(-4.67846979899401,-14.4635565391549,
11.4290038630183));
#58788=CARTESIAN_POINT('Ctrl Pts',(-7.17224139716313,-16.1560823648925,
11.2720037356661));
#58789=CARTESIAN_POINT('Ctrl Pts',(-9.95964810902439,-15.0102791451622,
11.1150036083138));
#58790=CARTESIAN_POINT('Ctrl Pts',(-10.5416023048445,-12.0530168592103,
10.9580034809616));
#58791=CARTESIAN_POINT('Ctrl Pts',(-8.39605225285175,-9.93639874276315,
10.8010033536093));
#58792=CARTESIAN_POINT('Ctrl Pts',(-5.44703946231937,-10.5582644088895,
10.6440032262571));
#58793=CARTESIAN_POINT('Ctrl Pts',(-4.3389177300236,-13.3610586997827,10.4870030989048));
#58794=CARTESIAN_POINT('Ctrl Pts',(-6.06537817248458,-15.8314493561443,
10.3300029715526));
#58795=CARTESIAN_POINT('Ctrl Pts',(-9.07827297916059,-15.7542336780869,
10.1730028442003));
#58796=CARTESIAN_POINT('Ctrl Pts',(-10.6759177126423,-13.1986413310391,
10.0160027168481));
#58797=CARTESIAN_POINT('Ctrl Pts',(-9.42568531367393,-10.4563017907707,
9.85900258949582));
#58798=CARTESIAN_POINT('Ctrl Pts',(-6.44867305906919,-9.98629452313723,
9.70200246214357));
#58799=CARTESIAN_POINT('Ctrl Pts',(-4.41439543168378,-12.2100809381968,
9.54500233479132));
#58800=CARTESIAN_POINT('Ctrl Pts',(-5.14700918959101,-15.1335697162506,
9.38800220743905));
#58801=CARTESIAN_POINT('Ctrl Pts',(-7.98957229546242,-16.1352407847476,
9.23100208008682));
#58802=CARTESIAN_POINT('Ctrl Pts',(-10.3931312708367,-14.3168859022886,
9.07400195273454));
#58803=CARTESIAN_POINT('Ctrl Pts',(-10.2023916579342,-11.3090414308585,
8.91700182538231));
#58804=CARTESIAN_POINT('Ctrl Pts',(-7.58839153117158,-9.80887031570234,
8.76000169803004));
#58805=CARTESIAN_POINT('Ctrl Pts',(-4.89512986460196,-11.1615904124476,
8.6030015706778));
#58806=CARTESIAN_POINT('Ctrl Pts',(-4.53768024140768,-14.1542046202714,
8.44600144332553));
#58807=CARTESIAN_POINT('Ctrl Pts',(-6.83657116343421,-16.103207075751,8.28900131597329));
#58808=CARTESIAN_POINT('Ctrl Pts',(-9.730365088632,-15.2609085756139,8.13200118862103));
#58809=CARTESIAN_POINT('Ctrl Pts',(-10.6241692413057,-12.3826062677939,
7.97500106126879));
#58810=CARTESIAN_POINT('Ctrl Pts',(-8.71650086357571,-10.0493014429898,
7.81800093391652));
#58811=CARTESIAN_POINT('Ctrl Pts',(-5.7179844908027,-10.3532909248038,7.66100080656428));
#58812=CARTESIAN_POINT('Ctrl Pts',(-4.31741852104351,-13.0219844243168,
7.50400067921201));
#58813=CARTESIAN_POINT('Ctrl Pts',(-5.7707038957789,-15.6623388861897,7.34700055185977));
#58814=CARTESIAN_POINT('Ctrl Pts',(-8.77466567722613,-15.9067231186349,
7.19000042450751));
#58815=CARTESIAN_POINT('Ctrl Pts',(-10.635622517451,-13.5359954659799,7.03300029715527));
#58816=CARTESIAN_POINT('Ctrl Pts',(-9.68483656420267,-10.6760100992742,
6.87600016980299));
#58817=CARTESIAN_POINT('Ctrl Pts',(-6.77488670400349,-9.89134344938279,
6.71900004245076));
#58818=CARTESIAN_POINT('Ctrl Pts',(-4.51515289168187,-11.8856134038101,
6.56199991509849));
#58819=CARTESIAN_POINT('Ctrl Pts',(-4.93196011880019,-14.8705394029777,
6.40499978774625));
#58820=CARTESIAN_POINT('Ctrl Pts',(-7.65155333996934,-16.1695088048751,
6.24799966039398));
#58821=CARTESIAN_POINT('Ctrl Pts',(-10.2352472352362,-14.6177249729221,
6.09099953304175));
#58822=CARTESIAN_POINT('Ctrl Pts',(-10.366218678266,-11.6066840532695,5.93399940568948));
#58823=CARTESIAN_POINT('Ctrl Pts',(-7.92702436581964,-9.83642178932047,
5.77699927833724));
#58824=CARTESIAN_POINT('Ctrl Pts',(-5.10491314800829,-10.8943366860512,
5.61999915098497));
#58825=CARTESIAN_POINT('Ctrl Pts',(-4.43049940492298,-13.8318110627544,
5.46299902363273));
#58826=CARTESIAN_POINT('Ctrl Pts',(-6.50853606369215,-16.0147350170509,
5.30599889628046));
#58827=CARTESIAN_POINT('Ctrl Pts',(-9.47562839437195,-15.4857545091874,
5.14899876892823));
#58828=CARTESIAN_POINT('Ctrl Pts',(-10.6711549127493,-12.7190258889931,
4.99199864157595));
#58829=CARTESIAN_POINT('Ctrl Pts',(-9.02307811531067,-10.1958643671286,
4.83499851422372));
#58830=CARTESIAN_POINT('Ctrl Pts',(-6.00923920635987,-10.1781024551261,
4.67799838687145));
#58831=CARTESIAN_POINT('Ctrl Pts',(-4.33218629439574,-12.6830583529922,
4.52099825951921));
#58832=CARTESIAN_POINT('Ctrl Pts',(-5.49573039231789,-15.4617896185815,
4.36399813216695));
#58833=CARTESIAN_POINT('Ctrl Pts',(-8.45653727388165,-16.027939294998,4.2069980048147));
#58834=CARTESIAN_POINT('Ctrl Pts',(-10.5596684670228,-13.8630664240827,
4.04999787746245));
#58835=CARTESIAN_POINT('Ctrl Pts',(-10.1318798475343,-11.9094616477065,
3.94533112589428));
#58836=CARTESIAN_POINT('Ctrl Pts',(-9.55433155034205,-11.2339557355397,
3.89299775011019));
#58837=CARTESIAN_POINT('Ctrl Pts',(-8.15019999797519,-15.4224678588016,
12.3210067496694));
#58838=CARTESIAN_POINT('Ctrl Pts',(-8.94991950449986,-15.2086689018368,
12.2686733738853));
#58839=CARTESIAN_POINT('Ctrl Pts',(-10.3090102212882,-13.934796573633,12.1640066223172));
#58840=CARTESIAN_POINT('Ctrl Pts',(-9.83684911929144,-11.1634414640457,
12.0070064949649));
#58841=CARTESIAN_POINT('Ctrl Pts',(-7.26545279971217,-10.0358906485204,
11.8500063676127));
#58842=CARTESIAN_POINT('Ctrl Pts',(-4.90626390376006,-11.5549394763523,
11.6930062402604));
#58843=CARTESIAN_POINT('Ctrl Pts',(-4.87194217881263,-14.3625408681667,
11.5360061129082));
#58844=CARTESIAN_POINT('Ctrl Pts',(-7.19471581082501,-15.9390101656796,
11.3790059855559));
#58845=CARTESIAN_POINT('Ctrl Pts',(-9.7909899911706,-14.871774694629,11.2220058582037));
#58846=CARTESIAN_POINT('Ctrl Pts',(-10.3330395766588,-12.1172919401552,
11.0650057308514));
#58847=CARTESIAN_POINT('Ctrl Pts',(-8.334609932745,-10.1458103684135,10.9080056034992));
#58848=CARTESIAN_POINT('Ctrl Pts',(-5.587811005632,-10.7250346939262,10.7510054761469));
#58849=CARTESIAN_POINT('Ctrl Pts',(-4.55567320170231,-13.3356413267153,
10.5940053487946));
#58850=CARTESIAN_POINT('Ctrl Pts',(-6.16375021862117,-15.6366372485469,
10.4370052214424));
#58851=CARTESIAN_POINT('Ctrl Pts',(-8.97005077080969,-15.5647162510099,
10.2800050940901));
#58852=CARTESIAN_POINT('Ctrl Pts',(-10.4581449743764,-13.1843609200512,
10.1230049667379));
#58853=CARTESIAN_POINT('Ctrl Pts',(-9.29364103490441,-10.6300636544808,
9.96600483938564));
#58854=CARTESIAN_POINT('Ctrl Pts',(-6.52076256750571,-10.1922847941736,
9.80900471203337));
#58855=CARTESIAN_POINT('Ctrl Pts',(-4.62597539591685,-12.2635861322432,
9.65200458468114));
#58856=CARTESIAN_POINT('Ctrl Pts',(-5.30835381443992,-14.9866112289011,
9.49500445732886));
#58857=CARTESIAN_POINT('Ctrl Pts',(-7.95600231380402,-15.9195976930836,
9.33800432997663));
#58858=CARTESIAN_POINT('Ctrl Pts',(-10.1947492042911,-14.2259274396741,
9.18100420262435));
#58859=CARTESIAN_POINT('Ctrl Pts',(-10.0170886102914,-11.424330921147,9.02400407527213));
#58860=CARTESIAN_POINT('Ctrl Pts',(-7.58233052218947,-10.0270265680341,
8.86700394791983));
#58861=CARTESIAN_POINT('Ctrl Pts',(-5.07374585958023,-11.2869906218872,
8.71000382056763));
#58862=CARTESIAN_POINT('Ctrl Pts',(-4.7408065638813,-14.0744012162745,8.55300369321533));
#58863=CARTESIAN_POINT('Ctrl Pts',(-6.88206249143947,-15.8897605361253,
8.39600356586311));
#58864=CARTESIAN_POINT('Ctrl Pts',(-9.57742891186941,-15.1052184602437,
8.23900343851083));
#58865=CARTESIAN_POINT('Ctrl Pts',(-10.4099448967086,-12.4242813966918,
8.0820033111586));
#58866=CARTESIAN_POINT('Ctrl Pts',(-8.633085376106,-10.2509713283274,7.92500318380633));
#58867=CARTESIAN_POINT('Ctrl Pts',(-5.84017732833291,-10.5341162455624,
7.7680030564541));
#58868=CARTESIAN_POINT('Ctrl Pts',(-4.53564819389297,-13.0198173807997,
7.61100292910182));
#58869=CARTESIAN_POINT('Ctrl Pts',(-5.88928176270212,-15.4791226867497,
7.45400280174959));
#58870=CARTESIAN_POINT('Ctrl Pts',(-8.68726182737255,-15.7067494877046,
7.29700267439731));
#58871=CARTESIAN_POINT('Ctrl Pts',(-10.4206128214897,-13.4985826755103,
7.14000254704508));
#58872=CARTESIAN_POINT('Ctrl Pts',(-9.53502227923051,-10.8347065600703,
6.9830024196928));
#58873=CARTESIAN_POINT('Ctrl Pts',(-6.82460773657105,-10.1038445173615,
6.82600229234058));
#58874=CARTESIAN_POINT('Ctrl Pts',(-4.71982391495681,-11.9613673428918,
6.66900216498829));
#58875=CARTESIAN_POINT('Ctrl Pts',(-5.10805066254405,-14.7416169092374,
6.51200203763607));
#58876=CARTESIAN_POINT('Ctrl Pts',(-7.64116132455058,-15.9515159544159,
6.35500191028379));
#58877=CARTESIAN_POINT('Ctrl Pts',(-10.0476912800297,-14.5061379694834,
6.19800178293156));
#58878=CARTESIAN_POINT('Ctrl Pts',(-10.1696820087074,-11.7015641832497,
6.04100165557928));
#58879=CARTESIAN_POINT('Ctrl Pts',(-7.8977432968925,-10.0526888365795,5.88400152822706));
#58880=CARTESIAN_POINT('Ctrl Pts',(-5.26914429923322,-11.0380624886186,
5.72700140087478));
#58881=CARTESIAN_POINT('Ctrl Pts',(-4.6409751194032,-13.7741141911592,5.57000127352254));
#58882=CARTESIAN_POINT('Ctrl Pts',(-6.57652076475734,-15.8073550081814,
5.41300114617028));
#58883=CARTESIAN_POINT('Ctrl Pts',(-9.34015951760427,-15.314646703854,5.25600101881803));
#58884=CARTESIAN_POINT('Ctrl Pts',(-10.4537087597631,-12.7376327180345,
5.09900089146577));
#58885=CARTESIAN_POINT('Ctrl Pts',(-8.91864061982905,-10.3874844299563,
4.94200076411353));
#58886=CARTESIAN_POINT('Ctrl Pts',(-6.11146070247677,-10.3709404525994,
4.78500063676126));
#58887=CARTESIAN_POINT('Ctrl Pts',(-4.54940334074414,-12.7041314766647,
4.62800050940902));
#58888=CARTESIAN_POINT('Ctrl Pts',(-5.63316319762975,-15.2923250862551,
4.47100038205676));
#58889=CARTESIAN_POINT('Ctrl Pts',(-8.39094749472666,-15.8196538685372,
4.31400025470451));
#58890=CARTESIAN_POINT('Ctrl Pts',(-10.3498669417512,-13.8032263717638,
4.15700012735226));
#58891=CARTESIAN_POINT('Ctrl Pts',(-9.95141179607851,-11.9835803122483,
4.05233337578409));
#58892=CARTESIAN_POINT('Ctrl Pts',(-9.41346599666503,-11.3543938533916,
4.));
#58893=CARTESIAN_POINT('Ctrl Pts',(-10.0159021674261,-12.9883695445715,
11.112583302492));
#58894=CARTESIAN_POINT('Ctrl Pts',(-10.0178571377502,-12.737164469747,11.0967241119451));
#58895=CARTESIAN_POINT('Ctrl Pts',(-9.98318366513377,-12.4864861117061,
11.0808649213983));
#58896=CARTESIAN_POINT('Ctrl Pts',(-9.90962637175846,-12.2477921372772,
11.0650057308514));
#58897=CARTESIAN_POINT('Ctrl Pts',(-9.66689636202086,-11.4601314162413,
11.0126723550673));
#58898=CARTESIAN_POINT('Ctrl Pts',(-9.00075314738293,-10.8029708923274,
10.9603389792832));
#58899=CARTESIAN_POINT('Ctrl Pts',(-8.20988171887847,-10.5709280179559,
10.9080056034991));
#58900=CARTESIAN_POINT('Ctrl Pts',(-7.419010290374,-10.3388851435844,10.8556722277151));
#58901=CARTESIAN_POINT('Ctrl Pts',(-6.503410648003,-10.5319599187553,10.803338851931));
#58902=CARTESIAN_POINT('Ctrl Pts',(-5.87358785949589,-11.0635984118056,
10.7510054761469));
#58903=CARTESIAN_POINT('Ctrl Pts',(-5.24376507098877,-11.5952369048559,
10.6986721003628));
#58904=CARTESIAN_POINT('Ctrl Pts',(-4.89971913634554,-12.4654391157856,
10.6463387245787));
#58905=CARTESIAN_POINT('Ctrl Pts',(-4.99570900517707,-13.2840395415557,
10.5940053487946));
#58906=CARTESIAN_POINT('Ctrl Pts',(-5.0916988740086,-14.1026399673258,10.5416719730106));
#58907=CARTESIAN_POINT('Ctrl Pts',(-5.62772454631489,-14.8696386079364,
10.4893385972265));
#58908=CARTESIAN_POINT('Ctrl Pts',(-6.36345414116612,-15.2411510953188,
10.4370052214424));
#58909=CARTESIAN_POINT('Ctrl Pts',(-7.09918373601734,-15.6126635827012,
10.3846718456583));
#58910=CARTESIAN_POINT('Ctrl Pts',(-8.03461725341351,-15.5886899168556,
10.3323384698742));
#58911=CARTESIAN_POINT('Ctrl Pts',(-8.75034971270605,-15.1799771954396,
10.2800050940901));
#58912=CARTESIAN_POINT('Ctrl Pts',(-9.46608217199859,-14.7712644740237,
10.2276717183061));
#58913=CARTESIAN_POINT('Ctrl Pts',(-9.96211357318751,-13.9778126970374,
10.175338342522));
#58914=CARTESIAN_POINT('Ctrl Pts',(-10.01604528387,-13.1553705976159,10.1230049667379));
#58915=CARTESIAN_POINT('Ctrl Pts',(-10.0196252693796,-13.1007769130985,
10.1195310786559));
#58916=CARTESIAN_POINT('Ctrl Pts',(-10.0212572306508,-13.0460554884989,
10.1160571905739));
#58917=CARTESIAN_POINT('Ctrl Pts',(-10.0209920718673,-12.9913179799917,
10.112583302492));
#58918=CARTESIAN_POINT('Ctrl Pts',(-8.29379928253297,-15.9596040105122,
12.));
#58919=CARTESIAN_POINT('Ctrl Pts',(-8.38688146826619,-15.9255541311756,
12.));
#58920=CARTESIAN_POINT('Ctrl Pts',(-8.47790052796864,-15.8867414890058,
12.));
#58921=CARTESIAN_POINT('Ctrl Pts',(-8.56664663605253,-15.843492548424,12.));
#58922=CARTESIAN_POINT('Ctrl Pts',(-8.65733876929825,-15.7992952448277,
12.));
#58923=CARTESIAN_POINT('Ctrl Pts',(-8.74565784480789,-15.750464336337,12.));
#58924=CARTESIAN_POINT('Ctrl Pts',(-8.83135101694567,-15.6973027457218,
12.));
#58925=CARTESIAN_POINT('Ctrl Pts',(-8.91318960012018,-15.6465324317433,
12.));
#58926=CARTESIAN_POINT('Ctrl Pts',(-8.99263343720554,-15.5918113841942,
12.));
#58927=CARTESIAN_POINT('Ctrl Pts',(-9.069430157416,-15.533374159028,12.));
#58928=CARTESIAN_POINT('Ctrl Pts',(-9.13662728760015,-15.4822415870076,
12.));
#58929=CARTESIAN_POINT('Ctrl Pts',(-9.20179743619592,-15.4282631425356,
12.));
#58930=CARTESIAN_POINT('Ctrl Pts',(-9.26474763112753,-15.3715835638146,
12.));
#58931=CARTESIAN_POINT('Ctrl Pts',(-9.27985611388604,-15.3579800723751,
12.));
#58932=CARTESIAN_POINT('Ctrl Pts',(-9.29484029179697,-15.3442173582628,
12.));
#58933=CARTESIAN_POINT('Ctrl Pts',(-9.30967505138841,-15.3303185989115,
12.));
#58934=CARTESIAN_POINT('Ctrl Pts',(-9.38210503428163,-15.26245859108,12.));
#58935=CARTESIAN_POINT('Ctrl Pts',(-9.45106917065939,-15.1912779029607,
12.));
#58936=CARTESIAN_POINT('Ctrl Pts',(-9.51632647275336,-15.1170649381822,
12.));
#58937=CARTESIAN_POINT('Ctrl Pts',(-9.58121888012541,-15.0432669448824,
12.));
#58938=CARTESIAN_POINT('Ctrl Pts',(-9.64244627908667,-14.9664696982533,
12.));
#58939=CARTESIAN_POINT('Ctrl Pts',(-9.69972810245665,-14.8869300127004,
12.));
#58940=CARTESIAN_POINT('Ctrl Pts',(-9.75408287639578,-14.81145473323,12.));
#58941=CARTESIAN_POINT('Ctrl Pts',(-9.80488505097158,-14.7335093955071,
12.));
#58942=CARTESIAN_POINT('Ctrl Pts',(-9.85185230919616,-14.6533004074739,
12.));
#58943=CARTESIAN_POINT('Ctrl Pts',(-9.8892295724543,-14.5894688666365,12.));
#58944=CARTESIAN_POINT('Ctrl Pts',(-9.92417736747258,-14.5242033609892,
12.));
#58945=CARTESIAN_POINT('Ctrl Pts',(-9.95653206305223,-14.4576058296606,
12.));
#58946=CARTESIAN_POINT('Ctrl Pts',(-9.96243497650182,-14.4454555233034,
12.));
#58947=CARTESIAN_POINT('Ctrl Pts',(-9.9682498087257,-14.4332643188572,12.));
#58948=CARTESIAN_POINT('Ctrl Pts',(-9.97397236800321,-14.4210401757467,
12.));
#58949=CARTESIAN_POINT('Ctrl Pts',(-10.014548795905,-14.3343635617469,12.));
#58950=CARTESIAN_POINT('Ctrl Pts',(-10.0505434398104,-14.2459232997935,
12.));
#58951=CARTESIAN_POINT('Ctrl Pts',(-10.0816927676552,-14.1559630239742,
12.));
#58952=CARTESIAN_POINT('Ctrl Pts',(-10.1128420955,-14.0660027481548,12.));
#58953=CARTESIAN_POINT('Ctrl Pts',(-10.1391465733587,-13.9745217251954,
12.));
#58954=CARTESIAN_POINT('Ctrl Pts',(-10.1602864633442,-13.8817537764296,
12.));
#58955=CARTESIAN_POINT('Ctrl Pts',(-10.1814515048034,-13.7888754557256,
12.));
#58956=CARTESIAN_POINT('Ctrl Pts',(-10.1974388881398,-13.6947059611701,
12.));
#58957=CARTESIAN_POINT('Ctrl Pts',(-10.2083240537505,-13.5996534977197,
12.));
#58958=CARTESIAN_POINT('Ctrl Pts',(-10.2138911337605,-13.5510401198348,
12.));
#58959=CARTESIAN_POINT('Ctrl Pts',(-10.2181228103627,-13.5021959582282,
12.));
#58960=CARTESIAN_POINT('Ctrl Pts',(-10.221024235662,-13.4531774228974,12.));
#58961=CARTESIAN_POINT('Ctrl Pts',(-10.2218608104944,-13.4390437924411,
12.));
#58962=CARTESIAN_POINT('Ctrl Pts',(-10.2225867738812,-13.4248956759012,
12.));
#58963=CARTESIAN_POINT('Ctrl Pts',(-10.2232022007112,-13.410734453067,12.));
#58964=CARTESIAN_POINT('Ctrl Pts',(-10.2238234019696,-13.3964403582763,
12.));
#58965=CARTESIAN_POINT('Ctrl Pts',(-10.2243315800161,-13.3821418174545,
12.));
#58966=CARTESIAN_POINT('Ctrl Pts',(-10.2247271750585,-13.3678432915664,
12.));
#58967=CARTESIAN_POINT('Ctrl Pts',(-10.2273082491492,-13.2745520448321,
12.));
#58968=CARTESIAN_POINT('Ctrl Pts',(-10.2251029799825,-13.1812181718667,
12.));
#58969=CARTESIAN_POINT('Ctrl Pts',(-10.2182398910409,-13.0882187710056,
12.));
#58970=CARTESIAN_POINT('Ctrl Pts',(-10.2113725866781,-12.9951622483964,
12.));
#58971=CARTESIAN_POINT('Ctrl Pts',(-10.1998413619504,-12.902439631583,12.));
#58972=CARTESIAN_POINT('Ctrl Pts',(-10.1837244231874,-12.810441427736,12.));
#58973=CARTESIAN_POINT('Ctrl Pts',(-10.1678505565058,-12.7198307203121,
12.));
#58974=CARTESIAN_POINT('Ctrl Pts',(-10.1475277985646,-12.629921903999,12.));
#58975=CARTESIAN_POINT('Ctrl Pts',(-10.1227882064871,-12.5411137713789,
12.));
#58976=CARTESIAN_POINT('Ctrl Pts',(-10.1129089207081,-12.5056499319226,
12.));
#58977=CARTESIAN_POINT('Ctrl Pts',(-10.1023248586868,-12.4703619714101,
12.));
#58978=CARTESIAN_POINT('Ctrl Pts',(-10.0910363601597,-12.435276902831,12.));
#58979=CARTESIAN_POINT('Ctrl Pts',(-10.0850884600019,-12.4167906103951,
12.));
#58980=CARTESIAN_POINT('Ctrl Pts',(-10.0789449767355,-12.398360662607,12.));
#58981=CARTESIAN_POINT('Ctrl Pts',(-10.0726058589696,-12.3799911333697,
12.));
#58982=CARTESIAN_POINT('Ctrl Pts',(-10.0672510463096,-12.3644739287129,
12.));
#58983=CARTESIAN_POINT('Ctrl Pts',(-10.0617592067699,-12.349007385008,12.));
#58984=CARTESIAN_POINT('Ctrl Pts',(-10.0561325433239,-12.3335987119335,
12.));
#58985=CARTESIAN_POINT('Ctrl Pts',(-10.0253173441252,-12.2492109864665,
12.));
#58986=CARTESIAN_POINT('Ctrl Pts',(-9.99044488561477,-12.166508346864,12.));
#58987=CARTESIAN_POINT('Ctrl Pts',(-9.95156719631022,-12.0858609769308,
12.));
#58988=CARTESIAN_POINT('Ctrl Pts',(-9.92246136851044,-12.0254842286268,
12.));
#58989=CARTESIAN_POINT('Ctrl Pts',(-9.89110980665403,-11.9662598549223,
12.));
#58990=CARTESIAN_POINT('Ctrl Pts',(-9.85752076592995,-11.9083564676894,
12.));
#58991=CARTESIAN_POINT('Ctrl Pts',(-9.84460179101728,-11.8860857391751,
12.));
#58992=CARTESIAN_POINT('Ctrl Pts',(-9.83135170784992,-11.8640105638195,
12.));
#58993=CARTESIAN_POINT('Ctrl Pts',(-9.81777057146904,-11.8421410854707,
12.));
#58994=CARTESIAN_POINT('Ctrl Pts',(-9.80600924137691,-11.8232020109641,
12.));
#58995=CARTESIAN_POINT('Ctrl Pts',(-9.79399765022805,-11.8044144459084,
12.));
#58996=CARTESIAN_POINT('Ctrl Pts',(-9.78175006557354,-11.7858062660097,
12.));
#58997=CARTESIAN_POINT('Ctrl Pts',(-9.73447815410214,-11.7139844123438,
12.));
#58998=CARTESIAN_POINT('Ctrl Pts',(-9.68365479534874,-11.6447676019631,
12.));
#58999=CARTESIAN_POINT('Ctrl Pts',(-9.62930896131935,-11.578509745124,12.));
#59000=CARTESIAN_POINT('Ctrl Pts',(-9.58717521523442,-11.5271407346737,
12.));
#59001=CARTESIAN_POINT('Ctrl Pts',(-9.54292346973057,-11.477550842089,12.));
#59002=CARTESIAN_POINT('Ctrl Pts',(-9.49655480089338,-11.4299227460007,
12.));
#59003=CARTESIAN_POINT('Ctrl Pts',(-9.47068894114788,-11.4033543392671,
12.));
#59004=CARTESIAN_POINT('Ctrl Pts',(-9.44416412664311,-11.377396721654,12.));
#59005=CARTESIAN_POINT('Ctrl Pts',(-9.41700750114215,-11.3520617378123,
12.));
#59006=CARTESIAN_POINT('Origin',(-7.50000000000001,-12.9903810567666,7.5));
#59007=CARTESIAN_POINT('Origin',(-7.5,12.9903810567666,4.));
#59008=CARTESIAN_POINT('Ctrl Pts',(-9.41346599666504,14.6263682601415,4.));
#59009=CARTESIAN_POINT('Ctrl Pts',(-9.47563132777586,14.5679481137415,4.));
#59010=CARTESIAN_POINT('Ctrl Pts',(-9.53442555802215,14.506276247837,4.));
#59011=CARTESIAN_POINT('Ctrl Pts',(-9.58983471826803,14.4417285757633,4.));
#59012=CARTESIAN_POINT('Ctrl Pts',(-9.64659435921208,14.3756076911582,4.));
#59013=CARTESIAN_POINT('Ctrl Pts',(-9.69980238305237,14.3064686172689,4.));
#59014=CARTESIAN_POINT('Ctrl Pts',(-9.7494149473681,14.2346691598829,4.));
#59015=CARTESIAN_POINT('Ctrl Pts',(-9.76242041292079,14.2158476096845,4.));
#59016=CARTESIAN_POINT('Ctrl Pts',(-9.77517863474719,14.1968430256296,4.));
#59017=CARTESIAN_POINT('Ctrl Pts',(-9.78768844229491,14.177661413676,4.));
#59018=CARTESIAN_POINT('Ctrl Pts',(-9.79776816908292,14.1622059074975,4.));
#59019=CARTESIAN_POINT('Ctrl Pts',(-9.80768698071961,14.1466346904616,4.));
#59020=CARTESIAN_POINT('Ctrl Pts',(-9.81743563533852,14.1309651390747,4.));
#59021=CARTESIAN_POINT('Ctrl Pts',(-9.86491280549081,14.0546524593777,4.));
#59022=CARTESIAN_POINT('Ctrl Pts',(-9.90840772399799,13.9759343990068,4.));
#59023=CARTESIAN_POINT('Ctrl Pts',(-9.94788354450479,13.8952025688597,4.));
#59024=CARTESIAN_POINT('Ctrl Pts',(-9.97942538424941,13.8306964885275,4.));
#59025=CARTESIAN_POINT('Ctrl Pts',(-10.0084008056984,13.7649036744675,4.));
#59026=CARTESIAN_POINT('Ctrl Pts',(-10.0347744493784,13.6980066802042,4.));
#59027=CARTESIAN_POINT('Ctrl Pts',(-10.0434535064654,13.6759921705975,4.));
#59028=CARTESIAN_POINT('Ctrl Pts',(-10.0518506786378,13.6538579807081,4.));
#59029=CARTESIAN_POINT('Ctrl Pts',(-10.0599643178554,13.6316103344208,4.));
#59030=CARTESIAN_POINT('Ctrl Pts',(-10.0673321856527,13.6114075977388,4.));
#59031=CARTESIAN_POINT('Ctrl Pts',(-10.0744676826305,13.591106675655,4.));
#59032=CARTESIAN_POINT('Ctrl Pts',(-10.0813601244641,13.5707407736482,4.));
#59033=CARTESIAN_POINT('Ctrl Pts',(-10.110937889366,13.4833439009404,4.));
#59034=CARTESIAN_POINT('Ctrl Pts',(-10.1360768470728,13.3946653712955,4.));
#59035=CARTESIAN_POINT('Ctrl Pts',(-10.1567422986514,13.3051020151044,4.));
#59036=CARTESIAN_POINT('Ctrl Pts',(-10.1777244132853,13.2141662521254,4.));
#59037=CARTESIAN_POINT('Ctrl Pts',(-10.194095376586,13.1223175335281,4.));
#59038=CARTESIAN_POINT('Ctrl Pts',(-10.205777094777,13.0299380601523,4.));
#59039=CARTESIAN_POINT('Ctrl Pts',(-10.2173678863481,12.938277637958,4.));
#59040=CARTESIAN_POINT('Ctrl Pts',(-10.2243424959595,12.8460937642312,4.));
#59041=CARTESIAN_POINT('Ctrl Pts',(-10.2265776894176,12.7537405691803,4.));
#59042=CARTESIAN_POINT('Ctrl Pts',(-10.2276571919675,12.7091379379498,4.));
#59043=CARTESIAN_POINT('Ctrl Pts',(-10.2276305022847,12.6644956114825,4.));
#59044=CARTESIAN_POINT('Ctrl Pts',(-10.226479393828,12.619852841063,4.));
#59045=CARTESIAN_POINT('Ctrl Pts',(-10.2261091350259,12.6054933090796,4.));
#59046=CARTESIAN_POINT('Ctrl Pts',(-10.2256225193086,12.5911337303501,4.));
#59047=CARTESIAN_POINT('Ctrl Pts',(-10.225018873735,12.5767754108853,4.));
#59048=CARTESIAN_POINT('Ctrl Pts',(-10.2243878291515,12.5617653783061,4.));
#59049=CARTESIAN_POINT('Ctrl Pts',(-10.2236292144324,12.5467651944381,4.));
#59050=CARTESIAN_POINT('Ctrl Pts',(-10.2227430773117,12.5317818464922,4.));
#59051=CARTESIAN_POINT('Ctrl Pts',(-10.21709364836,12.436257849471,4.));
#59052=CARTESIAN_POINT('Ctrl Pts',(-10.2062620470353,12.3413497626712,4.));
#59053=CARTESIAN_POINT('Ctrl Pts',(-10.1901757223778,12.2474518873064,4.));
#59054=CARTESIAN_POINT('Ctrl Pts',(-10.1886872627285,12.2387635634276,4.));
#59055=CARTESIAN_POINT('Ctrl Pts',(-10.1871537792193,12.2300838755081,4.));
#59056=CARTESIAN_POINT('Ctrl Pts',(-10.1855751929644,12.2214131286805,4.));
#59057=CARTESIAN_POINT('Ctrl Pts',(-10.1691864185716,12.1313940289104,4.));
#59058=CARTESIAN_POINT('Ctrl Pts',(-10.1479406949308,12.0423388878924,4.));
#59059=CARTESIAN_POINT('Ctrl Pts',(-10.1221403086027,11.9544825435439,4.));
#59060=CARTESIAN_POINT('Ctrl Pts',(-10.095748827746,11.8646133842016,4.));
#59061=CARTESIAN_POINT('Ctrl Pts',(-10.0645913960745,11.7759978814463,4.));
#59062=CARTESIAN_POINT('Ctrl Pts',(-10.0289372513566,11.6888902934565,4.));
#59063=CARTESIAN_POINT('Ctrl Pts',(-10.0090455594271,11.6402923725491,4.));
#59064=CARTESIAN_POINT('Ctrl Pts',(-9.98775327367975,11.5921639163278,4.));
#59065=CARTESIAN_POINT('Ctrl Pts',(-9.96510045219232,11.5445507349067,4.));
#59066=CARTESIAN_POINT('Ctrl Pts',(-9.95876521331174,11.5312349155799,4.));
#59067=CARTESIAN_POINT('Ctrl Pts',(-9.95232326498233,11.517959024353,4.));
#59068=CARTESIAN_POINT('Ctrl Pts',(-9.94578250287666,11.504737914807,4.));
#59069=CARTESIAN_POINT('Ctrl Pts',(-9.90302508933715,11.4183106087567,4.));
#59070=CARTESIAN_POINT('Ctrl Pts',(-9.85598190542476,11.3340799660434,4.));
#59071=CARTESIAN_POINT('Ctrl Pts',(-9.80499298346813,11.2522993127725,4.));
#59072=CARTESIAN_POINT('Ctrl Pts',(-9.75299886407878,11.1689064327755,4.));
#59073=CARTESIAN_POINT('Ctrl Pts',(-9.69690158938222,11.0880603146916,4.));
#59074=CARTESIAN_POINT('Ctrl Pts',(-9.63700679973682,11.0100365149775,4.));
#59075=CARTESIAN_POINT('Ctrl Pts',(-9.57664072131881,10.9313987763712,4.));
#59076=CARTESIAN_POINT('Ctrl Pts',(-9.5124166745289,10.855627103721,4.00000000000001));
#59077=CARTESIAN_POINT('Ctrl Pts',(-9.44459833298039,10.7830228983692,4.00000000000001));
#59078=CARTESIAN_POINT('Ctrl Pts',(-9.40866399637306,10.7445527161936,4.00000000000001));
#59079=CARTESIAN_POINT('Ctrl Pts',(-9.37171976510391,10.706972211061,4.));
#59080=CARTESIAN_POINT('Ctrl Pts',(-9.33380001260192,10.67032964942,4.));
#59081=CARTESIAN_POINT('Ctrl Pts',(-9.31851279266197,10.655557324655,4.));
#59082=CARTESIAN_POINT('Ctrl Pts',(-9.30306698875868,10.6409374727743,4.00000000000001));
#59083=CARTESIAN_POINT('Ctrl Pts',(-9.28746471547238,10.6264733925429,4.00000000000001));
#59084=CARTESIAN_POINT('Ctrl Pts',(-9.27676484992977,10.616554087142,4.00000000000001));
#59085=CARTESIAN_POINT('Ctrl Pts',(-9.265998221379,10.6067143856922,4.00000000000001));
#59086=CARTESIAN_POINT('Ctrl Pts',(-9.25516722641356,10.5969563651344,4.00000000000001));
#59087=CARTESIAN_POINT('Ctrl Pts',(-9.17938034347013,10.5286773229844,4.));
#59088=CARTESIAN_POINT('Ctrl Pts',(-9.10042408605055,10.4643755397515,4.));
#59089=CARTESIAN_POINT('Ctrl Pts',(-9.01862125042457,10.4043372079866,4.));
#59090=CARTESIAN_POINT('Ctrl Pts',(-8.9367488325877,10.344247807089,4.));
#59091=CARTESIAN_POINT('Ctrl Pts',(-8.85202442117708,10.2884282704825,4.));
#59092=CARTESIAN_POINT('Ctrl Pts',(-8.76472673601652,10.2371917535793,4.00000000000001));
#59093=CARTESIAN_POINT('Ctrl Pts',(-8.67911981959232,10.1869475780055,4.00000000000001));
#59094=CARTESIAN_POINT('Ctrl Pts',(-8.59103768625539,10.1411099279233,4.));
#59095=CARTESIAN_POINT('Ctrl Pts',(-8.50070929346997,10.1000104724858,4.));
#59096=CARTESIAN_POINT('Ctrl Pts',(-8.47449841652962,10.0880845128227,4.));
#59097=CARTESIAN_POINT('Ctrl Pts',(-8.4480982164028,10.0765577851635,4.));
#59098=CARTESIAN_POINT('Ctrl Pts',(-8.42151385798486,10.0654391093543,4.));
#59099=CARTESIAN_POINT('Ctrl Pts',(-8.38003010456224,10.0480888916659,4.));
#59100=CARTESIAN_POINT('Ctrl Pts',(-8.33809795636191,10.0317321930114,4.));
#59101=CARTESIAN_POINT('Ctrl Pts',(-8.29574920379127,10.0163624306404,4.));
#59102=CARTESIAN_POINT('Ctrl Pts',(-6.70620071746715,10.0211581030209,4.));
#59103=CARTESIAN_POINT('Ctrl Pts',(-6.61134536198573,10.0558566157721,4.));
#59104=CARTESIAN_POINT('Ctrl Pts',(-6.51853047906358,10.0955386450798,4.));
#59105=CARTESIAN_POINT('Ctrl Pts',(-6.42799833026157,10.1398859077314,4.));
#59106=CARTESIAN_POINT('Ctrl Pts',(-6.33621672682966,10.1848452169695,4.));
#59107=CARTESIAN_POINT('Ctrl Pts',(-6.24678063208038,10.2346001195317,4.));
#59108=CARTESIAN_POINT('Ctrl Pts',(-6.15997649545542,10.288859611306,4.));
#59109=CARTESIAN_POINT('Ctrl Pts',(-6.13531542249315,10.3042747440124,4.));
#59110=CARTESIAN_POINT('Ctrl Pts',(-6.11086702515844,10.3200536672633,4.));
#59111=CARTESIAN_POINT('Ctrl Pts',(-6.0866384800126,10.3361901726906,4.));
#59112=CARTESIAN_POINT('Ctrl Pts',(-6.06744058816026,10.3489762019054,4.));
#59113=CARTESIAN_POINT('Ctrl Pts',(-6.04837875428141,10.3619882719582,4.));
#59114=CARTESIAN_POINT('Ctrl Pts',(-6.0294755109822,10.37520976247,4.));
#59115=CARTESIAN_POINT('Ctrl Pts',(-5.9467711696009,10.43305563831,4.));
#59116=CARTESIAN_POINT('Ctrl Pts',(-5.86702033335456,10.4949586291912,4.));
#59117=CARTESIAN_POINT('Ctrl Pts',(-5.79049045427403,10.5606238082624,4.));
#59118=CARTESIAN_POINT('Ctrl Pts',(-5.73202499106291,10.6107891183003,4.));
#59119=CARTESIAN_POINT('Ctrl Pts',(-5.67544001899664,10.6631510546145,4.));
#59120=CARTESIAN_POINT('Ctrl Pts',(-5.62087181378523,10.7175895430331,4.));
#59121=CARTESIAN_POINT('Ctrl Pts',(-5.59237441395403,10.7460192002787,4.));
#59122=CARTESIAN_POINT('Ctrl Pts',(-5.56442730562685,10.7750153331146,4.));
#59123=CARTESIAN_POINT('Ctrl Pts',(-5.53705172637329,10.8045615976092,4.));
#59124=CARTESIAN_POINT('Ctrl Pts',(-5.52590399611565,10.8165932621689,4.));
#59125=CARTESIAN_POINT('Ctrl Pts',(-5.51485083286264,10.828716515658,4.));
#59126=CARTESIAN_POINT('Ctrl Pts',(-5.50390377375039,10.8409187451704,4.));
#59127=CARTESIAN_POINT('Ctrl Pts',(-5.43813900242605,10.9142239886428,4.));
#59128=CARTESIAN_POINT('Ctrl Pts',(-5.37610793089156,10.9904753850308,4.));
#59129=CARTESIAN_POINT('Ctrl Pts',(-5.31805547404601,11.0693968127291,4.));
#59130=CARTESIAN_POINT('Ctrl Pts',(-5.26107067938322,11.14686677001,4.));
#59131=CARTESIAN_POINT('Ctrl Pts',(-5.20791915062963,11.2269102402285,4.));
#59132=CARTESIAN_POINT('Ctrl Pts',(-5.15887680160751,11.3092877421736,4.));
#59133=CARTESIAN_POINT('Ctrl Pts',(-5.11076852001942,11.390096270703,4.));
#59134=CARTESIAN_POINT('Ctrl Pts',(-5.0666140967032,11.4731514387505,4.));
#59135=CARTESIAN_POINT('Ctrl Pts',(-5.0267215928916,11.558237595229,4.));
#59136=CARTESIAN_POINT('Ctrl Pts',(-5.00642757575884,11.6015224169963,4.));
#59137=CARTESIAN_POINT('Ctrl Pts',(-4.98723731004213,11.6453329516309,4.));
#59138=CARTESIAN_POINT('Ctrl Pts',(-4.96919657902753,11.6896410472644,4.));
#59139=CARTESIAN_POINT('Ctrl Pts',(-4.96034359773442,11.7113839988919,4.));
#59140=CARTESIAN_POINT('Ctrl Pts',(-4.95176748954608,11.7332467663051,4.));
#59141=CARTESIAN_POINT('Ctrl Pts',(-4.94347399674913,11.7552260059165,4.));
#59142=CARTESIAN_POINT('Ctrl Pts',(-4.93874124380541,11.7677686479032,4.));
#59143=CARTESIAN_POINT('Ctrl Pts',(-4.93410183231377,11.780345881655,4.));
#59144=CARTESIAN_POINT('Ctrl Pts',(-4.92955939125163,11.7929492290495,4.));
#59145=CARTESIAN_POINT('Ctrl Pts',(-4.89805310423436,11.8803658129868,4.));
#59146=CARTESIAN_POINT('Ctrl Pts',(-4.87116553516298,11.9691490179121,4.));
#59147=CARTESIAN_POINT('Ctrl Pts',(-4.84914983533523,12.059077444786,4.));
#59148=CARTESIAN_POINT('Ctrl Pts',(-4.84589756836606,12.0723621123006,4.));
#59149=CARTESIAN_POINT('Ctrl Pts',(-4.84275170968814,12.0856717889067,4.));
#59150=CARTESIAN_POINT('Ctrl Pts',(-4.83971317200452,12.0990057760668,4.));
#59151=CARTESIAN_POINT('Ctrl Pts',(-4.81880138299547,12.1907727887468,4.));
#59152=CARTESIAN_POINT('Ctrl Pts',(-4.80296850182884,12.2836914928978,4.));
#59153=CARTESIAN_POINT('Ctrl Pts',(-4.792106149773,12.377370023065,4.));
#59154=CARTESIAN_POINT('Ctrl Pts',(-4.78082380016171,12.4746706742486,4.));
#59155=CARTESIAN_POINT('Ctrl Pts',(-4.77490383217972,12.5727922441963,4.));
#59156=CARTESIAN_POINT('Ctrl Pts',(-4.77428144864228,12.6712822681824,4.));
#59157=CARTESIAN_POINT('Ctrl Pts',(-4.77410039443767,12.6999334645636,4.));
#59158=CARTESIAN_POINT('Ctrl Pts',(-4.77436800145517,12.72861569198,4.));
#59159=CARTESIAN_POINT('Ctrl Pts',(-4.77508351480076,12.7573173782009,4.));
#59160=CARTESIAN_POINT('Ctrl Pts',(-4.77547910205812,12.7731857353794,4.));
#59161=CARTESIAN_POINT('Ctrl Pts',(-4.77601160613275,12.7890600363428,4.));
#59162=CARTESIAN_POINT('Ctrl Pts',(-4.77668094646708,12.8049382921795,4.));
#59163=CARTESIAN_POINT('Ctrl Pts',(-4.77726157393708,12.8187120796562,4.));
#59164=CARTESIAN_POINT('Ctrl Pts',(-4.77794517105296,12.8324874411773,4.));
#59165=CARTESIAN_POINT('Ctrl Pts',(-4.77873077105928,12.846250960695,4.));
#59166=CARTESIAN_POINT('Ctrl Pts',(-4.7840331030193,12.9391465167459,4.));
#59167=CARTESIAN_POINT('Ctrl Pts',(-4.79398369008647,13.0316542436184,4.));
#59168=CARTESIAN_POINT('Ctrl Pts',(-4.80846381204201,13.1234011743035,4.));
#59169=CARTESIAN_POINT('Ctrl Pts',(-4.82290319752883,13.2148899962528,4.));
#59170=CARTESIAN_POINT('Ctrl Pts',(-4.84184707271793,13.3056232412176,4.));
#59171=CARTESIAN_POINT('Ctrl Pts',(-4.86522626081521,13.3952139858104,4.));
#59172=CARTESIAN_POINT('Ctrl Pts',(-4.88820180858057,13.4832579513734,4.));
#59173=CARTESIAN_POINT('Ctrl Pts',(-4.91546130118121,13.5701993091168,4.));
#59174=CARTESIAN_POINT('Ctrl Pts',(-4.94697947428434,13.6556416339958,4.));
#59175=CARTESIAN_POINT('Ctrl Pts',(-4.9623719301486,13.6973689006853,4.));
#59176=CARTESIAN_POINT('Ctrl Pts',(-4.97878066818245,13.7387381251278,4.));
#59177=CARTESIAN_POINT('Ctrl Pts',(-4.99620585058615,13.779699693788,4.));
#59178=CARTESIAN_POINT('Ctrl Pts',(-5.00196797407456,13.7932447810892,4.));
#59179=CARTESIAN_POINT('Ctrl Pts',(-5.00784125922211,13.8067452713773,4.));
#59180=CARTESIAN_POINT('Ctrl Pts',(-5.01382575727085,13.8201993070928,4.));
#59181=CARTESIAN_POINT('Ctrl Pts',(-5.01951346999181,13.8329861255467,4.));
#59182=CARTESIAN_POINT('Ctrl Pts',(-5.02529821878992,13.8457232464252,4.));
#59183=CARTESIAN_POINT('Ctrl Pts',(-5.03117811610162,13.8584059204054,4.));
#59184=CARTESIAN_POINT('Ctrl Pts',(-5.06862984407309,13.9391876127847,4.));
#59185=CARTESIAN_POINT('Ctrl Pts',(-5.10995846184345,14.0178080548726,4.));
#59186=CARTESIAN_POINT('Ctrl Pts',(-5.15509821873846,14.0939187469392,4.));
#59187=CARTESIAN_POINT('Ctrl Pts',(-5.19948177774165,14.1687544045606,4.));
#59188=CARTESIAN_POINT('Ctrl Pts',(-5.24755030145435,14.2411643668113,4.));
#59189=CARTESIAN_POINT('Ctrl Pts',(-5.299277628138,14.3107831411822,4.));
#59190=CARTESIAN_POINT('Ctrl Pts',(-5.34947359960038,14.37834089519,4.));
#59191=CARTESIAN_POINT('Ctrl Pts',(-5.40311538240653,14.4432707274223,4.));
#59192=CARTESIAN_POINT('Ctrl Pts',(-5.46020707398797,14.5051981890779,4.));
#59193=CARTESIAN_POINT('Ctrl Pts',(-5.47440626361873,14.5206000758857,4.));
#59194=CARTESIAN_POINT('Ctrl Pts',(-5.48881897228929,14.5358160294758,4.));
#59195=CARTESIAN_POINT('Ctrl Pts',(-5.50344549658044,14.5508398362218,4.));
#59196=CARTESIAN_POINT('Ctrl Pts',(-5.52930175835117,14.5773984001217,4.));
#59197=CARTESIAN_POINT('Ctrl Pts',(-5.55582619547196,14.603356583853,4.));
#59198=CARTESIAN_POINT('Ctrl Pts',(-5.58299280741585,14.6287008947316,4.));
#59199=CARTESIAN_POINT('Origin',(-7.5,12.9903810567666,14.2084234471775));
#59200=CARTESIAN_POINT('Ctrl Pts',(-10.5771718362758,12.9919049495641,11.7084234471775));
#59201=CARTESIAN_POINT('Ctrl Pts',(-10.5778105116372,13.0907937922778,11.7032843782051));
#59202=CARTESIAN_POINT('Ctrl Pts',(-10.5289894981275,14.1961054493059,11.6458119334487));
#59203=CARTESIAN_POINT('Ctrl Pts',(-9.19520332408216,16.188335839362,11.5360061129082));
#59204=CARTESIAN_POINT('Ctrl Pts',(-5.76804722455709,16.1681372027015,11.3790059855559));
#59205=CARTESIAN_POINT('Ctrl Pts',(-3.89395310615829,13.2989500353867,11.2220058582037));
#59206=CARTESIAN_POINT('Ctrl Pts',(-5.25343413560966,10.1527921984098,11.0650057308514));
#59207=CARTESIAN_POINT('Ctrl Pts',(-8.62743319586002,9.55126751773617,10.9080056034992));
#59208=CARTESIAN_POINT('Ctrl Pts',(-10.416413733365,11.4305453719444,10.7891448422745));
#59209=CARTESIAN_POINT('Ctrl Pts',(-10.5747253393417,12.713490324996,10.7226174568339));
#59210=CARTESIAN_POINT('Ctrl Pts',(-10.5724150045772,12.9877735244422,10.7084234471775));
#59211=CARTESIAN_POINT('Ctrl Pts',(-10.5702206634037,12.9870745539208,11.7915765528226));
#59212=CARTESIAN_POINT('Ctrl Pts',(-10.5655505963514,13.6681072977096,11.7563842836469));
#59213=CARTESIAN_POINT('Ctrl Pts',(-10.0102057878341,15.3711021382601,11.6688586386871));
#59214=CARTESIAN_POINT('Ctrl Pts',(-7.21365218567195,16.5973810760335,11.5289996179432));
#59215=CARTESIAN_POINT('Ctrl Pts',(-4.33342713054201,14.7428462583649,11.371999490591));
#59216=CARTESIAN_POINT('Ctrl Pts',(-4.29152522806557,11.3151739482887,11.2149993632387));
#59217=CARTESIAN_POINT('Ctrl Pts',(-7.12729264284838,9.39053585671186,11.0579992358865));
#59218=CARTESIAN_POINT('Ctrl Pts',(-9.97678331927841,10.5618592714599,10.9168582990811));
#59219=CARTESIAN_POINT('Ctrl Pts',(-10.5660598502819,12.2874997426315,10.8280507380598));
#59220=CARTESIAN_POINT('Ctrl Pts',(-10.5715490487462,12.9928368154298,10.7915765528225));
#59221=CARTESIAN_POINT('Ctrl Pts',(-5.58653400333492,14.6263682601415,12.));
#59222=CARTESIAN_POINT('Ctrl Pts',(-5.04858820392146,13.9971818012847,11.9476666242159));
#59223=CARTESIAN_POINT('Ctrl Pts',(-4.6501298356162,12.1775391083675,11.8429998726477));
#59224=CARTESIAN_POINT('Ctrl Pts',(-6.60905434274384,10.1611067275626,11.6859997452955));
#59225=CARTESIAN_POINT('Ctrl Pts',(-9.36683572422696,10.6884384302024,11.5289996179432));
#59226=CARTESIAN_POINT('Ctrl Pts',(-10.4505967777648,13.2766298839747,11.371999490591));
#59227=CARTESIAN_POINT('Ctrl Pts',(-8.88853891927017,15.609821813293,11.2149993632387));
#59228=CARTESIAN_POINT('Ctrl Pts',(-6.0813596511542,15.5932771353061,11.0579992358865));
#59229=CARTESIAN_POINT('Ctrl Pts',(-4.5462915063457,13.2431295206274,10.9009991085342));
#59230=CARTESIAN_POINT('Ctrl Pts',(-5.65984071462414,10.666115577374,10.743998981182));
#59231=CARTESIAN_POINT('Ctrl Pts',(-8.42347911845702,10.1734074649302,10.5869988538297));
#59232=CARTESIAN_POINT('Ctrl Pts',(-10.3590245740303,12.2066479805288,10.4299987264775));
#59233=CARTESIAN_POINT('Ctrl Pts',(-9.73085545152254,14.9426994258741,10.2729985991252));
#59234=CARTESIAN_POINT('Ctrl Pts',(-7.10225674886102,15.9280729453192,10.115998471773));
#59235=CARTESIAN_POINT('Ctrl Pts',(-4.8303182837872,14.2791977933351,9.9589983444207));
#59236=CARTESIAN_POINT('Ctrl Pts',(-4.95230900060974,11.4746243081013,9.80199821706846));
#59237=CARTESIAN_POINT('Ctrl Pts',(-7.35883869070172,10.0292464861065,9.64499808971619));
#59238=CARTESIAN_POINT('Ctrl Pts',(-9.89194907460283,11.2391453960705,9.48799796236395));
#59239=CARTESIAN_POINT('Ctrl Pts',(-10.2801757792987,14.0193946579201,9.33099783501168));
#59240=CARTESIAN_POINT('Ctrl Pts',(-8.17539218920641,15.8769172785782,9.17399770765945));
#59241=CARTESIAN_POINT('Ctrl Pts',(-5.46497794449781,15.1460553165716,9.01699758030717));
#59242=CARTESIAN_POINT('Ctrl Pts',(-4.57938749963505,12.4821794938336,8.85999745295494));
#59243=CARTESIAN_POINT('Ctrl Pts',(-6.31273830315983,10.2740129245224,8.70299732560267));
#59244=CARTESIAN_POINT('Ctrl Pts',(-9.11071806020523,10.501639700397,8.54599719825042));
#59245=CARTESIAN_POINT('Ctrl Pts',(-10.4643514801813,12.96094473598,8.38899707089817));
#59246=CARTESIAN_POINT('Ctrl Pts',(-9.15982248917363,15.4466455979041,8.23199694354592));
#59247=CARTESIAN_POINT('Ctrl Pts',(-6.36691474847379,15.7297904840163,8.07499681619367));
#59248=CARTESIAN_POINT('Ctrl Pts',(-4.59005542323444,13.5564806545976,7.91799668884141));
#59249=CARTESIAN_POINT('Ctrl Pts',(-5.42257131653894,10.8755438858135,7.76099656148916));
#59250=CARTESIAN_POINT('Ctrl Pts',(-8.11793744062105,10.0910018961859,7.6039964341369));
#59251=CARTESIAN_POINT('Ctrl Pts',(-10.2591931327486,11.9063610164495,7.44699630678465));
#59252=CARTESIAN_POINT('Ctrl Pts',(-9.92625387366264,14.6937713043528,7.2899961794324));
#59253=CARTESIAN_POINT('Ctrl Pts',(-7.41766948685395,15.953735219701,7.13299605208014));
#59254=CARTESIAN_POINT('Ctrl Pts',(-4.98291166647307,14.5564310201707,6.97599592472789));
#59255=CARTESIAN_POINT('Ctrl Pts',(-4.80525109196198,11.7548348097635,6.81899579737564));
#59256=CARTESIAN_POINT('Ctrl Pts',(-7.04399773638617,10.061164742401,6.66199567002339));
#59257=CARTESIAN_POINT('Ctrl Pts',(-9.69164594449512,10.9941511043189,6.50499554267113));
#59258=CARTESIAN_POINT('Ctrl Pts',(-10.3740242882686,13.7171759009976,6.34799541531889));
#59259=CARTESIAN_POINT('Ctrl Pts',(-8.47923732450549,15.7884770124268,6.19099528796661));
#59260=CARTESIAN_POINT('Ctrl Pts',(-5.70635916288519,15.3506981982192,6.03399516061438));
#59261=CARTESIAN_POINT('Ctrl Pts',(-4.54185534982472,12.7964012172524,5.87699503326211));
#59262=CARTESIAN_POINT('Ctrl Pts',(-6.02994939266268,10.4160461410637,5.71999490590986));
#59263=CARTESIAN_POINT('Ctrl Pts',(-8.83624963123305,10.3441251642037,5.56299477855761));
#59264=CARTESIAN_POINT('Ctrl Pts',(-10.4443264801503,12.6451208096654,5.40599465120535));
#59265=CARTESIAN_POINT('Ctrl Pts',(-9.41218877466708,15.2557271980297,5.24899452385311));
#59266=CARTESIAN_POINT('Ctrl Pts',(-6.66539017469168,15.834951382638,5.09199439650085));
#59267=CARTESIAN_POINT('Ctrl Pts',(-4.66696070971034,13.863470166724,4.9349942691486));
#59268=CARTESIAN_POINT('Ctrl Pts',(-5.20901029900842,11.1089874665202,4.77799414179634));
#59269=CARTESIAN_POINT('Ctrl Pts',(-7.8052841019297,10.0417525531808,4.62099401444409));
#59270=CARTESIAN_POINT('Ctrl Pts',(-10.128057595771,11.6182209055488,4.46399388709184));
#59271=CARTESIAN_POINT('Ctrl Pts',(-10.093735767433,14.4258233247707,4.30699375973958));
#59272=CARTESIAN_POINT('Ctrl Pts',(-7.73454710646218,15.9448696981551,4.14999363238733));
#59273=CARTESIAN_POINT('Ctrl Pts',(-5.16315153543426,14.8173229408266,3.99299350503507));
#59274=CARTESIAN_POINT('Ctrl Pts',(-4.69098902991507,12.045960940047,3.83599337768282));
#59275=CARTESIAN_POINT('Ctrl Pts',(-6.05008049550023,10.7720932116963,3.73132662611465));
#59276=CARTESIAN_POINT('Ctrl Pts',(-6.84980000202491,10.5582942547315,3.67899325033057));
#59277=CARTESIAN_POINT('Ctrl Pts',(-5.44566844965789,14.7468063779934,12.1070022498898));
#59278=CARTESIAN_POINT('Ctrl Pts',(-4.86812015246569,14.0713004658265,12.0546688741057));
#59279=CARTESIAN_POINT('Ctrl Pts',(-4.44032807310083,12.1176993038908,11.9500021225376));
#59280=CARTESIAN_POINT('Ctrl Pts',(-6.54346469885977,9.95282118939152,11.7930019951853));
#59281=CARTESIAN_POINT('Ctrl Pts',(-9.50426845016806,10.5189740011564,11.6360018678331));
#59282=CARTESIAN_POINT('Ctrl Pts',(-10.6678138328376,13.2977029522207,11.4790017404808));
#59283=CARTESIAN_POINT('Ctrl Pts',(-8.99076038754082,15.8026598219827,11.3220016131285));
#59284=CARTESIAN_POINT('Ctrl Pts',(-5.97692217562184,15.7848971577712,11.1650014857763));
#59285=CARTESIAN_POINT('Ctrl Pts',(-4.32884537294989,13.2617363588805,11.008001358424));
#59286=CARTESIAN_POINT('Ctrl Pts',(-5.52437185495265,10.4950077843859,10.8510012310718));
#59287=CARTESIAN_POINT('Ctrl Pts',(-8.49146381092469,9.96602748253219,10.6940011037195));
#59288=CARTESIAN_POINT('Ctrl Pts',(-10.5695002659417,12.1489511132149,10.5370009763673));
#59289=CARTESIAN_POINT('Ctrl Pts',(-9.89508658439861,15.0864252137885,10.380000849015));
#59290=CARTESIAN_POINT('Ctrl Pts',(-7.07297568330216,16.144339968164,10.2230007216628));
#59291=CARTESIAN_POINT('Ctrl Pts',(-4.63378163576147,14.3740779132334,10.0660005943105));
#59292=CARTESIAN_POINT('Ctrl Pts',(-4.76475306606344,11.3630373167398,9.90900046695826));
#59293=CARTESIAN_POINT('Ctrl Pts',(-7.34844667640581,9.81125365971957,9.75200033960601));
#59294=CARTESIAN_POINT('Ctrl Pts',(-10.068039598996,11.1102229164483,9.59500021225375));
#59295=CARTESIAN_POINT('Ctrl Pts',(-10.4848467800654,14.0951485887035,9.43800008490151));
#59296=CARTESIAN_POINT('Ctrl Pts',(-8.22511321630987,16.0894183231763,9.28099995754925));
#59297=CARTESIAN_POINT('Ctrl Pts',(-5.31516367599608,15.3047517599283,9.12399983019699));
#59298=CARTESIAN_POINT('Ctrl Pts',(-4.36437782731425,12.4447667074727,8.96699970284474));
#59299=CARTESIAN_POINT('Ctrl Pts',(-6.22533446291578,10.0740393155813,8.80999957549249));
#59300=CARTESIAN_POINT('Ctrl Pts',(-9.22929591409124,10.3184235210999,8.65299944814023));
#59301=CARTESIAN_POINT('Ctrl Pts',(-10.6825811290368,12.9587776927019,8.49599932078798));
#59302=CARTESIAN_POINT('Ctrl Pts',(-9.28201531326903,15.6274708987809,8.33899919343573));
#59303=CARTESIAN_POINT('Ctrl Pts',(-6.2834992701754,15.9314603471809,8.18199906608347));
#59304=CARTESIAN_POINT('Ctrl Pts',(-4.37583110219086,13.5981557789132,8.02499893873123));
#59305=CARTESIAN_POINT('Ctrl Pts',(-5.26963515659132,10.7198537875612,7.86799881137897));
#59306=CARTESIAN_POINT('Ctrl Pts',(-8.16342876362473,9.87755538002796,7.71099868402671));
#59307=CARTESIAN_POINT('Ctrl Pts',(-10.4623194328887,11.8265576212272,7.55399855667447));
#59308=CARTESIAN_POINT('Ctrl Pts',(-10.1048698490028,14.8191715000043,7.39699842932221));
#59309=CARTESIAN_POINT('Ctrl Pts',(-7.4116084785376,16.1718914480481,7.23999830196995));
#59310=CARTESIAN_POINT('Ctrl Pts',(-4.79760863920515,14.6717204977811,7.0829981746177));
#59311=CARTESIAN_POINT('Ctrl Pts',(-4.60686904722592,11.6638763571539,6.92599804726545));
#59312=CARTESIAN_POINT('Ctrl Pts',(-7.01042775842265,9.84552167443846,6.7689979199132));
#59313=CARTESIAN_POINT('Ctrl Pts',(-9.85299055159733,10.8471926331423,6.61199779256093));
#59314=CARTESIAN_POINT('Ctrl Pts',(-10.585604229252,13.770681089133,6.4549976652087));
#59315=CARTESIAN_POINT('Ctrl Pts',(-8.55132682499211,15.9944672608673,6.29799753785643));
#59316=CARTESIAN_POINT('Ctrl Pts',(-5.57431489867653,15.5244600427274,6.14099741050419));
#59317=CARTESIAN_POINT('Ctrl Pts',(-4.32408263542585,12.7821208080144,5.98399728315193));
#59318=CARTESIAN_POINT('Ctrl Pts',(-5.92172719634629,10.2265287344922,5.82699715579967));
#59319=CARTESIAN_POINT('Ctrl Pts',(-8.93462166631621,10.149313078634,5.66999702844742));
#59320=CARTESIAN_POINT('Ctrl Pts',(-10.6610819284076,12.61970343828,5.51299690109516));
#59321=CARTESIAN_POINT('Ctrl Pts',(-9.55296030180576,15.4224974667542,5.35599677374291));
#59322=CARTESIAN_POINT('Ctrl Pts',(-6.60394786249421,16.0443629816032,5.19899664639066));
#59323=CARTESIAN_POINT('Ctrl Pts',(-4.45839800260659,13.927745247179,5.04199651903841));
#59324=CARTESIAN_POINT('Ctrl Pts',(-5.04035220251703,10.9704830194925,4.88499639168615));
#59325=CARTESIAN_POINT('Ctrl Pts',(-7.82775850916875,9.82468039853088,4.7279962643339));
#59326=CARTESIAN_POINT('Ctrl Pts',(-10.3215299589949,11.5172052095439,4.57099613698165));
#59327=CARTESIAN_POINT('Ctrl Pts',(-10.2846814260484,14.53149772411,4.41399600962939));
#59328=CARTESIAN_POINT('Ctrl Pts',(-7.75181399705376,16.1623732644724,4.25699588227714));
#59329=CARTESIAN_POINT('Ctrl Pts',(-4.99111740815211,14.9518187617518,4.09999575492489));
#59330=CARTESIAN_POINT('Ctrl Pts',(-4.48419523986314,11.9764346130167,3.94299562757263));
#59331=CARTESIAN_POINT('Ctrl Pts',(-5.94334031085913,10.6087872809636,3.83832887600446));
#59332=CARTESIAN_POINT('Ctrl Pts',(-6.80193357383899,10.379248870828,3.78599550022038));
#59333=CARTESIAN_POINT('Ctrl Pts',(-5.30480289598085,14.8672444958453,12.2140044997796));
#59334=CARTESIAN_POINT('Ctrl Pts',(-4.68765210100993,14.1454191303684,12.1616711239955));
#59335=CARTESIAN_POINT('Ctrl Pts',(-4.23052631058544,12.0578594994142,12.0570043724274));
#59336=CARTESIAN_POINT('Ctrl Pts',(-6.47787505497571,9.74453565122039,11.9000042450751));
#59337=CARTESIAN_POINT('Ctrl Pts',(-9.64170117610916,10.3495095721105,11.7430041177229));
#59338=CARTESIAN_POINT('Ctrl Pts',(-10.8850308879103,13.3187760204667,11.5860039903706));
#59339=CARTESIAN_POINT('Ctrl Pts',(-9.09298185581149,15.9954978306723,11.4290038630184));
#59340=CARTESIAN_POINT('Ctrl Pts',(-5.87248470008946,15.9765171802363,11.2720037356661));
#59341=CARTESIAN_POINT('Ctrl Pts',(-4.11139923955409,13.2803431971336,11.1150036083138));
#59342=CARTESIAN_POINT('Ctrl Pts',(-5.38890299528115,10.3238999913978,10.9580034809616));
#59343=CARTESIAN_POINT('Ctrl Pts',(-8.55944850339236,9.75864750013418,10.8010033536093));
#59344=CARTESIAN_POINT('Ctrl Pts',(-10.7799759578531,12.091254245901,10.6440032262571));
#59345=CARTESIAN_POINT('Ctrl Pts',(-10.0593177172747,15.230151001703,10.4870030989048));
#59346=CARTESIAN_POINT('Ctrl Pts',(-7.04369461774331,16.3606069910088,10.3300029715526));
#59347=CARTESIAN_POINT('Ctrl Pts',(-4.43724498773573,14.4689580331317,10.1730028442003));
#59348=CARTESIAN_POINT('Ctrl Pts',(-4.57719713151714,11.2514503253782,10.0160027168481));
#59349=CARTESIAN_POINT('Ctrl Pts',(-7.33805466210989,9.59326083333269,9.85900258949581));
#59350=CARTESIAN_POINT('Ctrl Pts',(-10.2441301233891,10.9813004368261,9.70200246214358));
#59351=CARTESIAN_POINT('Ctrl Pts',(-10.689517780832,14.1709025194869,9.5450023347913));
#59352=CARTESIAN_POINT('Ctrl Pts',(-8.27483424341331,16.3019193677744,9.38800220743907));
#59353=CARTESIAN_POINT('Ctrl Pts',(-5.16534940749437,15.463448203285,9.2310020800868));
#59354=CARTESIAN_POINT('Ctrl Pts',(-4.14936815499344,12.4073539211118,9.07400195273456));
#59355=CARTESIAN_POINT('Ctrl Pts',(-6.13793062267174,9.87406570664018,8.9170018253823));
#59356=CARTESIAN_POINT('Ctrl Pts',(-9.34787376797726,10.1352073418028,8.76000169803005));
#59357=CARTESIAN_POINT('Ctrl Pts',(-10.9008107778922,12.9566106494239,8.6030015706778));
#59358=CARTESIAN_POINT('Ctrl Pts',(-9.40420813736444,15.8082961996578,8.44600144332554));
#59359=CARTESIAN_POINT('Ctrl Pts',(-6.20008379187702,16.1331302103455,8.28900131597328));
#59360=CARTESIAN_POINT('Ctrl Pts',(-4.16160678114728,13.6398309032289,8.13200118862104));
#59361=CARTESIAN_POINT('Ctrl Pts',(-5.1166989966437,10.564163689309,7.97500106126877));
#59362=CARTESIAN_POINT('Ctrl Pts',(-8.20892008662842,9.66410886387002,7.81800093391653));
#59363=CARTESIAN_POINT('Ctrl Pts',(-10.6654457330288,11.7467542260049,7.66100080656427));
#59364=CARTESIAN_POINT('Ctrl Pts',(-10.2834858243429,14.9445716956558,7.50400067921202));
#59365=CARTESIAN_POINT('Ctrl Pts',(-7.40554747022126,16.3900476763952,7.34700055185976));
#59366=CARTESIAN_POINT('Ctrl Pts',(-4.61230561193723,14.7870099753915,7.19000042450751));
#59367=CARTESIAN_POINT('Ctrl Pts',(-4.40848700248986,11.5729179045444,7.03300029715526));
#59368=CARTESIAN_POINT('Ctrl Pts',(-6.97685778045915,9.6298786064759,6.876000169803));
#59369=CARTESIAN_POINT('Ctrl Pts',(-10.0143351586995,10.7002341619658,6.71900004245076));
#59370=CARTESIAN_POINT('Ctrl Pts',(-10.7971841702354,13.8241862772684,6.5619999150985));
#59371=CARTESIAN_POINT('Ctrl Pts',(-8.62341632547871,16.2004575093079,6.40499978774625));
#59372=CARTESIAN_POINT('Ctrl Pts',(-5.44227063446788,15.6982218872355,6.24799966039399));
#59373=CARTESIAN_POINT('Ctrl Pts',(-4.10630992102698,12.7678403987764,6.09099953304174));
#59374=CARTESIAN_POINT('Ctrl Pts',(-5.81350500002991,10.0370113279208,5.93399940568948));
#59375=CARTESIAN_POINT('Ctrl Pts',(-9.03299370139936,9.95450099306433,5.77699927833723));
#59376=CARTESIAN_POINT('Ctrl Pts',(-10.877837376665,12.5942860668946,5.61999915098498));
#59377=CARTESIAN_POINT('Ctrl Pts',(-9.69373182894443,15.5892677354788,5.46299902363273));
#59378=CARTESIAN_POINT('Ctrl Pts',(-6.54250555029675,16.2537745805684,5.30599889628047));
#59379=CARTESIAN_POINT('Ctrl Pts',(-4.24983529550283,13.9920203276339,5.14899876892821));
#59380=CARTESIAN_POINT('Ctrl Pts',(-4.87169410602564,10.8319785724647,4.99199864157597));
#59381=CARTESIAN_POINT('Ctrl Pts',(-7.85023291640778,9.60760824388092,4.83499851422371));
#59382=CARTESIAN_POINT('Ctrl Pts',(-10.5150023222189,11.416189513539,4.67799838687146));
#59383=CARTESIAN_POINT('Ctrl Pts',(-10.4756270846638,14.6371721234493,4.52099825951921));
#59384=CARTESIAN_POINT('Ctrl Pts',(-7.76908088764536,16.3798768307898,4.36399813216695));
#59385=CARTESIAN_POINT('Ctrl Pts',(-4.81908328086994,15.086314582677,4.2069980048147));
#59386=CARTESIAN_POINT('Ctrl Pts',(-4.27740144981121,11.9069082859864,4.04999787746244));
#59387=CARTESIAN_POINT('Ctrl Pts',(-5.83660012621804,10.4454813502308,3.94533112589427));
#59388=CARTESIAN_POINT('Ctrl Pts',(-6.75406714565307,10.2002034869244,3.89299775011019));
#59389=CARTESIAN_POINT('Ctrl Pts',(-5.16393734230382,14.9876826136972,12.3210067496694));
#59390=CARTESIAN_POINT('Ctrl Pts',(-4.50718404955416,14.2195377949102,12.2686733738853));
#59391=CARTESIAN_POINT('Ctrl Pts',(-4.02072454807007,11.9980196949375,12.1640066223172));
#59392=CARTESIAN_POINT('Ctrl Pts',(-6.41228541109164,9.53625011304927,12.0070064949649));
#59393=CARTESIAN_POINT('Ctrl Pts',(-9.77913390205027,10.1800451430645,11.8500063676127));
#59394=CARTESIAN_POINT('Ctrl Pts',(-11.1022479429831,13.3398490887126,11.6930062402604));
#59395=CARTESIAN_POINT('Ctrl Pts',(-9.19520332408216,16.188335839362,11.5360061129082));
#59396=CARTESIAN_POINT('Ctrl Pts',(-5.76804722455709,16.1681372027015,11.3790059855559));
#59397=CARTESIAN_POINT('Ctrl Pts',(-3.89395310615829,13.2989500353867,11.2220058582037));
#59398=CARTESIAN_POINT('Ctrl Pts',(-5.25343413560966,10.1527921984098,11.0650057308514));
#59399=CARTESIAN_POINT('Ctrl Pts',(-8.62743319586002,9.55126751773617,10.9080056034992));
#59400=CARTESIAN_POINT('Ctrl Pts',(-10.9904516497645,12.0335573785871,10.7510054761469));
#59401=CARTESIAN_POINT('Ctrl Pts',(-10.2235488501508,15.3738767896174,10.5940053487946));
#59402=CARTESIAN_POINT('Ctrl Pts',(-7.01441355218445,16.5768740138536,10.4370052214424));
#59403=CARTESIAN_POINT('Ctrl Pts',(-4.24070833971001,14.56383815303,10.2800050940901));
#59404=CARTESIAN_POINT('Ctrl Pts',(-4.38964119697082,11.1398633340167,10.1230049667379));
#59405=CARTESIAN_POINT('Ctrl Pts',(-7.32766264781398,9.3752680069458,9.96600483938563));
#59406=CARTESIAN_POINT('Ctrl Pts',(-10.4202206477823,10.8523779572038,9.80900471203337));
#59407=CARTESIAN_POINT('Ctrl Pts',(-10.8941887815987,14.2466564502702,9.65200458468113));
#59408=CARTESIAN_POINT('Ctrl Pts',(-8.32455527051676,16.5144204123725,9.49500445732887));
#59409=CARTESIAN_POINT('Ctrl Pts',(-5.01553513899265,15.6221446466417,9.33800432997661));
#59410=CARTESIAN_POINT('Ctrl Pts',(-3.93435848267263,12.3699411347509,9.18100420262437));
#59411=CARTESIAN_POINT('Ctrl Pts',(-6.0505267824277,9.67409209769908,9.02400407527211));
#59412=CARTESIAN_POINT('Ctrl Pts',(-9.46645162186327,9.95199116250562,8.86700394791985));
#59413=CARTESIAN_POINT('Ctrl Pts',(-11.1190404267477,12.9544436061459,8.71000382056761));
#59414=CARTESIAN_POINT('Ctrl Pts',(-9.52640096145984,15.9891215005347,8.55300369321535));
#59415=CARTESIAN_POINT('Ctrl Pts',(-6.11666831357863,16.3348000735102,8.3960035658631));
#59416=CARTESIAN_POINT('Ctrl Pts',(-3.9473824601037,13.6815060275445,8.23900343851085));
#59417=CARTESIAN_POINT('Ctrl Pts',(-4.9637628366961,10.4084735910568,8.08200331115859));
#59418=CARTESIAN_POINT('Ctrl Pts',(-8.25441140963209,9.45066234771208,7.92500318380633));
#59419=CARTESIAN_POINT('Ctrl Pts',(-10.8685720331689,11.6669508307826,7.76800305645408));
#59420=CARTESIAN_POINT('Ctrl Pts',(-10.4621017996831,15.0699718913073,7.61100292910183));
#59421=CARTESIAN_POINT('Ctrl Pts',(-7.39948646190492,16.6082039047423,7.45400280174958));
#59422=CARTESIAN_POINT('Ctrl Pts',(-4.42700258466931,14.902299453002,7.29700267439732));
#59423=CARTESIAN_POINT('Ctrl Pts',(-4.21010495775379,11.4819594519348,7.14000254704507));
#59424=CARTESIAN_POINT('Ctrl Pts',(-6.94328780249567,9.41423553851335,6.98300241969282));
#59425=CARTESIAN_POINT('Ctrl Pts',(-10.1756797658017,10.5532756907892,6.82600229234056));
#59426=CARTESIAN_POINT('Ctrl Pts',(-11.0087641112188,13.8776914654038,6.66900216498831));
#59427=CARTESIAN_POINT('Ctrl Pts',(-8.69550582596531,16.4064477577484,6.51200203763606));
#59428=CARTESIAN_POINT('Ctrl Pts',(-5.31022637025923,15.8719837317436,6.3550019102838));
#59429=CARTESIAN_POINT('Ctrl Pts',(-3.88853720662811,12.7535599895385,6.19800178293155));
#59430=CARTESIAN_POINT('Ctrl Pts',(-5.70528280371351,9.84749392134933,6.04100165557929));
#59431=CARTESIAN_POINT('Ctrl Pts',(-9.13136573648253,9.75968890749465,5.88400152822705));
#59432=CARTESIAN_POINT('Ctrl Pts',(-11.0945928249223,12.5688686955092,5.72700140087479));
#59433=CARTESIAN_POINT('Ctrl Pts',(-9.83450335608313,15.7560380042034,5.57000127352253));
#59434=CARTESIAN_POINT('Ctrl Pts',(-6.48106323809927,16.4631861795336,5.41300114617029));
#59435=CARTESIAN_POINT('Ctrl Pts',(-4.04127258839909,14.0562954080889,5.25600101881802));
#59436=CARTESIAN_POINT('Ctrl Pts',(-4.70303600953422,10.693474125437,5.09900089146578));
#59437=CARTESIAN_POINT('Ctrl Pts',(-7.87270732364685,9.390536089231,4.94200076411351));
#59438=CARTESIAN_POINT('Ctrl Pts',(-10.7084746854428,11.3151738175341,4.78500063676127));
#59439=CARTESIAN_POINT('Ctrl Pts',(-10.6665727432792,14.7428465227886,4.62800050940901));
#59440=CARTESIAN_POINT('Ctrl Pts',(-7.78634777823694,16.5973803971072,4.47100038205676));
#59441=CARTESIAN_POINT('Ctrl Pts',(-4.64704915358778,15.2208104036021,4.31400025470451));
#59442=CARTESIAN_POINT('Ctrl Pts',(-4.07060765975928,11.8373819589561,4.15700012735225));
#59443=CARTESIAN_POINT('Ctrl Pts',(-5.72985994157694,10.2821754194981,4.05233337578409));
#59444=CARTESIAN_POINT('Ctrl Pts',(-6.70620071746715,10.0211581030209,4.));
#59445=CARTESIAN_POINT('Ctrl Pts',(-5.58653400333492,14.6263682601415,12.));
#59446=CARTESIAN_POINT('Ctrl Pts',(-5.52489667247578,14.5684443043264,12.));
#59447=CARTESIAN_POINT('Ctrl Pts',(-5.46662450511892,14.5073716307993,12.));
#59448=CARTESIAN_POINT('Ctrl Pts',(-5.41171706416437,14.4435345397783,12.));
#59449=CARTESIAN_POINT('Ctrl Pts',(-5.35535922399003,14.3780111697138,12.));
#59450=CARTESIAN_POINT('Ctrl Pts',(-5.30254577876706,14.3095749751578,12.));
#59451=CARTESIAN_POINT('Ctrl Pts',(-5.25330168675279,14.2385929714213,12.));
#59452=CARTESIAN_POINT('Ctrl Pts',(-5.20312907342738,14.1662725674732,12.));
#59453=CARTESIAN_POINT('Ctrl Pts',(-5.15666120991867,14.0913088475707,12.));
#59454=CARTESIAN_POINT('Ctrl Pts',(-5.1139575408143,14.0140482152174,12.));
#59455=CARTESIAN_POINT('Ctrl Pts',(-5.09461512222896,13.9790533887192,12.));
#59456=CARTESIAN_POINT('Ctrl Pts',(-5.07604545116087,13.9435868239722,12.));
#59457=CARTESIAN_POINT('Ctrl Pts',(-5.05825663128179,13.9076784991748,12.));
#59458=CARTESIAN_POINT('Ctrl Pts',(-5.04815176560046,13.887280923541,12.));
#59459=CARTESIAN_POINT('Ctrl Pts',(-5.03829889260597,13.8667407800149,12.));
#59460=CARTESIAN_POINT('Ctrl Pts',(-5.02869974914025,13.846063404379,12.));
#59461=CARTESIAN_POINT('Ctrl Pts',(-5.02048275827117,13.8283633035935,12.));
#59462=CARTESIAN_POINT('Ctrl Pts',(-5.0124495628302,13.8105575032607,12.));
#59463=CARTESIAN_POINT('Ctrl Pts',(-5.00461403680565,13.7926790499403,12.));
#59464=CARTESIAN_POINT('Ctrl Pts',(-4.96800796729637,13.7091543570335,12.));
#59465=CARTESIAN_POINT('Ctrl Pts',(-4.93566374876766,13.6239462866792,12.));
#59466=CARTESIAN_POINT('Ctrl Pts',(-4.90760852459924,13.5374526993157,12.));
#59467=CARTESIAN_POINT('Ctrl Pts',(-4.87909391214457,13.449542828816,12.));
#59468=CARTESIAN_POINT('Ctrl Pts',(-4.85500940725962,13.3603042433618,12.));
#59469=CARTESIAN_POINT('Ctrl Pts',(-4.83542253240114,13.2701175707646,12.));
#59470=CARTESIAN_POINT('Ctrl Pts',(-4.81671792757447,13.1839932613098,12.));
#59471=CARTESIAN_POINT('Ctrl Pts',(-4.80211484736484,13.0970034290495,12.));
#59472=CARTESIAN_POINT('Ctrl Pts',(-4.79171068325589,13.0094587764721,12.));
#59473=CARTESIAN_POINT('Ctrl Pts',(-4.78712088419529,12.9708384356209,12.));
#59474=CARTESIAN_POINT('Ctrl Pts',(-4.78334877386587,12.9321099201028,12.));
#59475=CARTESIAN_POINT('Ctrl Pts',(-4.78040530851934,12.893299212279,12.));
#59476=CARTESIAN_POINT('Ctrl Pts',(-4.77903296806464,12.8752043824944,12.));
#59477=CARTESIAN_POINT('Ctrl Pts',(-4.77784077628839,12.8570916824141,12.));
#59478=CARTESIAN_POINT('Ctrl Pts',(-4.77682996946529,12.8389637304098,12.));
#59479=CARTESIAN_POINT('Ctrl Pts',(-4.77585594563052,12.8214954497015,12.));
#59480=CARTESIAN_POINT('Ctrl Pts',(-4.7750503477527,12.8040101811658,12.));
#59481=CARTESIAN_POINT('Ctrl Pts',(-4.77441493543858,12.7865348449805,12.));
#59482=CARTESIAN_POINT('Ctrl Pts',(-4.77095144017316,12.6912805623749,12.));
#59483=CARTESIAN_POINT('Ctrl Pts',(-4.77253057533756,12.5961742600887,12.));
#59484=CARTESIAN_POINT('Ctrl Pts',(-4.77921451714525,12.501614579937,12.));
#59485=CARTESIAN_POINT('Ctrl Pts',(-4.78586350142022,12.4075494542275,12.));
#59486=CARTESIAN_POINT('Ctrl Pts',(-4.7975636844451,12.3140242926481,12.));
#59487=CARTESIAN_POINT('Ctrl Pts',(-4.81442425859455,12.2214137249389,12.));
#59488=CARTESIAN_POINT('Ctrl Pts',(-4.83092299201404,12.1307906503674,12.));
#59489=CARTESIAN_POINT('Ctrl Pts',(-4.85236265681916,12.0410424028911,12.));
#59490=CARTESIAN_POINT('Ctrl Pts',(-4.87846866601438,11.9524107169388,12.));
#59491=CARTESIAN_POINT('Ctrl Pts',(-4.89379308908251,11.9003832529699,12.));
#59492=CARTESIAN_POINT('Ctrl Pts',(-4.91072644984389,11.8487405476717,12.));
#59493=CARTESIAN_POINT('Ctrl Pts',(-4.92922132646561,11.7975326456,12.));
#59494=CARTESIAN_POINT('Ctrl Pts',(-4.93398223972469,11.7843508123318,12.));
#59495=CARTESIAN_POINT('Ctrl Pts',(-4.93884748217419,11.7711956209025,12.));
#59496=CARTESIAN_POINT('Ctrl Pts',(-4.94381359460063,11.7580750750315,12.));
#59497=CARTESIAN_POINT('Ctrl Pts',(-4.97686200318078,11.6707606682067,12.));
#59498=CARTESIAN_POINT('Ctrl Pts',(-5.01429316281797,11.5851876670551,12.));
#59499=CARTESIAN_POINT('Ctrl Pts',(-5.05577609967284,11.5015918684293,12.));
#59500=CARTESIAN_POINT('Ctrl Pts',(-5.09882544403038,11.414839468654,12.));
#59501=CARTESIAN_POINT('Ctrl Pts',(-5.14623844362019,11.330215691903,12.));
#59502=CARTESIAN_POINT('Ctrl Pts',(-5.19770129474244,11.2479859989681,12.));
#59503=CARTESIAN_POINT('Ctrl Pts',(-5.2497890294851,11.1647578384569,12.));
#59504=CARTESIAN_POINT('Ctrl Pts',(-5.30602595623937,11.0839814330439,12.));
#59505=CARTESIAN_POINT('Ctrl Pts',(-5.36613892032226,11.0059457826021,12.));
#59506=CARTESIAN_POINT('Ctrl Pts',(-5.4056128756235,10.9547026635106,12.));
#59507=CARTESIAN_POINT('Ctrl Pts',(-5.44675926231209,10.9046416780186,12.));
#59508=CARTESIAN_POINT('Ctrl Pts',(-5.48951145353165,10.8558504805206,12.));
#59509=CARTESIAN_POINT('Ctrl Pts',(-5.50097088386534,10.8427723361571,12.));
#59510=CARTESIAN_POINT('Ctrl Pts',(-5.5125457300662,10.8297854541688,12.));
#59511=CARTESIAN_POINT('Ctrl Pts',(-5.52423480193837,10.8168915966514,12.));
#59512=CARTESIAN_POINT('Ctrl Pts',(-5.53538763239833,10.8045892506277,12.));
#59513=CARTESIAN_POINT('Ctrl Pts',(-5.54663877351141,10.7923778862678,12.));
#59514=CARTESIAN_POINT('Ctrl Pts',(-5.55798379608792,10.7802620173577,12.));
#59515=CARTESIAN_POINT('Ctrl Pts',(-5.62980564817047,10.7035601739863,12.));
#59516=CARTESIAN_POINT('Ctrl Pts',(-5.70542329107336,10.630641847274,12.));
#59517=CARTESIAN_POINT('Ctrl Pts',(-5.78449319659024,10.5618401471187,12.));
#59518=CARTESIAN_POINT('Ctrl Pts',(-5.84379562572791,10.5102388720023,12.));
#59519=CARTESIAN_POINT('Ctrl Pts',(-5.90504126576837,10.4609534569649,12.));
#59520=CARTESIAN_POINT('Ctrl Pts',(-5.96810424452339,10.4141359861561,12.));
#59521=CARTESIAN_POINT('Ctrl Pts',(-5.99074689198795,10.39732625868,12.));
#59522=CARTESIAN_POINT('Ctrl Pts',(-6.01362396161954,10.3808348014861,12.));
#59523=CARTESIAN_POINT('Ctrl Pts',(-6.03673007192386,10.3646690702049,12.));
#59524=CARTESIAN_POINT('Ctrl Pts',(-6.05604446520068,10.351156138454,12.));
#59525=CARTESIAN_POINT('Ctrl Pts',(-6.07552143283976,10.3378692705033,12.));
#59526=CARTESIAN_POINT('Ctrl Pts',(-6.09513718668148,10.3248263089414,12.));
#59527=CARTESIAN_POINT('Ctrl Pts',(-6.18010809783264,10.2683272145418,12.));
#59528=CARTESIAN_POINT('Ctrl Pts',(-6.26775573276173,10.2163476819429,12.));
#59529=CARTESIAN_POINT('Ctrl Pts',(-6.35779277794461,10.1691997545039,12.));
#59530=CARTESIAN_POINT('Ctrl Pts',(-6.4298686728608,10.131457189133,12.));
#59531=CARTESIAN_POINT('Ctrl Pts',(-6.50347672461637,10.0968111469865,12.));
#59532=CARTESIAN_POINT('Ctrl Pts',(-6.57848633664494,10.0654390261441,12.));
#59533=CARTESIAN_POINT('Ctrl Pts',(-6.61998971216275,10.0480805986452,12.));
#59534=CARTESIAN_POINT('Ctrl Pts',(-6.6619224176942,10.0317247798523,12.));
#59535=CARTESIAN_POINT('Ctrl Pts',(-6.70425100699966,10.0163623331919,12.));
#59536=CARTESIAN_POINT('Ctrl Pts',(-10.0166112816083,12.988245230306,10.387416697508));
#59537=CARTESIAN_POINT('Ctrl Pts',(-10.0185036739199,12.7635802052187,10.4016107071645));
#59538=CARTESIAN_POINT('Ctrl Pts',(-9.99083720988162,12.539373330507,10.415804716821));
#59539=CARTESIAN_POINT('Ctrl Pts',(-9.93173881101679,12.3237831354866,10.4299987264775));
#59540=CARTESIAN_POINT('Ctrl Pts',(-9.71384275550587,11.5289011419959,10.4823321022615));
#59541=CARTESIAN_POINT('Ctrl Pts',(-9.06866093698144,10.8511543034631,10.5346654780456));
#59542=CARTESIAN_POINT('Ctrl Pts',(-8.28546362708042,10.5943989029373,10.5869988538297));
#59543=CARTESIAN_POINT('Ctrl Pts',(-7.50226631717939,10.3376435024115,10.6393322296138));
#59544=CARTESIAN_POINT('Ctrl Pts',(-6.58105351590176,10.5018795398927,10.6916656053979));
#59545=CARTESIAN_POINT('Ctrl Pts',(-5.93485558054988,11.0134998825089,10.743998981182));
#59546=CARTESIAN_POINT('Ctrl Pts',(-5.28865764519799,11.5251202251251,10.796332356966));
#59547=CARTESIAN_POINT('Ctrl Pts',(-4.91747457577184,12.3841248728762,10.8486657327501));
#59548=CARTESIAN_POINT('Ctrl Pts',(-4.98772773186019,13.2053184658649,10.9009991085342));
#59549=CARTESIAN_POINT('Ctrl Pts',(-5.05798088794854,14.0265120588536,10.9533324843183));
#59550=CARTESIAN_POINT('Ctrl Pts',(-5.56967026955137,14.8098945970798,11.0056658601024));
#59551=CARTESIAN_POINT('Ctrl Pts',(-6.29337817170545,15.2043433125241,11.0579992358865));
#59552=CARTESIAN_POINT('Ctrl Pts',(-7.01708607385953,15.5987920279684,11.1103326116706));
#59553=CARTESIAN_POINT('Ctrl Pts',(-7.95281249656485,15.6043069206307,11.1626659874546));
#59554=CARTESIAN_POINT('Ctrl Pts',(-8.68101868433327,15.2181990454088,11.2149993632387));
#59555=CARTESIAN_POINT('Ctrl Pts',(-9.4092248721017,14.8320911701869,11.2673327390228));
#59556=CARTESIAN_POINT('Ctrl Pts',(-9.92991082493323,14.0543605270808,11.3196661148069));
#59557=CARTESIAN_POINT('Ctrl Pts',(-10.0096269590927,13.2341299632324,11.371999490591));
#59558=CARTESIAN_POINT('Ctrl Pts',(-10.0174549790803,13.1535843959402,11.3771385595633));
#59559=CARTESIAN_POINT('Ctrl Pts',(-10.0210307346825,13.0726290026425,11.3822776285357));
#59560=CARTESIAN_POINT('Ctrl Pts',(-10.020507596494,12.9916292754481,11.387416697508));
#59561=CARTESIAN_POINT('Ctrl Pts',(-8.29379928253292,10.0211581030209,12.));
#59562=CARTESIAN_POINT('Ctrl Pts',(-9.27014005842312,10.2821754194981,11.9476666242159));
#59563=CARTESIAN_POINT('Ctrl Pts',(-10.9293920526294,11.8373837255142,11.8429998726477));
#59564=CARTESIAN_POINT('Ctrl Pts',(-10.3529510979028,15.2208095229378,11.6859997452955));
#59565=CARTESIAN_POINT('Ctrl Pts',(-7.21365218567195,16.5973810760335,11.5289996179432));
#59566=CARTESIAN_POINT('Ctrl Pts',(-4.33342713054201,14.7428462583649,11.371999490591));
#59567=CARTESIAN_POINT('Ctrl Pts',(-4.29152522806557,11.3151739482887,11.2149993632387));
#59568=CARTESIAN_POINT('Ctrl Pts',(-7.12729264284838,9.39053585671186,11.0579992358865));
#59569=CARTESIAN_POINT('Ctrl Pts',(-10.2969641018483,10.6934741072896,10.9009991085342));
#59570=CARTESIAN_POINT('Ctrl Pts',(-10.9587275214881,14.0562954105675,10.743998981182));
#59571=CARTESIAN_POINT('Ctrl Pts',(-8.5189368031419,16.4631863186891,10.5869988538297));
#59572=CARTESIAN_POINT('Ctrl Pts',(-5.16549655959477,15.7560380892136,10.4299987264775));
#59573=CARTESIAN_POINT('Ctrl Pts',(-3.90540705298465,12.5688686867556,10.2729985991252));
#59574=CARTESIAN_POINT('Ctrl Pts',(-5.86863420589283,9.75968879265402,10.115998471773));
#59575=CARTESIAN_POINT('Ctrl Pts',(-9.29471725902464,9.84749381445728,9.9589983444207));
#59576=CARTESIAN_POINT('Ctrl Pts',(-11.1114629177913,12.7535599804133,9.80199821706845));
#59577=CARTESIAN_POINT('Ctrl Pts',(-9.68977370564798,15.8719838318464,9.64499808971619));
#59578=CARTESIAN_POINT('Ctrl Pts',(-6.30449413259093,16.4064478755407,9.48799796236394));
#59579=CARTESIAN_POINT('Ctrl Pts',(-3.99123576757957,13.8776914962184,9.3309978350117));
#59580=CARTESIAN_POINT('Ctrl Pts',(-4.82432014168349,10.5532756064786,9.17399770765943));
#59581=CARTESIAN_POINT('Ctrl Pts',(-8.05671221676616,9.41423541495656,9.0169975803072));
#59582=CARTESIAN_POINT('Ctrl Pts',(-10.7898951559407,11.481959399778,8.85999745295492));
#59583=CARTESIAN_POINT('Ctrl Pts',(-10.572997521546,14.902299519094,8.70299732560269));
#59584=CARTESIAN_POINT('Ctrl Pts',(-7.60051354156566,16.6082040297755,8.54599719825042));
#59585=CARTESIAN_POINT('Ctrl Pts',(-4.53789809794217,15.0699719631857,8.38899707089818));
#59586=CARTESIAN_POINT('Ctrl Pts',(-4.1314278504052,11.6669507850401,8.23199694354592));
#59587=CARTESIAN_POINT('Ctrl Pts',(-6.74558856429446,9.45066222537301,8.07499681619367));
#59588=CARTESIAN_POINT('Ctrl Pts',(-10.0362372509614,10.4084735018199,7.91799668884141));
#59589=CARTESIAN_POINT('Ctrl Pts',(-11.0526176626825,13.6815060514322,7.76099656148917));
#59590=CARTESIAN_POINT('Ctrl Pts',(-8.88333173423194,16.3348001890992,7.6039964341369));
#59591=CARTESIAN_POINT('Ctrl Pts',(-5.47359896850368,15.9891216041795,7.44699630678466));
#59592=CARTESIAN_POINT('Ctrl Pts',(-3.88095944817013,12.9544436048999,7.28999617943239));
#59593=CARTESIAN_POINT('Ctrl Pts',(-5.53354831017302,9.95199105749957,7.13299605208015));
#59594=CARTESIAN_POINT('Ctrl Pts',(-8.9494732676674,9.67409198306777,6.97599592472789));
#59595=CARTESIAN_POINT('Ctrl Pts',(-11.0656416405671,12.3699411133323,6.81899579737564));
#59596=CARTESIAN_POINT('Ctrl Pts',(-9.98446494686864,15.6221447375545,6.66199567002338));
#59597=CARTESIAN_POINT('Ctrl Pts',(-6.67544470099851,16.5144205342573,6.50499554267113));
#59598=CARTESIAN_POINT('Ctrl Pts',(-4.10581110106408,14.2466564935293,6.34799541531888));
#59599=CARTESIAN_POINT('Ctrl Pts',(-4.57977925134152,10.8523778836063,6.19099528796662));
#59600=CARTESIAN_POINT('Ctrl Pts',(-7.67233735803906,9.3752678814539,6.03399516061438));
#59601=CARTESIAN_POINT('Ctrl Pts',(-10.6103589107324,11.1398632710606,5.87699503326211));
#59602=CARTESIAN_POINT('Ctrl Pts',(-10.7592917725406,14.5638382055826,5.71999490590987));
#59603=CARTESIAN_POINT('Ctrl Pts',(-7.98558646537732,16.576874141135,5.56299477855761));
#59604=CARTESIAN_POINT('Ctrl Pts',(-4.77645105419042,15.3738768659897,5.40599465120536));
#59605=CARTESIAN_POINT('Ctrl Pts',(-4.00954823259222,12.0335573562934,5.24899452385311));
#59606=CARTESIAN_POINT('Ctrl Pts',(-6.37256675930357,9.55126737969704,5.09199439650085));
#59607=CARTESIAN_POINT('Ctrl Pts',(-9.74656595354479,10.1527921341227,4.9349942691486));
#59608=CARTESIAN_POINT('Ctrl Pts',(-11.1060469959117,13.2989499872504,4.77799414179634));
#59609=CARTESIAN_POINT('Ctrl Pts',(-9.2319528795399,16.1681374132995,4.62099401444409));
#59610=CARTESIAN_POINT('Ctrl Pts',(-5.80479653057489,16.1883357805992,4.46399388709183));
#59611=CARTESIAN_POINT('Ctrl Pts',(-3.89775210281319,13.3398493780975,4.30699375973959));
#59612=CARTESIAN_POINT('Ctrl Pts',(-5.22086568363505,10.1800446040033,4.14999363238733));
#59613=CARTESIAN_POINT('Ctrl Pts',(-8.58771529500726,9.53625069635182,3.99299350503508));
#59614=CARTESIAN_POINT('Ctrl Pts',(-10.9792742142571,11.9980184020288,3.83599337768282));
#59615=CARTESIAN_POINT('Ctrl Pts',(-10.4928159504458,14.2195377949103,3.73132662611465));
#59616=CARTESIAN_POINT('Ctrl Pts',(-9.83606265769613,14.9876826136973,3.67899325033057));
#59617=CARTESIAN_POINT('Ctrl Pts',(-8.245932854347,10.2002034869244,12.1070022498898));
#59618=CARTESIAN_POINT('Ctrl Pts',(-9.16339987378202,10.4454813502309,12.0546688741057));
#59619=CARTESIAN_POINT('Ctrl Pts',(-10.7225982799205,11.9069099460203,11.9500021225376));
#59620=CARTESIAN_POINT('Ctrl Pts',(-10.1809169554557,15.086313755117,11.7930019951853));
#59621=CARTESIAN_POINT('Ctrl Pts',(-7.23091907843985,16.3798774687766,11.636001867833));
#59622=CARTESIAN_POINT('Ctrl Pts',(-4.52437279676603,14.6371718749705,11.4790017404808));
#59623=CARTESIAN_POINT('Ctrl Pts',(-4.48499759650499,11.4161896364091,11.3220016131285));
#59624=CARTESIAN_POINT('Ctrl Pts',(-7.14976705210776,9.60760802538281,11.1650014857763));
#59625=CARTESIAN_POINT('Ctrl Pts',(-10.1283059986405,10.8319785554116,11.008001358424));
#59626=CARTESIAN_POINT('Ctrl Pts',(-10.7501648077581,13.992020329963,10.8510012310718));
#59627=CARTESIAN_POINT('Ctrl Pts',(-8.45749448845756,16.2537747113328,10.6940011037195));
#59628=CARTESIAN_POINT('Ctrl Pts',(-5.30626809181812,15.5892678153629,10.5370009763673));
#59629=CARTESIAN_POINT('Ctrl Pts',(-4.12216250860425,12.5942860586688,10.380000849015));
#59630=CARTESIAN_POINT('Ctrl Pts',(-5.96700624445078,9.95450088514863,10.2230007216628));
#59631=CARTESIAN_POINT('Ctrl Pts',(-9.18649505892511,10.0370112274744,10.0660005943105));
#59632=CARTESIAN_POINT('Ctrl Pts',(-10.8936901958899,12.7678403902015,9.90900046695827));
#59633=CARTESIAN_POINT('Ctrl Pts',(-9.5577294368621,15.6982219813021,9.752000339606));
#59634=CARTESIAN_POINT('Ctrl Pts',(-6.3765836355766,16.2004576199972,9.59500021225376));
#59635=CARTESIAN_POINT('Ctrl Pts',(-4.20281571587151,13.8241863062249,9.4380000849015));
#59636=CARTESIAN_POINT('Ctrl Pts',(-4.98566475436435,10.7002340827391,9.28099995754925));
#59637=CARTESIAN_POINT('Ctrl Pts',(-8.02314223764118,9.62987849036962,9.123999830197));
#59638=CARTESIAN_POINT('Ctrl Pts',(-10.5915131043488,11.5729178555327,8.96699970284474));
#59639=CARTESIAN_POINT('Ctrl Pts',(-10.3876944878733,14.7870100374982,8.80999957549249));
#59640=CARTESIAN_POINT('Ctrl Pts',(-7.59445253304005,16.3900477938888,8.65299944814024));
#59641=CARTESIAN_POINT('Ctrl Pts',(-4.71651407945554,14.9445717631999,8.49599932078798));
#59642=CARTESIAN_POINT('Ctrl Pts',(-4.33455415756585,11.7467541830206,8.33899919343573));
#59643=CARTESIAN_POINT('Ctrl Pts',(-6.79107988887037,9.66410874890807,8.18199906608347));
#59644=CARTESIAN_POINT('Ctrl Pts',(-9.88330108572798,10.5641636054531,8.02499893873122));
#59645=CARTESIAN_POINT('Ctrl Pts',(-10.8383933342348,13.6398309256761,7.86799881137897));
#59646=CARTESIAN_POINT('Ctrl Pts',(-8.79991625305057,16.1331303189645,7.71099868402671));
#59647=CARTESIAN_POINT('Ctrl Pts',(-5.59579179682231,15.8082962970528,7.55399855667447));
#59648=CARTESIAN_POINT('Ctrl Pts',(-4.09918910456809,12.956610648253,7.39699842932221));
#59649=CARTESIAN_POINT('Ctrl Pts',(-5.65212616815729,10.1352072431286,7.23999830196996));
#59650=CARTESIAN_POINT('Ctrl Pts',(-8.86206942440258,9.8740655989212,7.0829981746177));
#59651=CARTESIAN_POINT('Ctrl Pts',(-10.8506319608149,12.4073539009847,6.92599804726545));
#59652=CARTESIAN_POINT('Ctrl Pts',(-9.83465067318943,15.4634482887157,6.76899791991319));
#59653=CARTESIAN_POINT('Ctrl Pts',(-6.72516572981961,16.3019194823095,6.61199779256095));
#59654=CARTESIAN_POINT('Ctrl Pts',(-4.3104821089062,14.1709025601374,6.45499766520868));
#59655=CARTESIAN_POINT('Ctrl Pts',(-4.75586978181755,10.9813003676665,6.29799753785644));
#59656=CARTESIAN_POINT('Ctrl Pts',(-7.6619453433902,9.59326071540802,6.14099741050417));
#59657=CARTESIAN_POINT('Ctrl Pts',(-10.4228029696916,11.2514502662184,5.98399728315193));
#59658=CARTESIAN_POINT('Ctrl Pts',(-10.5627551177461,14.4689580825154,5.82699715579967));
#59659=CARTESIAN_POINT('Ctrl Pts',(-7.95630539875948,16.360607110615,5.66999702844743));
#59660=CARTESIAN_POINT('Ctrl Pts',(-4.94068219283476,15.23015107347,5.51299690109516));
#59661=CARTESIAN_POINT('Ctrl Pts',(-4.22002393159755,12.0912542249516,5.35599677374292));
#59662=CARTESIAN_POINT('Ctrl Pts',(-6.44055145447491,9.75864737041887,5.19899664639066));
#59663=CARTESIAN_POINT('Ctrl Pts',(-9.61109708849724,10.3238999309873,5.04199651903841));
#59664=CARTESIAN_POINT('Ctrl Pts',(-10.8886008563611,13.2803431519,4.88499639168615));
#59665=CARTESIAN_POINT('Ctrl Pts',(-9.12751539773043,15.9765173781352,4.72799626433391));
#59666=CARTESIAN_POINT('Ctrl Pts',(-5.9070180076098,15.995497775453,4.57099613698164));
#59667=CARTESIAN_POINT('Ctrl Pts',(-4.11496915512444,13.3187762924015,4.4139960096294));
#59668=CARTESIAN_POINT('Ctrl Pts',(-5.35829843455949,10.3495090655549,4.25699588227714));
#59669=CARTESIAN_POINT('Ctrl Pts',(-8.52212560854514,9.74453619934955,4.09999575492489));
#59670=CARTESIAN_POINT('Ctrl Pts',(-10.7694725263739,12.0578582844684,3.94299562757263));
#59671=CARTESIAN_POINT('Ctrl Pts',(-10.31234789899,14.1454191303684,3.83832887600446));
#59672=CARTESIAN_POINT('Ctrl Pts',(-9.6951971040191,14.8672444958454,3.78599550022038));
#59673=CARTESIAN_POINT('Ctrl Pts',(-8.19806642616107,10.379248870828,12.2140044997796));
#59674=CARTESIAN_POINT('Ctrl Pts',(-9.05665968914092,10.6087872809636,12.1616711239955));
#59675=CARTESIAN_POINT('Ctrl Pts',(-10.5158045072117,11.9764361665263,12.0570043724274));
#59676=CARTESIAN_POINT('Ctrl Pts',(-10.0088828130085,14.9518179872963,11.9000042450751));
#59677=CARTESIAN_POINT('Ctrl Pts',(-7.24818597120775,16.1623738615197,11.7430041177229));
#59678=CARTESIAN_POINT('Ctrl Pts',(-4.71531846299006,14.531497491576,11.5860039903706));
#59679=CARTESIAN_POINT('Ctrl Pts',(-4.67846996494438,11.5172053245294,11.4290038630183));
#59680=CARTESIAN_POINT('Ctrl Pts',(-7.17224146136718,9.82468019405374,11.2720037356661));
#59681=CARTESIAN_POINT('Ctrl Pts',(-9.9596478954327,10.9704830035337,11.1150036083138));
#59682=CARTESIAN_POINT('Ctrl Pts',(-10.5416020940281,13.9277452493586,10.9580034809616));
#59683=CARTESIAN_POINT('Ctrl Pts',(-8.39605217377323,16.0443631039765,10.8010033536093));
#59684=CARTESIAN_POINT('Ctrl Pts',(-5.44703962404145,15.4224975415121,10.6440032262571));
#59685=CARTESIAN_POINT('Ctrl Pts',(-4.33891796422385,12.6197034305821,10.4870030989048));
#59686=CARTESIAN_POINT('Ctrl Pts',(-6.06537828300873,10.1493129776432,10.3300029715526));
#59687=CARTESIAN_POINT('Ctrl Pts',(-9.07827285882558,10.2265286404914,10.1730028442003));
#59688=CARTESIAN_POINT('Ctrl Pts',(-10.6759174739885,12.7821207999897,10.0160027168481));
#59689=CARTESIAN_POINT('Ctrl Pts',(-9.4256851680762,15.5244601307577,9.85900258949583));
#59690=CARTESIAN_POINT('Ctrl Pts',(-6.4486731385623,15.9944673644538,9.70200246214356));
#59691=CARTESIAN_POINT('Ctrl Pts',(-4.41439566416342,13.7706811162314,9.54500233479132));
#59692=CARTESIAN_POINT('Ctrl Pts',(-5.14700936704523,10.8471925589996,9.38800220743905));
#59693=CARTESIAN_POINT('Ctrl Pts',(-7.98957225851618,9.84552156578271,9.23100208008681));
#59694=CARTESIAN_POINT('Ctrl Pts',(-10.393131052757,11.6638763112873,9.07400195273455));
#59695=CARTESIAN_POINT('Ctrl Pts',(-10.2023914542005,14.6717205559024,8.9170018253823));
#59696=CARTESIAN_POINT('Ctrl Pts',(-7.58839152451442,16.1718915580022,8.76000169803004));
#59697=CARTESIAN_POINT('Ctrl Pts',(-4.89513006096893,14.8191715632141,8.6030015706778));
#59698=CARTESIAN_POINT('Ctrl Pts',(-4.53768046472649,11.8265575810012,8.44600144332554));
#59699=CARTESIAN_POINT('Ctrl Pts',(-6.83657121344629,9.87755527244308,8.28900131597329));
#59700=CARTESIAN_POINT('Ctrl Pts',(-9.73036492049458,10.7198537090864,8.13200118862103));
#59701=CARTESIAN_POINT('Ctrl Pts',(-10.6241690057872,13.59815579992,7.97500106126879));
#59702=CARTESIAN_POINT('Ctrl Pts',(-8.71650077186918,15.9314604488298,7.81800093391652));
#59703=CARTESIAN_POINT('Ctrl Pts',(-5.71798462514094,15.6274709899262,7.66100080656428));
#59704=CARTESIAN_POINT('Ctrl Pts',(-4.31741876096606,12.9587776916062,7.50400067921201));
#59705=CARTESIAN_POINT('Ctrl Pts',(-5.77070402614152,10.3184234287576,7.34700055185978));
#59706=CARTESIAN_POINT('Ctrl Pts',(-8.7746655811378,10.0740392147746,7.19000042450751));
#59707=CARTESIAN_POINT('Ctrl Pts',(-10.6356222810626,12.4447666886372,7.03300029715527));
#59708=CARTESIAN_POINT('Ctrl Pts',(-9.68483639951025,15.304751839877,6.876000169803));
#59709=CARTESIAN_POINT('Ctrl Pts',(-6.77488675864068,16.0894184303616,6.71900004245076));
#59710=CARTESIAN_POINT('Ctrl Pts',(-4.51515311674835,14.0951486267455,6.56199991509849));
#59711=CARTESIAN_POINT('Ctrl Pts',(-4.93196031229355,11.1102228517267,6.40499978774625));
#59712=CARTESIAN_POINT('Ctrl Pts',(-7.65155332874137,9.81125354936211,6.24799966039399));
#59713=CARTESIAN_POINT('Ctrl Pts',(-10.2352470286507,11.3630372613762,6.09099953304174));
#59714=CARTESIAN_POINT('Ctrl Pts',(-10.3662184629517,14.3740779594481,5.93399940568949));
#59715=CARTESIAN_POINT('Ctrl Pts',(-7.92702433214164,16.1443400800951,5.77699927833723));
#59716=CARTESIAN_POINT('Ctrl Pts',(-5.10491333147909,15.0864252809503,5.61999915098498));
#59717=CARTESIAN_POINT('Ctrl Pts',(-4.4304996306029,12.1489510936098,5.46299902363272));
#59718=CARTESIAN_POINT('Ctrl Pts',(-6.50853614964623,9.96602736114071,5.30599889628047));
#59719=CARTESIAN_POINT('Ctrl Pts',(-9.47562822344969,10.4950077278519,5.14899876892822));
#59720=CARTESIAN_POINT('Ctrl Pts',(-10.6711547168104,13.2617363165495,4.99199864157597));
#59721=CARTESIAN_POINT('Ctrl Pts',(-9.02307791592096,15.7848973429709,4.83499851422371));
#59722=CARTESIAN_POINT('Ctrl Pts',(-6.0092394846447,15.8026597703067,4.67799838687145));
#59723=CARTESIAN_POINT('Ctrl Pts',(-4.33218620743569,13.2977032067055,4.52099825951921));
#59724=CARTESIAN_POINT('Ctrl Pts',(-5.49573118548395,10.5189735271065,4.36399813216694));
#59725=CARTESIAN_POINT('Ctrl Pts',(-8.45653592208301,9.95282170234728,4.20699800481471));
#59726=CARTESIAN_POINT('Ctrl Pts',(-10.5596708384907,12.117698166908,4.04999787746244));
#59727=CARTESIAN_POINT('Ctrl Pts',(-10.1318798475343,14.0713004658266,3.94533112589427));
#59728=CARTESIAN_POINT('Ctrl Pts',(-9.55433155034207,14.7468063779934,3.89299775011019));
#59729=CARTESIAN_POINT('Ctrl Pts',(-8.15019999797515,10.5582942547315,12.3210067496694));
#59730=CARTESIAN_POINT('Ctrl Pts',(-8.94991950449982,10.7720932116964,12.2686733738853));
#59731=CARTESIAN_POINT('Ctrl Pts',(-10.3090107345028,12.0459623870324,12.1640066223172));
#59732=CARTESIAN_POINT('Ctrl Pts',(-9.83684867056136,14.8173222194755,12.0070064949649));
#59733=CARTESIAN_POINT('Ctrl Pts',(-7.26545286397565,15.9448702542628,11.8500063676127));
#59734=CARTESIAN_POINT('Ctrl Pts',(-4.90626412921408,14.4258231081815,11.6930062402604));
#59735=CARTESIAN_POINT('Ctrl Pts',(-4.87194233338379,11.6182210126498,11.5360061129081));
#59736=CARTESIAN_POINT('Ctrl Pts',(-7.19471587062657,10.0417523627247,11.3790059855559));
#59737=CARTESIAN_POINT('Ctrl Pts',(-9.79098979222489,11.1089874516557,11.2220058582036));
#59738=CARTESIAN_POINT('Ctrl Pts',(-10.3330393802981,13.8634701687541,11.0650057308514));
#59739=CARTESIAN_POINT('Ctrl Pts',(-8.33460985908889,15.8349514966202,10.9080056034991));
#59740=CARTESIAN_POINT('Ctrl Pts',(-5.5878111562648,15.2557272676614,10.7510054761469));
#59741=CARTESIAN_POINT('Ctrl Pts',(-4.55567341984345,12.6451208024954,10.5940053487946));
#59742=CARTESIAN_POINT('Ctrl Pts',(-6.16375032156668,10.3441250701379,10.4370052214424));
#59743=CARTESIAN_POINT('Ctrl Pts',(-8.97005065872605,10.4160460535085,10.2800050940901));
#59744=CARTESIAN_POINT('Ctrl Pts',(-10.4581447520871,12.796401209778,10.1230049667379));
#59745=CARTESIAN_POINT('Ctrl Pts',(-9.29364089929031,15.3506982802133,9.96600483938563));
#59746=CARTESIAN_POINT('Ctrl Pts',(-6.52076264154797,15.7884771089103,9.80900471203338));
#59747=CARTESIAN_POINT('Ctrl Pts',(-4.62597561245536,13.7171759262378,9.65200458468112));
#59748=CARTESIAN_POINT('Ctrl Pts',(-5.3083539797261,10.9941510352601,9.49500445732887));
#59749=CARTESIAN_POINT('Ctrl Pts',(-7.95600227939119,10.0611646411958,9.33800432997662));
#59750=CARTESIAN_POINT('Ctrl Pts',(-10.1947490011651,11.7548347670419,9.18100420262436));
#59751=CARTESIAN_POINT('Ctrl Pts',(-10.0170884205278,14.5564310743066,9.02400407527211));
#59752=CARTESIAN_POINT('Ctrl Pts',(-7.5823305159888,15.9537353221155,8.86700394791986));
#59753=CARTESIAN_POINT('Ctrl Pts',(-5.07374604248231,14.6937713632283,8.71000382056761));
#59754=CARTESIAN_POINT('Ctrl Pts',(-4.74080677188713,11.9063609789818,8.55300369321535));
#59755=CARTESIAN_POINT('Ctrl Pts',(-6.88206253802222,10.0910017959781,8.3960035658631));
#59756=CARTESIAN_POINT('Ctrl Pts',(-9.57742875526118,10.8755438127196,8.23900343851084));
#59757=CARTESIAN_POINT('Ctrl Pts',(-10.4099446773395,13.5564806741639,8.0820033111586));
#59758=CARTESIAN_POINT('Ctrl Pts',(-8.63308529068779,15.7297905786951,7.92500318380633));
#59759=CARTESIAN_POINT('Ctrl Pts',(-5.84017745345957,15.4466456827995,7.7680030564541));
#59760=CARTESIAN_POINT('Ctrl Pts',(-4.53564841736402,12.9609447349594,7.61100292910181));
#59761=CARTESIAN_POINT('Ctrl Pts',(-5.88928188412577,10.5016396143867,7.45400280174959));
#59762=CARTESIAN_POINT('Ctrl Pts',(-8.687261737873,10.2740128306281,7.29700267439731));
#59763=CARTESIAN_POINT('Ctrl Pts',(-10.4206126013104,12.4821794762896,7.14000254704508));
#59764=CARTESIAN_POINT('Ctrl Pts',(-9.53502212583107,15.1460553910382,6.98300241969281));
#59765=CARTESIAN_POINT('Ctrl Pts',(-6.82460778746177,15.8769173784138,6.82600229234057));
#59766=CARTESIAN_POINT('Ctrl Pts',(-4.71982412459047,14.0193946933536,6.66900216498831));
#59767=CARTESIAN_POINT('Ctrl Pts',(-5.10805084276957,11.2391453357869,6.51200203763605));
#59768=CARTESIAN_POINT('Ctrl Pts',(-7.64116131409251,10.0292463833162,6.35500191028381));
#59769=CARTESIAN_POINT('Ctrl Pts',(-10.0476910876099,11.474624256534,6.19800178293155));
#59770=CARTESIAN_POINT('Ctrl Pts',(-10.1696818081572,14.2791978363808,6.0410016555793));
#59771=CARTESIAN_POINT('Ctrl Pts',(-7.89774326552381,15.9280730495752,5.88400152822705));
#59772=CARTESIAN_POINT('Ctrl Pts',(-5.26914447012342,14.9426994884306,5.72700140087479));
#59773=CARTESIAN_POINT('Ctrl Pts',(-4.64097532960824,12.206647962268,5.57000127352254));
#59774=CARTESIAN_POINT('Ctrl Pts',(-6.57652084481755,10.1734073518625,5.41300114617028));
#59775=CARTESIAN_POINT('Ctrl Pts',(-9.34015935840215,10.6661155247165,5.25600101881803));
#59776=CARTESIAN_POINT('Ctrl Pts',(-10.4537085772597,13.243129481199,5.09900089146578));
#59777=CARTESIAN_POINT('Ctrl Pts',(-8.91864043411149,15.5932773078066,4.94200076411352));
#59778=CARTESIAN_POINT('Ctrl Pts',(-6.11146096167962,15.6098217651605,4.78500063676127));
#59779=CARTESIAN_POINT('Ctrl Pts',(-4.54940325974693,13.2766301210095,4.62800050940902));
#59780=CARTESIAN_POINT('Ctrl Pts',(-5.63316393640839,10.6884379886581,4.47100038205676));
#59781=CARTESIAN_POINT('Ctrl Pts',(-8.39094623562089,10.161107205345,4.31400025470451));
#59782=CARTESIAN_POINT('Ctrl Pts',(-10.3498691506075,12.1775380493476,4.15700012735225));
#59783=CARTESIAN_POINT('Ctrl Pts',(-9.95141179607851,13.9971818012848,4.05233337578409));
#59784=CARTESIAN_POINT('Ctrl Pts',(-9.41346599666504,14.6263682601415,4.));
#59785=CARTESIAN_POINT('Ctrl Pts',(-10.0159019782719,12.9923925656114,11.112583302492));
#59786=CARTESIAN_POINT('Ctrl Pts',(-10.017856950592,13.2435976299952,11.0967241119451));
#59787=CARTESIAN_POINT('Ctrl Pts',(-9.98318348246503,13.4942759769916,11.0808649213983));
#59788=CARTESIAN_POINT('Ctrl Pts',(-9.90962619541772,13.7329699372154,11.0650057308514));
#59789=CARTESIAN_POINT('Ctrl Pts',(-9.66689620656173,14.5206306113761,11.0126723550673));
#59790=CARTESIAN_POINT('Ctrl Pts',(-9.00075303282531,15.1777910539982,10.9603389792832));
#59791=CARTESIAN_POINT('Ctrl Pts',(-8.20988166215309,15.409833903816,10.9080056034991));
#59792=CARTESIAN_POINT('Ctrl Pts',(-7.41901029148087,15.6418767536339,10.8556722277151));
#59793=CARTESIAN_POINT('Ctrl Pts',(-6.50341072387283,15.4488020106477,10.803338851931));
#59794=CARTESIAN_POINT('Ctrl Pts',(-5.87358798399859,14.9171635616269,10.7510054761469));
#59795=CARTESIAN_POINT('Ctrl Pts',(-5.24376524412435,14.3855251126061,10.6986721003628));
#59796=CARTESIAN_POINT('Ctrl Pts',(-4.8997193319839,13.5153229575507,10.6463387245787));
#59797=CARTESIAN_POINT('Ctrl Pts',(-4.99570919286755,12.6967225912968,10.5940053487946));
#59798=CARTESIAN_POINT('Ctrl Pts',(-5.09169905375119,11.8781222250429,10.5416719730106));
#59799=CARTESIAN_POINT('Ctrl Pts',(-5.62772468765894,11.1111236475904,10.4893385972265));
#59800=CARTESIAN_POINT('Ctrl Pts',(-6.3634542274727,10.7396111894259,10.4370052214424));
#59801=CARTESIAN_POINT('Ctrl Pts',(-7.09918376728647,10.3680987312614,10.3846718456583));
#59802=CARTESIAN_POINT('Ctrl Pts',(-8.03461721300627,10.392072392385,10.3323384698742));
#59803=CARTESIAN_POINT('Ctrl Pts',(-8.750349618093,10.800785082325,10.2800050940901));
#59804=CARTESIAN_POINT('Ctrl Pts',(-9.46608202317973,11.209497772265,10.227671718306));
#59805=CARTESIAN_POINT('Ctrl Pts',(-9.9621133876334,12.0029494910215,10.175338342522));
#59806=CARTESIAN_POINT('Ctrl Pts',(-10.0160450943941,12.8253915288056,10.1230049667379));
#59807=CARTESIAN_POINT('Ctrl Pts',(-10.0196250796435,12.8799852092316,10.1195310786559));
#59808=CARTESIAN_POINT('Ctrl Pts',(-10.0212570407989,12.9347066297247,10.116057190574));
#59809=CARTESIAN_POINT('Ctrl Pts',(-10.0209918820407,12.9894441341194,10.112583302492));
#59810=CARTESIAN_POINT('Ctrl Pts',(-8.29379928253292,10.0211581030209,12.));
#59811=CARTESIAN_POINT('Ctrl Pts',(-8.38688154479599,10.0552080103525,12.));
#59812=CARTESIAN_POINT('Ctrl Pts',(-8.4779006806254,10.0940206699959,12.));
#59813=CARTESIAN_POINT('Ctrl Pts',(-8.56664686325615,10.1372696205127,12.));
#59814=CARTESIAN_POINT('Ctrl Pts',(-8.65733903335545,10.1814669150961,12.));
#59815=CARTESIAN_POINT('Ctrl Pts',(-8.74565814612796,10.2302978026812,12.));
#59816=CARTESIAN_POINT('Ctrl Pts',(-8.83135135493958,10.2834593640583,12.));
#59817=CARTESIAN_POINT('Ctrl Pts',(-8.91318992856164,10.3342296224599,12.));
#59818=CARTESIAN_POINT('Ctrl Pts',(-8.99263375816446,10.3889506025256,12.));
#59819=CARTESIAN_POINT('Ctrl Pts',(-9.06943047246088,10.4473877517771,12.));
#59820=CARTESIAN_POINT('Ctrl Pts',(-9.13662759747024,10.4985202573722,12.));
#59821=CARTESIAN_POINT('Ctrl Pts',(-9.20179774209257,10.5524986289602,12.));
#59822=CARTESIAN_POINT('Ctrl Pts',(-9.26474793392036,10.6091781306825,12.));
#59823=CARTESIAN_POINT('Ctrl Pts',(-9.27985634938565,10.6227815437226,12.));
#59824=CARTESIAN_POINT('Ctrl Pts',(-9.29484046111391,10.636544177759,12.));
#59825=CARTESIAN_POINT('Ctrl Pts',(-9.30967515586603,10.6504428556362,12.));
#59826=CARTESIAN_POINT('Ctrl Pts',(-9.38210515214773,10.718302774818,12.));
#59827=CARTESIAN_POINT('Ctrl Pts',(-9.45106930229927,10.7894833711807,12.));
#59828=CARTESIAN_POINT('Ctrl Pts',(-9.51632661790574,10.8636962448604,12.));
#59829=CARTESIAN_POINT('Ctrl Pts',(-9.58121902341258,10.9374941301685,12.));
#59830=CARTESIAN_POINT('Ctrl Pts',(-9.64244642197802,11.0142912680357,12.));
#59831=CARTESIAN_POINT('Ctrl Pts',(-9.69972824598415,11.0938308479656,12.));
#59832=CARTESIAN_POINT('Ctrl Pts',(-9.75408303717497,11.169306050327,12.));
#59833=CARTESIAN_POINT('Ctrl Pts',(-9.80488522775839,11.2472513152745,12.));
#59834=CARTESIAN_POINT('Ctrl Pts',(-9.85185250012922,11.3274602381139,12.));
#59835=CARTESIAN_POINT('Ctrl Pts',(-9.88922975528545,11.3912916940074,12.));
#59836=CARTESIAN_POINT('Ctrl Pts',(-9.92417754353756,11.4565571180282,12.));
#59837=CARTESIAN_POINT('Ctrl Pts',(-9.95653223361561,11.5231545729247,12.));
#59838=CARTESIAN_POINT('Ctrl Pts',(-9.96243512991986,11.5353048321122,12.));
#59839=CARTESIAN_POINT('Ctrl Pts',(-9.96824994557655,11.5474959894548,12.));
#59840=CARTESIAN_POINT('Ctrl Pts',(-9.97397248881904,11.5597200854486,12.));
#59841=CARTESIAN_POINT('Ctrl Pts',(-10.0145489524258,11.6463966845059,12.));
#59842=CARTESIAN_POINT('Ctrl Pts',(-10.0505436256048,11.7348369448931,12.));
#59843=CARTESIAN_POINT('Ctrl Pts',(-10.0816929753162,11.8247972357439,12.));
#59844=CARTESIAN_POINT('Ctrl Pts',(-10.1128423250276,11.9147575265948,12.));
#59845=CARTESIAN_POINT('Ctrl Pts',(-10.1391468173479,12.0062385811789,12.));
#59846=CARTESIAN_POINT('Ctrl Pts',(-10.1602867132728,12.0990065815937,12.));
#59847=CARTESIAN_POINT('Ctrl Pts',(-10.1814517508012,12.1918849106638,12.));
#59848=CARTESIAN_POINT('Ctrl Pts',(-10.197439126489,12.286054432468,12.));
#59849=CARTESIAN_POINT('Ctrl Pts',(-10.2083242813819,12.381106938598,12.));
#59850=CARTESIAN_POINT('Ctrl Pts',(-10.2138913557349,12.4297203367777,12.));
#59851=CARTESIAN_POINT('Ctrl Pts',(-10.2181230259612,12.4785645227018,12.));
#59852=CARTESIAN_POINT('Ctrl Pts',(-10.2210244442513,12.527583085919,12.));
#59853=CARTESIAN_POINT('Ctrl Pts',(-10.2218610165225,12.5417167152898,12.));
#59854=CARTESIAN_POINT('Ctrl Pts',(-10.2225869774383,12.5558648310221,12.));
#59855=CARTESIAN_POINT('Ctrl Pts',(-10.2232024018895,12.5700260533185,12.));
#59856=CARTESIAN_POINT('Ctrl Pts',(-10.2238236012139,12.5843201583174,12.));
#59857=CARTESIAN_POINT('Ctrl Pts',(-10.2243317772527,12.598618709654,12.));
#59858=CARTESIAN_POINT('Ctrl Pts',(-10.2247273702154,12.6129172463203,12.));
#59859=CARTESIAN_POINT('Ctrl Pts',(-10.227308430526,12.7062085557579,12.));
#59860=CARTESIAN_POINT('Ctrl Pts',(-10.2251031453087,12.7995425030326,12.));
#59861=CARTESIAN_POINT('Ctrl Pts',(-10.2182400386914,12.8925419864032,12.));
#59862=CARTESIAN_POINT('Ctrl Pts',(-10.2113727169558,12.985598587323,12.));
#59863=CARTESIAN_POINT('Ctrl Pts',(-10.1998414736524,13.0783212906945,12.));
#59864=CARTESIAN_POINT('Ctrl Pts',(-10.1837245157332,13.1703195860503,12.));
#59865=CARTESIAN_POINT('Ctrl Pts',(-10.167850633777,13.2609303630954,12.));
#59866=CARTESIAN_POINT('Ctrl Pts',(-10.1475278620093,13.3508392541549,12.));
#59867=CARTESIAN_POINT('Ctrl Pts',(-10.1227882581427,13.4396474637383,12.));
#59868=CARTESIAN_POINT('Ctrl Pts',(-10.1129089853156,13.4751112705354,12.));
#59869=CARTESIAN_POINT('Ctrl Pts',(-10.102324939091,13.5103991993701,12.));
#59870=CARTESIAN_POINT('Ctrl Pts',(-10.0910364592447,13.5454842372103,12.));
#59871=CARTESIAN_POINT('Ctrl Pts',(-10.0850885997417,13.5639704176856,12.));
#59872=CARTESIAN_POINT('Ctrl Pts',(-10.0789451599571,13.5824002543575,12.));
#59873=CARTESIAN_POINT('Ctrl Pts',(-10.0726060885077,13.6007696733809,12.));
#59874=CARTESIAN_POINT('Ctrl Pts',(-10.0672512100823,13.6162870888888,12.));
#59875=CARTESIAN_POINT('Ctrl Pts',(-10.0617593012071,13.6317538427315,12.));
#59876=CARTESIAN_POINT('Ctrl Pts',(-10.05613256518,13.6471627242414,12.));
#59877=CARTESIAN_POINT('Ctrl Pts',(-10.0253173594462,13.7315505205696,12.));
#59878=CARTESIAN_POINT('Ctrl Pts',(-9.99044489732798,13.8142532308756,12.));
#59879=CARTESIAN_POINT('Ctrl Pts',(-9.95156720789968,13.8949006686344,12.));
#59880=CARTESIAN_POINT('Ctrl Pts',(-9.92246136322671,13.9552775025255,12.));
#59881=CARTESIAN_POINT('Ctrl Pts',(-9.89110978386257,14.0145019588769,12.));
#59882=CARTESIAN_POINT('Ctrl Pts',(-9.85752072526523,14.0724054243587,12.));
#59883=CARTESIAN_POINT('Ctrl Pts',(-9.84460176992236,14.0946761373823,12.));
#59884=CARTESIAN_POINT('Ctrl Pts',(-9.83135170762611,14.1167512973966,12.));
#59885=CARTESIAN_POINT('Ctrl Pts',(-9.81777059343282,14.1386207605303,12.));
#59886=CARTESIAN_POINT('Ctrl Pts',(-9.80600921691784,14.1575599275555,12.));
#59887=CARTESIAN_POINT('Ctrl Pts',(-9.79399757751539,14.1763475835755,12.));
#59888=CARTESIAN_POINT('Ctrl Pts',(-9.78174994291027,14.194955852553,12.));
#59889=CARTESIAN_POINT('Ctrl Pts',(-9.73447804437696,14.2667777374594,12.));
#59890=CARTESIAN_POINT('Ctrl Pts',(-9.68365470418875,14.3359945738428,12.));
#59891=CARTESIAN_POINT('Ctrl Pts',(-9.62930889486242,14.4022524491644,12.));
#59892=CARTESIAN_POINT('Ctrl Pts',(-9.58717510546268,14.453621550103,12.));
#59893=CARTESIAN_POINT('Ctrl Pts',(-9.54292331405751,14.5032115233845,12.));
#59894=CARTESIAN_POINT('Ctrl Pts',(-9.49655459700825,14.5508396884611,12.));
#59895=CARTESIAN_POINT('Ctrl Pts',(-9.47068873424204,14.5774081091567,12.));
#59896=CARTESIAN_POINT('Ctrl Pts',(-9.44416391721335,14.6033657382126,12.));
#59897=CARTESIAN_POINT('Ctrl Pts',(-9.41700728965907,14.6287007311509,12.));
#59898=CARTESIAN_POINT('Origin',(-7.5,12.9903810567666,7.5));
#59899=CARTESIAN_POINT('Origin',(15.,1.36827403442078E-16,4.));
#59900=CARTESIAN_POINT('Ctrl Pts',(13.086534003335,1.63598720337497,4.));
#59901=CARTESIAN_POINT('Ctrl Pts',(13.0243671614557,1.57756563722365,4.));
#59902=CARTESIAN_POINT('Ctrl Pts',(12.9655713261624,1.51589246301216,4.));
#59903=CARTESIAN_POINT('Ctrl Pts',(12.9101605215997,1.45134356594541,4.));
#59904=CARTESIAN_POINT('Ctrl Pts',(12.8533994594265,1.38522173305508,4.));
#59905=CARTESIAN_POINT('Ctrl Pts',(12.8001899401135,1.31608182626898,4.));
#59906=CARTESIAN_POINT('Ctrl Pts',(12.7505758639603,1.24428161564212,4.));
#59907=CARTESIAN_POINT('Ctrl Pts',(12.737567030614,1.22545556774005,4.));
#59908=CARTESIAN_POINT('Ctrl Pts',(12.7248055528518,1.20644640781821,4.));
#59909=CARTESIAN_POINT('Ctrl Pts',(12.7122926030956,1.18726014528907,4.));
#59910=CARTESIAN_POINT('Ctrl Pts',(12.7022174307361,1.17181175736453,4.));
#59911=CARTESIAN_POINT('Ctrl Pts',(12.6923030248513,1.15624777849328,4.));
#59912=CARTESIAN_POINT('Ctrl Pts',(12.6825586157748,1.14058556199816,4.));
#59913=CARTESIAN_POINT('Ctrl Pts',(12.6350797654636,1.06427267050556,4.));
#59914=CARTESIAN_POINT('Ctrl Pts',(12.5915831545383,0.985554475328281,4.00000000000001));
#59915=CARTESIAN_POINT('Ctrl Pts',(12.5521056896097,0.904822546167765,4.00000000000001));
#59916=CARTESIAN_POINT('Ctrl Pts',(12.5205631790518,0.840317701884819,4.));
#59917=CARTESIAN_POINT('Ctrl Pts',(12.4915870127793,0.774526199173173,4.));
#59918=CARTESIAN_POINT('Ctrl Pts',(12.4652125787776,0.707630559635218,4.));
#59919=CARTESIAN_POINT('Ctrl Pts',(12.4565302425272,0.685608838292681,4.));
#59920=CARTESIAN_POINT('Ctrl Pts',(12.4481299823828,0.663467358107674,4.));
#59921=CARTESIAN_POINT('Ctrl Pts',(12.4400134491405,0.641212348322469,4.));
#59922=CARTESIAN_POINT('Ctrl Pts',(12.4326491678695,0.6210199648435,4.));
#59923=CARTESIAN_POINT('Ctrl Pts',(12.4255170259942,0.600729502784082,4.));
#59924=CARTESIAN_POINT('Ctrl Pts',(12.41862769741,0.580374130450127,4.));
#59925=CARTESIAN_POINT('Ctrl Pts',(12.3890480800735,0.492977497088245,4.));
#59926=CARTESIAN_POINT('Ctrl Pts',(12.363907391977,0.404299179172776,4.00000000000001));
#59927=CARTESIAN_POINT('Ctrl Pts',(12.3432403919349,0.314735964380019,4.00000000000001));
#59928=CARTESIAN_POINT('Ctrl Pts',(12.322257026321,0.223801736977766,4.00000000000001));
#59929=CARTESIAN_POINT('Ctrl Pts',(12.3058848583804,0.131954509394712,4.));
#59930=CARTESIAN_POINT('Ctrl Pts',(12.2942020415478,0.039576420273935,4.));
#59931=CARTESIAN_POINT('Ctrl Pts',(12.2826102453471,-0.0520819526881022,
4.));
#59932=CARTESIAN_POINT('Ctrl Pts',(12.2756346673422,-0.14426387445687,4.));
#59933=CARTESIAN_POINT('Ctrl Pts',(12.2733985971608,-0.236615283315844,
4.));
#59934=CARTESIAN_POINT('Ctrl Pts',(12.2723186623648,-0.28121741642928,4.));
#59935=CARTESIAN_POINT('Ctrl Pts',(12.2723449592516,-0.325859284098739,
4.));
#59936=CARTESIAN_POINT('Ctrl Pts',(12.2734957210626,-0.370501641907857,
4.));
#59937=CARTESIAN_POINT('Ctrl Pts',(12.2738658684163,-0.384861043177254,
4.));
#59938=CARTESIAN_POINT('Ctrl Pts',(12.2743523774935,-0.399220495972395,
4.));
#59939=CARTESIAN_POINT('Ctrl Pts',(12.2749559214615,-0.413578694513598,
4.));
#59940=CARTESIAN_POINT('Ctrl Pts',(12.2755868612803,-0.428588635239398,
4.));
#59941=CARTESIAN_POINT('Ctrl Pts',(12.2763453773817,-0.443588732674977,
4.));
#59942=CARTESIAN_POINT('Ctrl Pts',(12.2772314223084,-0.458571999977678,
4.));
#59943=CARTESIAN_POINT('Ctrl Pts',(12.2828802428556,-0.554095133908471,
4.));
#59944=CARTESIAN_POINT('Ctrl Pts',(12.2937114584574,-0.649002595692518,
4.));
#59945=CARTESIAN_POINT('Ctrl Pts',(12.3097976800713,-0.742900147453328,
4.));
#59946=CARTESIAN_POINT('Ctrl Pts',(12.3112861449746,-0.75158852771142,4.));
#59947=CARTESIAN_POINT('Ctrl Pts',(12.3128196370525,-0.760268274419424,
4.));
#59948=CARTESIAN_POINT('Ctrl Pts',(12.3143982352413,-0.768939082485976,
4.));
#59949=CARTESIAN_POINT('Ctrl Pts',(12.3307867311623,-0.858956607935255,
4.));
#59950=CARTESIAN_POINT('Ctrl Pts',(12.3520323002905,-0.948010485772638,
4.));
#59951=CARTESIAN_POINT('Ctrl Pts',(12.3778326203319,-1.03586583972401,4.));
#59952=CARTESIAN_POINT('Ctrl Pts',(12.4042241967268,-1.12573454219727,4.));
#59953=CARTESIAN_POINT('Ctrl Pts',(12.435381875245,-1.21434985801567,4.));
#59954=CARTESIAN_POINT('Ctrl Pts',(12.4710363747919,-1.30145748669412,4.));
#59955=CARTESIAN_POINT('Ctrl Pts',(12.4909273060557,-1.35005308827618,4.));
#59956=CARTESIAN_POINT('Ctrl Pts',(12.5122187298043,-1.39817934130794,4.));
#59957=CARTESIAN_POINT('Ctrl Pts',(12.534870586159,-1.44579043537726,4.));
#59958=CARTESIAN_POINT('Ctrl Pts',(12.5412077066689,-1.45911019319316,4.));
#59959=CARTESIAN_POINT('Ctrl Pts',(12.5476516035311,-1.47239000998161,4.));
#59960=CARTESIAN_POINT('Ctrl Pts',(12.5541943737652,-1.48561501829369,4.));
#59961=CARTESIAN_POINT('Ctrl Pts',(12.5969523561364,-1.57204242626194,4.));
#59962=CARTESIAN_POINT('Ctrl Pts',(12.6439961654632,-1.65627338500264,4.));
#59963=CARTESIAN_POINT('Ctrl Pts',(12.6949857265575,-1.73805452373085,4.));
#59964=CARTESIAN_POINT('Ctrl Pts',(12.7469808269627,-1.82144842687817,4.));
#59965=CARTESIAN_POINT('Ctrl Pts',(12.8030791489228,-1.90229571208266,4.));
#59966=CARTESIAN_POINT('Ctrl Pts',(12.8629750013787,-1.98032077373009,4.));
#59967=CARTESIAN_POINT('Ctrl Pts',(12.9233424571313,-2.05896018302908,4.));
#59968=CARTESIAN_POINT('Ctrl Pts',(12.9875679362272,-2.13473359370643,4.));
#59969=CARTESIAN_POINT('Ctrl Pts',(13.0553877098439,-2.20733955177719,4.));
#59970=CARTESIAN_POINT('Ctrl Pts',(13.0913230991629,-2.24581097730712,4.));
#59971=CARTESIAN_POINT('Ctrl Pts',(13.1282683996108,-2.28339271539353,4.));
#59972=CARTESIAN_POINT('Ctrl Pts',(13.1661892287502,-2.32003649064048,4.));
#59973=CARTESIAN_POINT('Ctrl Pts',(13.1814900570711,-2.33482203533466,4.));
#59974=CARTESIAN_POINT('Ctrl Pts',(13.196949744001,-2.34945484110134,4.));
#59975=CARTESIAN_POINT('Ctrl Pts',(13.2125661689314,-2.36393160001069,4.));
#59976=CARTESIAN_POINT('Ctrl Pts',(13.2232570858249,-2.37384230794012,4.));
#59977=CARTESIAN_POINT('Ctrl Pts',(13.2340146157559,-2.3836735202466,4.));
#59978=CARTESIAN_POINT('Ctrl Pts',(13.2448364129784,-2.39342320679516,4.));
#59979=CARTESIAN_POINT('Ctrl Pts',(13.320625051765,-2.46170349859172,4.));
#59980=CARTESIAN_POINT('Ctrl Pts',(13.3995829817648,-2.52600647852482,4.));
#59981=CARTESIAN_POINT('Ctrl Pts',(13.4813873531473,-2.58604589859231,4.));
#59982=CARTESIAN_POINT('Ctrl Pts',(13.5632614554873,-2.64613649693043,4.));
#59983=CARTESIAN_POINT('Ctrl Pts',(13.6479874247046,-2.70195710712452,4.));
#59984=CARTESIAN_POINT('Ctrl Pts',(13.7352864859208,-2.75319451696124,4.));
#59985=CARTESIAN_POINT('Ctrl Pts',(13.8208945029142,-2.80343942212848,4.));
#59986=CARTESIAN_POINT('Ctrl Pts',(13.9089775477651,-2.84927765377448,4.));
#59987=CARTESIAN_POINT('Ctrl Pts',(13.9993066119595,-2.89037749094858,4.));
#59988=CARTESIAN_POINT('Ctrl Pts',(14.025515470362,-2.90230255429857,4.));
#59989=CARTESIAN_POINT('Ctrl Pts',(14.0519135997525,-2.91382843622988,4.));
#59990=CARTESIAN_POINT('Ctrl Pts',(14.0784958352494,-2.92494631785187,4.));
#59991=CARTESIAN_POINT('Ctrl Pts',(14.1199798960696,-2.94229681034347,4.));
#59992=CARTESIAN_POINT('Ctrl Pts',(14.1619123028466,-2.95865373590191,4.));
#59993=CARTESIAN_POINT('Ctrl Pts',(14.204261268307,-2.97402368063354,4.));
#59994=CARTESIAN_POINT('Ctrl Pts',(15.7937992825329,-2.9692229537457,4.));
#59995=CARTESIAN_POINT('Ctrl Pts',(15.8886556608518,-2.93452406683594,4.));
#59996=CARTESIAN_POINT('Ctrl Pts',(15.9814715788842,-2.89484190048077,4.));
#59997=CARTESIAN_POINT('Ctrl Pts',(16.0720047548823,-2.85049467748599,4.));
#59998=CARTESIAN_POINT('Ctrl Pts',(16.1637866430073,-2.80553577910774,4.));
#59999=CARTESIAN_POINT('Ctrl Pts',(16.2532230529932,-2.75578154813471,4.));
#60000=CARTESIAN_POINT('Ctrl Pts',(16.3400275203182,-2.70152291880737,4.));
#60001=CARTESIAN_POINT('Ctrl Pts',(16.3646888442304,-2.686107932988,4.));
#60002=CARTESIAN_POINT('Ctrl Pts',(16.389137491053,-2.67032916740001,4.));
#60003=CARTESIAN_POINT('Ctrl Pts',(16.4133662837328,-2.65419282892726,4.));
#60004=CARTESIAN_POINT('Ctrl Pts',(16.4325631402962,-2.64140775212984,4.));
#60005=CARTESIAN_POINT('Ctrl Pts',(16.4516239542716,-2.62839666993241,4.));
#60006=CARTESIAN_POINT('Ctrl Pts',(16.4705261961219,-2.61517619923621,4.));
#60007=CARTESIAN_POINT('Ctrl Pts',(16.5532306656362,-2.55733163115156,4.));
#60008=CARTESIAN_POINT('Ctrl Pts',(16.6329816584356,-2.49543011909309,4.));
#60009=CARTESIAN_POINT('Ctrl Pts',(16.7095117106738,-2.42976651841151,4.));
#60010=CARTESIAN_POINT('Ctrl Pts',(16.7679773228431,-2.37960239988795,4.));
#60011=CARTESIAN_POINT('Ctrl Pts',(16.8245624524955,-2.32724171199687,4.));
#60012=CARTESIAN_POINT('Ctrl Pts',(16.8791308185435,-2.27280449707864,4.));
#60013=CARTESIAN_POINT('Ctrl Pts',(16.9076285190194,-2.2443752887693,4.));
#60014=CARTESIAN_POINT('Ctrl Pts',(16.9355759205114,-2.21537960309138,4.));
#60015=CARTESIAN_POINT('Ctrl Pts',(16.9629517841853,-2.18583377975445,4.));
#60016=CARTESIAN_POINT('Ctrl Pts',(16.9740993314633,-2.17380261732463,4.));
#60017=CARTESIAN_POINT('Ctrl Pts',(16.9851523150081,-2.16167987026619,4.));
#60018=CARTESIAN_POINT('Ctrl Pts',(16.9960991984116,-2.14947815004889,4.));
#60019=CARTESIAN_POINT('Ctrl Pts',(17.061864093391,-2.07617465177648,4.));
#60020=CARTESIAN_POINT('Ctrl Pts',(17.1238952962526,-1.9999250033291,4.));
#60021=CARTESIAN_POINT('Ctrl Pts',(17.1819478816723,-1.92100525783345,4.));
#60022=CARTESIAN_POINT('Ctrl Pts',(17.2389325987962,-1.84353722880334,4.));
#60023=CARTESIAN_POINT('Ctrl Pts',(17.2920840747574,-1.76349564200828,4.));
#60024=CARTESIAN_POINT('Ctrl Pts',(17.3411263889919,-1.681119910375,4.));
#60025=CARTESIAN_POINT('Ctrl Pts',(17.3892346863819,-1.6003130345782,4.));
#60026=CARTESIAN_POINT('Ctrl Pts',(17.4333891346359,-1.51725940586905,4.));
#60027=CARTESIAN_POINT('Ctrl Pts',(17.473281665729,-1.43217460910322,4.));
#60028=CARTESIAN_POINT('Ctrl Pts',(17.4935758753293,-1.38889009814213,4.));
#60029=CARTESIAN_POINT('Ctrl Pts',(17.5127663147042,-1.34507981852401,4.));
#60030=CARTESIAN_POINT('Ctrl Pts',(17.5308071984732,-1.30077191375233,4.));
#60031=CARTESIAN_POINT('Ctrl Pts',(17.5396600651807,-1.27902952130341,4.));
#60032=CARTESIAN_POINT('Ctrl Pts',(17.548236065603,-1.25716730274661,4.));
#60033=CARTESIAN_POINT('Ctrl Pts',(17.5565294575664,-1.23518860043795,4.));
#60034=CARTESIAN_POINT('Ctrl Pts',(17.5612619499656,-1.22264680305532,4.));
#60035=CARTESIAN_POINT('Ctrl Pts',(17.5659011120686,-1.21007041067208,4.));
#60036=CARTESIAN_POINT('Ctrl Pts',(17.5704433141742,-1.19746790314509,4.));
#60037=CARTESIAN_POINT('Ctrl Pts',(17.601949668132,-1.11005236027246,4.));
#60038=CARTESIAN_POINT('Ctrl Pts',(17.6288373085193,-1.02126995392761,4.));
#60039=CARTESIAN_POINT('Ctrl Pts',(17.6508530784154,-0.931342019285625,
4.));
#60040=CARTESIAN_POINT('Ctrl Pts',(17.6541059208438,-0.918055116184408,
4.));
#60041=CARTESIAN_POINT('Ctrl Pts',(17.6572523179739,-0.90474318860678,4.));
#60042=CARTESIAN_POINT('Ctrl Pts',(17.6602913566075,-0.891406935242469,
4.));
#60043=CARTESIAN_POINT('Ctrl Pts',(17.6812030503878,-0.79963987330047,4.));
#60044=CARTESIAN_POINT('Ctrl Pts',(17.6970357825963,-0.706720788882977,
4.));
#60045=CARTESIAN_POINT('Ctrl Pts',(17.7078979433461,-0.613041608366267,
4.));
#60046=CARTESIAN_POINT('Ctrl Pts',(17.71918010274,-0.515740208504458,4.));
#60047=CARTESIAN_POINT('Ctrl Pts',(17.7250998267343,-0.417617597139405,
4.));
#60048=CARTESIAN_POINT('Ctrl Pts',(17.7257219253175,-0.319126306900475,
4.));
#60049=CARTESIAN_POINT('Ctrl Pts',(17.7259028938113,-0.290475188042702,
4.));
#60050=CARTESIAN_POINT('Ctrl Pts',(17.7256352115795,-0.261793020088843,
4.));
#60051=CARTESIAN_POINT('Ctrl Pts',(17.7249196338,-0.233091376404626,4.));
#60052=CARTESIAN_POINT('Ctrl Pts',(17.7245239501318,-0.217220604586536,
4.));
#60053=CARTESIAN_POINT('Ctrl Pts',(17.7239913108662,-0.201343881980789,
4.));
#60054=CARTESIAN_POINT('Ctrl Pts',(17.7233217966467,-0.185463198608965,
4.));
#60055=CARTESIAN_POINT('Ctrl Pts',(17.7227411089474,-0.171689454568016,
4.));
#60056=CARTESIAN_POINT('Ctrl Pts',(17.7220574547657,-0.157914135821034,
4.));
#60057=CARTESIAN_POINT('Ctrl Pts',(17.7212718008001,-0.144150654953,4.));
#60058=CARTESIAN_POINT('Ctrl Pts',(17.7159690064325,-0.0512536391956395,
4.));
#60059=CARTESIAN_POINT('Ctrl Pts',(17.7060179260155,0.0412556969053557,
4.));
#60060=CARTESIAN_POINT('Ctrl Pts',(17.691537290537,0.133004324856137,4.));
#60061=CARTESIAN_POINT('Ctrl Pts',(17.6770974224585,0.224494652470098,4.));
#60062=CARTESIAN_POINT('Ctrl Pts',(17.6581530629752,0.315229493843254,4.));
#60063=CARTESIAN_POINT('Ctrl Pts',(17.6347733990709,0.404821867293602,4.));
#60064=CARTESIAN_POINT('Ctrl Pts',(17.6117974920603,0.492867018399034,4.));
#60065=CARTESIAN_POINT('Ctrl Pts',(17.5845376887683,0.579809603493695,4.));
#60066=CARTESIAN_POINT('Ctrl Pts',(17.5530192634714,0.665253146715262,4.));
#60067=CARTESIAN_POINT('Ctrl Pts',(17.5376266260196,0.706981166786664,4.));
#60068=CARTESIAN_POINT('Ctrl Pts',(17.521217712657,0.748351139728866,4.));
#60069=CARTESIAN_POINT('Ctrl Pts',(17.5037923624592,0.789313445373718,4.));
#60070=CARTESIAN_POINT('Ctrl Pts',(17.4980299458858,0.802859334911291,4.));
#60071=CARTESIAN_POINT('Ctrl Pts',(17.4921563593103,0.816360622497498,4.));
#60072=CARTESIAN_POINT('Ctrl Pts',(17.4861715515314,0.829815450098292,4.));
#60073=CARTESIAN_POINT('Ctrl Pts',(17.4804842577731,0.842601417477522,4.));
#60074=CARTESIAN_POINT('Ctrl Pts',(17.4746999465266,0.855337690933622,4.));
#60075=CARTESIAN_POINT('Ctrl Pts',(17.4688205030047,0.868019526422757,4.));
#60076=CARTESIAN_POINT('Ctrl Pts',(17.4313685751689,0.948802543693164,4.));
#60077=CARTESIAN_POINT('Ctrl Pts',(17.3900398049897,1.02742425086957,4.));
#60078=CARTESIAN_POINT('Ctrl Pts',(17.3448999527151,1.10353609749938,4.));
#60079=CARTESIAN_POINT('Ctrl Pts',(17.3005164856713,1.17837257715787,4.));
#60080=CARTESIAN_POINT('Ctrl Pts',(17.2524481398624,1.25078327494736,4.));
#60081=CARTESIAN_POINT('Ctrl Pts',(17.2007210868077,1.32040265351989,4.));
#60082=CARTESIAN_POINT('Ctrl Pts',(17.1505256542607,1.38796062589101,4.));
#60083=CARTESIAN_POINT('Ctrl Pts',(17.0968845380256,1.45289058144554,4.));
#60084=CARTESIAN_POINT('Ctrl Pts',(17.0397936511852,1.5148180351349,4.));
#60085=CARTESIAN_POINT('Ctrl Pts',(17.0255930287153,1.53022169128796,4.));
#60086=CARTESIAN_POINT('Ctrl Pts',(17.0111788466503,1.54543936332989,4.));
#60087=CARTESIAN_POINT('Ctrl Pts',(16.9965508084827,1.56046483491105,4.));
#60088=CARTESIAN_POINT('Ctrl Pts',(16.9706944922369,1.58702364891564,4.));
#60089=CARTESIAN_POINT('Ctrl Pts',(16.9441700096348,1.61298203696882,4.));
#60090=CARTESIAN_POINT('Ctrl Pts',(16.9170033607454,1.6383265094434,4.));
#60091=CARTESIAN_POINT('Origin',(15.,0.,14.2084234471775));
#60092=CARTESIAN_POINT('Ctrl Pts',(11.9228311771842,0.0015213020298664,
11.7084234471775));
#60093=CARTESIAN_POINT('Ctrl Pts',(11.9221922557771,0.100409703179003,11.7032843782051));
#60094=CARTESIAN_POINT('Ctrl Pts',(11.9710108327432,1.20571704782255,11.6458119334487));
#60095=CARTESIAN_POINT('Ctrl Pts',(13.3048024582519,3.19795728077006,11.5360061129082));
#60096=CARTESIAN_POINT('Ctrl Pts',(16.7319486542021,3.17774782202826,11.3790059855559));
#60097=CARTESIAN_POINT('Ctrl Pts',(18.606042966971,0.308570934784431,11.2220058582037));
#60098=CARTESIAN_POINT('Ctrl Pts',(17.246562375271,-2.83758641060089,11.0650057308514));
#60099=CARTESIAN_POINT('Ctrl Pts',(13.8725685599584,-3.4391081414099,10.9080056034992));
#60100=CARTESIAN_POINT('Ctrl Pts',(12.0835901505745,-1.55983373126709,10.7891448422745));
#60101=CARTESIAN_POINT('Ctrl Pts',(11.9252787513183,-0.276890505982443,
10.7226174568339));
#60102=CARTESIAN_POINT('Ctrl Pts',(11.9275890856804,-0.00260766251225678,
10.7084234471775));
#60103=CARTESIAN_POINT('Ctrl Pts',(11.9297760945785,-0.00333806817183434,
11.7915765528225));
#60104=CARTESIAN_POINT('Ctrl Pts',(11.9344491671038,0.677708095250012,11.7563842836469));
#60105=CARTESIAN_POINT('Ctrl Pts',(12.4898049314569,2.38075616290146,11.6688586386871));
#60106=CARTESIAN_POINT('Ctrl Pts',(15.2863460006058,3.60696666543133,11.5289996179432));
#60107=CARTESIAN_POINT('Ctrl Pts',(18.1665668486981,1.75247841941832,11.371999490591));
#60108=CARTESIAN_POINT('Ctrl Pts',(18.2084706556688,-1.6752137223659,11.2149993632387));
#60109=CARTESIAN_POINT('Ctrl Pts',(15.3727057323674,-3.59983386165072,11.0579992358865));
#60110=CARTESIAN_POINT('Ctrl Pts',(12.5232213208654,-2.42851998200457,10.9168582990811));
#60111=CARTESIAN_POINT('Ctrl Pts',(11.9339453360424,-0.702880789277512,
10.8280507380598));
#60112=CARTESIAN_POINT('Ctrl Pts',(11.9284560106028,0.0024556673498264,
10.7915765528226));
#60113=CARTESIAN_POINT('Ctrl Pts',(16.9134659966651,1.63598720337493,12.));
#60114=CARTESIAN_POINT('Ctrl Pts',(17.4514117960785,1.00680074451815,11.9476666242159));
#60115=CARTESIAN_POINT('Ctrl Pts',(17.8499101160228,-0.812800245940048,
11.8429998726477));
#60116=CARTESIAN_POINT('Ctrl Pts',(15.8909226224913,-2.8292934693942,11.6859997452955));
#60117=CARTESIAN_POINT('Ctrl Pts',(13.1331777991764,-2.30192506894816,11.5289996179432));
#60118=CARTESIAN_POINT('Ctrl Pts',(12.0494015740803,0.286239346000545,11.371999490591));
#60119=CARTESIAN_POINT('Ctrl Pts',(13.6114658170324,2.61944280277814,11.2149993632387));
#60120=CARTESIAN_POINT('Ctrl Pts',(16.4186369731426,2.60288926043798,11.0579992358865));
#60121=CARTESIAN_POINT('Ctrl Pts',(17.9537052771594,0.252750066152531,10.9009991085342));
#60122=CARTESIAN_POINT('Ctrl Pts',(16.8401564274426,-2.32426347443882,10.743998981182));
#60123=CARTESIAN_POINT('Ctrl Pts',(14.0765223197317,-2.81696917065216,10.5869988538297));
#60124=CARTESIAN_POINT('Ctrl Pts',(12.1409791666289,-0.783732381279285,
10.4299987264775));
#60125=CARTESIAN_POINT('Ctrl Pts',(12.7691475978345,1.95231594579313,10.2729985991252));
#60126=CARTESIAN_POINT('Ctrl Pts',(15.3977426901935,2.93768783020276,10.1159984717729));
#60127=CARTESIAN_POINT('Ctrl Pts',(17.6696781425075,1.28881506595247,9.95899834442072));
#60128=CARTESIAN_POINT('Ctrl Pts',(17.5476875690895,-1.51575474549275,9.80199821706844));
#60129=CARTESIAN_POINT('Ctrl Pts',(15.1411611231766,-2.96113057342894,9.6449980897162));
#60130=CARTESIAN_POINT('Ctrl Pts',(12.6080541376564,-1.75123331751949,9.48799796236395));
#60131=CARTESIAN_POINT('Ctrl Pts',(12.2198279573789,1.02901222386683,9.33099783501168));
#60132=CARTESIAN_POINT('Ctrl Pts',(14.3246087178457,2.88653234022692,9.17399770765945));
#60133=CARTESIAN_POINT('Ctrl Pts',(17.0350193212714,2.15567136478361,9.01699758030717));
#60134=CARTESIAN_POINT('Ctrl Pts',(17.920608575789,-0.508200880905659,8.85999745295495));
#60135=CARTESIAN_POINT('Ctrl Pts',(16.1872601015714,-2.71636448178362,8.70299732560267));
#60136=CARTESIAN_POINT('Ctrl Pts',(13.3892841040964,-2.48873801247178,8.54599719825043));
#60137=CARTESIAN_POINT('Ctrl Pts',(12.0356525030592,-0.0294362811014349,
8.38899707089817));
#60138=CARTESIAN_POINT('Ctrl Pts',(13.3401797411332,2.45626124056312,8.23199694354592));
#60139=CARTESIAN_POINT('Ctrl Pts',(16.1330837289975,2.73940574632503,8.07499681619367));
#60140=CARTESIAN_POINT('Ctrl Pts',(17.9099406666424,0.566098837129481,7.91799668884141));
#60141=CARTESIAN_POINT('Ctrl Pts',(17.0774258920138,-2.11483432920145,7.76099656148916));
#60142=CARTESIAN_POINT('Ctrl Pts',(14.3820633896886,-2.89937526470001,7.6039964341369));
#60143=CARTESIAN_POINT('Ctrl Pts',(12.240810574834,-1.08401858364571,7.44699630678465));
#60144=CARTESIAN_POINT('Ctrl Pts',(12.5737493864543,1.70338795860876,7.28999617943239));
#60145=CARTESIAN_POINT('Ctrl Pts',(15.0823304026287,2.96335018127148,7.13299605208015));
#60146=CARTESIAN_POINT('Ctrl Pts',(17.5170849510905,1.56604785867891,6.97599592472789));
#60147=CARTESIAN_POINT('Ctrl Pts',(17.6947452874587,-1.23554458602037,6.81899579737564));
#60148=CARTESIAN_POINT('Ctrl Pts',(15.4560016501892,-2.92921237979097,6.66199567002338));
#60149=CARTESIAN_POINT('Ctrl Pts',(12.8083570016989,-1.99622726741817,6.50499554267113));
#60150=CARTESIAN_POINT('Ctrl Pts',(12.1259795712872,0.726793862646375,6.34799541531888));
#60151=CARTESIAN_POINT('Ctrl Pts',(14.0207639954511,2.79809220508692,6.19099528796662));
#60152=CARTESIAN_POINT('Ctrl Pts',(16.793638419534,2.3603139527537,6.03399516061437));
#60153=CARTESIAN_POINT('Ctrl Pts',(17.9581406885776,-0.193979547267846,
5.87699503326211));
#60154=CARTESIAN_POINT('Ctrl Pts',(16.4700486085461,-2.57433151465002,5.71999490590987));
#60155=CARTESIAN_POINT('Ctrl Pts',(13.6637522053085,-2.64625223032612,5.56299477855761));
#60156=CARTESIAN_POINT('Ctrl Pts',(12.0556774054966,-0.345259977325435,
5.40599465120536));
#60157=CARTESIAN_POINT('Ctrl Pts',(13.0878139143641,2.26534344968177,5.2489945238531));
#60158=CARTESIAN_POINT('Ctrl Pts',(15.8346085061802,2.84456586771516,5.09199439650085));
#60159=CARTESIAN_POINT('Ctrl Pts',(17.8330357993722,0.87308907652308,4.9349942691486));
#60160=CARTESIAN_POINT('Ctrl Pts',(17.2909861426673,-1.8813930887419,4.77799414179634));
#60161=CARTESIAN_POINT('Ctrl Pts',(14.6947169782024,-2.94862097263666,4.62099401444409));
#60162=CARTESIAN_POINT('Ctrl Pts',(12.3719451483433,-1.37216452037615,4.46399388709184));
#60163=CARTESIAN_POINT('Ctrl Pts',(12.4062682448688,1.4354510150691,4.30699375973958));
#60164=CARTESIAN_POINT('Ctrl Pts',(14.7654540928384,2.95446651190592,4.14999363238733));
#60165=CARTESIAN_POINT('Ctrl Pts',(17.3368403233694,1.82697070537499,3.99299350503508));
#60166=CARTESIAN_POINT('Ctrl Pts',(17.8090202723047,-0.94447711406392,3.83599337768282));
#60167=CARTESIAN_POINT('Ctrl Pts',(16.4499195044998,-2.21828784507026,3.73132662611465));
#60168=CARTESIAN_POINT('Ctrl Pts',(15.6501999979751,-2.43208680203507,3.67899325033057));
#60169=CARTESIAN_POINT('Ctrl Pts',(17.0543315503421,1.75642532122682,12.1070022498898));
#60170=CARTESIAN_POINT('Ctrl Pts',(17.6318798475343,1.08091940905997,12.0546688741057));
#60171=CARTESIAN_POINT('Ctrl Pts',(18.0597148196982,-0.872636980364766,
11.9500021225376));
#60172=CARTESIAN_POINT('Ctrl Pts',(15.9565105706019,-3.03758041662798,11.7930019951853));
#60173=CARTESIAN_POINT('Ctrl Pts',(12.9957460688013,-2.47138820543743,11.6360018678331));
#60174=CARTESIAN_POINT('Ctrl Pts',(11.8321843976736,0.307311716258913,11.4790017404808));
#60175=CARTESIAN_POINT('Ctrl Pts',(13.5092446974389,2.81228096210878,11.3220016131285));
#60176=CARTESIAN_POINT('Ctrl Pts',(16.5230742001624,2.79450878096808,11.1650014857763));
#60177=CARTESIAN_POINT('Ctrl Pts',(18.1711511737633,0.271357022363162,11.008001358424));
#60178=CARTESIAN_POINT('Ctrl Pts',(16.9756250767187,-2.49537111982618,10.8510012310718));
#60179=CARTESIAN_POINT('Ctrl Pts',(14.0085377331406,-3.02434882757141,10.6940011037195));
#60180=CARTESIAN_POINT('Ctrl Pts',(11.9305037500974,-0.841429197431721,
10.5370009763673));
#60181=CARTESIAN_POINT('Ctrl Pts',(12.604916689446,2.09604155530799,10.380000849015));
#60182=CARTESIAN_POINT('Ctrl Pts',(15.4270237144567,3.15395455427992,10.2230007216628));
#60183=CARTESIAN_POINT('Ctrl Pts',(17.8662145274442,1.38369506286337,10.0660005943105));
#60184=CARTESIAN_POINT('Ctrl Pts',(17.7352432511039,-1.62734158938471,9.90900046695827));
#60185=CARTESIAN_POINT('Ctrl Pts',(15.1515531237706,-3.17912310554764,9.752000339606));
#60186=CARTESIAN_POINT('Ctrl Pts',(12.4319638497434,-1.88015562464175,9.59500021225376));
#60187=CARTESIAN_POINT('Ctrl Pts',(12.0151572316991,1.10476605325709,9.4380000849015));
#60188=CARTESIAN_POINT('Ctrl Pts',(14.2748877575176,3.09903309907051,9.28099995754925));
#60189=CARTESIAN_POINT('Ctrl Pts',(17.1848333884845,2.31436759501462,9.123999830197));
#60190=CARTESIAN_POINT('Ctrl Pts',(18.1356179591903,-0.54561361705707,8.96699970284474));
#60191=CARTESIAN_POINT('Ctrl Pts',(16.274663824375,-2.9163378219851,8.80999957549249));
#60192=CARTESIAN_POINT('Ctrl Pts',(13.2707064095419,-2.67195394559781,8.65299944814023));
#60193=CARTESIAN_POINT('Ctrl Pts',(11.817423147442,-0.0316033214579261,
8.49599932078798));
#60194=CARTESIAN_POINT('Ctrl Pts',(13.2179870812285,2.63708629845826,8.33899919343572));
#60195=CARTESIAN_POINT('Ctrl Pts',(16.2164990952103,2.94107533850731,8.18199906608348));
#60196=CARTESIAN_POINT('Ctrl Pts',(18.1241646998305,0.607773905443812,8.02499893873121));
#60197=CARTESIAN_POINT('Ctrl Pts',(17.2303618464606,-2.27052421824958,7.86799881137898));
#60198=CARTESIAN_POINT('Ctrl Pts',(14.3365721278107,-3.11282149405098,7.71099868402671));
#60199=CARTESIAN_POINT('Ctrl Pts',(12.0376845476387,-1.16382187163074,7.55399855667447));
#60200=CARTESIAN_POINT('Ctrl Pts',(12.3951336511175,1.8287879857503,7.39699842932221));
#60201=CARTESIAN_POINT('Ctrl Pts',(15.088391402809,3.1815061164965,7.23999830196995));
#60202=CARTESIAN_POINT('Ctrl Pts',(17.7023877293502,1.68133718134365,7.0829981746177));
#60203=CARTESIAN_POINT('Ctrl Pts',(17.893127065655,-1.3265029163517,6.92599804726544));
#60204=CARTESIAN_POINT('Ctrl Pts',(15.4895715829936,-3.14485515809799,6.7689979199132));
#60205=CARTESIAN_POINT('Ctrl Pts',(12.6470126114897,-2.1431855409282,6.61199779256094));
#60206=CARTESIAN_POINT('Ctrl Pts',(11.9143999144365,0.780298978519449,6.45499766520869));
#60207=CARTESIAN_POINT('Ctrl Pts',(13.9486745921371,3.00408217741771,6.29799753785644));
#60208=CARTESIAN_POINT('Ctrl Pts',(16.9256825057651,2.53407556251617,6.14099741050418));
#60209=CARTESIAN_POINT('Ctrl Pts',(18.1759131113316,-0.208259934991238,
5.98399728315193));
#60210=CARTESIAN_POINT('Ctrl Pts',(16.5782706577155,-2.76384867084273,5.82699715579967));
#60211=CARTESIAN_POINT('Ctrl Pts',(13.5653803054279,-2.84106404628923,5.66999702844742));
#60212=CARTESIAN_POINT('Ctrl Pts',(11.8389222432929,-0.370677328850485,
5.51299690109516));
#60213=CARTESIAN_POINT('Ctrl Pts',(12.9470425851866,2.43211352025748,5.35599677374291));
#60214=CARTESIAN_POINT('Ctrl Pts',(15.8960507212661,3.05397713847976,5.19899664639066));
#60215=CARTESIAN_POINT('Ctrl Pts',(18.0415982494816,0.937364154516702,5.04199651903841));
#60216=CARTESIAN_POINT('Ctrl Pts',(17.459643977202,-2.01989749884988,4.88499639168616));
#60217=CARTESIAN_POINT('Ctrl Pts',(14.6722426504805,-3.16569257287314,4.7279962643339));
#60218=CARTESIAN_POINT('Ctrl Pts',(12.1784729871356,-1.4731805380298,4.57099613698165));
#60219=CARTESIAN_POINT('Ctrl Pts',(12.215322881631,1.54112605834992,4.41399600962939));
#60220=CARTESIAN_POINT('Ctrl Pts',(14.7481872905369,3.17196844909489,4.25699588227714));
#60221=CARTESIAN_POINT('Ctrl Pts',(17.5088738513129,1.96146864806794,4.09999575492489));
#60222=CARTESIAN_POINT('Ctrl Pts',(18.0158147471675,-1.0140076371251,3.94299562757263));
#60223=CARTESIAN_POINT('Ctrl Pts',(16.5566596891409,-2.38159377580301,3.83832887600446));
#60224=CARTESIAN_POINT('Ctrl Pts',(15.698066426161,-2.61113218593862,3.78599550022038));
#60225=CARTESIAN_POINT('Ctrl Pts',(17.1951971040191,1.87686343907872,12.2140044997796));
#60226=CARTESIAN_POINT('Ctrl Pts',(17.8123478989901,1.15503807360179,12.1616711239955));
#60227=CARTESIAN_POINT('Ctrl Pts',(18.2695195233736,-0.932473714789483,
12.0570043724274));
#60228=CARTESIAN_POINT('Ctrl Pts',(16.0220985187125,-3.24586736386177,11.9000042450751));
#60229=CARTESIAN_POINT('Ctrl Pts',(12.8583143384262,-2.6408513419267,11.7430041177229));
#60230=CARTESIAN_POINT('Ctrl Pts',(11.6149672212669,0.328384086517278,11.5860039903706));
#60231=CARTESIAN_POINT('Ctrl Pts',(13.4070235778454,3.00511912143942,11.4290038630183));
#60232=CARTESIAN_POINT('Ctrl Pts',(16.6275114271823,2.98612830149817,11.2720037356661));
#60233=CARTESIAN_POINT('Ctrl Pts',(18.3885970703671,0.289963978573797,11.1150036083139));
#60234=CARTESIAN_POINT('Ctrl Pts',(17.1110937259949,-2.66647876521353,10.9580034809616));
#60235=CARTESIAN_POINT('Ctrl Pts',(13.9405531465495,-3.23172848449065,10.8010033536093));
#60236=CARTESIAN_POINT('Ctrl Pts',(11.7200283335659,-0.899126013584159,
10.6440032262571));
#60237=CARTESIAN_POINT('Ctrl Pts',(12.4406857810575,2.23976716482285,10.4870030989048));
#60238=CARTESIAN_POINT('Ctrl Pts',(15.4563047387199,3.37022127835708,10.3300029715526));
#60239=CARTESIAN_POINT('Ctrl Pts',(18.0627509123809,1.47857505977427,10.1730028442003));
#60240=CARTESIAN_POINT('Ctrl Pts',(17.9227989331183,-1.73892843327666,10.0160027168481));
#60241=CARTESIAN_POINT('Ctrl Pts',(15.1619451243646,-3.39711563766634,9.85900258949583));
#60242=CARTESIAN_POINT('Ctrl Pts',(12.2558735618304,-2.00907793176401,9.70200246214356));
#60243=CARTESIAN_POINT('Ctrl Pts',(11.8104865060192,1.18051988264736,9.54500233479131));
#60244=CARTESIAN_POINT('Ctrl Pts',(14.2251667971895,3.31153385791409,9.38800220743906));
#60245=CARTESIAN_POINT('Ctrl Pts',(17.3346474556976,2.47306382524563,9.2310020800868));
#60246=CARTESIAN_POINT('Ctrl Pts',(18.3506273425917,-0.583026353208485,
9.07400195273456));
#60247=CARTESIAN_POINT('Ctrl Pts',(16.3620675471785,-3.11631116218659,8.91700182538229));
#60248=CARTESIAN_POINT('Ctrl Pts',(13.1521287149875,-2.85516987872383,8.76000169803006));
#60249=CARTESIAN_POINT('Ctrl Pts',(11.5991937918248,-0.0337703618144171,
8.60300157067778));
#60250=CARTESIAN_POINT('Ctrl Pts',(13.0957944213239,2.81791135635341,8.44600144332555));
#60251=CARTESIAN_POINT('Ctrl Pts',(16.2999144614232,3.1427449306896,8.28900131597327));
#60252=CARTESIAN_POINT('Ctrl Pts',(18.3383887330186,0.649448973758145,8.13200118862104));
#60253=CARTESIAN_POINT('Ctrl Pts',(17.3832978009075,-2.42621410729771,7.97500106126878));
#60254=CARTESIAN_POINT('Ctrl Pts',(14.2910808659327,-3.32626772340195,7.81800093391653));
#60255=CARTESIAN_POINT('Ctrl Pts',(11.8345585204434,-1.24362515961579,7.66100080656427));
#60256=CARTESIAN_POINT('Ctrl Pts',(12.2165179157807,1.95418801289184,7.50400067921202));
#60257=CARTESIAN_POINT('Ctrl Pts',(15.0944524029892,3.39966205172151,7.34700055185976));
#60258=CARTESIAN_POINT('Ctrl Pts',(17.8876905076099,1.7966265040084,7.19000042450751));
#60259=CARTESIAN_POINT('Ctrl Pts',(18.0915088438512,-1.41746124668302,7.03300029715526));
#60260=CARTESIAN_POINT('Ctrl Pts',(15.523141515798,-3.36049793640501,6.87600016980301));
#60261=CARTESIAN_POINT('Ctrl Pts',(12.4856682212804,-2.29014381443823,6.71900004245075));
#60262=CARTESIAN_POINT('Ctrl Pts',(11.7028202575859,0.833804094392522,6.5619999150985));
#60263=CARTESIAN_POINT('Ctrl Pts',(13.8765851888231,3.21007214974851,6.40499978774624));
#60264=CARTESIAN_POINT('Ctrl Pts',(17.0577265919963,2.70783717227864,6.247999660394));
#60265=CARTESIAN_POINT('Ctrl Pts',(18.3936855340856,-0.22254032271463,6.09099953304174));
#60266=CARTESIAN_POINT('Ctrl Pts',(16.6864927068848,-2.95336582703543,5.93399940568949));
#60267=CARTESIAN_POINT('Ctrl Pts',(13.4670084055473,-3.03587586225233,5.77699927833723));
#60268=CARTESIAN_POINT('Ctrl Pts',(11.6221670810891,-0.396094680375534,
5.61999915098498));
#60269=CARTESIAN_POINT('Ctrl Pts',(12.806271256009,2.59888359083319,5.46299902363272));
#60270=CARTESIAN_POINT('Ctrl Pts',(15.957492936352,3.26338840924436,5.30599889628048));
#60271=CARTESIAN_POINT('Ctrl Pts',(18.250160699591,1.00163923251032,5.14899876892821));
#60272=CARTESIAN_POINT('Ctrl Pts',(17.6283018117366,-2.15840190895786,4.99199864157597));
#60273=CARTESIAN_POINT('Ctrl Pts',(14.6497683227587,-3.38276417310961,4.8349985142237));
#60274=CARTESIAN_POINT('Ctrl Pts',(11.9850008259279,-1.57419655568344,4.67799838687146));
#60275=CARTESIAN_POINT('Ctrl Pts',(12.0243775183933,1.64680110163074,4.5209982595192));
#60276=CARTESIAN_POINT('Ctrl Pts',(14.7309204882355,3.38947038628386,4.36399813216696));
#60277=CARTESIAN_POINT('Ctrl Pts',(17.6809073792564,2.09596659076089,4.20699800481469));
#60278=CARTESIAN_POINT('Ctrl Pts',(18.2226092220303,-1.08353816018628,4.04999787746244));
#60279=CARTESIAN_POINT('Ctrl Pts',(16.663399873782,-2.54489970653575,3.94533112589427));
#60280=CARTESIAN_POINT('Ctrl Pts',(15.7459328543469,-2.79017756984216,3.89299775011019));
#60281=CARTESIAN_POINT('Ctrl Pts',(17.3360626576962,1.99730155693062,12.3210067496694));
#60282=CARTESIAN_POINT('Ctrl Pts',(17.9928159504458,1.22915673814361,12.2686733738853));
#60283=CARTESIAN_POINT('Ctrl Pts',(18.4793242270491,-0.9923104492142,12.1640066223172));
#60284=CARTESIAN_POINT('Ctrl Pts',(16.087686466823,-3.45415431109555,12.0070064949649));
#60285=CARTESIAN_POINT('Ctrl Pts',(12.7208826080511,-2.81031447841596,11.8500063676127));
#60286=CARTESIAN_POINT('Ctrl Pts',(11.3977500448602,0.349456456775644,11.6930062402604));
#60287=CARTESIAN_POINT('Ctrl Pts',(13.3048024582519,3.19795728077006,11.5360061129082));
#60288=CARTESIAN_POINT('Ctrl Pts',(16.7319486542021,3.17774782202826,11.3790059855559));
#60289=CARTESIAN_POINT('Ctrl Pts',(18.606042966971,0.308570934784431,11.2220058582037));
#60290=CARTESIAN_POINT('Ctrl Pts',(17.246562375271,-2.83758641060089,11.0650057308514));
#60291=CARTESIAN_POINT('Ctrl Pts',(13.8725685599584,-3.4391081414099,10.9080056034992));
#60292=CARTESIAN_POINT('Ctrl Pts',(11.5095529170344,-0.956822829736598,
10.7510054761469));
#60293=CARTESIAN_POINT('Ctrl Pts',(12.276454872669,2.38349277433771,10.5940053487947));
#60294=CARTESIAN_POINT('Ctrl Pts',(15.4855857629831,3.58648800243424,10.4370052214424));
#60295=CARTESIAN_POINT('Ctrl Pts',(18.2592872973176,1.57345505668517,10.2800050940901));
#60296=CARTESIAN_POINT('Ctrl Pts',(18.1103546151327,-1.85051527716861,10.1230049667379));
#60297=CARTESIAN_POINT('Ctrl Pts',(15.1723371249586,-3.61510816978504,9.96600483938563));
#60298=CARTESIAN_POINT('Ctrl Pts',(12.0797832739173,-2.13800023888626,9.80900471203338));
#60299=CARTESIAN_POINT('Ctrl Pts',(11.6058157803393,1.25627371203762,9.65200458468112));
#60300=CARTESIAN_POINT('Ctrl Pts',(14.1754458368614,3.52403461675767,9.49500445732887));
#60301=CARTESIAN_POINT('Ctrl Pts',(17.4844615229107,2.63176005547664,9.33800432997661));
#60302=CARTESIAN_POINT('Ctrl Pts',(18.565636725993,-0.620439089359897,9.18100420262437));
#60303=CARTESIAN_POINT('Ctrl Pts',(16.4494712699821,-3.31628450238807,9.0240040752721));
#60304=CARTESIAN_POINT('Ctrl Pts',(13.033551020433,-3.03838581184986,8.86700394791986));
#60305=CARTESIAN_POINT('Ctrl Pts',(11.3809644362075,-0.0359374021709085,
8.7100038205676));
#60306=CARTESIAN_POINT('Ctrl Pts',(12.9736017614192,2.99873641424856,8.55300369321535));
#60307=CARTESIAN_POINT('Ctrl Pts',(16.383329827636,3.34441452287188,8.39600356586309));
#60308=CARTESIAN_POINT('Ctrl Pts',(18.5526127662067,0.691124042072478,8.23900343851084));
#60309=CARTESIAN_POINT('Ctrl Pts',(17.5362337553543,-2.58190399634584,8.08200331115859));
#60310=CARTESIAN_POINT('Ctrl Pts',(14.2455896040548,-3.53971395275292,7.92500318380633));
#60311=CARTESIAN_POINT('Ctrl Pts',(11.6314324932481,-1.32342844760082,7.76800305645409));
#60312=CARTESIAN_POINT('Ctrl Pts',(12.0379021804438,2.07958804003338,7.61100292910183));
#60313=CARTESIAN_POINT('Ctrl Pts',(15.1005134031695,3.61781798694653,7.45400280174957));
#60314=CARTESIAN_POINT('Ctrl Pts',(18.0729932858696,1.91191582667314,7.29700267439733));
#60315=CARTESIAN_POINT('Ctrl Pts',(18.2898906220475,-1.50841957701434,7.14000254704506));
#60316=CARTESIAN_POINT('Ctrl Pts',(15.5567114486024,-3.57614071471203,6.98300241969282));
#60317=CARTESIAN_POINT('Ctrl Pts',(12.3243238310711,-2.43710208794826,6.82600229234056));
#60318=CARTESIAN_POINT('Ctrl Pts',(11.4912406007353,0.887309210265594,6.66900216498831));
#60319=CARTESIAN_POINT('Ctrl Pts',(13.8044957855091,3.41606212207931,6.51200203763605));
#60320=CARTESIAN_POINT('Ctrl Pts',(17.1897706782275,2.88159878204111,6.35500191028381));
#60321=CARTESIAN_POINT('Ctrl Pts',(18.6114579568395,-0.236820710438023,
6.19800178293155));
#60322=CARTESIAN_POINT('Ctrl Pts',(16.7947147560542,-3.14288298322814,6.04100165557929));
#60323=CARTESIAN_POINT('Ctrl Pts',(13.3686365056666,-3.23068767821543,5.88400152822705));
#60324=CARTESIAN_POINT('Ctrl Pts',(11.4054119188853,-0.421512031900586,
5.72700140087479));
#60325=CARTESIAN_POINT('Ctrl Pts',(12.6654999268314,2.7656536614089,5.57000127352253));
#60326=CARTESIAN_POINT('Ctrl Pts',(16.0189351514379,3.47279968000896,5.41300114617029));
#60327=CARTESIAN_POINT('Ctrl Pts',(18.4587231497003,1.06591431050395,5.25600101881802));
#60328=CARTESIAN_POINT('Ctrl Pts',(17.7969596462713,-2.29690631906584,5.09900089146578));
#60329=CARTESIAN_POINT('Ctrl Pts',(14.6272939950368,-3.59983577334609,4.94200076411352));
#60330=CARTESIAN_POINT('Ctrl Pts',(11.7915286647202,-1.67521257333708,4.78500063676127));
#60331=CARTESIAN_POINT('Ctrl Pts',(11.8334321551556,1.75247614491157,4.62800050940901));
#60332=CARTESIAN_POINT('Ctrl Pts',(14.713653685934,3.60697232347283,4.47100038205677));
#60333=CARTESIAN_POINT('Ctrl Pts',(17.8529409071999,2.23046453345384,4.3140002547045));
#60334=CARTESIAN_POINT('Ctrl Pts',(18.4294036968932,-1.15306868324745,4.15700012735226));
#60335=CARTESIAN_POINT('Ctrl Pts',(16.7701400584231,-2.7082056372685,4.05233337578409));
#60336=CARTESIAN_POINT('Ctrl Pts',(15.7937992825329,-2.9692229537457,4.));
#60337=CARTESIAN_POINT('Ctrl Pts',(16.9134659966651,1.63598720337493,12.));
#60338=CARTESIAN_POINT('Ctrl Pts',(16.9751046175812,1.57806203522303,12.));
#60339=CARTESIAN_POINT('Ctrl Pts',(17.0333781400082,1.51698823254714,12.));
#60340=CARTESIAN_POINT('Ctrl Pts',(17.0882869575319,1.45315007481724,12.));
#60341=CARTESIAN_POINT('Ctrl Pts',(17.144646063235,1.38762578124011,12.));
#60342=CARTESIAN_POINT('Ctrl Pts',(17.1974608152615,1.31918874417436,12.));
#60343=CARTESIAN_POINT('Ctrl Pts',(17.246706209466,1.24820595309377,12.));
#60344=CARTESIAN_POINT('Ctrl Pts',(17.2968789923958,1.17588641486748,12.));
#60345=CARTESIAN_POINT('Ctrl Pts',(17.3433471915708,1.10092373974675,12.));
#60346=CARTESIAN_POINT('Ctrl Pts',(17.3860513180704,1.02366428011772,12.));
#60347=CARTESIAN_POINT('Ctrl Pts',(17.4053930048836,0.988671683523578,12.));
#60348=CARTESIAN_POINT('Ctrl Pts',(17.4239620441889,0.953207420756028,12.));
#60349=CARTESIAN_POINT('Ctrl Pts',(17.4417503295423,0.917301461090561,12.));
#60350=CARTESIAN_POINT('Ctrl Pts',(17.4518550628932,0.896904883178727,12.));
#60351=CARTESIAN_POINT('Ctrl Pts',(17.4617078263978,0.876365752925188,12.));
#60352=CARTESIAN_POINT('Ctrl Pts',(17.4713068826732,0.855689404786285,12.));
#60353=CARTESIAN_POINT('Ctrl Pts',(17.4795241183999,0.837989495363037,12.));
#60354=CARTESIAN_POINT('Ctrl Pts',(17.4875575606575,0.820183889043797,12.));
#60355=CARTESIAN_POINT('Ctrl Pts',(17.4953933345483,0.802305631697034,12.));
#60356=CARTESIAN_POINT('Ctrl Pts',(17.5320009593848,0.718780947752926,12.));
#60357=CARTESIAN_POINT('Ctrl Pts',(17.5643466650844,0.633572893252199,12.));
#60358=CARTESIAN_POINT('Ctrl Pts',(17.5924032599934,0.547079296293481,12.));
#60359=CARTESIAN_POINT('Ctrl Pts',(17.6209190605514,0.45917004827483,12.));
#60360=CARTESIAN_POINT('Ctrl Pts',(17.6450046970528,0.369932078122487,12.));
#60361=CARTESIAN_POINT('Ctrl Pts',(17.6645925974806,0.27974597155399,12.));
#60362=CARTESIAN_POINT('Ctrl Pts',(17.6832979692358,0.193623180766213,12.));
#60363=CARTESIAN_POINT('Ctrl Pts',(17.6979018128389,0.106634841931331,12.));
#60364=CARTESIAN_POINT('Ctrl Pts',(17.7083066964275,0.0190916104279826,
12.));
#60365=CARTESIAN_POINT('Ctrl Pts',(17.7128967523775,-0.0195275944118574,
12.));
#60366=CARTESIAN_POINT('Ctrl Pts',(17.7166691326112,-0.0582549851430788,
12.));
#60367=CARTESIAN_POINT('Ctrl Pts',(17.7196128778618,-0.0970645844891166,
12.));
#60368=CARTESIAN_POINT('Ctrl Pts',(17.720985220376,-0.115157204130783,12.));
#60369=CARTESIAN_POINT('Ctrl Pts',(17.7221774501012,-0.13326769426837,12.));
#60370=CARTESIAN_POINT('Ctrl Pts',(17.7231883308136,-0.151393437782305,
12.));
#60371=CARTESIAN_POINT('Ctrl Pts',(17.724162595519,-0.168862632662539,12.));
#60372=CARTESIAN_POINT('Ctrl Pts',(17.7249684090533,-0.186348823197974,
12.));
#60373=CARTESIAN_POINT('Ctrl Pts',(17.7256040109254,-0.203825085573831,
12.));
#60374=CARTESIAN_POINT('Ctrl Pts',(17.7290683171088,-0.299078303780242,
12.));
#60375=CARTESIAN_POINT('Ctrl Pts',(17.7274898676139,-0.394183686637061,
12.));
#60376=CARTESIAN_POINT('Ctrl Pts',(17.7208064378308,-0.488742644592356,
12.));
#60377=CARTESIAN_POINT('Ctrl Pts',(17.71415791669,-0.582807705707687,12.));
#60378=CARTESIAN_POINT('Ctrl Pts',(17.7024579548962,-0.676332990245415,
12.));
#60379=CARTESIAN_POINT('Ctrl Pts',(17.6855973100545,-0.768943912339204,
12.));
#60380=CARTESIAN_POINT('Ctrl Pts',(17.6690987547922,-0.859565975160523,
12.));
#60381=CARTESIAN_POINT('Ctrl Pts',(17.6476591367551,-0.949313458601225,
12.));
#60382=CARTESIAN_POINT('Ctrl Pts',(17.6215530748909,-1.03794459575461,12.));
#60383=CARTESIAN_POINT('Ctrl Pts',(17.6062284518588,-1.08997231149527,12.));
#60384=CARTESIAN_POINT('Ctrl Pts',(17.5892948213721,-1.14161533429799,12.));
#60385=CARTESIAN_POINT('Ctrl Pts',(17.5707996132467,-1.19282361176805,12.));
#60386=CARTESIAN_POINT('Ctrl Pts',(17.5660385338913,-1.20600576527691,12.));
#60387=CARTESIAN_POINT('Ctrl Pts',(17.5611731178881,-1.21916127939291,12.));
#60388=CARTESIAN_POINT('Ctrl Pts',(17.5562068240413,-1.23228215182306,12.));
#60389=CARTESIAN_POINT('Ctrl Pts',(17.5231582789659,-1.31959590274395,12.));
#60390=CARTESIAN_POINT('Ctrl Pts',(17.4857269461903,-1.40516846103908,12.));
#60391=CARTESIAN_POINT('Ctrl Pts',(17.4442438276358,-1.48876399852657,12.));
#60392=CARTESIAN_POINT('Ctrl Pts',(17.4011939593262,-1.57551680317371,12.));
#60393=CARTESIAN_POINT('Ctrl Pts',(17.3537803586004,-1.6601411473433,12.));
#60394=CARTESIAN_POINT('Ctrl Pts',(17.302316868041,-1.74237153203792,12.));
#60395=CARTESIAN_POINT('Ctrl Pts',(17.2502282381553,-1.82560078887907,12.));
#60396=CARTESIAN_POINT('Ctrl Pts',(17.1939903374979,-1.90637839472423,12.));
#60397=CARTESIAN_POINT('Ctrl Pts',(17.133876364298,-1.98441530832993,12.));
#60398=CARTESIAN_POINT('Ctrl Pts',(17.0944014617075,-2.03565962639887,12.));
#60399=CARTESIAN_POINT('Ctrl Pts',(17.0532540884055,-2.08572182092047,12.));
#60400=CARTESIAN_POINT('Ctrl Pts',(17.0105008848643,-2.13451422415292,12.));
#60401=CARTESIAN_POINT('Ctrl Pts',(16.9990423392555,-2.14759137233113,12.));
#60402=CARTESIAN_POINT('Ctrl Pts',(16.9874683992165,-2.16057727630897,12.));
#60403=CARTESIAN_POINT('Ctrl Pts',(16.9757802548447,-2.17347017426791,12.));
#60404=CARTESIAN_POINT('Ctrl Pts',(16.9646250327531,-2.18577521906894,12.));
#60405=CARTESIAN_POINT('Ctrl Pts',(16.953371454143,-2.19798925370335,12.));
#60406=CARTESIAN_POINT('Ctrl Pts',(16.942023959817,-2.2101077517839,12.));
#60407=CARTESIAN_POINT('Ctrl Pts',(16.8702005619852,-2.28681117932109,12.));
#60408=CARTESIAN_POINT('Ctrl Pts',(16.7945813632066,-2.35973107336475,12.));
#60409=CARTESIAN_POINT('Ctrl Pts',(16.7155099454751,-2.42853427108366,12.));
#60410=CARTESIAN_POINT('Ctrl Pts',(16.6562063821765,-2.48013666937285,12.));
#60411=CARTESIAN_POINT('Ctrl Pts',(16.5949596324728,-2.52942316838901,12.));
#60412=CARTESIAN_POINT('Ctrl Pts',(16.5318955908763,-2.57624166180053,12.));
#60413=CARTESIAN_POINT('Ctrl Pts',(16.509253132243,-2.59305133294597,12.));
#60414=CARTESIAN_POINT('Ctrl Pts',(16.4863762692883,-2.60954274193113,12.));
#60415=CARTESIAN_POINT('Ctrl Pts',(16.4632703841368,-2.62570843265804,12.));
#60416=CARTESIAN_POINT('Ctrl Pts',(16.4439550552025,-2.63922211680365,12.));
#60417=CARTESIAN_POINT('Ctrl Pts',(16.4244771453842,-2.65250971655999,12.));
#60418=CARTESIAN_POINT('Ctrl Pts',(16.4048604457735,-2.66555338685653,12.));
#60419=CARTESIAN_POINT('Ctrl Pts',(16.3198883986288,-2.72205358257614,12.));
#60420=CARTESIAN_POINT('Ctrl Pts',(16.2322397460524,-2.7740341002851,12.));
#60421=CARTESIAN_POINT('Ctrl Pts',(16.1422018474634,-2.82118285115376,12.));
#60422=CARTESIAN_POINT('Ctrl Pts',(16.0701250286698,-2.85892620174232,12.));
#60423=CARTESIAN_POINT('Ctrl Pts',(15.9965161480314,-2.89357290485328,12.));
#60424=CARTESIAN_POINT('Ctrl Pts',(15.9215058272316,-2.92494553699154,12.));
#60425=CARTESIAN_POINT('Ctrl Pts',(15.8800022019638,-2.94230418782848,12.));
#60426=CARTESIAN_POINT('Ctrl Pts',(15.8380692864041,-2.95866019100725,12.));
#60427=CARTESIAN_POINT('Ctrl Pts',(15.795740524146,-2.97402278592473,12.));
#60428=CARTESIAN_POINT('Ctrl Pts',(12.4833920687165,-0.00213593309729046,
10.387416697508));
#60429=CARTESIAN_POINT('Ctrl Pts',(12.4814996767346,-0.226800666605093,
10.4016107071645));
#60430=CARTESIAN_POINT('Ctrl Pts',(12.5091661046464,-0.451007239373056,
10.415804716821));
#60431=CARTESIAN_POINT('Ctrl Pts',(12.5682644306803,-0.666597124996037,
10.4299987264775));
#60432=CARTESIAN_POINT('Ctrl Pts',(12.7861602176632,-1.46147797773692,10.4823321022615));
#60433=CARTESIAN_POINT('Ctrl Pts',(13.4313412686974,-2.13922357419454,10.5346654780456));
#60434=CARTESIAN_POINT('Ctrl Pts',(14.2145374788331,-2.39597875638779,10.5869988538297));
#60435=CARTESIAN_POINT('Ctrl Pts',(14.9977336889687,-2.65273393858105,10.6393322296138));
#60436=CARTESIAN_POINT('Ctrl Pts',(15.9189450582056,-2.48849870650994,10.6916656053979));
#60437=CARTESIAN_POINT('Ctrl Pts',(16.5651422177769,-1.97687883370916,10.743998981182));
#60438=CARTESIAN_POINT('Ctrl Pts',(17.2113393773482,-1.46525896090837,10.7963323569661));
#60439=CARTESIAN_POINT('Ctrl Pts',(17.5825223272538,-0.60625444737792,10.8486657327501));
#60440=CARTESIAN_POINT('Ctrl Pts',(17.5122690848705,0.214937675101548,10.9009991085342));
#60441=CARTESIAN_POINT('Ctrl Pts',(17.4420158424871,1.03612979758102,10.9533324843183));
#60442=CARTESIAN_POINT('Ctrl Pts',(16.9303264078149,1.8195095290095,11.0056658601024));
#60443=CARTESIAN_POINT('Ctrl Pts',(16.206619831127,2.2139583184471,11.0579992358865));
#60444=CARTESIAN_POINT('Ctrl Pts',(15.4829132544392,2.60840710788471,11.1103326116706));
#60445=CARTESIAN_POINT('Ctrl Pts',(14.5471895357358,2.61392495533142,11.1626659874547));
#60446=CARTESIAN_POINT('Ctrl Pts',(13.8189836358921,2.22781663625852,11.2149993632387));
#60447=CARTESIAN_POINT('Ctrl Pts',(13.0907777360484,1.84170831718561,11.2673327390228));
#60448=CARTESIAN_POINT('Ctrl Pts',(12.5700896550643,1.06397383159308,11.3196661148069));
#60449=CARTESIAN_POINT('Ctrl Pts',(12.4903749854216,0.243745852972027,11.371999490591));
#60450=CARTESIAN_POINT('Ctrl Pts',(12.4825471092477,0.163200539545801,11.3771385595633));
#60451=CARTESIAN_POINT('Ctrl Pts',(12.4789715321031,0.0822454620963692,
11.3822776285357));
#60452=CARTESIAN_POINT('Ctrl Pts',(12.4794948718273,0.00124609658704006,
11.387416697508));
#60453=CARTESIAN_POINT('Ctrl Pts',(14.2062007174671,-2.96922295374568,12.));
#60454=CARTESIAN_POINT('Ctrl Pts',(13.2298599415769,-2.70820563726846,11.9476666242159));
#60455=CARTESIAN_POINT('Ctrl Pts',(11.5705939465555,-1.15308308242658,11.8429998726477));
#60456=CARTESIAN_POINT('Ctrl Pts',(12.1470611574329,2.23047193499529,11.6859997452955));
#60457=CARTESIAN_POINT('Ctrl Pts',(15.2863460006058,3.60696666543133,11.5289996179432));
#60458=CARTESIAN_POINT('Ctrl Pts',(18.1665668486981,1.75247841941832,11.371999490591));
#60459=CARTESIAN_POINT('Ctrl Pts',(18.2084706556688,-1.6752137223659,11.2149993632387));
#60460=CARTESIAN_POINT('Ctrl Pts',(15.3727057323674,-3.59983386165072,11.0579992358865));
#60461=CARTESIAN_POINT('Ctrl Pts',(12.2030412422492,-2.29690621757914,10.9009991085342));
#60462=CARTESIAN_POINT('Ctrl Pts',(11.5412777161188,1.06591431606771,10.743998981182));
#60463=CARTESIAN_POINT('Ctrl Pts',(13.9810651784412,3.47279856287599,10.5869988538297));
#60464=CARTESIAN_POINT('Ctrl Pts',(17.3344994031312,2.76565299665532,10.4299987264775));
#60465=CARTESIAN_POINT('Ctrl Pts',(18.5945871152999,-0.421511967551375,
10.2729985991252));
#60466=CARTESIAN_POINT('Ctrl Pts',(16.6313630370479,-3.23068676566348,10.115998471773));
#60467=CARTESIAN_POINT('Ctrl Pts',(13.205285741413,-3.14288213812672,9.9589983444207));
#60468=CARTESIAN_POINT('Ctrl Pts',(11.388543028433,-0.236820637232293,9.80199821706845));
#60469=CARTESIAN_POINT('Ctrl Pts',(12.8102299232355,2.88159798857394,9.6449980897162));
#60470=CARTESIAN_POINT('Ctrl Pts',(16.1955038860992,3.41606118929613,9.48799796236394));
#60471=CARTESIAN_POINT('Ctrl Pts',(18.5087584392439,0.887308966009096,9.3309978350117));
#60472=CARTESIAN_POINT('Ctrl Pts',(17.6756754360527,-2.43710142000481,9.17399770765943));
#60473=CARTESIAN_POINT('Ctrl Pts',(14.4432887039958,-3.57613973602564,9.0169975803072));
#60474=CARTESIAN_POINT('Ctrl Pts',(11.7101102785552,-1.50841916383422,8.85999745295492));
#60475=CARTESIAN_POINT('Ctrl Pts',(11.9270075555053,1.91191530312036,8.70299732560268));
#60476=CARTESIAN_POINT('Ctrl Pts',(14.8994866243195,3.61781699652394,8.54599719825042));
#60477=CARTESIAN_POINT('Ctrl Pts',(17.9620970086125,2.07958747065415,8.38899707089818));
#60478=CARTESIAN_POINT('Ctrl Pts',(18.3685665845007,-1.32342808525659,8.23199694354591));
#60479=CARTESIAN_POINT('Ctrl Pts',(15.7544101894084,-3.53971298366467,8.07499681619367));
#60480=CARTESIAN_POINT('Ctrl Pts',(12.4637669390099,-2.58190328946754,7.91799668884141));
#60481=CARTESIAN_POINT('Ctrl Pts',(11.4473882064255,0.691123852849571,7.76099656148916));
#60482=CARTESIAN_POINT('Ctrl Pts',(13.6166705510885,3.34441360725337,7.60399643413689));
#60483=CARTESIAN_POINT('Ctrl Pts',(17.0263976837988,2.99873559323853,7.44699630678466));
#60484=CARTESIAN_POINT('Ctrl Pts',(18.6190345729722,-0.0359373922966709,
7.2899961794324));
#60485=CARTESIAN_POINT('Ctrl Pts',(16.9664484412042,-3.03838498006983,7.13299605208014));
#60486=CARTESIAN_POINT('Ctrl Pts',(13.5505291268344,-3.3162835943375,6.97599592472789));
#60487=CARTESIAN_POINT('Ctrl Pts',(11.4343642502377,-0.620438919723572,
6.81899579737564));
#60488=CARTESIAN_POINT('Ctrl Pts',(12.5155391572145,2.63175933537736,6.66199567002338));
#60489=CARTESIAN_POINT('Ctrl Pts',(15.824553937525,3.52403365117268,6.50499554267113));
#60490=CARTESIAN_POINT('Ctrl Pts',(18.3941832901488,1.25627336953411,6.34799541531888));
#60491=CARTESIAN_POINT('Ctrl Pts',(17.9202159270872,-2.13799965619268,6.19099528796662));
#60492=CARTESIAN_POINT('Ctrl Pts',(14.8276629212552,-3.61510717519363,6.03399516061437));
#60493=CARTESIAN_POINT('Ctrl Pts',(11.889646238299,-1.85051477939823,5.87699503326212));
#60494=CARTESIAN_POINT('Ctrl Pts',(11.7407135913467,1.57345464202167,5.71999490590987));
#60495=CARTESIAN_POINT('Ctrl Pts',(14.5144143770745,3.58648699137295,5.56299477855761));
#60496=CARTESIAN_POINT('Ctrl Pts',(17.7235443678513,2.3834921742297,5.40599465120536));
#60497=CARTESIAN_POINT('Ctrl Pts',(18.4904461542425,-0.956822661448993,
5.2489945238531));
#60498=CARTESIAN_POINT('Ctrl Pts',(16.1274310791049,-3.43910703392132,5.09199439650085));
#60499=CARTESIAN_POINT('Ctrl Pts',(12.7534383414036,-2.83758592474999,4.9349942691486));
#60500=CARTESIAN_POINT('Ctrl Pts',(11.3939578227468,0.308571354444121,4.77799414179634));
#60501=CARTESIAN_POINT('Ctrl Pts',(13.2680522040149,3.17774609218688,4.62099401444409));
#60502=CARTESIAN_POINT('Ctrl Pts',(16.6951963308219,3.19795784272698,4.46399388709183));
#60503=CARTESIAN_POINT('Ctrl Pts',(18.6022504225887,0.349454018091392,4.30699375973959));
#60504=CARTESIAN_POINT('Ctrl Pts',(17.2791139286761,-2.8103099931699,4.14999363238733));
#60505=CARTESIAN_POINT('Ctrl Pts',(13.9123194271849,-3.45415924122653,3.99299350503508));
#60506=CARTESIAN_POINT('Ctrl Pts',(11.5206656746196,-0.992299917670973,
3.83599337768282));
#60507=CARTESIAN_POINT('Ctrl Pts',(12.0071840495542,1.22915673814367,3.73132662611465));
#60508=CARTESIAN_POINT('Ctrl Pts',(12.6639373423039,1.99730155693067,3.67899325033057));
#60509=CARTESIAN_POINT('Ctrl Pts',(14.254067145653,-2.79017756984214,12.1070022498898));
#60510=CARTESIAN_POINT('Ctrl Pts',(13.336600126218,-2.54489970653572,12.0546688741057));
#60511=CARTESIAN_POINT('Ctrl Pts',(11.7773885635194,-1.08355169108889,11.9500021225376));
#60512=CARTESIAN_POINT('Ctrl Pts',(12.3190945608781,2.0959735459863,11.7930019951853));
#60513=CARTESIAN_POINT('Ctrl Pts',(15.2690792172061,3.38946506942463,11.636001867833));
#60514=CARTESIAN_POINT('Ctrl Pts',(17.9756215455284,1.64680323898379,11.4790017404808));
#60515=CARTESIAN_POINT('Ctrl Pts',(18.014998535442,-1.57419763542533,11.3220016131285));
#60516=CARTESIAN_POINT('Ctrl Pts',(15.3502314210832,-3.38276237669027,11.1650014857763));
#60517=CARTESIAN_POINT('Ctrl Pts',(12.3716990232057,-2.15840181359085,11.008001358424));
#60518=CARTESIAN_POINT('Ctrl Pts',(11.7498401140189,1.00163923773859,10.8510012310718));
#60519=CARTESIAN_POINT('Ctrl Pts',(14.0425073736352,3.26338735947497,10.6940011037195));
#60520=CARTESIAN_POINT('Ctrl Pts',(17.1937281143572,2.59888296616453,10.5370009763673));
#60521=CARTESIAN_POINT('Ctrl Pts',(18.3778320113351,-0.396094619906611,
10.380000849015));
#60522=CARTESIAN_POINT('Ctrl Pts',(16.5329911647418,-3.03587500472764,10.2230007216628));
#60523=CARTESIAN_POINT('Ctrl Pts',(13.3135077605849,-2.95336503289398,10.0660005943105));
#60524=CARTESIAN_POINT('Ctrl Pts',(11.6063153917746,-0.222540253923235,
9.90900046695825));
#60525=CARTESIAN_POINT('Ctrl Pts',(12.9422739731982,2.70783642665787,9.75200033960602));
#60526=CARTESIAN_POINT('Ctrl Pts',(16.1234145025873,3.21007127321255,9.59500021225374));
#60527=CARTESIAN_POINT('Ctrl Pts',(18.297178840283,0.83380386486479,9.43800008490151));
#60528=CARTESIAN_POINT('Ctrl Pts',(17.5143310900362,-2.29014318677205,9.28099995754924));
#60529=CARTESIAN_POINT('Ctrl Pts',(14.4768586275985,-3.36049701673381,9.12399983019701));
#60530=CARTESIAN_POINT('Ctrl Pts',(11.9084920024447,-1.41746085841783,8.96699970284473));
#60531=CARTESIAN_POINT('Ctrl Pts',(12.1123102830297,1.79662601202607,8.8099995754925));
#60532=CARTESIAN_POINT('Ctrl Pts',(14.9055476228422,3.39966112102182,8.65299944814023));
#60533=CARTESIAN_POINT('Ctrl Pts',(17.7834813221759,1.95418747784641,8.49599932078799));
#60534=CARTESIAN_POINT('Ctrl Pts',(18.1654406129175,-1.24362481912106,8.33899919343572));
#60535=CARTESIAN_POINT('Ctrl Pts',(15.7089189399847,-3.32626681275013,8.18199906608348));
#60536=CARTESIAN_POINT('Ctrl Pts',(12.6167028515863,-2.42621344304447,8.02499893873122));
#60537=CARTESIAN_POINT('Ctrl Pts',(11.6616121809635,0.649448795945457,7.86799881137897));
#60538=CARTESIAN_POINT('Ctrl Pts',(13.7000858944641,3.14274407028327,7.71099868402671));
#60539=CARTESIAN_POINT('Ctrl Pts',(16.9042050573477,2.81791058485063,7.55399855667447));
#60540=CARTESIAN_POINT('Ctrl Pts',(18.4008052771018,-0.033770352535599,
7.3969984293222));
#60541=CARTESIAN_POINT('Ctrl Pts',(16.8478707791132,-2.85516909710049,7.23999830196996));
#60542=CARTESIAN_POINT('Ctrl Pts',(13.6379328257098,-3.11631030889185,7.08299817461769));
#60543=CARTESIAN_POINT('Ctrl Pts',(11.6493735747719,-0.583026193801301,
6.92599804726545));
#60544=CARTESIAN_POINT('Ctrl Pts',(12.6653531834158,2.47306314856864,6.76899791991319));
#60545=CARTESIAN_POINT('Ctrl Pts',(15.7748329908015,3.31153295055427,6.61199779256095));
#60546=CARTESIAN_POINT('Ctrl Pts',(18.1895126205188,1.18051956079695,6.45499766520868));
#60547=CARTESIAN_POINT('Ctrl Pts',(17.7441256873539,-2.00907738420709,6.29799753785643));
#60548=CARTESIAN_POINT('Ctrl Pts',(14.8380549190625,-3.39711470304921,6.14099741050418));
#60549=CARTESIAN_POINT('Ctrl Pts',(12.0772018688511,-1.73892796552204,5.98399728315193));
#60550=CARTESIAN_POINT('Ctrl Pts',(11.9372499226966,1.47857467011516,5.82699715579967));
#60551=CARTESIAN_POINT('Ctrl Pts',(14.5436953928922,3.3702203282632,5.66999702844742));
#60552=CARTESIAN_POINT('Ctrl Pts',(17.5593135052598,2.2397666009016,5.51299690109516));
#60553=CARTESIAN_POINT('Ctrl Pts',(18.2799707937134,-0.89912585544437,5.35599677374292));
#60554=CARTESIAN_POINT('Ctrl Pts',(16.0594465142784,-3.23172744378409,5.19899664639066));
#60555=CARTESIAN_POINT('Ctrl Pts',(12.888906947464,-2.66647830865965,5.04199651903841));
#60556=CARTESIAN_POINT('Ctrl Pts',(11.6114036717303,0.289964372927834,4.88499639168615));
#60557=CARTESIAN_POINT('Ctrl Pts',(13.3724893792839,2.98612667596695,4.72799626433391));
#60558=CARTESIAN_POINT('Ctrl Pts',(16.5929752842478,3.0051196495101,4.57099613698165));
#60559=CARTESIAN_POINT('Ctrl Pts',(18.3850332179946,0.328381794886706,4.41399600962939));
#60560=CARTESIAN_POINT('Ctrl Pts',(17.1416824071377,-2.64084712714285,4.25699588227714));
#60561=CARTESIAN_POINT('Ctrl Pts',(13.9779070198844,-3.24587199670379,4.09999575492489));
#60562=CARTESIAN_POINT('Ctrl Pts',(11.7304709872286,-0.932463818302713,
3.94299562757263));
#60563=CARTESIAN_POINT('Ctrl Pts',(12.1876521010099,1.15503807360185,3.83832887600446));
#60564=CARTESIAN_POINT('Ctrl Pts',(12.8048028959809,1.87686343907877,3.78599550022038));
#60565=CARTESIAN_POINT('Ctrl Pts',(14.3019335738389,-2.6111321859386,12.2140044997796));
#60566=CARTESIAN_POINT('Ctrl Pts',(13.4433403108591,-2.38159377580297,12.1616711239955));
#60567=CARTESIAN_POINT('Ctrl Pts',(11.9841831804832,-1.0140202997512,12.0570043724274));
#60568=CARTESIAN_POINT('Ctrl Pts',(12.4911279643235,1.96147515697731,11.9000042450751));
#60569=CARTESIAN_POINT('Ctrl Pts',(15.2518124338064,3.17196347341793,11.7430041177229));
#60570=CARTESIAN_POINT('Ctrl Pts',(17.7846762423587,1.54112805854926,11.5860039903706));
#60571=CARTESIAN_POINT('Ctrl Pts',(17.8215264152151,-1.47318154848477,11.4290038630184));
#60572=CARTESIAN_POINT('Ctrl Pts',(15.3277571097989,-3.16569089172983,11.2720037356661));
#60573=CARTESIAN_POINT('Ctrl Pts',(12.5403568041622,-2.01989740960257,11.1150036083138));
#60574=CARTESIAN_POINT('Ctrl Pts',(11.958402511919,0.937364159409468,10.9580034809616));
#60575=CARTESIAN_POINT('Ctrl Pts',(14.1039495688293,3.05397615607396,10.8010033536093));
#60576=CARTESIAN_POINT('Ctrl Pts',(17.0529568255832,2.43211293567374,10.6440032262571));
#60577=CARTESIAN_POINT('Ctrl Pts',(18.1610769073704,-0.370677272261844,
10.4870030989048));
#60578=CARTESIAN_POINT('Ctrl Pts',(16.4346192924356,-2.8410632437918,10.3300029715526));
#60579=CARTESIAN_POINT('Ctrl Pts',(13.4217297797568,-2.76384792766124,10.1730028442003));
#60580=CARTESIAN_POINT('Ctrl Pts',(11.8240877551162,-0.208259870614178,
10.0160027168481));
#60581=CARTESIAN_POINT('Ctrl Pts',(13.0743180231609,2.5340748647418,9.85900258949582));
#60582=CARTESIAN_POINT('Ctrl Pts',(16.0513251190755,3.00408135712897,9.70200246214356));
#60583=CARTESIAN_POINT('Ctrl Pts',(18.085599241322,0.780298763720488,9.54500233479132));
#60584=CARTESIAN_POINT('Ctrl Pts',(17.3529867440197,-2.14318495353929,9.38800220743906));
#60585=CARTESIAN_POINT('Ctrl Pts',(14.5104285512012,-3.14485429744199,9.23100208008681));
#60586=CARTESIAN_POINT('Ctrl Pts',(12.1068737263342,-1.32650255300144,9.07400195273456));
#60587=CARTESIAN_POINT('Ctrl Pts',(12.2976130105542,1.68133672093178,8.9170018253823));
#60588=CARTESIAN_POINT('Ctrl Pts',(14.9116086213649,3.1815052455197,8.76000169803005));
#60589=CARTESIAN_POINT('Ctrl Pts',(17.6048656357394,1.82878748503868,8.60300157067779));
#60590=CARTESIAN_POINT('Ctrl Pts',(17.9623146413344,-1.16382155298553,8.44600144332554));
#60591=CARTESIAN_POINT('Ctrl Pts',(15.663427690561,-3.11282064183558,8.28900131597329));
#60592=CARTESIAN_POINT('Ctrl Pts',(12.7696387641627,-2.27052359662139,8.13200118862103));
#60593=CARTESIAN_POINT('Ctrl Pts',(11.8758361555014,0.607773739041346,7.97500106126878));
#60594=CARTESIAN_POINT('Ctrl Pts',(13.7835012378397,2.94107453331316,7.81800093391652));
#60595=CARTESIAN_POINT('Ctrl Pts',(16.7820124308966,2.63708557646273,7.66100080656428));
#60596=CARTESIAN_POINT('Ctrl Pts',(18.1825759812315,-0.031603312774529,
7.50400067921202));
#60597=CARTESIAN_POINT('Ctrl Pts',(16.7292931170223,-2.67195321413115,7.34700055185977));
#60598=CARTESIAN_POINT('Ctrl Pts',(13.7253365245851,-2.9163370234462,7.1900004245075));
#60599=CARTESIAN_POINT('Ctrl Pts',(11.8643828993062,-0.545613467879027,
7.03300029715527));
#60600=CARTESIAN_POINT('Ctrl Pts',(12.8151672096171,2.31436696175991,6.876000169803));
#60601=CARTESIAN_POINT('Ctrl Pts',(15.725112044078,3.09903224993587,6.71900004245076));
#60602=CARTESIAN_POINT('Ctrl Pts',(17.9848419508889,1.10476575205979,6.56199991509849));
#60603=CARTESIAN_POINT('Ctrl Pts',(17.5680354476207,-1.8801551122215,6.40499978774625));
#60604=CARTESIAN_POINT('Ctrl Pts',(14.8484469168698,-3.17912223090478,6.24799966039399));
#60605=CARTESIAN_POINT('Ctrl Pts',(12.2647574994032,-1.62734115164585,6.09099953304174));
#60606=CARTESIAN_POINT('Ctrl Pts',(12.1337862540464,1.38369469820864,5.93399940568949));
#60607=CARTESIAN_POINT('Ctrl Pts',(14.5729764087098,3.15395366515346,5.77699927833723));
#60608=CARTESIAN_POINT('Ctrl Pts',(17.3950826426682,2.0960410275735,5.61999915098498));
#60609=CARTESIAN_POINT('Ctrl Pts',(18.0694954331843,-0.841429049439745,
5.46299902363272));
#60610=CARTESIAN_POINT('Ctrl Pts',(15.991461949452,-3.02434785364687,5.30599889628047));
#60611=CARTESIAN_POINT('Ctrl Pts',(13.0243755535244,-2.49537069256931,5.14899876892822));
#60612=CARTESIAN_POINT('Ctrl Pts',(11.8288495207139,0.271357391411547,4.99199864157596));
#60613=CARTESIAN_POINT('Ctrl Pts',(13.4769265545529,2.79450725974701,4.83499851422372));
#60614=CARTESIAN_POINT('Ctrl Pts',(16.4907542376736,2.81228145629323,4.67799838687145));
#60615=CARTESIAN_POINT('Ctrl Pts',(18.1678160134006,0.307309571682018,4.52099825951921));
#60616=CARTESIAN_POINT('Ctrl Pts',(17.0042508855994,-2.47138426111579,4.36399813216695));
#60617=CARTESIAN_POINT('Ctrl Pts',(14.0434946125838,-3.03758475218105,4.2069980048147));
#60618=CARTESIAN_POINT('Ctrl Pts',(11.9402762998377,-0.872627718934448,
4.04999787746244));
#60619=CARTESIAN_POINT('Ctrl Pts',(12.3681201524657,1.08091940906002,3.94533112589428));
#60620=CARTESIAN_POINT('Ctrl Pts',(12.9456684496579,1.75642532122687,3.89299775011019));
#60621=CARTESIAN_POINT('Ctrl Pts',(14.3498000020249,-2.43208680203506,12.3210067496694));
#60622=CARTESIAN_POINT('Ctrl Pts',(13.5500804955002,-2.21828784507023,12.2686733738853));
#60623=CARTESIAN_POINT('Ctrl Pts',(12.1909777974471,-0.944488908413503,
12.1640066223172));
#60624=CARTESIAN_POINT('Ctrl Pts',(12.6631613677687,1.82697676796832,12.0070064949649));
#60625=CARTESIAN_POINT('Ctrl Pts',(15.2345456504068,2.95446187741122,11.8500063676127));
#60626=CARTESIAN_POINT('Ctrl Pts',(17.593730939189,1.43545287811473,11.6930062402604));
#60627=CARTESIAN_POINT('Ctrl Pts',(17.6280542949882,-1.37216546154421,11.5360061129082));
#60628=CARTESIAN_POINT('Ctrl Pts',(15.3052827985147,-2.94861940676938,11.3790059855559));
#60629=CARTESIAN_POINT('Ctrl Pts',(12.7090145851187,-1.88139300561428,11.2220058582036));
#60630=CARTESIAN_POINT('Ctrl Pts',(12.1669649098191,0.873089081080348,11.0650057308514));
#60631=CARTESIAN_POINT('Ctrl Pts',(14.1653917640233,2.84456495267294,10.9080056034991));
#60632=CARTESIAN_POINT('Ctrl Pts',(16.9121855368091,2.26534290518294,10.7510054761469));
#60633=CARTESIAN_POINT('Ctrl Pts',(17.9443218034057,-0.345259924617078,
10.5940053487946));
#60634=CARTESIAN_POINT('Ctrl Pts',(16.3362474201295,-2.64625148285596,10.4370052214424));
#60635=CARTESIAN_POINT('Ctrl Pts',(13.5299517989286,-2.57433082242851,10.2800050940901));
#60636=CARTESIAN_POINT('Ctrl Pts',(12.0418601184578,-0.193979487305122,
10.1230049667379));
#60637=CARTESIAN_POINT('Ctrl Pts',(13.2063620731236,2.36031330282573,9.96600483938562));
#60638=CARTESIAN_POINT('Ctrl Pts',(15.9792357355636,2.79809144104539,9.80900471203338));
#60639=CARTESIAN_POINT('Ctrl Pts',(17.874019642361,0.726793662576183,9.65200458468112));
#60640=CARTESIAN_POINT('Ctrl Pts',(17.1916423980032,-1.99622672030653,9.49500445732887));
#60641=CARTESIAN_POINT('Ctrl Pts',(14.5439984748038,-2.92921157815017,9.33800432997662));
#60642=CARTESIAN_POINT('Ctrl Pts',(12.3052554502237,-1.23554424758505,9.18100420262436));
#60643=CARTESIAN_POINT('Ctrl Pts',(12.4829157380786,1.56604742983749,9.02400407527211));
#60644=CARTESIAN_POINT('Ctrl Pts',(14.9176696198875,2.96334937001758,8.86700394791986));
#60645=CARTESIAN_POINT('Ctrl Pts',(17.4262499493028,1.70338749223094,8.7100038205676));
#60646=CARTESIAN_POINT('Ctrl Pts',(17.7591886697512,-1.08401828684999,8.55300369321535));
#60647=CARTESIAN_POINT('Ctrl Pts',(15.6179364411373,-2.89937447092104,8.3960035658631));
#60648=CARTESIAN_POINT('Ctrl Pts',(12.922574676739,-2.11483375019832,8.23900343851085));
#60649=CARTESIAN_POINT('Ctrl Pts',(12.0900601300394,0.566098682137233,8.08200331115859));
#60650=CARTESIAN_POINT('Ctrl Pts',(13.8669165812153,2.73940499634305,7.92500318380633));
#60651=CARTESIAN_POINT('Ctrl Pts',(16.6598198044455,2.45626056807483,7.76800305645408));
#60652=CARTESIAN_POINT('Ctrl Pts',(17.9643466853611,-0.029436273013457,
7.61100292910183));
#60653=CARTESIAN_POINT('Ctrl Pts',(16.6107154549314,-2.4887373311618,7.45400280174958));
#60654=CARTESIAN_POINT('Ctrl Pts',(13.8127402234604,-2.71636373800054,7.29700267439732));
#60655=CARTESIAN_POINT('Ctrl Pts',(12.0793922238404,-0.508200741956758,
7.14000254704508));
#60656=CARTESIAN_POINT('Ctrl Pts',(12.9649812358183,2.15567077495119,6.98300241969281));
#60657=CARTESIAN_POINT('Ctrl Pts',(15.6753910973545,2.88653154931746,6.82600229234056));
#60658=CARTESIAN_POINT('Ctrl Pts',(17.780171281259,1.02901194332264,6.66900216498831));
#60659=CARTESIAN_POINT('Ctrl Pts',(17.3919452078874,-1.75123284023591,6.51200203763606));
#60660=CARTESIAN_POINT('Ctrl Pts',(14.8588389146771,-2.96112975876036,6.3550019102838));
#60661=CARTESIAN_POINT('Ctrl Pts',(12.4523131299553,-1.51575433776966,6.19800178293155));
#60662=CARTESIAN_POINT('Ctrl Pts',(12.3303225853962,1.28881472630212,6.04100165557929));
#60663=CARTESIAN_POINT('Ctrl Pts',(14.6022574245275,2.93768700204372,5.88400152822705));
#60664=CARTESIAN_POINT('Ctrl Pts',(17.2308517800767,1.95231545424541,5.72700140087478));
#60665=CARTESIAN_POINT('Ctrl Pts',(17.8590200726551,-0.783732243435121,
5.57000127352254));
#60666=CARTESIAN_POINT('Ctrl Pts',(15.9234773846255,-2.81696826350965,5.41300114617029));
#60667=CARTESIAN_POINT('Ctrl Pts',(13.1598441595847,-2.32426307647897,5.25600101881803));
#60668=CARTESIAN_POINT('Ctrl Pts',(12.0462953696974,0.252750409895257,5.09900089146578));
#60669=CARTESIAN_POINT('Ctrl Pts',(13.5813637298219,2.60288784352708,4.94200076411352));
#60670=CARTESIAN_POINT('Ctrl Pts',(16.3885331910994,2.61944326307635,4.78500063676127));
#60671=CARTESIAN_POINT('Ctrl Pts',(17.9505988088066,0.286237348477332,4.62800050940901));
#60672=CARTESIAN_POINT('Ctrl Pts',(16.8668193640612,-2.30192139508873,4.47100038205677));
#60673=CARTESIAN_POINT('Ctrl Pts',(14.1090822052833,-2.82929750765831,4.3140002547045));
#60674=CARTESIAN_POINT('Ctrl Pts',(12.1500816124467,-0.812791619566185,
4.15700012735226));
#60675=CARTESIAN_POINT('Ctrl Pts',(12.5485882039215,1.0068007445182,4.05233337578409));
#60676=CARTESIAN_POINT('Ctrl Pts',(13.086534003335,1.63598720337497,4.));
#60677=CARTESIAN_POINT('Ctrl Pts',(12.4841021658346,0.00201143405015815,
11.112583302492));
#60678=CARTESIAN_POINT('Ctrl Pts',(12.4821471482924,0.253216278985343,11.0967241119451));
#60679=CARTESIAN_POINT('Ctrl Pts',(12.5168205167969,0.503894392425629,11.0808649213983));
#60680=CARTESIAN_POINT('Ctrl Pts',(12.5903776647364,0.742588045230009,11.0650057308514));
#60681=CARTESIAN_POINT('Ctrl Pts',(12.8331071945538,1.53024770494455,11.0126723550673));
#60682=CARTESIAN_POINT('Ctrl Pts',(13.4992494792886,2.18740632880874,10.9603389792832));
#60683=CARTESIAN_POINT('Ctrl Pts',(14.2901195837869,2.41944863282584,10.9080056034991));
#60684=CARTESIAN_POINT('Ctrl Pts',(15.0809896882853,2.65149093684294,10.8556722277151));
#60685=CARTESIAN_POINT('Ctrl Pts',(15.9965876125472,2.45841692101294,10.803338851931));
#60686=CARTESIAN_POINT('Ctrl Pts',(16.6264092857776,1.92677944146461,10.7510054761469));
#60687=CARTESIAN_POINT('Ctrl Pts',(17.256230959008,1.39514196191627,10.6986721003628));
#60688=CARTESIAN_POINT('Ctrl Pts',(17.6002763812068,0.524941018649596,10.6463387245787));
#60689=CARTESIAN_POINT('Ctrl Pts',(17.5042866950936,-0.293658046023555,
10.5940053487946));
#60690=CARTESIAN_POINT('Ctrl Pts',(17.4082970089803,-1.11225711069671,10.5416719730106));
#60691=CARTESIAN_POINT('Ctrl Pts',(16.8722722145549,-1.87925429677634,10.4893385972265));
#60692=CARTESIAN_POINT('Ctrl Pts',(16.1365438804754,-2.25076611307824,10.4370052214424));
#60693=CARTESIAN_POINT('Ctrl Pts',(15.4008155463959,-2.62227792938014,10.3846718456583));
#60694=CARTESIAN_POINT('Ctrl Pts',(14.4653836726623,-2.59830437590432,10.3323384698742));
#60695=CARTESIAN_POINT('Ctrl Pts',(13.749652455717,-2.18959237664585,10.2800050940901));
#60696=CARTESIAN_POINT('Ctrl Pts',(13.0339212387717,-1.78088037738738,10.2276717183061));
#60697=CARTESIAN_POINT('Ctrl Pts',(12.5378906786147,-0.98742993234625,10.175338342522));
#60698=CARTESIAN_POINT('Ctrl Pts',(12.4839590576472,-0.164989244803877,
10.1230049667379));
#60699=CARTESIAN_POINT('Ctrl Pts',(12.4803790780928,-0.110395654006944,
10.1195310786559));
#60700=CARTESIAN_POINT('Ctrl Pts',(12.4787471194664,-0.0556743234800699,
10.1160571905739));
#60701=CARTESIAN_POINT('Ctrl Pts',(12.4790122776664,-0.000936909191352325,
10.112583302492));
#60702=CARTESIAN_POINT('Ctrl Pts',(14.2062007174671,-2.96922295374568,12.));
#60703=CARTESIAN_POINT('Ctrl Pts',(14.1131167498864,-2.9351724226013,12.));
#60704=CARTESIAN_POINT('Ctrl Pts',(14.0220959175279,-2.89635937351053,12.));
#60705=CARTESIAN_POINT('Ctrl Pts',(13.9333480734334,-2.85311020134011,12.));
#60706=CARTESIAN_POINT('Ctrl Pts',(13.8426550828426,-2.80891310782501,12.));
#60707=CARTESIAN_POINT('Ctrl Pts',(13.7543351402525,-2.76008268621842,12.));
#60708=CARTESIAN_POINT('Ctrl Pts',(13.6686411145779,-2.7069217762808,12.));
#60709=CARTESIAN_POINT('Ctrl Pts',(13.5868027530609,-2.65615275554924,12.));
#60710=CARTESIAN_POINT('Ctrl Pts',(13.5073590893475,-2.60143327816087,12.));
#60711=CARTESIAN_POINT('Ctrl Pts',(13.4305625059366,-2.54299781905995,12.));
#60712=CARTESIAN_POINT('Ctrl Pts',(13.3633654954521,-2.49186679234665,12.));
#60713=CARTESIAN_POINT('Ctrl Pts',(13.298195438544,-2.43789004325195,12.));
#60714=CARTESIAN_POINT('Ctrl Pts',(13.235245315039,-2.38121225533745,12.));
#60715=CARTESIAN_POINT('Ctrl Pts',(13.2201383978307,-2.36761058782836,12.));
#60716=CARTESIAN_POINT('Ctrl Pts',(13.2051557596309,-2.35384973663533,12.));
#60717=CARTESIAN_POINT('Ctrl Pts',(13.1903225084953,-2.33995287271397,12.));
#60718=CARTESIAN_POINT('Ctrl Pts',(13.1178922144325,-2.27209492767057,12.));
#60719=CARTESIAN_POINT('Ctrl Pts',(13.0489277577742,-2.20091637429481,12.));
#60720=CARTESIAN_POINT('Ctrl Pts',(12.9836701413723,-2.12670552844038,12.));
#60721=CARTESIAN_POINT('Ctrl Pts',(12.9187777778625,-2.05291004752833,12.));
#60722=CARTESIAN_POINT('Ctrl Pts',(12.8575503884276,-1.97611533073339,12.));
#60723=CARTESIAN_POINT('Ctrl Pts',(12.800268550456,-1.89657810132058,12.));
#60724=CARTESIAN_POINT('Ctrl Pts',(12.7459133734412,-1.82110461204208,12.));
#60725=CARTESIAN_POINT('Ctrl Pts',(12.6951108248742,-1.74316096291563,12.));
#60726=CARTESIAN_POINT('Ctrl Pts',(12.6481432361601,-1.66295348615981,12.));
#60727=CARTESIAN_POINT('Ctrl Pts',(12.6107661639977,-1.59912392350293,12.));
#60728=CARTESIAN_POINT('Ctrl Pts',(12.5758185286433,-1.533860318552,12.));
#60729=CARTESIAN_POINT('Ctrl Pts',(12.5434639629309,-1.46726456665475,12.));
#60730=CARTESIAN_POINT('Ctrl Pts',(12.5375614518629,-1.45511536440159,12.));
#60731=CARTESIAN_POINT('Ctrl Pts',(12.5317470084536,-1.4429252625298,12.));
#60732=CARTESIAN_POINT('Ctrl Pts',(12.5260248255016,-1.43070222232707,12.));
#60733=CARTESIAN_POINT('Ctrl Pts',(12.4854475610481,-1.34402594180728,12.));
#60734=CARTESIAN_POINT('Ctrl Pts',(12.4494522312093,-1.25558570069036,12.));
#60735=CARTESIAN_POINT('Ctrl Pts',(12.4183023908741,-1.16562505800954,12.));
#60736=CARTESIAN_POINT('Ctrl Pts',(12.3871525505389,-1.07566441532873,12.));
#60737=CARTESIAN_POINT('Ctrl Pts',(12.3608477335802,-0.984182637916221,
12.));
#60738=CARTESIAN_POINT('Ctrl Pts',(12.3397077040223,-0.891413467157708,
12.));
#60739=CARTESIAN_POINT('Ctrl Pts',(12.3185427547458,-0.798534940751147,
12.));
#60740=CARTESIAN_POINT('Ctrl Pts',(12.3025555503081,-0.704364799779564,
12.));
#60741=CARTESIAN_POINT('Ctrl Pts',(12.2916706351494,-0.609311329981899,
12.));
#60742=CARTESIAN_POINT('Ctrl Pts',(12.2861036872675,-0.560697472671795,
12.));
#60743=CARTESIAN_POINT('Ctrl Pts',(12.2818721595795,-0.511852737800975,
12.));
#60744=CARTESIAN_POINT('Ctrl Pts',(12.2789708979829,-0.462833545994333,
12.));
#60745=CARTESIAN_POINT('Ctrl Pts',(12.2781343831999,-0.448699943341852,
12.));
#60746=CARTESIAN_POINT('Ctrl Pts',(12.277408477694,-0.434551848133338,12.));
#60747=CARTESIAN_POINT('Ctrl Pts',(12.2767931065317,-0.42039064034991,12.));
#60748=CARTESIAN_POINT('Ctrl Pts',(12.2761719502385,-0.406096302442059,
12.));
#60749=CARTESIAN_POINT('Ctrl Pts',(12.2756638189297,-0.391797511344244,
12.));
#60750=CARTESIAN_POINT('Ctrl Pts',(12.2752682723578,-0.377498729044968,
12.));
#60751=CARTESIAN_POINT('Ctrl Pts',(12.2726875200461,-0.28420600930709,12.));
#60752=CARTESIAN_POINT('Ctrl Pts',(12.2748931639065,-0.190870392884388,
12.));
#60753=CARTESIAN_POINT('Ctrl Pts',(12.2817566653744,-0.0978690578159151,
12.));
#60754=CARTESIAN_POINT('Ctrl Pts',(12.2886243750566,-0.004810700899435,
12.));
#60755=CARTESIAN_POINT('Ctrl Pts',(12.3001560328895,0.0879139420894839,
12.));
#60756=CARTESIAN_POINT('Ctrl Pts',(12.3162734180046,0.179914286846824,12.));
#60757=CARTESIAN_POINT('Ctrl Pts',(12.3321476400437,0.270526621907842,12.));
#60758=CARTESIAN_POINT('Ctrl Pts',(12.3524707190227,0.360437184721369,12.));
#60759=CARTESIAN_POINT('Ctrl Pts',(12.3772105840448,0.449247114668589,12.));
#60760=CARTESIAN_POINT('Ctrl Pts',(12.387089561874,0.484710175124557,12.));
#60761=CARTESIAN_POINT('Ctrl Pts',(12.3976732487818,0.519997379566271,12.));
#60762=CARTESIAN_POINT('Ctrl Pts',(12.4089613041164,0.555081714039806,12.));
#60763=CARTESIAN_POINT('Ctrl Pts',(12.4149082466012,0.573565368933964,12.));
#60764=CARTESIAN_POINT('Ctrl Pts',(12.4210507056737,0.591992698996559,12.));
#60765=CARTESIAN_POINT('Ctrl Pts',(12.427388732547,0.610359631690939,12.));
#60766=CARTESIAN_POINT('Ctrl Pts',(12.4327450955641,0.62588180617673,12.));
#60767=CARTESIAN_POINT('Ctrl Pts',(12.4382385696775,0.641353302839583,12.));
#60768=CARTESIAN_POINT('Ctrl Pts',(12.4438669442654,0.656766888688516,12.));
#60769=CARTESIAN_POINT('Ctrl Pts',(12.4746822935363,0.741156266835812,12.));
#60770=CARTESIAN_POINT('Ctrl Pts',(12.5095548332415,0.823860554446091,12.));
#60771=CARTESIAN_POINT('Ctrl Pts',(12.5484325218527,0.904509504080283,12.));
#60772=CARTESIAN_POINT('Ctrl Pts',(12.5775387438767,0.964888253895875,12.));
#60773=CARTESIAN_POINT('Ctrl Pts',(12.6088907149234,1.02411455960934,12.));
#60774=CARTESIAN_POINT('Ctrl Pts',(12.6424801735134,1.08201977519688,12.));
#60775=CARTESIAN_POINT('Ctrl Pts',(12.6553986892758,1.10429013833142,12.));
#60776=CARTESIAN_POINT('Ctrl Pts',(12.6686482828058,1.12636495172308,12.));
#60777=CARTESIAN_POINT('Ctrl Pts',(12.6822288987083,1.1482340709878,12.));
#60778=CARTESIAN_POINT('Ctrl Pts',(12.6939913183076,1.16717531480961,12.));
#60779=CARTESIAN_POINT('Ctrl Pts',(12.706004041963,1.18596501264398,12.));
#60780=CARTESIAN_POINT('Ctrl Pts',(12.7182527989854,1.20457528100954,12.));
#60781=CARTESIAN_POINT('Ctrl Pts',(12.765524404259,1.27639785521913,12.));
#60782=CARTESIAN_POINT('Ctrl Pts',(12.8163473248132,1.34561526270953,12.));
#60783=CARTESIAN_POINT('Ctrl Pts',(12.8706925767079,1.41187353983322,12.));
#60784=CARTESIAN_POINT('Ctrl Pts',(12.9128273378038,1.46324466389474,12.));
#60785=CARTESIAN_POINT('Ctrl Pts',(12.9570801591186,1.51283644006015,12.));
#60786=CARTESIAN_POINT('Ctrl Pts',(13.0034499581199,1.56046614478315,12.));
#60787=CARTESIAN_POINT('Ctrl Pts',(13.0293158880168,1.58703487335031,12.));
#60788=CARTESIAN_POINT('Ctrl Pts',(13.0558407610521,1.61299275362867,12.));
#60789=CARTESIAN_POINT('Ctrl Pts',(13.0829974340784,1.63832794503775,12.));
#60790=CARTESIAN_POINT('Origin',(15.,0.,7.5));
#60791=CARTESIAN_POINT('Origin',(-7.5,12.9903810567666,3.));
#60792=CARTESIAN_POINT('Origin',(15.,0.,3.));
#60793=CARTESIAN_POINT('Origin',(-7.50000000000001,-12.9903810567666,3.));
#60794=CARTESIAN_POINT('Origin',(5.55111512312578E-16,0.,14.));
#60795=CARTESIAN_POINT('',(-5.65685424949238,-6.92764844988394E-16,12.));
#60796=CARTESIAN_POINT('Origin',(5.55111512312578E-16,0.,12.));
#60797=CARTESIAN_POINT('',(1.87717472568372E-16,-4.49927934798557E-32,8.));
#60798=CARTESIAN_POINT('Origin',(5.55111512312578E-16,0.,14.));
#60799=CARTESIAN_POINT('Origin',(0.,0.,0.));
#60800=CARTESIAN_POINT('',(-30.,-3.67394039744206E-15,12.));
#60801=CARTESIAN_POINT('Origin',(0.,0.,12.));
#60802=CARTESIAN_POINT('',(-30.,-3.67394039744206E-15,0.));
#60803=CARTESIAN_POINT('',(-30.,-3.67394039744206E-15,0.));
#60804=CARTESIAN_POINT('Origin',(0.,0.,0.));
#60805=CARTESIAN_POINT('Origin',(0.,0.,12.));
#60806=CARTESIAN_POINT('Origin',(0.,0.,0.));
#60807=CARTESIAN_POINT('',(0.,0.,0.));
#60808=CARTESIAN_POINT('Origin',(-7.5,12.9903810567666,15.));
#60809=CARTESIAN_POINT('',(-11.,12.9903810567666,18.));
#60810=CARTESIAN_POINT('Origin',(-7.5,12.9903810567666,18.));
#60811=CARTESIAN_POINT('',(-11.,12.9903810567666,12.));
#60812=CARTESIAN_POINT('',(-11.,12.9903810567666,15.));
#60813=CARTESIAN_POINT('Origin',(-7.5,12.9903810567666,12.));
#60814=CARTESIAN_POINT('Origin',(15.,0.,15.));
#60815=CARTESIAN_POINT('',(11.5,4.28626379701574E-16,18.));
#60816=CARTESIAN_POINT('Origin',(15.,0.,18.));
#60817=CARTESIAN_POINT('',(11.5,4.28626379701574E-16,12.));
#60818=CARTESIAN_POINT('',(11.5,4.28626379701574E-16,15.));
#60819=CARTESIAN_POINT('Origin',(15.,0.,12.));
#60820=CARTESIAN_POINT('Origin',(-7.50000000000001,-12.9903810567666,15.));
#60821=CARTESIAN_POINT('',(-11.,-12.9903810567666,18.));
#60822=CARTESIAN_POINT('Origin',(-7.50000000000001,-12.9903810567666,18.));
#60823=CARTESIAN_POINT('',(-11.,-12.9903810567666,12.));
#60824=CARTESIAN_POINT('',(-11.,-12.9903810567666,15.));
#60825=CARTESIAN_POINT('Origin',(-7.50000000000001,-12.9903810567666,12.));
#60826=CARTESIAN_POINT('Origin',(5.55111512312578E-16,0.,14.));
#60827=CARTESIAN_POINT('',(-5.65685424949238,-6.92764844988394E-16,12.));
#60828=CARTESIAN_POINT('Origin',(5.55111512312578E-16,0.,12.));
#60829=CARTESIAN_POINT('',(-5.5,6.73555739531044E-16,16.3979157616564));
#60830=CARTESIAN_POINT('Origin',(5.55111512312578E-16,0.,14.));
#60831=CARTESIAN_POINT('Origin',(0.,0.,16.3979157616564));
#60832=CARTESIAN_POINT('Origin',(0.,0.,12.));
#60833=CARTESIAN_POINT('',(-5.5,-6.73555739531044E-16,18.));
#60834=CARTESIAN_POINT('Origin',(0.,0.,18.));
#60835=CARTESIAN_POINT('',(-5.5,-6.73555739531044E-16,12.));
#60836=CARTESIAN_POINT('Origin',(0.,0.,12.));
#60837=CARTESIAN_POINT('',(-22.,-2.69422295812418E-15,18.));
#60838=CARTESIAN_POINT('Origin',(0.,0.,18.));
#60839=CARTESIAN_POINT('',(-22.,-2.69422295812418E-15,12.));
#60840=CARTESIAN_POINT('',(-22.,-2.69422295812418E-15,12.));
#60841=CARTESIAN_POINT('Origin',(0.,0.,12.));
#60842=CARTESIAN_POINT('Origin',(0.,0.,18.));
#60843=CARTESIAN_POINT('Origin',(0.,0.,12.));
#60844=CARTESIAN_POINT('',(0.,0.,0.));
#60845=CARTESIAN_POINT('Origin',(0.,0.,16.));
#60846=CARTESIAN_POINT('',(-4.94751652564198,0.00256483971322934,26.3223204546569));
#60847=CARTESIAN_POINT('',(-4.94433041235646,0.00147179461986118,26.1776795453432));
#60848=CARTESIAN_POINT('',(-4.942,-6.05220448138622E-16,16.));
#60849=CARTESIAN_POINT('',(2.16917135428601,4.44050218283304,26.));
#60850=CARTESIAN_POINT('Ctrl Pts',(-4.94751652564198,0.00256483971322934,
26.3223204546569));
#60851=CARTESIAN_POINT('Ctrl Pts',(-4.94869886604438,0.171401137605494,
26.3168647682864));
#60852=CARTESIAN_POINT('Ctrl Pts',(-4.9408321732254,0.340133662244093,26.311409081916));
#60853=CARTESIAN_POINT('Ctrl Pts',(-4.92355817442292,0.507901950004805,
26.3059533955455));
#60854=CARTESIAN_POINT('Ctrl Pts',(-4.75600008116697,2.13525730225587,26.2530331414635));
#60855=CARTESIAN_POINT('Ctrl Pts',(-3.70330534691493,3.67188727651734,26.2001128873815));
#60856=CARTESIAN_POINT('Ctrl Pts',(-2.24451326222463,4.41286251356918,26.1471926332996));
#60857=CARTESIAN_POINT('Ctrl Pts',(-0.892016301737719,5.09984646860033,
26.0981284221997));
#60858=CARTESIAN_POINT('Ctrl Pts',(0.80955341496604,5.10290231670094,26.0490642110999));
#60859=CARTESIAN_POINT('Ctrl Pts',(2.17574200330363,4.4448669900444,26.));
#60860=CARTESIAN_POINT('',(-2.16917135428577,4.44050218283316,26.));
#60861=CARTESIAN_POINT('Origin',(0.,0.,26.));
#60862=CARTESIAN_POINT('Ctrl Pts',(-2.16917135428577,4.44050218283316,26.));
#60863=CARTESIAN_POINT('Ctrl Pts',(-2.90742207776898,4.07986902565299,26.026460127041));
#60864=CARTESIAN_POINT('Ctrl Pts',(-3.54838487149729,3.53163056089739,26.0529202540819));
#60865=CARTESIAN_POINT('Ctrl Pts',(-4.02597159025063,2.86203897562359,26.0793803811229));
#60866=CARTESIAN_POINT('Ctrl Pts',(-4.50355830900396,2.19244739034978,26.1058405081639));
#60867=CARTESIAN_POINT('Ctrl Pts',(-4.81776895278232,1.40150268455777,26.1323006352049));
#60868=CARTESIAN_POINT('Ctrl Pts',(-4.91302280979298,0.586752670320857,
26.1587607622459));
#60869=CARTESIAN_POINT('Ctrl Pts',(-4.93572472976967,0.39257271577962,26.1650670232783));
#60870=CARTESIAN_POINT('Ctrl Pts',(-4.94598956917588,0.197040583288091,
26.1713732843108));
#60871=CARTESIAN_POINT('Ctrl Pts',(-4.94433041235646,0.00147179461986118,
26.1776795453432));
#60872=CARTESIAN_POINT('Origin',(0.,0.,16.));
#60873=CARTESIAN_POINT('',(-4.93516121822955,0.00250487983550263,27.3223204546569));
#60874=CARTESIAN_POINT('',(-4.93474635697119,0.00209204260276723,27.1776795453432));
#60875=CARTESIAN_POINT('',(-4.942,-6.05220448138622E-16,16.));
#60876=CARTESIAN_POINT('Ctrl Pts',(-4.93516121822955,0.00250487983550263,
27.3223204546569));
#60877=CARTESIAN_POINT('Ctrl Pts',(-4.93820686879495,0.665010559781625,
27.3010529594449));
#60878=CARTESIAN_POINT('Ctrl Pts',(-4.81416865933799,1.32642295622759,27.2797854642328));
#60879=CARTESIAN_POINT('Ctrl Pts',(-4.55764236207275,1.93168318346768,27.2585179690208));
#60880=CARTESIAN_POINT('Ctrl Pts',(-3.91932380623715,3.43776204663053,27.2055977149389));
#60881=CARTESIAN_POINT('Ctrl Pts',(-2.46067639950694,4.59616252449921,27.1526774608569));
#60882=CARTESIAN_POINT('Ctrl Pts',(-0.849145821918294,4.87674835967949,
27.0997572067749));
#60883=CARTESIAN_POINT('Ctrl Pts',(0.762384755670364,5.15733419485977,27.046836952693));
#60884=CARTESIAN_POINT('Ctrl Pts',(2.52679850411746,4.56010538735165,26.993916698611));
#60885=CARTESIAN_POINT('Ctrl Pts',(3.63656998987608,3.35842905030792,26.940996444529));
#60886=CARTESIAN_POINT('Ctrl Pts',(4.7463414756347,2.15675271326421,26.8880761904471));
#60887=CARTESIAN_POINT('Ctrl Pts',(5.20147069870486,0.350628846684903,26.8351559363651));
#60888=CARTESIAN_POINT('Ctrl Pts',(4.79388038130065,-1.23355926618448,26.7822356822831));
#60889=CARTESIAN_POINT('Ctrl Pts',(4.38629006389643,-2.81774737905389,26.7293154282012));
#60890=CARTESIAN_POINT('Ctrl Pts',(3.11598020601782,-4.17999973821337,26.6763951741192));
#60891=CARTESIAN_POINT('Ctrl Pts',(1.56388702368888,-4.69668637868557,26.6234749200373));
#60892=CARTESIAN_POINT('Ctrl Pts',(0.011793841359943,-5.21337301915776,
26.5705546659553));
#60893=CARTESIAN_POINT('Ctrl Pts',(-1.82208266541932,-4.88449394094269,
26.5176344118733));
#60894=CARTESIAN_POINT('Ctrl Pts',(-3.09781019267902,-3.86101403671482,
26.4647141577914));
#60895=CARTESIAN_POINT('Ctrl Pts',(-4.24201965745686,-2.94304733269382,
26.4172495900799));
#60896=CARTESIAN_POINT('Ctrl Pts',(-4.93723014327371,-1.46631393177114,
26.3697850223684));
#60897=CARTESIAN_POINT('Ctrl Pts',(-4.94751652564198,0.00256483971322934,
26.3223204546569));
#60898=CARTESIAN_POINT('Ctrl Pts',(-4.94433041235646,0.00147179461986118,
26.1776795453432));
#60899=CARTESIAN_POINT('Ctrl Pts',(-4.93206642200618,-1.44411412527272,
26.2242935383928));
#60900=CARTESIAN_POINT('Ctrl Pts',(-4.26830822622625,-2.89170283737207,
26.2709075314422));
#60901=CARTESIAN_POINT('Ctrl Pts',(-3.16027114216866,-3.81000496542323,
26.3175215244917));
#60902=CARTESIAN_POINT('Ctrl Pts',(-1.90233119357243,-4.85254131044005,
26.3704417785737));
#60903=CARTESIAN_POINT('Ctrl Pts',(-0.071770729429417,-5.21289273822024,
26.4233620326557));
#60904=CARTESIAN_POINT('Ctrl Pts',(1.48894305049924,-4.72167819128264,26.4762822867377));
#60905=CARTESIAN_POINT('Ctrl Pts',(3.0496568304279,-4.23046364434503,26.5292025408196));
#60906=CARTESIAN_POINT('Ctrl Pts',(4.34052392614221,-2.88768312268964,26.5821227949016));
#60907=CARTESIAN_POINT('Ctrl Pts',(4.77319109373772,-1.30997581823277,26.6350430489835));
#60908=CARTESIAN_POINT('Ctrl Pts',(5.20585826133323,0.267731486224089,26.6879633030655));
#60909=CARTESIAN_POINT('Ctrl Pts',(4.78032550080995,2.08036557348242,26.7408835571475));
#60910=CARTESIAN_POINT('Ctrl Pts',(3.69010138443177,3.29954694578963,26.7938038112294));
#60911=CARTESIAN_POINT('Ctrl Pts',(2.59987726805358,4.51872831809683,26.8467240653114));
#60912=CARTESIAN_POINT('Ctrl Pts',(0.844961795820489,5.14445697545292,26.8996443193934));
#60913=CARTESIAN_POINT('Ctrl Pts',(-0.770932625263734,4.88981277963295,
26.9525645734753));
#60914=CARTESIAN_POINT('Ctrl Pts',(-2.38682704634796,4.63516858381299,27.0054848275573));
#60915=CARTESIAN_POINT('Ctrl Pts',(-3.86370041628332,3.50015153481698,27.0584050816393));
#60916=CARTESIAN_POINT('Ctrl Pts',(-4.52604495623161,2.00446386165791,27.1113253357212));
#60917=CARTESIAN_POINT('Ctrl Pts',(-4.80287247849846,1.37933979454018,27.1334434055952));
#60918=CARTESIAN_POINT('Ctrl Pts',(-4.93741567156095,0.691212705388757,
27.1555614754692));
#60919=CARTESIAN_POINT('Ctrl Pts',(-4.93474635697119,0.00209204260276723,
27.1776795453432));
#60920=CARTESIAN_POINT('Origin',(0.,0.,16.));
#60921=CARTESIAN_POINT('',(-4.93883733219525,-0.00423015144557837,28.3223204546569));
#60922=CARTESIAN_POINT('',(-4.93956784471338,-0.00436622746695347,28.1776795453432));
#60923=CARTESIAN_POINT('',(-4.942,-6.05220448138622E-16,16.));
#60924=CARTESIAN_POINT('Ctrl Pts',(-4.93883733219525,-0.00423015144557837,
28.3223204546569));
#60925=CARTESIAN_POINT('Ctrl Pts',(-4.92943499320705,1.14867573667121,28.2852411506033));
#60926=CARTESIAN_POINT('Ctrl Pts',(-4.52687920768094,2.30749865084404,28.2481618465497));
#60927=CARTESIAN_POINT('Ctrl Pts',(-3.78946858460819,3.18489002165513,28.2110825424962));
#60928=CARTESIAN_POINT('Ctrl Pts',(-2.73702279222337,4.43711887162355,28.1581622884142));
#60929=CARTESIAN_POINT('Ctrl Pts',(-1.00249392936347,5.11608531143494,28.1052420343322));
#60930=CARTESIAN_POINT('Ctrl Pts',(0.62037219239006,4.91108322945104,28.0523217802503));
#60931=CARTESIAN_POINT('Ctrl Pts',(2.2432383141436,4.70608114746714,27.9994015261683));
#60932=CARTESIAN_POINT('Ctrl Pts',(3.75444169479077,3.61711054368793,27.9464812720863));
#60933=CARTESIAN_POINT('Ctrl Pts',(4.46243050532182,2.1425023369291,27.8935610180044));
#60934=CARTESIAN_POINT('Ctrl Pts',(5.17041931585287,0.667894130170271,27.8406407639224));
#60935=CARTESIAN_POINT('Ctrl Pts',(5.07519355626782,-1.19235167956817,27.7877205098404));
#60936=CARTESIAN_POINT('Ctrl Pts',(4.22033397580047,-2.58696076330049,27.7348002557585));
#60937=CARTESIAN_POINT('Ctrl Pts',(3.36547439533311,-3.98156984703282,27.6818800016765));
#60938=CARTESIAN_POINT('Ctrl Pts',(1.75098099398345,-4.91054220475902,27.6289597475946));
#60939=CARTESIAN_POINT('Ctrl Pts',(0.115662973237938,-4.94876098597613,
27.5760394935126));
#60940=CARTESIAN_POINT('Ctrl Pts',(-1.51965504750756,-4.98697976719323,
27.5231192394306));
#60941=CARTESIAN_POINT('Ctrl Pts',(-3.17579768764892,-4.13444497190124,
27.4701989853487));
#60942=CARTESIAN_POINT('Ctrl Pts',(-4.09487415524911,-2.78129895002674,
27.4172787312667));
#60943=CARTESIAN_POINT('Ctrl Pts',(-4.6445938479574,-1.97195278400361,27.3856259723968));
#60944=CARTESIAN_POINT('Ctrl Pts',(-4.9306283269799,-0.98351309398954,27.3539732135268));
#60945=CARTESIAN_POINT('Ctrl Pts',(-4.93516121822955,0.00250487983550263,
27.3223204546569));
#60946=CARTESIAN_POINT('Ctrl Pts',(-4.93474635697119,0.00209204260276723,
27.1776795453432));
#60947=CARTESIAN_POINT('Ctrl Pts',(-4.93102900187776,-0.957594843168012,
27.2084817295512));
#60948=CARTESIAN_POINT('Ctrl Pts',(-4.66120098345796,-1.91920867090262,
27.2392839137591));
#60949=CARTESIAN_POINT('Ctrl Pts',(-4.13896060662357,-2.7152702966968,27.2700860979671));
#60950=CARTESIAN_POINT('Ctrl Pts',(-3.24171600710599,-4.08295848457032,
27.3230063520491));
#60951=CARTESIAN_POINT('Ctrl Pts',(-1.59941109810958,-4.96197656299522,
27.375926606131));
#60952=CARTESIAN_POINT('Ctrl Pts',(0.0363198151755977,-4.94999037586593,
27.428846860213));
#60953=CARTESIAN_POINT('Ctrl Pts',(1.67205072846078,-4.93800418873663,27.481767114295));
#60954=CARTESIAN_POINT('Ctrl Pts',(3.30120764603473,-4.03501373605313,27.5346873683769));
#60955=CARTESIAN_POINT('Ctrl Pts',(4.17831072893992,-2.65428408264511,27.5876076224589));
#60956=CARTESIAN_POINT('Ctrl Pts',(5.0554138118451,-1.27355442923711,27.6405278765408));
#60957=CARTESIAN_POINT('Ctrl Pts',(5.18046306008153,0.584914424895401,27.6934481306228));
#60958=CARTESIAN_POINT('Ctrl Pts',(4.49620935947501,2.07068111644173,27.7463683847048));
#60959=CARTESIAN_POINT('Ctrl Pts',(3.81195565886849,3.55644780798807,27.7992886387867));
#60960=CARTESIAN_POINT('Ctrl Pts',(2.318399009419,4.66951233694822,27.8522088928687));
#60961=CARTESIAN_POINT('Ctrl Pts',(0.69902662395141,4.900507696898,27.9051291469507));
#60962=CARTESIAN_POINT('Ctrl Pts',(-0.920345761516168,5.13150305684779,
27.9580494010326));
#60963=CARTESIAN_POINT('Ctrl Pts',(-2.66553388300184,4.48042924778721,28.0109696551146));
#60964=CARTESIAN_POINT('Ctrl Pts',(-3.73791972674343,3.24523368575399,28.0638899091965));
#60965=CARTESIAN_POINT('Ctrl Pts',(-4.5065378238221,2.35992391786528,28.1018197879121));
#60966=CARTESIAN_POINT('Ctrl Pts',(-4.92952982972571,1.17454424098757,28.1397496666277));
#60967=CARTESIAN_POINT('Ctrl Pts',(-4.93956784471338,-0.00436622746695347,
28.1776795453432));
#60968=CARTESIAN_POINT('Origin',(0.,0.,16.));
#60969=CARTESIAN_POINT('',(-4.95011095070931,-1.6828919353247E-5,29.3223204546569));
#60970=CARTESIAN_POINT('',(-4.9500545842803,0.000473333830474247,29.1776795453432));
#60971=CARTESIAN_POINT('',(-4.942,-6.05220448138622E-16,16.));
#60972=CARTESIAN_POINT('Ctrl Pts',(-4.95011089075521,-1.68287949581236E-5,
29.3223204546569));
#60973=CARTESIAN_POINT('Ctrl Pts',(-4.95002830796364,1.63484509113909,29.2694293417618));
#60974=CARTESIAN_POINT('Ctrl Pts',(-4.06015814856933,3.2697840224184,29.2165382288666));
#60975=CARTESIAN_POINT('Ctrl Pts',(-2.68714856385847,4.15726245203154,29.1636471159715));
#60976=CARTESIAN_POINT('Ctrl Pts',(-1.31338249801809,5.04522985178176,29.1107268618895));
#60977=CARTESIAN_POINT('Ctrl Pts',(0.544055526265072,5.1849128728298,29.0578066078076));
#60978=CARTESIAN_POINT('Ctrl Pts',(2.03517352301083,4.51239041724249,29.0048863537256));
#60979=CARTESIAN_POINT('Ctrl Pts',(3.52629151975661,3.83986796165517,28.9519660996436));
#60980=CARTESIAN_POINT('Ctrl Pts',(4.65108948896497,2.3551400294325,28.8990458455617));
#60981=CARTESIAN_POINT('Ctrl Pts',(4.89484265904535,0.737640825291349,28.8461255914797));
#60982=CARTESIAN_POINT('Ctrl Pts',(5.13859582912572,-0.879858378849781,
28.7932053373978));
#60983=CARTESIAN_POINT('Ctrl Pts',(4.50130420007813,-2.63012885490939,28.7402850833158));
#60984=CARTESIAN_POINT('Ctrl Pts',(3.27460223530322,-3.71222015364772,28.6873648292338));
#60985=CARTESIAN_POINT('Ctrl Pts',(2.04790027052829,-4.79431145238607,28.6344445751519));
#60986=CARTESIAN_POINT('Ctrl Pts',(0.231787970026049,-5.20822357380314,
28.5815243210699));
#60987=CARTESIAN_POINT('Ctrl Pts',(-1.34265409528112,-4.76454391006902,
28.5286040669879));
#60988=CARTESIAN_POINT('Ctrl Pts',(-2.91709616058829,-4.3208642463349,28.475683812906));
#60989=CARTESIAN_POINT('Ctrl Pts',(-4.24986799070038,-3.01959279744957,
28.422763558824));
#60990=CARTESIAN_POINT('Ctrl Pts',(-4.73107254480156,-1.45621144294418,
28.369843304742));
#60991=CARTESIAN_POINT('Ctrl Pts',(-4.87511450807598,-0.988234742120547,
28.3540023547137));
#60992=CARTESIAN_POINT('Ctrl Pts',(-4.94285418164439,-0.496772420704347,
28.3381614046853));
#60993=CARTESIAN_POINT('Ctrl Pts',(-4.93883733219525,-0.00423015144557837,
28.3223204546569));
#60994=CARTESIAN_POINT('Ctrl Pts',(-4.93956784471338,-0.00436622746695347,
28.1776795453432));
#60995=CARTESIAN_POINT('Ctrl Pts',(-4.9435349971983,-0.470286790462875,
28.1926699207096));
#60996=CARTESIAN_POINT('Ctrl Pts',(-4.88300154657712,-0.935196907127989,
28.207660296076));
#60997=CARTESIAN_POINT('Ctrl Pts',(-4.75381137141076,-1.38017405347592,
28.2226506714425));
#60998=CARTESIAN_POINT('Ctrl Pts',(-4.29773360633903,-2.95106891566672,
28.2755709255244));
#60999=CARTESIAN_POINT('Ctrl Pts',(-2.98599451019808,-4.27354132504245,
28.3284911796064));
#61000=CARTESIAN_POINT('Ctrl Pts',(-1.41886776017779,-4.74240604726615,
28.3814114336883));
#61001=CARTESIAN_POINT('Ctrl Pts',(0.148258989842506,-5.21127076948986,
28.4343316877703));
#61002=CARTESIAN_POINT('Ctrl Pts',(1.97077339374215,-4.82652780456152,28.4872519418523));
#61003=CARTESIAN_POINT('Ctrl Pts',(3.21466598259635,-3.76424227707361,28.5401721959342));
#61004=CARTESIAN_POINT('Ctrl Pts',(4.45855857145055,-2.7019567495857,28.5930924500162));
#61005=CARTESIAN_POINT('Ctrl Pts',(5.1238293452593,-0.962128659538206,28.6460127040981));
#61006=CARTESIAN_POINT('Ctrl Pts',(4.90603973778863,0.659070540261458,28.6989329581801));
#61007=CARTESIAN_POINT('Ctrl Pts',(4.68825013031796,2.28026974006111,28.7518532122621));
#61008=CARTESIAN_POINT('Ctrl Pts',(3.58740014156788,3.78284004961294,28.8047734663441));
#61009=CARTESIAN_POINT('Ctrl Pts',(2.10725580021387,4.47918211041389,28.857693720426));
#61010=CARTESIAN_POINT('Ctrl Pts',(0.627111458859856,5.17552417121484,28.910613974508));
#61011=CARTESIAN_POINT('Ctrl Pts',(-1.23232723509808,5.0656379832649,28.9635342285899));
#61012=CARTESIAN_POINT('Ctrl Pts',(-2.62015287286002,4.19980926793105,29.0164544826719));
#61013=CARTESIAN_POINT('Ctrl Pts',(-4.00797851062198,3.33398055259719,29.0693747367538));
#61014=CARTESIAN_POINT('Ctrl Pts',(-4.92419109218792,1.71220930987939,29.1222949908358));
#61015=CARTESIAN_POINT('Ctrl Pts',(-4.94951767608282,0.0766427647882502,
29.1752152449178));
#61016=CARTESIAN_POINT('Ctrl Pts',(-4.94991079785034,0.0512553373413882,
29.1760366783929));
#61017=CARTESIAN_POINT('Ctrl Pts',(-4.95008927347619,0.0258645861152391,
29.1768581118681));
#61018=CARTESIAN_POINT('Ctrl Pts',(-4.9500545842803,0.000473333830474247,
29.1776795453432));
#61019=CARTESIAN_POINT('Origin',(0.,0.,16.));
#61020=CARTESIAN_POINT('',(-4.93888642291793,0.00424076360118208,30.3223204546569));
#61021=CARTESIAN_POINT('',(-4.93818673588435,0.0040670116119004,30.1776795453432));
#61022=CARTESIAN_POINT('',(-4.942,-6.05220448138622E-16,16.));
#61023=CARTESIAN_POINT('Ctrl Pts',(-4.93888642291793,0.00424076360118208,
30.3223204546569));
#61024=CARTESIAN_POINT('Ctrl Pts',(-4.94290141421135,0.49495855667818,30.3065377870022));
#61025=CARTESIAN_POINT('Ctrl Pts',(-4.87566910369714,0.984600773625852,
30.2907551193474));
#61026=CARTESIAN_POINT('Ctrl Pts',(-4.7326693925228,1.45101307944963,30.2749724516927));
#61027=CARTESIAN_POINT('Ctrl Pts',(-4.25318257733109,3.01492218981842,30.2220521976108));
#61028=CARTESIAN_POINT('Ctrl Pts',(-2.92184129195003,4.31765692360063,30.1691319435288));
#61029=CARTESIAN_POINT('Ctrl Pts',(-1.3478876419775,4.76306597049205,30.1162116894468));
#61030=CARTESIAN_POINT('Ctrl Pts',(0.226066007995039,5.20847501738348,30.0632914353649));
#61031=CARTESIAN_POINT('Ctrl Pts',(2.04263202255905,4.79655837738413,30.0103711812829));
#61032=CARTESIAN_POINT('Ctrl Pts',(3.27052205003055,3.71581539574951,29.9574509272009));
#61033=CARTESIAN_POINT('Ctrl Pts',(4.49841207750204,2.6350724141149,29.904530673119));
#61034=CARTESIAN_POINT('Ctrl Pts',(5.13762611788102,0.885503090845023,29.851610419037));
#61035=CARTESIAN_POINT('Ctrl Pts',(4.89565006291192,-0.732262930536752,
29.798690164955));
#61036=CARTESIAN_POINT('Ctrl Pts',(4.65367400794282,-2.35002895191851,29.7457699108731));
#61037=CARTESIAN_POINT('Ctrl Pts',(3.53050785762567,-3.83599167141216,29.6928496567911));
#61038=CARTESIAN_POINT('Ctrl Pts',(2.04012959776072,-4.51015185496902,29.6399294027091));
#61039=CARTESIAN_POINT('Ctrl Pts',(0.549751337895761,-5.18431203852589,
29.5870091486272));
#61040=CARTESIAN_POINT('Ctrl Pts',(-1.307839031517,-5.04666968614595,29.5340888945452));
#61041=CARTESIAN_POINT('Ctrl Pts',(-2.68257979015076,-4.16021203843222,
29.4811686404633));
#61042=CARTESIAN_POINT('Ctrl Pts',(-4.05807756664059,-3.27326625194488,
29.4282192451945));
#61043=CARTESIAN_POINT('Ctrl Pts',(-4.95019356454733,-1.6366802542765,29.3752698499257));
#61044=CARTESIAN_POINT('Ctrl Pts',(-4.95011089075521,-1.68287949581236E-5,
29.3223204546569));
#61045=CARTESIAN_POINT('Ctrl Pts',(-4.9500545842803,0.000473333830474247,
29.1776795453432));
#61046=CARTESIAN_POINT('Ctrl Pts',(-4.94785444726563,-1.60994837137546,
29.2297783659501));
#61047=CARTESIAN_POINT('Ctrl Pts',(-4.08816932384676,-3.22238565418073,
29.2818771865568));
#61048=CARTESIAN_POINT('Ctrl Pts',(-2.74893267905414,-4.11666957233305,
29.3339760071636));
#61049=CARTESIAN_POINT('Ctrl Pts',(-1.38858051190673,-5.0250535168987,29.3868962612456));
#61050=CARTESIAN_POINT('Ctrl Pts',(0.466564408611941,-5.19245955856552,
29.4398165153276));
#61051=CARTESIAN_POINT('Ctrl Pts',(1.96755945318719,-4.54228015350161,29.4927367694096));
#61052=CARTESIAN_POINT('Ctrl Pts',(3.46855449776245,-3.8921007484377,29.5456570234915));
#61053=CARTESIAN_POINT('Ctrl Pts',(4.61539966639428,-2.42433589664307,29.5985772775735));
#61054=CARTESIAN_POINT('Ctrl Pts',(4.88328108437524,-0.810657201852559,
29.6514975316554));
#61055=CARTESIAN_POINT('Ctrl Pts',(5.15116250235621,0.803021492937955,29.7044177857374));
#61056=CARTESIAN_POINT('Ctrl Pts',(4.54008016968629,2.56261403072434,29.7573380398194));
#61057=CARTESIAN_POINT('Ctrl Pts',(3.3296746999557,3.66290398769728,29.8102582939013));
#61058=CARTESIAN_POINT('Ctrl Pts',(2.11926923022511,4.76319394467022,29.8631785479833));
#61059=CARTESIAN_POINT('Ctrl Pts',(0.309540623433855,5.20418132082974,29.9160988020653));
#61060=CARTESIAN_POINT('Ctrl Pts',(-1.27135167326916,4.78406356027939,29.9690190561472));
#61061=CARTESIAN_POINT('Ctrl Pts',(-2.85224396997218,4.36394579972904,30.0219393102292));
#61062=CARTESIAN_POINT('Ctrl Pts',(-4.20429995658695,3.0827229024688,30.0748595643112));
#61063=CARTESIAN_POINT('Ctrl Pts',(-4.70879816265426,1.5267020327104,30.1277798183931));
#61064=CARTESIAN_POINT('Ctrl Pts',(-4.86736582366476,1.03763272218799,30.1444130607098));
#61065=CARTESIAN_POINT('Ctrl Pts',(-4.94220382950374,0.521416307353422,
30.1610463030265));
#61066=CARTESIAN_POINT('Ctrl Pts',(-4.93818673588435,0.0040670116119004,
30.1776795453432));
#61067=CARTESIAN_POINT('Origin',(0.,0.,16.));
#61068=CARTESIAN_POINT('',(-4.9351415428321,-0.00248504100164359,31.3223204546569));
#61069=CARTESIAN_POINT('',(-4.93557330743154,-0.0028385321285674,31.1776795453432));
#61070=CARTESIAN_POINT('',(-4.942,-6.05220448138622E-16,16.));
#61071=CARTESIAN_POINT('Ctrl Pts',(-4.9351415428321,-0.00248504100164359,
31.3223204546569));
#61072=CARTESIAN_POINT('Ctrl Pts',(-4.93066017409234,0.981733357670619,
31.2907259781606));
#61073=CARTESIAN_POINT('Ctrl Pts',(-4.6457448695693,1.96834170751759,31.2591315016643));
#61074=CARTESIAN_POINT('Ctrl Pts',(-4.09792294976925,2.77680140323666,31.227537025168));
#61075=CARTESIAN_POINT('Ctrl Pts',(-3.18032980050788,4.13095875151604,31.1746167710861));
#61076=CARTESIAN_POINT('Ctrl Pts',(-1.52513305096331,4.98530711426681,31.1216965170041));
#61077=CARTESIAN_POINT('Ctrl Pts',(0.110223986946674,4.94888363249201,31.0687762629222));
#61078=CARTESIAN_POINT('Ctrl Pts',(1.74558102485669,4.91246015071721,31.0158560088402));
#61079=CARTESIAN_POINT('Ctrl Pts',(3.36109835113211,3.98526482441679,30.9629357547582));
#61080=CARTESIAN_POINT('Ctrl Pts',(4.2174905639687,2.59159639567501,30.9100155006763));
#61081=CARTESIAN_POINT('Ctrl Pts',(5.0738827768053,1.19792796693324,30.8570952465943));
#61082=CARTESIAN_POINT('Ctrl Pts',(5.17114987620307,-0.662213564249888,
30.8041749925123));
#61083=CARTESIAN_POINT('Ctrl Pts',(4.46478095192916,-2.13759902381238,30.7512547384304));
#61084=CARTESIAN_POINT('Ctrl Pts',(3.75841202765526,-3.61298448337487,30.6983344843484));
#61085=CARTESIAN_POINT('Ctrl Pts',(2.2484070797097,-4.70361387131672,30.6454142302665));
#61086=CARTESIAN_POINT('Ctrl Pts',(0.625767434156371,-4.91039852288288,
30.5924939761845));
#61087=CARTESIAN_POINT('Ctrl Pts',(-0.996872211396971,-5.11718317444904,
30.5395737221025));
#61088=CARTESIAN_POINT('Ctrl Pts',(-2.73214655455809,-4.44012308963949,
30.4866534680206));
#61089=CARTESIAN_POINT('Ctrl Pts',(-3.78596755363747,-3.18905130375701,
30.4337332139386));
#61090=CARTESIAN_POINT('Ctrl Pts',(-4.52550233311024,-2.31109280977609,
30.3965956275114));
#61091=CARTESIAN_POINT('Ctrl Pts',(-4.92943890178742,-1.1504483453926,30.3594580410841));
#61092=CARTESIAN_POINT('Ctrl Pts',(-4.93888642291793,0.00424076360118208,
30.3223204546569));
#61093=CARTESIAN_POINT('Ctrl Pts',(-4.93818673588435,0.0040670116119004,
30.1776795453432));
#61094=CARTESIAN_POINT('Ctrl Pts',(-4.92942306127099,-1.12458004491972,
30.2139665571085));
#61095=CARTESIAN_POINT('Ctrl Pts',(-4.54535955813864,-2.25861888984588,
30.2502535688737));
#61096=CARTESIAN_POINT('Ctrl Pts',(-3.83660874069347,-3.12794382961597,
30.286540580639));
#61097=CARTESIAN_POINT('Ctrl Pts',(-2.80298068714555,-4.39574997992736,
30.339460834721));
#61098=CARTESIAN_POINT('Ctrl Pts',(-1.0787841545299,-5.10054343829356,30.3923810888029));
#61099=CARTESIAN_POINT('Ctrl Pts',(0.546962191086786,-4.91979995442398,
30.4453013428849));
#61100=CARTESIAN_POINT('Ctrl Pts',(2.17270853670347,-4.73905647055441,30.4982215969669));
#61101=CARTESIAN_POINT('Ctrl Pts',(3.7000046953212,-3.67277604444905,30.5511418510488));
#61102=CARTESIAN_POINT('Ctrl Pts',(4.4299366186172,-2.20890488388769,30.6040621051308));
#61103=CARTESIAN_POINT('Ctrl Pts',(5.1598685419132,-0.745033723326325,30.6569823592128));
#61104=CARTESIAN_POINT('Ctrl Pts',(5.09243622988746,1.11642817169105,30.7099026132947));
#61105=CARTESIAN_POINT('Ctrl Pts',(4.25849773850338,2.52364740836047,30.7628228673767));
#61106=CARTESIAN_POINT('Ctrl Pts',(3.42455924711931,3.93086664502988,30.8157431214587));
#61107=CARTESIAN_POINT('Ctrl Pts',(1.8241145763769,4.88384322335134,30.8686633755406));
#61108=CARTESIAN_POINT('Ctrl Pts',(0.189551650661496,4.9464805066113,30.9215836296226));
#61109=CARTESIAN_POINT('Ctrl Pts',(-1.44501127505389,5.00911778987126,30.9745038837045));
#61110=CARTESIAN_POINT('Ctrl Pts',(-3.11369245574226,4.18141577806974,31.0274241377865));
#61111=CARTESIAN_POINT('Ctrl Pts',(-4.05287789782628,2.84214355302423,31.0803443918685));
#61112=CARTESIAN_POINT('Ctrl Pts',(-4.62868616337827,2.0210447769463,31.1127894430267));
#61113=CARTESIAN_POINT('Ctrl Pts',(-4.93028912913986,1.0076552769297,31.145234494185));
#61114=CARTESIAN_POINT('Ctrl Pts',(-4.93557330743154,-0.0028385321285674,
31.1776795453432));
#61115=CARTESIAN_POINT('Origin',(0.,0.,16.));
#61116=CARTESIAN_POINT('',(-4.94795422753399,-0.0028972882267797,32.3223204546569));
#61117=CARTESIAN_POINT('',(-4.94851874366221,-0.00251525819571033,32.1776795453432));
#61118=CARTESIAN_POINT('',(-4.942,-6.05220448138622E-16,16.));
#61119=CARTESIAN_POINT('Ctrl Pts',(-4.94795422753399,-0.0028972882267797,
32.3223204546569));
#61120=CARTESIAN_POINT('Ctrl Pts',(-4.93774012235113,1.46412544671205,32.2749141693191));
#61121=CARTESIAN_POINT('Ctrl Pts',(-4.24380482164535,2.93954073272814,32.2275078839812));
#61122=CARTESIAN_POINT('Ctrl Pts',(-3.10183998936669,3.85774379859783,32.1801015986434));
#61123=CARTESIAN_POINT('Ctrl Pts',(-1.82704976595674,4.88274584628794,32.1271813445614));
#61124=CARTESIAN_POINT('Ctrl Pts',(0.00605460139836145,5.21337522038518,
32.0742610904795));
#61125=CARTESIAN_POINT('Ctrl Pts',(1.55861655774584,4.69833086969986,32.0213408363975));
#61126=CARTESIAN_POINT('Ctrl Pts',(3.11117851409333,4.18328651901453,31.9684205823155));
#61127=CARTESIAN_POINT('Ctrl Pts',(4.38319805943319,2.82256844354664,31.9155003282335));
#61128=CARTESIAN_POINT('Ctrl Pts',(4.79257962264663,1.23886201646757,31.8625800741516));
#61129=CARTESIAN_POINT('Ctrl Pts',(5.20196118586006,-0.344844410611489,
31.8096598200696));
#61130=CARTESIAN_POINT('Ctrl Pts',(4.74870476694708,-2.15153918930172,31.7567395659877));
#61131=CARTESIAN_POINT('Ctrl Pts',(3.64022742565071,-3.35445119576896,31.7038193119057));
#61132=CARTESIAN_POINT('Ctrl Pts',(2.53175008435434,-4.5573632022362,31.6508990578238));
#61133=CARTESIAN_POINT('Ctrl Pts',(0.768051820674579,-5.15649243648045,
31.5979788037418));
#61134=CARTESIAN_POINT('Ctrl Pts',(-0.843772103495588,-4.87766821059161,
31.5450585496598));
#61135=CARTESIAN_POINT('Ctrl Pts',(-2.45559602766576,-4.59884398470276,
31.4921382955779));
#61136=CARTESIAN_POINT('Ctrl Pts',(-3.91554561232635,-3.44206629868081,
31.4392180414959));
#61137=CARTESIAN_POINT('Ctrl Pts',(-4.55552563016757,-1.93669428876581,
31.386297787414));
#61138=CARTESIAN_POINT('Ctrl Pts',(-4.81342445844275,-1.33006022730727,
31.3649720098283));
#61139=CARTESIAN_POINT('Ctrl Pts',(-4.93816639665535,-0.66681706968053,
31.3436462322426));
#61140=CARTESIAN_POINT('Ctrl Pts',(-4.9351415428321,-0.00248504100164359,
31.3223204546569));
#61141=CARTESIAN_POINT('Ctrl Pts',(-4.93557330743154,-0.0028385321285674,
31.1776795453432));
#61142=CARTESIAN_POINT('Ctrl Pts',(-4.93890801084376,-0.640534114505631,
31.1981547482669));
#61143=CARTESIAN_POINT('Ctrl Pts',(-4.82423274680824,-1.27707647808528,
31.2186299511906));
#61144=CARTESIAN_POINT('Ctrl Pts',(-4.58598979744053,-1.86340999470999,
31.2391051541143));
#61145=CARTESIAN_POINT('Ctrl Pts',(-3.97022655149108,-3.3788488791092,31.2920254081963));
#61146=CARTESIAN_POINT('Ctrl Pts',(-2.5290103561125,-4.55888420961813,31.3449456622783));
#61147=CARTESIAN_POINT('Ctrl Pts',(-0.921863753563045,-4.86351379667883,
31.3978659163602));
#61148=CARTESIAN_POINT('Ctrl Pts',(0.685282848986421,-5.16814338373953,
31.4507861704422));
#61149=CARTESIAN_POINT('Ctrl Pts',(2.45835985870677,-4.59736722735202,31.5037064245242));
#61150=CARTESIAN_POINT('Ctrl Pts',(3.5859801562746,-3.4123812139678,31.5566266786061));
#61151=CARTESIAN_POINT('Ctrl Pts',(4.71360045384243,-2.22739520058358,31.6095469326881));
#61152=CARTESIAN_POINT('Ctrl Pts',(5.19576403925773,-0.428199330202661,
31.6624671867701));
#61153=CARTESIAN_POINT('Ctrl Pts',(4.81182549189739,1.16186688830996,31.715387440852));
#61154=CARTESIAN_POINT('Ctrl Pts',(4.42788694453706,2.75193310682255,31.768307694934));
#61155=CARTESIAN_POINT('Ctrl Pts',(3.17784626440109,4.13286967346687,31.8212279490159));
#61156=CARTESIAN_POINT('Ctrl Pts',(1.63374115821347,4.67273892471915,31.8741482030979));
#61157=CARTESIAN_POINT('Ctrl Pts',(0.0896360520258116,5.21260817597145,
31.9270684571799));
#61158=CARTESIAN_POINT('Ctrl Pts',(-1.74853348021352,4.91141011183171,31.9799887112618));
#61159=CARTESIAN_POINT('Ctrl Pts',(-3.0395929867415,3.90697756655707,32.0329089653438));
#61160=CARTESIAN_POINT('Ctrl Pts',(-4.21688283424399,2.99105678050979,32.0811658253436));
#61161=CARTESIAN_POINT('Ctrl Pts',(-4.93923809973741,1.49038033345358,32.1294226853434));
#61162=CARTESIAN_POINT('Ctrl Pts',(-4.94851874366221,-0.00251525819571033,
32.1776795453432));
#61163=CARTESIAN_POINT('Origin',(0.,0.,16.));
#61164=CARTESIAN_POINT('',(-4.94391378591308,0.00432614989180041,33.3223204546569));
#61165=CARTESIAN_POINT('',(-4.943114998001,0.00443591996608837,33.1776795453432));
#61166=CARTESIAN_POINT('',(-4.942,-6.05220448138622E-16,16.));
#61167=CARTESIAN_POINT('Ctrl Pts',(-4.94391378591308,0.00432614989180041,
33.3223204546569));
#61168=CARTESIAN_POINT('Ctrl Pts',(-4.94684012248784,0.323678273041629,
33.3120226145595));
#61169=CARTESIAN_POINT('Ctrl Pts',(-4.91854579890533,0.642514059921896,
33.3017247744621));
#61170=CARTESIAN_POINT('Ctrl Pts',(-4.8571468315969,0.954841972036427,33.2914269343646));
#61171=CARTESIAN_POINT('Ctrl Pts',(-4.54161960262542,2.55988461298029,33.2385066802827));
#61172=CARTESIAN_POINT('Ctrl Pts',(-3.3518326489115,3.99306094874791,33.1855864262007));
#61173=CARTESIAN_POINT('Ctrl Pts',(-1.83225065173251,4.59852759962142,33.1326661721187));
#61174=CARTESIAN_POINT('Ctrl Pts',(-0.312668654553525,5.20399425049493,
33.0797459180367));
#61175=CARTESIAN_POINT('Ctrl Pts',(1.53670838609054,4.98175121647435,33.0268256639548));
#61176=CARTESIAN_POINT('Ctrl Pts',(2.86957729142234,4.03350030417842,32.9739054098728));
#61177=CARTESIAN_POINT('Ctrl Pts',(4.20244619675414,3.0852493918825,32.9209851557909));
#61178=CARTESIAN_POINT('Ctrl Pts',(5.01880696677368,1.41099060131123,32.8680649017089));
#61179=CARTESIAN_POINT('Ctrl Pts',(4.94508044508782,-0.223109674519649,
32.8151446476269));
#61180=CARTESIAN_POINT('Ctrl Pts',(4.87135392340196,-1.85720995035054,32.762224393545));
#61181=CARTESIAN_POINT('Ctrl Pts',(3.90754011001068,-3.45115171144104,32.709304139463));
#61182=CARTESIAN_POINT('Ctrl Pts',(2.49469492595997,-4.27552286412362,32.6563838853811));
#61183=CARTESIAN_POINT('Ctrl Pts',(1.08184974190924,-5.0998940168062,32.6034636312991));
#61184=CARTESIAN_POINT('Ctrl Pts',(-0.780026812800927,-5.15469456108083,
32.5505433772171));
#61185=CARTESIAN_POINT('Ctrl Pts',(-2.2389115908552,-4.41484693093525,32.4976231231352));
#61186=CARTESIAN_POINT('Ctrl Pts',(-3.69779636890945,-3.67499930078968,
32.4447028690532));
#61187=CARTESIAN_POINT('Ctrl Pts',(-4.75368937030783,-2.14050349622394,
32.3917826149712));
#61188=CARTESIAN_POINT('Ctrl Pts',(-4.92339783127462,-0.513568233299591,
32.3388623608893));
#61189=CARTESIAN_POINT('Ctrl Pts',(-4.94108042115667,-0.344051469933491,
32.3333483921451));
#61190=CARTESIAN_POINT('Ctrl Pts',(-4.94914226106849,-0.173531149322059,
32.327834423401));
#61191=CARTESIAN_POINT('Ctrl Pts',(-4.94795422753399,-0.0028972882267797,
32.3223204546569));
#61192=CARTESIAN_POINT('Ctrl Pts',(-4.94851874366221,-0.00251525819571033,
32.1776795453432));
#61193=CARTESIAN_POINT('Ctrl Pts',(-4.94941559646112,-0.146784082719192,
32.1823429394254));
#61194=CARTESIAN_POINT('Ctrl Pts',(-4.9436532640282,-0.290980244219974,
32.1870063335075));
#61195=CARTESIAN_POINT('Ctrl Pts',(-4.93099878465363,-0.434569000702025,
32.1916697275897));
#61196=CARTESIAN_POINT('Ctrl Pts',(-4.78739559522113,-2.06401599627693,
32.2445899816717));
#61197=CARTESIAN_POINT('Ctrl Pts',(-3.75623973553951,-3.61524296101718,
32.2975102357536));
#61198=CARTESIAN_POINT('Ctrl Pts',(-2.30940387553184,-4.3783847444355,32.3504304898356));
#61199=CARTESIAN_POINT('Ctrl Pts',(-0.862568015524189,-5.14152652785381,
32.4033507439175));
#61200=CARTESIAN_POINT('Ctrl Pts',(0.999947844809495,-5.11658312995021,
32.4562709979995));
#61201=CARTESIAN_POINT('Ctrl Pts',(2.4258280021366,-4.3149690305583,32.5091912520815));
#61202=CARTESIAN_POINT('Ctrl Pts',(3.85170815946372,-3.51335493116639,32.5621115061634));
#61203=CARTESIAN_POINT('Ctrl Pts',(4.84095261378425,-1.93507013028614,32.6150317602454));
#61204=CARTESIAN_POINT('Ctrl Pts',(4.9408679943685,-0.30236185746891,32.6679520143274));
#61205=CARTESIAN_POINT('Ctrl Pts',(5.04078337495275,1.33034641534833,32.7208722684093));
#61206=CARTESIAN_POINT('Ctrl Pts',(4.25136968180072,3.01747816010256,32.7737925224913));
#61207=CARTESIAN_POINT('Ctrl Pts',(2.93387467737636,3.9869761233392,32.8267127765732));
#61208=CARTESIAN_POINT('Ctrl Pts',(1.616379672952,4.95647408657584,32.8796330306552));
#61209=CARTESIAN_POINT('Ctrl Pts',(-0.229196642744684,5.20833826829488,
32.9325532847372));
#61210=CARTESIAN_POINT('Ctrl Pts',(-1.75829036071957,4.62731177229585,32.9854735388191));
#61211=CARTESIAN_POINT('Ctrl Pts',(-3.28738407869442,4.04628527629685,33.0383937929011));
#61212=CARTESIAN_POINT('Ctrl Pts',(-4.49999519894748,2.63236810257984,33.091314046983));
#61213=CARTESIAN_POINT('Ctrl Pts',(-4.8412143530065,1.03259034416892,33.144234301065));
#61214=CARTESIAN_POINT('Ctrl Pts',(-4.91309708900794,0.695574086725974,
33.1553827158244));
#61215=CARTESIAN_POINT('Ctrl Pts',(-4.94630788623483,0.350309429675576,
33.1665311305838));
#61216=CARTESIAN_POINT('Ctrl Pts',(-4.943114998001,0.00443591996608837,
33.1776795453432));
#61217=CARTESIAN_POINT('Origin',(0.,0.,16.));
#61218=CARTESIAN_POINT('',(-4.93390856647989,0.000179243442527399,34.3223204546569));
#61219=CARTESIAN_POINT('',(-4.93391474235666,-0.000255694835337854,34.1776795453433));
#61220=CARTESIAN_POINT('',(-4.942,-6.05220448138622E-16,16.));
#61221=CARTESIAN_POINT('Ctrl Pts',(-4.93390856647989,0.000179243442527399,
34.3223204546569));
#61222=CARTESIAN_POINT('Ctrl Pts',(-4.93417188922503,0.81404442559312,34.2962108057179));
#61223=CARTESIAN_POINT('Ctrl Pts',(-4.7439659144325,1.62779374632659,34.2701011567789));
#61224=CARTESIAN_POINT('Ctrl Pts',(-4.36261434797766,2.33905848282458,34.24399150784));
#61225=CARTESIAN_POINT('Ctrl Pts',(-3.58967320891792,3.780683020289,34.191071253758));
#61226=CARTESIAN_POINT('Ctrl Pts',(-2.03148547319181,4.80128989115793,34.138150999676));
#61227=CARTESIAN_POINT('Ctrl Pts',(-0.401101646399658,4.93383380390034,
34.0852307455941));
#61228=CARTESIAN_POINT('Ctrl Pts',(1.22928218039249,5.06637771664275,34.0323104915121));
#61229=CARTESIAN_POINT('Ctrl Pts',(2.93186209825069,4.31085867125863,33.9793902374301));
#61230=CARTESIAN_POINT('Ctrl Pts',(3.92751153377263,3.01301372173064,33.9264699833482));
#61231=CARTESIAN_POINT('Ctrl Pts',(4.92316096929458,1.71516877220265,33.8735497292662));
#61232=CARTESIAN_POINT('Ctrl Pts',(5.21187992248028,-0.125002081469193,
33.8206294751842));
#61233=CARTESIAN_POINT('Ctrl Pts',(4.66154619083434,-1.6654085522694,33.7677092211023));
#61234=CARTESIAN_POINT('Ctrl Pts',(4.1112124591884,-3.2058150230696,33.7147889670203));
#61235=CARTESIAN_POINT('Ctrl Pts',(2.72182604271081,-4.44645711099814,33.6618687129384));
#61236=CARTESIAN_POINT('Ctrl Pts',(1.12919138526205,-4.8195980486659,33.6089484588564));
#61237=CARTESIAN_POINT('Ctrl Pts',(-0.463443272186686,-5.19273898633366,
33.5560282047744));
#61238=CARTESIAN_POINT('Ctrl Pts',(-2.25932617060659,-4.69837877374066,
33.5031079506925));
#61239=CARTESIAN_POINT('Ctrl Pts',(-3.43663386770201,-3.56274419438412,
33.4501876966105));
#61240=CARTESIAN_POINT('Ctrl Pts',(-4.384847305511,-2.64809463314952,33.407565282626));
#61241=CARTESIAN_POINT('Ctrl Pts',(-4.93180177720373,-1.3174615522823,33.3649428686414));
#61242=CARTESIAN_POINT('Ctrl Pts',(-4.94391378591308,0.00432614989180041,
33.3223204546569));
#61243=CARTESIAN_POINT('Ctrl Pts',(-4.943114998001,0.00443591996608837,
33.1776795453432));
#61244=CARTESIAN_POINT('Ctrl Pts',(-4.93115160973848,-1.2915126956278,33.2194513846658));
#61245=CARTESIAN_POINT('Ctrl Pts',(-4.40811124636647,-2.59600908794704,
33.2612232239884));
#61246=CARTESIAN_POINT('Ctrl Pts',(-3.49331109260409,-3.50718930782419,
33.3029950633109));
#61247=CARTESIAN_POINT('Ctrl Pts',(-2.33436149027767,-4.6615528583015,33.3559153173929));
#61248=CARTESIAN_POINT('Ctrl Pts',(-0.54663509775989,-5.18464161615124,
33.4088355714748));
#61249=CARTESIAN_POINT('Ctrl Pts',(1.0517771843263,-4.83708217680429,33.4617558255568));
#61250=CARTESIAN_POINT('Ctrl Pts',(2.65018946641248,-4.48952273745735,33.5146760796387));
#61251=CARTESIAN_POINT('Ctrl Pts',(4.05928763806706,-3.27131510091373,33.5675963337207));
#61252=CARTESIAN_POINT('Ctrl Pts',(4.63424685520885,-1.73992968697417,33.6205165878027));
#61253=CARTESIAN_POINT('Ctrl Pts',(5.20920607235062,-0.208544273034641,
33.6734368418847));
#61254=CARTESIAN_POINT('Ctrl Pts',(4.95002633497964,1.63601891830083,33.7263570959666));
#61255=CARTESIAN_POINT('Ctrl Pts',(3.97531224929094,2.94965959921896,33.7792773500486));
#61256=CARTESIAN_POINT('Ctrl Pts',(3.00059816360222,4.26330028013712,33.8321976041305));
#61257=CARTESIAN_POINT('Ctrl Pts',(1.31034972959575,5.04601845063795,33.8851178582125));
#61258=CARTESIAN_POINT('Ctrl Pts',(-0.321949554671762,4.93963032168135,
33.9380381122945));
#61259=CARTESIAN_POINT('Ctrl Pts',(-1.95424883893928,4.83324219272475,33.9909583663764));
#61260=CARTESIAN_POINT('Ctrl Pts',(-3.52859897346783,3.83774776431073,34.0438786204584));
#61261=CARTESIAN_POINT('Ctrl Pts',(-4.32455329212167,2.40870049076816,34.0967988745404));
#61262=CARTESIAN_POINT('Ctrl Pts',(-4.73005222214988,1.68067235297088,34.1237590981413));
#61263=CARTESIAN_POINT('Ctrl Pts',(-4.93352684267558,0.840120210825594,
34.1507193217423));
#61264=CARTESIAN_POINT('Ctrl Pts',(-4.93391474235666,-0.000255694835337854,
34.1776795453433));
#61265=CARTESIAN_POINT('Origin',(0.,0.,16.));
#61266=CARTESIAN_POINT('',(-4.94325592752636,-0.00441992691212867,35.3223204546569));
#61267=CARTESIAN_POINT('',(-4.94405342481732,-0.00430212276008984,35.1776795453432));
#61268=CARTESIAN_POINT('',(-4.942,-6.05220448138622E-16,16.));
#61269=CARTESIAN_POINT('Ctrl Pts',(-4.94325592752636,-0.00441992691212867,
35.3223204546569));
#61270=CARTESIAN_POINT('Ctrl Pts',(-4.93125773853651,1.29607520943411,35.2803989968764));
#61271=CARTESIAN_POINT('Ctrl Pts',(-4.40405811483643,2.60517623543917,35.2384775390958));
#61272=CARTESIAN_POINT('Ctrl Pts',(-3.48340604301779,3.51702727807467,35.1965560813153));
#61273=CARTESIAN_POINT('Ctrl Pts',(-2.32120548652017,4.66811770803537,35.1436358272333));
#61274=CARTESIAN_POINT('Ctrl Pts',(-0.53201099429802,5.18616256481328,35.0907155731514));
#61275=CARTESIAN_POINT('Ctrl Pts',(1.06541470817911,4.83409661000376,35.0377953190694));
#61276=CARTESIAN_POINT('Ctrl Pts',(2.66284041065621,4.48203065519423,34.9848750649874));
#61277=CARTESIAN_POINT('Ctrl Pts',(4.0684973233883,3.25985388879729,34.9319548109055));
#61278=CARTESIAN_POINT('Ctrl Pts',(4.63913537493446,1.72685306505386,34.8790345568235));
#61279=CARTESIAN_POINT('Ctrl Pts',(5.20977342648062,0.193852241310417,34.8261143027416));
#61280=CARTESIAN_POINT('Ctrl Pts',(4.94539261684082,-1.64997263977952,34.7731940486596));
#61281=CARTESIAN_POINT('Ctrl Pts',(3.96697764231472,-2.96085915244703,34.7202737945776));
#61282=CARTESIAN_POINT('Ctrl Pts',(2.98856266778862,-4.27174566511454,34.6673535404957));
#61283=CARTESIAN_POINT('Ctrl Pts',(1.29611352837622,-5.04969380935962,34.6144332864137));
#61284=CARTESIAN_POINT('Ctrl Pts',(-0.335879201461312,-4.93870263300798,
34.5615130323317));
#61285=CARTESIAN_POINT('Ctrl Pts',(-1.96787193129885,-4.82771145665634,
34.5085927782498));
#61286=CARTESIAN_POINT('Ctrl Pts',(-3.53940825156152,-3.82778095970798,
34.4556725241678));
#61287=CARTESIAN_POINT('Ctrl Pts',(-4.33132914049615,-2.39649460920384,
34.4027522700858));
#61288=CARTESIAN_POINT('Ctrl Pts',(-4.73253428635246,-1.67137236904084,
34.3759416649429));
#61289=CARTESIAN_POINT('Ctrl Pts',(-4.93363817440523,-0.835535479848384,
34.3491310597999));
#61290=CARTESIAN_POINT('Ctrl Pts',(-4.93390856647989,0.000179243442527399,
34.3223204546569));
#61291=CARTESIAN_POINT('Ctrl Pts',(-4.93391474235666,-0.000255694835337854,
34.1776795453433));
#61292=CARTESIAN_POINT('Ctrl Pts',(-4.93428825140812,-0.80945462617062,
34.2036395758242));
#61293=CARTESIAN_POINT('Ctrl Pts',(-4.7463640914517,-1.61849015480256,34.2295996063052));
#61294=CARTESIAN_POINT('Ctrl Pts',(-4.36919376142154,-2.32674560401052,
34.2555596367863));
#61295=CARTESIAN_POINT('Ctrl Pts',(-3.60032140928848,-3.77054430657554,
34.3084798908682));
#61296=CARTESIAN_POINT('Ctrl Pts',(-2.04501820224325,-4.79554159303451,
34.3614001449502));
#61297=CARTESIAN_POINT('Ctrl Pts',(-0.415014641507274,-4.93268305062891,
34.4143203990321));
#61298=CARTESIAN_POINT('Ctrl Pts',(1.21498891922872,-5.0698245082233,34.4672406531141));
#61299=CARTESIAN_POINT('Ctrl Pts',(2.91969283365546,-4.31911013695313,34.5201609071961));
#61300=CARTESIAN_POINT('Ctrl Pts',(3.91899855510175,-3.02407829854611,34.573081161278));
#61301=CARTESIAN_POINT('Ctrl Pts',(4.91830427654803,-1.72904646013911,34.62600141536));
#61302=CARTESIAN_POINT('Ctrl Pts',(5.21221180501386,0.110302845404735,34.678921669442));
#61303=CARTESIAN_POINT('Ctrl Pts',(4.66622456671209,1.65225528404048,34.7318419235239));
#61304=CARTESIAN_POINT('Ctrl Pts',(4.12023732841032,3.19420772267622,34.7847621776059));
#61305=CARTESIAN_POINT('Ctrl Pts',(2.73435532334095,4.43876329440389,34.8376824316879));
#61306=CARTESIAN_POINT('Ctrl Pts',(1.14277932318225,4.81639436187842,34.8906026857698));
#61307=CARTESIAN_POINT('Ctrl Pts',(-0.448796676976434,5.19402542935295,
34.9435229398518));
#61308=CARTESIAN_POINT('Ctrl Pts',(-2.24606667222443,4.70473199257438,34.9964431939337));
#61309=CARTESIAN_POINT('Ctrl Pts',(-3.42657246357288,3.57242220104389,35.0493634480157));
#61310=CARTESIAN_POINT('Ctrl Pts',(-4.38069925079363,2.65724913586347,35.0921354804582));
#61311=CARTESIAN_POINT('Ctrl Pts',(-4.93192805452064,1.32202900724285,35.1349075129007));
#61312=CARTESIAN_POINT('Ctrl Pts',(-4.94405342481732,-0.00430212276008983,
35.1776795453432));
#61313=CARTESIAN_POINT('Origin',(0.,0.,16.));
#61314=CARTESIAN_POINT('',(-4.94842418382236,0.0025848059749288,36.3223204546569));
#61315=CARTESIAN_POINT('',(-4.9478484900732,0.00296101277178129,36.1776795453433));
#61316=CARTESIAN_POINT('',(-4.942,-6.05220448138622E-16,16.));
#61317=CARTESIAN_POINT('Ctrl Pts',(-4.94842418382236,0.0025848059749288,
36.3223204546569));
#61318=CARTESIAN_POINT('Ctrl Pts',(-4.94937063025513,0.151489796715591,
36.3175074421168));
#61319=CARTESIAN_POINT('Ctrl Pts',(-4.94323189211144,0.300315679824302,
36.3126944295766));
#61320=CARTESIAN_POINT('Ctrl Pts',(-4.92975351682066,0.448473855033485,
36.3078814170365));
#61321=CARTESIAN_POINT('Ctrl Pts',(-4.78155547265312,2.07750935224505,36.2549611629546));
#61322=CARTESIAN_POINT('Ctrl Pts',(-3.74602889959972,3.62582202129232,36.2020409088726));
#61323=CARTESIAN_POINT('Ctrl Pts',(-2.2970465727752,4.38488033790615,36.1491206547906));
#61324=CARTESIAN_POINT('Ctrl Pts',(-0.848064245950652,5.14393865451998,
36.0962004007087));
#61325=CARTESIAN_POINT('Ctrl Pts',(1.01437383464502,5.11374261870034,36.0432801466267));
#61326=CARTESIAN_POINT('Ctrl Pts',(2.43798755887529,4.30811039761326,35.9903598925447));
#61327=CARTESIAN_POINT('Ctrl Pts',(3.86160128310556,3.50247817652618,35.9374396384628));
#61328=CARTESIAN_POINT('Ctrl Pts',(4.84639065097043,1.92140977017166,35.8845193843808));
#61329=CARTESIAN_POINT('Ctrl Pts',(4.94170100734347,0.28842622847917,35.8315991302989));
#61330=CARTESIAN_POINT('Ctrl Pts',(5.03701136371651,-1.34455731321331,35.7786788762169));
#61331=CARTESIAN_POINT('Ctrl Pts',(4.24284270859772,-3.02945599024377,35.7257586221349));
#61332=CARTESIAN_POINT('Ctrl Pts',(2.92261874766819,-3.99523443505293,35.6728383680529));
#61333=CARTESIAN_POINT('Ctrl Pts',(1.60239478673866,-4.96101287986208,35.619918113971));
#61334=CARTESIAN_POINT('Ctrl Pts',(-0.243884480001596,-5.20767109244996,
35.566997859889));
#61335=CARTESIAN_POINT('Ctrl Pts',(-1.77133346242501,-4.62233450759977,
35.5140776058071));
#61336=CARTESIAN_POINT('Ctrl Pts',(-3.29878244484848,-4.03699792274956,
35.4611573517251));
#61337=CARTESIAN_POINT('Ctrl Pts',(-4.50740114295507,-2.61966654046123,
35.4082370976431));
#61338=CARTESIAN_POINT('Ctrl Pts',(-4.84410718162179,-1.01893284774532,
35.3553168435612));
#61339=CARTESIAN_POINT('Ctrl Pts',(-4.91408721473011,-0.686240873293583,
35.3443180472597));
#61340=CARTESIAN_POINT('Ctrl Pts',(-4.94640385328257,-0.345626598935659,
35.3333192509583));
#61341=CARTESIAN_POINT('Ctrl Pts',(-4.94325592752636,-0.00441992691212867,
35.3223204546569));
#61342=CARTESIAN_POINT('Ctrl Pts',(-4.94405342481732,-0.00430212276008983,
35.1776795453432));
#61343=CARTESIAN_POINT('Ctrl Pts',(-4.94693032680687,-0.318991453753773,
35.1878277669827));
#61344=CARTESIAN_POINT('Ctrl Pts',(-4.91945907962359,-0.633180389759553,
35.1979759886221));
#61345=CARTESIAN_POINT('Ctrl Pts',(-4.85982046564743,-0.941139879242983,
35.2081242102616));
#61346=CARTESIAN_POINT('Ctrl Pts',(-4.54882108892463,-2.5470660217169,35.2610444643436));
#61347=CARTESIAN_POINT('Ctrl Pts',(-3.36308074803015,-3.98359216038229,
35.3139647184255));
#61348=CARTESIAN_POINT('Ctrl Pts',(-1.84521233241245,-4.59334199455474,
35.3668849725075));
#61349=CARTESIAN_POINT('Ctrl Pts',(-0.327343916794751,-5.2030918287272,
35.4198052265894));
#61350=CARTESIAN_POINT('Ctrl Pts',(1.52265257354617,-4.98606535840671,35.4727254806714));
#61351=CARTESIAN_POINT('Ctrl Pts',(2.858190490191,-4.04157721099188,35.5256457347534));
#61352=CARTESIAN_POINT('Ctrl Pts',(4.19372840683581,-3.09708906357705,35.5785659888353));
#61353=CARTESIAN_POINT('Ctrl Pts',(5.01480774978454,-1.42513923906789,35.6314862429173));
#61354=CARTESIAN_POINT('Ctrl Pts',(4.94569007160633,0.20916248765404,35.6844064969993));
#61355=CARTESIAN_POINT('Ctrl Pts',(4.87657239342812,1.843464214376,35.7373267510812));
#61356=CARTESIAN_POINT('Ctrl Pts',(3.91725769412294,3.44011784331073,35.7902470051632));
#61357=CARTESIAN_POINT('Ctrl Pts',(2.50674303141734,4.26847028864764,35.8431672592451));
#61358=CARTESIAN_POINT('Ctrl Pts',(1.09622836871175,5.09682273398456,35.8960875133271));
#61359=CARTESIAN_POINT('Ctrl Pts',(-0.765486257394255,5.15687399572365,
35.9490077674091));
#61360=CARTESIAN_POINT('Ctrl Pts',(-2.2264518005877,4.42114369934827,36.001928021491));
#61361=CARTESIAN_POINT('Ctrl Pts',(-3.68741734378115,3.68541340297289,36.054848275573));
#61362=CARTESIAN_POINT('Ctrl Pts',(-4.74763380406204,2.15390154848305,36.107768529655));
#61363=CARTESIAN_POINT('Ctrl Pts',(-4.92192993683911,0.527451350812649,
36.1606887837369));
#61364=CARTESIAN_POINT('Ctrl Pts',(-4.94058331188609,0.353386757129483,
36.166352370939));
#61365=CARTESIAN_POINT('Ctrl Pts',(-4.94908977224877,0.178234784323597,
36.1720159581411));
#61366=CARTESIAN_POINT('Ctrl Pts',(-4.9478484900732,0.00296101277178129,
36.1776795453433));
#61367=CARTESIAN_POINT('Origin',(0.,0.,16.));
#61368=CARTESIAN_POINT('',(-4.93549302535697,0.00277814199197368,37.3223204546569));
#61369=CARTESIAN_POINT('',(-4.9350718820976,0.00242042316235142,37.1776795453432));
#61370=CARTESIAN_POINT('',(-4.942,-6.05220448138622E-16,16.));
#61371=CARTESIAN_POINT('Ctrl Pts',(-4.93549302535697,0.00277814199197368,
37.3223204546569));
#61372=CARTESIAN_POINT('Ctrl Pts',(-4.93877741300468,0.645159704289348,
37.3016956332752));
#61373=CARTESIAN_POINT('Ctrl Pts',(-4.82236482292357,1.2863972760676,37.2810708118936));
#61374=CARTESIAN_POINT('Ctrl Pts',(-4.5807162353096,1.87633613908203,37.2604459905119));
#61375=CARTESIAN_POINT('Ctrl Pts',(-3.96068154902433,3.39003237653315,37.2075257364299));
#61376=CARTESIAN_POINT('Ctrl Pts',(-2.51614312549289,4.56599842518147,37.1546054823479));
#61377=CARTESIAN_POINT('Ctrl Pts',(-0.908143809323614,4.86609426099016,
37.101685228266));
#61378=CARTESIAN_POINT('Ctrl Pts',(0.699855506845637,5.16619009679885,37.048764974184));
#61379=CARTESIAN_POINT('Ctrl Pts',(2.47131571565271,4.59041571976794,36.995844720102));
#61380=CARTESIAN_POINT('Ctrl Pts',(3.59558957056917,3.40225427845545,36.9429244660201));
#61381=CARTESIAN_POINT('Ctrl Pts',(4.71986342548563,2.21409283714297,36.8900042119381));
#61382=CARTESIAN_POINT('Ctrl Pts',(5.19695092651147,0.413544331548897,36.8370839578562));
#61383=CARTESIAN_POINT('Ctrl Pts',(4.80852954676355,-1.17543274293179,36.7841637037742));
#61384=CARTESIAN_POINT('Ctrl Pts',(4.42010816701563,-2.76440981741246,36.7312434496922));
#61385=CARTESIAN_POINT('Ctrl Pts',(3.16617790649396,-4.14181546077975,36.6783231956103));
#61386=CARTESIAN_POINT('Ctrl Pts',(1.6205564033125,-4.67732781392721,36.6254029415283));
#61387=CARTESIAN_POINT('Ctrl Pts',(0.0749349001310295,-5.21284016707467,
36.5724826874463));
#61388=CARTESIAN_POINT('Ctrl Pts',(-1.76237784571023,-4.90645923000227,
36.5195624333644));
#61389=CARTESIAN_POINT('Ctrl Pts',(-3.05059946099004,-3.89838959877812,
36.4666421792824));
#61390=CARTESIAN_POINT('Ctrl Pts',(-4.22165937898849,-2.98200228957926,
36.4185349377406));
#61391=CARTESIAN_POINT('Ctrl Pts',(-4.93896421945116,-1.48575712054711,
36.3704276961987));
#61392=CARTESIAN_POINT('Ctrl Pts',(-4.94842418382236,0.0025848059749288,
36.3223204546569));
#61393=CARTESIAN_POINT('Ctrl Pts',(-4.9478484900732,0.00296101277178129,
36.1776795453433));
#61394=CARTESIAN_POINT('Ctrl Pts',(-4.93749129838862,-1.4595139062905,36.2249362122231));
#61395=CARTESIAN_POINT('Ctrl Pts',(-4.24848225306339,-2.93046862920176,
36.2721928791029));
#61396=CARTESIAN_POINT('Ctrl Pts',(-3.11270745258791,-3.84898058519796,
36.3194495459828));
#61397=CARTESIAN_POINT('Ctrl Pts',(-1.84081303028634,-4.87757378268728,
36.3723698000648));
#61398=CARTESIAN_POINT('Ctrl Pts',(-0.00864838040995825,-5.21337163681495,
36.4252900541467));
#61399=CARTESIAN_POINT('Ctrl Pts',(1.54535997115889,-4.70270792099264,36.4782103082287));
#61400=CARTESIAN_POINT('Ctrl Pts',(3.09936832272773,-4.19204420517033,36.5311305623107));
#61401=CARTESIAN_POINT('Ctrl Pts',(4.37522037598902,-2.83491891939801,36.5840508163926));
#61402=CARTESIAN_POINT('Ctrl Pts',(4.78906674566614,-1.25237332141095,36.6369710704746));
#61403=CARTESIAN_POINT('Ctrl Pts',(5.20291311534324,0.330172276576089,36.6898913245566));
#61404=CARTESIAN_POINT('Ctrl Pts',(4.75475380143625,2.13813818677785,36.7428115786385));
#61405=CARTESIAN_POINT('Ctrl Pts',(3.64967335059123,3.34417159616718,36.7957318327205));
#61406=CARTESIAN_POINT('Ctrl Pts',(2.54459289974621,4.55020500555648,36.8486520868024));
#61407=CARTESIAN_POINT('Ctrl Pts',(0.782591311963154,5.15430591413334,36.9015723408844));
#61408=CARTESIAN_POINT('Ctrl Pts',(-0.830012575668756,4.88002851988171,
36.9544925949664));
#61409=CARTESIAN_POINT('Ctrl Pts',(-2.44261646330071,4.60575112563006,37.0074128490484));
#61410=CARTESIAN_POINT('Ctrl Pts',(-3.9058226507815,3.45309542854993,37.0603331031303));
#61411=CARTESIAN_POINT('Ctrl Pts',(-4.5500456396125,1.94953427978849,37.1132533572123));
#61412=CARTESIAN_POINT('Ctrl Pts',(-4.81147567364344,1.33937902438292,37.1347287532559));
#61413=CARTESIAN_POINT('Ctrl Pts',(-4.93803628002896,0.671436970049187,
37.1562041492996));
#61414=CARTESIAN_POINT('Ctrl Pts',(-4.9350718820976,0.00242042316235142,
37.1776795453432));
#61415=CARTESIAN_POINT('Origin',(0.,0.,16.));
#61416=CARTESIAN_POINT('',(-4.93830712716952,-0.00410043205665789,38.3223204546569));
#61417=CARTESIAN_POINT('',(-4.93901314208066,-0.00426717980477184,38.1776795453432));
#61418=CARTESIAN_POINT('',(-4.942,-6.05220448138622E-16,16.));
#61419=CARTESIAN_POINT('Ctrl Pts',(-4.93830712716952,-0.00410043205665789,
38.3223204546569));
#61420=CARTESIAN_POINT('Ctrl Pts',(-4.92941979674321,1.12913042651997,38.2858838244337));
#61421=CARTESIAN_POINT('Ctrl Pts',(-4.54190399082784,2.26785272885638,38.2494471942104));
#61422=CARTESIAN_POINT('Ctrl Pts',(-3.8277718834972,3.13875149433059,38.2130105639872));
#61423=CARTESIAN_POINT('Ctrl Pts',(-2.79057244061549,4.40363750783395,38.1600903099052));
#61424=CARTESIAN_POINT('Ctrl Pts',(-1.06439510407127,5.10356550944081,38.1071700558233));
#61425=CARTESIAN_POINT('Ctrl Pts',(0.560835013546147,4.91823775582626,38.0542498017413));
#61426=CARTESIAN_POINT('Ctrl Pts',(2.18606513116352,4.73291000221171,38.0013295476593));
#61427=CARTESIAN_POINT('Ctrl Pts',(3.71034802985413,3.66232649337579,37.9484092935774));
#61428=CARTESIAN_POINT('Ctrl Pts',(4.43614857526344,2.19640259366137,37.8954890394954));
#61429=CARTESIAN_POINT('Ctrl Pts',(5.16194912067276,0.730478693946923,37.8425687854135));
#61430=CARTESIAN_POINT('Ctrl Pts',(5.08926731280079,-1.13078559664599,37.7896485313315));
#61431=CARTESIAN_POINT('Ctrl Pts',(4.25136345697712,-2.53564731221314,37.7367282772495));
#61432=CARTESIAN_POINT('Ctrl Pts',(3.41345960115345,-3.94050902778028,37.6838080231676));
#61433=CARTESIAN_POINT('Ctrl Pts',(1.81033369737808,-4.88896816832161,37.6308877690856));
#61434=CARTESIAN_POINT('Ctrl Pts',(0.175600643277768,-4.9469953455946,37.5779675150036));
#61435=CARTESIAN_POINT('Ctrl Pts',(-1.45913241082256,-5.00502252286759,
37.5250472609217));
#61436=CARTESIAN_POINT('Ctrl Pts',(-3.12547261524786,-4.17261773687219,
37.4721270068397));
#61437=CARTESIAN_POINT('Ctrl Pts',(-4.06087724294093,-2.83070213074755,
37.4192067527577));
#61438=CARTESIAN_POINT('Ctrl Pts',(-4.63172289977408,-2.01177663806308,
37.3869113200575));
#61439=CARTESIAN_POINT('Ctrl Pts',(-4.93035015801884,-1.00309677586341,
37.3546158873572));
#61440=CARTESIAN_POINT('Ctrl Pts',(-4.93549302535697,0.00277814199197368,
37.3223204546569));
#61441=CARTESIAN_POINT('Ctrl Pts',(-4.9350718820976,0.00242042316235142,
37.1776795453432));
#61442=CARTESIAN_POINT('Ctrl Pts',(-4.93073133015009,-0.977171771522589,
37.2091244033815));
#61443=CARTESIAN_POINT('Ctrl Pts',(-4.64869419974499,-1.95906763650772,
37.2405692614198));
#61444=CARTESIAN_POINT('Ctrl Pts',(-4.10573795122914,-2.76523328246712,
37.2720141194581));
#61445=CARTESIAN_POINT('Ctrl Pts',(-3.19196748383364,-4.12197309551857,
37.3249343735401));
#61446=CARTESIAN_POINT('Ctrl Pts',(-1.53918675886144,-4.9809861211788,37.3778546276221));
#61447=CARTESIAN_POINT('Ctrl Pts',(0.0962665215178138,-4.94917487945839,
37.4307748817041));
#61448=CARTESIAN_POINT('Ctrl Pts',(1.73171980189707,-4.91736363773799,37.483695135786));
#61449=CARTESIAN_POINT('Ctrl Pts',(3.34984563768341,-3.99472812863699,37.536615389868));
#61450=CARTESIAN_POINT('Ctrl Pts',(4.21016493327244,-2.60348045225429,37.5895356439499));
#61451=CARTESIAN_POINT('Ctrl Pts',(5.07048422886148,-1.21223277587156,37.6424558980319));
#61452=CARTESIAN_POINT('Ctrl Pts',(5.17299698425316,0.64762706779285,37.6953761521139));
#61453=CARTESIAN_POINT('Ctrl Pts',(4.47079179693381,2.12499880919883,37.7482964061958));
#61454=CARTESIAN_POINT('Ctrl Pts',(3.76858660961448,3.60237055060479,37.8012166602778));
#61455=CARTESIAN_POINT('Ctrl Pts',(2.26166347958414,4.69725418975229,37.8541369143597));
#61456=CARTESIAN_POINT('Ctrl Pts',(0.639613445927835,4.90861425153937,37.9070571684417));
#61457=CARTESIAN_POINT('Ctrl Pts',(-0.982436587728495,5.11997431332645,
37.9599774225237));
#61458=CARTESIAN_POINT('Ctrl Pts',(-2.71961352501084,4.44781079775303,38.0128976766056));
#61459=CARTESIAN_POINT('Ctrl Pts',(-3.77695866803847,3.19971599529649,38.0658179306876));
#61460=CARTESIAN_POINT('Ctrl Pts',(-4.52195594113156,2.32031797609409,38.1031051355728));
#61461=CARTESIAN_POINT('Ctrl Pts',(-4.92945048540112,1.15499867080211,38.140392340458));
#61462=CARTESIAN_POINT('Ctrl Pts',(-4.93901314208066,-0.00426717980477184,
38.1776795453432));
#61463=CARTESIAN_POINT('Origin',(0.,0.,16.));
#61464=CARTESIAN_POINT('',(-4.95007301157197,-0.000387401246429997,39.3223204546569));
#61465=CARTESIAN_POINT('',(-4.95010830192917,0.000103228088722096,39.1776795453432));
#61466=CARTESIAN_POINT('',(-4.942,-6.05220448138622E-16,16.));
#61467=CARTESIAN_POINT('Ctrl Pts',(-4.95007301157197,-0.000387401246429997,
39.3223204546569));
#61468=CARTESIAN_POINT('Ctrl Pts',(-4.94825412650634,1.61464285750734,39.2700720155921));
#61469=CARTESIAN_POINT('Ctrl Pts',(-4.08291838964434,3.23134503628798,39.2178235765273));
#61470=CARTESIAN_POINT('Ctrl Pts',(-2.73731172677047,4.12440578092639,39.1655751374625));
#61471=CARTESIAN_POINT('Ctrl Pts',(-1.37440313527419,5.0289495790347,39.1126548833806));
#61472=CARTESIAN_POINT('Ctrl Pts',(0.481206517102607,5.19112301285789,39.0597346292986));
#61473=CARTESIAN_POINT('Ctrl Pts',(1.98036191326499,4.53671304225247,39.0068143752166));
#61474=CARTESIAN_POINT('Ctrl Pts',(3.47951730942733,3.88230307164706,38.9538941211347));
#61475=CARTESIAN_POINT('Ctrl Pts',(4.62221844937522,2.41130969661302,38.9009738670527));
#61476=CARTESIAN_POINT('Ctrl Pts',(4.88554783933805,0.796881951604831,38.8480536129708));
#61477=CARTESIAN_POINT('Ctrl Pts',(5.14887722930088,-0.817545793403355,
38.7951333588888));
#61478=CARTESIAN_POINT('Ctrl Pts',(4.53283486927871,-2.57540790838573,38.7422131048068));
#61479=CARTESIAN_POINT('Ctrl Pts',(3.31933115184711,-3.67227984222765,38.6892928507249));
#61480=CARTESIAN_POINT('Ctrl Pts',(2.10582743441549,-4.76915177606959,38.6363725966429));
#61481=CARTESIAN_POINT('Ctrl Pts',(0.294862359574459,-5.20503352877106,
38.5834523425609));
#61482=CARTESIAN_POINT('Ctrl Pts',(-1.28483879610452,-4.78045895320511,
38.530532088479));
#61483=CARTESIAN_POINT('Ctrl Pts',(-2.86453995178352,-4.35588437763916,
38.477611834397));
#61484=CARTESIAN_POINT('Ctrl Pts',(-4.21297718830044,-3.07085347380577,
38.424691580315));
#61485=CARTESIAN_POINT('Ctrl Pts',(-4.71308503194927,-1.51341600918913,
38.3717713262331));
#61486=CARTESIAN_POINT('Ctrl Pts',(-4.86885884155228,-1.02830470737132,
38.3552877023743));
#61487=CARTESIAN_POINT('Ctrl Pts',(-4.94232768041382,-0.516764503992941,
38.3388040785156));
#61488=CARTESIAN_POINT('Ctrl Pts',(-4.93830712716952,-0.00410043205665789,
38.3223204546569));
#61489=CARTESIAN_POINT('Ctrl Pts',(-4.93901314208066,-0.00426717980477184,
38.1776795453432));
#61490=CARTESIAN_POINT('Ctrl Pts',(-4.94302238554053,-0.490301467717737,
38.19331259454));
#61491=CARTESIAN_POINT('Ctrl Pts',(-4.87708344029753,-0.975271683602742,
38.2089456437367));
#61492=CARTESIAN_POINT('Ctrl Pts',(-4.7367428403112,-1.43766007643938,38.2245786929335));
#61493=CARTESIAN_POINT('Ctrl Pts',(-4.26166852078334,-3.00291525637914,
38.2774989470154));
#61494=CARTESIAN_POINT('Ctrl Pts',(-2.9340065329546,-4.30939952691902,38.3304192010974));
#61495=CARTESIAN_POINT('Ctrl Pts',(-1.36131527943717,-4.75924573231914,
38.3833394551794));
#61496=CARTESIAN_POINT('Ctrl Pts',(0.211375974080253,-5.20909193771926,
38.4362597092614));
#61497=CARTESIAN_POINT('Ctrl Pts',(2.0290964932864,-4.80230007797962,38.4891799633433));
#61498=CARTESIAN_POINT('Ctrl Pts',(3.2600296070944,-3.72502432092665,38.5421002174252));
#61499=CARTESIAN_POINT('Ctrl Pts',(4.4909627209024,-2.64774856387368,38.5950204715072));
#61500=CARTESIAN_POINT('Ctrl Pts',(5.13510842931226,-0.899988909507443,
38.6479407255892));
#61501=CARTESIAN_POINT('Ctrl Pts',(4.89769581831224,0.718453131327276,38.7008609796712));
#61502=CARTESIAN_POINT('Ctrl Pts',(4.66028320731222,2.33689517216197,38.7537812337531));
#61503=CARTESIAN_POINT('Ctrl Pts',(3.54131227690224,3.82601959946517,38.8067014878351));
#61504=CARTESIAN_POINT('Ctrl Pts',(2.05284121454405,4.50438033235388,38.859621741917));
#61505=CARTESIAN_POINT('Ctrl Pts',(0.564370152185806,5.18274106524261,38.912541995999));
#61506=CARTESIAN_POINT('Ctrl Pts',(-1.29360104212064,5.05033810371689,38.965462250081));
#61507=CARTESIAN_POINT('Ctrl Pts',(-2.67083637362622,4.16776106512145,39.0183825041629));
#61508=CARTESIAN_POINT('Ctrl Pts',(-4.04807170513178,3.28518402652602,39.0713027582449));
#61509=CARTESIAN_POINT('Ctrl Pts',(-4.94457117383642,1.65243291086087,39.1242230123269));
#61510=CARTESIAN_POINT('Ctrl Pts',(-4.95008293089447,0.0166795651704946,
39.1771432664088));
#61511=CARTESIAN_POINT('Ctrl Pts',(-4.95010154909182,0.0111541440981086,
39.1773220260536));
#61512=CARTESIAN_POINT('Ctrl Pts',(-4.95011000089745,0.00562868876953041,
39.1775007856984));
#61513=CARTESIAN_POINT('Ctrl Pts',(-4.95010830192917,0.000103228088722096,
39.1776795453432));
#61514=CARTESIAN_POINT('Origin',(0.,0.,16.));
#61515=CARTESIAN_POINT('',(-4.93943724668283,0.00434520414469897,40.3223204546569));
#61516=CARTESIAN_POINT('',(-4.9387122051873,0.0042019715207839,40.1776795453432));
#61517=CARTESIAN_POINT('',(-4.942,-6.05220448138622E-16,16.));
#61518=CARTESIAN_POINT('Ctrl Pts',(-4.93943724668283,0.00434520414469897,
40.3223204546569));
#61519=CARTESIAN_POINT('Ctrl Pts',(-4.94341650816428,0.474947915493244,
40.3071804608325));
#61520=CARTESIAN_POINT('Ctrl Pts',(-4.88164614501736,0.944527111103383,
40.2920404670082));
#61521=CARTESIAN_POINT('Ctrl Pts',(-4.74989944410437,1.39357590613184,40.2769004731838));
#61522=CARTESIAN_POINT('Ctrl Pts',(-4.28939272477215,2.96317868165193,40.2239802191018));
#61523=CARTESIAN_POINT('Ctrl Pts',(-2.97393022079225,4.28194545604953,40.1710599650198));
#61524=CARTESIAN_POINT('Ctrl Pts',(-1.40548766464857,4.74638841223249,40.1181397109379));
#61525=CARTESIAN_POINT('Ctrl Pts',(0.162954891495088,5.21083136841545,40.0652194568559));
#61526=CARTESIAN_POINT('Ctrl Pts',(1.98437749980252,4.82095050638379,40.012299202774));
#61527=CARTESIAN_POINT('Ctrl Pts',(3.22526935667327,3.75516126313619,39.959378948692));
#61528=CARTESIAN_POINT('Ctrl Pts',(4.46616121354403,2.68937201988858,39.90645869461));
#61529=CARTESIAN_POINT('Ctrl Pts',(5.1265223189781,0.947674395425016,39.8535384405281));
#61530=CARTESIAN_POINT('Ctrl Pts',(4.90416134563252,-0.672904176876648,
39.8006181864461));
#61531=CARTESIAN_POINT('Ctrl Pts',(4.68180037228695,-2.29348274917834,39.7476979323641));
#61532=CARTESIAN_POINT('Ctrl Pts',(3.57671732016171,-3.79294226931812,39.6947776782822));
#61533=CARTESIAN_POINT('Ctrl Pts',(2.09461507151,-4.4851071600863,39.6418574242002));
#61534=CARTESIAN_POINT('Ctrl Pts',(0.612512822858338,-5.17727205085446,
39.5889371701182));
#61535=CARTESIAN_POINT('Ctrl Pts',(-1.24660862231976,-5.06214231225107,
39.5360169160363));
#61536=CARTESIAN_POINT('Ctrl Pts',(-2.63198689690885,-4.19240307100288,
39.4830966619543));
#61537=CARTESIAN_POINT('Ctrl Pts',(-4.01736517149795,-3.32266382975467,
39.4301764078723));
#61538=CARTESIAN_POINT('Ctrl Pts',(-4.92900027549801,-1.69831508586162,
39.3772561537904));
#61539=CARTESIAN_POINT('Ctrl Pts',(-4.9497140621902,-0.0626836327184169,
39.3243358997084));
#61540=CARTESIAN_POINT('Ctrl Pts',(-4.94997702073422,-0.0419195265770804,
39.3236640846913));
#61541=CARTESIAN_POINT('Ctrl Pts',(-4.95009639895585,-0.0211536021213772,
39.3229922696741));
#61542=CARTESIAN_POINT('Ctrl Pts',(-4.95007301157197,-0.000387401246429997,
39.3223204546569));
#61543=CARTESIAN_POINT('Ctrl Pts',(-4.95010830192917,0.000103228088722096,
39.1776795453432));
#61544=CARTESIAN_POINT('Ctrl Pts',(-4.94960703596349,-1.6301363826534,39.2304210397804));
#61545=CARTESIAN_POINT('Ctrl Pts',(-4.06548675829959,-3.26084190194751,
39.2831625342175));
#61546=CARTESIAN_POINT('Ctrl Pts',(-2.6988623875562,-4.14966758230844,39.3359040286547));
#61547=CARTESIAN_POINT('Ctrl Pts',(-1.32760604174843,-5.04150580838138,
39.3888242827367));
#61548=CARTESIAN_POINT('Ctrl Pts',(0.529430695278565,-5.18642668481171,
39.4417445368187));
#61549=CARTESIAN_POINT('Ctrl Pts',(2.02243945069843,-4.51811220521201,39.4946647909006));
#61550=CARTESIAN_POINT('Ctrl Pts',(3.51544820611836,-3.84979772561229,39.5475850449826));
#61551=CARTESIAN_POINT('Ctrl Pts',(4.6444289799311,-2.36824788998248,39.6005052990645));
#61552=CARTESIAN_POINT('Ctrl Pts',(4.89274292745657,-0.751442530371268,
39.6534255531465));
#61553=CARTESIAN_POINT('Ctrl Pts',(5.14105687498204,0.865362829239897,39.7063458072285));
#61554=CARTESIAN_POINT('Ctrl Pts',(4.50870399622024,2.61742371283248,39.7592660613104));
#61555=CARTESIAN_POINT('Ctrl Pts',(3.2850586262277,3.70297030137619,39.8121863153924));
#61556=CARTESIAN_POINT('Ctrl Pts',(2.06141325623513,4.78851688991993,39.8651065694743));
#61557=CARTESIAN_POINT('Ctrl Pts',(0.246475395011777,5.2075491834148,39.9180268235563));
#61558=CARTESIAN_POINT('Ctrl Pts',(-1.32921167314713,4.76831160460351,39.9709470776383));
#61559=CARTESIAN_POINT('Ctrl Pts',(-2.90489874130597,4.32907402579225,40.0238673317202));
#61560=CARTESIAN_POINT('Ctrl Pts',(-4.24133501640037,3.03156657467491,40.0767875858022));
#61561=CARTESIAN_POINT('Ctrl Pts',(-4.72694684795839,1.46954847732333,40.1297078398842));
#61562=CARTESIAN_POINT('Ctrl Pts',(-4.87368101212714,0.997563642860038,
40.1456984083705));
#61563=CARTESIAN_POINT('Ctrl Pts',(-4.94273254556439,0.501428253000672,
40.1616889768569));
#61564=CARTESIAN_POINT('Ctrl Pts',(-4.9387122051873,0.0042019715207839,
40.1776795453432));
#61565=CARTESIAN_POINT('Origin',(0.,0.,16.));
#61566=CARTESIAN_POINT('',(-4.93485552516168,-0.00220275864159403,41.3223204546569));
#61567=CARTESIAN_POINT('',(-4.93524162710697,-0.00257366327817901,41.1776795453432));
#61568=CARTESIAN_POINT('',(-4.942,-6.05220448138622E-16,16.));
#61569=CARTESIAN_POINT('Ctrl Pts',(-4.93485552516168,-0.00220275864159403,
41.3223204546569));
#61570=CARTESIAN_POINT('Ctrl Pts',(-4.93097721826847,0.962135133190097,
41.291368651991));
#61571=CARTESIAN_POINT('Ctrl Pts',(-4.65830472720369,1.92849849558568,41.2604168493251));
#61572=CARTESIAN_POINT('Ctrl Pts',(-4.13125993704044,2.72695615437044,41.2294650466591));
#61573=CARTESIAN_POINT('Ctrl Pts',(-3.23013813457067,4.09212969959618,41.1765447925771));
#61574=CARTESIAN_POINT('Ctrl Pts',(-1.58541225739997,4.96646613003761,41.1236245384952));
#61575=CARTESIAN_POINT('Ctrl Pts',(0.0502660136753988,4.94985574164777,
41.0707042844132));
#61576=CARTESIAN_POINT('Ctrl Pts',(1.68594428475072,4.93324535325794,41.0177840303312));
#61577=CARTESIAN_POINT('Ctrl Pts',(3.31257494973071,4.0256881460368,40.9648637762493));
#61578=CARTESIAN_POINT('Ctrl Pts',(4.18578697328013,2.64249615885673,40.9119435221673));
#61579=CARTESIAN_POINT('Ctrl Pts',(5.05899899682956,1.25930417167664,40.8590232680854));
#61580=CARTESIAN_POINT('Ctrl Pts',(5.17879237894847,-0.599522595462416,
40.8061030140034));
#61581=CARTESIAN_POINT('Ctrl Pts',(4.49034783841098,-2.08335662461616,40.7531827599214));
#61582=CARTESIAN_POINT('Ctrl Pts',(3.8019032978735,-3.56719065376989,40.7002625058395));
#61583=CARTESIAN_POINT('Ctrl Pts',(2.30522083467963,-4.67603194493831,40.6473422517575));
#61584=CARTESIAN_POINT('Ctrl Pts',(0.685205202367444,-4.90245778828362,
40.5944219976755));
#61585=CARTESIAN_POINT('Ctrl Pts',(-0.93481042994472,-5.12888363162893,
40.5415017435936));
#61586=CARTESIAN_POINT('Ctrl Pts',(-2.6781592313752,-4.47289402715115,40.4885814895116));
#61587=CARTESIAN_POINT('Ctrl Pts',(-3.74705816474816,-3.23467983659099,
40.4356612354296));
#61588=CARTESIAN_POINT('Ctrl Pts',(-4.51015502798955,-2.35070724073872,
40.397880975172));
#61589=CARTESIAN_POINT('Ctrl Pts',(-4.92950741869571,-1.16999430476845,
40.3601007149145));
#61590=CARTESIAN_POINT('Ctrl Pts',(-4.93943724668283,0.00434520414469897,
40.3223204546569));
#61591=CARTESIAN_POINT('Ctrl Pts',(-4.9387122051873,0.0042019715207839,
40.1776795453432));
#61592=CARTESIAN_POINT('Ctrl Pts',(-4.92942736292292,-1.14412557296836,
40.2146092309388));
#61593=CARTESIAN_POINT('Ctrl Pts',(-4.53040370843391,-2.2982715368062,40.2515389165345));
#61594=CARTESIAN_POINT('Ctrl Pts',(-3.79843588104676,-3.17419030434592,
40.2884686021301));
#61595=CARTESIAN_POINT('Ctrl Pts',(-2.74952569455548,-4.42938224507769,
40.341388856212));
#61596=CARTESIAN_POINT('Ctrl Pts',(-1.01691793355136,-5.11323738295533,
40.394309110294));
#61597=CARTESIAN_POINT('Ctrl Pts',(0.606519628933596,-4.91281316257247,
40.4472293643759));
#61598=CARTESIAN_POINT('Ctrl Pts',(2.22995719141853,-4.71238894218962,40.5001496184579));
#61599=CARTESIAN_POINT('Ctrl Pts',(3.74422455538428,-3.62768536354625,40.5530698725399));
#61600=CARTESIAN_POINT('Ctrl Pts',(4.45636984813063,-2.15507935058069,40.6059901266218));
#61601=CARTESIAN_POINT('Ctrl Pts',(5.16851514087698,-0.682473337615157,
40.6589103807038));
#61602=CARTESIAN_POINT('Ctrl Pts',(5.07853836240398,1.17803510967258,40.7118306347858));
#61603=CARTESIAN_POINT('Ctrl Pts',(4.22761426072911,2.57504891081838,40.7647508888677));
#61604=CARTESIAN_POINT('Ctrl Pts',(3.37669015905424,3.97206271196421,40.8176711429497));
#61605=CARTESIAN_POINT('Ctrl Pts',(1.76481873417747,4.90558186696812,40.8705913970317));
#61606=CARTESIAN_POINT('Ctrl Pts',(0.12961696774931,4.94841375314338,40.9235116511136));
#61607=CARTESIAN_POINT('Ctrl Pts',(-1.50558479867887,4.99124563931864,40.9764319051956));
#61608=CARTESIAN_POINT('Ctrl Pts',(-3.16411690665841,4.14339025666527,41.0293521592775));
#61609=CARTESIAN_POINT('Ctrl Pts',(-4.0870097333165,2.79283917732535,41.0822724133595));
#61610=CARTESIAN_POINT('Ctrl Pts',(-4.6416213166461,1.98122676595515,41.1140747906874));
#61611=CARTESIAN_POINT('Ctrl Pts',(-4.93056429073029,0.988070940573039,
41.1458771680153));
#61612=CARTESIAN_POINT('Ctrl Pts',(-4.93524162710697,-0.00257366327817901,
41.1776795453432));
#61613=CARTESIAN_POINT('Origin',(0.,0.,16.));
#61614=CARTESIAN_POINT('',(-4.94748713622925,-0.00316321289392352,42.3223204546569));
#61615=CARTESIAN_POINT('',(-4.94809820533655,-0.00280696805152256,42.1776795453432));
#61616=CARTESIAN_POINT('',(-4.942,-6.05220448138622E-16,16.));
#61617=CARTESIAN_POINT('Ctrl Pts',(-4.94748713622925,-0.00316321289392352,
42.3223204546569));
#61618=CARTESIAN_POINT('Ctrl Pts',(-4.93670139323051,1.44433029491444,42.2755568431494));
#61619=CARTESIAN_POINT('Ctrl Pts',(-4.26377312667576,2.9005508041267,42.2287932316419));
#61620=CARTESIAN_POINT('Ctrl Pts',(-3.14834440585587,3.81988560527279,42.1820296201344));
#61621=CARTESIAN_POINT('Ctrl Pts',(-1.88606441050834,4.8602550227471,42.1291093660525));
#61622=CARTESIAN_POINT('Ctrl Pts',(-0.0570997319322858,5.21306603328002,
42.0761891119705));
#61623=CARTESIAN_POINT('Ctrl Pts',(1.50158745972911,4.71686693007535,42.0232688578886));
#61624=CARTESIAN_POINT('Ctrl Pts',(3.06027465139055,4.22066782687068,41.9703486038066));
#61625=CARTESIAN_POINT('Ctrl Pts',(4.34868435613734,2.87545860992836,41.9174283497246));
#61626=CARTESIAN_POINT('Ctrl Pts',(4.77722061558389,1.29682756189652,41.8645080956427));
#61627=CARTESIAN_POINT('Ctrl Pts',(5.20575687503042,-0.281803486135251,
41.8115878415607));
#61628=CARTESIAN_POINT('Ctrl Pts',(4.77441968917683,-2.09385636525649,41.7586675874787));
#61629=CARTESIAN_POINT('Ctrl Pts',(3.68059554195264,-3.31010800304349,41.7057473333968));
#61630=CARTESIAN_POINT('Ctrl Pts',(2.58677139472839,-4.52635964083055,41.6528270793148));
#61631=CARTESIAN_POINT('Ctrl Pts',(0.830460286133465,-5.14681003728328,
41.5999068252328));
#61632=CARTESIAN_POINT('Ctrl Pts',(-0.78462299692839,-4.88753161503282,
41.5469865711509));
#61633=CARTESIAN_POINT('Ctrl Pts',(-2.39970627999022,-4.62825319278237,
41.4940663170689));
#61634=CARTESIAN_POINT('Ctrl Pts',(-3.87356173751901,-3.48924595182876,
41.4411460629869));
#61635=CARTESIAN_POINT('Ctrl Pts',(-4.531730602399,-1.99173700134697,41.388225808905));
#61636=CARTESIAN_POINT('Ctrl Pts',(-4.80495209353668,-1.37008555249385,
41.366257357489));
#61637=CARTESIAN_POINT('Ctrl Pts',(-4.93760820478682,-0.686654334984092,
41.3442889060729));
#61638=CARTESIAN_POINT('Ctrl Pts',(-4.93485552516168,-0.00220275864159403,
41.3223204546569));
#61639=CARTESIAN_POINT('Ctrl Pts',(-4.93524162710697,-0.00257366327817901,
41.1776795453432));
#61640=CARTESIAN_POINT('Ctrl Pts',(-4.93834753998013,-0.660395889443513,
41.1987974220973));
#61641=CARTESIAN_POINT('Ctrl Pts',(-4.81610883381463,-1.31711081291602,
41.2199152988513));
#61642=CARTESIAN_POINT('Ctrl Pts',(-4.56308028711322,-1.91882712196431,
41.2410331756054));
#61643=CARTESIAN_POINT('Ctrl Pts',(-3.92900446891528,-3.42669556588764,
41.2939534296874));
#61644=CARTESIAN_POINT('Ctrl Pts',(-2.47359928718284,-4.58918567770784,
41.3468736837693));
#61645=CARTESIAN_POINT('Ctrl Pts',(-0.862880381041693,-4.87432422789462,
41.3997939378513));
#61646=CARTESIAN_POINT('Ctrl Pts',(0.74783852509941,-5.15946277808138,41.4527141919333));
#61647=CARTESIAN_POINT('Ctrl Pts',(2.51387115564923,-4.56724976663472,41.5056344460152));
#61648=CARTESIAN_POINT('Ctrl Pts',(3.62705400678358,-3.36869091228363,41.5585547000972));
#61649=CARTESIAN_POINT('Ctrl Pts',(4.74023685791794,-2.17013205793252,41.6114749541791));
#61650=CARTESIAN_POINT('Ctrl Pts',(5.20056992963686,-0.36522736067698,41.6643952082611));
#61651=CARTESIAN_POINT('Ctrl Pts',(4.79739777779339,1.22007122425299,41.7173154623431));
#61652=CARTESIAN_POINT('Ctrl Pts',(4.3942256259499,2.80536980918301,41.770235716425));
#61653=CARTESIAN_POINT('Ctrl Pts',(3.12754825054399,4.17106228178741,41.823155970507));
#61654=CARTESIAN_POINT('Ctrl Pts',(1.57701656414349,4.69218690879255,41.8760762245889));
#61655=CARTESIAN_POINT('Ctrl Pts',(0.0264848777430365,5.21331153579767,
41.9289964786709));
#61656=CARTESIAN_POINT('Ctrl Pts',(-1.80790111965202,4.88986831720356,41.9819167327529));
#61657=CARTESIAN_POINT('Ctrl Pts',(-3.08669837960869,3.86986980968975,42.0348369868349));
#61658=CARTESIAN_POINT('Ctrl Pts',(-4.2372765819408,2.95214181174547,42.0824511730043));
#61659=CARTESIAN_POINT('Ctrl Pts',(-4.93809323584742,1.47053667915491,42.1300653591738));
#61660=CARTESIAN_POINT('Ctrl Pts',(-4.94809820533655,-0.00280696805152256,
42.1776795453432));
#61661=CARTESIAN_POINT('Origin',(0.,0.,16.));
#61662=CARTESIAN_POINT('',(-4.94451025515232,0.00421302333877771,43.3223204546569));
#61663=CARTESIAN_POINT('',(-4.94371934458518,0.00435719887056521,43.1776795453432));
#61664=CARTESIAN_POINT('',(-4.942,-6.05220448138622E-16,16.));
#61665=CARTESIAN_POINT('Ctrl Pts',(-4.94451025515232,0.00421302333877771,
43.3223204546569));
#61666=CARTESIAN_POINT('Ctrl Pts',(-4.94721961825891,0.30354166338666,43.3126652883898));
#61667=CARTESIAN_POINT('Ctrl Pts',(-4.9223727794906,0.602421473877891,43.3030101221227));
#61668=CARTESIAN_POINT('Ctrl Pts',(-4.8683572221906,0.895933308008362,43.2933549558557));
#61669=CARTESIAN_POINT('Ctrl Pts',(-4.57229634269635,2.50468041899365,43.2404347017737));
#61670=CARTESIAN_POINT('Ctrl Pts',(-3.39995792978838,3.95216446044364,43.1875144476917));
#61671=CARTESIAN_POINT('Ctrl Pts',(-1.88782194598489,4.57599462800297,43.1345941936098));
#61672=CARTESIAN_POINT('Ctrl Pts',(-0.375685962181428,5.19982479556229,
43.0816739395278));
#61673=CARTESIAN_POINT('Ctrl Pts',(1.47624759251752,5.00000108923096,43.0287536854458));
#61674=CARTESIAN_POINT('Ctrl Pts',(2.82050563945827,4.06796588887349,42.9758334313639));
#61675=CARTESIAN_POINT('Ctrl Pts',(4.16476368639908,3.13593068851599,42.9229131772819));
#61676=CARTESIAN_POINT('Ctrl Pts',(5.00134622558163,1.47168399413228,42.8699929231999));
#61677=CARTESIAN_POINT('Ctrl Pts',(4.9474203102028,-0.163189489389038,42.817072669118));
#61678=CARTESIAN_POINT('Ctrl Pts',(4.89349439482397,-1.79806297291028,42.764152415036));
#61679=CARTESIAN_POINT('Ctrl Pts',(3.94906002488378,-3.40356324556919,42.7112321609541));
#61680=CARTESIAN_POINT('Ctrl Pts',(2.54630479212863,-4.24498886227479,42.6583119068721));
#61681=CARTESIAN_POINT('Ctrl Pts',(1.14354955937346,-5.0864144789804,42.6053916527901));
#61682=CARTESIAN_POINT('Ctrl Pts',(-0.717526536196703,-5.16376543973274,
42.5524713987082));
#61683=CARTESIAN_POINT('Ctrl Pts',(-2.18526664959422,-4.44164476353361,
42.4995511446262));
#61684=CARTESIAN_POINT('Ctrl Pts',(-3.65300676299177,-3.71952408733446,
42.4466308905442));
#61685=CARTESIAN_POINT('Ctrl Pts',(-4.72741089421663,-2.19793177418379,
42.3937106364623));
#61686=CARTESIAN_POINT('Ctrl Pts',(-4.91681530376954,-0.573171705400564,
42.3407903823803));
#61687=CARTESIAN_POINT('Ctrl Pts',(-4.93885025563959,-0.38415018261489,
42.3346337398059));
#61688=CARTESIAN_POINT('Ctrl Pts',(-4.94890712844976,-0.19373232997381,
42.3284770972314));
#61689=CARTESIAN_POINT('Ctrl Pts',(-4.94748713622925,-0.00316321289392352,
42.3223204546569));
#61690=CARTESIAN_POINT('Ctrl Pts',(-4.94809820533655,-0.00280696805152256,
42.1776795453432));
#61691=CARTESIAN_POINT('Ctrl Pts',(-4.94921314716046,-0.166994620502292,
42.1829856132557));
#61692=CARTESIAN_POINT('Ctrl Pts',(-4.94174917029318,-0.331079676814377,
42.1882916811682));
#61693=CARTESIAN_POINT('Ctrl Pts',(-4.92537268191333,-0.494270345953525,
42.1935977490807));
#61694=CARTESIAN_POINT('Ctrl Pts',(-4.76204120174297,-2.12185819764955,
42.2465180031627));
#61695=CARTESIAN_POINT('Ctrl Pts',(-3.71216971888389,-3.6604801046081,42.2994382572447));
#61696=CARTESIAN_POINT('Ctrl Pts',(-2.25619545826342,-4.40603918329588,
42.3523585113266));
#61697=CARTESIAN_POINT('Ctrl Pts',(-0.800221197642949,-5.15159826198366,
42.4052787654086));
#61698=CARTESIAN_POINT('Ctrl Pts',(1.06185584073894,-5.10409451240069,42.4581990194906));
#61699=CARTESIAN_POINT('Ctrl Pts',(2.4779207651768,-4.28526637586659,42.5111192735725));
#61700=CARTESIAN_POINT('Ctrl Pts',(3.89398568961467,-3.46643823933247,42.5640395276545));
#61701=CARTESIAN_POINT('Ctrl Pts',(4.8640385001085,-1.87628571584728,42.6169597817364));
#61702=CARTESIAN_POINT('Ctrl Pts',(4.9441682152519,-0.242486886078373,42.6698800358184));
#61703=CARTESIAN_POINT('Ctrl Pts',(5.02429793039529,1.39131194369048,42.7228002899004));
#61704=CARTESIAN_POINT('Ctrl Pts',(4.21450455018825,3.06875707974299,42.7757205439823));
#61705=CARTESIAN_POINT('Ctrl Pts',(2.88536189314395,4.02222400870711,42.8286407980643));
#61706=CARTESIAN_POINT('Ctrl Pts',(1.55621923609964,4.97569093767124,42.8815610521463));
#61707=CARTESIAN_POINT('Ctrl Pts',(-0.292272697781964,5.20517965954696,
42.9344813062282));
#61708=CARTESIAN_POINT('Ctrl Pts',(-1.81421576809595,4.60567263029181,42.9874015603102));
#61709=CARTESIAN_POINT('Ctrl Pts',(-3.33615883840994,4.00616560103666,43.0403218143921));
#61710=CARTESIAN_POINT('Ctrl Pts',(-4.53155304515633,2.57766282065063,43.0932420684741));
#61711=CARTESIAN_POINT('Ctrl Pts',(-4.85336774243223,0.97386897853116,43.1461623225561));
#61712=CARTESIAN_POINT('Ctrl Pts',(-4.91725446964838,0.655483458634976,
43.1566680634851));
#61713=CARTESIAN_POINT('Ctrl Pts',(-4.94671318283581,0.330189668722103,
43.1671738044142));
#61714=CARTESIAN_POINT('Ctrl Pts',(-4.94371934458518,0.00435719887056521,
43.1776795453432));
#61715=CARTESIAN_POINT('Origin',(0.,0.,16.));
#61716=CARTESIAN_POINT('',(-4.93394997286128,0.000507016503537849,44.3223204546569));
#61717=CARTESIAN_POINT('',(-4.93390371744476,7.29331094537614E-5,44.1776795453432));
#61718=CARTESIAN_POINT('',(-4.942,-6.05220448138622E-16,16.));
#61719=CARTESIAN_POINT('Ctrl Pts',(-4.93394997286128,0.000507016503537849,
44.3223204546569));
#61720=CARTESIAN_POINT('Ctrl Pts',(-4.93467682586532,0.794322762801275,
44.2968534795483));
#61721=CARTESIAN_POINT('Ctrl Pts',(-4.75416264908751,1.58782655048687,44.2713865044396));
#61722=CARTESIAN_POINT('Ctrl Pts',(-4.39062917456631,2.28603892939324,44.245919529331));
#61723=CARTESIAN_POINT('Ctrl Pts',(-3.63520833024163,3.73692095748179,44.192999275249));
#61724=CARTESIAN_POINT('Ctrl Pts',(-2.08949837449215,4.77632854708712,44.1400790211671));
#61725=CARTESIAN_POINT('Ctrl Pts',(-0.460839790231528,4.92861291064672,
44.0871587670851));
#61726=CARTESIAN_POINT('Ctrl Pts',(1.16781879402907,5.08089727420631,44.0342385130031));
#61727=CARTESIAN_POINT('Ctrl Pts',(2.8794260068008,4.3460584117202,43.9813182589212));
#61728=CARTESIAN_POINT('Ctrl Pts',(3.8907242466578,3.06036980963467,43.9283980048392));
#61729=CARTESIAN_POINT('Ctrl Pts',(4.90202248651478,1.77468120754915,43.8754777507573));
#61730=CARTESIAN_POINT('Ctrl Pts',(5.21301175345704,-0.0618571341358118,
43.8225574966753));
#61731=CARTESIAN_POINT('Ctrl Pts',(4.68137860928635,-1.60881722136807,43.7696372425933));
#61732=CARTESIAN_POINT('Ctrl Pts',(4.14974546511566,-3.15577730860032,43.7167169885114));
#61733=CARTESIAN_POINT('Ctrl Pts',(2.77548990983206,-4.41315914137991,43.6637967344294));
#61734=CARTESIAN_POINT('Ctrl Pts',(1.18749227412456,-4.80556558941283,43.6108764803475));
#61735=CARTESIAN_POINT('Ctrl Pts',(-0.400505361582988,-5.19797203744577,
43.5579562262655));
#61736=CARTESIAN_POINT('Ctrl Pts',(-2.20224507771443,-4.72540310073197,
43.5050359721835));
#61737=CARTESIAN_POINT('Ctrl Pts',(-3.3932232627399,-3.60411354211475,43.4521157181016));
#61738=CARTESIAN_POINT('Ctrl Pts',(-4.36691049562677,-2.68740042232609,
43.4088506302867));
#61739=CARTESIAN_POINT('Ctrl Pts',(-4.93236951831919,-1.33708753420181,
43.3655855424718));
#61740=CARTESIAN_POINT('Ctrl Pts',(-4.94451025515232,0.00421302333877771,
43.3223204546569));
#61741=CARTESIAN_POINT('Ctrl Pts',(-4.94371934458518,0.00435719887056521,
43.1776795453432));
#61742=CARTESIAN_POINT('Ctrl Pts',(-4.93163241109647,-1.31111647133373,
43.2200940584961));
#61743=CARTESIAN_POINT('Ctrl Pts',(-4.39058351177215,-2.63537038181765,
43.262508571649));
#61744=CARTESIAN_POINT('Ctrl Pts',(-3.45056931084653,-3.5492493095965,43.3049230848019));
#61745=CARTESIAN_POINT('Ctrl Pts',(-2.27772099417954,-4.68948885175174,
43.3578433388839));
#61746=CARTESIAN_POINT('Ctrl Pts',(-0.483789173040172,-5.19088303220938,
43.4107635929659));
#61747=CARTESIAN_POINT('Ctrl Pts',(1.11029555303778,-4.82398621634968,43.4636838470478));
#61748=CARTESIAN_POINT('Ctrl Pts',(2.70438027911579,-4.45708940048996,43.5166041011298));
#61749=CARTESIAN_POINT('Ctrl Pts',(4.09861791013234,-3.22190158831284,43.5695243552118));
#61750=CARTESIAN_POINT('Ctrl Pts',(4.65498401236277,-1.68366358732205,43.6224446092938));
#61751=CARTESIAN_POINT('Ctrl Pts',(5.21135011459319,-0.145425586331283,
43.6753648633757));
#61752=CARTESIAN_POINT('Ctrl Pts',(4.92984468803749,1.69586260347318,43.7282851174576));
#61753=CARTESIAN_POINT('Ctrl Pts',(3.93928891523517,2.99759938499667,43.7812053715396));
#61754=CARTESIAN_POINT('Ctrl Pts',(2.94873314243287,4.29933616652015,43.8341256256216));
#61755=CARTESIAN_POINT('Ctrl Pts',(1.24912702338399,5.06152153976273,43.8870458797035));
#61756=CARTESIAN_POINT('Ctrl Pts',(-0.381763724262289,4.93536783730094,
43.9399661337855));
#61757=CARTESIAN_POINT('Ctrl Pts',(-2.01265447190855,4.80921413483915,43.9928863878675));
#61758=CARTESIAN_POINT('Ctrl Pts',(-3.57482984815219,3.79472135667302,44.0458066419495));
#61759=CARTESIAN_POINT('Ctrl Pts',(-4.35341454219008,2.35613689213404,44.0987268960314));
#61760=CARTESIAN_POINT('Ctrl Pts',(-4.74060923336151,1.6407204811301,44.125044445802));
#61761=CARTESIAN_POINT('Ctrl Pts',(-4.93401170909488,0.820420654182907,
44.1513619955726));
#61762=CARTESIAN_POINT('Ctrl Pts',(-4.93390371744476,7.29331094537614E-5,
44.1776795453432));
#61763=CARTESIAN_POINT('Origin',(0.,0.,16.));
#61764=CARTESIAN_POINT('',(-4.94264971735337,-0.00447858357024544,45.3223204546569));
#61765=CARTESIAN_POINT('',(-4.94345166054126,-0.00439535110808767,45.1776795453432));
#61766=CARTESIAN_POINT('',(-4.942,-6.05220448138622E-16,16.));
#61767=CARTESIAN_POINT('Ctrl Pts',(-4.94264971735337,-0.00447858357024544,
45.3223204546569));
#61768=CARTESIAN_POINT('Ctrl Pts',(-4.93082575729553,1.27648252745284,45.2810416707067));
#61769=CARTESIAN_POINT('Ctrl Pts',(-4.42134998955586,2.56578412734584,45.2397628867565));
#61770=CARTESIAN_POINT('Ctrl Pts',(-3.52575508348954,3.47457186233093,45.1984841028063));
#61771=CARTESIAN_POINT('Ctrl Pts',(-2.37758390575486,4.63965651937944,45.1455638487244));
#61772=CARTESIAN_POINT('Ctrl Pts',(-0.594796197848898,5.17933734465609,
45.0926435946425));
#61773=CARTESIAN_POINT('Ctrl Pts',(1.00677715711088,4.84664815013159,45.0397233405605));
#61774=CARTESIAN_POINT('Ctrl Pts',(2.60835051207067,4.51395895560708,44.9868030864785));
#61775=CARTESIAN_POINT('Ctrl Pts',(4.02870951408424,3.30889974128137,44.9338828323965));
#61776=CARTESIAN_POINT('Ctrl Pts',(4.61787619111481,1.78292400813641,44.8809625783145));
#61777=CARTESIAN_POINT('Ctrl Pts',(5.20704286814536,0.25694827499149,44.8280423242326));
#61778=CARTESIAN_POINT('Ctrl Pts',(4.96501722019298,-1.58994397697268,44.7751220701506));
#61779=CARTESIAN_POINT('Ctrl Pts',(4.00255388014552,-2.91258664622809,44.7222018160687));
#61780=CARTESIAN_POINT('Ctrl Pts',(3.04009054009802,-4.23522931548356,44.6692815619867));
#61781=CARTESIAN_POINT('Ctrl Pts',(1.35718950795542,-5.03362240203022,44.6163613079047));
#61782=CARTESIAN_POINT('Ctrl Pts',(-0.276028001533181,-4.94240903584718,
44.5634410538228));
#61783=CARTESIAN_POINT('Ctrl Pts',(-1.90924551102172,-4.85119566966413,
44.5105207997408));
#61784=CARTESIAN_POINT('Ctrl Pts',(-3.49277949785625,-3.8703758507514,44.4576005456588));
#61785=CARTESIAN_POINT('Ctrl Pts',(-4.30198062482356,-2.4487877080092,44.4046802915769));
#61786=CARTESIAN_POINT('Ctrl Pts',(-4.72176742799645,-1.71131475847591,
44.3772270126036));
#61787=CARTESIAN_POINT('Ctrl Pts',(-4.93316642875337,-0.85522261151742,
44.3497737336302));
#61788=CARTESIAN_POINT('Ctrl Pts',(-4.93394997286128,0.000507016503537849,
44.3223204546569));
#61789=CARTESIAN_POINT('Ctrl Pts',(-4.93390371744476,7.29331094537614E-5,
44.1776795453432));
#61790=CARTESIAN_POINT('Ctrl Pts',(-4.93379455568915,-0.829163376745596,
44.2042822496546));
#61791=CARTESIAN_POINT('Ctrl Pts',(-4.73595877931974,-1.65844862422957,
44.2308849539659));
#61792=CARTESIAN_POINT('Ctrl Pts',(-4.34068739432695,-2.37950250585247,
44.2574876582773));
#61793=CARTESIAN_POINT('Ctrl Pts',(-3.55438154059382,-3.813881288388,44.3104079123592));
#61794=CARTESIAN_POINT('Ctrl Pts',(-1.98677582129545,-4.81996270254719,
44.3633281664412));
#61795=CARTESIAN_POINT('Ctrl Pts',(-0.355230555152893,-4.9373485276323,
44.4162484205232));
#61796=CARTESIAN_POINT('Ctrl Pts',(1.27631471098969,-5.05473435271742,44.4691686746052));
#61797=CARTESIAN_POINT('Ctrl Pts',(2.97179952397649,-4.28342458872844,44.5220889286871));
#61798=CARTESIAN_POINT('Ctrl Pts',(3.95534413875573,-2.9763823636485,44.5750091827691));
#61799=CARTESIAN_POINT('Ctrl Pts',(4.93888875353493,-1.66934013856861,44.627929436851));
#61800=CARTESIAN_POINT('Ctrl Pts',(5.21049317010665,0.173434547602146,44.680849690933));
#61801=CARTESIAN_POINT('Ctrl Pts',(4.64586705931524,1.70865985432931,44.733769945015));
#61802=CARTESIAN_POINT('Ctrl Pts',(4.08124094852381,3.24388516105654,44.7866901990969));
#61803=CARTESIAN_POINT('Ctrl Pts',(2.68038431036912,4.47156108834011,44.8396104531789));
#61804=CARTESIAN_POINT('Ctrl Pts',(1.08435053733238,4.82988438193028,44.8925307072609));
#61805=CARTESIAN_POINT('Ctrl Pts',(-0.511683235704347,5.18820767552046,
44.9454509613428));
#61806=CARTESIAN_POINT('Ctrl Pts',(-2.30289414362315,4.67717833541725,44.9983712154248));
#61807=CARTESIAN_POINT('Ctrl Pts',(-3.46959671833554,3.53065119244912,45.0512914695067));
#61808=CARTESIAN_POINT('Ctrl Pts',(-4.39839859233384,2.61791080594467,45.0934208281189));
#61809=CARTESIAN_POINT('Ctrl Pts',(-4.93141112790613,1.30241637823199,45.1355501867311));
#61810=CARTESIAN_POINT('Ctrl Pts',(-4.94345166054126,-0.00439535110808767,
45.1776795453432));
#61811=CARTESIAN_POINT('Origin',(0.,0.,16.));
#61812=CARTESIAN_POINT('',(-4.94881445934699,0.00227942523971326,46.3223204546569));
#61813=CARTESIAN_POINT('',(-4.94828946219151,0.00267981890309541,46.1776795453432));
#61814=CARTESIAN_POINT('',(-4.942,-6.05220448138622E-16,16.));
#61815=CARTESIAN_POINT('Ctrl Pts',(-4.94881445934699,0.00227942523971326,
46.3223204546569));
#61816=CARTESIAN_POINT('Ctrl Pts',(-4.94955378308614,0.131274482234953,
46.3181501159471));
#61817=CARTESIAN_POINT('Ctrl Pts',(-4.94494719039334,0.260215895992481,
46.3139797772374));
#61818=CARTESIAN_POINT('Ctrl Pts',(-4.93482452766902,0.388722801454193,
46.3098094385276));
#61819=CARTESIAN_POINT('Ctrl Pts',(-4.80637120034064,2.01943401260374,46.2568891844456));
#61820=CARTESIAN_POINT('Ctrl Pts',(-3.78967659005442,3.58017725671765,46.2039689303636));
#61821=CARTESIAN_POINT('Ctrl Pts',(-2.34999567814797,4.35673258852779,46.1510486762817));
#61822=CARTESIAN_POINT('Ctrl Pts',(-0.910314766241556,5.13328792033792,
46.0981284221997));
#61823=CARTESIAN_POINT('Ctrl Pts',(0.952352447285067,5.12565533984434,46.0452081681177));
#61824=CARTESIAN_POINT('Ctrl Pts',(2.38562099756669,4.33732763245101,45.9922879140358));
#61825=CARTESIAN_POINT('Ctrl Pts',(3.81888954784836,3.54899992505766,45.9393676599538));
#61826=CARTESIAN_POINT('Ctrl Pts',(4.82275943488501,1.97997709076453,45.8864474058719));
#61827=CARTESIAN_POINT('Ctrl Pts',(4.93784446656618,0.348267941757418,45.8335271517899));
#61828=CARTESIAN_POINT('Ctrl Pts',(5.05292949824735,-1.28344120724965,45.7806068977079));
#61829=CARTESIAN_POINT('Ctrl Pts',(4.27922967457309,-2.97783667097068,45.727686643626));
#61830=CARTESIAN_POINT('Ctrl Pts',(2.97080185134115,-3.95953720721528,45.674766389544));
#61831=CARTESIAN_POINT('Ctrl Pts',(1.66237402810921,-4.94123774345989,45.621846135462));
#61832=CARTESIAN_POINT('Ctrl Pts',(-0.18078179468041,-5.21024335222807,
45.5689258813801));
#61833=CARTESIAN_POINT('Ctrl Pts',(-1.71520936255536,-4.64345295850584,
45.5160056272981));
#61834=CARTESIAN_POINT('Ctrl Pts',(-3.24963693043034,-4.0766625647836,45.4630853732162));
#61835=CARTESIAN_POINT('Ctrl Pts',(-4.47533624339064,-2.67407616857091,
45.4101651191342));
#61836=CARTESIAN_POINT('Ctrl Pts',(-4.8314085760891,-1.07753872605438,45.3572448650522));
#61837=CARTESIAN_POINT('Ctrl Pts',(-4.90973785658425,-0.726330228027688,
45.3456033949204));
#61838=CARTESIAN_POINT('Ctrl Pts',(-4.94598431844091,-0.365736088925451,
45.3339619247887));
#61839=CARTESIAN_POINT('Ctrl Pts',(-4.94264971735337,-0.00447858357024544,
45.3223204546569));
#61840=CARTESIAN_POINT('Ctrl Pts',(-4.94345166054126,-0.00439535110808767,
45.1776795453432));
#61841=CARTESIAN_POINT('Ctrl Pts',(-4.94653568871891,-0.339118433408757,
45.188470440813));
#61842=CARTESIAN_POINT('Ctrl Pts',(-4.91544069255685,-0.673271876348126,
45.1992613362828));
#61843=CARTESIAN_POINT('Ctrl Pts',(-4.848063077171,-0.999941813506336,45.2100522317526));
#61844=CARTESIAN_POINT('Ctrl Pts',(-4.51763261978812,-2.60198273066066,
45.2629724858346));
#61845=CARTESIAN_POINT('Ctrl Pts',(-3.31457746351644,-4.02403961913634,
45.3158927399166));
#61846=CARTESIAN_POINT('Ctrl Pts',(-1.78943402176491,-4.61535752812037,
45.3688129939985));
#61847=CARTESIAN_POINT('Ctrl Pts',(-0.264290580013278,-5.20667543710444,
45.4217332480805));
#61848=CARTESIAN_POINT('Ctrl Pts',(1.58294114721826,-4.96725436659668,45.4746535021624));
#61849=CARTESIAN_POINT('Ctrl Pts',(2.90693970933454,-4.00665705506737,45.5275737562444));
#61850=CARTESIAN_POINT('Ctrl Pts',(4.23093827145077,-3.0460597435381,45.5804940103263));
#61851=CARTESIAN_POINT('Ctrl Pts',(5.0317036684518,-1.36428619098739,45.6334142644083));
#61852=CARTESIAN_POINT('Ctrl Pts',(4.94279342482124,0.2690583397166,45.6863345184903));
#61853=CARTESIAN_POINT('Ctrl Pts',(4.85388318119067,1.90240287042061,45.7392547725723));
#61854=CARTESIAN_POINT('Ctrl Pts',(3.87529729692844,3.4873183792779,45.7921750266543));
#61855=CARTESIAN_POINT('Ctrl Pts',(2.45485161832049,4.29852332349801,45.8450952807362));
#61856=CARTESIAN_POINT('Ctrl Pts',(1.03440593971258,5.1097282677181,45.8980155348182));
#61857=CARTESIAN_POINT('Ctrl Pts',(-0.827899533241065,5.1472226473011,45.9509357889001));
#61858=CARTESIAN_POINT('Ctrl Pts',(-2.27984537368615,4.39384846150945,46.0038560429821));
#61859=CARTESIAN_POINT('Ctrl Pts',(-3.73179121413126,3.64047427571779,46.056776297064));
#61860=CARTESIAN_POINT('Ctrl Pts',(-4.77337742206781,2.0962315245515,46.109696551146));
#61861=CARTESIAN_POINT('Ctrl Pts',(-4.92795824091158,0.46778927569873,46.162616805228));
#61862=CARTESIAN_POINT('Ctrl Pts',(-4.94262440066108,0.31328760891278,46.1676377185997));
#61863=CARTESIAN_POINT('Ctrl Pts',(-4.94930605767903,0.158028008604056,
46.1726586319715));
#61864=CARTESIAN_POINT('Ctrl Pts',(-4.94828946219151,0.00267981890309541,
46.1776795453432));
#61865=CARTESIAN_POINT('Origin',(0.,0.,16.));
#61866=CARTESIAN_POINT('',(-4.9358501160701,0.00303175399314515,47.3223204546569));
#61867=CARTESIAN_POINT('',(-4.93538463697233,0.00269292579073279,47.1776795453432));
#61868=CARTESIAN_POINT('',(-4.942,-6.05220448138622E-16,16.));
#61869=CARTESIAN_POINT('Ctrl Pts',(-4.9358501160701,0.00303175399314515,
47.3223204546569));
#61870=CARTESIAN_POINT('Ctrl Pts',(-4.93933793021421,0.625283723714611,
47.3023383071056));
#61871=CARTESIAN_POINT('Ctrl Pts',(-4.83028758168748,1.24635811395051,47.2823561595543));
#61872=CARTESIAN_POINT('Ctrl Pts',(-4.60310972348256,1.82070849089976,47.2623740120029));
#61873=CARTESIAN_POINT('Ctrl Pts',(-4.00145717602152,3.34180464946569,47.2094537579209));
#61874=CARTESIAN_POINT('Ctrl Pts',(-2.57127018656423,4.53518329005682,47.156533503839));
#61875=CARTESIAN_POINT('Ctrl Pts',(-0.967024164301558,4.85473612062603,
47.103613249757));
#61876=CARTESIAN_POINT('Ctrl Pts',(0.637221857961163,5.17428895119525,47.050692995675));
#61877=CARTESIAN_POINT('Ctrl Pts',(2.41552691302929,4.62001597174252,46.9977727415931));
#61878=CARTESIAN_POINT('Ctrl Pts',(3.55411144818602,3.44556096290971,46.9448524875111));
#61879=CARTESIAN_POINT('Ctrl Pts',(4.69269598334273,2.27110595407693,46.8919322334292));
#61880=CARTESIAN_POINT('Ctrl Pts',(5.19155999858808,0.476468915864107,46.8390119793472));
#61881=CARTESIAN_POINT('Ctrl Pts',(4.82241570154595,-1.11709683409153,46.7860917252652));
#61882=CARTESIAN_POINT('Ctrl Pts',(4.45327140450381,-2.71066258404717,46.7331714711833));
#61883=CARTESIAN_POINT('Ctrl Pts',(3.21611879517418,-4.10315704574563,46.6802512171013));
#61884=CARTESIAN_POINT('Ctrl Pts',(1.67709780224552,-4.65735348636513,46.6273309630194));
#61885=CARTESIAN_POINT('Ctrl Pts',(0.138076809316829,-5.21154992698464,
46.5744107089374));
#61886=CARTESIAN_POINT('Ctrl Pts',(-1.7028125672109,-4.92744834652514,46.5214904548554));
#61887=CARTESIAN_POINT('Ctrl Pts',(-3.00315123328947,-3.93505796720279,
46.4685702007734));
#61888=CARTESIAN_POINT('Ctrl Pts',(-4.2010177406636,-3.02087212574391,46.4198202854013));
#61889=CARTESIAN_POINT('Ctrl Pts',(-4.94017200312835,-1.50563121453851,
46.3710703700291));
#61890=CARTESIAN_POINT('Ctrl Pts',(-4.94881445934699,0.00227942523971326,
46.3223204546569));
#61891=CARTESIAN_POINT('Ctrl Pts',(-4.94828946219151,0.00267981890309541,
46.1776795453432));
#61892=CARTESIAN_POINT('Ctrl Pts',(-4.93859117623925,-1.47933656262951,
46.2255788860534));
#61893=CARTESIAN_POINT('Ctrl Pts',(-4.22826766932132,-2.96941554830109,
46.2734782267636));
#61894=CARTESIAN_POINT('Ctrl Pts',(-3.06585319961028,-3.88640494404102,
46.3213775674738));
#61895=CARTESIAN_POINT('Ctrl Pts',(-1.78159190971431,-4.89951516838867,
46.3742978215558));
#61896=CARTESIAN_POINT('Ctrl Pts',(0.0545060998286173,-5.21309387054478,
46.4272180756378));
#61897=CARTESIAN_POINT('Ctrl Pts',(1.60221433767964,-4.68364264720964,46.4801383297198));
#61898=CARTESIAN_POINT('Ctrl Pts',(3.14992257553069,-4.15419142387448,46.5330585838017));
#61899=CARTESIAN_POINT('Ctrl Pts',(4.40924104168984,-2.78171027504809,46.5859788378836));
#61900=CARTESIAN_POINT('Ctrl Pts',(4.80388637285101,-1.19426753592463,46.6388990919656));
#61901=CARTESIAN_POINT('Ctrl Pts',(5.19853170401218,0.393175203198827,46.6918193460476));
#61902=CARTESIAN_POINT('Ctrl Pts',(4.72850390017529,2.19557953261941,46.7447396001296));
#61903=CARTESIAN_POINT('Ctrl Pts',(3.60889486296925,3.38813770361555,46.7976598542115));
#61904=CARTESIAN_POINT('Ctrl Pts',(2.48928582576321,4.58069587461169,46.8505801082935));
#61905=CARTESIAN_POINT('Ctrl Pts',(0.720095555188062,5.16340788718348,46.9035003623755));
#61906=CARTESIAN_POINT('Ctrl Pts',(-0.889067460630859,4.86961582479301,
46.9564206164574));
#61907=CARTESIAN_POINT('Ctrl Pts',(-2.49823047644978,4.57582376240254,47.0093408705394));
#61908=CARTESIAN_POINT('Ctrl Pts',(-3.9473662375124,3.40552762504981,47.0622611246213));
#61909=CARTESIAN_POINT('Ctrl Pts',(-4.57332808734244,1.89427279876787,47.1151813787033));
#61910=CARTESIAN_POINT('Ctrl Pts',(-4.81974582587867,1.29934836887573,47.1360141009166));
#61911=CARTESIAN_POINT('Ctrl Pts',(-4.93859613551441,0.651585501425685,
47.1568468231299));
#61912=CARTESIAN_POINT('Ctrl Pts',(-4.93538463697233,0.00269292579073279,
47.1776795453432));
#61913=CARTESIAN_POINT('Origin',(0.,0.,16.));
#61914=CARTESIAN_POINT('',(-4.93779824682792,-0.00394849367342132,48.3223204546569));
#61915=CARTESIAN_POINT('',(-4.93847649956811,-0.00414486738929824,48.1776795453433));
#61916=CARTESIAN_POINT('',(-4.942,-6.05220448138622E-16,16.));
#61917=CARTESIAN_POINT('Ctrl Pts',(-4.93779824682792,-0.00394849367342132,
48.3223204546569));
#61918=CARTESIAN_POINT('Ctrl Pts',(-4.92945107906705,1.10958389040538,48.286526498264));
#61919=CARTESIAN_POINT('Ctrl Pts',(-4.55663414200584,2.22817899674935,48.2507325418711));
#61920=CARTESIAN_POINT('Ctrl Pts',(-3.86551329136296,3.09215224876629,48.2149385854782));
#61921=CARTESIAN_POINT('Ctrl Pts',(-2.8437125545035,4.36950989861378,48.1620183313963));
#61922=CARTESIAN_POINT('Ctrl Pts',(-1.12614067807074,5.09029714456033,48.1090980773143));
#61923=CARTESIAN_POINT('Ctrl Pts',(0.50121521532169,4.92467073449426,48.0561778232323));
#61924=CARTESIAN_POINT('Ctrl Pts',(2.12857110871417,4.75904432442819,48.0032575691504));
#61925=CARTESIAN_POINT('Ctrl Pts',(3.66571101906626,3.70700425834946,47.9503373150684));
#61926=CARTESIAN_POINT('Ctrl Pts',(4.40921624712591,2.2499801379868,47.8974170609865));
#61927=CARTESIAN_POINT('Ctrl Pts',(5.15272147518552,0.792956017624232,47.8444968069045));
#61928=CARTESIAN_POINT('Ctrl Pts',(5.10259202095273,-1.06905215702231,47.7915765528226));
#61929=CARTESIAN_POINT('Ctrl Pts',(4.28176788829653,-2.4839610073443,47.7386562987406));
#61930=CARTESIAN_POINT('Ctrl Pts',(3.46094375564028,-3.89886985766637,47.6857360446586));
#61931=CARTESIAN_POINT('Ctrl Pts',(1.86942494456057,-4.86667938366393,47.6328157905766));
#61932=CARTESIAN_POINT('Ctrl Pts',(0.235514769794999,-4.94450516517706,
47.5798955364947));
#61933=CARTESIAN_POINT('Ctrl Pts',(-1.39839540497048,-5.02233094669018,
47.5269752824127));
#61934=CARTESIAN_POINT('Ctrl Pts',(-3.07469694342178,-4.21017298371899,
47.4740550283308));
#61935=CARTESIAN_POINT('Ctrl Pts',(-4.02628865991507,-2.87968716396305,
47.4211347742488));
#61936=CARTESIAN_POINT('Ctrl Pts',(-4.61856906134665,-2.05157920362054,
47.3881966677182));
#61937=CARTESIAN_POINT('Ctrl Pts',(-4.93010088448512,-1.0226738972605,47.3552585611876));
#61938=CARTESIAN_POINT('Ctrl Pts',(-4.9358501160701,0.00303175399314515,
47.3223204546569));
#61939=CARTESIAN_POINT('Ctrl Pts',(-4.93538463697233,0.00269292579073279,
47.1776795453432));
#61940=CARTESIAN_POINT('Ctrl Pts',(-4.93043813690577,-0.996761729574154,
47.2097670772119));
#61941=CARTESIAN_POINT('Ctrl Pts',(-4.63591709407219,-1.99889645937005,
47.2418546090805));
#61942=CARTESIAN_POINT('Ctrl Pts',(-4.07193915439288,-2.81476655400573,
47.2739421409492));
#61943=CARTESIAN_POINT('Ctrl Pts',(-3.1418004330159,-4.16033756528617,47.3268623950311));
#61944=CARTESIAN_POINT('Ctrl Pts',(-1.47873505166457,-4.99926607263594,
47.3797826491131));
#61945=CARTESIAN_POINT('Ctrl Pts',(0.156212871657996,-4.94764557838933,
47.4327029031951));
#61946=CARTESIAN_POINT('Ctrl Pts',(1.79116079498061,-4.89602508414272,47.4856231572771));
#61947=CARTESIAN_POINT('Ctrl Pts',(3.39799126027446,-3.95385558829969,47.538543411359));
#61948=CARTESIAN_POINT('Ctrl Pts',(4.24139410598325,-2.552288241629,47.591463665441));
#61949=CARTESIAN_POINT('Ctrl Pts',(5.08479695169201,-1.15072089495835,47.6443839195229));
#61950=CARTESIAN_POINT('Ctrl Pts',(5.16477217781576,0.710244302539926,47.6973041736049));
#61951=CARTESIAN_POINT('Ctrl Pts',(4.44472189944271,2.17900125452958,47.7502244276869));
#61952=CARTESIAN_POINT('Ctrl Pts',(3.72467162106964,3.64775820651928,47.8031446817689));
#61953=CARTESIAN_POINT('Ctrl Pts',(2.20459583819974,4.72430691300034,47.8560649358508));
#61954=CARTESIAN_POINT('Ctrl Pts',(0.580104444733958,4.91600224408279,47.9089851899327));
#61955=CARTESIAN_POINT('Ctrl Pts',(-1.04438694873177,5.10769757516524,47.9619054440147));
#61956=CARTESIAN_POINT('Ctrl Pts',(-2.77329395279337,4.41453953084916,48.0148256980967));
#61957=CARTESIAN_POINT('Ctrl Pts',(-3.81544231731622,3.15372781860764,48.0677459521787));
#61958=CARTESIAN_POINT('Ctrl Pts',(-4.53707600502276,2.28068110435693,48.1043904832335));
#61959=CARTESIAN_POINT('Ctrl Pts',(-4.92941962837742,1.13545330336185,48.1410350142884));
#61960=CARTESIAN_POINT('Ctrl Pts',(-4.93847649956811,-0.00414486738929824,
48.1776795453433));
#61961=CARTESIAN_POINT('Origin',(0.,0.,16.));
#61962=CARTESIAN_POINT('',(-4.94996872029631,-0.000754789231165454,49.3223204546569));
#61963=CARTESIAN_POINT('',(-4.95009281286112,-0.000267728824007536,49.1776795453432));
#61964=CARTESIAN_POINT('',(-4.942,-6.05220448138622E-16,16.));
#61965=CARTESIAN_POINT('Ctrl Pts',(-4.94996872029631,-0.000754789231165454,
49.3223204546569));
#61966=CARTESIAN_POINT('Ctrl Pts',(-4.94657205241788,1.59450047399929,49.2707146894224));
#61967=CARTESIAN_POINT('Ctrl Pts',(-4.10534559557285,3.19283284813315,49.219108924188));
#61968=CARTESIAN_POINT('Ctrl Pts',(-2.78707318578254,4.09094385103807,49.1675031589536));
#61969=CARTESIAN_POINT('Ctrl Pts',(-1.4352220784804,5.01193130760659,49.1145829048716));
#61970=CARTESIAN_POINT('Ctrl Pts',(0.418286878732396,5.19657136329379,49.0616626507896));
#61971=CARTESIAN_POINT('Ctrl Pts',(1.92525967895112,4.56036990866522,49.0087423967077));
#61972=CARTESIAN_POINT('Ctrl Pts',(3.4322324791698,3.92416845403667,48.9558221426257));
#61973=CARTESIAN_POINT('Ctrl Pts',(4.59266912239443,2.4671254890924,48.9029018885438));
#61974=CARTESIAN_POINT('Ctrl Pts',(4.87553607768602,0.856006127569342,48.8499816344618));
#61975=CARTESIAN_POINT('Ctrl Pts',(5.15840303297761,-0.755113233953766,
48.7970613803799));
#61976=CARTESIAN_POINT('Ctrl Pts',(4.56370030033613,-2.52030899205568,48.7441411262979));
#61977=CARTESIAN_POINT('Ctrl Pts',(3.36357293293406,-3.63180060852569,48.6912208722159));
#61978=CARTESIAN_POINT('Ctrl Pts',(2.16344556553202,-4.74329222499568,48.6383006181339));
#61979=CARTESIAN_POINT('Ctrl Pts',(0.357893563369426,-5.20107969983381,
48.585380364052));
#61980=CARTESIAN_POINT('Ctrl Pts',(-1.22683490171212,-4.79567249290391,
48.53246010997));
#61981=CARTESIAN_POINT('Ctrl Pts',(-2.81156336679367,-4.39026528597401,
48.4795398558881));
#61982=CARTESIAN_POINT('Ctrl Pts',(-4.17546829479417,-3.12166339727609,
48.4266196018061));
#61983=CARTESIAN_POINT('Ctrl Pts',(-4.69440596015137,-1.57039842605291,
48.3736993477241));
#61984=CARTESIAN_POINT('Ctrl Pts',(-4.86234697051046,-1.0683708724689,48.356573050035));
#61985=CARTESIAN_POINT('Ctrl Pts',(-4.94179210764521,-0.536739194059861,
48.339446752346));
#61986=CARTESIAN_POINT('Ctrl Pts',(-4.93779824682792,-0.00394849367342132,
48.3223204546569));
#61987=CARTESIAN_POINT('Ctrl Pts',(-4.93847649956811,-0.00414486738929824,
48.1776795453433));
#61988=CARTESIAN_POINT('Ctrl Pts',(-4.942499122392,-0.510299091646249,48.1939552683704));
#61989=CARTESIAN_POINT('Ctrl Pts',(-4.87091055869885,-1.01534275567644,
48.2102309913974));
#61990=CARTESIAN_POINT('Ctrl Pts',(-4.7189797263556,-1.49493463832769,48.2265067144245));
#61991=CARTESIAN_POINT('Ctrl Pts',(-4.224979045888,-3.05432000285457,48.2794269685065));
#61992=CARTESIAN_POINT('Ctrl Pts',(-2.88158795996869,-4.34462535174135,
48.3323472225885));
#61993=CARTESIAN_POINT('Ctrl Pts',(-1.30356274672183,-4.77538725089245,
48.3852674766704));
#61994=CARTESIAN_POINT('Ctrl Pts',(0.274462466525034,-5.20614915004355,
48.4381877307524));
#61995=CARTESIAN_POINT('Ctrl Pts',(2.08712180709941,-4.77736759945896,48.4911079848343));
#61996=CARTESIAN_POINT('Ctrl Pts',(3.30491467655429,-3.68525958533767,48.5440282389163));
#61997=CARTESIAN_POINT('Ctrl Pts',(4.5227075460092,-2.59315157121635,48.5969484929983));
#61998=CARTESIAN_POINT('Ctrl Pts',(5.14563394434455,-0.837717093558183,
48.6498687470803));
#61999=CARTESIAN_POINT('Ctrl Pts',(4.88863323791471,0.7777302204381,48.7027890011622));
#62000=CARTESIAN_POINT('Ctrl Pts',(4.63163253148487,2.39317753443434,48.7557092552442));
#62001=CARTESIAN_POINT('Ctrl Pts',(3.49470472029,3.86863768476876,48.8086295093261));
#62002=CARTESIAN_POINT('Ctrl Pts',(1.99812533468889,4.52891757238984,48.8615497634081));
#62003=CARTESIAN_POINT('Ctrl Pts',(0.501545949087793,5.18919746001092,48.91447001749));
#62004=CARTESIAN_POINT('Ctrl Pts',(-1.35468501091949,5.03429708491863,48.967390271572));
#62005=CARTESIAN_POINT('Ctrl Pts',(-2.7211279083772,4.13510122450199,49.020310525654));
#62006=CARTESIAN_POINT('Ctrl Pts',(-4.07559217393182,3.24378797391906,49.0727668655504));
#62007=CARTESIAN_POINT('Ctrl Pts',(-4.94881798417885,1.62117145762289,49.1252232054468));
#62008=CARTESIAN_POINT('Ctrl Pts',(-4.95009281286112,-0.000267728824007536,
49.1776795453432));
#62009=CARTESIAN_POINT('Origin',(0.,0.,16.));
#62010=CARTESIAN_POINT('',(-4.94000433004934,0.00442567287284368,50.3223204546569));
#62011=CARTESIAN_POINT('',(-4.93925722597112,0.00431400617654748,50.1776795453432));
#62012=CARTESIAN_POINT('',(-4.942,-6.05220448138622E-16,16.));
#62013=CARTESIAN_POINT('Ctrl Pts',(-4.94000433004934,0.00442567287284368,
50.3223204546569));
#62014=CARTESIAN_POINT('Ctrl Pts',(-4.94391985550658,0.454920647205931,
50.3078231346629));
#62015=CARTESIAN_POINT('Ctrl Pts',(-4.88736862134446,0.904450331901516,
50.2933258146688));
#62016=CARTESIAN_POINT('Ctrl Pts',(-4.76643244788693,1.33593422554585,50.2788284946748));
#62017=CARTESIAN_POINT('Ctrl Pts',(-4.3249734037525,2.91100032695947,50.2259082405929));
#62018=CARTESIAN_POINT('Ctrl Pts',(-3.02558272518919,4.24560561283798,50.1729879865109));
#62019=CARTESIAN_POINT('Ctrl Pts',(-1.46288143191014,4.72901432133872,50.120067732429));
#62020=CARTESIAN_POINT('Ctrl Pts',(0.0998198613689605,5.21242302983948,
50.067147478347));
#62021=CARTESIAN_POINT('Ctrl Pts',(1.92583176936386,4.84463516096244,50.014227224265));
#62022=CARTESIAN_POINT('Ctrl Pts',(3.17954335484605,3.79395606061911,49.961306970183));
#62023=CARTESIAN_POINT('Ctrl Pts',(4.43325494032821,2.74327696027582,49.9083867161011));
#62024=CARTESIAN_POINT('Ctrl Pts',(5.11466620329769,1.00970662846638,49.8554664620191));
#62025=CARTESIAN_POINT('Ctrl Pts',(4.91195294283073,-0.613446674675755,
49.8025462079371));
#62026=CARTESIAN_POINT('Ctrl Pts',(4.70923968236377,-2.23659997781789,49.7496259538552));
#62027=CARTESIAN_POINT('Ctrl Pts',(3.62240189846027,-3.74933625229266,49.6967056997732));
#62028=CARTESIAN_POINT('Ctrl Pts',(2.14879315998069,-4.45940427533482,49.6437854456913));
#62029=CARTESIAN_POINT('Ctrl Pts',(0.675184421501018,-5.16947229837701,
49.5908651916093));
#62030=CARTESIAN_POINT('Ctrl Pts',(-1.18519527155483,-5.0768720699865,49.5379449375273));
#62031=CARTESIAN_POINT('Ctrl Pts',(-2.58100775862557,-4.22397886893019,
49.4850246834454));
#62032=CARTESIAN_POINT('Ctrl Pts',(-3.97682024569624,-3.37108566787394,
49.4321044293634));
#62033=CARTESIAN_POINT('Ctrl Pts',(-4.9080655267819,-1.75789949415196,49.3791841752814));
#62034=CARTESIAN_POINT('Ctrl Pts',(-4.94859153862899,-0.12263897856609,
49.3262639211994));
#62035=CARTESIAN_POINT('Ctrl Pts',(-4.94959816627151,-0.0820206605359307,
49.3249494323519));
#62036=CARTESIAN_POINT('Ctrl Pts',(-4.9500552393514,-0.0413887231133244,
49.3236349435044));
#62037=CARTESIAN_POINT('Ctrl Pts',(-4.94996872029631,-0.000754789231165454,
49.3223204546569));
#62038=CARTESIAN_POINT('Ctrl Pts',(-4.95009281286112,-0.000267728824007536,
49.1776795453432));
#62039=CARTESIAN_POINT('Ctrl Pts',(-4.95010408721063,-0.0146074376385199,
49.1781434595288));
#62040=CARTESIAN_POINT('Ctrl Pts',(-4.95004716359657,-0.02894705437045,
49.1786073737143));
#62041=CARTESIAN_POINT('Ctrl Pts',(-4.94992177176232,-0.0432860723615371,
49.1790712878999));
#62042=CARTESIAN_POINT('Ctrl Pts',(-4.93561790278161,-1.6789861630675,49.2319915419818));
#62043=CARTESIAN_POINT('Ctrl Pts',(-4.03035532991194,-3.30689499873837,
49.2849117960638));
#62044=CARTESIAN_POINT('Ctrl Pts',(-2.6483960323012,-4.18205663360964,49.3378320501458));
#62045=CARTESIAN_POINT('Ctrl Pts',(-1.26643673469055,-5.05721826848085,
49.3907523042277));
#62046=CARTESIAN_POINT('Ctrl Pts',(0.592219287661027,-5.17963270255261,
49.4436725583097));
#62047=CARTESIAN_POINT('Ctrl Pts',(2.07702265223193,-4.49328122119488,49.4965928123917));
#62048=CARTESIAN_POINT('Ctrl Pts',(3.56182601680279,-3.80692973983718,49.5495130664736));
#62049=CARTESIAN_POINT('Ctrl Pts',(4.67277672359291,-2.31181234304998,49.6024333205556));
#62050=CARTESIAN_POINT('Ctrl Pts',(4.90148676195955,-0.692117586080884,
49.6553535746375));
#62051=CARTESIAN_POINT('Ctrl Pts',(5.13019680032621,0.927577170888348,49.7082738287195));
#62052=CARTESIAN_POINT('Ctrl Pts',(4.47666617026921,2.67184928803957,49.7611940828015));
#62053=CARTESIAN_POINT('Ctrl Pts',(3.23996046927922,3.7424932048215,49.8141143368834));
#62054=CARTESIAN_POINT('Ctrl Pts',(2.00325476828929,4.81313712160337,49.8670345909654));
#62055=CARTESIAN_POINT('Ctrl Pts',(0.183373996366374,5.21015283801606,49.9199548450474));
#62056=CARTESIAN_POINT('Ctrl Pts',(-1.38687661076657,4.75185989872763,49.9728750991293));
#62057=CARTESIAN_POINT('Ctrl Pts',(-2.95712721789961,4.29356695943917,50.0257953532113));
#62058=CARTESIAN_POINT('Ctrl Pts',(-4.27774766024261,2.97996536444961,50.0787156072932));
#62059=CARTESIAN_POINT('Ctrl Pts',(-4.74440185394119,1.41217926586765,50.1316358613752));
#62060=CARTESIAN_POINT('Ctrl Pts',(-4.87974057311241,0.957491050521679,
50.1469837560312));
#62061=CARTESIAN_POINT('Ctrl Pts',(-4.94325117479429,0.481423074070403,
50.1623316506872));
#62062=CARTESIAN_POINT('Ctrl Pts',(-4.93925722597112,0.00431400617654748,
50.1776795453432));
#62063=CARTESIAN_POINT('Origin',(0.,0.,16.));
#62064=CARTESIAN_POINT('',(-4.9346053643787,-0.00190906406864477,51.3223204546569));
#62065=CARTESIAN_POINT('',(-4.93494424898874,-0.00229539766483815,51.1776795453432));
#62066=CARTESIAN_POINT('',(-4.942,-6.05220448138622E-16,16.));
#62067=CARTESIAN_POINT('Ctrl Pts',(-4.9346053643787,-0.00190906406864477,
51.3223204546569));
#62068=CARTESIAN_POINT('Ctrl Pts',(-4.93132359046474,0.942525285964724,
51.2920113258213));
#62069=CARTESIAN_POINT('Ctrl Pts',(-4.67058264693544,1.88863740917005,51.2617021969857));
#62070=CARTESIAN_POINT('Ctrl Pts',(-4.16399066183724,2.67671072463696,51.2313930681501));
#62071=CARTESIAN_POINT('Ctrl Pts',(-3.27947244580022,4.05270012756452,51.1784728140682));
#62072=CARTESIAN_POINT('Ctrl Pts',(-1.64545880455478,4.94689631680689,51.1255525599862));
#62073=CARTESIAN_POINT('Ctrl Pts',(-0.00969933613304136,4.95010145937766,
51.0726323059043));
#62074=CARTESIAN_POINT('Ctrl Pts',(1.62606013228874,4.95330660194842,51.0197120518223));
#62075=CARTESIAN_POINT('Ctrl Pts',(3.26356542788682,4.06552069784751,50.9667917977403));
#62076=CARTESIAN_POINT('Ctrl Pts',(4.15346911827026,2.69300813567829,50.9138715436584));
#62077=CARTESIAN_POINT('Ctrl Pts',(5.04337280865373,1.32049557350902,50.8609512895764));
#62078=CARTESIAN_POINT('Ctrl Pts',(5.18567489382252,-0.536743646728604,
50.8080310354945));
#62079=CARTESIAN_POINT('Ctrl Pts',(4.5152557662665,-2.0288084927985,50.7551107814125));
#62080=CARTESIAN_POINT('Ctrl Pts',(3.8448366387105,-3.52087333886836,50.7021905273305));
#62081=CARTESIAN_POINT('Ctrl Pts',(2.36169629842972,-4.64776381077051,50.6492702732485));
#62082=CARTESIAN_POINT('Ctrl Pts',(0.74454241669244,-4.89379761790371,50.5963500191666));
#62083=CARTESIAN_POINT('Ctrl Pts',(-0.872611465044887,-5.13983142503691,
50.5434297650846));
#62084=CARTESIAN_POINT('Ctrl Pts',(-2.62377888823873,-4.50500856740112,
50.4905095110027));
#62085=CARTESIAN_POINT('Ctrl Pts',(-3.70759889498285,-3.27983368010881,
50.4375892569207));
#62086=CARTESIAN_POINT('Ctrl Pts',(-4.49451017129344,-2.39029120233235,
50.3991663228328));
#62087=CARTESIAN_POINT('Ctrl Pts',(-4.92962682740573,-1.18954250282331,
50.3607433887448));
#62088=CARTESIAN_POINT('Ctrl Pts',(-4.94000433004934,0.00442567287284368,
50.3223204546569));
#62089=CARTESIAN_POINT('Ctrl Pts',(-4.93925722597112,0.00431400617654748,
50.1776795453432));
#62090=CARTESIAN_POINT('Ctrl Pts',(-4.92947985362941,-1.16367116612706,
50.2152519047692));
#62091=CARTESIAN_POINT('Ctrl Pts',(-4.51515233090316,-2.33789552818176,
50.2528242641951));
#62092=CARTESIAN_POINT('Ctrl Pts',(-3.75970560074729,-3.21997096669155,
50.2903966236211));
#62093=CARTESIAN_POINT('Ctrl Pts',(-2.69566720880064,-4.46236449849485,
50.3433168777031));
#62094=CARTESIAN_POINT('Ctrl Pts',(-0.95490247985317,-5.12518095992721,
50.396237131785));
#62095=CARTESIAN_POINT('Ctrl Pts',(0.665988059953313,-4.90510541524102,
50.449157385867));
#62096=CARTESIAN_POINT('Ctrl Pts',(2.28687859975984,-4.68502987055481,50.5020776399489));
#62097=CARTESIAN_POINT('Ctrl Pts',(3.78789495042532,-3.58206231974999,50.5549978940309));
#62098=CARTESIAN_POINT('Ctrl Pts',(4.48214910531455,-2.10093755936608,50.6079181481129));
#62099=CARTESIAN_POINT('Ctrl Pts',(5.17640326020376,-0.619812798982218,
50.6608384021949));
#62100=CARTESIAN_POINT('Ctrl Pts',(5.06389521931669,1.2394691709808,50.7137586562768));
#62101=CARTESIAN_POINT('Ctrl Pts',(4.19611038046471,2.62607252481409,50.7666789103588));
#62102=CARTESIAN_POINT('Ctrl Pts',(3.32832554161272,4.01267587864738,50.8195991644407));
#62103=CARTESIAN_POINT('Ctrl Pts',(1.70526390479588,4.92660061635104,50.8725194185227));
#62104=CARTESIAN_POINT('Ctrl Pts',(0.0696632635531223,4.94962081985461,
50.9254396726047));
#62105=CARTESIAN_POINT('Ctrl Pts',(-1.56593737768968,4.97264102335818,50.9783599266866));
#62106=CARTESIAN_POINT('Ctrl Pts',(-3.21407702335836,4.1047566926616,51.0312801807686));
#62107=CARTESIAN_POINT('Ctrl Pts',(-4.12054180005445,2.74312495242765,51.0842004348505));
#62108=CARTESIAN_POINT('Ctrl Pts',(-4.65427267801061,1.94138954819395,51.1153601383481));
#62109=CARTESIAN_POINT('Ctrl Pts',(-4.93087142137606,0.968476272531438,
51.1465198418457));
#62110=CARTESIAN_POINT('Ctrl Pts',(-4.93494424898874,-0.00229539766483815,
51.1776795453432));
#62111=CARTESIAN_POINT('Origin',(0.,0.,16.));
#62112=CARTESIAN_POINT('',(-4.94698954266231,-0.00340802453188072,52.3223204546568));
#62113=CARTESIAN_POINT('',(-4.94764183754834,-0.00307943510729547,52.1776795453432));
#62114=CARTESIAN_POINT('',(-4.942,-6.05220448138622E-16,16.));
#62115=CARTESIAN_POINT('Ctrl Pts',(-4.94698954266231,-0.00340802453188072,
52.3223204546568));
#62116=CARTESIAN_POINT('Ctrl Pts',(-4.93574079437759,1.42456851634609,52.2761995169797));
#62117=CARTESIAN_POINT('Ctrl Pts',(-4.28342182577614,2.86150661417242,52.2300785793026));
#62118=CARTESIAN_POINT('Ctrl Pts',(-3.19438680274345,3.78146684366169,52.1839576416255));
#62119=CARTESIAN_POINT('Ctrl Pts',(-1.94480227507184,4.83705095668842,52.1310373875436));
#62120=CARTESIAN_POINT('Ctrl Pts',(-0.120245685876333,5.21199182863453,
52.0781171334615));
#62121=CARTESIAN_POINT('Ctrl Pts',(1.44433800372382,4.73471079013843,52.0251968793796));
#62122=CARTESIAN_POINT('Ctrl Pts',(3.00892169332389,4.25742975164236,51.9722766252976));
#62123=CARTESIAN_POINT('Ctrl Pts',(4.31353248332859,2.92792680270421,51.9193563712157));
#62124=CARTESIAN_POINT('Ctrl Pts',(4.7611605513041,1.3546027978562,51.8664361171337));
#62125=CARTESIAN_POINT('Ctrl Pts',(5.20878861927959,-0.218721206991761,
51.8135158630518));
#62126=CARTESIAN_POINT('Ctrl Pts',(4.79943396522586,-2.03586626774964,51.7605956089698));
#62127=CARTESIAN_POINT('Ctrl Pts',(3.72042353078829,-3.26527905190521,51.7076753548878));
#62128=CARTESIAN_POINT('Ctrl Pts',(2.64141309635066,-4.49469183606084,51.6547551008059));
#62129=CARTESIAN_POINT('Ctrl Pts',(0.892746881529132,-5.1363723436142,51.6018348467239));
#62130=CARTESIAN_POINT('Ctrl Pts',(-0.725358746921474,-4.8966777741157,
51.5489145926419));
#62131=CARTESIAN_POINT('Ctrl Pts',(-2.34346437537199,-4.65698320461722,
51.49599433856));
#62132=CARTESIAN_POINT('Ctrl Pts',(-3.83100941745154,-3.535913558067,51.443074084478));
#62133=CARTESIAN_POINT('Ctrl Pts',(-4.50727054307715,-2.04648742648548,
51.3901538303961));
#62134=CARTESIAN_POINT('Ctrl Pts',(-4.79621520662888,-1.41010346743882,
51.3675427051497));
#62135=CARTESIAN_POINT('Ctrl Pts',(-4.93705362349566,-0.70647314083382,
51.3449315799033));
#62136=CARTESIAN_POINT('Ctrl Pts',(-4.9346053643787,-0.00190906406864477,
51.3223204546569));
#62137=CARTESIAN_POINT('Ctrl Pts',(-4.93494424898874,-0.00229539766483815,
51.1776795453432));
#62138=CARTESIAN_POINT('Ctrl Pts',(-4.9377885305877,-0.680239141156077,
51.1994400959276));
#62139=CARTESIAN_POINT('Ctrl Pts',(-4.80772180958983,-1.35713842276963,
51.221200646512));
#62140=CARTESIAN_POINT('Ctrl Pts',(-4.53950114466406,-1.9739626613036,51.2429611970964));
#62141=CARTESIAN_POINT('Ctrl Pts',(-3.88720580485411,-3.47403938502989,
51.2958814511784));
#62142=CARTESIAN_POINT('Ctrl Pts',(-2.41782521751062,-4.61881368271118,
51.3488017052603));
#62143=CARTESIAN_POINT('Ctrl Pts',(-0.803770380809228,-4.88441935193539,
51.4017219593423));
#62144=CARTESIAN_POINT('Ctrl Pts',(0.810284455892164,-5.1500250211596,51.4546422134243));
#62145=CARTESIAN_POINT('Ctrl Pts',(2.56901354195146,-4.53646206192671,51.5075624675063));
#62146=CARTESIAN_POINT('Ctrl Pts',(3.6675955870482,-3.32450625514402,51.5604827215882));
#62147=CARTESIAN_POINT('Ctrl Pts',(4.7661776321449,-2.11255044836137,51.6134029756702));
#62148=CARTESIAN_POINT('Ctrl Pts',(5.20461263627908,-0.302201794028944,
51.6663232297521));
#62149=CARTESIAN_POINT('Ctrl Pts',(4.78226604547315,1.27809651472091,51.7192434838341));
#62150=CARTESIAN_POINT('Ctrl Pts',(4.3599194546672,2.85839482347081,51.7721637379161));
#62151=CARTESIAN_POINT('Ctrl Pts',(3.07679126892111,4.20864278663813,51.825083991998));
#62152=CARTESIAN_POINT('Ctrl Pts',(1.52006054286266,4.71094631434696,51.87800424608));
#62153=CARTESIAN_POINT('Ctrl Pts',(-0.0366701831957017,5.21324984205576,
51.930924500162));
#62154=CARTESIAN_POINT('Ctrl Pts',(-1.86700344956638,4.86760893430616,51.9838447542439));
#62155=CARTESIAN_POINT('Ctrl Pts',(-3.13335079942941,3.83219414935389,52.0367650083259));
#62156=CARTESIAN_POINT('Ctrl Pts',(-4.25734861844162,2.9131698704424,52.083736520665));
#62157=CARTESIAN_POINT('Ctrl Pts',(-4.93702884968978,1.45073013335928,52.1307080330041));
#62158=CARTESIAN_POINT('Ctrl Pts',(-4.94764183754834,-0.00307943510729547,
52.1776795453432));
#62159=CARTESIAN_POINT('Origin',(0.,0.,16.));
#62160=CARTESIAN_POINT('',(-4.94509673752737,0.0040742516207555,53.3223204546569));
#62161=CARTESIAN_POINT('',(-4.94431829400652,0.00425244366110885,53.1776795453432));
#62162=CARTESIAN_POINT('',(-4.942,-6.05220448138622E-16,16.));
#62163=CARTESIAN_POINT('Ctrl Pts',(-4.94509673752737,0.0040742516207555,
53.3223204546569));
#62164=CARTESIAN_POINT('Ctrl Pts',(-4.94757864022345,0.283393084706415,
53.3133079622201));
#62165=CARTESIAN_POINT('Ctrl Pts',(-4.92595073565188,0.562327591030859,
53.3042954697834));
#62166=CARTESIAN_POINT('Ctrl Pts',(-4.87885318126865,0.836893165749963,
53.2952829773467));
#62167=CARTESIAN_POINT('Ctrl Pts',(-4.60230209819144,2.44910866310731,53.2423627232647));
#62168=CARTESIAN_POINT('Ctrl Pts',(-3.44758426677398,3.91068799192893,53.1894424691828));
#62169=CARTESIAN_POINT('Ctrl Pts',(-1.94311620233063,4.55279012908506,53.1365222151008));
#62170=CARTESIAN_POINT('Ctrl Pts',(-0.438648137887247,5.19489226624121,
53.0836019610189));
#62171=CARTESIAN_POINT('Ctrl Pts',(1.4155701595821,5.01751721173186,53.0306817069369));
#62172=CARTESIAN_POINT('Ctrl Pts',(2.77102007823768,4.10183449949628,52.9777614528549));
#62173=CARTESIAN_POINT('Ctrl Pts',(4.12646999689325,3.1861517872607,52.924841198773));
#62174=CARTESIAN_POINT('Ctrl Pts',(4.98315153673507,1.53216141729899,52.871920944691));
#62175=CARTESIAN_POINT('Ctrl Pts',(4.9490341412924,-0.10324535619766,52.8190006906091));
#62176=CARTESIAN_POINT('Ctrl Pts',(4.91491674584974,-1.73865212969422,52.7660804365271));
#62177=CARTESIAN_POINT('Ctrl Pts',(3.99000041512261,-3.35547530672568,52.7131601824451));
#62178=CARTESIAN_POINT('Ctrl Pts',(2.59754098802034,-4.21383190822896,52.6602399283632));
#62179=CARTESIAN_POINT('Ctrl Pts',(1.205081560918,-5.07218850973229,52.6073196742812));
#62180=CARTESIAN_POINT('Ctrl Pts',(-0.654920962559591,-5.17207853570735,
52.5543994201993));
#62181=CARTESIAN_POINT('Ctrl Pts',(-2.13130102041059,-4.4677907846777,52.5014791661173));
#62182=CARTESIAN_POINT('Ctrl Pts',(-3.6076810782616,-3.76350303364805,52.4485589120353));
#62183=CARTESIAN_POINT('Ctrl Pts',(-4.70043867048604,-2.25503750561363,
52.3956386579533));
#62184=CARTESIAN_POINT('Ctrl Pts',(-4.90951123352436,-0.632691064542821,
52.3427184038713));
#62185=CARTESIAN_POINT('Ctrl Pts',(-4.93637335904372,-0.424248248792036,
52.3359190874665));
#62186=CARTESIAN_POINT('Ctrl Pts',(-4.94864787405361,-0.213925520686765,
52.3291197710617));
#62187=CARTESIAN_POINT('Ctrl Pts',(-4.94698954266231,-0.00340802453188072,
52.3223204546568));
#62188=CARTESIAN_POINT('Ctrl Pts',(-4.94764183754834,-0.00307943510729547,
52.1776795453432));
#62189=CARTESIAN_POINT('Ctrl Pts',(-4.94898592720496,-0.187198217650565,
52.1836282870861));
#62190=CARTESIAN_POINT('Ctrl Pts',(-4.93959875206843,-0.371178579690442,
52.1895770288289));
#62191=CARTESIAN_POINT('Ctrl Pts',(-4.91902378063747,-0.553899157022463,
52.1955257705718));
#62192=CARTESIAN_POINT('Ctrl Pts',(-4.73598797862701,-2.17938901629118,
52.2484460246538));
#62193=CARTESIAN_POINT('Ctrl Pts',(-3.66755494125079,-3.70518007267354,
52.3013662787357));
#62194=CARTESIAN_POINT('Ctrl Pts',(-2.2026559442682,-4.43304703582165,52.3542865328177));
#62195=CARTESIAN_POINT('Ctrl Pts',(-0.737756947285612,-5.16091399896976,
52.4072067868996));
#62196=CARTESIAN_POINT('Ctrl Pts',(1.12360800930335,-5.09085686888362,52.4601270409816));
#62197=CARTESIAN_POINT('Ctrl Pts',(2.52964989329714,-4.2549348582521,52.5130472950635));
#62198=CARTESIAN_POINT('Ctrl Pts',(3.93569177729098,-3.41901284762056,52.5659675491455));
#62199=CARTESIAN_POINT('Ctrl Pts',(4.88641058868961,-1.81722595644361,52.6188878032275));
#62200=CARTESIAN_POINT('Ctrl Pts',(4.94674287935491,-0.182576329732651,
52.6718080573094));
#62201=CARTESIAN_POINT('Ctrl Pts',(5.0070751700202,1.45207329697826,52.7247283113914));
#62202=CARTESIAN_POINT('Ctrl Pts',(4.17702093995222,3.11958565922317,52.7776485654734));
#62203=CARTESIAN_POINT('Ctrl Pts',(2.83642568199835,4.05688163262466,52.8305688195553));
#62204=CARTESIAN_POINT('Ctrl Pts',(1.49583042404448,4.99417760602615,52.8834890736373));
#62205=CARTESIAN_POINT('Ctrl Pts',(-0.355305861795278,5.20125719058422,
52.9364093277193));
#62206=CARTESIAN_POINT('Ctrl Pts',(-1.86987493927361,4.58335760574097,52.9893295818012));
#62207=CARTESIAN_POINT('Ctrl Pts',(-3.384444016752,3.9654580208977,53.0422498358832));
#62208=CARTESIAN_POINT('Ctrl Pts',(-4.56244588586893,2.52257926665306,53.0951700899651));
#62209=CARTESIAN_POINT('Ctrl Pts',(-4.86480890004871,0.915004697602124,
53.1480903440471));
#62210=CARTESIAN_POINT('Ctrl Pts',(-4.92116211960056,0.615391324314909,
53.1579534111458));
#62211=CARTESIAN_POINT('Ctrl Pts',(-4.94709912492537,0.310057072885753,
53.1678164782445));
#62212=CARTESIAN_POINT('Ctrl Pts',(-4.94431829400652,0.00425244366110885,
53.1776795453432));
#62213=CARTESIAN_POINT('Origin',(0.,0.,16.));
#62214=CARTESIAN_POINT('',(-4.93403082595878,0.000832190755156725,54.3223204546569));
#62215=CARTESIAN_POINT('',(-4.93393232083006,0.000401187422265207,54.1776795453432));
#62216=CARTESIAN_POINT('',(-4.942,-6.05220448138622E-16,16.));
#62217=CARTESIAN_POINT('Ctrl Pts',(-4.93403082595878,0.000832190755156725,
54.3223204546569));
#62218=CARTESIAN_POINT('Ctrl Pts',(-4.93519480376781,0.77458390453562,54.2974961533786));
#62219=CARTESIAN_POINT('Ctrl Pts',(-4.76408859627892,1.54784860488958,54.2726718521003));
#62220=CARTESIAN_POINT('Ctrl Pts',(-4.41799967623941,2.23268389970517,54.2478475508221));
#62221=CARTESIAN_POINT('Ctrl Pts',(-3.6802099846732,3.69261050145239,54.1949272967401));
#62222=CARTESIAN_POINT('Ctrl Pts',(-2.14720464186602,4.75066627671043,54.1420070426582));
#62223=CARTESIAN_POINT('Ctrl Pts',(-0.52051030581542,4.92266874335397,54.0890867885762));
#62224=CARTESIAN_POINT('Ctrl Pts',(1.10618403023518,5.0946712099975,54.0361665344942));
#62225=CARTESIAN_POINT('Ctrl Pts',(2.82656735952921,4.38062036802653,53.9832462804122));
#62226=CARTESIAN_POINT('Ctrl Pts',(3.85336599568517,3.10727678821045,53.9303260263302));
#62227=CARTESIAN_POINT('Ctrl Pts',(4.8801646318411,1.83393320839441,53.8774057722483));
#62228=CARTESIAN_POINT('Ctrl Pts',(5.21337857485901,0.00129689073330608,
53.8244855181664));
#62229=CARTESIAN_POINT('Ctrl Pts',(4.70052403533771,-1.55198979650856,53.7715652640844));
#62230=CARTESIAN_POINT('Ctrl Pts',(4.18766949581641,-3.10527648375042,53.7186450100024));
#62231=CARTESIAN_POINT('Ctrl Pts',(2.82874647375599,-4.37921354057296,53.6657247559204));
#62232=CARTESIAN_POINT('Ctrl Pts',(1.24561889847324,-4.79082791331733,53.6128045018385));
#62233=CARTESIAN_POINT('Ctrl Pts',(-0.337508676809509,-5.2024422860617,
53.5598842477565));
#62234=CARTESIAN_POINT('Ctrl Pts',(-2.14484080531469,-4.75173397472772,
53.5069639936746));
#62235=CARTESIAN_POINT('Ctrl Pts',(-3.34931470219873,-3.64495398611418,
53.4540437395926));
#62236=CARTESIAN_POINT('Ctrl Pts',(-4.34866275314335,-2.72666225118592,
53.4101359779474));
#62237=CARTESIAN_POINT('Ctrl Pts',(-4.93300521093011,-1.35673296483636,
53.3662282163021));
#62238=CARTESIAN_POINT('Ctrl Pts',(-4.94509673752737,0.0040742516207555,
53.3223204546569));
#62239=CARTESIAN_POINT('Ctrl Pts',(-4.94431829400652,0.00425244366110885,
53.1776795453432));
#62240=CARTESIAN_POINT('Ctrl Pts',(-4.93217858577541,-1.33073665953657,
53.2207367323265));
#62241=CARTESIAN_POINT('Ctrl Pts',(-4.37274694612505,-2.67469001651735,
53.2637939193098));
#62242=CARTESIAN_POINT('Ctrl Pts',(-3.4073211579765,-3.59078845896452,53.306851106293));
#62243=CARTESIAN_POINT('Ctrl Pts',(-2.22074624248181,-4.71673666262315,
53.359771360375));
#62244=CARTESIAN_POINT('Ctrl Pts',(-0.42087225224974,-5.19636268608309,
53.4126916144569));
#62245=CARTESIAN_POINT('Ctrl Pts',(1.16865098585596,-4.81018233582522,53.4656118685389));
#62246=CARTESIAN_POINT('Ctrl Pts',(2.75817422396157,-4.42400198556738,53.5185321226208));
#62247=CARTESIAN_POINT('Ctrl Pts',(4.13734670994089,-3.17201526159183,53.5714523767028));
#62248=CARTESIAN_POINT('Ctrl Pts',(4.6750380505237,-1.62715041000601,53.6243726307848));
#62249=CARTESIAN_POINT('Ctrl Pts',(5.2127293911065,-0.0822855584201898,
53.6772928848668));
#62250=CARTESIAN_POINT('Ctrl Pts',(4.90893958629287,1.75545742077581,53.7302131389487));
#62251=CARTESIAN_POINT('Ctrl Pts',(3.9026874904557,3.045099273007,53.7831333930307));
#62252=CARTESIAN_POINT('Ctrl Pts',(2.89643539461849,4.33474112523822,53.8360536471126));
#62253=CARTESIAN_POINT('Ctrl Pts',(1.18772100775765,5.0762818505045,53.8889739011946));
#62254=CARTESIAN_POINT('Ctrl Pts',(-0.441521870018959,4.93038108759577,
53.9418941552766));
#62255=CARTESIAN_POINT('Ctrl Pts',(-2.07076474779552,4.78448032468705,53.9948144093585));
#62256=CARTESIAN_POINT('Ctrl Pts',(-3.62053611648792,3.75113807360336,54.0477346634405));
#62257=CARTESIAN_POINT('Ctrl Pts',(-4.38163692859106,2.30322753036564,54.1006549175225));
#62258=CARTESIAN_POINT('Ctrl Pts',(-4.75089382782116,1.60075691273335,54.1263297934627));
#62259=CARTESIAN_POINT('Ctrl Pts',(-4.9345120375631,0.800704467282281,54.152004669403));
#62260=CARTESIAN_POINT('Ctrl Pts',(-4.93393232083006,0.000401187422265207,
54.1776795453432));
#62261=CARTESIAN_POINT('Origin',(0.,0.,16.));
#62262=CARTESIAN_POINT('',(-4.94204396072975,-0.00451108372972908,55.3223204546568));
#62263=CARTESIAN_POINT('',(-4.94284599866247,-0.00446247280752122,55.1776795453432));
#62264=CARTESIAN_POINT('',(-4.942,-6.05220448138622E-16,16.));
#62265=CARTESIAN_POINT('Ctrl Pts',(-4.94204396072975,-0.00451108372972908,
55.3223204546568));
#62266=CARTESIAN_POINT('Ctrl Pts',(-4.93045565886636,1.25690241555476,55.281684344537));
#62267=CARTESIAN_POINT('Ctrl Pts',(-4.43833582829864,2.52635331123123,55.2410482344173));
#62268=CARTESIAN_POINT('Ctrl Pts',(-3.56758671933519,3.43160655309978,55.2004121242975));
#62269=CARTESIAN_POINT('Ctrl Pts',(-2.43361341450575,4.61051446104039,55.1474918702155));
#62270=CARTESIAN_POINT('Ctrl Pts',(-0.65749411504605,5.17175205664432,55.0945716161334));
#62271=CARTESIAN_POINT('Ctrl Pts',(0.947991861475882,4.85848844455039,55.0416513620514));
#62272=CARTESIAN_POINT('Ctrl Pts',(2.55347783799768,4.54522483245649,54.9887311079695));
#62273=CARTESIAN_POINT('Ctrl Pts',(3.98833049158174,3.35746001266491,54.9358108538876));
#62274=CARTESIAN_POINT('Ctrl Pts',(4.59593933387555,1.83873330708663,54.8828905998056));
#62275=CARTESIAN_POINT('Ctrl Pts',(5.2035481761694,0.320006601508274,54.8299703457237));
#62276=CARTESIAN_POINT('Ctrl Pts',(4.98391320717291,-1.52968198985681,54.7770500916417));
#62277=CARTESIAN_POINT('Ctrl Pts',(4.0375427431176,-2.86388671786309,54.7241298375597));
#62278=CARTESIAN_POINT('Ctrl Pts',(3.09117227906232,-4.19809144586933,54.6712095834777));
#62279=CARTESIAN_POINT('Ctrl Pts',(1.41806631994828,-5.0168123105168,54.6182893293958));
#62280=CARTESIAN_POINT('Ctrl Pts',(-0.216136294490469,-4.94539014006561,
54.5653690753138));
#62281=CARTESIAN_POINT('Ctrl Pts',(-1.85033890892918,-4.87396796961441,
54.5124488212319));
#62282=CARTESIAN_POINT('Ctrl Pts',(-3.4456381786926,-3.91240276406461,54.4595285671499));
#62283=CARTESIAN_POINT('Ctrl Pts',(-4.27200079341172,-2.50072144717157,
54.4066083130679));
#62284=CARTESIAN_POINT('Ctrl Pts',(-4.7107259171786,-1.75124409976784,54.3785123602642));
#62285=CARTESIAN_POINT('Ctrl Pts',(-4.93271344484821,-0.874894033659396,
54.3504164074605));
#62286=CARTESIAN_POINT('Ctrl Pts',(-4.93403082595878,0.000832190755156725,
54.3223204546569));
#62287=CARTESIAN_POINT('Ctrl Pts',(-4.93393232083006,0.000401187422265207,
54.1776795453432));
#62288=CARTESIAN_POINT('Ctrl Pts',(-4.93331714350093,-0.848855710199169,
54.2049249234849));
#62289=CARTESIAN_POINT('Ctrl Pts',(-4.72528049547278,-1.69839506725433,
54.2321703016266));
#62290=CARTESIAN_POINT('Ctrl Pts',(-4.31154403127411,-2.43191021565593,
54.2594156797684));
#62291=CARTESIAN_POINT('Ctrl Pts',(-3.50792006634005,-3.85665858304818,
54.3123359338503));
#62292=CARTESIAN_POINT('Ctrl Pts',(-1.92824188095795,-4.8436764824408,54.3652561879323));
#62293=CARTESIAN_POINT('Ctrl Pts',(-0.295394338707872,-4.9412894486446,
54.4181764420142));
#62294=CARTESIAN_POINT('Ctrl Pts',(1.33745320354216,-5.0389024148484,54.4710966960962));
#62295=CARTESIAN_POINT('Ctrl Pts',(3.02347010266025,-4.24711044786332,54.5240169501782));
#62296=CARTESIAN_POINT('Ctrl Pts',(3.99110927558139,-2.92824964458212,54.5769372042601));
#62297=CARTESIAN_POINT('Ctrl Pts',(4.95874844850256,-1.60938884130088,54.6298574583421));
#62298=CARTESIAN_POINT('Ctrl Pts',(5.20800989522687,0.236540798276539,54.6827777124241));
#62299=CARTESIAN_POINT('Ctrl Pts',(4.62482777083827,1.76481367875202,54.735697966506));
#62300=CARTESIAN_POINT('Ctrl Pts',(4.04164564644968,3.29308655922746,54.788618220588));
#62301=CARTESIAN_POINT('Ctrl Pts',(2.62601995094824,4.50370268060093,54.8415384746699));
#62302=CARTESIAN_POINT('Ctrl Pts',(1.02576262302031,4.84266561635652,54.8944587287519));
#62303=CARTESIAN_POINT('Ctrl Pts',(-0.574494704907621,5.1816285521121,54.9473789828339));
#62304=CARTESIAN_POINT('Ctrl Pts',(-2.35938366526199,4.64893830224978,55.0002992369159));
#62305=CARTESIAN_POINT('Ctrl Pts',(-3.51211180971311,3.48836206072432,55.0532194909978));
#62306=CARTESIAN_POINT('Ctrl Pts',(-4.4157898059278,2.57853157081683,55.0947061757796));
#62307=CARTESIAN_POINT('Ctrl Pts',(-4.93095870305679,1.2828191742603,55.1361928605614));
#62308=CARTESIAN_POINT('Ctrl Pts',(-4.94284599866247,-0.00446247280752122,
55.1776795453432));
#62309=CARTESIAN_POINT('Origin',(0.,0.,16.));
#62310=CARTESIAN_POINT('',(-4.94916162572937,0.00195780085970945,56.3223204546569));
#62311=CARTESIAN_POINT('',(-4.9486927940556,0.00238008058365034,56.1776795453432));
#62312=CARTESIAN_POINT('',(-4.942,-6.05220448138622E-16,16.));
#62313=CARTESIAN_POINT('Ctrl Pts',(-4.94916162572937,0.00195780085970945,
56.3223204546569));
#62314=CARTESIAN_POINT('Ctrl Pts',(-4.94971144692239,0.111053665337975,
56.3187927897774));
#62315=CARTESIAN_POINT('Ctrl Pts',(-4.94641661384693,0.220115719674017,
56.315265124898));
#62316=CARTESIAN_POINT('Ctrl Pts',(-4.93917135292333,0.328914702796541,
56.3117374600186));
#62317=CARTESIAN_POINT('Ctrl Pts',(-4.83048159296228,1.96106232098248,56.2588172059367));
#62318=CARTESIAN_POINT('Ctrl Pts',(-3.83276814539685,3.53400710106189,56.2058969518547));
#62319=CARTESIAN_POINT('Ctrl Pts',(-2.40259992160997,4.32794548855851,56.1529766977728));
#62320=CARTESIAN_POINT('Ctrl Pts',(-0.972431697823093,5.12188387605513,
56.1000564436908));
#62321=CARTESIAN_POINT('Ctrl Pts',(0.890191302185183,5.13681587096895,56.0471361896088));
#62322=CARTESIAN_POINT('Ctrl Pts',(2.33290434633096,4.36590836437554,55.9942159355269));
#62323=CARTESIAN_POINT('Ctrl Pts',(3.77561739047674,3.59500085778213,55.9412956814449));
#62324=CARTESIAN_POINT('Ctrl Pts',(4.79842047875997,2.03825384968152,55.8883754273629));
#62325=CARTESIAN_POINT('Ctrl Pts',(4.93326329701873,0.408058546708748,55.8354551732809));
#62326=CARTESIAN_POINT('Ctrl Pts',(5.0681061152775,-1.22213675626403,55.782534919199));
#62327=CARTESIAN_POINT('Ctrl Pts',(4.31498866351168,-2.92578035410902,55.729614665117));
#62328=CARTESIAN_POINT('Ctrl Pts',(3.01854898978546,-3.92325891721657,55.6766944110351));
#62329=CARTESIAN_POINT('Ctrl Pts',(1.72210931605921,-4.92073748032415,55.6237741569531));
#62330=CARTESIAN_POINT('Ctrl Pts',(-0.117652579627481,-5.21205100869435,
55.5708539028712));
#62331=CARTESIAN_POINT('Ctrl Pts',(-1.65883355567899,-4.66388998260118,
55.5179336487892));
#62332=CARTESIAN_POINT('Ctrl Pts',(-3.20001453173045,-4.11572895650802,
55.4650133947072));
#62333=CARTESIAN_POINT('Ctrl Pts',(-4.4426145881467,-2.72809337595155,55.4120931406252));
#62334=CARTESIAN_POINT('Ctrl Pts',(-4.81800096125524,-1.13598647553473,
55.3591728865432));
#62335=CARTESIAN_POINT('Ctrl Pts',(-4.90513773579808,-0.766417759225417,
55.3468887425811));
#62336=CARTESIAN_POINT('Ctrl Pts',(-4.94554706100059,-0.385831662281748,
55.334604598619));
#62337=CARTESIAN_POINT('Ctrl Pts',(-4.94204396072975,-0.00451108372972908,
55.3223204546568));
#62338=CARTESIAN_POINT('Ctrl Pts',(-4.94284599866247,-0.00446247280752122,
55.1776795453432));
#62339=CARTESIAN_POINT('Ctrl Pts',(-4.94612209119225,-0.359232298306442,
55.1891131146434));
#62340=CARTESIAN_POINT('Ctrl Pts',(-4.91117232521921,-0.713361781229651,
55.2005466839435));
#62341=CARTESIAN_POINT('Ctrl Pts',(-4.83559423534505,-1.05859700628939,
55.2119802532437));
#62342=CARTESIAN_POINT('Ctrl Pts',(-4.48578118797803,-2.6565175985889,55.2649005073256));
#62343=CARTESIAN_POINT('Ctrl Pts',(-3.26558776469621,-4.06389654999934,
55.3178207614076));
#62344=CARTESIAN_POINT('Ctrl Pts',(-1.73339311164005,-4.63669575788038,
55.3707410154896));
#62345=CARTESIAN_POINT('Ctrl Pts',(-0.201198458583838,-5.20949496576144,
55.4236612695715));
#62346=CARTESIAN_POINT('Ctrl Pts',(1.64299742424673,-4.94771443011306,55.4765815236535));
#62347=CARTESIAN_POINT('Ctrl Pts',(2.95526233502001,-3.97114892214321,55.5295017777355));
#62348=CARTESIAN_POINT('Ctrl Pts',(4.26752724579325,-2.9945834141734,55.5824220318174));
#62349=CARTESIAN_POINT('Ctrl Pts',(5.04786118450924,-1.30323293388218,55.6353422858994));
#62350=CARTESIAN_POINT('Ctrl Pts',(4.93917142300628,0.328914707462642,55.6882625399813));
#62351=CARTESIAN_POINT('Ctrl Pts',(4.83048166150332,1.96106234880747,55.7411827940633));
#62352=CARTESIAN_POINT('Ctrl Pts',(3.83276819978142,3.5340071512059,55.7941030481453));
#62353=CARTESIAN_POINT('Ctrl Pts',(2.40259995570176,4.32794554996814,55.8470233022272));
#62354=CARTESIAN_POINT('Ctrl Pts',(0.972431711622098,5.12188394873038,55.8999435563092));
#62355=CARTESIAN_POINT('Ctrl Pts',(-0.890191314815322,5.13681594385641,
55.9528638103912));
#62356=CARTESIAN_POINT('Ctrl Pts',(-2.33290437943218,4.36590842632473,56.0057840644731));
#62357=CARTESIAN_POINT('Ctrl Pts',(-3.77561744404904,3.59500090879304,56.0587043185551));
#62358=CARTESIAN_POINT('Ctrl Pts',(-4.79842054684533,2.03825387860361,56.1116245726371));
#62359=CARTESIAN_POINT('Ctrl Pts',(-4.93326336701772,0.408058552499706,
56.164544826719));
#62360=CARTESIAN_POINT('Ctrl Pts',(-4.94441928789138,0.273187967299986,
56.1689230662604));
#62361=CARTESIAN_POINT('Ctrl Pts',(-4.94949737612309,0.137814649647994,
56.1733013058018));
#62362=CARTESIAN_POINT('Ctrl Pts',(-4.9486927940556,0.00238008058365034,
56.1776795453432));
#62363=CARTESIAN_POINT('Origin',(0.,0.,16.));
#62364=CARTESIAN_POINT('',(-4.93623902664834,0.00326946414225537,57.3223204546569));
#62365=CARTESIAN_POINT('',(-4.93573111423024,0.00295138605979709,57.1776795453432));
#62366=CARTESIAN_POINT('',(-4.942,-6.05220448138622E-16,16.));
#62367=CARTESIAN_POINT('Ctrl Pts',(-4.93623902664834,0.00326946414225537,
57.3223204546569));
#62368=CARTESIAN_POINT('Ctrl Pts',(-4.93989713650663,0.605389273547052,
57.3029809809359));
#62369=CARTESIAN_POINT('Ctrl Pts',(-4.83794904041642,1.20631307007342,57.2836415072149));
#62370=CARTESIAN_POINT('Ctrl Pts',(-4.62482770521538,1.76481365371148,57.2643020334939));
#62371=CARTESIAN_POINT('Ctrl Pts',(-4.04164558910142,3.29308651250188,57.211381779412));
#62372=CARTESIAN_POINT('Ctrl Pts',(-2.6260199136863,4.50370261669748,57.15846152533));
#62373=CARTESIAN_POINT('Ctrl Pts',(-1.02576260846464,4.84266554764316,57.1055412712481));
#62374=CARTESIAN_POINT('Ctrl Pts',(0.574494696756969,5.18162847858883,57.0526210171661));
#62375=CARTESIAN_POINT('Ctrl Pts',(2.35938363178511,4.64893823628462,56.9997007630841));
#62376=CARTESIAN_POINT('Ctrl Pts',(3.51211175987971,3.48836201122659,56.9467805090022));
#62377=CARTESIAN_POINT('Ctrl Pts',(4.66483988797431,2.32778578616857,56.8938602549202));
#62378=CARTESIAN_POINT('Ctrl Pts',(5.18540720913538,0.539323578356728,56.8409400008383));
#62379=CARTESIAN_POINT('Ctrl Pts',(4.83559416673167,-1.05859699126952,56.7880197467563));
#62380=CARTESIAN_POINT('Ctrl Pts',(4.48578112432795,-2.65651756089581,56.7350994926743));
#62381=CARTESIAN_POINT('Ctrl Pts',(3.26558771835941,-4.0638964923365,56.6821792385924));
#62382=CARTESIAN_POINT('Ctrl Pts',(1.73339308704371,-4.63669569208971,56.6292589845104));
#62383=CARTESIAN_POINT('Ctrl Pts',(0.201198455728012,-5.20949489184292,
56.5763387304284));
#62384=CARTESIAN_POINT('Ctrl Pts',(-1.64299740093485,-4.94771435990864,
56.5234184763465));
#62385=CARTESIAN_POINT('Ctrl Pts',(-2.95526229308795,-3.97114886579523,
56.4704982222645));
#62386=CARTESIAN_POINT('Ctrl Pts',(-4.18005158912286,-3.0596812412178,56.4211056330619));
#62387=CARTESIAN_POINT('Ctrl Pts',(-4.94146330594845,-1.52554761761349,
56.3717130438594));
#62388=CARTESIAN_POINT('Ctrl Pts',(-4.94916162572937,0.00195780085970945,
56.3223204546569));
#62389=CARTESIAN_POINT('Ctrl Pts',(-4.9486927940556,0.00238008058365034,
56.1776795453432));
#62390=CARTESIAN_POINT('Ctrl Pts',(-4.93977230579782,-1.49919761032442,
56.2262215598838));
#62391=CARTESIAN_POINT('Ctrl Pts',(-4.20773066973569,-3.00830456759471,
56.2747635744243));
#62392=CARTESIAN_POINT('Ctrl Pts',(-3.018549032617,-3.92325897288391,56.3233055889649));
#62393=CARTESIAN_POINT('Ctrl Pts',(-1.72210934049551,-4.92073755014514,
56.3762258430469));
#62394=CARTESIAN_POINT('Ctrl Pts',(0.117652581295909,-5.2120510826492,56.4291460971289));
#62395=CARTESIAN_POINT('Ctrl Pts',(1.65883357921563,-4.66389004877836,56.4820663512108));
#62396=CARTESIAN_POINT('Ctrl Pts',(3.2000145771353,-4.11572901490753,56.5349866052928));
#62397=CARTESIAN_POINT('Ctrl Pts',(4.44261465118334,-2.72809341466183,56.5879068593747));
#62398=CARTESIAN_POINT('Ctrl Pts',(4.8180010296186,-1.13598649165438,56.6408271134567));
#62399=CARTESIAN_POINT('Ctrl Pts',(5.19338740805387,0.456120431353115,56.6937473675386));
#62400=CARTESIAN_POINT('Ctrl Pts',(4.70156009087639,2.25269867712231,56.7466676216206));
#62401=CARTESIAN_POINT('Ctrl Pts',(3.56758676995704,3.43160660179086,56.7995878757026));
#62402=CARTESIAN_POINT('Ctrl Pts',(2.43361344903769,4.61051452645941,56.8525081297845));
#62403=CARTESIAN_POINT('Ctrl Pts',(0.65749412437644,5.17175213002719,56.9054283838665));
#62404=CARTESIAN_POINT('Ctrl Pts',(-0.94799187492607,4.85848851348866,56.9583486379485));
#62405=CARTESIAN_POINT('Ctrl Pts',(-2.55347787422853,4.54522489695015,57.0112688920304));
#62406=CARTESIAN_POINT('Ctrl Pts',(-3.98833054817231,3.35746006030537,57.0641891461124));
#62407=CARTESIAN_POINT('Ctrl Pts',(-4.59593939908791,1.83873333317766,57.1171094001944));
#62408=CARTESIAN_POINT('Ctrl Pts',(-4.82775332951413,1.25931120769625,57.1372994485773));
#62409=CARTESIAN_POINT('Ctrl Pts',(-4.93915674573565,0.631715508347176,
57.1574894969603));
#62410=CARTESIAN_POINT('Ctrl Pts',(-4.93573111423024,0.00295138605979709,
57.1776795453432));
#62411=CARTESIAN_POINT('Origin',(0.,0.,16.));
#62412=CARTESIAN_POINT('',(-4.9373129524182,-0.00377529733612325,58.3223204546568));
#62413=CARTESIAN_POINT('',(-4.93796046055574,-0.00400002009900308,58.1776795453432));
#62414=CARTESIAN_POINT('',(-4.942,-6.05220448138622E-16,16.));
#62415=CARTESIAN_POINT('Ctrl Pts',(-4.9373129524182,-0.00377529733612325,
58.3223204546568));
#62416=CARTESIAN_POINT('Ctrl Pts',(-4.92952693668152,1.09003472006405,58.2871691720943));
#62417=CARTESIAN_POINT('Ctrl Pts',(-4.57107143779465,2.18847891881712,58.2520178895318));
#62418=CARTESIAN_POINT('Ctrl Pts',(-3.90268743507911,3.04509922980021,58.2168666069693));
#62419=CARTESIAN_POINT('Ctrl Pts',(-2.89643535351957,4.33474106373227,58.1639463528874));
#62420=CARTESIAN_POINT('Ctrl Pts',(-1.18772099090388,5.07628177847635,58.1110260988054));
#62421=CARTESIAN_POINT('Ctrl Pts',(0.441521863755048,4.93038101763753,58.0581058447234));
#62422=CARTESIAN_POINT('Ctrl Pts',(2.07076471841393,4.78448025679871,58.0051855906414));
#62423=CARTESIAN_POINT('Ctrl Pts',(3.62053606511612,3.75113802037702,57.9522653365595));
#62424=CARTESIAN_POINT('Ctrl Pts',(4.38163686641958,2.30322749768385,57.8993450824775));
#62425=CARTESIAN_POINT('Ctrl Pts',(5.14273766772306,0.855316974990642,57.8464248283956));
#62426=CARTESIAN_POINT('Ctrl Pts',(5.11516792362781,-1.00716183397399,57.7935045743136));
#62427=CARTESIAN_POINT('Ctrl Pts',(4.31154397009623,-2.43191018115001,57.7405843202316));
#62428=CARTESIAN_POINT('Ctrl Pts',(3.50792001656464,-3.85665852832602,57.6876640661497));
#62429=CARTESIAN_POINT('Ctrl Pts',(1.92824185359667,-4.84367641371333,57.6347438120677));
#62430=CARTESIAN_POINT('Ctrl Pts',(0.295394334515388,-4.94128937853172,
57.5818235579858));
#62431=CARTESIAN_POINT('Ctrl Pts',(-1.33745318456585,-5.03890234335011,
57.5289033039038));
#62432=CARTESIAN_POINT('Ctrl Pts',(-3.02347005976055,-4.24711038759957,
57.4759830498218));
#62433=CARTESIAN_POINT('Ctrl Pts',(-3.99110921895138,-2.92824960303174,
57.4230627957398));
#62434=CARTESIAN_POINT('Ctrl Pts',(-4.60512891022411,-2.09136068211493,
57.3894820153788));
#62435=CARTESIAN_POINT('Ctrl Pts',(-4.9298871379951,-1.04224259902719,57.3559012350179));
#62436=CARTESIAN_POINT('Ctrl Pts',(-4.93623902664834,0.00326946414225537,
57.3223204546569));
#62437=CARTESIAN_POINT('Ctrl Pts',(-4.93573111423024,0.00295138605979709,
57.1776795453432));
#62438=CARTESIAN_POINT('Ctrl Pts',(-4.93017780293081,-1.01634181563486,
57.2104097510422));
#62439=CARTESIAN_POINT('Ctrl Pts',(-4.62285556832308,-2.03870561435216,
57.2431399567412));
#62440=CARTESIAN_POINT('Ctrl Pts',(-4.03754280040764,-2.86388675849859,
57.2758701624402));
#62441=CARTESIAN_POINT('Ctrl Pts',(-3.09117232292437,-4.19809150543631,
57.3287904165222));
#62442=CARTESIAN_POINT('Ctrl Pts',(-1.41806634007047,-5.01681238170109,
57.3817106706042));
#62443=CARTESIAN_POINT('Ctrl Pts',(0.216136297556334,-4.94539021023678,
57.4346309246861));
#62444=CARTESIAN_POINT('Ctrl Pts',(1.85033893518309,-4.87396803877247,57.4875511787681));
#62445=CARTESIAN_POINT('Ctrl Pts',(3.4456382275827,-3.91240281957913,57.5404714328501));
#62446=CARTESIAN_POINT('Ctrl Pts',(4.27200085402752,-2.50072148265561,57.593391686932));
#62447=CARTESIAN_POINT('Ctrl Pts',(5.0983634804724,-1.08904014573198,57.646311941014));
#62448=CARTESIAN_POINT('Ctrl Pts',(5.15578944096228,0.772757308922017,57.699232195096));
#62449=CARTESIAN_POINT('Ctrl Pts',(4.41799973892759,2.23268393138458,57.7521524491779));
#62450=CARTESIAN_POINT('Ctrl Pts',(3.68021003689295,3.69261055384702,57.8050727032599));
#62451=CARTESIAN_POINT('Ctrl Pts',(2.14720467233395,4.75066634411819,57.8579929573418));
#62452=CARTESIAN_POINT('Ctrl Pts',(0.520510313201973,4.9226688132026,57.9109132114238));
#62453=CARTESIAN_POINT('Ctrl Pts',(-1.1061840459301,5.09467128228702,57.9638334655058));
#62454=CARTESIAN_POINT('Ctrl Pts',(-2.8265673996351,4.38062043018456,58.0167537195877));
#62455=CARTESIAN_POINT('Ctrl Pts',(-3.85336605036076,3.10727683230095,58.0696739736697));
#62456=CARTESIAN_POINT('Ctrl Pts',(-4.5519012154505,2.2410161688934,58.1056758308942));
#62457=CARTESIAN_POINT('Ctrl Pts',(-4.92943605312281,1.11590730173118,58.1416776881187));
#62458=CARTESIAN_POINT('Ctrl Pts',(-4.93796046055574,-0.00400002009900308,
58.1776795453432));
#62459=CARTESIAN_POINT('Origin',(0.,0.,16.));
#62460=CARTESIAN_POINT('',(-4.94980236868244,-0.00111614563719775,59.3223204546569));
#62461=CARTESIAN_POINT('',(-4.95000952859661,-0.000636468299896517,59.1776795453432));
#62462=CARTESIAN_POINT('',(-4.942,-6.05220448138622E-16,16.));
#62463=CARTESIAN_POINT('Ctrl Pts',(-4.94980236868244,-0.00111614563719775,
59.3223204546569));
#62464=CARTESIAN_POINT('Ctrl Pts',(-4.94498060556177,1.57441454729254,59.2713573632528));
#62465=CARTESIAN_POINT('Ctrl Pts',(-4.12744131963774,3.15424986030506,59.2203942718487));
#62466=CARTESIAN_POINT('Ctrl Pts',(-2.83642564175097,4.05688157506129,59.1694311804446));
#62467=CARTESIAN_POINT('Ctrl Pts',(-1.49583040281886,4.99417753516308,59.1165109263627));
#62468=CARTESIAN_POINT('Ctrl Pts',(0.355305856754859,5.20125711678249,59.0635906722807));
#62469=CARTESIAN_POINT('Ctrl Pts',(1.86987491274258,4.58335754070639,59.0106704181987));
#62470=CARTESIAN_POINT('Ctrl Pts',(3.38444396873026,3.96545796463031,58.9577501641168));
#62471=CARTESIAN_POINT('Ctrl Pts',(4.56244582113197,2.52257923085877,58.9048299100348));
#62472=CARTESIAN_POINT('Ctrl Pts',(4.86480883102114,0.915004684618019,58.8519096559529));
#62473=CARTESIAN_POINT('Ctrl Pts',(5.16717184091031,-0.692569861622737,
58.7989894018709));
#62474=CARTESIAN_POINT('Ctrl Pts',(4.59389600828695,-2.46484022033272,58.7460691477889));
#62475=CARTESIAN_POINT('Ctrl Pts',(3.40732110962866,-3.59078840801476,58.6931488937069));
#62476=CARTESIAN_POINT('Ctrl Pts',(2.22074621097036,-4.7167365956968,58.640228639625));
#62477=CARTESIAN_POINT('Ctrl Pts',(0.42087224627713,-5.1963626123509,58.5873083855431));
#62478=CARTESIAN_POINT('Ctrl Pts',(-1.16865096927437,-4.81018226757243,
58.5343881314611));
#62479=CARTESIAN_POINT('Ctrl Pts',(-2.75817418482588,-4.42400192279397,
58.4814678773791));
#62480=CARTESIAN_POINT('Ctrl Pts',(-4.13734665123566,-3.17201521658293,
58.4285476232971));
#62481=CARTESIAN_POINT('Ctrl Pts',(-4.67503798418886,-1.62715038691743,
58.3756273692152));
#62482=CARTESIAN_POINT('Ctrl Pts',(-4.85557797114165,-1.10843293863767,
58.3578583976957));
#62483=CARTESIAN_POINT('Ctrl Pts',(-4.94124878297087,-0.556696204625704,
58.3400894261763));
#62484=CARTESIAN_POINT('Ctrl Pts',(-4.9373129524182,-0.00377529733612325,
58.3223204546568));
#62485=CARTESIAN_POINT('Ctrl Pts',(-4.93796046055574,-0.00400002009900308,
58.1776795453432));
#62486=CARTESIAN_POINT('Ctrl Pts',(-4.94196634578065,-0.530279439411995,
58.1945979422007));
#62487=CARTESIAN_POINT('Ctrl Pts',(-4.86448168129051,-1.05541017361004,
58.2115163390581));
#62488=CARTESIAN_POINT('Ctrl Pts',(-4.70052410203468,-1.55198981852916,
58.2284347359156));
#62489=CARTESIAN_POINT('Ctrl Pts',(-4.18766955523667,-3.10527652781102,
58.2813549899975));
#62490=CARTESIAN_POINT('Ctrl Pts',(-2.82874651389436,-4.37921360271005,
58.3342752440795));
#62491=CARTESIAN_POINT('Ctrl Pts',(-1.24561891614835,-4.79082798129515,
58.3871954981615));
#62492=CARTESIAN_POINT('Ctrl Pts',(0.337508681597706,-5.20244235988026,
58.4401157522434));
#62493=CARTESIAN_POINT('Ctrl Pts',(2.14484083574746,-4.75173404215139,58.4930360063254));
#62494=CARTESIAN_POINT('Ctrl Pts',(3.34931474972224,-3.6449540378337,58.5459562604074));
#62495=CARTESIAN_POINT('Ctrl Pts',(4.55378866369698,-2.53817403351603,58.5988765144893));
#62496=CARTESIAN_POINT('Ctrl Pts',(5.15540433749678,-0.775322342609574,
58.6517967685713));
#62497=CARTESIAN_POINT('Ctrl Pts',(4.87885325049583,0.836893177623885,58.7047170226533));
#62498=CARTESIAN_POINT('Ctrl Pts',(4.60230216349487,2.44910869785739,58.7576372767352));
#62499=CARTESIAN_POINT('Ctrl Pts',(3.44758431569312,3.91068804741789,58.8105575308172));
#62500=CARTESIAN_POINT('Ctrl Pts',(1.94311622990263,4.5527901936852,58.8634777848992));
#62501=CARTESIAN_POINT('Ctrl Pts',(0.438648144112182,5.19489233995249,58.9163980389811));
#62502=CARTESIAN_POINT('Ctrl Pts',(-1.41557017966698,5.01751728292666,58.969318293063));
#62503=CARTESIAN_POINT('Ctrl Pts',(-2.77102011755545,4.10183455769855,59.022238547145));
#62504=CARTESIAN_POINT('Ctrl Pts',(-4.09812694403132,3.205299199536,59.0740522132111));
#62505=CARTESIAN_POINT('Ctrl Pts',(-4.94710627363632,1.60101008771938,59.1258658792772));
#62506=CARTESIAN_POINT('Ctrl Pts',(-4.95000952859661,-0.000636468299896517,
59.1776795453432));
#62507=CARTESIAN_POINT('Origin',(0.,0.,16.));
#62508=CARTESIAN_POINT('',(-4.9405850371911,0.0044815032353801,60.3223204546569));
#62509=CARTESIAN_POINT('',(-4.93981933179839,0.00440230787564107,60.1776795453432));
#62510=CARTESIAN_POINT('',(-4.942,-6.05220448138622E-16,16.));
#62511=CARTESIAN_POINT('Ctrl Pts',(-4.9405850371911,0.0044815032353801,
60.3223204546569));
#62512=CARTESIAN_POINT('Ctrl Pts',(-4.94441025446321,0.434877172261215,
60.3084658084932));
#62513=CARTESIAN_POINT('Ctrl Pts',(-4.89283730030809,0.864370712953886,
60.2946111623296));
#62514=CARTESIAN_POINT('Ctrl Pts',(-4.78226597761638,1.27809649658665,60.2807565161659));
#62515=CARTESIAN_POINT('Ctrl Pts',(-4.3599193928029,2.85839478291331,60.2278362620839));
#62516=CARTESIAN_POINT('Ctrl Pts',(-3.07679122526311,4.20864272692144,60.1749160080019));
#62517=CARTESIAN_POINT('Ctrl Pts',(-1.52006052129332,4.71094624750269,60.12199575392));
#62518=CARTESIAN_POINT('Ctrl Pts',(0.0366701826763779,5.21324976808391,
60.069075499838));
#62519=CARTESIAN_POINT('Ctrl Pts',(1.867003423076,4.86760886523835,60.016155245756));
#62520=CARTESIAN_POINT('Ctrl Pts',(3.1333507549704,3.83219409497753,59.9632349916741));
#62521=CARTESIAN_POINT('Ctrl Pts',(4.39969808686486,2.79677932471666,59.9103147375921));
#62522=CARTESIAN_POINT('Ctrl Pts',(5.102059510254,1.07159068704033,59.8573944835102));
#62523=CARTESIAN_POINT('Ctrl Pts',(4.91902371084035,-0.55389914916401,59.8044742294282));
#62524=CARTESIAN_POINT('Ctrl Pts',(4.73598791142671,-2.1793889853683,59.7515539753462));
#62525=CARTESIAN_POINT('Ctrl Pts',(3.66755488921043,-3.70518002010068,59.6986337212642));
#62526=CARTESIAN_POINT('Ctrl Pts',(2.20265591301344,-4.43304697292067,59.6457134671823));
#62527=CARTESIAN_POINT('Ctrl Pts',(0.737756936816448,-5.16091392574066,
59.5927932131003));
#62528=CARTESIAN_POINT('Ctrl Pts',(-1.12360799336121,-5.09085679664823,
59.5398729590184));
#62529=CARTESIAN_POINT('Ctrl Pts',(-2.52964985740424,-4.25493479787751,
59.4869527049364));
#62530=CARTESIAN_POINT('Ctrl Pts',(-3.93569172144728,-3.41901279910679,
59.4340324508545));
#62531=CARTESIAN_POINT('Ctrl Pts',(-4.88641051935565,-1.8172259306578,59.3811121967725));
#62532=CARTESIAN_POINT('Ctrl Pts',(-4.94674280916461,-0.182576327141242,
59.3281919426905));
#62533=CARTESIAN_POINT('Ctrl Pts',(-4.94897409296954,-0.122121681733242,
59.3262347800127));
#62534=CARTESIAN_POINT('Ctrl Pts',(-4.94998754141356,-0.0616220879792628,
59.3242776173348));
#62535=CARTESIAN_POINT('Ctrl Pts',(-4.94980236868244,-0.00111614563719775,
59.3223204546569));
#62536=CARTESIAN_POINT('Ctrl Pts',(-4.95000952859661,-0.000636468299896517,
59.1776795453432));
#62537=CARTESIAN_POINT('Ctrl Pts',(-4.95007153361169,-0.0348429435249772,
59.1787861333591));
#62538=CARTESIAN_POINT('Ctrl Pts',(-4.94974762270576,-0.0690482134159459,
59.179892721375));
#62539=CARTESIAN_POINT('Ctrl Pts',(-4.94903421151526,-0.103245357661693,
59.1809993093909));
#62540=CARTESIAN_POINT('Ctrl Pts',(-4.9149168155888,-1.73865215436347,59.2339195634729));
#62541=CARTESIAN_POINT('Ctrl Pts',(-3.99000047173805,-3.35547535433661,
59.2868398175548));
#62542=CARTESIAN_POINT('Ctrl Pts',(-2.59754102487793,-4.21383196801951,
59.3397600716368));
#62543=CARTESIAN_POINT('Ctrl Pts',(-1.20508157801781,-5.07218858170242,
59.3926803257188));
#62544=CARTESIAN_POINT('Ctrl Pts',(0.654920971851715,-5.17207860909511,
59.4456005798008));
#62545=CARTESIAN_POINT('Ctrl Pts',(2.13130105065146,-4.46779084807236,59.4985208338827));
#62546=CARTESIAN_POINT('Ctrl Pts',(3.60768112945116,-3.76350308704963,59.5514410879647));
#62547=CARTESIAN_POINT('Ctrl Pts',(4.70043873718116,-2.25503753761151,59.6043613420466));
#62548=CARTESIAN_POINT('Ctrl Pts',(4.90951130318629,-0.632691073520989,
59.6572815961286));
#62549=CARTESIAN_POINT('Ctrl Pts',(5.11858386919144,0.98965539056958,59.7102018502105));
#62550=CARTESIAN_POINT('Ctrl Pts',(4.44397139347178,2.7258827693125,59.7631221042925));
#62551=CARTESIAN_POINT('Ctrl Pts',(3.19438684806975,3.78146689731725,59.8160423583745));
#62552=CARTESIAN_POINT('Ctrl Pts',(1.94480230266778,4.83705102532194,59.8689626124565));
#62553=CARTESIAN_POINT('Ctrl Pts',(0.120245687583507,5.21199190258845,59.9218828665384));
#62554=CARTESIAN_POINT('Ctrl Pts',(-1.44433802421679,4.7347108573205,59.9748031206203));
#62555=CARTESIAN_POINT('Ctrl Pts',(-3.00892173601718,4.25742981205253,60.0277233747023));
#62556=CARTESIAN_POINT('Ctrl Pts',(-4.31353254453361,2.92792684424999,60.0806436287843));
#62557=CARTESIAN_POINT('Ctrl Pts',(-4.7611606188609,1.35460281707783,60.1335638828663));
#62558=CARTESIAN_POINT('Ctrl Pts',(-4.88554531419032,0.917415247758462,
60.1482691036919));
#62559=CARTESIAN_POINT('Ctrl Pts',(-4.94375845579816,0.461401140068047,
60.1629743245176));
#62560=CARTESIAN_POINT('Ctrl Pts',(-4.93981933179839,0.00440230787564107,
60.1776795453432));
#62561=CARTESIAN_POINT('Origin',(0.,0.,16.));
#62562=CARTESIAN_POINT('',(-4.93439206002794,-0.00160550854955477,61.3223204546568));
#62563=CARTESIAN_POINT('',(-4.93468237204831,-0.00200522711461992,61.1776795453432));
#62564=CARTESIAN_POINT('',(-4.942,-6.05220448138622E-16,16.));
#62565=CARTESIAN_POINT('Ctrl Pts',(-4.93439206002794,-0.00160550854955477,
61.3223204546568));
#62566=CARTESIAN_POINT('Ctrl Pts',(-4.93169731118072,0.922902919227787,
61.2926539996516));
#62567=CARTESIAN_POINT('Ctrl Pts',(-4.68258000927622,1.84875941269167,61.2629875446464));
#62568=CARTESIAN_POINT('Ctrl Pts',(-4.19611032092476,2.62607248755302,61.2333210896412));
#62569=CARTESIAN_POINT('Ctrl Pts',(-3.3283254943857,4.01267582171134,61.1804008355592));
#62570=CARTESIAN_POINT('Ctrl Pts',(-1.7052638805986,4.92660054644685,61.1274805814773));
#62571=CARTESIAN_POINT('Ctrl Pts',(-0.0696632625637214,4.94962074962347,
61.0745603273953));
#62572=CARTESIAN_POINT('Ctrl Pts',(1.56593735547125,4.97264095280009,61.0216400733134));
#62573=CARTESIAN_POINT('Ctrl Pts',(3.21407697775393,4.10475663441781,60.9687198192314));
#62574=CARTESIAN_POINT('Ctrl Pts',(4.12054174158777,2.74312491350412,60.9157995651494));
#62575=CARTESIAN_POINT('Ctrl Pts',(5.02700650542156,1.3814931925905,60.8628793110674));
#62576=CARTESIAN_POINT('Ctrl Pts',(5.19179641080646,-0.473885930854428,
60.8099590569854));
#62577=CARTESIAN_POINT('Ctrl Pts',(4.53950108025175,-1.97396263329564,60.7570388029035));
#62578=CARTESIAN_POINT('Ctrl Pts',(3.88720574969703,-3.47403933573684,60.7041185488216));
#62579=CARTESIAN_POINT('Ctrl Pts',(2.41782518320256,-4.61881361717445,60.6511982947396));
#62580=CARTESIAN_POINT('Ctrl Pts',(0.803770369403307,-4.88441928262956,
60.5982780406577));
#62581=CARTESIAN_POINT('Ctrl Pts',(-0.810284444395997,-5.15002494808468,
60.5453577865757));
#62582=CARTESIAN_POINT('Ctrl Pts',(-2.56901350550008,-4.53646199755745,
60.4924375324937));
#62583=CARTESIAN_POINT('Ctrl Pts',(-3.66759553500858,-3.32450620797124,
60.4395172784117));
#62584=CARTESIAN_POINT('Ctrl Pts',(-4.47856622242051,-2.42984327576097,
60.4004516704934));
#62585=CARTESIAN_POINT('Ctrl Pts',(-4.92979916533343,-1.20909466877745,
60.3613860625752));
#62586=CARTESIAN_POINT('Ctrl Pts',(-4.9405850371911,0.0044815032353801,
60.3223204546569));
#62587=CARTESIAN_POINT('Ctrl Pts',(-4.93981933179839,0.00440230787564107,
60.1776795453432));
#62588=CARTESIAN_POINT('Ctrl Pts',(-4.9295825759933,-1.18321845466868,60.2158945785995));
#62589=CARTESIAN_POINT('Ctrl Pts',(-4.49960389811683,-2.3774895002097,60.2541096118559));
#62590=CARTESIAN_POINT('Ctrl Pts',(-3.72042358357856,-3.26527909823641,
60.2923246451122));
#62591=CARTESIAN_POINT('Ctrl Pts',(-2.64141313383085,-4.49469189983651,
60.3452448991941));
#62592=CARTESIAN_POINT('Ctrl Pts',(-0.892746894197383,-5.13637241649503,
60.3981651532761));
#62593=CARTESIAN_POINT('Ctrl Pts',(0.72535875721281,-4.89667784359578,60.451085407358));
#62594=CARTESIAN_POINT('Ctrl Pts',(2.34346440862305,-4.65698327069652,60.50400566144));
#62595=CARTESIAN_POINT('Ctrl Pts',(3.83100947181002,-3.53591360823934,60.556925915522));
#62596=CARTESIAN_POINT('Ctrl Pts',(4.50727060703144,-2.0464874555241,60.6098461696039));
#62597=CARTESIAN_POINT('Ctrl Pts',(5.18353174225287,-0.557061302808867,
60.6627664236859));
#62598=CARTESIAN_POINT('Ctrl Pts',(5.04850894950886,1.30072134016443,60.7156866777678));
#62599=CARTESIAN_POINT('Ctrl Pts',(4.16399072092151,2.67671076261644,60.7686069318498));
#62600=CARTESIAN_POINT('Ctrl Pts',(3.27947249233419,4.0527001850684,60.8215271859318));
#62601=CARTESIAN_POINT('Ctrl Pts',(1.64545882790348,4.94689638699909,60.8744474400138));
#62602=CARTESIAN_POINT('Ctrl Pts',(0.00969933627160482,4.95010152961563,
60.9273676940957));
#62603=CARTESIAN_POINT('Ctrl Pts',(-1.62606015536036,4.95330667223218,60.9802879481777));
#62604=CARTESIAN_POINT('Ctrl Pts',(-3.26356547419351,4.06552075553457,61.0332082022597));
#62605=CARTESIAN_POINT('Ctrl Pts',(-4.15346917720423,2.69300817389058,61.0861284563416));
#62606=CARTESIAN_POINT('Ctrl Pts',(-4.66664165108668,1.90153413622322,61.1166454860088));
#62607=CARTESIAN_POINT('Ctrl Pts',(-4.93120852346023,0.948870286286938,
61.147162515676));
#62608=CARTESIAN_POINT('Ctrl Pts',(-4.93468237204831,-0.00200522711461992,
61.1776795453432));
#62609=CARTESIAN_POINT('Origin',(0.,0.,16.));
#62610=CARTESIAN_POINT('',(-4.94646539259968,-0.00363051697945815,62.3223204546568));
#62611=CARTESIAN_POINT('',(-4.94715367607242,-0.003331217148393,62.1776795453432));
#62612=CARTESIAN_POINT('',(-4.942,-6.05220448138622E-16,16.));
#62613=CARTESIAN_POINT('Ctrl Pts',(-4.94646539259968,-0.00363051697945815,
62.3223204546568));
#62614=CARTESIAN_POINT('Ctrl Pts',(-4.93485651568824,1.40483737949782,62.2768421908101));
#62615=CARTESIAN_POINT('Ctrl Pts',(-4.3027525120455,2.82241015727549,62.2313639269634));
#62616=CARTESIAN_POINT('Ctrl Pts',(-3.23996042330606,3.74249315171913,62.1858856631166));
#62617=CARTESIAN_POINT('Ctrl Pts',(-2.00325473986379,4.81313705330919,62.1329654090346));
#62618=CARTESIAN_POINT('Ctrl Pts',(-0.183373993763468,5.2101527640882,62.0800451549526));
#62619=CARTESIAN_POINT('Ctrl Pts',(1.3868765910888,4.75185983130228,62.0271249008706));
#62620=CARTESIAN_POINT('Ctrl Pts',(2.95712717594107,4.29356689851636,61.9742046467886));
#62621=CARTESIAN_POINT('Ctrl Pts',(4.2777475995453,2.97996532216552,61.9212843927068));
#62622=CARTESIAN_POINT('Ctrl Pts',(4.74440178662215,1.4121792458292,61.8683641386248));
#62623=CARTESIAN_POINT('Ctrl Pts',(5.21105597369902,-0.155606830507172,
61.8154438845429));
#62624=CARTESIAN_POINT('Ctrl Pts',(4.82374392424848,-1.97757740682905,61.7625236304608));
#62625=CARTESIAN_POINT('Ctrl Pts',(3.75970554739938,-3.21997092100356,61.7096033763788));
#62626=CARTESIAN_POINT('Ctrl Pts',(2.69566717055032,-4.46236443517805,61.6566831222968));
#62627=CARTESIAN_POINT('Ctrl Pts',(0.954902466302742,-5.12518088720521,
61.603762868215));
#62628=CARTESIAN_POINT('Ctrl Pts',(-0.665988050504544,-4.90510534564135,
61.550842614133));
#62629=CARTESIAN_POINT('Ctrl Pts',(-2.28687856731188,-4.68502980407749,
61.4979223600511));
#62630=CARTESIAN_POINT('Ctrl Pts',(-3.78789489667891,-3.58206226892256,
61.4450021059691));
#62631=CARTESIAN_POINT('Ctrl Pts',(-4.4821490417169,-2.10093752955449,61.3920818518871));
#62632=CARTESIAN_POINT('Ctrl Pts',(-4.78721270168923,-1.45011342271034,
61.3688280528103));
#62633=CARTESIAN_POINT('Ctrl Pts',(-4.9365043160506,-0.726273596479458,
61.3455742537336));
#62634=CARTESIAN_POINT('Ctrl Pts',(-4.93439206002794,-0.00160550854955477,
61.3223204546568));
#62635=CARTESIAN_POINT('Ctrl Pts',(-4.93468237204831,-0.00200522711461992,
61.1776795453432));
#62636=CARTESIAN_POINT('Ctrl Pts',(-4.93723260089922,-0.700063909415997,
61.200082769758));
#62637=CARTESIAN_POINT('Ctrl Pts',(-4.79907061241107,-1.39715879423438,
61.2224859941727));
#62638=CARTESIAN_POINT('Ctrl Pts',(-4.51525583033475,-2.02880852158482,
61.2448892185875));
#62639=CARTESIAN_POINT('Ctrl Pts',(-3.84483669326632,-3.520873388826,61.2978094726695));
#62640=CARTESIAN_POINT('Ctrl Pts',(-2.36169633194117,-4.64776387671811,
61.3507297267514));
#62641=CARTESIAN_POINT('Ctrl Pts',(-0.744542427257826,-4.89379768734264,
61.4036499808334));
#62642=CARTESIAN_POINT('Ctrl Pts',(0.872611477425563,-5.13983149796717,
61.4565702349153));
#62643=CARTESIAN_POINT('Ctrl Pts',(2.62377892546721,-4.50500863132408,61.5094904889973));
#62644=CARTESIAN_POINT('Ctrl Pts',(3.7075989475901,-3.27983372664773,61.5624107430792));
#62645=CARTESIAN_POINT('Ctrl Pts',(4.79141896971299,-2.05465882197138,61.6153309971612));
#62646=CARTESIAN_POINT('Ctrl Pts',(5.20789156591715,-0.23913187926188,61.6682512512432));
#62647=CARTESIAN_POINT('Ctrl Pts',(4.76643251551905,1.33593424450079,61.7211715053252));
#62648=CARTESIAN_POINT('Ctrl Pts',(4.32497346512095,2.91100036826346,61.7740917594072));
#62649=CARTESIAN_POINT('Ctrl Pts',(3.02558276812051,4.24560567307922,61.8270120134891));
#62650=CARTESIAN_POINT('Ctrl Pts',(1.46288145266801,4.72901438843942,61.879932267571));
#62651=CARTESIAN_POINT('Ctrl Pts',(-0.099819862784441,5.2124231037996,61.932852521653));
#62652=CARTESIAN_POINT('Ctrl Pts',(-1.92583179668899,4.84463522970427,61.985772775735));
#62653=CARTESIAN_POINT('Ctrl Pts',(-3.17954339996051,3.79395611445292,62.038693029817));
#62654=CARTESIAN_POINT('Ctrl Pts',(-4.27710053403159,2.87414301265627,62.0850218683257));
#62655=CARTESIAN_POINT('Ctrl Pts',(-4.93604317278978,1.43095786114934,62.1313507068344));
#62656=CARTESIAN_POINT('Ctrl Pts',(-4.94715367607242,-0.003331217148393,
62.1776795453432));
#62657=CARTESIAN_POINT('Origin',(0.,0.,16.));
#62658=CARTESIAN_POINT('',(-4.94566965389892,0.00391030538274315,63.3223204546568));
#62659=CARTESIAN_POINT('',(-4.94490839420487,0.00412192395711707,63.1776795453432));
#62660=CARTESIAN_POINT('',(-4.942,-6.05220448138622E-16,16.));
#62661=CARTESIAN_POINT('Ctrl Pts',(-4.94566965389892,0.00391030538274314,
63.3223204546568));
#62662=CARTESIAN_POINT('Ctrl Pts',(-4.94791640205867,0.263233220344943,
63.3139506360505));
#62663=CARTESIAN_POINT('Ctrl Pts',(-4.92928016281063,0.522232554885722,
63.3055808174441));
#62664=CARTESIAN_POINT('Ctrl Pts',(-4.88863316854879,0.777730209403516,
63.2972109988377));
#62665=CARTESIAN_POINT('Ctrl Pts',(-4.63163246576532,2.39317750047789,63.2442907447558));
#62666=CARTESIAN_POINT('Ctrl Pts',(-3.49470467070217,3.86863762987662,63.1913704906738));
#62667=CARTESIAN_POINT('Ctrl Pts',(-1.99812530633611,4.52891750812856,63.1384502365919));
#62668=CARTESIAN_POINT('Ctrl Pts',(-0.501545941970182,5.18919738638045,
63.0855299825099));
#62669=CARTESIAN_POINT('Ctrl Pts',(1.35468499169859,5.0342970134857,63.0326097284279));
#62670=CARTESIAN_POINT('Ctrl Pts',(2.72112786976736,4.1351011658277,62.979689474346));
#62671=CARTESIAN_POINT('Ctrl Pts',(4.08757074783617,3.23590531816966,62.926769220264));
#62672=CARTESIAN_POINT('Ctrl Pts',(4.96422557030495,1.59241399574832,62.8738489661821));
#62673=CARTESIAN_POINT('Ctrl Pts',(4.94992170152689,-0.0432860717482803,
62.8209287121001));
#62674=CARTESIAN_POINT('Ctrl Pts',(4.93561783274882,-1.67898613924493,62.7680084580182));
#62675=CARTESIAN_POINT('Ctrl Pts',(4.03035527272386,-3.30689495181684,62.7150882039362));
#62676=CARTESIAN_POINT('Ctrl Pts',(2.64839599472191,-4.18205657427003,62.6621679498542));
#62677=CARTESIAN_POINT('Ctrl Pts',(1.26643671671996,-5.05721819672321,62.6092476957723));
#62678=CARTESIAN_POINT('Ctrl Pts',(-0.592219279258987,-5.17963262905766,
62.5563274416903));
#62679=CARTESIAN_POINT('Ctrl Pts',(-2.07702262276162,-4.49328115743837,
62.5034071876083));
#62680=CARTESIAN_POINT('Ctrl Pts',(-3.56182596626416,-3.80692968581911,
62.4504869335263));
#62681=CARTESIAN_POINT('Ctrl Pts',(-4.67277665729038,-2.31181231024634,
62.3975666794443));
#62682=CARTESIAN_POINT('Ctrl Pts',(-4.9014866924115,-0.692117576259364,
62.3446464253624));
#62683=CARTESIAN_POINT('Ctrl Pts',(-4.93364938470368,-0.464345570938786,
62.3372044351272));
#62684=CARTESIAN_POINT('Ctrl Pts',(-4.94836505061889,-0.234109947053592,
62.329762444892));
#62685=CARTESIAN_POINT('Ctrl Pts',(-4.94646539259968,-0.00363051697945815,
62.3223204546568));
#62686=CARTESIAN_POINT('Ctrl Pts',(-4.94715367607242,-0.003331217148393,
62.1776795453432));
#62687=CARTESIAN_POINT('Ctrl Pts',(-4.94873441814843,-0.207394078888273,
62.1842709609164));
#62688=CARTESIAN_POINT('Ctrl Pts',(-4.93720170764577,-0.4112768658406,62.1908623764896));
#62689=CARTESIAN_POINT('Ctrl Pts',(-4.91195301252751,-0.613446683379284,
62.1974537920628));
#62690=CARTESIAN_POINT('Ctrl Pts',(-4.70923974918446,-2.23660000955276,
62.2503740461448));
#62691=CARTESIAN_POINT('Ctrl Pts',(-3.6224019498598,-3.74933630549224,62.3032943002267));
#62692=CARTESIAN_POINT('Ctrl Pts',(-2.14879319047093,-4.45940433860991,
62.3562145543087));
#62693=CARTESIAN_POINT('Ctrl Pts',(-0.675184431082104,-5.16947237172755,
62.4091348083907));
#62694=CARTESIAN_POINT('Ctrl Pts',(1.18519528837092,-5.07687214202343,62.4620550624727));
#62695=CARTESIAN_POINT('Ctrl Pts',(2.58100779524721,-4.22397892886556,62.5149753165546));
#62696=CARTESIAN_POINT('Ctrl Pts',(3.97682030212355,-3.37108571570767,62.5678955706366));
#62697=CARTESIAN_POINT('Ctrl Pts',(4.90806559642314,-1.75789951909599,62.6208158247185));
#62698=CARTESIAN_POINT('Ctrl Pts',(4.94859160884553,-0.122638980307035,
62.6737360788005));
#62699=CARTESIAN_POINT('Ctrl Pts',(4.98911762126792,1.51262155848192,62.7266563328825));
#62700=CARTESIAN_POINT('Ctrl Pts',(4.13892435181312,3.16995643944814,62.7795765869645));
#62701=CARTESIAN_POINT('Ctrl Pts',(2.78707322532942,4.09094390908492,62.8324968410464));
#62702=CARTESIAN_POINT('Ctrl Pts',(1.43522209884579,5.01193137872164,62.8854170951284));
#62703=CARTESIAN_POINT('Ctrl Pts',(-0.418286884666658,5.19657143702902,
62.9383373492103));
#62704=CARTESIAN_POINT('Ctrl Pts',(-1.92525970626815,4.56036997337358,62.9912576032922));
#62705=CARTESIAN_POINT('Ctrl Pts',(-3.43223252786973,3.92416850971811,63.0441778573742));
#62706=CARTESIAN_POINT('Ctrl Pts',(-4.59266918756032,2.46712552409973,63.0970981114562));
#62707=CARTESIAN_POINT('Ctrl Pts',(-4.87553614686583,0.856006139716171,
63.1500183655382));
#62708=CARTESIAN_POINT('Ctrl Pts',(-4.9248205778018,0.57529784411246,63.1592387588066));
#62709=CARTESIAN_POINT('Ctrl Pts',(-4.94746485856309,0.289912292218248,
63.1684591520749));
#62710=CARTESIAN_POINT('Ctrl Pts',(-4.94490839420487,0.00412192395711708,
63.1776795453432));
#62711=CARTESIAN_POINT('Origin',(0.,0.,16.));
#62712=CARTESIAN_POINT('',(-4.93415080838549,0.00115309545102804,64.3223204546568));
#62713=CARTESIAN_POINT('',(-4.9340004404197,0.000727385793248169,64.1776795453432));
#62714=CARTESIAN_POINT('',(-4.942,-6.05220448138622E-16,16.));
#62715=CARTESIAN_POINT('Ctrl Pts',(-4.93415080838549,0.00115309545102804,
64.3223204546568));
#62716=CARTESIAN_POINT('Ctrl Pts',(-4.93572402472308,0.754827492624239,
64.2981388272089));
#62717=CARTESIAN_POINT('Ctrl Pts',(-4.77374496051519,1.5078605887699,64.273957199761));
#62718=CARTESIAN_POINT('Ctrl Pts',(-4.44472183637519,2.17900122361227,64.2497755723131));
#62719=CARTESIAN_POINT('Ctrl Pts',(-3.72467156821878,3.64775815476123,64.1968553182311));
#62720=CARTESIAN_POINT('Ctrl Pts',(-2.20459580691742,4.72430684596657,64.1439350641492));
#62721=CARTESIAN_POINT('Ctrl Pts',(-0.580104436501948,4.91600217432875,
64.0910148100672));
#62722=CARTESIAN_POINT('Ctrl Pts',(1.04438693391362,5.10769750269094,64.0380945559853));
#62723=CARTESIAN_POINT('Ctrl Pts',(2.77329391344336,4.41453946820987,63.9851743019033));
#62724=CARTESIAN_POINT('Ctrl Pts',(3.81544226317875,3.15372777385805,63.9322540478213));
#62725=CARTESIAN_POINT('Ctrl Pts',(4.85759061291414,1.89291607950622,63.8793337937393));
#62726=CARTESIAN_POINT('Ctrl Pts',(5.2129803328552,0.0644507252837223,63.8264135396574));
#62727=CARTESIAN_POINT('Ctrl Pts',(4.71897965939677,-1.49493461711666,63.7734932855754));
#62728=CARTESIAN_POINT('Ctrl Pts',(4.22497898593836,-3.05431995951699,63.7205730314935));
#62729=CARTESIAN_POINT('Ctrl Pts',(2.88158791908043,-4.34462529009514,63.6676527774115));
#62730=CARTESIAN_POINT('Ctrl Pts',(1.30356272822442,-4.77538718313377,63.6147325233296));
#62731=CARTESIAN_POINT('Ctrl Pts',(-0.274462462631595,-5.2061490761724,
63.5618122692476));
#62732=CARTESIAN_POINT('Ctrl Pts',(-2.08712177748574,-4.77736753167153,
63.5088920151656));
#62733=CARTESIAN_POINT('Ctrl Pts',(-3.30491462966089,-3.68525953304616,
63.4559717610837));
#62734=CARTESIAN_POINT('Ctrl Pts',(-4.33010248683659,-2.76587832883282,
63.4114213256081));
#62735=CARTESIAN_POINT('Ctrl Pts',(-4.93371077956384,-1.37640022865803,
63.3668708901324));
#62736=CARTESIAN_POINT('Ctrl Pts',(-4.94566965389892,0.00391030538274314,
63.3223204546568));
#62737=CARTESIAN_POINT('Ctrl Pts',(-4.94490839420487,0.00412192395711708,
63.1776795453432));
#62738=CARTESIAN_POINT('Ctrl Pts',(-4.9327920849133,-1.35037554176026,63.2213794061568));
#62739=CARTESIAN_POINT('Ctrl Pts',(-4.35459996207,-2.71396626059995,63.2650792669704));
#62740=CARTESIAN_POINT('Ctrl Pts',(-3.36357298066115,-3.6318006600574,63.308779127784));
#62741=CARTESIAN_POINT('Ctrl Pts',(-2.16344559623047,-4.74329229229879,
63.361699381866));
#62742=CARTESIAN_POINT('Ctrl Pts',(-0.35789356844863,-5.2010797736329,63.4146196359481));
#62743=CARTESIAN_POINT('Ctrl Pts',(1.22683491911902,-4.7956725609509,63.46753989003));
#62744=CARTESIAN_POINT('Ctrl Pts',(2.81156340668672,-4.39026534826889,63.520460144112));
#62745=CARTESIAN_POINT('Ctrl Pts',(4.17546835404021,-3.12166344157071,63.5733803981938));
#62746=CARTESIAN_POINT('Ctrl Pts',(4.69440602676098,-1.57039844833637,63.6263006522758));
#62747=CARTESIAN_POINT('Ctrl Pts',(5.21334369948175,-0.0191334551020692,
63.6792209063577));
#62748=CARTESIAN_POINT('Ctrl Pts',(4.88731409756984,1.81479462466838,63.7321411604398));
#62749=CARTESIAN_POINT('Ctrl Pts',(3.86551334621209,3.09215229264073,63.7850614145218));
#62750=CARTESIAN_POINT('Ctrl Pts',(2.84371259485431,4.36950996061312,63.8379816686038));
#62751=CARTESIAN_POINT('Ctrl Pts',(1.12614069405063,5.09029721678739,63.8909019226856));
#62752=CARTESIAN_POINT('Ctrl Pts',(-0.501215222432739,4.92467080437148,
63.9438221767676));
#62753=CARTESIAN_POINT('Ctrl Pts',(-2.12857113891606,4.75904439195557,63.9967424308495));
#62754=CARTESIAN_POINT('Ctrl Pts',(-3.66571107107909,3.70700431094953,64.0496626849316));
#62755=CARTESIAN_POINT('Ctrl Pts',(-4.40921630968873,2.24998016991306,64.1025829390136));
#62756=CARTESIAN_POINT('Ctrl Pts',(-4.76090724023141,1.56078236823718,64.1276151411235));
#62757=CARTESIAN_POINT('Ctrl Pts',(-4.93502599479208,0.780971213387874,
64.1526473432333));
#62758=CARTESIAN_POINT('Ctrl Pts',(-4.9340004404197,0.000727385793248169,
64.1776795453432));
#62759=CARTESIAN_POINT('Origin',(0.,0.,16.));
#62760=CARTESIAN_POINT('',(-4.94144181990917,-0.00451754960951789,65.3223204546568));
#62761=CARTESIAN_POINT('',(-4.94223974397651,-0.00450342756324047,65.1776795453432));
#62762=CARTESIAN_POINT('',(-4.942,-6.05220448138622E-16,16.));
#62763=CARTESIAN_POINT('Ctrl Pts',(-4.94144181990917,-0.00451754960951789,
65.3223204546568));
#62764=CARTESIAN_POINT('Ctrl Pts',(-4.93014544737618,1.2373328062097,65.2823270183674));
#62765=CARTESIAN_POINT('Ctrl Pts',(-4.45501720554112,2.48688539619672,65.2423335820779));
#62766=CARTESIAN_POINT('Ctrl Pts',(-3.60889481176119,3.38813765554137,65.2023401457884));
#62767=CARTESIAN_POINT('Ctrl Pts',(-2.48928579044125,4.58069580961582,65.1494198917065));
#62768=CARTESIAN_POINT('Ctrl Pts',(-0.720095544969354,5.16340781391902,
65.0964996376245));
#62769=CARTESIAN_POINT('Ctrl Pts',(0.889067448016765,4.86961575569687,65.0435793835425));
#62770=CARTESIAN_POINT('Ctrl Pts',(2.49823044100288,4.57582369747472,64.9906591294606));
#62771=CARTESIAN_POINT('Ctrl Pts',(3.94736618150317,3.40552757672724,64.9377388753786));
#62772=CARTESIAN_POINT('Ctrl Pts',(4.57332802245098,1.89427277188866,64.8848186212967));
#62773=CARTESIAN_POINT('Ctrl Pts',(5.19928986339881,0.383017967050043,64.8318983672147));
#62774=CARTESIAN_POINT('Ctrl Pts',(5.00207780479406,-1.46919552187978,64.7789781131327));
#62775=CARTESIAN_POINT('Ctrl Pts',(4.07193909661463,-2.81476651406745,64.7260578590508));
#62776=CARTESIAN_POINT('Ctrl Pts',(3.14180038843529,-4.16033750625501,64.6731376049688));
#62777=CARTESIAN_POINT('Ctrl Pts',(1.47873503068148,-4.99926600170063,64.6202173508868));
#62778=CARTESIAN_POINT('Ctrl Pts',(-0.156212869442396,-4.94764550818617,
64.5672970968049));
#62779=CARTESIAN_POINT('Ctrl Pts',(-1.79116076956636,-4.8960250146717,64.5143768427229));
#62780=CARTESIAN_POINT('Ctrl Pts',(-3.39799121206035,-3.95385553219706,
64.461456588641));
#62781=CARTESIAN_POINT('Ctrl Pts',(-4.24139404580168,-2.55228820541339,
64.408536334559));
#62782=CARTESIAN_POINT('Ctrl Pts',(-4.69940845940318,-1.7911595826268,64.379797707925));
#62783=CARTESIAN_POINT('Ctrl Pts',(-4.93228112128365,-0.89455035340317,
64.3510590812909));
#62784=CARTESIAN_POINT('Ctrl Pts',(-4.93415080838549,0.00115309545102804,
64.3223204546568));
#62785=CARTESIAN_POINT('Ctrl Pts',(-4.9340004404197,0.000727385793248169,
64.1776795453432));
#62786=CARTESIAN_POINT('Ctrl Pts',(-4.93285788358386,-0.868532151155221,
64.2055675973153));
#62787=CARTESIAN_POINT('Ctrl Pts',(-4.71432797343864,-1.73832871715993,
64.2334556492873));
#62788=CARTESIAN_POINT('Ctrl Pts',(-4.28176794905193,-2.48396104258879,
64.2613437012593));
#62789=CARTESIAN_POINT('Ctrl Pts',(-3.46094380474913,-3.89886991298749,
64.3142639553413));
#62790=CARTESIAN_POINT('Ctrl Pts',(-1.86942497108703,-4.86667945271791,
64.3671842094234));
#62791=CARTESIAN_POINT('Ctrl Pts',(-0.23551477313756,-4.94450523533559,
64.4201044635053));
#62792=CARTESIAN_POINT('Ctrl Pts',(1.39839542481181,-5.02233101795326,64.4730247175873));
#62793=CARTESIAN_POINT('Ctrl Pts',(3.0746969870487,-4.21017304345841,64.5259449716692));
#62794=CARTESIAN_POINT('Ctrl Pts',(4.0262887170445,-2.87968720482404,64.5788652257512));
#62795=CARTESIAN_POINT('Ctrl Pts',(4.97788044704027,-1.5492013661897,64.6317854798331));
#62796=CARTESIAN_POINT('Ctrl Pts',(5.20476234479506,0.299612336584008,64.6847057339151));
#62797=CARTESIAN_POINT('Ctrl Pts',(4.6031097887974,1.82070851673316,64.7376259879971));
#62798=CARTESIAN_POINT('Ctrl Pts',(4.00145723279969,3.34180469688243,64.790546242079));
#62799=CARTESIAN_POINT('Ctrl Pts',(2.57127022304931,4.535183354407,64.843466496161));
#62800=CARTESIAN_POINT('Ctrl Pts',(0.967024178023638,4.85473618951069,64.896386750243));
#62801=CARTESIAN_POINT('Ctrl Pts',(-0.637221867001943,5.17428902461436,
64.9493070043249));
#62802=CARTESIAN_POINT('Ctrl Pts',(-2.41552694730285,4.62001603729727,65.0022272584069));
#62803=CARTESIAN_POINT('Ctrl Pts',(-3.55411149861537,3.44556101180013,65.0551475124888));
#62804=CARTESIAN_POINT('Ctrl Pts',(-4.43287447301319,2.53911309775405,65.0959915234403));
#62805=CARTESIAN_POINT('Ctrl Pts',(-4.93056880366583,1.26323522569467,65.1368355343917));
#62806=CARTESIAN_POINT('Ctrl Pts',(-4.94223974397651,-0.00450342756324047,
65.1776795453432));
#62807=CARTESIAN_POINT('Origin',(0.,0.,16.));
#62808=CARTESIAN_POINT('',(-4.94946148968121,0.00162189178913478,66.3223204546568));
#62809=CARTESIAN_POINT('',(-4.94905436241693,0.00206350582114702,66.1776795453432));
#62810=CARTESIAN_POINT('',(-4.942,-6.05220448138622E-16,16.));
#62811=CARTESIAN_POINT('Ctrl Pts',(-4.94946148968121,0.00162189178913478,
66.3223204546568));
#62812=CARTESIAN_POINT('Ctrl Pts',(-4.94984329083445,0.0908281755408331,
66.3194354636078));
#62813=CARTESIAN_POINT('Ctrl Pts',(-4.94764036946139,0.180015220631608,
66.3165504725587));
#62814=CARTESIAN_POINT('Ctrl Pts',(-4.9427933546869,0.26905833589981,66.3136654815097));
#62815=CARTESIAN_POINT('Ctrl Pts',(-4.8538831123176,1.90240284342791,66.2607452274277));
#62816=CARTESIAN_POINT('Ctrl Pts',(-3.87529724194047,3.48731832979629,66.2078249733457));
#62817=CARTESIAN_POINT('Ctrl Pts',(-2.45485158348742,4.2985232625058,66.1549047192638));
#62818=CARTESIAN_POINT('Ctrl Pts',(-1.03440592503428,5.10972819521536,66.1019844651818));
#62819=CARTESIAN_POINT('Ctrl Pts',(0.827899521494876,5.14722257426599,66.0490642110999));
#62820=CARTESIAN_POINT('Ctrl Pts',(2.27984534133793,4.39384839916376,65.9961439570179));
#62821=CARTESIAN_POINT('Ctrl Pts',(3.7317911611809,3.64047422406158,65.9432237029359));
#62822=CARTESIAN_POINT('Ctrl Pts',(4.77337735433786,2.09623149480659,65.8903034488539));
#62823=CARTESIAN_POINT('Ctrl Pts',(4.9279581709879,0.467789269060101,65.8373831947719));
#62824=CARTESIAN_POINT('Ctrl Pts',(5.08253898763794,-1.16065295668643,65.78446294069));
#62825=CARTESIAN_POINT('Ctrl Pts',(4.35011442778111,-2.87329467892442,65.7315426866081));
#62826=CARTESIAN_POINT('Ctrl Pts',(3.06585315610755,-3.88640488889663,65.6786224325261));
#62827=CARTESIAN_POINT('Ctrl Pts',(1.78159188443402,-4.89951509886881,65.6257021784442));
#62828=CARTESIAN_POINT('Ctrl Pts',(-0.0545060990562027,-5.21309379657515,
65.5727819243622));
#62829=CARTESIAN_POINT('Ctrl Pts',(-1.60221431494639,-4.6836425807522,65.5198616702802));
#62830=CARTESIAN_POINT('Ctrl Pts',(-3.14992253083658,-4.15419136492924,
65.4669414161983));
#62831=CARTESIAN_POINT('Ctrl Pts',(-4.40924097912677,-2.78171023557699,
65.4140211621163));
#62832=CARTESIAN_POINT('Ctrl Pts',(-4.80388630468793,-1.19426751897802,
65.3611009080343));
#62833=CARTESIAN_POINT('Ctrl Pts',(-4.90028622386234,-0.806503266718003,
65.3481740902418));
#62834=CARTESIAN_POINT('Ctrl Pts',(-4.9450930727896,-0.405912747537303,
65.3352472724493));
#62835=CARTESIAN_POINT('Ctrl Pts',(-4.94144181990917,-0.00451754960951789,
65.3223204546568));
#62836=CARTESIAN_POINT('Ctrl Pts',(-4.94223974397651,-0.00450342756324047,
65.1776795453432));
#62837=CARTESIAN_POINT('Ctrl Pts',(-4.94569046072715,-0.379332437889885,
65.1897557884737));
#62838=CARTESIAN_POINT('Ctrl Pts',(-4.90665339169033,-0.753449924055778,
65.2018320316042));
#62839=CARTESIAN_POINT('Ctrl Pts',(-4.82241576997234,-1.11709684994147,
65.2139082747347));
#62840=CARTESIAN_POINT('Ctrl Pts',(-4.45327146769261,-2.71066262250856,
65.2668285288167));
#62841=CARTESIAN_POINT('Ctrl Pts',(-3.21611884080908,-4.10315710396555,
65.3197487828986));
#62842=CARTESIAN_POINT('Ctrl Pts',(-1.67709782604308,-4.65735355244893,
65.3726690369806));
#62843=CARTESIAN_POINT('Ctrl Pts',(-0.138076811276997,-5.21155000093235,
65.4255892910626));
#62844=CARTESIAN_POINT('Ctrl Pts',(1.70281259137165,-4.92744841644198,65.4785095451446));
#62845=CARTESIAN_POINT('Ctrl Pts',(3.00315127590115,-3.9350580230386,65.5314297992265));
#62846=CARTESIAN_POINT('Ctrl Pts',(4.30348996043062,-2.94266762963524,65.5843500533085));
#62847=CARTESIAN_POINT('Ctrl Pts',(5.06327792684106,-1.24198842731896,65.6372703073904));
#62848=CARTESIAN_POINT('Ctrl Pts',(4.93482459769029,0.388722806969066,65.6901905614724));
#62849=CARTESIAN_POINT('Ctrl Pts',(4.80637126853953,2.019434041257,65.7431108155543));
#62850=CARTESIAN_POINT('Ctrl Pts',(3.78967664382766,3.58017730751661,65.7960310696363));
#62851=CARTESIAN_POINT('Ctrl Pts',(2.34999571149359,4.35673265034576,65.8489513237183));
#62852=CARTESIAN_POINT('Ctrl Pts',(0.910314779159406,5.13328799317498,65.9018715778003));
#62853=CARTESIAN_POINT('Ctrl Pts',(-0.952352460797159,5.1256554125735,65.9547918318822));
#62854=CARTESIAN_POINT('Ctrl Pts',(-2.38562103141592,4.33732769399468,66.0077120859641));
#62855=CARTESIAN_POINT('Ctrl Pts',(-3.81888960203473,3.54899997541583,66.0606323400461));
#62856=CARTESIAN_POINT('Ctrl Pts',(-4.82275950331579,1.97997711885965,66.1135525941282));
#62857=CARTESIAN_POINT('Ctrl Pts',(-4.93784453663019,0.348267946699855,
66.1664728482101));
#62858=CARTESIAN_POINT('Ctrl Pts',(-4.94596822597675,0.233087909497783,
66.1702084139211));
#62859=CARTESIAN_POINT('Ctrl Pts',(-4.94966332434242,0.117595522185004,
66.1739439796322));
#62860=CARTESIAN_POINT('Ctrl Pts',(-4.94905436241693,0.00206350582114702,
66.1776795453432));
#62861=CARTESIAN_POINT('Origin',(0.,0.,16.));
#62862=CARTESIAN_POINT('',(-4.93665814957204,0.00348993981812262,67.3223204546568));
#62863=CARTESIAN_POINT('',(-4.93610990017314,0.00319438934087567,67.1776795453432));
#62864=CARTESIAN_POINT('',(-4.942,-6.05220448138622E-16,16.));
#62865=CARTESIAN_POINT('Ctrl Pts',(-4.93665814957204,0.00348993981812262,
67.3223204546568));
#62866=CARTESIAN_POINT('Ctrl Pts',(-4.94045351450443,0.585476451976408,
67.3036236547662));
#62867=CARTESIAN_POINT('Ctrl Pts',(-4.84535018635696,1.16626258658175,67.2849268548756));
#62868=CARTESIAN_POINT('Ctrl Pts',(-4.64586699339373,1.70865983008581,67.266230054985));
#62869=CARTESIAN_POINT('Ctrl Pts',(-4.08124089061357,3.24388511502926,67.213309800903));
#62870=CARTESIAN_POINT('Ctrl Pts',(-2.68038427233572,4.47156102489275,67.1603895468211));
#62871=CARTESIAN_POINT('Ctrl Pts',(-1.08435052194541,4.82988431339829,67.1074692927391));
#62872=CARTESIAN_POINT('Ctrl Pts',(0.511683228444911,5.18820760190384,67.0545490386571));
#62873=CARTESIAN_POINT('Ctrl Pts',(2.3028941109477,4.67717826905144,67.0016287845752));
#62874=CARTESIAN_POINT('Ctrl Pts',(3.4695966691053,3.53065114235145,66.9487085304932));
#62875=CARTESIAN_POINT('Ctrl Pts',(4.6362992272629,2.38412401565146,66.8957882764113));
#62876=CARTESIAN_POINT('Ctrl Pts',(5.17849346107531,0.602099095103884,66.8428680223293));
#62877=CARTESIAN_POINT('Ctrl Pts',(4.84806300838071,-0.999941799318743,
66.7899477682473));
#62878=CARTESIAN_POINT('Ctrl Pts',(4.51763255568609,-2.60198269374146,66.7370275141654));
#62879=CARTESIAN_POINT('Ctrl Pts',(3.31457741648437,-4.02403956203921,66.6841072600834));
#62880=CARTESIAN_POINT('Ctrl Pts',(1.78943399637315,-4.61535746263258,66.6311870060014));
#62881=CARTESIAN_POINT('Ctrl Pts',(0.264290576262007,-5.20667536322592,
66.5782667519194));
#62882=CARTESIAN_POINT('Ctrl Pts',(-1.5829411247586,-4.96725429611497,66.5253464978375));
#62883=CARTESIAN_POINT('Ctrl Pts',(-2.90693966808815,-4.00665699821556,
66.4724262437555));
#62884=CARTESIAN_POINT('Ctrl Pts',(-4.15875934507,-3.09842744975845,66.4223909807226));
#62885=CARTESIAN_POINT('Ctrl Pts',(-4.94283979803511,-1.54550938030458,
66.3723557176897));
#62886=CARTESIAN_POINT('Ctrl Pts',(-4.94946148968121,0.00162189178913478,
66.3223204546568));
#62887=CARTESIAN_POINT('Ctrl Pts',(-4.94905436241693,0.00206350582114702,
66.1776795453432));
#62888=CARTESIAN_POINT('Ctrl Pts',(-4.94103640614155,-1.51909999692026,
66.2268642337141));
#62889=CARTESIAN_POINT('Ctrl Pts',(-4.18686966888732,-3.04713356331113,
66.276048922085));
#62890=CARTESIAN_POINT('Ctrl Pts',(-2.97080189349508,-3.95953726339747,
66.3252336104559));
#62891=CARTESIAN_POINT('Ctrl Pts',(-1.66237405169773,-4.94123781357185,
66.3781538645379));
#62892=CARTESIAN_POINT('Ctrl Pts',(0.180781797244686,-5.21024342615729,
66.4310741186199));
#62893=CARTESIAN_POINT('Ctrl Pts',(1.71520938689206,-4.643453024393,66.4839943727019));
#62894=CARTESIAN_POINT('Ctrl Pts',(3.24963697653938,-4.07666262262872,66.5369146267838));
#62895=CARTESIAN_POINT('Ctrl Pts',(4.47533630689159,-2.6740762065147,66.5898348808657));
#62896=CARTESIAN_POINT('Ctrl Pts',(4.83140864464272,-1.0775387413447,66.6427551349477));
#62897=CARTESIAN_POINT('Ctrl Pts',(5.18748098239386,0.518998723825342,66.6956753890297));
#62898=CARTESIAN_POINT('Ctrl Pts',(4.67392632754393,2.30948723805131,66.7485956431117));
#62899=CARTESIAN_POINT('Ctrl Pts',(3.52575513351784,3.47457191163166,66.8015158971936));
#62900=CARTESIAN_POINT('Ctrl Pts',(2.37758393949173,4.63965658521205,66.8544361512756));
#62901=CARTESIAN_POINT('Ctrl Pts',(0.59479620628932,5.17933741814667,66.9073564053575));
#62902=CARTESIAN_POINT('Ctrl Pts',(-1.0067771713956,4.84664821890178,66.9602766594395));
#62903=CARTESIAN_POINT('Ctrl Pts',(-2.60835054908043,4.5139590196569,67.0131969135215));
#62904=CARTESIAN_POINT('Ctrl Pts',(-4.02870957124789,3.3088997882326,67.0661171676034));
#62905=CARTESIAN_POINT('Ctrl Pts',(-4.61787625663849,1.78292403343541,67.1190374216854));
#62906=CARTESIAN_POINT('Ctrl Pts',(-4.83549920786993,1.2192680163841,67.138584796238));
#62907=CARTESIAN_POINT('Ctrl Pts',(-4.93971654397597,0.611827024271365,
67.1581321707906));
#62908=CARTESIAN_POINT('Ctrl Pts',(-4.93610990017314,0.00319438934087567,
67.1776795453432));
#62909=CARTESIAN_POINT('Origin',(0.,0.,16.));
#62910=CARTESIAN_POINT('',(-4.93685333923596,-0.0035819126635156,68.3223204546569));
#62911=CARTESIAN_POINT('',(-4.9374673003319,-0.00383358773467055,68.1776795453432));
#62912=CARTESIAN_POINT('',(-4.942,-6.05220448138622E-16,16.));
#62913=CARTESIAN_POINT('Ctrl Pts',(-4.93685333923596,-0.0035819126635156,
68.3223204546569));
#62914=CARTESIAN_POINT('Ctrl Pts',(-4.92964532583484,1.0704814894781,68.2878118459247));
#62915=CARTESIAN_POINT('Ctrl Pts',(-4.585217373837,2.14875374624117,68.2533032371925));
#62916=CARTESIAN_POINT('Ctrl Pts',(-3.93928885933925,2.99759934246388,68.2187946284603));
#62917=CARTESIAN_POINT('Ctrl Pts',(-2.94873310059188,4.29933610551658,68.1658743743783));
#62918=CARTESIAN_POINT('Ctrl Pts',(-1.24912700565894,5.06152146794402,68.1129541202964));
#62919=CARTESIAN_POINT('Ctrl Pts',(0.3817637188463,4.93536776727194,68.0600338662144));
#62920=CARTESIAN_POINT('Ctrl Pts',(2.01265444335154,4.80921406659986,68.0071136121325));
#62921=CARTESIAN_POINT('Ctrl Pts',(3.57482979742896,3.79472130282827,67.9541933580505));
#62922=CARTESIAN_POINT('Ctrl Pts',(4.35341448041909,2.35613685870146,67.9012731039685));
#62923=CARTESIAN_POINT('Ctrl Pts',(5.13199916340922,0.91755241457464,67.8483528498866));
#62924=CARTESIAN_POINT('Ctrl Pts',(5.12699317531198,-0.945123709907305,
67.7954325958046));
#62925=CARTESIAN_POINT('Ctrl Pts',(4.34068733273566,-2.37950247209,67.7425123417227));
#62926=CARTESIAN_POINT('Ctrl Pts',(3.55438149015938,-3.81388123427261,67.6895920876407));
#62927=CARTESIAN_POINT('Ctrl Pts',(1.98677579310383,-4.81996263415611,67.6366718335588));
#62928=CARTESIAN_POINT('Ctrl Pts',(0.355230550111662,-4.93734845757534,
67.5837515794768));
#62929=CARTESIAN_POINT('Ctrl Pts',(-1.27631469288069,-5.05473428099459,
67.5308313253949));
#62930=CARTESIAN_POINT('Ctrl Pts',(-2.9717994818098,-4.28342452794957,67.4779110713129));
#62931=CARTESIAN_POINT('Ctrl Pts',(-3.95534408263313,-2.97638232141527,
67.4249908172309));
#62932=CARTESIAN_POINT('Ctrl Pts',(-4.59140099837083,-2.13111995717548,
67.3907673630395));
#62933=CARTESIAN_POINT('Ctrl Pts',(-4.92971094477425,-1.06180405997696,
67.3565439088482));
#62934=CARTESIAN_POINT('Ctrl Pts',(-4.93665814957204,0.00348993981812262,
67.3223204546568));
#62935=CARTESIAN_POINT('Ctrl Pts',(-4.93610990017314,0.00319438934087567,
67.1776795453432));
#62936=CARTESIAN_POINT('Ctrl Pts',(-4.929952342348,-1.03591311578948,67.2110524248726));
#62937=CARTESIAN_POINT('Ctrl Pts',(-4.60950819503561,-2.07849403525122,
67.2444253044019));
#62938=CARTESIAN_POINT('Ctrl Pts',(-4.00255393693903,-2.91258668755472,
67.2777981839313));
#62939=CARTESIAN_POINT('Ctrl Pts',(-3.0400905832352,-4.23522937557753,67.3307184380133));
#62940=CARTESIAN_POINT('Ctrl Pts',(-1.35718952721374,-5.03362247345304,
67.3836386920952));
#62941=CARTESIAN_POINT('Ctrl Pts',(0.276028005448868,-4.94240910597606,
67.4365589461772));
#62942=CARTESIAN_POINT('Ctrl Pts',(1.90924553811157,-4.85119573849907,67.4894792002592));
#62943=CARTESIAN_POINT('Ctrl Pts',(3.49277954741543,-3.87037590566948,67.5423994543411));
#62944=CARTESIAN_POINT('Ctrl Pts',(4.30198068586489,-2.4487877427561,67.5953197084231));
#62945=CARTESIAN_POINT('Ctrl Pts',(5.11118182431431,-1.0271995798428,67.6482399625051));
#62946=CARTESIAN_POINT('Ctrl Pts',(5.14605009190941,0.835156913154248,67.7011602165871));
#62947=CARTESIAN_POINT('Ctrl Pts',(4.39062923686613,2.28603896182972,67.754080470669));
#62948=CARTESIAN_POINT('Ctrl Pts',(3.63520838182284,3.73692101050519,67.8070007247509));
#62949=CARTESIAN_POINT('Ctrl Pts',(2.08949840414118,4.77632861485907,67.8599209788329));
#62950=CARTESIAN_POINT('Ctrl Pts',(0.460839796771268,4.92861298057972,67.9128412329148));
#62951=CARTESIAN_POINT('Ctrl Pts',(-1.16781881059865,5.08089734630037,67.9657614869968));
#62952=CARTESIAN_POINT('Ctrl Pts',(-2.87942604765681,4.34605847338777,68.0186817410788));
#62953=CARTESIAN_POINT('Ctrl Pts',(-3.89072430186352,3.06036985305955,68.0716019951608));
#62954=CARTESIAN_POINT('Ctrl Pts',(-4.56643308401115,2.20132447426127,68.1069611785549));
#62955=CARTESIAN_POINT('Ctrl Pts',(-4.92949771464715,1.09635914283018,68.142320361949));
#62956=CARTESIAN_POINT('Ctrl Pts',(-4.9374673003319,-0.00383358773467055,
68.1776795453432));
#62957=CARTESIAN_POINT('Origin',(0.,0.,16.));
#62958=CARTESIAN_POINT('',(-4.94957828458471,-0.00146882823891858,69.3223204546568));
#62959=CARTESIAN_POINT('',(-4.94986277816997,-0.00100007488610477,69.1776795453432));
#62960=CARTESIAN_POINT('',(-4.942,-6.05220448138622E-16,16.));
#62961=CARTESIAN_POINT('Ctrl Pts',(-4.94957828458471,-0.00146882823891858,
69.3223204546568));
#62962=CARTESIAN_POINT('Ctrl Pts',(-4.94347825971363,1.5543817607618,69.2720000370831));
#62963=CARTESIAN_POINT('Ctrl Pts',(-4.14920711766337,3.115598423098,69.2216796195094));
#62964=CARTESIAN_POINT('Ctrl Pts',(-2.8853618522021,4.0222239516356,69.1713592019357));
#62965=CARTESIAN_POINT('Ctrl Pts',(-1.55621921401708,4.97569086707049,69.1184389478537));
#62966=CARTESIAN_POINT('Ctrl Pts',(0.292272693635941,5.20517958568956,69.0655186937718));
#62967=CARTESIAN_POINT('Ctrl Pts',(1.81421574235462,4.60567256494064,69.0125984396898));
#62968=CARTESIAN_POINT('Ctrl Pts',(3.3361587910733,4.00616554419172,68.9596781856078));
#62969=CARTESIAN_POINT('Ctrl Pts',(4.53155298085772,2.57766278407475,68.9067579315258));
#62970=CARTESIAN_POINT('Ctrl Pts',(4.85336767356702,0.973868964711821,68.8538376774439));
#62971=CARTESIAN_POINT('Ctrl Pts',(5.17518236627633,-0.629924854651203,
68.8009174233619));
#62972=CARTESIAN_POINT('Ctrl Pts',(4.62341756191056,-2.40900973326008,68.74799716928));
#62973=CARTESIAN_POINT('Ctrl Pts',(3.45056926188509,-3.5492492592361,68.695076915198));
#62974=CARTESIAN_POINT('Ctrl Pts',(2.27772096185968,-4.68948878521204,68.6421566611161));
#62975=CARTESIAN_POINT('Ctrl Pts',(0.483789166174606,-5.19088295855499,
68.5892364070341));
#62976=CARTESIAN_POINT('Ctrl Pts',(-1.11029553728448,-4.82398614790096,
68.5363161529521));
#62977=CARTESIAN_POINT('Ctrl Pts',(-2.70438024074366,-4.45708933724691,
68.4833958988701));
#62978=CARTESIAN_POINT('Ctrl Pts',(-4.09861785197692,-3.22190154259576,
68.4304756447882));
#62979=CARTESIAN_POINT('Ctrl Pts',(-4.65498394631264,-1.6836635634312,68.3775553907063));
#62980=CARTESIAN_POINT('Ctrl Pts',(-4.84855095371391,-1.14849054456963,
68.3591437453565));
#62981=CARTESIAN_POINT('Ctrl Pts',(-4.94069908646524,-0.576635280213381,
68.3407321000067));
#62982=CARTESIAN_POINT('Ctrl Pts',(-4.93685333923596,-0.0035819126635156,
68.3223204546569));
#62983=CARTESIAN_POINT('Ctrl Pts',(-4.9374673003319,-0.00383358773467055,
68.1776795453432));
#62984=CARTESIAN_POINT('Ctrl Pts',(-4.94142537979325,-0.550242199503817,
68.195240616031));
#62985=CARTESIAN_POINT('Ctrl Pts',(-4.85779595713247,-1.09547360479138,
68.2128016867188));
#62986=CARTESIAN_POINT('Ctrl Pts',(-4.68137867571166,-1.60881724419501,
68.2303627574066));
#62987=CARTESIAN_POINT('Ctrl Pts',(-4.14974552399779,-3.15577735337756,
68.2832830114886));
#62988=CARTESIAN_POINT('Ctrl Pts',(-2.77548994921469,-4.41315920399872,
68.3362032655706));
#62989=CARTESIAN_POINT('Ctrl Pts',(-1.18749229097476,-4.8055656575998,68.3891235196525));
#62990=CARTESIAN_POINT('Ctrl Pts',(0.400505367265077,-5.19797211120086,
68.4420437737345));
#62991=CARTESIAN_POINT('Ctrl Pts',(2.20224510896182,-4.72540316778197,68.4949640278164));
#62992=CARTESIAN_POINT('Ctrl Pts',(3.39322331088645,-3.60411359325479,68.5478842818984));
#62993=CARTESIAN_POINT('Ctrl Pts',(4.58420151281108,-2.48282401872761,68.6008045359804));
#62994=CARTESIAN_POINT('Ctrl Pts',(5.16441817496363,-0.71281381309235,68.6537247900624));
#62995=CARTESIAN_POINT('Ctrl Pts',(4.8683572912689,0.895933320719813,68.7066450441443));
#62996=CARTESIAN_POINT('Ctrl Pts',(4.57229640757415,2.50468045453207,68.7595652982263));
#62997=CARTESIAN_POINT('Ctrl Pts',(3.39995797803181,3.95216451652107,68.8124855523082));
#62998=CARTESIAN_POINT('Ctrl Pts',(1.88782197277238,4.57599469293234,68.8654058063902));
#62999=CARTESIAN_POINT('Ctrl Pts',(0.375685967513026,5.19982486934357,68.9183260604721));
#63000=CARTESIAN_POINT('Ctrl Pts',(-1.47624761346349,5.00000116017722,68.9712463145541));
#63001=CARTESIAN_POINT('Ctrl Pts',(-2.82050567947833,4.06796594659513,69.0241665686361));
#63002=CARTESIAN_POINT('Ctrl Pts',(-4.1203297308193,3.16673885490861,69.0753375608718));
#63003=CARTESIAN_POINT('Ctrl Pts',(-4.94548567424374,1.58090626393571,69.1265085531075));
#63004=CARTESIAN_POINT('Ctrl Pts',(-4.94986277816997,-0.00100007488610477,
69.1776795453432));
#63005=CARTESIAN_POINT('Origin',(0.,0.,16.));
#63006=CARTESIAN_POINT('',(-4.94117660785543,0.00451214175946527,70.3223204546568));
#63007=CARTESIAN_POINT('',(-4.94039592783718,0.00446617472429873,70.1776795453432));
#63008=CARTESIAN_POINT('',(-4.942,-6.05220448138622E-16,16.));
#63009=CARTESIAN_POINT('Ctrl Pts',(-4.94117660785543,0.00451214175946527,
70.3223204546568));
#63010=CARTESIAN_POINT('Ctrl Pts',(-4.94488654917412,0.414817947726635,
70.3091084823236));
#63011=CARTESIAN_POINT('Ctrl Pts',(-4.8980529188199,0.824288512579107,70.2958965099902));
#63012=CARTESIAN_POINT('Ctrl Pts',(-4.79739770972192,1.22007120694207,70.2826845376569));
#63013=CARTESIAN_POINT('Ctrl Pts',(-4.39422556359881,2.80536976937794,70.229764283575));
#63014=CARTESIAN_POINT('Ctrl Pts',(-3.12754820616573,4.17106222260404,70.176844029493));
#63015=CARTESIAN_POINT('Ctrl Pts',(-1.57701654176587,4.69218684221452,70.123923775411));
#63016=CARTESIAN_POINT('Ctrl Pts',(-0.0264848773660925,5.21331146182497,
70.071003521329));
#63017=CARTESIAN_POINT('Ctrl Pts',(1.80790109400033,4.88986824781988,70.0180832672471));
#63018=CARTESIAN_POINT('Ctrl Pts',(3.0866983358117,3.86986975477877,69.9651630131651));
#63019=CARTESIAN_POINT('Ctrl Pts',(4.36549557762306,2.84987126173766,69.9122427590831));
#63020=CARTESIAN_POINT('Ctrl Pts',(5.08870408987935,1.13331748966031,69.8593225050012));
#63021=CARTESIAN_POINT('Ctrl Pts',(4.9253726120261,-0.494270338941504,69.8064022509192));
#63022=CARTESIAN_POINT('Ctrl Pts',(4.76204113417285,-2.12185816754332,69.7534819968373));
#63023=CARTESIAN_POINT('Ctrl Pts',(3.71216966621028,-3.66048005266973,69.7005617427553));
#63024=CARTESIAN_POINT('Ctrl Pts',(2.25619542624873,-4.40603912077827,69.6476414886733));
#63025=CARTESIAN_POINT('Ctrl Pts',(0.80022118628726,-5.15159818888676,69.5947212345913));
#63026=CARTESIAN_POINT('Ctrl Pts',(-1.06185582567303,-5.10409443997744,
69.5418009805094));
#63027=CARTESIAN_POINT('Ctrl Pts',(-2.47792073001783,-4.28526631506165,
69.4888807264275));
#63028=CARTESIAN_POINT('Ctrl Pts',(-3.89398563436272,-3.46643819014582,
69.4359604723455));
#63029=CARTESIAN_POINT('Ctrl Pts',(-4.864038431092,-1.87628568922347,69.3830402182635));
#63030=CARTESIAN_POINT('Ctrl Pts',(-4.94416814509815,-0.242486882636884,
69.3301199641816));
#63031=CARTESIAN_POINT('Ctrl Pts',(-4.94810471266539,-0.162222532848887,
69.3275201276733));
#63032=CARTESIAN_POINT('Ctrl Pts',(-4.94989344626512,-0.081852842476203,
69.3249202911651));
#63033=CARTESIAN_POINT('Ctrl Pts',(-4.94957828458471,-0.00146882823891858,
69.3223204546568));
#63034=CARTESIAN_POINT('Ctrl Pts',(-4.94986277816997,-0.00100007488610477,
69.1776795453432));
#63035=CARTESIAN_POINT('Ctrl Pts',(-4.95001240788323,-0.0550769704471047,
69.1794288071895));
#63036=CARTESIAN_POINT('Ctrl Pts',(-4.94920288408253,-0.10914927783116,
69.1811780690357));
#63037=CARTESIAN_POINT('Ctrl Pts',(-4.94742038040276,-0.163189491703912,
69.182927330882));
#63038=CARTESIAN_POINT('Ctrl Pts',(-4.89349446425897,-1.79806299842275,
69.2358475849639));
#63039=CARTESIAN_POINT('Ctrl Pts',(-3.94906008091826,-3.40356329386249,
69.2887678390458));
#63040=CARTESIAN_POINT('Ctrl Pts',(-2.54630482825922,-4.24498892250744,
69.3416880931278));
#63041=CARTESIAN_POINT('Ctrl Pts',(-1.14354957560017,-5.0864145511524,69.3946083472098));
#63042=CARTESIAN_POINT('Ctrl Pts',(0.717526546377131,-5.16376551300254,
69.4475286012918));
#63043=CARTESIAN_POINT('Ctrl Pts',(2.18526668060081,-4.44164482655728,69.5004488553738));
#63044=CARTESIAN_POINT('Ctrl Pts',(3.65300681482441,-3.71952414011206,69.5533691094558));
#63045=CARTESIAN_POINT('Ctrl Pts',(4.72741096129446,-2.19793180537131,69.6062893635377));
#63046=CARTESIAN_POINT('Ctrl Pts',(4.91681537353513,-0.573171713534203,
69.6592096176196));
#63047=CARTESIAN_POINT('Ctrl Pts',(5.1062197857758,1.05158837830299,69.7121298717016));
#63048=CARTESIAN_POINT('Ctrl Pts',(4.41062446378718,2.77951622723674,69.7650501257836));
#63049=CARTESIAN_POINT('Ctrl Pts',(3.14834445052908,3.81988565947332,69.8179703798655));
#63050=CARTESIAN_POINT('Ctrl Pts',(1.88606443727098,4.8602550917099,69.8708906339475));
#63051=CARTESIAN_POINT('Ctrl Pts',(0.0570997327434936,5.21306610724925,
69.9238108880295));
#63052=CARTESIAN_POINT('Ctrl Pts',(-1.50158748103454,4.71686699700421,69.9767311421114));
#63053=CARTESIAN_POINT('Ctrl Pts',(-3.06027469481266,4.22066788675913,70.0296513961934));
#63054=CARTESIAN_POINT('Ctrl Pts',(-4.34868441784121,2.87545865072958,70.0825716502754));
#63055=CARTESIAN_POINT('Ctrl Pts',(-4.77722068336862,1.29682758029823,70.1354919043573));
#63056=CARTESIAN_POINT('Ctrl Pts',(-4.8910960129131,0.877336517731382,70.1495544513526));
#63057=CARTESIAN_POINT('Ctrl Pts',(-4.9442531721895,0.441362859310636,70.1636169983479));
#63058=CARTESIAN_POINT('Ctrl Pts',(-4.94039592783718,0.00446617472429873,
70.1776795453432));
#63059=CARTESIAN_POINT('Origin',(0.,0.,16.));
#63060=CARTESIAN_POINT('',(-4.93421645959303,-0.00129368103133631,71.3223204546568));
#63061=CARTESIAN_POINT('',(-4.93445704478049,-0.00170468936910681,71.1776795453431));
#63062=CARTESIAN_POINT('',(-4.942,-6.05220448138622E-16,16.));
#63063=CARTESIAN_POINT('Ctrl Pts',(-4.93421645959303,-0.00129368103133631,
71.3223204546568));
#63064=CARTESIAN_POINT('Ctrl Pts',(-4.93209641645617,0.903267203006942,
71.293296673482));
#63065=CARTESIAN_POINT('Ctrl Pts',(-4.69429817649842,1.80886543486343,71.2642728923071));
#63066=CARTESIAN_POINT('Ctrl Pts',(-4.22761420074216,2.5750488742813,71.2352491111322));
#63067=CARTESIAN_POINT('Ctrl Pts',(-3.37669011114097,3.97206265560444,71.1823288570503));
#63068=CARTESIAN_POINT('Ctrl Pts',(-1.76481870913523,4.90558179736215,71.1294086029683));
#63069=CARTESIAN_POINT('Ctrl Pts',(-0.129616965909283,4.94841368292938,
71.0764883488863));
#63070=CARTESIAN_POINT('Ctrl Pts',(1.50558477731675,4.9912455684966,71.0235680948044));
#63071=CARTESIAN_POINT('Ctrl Pts',(3.164116861763,4.14339019787323,70.9706478407224));
#63072=CARTESIAN_POINT('Ctrl Pts',(4.08700967532571,2.79283913769631,70.9177275866405));
#63073=CARTESIAN_POINT('Ctrl Pts',(5.00990248888837,1.44228807751946,70.8648073325585));
#63074=CARTESIAN_POINT('Ctrl Pts',(5.19715603156758,-0.410958672210887,
70.8118870784765));
#63075=CARTESIAN_POINT('Ctrl Pts',(4.56308022236637,-1.91882709473861,70.7589668243946));
#63076=CARTESIAN_POINT('Ctrl Pts',(3.92900441316517,-3.42669551726634,70.7060465703126));
#63077=CARTESIAN_POINT('Ctrl Pts',(2.47359925208355,-4.58918561259145,70.6531263162307));
#63078=CARTESIAN_POINT('Ctrl Pts',(0.86288036879719,-4.87432415873202,70.6002060621487));
#63079=CARTESIAN_POINT('Ctrl Pts',(-0.747838514489167,-5.1594627048726,
70.5472858080667));
#63080=CARTESIAN_POINT('Ctrl Pts',(-2.51387111998026,-4.56724970182864,
70.4943655539847));
#63081=CARTESIAN_POINT('Ctrl Pts',(-3.62705395531922,-3.36869086448392,
70.4414452999028));
#63082=CARTESIAN_POINT('Ctrl Pts',(-4.46232163175454,-2.46936200011537,
70.4017370181541));
#63083=CARTESIAN_POINT('Ctrl Pts',(-4.93002646377116,-1.22865260726002,
70.3620287364055));
#63084=CARTESIAN_POINT('Ctrl Pts',(-4.94117660785543,0.00451214175946527,
70.3223204546568));
#63085=CARTESIAN_POINT('Ctrl Pts',(-4.94039592783718,0.00446617472429873,
70.1776795453432));
#63086=CARTESIAN_POINT('Ctrl Pts',(-4.92973756905946,-1.20276914349332,
70.2165372524299));
#63087=CARTESIAN_POINT('Ctrl Pts',(-4.48375687255021,-2.4170520476298,70.2553949595166));
#63088=CARTESIAN_POINT('Ctrl Pts',(-3.68059559417778,-3.31010805001079,
70.2942526666032));
#63089=CARTESIAN_POINT('Ctrl Pts',(-2.58677143143322,-4.52635970505561,
70.3471729206852));
#63090=CARTESIAN_POINT('Ctrl Pts',(-0.83046029791784,-5.14681011031225,
70.4000931747671));
#63091=CARTESIAN_POINT('Ctrl Pts',(0.784623008060776,-4.88753168438311,
70.453013428849));
#63092=CARTESIAN_POINT('Ctrl Pts',(2.3997063140393,-4.62825325845398,70.505933682931));
#63093=CARTESIAN_POINT('Ctrl Pts',(3.87356179248119,-3.48924600133894,70.558853937013));
#63094=CARTESIAN_POINT('Ctrl Pts',(4.53173066670028,-1.99173702960891,70.611774191095));
#63095=CARTESIAN_POINT('Ctrl Pts',(5.18989954091941,-0.494228057878804,
70.664694445177));
#63096=CARTESIAN_POINT('Ctrl Pts',(5.0323818109159,1.36178262846646,70.7176146992589));
#63097=CARTESIAN_POINT('Ctrl Pts',(4.13125999566019,2.72695619306305,70.7705349533408));
#63098=CARTESIAN_POINT('Ctrl Pts',(3.23013818040442,4.09212975765972,70.8234552074228));
#63099=CARTESIAN_POINT('Ctrl Pts',(1.58541227989642,4.96646620050757,70.8763754615048));
#63100=CARTESIAN_POINT('Ctrl Pts',(-0.0502660143879759,4.94985581188227,
70.9292957155868));
#63101=CARTESIAN_POINT('Ctrl Pts',(-1.68594430867228,4.93324542325696,70.9822159696687));
#63102=CARTESIAN_POINT('Ctrl Pts',(-3.3125749967329,4.02568820315859,71.0351362237507));
#63103=CARTESIAN_POINT('Ctrl Pts',(-4.18578703267271,2.64249619635225,71.0880564778327));
#63104=CARTESIAN_POINT('Ctrl Pts',(-4.67872962214464,1.86166150614078,71.1179308336695));
#63105=CARTESIAN_POINT('Ctrl Pts',(-4.93157361279594,0.929252063276933,
71.1478051895063));
#63106=CARTESIAN_POINT('Ctrl Pts',(-4.93445704478049,-0.00170468936910681,
71.1776795453431));
#63107=CARTESIAN_POINT('Origin',(0.,0.,16.));
#63108=CARTESIAN_POINT('',(-4.9459185577707,-0.00382965742011687,72.3223204546568));
#63109=CARTESIAN_POINT('',(-4.9466376895248,-0.00356105100536129,72.1776795453432));
#63110=CARTESIAN_POINT('',(-4.942,-6.05220448138622E-16,16.));
#63111=CARTESIAN_POINT('Ctrl Pts',(-4.9459185577707,-0.00382965742011687,
72.3223204546568));
#63112=CARTESIAN_POINT('Ctrl Pts',(-4.93404671791329,1.38513423103216,72.2774848646404));
#63113=CARTESIAN_POINT('Ctrl Pts',(-4.32176677967432,2.78326338156107,72.232649274624));
#63114=CARTESIAN_POINT('Ctrl Pts',(-3.28505857961465,3.70297024883463,72.1878136846076));
#63115=CARTESIAN_POINT('Ctrl Pts',(-2.06141322698447,4.78851682197505,72.1348934305256));
#63116=CARTESIAN_POINT('Ctrl Pts',(-0.246475391513582,5.20754910952386,
72.0819731764437));
#63117=CARTESIAN_POINT('Ctrl Pts',(1.32921165428745,4.76831153694478,72.0290529223617));
#63118=CARTESIAN_POINT('Ctrl Pts',(2.90489870008848,4.32907396436569,71.9761326682797));
#63119=CARTESIAN_POINT('Ctrl Pts',(4.24133495621976,3.03156653165866,71.9232124141978));
#63120=CARTESIAN_POINT('Ctrl Pts',(4.72694678088706,1.46954845647079,71.8702921601158));
#63121=CARTESIAN_POINT('Ctrl Pts',(5.21255860555439,-0.09246961871717,71.8173719060338));
#63122=CARTESIAN_POINT('Ctrl Pts',(4.84734599875778,-1.91899833638585,71.7644516519519));
#63123=CARTESIAN_POINT('Ctrl Pts',(3.79843582714949,-3.17419025930731,71.7115313978699));
#63124=CARTESIAN_POINT('Ctrl Pts',(2.74952565554119,-4.42938218222877,71.658611143788));
#63125=CARTESIAN_POINT('Ctrl Pts',(1.0169179191211,-5.1132373104028,71.605690889706));
#63126=CARTESIAN_POINT('Ctrl Pts',(-0.60651962032857,-4.91281309286346,
71.552770635624));
#63127=CARTESIAN_POINT('Ctrl Pts',(-2.22995715977815,-4.71238887532414,
71.4998503815421));
#63128=CARTESIAN_POINT('Ctrl Pts',(-3.74422450225742,-3.62768531207155,
71.4469301274601));
#63129=CARTESIAN_POINT('Ctrl Pts',(-4.45636978489872,-2.15507932000099,
71.3940098733781));
#63130=CARTESIAN_POINT('Ctrl Pts',(-4.77794345735694,-1.49011484084619,
71.370113400471));
#63131=CARTESIAN_POINT('Ctrl Pts',(-4.93596197831358,-0.746055865118146,
71.3462169275639));
#63132=CARTESIAN_POINT('Ctrl Pts',(-4.93421645959303,-0.00129368103133631,
71.3223204546568));
#63133=CARTESIAN_POINT('Ctrl Pts',(-4.93445704478049,-0.00170468936910681,
71.1776795453431));
#63134=CARTESIAN_POINT('Ctrl Pts',(-4.93668140337337,-0.71987028628676,
71.2007254435883));
#63135=CARTESIAN_POINT('Ctrl Pts',(-4.79015415455198,-1.43717138679696,
71.2237713418334));
#63136=CARTESIAN_POINT('Ctrl Pts',(-4.49034790212576,-2.08335665417659,
71.2468172400785));
#63137=CARTESIAN_POINT('Ctrl Pts',(-3.80190335182005,-3.56719070438483,
71.2997374941605));
#63138=CARTESIAN_POINT('Ctrl Pts',(-2.30522086738965,-4.67603201128707,
71.3526577482425));
#63139=CARTESIAN_POINT('Ctrl Pts',(-0.685205212090817,-4.90245785784546,
71.4055780023244));
#63140=CARTESIAN_POINT('Ctrl Pts',(0.934810443208014,-5.12888370440385,
71.4584982564064));
#63141=CARTESIAN_POINT('Ctrl Pts',(2.67815926937537,-4.47289409061839,71.5114185104883));
#63142=CARTESIAN_POINT('Ctrl Pts',(3.74705821791536,-3.23467988248916,71.5643387645703));
#63143=CARTESIAN_POINT('Ctrl Pts',(4.8159571664554,-1.99646567435987,71.6172590186523));
#63144=CARTESIAN_POINT('Ctrl Pts',(5.21040623736806,-0.176026871886955,
71.6701792727342));
#63145=CARTESIAN_POINT('Ctrl Pts',(4.74989951150191,1.39357592590467,71.7230995268162));
#63146=CARTESIAN_POINT('Ctrl Pts',(4.28939278563578,2.96317872369621,71.7760197808982));
#63147=CARTESIAN_POINT('Ctrl Pts',(2.97393026299076,4.28194551680631,71.8289400349801));
#63148=CARTESIAN_POINT('Ctrl Pts',(1.40548768459228,4.74638847957966,71.8818602890621));
#63149=CARTESIAN_POINT('Ctrl Pts',(-0.162954893806299,5.21083144235304,
71.934780543144));
#63150=CARTESIAN_POINT('Ctrl Pts',(-1.98437752795848,4.82095057478956,71.987700797226));
#63151=CARTESIAN_POINT('Ctrl Pts',(-3.22526940243671,3.7551613164194,72.040621051308));
#63152=CARTESIAN_POINT('Ctrl Pts',(-4.29653392126676,2.83506324782479,72.0863072159864));
#63153=CARTESIAN_POINT('Ctrl Pts',(-4.93513440489649,1.41121710573191,72.1319933806648));
#63154=CARTESIAN_POINT('Ctrl Pts',(-4.9466376895248,-0.00356105100536129,
72.1776795453432));
#63155=CARTESIAN_POINT('Origin',(0.,0.,16.));
#63156=CARTESIAN_POINT('',(-4.94622533435752,0.00372181280100414,73.3223204546568));
#63157=CARTESIAN_POINT('',(-4.94548609638219,0.00396606047658106,73.1776795453432));
#63158=CARTESIAN_POINT('',(-4.942,-6.05220448138622E-16,16.));
#63159=CARTESIAN_POINT('Ctrl Pts',(-4.94622533435752,0.00372181280100414,
73.3223204546568));
#63160=CARTESIAN_POINT('Ctrl Pts',(-4.94823216917571,0.243062776937041,
73.3145933098808));
#63161=CARTESIAN_POINT('Ctrl Pts',(-4.93236152324834,0.482136497176127,
73.3068661651048));
#63162=CARTESIAN_POINT('Ctrl Pts',(-4.89769574881769,0.718453121134063,
73.2991390203288));
#63163=CARTESIAN_POINT('Ctrl Pts',(-4.66028314118601,2.33689513900433,73.2462187662469));
#63164=CARTESIAN_POINT('Ctrl Pts',(-3.5413122266531,3.82601954517773,73.1932985121649));
#63165=CARTESIAN_POINT('Ctrl Pts',(-2.05284118541496,4.50438026844074,73.1403782580829));
#63166=CARTESIAN_POINT('Ctrl Pts',(-0.564370144176819,5.18274099170376,
73.087458004001));
#63167=CARTESIAN_POINT('Ctrl Pts',(1.29360102376645,5.05033803205637,73.034537749919));
#63168=CARTESIAN_POINT('Ctrl Pts',(2.67083633572998,4.16776100598374,72.9816174958371));
#63169=CARTESIAN_POINT('Ctrl Pts',(4.04807164769343,3.28518397991116,72.9286972417551));
#63170=CARTESIAN_POINT('Ctrl Pts',(4.9445711036771,1.6524328874135,72.8757769876731));
#63171=CARTESIAN_POINT('Ctrl Pts',(4.95008286065676,0.0166795649332413,
72.8228567335911));
#63172=CARTESIAN_POINT('Ctrl Pts',(4.95559461763642,-1.61907375754711,72.7699364795092));
#63173=CARTESIAN_POINT('Ctrl Pts',(4.07011867561174,-3.25782931001015,72.7170162254272));
#63174=CARTESIAN_POINT('Ctrl Pts',(2.69886234926083,-4.14966752342842,72.6640959713453));
#63175=CARTESIAN_POINT('Ctrl Pts',(1.32760602290984,-5.04150573684673,72.6111757172633));
#63176=CARTESIAN_POINT('Ctrl Pts',(-0.529430687767451,-5.18642661122039,
72.5582554631813));
#63177=CARTESIAN_POINT('Ctrl Pts',(-2.02243942200268,-4.51811214110315,
72.5053352090994));
#63178=CARTESIAN_POINT('Ctrl Pts',(-3.51544815623782,-3.84979767098594,
72.4524149550174));
#63179=CARTESIAN_POINT('Ctrl Pts',(-4.64442891403086,-2.36824785637795,
72.3994947009354));
#63180=CARTESIAN_POINT('Ctrl Pts',(-4.89274285803262,-0.751442519707904,
72.3465744468535));
#63181=CARTESIAN_POINT('Ctrl Pts',(-4.93067795216383,-0.50444204261031,
72.3384897827879));
#63182=CARTESIAN_POINT('Ctrl Pts',(-4.9480592642285,-0.254284852349217,
72.3304051187224));
#63183=CARTESIAN_POINT('Ctrl Pts',(-4.9459185577707,-0.00382965742011687,
72.3223204546568));
#63184=CARTESIAN_POINT('Ctrl Pts',(-4.9466376895248,-0.00356105100536129,
72.1776795453432));
#63185=CARTESIAN_POINT('Ctrl Pts',(-4.94845915538918,-0.227581424440414,
72.1849136347467));
#63186=CARTESIAN_POINT('Ctrl Pts',(-4.93455770132463,-0.451374440445247,
72.1921477241503));
#63187=CARTESIAN_POINT('Ctrl Pts',(-4.90416141521875,-0.672904186423828,
72.1993818135539));
#63188=CARTESIAN_POINT('Ctrl Pts',(-4.68180043871832,-2.29348278172022,
72.2523020676359));
#63189=CARTESIAN_POINT('Ctrl Pts',(-3.57671737091314,-3.79294232313627,
72.3052223217178));
#63190=CARTESIAN_POINT('Ctrl Pts',(-2.09461510123176,-4.48510722372598,
72.3581425757998));
#63191=CARTESIAN_POINT('Ctrl Pts',(-0.612512831550301,-5.17727212431573,
72.4110628298817));
#63192=CARTESIAN_POINT('Ctrl Pts',(1.24660864000739,-5.06214238407903,72.4639830839637));
#63193=CARTESIAN_POINT('Ctrl Pts',(2.63198693425408,-4.19240313049007,72.5169033380457));
#63194=CARTESIAN_POINT('Ctrl Pts',(4.01736522850069,-3.32266387690115,72.5698235921276));
#63195=CARTESIAN_POINT('Ctrl Pts',(4.92900034543634,-1.69831510996005,72.6227438462096));
#63196=CARTESIAN_POINT('Ctrl Pts',(4.94971413242267,-0.0626836336085702,
72.6756641002916));
#63197=CARTESIAN_POINT('Ctrl Pts',(4.97042791940901,1.57294784274291,72.7285843543735));
#63198=CARTESIAN_POINT('Ctrl Pts',(4.10022037644603,3.21986202850478,72.7815046084555));
#63199=CARTESIAN_POINT('Ctrl Pts',(2.73731176561134,4.12440583944801,72.8344248625374));
#63200=CARTESIAN_POINT('Ctrl Pts',(1.37440315477665,5.02894965039124,72.8873451166194));
#63201=CARTESIAN_POINT('Ctrl Pts',(-0.481206523929751,5.19112308651582,
72.9402653707013));
#63202=CARTESIAN_POINT('Ctrl Pts',(-1.98036194136401,4.53671310662511,72.9931856247833));
#63203=CARTESIAN_POINT('Ctrl Pts',(-3.47951735879827,3.8823031267344,73.0461058788653));
#63204=CARTESIAN_POINT('Ctrl Pts',(-4.62221851496038,2.41130973082838,73.0990261329473));
#63205=CARTESIAN_POINT('Ctrl Pts',(-4.88554790865992,0.796881962912803,
73.1519463870292));
#63206=CARTESIAN_POINT('Ctrl Pts',(-4.92823035034716,0.535203165516849,
73.1605241064672));
#63207=CARTESIAN_POINT('Ctrl Pts',(-4.94780958080646,0.269756002185876,
73.1691018259052));
#63208=CARTESIAN_POINT('Ctrl Pts',(-4.94548609638219,0.00396606047658106,
73.1776795453432));
#63209=CARTESIAN_POINT('Origin',(0.,0.,16.));
#63210=CARTESIAN_POINT('',(-4.93430944804537,0.00146807591443893,74.3223204546568));
#63211=CARTESIAN_POINT('',(-4.93410780896188,0.00104985362950368,74.1776795453432));
#63212=CARTESIAN_POINT('',(-4.942,-6.05220448138622E-16,16.));
#63213=CARTESIAN_POINT('Ctrl Pts',(-4.93430944804537,0.00146807591443893,
74.3223204546568));
#63214=CARTESIAN_POINT('Ctrl Pts',(-4.93626271862051,0.735053226945857,
74.2987815010393));
#63215=CARTESIAN_POINT('Ctrl Pts',(-4.78313292282981,1.46786315098495,74.2752425474217));
#63216=CARTESIAN_POINT('Ctrl Pts',(-4.47079173349639,2.12499877904777,74.2517035938041));
#63217=CARTESIAN_POINT('Ctrl Pts',(-3.76858655614047,3.60237049949084,74.1987833397222));
#63218=CARTESIAN_POINT('Ctrl Pts',(-2.2616634474919,4.69725412310252,74.1458630856402));
#63219=CARTESIAN_POINT('Ctrl Pts',(-0.639613436851163,4.9086141818902,74.0929428315583));
#63220=CARTESIAN_POINT('Ctrl Pts',(0.982436573789575,5.11997424067789,74.0400225774763));
#63221=CARTESIAN_POINT('Ctrl Pts',(2.71961348642258,4.44781073464159,73.9871023233943));
#63222=CARTESIAN_POINT('Ctrl Pts',(3.77695861444706,3.19971594989436,73.9341820693124));
#63223=CARTESIAN_POINT('Ctrl Pts',(4.83430374247159,1.95162116514706,73.8812618152304));
#63224=CARTESIAN_POINT('Ctrl Pts',(5.21181708588759,0.127595101688968,73.8283415611484));
#63225=CARTESIAN_POINT('Ctrl Pts',(4.73674277310034,-1.43766005604103,73.7754213070665));
#63226=CARTESIAN_POINT('Ctrl Pts',(4.26166846031312,-3.00291521377094,73.7225010529845));
#63227=CARTESIAN_POINT('Ctrl Pts',(2.9340064913226,-4.30939946577263,73.6695807989026));
#63228=CARTESIAN_POINT('Ctrl Pts',(1.36131526012037,-4.7592456647895,73.6166605448206));
#63229=CARTESIAN_POINT('Ctrl Pts',(-0.211375971081961,-5.2090918638064,
73.5637402907386));
#63230=CARTESIAN_POINT('Ctrl Pts',(-2.02909646449615,-4.80230000983842,
73.5108200366566));
#63231=CARTESIAN_POINT('Ctrl Pts',(-3.260029560838,-3.72502426807083,73.4578997825747));
#63232=CARTESIAN_POINT('Ctrl Pts',(-4.31122810355742,-2.80504681907828,
73.4127066732687));
#63233=CARTESIAN_POINT('Ctrl Pts',(-4.9344881263814,-1.3960917881023,73.3675135639628));
#63234=CARTESIAN_POINT('Ctrl Pts',(-4.94622533435752,0.00372181280100414,
73.3223204546568));
#63235=CARTESIAN_POINT('Ctrl Pts',(-4.94548609638219,0.00396606047658106,
73.1776795453432));
#63236=CARTESIAN_POINT('Ctrl Pts',(-4.9334748398561,-1.37003547728531,73.2220220799872));
#63237=CARTESIAN_POINT('Ctrl Pts',(-4.33614096919029,-2.75319733775313,
73.2663646146311));
#63238=CARTESIAN_POINT('Ctrl Pts',(-3.3193311989464,-3.67227989433378,73.3107071492751));
#63239=CARTESIAN_POINT('Ctrl Pts',(-2.10582746429627,-4.76915184373973,
73.3636274033571));
#63240=CARTESIAN_POINT('Ctrl Pts',(-0.29486236375909,-5.2050336026263,73.416547657439));
#63241=CARTESIAN_POINT('Ctrl Pts',(1.28483881433472,-4.78045902103617,73.469467911521));
#63242=CARTESIAN_POINT('Ctrl Pts',(2.86453999242835,-4.35588443944609,73.522388165603));
#63243=CARTESIAN_POINT('Ctrl Pts',(4.21297724807857,-3.07085351737952,73.5753084196849));
#63244=CARTESIAN_POINT('Ctrl Pts',(4.71308509882384,-1.51341603066432,73.6282286737669));
#63245=CARTESIAN_POINT('Ctrl Pts',(5.21319294956918,0.0440214560510618,
73.6811489278489));
#63246=CARTESIAN_POINT('Ctrl Pts',(4.8649713954092,1.87386550741532,73.7340691819308));
#63247=CARTESIAN_POINT('Ctrl Pts',(3.82777193781054,3.13875153886656,73.7869894360128));
#63248=CARTESIAN_POINT('Ctrl Pts',(2.790572480212,4.40363757031766,73.8399096900947));
#63249=CARTESIAN_POINT('Ctrl Pts',(1.06439511917504,5.10356558185611,73.8928299441767));
#63250=CARTESIAN_POINT('Ctrl Pts',(-0.560835021503018,4.91823782561222,
73.9457501982587));
#63251=CARTESIAN_POINT('Ctrl Pts',(-2.18606516218117,4.73291006936832,73.9986704523406));
#63252=CARTESIAN_POINT('Ctrl Pts',(-3.71034808250029,3.662326545342,74.0515907064226));
#63253=CARTESIAN_POINT('Ctrl Pts',(-4.43614863820842,2.1964026248274,74.1045109605045));
#63254=CARTESIAN_POINT('Ctrl Pts',(-4.77065068257367,1.52079753684611,74.1289004887841));
#63255=CARTESIAN_POINT('Ctrl Pts',(-4.9355517737741,0.761220515306077,74.1532900170636));
#63256=CARTESIAN_POINT('Ctrl Pts',(-4.93410780896188,0.00104985362950368,
74.1776795453432));
#63257=CARTESIAN_POINT('Origin',(0.,0.,16.));
#63258=CARTESIAN_POINT('',(-4.94084634488987,-0.00449823523784309,75.3223204546568));
#63259=CARTESIAN_POINT('',(-4.94163609422309,-0.00451829382380276,75.1776795453432));
#63260=CARTESIAN_POINT('',(-4.942,-6.05220448138622E-16,16.));
#63261=CARTESIAN_POINT('Ctrl Pts',(-4.94084634488987,-0.00449823523784309,
75.3223204546568));
#63262=CARTESIAN_POINT('Ctrl Pts',(-4.92989311437387,1.21777170867941,75.2829696921977));
#63263=CARTESIAN_POINT('Ctrl Pts',(-4.47139568953686,2.44738194782565,75.2436189297386));
#63264=CARTESIAN_POINT('Ctrl Pts',(-3.64967329880456,3.34417154871685,75.2042681672795));
#63265=CARTESIAN_POINT('Ctrl Pts',(-2.54459286363954,4.55020494099322,75.1513479131975));
#63266=CARTESIAN_POINT('Ctrl Pts',(-0.782591300857919,5.15430584099797,
75.0984276591155));
#63267=CARTESIAN_POINT('Ctrl Pts',(0.83001256389233,4.88002845063787,75.0455074050336));
#63268=CARTESIAN_POINT('Ctrl Pts',(2.44261642864267,4.60575106027776,74.9925871509516));
#63269=CARTESIAN_POINT('Ctrl Pts',(3.90582259536151,3.45309537955268,74.9396668968697));
#63270=CARTESIAN_POINT('Ctrl Pts',(4.55004557505128,1.94953425212549,74.8867466427877));
#63271=CARTESIAN_POINT('Ctrl Pts',(5.19426855474108,0.445973124698207,74.8338263887057));
#63272=CARTESIAN_POINT('Ctrl Pts',(5.01950834740155,-1.40849344943142,74.7809061346238));
#63273=CARTESIAN_POINT('Ctrl Pts',(4.10573789297132,-2.76523324323168,74.7279858805418));
#63274=CARTESIAN_POINT('Ctrl Pts',(3.19196743854115,-4.12197303703186,74.6750656264599));
#63275=CARTESIAN_POINT('Ctrl Pts',(1.53918673702048,-4.98098605050295,74.6221453723779));
#63276=CARTESIAN_POINT('Ctrl Pts',(-0.0962665201530125,-4.94917480923354,
74.5692251182959));
#63277=CARTESIAN_POINT('Ctrl Pts',(-1.73171977732641,-4.91736356796412,
74.516304864214));
#63278=CARTESIAN_POINT('Ctrl Pts',(-3.34984559015253,-3.99472807195434,
74.463384610132));
#63279=CARTESIAN_POINT('Ctrl Pts',(-4.21016487353403,-2.60348041531225,
74.4104643560501));
#63280=CARTESIAN_POINT('Ctrl Pts',(-4.68781373971693,-1.8310603631163,74.3810830555857));
#63281=CARTESIAN_POINT('Ctrl Pts',(-4.93187137749265,-0.914192241399431,
74.3517017551212));
#63282=CARTESIAN_POINT('Ctrl Pts',(-4.93430944804537,0.00146807591443893,
74.3223204546568));
#63283=CARTESIAN_POINT('Ctrl Pts',(-4.93410780896188,0.00104985362950368,
74.1776795453432));
#63284=CARTESIAN_POINT('Ctrl Pts',(-4.93241866747241,-0.888193286408816,
74.2062102711456));
#63285=CARTESIAN_POINT('Ctrl Pts',(-4.70309992547236,-1.77824877440845,
74.234740996948));
#63286=CARTESIAN_POINT('Ctrl Pts',(-4.25136351730091,-2.53564734819139,
74.2632717227504));
#63287=CARTESIAN_POINT('Ctrl Pts',(-3.41345964958825,-3.94050908369249,
74.3161919768324));
#63288=CARTESIAN_POINT('Ctrl Pts',(-1.8103337230659,-4.88896823769192,74.3691122309144));
#63289=CARTESIAN_POINT('Ctrl Pts',(-0.175600645770052,-4.94699541578848,
74.4220324849964));
#63290=CARTESIAN_POINT('Ctrl Pts',(1.45913243152579,-5.00502259388504,74.4749527390783));
#63291=CARTESIAN_POINT('Ctrl Pts',(3.12547265959522,-4.17261779607872,74.5278729931603));
#63292=CARTESIAN_POINT('Ctrl Pts',(4.06087730056111,-2.83070217091354,74.5807932472422));
#63293=CARTESIAN_POINT('Ctrl Pts',(4.99628194152704,-1.48878654574829,74.6337135013242));
#63294=CARTESIAN_POINT('Ctrl Pts',(5.20075099538943,0.36263990677569,74.6866337554061));
#63295=CARTESIAN_POINT('Ctrl Pts',(4.58071630030657,1.87633616570506,74.7395540094881));
#63296=CARTESIAN_POINT('Ctrl Pts',(3.96068160522376,3.39003242463435,74.7924742635701));
#63297=CARTESIAN_POINT('Ctrl Pts',(2.51614316119567,4.56599848996891,74.8453945176521));
#63298=CARTESIAN_POINT('Ctrl Pts',(0.908143822210297,4.86609433003599,74.898314771734));
#63299=CARTESIAN_POINT('Ctrl Pts',(-0.699855516775171,5.16619017010308,
74.951235025816));
#63300=CARTESIAN_POINT('Ctrl Pts',(-2.47131575071806,4.59041578490263,75.0041552798979));
#63301=CARTESIAN_POINT('Ctrl Pts',(-3.59558962158726,3.4022543267312,75.0570755339799));
#63302=CARTESIAN_POINT('Ctrl Pts',(-4.44965416990239,2.49965701001681,75.097276871101));
#63303=CARTESIAN_POINT('Ctrl Pts',(-4.93023943833446,1.2436624400959,75.1374782082221));
#63304=CARTESIAN_POINT('Ctrl Pts',(-4.94163609422309,-0.00451829382380276,
75.1776795453432));
#63305=CARTESIAN_POINT('Origin',(0.,0.,16.));
#63306=CARTESIAN_POINT('',(-4.949709811623,0.00127385101247733,76.3223204546568));
#63307=CARTESIAN_POINT('',(-4.94936999019276,0.00173199160742904,76.1776795453431));
#63308=CARTESIAN_POINT('',(-4.942,-6.05220448138622E-16,16.));
#63309=CARTESIAN_POINT('Ctrl Pts',(-4.949709811623,0.00127385101247733,
76.3223204546568));
#63310=CARTESIAN_POINT('Ctrl Pts',(-4.94994903879905,0.0705988515890139,
76.3200781374381));
#63311=CARTESIAN_POINT('Ctrl Pts',(-4.94861862980554,0.139914463982202,
76.3178358202194));
#63312=CARTESIAN_POINT('Ctrl Pts',(-4.94569000143091,0.209162484687126,
76.3155935030007));
#63313=CARTESIAN_POINT('Ctrl Pts',(-4.87657232423312,1.84346418821971,76.2626732489188));
#63314=CARTESIAN_POINT('Ctrl Pts',(-3.91725763853945,3.44011779449909,76.2097529948368));
#63315=CARTESIAN_POINT('Ctrl Pts',(-2.50674299584768,4.26847022808205,76.1568327407548));
#63316=CARTESIAN_POINT('Ctrl Pts',(-1.09622835315598,5.09682266166495,76.1039124866729));
#63317=CARTESIAN_POINT('Ctrl Pts',(0.765486246533761,5.15687392255156,76.0509922325909));
#63318=CARTESIAN_POINT('Ctrl Pts',(2.22645176899709,4.4211436366153,75.9980719785089));
#63319=CARTESIAN_POINT('Ctrl Pts',(3.68741729146043,3.68541335067904,75.9451517244269));
#63320=CARTESIAN_POINT('Ctrl Pts',(4.74763373669735,2.15390151791992,75.892231470345));
#63321=CARTESIAN_POINT('Ctrl Pts',(4.92192986700097,0.527451343327534,75.8393112162631));
#63322=CARTESIAN_POINT('Ctrl Pts',(5.09622599730458,-1.09899883126485,75.7863909621811));
#63323=CARTESIAN_POINT('Ctrl Pts',(4.38460181267489,-2.8203873476905,75.7334707080991));
#63324=CARTESIAN_POINT('Ctrl Pts',(3.1127074084203,-3.84898053058463,75.6805504540171));
#63325=CARTESIAN_POINT('Ctrl Pts',(1.84081300416571,-4.87757371347876,75.6276301999351));
#63326=CARTESIAN_POINT('Ctrl Pts',(0.00864838028622472,-5.21337156284137,
75.5747099458532));
#63327=CARTESIAN_POINT('Ctrl Pts',(-1.54535994923236,-4.70270785426469,
75.5217896917713));
#63328=CARTESIAN_POINT('Ctrl Pts',(-3.09936827875094,-4.19204414568801,
75.4688694376893));
#63329=CARTESIAN_POINT('Ctrl Pts',(-4.37522031390861,-2.83491887917204,
75.4159491836074));
#63330=CARTESIAN_POINT('Ctrl Pts',(-4.78906667771331,-1.25237330364,75.3630289295254));
#63331=CARTESIAN_POINT('Ctrl Pts',(-4.89518266041626,-0.846586534424758,
75.3494594379025));
#63332=CARTESIAN_POINT('Ctrl Pts',(-4.94462339418807,-0.425978804568305,
75.3358899462797));
#63333=CARTESIAN_POINT('Ctrl Pts',(-4.94084634488987,-0.00449823523784309,
75.3223204546568));
#63334=CARTESIAN_POINT('Ctrl Pts',(-4.94163609422309,-0.00451829382380276,
75.1776795453432));
#63335=CARTESIAN_POINT('Ctrl Pts',(-4.94524177329398,-0.3994182708838,75.1903984623041));
#63336=CARTESIAN_POINT('Ctrl Pts',(-4.90188327382623,-0.793536109632625,
75.2031173792649));
#63337=CARTESIAN_POINT('Ctrl Pts',(-4.80852961499291,-1.17543275960954,
75.2158362962258));
#63338=CARTESIAN_POINT('Ctrl Pts',(-4.42010822973382,-2.76440985663659,
75.2687565503078));
#63339=CARTESIAN_POINT('Ctrl Pts',(-3.16617795142011,-4.14181551954833,
75.3216768043897));
#63340=CARTESIAN_POINT('Ctrl Pts',(-1.62055642630759,-4.6773278802945,75.3745970584716));
#63341=CARTESIAN_POINT('Ctrl Pts',(-0.0749349011951517,-5.21284024104065,
75.4275173125536));
#63342=CARTESIAN_POINT('Ctrl Pts',(1.76237787071597,-4.90645929962131,75.4804375666356));
#63343=CARTESIAN_POINT('Ctrl Pts',(3.05059950427476,-3.89838965409382,75.5333578207175));
#63344=CARTESIAN_POINT('Ctrl Pts',(4.3388211378337,-2.8903200085662,75.5862780747995));
#63345=CARTESIAN_POINT('Ctrl Pts',(5.07795163304007,-1.18056165893029,75.6391983288815));
#63346=CARTESIAN_POINT('Ctrl Pts',(4.92975358676999,0.448473861396107,75.6921185829634));
#63347=CARTESIAN_POINT('Ctrl Pts',(4.78155554049993,2.07750938172241,75.7450388370454));
#63348=CARTESIAN_POINT('Ctrl Pts',(3.74602895275332,3.62582207273939,75.7979590911274));
#63349=CARTESIAN_POINT('Ctrl Pts',(2.29704660536897,4.38488040012382,75.8508793452094));
#63350=CARTESIAN_POINT('Ctrl Pts',(0.848064257984615,5.14393872750825,75.9037995992913));
#63351=CARTESIAN_POINT('Ctrl Pts',(-1.0143738490375,5.11374269126039,75.9567198533733));
#63352=CARTESIAN_POINT('Ctrl Pts',(-2.43798759346781,4.30811045874223,76.0096401074552));
#63353=CARTESIAN_POINT('Ctrl Pts',(-3.86160133789813,3.50247822622406,76.0625603615372));
#63354=CARTESIAN_POINT('Ctrl Pts',(-4.84639071973656,1.92140979743563,76.1154806156192));
#63355=CARTESIAN_POINT('Ctrl Pts',(-4.94170107746221,0.28842623257243,76.1684008697011));
#63356=CARTESIAN_POINT('Ctrl Pts',(-4.94727143302206,0.192987506953041,
76.1714937615818));
#63357=CARTESIAN_POINT('Ctrl Pts',(-4.94980355369306,0.0973714523878282,
76.1745866534625));
#63358=CARTESIAN_POINT('Ctrl Pts',(-4.94936999019276,0.00173199160742904,
76.1776795453431));
#63359=CARTESIAN_POINT('Origin',(0.,0.,16.));
#63360=CARTESIAN_POINT('',(-4.93710573305067,0.00369191742993435,77.3223204546568));
#63361=CARTESIAN_POINT('',(-4.93651943436554,0.00342058198068374,77.1776795453431));
#63362=CARTESIAN_POINT('',(-4.942,-6.05220448138622E-16,16.));
#63363=CARTESIAN_POINT('Ctrl Pts',(-4.93710573305067,0.00369191742993435,
77.3223204546568));
#63364=CARTESIAN_POINT('Ctrl Pts',(-4.94100558540341,0.565545404544723,
77.3042663285965));
#63365=CARTESIAN_POINT('Ctrl Pts',(-4.85249197896959,1.12620708123838,77.2862122025363));
#63366=CARTESIAN_POINT('Ctrl Pts',(-4.66622450050179,1.65225526059718,77.2681580764761));
#63367=CARTESIAN_POINT('Ctrl Pts',(-4.12023726994686,3.19420767735372,77.2152378223941));
#63368=CARTESIAN_POINT('Ctrl Pts',(-2.73435528454182,4.43876323142188,77.1623175683121));
#63369=CARTESIAN_POINT('Ctrl Pts',(-1.14277930696628,4.81639429353784,77.1093973142302));
#63370=CARTESIAN_POINT('Ctrl Pts',(0.448796670609252,5.1940253556538,77.0564770601482));
#63371=CARTESIAN_POINT('Ctrl Pts',(2.24606664035538,4.70473192581759,77.0035568060662));
#63372=CARTESIAN_POINT('Ctrl Pts',(3.42657241495318,3.57242215035347,76.9506365519843));
#63373=CARTESIAN_POINT('Ctrl Pts',(4.60707818955111,2.44011237488923,76.8977162979023));
#63374=CARTESIAN_POINT('Ctrl Pts',(5.1708197690006,0.664786253797156,76.8447960438203));
#63375=CARTESIAN_POINT('Ctrl Pts',(4.85982039669027,-0.941139865890017,
76.7918757897384));
#63376=CARTESIAN_POINT('Ctrl Pts',(4.54882102437996,-2.54706598557701,76.7389555356564));
#63377=CARTESIAN_POINT('Ctrl Pts',(3.36308070030987,-3.983592103859,76.6860352815744));
#63378=CARTESIAN_POINT('Ctrl Pts',(1.84521230622943,-4.59334192937927,76.6331150274925));
#63379=CARTESIAN_POINT('Ctrl Pts',(0.327343912148982,-5.20309175489953,
76.5801947734105));
#63380=CARTESIAN_POINT('Ctrl Pts',(-1.52265255194192,-4.98606528765813,
76.5272745193286));
#63381=CARTESIAN_POINT('Ctrl Pts',(-2.85819044963632,-4.04157715364459,
76.4743542652466));
#63382=CARTESIAN_POINT('Ctrl Pts',(-4.13713943489684,-3.13710851769457,
76.4236763283833));
#63383=CARTESIAN_POINT('Ctrl Pts',(-4.94430311018814,-1.56551963073416,
76.3729983915201));
#63384=CARTESIAN_POINT('Ctrl Pts',(-4.949709811623,0.00127385101247733,
76.3223204546568));
#63385=CARTESIAN_POINT('Ctrl Pts',(-4.94936999019276,0.00173199160742904,
76.1776795453431));
#63386=CARTESIAN_POINT('Ctrl Pts',(-4.9423851596845,-1.5390467478049,76.2275069075444));
#63387=CARTESIAN_POINT('Ctrl Pts',(-4.16568308583621,-3.08590036450939,
76.2773342697457));
#63388=CARTESIAN_POINT('Ctrl Pts',(-2.92261878913845,-3.99523449174163,
76.327161631947));
#63389=CARTESIAN_POINT('Ctrl Pts',(-1.60239480947616,-4.96101295025462,
76.380081886029));
#63390=CARTESIAN_POINT('Ctrl Pts',(0.243884483461281,-5.20767116634268,
76.4330021401109));
#63391=CARTESIAN_POINT('Ctrl Pts',(1.77133348755807,-4.62233457318728,76.4859223941929));
#63392=CARTESIAN_POINT('Ctrl Pts',(3.29878249165486,-4.03699798003188,76.5388426482749));
#63393=CARTESIAN_POINT('Ctrl Pts',(4.507401206911,-2.61966657763301,76.5917629023568));
#63394=CARTESIAN_POINT('Ctrl Pts',(4.84410725035561,-1.01893286220407,76.6446831564388));
#63395=CARTESIAN_POINT('Ctrl Pts',(5.18081329380023,0.581800853224953,76.6976034105207));
#63396=CARTESIAN_POINT('Ctrl Pts',(4.64560666543322,2.36593688168406,76.7505236646027));
#63397=CARTESIAN_POINT('Ctrl Pts',(3.483406092445,3.51702732797801,76.8034439186847));
#63398=CARTESIAN_POINT('Ctrl Pts',(2.32120551945685,4.6681177742719,76.8563641727667));
#63399=CARTESIAN_POINT('Ctrl Pts',(0.532011001847567,5.1861626384007,76.9092844268486));
#63400=CARTESIAN_POINT('Ctrl Pts',(-1.06541472329578,4.83409667859588,76.9622046809306));
#63401=CARTESIAN_POINT('Ctrl Pts',(-2.66284044843913,4.48203071879105,77.0151249350126));
#63402=CARTESIAN_POINT('Ctrl Pts',(-4.06849738111654,3.2598539350526,77.0680451890945));
#63403=CARTESIAN_POINT('Ctrl Pts',(-4.63913544075982,1.72685308955721,77.1209654431764));
#63404=CARTESIAN_POINT('Ctrl Pts',(-4.84298445708464,1.17921924512925,77.1398701438987));
#63405=CARTESIAN_POINT('Ctrl Pts',(-4.94027400061573,0.591920131780996,
77.1587748446209));
#63406=CARTESIAN_POINT('Ctrl Pts',(-4.93651943436554,0.00342058198068374,
77.1776795453431));
#63407=CARTESIAN_POINT('Origin',(0.,0.,16.));
#63408=CARTESIAN_POINT('',(-4.93642136366389,-0.0033694929564293,78.3223204546568));
#63409=CARTESIAN_POINT('',(-4.93699915860479,-0.00364661157755484,78.1776795453431));
#63410=CARTESIAN_POINT('',(-4.942,-6.05220448138622E-16,16.));
#63411=CARTESIAN_POINT('Ctrl Pts',(-4.93642136366389,-0.0033694929564293,
78.3223204546568));
#63412=CARTESIAN_POINT('Ctrl Pts',(-4.92980420575396,1.05092284524382,78.288454519755));
#63413=CARTESIAN_POINT('Ctrl Pts',(-4.59907343284897,2.10900469043804,78.2545885848532));
#63414=CARTESIAN_POINT('Ctrl Pts',(-3.975312192884,2.94965955736624,78.2207226499514));
#63415=CARTESIAN_POINT('Ctrl Pts',(-3.00059812102546,4.26330021964482,78.1678023958694));
#63416=CARTESIAN_POINT('Ctrl Pts',(-1.31034971100207,5.04601837903923,78.1148821417875));
#63417=CARTESIAN_POINT('Ctrl Pts',(0.321949550104491,4.93963025159188,78.0619618877055));
#63418=CARTESIAN_POINT('Ctrl Pts',(1.95424881121096,4.83324212414454,78.0090416336236));
#63419=CARTESIAN_POINT('Ctrl Pts',(3.52859892340051,3.83774770985554,77.9561213795416));
#63420=CARTESIAN_POINT('Ctrl Pts',(4.32455323076013,2.40870045658987,77.9032011254596));
#63421=CARTESIAN_POINT('Ctrl Pts',(5.12050753811972,0.979653203324283,77.8502808713777));
#63422=CARTESIAN_POINT('Ctrl Pts',(5.13806604064937,-0.882946888918111,
77.7973606172957));
#63423=CARTESIAN_POINT('Ctrl Pts',(4.36919369942578,-2.32674557099659,77.7444403632137));
#63424=CARTESIAN_POINT('Ctrl Pts',(3.60032135820212,-3.77054425307524,77.6915201091318));
#63425=CARTESIAN_POINT('Ctrl Pts',(2.04501817322514,-4.79554152499005,77.6385998550498));
#63426=CARTESIAN_POINT('Ctrl Pts',(0.415014635617477,-4.93268298063817,
77.5856796009678));
#63427=CARTESIAN_POINT('Ctrl Pts',(-1.21498890199009,-5.06982443628629,
77.5327593468859));
#63428=CARTESIAN_POINT('Ctrl Pts',(-2.91969279222824,-4.3191100756678,77.4798390928039));
#63429=CARTESIAN_POINT('Ctrl Pts',(-3.91899849949491,-3.02407825563606,
77.4269188387219));
#63430=CARTESIAN_POINT('Ctrl Pts',(-4.57738386303512,-2.17085587390878,
77.3920527107002));
#63431=CARTESIAN_POINT('Ctrl Pts',(-4.92957433823582,-1.08135952985832,
77.3571865826785));
#63432=CARTESIAN_POINT('Ctrl Pts',(-4.93710573305067,0.00369191742993435,
77.3223204546568));
#63433=CARTESIAN_POINT('Ctrl Pts',(-4.93651943436554,0.00342058198068374,
77.1776795453431));
#63434=CARTESIAN_POINT('Ctrl Pts',(-4.92976377869543,-1.05547678606275,
77.2116950987028));
#63435=CARTESIAN_POINT('Ctrl Pts',(-4.59587353108828,-2.11826061804498,
77.2457106520626));
#63436=CARTESIAN_POINT('Ctrl Pts',(-3.96697769860343,-2.96085919445861,
77.2797262054223));
#63437=CARTESIAN_POINT('Ctrl Pts',(-2.98856271019464,-4.27174572572668,
77.3326464595043));
#63438=CARTESIAN_POINT('Ctrl Pts',(-1.29611354676788,-5.0496938810105,77.3855667135863));
#63439=CARTESIAN_POINT('Ctrl Pts',(0.335879206226305,-4.93870270308427,
77.4384869676682));
#63440=CARTESIAN_POINT('Ctrl Pts',(1.96787195922058,-4.82771152515804,77.4914072217502));
#63441=CARTESIAN_POINT('Ctrl Pts',(3.53940830178236,-3.82778101402163,77.5443274758322));
#63442=CARTESIAN_POINT('Ctrl Pts',(4.33132920195393,-2.39649464320875,77.5972477299141));
#63443=CARTESIAN_POINT('Ctrl Pts',(5.12325010212551,-0.96520827239587,77.6501679839961));
#63444=CARTESIAN_POINT('Ctrl Pts',(5.13555555990697,0.897433958093309,77.7030882380781));
#63445=CARTESIAN_POINT('Ctrl Pts',(4.36261440987998,2.33905851601337,77.75600849216));
#63446=CARTESIAN_POINT('Ctrl Pts',(3.58967325985303,3.78068307393336,77.808928746242));
#63447=CARTESIAN_POINT('Ctrl Pts',(2.03148550201762,4.8012899592841,77.8618490003239));
#63448=CARTESIAN_POINT('Ctrl Pts',(0.40110165209169,4.93383387390743,77.9147692544059));
#63449=CARTESIAN_POINT('Ctrl Pts',(-1.22928219783424,5.06637778853077,77.9676895084879));
#63450=CARTESIAN_POINT('Ctrl Pts',(-2.93186213985079,4.31085873242671,78.0206097625698));
#63451=CARTESIAN_POINT('Ctrl Pts',(-3.92751158950039,3.01301376448353,78.0735300166518));
#63452=CARTESIAN_POINT('Ctrl Pts',(-4.58067311036902,2.16160728461073,78.1082465262156));
#63453=CARTESIAN_POINT('Ctrl Pts',(-4.92960256861,1.07680737701515,78.1429630357793));
#63454=CARTESIAN_POINT('Ctrl Pts',(-4.93699915860479,-0.00364661157755484,
78.1776795453431));
#63455=CARTESIAN_POINT('Origin',(0.,0.,16.));
#63456=CARTESIAN_POINT('',(-4.94930076406873,-0.0018103975202266,79.3223204546568));
#63457=CARTESIAN_POINT('',(-4.94965689841004,-0.00135584006909748,79.1776795453431));
#63458=CARTESIAN_POINT('',(-4.942,-6.05220448138622E-16,16.));
#63459=CARTESIAN_POINT('Ctrl Pts',(-4.94930076406873,-0.0018103975202266,
79.3223204546568));
#63460=CARTESIAN_POINT('Ctrl Pts',(-4.94206344439878,1.53439887470602,79.2726427109135));
#63461=CARTESIAN_POINT('Ctrl Pts',(-4.17064455342085,3.07688083896746,79.2229649671701));
#63462=CARTESIAN_POINT('Ctrl Pts',(-2.93387463574621,3.9869760667678,79.1732872234267));
#63463=CARTESIAN_POINT('Ctrl Pts',(-1.61637965001588,4.95647401624775,79.1203669693448));
#63464=CARTESIAN_POINT('Ctrl Pts',(0.229196639493549,5.20833819439267,79.0674467152628));
#63465=CARTESIAN_POINT('Ctrl Pts',(1.75829033577168,4.62731170663768,79.0145264611808));
#63466=CARTESIAN_POINT('Ctrl Pts',(3.28738403204981,4.04628521888269,78.9616062070989));
#63467=CARTESIAN_POINT('Ctrl Pts',(4.49999513509664,2.6323680652278,78.9086859530169));
#63468=CARTESIAN_POINT('Ctrl Pts',(4.84121428431374,1.03259032951638,78.8557656989349));
#63469=CARTESIAN_POINT('Ctrl Pts',(5.18243343353085,-0.567187406195048,
78.802845444853));
#63470=CARTESIAN_POINT('Ctrl Pts',(4.65226062891823,-2.35282572396301,78.749925190771));
#63471=CARTESIAN_POINT('Ctrl Pts',(3.49331104303619,-3.50718925806059,78.6970049366891));
#63472=CARTESIAN_POINT('Ctrl Pts',(2.33436145715409,-4.66155279215825,78.6440846826071));
#63473=CARTESIAN_POINT('Ctrl Pts',(0.546635090002505,-5.18464154258545,
78.5911644285251));
#63474=CARTESIAN_POINT('Ctrl Pts',(-1.05177716940348,-4.83708210816974,
78.5382441744432));
#63475=CARTESIAN_POINT('Ctrl Pts',(-2.65018942880937,-4.48952267375405,
78.4853239203612));
#63476=CARTESIAN_POINT('Ctrl Pts',(-4.05928758046969,-3.27131505449554,
78.4324036662792));
#63477=CARTESIAN_POINT('Ctrl Pts',(-4.63424678945294,-1.73992966228502,
78.3794834121973));
#63478=CARTESIAN_POINT('Ctrl Pts',(-4.84126499965602,-1.18854330639521,
78.3604290930171));
#63479=CARTESIAN_POINT('Ctrl Pts',(-4.94014443935181,-0.596556209328453,
78.3413747738369));
#63480=CARTESIAN_POINT('Ctrl Pts',(-4.93642136366389,-0.0033694929564293,
78.3223204546568));
#63481=CARTESIAN_POINT('Ctrl Pts',(-4.93699915860479,-0.00364661157755484,
78.1776795453431));
#63482=CARTESIAN_POINT('Ctrl Pts',(-4.94087759097782,-0.57018710251793,
78.1958832898613));
#63483=CARTESIAN_POINT('Ctrl Pts',(-4.85085250590991,-1.13553269504931,
78.2140870343795));
#63484=CARTESIAN_POINT('Ctrl Pts',(-4.66154625697823,-1.66540857589943,
78.2322907788976));
#63485=CARTESIAN_POINT('Ctrl Pts',(-4.11121251752373,-3.20581506855694,
78.2852110329796));
#63486=CARTESIAN_POINT('Ctrl Pts',(-2.72182608133198,-4.44645717408944,
78.3381312870616));
#63487=CARTESIAN_POINT('Ctrl Pts',(-1.12919140128498,-4.819598117052,78.3910515411436));
#63488=CARTESIAN_POINT('Ctrl Pts',(0.463443278761841,-5.19273906001451,
78.4439717952256));
#63489=CARTESIAN_POINT('Ctrl Pts',(2.25932620266378,-4.69837884040726,78.4968920493075));
#63490=CARTESIAN_POINT('Ctrl Pts',(3.43663391646442,-3.56274424493725,78.5498123033895));
#63491=CARTESIAN_POINT('Ctrl Pts',(4.6139416302652,-2.42710964946711,78.6027325574714));
#63492=CARTESIAN_POINT('Ctrl Pts',(5.17267413396446,-0.65020067813383,78.6556528115534));
#63493=CARTESIAN_POINT('Ctrl Pts',(4.85714690051601,0.954841985584431,78.7085730656353));
#63494=CARTESIAN_POINT('Ctrl Pts',(4.54161966706758,2.5598846493026,78.7614933197173));
#63495=CARTESIAN_POINT('Ctrl Pts',(3.35183269647175,3.99306100540591,78.8144135737993));
#63496=CARTESIAN_POINT('Ctrl Pts',(1.83225067773116,4.59852766487066,78.8673338278812));
#63497=CARTESIAN_POINT('Ctrl Pts',(0.312668658990661,5.20399432433538,78.9202540819632));
#63498=CARTESIAN_POINT('Ctrl Pts',(-1.53670840789443,4.98175128716162,78.9731743360452));
#63499=CARTESIAN_POINT('Ctrl Pts',(-2.86957733213866,4.03350036141105,79.0260945901271));
#63500=CARTESIAN_POINT('Ctrl Pts',(-4.14220208735026,3.12810930583763,79.0766229085325));
#63501=CARTESIAN_POINT('Ctrl Pts',(-4.94395467452422,1.56085664483311,79.1271512269378));
#63502=CARTESIAN_POINT('Ctrl Pts',(-4.94965689841004,-0.00135584006909748,
79.1776795453431));
#63503=CARTESIAN_POINT('Origin',(0.,0.,16.));
#63504=CARTESIAN_POINT('',(-4.94177616066966,0.00451715357047341,80.3223204546568));
#63505=CARTESIAN_POINT('',(-4.94098429374081,0.00450501606805162,80.1776795453432));
#63506=CARTESIAN_POINT('',(-4.942,-6.05220448138622E-16,16.));
#63507=CARTESIAN_POINT('Ctrl Pts',(-4.94177616066966,0.00451715357047341,
80.3223204546568));
#63508=CARTESIAN_POINT('Ctrl Pts',(-4.94534763047119,0.394743465756727,
80.3097511561539));
#63509=CARTESIAN_POINT('Ctrl Pts',(-4.90301618269456,0.784203971238864,
80.2971818576509));
#63510=CARTESIAN_POINT('Ctrl Pts',(-4.81182542362119,1.16186687182505,80.284612559148));
#63511=CARTESIAN_POINT('Ctrl Pts',(-4.42788688170829,2.75193306777578,80.231692305066));
#63512=CARTESIAN_POINT('Ctrl Pts',(-3.17784621930909,4.13286961482545,80.178772050984));
#63513=CARTESIAN_POINT('Ctrl Pts',(-1.63374113503097,4.67273885841708,80.125851796902));
#63514=CARTESIAN_POINT('Ctrl Pts',(-0.0896360507527699,5.21260810200875,
80.07293154282));
#63515=CARTESIAN_POINT('Ctrl Pts',(1.74853345540447,4.91141004214231,80.0200112887381));
#63516=CARTESIAN_POINT('Ctrl Pts',(3.03959294361313,3.90697751111939,79.9670910346562));
#63517=CARTESIAN_POINT('Ctrl Pts',(4.33065243182171,2.90254498009653,79.9141707805742));
#63518=CARTESIAN_POINT('Ctrl Pts',(5.0746019020818,1.1948779779175,79.8612505264923));
#63519=CARTESIAN_POINT('Ctrl Pts',(4.93099871468662,-0.43456899453677,79.8083302724103));
#63520=CARTESIAN_POINT('Ctrl Pts',(4.78739552729143,-2.06401596699104,79.7554100183283));
#63521=CARTESIAN_POINT('Ctrl Pts',(3.7562396822408,-3.61524290972046,79.7024897642464));
#63522=CARTESIAN_POINT('Ctrl Pts',(2.30940384276248,-4.37838468231013,79.6495695101644));
#63523=CARTESIAN_POINT('Ctrl Pts',(0.86256800328416,-5.14152645489981,79.5966492560824));
#63524=CARTESIAN_POINT('Ctrl Pts',(-0.999947830621951,-5.1165830573498,
79.5437290020005));
#63525=CARTESIAN_POINT('Ctrl Pts',(-2.4258279677168,-4.31496896933192,79.4908087479185));
#63526=CARTESIAN_POINT('Ctrl Pts',(-3.85170810481173,-3.51335488131399,
79.4378884938365));
#63527=CARTESIAN_POINT('Ctrl Pts',(-4.84095254509543,-1.93507010282805,
79.3849682397546));
#63528=CARTESIAN_POINT('Ctrl Pts',(-4.9408679242616,-0.302361853177563,
79.3320479856726));
#63529=CARTESIAN_POINT('Ctrl Pts',(-4.94698990261473,-0.202323153982769,
79.328805475334));
#63530=CARTESIAN_POINT('Ctrl Pts',(-4.94977315033439,-0.10208013749047,
79.3255629649954));
#63531=CARTESIAN_POINT('Ctrl Pts',(-4.94930076406873,-0.0018103975202266,
79.3223204546568));
#63532=CARTESIAN_POINT('Ctrl Pts',(-4.94965689841004,-0.00135584006909748,
79.1776795453431));
#63533=CARTESIAN_POINT('Ctrl Pts',(-4.9499268332343,-0.0753086628631314,
79.1800714810198));
#63534=CARTESIAN_POINT('Ctrl Pts',(-4.94841287075996,-0.149250190949008,
79.1824634166964));
#63535=CARTESIAN_POINT('Ctrl Pts',(-4.94508051525459,-0.223109677684533,
79.184855352373));
#63536=CARTESIAN_POINT('Ctrl Pts',(-4.87135399252289,-1.85720997670206,
79.237775606455));
#63537=CARTESIAN_POINT('Ctrl Pts',(-3.90754016545605,-3.45115176040958,
79.290695860537));
#63538=CARTESIAN_POINT('Ctrl Pts',(-2.49469496135826,-4.27552292478954,
79.3436161146189));
#63539=CARTESIAN_POINT('Ctrl Pts',(-1.08184975726055,-5.09989408916944,
79.3965363687009));
#63540=CARTESIAN_POINT('Ctrl Pts',(0.780026823868144,-5.15469463422192,
79.4494566227829));
#63541=CARTESIAN_POINT('Ctrl Pts',(2.23891162262289,-4.41484699357874,79.5023768768648));
#63542=CARTESIAN_POINT('Ctrl Pts',(3.69779642137764,-3.67499935293556,79.5552971309468));
#63543=CARTESIAN_POINT('Ctrl Pts',(4.75368943775855,-2.14050352659667,79.6082173850287));
#63544=CARTESIAN_POINT('Ctrl Pts',(4.92339790113362,-0.51356824058747,79.6611376391107));
#63545=CARTESIAN_POINT('Ctrl Pts',(5.0931063645087,1.11336704542182,79.7140578931926));
#63546=CARTESIAN_POINT('Ctrl Pts',(4.37663027487802,2.83274179110132,79.7669781472746));
#63547=CARTESIAN_POINT('Ctrl Pts',(3.10184003337994,3.85774385333563,79.8198984013566));
#63548=CARTESIAN_POINT('Ctrl Pts',(1.82704979188194,4.88274591556987,79.8728186554386));
#63549=CARTESIAN_POINT('Ctrl Pts',(-0.00605460148340203,5.21337529435879,
79.9257389095204));
#63550=CARTESIAN_POINT('Ctrl Pts',(-1.55861657986055,4.69833093636568,79.9786591636024));
#63551=CARTESIAN_POINT('Ctrl Pts',(-3.11117855823778,4.18328657837255,80.0315794176844));
#63552=CARTESIAN_POINT('Ctrl Pts',(-4.38319812162688,2.82256848359726,80.0844996717665));
#63553=CARTESIAN_POINT('Ctrl Pts',(-4.79257969064933,1.23886203404666,80.1374199258484));
#63554=CARTESIAN_POINT('Ctrl Pts',(-4.89639341618109,0.837255124705079,
80.1508397990133));
#63555=CARTESIAN_POINT('Ctrl Pts',(-4.94473415317796,0.421308677192607,
80.1642596721782));
#63556=CARTESIAN_POINT('Ctrl Pts',(-4.94098429374081,0.00450501606805162,
80.1776795453432));
#63557=CARTESIAN_POINT('Origin',(0.,0.,16.));
#63558=CARTESIAN_POINT('',(-4.93407925753408,-0.000975201913082646,81.3223204546568));
#63559=CARTESIAN_POINT('',(-4.93426916398102,-0.00139536187133696,81.1776795453431));
#63560=CARTESIAN_POINT('',(-4.942,-6.05220448138622E-16,16.));
#63561=CARTESIAN_POINT('Ctrl Pts',(-4.93407925753408,-0.000975201913082646,
81.3223204546568));
#63562=CARTESIAN_POINT('Ctrl Pts',(-4.93251895945243,0.883617373199263,
81.2939393473123));
#63563=CARTESIAN_POINT('Ctrl Pts',(-4.70573849196771,1.76895636928203,81.2655582399678));
#63564=CARTESIAN_POINT('Ctrl Pts',(-4.25849767807825,2.52364737255269,81.2371771326233));
#63565=CARTESIAN_POINT('Ctrl Pts',(-3.42455919852679,3.93086658925474,81.1842568785413));
#63566=CARTESIAN_POINT('Ctrl Pts',(-1.8241145504932,4.88384315405391,81.1313366244594));
#63567=CARTESIAN_POINT('Ctrl Pts',(-0.189551647970844,4.94648043642473,
81.0784163703775));
#63568=CARTESIAN_POINT('Ctrl Pts',(1.44501125455142,5.00911771879556,81.0254961162955));
#63569=CARTESIAN_POINT('Ctrl Pts',(3.11369241156233,4.18141571873815,80.9725758622135));
#63570=CARTESIAN_POINT('Ctrl Pts',(4.05287784031979,2.84214351269564,80.9196556081315));
#63571=CARTESIAN_POINT('Ctrl Pts',(4.99206326907725,1.50287130665312,80.8667353540495));
#63572=CARTESIAN_POINT('Ctrl Pts',(5.20175296958118,-0.347971105374417,
80.8138150999676));
#63573=CARTESIAN_POINT('Ctrl Pts',(4.58598973236862,-1.86340996827063,80.7608948458856));
#63574=CARTESIAN_POINT('Ctrl Pts',(3.97022649515609,-3.37884883116675,80.7079745918037));
#63575=CARTESIAN_POINT('Ctrl Pts',(2.52901032022692,-4.5588841449317,80.6550543377218));
#63576=CARTESIAN_POINT('Ctrl Pts',(0.92186374048162,-4.86351372766964,80.6021340836398));
#63577=CARTESIAN_POINT('Ctrl Pts',(-0.685282839263774,-5.16814331040758,
80.5492138295578));
#63578=CARTESIAN_POINT('Ctrl Pts',(-2.45835982382543,-4.59736716211862,
80.4962935754758));
#63579=CARTESIAN_POINT('Ctrl Pts',(-3.58598010539301,-3.41238116554821,
80.4433733213938));
#63580=CARTESIAN_POINT('Ctrl Pts',(-4.44577484147009,-2.5088458719475,80.4030223658148));
#63581=CARTESIAN_POINT('Ctrl Pts',(-4.93031074601031,-1.24821819877227,
80.3626714102358));
#63582=CARTESIAN_POINT('Ctrl Pts',(-4.94177616066966,0.00451715357047341,
80.3223204546568));
#63583=CARTESIAN_POINT('Ctrl Pts',(-4.94098429374081,0.00450501606805162,
80.1776795453432));
#63584=CARTESIAN_POINT('Ctrl Pts',(-4.92994686631264,-1.22232501277905,
80.2171799262602));
#63585=CARTESIAN_POINT('Ctrl Pts',(-4.46760970741441,-2.45658172320469,
80.2566803071772));
#63586=CARTESIAN_POINT('Ctrl Pts',(-3.64022747730309,-3.35445124336543,
80.2961806880942));
#63587=CARTESIAN_POINT('Ctrl Pts',(-2.53175012027843,-4.55736326690124,
80.3491009421762));
#63588=CARTESIAN_POINT('Ctrl Pts',(-0.768051831573162,-5.1564925096469,
80.4020211962582));
#63589=CARTESIAN_POINT('Ctrl Pts',(0.843772115467599,-4.87766827980189,
80.4549414503402));
#63590=CARTESIAN_POINT('Ctrl Pts',(2.45559606250818,-4.59884404995691,80.5078617044222));
#63591=CARTESIAN_POINT('Ctrl Pts',(3.91554566788429,-3.4420663475215,80.5607819585041));
#63592=CARTESIAN_POINT('Ctrl Pts',(4.55552569480652,-1.93669431624669,80.613702212586));
#63593=CARTESIAN_POINT('Ctrl Pts',(5.19550572172878,-0.431322284971791,
80.666622466668));
#63594=CARTESIAN_POINT('Ctrl Pts',(5.01551617019705,1.42264407514254,80.71954272075));
#63595=CARTESIAN_POINT('Ctrl Pts',(4.09792300791601,2.7768014426365,80.7724629748319));
#63596=CARTESIAN_POINT('Ctrl Pts',(3.18032984563491,4.13095881013054,80.8253832289139));
#63597=CARTESIAN_POINT('Ctrl Pts',(1.52513307260442,4.98530718500416,80.8783034829959));
#63598=CARTESIAN_POINT('Ctrl Pts',(-0.110223988510079,4.94888370271273,
80.9312237370779));
#63599=CARTESIAN_POINT('Ctrl Pts',(-1.74558104962448,4.9124602204213,80.9841439911598));
#63600=CARTESIAN_POINT('Ctrl Pts',(-3.36109839882289,3.98526488096493,81.0370642452417));
#63601=CARTESIAN_POINT('Ctrl Pts',(-4.21749062381118,2.59159643244825,81.0899844993237));
#63602=CARTESIAN_POINT('Ctrl Pts',(-4.69053795942863,1.82177259814856,81.1192161813301));
#63603=CARTESIAN_POINT('Ctrl Pts',(-4.93196472022524,0.909620752018895,
81.1484478633366));
#63604=CARTESIAN_POINT('Ctrl Pts',(-4.93426916398102,-0.00139536187133696,
81.1776795453431));
#63605=CARTESIAN_POINT('Origin',(0.,0.,16.));
#63606=CARTESIAN_POINT('',(-4.94535283272668,-0.00400458364991862,82.3223204546568));
#63607=CARTESIAN_POINT('',(-4.94609777444767,-0.00376784846301249,82.1776795453432));
#63608=CARTESIAN_POINT('',(-4.942,-6.05220448138622E-16,16.));
#63609=CARTESIAN_POINT('Ctrl Pts',(-4.94535283272668,-0.00400458364991862,
82.3223204546568));
#63610=CARTESIAN_POINT('Ctrl Pts',(-4.93330953662462,1.36545649397123,82.2781275384708));
#63611=CARTESIAN_POINT('Ctrl Pts',(-4.34046622285376,2.74406818932791,82.2339346222847));
#63612=CARTESIAN_POINT('Ctrl Pts',(-3.32967465270896,3.66290393572493,82.1897417060986));
#63613=CARTESIAN_POINT('Ctrl Pts',(-2.11926920015238,4.76319387708596,82.1368214520167));
#63614=CARTESIAN_POINT('Ctrl Pts',(-0.309540619040862,5.20418124698654,
82.0839011979348));
#63615=CARTESIAN_POINT('Ctrl Pts',(1.27135165523017,4.78406349239674,82.0309809438528));
#63616=CARTESIAN_POINT('Ctrl Pts',(2.85224392950138,4.3639457378069,81.9780606897708));
#63617=CARTESIAN_POINT('Ctrl Pts',(4.20429989693216,3.08272285872646,81.9251404356888));
#63618=CARTESIAN_POINT('Ctrl Pts',(4.7087980958408,1.52670201104665,81.8722201816068));
#63619=CARTESIAN_POINT('Ctrl Pts',(5.21329629474935,-0.0293188366329011,
81.8192999275248));
#63620=CARTESIAN_POINT('Ctrl Pts',(4.87023672513615,-1.86013765291182,81.7663796734429));
#63621=CARTESIAN_POINT('Ctrl Pts',(3.83660868625431,-3.12794378523385,81.713459419361));
#63622=CARTESIAN_POINT('Ctrl Pts',(2.80298064737236,-4.39574991755603,81.660539165279));
#63623=CARTESIAN_POINT('Ctrl Pts',(1.07878413922189,-5.10054336592114,81.607618911197));
#63624=CARTESIAN_POINT('Ctrl Pts',(-0.546962183326737,-4.91979988461579,
81.554698657115));
#63625=CARTESIAN_POINT('Ctrl Pts',(-2.17270850587518,-4.73905640331046,
81.5017784030331));
#63626=CARTESIAN_POINT('Ctrl Pts',(-3.70000464282163,-3.6727759923347,81.4488581489512));
#63627=CARTESIAN_POINT('Ctrl Pts',(-4.42993655576027,-2.20890485254455,
81.3959378948692));
#63628=CARTESIAN_POINT('Ctrl Pts',(-4.7684063275082,-1.53010711570026,81.3713987481318));
#63629=CARTESIAN_POINT('Ctrl Pts',(-4.93542833750884,-0.765820165151225,
81.3468596013943));
#63630=CARTESIAN_POINT('Ctrl Pts',(-4.93407925753408,-0.000975201913082646,
81.3223204546568));
#63631=CARTESIAN_POINT('Ctrl Pts',(-4.93426916398102,-0.00139536187133696,
81.1776795453431));
#63632=CARTESIAN_POINT('Ctrl Pts',(-4.93613662347209,-0.739658417382295,
81.2013681174186));
#63633=CARTESIAN_POINT('Ctrl Pts',(-4.78097132279663,-1.47717563214288,
81.2250566894941));
#63634=CARTESIAN_POINT('Ctrl Pts',(-4.46478101528126,-2.13759905414229,
81.2487452615696));
#63635=CARTESIAN_POINT('Ctrl Pts',(-3.75841208098482,-3.61298453463955,
81.3016655156515));
#63636=CARTESIAN_POINT('Ctrl Pts',(-2.24840711161364,-4.7036139380569,81.3545857697334));
#63637=CARTESIAN_POINT('Ctrl Pts',(-0.625767443036273,-4.91039859255742,
81.4075060238154));
#63638=CARTESIAN_POINT('Ctrl Pts',(0.996872225541001,-5.11718324705793,
81.4604262778974));
#63639=CARTESIAN_POINT('Ctrl Pts',(2.73214659332435,-4.44012315264172,81.5133465319795));
#63640=CARTESIAN_POINT('Ctrl Pts',(3.7859676073568,-3.18905134900772,81.5662667860614));
#63641=CARTESIAN_POINT('Ctrl Pts',(4.83978862138919,-1.9379795453738,81.6191870401434));
#63642=CARTESIAN_POINT('Ctrl Pts',(5.21215628167071,-0.112896032521955,
81.6721072942252));
#63643=CARTESIAN_POINT('Ctrl Pts',(4.7326694596758,1.45101310003748,81.7250275483072));
#63644=CARTESIAN_POINT('Ctrl Pts',(4.25318263768082,3.01492223259719,81.7779478023891));
#63645=CARTESIAN_POINT('Ctrl Pts',(2.92184133340926,4.31765698486456,81.8308680564712));
#63646=CARTESIAN_POINT('Ctrl Pts',(1.34788766110338,4.7630660380761,81.8837883105532));
#63647=CARTESIAN_POINT('Ctrl Pts',(-0.226066011202234,5.20847509128757,
81.9367085646351));
#63648=CARTESIAN_POINT('Ctrl Pts',(-2.04263205154196,4.79655844544351,81.989628818717));
#63649=CARTESIAN_POINT('Ctrl Pts',(-3.27052209643622,3.71581544847434,82.042549072799));
#63650=CARTESIAN_POINT('Ctrl Pts',(-4.31565037405029,2.79593253903751,82.087592563647));
#63651=CARTESIAN_POINT('Ctrl Pts',(-4.93430071630666,1.39150518826543,82.1326360544951));
#63652=CARTESIAN_POINT('Ctrl Pts',(-4.94609777444767,-0.00376784846301249,
82.1776795453432));
#63653=CARTESIAN_POINT('Origin',(0.,0.,16.));
#63654=CARTESIAN_POINT('',(-4.94676006163664,0.00350952918951444,83.3223204546568));
#63655=CARTESIAN_POINT('',(-4.94604776483535,0.00378542647206983,83.1776795453431));
#63656=CARTESIAN_POINT('',(-4.942,-6.05220448138622E-16,16.));
#63657=CARTESIAN_POINT('Ctrl Pts',(-4.94676006163664,0.00350952918951444,
83.3223204546568));
#63658=CARTESIAN_POINT('Ctrl Pts',(-4.94852531327494,0.222882433779423,
83.3152359837111));
#63659=CARTESIAN_POINT('Ctrl Pts',(-4.93519531289187,0.442039477932862,
83.3081515127655));
#63660=CARTESIAN_POINT('Ctrl Pts',(-4.90603966821321,0.659070530865341,
83.3010670418199));
#63661=CARTESIAN_POINT('Ctrl Pts',(-4.68825006385762,2.28026970762846,83.2481467877379));
#63662=CARTESIAN_POINT('Ctrl Pts',(-3.58740009065817,3.78283999594482,83.1952265336559));
#63663=CARTESIAN_POINT('Ctrl Pts',(-2.10725577029135,4.47918204688364,83.1423062795739));
#63664=CARTESIAN_POINT('Ctrl Pts',(-0.627111449924431,5.1755240978225,83.089386025492));
#63665=CARTESIAN_POINT('Ctrl Pts',(1.23232721760991,5.06563791138373,83.0364657714101));
#63666=CARTESIAN_POINT('Ctrl Pts',(2.62015283567102,4.19980920832437,82.9835455173281));
#63667=CARTESIAN_POINT('Ctrl Pts',(4.00797845373196,3.33398050526512,82.9306252632462));
#63668=CARTESIAN_POINT('Ctrl Pts',(4.9241910223198,1.71220928558549,82.8777050091641));
#63669=CARTESIAN_POINT('Ctrl Pts',(4.94951760585997,0.0766427637077434,
82.8247847550821));
#63670=CARTESIAN_POINT('Ctrl Pts',(4.97484418940015,-1.55892375817019,82.7718645010002));
#63671=CARTESIAN_POINT('Ctrl Pts',(4.10928478789245,-3.20828558224624,82.7189442469183));
#63672=CARTESIAN_POINT('Ctrl Pts',(2.74893264004429,-4.11666951392571,82.6660239928363));
#63673=CARTESIAN_POINT('Ctrl Pts',(1.38858049219621,-5.02505344560512,82.6131037387543));
#63674=CARTESIAN_POINT('Ctrl Pts',(-0.466564401992278,-5.19245948488802,
82.5601834846723));
#63675=CARTESIAN_POINT('Ctrl Pts',(-1.96755942526789,-4.5422800890475,82.5072632305904));
#63676=CARTESIAN_POINT('Ctrl Pts',(-3.4685544485435,-3.89210069320699,82.4543429765084));
#63677=CARTESIAN_POINT('Ctrl Pts',(-4.61539960090623,-2.42433586224305,
82.4014227224265));
#63678=CARTESIAN_POINT('Ctrl Pts',(-4.88328101508674,-0.810657190350331,
82.3485024683445));
#63679=CARTESIAN_POINT('Ctrl Pts',(-4.92745864911638,-0.544537549215846,
82.3397751304486));
#63680=CARTESIAN_POINT('Ctrl Pts',(-4.94773117576294,-0.274449500871191,
82.3310477925527));
#63681=CARTESIAN_POINT('Ctrl Pts',(-4.94535283272668,-0.00400458364991862,
82.3223204546568));
#63682=CARTESIAN_POINT('Ctrl Pts',(-4.94609777444767,-0.00376784846301249,
82.1776795453432));
#63683=CARTESIAN_POINT('Ctrl Pts',(-4.94816072809722,-0.247759491874606,
82.1855563085771));
#63684=CARTESIAN_POINT('Ctrl Pts',(-4.93166636384428,-0.49147120021732,
82.193433071811));
#63685=CARTESIAN_POINT('Ctrl Pts',(-4.89565013237716,-0.732262940926013,
82.201309835045));
#63686=CARTESIAN_POINT('Ctrl Pts',(-4.65367407397507,-2.35002898526266,
82.2542300891269));
#63687=CARTESIAN_POINT('Ctrl Pts',(-3.53050790772224,-3.83599172584166,
82.3071503432088));
#63688=CARTESIAN_POINT('Ctrl Pts',(-2.04012962670993,-4.51015191896435,
82.3600705972908));
#63689=CARTESIAN_POINT('Ctrl Pts',(-0.549751345697456,-5.18431211208712,
82.4129908513727));
#63690=CARTESIAN_POINT('Ctrl Pts',(1.3078390500746,-5.04666975775335,82.4659111054547));
#63691=CARTESIAN_POINT('Ctrl Pts',(2.68257982821446,-4.16021209746218,82.5188313595367));
#63692=CARTESIAN_POINT('Ctrl Pts',(4.05732060635432,-3.273754437171,82.5717516136187));
#63693=CARTESIAN_POINT('Ctrl Pts',(4.94921176686199,-1.63848147092241,82.6246718677007));
#63694=CARTESIAN_POINT('Ctrl Pts',(4.95011028710458,-0.00271908696136483,
82.6775921217826));
#63695=CARTESIAN_POINT('Ctrl Pts',(4.95100880734717,1.63304329699958,82.7305123758646));
#63696=CARTESIAN_POINT('Ctrl Pts',(4.06091468732478,3.26929509867298,82.7834326299465));
#63697=CARTESIAN_POINT('Ctrl Pts',(2.68714860199004,4.15726251102139,82.8363528840285));
#63698=CARTESIAN_POINT('Ctrl Pts',(1.31338251665521,5.04522992336985,82.8892731381104));
#63699=CARTESIAN_POINT('Ctrl Pts',(-0.544055533992037,5.18491294639323,
82.9421933921924));
#63700=CARTESIAN_POINT('Ctrl Pts',(-2.0351735518924,4.51239048126625,82.9951136462744));
#63701=CARTESIAN_POINT('Ctrl Pts',(-3.52629156979259,3.83986801613934,83.0480339003563));
#63702=CARTESIAN_POINT('Ctrl Pts',(-4.651089554946,2.35514006286229,83.1009541544383));
#63703=CARTESIAN_POINT('Ctrl Pts',(-4.8948427284911,0.737640835765265,83.1538744085202));
#63704=CARTESIAN_POINT('Ctrl Pts',(-4.9313919209059,0.495107417134616,83.1618094541278));
#63705=CARTESIAN_POINT('Ctrl Pts',(-4.94813254848979,0.249588896780995,
83.1697444997355));
#63706=CARTESIAN_POINT('Ctrl Pts',(-4.94604776483535,0.00378542647206983,
83.1776795453431));
#63707=CARTESIAN_POINT('Origin',(0.,0.,16.));
#63708=CARTESIAN_POINT('',(-4.93450205841395,0.0017791821159216,84.3223204546568));
#63709=CARTESIAN_POINT('',(-4.93425329604086,0.00136738585504144,84.1776795453431));
#63710=CARTESIAN_POINT('',(-4.942,-6.05220448138622E-16,16.));
#63711=CARTESIAN_POINT('Ctrl Pts',(-4.93450205841395,0.0017791821159216,
84.3223204546568));
#63712=CARTESIAN_POINT('Ctrl Pts',(-4.9368080070955,0.715261896051447,84.2994241748696));
#63713=CARTESIAN_POINT('Ctrl Pts',(-4.79225594661696,1.42785481900567,84.2765278950824));
#63714=CARTESIAN_POINT('Ctrl Pts',(-4.49620929648531,2.07068108576527,84.2536316152951));
#63715=CARTESIAN_POINT('Ctrl Pts',(-3.81195560589931,3.55644775544483,84.2007113612132));
#63716=CARTESIAN_POINT('Ctrl Pts',(-2.31839897625278,4.66951227096791,84.1477911071313));
#63717=CARTESIAN_POINT('Ctrl Pts',(-0.699026613519106,4.90050762812279,
84.0948708530493));
#63718=CARTESIAN_POINT('Ctrl Pts',(0.92034574921447,5.13150298527765,84.0419505989674));
#63719=CARTESIAN_POINT('Ctrl Pts',(2.66553384503535,4.48042918406423,83.9890303448854));
#63720=CARTESIAN_POINT('Ctrl Pts',(3.73791967339092,3.24523363926685,83.9361100908034));
#63721=CARTESIAN_POINT('Ctrl Pts',(4.81030550174656,2.01003809446939,83.8831898367214));
#63722=CARTESIAN_POINT('Ctrl Pts',(5.20988906263709,0.190720806087873,83.8302695826395));
#63723=CARTESIAN_POINT('Ctrl Pts',(4.75381130414694,-1.38017403364147,83.7773493285575));
#63724=CARTESIAN_POINT('Ctrl Pts',(4.29773354565674,-2.951068873371,83.7244290744756));
#63725=CARTESIAN_POINT('Ctrl Pts',(2.9859944677857,-4.27354126444818,83.6715088203937));
#63726=CARTESIAN_POINT('Ctrl Pts',(1.41886773993217,-4.74240598011873,83.6185885663117));
#63727=CARTESIAN_POINT('Ctrl Pts',(-0.148258987921171,-5.21127069578923,
83.5656683122296));
#63728=CARTESIAN_POINT('Ctrl Pts',(-1.97077336575683,-4.82652773605328,
83.5127480581476));
#63729=CARTESIAN_POINT('Ctrl Pts',(-3.21466593691877,-3.76424222358033,
83.4598278040656));
#63730=CARTESIAN_POINT('Ctrl Pts',(-4.29203775090064,-2.84416560597453,
83.4139920209293));
#63731=CARTESIAN_POINT('Ctrl Pts',(-4.93533906889132,-1.41581012896607,
83.3681562377931));
#63732=CARTESIAN_POINT('Ctrl Pts',(-4.94676006163664,0.00350952918951444,
83.3223204546568));
#63733=CARTESIAN_POINT('Ctrl Pts',(-4.94604776483535,0.00378542647206983,
83.1776795453431));
#63734=CARTESIAN_POINT('Ctrl Pts',(-4.93422874929891,-1.38971889629444,
83.2226647538174));
#63735=CARTESIAN_POINT('Ctrl Pts',(-4.31736833349613,-2.79238139987207,
83.2676499622918));
#63736=CARTESIAN_POINT('Ctrl Pts',(-3.27460228178232,-3.71222020633235,
83.3126351707661));
#63737=CARTESIAN_POINT('Ctrl Pts',(-2.04790029959144,-4.7943115204161,83.3655554248481));
#63738=CARTESIAN_POINT('Ctrl Pts',(-0.231787973272793,-5.20822364766616,
83.4184756789301));
#63739=CARTESIAN_POINT('Ctrl Pts',(1.34265411435701,-4.76454397765274,83.4713959330121));
#63740=CARTESIAN_POINT('Ctrl Pts',(2.91709620198673,-4.32086430763936,83.524316187094));
#63741=CARTESIAN_POINT('Ctrl Pts',(4.24986805092773,-3.01959284036256,83.577236441176));
#63742=CARTESIAN_POINT('Ctrl Pts',(4.73107261188716,-1.45621146364564,83.630156695258));
#63743=CARTESIAN_POINT('Ctrl Pts',(5.21227717284655,0.107169913071196,83.6830769493399));
#63744=CARTESIAN_POINT('Ctrl Pts',(4.84191444582465,1.93266119922796,83.7359972034218));
#63745=CARTESIAN_POINT('Ctrl Pts',(3.78946863845564,3.18489006691465,83.7889174575038));
#63746=CARTESIAN_POINT('Ctrl Pts',(2.73702283108663,4.43711893460135,83.8418377115857));
#63747=CARTESIAN_POINT('Ctrl Pts',(1.00249394337044,5.11608538381779,83.8947579656677));
#63748=CARTESIAN_POINT('Ctrl Pts',(-0.620372201325573,4.91108329901265,
83.9476782197497));
#63749=CARTESIAN_POINT('Ctrl Pts',(-2.24323834602159,4.70608121420751,84.0005984738317));
#63750=CARTESIAN_POINT('Ctrl Pts',(-3.75444174769753,3.6171105953808,84.0535187279136));
#63751=CARTESIAN_POINT('Ctrl Pts',(-4.4624305684118,2.14250236754745,84.1064389819956));
#63752=CARTESIAN_POINT('Ctrl Pts',(-4.78012570742429,1.48080284317098,84.1301858364447));
#63753=CARTESIAN_POINT('Ctrl Pts',(-4.93608736949663,0.741452199377731,
84.1539326908939));
#63754=CARTESIAN_POINT('Ctrl Pts',(-4.93425329604086,0.00136738585504144,
84.1776795453431));
#63755=CARTESIAN_POINT('Origin',(0.,0.,16.));
#63756=CARTESIAN_POINT('',(-4.93983901057914,-0.00407131671605609,85.3223204546568));
#63757=CARTESIAN_POINT('',(-4.94096920053978,-0.0044629540342261,85.1776795453431));
#63758=CARTESIAN_POINT('',(-4.942,-6.05220448138622E-16,16.));
#63759=CARTESIAN_POINT('Ctrl Pts',(-4.93983901057914,-0.00407131671605609,
85.3223204546568));
#63760=CARTESIAN_POINT('Ctrl Pts',(-4.92935782359351,1.19852489561668,85.283612366028));
#63761=CARTESIAN_POINT('Ctrl Pts',(-4.48753687762877,2.40778661262928,85.2449042773993));
#63762=CARTESIAN_POINT('Ctrl Pts',(-3.69010132050912,3.2995468819145,85.2061961887705));
#63763=CARTESIAN_POINT('Ctrl Pts',(-2.59987718928131,4.51872823916,85.1532759346885));
#63764=CARTESIAN_POINT('Ctrl Pts',(-0.844961773498813,5.14445691330988,
85.1003556806066));
#63765=CARTESIAN_POINT('Ctrl Pts',(0.770932612771407,4.88981272332166,85.0474354265247));
#63766=CARTESIAN_POINT('Ctrl Pts',(2.38682699904172,4.63516853333343,84.9945151724427));
#63767=CARTESIAN_POINT('Ctrl Pts',(3.86370035579973,3.500151479207,84.9415949183607));
#63768=CARTESIAN_POINT('Ctrl Pts',(4.52604489048226,2.00446382425534,84.8886746642787));
#63769=CARTESIAN_POINT('Ctrl Pts',(5.18838942516471,0.508776169303851,84.8357544101967));
#63770=CARTESIAN_POINT('Ctrl Pts',(5.0362051377719,-1.34758208647277,84.7828341561149));
#63771=CARTESIAN_POINT('Ctrl Pts',(4.13896054991356,-2.7152702523835,84.7299139020329));
#63772=CARTESIAN_POINT('Ctrl Pts',(3.24171596205511,-4.08295841829439,84.6769936479509));
#63773=CARTESIAN_POINT('Ctrl Pts',(1.59941107373096,-4.96197649433929,84.6240733938688));
#63774=CARTESIAN_POINT('Ctrl Pts',(-0.0363198163526684,-4.94999030922869,
84.5711531397869));
#63775=CARTESIAN_POINT('Ctrl Pts',(-1.67205070643629,-4.93800412411811,
84.518232885705));
#63776=CARTESIAN_POINT('Ctrl Pts',(-3.30120759827939,-4.03501367785208,
84.4653126316231));
#63777=CARTESIAN_POINT('Ctrl Pts',(-4.17831066843813,-2.65428404280099,
84.4123923775412));
#63778=CARTESIAN_POINT('Ctrl Pts',(-4.67592959505013,-1.87093574279885,
84.3823684032464));
#63779=CARTESIAN_POINT('Ctrl Pts',(-4.93147825958796,-0.9338132749143,84.3523444289516));
#63780=CARTESIAN_POINT('Ctrl Pts',(-4.93450205841395,0.0017791821159216,
84.3223204546568));
#63781=CARTESIAN_POINT('Ctrl Pts',(-4.93425329604086,0.00136738585504144,
84.1776795453431));
#63782=CARTESIAN_POINT('Ctrl Pts',(-4.93200010676076,-0.907838929165127,
84.2068529449759));
#63783=CARTESIAN_POINT('Ctrl Pts',(-4.6915933103023,-1.81815329167953,84.2360263446087));
#63784=CARTESIAN_POINT('Ctrl Pts',(-4.22033403606684,-2.58696080038834,
84.2651997442415));
#63785=CARTESIAN_POINT('Ctrl Pts',(-3.36547444325506,-3.98156990365044,
84.3181199983235));
#63786=CARTESIAN_POINT('Ctrl Pts',(-1.75098101787896,-4.91054227333463,
84.3710402524054));
#63787=CARTESIAN_POINT('Ctrl Pts',(-0.115662974249316,-4.94876105553069,
84.4239605064874));
#63788=CARTESIAN_POINT('Ctrl Pts',(1.51965506938033,-4.98697983772675,84.4768807605693));
#63789=CARTESIAN_POINT('Ctrl Pts',(3.17579773126353,-4.1344450324347,84.5298010146513));
#63790=CARTESIAN_POINT('Ctrl Pts',(4.09487421234139,-2.78129899063739,84.5827212687333));
#63791=CARTESIAN_POINT('Ctrl Pts',(5.01395069341925,-1.42815294884008,84.6356415228152));
#63792=CARTESIAN_POINT('Ctrl Pts',(5.19596099369178,0.425604329462498,84.6885617768972));
#63793=CARTESIAN_POINT('Ctrl Pts',(4.55764242829978,1.93168321282745,84.7414820309791));
#63794=CARTESIAN_POINT('Ctrl Pts',(3.91932386290774,3.43776209619249,84.7944022850611));
#63795=CARTESIAN_POINT('Ctrl Pts',(2.46067643185109,4.59616258461988,84.8473225391431));
#63796=CARTESIAN_POINT('Ctrl Pts',(0.849145831707845,4.87674842560418,84.9002427932251));
#63797=CARTESIAN_POINT('Ctrl Pts',(-0.762384768435213,5.15733426658845,
84.9531630473071));
#63798=CARTESIAN_POINT('Ctrl Pts',(-2.52679853766482,4.5601054601299,85.006083301389));
#63799=CARTESIAN_POINT('Ctrl Pts',(-3.63657003853315,3.35842910333814,85.059003555471));
#63800=CARTESIAN_POINT('Ctrl Pts',(-4.46614045337841,2.46015846561364,85.0985622187617));
#63801=CARTESIAN_POINT('Ctrl Pts',(-4.92991110676884,1.22413577549367,85.1381208820524));
#63802=CARTESIAN_POINT('Ctrl Pts',(-4.94096920053978,-0.0044629540342261,
85.1776795453431));
#63803=CARTESIAN_POINT('Origin',(0.,0.,24.1514101080949));
#63804=CARTESIAN_POINT('',(-4.37008825460381,-0.00360173951420115,85.6514101080948));
#63805=CARTESIAN_POINT('',(-4.37741404908174,0.00054794132368214,85.8485898919049));
#63806=CARTESIAN_POINT('',(-4.372,3.82579154166093E-12,24.1514101080949));
#63807=CARTESIAN_POINT('',(2.54472701347433,-3.56250531650779,85.9999999999999));
#63808=CARTESIAN_POINT('Ctrl Pts',(-4.37008825460381,-0.00360173951420056,
85.6514101080948));
#63809=CARTESIAN_POINT('Ctrl Pts',(-4.37349270028371,-0.394222905349127,
85.665622273548));
#63810=CARTESIAN_POINT('Ctrl Pts',(-4.14658524106498,-2.2356015936124,85.7327546930832));
#63811=CARTESIAN_POINT('Ctrl Pts',(-1.63914477126166,-4.84388062782939,
85.8489513237184));
#63812=CARTESIAN_POINT('Ctrl Pts',(1.44818750565376,-4.33531680853971,85.9509357889001));
#63813=CARTESIAN_POINT('Ctrl Pts',(2.54472701347433,-3.56250531650779,85.9999999999999));
#63814=CARTESIAN_POINT('',(-2.53835875722777,-3.5596515025498,86.));
#63815=CARTESIAN_POINT('Origin',(0.,0.,86.));
#63816=CARTESIAN_POINT('Ctrl Pts',(-4.37741404908174,0.000547941323682409,
85.8485898919049));
#63817=CARTESIAN_POINT('Ctrl Pts',(-4.37702756934774,-0.658293262144059,
85.8725998008956));
#63818=CARTESIAN_POINT('Ctrl Pts',(-4.04502790407186,-2.04740376323306,
85.9230698369273));
#63819=CARTESIAN_POINT('Ctrl Pts',(-3.130164636136,-3.13763950664809,85.973539872959));
#63820=CARTESIAN_POINT('Ctrl Pts',(-2.53835875722777,-3.5596515025498,86.));
#63821=CARTESIAN_POINT('Origin',(0.,0.,24.1514101080949));
#63822=CARTESIAN_POINT('',(-4.3653668553998,0.00157397495328755,84.6514101080948));
#63823=CARTESIAN_POINT('',(-4.37108809080528,-0.00394820619502134,84.8485898919049));
#63824=CARTESIAN_POINT('',(-4.372,3.82579154166093E-12,24.1514101080949));
#63825=CARTESIAN_POINT('Ctrl Pts',(-4.3653668553998,0.00157397495328733,
84.6514101080948));
#63826=CARTESIAN_POINT('Ctrl Pts',(-4.36269181524081,-0.826109194237039,
84.6814340823896));
#63827=CARTESIAN_POINT('Ctrl Pts',(-3.73813921667308,-3.11640593107392,
84.7643783107663));
#63828=CARTESIAN_POINT('Ctrl Pts',(-0.0379465312430282,-5.16730640666113,
84.9002427932251));
#63829=CARTESIAN_POINT('Ctrl Pts',(4.32070804489202,-2.83440452778566,85.059003555471));
#63830=CARTESIAN_POINT('Ctrl Pts',(4.72460304963626,2.09234474027741,85.2177643177169));
#63831=CARTESIAN_POINT('Ctrl Pts',(0.805001482004623,5.10466438453535,85.3765250799626));
#63832=CARTESIAN_POINT('Ctrl Pts',(-3.43558144629758,3.5926517202867,85.5210736767555));
#63833=CARTESIAN_POINT('Ctrl Pts',(-4.3608159459227,1.06028952724385,85.6127020194661));
#63834=CARTESIAN_POINT('Ctrl Pts',(-4.37008825460381,-0.00360173951420056,
85.6514101080948));
#63835=CARTESIAN_POINT('Ctrl Pts',(-4.37108809080528,-0.00394820619502242,
84.8485898919049));
#63836=CARTESIAN_POINT('Ctrl Pts',(-4.37439235100703,-0.371064815037356,
84.8619514826962));
#63837=CARTESIAN_POINT('Ctrl Pts',(-4.16412636077677,-2.18847582560682,
84.9282333275694));
#63838=CARTESIAN_POINT('Ctrl Pts',(-1.63279460579437,-4.90302030367583,
85.0474354265246));
#63839=CARTESIAN_POINT('Ctrl Pts',(3.23428855022947,-4.03017982392474,85.2061961887705));
#63840=CARTESIAN_POINT('Ctrl Pts',(5.13873193725801,0.529582954402255,85.3649569510164));
#63841=CARTESIAN_POINT('Ctrl Pts',(2.34489518331184,4.6077777382683,85.5237177132623));
#63842=CARTESIAN_POINT('Ctrl Pts',(-2.60449736313211,4.46265913321349,85.6824784755082));
#63843=CARTESIAN_POINT('Ctrl Pts',(-4.34126539015093,1.58670061603872,85.7907692017224));
#63844=CARTESIAN_POINT('Ctrl Pts',(-4.37745348944865,0.0677828737684449,
85.8461396738546));
#63845=CARTESIAN_POINT('Ctrl Pts',(-4.37741404908174,0.000547941323682409,
85.8485898919049));
#63846=CARTESIAN_POINT('Origin',(0.,0.,24.1514101080949));
#63847=CARTESIAN_POINT('',(-4.37621104602901,0.00310474739351271,83.6514101080948));
#63848=CARTESIAN_POINT('',(-4.36514678476137,0.00120967441979231,83.8485898919049));
#63849=CARTESIAN_POINT('',(-4.372,3.82579154166093E-12,24.1514101080949));
#63850=CARTESIAN_POINT('Ctrl Pts',(-4.37621104602901,0.00310474739351276,
83.6514101080948));
#63851=CARTESIAN_POINT('Ctrl Pts',(-4.36610732682993,-1.25251353375917,
83.6972458912311));
#63852=CARTESIAN_POINT('Ctrl Pts',(-3.13993685867563,-3.97504379283746,
83.7960019284495));
#63853=CARTESIAN_POINT('Ctrl Pts',(1.4811502559097,-4.9505810809301,83.9476782197498));
#63854=CARTESIAN_POINT('Ctrl Pts',(4.96248771955931,-1.44075755171813,84.1064389819956));
#63855=CARTESIAN_POINT('Ctrl Pts',(3.90199844707087,3.38768549854763,84.2651997442416));
#63856=CARTESIAN_POINT('Ctrl Pts',(-0.729706746127024,5.11562640844579,
84.4239605064874));
#63857=CARTESIAN_POINT('Ctrl Pts',(-3.94395824097378,2.72022390956171,84.5526972944385));
#63858=CARTESIAN_POINT('Ctrl Pts',(-4.36740684075686,0.63276507679951,84.6285138283076));
#63859=CARTESIAN_POINT('Ctrl Pts',(-4.3653668553998,0.00157397495328733,
84.6514101080948));
#63860=CARTESIAN_POINT('Ctrl Pts',(-4.36514678476137,0.00120967441979238,
83.8485898919049));
#63861=CARTESIAN_POINT('Ctrl Pts',(-4.36315347364677,-0.803130675494322,
83.8777632915377));
#63862=CARTESIAN_POINT('Ctrl Pts',(-3.76467753114223,-3.06929475283447,
83.9598569452526));
#63863=CARTESIAN_POINT('Ctrl Pts',(-0.120745397495975,-5.1659971710397,
84.0948708530492));
#63864=CARTESIAN_POINT('Ctrl Pts',(4.27463443926266,-2.90338152834273,84.2536316152952));
#63865=CARTESIAN_POINT('Ctrl Pts',(4.75768727179541,2.01646478129229,84.412392377541));
#63866=CARTESIAN_POINT('Ctrl Pts',(0.886457060193665,5.09084373843816,84.571153139787));
#63867=CARTESIAN_POINT('Ctrl Pts',(-3.40216585276062,3.63920626636618,84.7165523112416));
#63868=CARTESIAN_POINT('Ctrl Pts',(-4.36130541456655,1.08294650151228,84.8090312286142));
#63869=CARTESIAN_POINT('Ctrl Pts',(-4.37108809080528,-0.00394820619502242,
84.8485898919049));
#63870=CARTESIAN_POINT('Origin',(0.,0.,24.1514101080949));
#63871=CARTESIAN_POINT('',(-4.37496612397431,-0.00354270330085218,82.6514101080948));
#63872=CARTESIAN_POINT('',(-4.37558090405915,0.00334882326136696,82.8485898919049));
#63873=CARTESIAN_POINT('',(-4.372,3.82579154166093E-12,24.1514101080949));
#63874=CARTESIAN_POINT('Ctrl Pts',(-4.37496612397431,-0.00354270330085171,
82.6514101080948));
#63875=CARTESIAN_POINT('Ctrl Pts',(-4.37707015387208,-0.242795066330439,
82.6601374459907));
#63876=CARTESIAN_POINT('Ctrl Pts',(-4.25038678075279,-1.93057999813071,
82.7217850379685));
#63877=CARTESIAN_POINT('Ctrl Pts',(-2.05392817541576,-4.74166978382725,
82.8363528840287));
#63878=CARTESIAN_POINT('Ctrl Pts',(2.86960084768762,-4.29737645901297,82.9951136462743));
#63879=CARTESIAN_POINT('Ctrl Pts',(5.16678358952832,0.0800071275065655,
83.1538744085204));
#63880=CARTESIAN_POINT('Ctrl Pts',(2.73516803922529,4.38416562959496,83.312635170766));
#63881=CARTESIAN_POINT('Ctrl Pts',(-2.19975659925683,4.67580205641259,83.4713959330121));
#63882=CARTESIAN_POINT('Ctrl Pts',(-4.27789107195956,1.83931825768632,83.5843209121216));
#63883=CARTESIAN_POINT('Ctrl Pts',(-4.37777269721528,0.197175637492073,
83.6443256371492));
#63884=CARTESIAN_POINT('Ctrl Pts',(-4.37621104602901,0.00310474739351276,
83.6514101080948));
#63885=CARTESIAN_POINT('Ctrl Pts',(-4.37558090405915,0.0033488232613671,
82.8485898919049));
#63886=CARTESIAN_POINT('Ctrl Pts',(-4.36512506919086,-1.22943160958811,
82.8935751003793));
#63887=CARTESIAN_POINT('Ctrl Pts',(-3.17743944272853,-3.93007838737006,
82.9914805629356));
#63888=CARTESIAN_POINT('Ctrl Pts',(1.40159167776471,-4.9736903294079,83.142306279574));
#63889=CARTESIAN_POINT('Ctrl Pts',(4.93874982643145,-1.52013376024582,83.3010670418199));
#63890=CARTESIAN_POINT('Ctrl Pts',(3.95581224496304,3.32469499516411,83.4598278040656));
#63891=CARTESIAN_POINT('Ctrl Pts',(-0.647603556591826,5.12666260907039,
83.6185885663118));
#63892=CARTESIAN_POINT('Ctrl Pts',(-3.92132004033239,2.76762804019117,83.7481759289246));
#63893=CARTESIAN_POINT('Ctrl Pts',(-4.36676931999915,0.655934645021535,
83.8248430374557));
#63894=CARTESIAN_POINT('Ctrl Pts',(-4.36514678476137,0.00120967441979238,
83.8485898919049));
#63895=CARTESIAN_POINT('Origin',(0.,0.,24.1514101080949));
#63896=CARTESIAN_POINT('',(-4.36499281949393,-0.000862724152283187,81.6514101080949));
#63897=CARTESIAN_POINT('',(-4.37562514566675,-0.00333327265474082,81.8485898919049));
#63898=CARTESIAN_POINT('',(-4.372,3.82579154166093E-12,24.1514101080949));
#63899=CARTESIAN_POINT('Ctrl Pts',(-4.36499281949393,-0.000862724152282945,
81.6514101080949));
#63900=CARTESIAN_POINT('Ctrl Pts',(-4.36618629939077,-0.677492060307118,
81.6759492548323));
#63901=CARTESIAN_POINT('Ctrl Pts',(-3.8997785113075,-2.81175799367349,81.7534086556517));
#63902=CARTESIAN_POINT('Ctrl Pts',(-0.57097184883837,-5.13576134197884,
81.8837883105532));
#63903=CARTESIAN_POINT('Ctrl Pts',(4.00502195951943,-3.26524922770216,82.0425490727989));
#63904=CARTESIAN_POINT('Ctrl Pts',(4.91549733690694,1.59371871934676,82.2013098350451));
#63905=CARTESIAN_POINT('Ctrl Pts',(1.32715940311121,4.99406661129702,82.3600705972907));
#63906=CARTESIAN_POINT('Ctrl Pts',(-3.21180689907642,3.88802958864094,82.510104021641));
#63907=CARTESIAN_POINT('Ctrl Pts',(-4.36431187659278,1.20796758228371,82.6072171919088));
#63908=CARTESIAN_POINT('Ctrl Pts',(-4.37496612397431,-0.00354270330085171,
82.6514101080948));
#63909=CARTESIAN_POINT('Ctrl Pts',(-4.37562514566675,-0.00333327265474043,
81.8485898919049));
#63910=CARTESIAN_POINT('Ctrl Pts',(-4.37745016253379,-0.219183427450699,
81.8564666551388));
#63911=CARTESIAN_POINT('Ctrl Pts',(-4.26482187642182,-1.88331740650866,
81.9172636724547));
#63912=CARTESIAN_POINT('Ctrl Pts',(-2.12968395259116,-4.7081313086182,82.0309809438528));
#63913=CARTESIAN_POINT('Ctrl Pts',(2.80033539806548,-4.3428303941221,82.1897417060986));
#63914=CARTESIAN_POINT('Ctrl Pts',(5.16740226597732,-0.00283844241944707,
82.3485024683445));
#63915=CARTESIAN_POINT('Ctrl Pts',(2.80510471878759,4.33975132503298,82.5072632305904));
#63916=CARTESIAN_POINT('Ctrl Pts',(-2.12451031000386,4.71046814615349,82.6660239928362));
#63917=CARTESIAN_POINT('Ctrl Pts',(-4.26384621089875,1.88655500314254,82.7797995466078));
#63918=CARTESIAN_POINT('Ctrl Pts',(-4.37742523310327,0.220801832606586,
82.8406548462974));
#63919=CARTESIAN_POINT('Ctrl Pts',(-4.37558090405915,0.0033488232613671,
82.8485898919049));
#63920=CARTESIAN_POINT('Origin',(0.,0.,24.1514101080949));
#63921=CARTESIAN_POINT('',(-4.37180197783241,0.00399615447510604,80.6514101080948));
#63922=CARTESIAN_POINT('',(-4.3651608225263,-0.00123442373144794,80.8485898919049));
#63923=CARTESIAN_POINT('',(-4.372,3.82579154166093E-12,24.1514101080949));
#63924=CARTESIAN_POINT('Ctrl Pts',(-4.37180197783241,0.00399615447510625,
80.6514101080948));
#63925=CARTESIAN_POINT('Ctrl Pts',(-4.36165896025063,-1.10425130818043,
80.6917610636739));
#63926=CARTESIAN_POINT('Ctrl Pts',(-3.37083349090091,-3.68210362881494,
80.7850322733349));
#63927=CARTESIAN_POINT('Ctrl Pts',(0.962330231331446,-5.07700442602626,
80.9312237370778));
#63928=CARTESIAN_POINT('Ctrl Pts',(4.78729812901886,-1.94520694012218,81.0899844993237));
#63929=CARTESIAN_POINT('Ctrl Pts',(4.2307845491307,2.96690335452649,81.2487452615696));
#63930=CARTESIAN_POINT('Ctrl Pts',(-0.19787228117179,5.16361307382143,81.4075060238155));
#63931=CARTESIAN_POINT('Ctrl Pts',(-3.78889879581372,3.02535473653369,81.541727639324));
#63932=CARTESIAN_POINT('Ctrl Pts',(-4.36361248294727,0.781702783413628,
81.6230290007504));
#63933=CARTESIAN_POINT('Ctrl Pts',(-4.36499281949393,-0.000862724152282945,
81.6514101080949));
#63934=CARTESIAN_POINT('Ctrl Pts',(-4.3651608225263,-0.00123442373144732,
80.8485898919049));
#63935=CARTESIAN_POINT('Ctrl Pts',(-4.36681289312482,-0.654347754103861,
80.8722784639804));
#63936=CARTESIAN_POINT('Ctrl Pts',(-3.92288549979199,-2.76438197736347,
80.9488872901379));
#63937=CARTESIAN_POINT('Ctrl Pts',(-0.653236375128765,-5.12594736724498,
81.0784163703773));
#63938=CARTESIAN_POINT('Ctrl Pts',(3.95215792026738,-3.32903919274863,81.2371771326234));
#63939=CARTESIAN_POINT('Ctrl Pts',(4.94041656702063,1.51470733791976,81.3959378948691));
#63940=CARTESIAN_POINT('Ctrl Pts',(1.40705506422376,4.97214744531344,81.5546986571151));
#63941=CARTESIAN_POINT('Ctrl Pts',(-3.17488990257063,3.9331654538798,81.7055826561271));
#63942=CARTESIAN_POINT('Ctrl Pts',(-4.36518873567112,1.23101187436481,81.8035464010569));
#63943=CARTESIAN_POINT('Ctrl Pts',(-4.37562514566675,-0.00333327265474043,
81.8485898919049));
#63944=CARTESIAN_POINT('Origin',(0.,0.,24.1514101080949));
#63945=CARTESIAN_POINT('',(-4.37845870912757,-0.00160159003492085,79.6514101080949));
#63946=CARTESIAN_POINT('',(-4.37110144318797,0.00398541688994905,79.8485898919049));
#63947=CARTESIAN_POINT('',(-4.372,3.82579154166093E-12,24.1514101080949));
#63948=CARTESIAN_POINT('Ctrl Pts',(-4.37845870912757,-0.00160159003492056,
79.6514101080949));
#63949=CARTESIAN_POINT('Ctrl Pts',(-4.37887661134401,-0.0903064267712891,
79.6546526184335));
#63950=CARTESIAN_POINT('Ctrl Pts',(-4.3362288360819,-1.62633270599671,79.7108153828541));
#63951=CARTESIAN_POINT('Ctrl Pts',(-2.53231305975701,-4.50438053270811,
79.8198984013567));
#63952=CARTESIAN_POINT('Ctrl Pts',(2.41077833593552,-4.57057996659486,79.9786591636024));
#63953=CARTESIAN_POINT('Ctrl Pts',(5.14745176039643,-0.453645004871452,
80.1374199258484));
#63954=CARTESIAN_POINT('Ctrl Pts',(3.1730201027819,4.07847972207792,80.2961806880942));
#63955=CARTESIAN_POINT('Ctrl Pts',(-1.70545647406065,4.87785522859546,80.4549414503402));
#63956=CARTESIAN_POINT('Ctrl Pts',(-4.17984164299754,2.14436901967187,80.573351257007));
#63957=CARTESIAN_POINT('Ctrl Pts',(-4.37496152173606,0.349214575534816,
80.6388408095919));
#63958=CARTESIAN_POINT('Ctrl Pts',(-4.37180197783241,0.00399615447510625,
80.6514101080948));
#63959=CARTESIAN_POINT('Ctrl Pts',(-4.37110144318797,0.00398541688994905,
79.8485898919049));
#63960=CARTESIAN_POINT('Ctrl Pts',(-4.36133704968111,-1.0813445883965,79.888090272822));
#63961=CARTESIAN_POINT('Ctrl Pts',(-3.40435481309659,-3.63610732924809,
79.980510907821));
#63962=CARTESIAN_POINT('Ctrl Pts',(0.880810665839244,-5.09178031191025,
80.125851796902));
#63963=CARTESIAN_POINT('Ctrl Pts',(4.75549683016874,-2.02170820645871,80.2846125591479));
#63964=CARTESIAN_POINT('Ctrl Pts',(4.27780703699033,2.89869300342805,80.4433733213939));
#63965=CARTESIAN_POINT('Ctrl Pts',(-0.11506242376767,5.16612183484124,80.6021340836397));
#63966=CARTESIAN_POINT('Ctrl Pts',(-3.76287956508864,3.07252682993506,80.7372062738101));
#63967=CARTESIAN_POINT('Ctrl Pts',(-4.36312216851904,0.804706986612936,
80.8193582098985));
#63968=CARTESIAN_POINT('Ctrl Pts',(-4.3651608225263,-0.00123442373144732,
80.8485898919049));
#63969=CARTESIAN_POINT('Origin',(0.,0.,24.1514101080949));
#63970=CARTESIAN_POINT('',(-4.36706479197461,-0.00298086264687759,78.6514101080949));
#63971=CARTESIAN_POINT('',(-4.37877376767475,-0.00119946029119966,78.8485898919049));
#63972=CARTESIAN_POINT('',(-4.372,3.82579154166093E-12,24.1514101080949));
#63973=CARTESIAN_POINT('Ctrl Pts',(-4.36706479197461,-0.00298086264687698,
78.6514101080949));
#63974=CARTESIAN_POINT('Ctrl Pts',(-4.37035845585727,-0.527750657057906,
78.670464427275));
#63975=CARTESIAN_POINT('Ctrl Pts',(-4.03993636744864,-2.50597397148776,
78.7424390005372));
#63976=CARTESIAN_POINT('Ctrl Pts',(-1.0979463908737,-5.04941255383462,78.8673338278812));
#63977=CARTESIAN_POINT('Ctrl Pts',(3.64665478912629,-3.66114220769932,79.0260945901272));
#63978=CARTESIAN_POINT('Ctrl Pts',(5.05372611759689,1.07791731796727,79.184855352373));
#63979=CARTESIAN_POINT('Ctrl Pts',(1.83547293516864,4.83043398881696,79.3436161146189));
#63980=CARTESIAN_POINT('Ctrl Pts',(-2.96262225304742,4.17564214514766,79.4991343665262));
#63981=CARTESIAN_POINT('Ctrl Pts',(-4.37205612685341,1.35742450024673,79.6017323643515));
#63982=CARTESIAN_POINT('Ctrl Pts',(-4.37845870912757,-0.00160159003492056,
79.6514101080949));
#63983=CARTESIAN_POINT('Ctrl Pts',(-4.37877376767475,-0.00119946029119964,
78.8485898919049));
#63984=CARTESIAN_POINT('Ctrl Pts',(-4.37901256877795,-0.0666227183370213,
78.8509818275816));
#63985=CARTESIAN_POINT('Ctrl Pts',(-4.34804095188971,-1.57926832145057,
78.9062940173403));
#63986=CARTESIAN_POINT('Ctrl Pts',(-2.60420306585193,-4.46320294918618,
79.0145264611808));
#63987=CARTESIAN_POINT('Ctrl Pts',(2.33719176176521,-4.60864284172174,79.1732872234268));
#63988=CARTESIAN_POINT('Ctrl Pts',(5.13951729856278,-0.536112032685121,
79.3320479856725));
#63989=CARTESIAN_POINT('Ctrl Pts',(3.23799961511593,4.02708488442023,79.4908087479186));
#63990=CARTESIAN_POINT('Ctrl Pts',(-1.62703422207133,4.90457070639472,79.6495695101643));
#63991=CARTESIAN_POINT('Ctrl Pts',(-4.16301218854004,2.19175778571074,79.7688298914932));
#63992=CARTESIAN_POINT('Ctrl Pts',(-4.37441880163748,0.372715810744746,
79.83517001874));
#63993=CARTESIAN_POINT('Ctrl Pts',(-4.37110144318797,0.00398541688994905,
79.8485898919049));
#63994=CARTESIAN_POINT('Origin',(0.,0.,24.1514101080949));
#63995=CARTESIAN_POINT('',(-4.36767022761989,0.00326609935392151,77.6514101080949));
#63996=CARTESIAN_POINT('',(-4.36757594524889,-0.00322601897944697,77.8485898919049));
#63997=CARTESIAN_POINT('',(-4.372,3.82579154166093E-12,24.1514101080949));
#63998=CARTESIAN_POINT('Ctrl Pts',(-4.36767022761989,0.00326609935392137,
77.6514101080949));
#63999=CARTESIAN_POINT('Ctrl Pts',(-4.36100748821687,-0.956637771051708,
77.6862762361166));
#64000=CARTESIAN_POINT('Ctrl Pts',(-3.57653367776381,-3.38339660944801,
77.7740626182202));
#64001=CARTESIAN_POINT('Ctrl Pts',(0.433232280173729,-5.14920995954434,
77.9147692544059));
#64002=CARTESIAN_POINT('Ctrl Pts',(4.56098553273524,-2.42888130344712,78.0735300166518));
#64003=CARTESIAN_POINT('Ctrl Pts',(4.51438550862023,2.51443371271033,78.2322907788977));
#64004=CARTESIAN_POINT('Ctrl Pts',(0.336081973315249,5.15646219061744,78.3910515411436));
#64005=CARTESIAN_POINT('Ctrl Pts',(-3.61142097688492,3.32845736892325,78.5307579842093));
#64006=CARTESIAN_POINT('Ctrl Pts',(-4.36121084329327,0.929711590329863,
78.6175441731931));
#64007=CARTESIAN_POINT('Ctrl Pts',(-4.36706479197461,-0.00298086264687698,
78.6514101080949));
#64008=CARTESIAN_POINT('Ctrl Pts',(-4.36757594524889,-0.00322601897944683,
77.8485898919049));
#64009=CARTESIAN_POINT('Ctrl Pts',(-4.37100704730013,-0.504422908173594,
77.8667936364231));
#64010=CARTESIAN_POINT('Ctrl Pts',(-4.05983800326864,-2.45852322858237,
77.9379176350233));
#64011=CARTESIAN_POINT('Ctrl Pts',(-1.17875882811733,-5.03116107861318,
78.0619618877055));
#64012=CARTESIAN_POINT('Ctrl Pts',(3.58748974126774,-3.71913585798031,78.2207226499514));
#64013=CARTESIAN_POINT('Ctrl Pts',(5.07035811814355,0.996756102360001,78.3794834121972));
#64014=CARTESIAN_POINT('Ctrl Pts',(1.91267986918918,4.80038643150889,78.5382441744432));
#64015=CARTESIAN_POINT('Ctrl Pts',(-2.92159273453857,4.2194430180671,78.6946130010123));
#64016=CARTESIAN_POINT('Ctrl Pts',(-4.37372922642899,1.38083068620526,78.7980615734996));
#64017=CARTESIAN_POINT('Ctrl Pts',(-4.37877376767475,-0.00119946029119964,
78.8485898919049));
#64018=CARTESIAN_POINT('Origin',(0.,0.,24.1514101080949));
#64019=CARTESIAN_POINT('',(-4.37882057798781,0.00112692768741051,76.6514101080949));
#64020=CARTESIAN_POINT('',(-4.36715155140556,0.00302605917446269,76.8485898919049));
#64021=CARTESIAN_POINT('',(-4.372,3.82579154166093E-12,24.1514101080949));
#64022=CARTESIAN_POINT('Ctrl Pts',(-4.37882057798781,0.00112692768741048,
76.6514101080949));
#64023=CARTESIAN_POINT('Ctrl Pts',(-4.37403747425012,-1.38495585300809,
76.7020880449581));
#64024=CARTESIAN_POINT('Ctrl Pts',(-2.91430837048911,-4.22712294708155,
76.8056862359034));
#64025=CARTESIAN_POINT('Ctrl Pts',(1.92621046639379,-4.79497306094723,76.9622046809306));
#64026=CARTESIAN_POINT('Ctrl Pts',(5.07314897115,-0.982452509068445,77.1209654431764));
#64027=CARTESIAN_POINT('Ctrl Pts',(3.5769865761566,3.7292385885125,77.2797262054224));
#64028=CARTESIAN_POINT('Ctrl Pts',(-1.19294319381297,5.02781661881079,77.4384869676682));
#64029=CARTESIAN_POINT('Ctrl Pts',(-4.06328911396928,2.45017653498889,77.5623816018925));
#64030=CARTESIAN_POINT('Ctrl Pts',(-4.37112027911439,0.500316573992826,
77.6333559820347));
#64031=CARTESIAN_POINT('Ctrl Pts',(-4.36767022761989,0.00326609935392137,
77.6514101080949));
#64032=CARTESIAN_POINT('Ctrl Pts',(-4.36715155140556,0.00302605917446276,
76.8485898919049));
#64033=CARTESIAN_POINT('Ctrl Pts',(-4.36117507900865,-0.933740289083742,
76.8826054452647));
#64034=CARTESIAN_POINT('Ctrl Pts',(-3.60625270295825,-3.33668347601213,
76.9695412527065));
#64035=CARTESIAN_POINT('Ctrl Pts',(0.350623091062388,-5.15549392607834,
77.1093973142301));
#64036=CARTESIAN_POINT('Ctrl Pts',(4.52145892049186,-2.50169210817825,77.268158076476));
#64037=CARTESIAN_POINT('Ctrl Pts',(4.55411743612604,2.44173474230699,77.4269188387219));
#64038=CARTESIAN_POINT('Ctrl Pts',(0.4187085668894,5.15041137287398,77.5856796009678));
#64039=CARTESIAN_POINT('Ctrl Pts',(-3.58180307113106,3.37518619718569,77.7262366186955));
#64040=CARTESIAN_POINT('Ctrl Pts',(-4.36103246255736,0.952610654051967,
77.8138733823412));
#64041=CARTESIAN_POINT('Ctrl Pts',(-4.36757594524889,-0.00322601897944683,
77.8485898919049));
#64042=CARTESIAN_POINT('Origin',(0.,0.,24.1514101080949));
#64043=CARTESIAN_POINT('',(-4.37097940507052,-0.00397941814148454,75.6514101080949));
#64044=CARTESIAN_POINT('',(-4.37851995085447,0.0015322273023494,75.8485898919049));
#64045=CARTESIAN_POINT('',(-4.372,3.82579154166093E-12,24.1514101080949));
#64046=CARTESIAN_POINT('Ctrl Pts',(-4.37097940507052,-0.00397941814148494,
75.6514101080949));
#64047=CARTESIAN_POINT('Ctrl Pts',(-4.3743208173595,-0.376847295339705,
75.6649795997177));
#64048=CARTESIAN_POINT('Ctrl Pts',(-4.16000539985281,-2.20009534110889,
75.7314693454226));
#64049=CARTESIAN_POINT('Ctrl Pts',(-1.61319567320764,-4.90913975519121,
75.8508793452094));
#64050=CARTESIAN_POINT('Ctrl Pts',(3.24934402869518,-4.01793688343129,76.0096401074552));
#64051=CARTESIAN_POINT('Ctrl Pts',(5.13798482303055,0.550604553524979,76.1684008697012));
#64052=CARTESIAN_POINT('Ctrl Pts',(2.32418496553848,4.61521588466023,76.3271616319469));
#64053=CARTESIAN_POINT('Ctrl Pts',(-2.61677996556865,4.45584066454958,76.485922394193));
#64054=CARTESIAN_POINT('Ctrl Pts',(-4.35007811558771,1.57099298812344,76.5940052195755));
#64055=CARTESIAN_POINT('Ctrl Pts',(-4.37903221319898,0.0624561269022633,
76.6491677908762));
#64056=CARTESIAN_POINT('Ctrl Pts',(-4.37882057798781,0.00112692768741048,
76.6514101080949));
#64057=CARTESIAN_POINT('Ctrl Pts',(-4.37851995085447,0.00153222730234961,
75.8485898919049));
#64058=CARTESIAN_POINT('Ctrl Pts',(-4.37234073616906,-1.36153629732671,
75.8984172541062));
#64059=CARTESIAN_POINT('Ctrl Pts',(-2.9554520406374,-4.18336396709743,76.0011648703895));
#64060=CARTESIAN_POINT('Ctrl Pts',(1.84908863423975,-4.82523837717284,76.1568327407549));
#64061=CARTESIAN_POINT('Ctrl Pts',(5.05674607440601,-1.06366033713594,76.3155935030006));
#64062=CARTESIAN_POINT('Ctrl Pts',(3.63631504695578,3.6714121333759,76.4743542652466));
#64063=CARTESIAN_POINT('Ctrl Pts',(-1.11218258415778,5.04629607467818,76.6331150274925));
#64064=CARTESIAN_POINT('Ctrl Pts',(-4.04347203458464,2.49762731386996,76.7578602363785));
#64065=CARTESIAN_POINT('Ctrl Pts',(-4.37047307379395,0.523649295054832,
76.8296851911827));
#64066=CARTESIAN_POINT('Ctrl Pts',(-4.36715155140556,0.00302605917446276,
76.8485898919049));
#64067=CARTESIAN_POINT('Origin',(0.,0.,24.1514101080949));
#64068=CARTESIAN_POINT('',(-4.36519646031047,0.00129875109319553,74.6514101080949));
#64069=CARTESIAN_POINT('',(-4.37167806635839,-0.00399716320838295,74.8485898919049));
#64070=CARTESIAN_POINT('',(-4.372,3.82579154166093E-12,24.1514101080949));
#64071=CARTESIAN_POINT('Ctrl Pts',(-4.36519646031047,0.00129875109319548,
74.6514101080949));
#64072=CARTESIAN_POINT('Ctrl Pts',(-4.36303959174397,-0.808751209913892,
74.6807914085593));
#64073=CARTESIAN_POINT('Ctrl Pts',(-3.75824647517972,-3.08081912741743,
74.7630929631056));
#64074=CARTESIAN_POINT('Ctrl Pts',(-0.100492272925181,-5.16642571988962,
74.898314771734));
#64075=CARTESIAN_POINT('Ctrl Pts',(4.28596496729055,-2.88661700182285,75.0570755339799));
#64076=CARTESIAN_POINT('Ctrl Pts',(4.74977615293751,2.03511176917654,75.2158362962258));
#64077=CARTESIAN_POINT('Ctrl Pts',(0.866447119614458,5.09424408572719,75.3745970584717));
#64078=CARTESIAN_POINT('Ctrl Pts',(-3.41018887347201,3.62800267766814,75.5197883290947));
#64079=CARTESIAN_POINT('Ctrl Pts',(-4.36128949737787,1.07731645292395,75.6120593456358));
#64080=CARTESIAN_POINT('Ctrl Pts',(-4.37097940507052,-0.00397941814148494,
75.6514101080949));
#64081=CARTESIAN_POINT('Ctrl Pts',(-4.37167806635839,-0.00399716320838302,
74.8485898919049));
#64082=CARTESIAN_POINT('Ctrl Pts',(-4.37486787390589,-0.3533501983587,74.8613088088659));
#64083=CARTESIAN_POINT('Ctrl Pts',(-4.1769137234544,-2.15270356402942,74.9269479799088));
#64084=CARTESIAN_POINT('Ctrl Pts',(-1.69169300421356,-4.88264569196979,
75.0455074050335));
#64085=CARTESIAN_POINT('Ctrl Pts',(3.18450981172911,-4.06951488912588,75.2042681672795));
#64086=CARTESIAN_POINT('Ctrl Pts',(5.14615197585861,0.468160245196775,75.3630289295254));
#64087=CARTESIAN_POINT('Ctrl Pts',(2.39787866042351,4.57736082297456,75.5217896917712));
#64088=CARTESIAN_POINT('Ctrl Pts',(-2.54500644918866,4.49722095825909,75.6805504540172));
#64089=CARTESIAN_POINT('Ctrl Pts',(-4.33833518668749,1.61805156266242,75.7894838540617));
#64090=CARTESIAN_POINT('Ctrl Pts',(-4.37890350804243,0.0861408316175627,
75.8454970000243));
#64091=CARTESIAN_POINT('Ctrl Pts',(-4.37851995085447,0.00153222730234961,
75.8485898919049));
#64092=CARTESIAN_POINT('Origin',(0.,0.,24.1514101080949));
#64093=CARTESIAN_POINT('',(-4.37573799308197,0.00329254665532695,73.6514101080949));
#64094=CARTESIAN_POINT('',(-4.36501807785945,0.000928765700389245,73.8485898919049));
#64095=CARTESIAN_POINT('',(-4.372,3.82579154166093E-12,24.1514101080949));
#64096=CARTESIAN_POINT('Ctrl Pts',(-4.37573799308197,0.00329254665532727,
73.6514101080949));
#64097=CARTESIAN_POINT('Ctrl Pts',(-4.36535453025917,-1.23506946531353,
73.6966032174009));
#64098=CARTESIAN_POINT('Ctrl Pts',(-3.16833117156948,-3.94108625070045,
73.7947165807888));
#64099=CARTESIAN_POINT('Ctrl Pts',(1.42107208653042,-4.9681593715318,73.9457501982587));
#64100=CARTESIAN_POINT('Ctrl Pts',(4.94466868411869,-1.50076814343543,74.1045109605046));
#64101=CARTESIAN_POINT('Ctrl Pts',(3.94275346512999,3.34017193109278,74.2632717227505));
#64102=CARTESIAN_POINT('Ctrl Pts',(-0.667690158118302,5.12408462740484,
74.4220324849963));
#64103=CARTESIAN_POINT('Ctrl Pts',(-3.9268970087966,2.75604594892831,74.5514119467779));
#64104=CARTESIAN_POINT('Ctrl Pts',(-4.3669244447204,0.650273716756605,74.6278711544774));
#64105=CARTESIAN_POINT('Ctrl Pts',(-4.36519646031047,0.00129875109319548,
74.6514101080949));
#64106=CARTESIAN_POINT('Ctrl Pts',(-4.36501807785945,0.000928765700389245,
73.8485898919049));
#64107=CARTESIAN_POINT('Ctrl Pts',(-4.36352375843653,-0.785750920308218,
73.8771206177074));
#64108=CARTESIAN_POINT('Ctrl Pts',(-3.78436122884701,-3.0336560998423,73.9585715975918));
#64109=CARTESIAN_POINT('Ctrl Pts',(-0.183308880309829,-5.16415065893858,
74.0929428315583));
#64110=CARTESIAN_POINT('Ctrl Pts',(4.23913515679244,-2.95495977912772,74.2517035938041));
#64111=CARTESIAN_POINT('Ctrl Pts',(4.78179321232898,1.95870055096247,74.4104643560501));
#64112=CARTESIAN_POINT('Ctrl Pts',(0.948008058166557,5.07969830752458,74.5692251182959));
#64113=CARTESIAN_POINT('Ctrl Pts',(-3.37677384390662,3.67402258696438,74.7152669635808));
#64114=CARTESIAN_POINT('Ctrl Pts',(-4.36159587705234,1.10022100123729,74.8083885547839));
#64115=CARTESIAN_POINT('Ctrl Pts',(-4.37167806635839,-0.00399716320838302,
74.8485898919049));
#64116=CARTESIAN_POINT('Origin',(0.,0.,24.1514101080949));
#64117=CARTESIAN_POINT('',(-4.37546659946853,-0.00338795269852561,72.6514101080949));
#64118=CARTESIAN_POINT('',(-4.37508401727703,0.00350862331529297,72.848589891905));
#64119=CARTESIAN_POINT('',(-4.372,3.82579154166093E-12,24.1514101080949));
#64120=CARTESIAN_POINT('Ctrl Pts',(-4.37546659946853,-0.00338795269852542,
72.6514101080949));
#64121=CARTESIAN_POINT('Ctrl Pts',(-4.37736040129649,-0.224956166423907,
72.6594947721605));
#64122=CARTESIAN_POINT('Ctrl Pts',(-4.26133239251396,-1.89486696261105,
72.720499690308));
#64123=CARTESIAN_POINT('Ctrl Pts',(-2.1112172128698,-4.71644095649861,72.8344248625374));
#64124=CARTESIAN_POINT('Ctrl Pts',(2.81733266516402,-4.33182294996633,72.9931856247833));
#64125=CARTESIAN_POINT('Ctrl Pts',(5.16737363149282,0.0174117376300544,
73.1519463870293));
#64126=CARTESIAN_POINT('Ctrl Pts',(2.78807641079671,4.35071067109887,73.3107071492751));
#64127=CARTESIAN_POINT('Ctrl Pts',(-2.14295350396336,4.70210630419026,73.469467911521));
#64128=CARTESIAN_POINT('Ctrl Pts',(-4.26731753777204,1.87500660994908,73.5830355644609));
#64129=CARTESIAN_POINT('Ctrl Pts',(-4.37751336374666,0.215028421847947,
73.6436829633189));
#64130=CARTESIAN_POINT('Ctrl Pts',(-4.37573799308197,0.00329254665532727,
73.6514101080949));
#64131=CARTESIAN_POINT('Ctrl Pts',(-4.37508401727703,0.00350862331529318,
72.848589891905));
#64132=CARTESIAN_POINT('Ctrl Pts',(-4.36445811409486,-1.21201843518349,
72.892932426549));
#64133=CARTESIAN_POINT('Ctrl Pts',(-3.20535851125622,-3.89598203052578,
72.9901952152748));
#64134=CARTESIAN_POINT('Ctrl Pts',(1.34123860080759,-4.99030391755056,73.140378258083));
#64135=CARTESIAN_POINT('Ctrl Pts',(4.91997252333115,-1.57984953191204,73.2991390203287));
#64136=CARTESIAN_POINT('Ctrl Pts',(3.99579730998455,3.27653140246455,73.4578997825747));
#64137=CARTESIAN_POINT('Ctrl Pts',(-0.585453654677876,5.13413071435083,
73.6166605448206));
#64138=CARTESIAN_POINT('Ctrl Pts',(-3.90388041542688,2.80342624447369,73.746890581264));
#64139=CARTESIAN_POINT('Ctrl Pts',(-4.36629549877317,0.673422924511184,
73.8242003636254));
#64140=CARTESIAN_POINT('Ctrl Pts',(-4.36501807785945,0.000928765700389245,
73.8485898919049));
#64141=CARTESIAN_POINT('Origin',(0.,0.,24.1514101080949));
#64142=CARTESIAN_POINT('',(-4.3651141969528,-0.00114447055126671,71.6514101080949));
#64143=CARTESIAN_POINT('',(-4.37610278806197,-0.00315032678594118,71.8485898919049));
#64144=CARTESIAN_POINT('',(-4.372,3.82579154166093E-12,24.1514101080949));
#64145=CARTESIAN_POINT('Ctrl Pts',(-4.3651141969528,-0.00114447055126629,
71.6514101080949));
#64146=CARTESIAN_POINT('Ctrl Pts',(-4.36665839117516,-0.660007333527467,
71.675306581002));
#64147=CARTESIAN_POINT('Ctrl Pts',(-3.91728495207162,-2.77596398718315,
71.7521233079911));
#64148=CARTESIAN_POINT('Ctrl Pts',(-0.63314364249968,-5.12846785541421,
71.8818602890621));
#64149=CARTESIAN_POINT('Ctrl Pts',(3.9651734499498,-3.31352575482195,72.040621051308));
#64150=CARTESIAN_POINT('Ctrl Pts',(4.93444268320512,1.53405632954553,72.1993818135539));
#64151=CARTESIAN_POINT('Ctrl Pts',(1.38755924827672,4.97762320275213,72.3581425757998));
#64152=CARTESIAN_POINT('Ctrl Pts',(-3.18397114357576,3.92214967618973,72.50881867398));
#64153=CARTESIAN_POINT('Ctrl Pts',(-4.36496403292504,1.22537573008428,72.6065745180785));
#64154=CARTESIAN_POINT('Ctrl Pts',(-4.37546659946853,-0.00338795269852542,
72.6514101080949));
#64155=CARTESIAN_POINT('Ctrl Pts',(-4.37610278806197,-0.00315032678594042,
71.8485898919049));
#64156=CARTESIAN_POINT('Ctrl Pts',(-4.37771416984263,-0.201332656341541,
71.8558239813086));
#64157=CARTESIAN_POINT('Ctrl Pts',(-4.27545064435103,-1.84762538881353,
71.9159783247941));
#64158=CARTESIAN_POINT('Ctrl Pts',(-2.18656114390733,-4.68198724237597,
72.0290529223616));
#64159=CARTESIAN_POINT('Ctrl Pts',(2.74752166081747,-4.3764344959288,72.1878136846077));
#64160=CARTESIAN_POINT('Ctrl Pts',(5.16698871742013,-0.0654352188752399,
72.3465744468534));
#64161=CARTESIAN_POINT('Ctrl Pts',(2.85746987211454,4.30545236923763,72.5053352090995));
#64162=CARTESIAN_POINT('Ctrl Pts',(-2.06729268270395,4.73585843726931,72.6640959713451));
#64163=CARTESIAN_POINT('Ctrl Pts',(-4.2529565583671,1.92226442851864,72.7785141989471));
#64164=CARTESIAN_POINT('Ctrl Pts',(-4.37713951584072,0.238642906024094,
72.840012172467));
#64165=CARTESIAN_POINT('Ctrl Pts',(-4.37508401727703,0.00350862331529318,
72.848589891905));
#64166=CARTESIAN_POINT('Origin',(0.,0.,24.1514101080949));
#64167=CARTESIAN_POINT('',(-4.37127157619262,0.00399172071570709,70.6514101080949));
#64168=CARTESIAN_POINT('',(-4.36532703354517,-0.00150807403881736,70.8485898919049));
#64169=CARTESIAN_POINT('',(-4.372,3.82579154166093E-12,24.1514101080949));
#64170=CARTESIAN_POINT('Ctrl Pts',(-4.37127157619262,0.00399172071570714,
70.6514101080949));
#64171=CARTESIAN_POINT('Ctrl Pts',(-4.36140746653353,-1.08694237129441,
70.6911183898435));
#64172=CARTESIAN_POINT('Ctrl Pts',(-3.39621711134158,-3.64736222930015,
70.7837469256742));
#64173=CARTESIAN_POINT('Ctrl Pts',(0.900757702520816,-5.08828939599587,
70.9292957155868));
#64174=CARTESIAN_POINT('Ctrl Pts',(4.76338297422217,-2.00305667841551,71.0880564778326));
#64175=CARTESIAN_POINT('Ctrl Pts',(4.26641464848803,2.9154346954137,71.2468172400786));
#64176=CARTESIAN_POINT('Ctrl Pts',(-0.135306682874774,5.16563118288797,
71.4055780023244));
#64177=CARTESIAN_POINT('Ctrl Pts',(-3.76928933575608,3.06100151884775,71.5404422916632));
#64178=CARTESIAN_POINT('Ctrl Pts',(-4.36323867518121,0.799086242725653,
71.62238632692));
#64179=CARTESIAN_POINT('Ctrl Pts',(-4.3651141969528,-0.00114447055126629,
71.6514101080949));
#64180=CARTESIAN_POINT('Ctrl Pts',(-4.36532703354517,-0.00150807403881757,
70.8485898919049));
#64181=CARTESIAN_POINT('Ctrl Pts',(-4.36729483924552,-0.636841944886774,
70.8716357901501));
#64182=CARTESIAN_POINT('Ctrl Pts',(-3.94000526365074,-2.72857085726927,
70.9476019424773));
#64183=CARTESIAN_POINT('Ctrl Pts',(-0.715283247733823,-5.11765806295492,
71.0764883488864));
#64184=CARTESIAN_POINT('Ctrl Pts',(3.91154054911197,-3.37667065413102,71.2352491111322));
#64185=CARTESIAN_POINT('Ctrl Pts',(4.95840295584866,1.45474887910182,71.3940098733782));
#64186=CARTESIAN_POINT('Ctrl Pts',(1.46718352100222,4.95473780229749,71.552770635624));
#64187=CARTESIAN_POINT('Ctrl Pts',(-3.14657975547223,3.96714821422749,71.7042973084663));
#64188=CARTESIAN_POINT('Ctrl Pts',(-4.36592626835323,1.24845026027391,71.8029037272266));
#64189=CARTESIAN_POINT('Ctrl Pts',(-4.37610278806197,-0.00315032678594042,
71.8485898919049));
#64190=CARTESIAN_POINT('Origin',(0.,0.,24.1514101080949));
#64191=CARTESIAN_POINT('',(-4.37870422100453,-0.0012994166445059,69.6514101080949));
#64192=CARTESIAN_POINT('',(-4.3705809381838,0.00395105542623939,69.848589891905));
#64193=CARTESIAN_POINT('',(-4.372,3.82579154166093E-12,24.1514101080949));
#64194=CARTESIAN_POINT('Ctrl Pts',(-4.37870422100453,-0.00129941664450634,
69.6514101080949));
#64195=CARTESIAN_POINT('Ctrl Pts',(-4.3789830325923,-0.0724121058889038,
69.6540099446031));
#64196=CARTESIAN_POINT('Ctrl Pts',(-4.34518999704772,-1.59076889411841,
69.7095300351934));
#64197=CARTESIAN_POINT('Ctrl Pts',(-2.58669250630018,-4.47337403912361,
69.8179703798655));
#64198=CARTESIAN_POINT('Ctrl Pts',(2.35523426198658,-4.5994483350962,69.9767311421114));
#64199=CARTESIAN_POINT('Ctrl Pts',(5.14157869213602,-0.51596702281012,70.1354919043573));
#64200=CARTESIAN_POINT('Ctrl Pts',(3.22219325167658,4.03974306916968,70.2942526666032));
#64201=CARTESIAN_POINT('Ctrl Pts',(-1.6462418758917,4.89815690868675,70.4530134288491));
#64202=CARTESIAN_POINT('Ctrl Pts',(-4.16716700492617,2.18017319825989,70.5720659093463));
#64203=CARTESIAN_POINT('Ctrl Pts',(-4.3745536205967,0.366973708511667,70.6381981357616));
#64204=CARTESIAN_POINT('Ctrl Pts',(-4.37127157619262,0.00399172071570714,
70.6514101080949));
#64205=CARTESIAN_POINT('Ctrl Pts',(-4.3705809381838,0.00395105542623928,
69.848589891905));
#64206=CARTESIAN_POINT('Ctrl Pts',(-4.36115189233779,-1.06404425239527,
69.8874475989916));
#64207=CARTESIAN_POINT('Ctrl Pts',(-3.42928322572819,-3.60126660220352,
69.9792255601602));
#64208=CARTESIAN_POINT('Ctrl Pts',(0.819065126108891,-5.102076684352,70.1239237754111));
#64209=CARTESIAN_POINT('Ctrl Pts',(4.73065728621489,-2.07916709626671,70.2826845376568));
#64210=CARTESIAN_POINT('Ctrl Pts',(4.31260739816882,2.84665972730784,70.4414452999028));
#64211=CARTESIAN_POINT('Ctrl Pts',(-0.0524725109896868,5.16713661609669,
70.6002060621488));
#64212=CARTESIAN_POINT('Ctrl Pts',(-3.74285914641375,3.1081338808624,70.7359209261493));
#64213=CARTESIAN_POINT('Ctrl Pts',(-4.36277617060702,0.822074063266301,
70.8187155360681));
#64214=CARTESIAN_POINT('Ctrl Pts',(-4.36532703354517,-0.00150807403881757,
70.8485898919049));
#64215=CARTESIAN_POINT('Origin',(0.,0.,24.1514101080949));
#64216=CARTESIAN_POINT('',(-4.36744694438276,-0.00316878230680772,68.6514101080949));
#64217=CARTESIAN_POINT('',(-4.37895590169143,-0.000884728325120654,68.848589891905));
#64218=CARTESIAN_POINT('',(-4.372,3.82579154166093E-12,24.1514101080949));
#64219=CARTESIAN_POINT('Ctrl Pts',(-4.36744694438276,-0.0031687823068071,
68.6514101080949));
#64220=CARTESIAN_POINT('Ctrl Pts',(-4.37084913112638,-0.510127366468858,
68.6698217534447));
#64221=CARTESIAN_POINT('Ctrl Pts',(-4.05501785193817,-2.47012128343436,
68.7411536528764));
#64222=CARTESIAN_POINT('Ctrl Pts',(-1.15903350388962,-5.03574172817834,
68.8654058063903));
#64223=CARTESIAN_POINT('Ctrl Pts',(3.60203679805415,-3.70504849111566,69.0241665686361));
#64224=CARTESIAN_POINT('Ctrl Pts',(5.06641299677213,1.01661829719571,69.182927330882));
#64225=CARTESIAN_POINT('Ctrl Pts',(1.89385326524434,4.80784496690336,69.3416880931279));
#64226=CARTESIAN_POINT('Ctrl Pts',(-2.93168118063718,4.20875891624129,69.4978490188655));
#64227=CARTESIAN_POINT('Ctrl Pts',(-4.37330776031301,1.37510260179151,69.6010896905212));
#64228=CARTESIAN_POINT('Ctrl Pts',(-4.37870422100453,-0.00129941664450634,
69.6514101080949));
#64229=CARTESIAN_POINT('Ctrl Pts',(-4.37895590169143,-0.00088472832512114,
68.848589891905));
#64230=CARTESIAN_POINT('Ctrl Pts',(-4.37908827342486,-0.0487245072402155,
68.8503391537513));
#64231=CARTESIAN_POINT('Ctrl Pts',(-4.35670634828455,-1.54372976222875,
68.9050086696796));
#64232=CARTESIAN_POINT('Ctrl Pts',(-2.65807841962993,-4.43132861441282,
69.0125984396897));
#64233=CARTESIAN_POINT('Ctrl Pts',(2.2811920004135,-4.63661700284439,69.1713592019357));
#64234=CARTESIAN_POINT('Ctrl Pts',(5.1326458217616,-0.598331882962418,69.3301199641815));
#64235=CARTESIAN_POINT('Ctrl Pts',(3.28654540832559,3.98756485249208,69.4888807264275));
#64236=CARTESIAN_POINT('Ctrl Pts',(-1.56750175164667,4.92392043319156,69.6476414886732));
#64237=CARTESIAN_POINT('Ctrl Pts',(-4.14999820818835,2.2275746797718,69.7675445438326));
#64238=CARTESIAN_POINT('Ctrl Pts',(-4.37399329599569,0.390456985212737,
69.8345273449097));
#64239=CARTESIAN_POINT('Ctrl Pts',(-4.3705809381838,0.00395105542623928,
69.848589891905));
#64240=CARTESIAN_POINT('Origin',(0.,0.,24.1514101080949));
#64241=CARTESIAN_POINT('',(-4.36727426748866,0.00308741741996557,67.6514101080949));
#64242=CARTESIAN_POINT('',(-4.36799009248299,-0.00339142969553563,67.8485898919049));
#64243=CARTESIAN_POINT('',(-4.372,3.82579154166093E-12,24.1514101080949));
#64244=CARTESIAN_POINT('Ctrl Pts',(-4.36727426748866,0.0030874174199657,
67.6514101080949));
#64245=CARTESIAN_POINT('Ctrl Pts',(-4.36112833884136,-0.939337788388386,
67.6856335622863));
#64246=CARTESIAN_POINT('Ctrl Pts',(-3.59904165290846,-3.34810943987296,
67.7727772705596));
#64247=CARTESIAN_POINT('Ctrl Pts',(0.370823889097725,-5.15408023407956,
67.9128412329148));
#64248=CARTESIAN_POINT('Ctrl Pts',(4.53122783943781,-2.48395404207855,68.0716019951608));
#64249=CARTESIAN_POINT('Ctrl Pts',(4.5445136629679,2.45956276259679,68.2303627574067));
#64250=CARTESIAN_POINT('Ctrl Pts',(0.398521768172548,5.15201259862078,68.3891235196525));
#64251=CARTESIAN_POINT('Ctrl Pts',(-3.58909538685354,3.36377270257325,68.5294726365487));
#64252=CARTESIAN_POINT('Ctrl Pts',(-4.36107028825353,0.947014381222592,
68.6169014993627));
#64253=CARTESIAN_POINT('Ctrl Pts',(-4.36744694438276,-0.0031687823068071,
68.6514101080949));
#64254=CARTESIAN_POINT('Ctrl Pts',(-4.36799009248299,-0.00339142969553514,
67.8485898919049));
#64255=CARTESIAN_POINT('Ctrl Pts',(-4.37149165529305,-0.486778408785156,
67.8661509625928));
#64256=CARTESIAN_POINT('Ctrl Pts',(-4.07455789488293,-2.42267137940883,
67.9366322873626));
#64257=CARTESIAN_POINT('Ctrl Pts',(-1.23961891643423,-5.01651264483955,
68.0600338662145));
#64258=CARTESIAN_POINT('Ctrl Pts',(3.54217356679019,-3.76232117137135,68.2187946284603));
#64259=CARTESIAN_POINT('Ctrl Pts',(5.08206060458778,0.935261559732356,68.3775553907062));
#64260=CARTESIAN_POINT('Ctrl Pts',(1.97069054350433,4.77686434343271,68.5363161529522));
#64261=CARTESIAN_POINT('Ctrl Pts',(-2.89016105242335,4.25237825733215,68.6933276533517));
#64262=CARTESIAN_POINT('Ctrl Pts',(-4.37508364382578,1.39856782394589,68.7974188996693));
#64263=CARTESIAN_POINT('Ctrl Pts',(-4.37895590169143,-0.00088472832512114,
68.848589891905));
#64264=CARTESIAN_POINT('Origin',(0.,0.,24.1514101080949));
#64265=CARTESIAN_POINT('',(-4.37860089698225,0.00143482616460942,66.6514101080949));
#64266=CARTESIAN_POINT('',(-4.36678925203502,0.00282595512297229,66.8485898919049));
#64267=CARTESIAN_POINT('',(-4.372,3.82579154166093E-12,24.1514101080949));
#64268=CARTESIAN_POINT('Ctrl Pts',(-4.37860089698225,0.00143482616460969,
66.6514101080949));
#64269=CARTESIAN_POINT('Ctrl Pts',(-4.37274293747686,-1.3672535432393,66.7014453711278));
#64270=CARTESIAN_POINT('Ctrl Pts',(-2.94545539126712,-4.19408159696058,
66.8044008882426));
#64271=CARTESIAN_POINT('Ctrl Pts',(1.86798369006022,-4.81795499664787,66.9602766594396));
#64272=CARTESIAN_POINT('Ctrl Pts',(5.06087547593053,-1.04383563513614,67.1190374216854));
#64273=CARTESIAN_POINT('Ctrl Pts',(3.62189943977487,3.68563398402679,67.2777981839313));
#64274=CARTESIAN_POINT('Ctrl Pts',(-1.13194959602156,5.04189880185246,67.4365589461772));
#64275=CARTESIAN_POINT('Ctrl Pts',(-4.04836008668961,2.48602916041319,67.5610962542317));
#64276=CARTESIAN_POINT('Ctrl Pts',(-4.37063188292449,0.517948815873062,
67.6327133082043));
#64277=CARTESIAN_POINT('Ctrl Pts',(-4.36727426748866,0.0030874174199657,
67.6514101080949));
#64278=CARTESIAN_POINT('Ctrl Pts',(-4.36678925203502,0.00282595512297222,
66.8485898919049));
#64279=CARTESIAN_POINT('Ctrl Pts',(-4.36134189412171,-0.916433051844979,
66.8819627714344));
#64280=CARTESIAN_POINT('Ctrl Pts',(-3.62832781641238,-3.30133069322053,
66.9682559050458));
#64281=CARTESIAN_POINT('Ctrl Pts',(0.288144638596748,-5.15936302667923,
67.1074692927391));
#64282=CARTESIAN_POINT('Ctrl Pts',(4.49082211047655,-2.55628068604989,67.266230054985));
#64283=CARTESIAN_POINT('Ctrl Pts',(4.58336201290063,2.38638782106256,67.4249908172308));
#64284=CARTESIAN_POINT('Ctrl Pts',(0.481069000502546,5.14496130117338,67.5837515794768));
#64285=CARTESIAN_POINT('Ctrl Pts',(-3.55904252406398,3.41043311335412,67.7249512710348));
#64286=CARTESIAN_POINT('Ctrl Pts',(-4.36093970223245,0.969907359868089,
67.8132307085108));
#64287=CARTESIAN_POINT('Ctrl Pts',(-4.36799009248299,-0.00339142969553514,
67.8485898919049));
#64288=CARTESIAN_POINT('Origin',(0.,0.,24.1514101080949));
#64289=CARTESIAN_POINT('',(-4.37150619923976,-0.00399650483370713,65.6514101080949));
#64290=CARTESIAN_POINT('',(-4.37824072692977,0.00182550535674644,65.8485898919049));
#64291=CARTESIAN_POINT('',(-4.372,3.82579154166093E-12,24.1514101080949));
#64292=CARTESIAN_POINT('Ctrl Pts',(-4.37150619923976,-0.00399650483370689,
65.6514101080949));
#64293=CARTESIAN_POINT('Ctrl Pts',(-4.37473632420811,-0.359095615586663,
65.6643369258874));
#64294=CARTESIAN_POINT('Ctrl Pts',(-4.17282222069464,-2.16428561428065,
65.7301839977619));
#64295=CARTESIAN_POINT('Ctrl Pts',(-1.67254574036732,-4.88923758498539,
65.8489513237183));
#64296=CARTESIAN_POINT('Ctrl Pts',(3.20043304382085,-4.05700403599433,66.0077120859643));
#64297=CARTESIAN_POINT('Ctrl Pts',(5.14427774780404,0.488323529540513,66.16647284821));
#64298=CARTESIAN_POINT('Ctrl Pts',(2.3799223229872,4.58672248480354,66.3252336104561));
#64299=CARTESIAN_POINT('Ctrl Pts',(-2.56261070750152,4.48721291871176,66.4839943727018));
#64300=CARTESIAN_POINT('Ctrl Pts',(-4.34124164729195,1.60654622778481,66.5927198719149));
#64301=CARTESIAN_POINT('Ctrl Pts',(-4.37893866198466,0.0803522427089276,
66.6485251170459));
#64302=CARTESIAN_POINT('Ctrl Pts',(-4.37860089698225,0.00143482616460969,
66.6514101080949));
#64303=CARTESIAN_POINT('Ctrl Pts',(-4.37824072692977,0.00182550535674642,
65.8485898919049));
#64304=CARTESIAN_POINT('Ctrl Pts',(-4.37114754505431,-1.34389016319695,
65.8977745802759));
#64305=CARTESIAN_POINT('Ctrl Pts',(-2.98610974303986,-4.15014526257514,
65.9998795227288));
#64306=CARTESIAN_POINT('Ctrl Pts',(1.79050088812788,-4.84728385216189,66.1549047192638));
#64307=CARTESIAN_POINT('Ctrl Pts',(5.04349004573647,-1.12483880283976,66.3136654815096));
#64308=CARTESIAN_POINT('Ctrl Pts',(3.68052305807757,3.62709307749002,66.4724262437556));
#64309=CARTESIAN_POINT('Ctrl Pts',(-1.05097105537457,5.05939858230018,66.6311870060014));
#64310=CARTESIAN_POINT('Ctrl Pts',(-4.02817917541877,2.53347937952348,66.7565748887179));
#64311=CARTESIAN_POINT('Ctrl Pts',(-4.36997991304344,0.541260167974116,
66.8290425173524));
#64312=CARTESIAN_POINT('Ctrl Pts',(-4.36678925203502,0.00282595512297222,
66.8485898919049));
#64313=CARTESIAN_POINT('Origin',(0.,0.,24.1514101080949));
#64314=CARTESIAN_POINT('',(-4.36505611781897,0.00102009982110932,64.6514101080949));
#64315=CARTESIAN_POINT('',(-4.37221209240493,-0.00398401159164008,64.848589891905));
#64316=CARTESIAN_POINT('',(-4.372,3.82579154166093E-12,24.1514101080949));
#64317=CARTESIAN_POINT('Ctrl Pts',(-4.36505611781897,0.00102009982110941,
64.6514101080949));
#64318=CARTESIAN_POINT('Ctrl Pts',(-4.36340207653842,-0.791374776421536,
64.680148734729));
#64319=CARTESIAN_POINT('Ctrl Pts',(-3.7780282066601,-3.04518855619851,64.7618076154451));
#64320=CARTESIAN_POINT('Ctrl Pts',(-0.163070050579303,-5.16482928804609,
64.8963867502428));
#64321=CARTESIAN_POINT('Ctrl Pts',(4.25068252576661,-2.93832460446375,65.0551475124889));
#64322=CARTESIAN_POINT('Ctrl Pts',(4.77408061574266,1.97742450941745,65.2139082747347));
#64323=CARTESIAN_POINT('Ctrl Pts',(0.928094299999949,5.08337431106172,65.3726690369806));
#64324=CARTESIAN_POINT('Ctrl Pts',(-3.38499698876322,3.66278651613716,65.518502981434));
#64325=CARTESIAN_POINT('Ctrl Pts',(-4.36151272681657,1.09462141415472,65.6114166718055));
#64326=CARTESIAN_POINT('Ctrl Pts',(-4.37150619923976,-0.00399650483370689,
65.6514101080949));
#64327=CARTESIAN_POINT('Ctrl Pts',(-4.37221209240492,-0.00398401159164036,
64.848589891905));
#64328=CARTESIAN_POINT('Ctrl Pts',(-4.37526481066381,-0.335581023561335,
64.8606661350355));
#64329=CARTESIAN_POINT('Ctrl Pts',(-4.18939334686749,-2.11690750379085,
64.925662632248));
#64330=CARTESIAN_POINT('Ctrl Pts',(-1.75071636731768,-4.86179456322688,
65.0435793835425));
#64331=CARTESIAN_POINT('Ctrl Pts',(3.1349787773885,-4.10779286711735,65.2023401457884));
#64332=CARTESIAN_POINT('Ctrl Pts',(5.15144558585509,0.405786335144852,65.3611009080343));
#64333=CARTESIAN_POINT('Ctrl Pts',(2.45315204119292,4.54797748857745,65.5198616702802));
#64334=CARTESIAN_POINT('Ctrl Pts',(-2.49034118407384,4.52772072468283,65.6786224325261));
#64335=CARTESIAN_POINT('Ctrl Pts',(-4.32920116011288,1.65362984026736,65.788198506401));
#64336=CARTESIAN_POINT('Ctrl Pts',(-4.37877945245337,0.104032299273348,
65.844854326194));
#64337=CARTESIAN_POINT('Ctrl Pts',(-4.37824072692977,0.00182550535674642,
65.8485898919049));
#64338=CARTESIAN_POINT('Origin',(0.,0.,24.1514101080949));
#64339=CARTESIAN_POINT('',(-4.37524640365158,0.00345929889477671,63.6514101080949));
#64340=CARTESIAN_POINT('',(-4.36492309298158,0.000643490633093768,63.848589891905));
#64341=CARTESIAN_POINT('',(-4.372,3.82579154166093E-12,24.1514101080949));
#64342=CARTESIAN_POINT('Ctrl Pts',(-4.37524640365158,0.00345929889477663,
63.6514101080949));
#64343=CARTESIAN_POINT('Ctrl Pts',(-4.36466684100657,-1.21764908937452,
63.6959605435705));
#64344=CARTESIAN_POINT('Ctrl Pts',(-3.19636598506899,-3.90702309781776,
63.7934312331281));
#64345=CARTESIAN_POINT('Ctrl Pts',(1.36078442693529,-4.98500944427043,63.9438221767676));
#64346=CARTESIAN_POINT('Ctrl Pts',(4.92612583383742,-1.56055685101642,64.1025829390136));
#64347=CARTESIAN_POINT('Ctrl Pts',(3.98292640713875,3.29216504011747,64.2613437012594));
#64348=CARTESIAN_POINT('Ctrl Pts',(-0.605568927444514,5.13179692604536,
64.4201044635054));
#64349=CARTESIAN_POINT('Ctrl Pts',(-3.90955357406592,2.79184753823524,64.5501265991171));
#64350=CARTESIAN_POINT('Ctrl Pts',(-4.36644788265656,0.667767259764548,
64.627228480647));
#64351=CARTESIAN_POINT('Ctrl Pts',(-4.36505611781897,0.00102009982110941,
64.6514101080949));
#64352=CARTESIAN_POINT('Ctrl Pts',(-4.36492309298158,0.000643490633093699,
63.8485898919049));
#64353=CARTESIAN_POINT('Ctrl Pts',(-4.36391231627522,-0.768357459497397,
63.876477943877));
#64354=CARTESIAN_POINT('Ctrl Pts',(-3.80373422012026,-2.9979881039429,63.9572862499311));
#64355=CARTESIAN_POINT('Ctrl Pts',(-0.245853021615901,-5.16155116855183,
64.0910148100673));
#64356=CARTESIAN_POINT('Ctrl Pts',(4.20302825930282,-3.00609507922124,64.249775572313));
#64357=CARTESIAN_POINT('Ctrl Pts',(4.80516969413782,1.90063104898239,64.408536334559));
#64358=CARTESIAN_POINT('Ctrl Pts',(1.00947304907845,5.06784158562605,64.5672970968048));
#64359=CARTESIAN_POINT('Ctrl Pts',(-3.35112485942778,3.70870379987186,64.7139816159202));
#64360=CARTESIAN_POINT('Ctrl Pts',(-4.36188725407156,1.11753630245885,64.8077458809536));
#64361=CARTESIAN_POINT('Ctrl Pts',(-4.37221209240492,-0.00398401159164036,
64.848589891905));
#64362=CARTESIAN_POINT('Origin',(0.,0.,24.1514101080949));
#64363=CARTESIAN_POINT('',(-4.37595036350582,-0.00321178070193251,62.6514101080949));
#64364=CARTESIAN_POINT('',(-4.37457294606715,0.00364650982632456,62.848589891905));
#64365=CARTESIAN_POINT('',(-4.372,3.82579154166093E-12,24.1514101080949));
#64366=CARTESIAN_POINT('Ctrl Pts',(-4.37595036350582,-0.00321178070193263,
62.6514101080949));
#64367=CARTESIAN_POINT('Ctrl Pts',(-4.37763091892069,-0.207108192738585,
62.6588520983301));
#64368=CARTESIAN_POINT('Ctrl Pts',(-4.27203828701875,-1.85916971844638,
62.7192143426473));
#64369=CARTESIAN_POINT('Ctrl Pts',(-2.16819641913028,-4.69051998227545,
62.8324968410464));
#64370=CARTESIAN_POINT('Ctrl Pts',(2.76465101981334,-4.3656337632353,62.9912576032923));
#64371=CARTESIAN_POINT('Ctrl Pts',(5.16720539805885,-0.0451861740625634,
63.1500183655382));
#64372=CARTESIAN_POINT('Ctrl Pts',(2.8405755616569,4.31661718184185,63.308779127784));
#64373=CARTESIAN_POINT('Ctrl Pts',(-2.08583579528372,4.72772064013601,63.46753989003));
#64374=CARTESIAN_POINT('Ctrl Pts',(-4.25650552345673,1.91071093035616,63.5817502168002));
#64375=CARTESIAN_POINT('Ctrl Pts',(-4.37723401655206,0.232872448270317,
63.6430402894885));
#64376=CARTESIAN_POINT('Ctrl Pts',(-4.37524640365158,0.00345929889477663,
63.6514101080949));
#64377=CARTESIAN_POINT('Ctrl Pts',(-4.37457294606715,0.00364650982632473,
62.848589891905));
#64378=CARTESIAN_POINT('Ctrl Pts',(-4.36385410668696,-1.19462603572661,
62.8922897527186));
#64379=CARTESIAN_POINT('Ctrl Pts',(-3.23292058066413,-3.86178527014851,
62.9889098676142));
#64380=CARTESIAN_POINT('Ctrl Pts',(1.28068854395033,-5.00618527695598,63.1384502365919));
#64381=CARTESIAN_POINT('Ctrl Pts',(4.90047350742458,-1.63933327204883,63.2972109988377));
#64382=CARTESIAN_POINT('Ctrl Pts',(4.03519542999152,3.22788661752423,63.4559717610837));
#64383=CARTESIAN_POINT('Ctrl Pts',(-0.523216761619089,5.14084607765855,
63.6147325233295));
#64384=CARTESIAN_POINT('Ctrl Pts',(-3.886148042221,2.83920884682887,63.7456052336033));
#64385=CARTESIAN_POINT('Ctrl Pts',(-4.3658303620453,0.690895618159912,63.8235576897951));
#64386=CARTESIAN_POINT('Ctrl Pts',(-4.36492309298158,0.000643490633093699,
63.8485898919049));
#64387=CARTESIAN_POINT('Origin',(0.,0.,24.1514101080949));
#64388=CARTESIAN_POINT('',(-4.36526954399882,-0.00142033253192601,61.6514101080949));
#64389=CARTESIAN_POINT('',(-4.37655926179451,-0.0029470014875782,61.848589891905));
#64390=CARTESIAN_POINT('',(-4.372,3.82579154166093E-12,24.1514101080949));
#64391=CARTESIAN_POINT('Ctrl Pts',(-4.36526954399882,-0.00142033253192606,
61.6514101080949));
#64392=CARTESIAN_POINT('Ctrl Pts',(-4.36713817680575,-0.642506710603713,
61.6746639071717));
#64393=CARTESIAN_POINT('Ctrl Pts',(-3.93449886856382,-2.74015675637768,
61.7508379603305));
#64394=CARTESIAN_POINT('Ctrl Pts',(-0.695222522116061,-5.12042176590928,
61.879932267571));
#64395=CARTESIAN_POINT('Ctrl Pts',(3.92474305071123,-3.3613160223265,62.038693029817));
#64396=CARTESIAN_POINT('Ctrl Pts',(4.95266390069012,1.47416881762428,62.1974537920629));
#64397=CARTESIAN_POINT('Ctrl Pts',(1.4477554676688,4.96044932661243,62.3562145543087));
#64398=CARTESIAN_POINT('Ctrl Pts',(-3.15577720759182,3.95616660035224,62.5075333263195));
#64399=CARTESIAN_POINT('Ctrl Pts',(-4.36568043030908,1.24280635839108,62.6059318442481));
#64400=CARTESIAN_POINT('Ctrl Pts',(-4.37595036350582,-0.00321178070193263,
62.6514101080949));
#64401=CARTESIAN_POINT('Ctrl Pts',(-4.37655926179451,-0.00294700148757761,
61.848589891905));
#64402=CARTESIAN_POINT('Ctrl Pts',(-4.37795768436782,-0.183473677232841,
61.8551813074782));
#64403=CARTESIAN_POINT('Ctrl Pts',(-4.28584228404936,-1.81194987404807,
61.9146929771335));
#64404=CARTESIAN_POINT('Ctrl Pts',(-2.24311745571471,-4.65515609337478,
62.0271249008706));
#64405=CARTESIAN_POINT('Ctrl Pts',(2.69430472161155,-4.40939635788372,62.1858856631165));
#64406=CARTESIAN_POINT('Ctrl Pts',(5.16581691910958,-0.128022388891978,
62.3446464253625));
#64407=CARTESIAN_POINT('Ctrl Pts',(2.90941568030617,4.27052158090844,62.5034071876082));
#64408=CARTESIAN_POINT('Ctrl Pts',(-2.00977165837252,4.76055375508134,62.6621679498542));
#64409=CARTESIAN_POINT('Ctrl Pts',(-4.24182569275328,1.95798917979278,62.7772288512864));
#64410=CARTESIAN_POINT('Ctrl Pts',(-4.37683455314381,0.256474411491908,
62.8393694986367));
#64411=CARTESIAN_POINT('Ctrl Pts',(-4.37457294606715,0.00364650982632473,
62.848589891905));
#64412=CARTESIAN_POINT('Origin',(0.,0.,24.1514101080949));
#64413=CARTESIAN_POINT('',(-4.37074823605818,0.00396461597538121,60.6514101080949));
#64414=CARTESIAN_POINT('',(-4.36552637203463,-0.001773948386046,60.848589891905));
#64415=CARTESIAN_POINT('',(-4.372,3.82579154166093E-12,24.1514101080949));
#64416=CARTESIAN_POINT('Ctrl Pts',(-4.37074823605818,0.00396461597538186,
60.6514101080949));
#64417=CARTESIAN_POINT('Ctrl Pts',(-4.36120638422482,-1.0696402047533,60.6904757160132));
#64418=CARTESIAN_POINT('Ctrl Pts',(-3.42125648388678,-3.61254525965742,
60.7824615780135));
#64419=CARTESIAN_POINT('Ctrl Pts',(0.839052987504236,-5.09882765939536,
60.9273676940957));
#64420=CARTESIAN_POINT('Ctrl Pts',(4.73876879287487,-2.06061246810993,61.0861284563416));
#64421=CARTESIAN_POINT('Ctrl Pts',(4.30141865142892,2.86353819621711,61.2448892185875));
#64422=CARTESIAN_POINT('Ctrl Pts',(-0.0727212283482856,5.16689123545314,
61.4036499808334));
#64423=CARTESIAN_POINT('Ctrl Pts',(-3.74936971792349,3.0966186529212,61.5391569440025));
#64424=CARTESIAN_POINT('Ctrl Pts',(-4.36288560187799,0.816457216282587,
61.6217436530897));
#64425=CARTESIAN_POINT('Ctrl Pts',(-4.36526954399882,-0.00142033253192606,
61.6514101080949));
#64426=CARTESIAN_POINT('Ctrl Pts',(-4.36552637203463,-0.00177394838604503,
60.848589891905));
#64427=CARTESIAN_POINT('Ctrl Pts',(-4.36778246279527,-0.619319994324535,
60.8709931163198));
#64428=CARTESIAN_POINT('Ctrl Pts',(-3.95683545179798,-2.6927488906017,60.9463165948165));
#64429=CARTESIAN_POINT('Ctrl Pts',(-0.777225152475865,-5.10861774222493,
61.0745603273954));
#64430=CARTESIAN_POINT('Ctrl Pts',(3.87034915924295,-3.42380658907068,61.2333210896411));
#64431=CARTESIAN_POINT('Ctrl Pts',(4.97566169906822,1.39457693593507,61.3920818518871));
#64432=CARTESIAN_POINT('Ctrl Pts',(1.52709666834069,4.93660105126586,61.550842614133));
#64433=CARTESIAN_POINT('Ctrl Pts',(-3.11790932935563,4.00102289357066,61.7030119608056));
#64434=CARTESIAN_POINT('Ctrl Pts',(-4.36673022084793,1.26591415802506,61.8022610533963));
#64435=CARTESIAN_POINT('Ctrl Pts',(-4.37655926179451,-0.00294700148757761,
61.848589891905));
#64436=CARTESIAN_POINT('Origin',(0.,0.,24.1514101080949));
#64437=CARTESIAN_POINT('',(-4.37890245970854,-0.00098741172007078,59.6514101080949));
#64438=CARTESIAN_POINT('',(-4.37007084553272,0.00389455484668386,59.848589891905));
#64439=CARTESIAN_POINT('',(-4.372,3.82579154166093E-12,24.1514101080949));
#64440=CARTESIAN_POINT('Ctrl Pts',(-4.37890245970854,-0.000987411720070989,
59.6514101080949));
#64441=CARTESIAN_POINT('Ctrl Pts',(-4.37906627500205,-0.054514724532804,
59.6533672707728));
#64442=CARTESIAN_POINT('Ctrl Pts',(-4.35392740184128,-1.55522413176342,
59.7082446875327));
#64443=CARTESIAN_POINT('Ctrl Pts',(-2.6406923556686,-4.44171107781315,59.8160423583745));
#64444=CARTESIAN_POINT('Ctrl Pts',(2.29934455736468,-4.62764173446609,59.9748031206204));
#64445=CARTESIAN_POINT('Ctrl Pts',(5.13495109710383,-0.578213322578349,
60.1335638828663));
#64446=CARTESIAN_POINT('Ctrl Pts',(3.27089354364999,4.00041358388897,60.2923246451122));
#64447=CARTESIAN_POINT('Ctrl Pts',(-1.58678569169648,4.91773978415717,60.451085407358));
#64448=CARTESIAN_POINT('Ctrl Pts',(-4.15423631088884,2.21598713963915,60.5707805616856));
#64449=CARTESIAN_POINT('Ctrl Pts',(-4.37413226072698,0.384719343814296,
60.6375554619313));
#64450=CARTESIAN_POINT('Ctrl Pts',(-4.37074823605818,0.00396461597538186,
60.6514101080949));
#64451=CARTESIAN_POINT('Ctrl Pts',(-4.37007084553272,0.00389455484668389,
59.848589891905));
#64452=CARTESIAN_POINT('Ctrl Pts',(-4.36101477584936,-1.0467484993519,59.8868049251613));
#64453=CARTESIAN_POINT('Ctrl Pts',(-3.45386988791881,-3.56635453916342,
59.9779402124996));
#64454=CARTESIAN_POINT('Ctrl Pts',(0.757199388556149,-5.11162432694214,
60.12199575392));
#64455=CARTESIAN_POINT('Ctrl Pts',(4.70512351821232,-2.13632086826434,60.2807565161658));
#64456=CARTESIAN_POINT('Ctrl Pts',(4.34677488413138,2.79420870381954,60.4395172784118));
#64457=CARTESIAN_POINT('Ctrl Pts',(0.0101251021257834,5.16739311995163,
60.5982780406576));
#64458=CARTESIAN_POINT('Ctrl Pts',(-3.72252569100569,3.14370820853236,60.7346355784887));
#64459=CARTESIAN_POINT('Ctrl Pts',(-4.36245318991586,0.839429561242695,
60.8180728622378));
#64460=CARTESIAN_POINT('Ctrl Pts',(-4.36552637203463,-0.00177394838604503,
60.848589891905));
#64461=CARTESIAN_POINT('Origin',(0.,0.,24.1514101080949));
#64462=CARTESIAN_POINT('',(-4.36785354673662,-0.00333986239341869,58.6514101080949));
#64463=CARTESIAN_POINT('',(-4.37908572622912,-0.000563059365845109,58.848589891905));
#64464=CARTESIAN_POINT('',(-4.372,3.82579154166093E-12,24.1514101080949));
#64465=CARTESIAN_POINT('Ctrl Pts',(-4.36785354673662,-0.00333986239341826,
58.6514101080949));
#64466=CARTESIAN_POINT('Ctrl Pts',(-4.3713354267805,-0.492488022383476,
58.6691790796144));
#64467=CARTESIAN_POINT('Ctrl Pts',(-4.0698257693161,-2.43426901092249,58.7398683052158));
#64468=CARTESIAN_POINT('Ctrl Pts',(-1.21995052871669,-5.02133190732686,
58.8634777848992));
#64469=CARTESIAN_POINT('Ctrl Pts',(3.55689020801282,-3.74841105859499,59.022238547145));
#64470=CARTESIAN_POINT('Ctrl Pts',(5.07835637974298,0.955170087669591,59.1809993093909));
#64471=CARTESIAN_POINT('Ctrl Pts',(1.95195567231696,4.78455039364876,59.3397600716368));
#64472=CARTESIAN_POINT('Ctrl Pts',(-2.90036961753982,4.24173919554959,59.4965636712048));
#64473=CARTESIAN_POINT('Ctrl Pts',(-4.37463682871597,1.39282484839483,59.6004470166909));
#64474=CARTESIAN_POINT('Ctrl Pts',(-4.37890245970854,-0.000987411720070989,
59.6514101080949));
#64475=CARTESIAN_POINT('Ctrl Pts',(-4.37908572622912,-0.000563059365844233,
58.848589891905));
#64476=CARTESIAN_POINT('Ctrl Pts',(-4.37914057971478,-0.0308242308936409,
58.8496964799209));
#64477=CARTESIAN_POINT('Ctrl Pts',(-4.36515029335745,-1.50821048731078,
58.9037233220189));
#64478=CARTESIAN_POINT('Ctrl Pts',(-2.71156370034918,-4.39880398208026,
59.0106704181988));
#64479=CARTESIAN_POINT('Ctrl Pts',(2.22485747409188,-4.66391074033302,59.1694311804446));
#64480=CARTESIAN_POINT('Ctrl Pts',(5.12502112908765,-0.660463928024547,
59.3281919426906));
#64481=CARTESIAN_POINT('Ctrl Pts',(3.33460890093368,3.94745964534539,59.4869527049363));
#64482=CARTESIAN_POINT('Ctrl Pts',(-1.5077392503099,4.94254757457034,59.6457134671823));
#64483=CARTESIAN_POINT('Ctrl Pts',(-4.13672535981933,2.2634000371691,59.7662591961718));
#64484=CARTESIAN_POINT('Ctrl Pts',(-4.37355563916387,0.408184092349566,
59.8338846710794));
#64485=CARTESIAN_POINT('Ctrl Pts',(-4.37007084553272,0.00389455484668389,
59.848589891905));
#64486=CARTESIAN_POINT('Origin',(0.,0.,24.1514101080949));
#64487=CARTESIAN_POINT('',(-4.36690348533115,0.0028923709500598,57.6514101080949));
#64488=CARTESIAN_POINT('',(-4.36842637263245,-0.00353866609716813,57.848589891905));
#64489=CARTESIAN_POINT('',(-4.372,3.82579154166093E-12,24.1514101080949));
#64490=CARTESIAN_POINT('Ctrl Pts',(-4.36690348533115,0.00289237095005987,
57.6514101080949));
#64491=CARTESIAN_POINT('Ctrl Pts',(-4.36128421030265,-0.922032505654121,
57.6849908884559));
#64492=CARTESIAN_POINT('Ctrl Pts',(-3.62122223271516,-3.31277225264101,
57.7714919228989));
#64493=CARTESIAN_POINT('Ctrl Pts',(0.308361079608735,-5.1581941472416,57.9109132114238));
#64494=CARTESIAN_POINT('Ctrl Pts',(4.50080518836808,-2.53866226040682,58.0696739736697));
#64495=CARTESIAN_POINT('Ctrl Pts',(4.57397490984839,2.40433087160068,58.2284347359156));
#64496=CARTESIAN_POINT('Ctrl Pts',(0.460903079952699,5.14680694867653,58.3871954981615));
#64497=CARTESIAN_POINT('Ctrl Pts',(-3.56644148611271,3.39903679271645,58.5281872888879));
#64498=CARTESIAN_POINT('Ctrl Pts',(-4.36096555385885,0.964312382866099,
58.6162588255324));
#64499=CARTESIAN_POINT('Ctrl Pts',(-4.36785354673662,-0.00333986239341826,
58.6514101080949));
#64500=CARTESIAN_POINT('Ctrl Pts',(-4.36842637263245,-0.00353866609716848,
57.848589891905));
#64501=CARTESIAN_POINT('Ctrl Pts',(-4.37197022738872,-0.469118111917197,
57.8655082887625));
#64502=CARTESIAN_POINT('Ctrl Pts',(-4.08900712877109,-2.3868217079302,57.935346939702));
#64503=CARTESIAN_POINT('Ctrl Pts',(-1.30029709065152,-5.00112803773905,
58.0581058447233));
#64504=CARTESIAN_POINT('Ctrl Pts',(3.49633757827368,-3.80495436405849,58.2168666069693));
#64505=CARTESIAN_POINT('Ctrl Pts',(5.09301729854088,0.873629767452735,58.3756273692151));
#64506=CARTESIAN_POINT('Ctrl Pts',(2.02841201894453,4.75264125042254,58.5343881314611));
#64507=CARTESIAN_POINT('Ctrl Pts',(-2.85835725119982,4.28517149950547,58.6920423056909));
#64508=CARTESIAN_POINT('Ctrl Pts',(-4.37651732665532,1.41635291451315,58.796776225839));
#64509=CARTESIAN_POINT('Ctrl Pts',(-4.37908572622912,-0.000563059365844233,
58.848589891905));
#64510=CARTESIAN_POINT('Origin',(0.,0.,24.1514101080949));
#64511=CARTESIAN_POINT('',(-4.37833561871486,0.00173199218209078,56.6514101080949));
#64512=CARTESIAN_POINT('',(-4.36645415447485,0.00261097933498017,56.848589891905));
#64513=CARTESIAN_POINT('',(-4.372,3.82579154166093E-12,24.1514101080949));
#64514=CARTESIAN_POINT('Ctrl Pts',(-4.37833561871486,0.00173199218209092,
56.6514101080949));
#64515=CARTESIAN_POINT('Ctrl Pts',(-4.3715252071243,-1.34959412873374,56.7008026972975));
#64516=CARTESIAN_POINT('Ctrl Pts',(-2.97623248528167,-4.16090558093235,
56.803115540582));
#64517=CARTESIAN_POINT('Ctrl Pts',(1.8094827870843,-4.8402298973603,56.9583486379485));
#64518=CARTESIAN_POINT('Ctrl Pts',(5.04785929713791,-1.10506557830443,57.1171094001944));
#64519=CARTESIAN_POINT('Ctrl Pts',(3.66628078958101,3.64148851268323,57.2758701624403));
#64520=CARTESIAN_POINT('Ctrl Pts',(-1.07078988460527,5.05524108614831,57.4346309246862));
#64521=CARTESIAN_POINT('Ctrl Pts',(-4.03315651405818,2.52188158975817,57.559810906571));
#64522=CARTESIAN_POINT('Ctrl Pts',(-4.37013967640761,0.535564934025079,
57.632070634374));
#64523=CARTESIAN_POINT('Ctrl Pts',(-4.36690348533115,0.00289237095005987,
57.6514101080949));
#64524=CARTESIAN_POINT('Ctrl Pts',(-4.36645415447485,0.00261097933498031,
56.848589891905));
#64525=CARTESIAN_POINT('Ctrl Pts',(-4.36154135054989,-0.899119064739272,
56.881320097604));
#64526=CARTESIAN_POINT('Ctrl Pts',(-3.65007828630307,-3.26593148213623,
56.9669705573851));
#64527=CARTESIAN_POINT('Ctrl Pts',(0.225623900899773,-5.162474990657,57.1055412712481));
#64528=CARTESIAN_POINT('Ctrl Pts',(4.45952627223033,-2.61049412968195,57.2643020334939));
#64529=CARTESIAN_POINT('Ctrl Pts',(4.61193398121205,2.33069069735948,57.4230627957398));
#64530=CARTESIAN_POINT('Ctrl Pts',(0.543358837230748,5.13875620630321,57.5818235579857));
#64531=CARTESIAN_POINT('Ctrl Pts',(-3.53595095853239,3.44562506237492,57.7236659233741));
#64532=CARTESIAN_POINT('Ctrl Pts',(-4.36088515262005,0.98720087478414,57.8125880346805));
#64533=CARTESIAN_POINT('Ctrl Pts',(-4.36842637263245,-0.00353866609716848,
57.848589891905));
#64534=CARTESIAN_POINT('Origin',(0.,0.,24.1514101080949));
#64535=CARTESIAN_POINT('',(-4.37203889039062,-0.00399078471529107,55.6514101080949));
#64536=CARTESIAN_POINT('',(-4.37792086111113,0.00210556704416318,55.848589891905));
#64537=CARTESIAN_POINT('',(-4.372,3.82579154166093E-12,24.1514101080949));
#64538=CARTESIAN_POINT('Ctrl Pts',(-4.37203889039062,-0.0039907847152907,
55.6514101080949));
#64539=CARTESIAN_POINT('Ctrl Pts',(-4.37513795036318,-0.341330640933386,
55.6636942520571));
#64540=CARTESIAN_POINT('Ctrl Pts',(-4.18538392269166,-2.12848606629693,
55.7288986501012));
#64541=CARTESIAN_POINT('Ctrl Pts',(-1.7316503614075,-4.86861791907028,55.8470233022273));
#64542=CARTESIAN_POINT('Ctrl Pts',(3.15105239533607,-4.09547582313724,56.0057840644731));
#64543=CARTESIAN_POINT('Ctrl Pts',(5.14981574971942,0.425970844068908,56.1645448267191));
#64544=CARTESIAN_POINT('Ctrl Pts',(2.43531042678924,4.55755598333432,56.3233055889649));
#64545=CARTESIAN_POINT('Ctrl Pts',(-2.50806538626398,4.517926674292,56.4820663512109));
#64546=CARTESIAN_POINT('Ctrl Pts',(-4.33218063910257,1.64211842271798,56.5914345242541));
#64547=CARTESIAN_POINT('Ctrl Pts',(-4.37882202467515,0.0982449665847532,
56.6478824432155));
#64548=CARTESIAN_POINT('Ctrl Pts',(-4.37833561871486,0.00173199218209092,
56.6514101080949));
#64549=CARTESIAN_POINT('Ctrl Pts',(-4.37792086111113,0.00210556704416347,
55.848589891905));
#64550=CARTESIAN_POINT('Ctrl Pts',(-4.37002924341455,-1.32628327647185,
55.8971319064456));
#64551=CARTESIAN_POINT('Ctrl Pts',(-3.01639925320847,-4.11679727890053,
55.9985941750683));
#64552=CARTESIAN_POINT('Ctrl Pts',(1.73165038597632,-4.86861798815274,56.1529766977727));
#64553=CARTESIAN_POINT('Ctrl Pts',(5.02949388480597,-1.18585219842773,56.3117374600186));
#64554=CARTESIAN_POINT('Ctrl Pts',(3.72419095237009,3.58224174562538,56.4704982222645));
#64555=CARTESIAN_POINT('Ctrl Pts',(-0.989605296568694,5.07175862308326,
56.6292589845104));
#64556=CARTESIAN_POINT('Ctrl Pts',(-4.01260884555851,2.56932936205486,56.7552895410572));
#64557=CARTESIAN_POINT('Ctrl Pts',(-4.36948468076768,0.558854755667328,
56.8283998435221));
#64558=CARTESIAN_POINT('Ctrl Pts',(-4.36645415447485,0.00261097933498031,
56.848589891905));
#64559=CARTESIAN_POINT('Origin',(0.,0.,24.1514101080949));
#64560=CARTESIAN_POINT('',(-4.36494997391578,0.000736207605459677,54.651410108095));
#64561=CARTESIAN_POINT('',(-4.37274842293649,-0.00394778047225652,54.848589891905));
#64562=CARTESIAN_POINT('',(-4.372,3.82579154166093E-12,24.1514101080949));
#64563=CARTESIAN_POINT('Ctrl Pts',(-4.36494997391578,0.000736207605459838,
54.651410108095));
#64564=CARTESIAN_POINT('Ctrl Pts',(-4.36378453680234,-0.773985575709198,
54.6795060608986));
#64565=CARTESIAN_POINT('Ctrl Pts',(-3.79750074957444,-3.0095293451424,54.7605222677843));
#64566=CARTESIAN_POINT('Ctrl Pts',(-0.22562389770033,-5.16247491740555,
54.8944587287519));
#64567=CARTESIAN_POINT('Ctrl Pts',(4.21477629650059,-2.98960100791253,55.0532194909978));
#64568=CARTESIAN_POINT('Ctrl Pts',(4.79768448212587,1.91944706257383,55.2119802532437));
#64569=CARTESIAN_POINT('Ctrl Pts',(0.989605282528937,5.07175855111871,55.3707410154895));
#64570=CARTESIAN_POINT('Ctrl Pts',(-3.35946002969715,3.69749334286384,55.5172176337734));
#64571=CARTESIAN_POINT('Ctrl Pts',(-4.36178715915881,1.11193390546508,55.6107739979751));
#64572=CARTESIAN_POINT('Ctrl Pts',(-4.37203889039062,-0.0039907847152907,
55.6514101080949));
#64573=CARTESIAN_POINT('Ctrl Pts',(-4.37274842293649,-0.00394778047225635,
54.848589891905));
#64574=CARTESIAN_POINT('Ctrl Pts',(-4.37564665776889,-0.317799192266558,
54.8600234612052));
#64575=CARTESIAN_POINT('Ctrl Pts',(-4.20162062889501,-2.08112280559727,
54.9243772845874));
#64576=CARTESIAN_POINT('Ctrl Pts',(-1.80948281276126,-4.84022996603858,
55.0416513620516));
#64577=CARTESIAN_POINT('Ctrl Pts',(3.08498768485217,-4.1454680264268,55.2004121242973));
#64578=CARTESIAN_POINT('Ctrl Pts',(5.15598322111311,0.34335287594041,55.3591728865433));
#64579=CARTESIAN_POINT('Ctrl Pts',(2.50806542185317,4.51792673839683,55.5179336487891));
#64580=CARTESIAN_POINT('Ctrl Pts',(-2.43531046134262,4.55755604800332,55.6766944110351));
#64581=CARTESIAN_POINT('Ctrl Pts',(-4.31984022389642,1.68922674479917,55.7869131587403));
#64582=CARTESIAN_POINT('Ctrl Pts',(-4.37863264435646,0.121919394632788,
55.8442116523636));
#64583=CARTESIAN_POINT('Ctrl Pts',(-4.37792086111113,0.00210556704416347,
55.848589891905));
#64584=CARTESIAN_POINT('Origin',(0.,0.,24.1514101080949));
#64585=CARTESIAN_POINT('',(-4.37473956626258,0.00360433591460132,53.6514101080949));
#64586=CARTESIAN_POINT('',(-4.36486283016371,0.00035491530368581,53.848589891905));
#64587=CARTESIAN_POINT('',(-4.372,3.82579154166093E-12,24.1514101080949));
#64588=CARTESIAN_POINT('Ctrl Pts',(-4.37473956626258,0.00360433591460166,
53.6514101080949));
#64589=CARTESIAN_POINT('Ctrl Pts',(-4.36404265119134,-1.20025020685171,
53.6953178697402));
#64590=CARTESIAN_POINT('Ctrl Pts',(-3.22404333927935,-3.87285840602707,
53.7921458854674));
#64591=CARTESIAN_POINT('Ctrl Pts',(1.30029707219943,-5.00112796677752,53.9418941552766));
#64592=CARTESIAN_POINT('Ctrl Pts',(4.90686007449561,-1.62011654684958,54.1006549175225));
#64593=CARTESIAN_POINT('Ctrl Pts',(4.02251485462088,3.2436750238594,54.2594156797684));
#64594=CARTESIAN_POINT('Ctrl Pts',(-0.543358829519001,5.13875613338857,
54.4181764420142));
#64595=CARTESIAN_POINT('Ctrl Pts',(-3.89191662696183,2.82763508414209,54.5488412514565));
#64596=CARTESIAN_POINT('Ctrl Pts',(-4.3659797009454,0.685245008222085,54.6265858068167));
#64597=CARTESIAN_POINT('Ctrl Pts',(-4.36494997391578,0.000736207605459838,
54.651410108095));
#64598=CARTESIAN_POINT('Ctrl Pts',(-4.36486283016371,0.000354915303685741,
53.848589891905));
#64599=CARTESIAN_POINT('Ctrl Pts',(-4.36431860610875,-0.750950458311704,
53.8758352700467));
#64600=CARTESIAN_POINT('Ctrl Pts',(-3.82280092431587,-2.96229440941745,
53.9560009022705));
#64601=CARTESIAN_POINT('Ctrl Pts',(-0.308361083986154,-5.15819422043212,
54.0890867885761));
#64602=CARTESIAN_POINT('Ctrl Pts',(4.16630456733569,-3.05678923480409,54.2478475508221));
#64603=CARTESIAN_POINT('Ctrl Pts',(4.82784101720183,1.84228262935957,54.4066083130679));
#64604=CARTESIAN_POINT('Ctrl Pts',(1.07078989980086,5.0552411578777,54.5653690753139));
#64605=CARTESIAN_POINT('Ctrl Pts',(-3.3251283689399,3.74330363517374,54.7126962682595));
#64606=CARTESIAN_POINT('Ctrl Pts',(-4.36223218327779,1.13486147913407,54.8071032071232));
#64607=CARTESIAN_POINT('Ctrl Pts',(-4.37274842293649,-0.00394778047225635,
54.848589891905));
#64608=CARTESIAN_POINT('Origin',(0.,0.,24.1514101080949));
#64609=CARTESIAN_POINT('',(-4.37641405919053,-0.00301495007056918,52.6514101080949));
#64610=CARTESIAN_POINT('',(-4.37405090679819,0.00376197565890995,52.848589891905));
#64611=CARTESIAN_POINT('',(-4.372,3.82579154166093E-12,24.1514101080949));
#64612=CARTESIAN_POINT('Ctrl Pts',(-4.37641405919053,-0.00301495007056837,
52.651410108095));
#64613=CARTESIAN_POINT('Ctrl Pts',(-4.37788112208874,-0.189251796122769,
52.6582094244998));
#64614=CARTESIAN_POINT('Ctrl Pts',(-4.28250642368832,-1.82348881026957,
52.7179289949866));
#64615=CARTESIAN_POINT('Ctrl Pts',(-2.22485744252472,-4.66391067415503,
52.8305688195554));
#64616=CARTESIAN_POINT('Ctrl Pts',(2.71156366187259,-4.39880391966578,52.9893295818012));
#64617=CARTESIAN_POINT('Ctrl Pts',(5.16627887713359,-0.107777454683187,
53.1480903440472));
#64618=CARTESIAN_POINT('Ctrl Pts',(2.89265785799892,4.28189022893068,53.306851106293));
#64619=CARTESIAN_POINT('Ctrl Pts',(-2.02841199016113,4.75264118298715,53.4656118685389));
#64620=CARTESIAN_POINT('Ctrl Pts',(-4.24545291415805,1.94643078465362,53.5804648691395));
#64621=CARTESIAN_POINT('Ctrl Pts',(-4.37693521146432,0.250707115811383,
53.6423976156582));
#64622=CARTESIAN_POINT('Ctrl Pts',(-4.37473956626258,0.00360433591460166,
53.6514101080949));
#64623=CARTESIAN_POINT('Ctrl Pts',(-4.37405090679819,0.00376197565890985,
52.848589891905));
#64624=CARTESIAN_POINT('Ctrl Pts',(-4.36331136726339,-1.17725226132736,
52.8916470788883));
#64625=CARTESIAN_POINT('Ctrl Pts',(-3.26012737634599,-3.8274917595608,52.9876245199536));
#64626=CARTESIAN_POINT('Ctrl Pts',(1.21995054602492,-5.021331978576,53.1365222151008));
#64627=CARTESIAN_POINT('Ctrl Pts',(4.88025534693686,-1.69857643999627,53.2952829773467));
#64628=CARTESIAN_POINT('Ctrl Pts',(4.07400138499168,3.17876814016096,53.4540437395925));
#64629=CARTESIAN_POINT('Ctrl Pts',(-0.460903086490536,5.14680702170578,
53.6128045018385));
#64630=CARTESIAN_POINT('Ctrl Pts',(-3.86811921206171,2.87497489714133,53.7443198859426));
#64631=CARTESIAN_POINT('Ctrl Pts',(-4.365375683574,0.708352879597865,53.8229150159648));
#64632=CARTESIAN_POINT('Ctrl Pts',(-4.36486283016371,0.000354915303685741,
53.848589891905));
#64633=CARTESIAN_POINT('Origin',(0.,0.,24.1514101080949));
#64634=CARTESIAN_POINT('',(-4.36545824626946,-0.00168887658937792,51.651410108095));
#64635=CARTESIAN_POINT('',(-4.37699111974124,-0.00272425946348631,51.848589891905));
#64636=CARTESIAN_POINT('',(-4.372,3.82579154166093E-12,24.1514101080949));
#64637=CARTESIAN_POINT('Ctrl Pts',(-4.36545824626946,-0.00168887658937779,
51.651410108095));
#64638=CARTESIAN_POINT('Ctrl Pts',(-4.36762412827266,-0.624989998325019,
51.6740212333413));
#64639=CARTESIAN_POINT('Ctrl Pts',(-3.95142248851676,-2.70433810681889,
51.7495526126697));
#64640=CARTESIAN_POINT('Ctrl Pts',(-0.757199377814005,-5.111624254412,51.87800424608));
#64641=CARTESIAN_POINT('Ctrl Pts',(3.88373669535471,-3.40861301664037,52.0367650083259));
#64642=CARTESIAN_POINT('Ctrl Pts',(4.97015831465276,1.41406497140078,52.1955257705718));
#64643=CARTESIAN_POINT('Ctrl Pts',(1.50773922891819,4.94254750443899,52.3542865328176));
#64644=CARTESIAN_POINT('Ctrl Pts',(-3.12722350039883,3.99007665346195,52.5062479786588));
#64645=CARTESIAN_POINT('Ctrl Pts',(-4.36646271813384,1.26026174695854,52.6052891704178));
#64646=CARTESIAN_POINT('Ctrl Pts',(-4.37641405919053,-0.00301495007056837,
52.651410108095));
#64647=CARTESIAN_POINT('Ctrl Pts',(-4.37699111974124,-0.00272425946348602,
51.848589891905));
#64648=CARTESIAN_POINT('Ctrl Pts',(-4.37818018489292,-0.165607164620367,
51.8545386336479));
#64649=CARTESIAN_POINT('Ctrl Pts',(-4.29599872620153,-1.77629134844302,
51.9134076294728));
#64650=CARTESIAN_POINT('Ctrl Pts',(-2.2993445899923,-4.62764180012773,52.0251968793796));
#64651=CARTESIAN_POINT('Ctrl Pts',(2.64069239313623,-4.44171114083851,52.1839576416255));
#64652=CARTESIAN_POINT('Ctrl Pts',(5.16388703706709,-0.190590771620509,
52.3427184038713));
#64653=CARTESIAN_POINT('Ctrl Pts',(2.96093453169081,4.23496409345547,52.5014791661172));
#64654=CARTESIAN_POINT('Ctrl Pts',(-1.95195570001178,4.78455046153847,52.6602399283632));
#64655=CARTESIAN_POINT('Ctrl Pts',(-4.23045159262607,1.99372864599193,52.7759435036257));
#64656=CARTESIAN_POINT('Ctrl Pts',(-4.37651100246309,0.274295735060812,
52.8387268248063));
#64657=CARTESIAN_POINT('Ctrl Pts',(-4.37405090679819,0.00376197565890985,
52.848589891905));
#64658=CARTESIAN_POINT('Origin',(0.,0.,24.1514101080949));
#64659=CARTESIAN_POINT('',(-4.3702345064702,0.00391522497022664,50.651410108095));
#64660=CARTESIAN_POINT('',(-4.36575804463348,-0.0020306512688445,50.848589891905));
#64661=CARTESIAN_POINT('',(-4.372,3.82579154166093E-12,24.1514101080949));
#64662=CARTESIAN_POINT('Ctrl Pts',(-4.3702345064702,0.00391522497022637,
50.651410108095));
#64663=CARTESIAN_POINT('Ctrl Pts',(-4.36105392339508,-1.0523431449496,50.6898330421829));
#64664=CARTESIAN_POINT('Ctrl Pts',(-3.44595349118066,-3.57765592823792,
50.7811762303528));
#64665=CARTESIAN_POINT('Ctrl Pts',(0.777225141445664,-5.10861766973804,
50.9254396726047));
#64666=CARTESIAN_POINT('Ctrl Pts',(4.71345919711634,-2.11786586288516,51.0842004348506));
#64667=CARTESIAN_POINT('Ctrl Pts',(4.33579142110028,2.81122147273531,51.2429611970965));
#64668=CARTESIAN_POINT('Ctrl Pts',(-0.0101251019801382,5.16739304663044,
51.4017219593423));
#64669=CARTESIAN_POINT('Ctrl Pts',(-3.72913776533524,3.13220382459871,51.5378715963418));
#64670=CARTESIAN_POINT('Ctrl Pts',(-4.36255498533209,0.833816380056773,
51.6211009792594));
#64671=CARTESIAN_POINT('Ctrl Pts',(-4.36545824626946,-0.00168887658937779,
51.651410108095));
#64672=CARTESIAN_POINT('Ctrl Pts',(-4.36575804463348,-0.00203065126884408,
50.848589891905));
#64673=CARTESIAN_POINT('Ctrl Pts',(-4.36827427270984,-0.601781773597835,
50.8703504424894));
#64674=CARTESIAN_POINT('Ctrl Pts',(-3.97337829241374,-2.65691780935309,
50.9450312471558));
#64675=CARTESIAN_POINT('Ctrl Pts',(-0.839052999411725,-5.09882773174331,
51.0726323059043));
#64676=CARTESIAN_POINT('Ctrl Pts',(3.82858979556074,-3.47044008032763,51.2313930681501));
#64677=CARTESIAN_POINT('Ctrl Pts',(4.99219026383802,1.33420033857639,51.390153830396));
#64678=CARTESIAN_POINT('Ctrl Pts',(1.58678571421362,4.91773985393535,51.548914592642));
#64679=CARTESIAN_POINT('Ctrl Pts',(-3.08887708143298,4.03478571508497,51.7017266131449));
#64680=CARTESIAN_POINT('Ctrl Pts',(-4.36760221182464,1.28340593748707,51.8016183795659));
#64681=CARTESIAN_POINT('Ctrl Pts',(-4.37699111974124,-0.00272425946348602,
51.848589891905));
#64682=CARTESIAN_POINT('Origin',(0.,0.,24.1514101080949));
#64683=CARTESIAN_POINT('',(-4.3790496246733,-0.000667733410364872,49.651410108095));
#64684=CARTESIAN_POINT('',(-4.36957357182231,0.00381643768188569,49.848589891905));
#64685=CARTESIAN_POINT('',(-4.372,3.82579154166093E-12,24.1514101080949));
#64686=CARTESIAN_POINT('Ctrl Pts',(-4.3790496246733,-0.000667733410364751,
49.651410108095));
#64687=CARTESIAN_POINT('Ctrl Pts',(-4.37912616480055,-0.0366150338825652,
49.6527245969425));
#64688=CARTESIAN_POINT('Ctrl Pts',(-4.36244279655587,-1.51969860268292,
49.706959339872));
#64689=CARTESIAN_POINT('Ctrl Pts',(-2.69430468338317,-4.40939629531691,
49.8141143368835));
#64690=CARTESIAN_POINT('Ctrl Pts',(2.2431174238849,-4.6551560273227,49.9728750991294));
#64691=CARTESIAN_POINT('Ctrl Pts',(5.12756994789964,-0.640374769530455,
50.1316358613752));
#64692=CARTESIAN_POINT('Ctrl Pts',(3.31911383193326,3.96049703783808,50.2903966236212));
#64693=CARTESIAN_POINT('Ctrl Pts',(-1.52709664667054,4.93660098122003,50.4491573858669));
#64694=CARTESIAN_POINT('Ctrl Pts',(-4.14104743841719,2.25180987009099,50.569495214025));
#64695=CARTESIAN_POINT('Ctrl Pts',(-4.37369842336595,0.402451046051582,
50.636912788101));
#64696=CARTESIAN_POINT('Ctrl Pts',(-4.3702345064702,0.00391522497022637,
50.651410108095));
#64697=CARTESIAN_POINT('Ctrl Pts',(-4.36957357182231,0.00381643768188559,
49.848589891905));
#64698=CARTESIAN_POINT('Ctrl Pts',(-4.36092390126923,-1.02945575440987,
49.886162251331));
#64699=CARTESIAN_POINT('Ctrl Pts',(-3.47811671755736,-3.53137427358546,
49.976654864839));
#64700=CARTESIAN_POINT('Ctrl Pts',(0.695222531978707,-5.12042183856424,
50.1200677324289));
#64701=CARTESIAN_POINT('Ctrl Pts',(4.67889927324325,-2.19316113513354,50.2788284946747));
#64702=CARTESIAN_POINT('Ctrl Pts',(4.38030448079635,2.74134763015048,50.4375892569207));
#64703=CARTESIAN_POINT('Ctrl Pts',(0.0727212293821569,5.16689130876717,
50.5963500191666));
#64704=CARTESIAN_POINT('Ctrl Pts',(-3.70187703653703,3.1792474229629,50.733350230828));
#64705=CARTESIAN_POINT('Ctrl Pts',(-4.36215496848489,0.85677423381658,50.8174301884075));
#64706=CARTESIAN_POINT('Ctrl Pts',(-4.36575804463348,-0.00203065126884408,
50.848589891905));
#64707=CARTESIAN_POINT('Origin',(0.,0.,24.1514101080949));
#64708=CARTESIAN_POINT('',(-4.36828286829859,-0.0034930826256922,48.651410108095));
#64709=CARTESIAN_POINT('',(-4.37915940465982,-0.00023684953408154,48.848589891905));
#64710=CARTESIAN_POINT('',(-4.372,3.82579154166093E-12,24.1514101080949));
#64711=CARTESIAN_POINT('Ctrl Pts',(-4.36828286829859,-0.00349308262569223,
48.651410108095));
#64712=CARTESIAN_POINT('Ctrl Pts',(-4.37181608551705,-0.47483281190334,
48.6685364057841));
#64713=CARTESIAN_POINT('Ctrl Pts',(-4.08436231910608,-2.39841849396994,
48.7385829575551));
#64714=CARTESIAN_POINT('Ctrl Pts',(-1.2806885257803,-5.00618520592171,48.8615497634081));
#64715=CARTESIAN_POINT('Ctrl Pts',(3.51122164426531,-3.79122354667958,49.020310525654));
#64716=CARTESIAN_POINT('Ctrl Pts',(5.0895545138177,0.893581706914796,49.1790712878999));
#64717=CARTESIAN_POINT('Ctrl Pts',(2.00977162985725,4.76055368753214,49.3378320501457));
#64718=CARTESIAN_POINT('Ctrl Pts',(-2.86868632585708,4.274578831514,49.4952783235442));
#64719=CARTESIAN_POINT('Ctrl Pts',(-4.37604472140215,1.41059410609646,49.5998043428605));
#64720=CARTESIAN_POINT('Ctrl Pts',(-4.3790496246733,-0.000667733410364751,
49.651410108095));
#64721=CARTESIAN_POINT('Ctrl Pts',(-4.37915940465982,-0.000236849534081855,
48.848589891905));
#64722=CARTESIAN_POINT('Ctrl Pts',(-4.37916937864932,-0.0129226461636581,
48.8490538060906));
#64723=CARTESIAN_POINT('Ctrl Pts',(-4.37337449519616,-1.47271062880396,
48.9024379743582));
#64724=CARTESIAN_POINT('Ctrl Pts',(-2.76465105904324,-4.36563382517906,
49.0087423967076));
#64725=CARTESIAN_POINT('Ctrl Pts',(2.16819644989342,-4.69052004883103,49.1675031589536));
#64726=CARTESIAN_POINT('Ctrl Pts',(5.11664433946473,-0.72249904999246,49.3262639211995));
#64727=CARTESIAN_POINT('Ctrl Pts',(3.38218303962157,3.90677514842007,49.4850246834453));
#64728=CARTESIAN_POINT('Ctrl Pts',(-1.44775548820939,4.96044939699782,49.6437854456913));
#64729=CARTESIAN_POINT('Ctrl Pts',(-4.12319150304179,2.29923281750856,49.7649738485111));
#64730=CARTESIAN_POINT('Ctrl Pts',(-4.37310686689576,0.425896738132308,
49.833241997249));
#64731=CARTESIAN_POINT('Ctrl Pts',(-4.36957357182231,0.00381643768188559,
49.848589891905));
#64732=CARTESIAN_POINT('Origin',(0.,0.,24.1514101080949));
#64733=CARTESIAN_POINT('',(-4.36655943089002,0.00268207779483023,47.651410108095));
#64734=CARTESIAN_POINT('',(-4.36888289277856,-0.00366680700230215,47.848589891905));
#64735=CARTESIAN_POINT('',(-4.372,3.82579154166093E-12,24.1514101080949));
#64736=CARTESIAN_POINT('Ctrl Pts',(-4.36655943089002,0.00268207779483047,
47.651410108095));
#64737=CARTESIAN_POINT('Ctrl Pts',(-4.36147330371707,-0.90472081724388,
47.6843482146256));
#64738=CARTESIAN_POINT('Ctrl Pts',(-3.64307749349284,-3.2773877690834,47.7702065752383));
#64739=CARTESIAN_POINT('Ctrl Pts',(0.245853018125491,-5.16155109531365,
47.9089851899327));
#64740=CARTESIAN_POINT('Ctrl Pts',(4.46972204405066,-2.59299792999961,48.0677459521787));
#64741=CARTESIAN_POINT('Ctrl Pts',(4.60276492582317,2.34874614500311,48.2265067144246));
#64742=CARTESIAN_POINT('Ctrl Pts',(0.523216754197009,5.14084600471386,48.3852674766704));
#64743=CARTESIAN_POINT('Ctrl Pts',(-3.54345722553092,3.4342468351364,48.5269019412272));
#64744=CARTESIAN_POINT('Ctrl Pts',(-4.36089844550389,0.981606792564894,
48.6156161517021));
#64745=CARTESIAN_POINT('Ctrl Pts',(-4.36828286829859,-0.00349308262569223,
48.651410108095));
#64746=CARTESIAN_POINT('Ctrl Pts',(-4.36888289277856,-0.00366680700230278,
47.848589891905));
#64747=CARTESIAN_POINT('Ctrl Pts',(-4.37244155465394,-0.451442255901039,
47.8648656149322));
#64748=CARTESIAN_POINT('Ctrl Pts',(-4.10318789366455,-2.35097548418382,
47.9340615920413));
#64749=CARTESIAN_POINT('Ctrl Pts',(-1.36078444624568,-4.98500951500319,
48.0561778232324));
#64750=CARTESIAN_POINT('Ctrl Pts',(3.44998850215064,-3.84702917961962,48.2149385854782));
#64751=CARTESIAN_POINT('Ctrl Pts',(5.10322659210776,0.811869769988193,48.3736993477241));
#64752=CARTESIAN_POINT('Ctrl Pts',(2.08583582488191,4.72772070721777,48.53246010997));
#64753=CARTESIAN_POINT('Ctrl Pts',(-2.82618015492052,4.31781852687336,48.6907569580302));
#64754=CARTESIAN_POINT('Ctrl Pts',(-4.37803161206443,1.43418891395024,48.7961335520086));
#64755=CARTESIAN_POINT('Ctrl Pts',(-4.37915940465982,-0.000236849534081855,
48.848589891905));
#64756=CARTESIAN_POINT('Origin',(0.,0.,24.1514101080949));
#64757=CARTESIAN_POINT('',(-4.37802849378088,0.00201652107500087,46.651410108095));
#64758=CARTESIAN_POINT('',(-4.36614763918315,0.00238232933584437,46.848589891905));
#64759=CARTESIAN_POINT('',(-4.372,3.82579154166093E-12,24.1514101080949));
#64760=CARTESIAN_POINT('Ctrl Pts',(-4.37802849378088,0.00201652107500106,
46.651410108095));
#64761=CARTESIAN_POINT('Ctrl Pts',(-4.37038284048536,-1.33197484216078,
46.7001600234672));
#64762=CARTESIAN_POINT('Ctrl Pts',(-3.00664095593531,-4.12759897737828,
46.8018301929213));
#64763=CARTESIAN_POINT('Ctrl Pts',(1.75071634247466,-4.86179449424254,46.9564206164574));
#64764=CARTESIAN_POINT('Ctrl Pts',(5.03410234489664,-1.16613335307792,47.1151813787034));
#64765=CARTESIAN_POINT('Ctrl Pts',(3.71012411261097,3.59680865283067,47.2739421409492));
#64766=CARTESIAN_POINT('Ctrl Pts',(-1.00947303475291,5.06784151371782,47.4327029031951));
#64767=CARTESIAN_POINT('Ctrl Pts',(-4.01767618670528,2.55773240591479,47.5585255589103));
#64768=CARTESIAN_POINT('Ctrl Pts',(-4.36964496780575,0.553164799693178,
47.6314279605436));
#64769=CARTESIAN_POINT('Ctrl Pts',(-4.36655943089002,0.00268207779483047,
47.651410108095));
#64770=CARTESIAN_POINT('Ctrl Pts',(-4.36614763918315,0.00238232933584499,
46.848589891905));
#64771=CARTESIAN_POINT('Ctrl Pts',(-4.36177165814571,-0.881797305075611,
46.8806774237737));
#64772=CARTESIAN_POINT('Ctrl Pts',(-3.67150621186276,-3.23048848803606,
46.9656852097244));
#64773=CARTESIAN_POINT('Ctrl Pts',(0.163070052891163,-5.16482936133098,
47.103613249757));
#64774=CARTESIAN_POINT('Ctrl Pts',(4.42757599841828,-2.66432448325026,47.2623740120029));
#64775=CARTESIAN_POINT('Ctrl Pts',(4.63982914812316,2.27465154475207,47.4211347742487));
#64776=CARTESIAN_POINT('Ctrl Pts',(0.605568936039063,5.13179699886122,47.5798955364947));
#64777=CARTESIAN_POINT('Ctrl Pts',(-3.51252635231322,3.4807591641629,47.7223805757134));
#64778=CARTESIAN_POINT('Ctrl Pts',(-4.36087062227061,1.00449248124495,47.8119453608502));
#64779=CARTESIAN_POINT('Ctrl Pts',(-4.36888289277856,-0.00366680700230278,
47.848589891905));
#64780=CARTESIAN_POINT('Origin',(0.,0.,24.1514101080949));
#64781=CARTESIAN_POINT('',(-4.37257478030532,-0.00396203305634906,45.651410108095));
#64782=CARTESIAN_POINT('',(-4.37756404870526,0.00237073416934012,45.848589891905));
#64783=CARTESIAN_POINT('',(-4.372,3.82579154166093E-12,24.1514101080949));
#64784=CARTESIAN_POINT('Ctrl Pts',(-4.37257478030532,-0.00396203305634935,
45.651410108095));
#64785=CARTESIAN_POINT('Ctrl Pts',(-4.3755247754399,-0.323552849206446,
45.6630515782267));
#64786=CARTESIAN_POINT('Ctrl Pts',(-4.19769260696374,-2.0926975991144,45.7276133024405));
#64787=CARTESIAN_POINT('Ctrl Pts',(-1.79050086272392,-4.84728378338218,
45.8450952807362));
#64788=CARTESIAN_POINT('Ctrl Pts',(3.1012093298518,-4.13334659912459,46.0038560429821));
#64789=CARTESIAN_POINT('Ctrl Pts',(5.15459801607478,0.363555647367575,46.162616805228));
#64790=CARTESIAN_POINT('Ctrl Pts',(2.49034114873962,4.52772066043712,46.3213775674739));
#64791=CARTESIAN_POINT('Ctrl Pts',(-2.45315200638293,4.54797742404625,46.4801383297198));
#64792=CARTESIAN_POINT('Ctrl Pts',(-4.32289330486948,1.67770933141668,46.5901491765935));
#64793=CARTESIAN_POINT('Ctrl Pts',(-4.37868254545781,0.116133556522668,
46.6472397693852));
#64794=CARTESIAN_POINT('Ctrl Pts',(-4.37802849378088,0.00201652107500106,
46.651410108095));
#64795=CARTESIAN_POINT('Ctrl Pts',(-4.37756404870526,0.00237073416934035,
45.848589891905));
#64796=CARTESIAN_POINT('Ctrl Pts',(-4.36898434288233,-1.30871296070451,
45.8964892326153));
#64797=CARTESIAN_POINT('Ctrl Pts',(-3.04632193268225,-4.08332402648612,
45.9973088274075));
#64798=CARTESIAN_POINT('Ctrl Pts',(1.67254576409749,-4.88923765436041,46.1510486762816));
#64799=CARTESIAN_POINT('Ctrl Pts',(5.01475964555148,-1.2466915701828,46.3098094385276));
#64800=CARTESIAN_POINT('Ctrl Pts',(3.76731232156889,3.53686471971598,46.4685702007735));
#64801=CARTESIAN_POINT('Ctrl Pts',(-0.928094313166731,5.08337438319113,
46.6273309630193));
#64802=CARTESIAN_POINT('Ctrl Pts',(-3.99675882839479,2.60517577302872,46.7540041933965));
#64803=CARTESIAN_POINT('Ctrl Pts',(-4.36898873016318,0.576432985076398,
46.8277571696918));
#64804=CARTESIAN_POINT('Ctrl Pts',(-4.36614763918315,0.00238232933584499,
46.848589891905));
#64805=CARTESIAN_POINT('Origin',(0.,0.,24.1514101080949));
#64806=CARTESIAN_POINT('',(-4.36487844624636,0.000448538275869127,44.651410108095));
#64807=CARTESIAN_POINT('',(-4.37328422903404,-0.00388840045026428,44.848589891905));
#64808=CARTESIAN_POINT('',(-4.372,3.82579154166093E-12,24.1514101080949));
#64809=CARTESIAN_POINT('Ctrl Pts',(-4.36487844624636,0.00044853827586927,
44.651410108095));
#64810=CARTESIAN_POINT('Ctrl Pts',(-4.36418527448618,-0.756583014477848,
44.6788633870683));
#64811=CARTESIAN_POINT('Ctrl Pts',(-3.8166662948363,-2.9738437257919,44.7592369201236));
#64812=CARTESIAN_POINT('Ctrl Pts',(-0.288144634510089,-5.15936295347187,
44.8925307072609));
#64813=CARTESIAN_POINT('Ctrl Pts',(4.17825154873217,-3.04043868735616,45.0512914695067));
#64814=CARTESIAN_POINT('Ctrl Pts',(4.8205842882194,1.86118793683688,45.2100522317526));
#64815=CARTESIAN_POINT('Ctrl Pts',(1.05097104046387,5.05939851051103,45.3688129939986));
#64816=CARTESIAN_POINT('Ctrl Pts',(-3.33357615425217,3.73211986818334,45.5159322861126));
#64817=CARTESIAN_POINT('Ctrl Pts',(-4.36211457120495,1.12925568798617,45.6101313241448));
#64818=CARTESIAN_POINT('Ctrl Pts',(-4.37257478030532,-0.00396203305634935,
45.651410108095));
#64819=CARTESIAN_POINT('Ctrl Pts',(-4.37328422903404,-0.00388840045026397,
44.848589891905));
#64820=CARTESIAN_POINT('Ctrl Pts',(-4.37601255181714,-0.300005218706897,
44.8593807873749));
#64821=CARTESIAN_POINT('Ctrl Pts',(-4.21359764945945,-2.04535030654532,
44.9230919369267));
#64822=CARTESIAN_POINT('Ctrl Pts',(-1.8679837165673,-4.81795506501003,45.0397233405604));
#64823=CARTESIAN_POINT('Ctrl Pts',(3.03454387031403,-4.18253483822383,45.1984841028063));
#64824=CARTESIAN_POINT('Ctrl Pts',(5.15976421573454,0.280869029694986,45.3572448650522));
#64825=CARTESIAN_POINT('Ctrl Pts',(2.56261074386464,4.4872129823807,45.5160056272982));
#64826=CARTESIAN_POINT('Ctrl Pts',(-2.37992235675453,4.58672254988638,45.6747663895439));
#64827=CARTESIAN_POINT('Ctrl Pts',(-4.31025055648257,1.72484198053187,45.7856278110796));
#64828=CARTESIAN_POINT('Ctrl Pts',(-4.37846339218375,0.139801386813307,
45.8435689785333));
#64829=CARTESIAN_POINT('Ctrl Pts',(-4.37756404870526,0.00237073416934035,
45.848589891905));
#64830=CARTESIAN_POINT('Origin',(0.,0.,24.1514101080949));
#64831=CARTESIAN_POINT('',(-4.37422072754471,0.00372710199133062,43.651410108095));
#64832=CARTESIAN_POINT('',(-4.36483752583336,6.45211600033835E-5,43.848589891905));
#64833=CARTESIAN_POINT('',(-4.372,3.82579154166093E-12,24.1514101080949));
#64834=CARTESIAN_POINT('Ctrl Pts',(-4.37422072754471,0.00372710199133028,
43.651410108095));
#64835=CARTESIAN_POINT('Ctrl Pts',(-4.36348027804383,-1.18287063932153,
43.6946751959099));
#64836=CARTESIAN_POINT('Ctrl Pts',(-3.25136487986307,-3.83859580238497,
43.7908605378067));
#64837=CARTESIAN_POINT('Ctrl Pts',(1.23961889884326,-5.01651257365967,43.9399661337855));
#64838=CARTESIAN_POINT('Ctrl Pts',(4.88687423334376,-1.67943849054845,44.0987268960314));
#64839=CARTESIAN_POINT('Ctrl Pts',(4.06151299797099,3.19470899822934,44.2574876582773));
#64840=CARTESIAN_POINT('Ctrl Pts',(-0.481068993674721,5.1449612281707,44.4162484205232));
#64841=CARTESIAN_POINT('Ctrl Pts',(-3.87398394218857,2.8634067002645,44.5475559037957));
#64842=CARTESIAN_POINT('Ctrl Pts',(-4.36552146553668,0.702707227634927,
44.6259431329863));
#64843=CARTESIAN_POINT('Ctrl Pts',(-4.36487844624636,0.00044853827586927,
44.651410108095));
#64844=CARTESIAN_POINT('Ctrl Pts',(-4.36483752583336,6.45211600032447E-5,
43.848589891905));
#64845=CARTESIAN_POINT('Ctrl Pts',(-4.36474095456816,-0.733529397636361,
43.8751925962164));
#64846=CARTESIAN_POINT('Ctrl Pts',(-3.84156354313547,-2.92657717231582,
43.9547155546098));
#64847=CARTESIAN_POINT('Ctrl Pts',(-0.370823894361365,-5.15408030721166,
44.0871587670851));
#64848=CARTESIAN_POINT('Ctrl Pts',(4.12896947009338,-3.10703480650815,44.245919529331));
#64849=CARTESIAN_POINT('Ctrl Pts',(4.84980385450403,1.78366385472551,44.4046802915768));
#64850=CARTESIAN_POINT('Ctrl Pts',(1.13194961208497,5.04189887339256,44.5634410538228));
#64851=CARTESIAN_POINT('Ctrl Pts',(-3.29878256966109,3.77781872906067,44.7114109205989));
#64852=CARTESIAN_POINT('Ctrl Pts',(-4.36263242638615,1.15219838236422,44.8064605332929));
#64853=CARTESIAN_POINT('Ctrl Pts',(-4.37328422903404,-0.00388840045026397,
44.848589891905));
#64854=CARTESIAN_POINT('Origin',(0.,0.,24.1514101080949));
#64855=CARTESIAN_POINT('',(-4.37685426135052,-0.00279837449763291,42.651410108095));
#64856=CARTESIAN_POINT('',(-4.37352103895722,0.00385464862035001,42.848589891905));
#64857=CARTESIAN_POINT('',(-4.372,3.82579154166093E-12,24.1514101080949));
#64858=CARTESIAN_POINT('Ctrl Pts',(-4.37685426135052,-0.00279837449763325,
42.651410108095));
#64859=CARTESIAN_POINT('Ctrl Pts',(-4.37811047462212,-0.171387646022154,
42.6575667506695));
#64860=CARTESIAN_POINT('Ctrl Pts',(-4.29273874071207,-1.78782473877565,
42.7166436473259));
#64861=CARTESIAN_POINT('Ctrl Pts',(-2.28119196804685,-4.63661693705371,
42.8286407980642));
#64862=CARTESIAN_POINT('Ctrl Pts',(2.65807838191241,-4.43132855153674,42.9874015603103));
#64863=CARTESIAN_POINT('Ctrl Pts',(5.1645942046841,-0.170352918960309,43.146162322556));
#64864=CARTESIAN_POINT('Ctrl Pts',(2.94431565674484,4.24653490854626,43.304923084802));
#64865=CARTESIAN_POINT('Ctrl Pts',(-1.97069051554003,4.77686427565358,43.4636838470478));
#64866=CARTESIAN_POINT('Ctrl Pts',(-4.23415771881522,1.98216556151801,43.5791795214788));
#64867=CARTESIAN_POINT('Ctrl Pts',(-4.37661759834636,0.26853179933828,43.6417549418279));
#64868=CARTESIAN_POINT('Ctrl Pts',(-4.37422072754471,0.00372710199133028,
43.651410108095));
#64869=CARTESIAN_POINT('Ctrl Pts',(-4.37352103895722,0.00385464862035015,
42.848589891905));
#64870=CARTESIAN_POINT('Ctrl Pts',(-4.36282818723577,-1.15989502481933,
42.891004405058));
#64871=CARTESIAN_POINT('Ctrl Pts',(-3.28698059005484,-3.79310505340026,
42.9863391722929));
#64872=CARTESIAN_POINT('Ctrl Pts',(1.15903352033341,-5.0357417996319,43.1345941936098));
#64873=CARTESIAN_POINT('Ctrl Pts',(4.85932100888344,-1.75757034181863,43.2933549558556));
#64874=CARTESIAN_POINT('Ctrl Pts',(4.11220948021047,3.12918317851219,43.4521157181016));
#64875=CARTESIAN_POINT('Ctrl Pts',(-0.398521773825228,5.15201267172389,
43.6108764803474));
#64876=CARTESIAN_POINT('Ctrl Pts',(-3.84979170382512,2.91072243457703,43.7430345382819));
#64877=CARTESIAN_POINT('Ctrl Pts',(-4.36493306195062,0.725795042513237,
43.8222723421345));
#64878=CARTESIAN_POINT('Ctrl Pts',(-4.36483752583336,6.45211600032447E-5,
43.848589891905));
#64879=CARTESIAN_POINT('Origin',(0.,0.,24.1514101080949));
#64880=CARTESIAN_POINT('',(-4.36567955402809,-0.00194869704108157,41.651410108095));
#64881=CARTESIAN_POINT('',(-4.37739485101806,-0.00248321819134589,41.848589891905));
#64882=CARTESIAN_POINT('',(-4.372,3.82579154166093E-12,24.1514101080949));
#64883=CARTESIAN_POINT('Ctrl Pts',(-4.3656795540281,-0.00194869704108112,
41.651410108095));
#64884=CARTESIAN_POINT('Ctrl Pts',(-4.36811474531132,-0.607457052316279,
41.673378559511));
#64885=CARTESIAN_POINT('Ctrl Pts',(-3.96805804018506,-2.66850978845469,
41.748267265009));
#64886=CARTESIAN_POINT('Ctrl Pts',(-0.819065114488867,-5.10207661195736,
41.8760762245889));
#64887=CARTESIAN_POINT('Ctrl Pts',(3.8421604015636,-3.45540979692878,42.0348369868349));
#64888=CARTESIAN_POINT('Ctrl Pts',(4.98692335778749,1.35375361111553,42.1935977490807));
#64889=CARTESIAN_POINT('Ctrl Pts',(1.56750172940691,4.92392036332446,42.3523585113267));
#64890=CARTESIAN_POINT('Ctrl Pts',(-3.09830846639719,4.02387607629251,42.504962630998));
#64891=CARTESIAN_POINT('Ctrl Pts',(-4.36731252351321,1.27774424309386,42.6046464965875));
#64892=CARTESIAN_POINT('Ctrl Pts',(-4.37685426135052,-0.00279837449763325,
42.651410108095));
#64893=CARTESIAN_POINT('Ctrl Pts',(-4.37739485101806,-0.00248321819134518,
41.8485898919051));
#64894=CARTESIAN_POINT('Ctrl Pts',(-4.37838119777137,-0.1477338083412,41.8538959598176));
#64895=CARTESIAN_POINT('Ctrl Pts',(-4.30592187837124,-1.74065025431473,
41.9121222818121));
#64896=CARTESIAN_POINT('Ctrl Pts',(-2.35523429540729,-4.59944840035779,
42.0232688578885));
#64897=CARTESIAN_POINT('Ctrl Pts',(2.58669254300161,-4.47337410259821,42.1820296201345));
#64898=CARTESIAN_POINT('Ctrl Pts',(5.16119935450289,-0.253131185149624,
42.3407903823802));
#64899=CARTESIAN_POINT('Ctrl Pts',(3.01201886587614,4.19878512494061,42.4995511446263));
#64900=CARTESIAN_POINT('Ctrl Pts',(-1.89385329211466,4.80784503512363,42.6583119068721));
#64901=CARTESIAN_POINT('Ctrl Pts',(-4.21883224032928,2.02948215439444,42.774658155965));
#64902=CARTESIAN_POINT('Ctrl Pts',(-4.37616957413132,0.292106279171763,
42.838084150976));
#64903=CARTESIAN_POINT('Ctrl Pts',(-4.37352103895722,0.00385464862035015,
42.848589891905));
#64904=CARTESIAN_POINT('Origin',(0.,0.,24.1514101080949));
#64905=CARTESIAN_POINT('',(-4.36973282931957,0.00384403733829788,40.651410108095));
#64906=CARTESIAN_POINT('',(-4.36602112377814,-0.00227682230535847,40.848589891905));
#64907=CARTESIAN_POINT('',(-4.372,3.82579154166093E-12,24.1514101080949));
#64908=CARTESIAN_POINT('Ctrl Pts',(-4.36973282931958,0.00384403733829777,
40.651410108095));
#64909=CARTESIAN_POINT('Ctrl Pts',(-4.36094828703741,-1.03504959539527,
40.6891903683526));
#64910=CARTESIAN_POINT('Ctrl Pts',(-3.47031004267523,-3.54269738683393,
40.7798908826921));
#64911=CARTESIAN_POINT('Ctrl Pts',(0.715283237582617,-5.11765799033974,
40.9235116511136));
#64912=CARTESIAN_POINT('Ctrl Pts',(4.6874579011302,-2.17480846080452,41.0822724133595));
#64913=CARTESIAN_POINT('Ctrl Pts',(4.36952791329752,2.75849220244841,41.2410331756054));
#64914=CARTESIAN_POINT('Ctrl Pts',(0.052472510246957,5.16713654277911,41.3997939378513));
#64915=CARTESIAN_POINT('Ctrl Pts',(-3.70859131189293,3.16775466245737,41.5365862486812));
#64916=CARTESIAN_POINT('Ctrl Pts',(-4.36224856298441,0.851164468294318,
41.620458305429));
#64917=CARTESIAN_POINT('Ctrl Pts',(-4.3656795540281,-0.00194869704108112,
41.651410108095));
#64918=CARTESIAN_POINT('Ctrl Pts',(-4.36602112377814,-0.00227682230535861,
40.848589891905));
#64919=CARTESIAN_POINT('Ctrl Pts',(-4.36876880712171,-0.584227201261346,
40.8697077686591));
#64920=CARTESIAN_POINT('Ctrl Pts',(-3.98963601281,-2.62107929020566,40.9437458994952));
#64921=CARTESIAN_POINT('Ctrl Pts',(-0.90075771530386,-5.08828946819429,
41.0707042844132));
#64922=CARTESIAN_POINT('Ctrl Pts',(3.78626858625262,-3.51656428443629,41.2294650466591));
#64923=CARTESIAN_POINT('Ctrl Pts',(5.00798622459088,1.27362794729248,41.3882258089049));
#64924=CARTESIAN_POINT('Ctrl Pts',(1.64624189925253,4.89815697818699,41.5469865711509));
#64925=CARTESIAN_POINT('Ctrl Pts',(-3.0594815075565,4.0684328488748,41.7004412654842));
#64926=CARTESIAN_POINT('Ctrl Pts',(-4.36854383389695,1.30092803749072,41.8009757057356));
#64927=CARTESIAN_POINT('Ctrl Pts',(-4.37739485101806,-0.00248321819134518,
41.8485898919051));
#64928=CARTESIAN_POINT('Origin',(0.,0.,24.1514101080949));
#64929=CARTESIAN_POINT('',(-4.37914188721017,-0.000342719191574727,39.651410108095));
#64930=CARTESIAN_POINT('',(-4.36909141260198,0.00371732487008336,39.848589891905));
#64931=CARTESIAN_POINT('',(-4.372,3.82579154166093E-12,24.1514101080949));
#64932=CARTESIAN_POINT('Ctrl Pts',(-4.37914188721017,-0.000342719191574457,
39.651410108095));
#64933=CARTESIAN_POINT('Ctrl Pts',(-4.37916257714185,-0.0187137896541573,
39.6520819231122));
#64934=CARTESIAN_POINT('Ctrl Pts',(-4.37073789868075,-1.48419245149001,
39.7056739922113));
#64935=CARTESIAN_POINT('Ctrl Pts',(-2.74752162183386,-4.3764344338297,39.8121863153924));
#64936=CARTESIAN_POINT('Ctrl Pts',(2.18656111288008,-4.68198717594309,39.9709470776383));
#64937=CARTESIAN_POINT('Ctrl Pts',(5.11943632770732,-0.702442241472902,
40.1297078398842));
#64938=CARTESIAN_POINT('Ctrl Pts',(3.36684704019806,3.9199992887709,40.2884686021301));
#64939=CARTESIAN_POINT('Ctrl Pts',(-1.46718350018236,4.95473773199425,40.4472293643759));
#64940=CARTESIAN_POINT('Ctrl Pts',(-4.12759825135317,2.28764036559584,40.5682098663642));
#64941=CARTESIAN_POINT('Ctrl Pts',(-4.37325313105903,0.420168410874277,
40.6362701142706));
#64942=CARTESIAN_POINT('Ctrl Pts',(-4.36973282931958,0.00384403733829777,
40.651410108095));
#64943=CARTESIAN_POINT('Ctrl Pts',(-4.36909141260198,0.0037173248700835,
39.848589891905));
#64944=CARTESIAN_POINT('Ctrl Pts',(-4.36087746473157,-1.01216450930882,
39.8855195775007));
#64945=CARTESIAN_POINT('Ctrl Pts',(-3.50202565789313,-3.49632888214117,
39.9753695171783));
#64946=CARTESIAN_POINT('Ctrl Pts',(0.6331436514814,-5.12846792818335,40.1181397109379));
#64947=CARTESIAN_POINT('Ctrl Pts',(4.65198839971611,-2.2496795555641,40.2769004731838));
#64948=CARTESIAN_POINT('Ctrl Pts',(4.41319126769477,2.68808426366416,40.4356612354296));
#64949=CARTESIAN_POINT('Ctrl Pts',(0.135306684796697,5.16563125618407,40.5944219976755));
#64950=CARTESIAN_POINT('Ctrl Pts',(-3.68091103301737,3.21474907678104,40.7320648831673));
#64951=CARTESIAN_POINT('Ctrl Pts',(-4.36188326164895,0.874108893605594,
40.8167875145772));
#64952=CARTESIAN_POINT('Ctrl Pts',(-4.36602112377814,-0.00227682230535861,
40.848589891905));
#64953=CARTESIAN_POINT('Origin',(0.,0.,24.1514101080949));
#64954=CARTESIAN_POINT('',(-4.36873305544013,-0.00362749675167218,38.651410108095));
#64955=CARTESIAN_POINT('',(-4.37917310725098,9.13219796030052E-5,38.848589891905));
#64956=CARTESIAN_POINT('',(-4.372,3.82579154166093E-12,24.1514101080949));
#64957=CARTESIAN_POINT('Ctrl Pts',(-4.36873305544013,-0.00362749675167234,
38.651410108095));
#64958=CARTESIAN_POINT('Ctrl Pts',(-4.37228988643661,-0.457161961038693,
38.6678937319537));
#64959=CARTESIAN_POINT('Ctrl Pts',(-4.0986296928328,-2.36257101965516,38.7372976098944));
#64960=CARTESIAN_POINT('Ctrl Pts',(-1.34123858177823,-4.99030384674165,
38.8596217419171));
#64961=CARTESIAN_POINT('Ctrl Pts',(3.46503780867414,-3.83347967263602,39.0183825041629));
#64962=CARTESIAN_POINT('Ctrl Pts',(5.10000575566994,0.831862193027325,39.1771432664089));
#64963=CARTESIAN_POINT('Ctrl Pts',(2.06729265337245,4.73585837007054,39.3359040286547));
#64964=CARTESIAN_POINT('Ctrl Pts',(-2.83663011433148,4.30727362250648,39.4939929758834));
#64965=CARTESIAN_POINT('Ctrl Pts',(-4.37753278856417,1.42841330898948,39.5991616690302));
#64966=CARTESIAN_POINT('Ctrl Pts',(-4.37914188721017,-0.000342719191574457,
39.651410108095));
#64967=CARTESIAN_POINT('Ctrl Pts',(-4.37917310725098,9.13219796029981E-5,
38.848589891905));
#64968=CARTESIAN_POINT('Ctrl Pts',(-4.37872965626048,-1.44211984317019,
38.9013313863422));
#64969=CARTESIAN_POINT('Ctrl Pts',(-2.81178331229755,-4.33225607926283,
39.0069931348614));
#64970=CARTESIAN_POINT('Ctrl Pts',(2.11121724282438,-4.71644102342194,39.1655751374625));
#64971=CARTESIAN_POINT('Ctrl Pts',(5.10751668218689,-0.784428145210908,
39.3243358997084));
#64972=CARTESIAN_POINT('Ctrl Pts',(3.42926084288352,3.86551733216684,39.4830966619543));
#64973=CARTESIAN_POINT('Ctrl Pts',(-1.38755926796319,4.97762327338117,39.6418574242002));
#64974=CARTESIAN_POINT('Ctrl Pts',(-4.1093944849834,2.33507192947434,39.7636885008504));
#64975=CARTESIAN_POINT('Ctrl Pts',(-4.37264805528242,0.443594561337992,
39.8325993234187));
#64976=CARTESIAN_POINT('Ctrl Pts',(-4.36909141260198,0.0037173248700835,
39.848589891905));
#64977=CARTESIAN_POINT('Origin',(0.,0.,24.1514101080949));
#64978=CARTESIAN_POINT('',(-4.36624352627694,0.00245771687439172,37.651410108095));
#64979=CARTESIAN_POINT('',(-4.36935764006,-0.00377501215838794,37.848589891905));
#64980=CARTESIAN_POINT('',(-4.372,3.82579154166093E-12,24.1514101080949));
#64981=CARTESIAN_POINT('Ctrl Pts',(-4.36624352627694,0.00245771687439181,
37.651410108095));
#64982=CARTESIAN_POINT('Ctrl Pts',(-4.36169382655995,-0.887401680305794,
37.6837055407953));
#64983=CARTESIAN_POINT('Ctrl Pts',(-3.66460952904662,-3.24195865307006,
37.7689212275775));
#64984=CARTESIAN_POINT('Ctrl Pts',(0.183308877707052,-5.16415058566349,
37.9070571684418));
#64985=CARTESIAN_POINT('Ctrl Pts',(4.43798296793759,-2.64695307709652,38.0658179306876));
#64986=CARTESIAN_POINT('Ctrl Pts',(4.63087948595682,2.29281673986369,38.2245786929335));
#64987=CARTESIAN_POINT('Ctrl Pts',(0.585453646372677,5.13413064150142,38.3833394551794));
#64988=CARTESIAN_POINT('Ctrl Pts',(-3.52014057613125,3.46939996827985,38.5256165935665));
#64989=CARTESIAN_POINT('Ctrl Pts',(-4.36087077121817,0.99889887186349,38.6149734778717));
#64990=CARTESIAN_POINT('Ctrl Pts',(-4.36873305544013,-0.00362749675167234,
38.651410108095));
#64991=CARTESIAN_POINT('Ctrl Pts',(-4.36935764006,-0.00377501215838787,
37.848589891905));
#64992=CARTESIAN_POINT('Ctrl Pts',(-4.37290446571934,-0.43375111631892,
37.8642229411018));
#64993=CARTESIAN_POINT('Ctrl Pts',(-4.11710236903147,-2.31513392579321,
37.9327762443806));
#64994=CARTESIAN_POINT('Ctrl Pts',(-1.42107210669624,-4.96815944202542,
38.0542498017413));
#64995=CARTESIAN_POINT('Ctrl Pts',(3.40313314014881,-3.88853944357485,38.2130105639872));
#64996=CARTESIAN_POINT('Ctrl Pts',(5.11268698707437,0.749990630619295,38.3717713262331));
#64997=CARTESIAN_POINT('Ctrl Pts',(2.14295353437204,4.70210637090854,38.5305320884789));
#64998=CARTESIAN_POINT('Ctrl Pts',(-2.78807645035559,4.35071073283309,38.6892928507248));
#64999=CARTESIAN_POINT('Ctrl Pts',(-4.37695363416618,1.45696557727882,38.7953121185335));
#65000=CARTESIAN_POINT('Ctrl Pts',(-4.37917461026378,0.0049794875180062,
38.8484111322603));
#65001=CARTESIAN_POINT('Ctrl Pts',(-4.37917310725098,9.13219796029981E-5,
38.848589891905));
#65002=CARTESIAN_POINT('Origin',(0.,0.,24.1514101080949));
#65003=CARTESIAN_POINT('',(-4.37768323182342,0.00228667983145002,36.651410108095));
#65004=CARTESIAN_POINT('',(-4.36587095680509,0.00214125659340675,36.848589891905));
#65005=CARTESIAN_POINT('',(-4.372,3.82579154166093E-12,24.1514101080949));
#65006=CARTESIAN_POINT('Ctrl Pts',(-4.37768323182342,0.00228667983144982,
36.651410108095));
#65007=CARTESIAN_POINT('Ctrl Pts',(-4.36931436006514,-1.31439298482965,
36.6995173496368));
#65008=CARTESIAN_POINT('Ctrl Pts',(-3.03668215072675,-4.09416581339981,
36.8005448452606));
#65009=CARTESIAN_POINT('Ctrl Pts',(1.69169298020808,-4.88264562268956,36.9544925949664));
#65010=CARTESIAN_POINT('Ctrl Pts',(5.01960663803976,-1.22702999775959,37.1132533572123));
#65011=CARTESIAN_POINT('Ctrl Pts',(3.75342297485632,3.55160096123927,37.2720141194582));
#65012=CARTESIAN_POINT('Ctrl Pts',(-0.94800804471325,5.07969823544803,37.430774881704));
#65013=CARTESIAN_POINT('Ctrl Pts',(-4.00191688963235,2.59358013793749,37.5572402112497));
#65014=CARTESIAN_POINT('Ctrl Pts',(-4.36914909948521,0.570748326013101,
37.6307852867133));
#65015=CARTESIAN_POINT('Ctrl Pts',(-4.36624352627694,0.00245771687439181,
37.651410108095));
#65016=CARTESIAN_POINT('Ctrl Pts',(-4.36587095680509,0.00214125659340626,
36.848589891905));
#65017=CARTESIAN_POINT('Ctrl Pts',(-4.36203103509102,-0.864466812036311,
36.8800347499434));
#65018=CARTESIAN_POINT('Ctrl Pts',(-3.6926137083843,-3.19500429871341,36.9643998620637));
#65019=CARTESIAN_POINT('Ctrl Pts',(0.100492274349119,-5.16642579319712,
37.101685228266));
#65020=CARTESIAN_POINT('Ctrl Pts',(4.39497597774354,-2.71776384714963,37.2604459905118));
#65021=CARTESIAN_POINT('Ctrl Pts',(4.66704342001788,2.21827858698683,37.4192067527577));
#65022=CARTESIAN_POINT('Ctrl Pts',(0.66769016759438,5.12408470011126,37.5779675150036));
#65023=CARTESIAN_POINT('Ctrl Pts',(-3.48876670478196,3.51583248140767,37.7210952280527));
#65024=CARTESIAN_POINT('Ctrl Pts',(-4.36089792030941,1.02178352666142,37.8113026870198));
#65025=CARTESIAN_POINT('Ctrl Pts',(-4.36935764006,-0.00377501215838787,
37.848589891905));
#65026=CARTESIAN_POINT('Origin',(0.,0.,24.1514101080949));
#65027=CARTESIAN_POINT('',(-4.37311107145795,-0.00391014173522758,35.651410108095));
#65028=CARTESIAN_POINT('',(-4.3771739373938,0.00261949572194539,35.848589891905));
#65029=CARTESIAN_POINT('',(-4.372,3.82579154166093E-12,24.1514101080949));
#65030=CARTESIAN_POINT('Ctrl Pts',(-4.37311107145795,-0.00391014173522778,
35.651410108095));
#65031=CARTESIAN_POINT('Ctrl Pts',(-4.3758959220056,-0.305762745961795,
35.6624089043964));
#65032=CARTESIAN_POINT('Ctrl Pts',(-4.20975035875682,-2.05692106559916,
35.7263279547798));
#65033=CARTESIAN_POINT('Ctrl Pts',(-1.84908860800444,-4.8252383087059,35.8431672592452));
#65034=CARTESIAN_POINT('Ctrl Pts',(3.05091116183891,-4.17061080641931,36.0019280214911));
#65035=CARTESIAN_POINT('Ctrl Pts',(5.15862384507246,0.301087098868051,36.1606887837369));
#65036=CARTESIAN_POINT('Ctrl Pts',(2.54500641307862,4.49722089444621,36.3194495459828));
#65037=CARTESIAN_POINT('Ctrl Pts',(-2.39787862639785,4.5773607580263,36.4782103082287));
#65038=CARTESIAN_POINT('Ctrl Pts',(-4.31337783157312,1.71331867151843,36.5888638289328));
#65039=CARTESIAN_POINT('Ctrl Pts',(-4.37852051709334,0.134017278681583,
36.6465970955549));
#65040=CARTESIAN_POINT('Ctrl Pts',(-4.37768323182342,0.00228667983144982,
36.651410108095));
#65041=CARTESIAN_POINT('Ctrl Pts',(-4.3771739373938,0.00261949572194524,
35.848589891905));
#65042=CARTESIAN_POINT('Ctrl Pts',(-4.36801132265503,-1.29117660831409,
35.8958465587849));
#65043=CARTESIAN_POINT('Ctrl Pts',(-3.07587918570516,-4.04972946385307,
35.9960234797468));
#65044=CARTESIAN_POINT('Ctrl Pts',(1.61319569609569,-4.90913982484862,36.1491206547906));
#65045=CARTESIAN_POINT('Ctrl Pts',(4.99928949022287,-1.30734798992603,36.3078814170365));
#65046=CARTESIAN_POINT('Ctrl Pts',(3.80988083761225,3.49096865884117,36.4666421792824));
#65047=CARTESIAN_POINT('Ctrl Pts',(-0.866447131906533,5.09424415801081,
36.6254029415283));
#65048=CARTESIAN_POINT('Ctrl Pts',(-3.9806269029927,2.64101706972627,36.7527188457358));
#65049=CARTESIAN_POINT('Ctrl Pts',(-4.36849344724489,0.59399482660225,36.8271144958614));
#65050=CARTESIAN_POINT('Ctrl Pts',(-4.36587095680509,0.00214125659340626,
36.848589891905));
#65051=CARTESIAN_POINT('Origin',(0.,0.,24.1514101080949));
#65052=CARTESIAN_POINT('',(-4.36484181559087,0.000158569877717519,34.651410108095));
#65053=CARTESIAN_POINT('',(-4.37381658707025,-0.00380592486605935,34.848589891905));
#65054=CARTESIAN_POINT('',(-4.372,3.82579154166093E-12,24.1514101080949));
#65055=CARTESIAN_POINT('Ctrl Pts',(-4.36484181559087,0.000158569877717965,
34.651410108095));
#65056=CARTESIAN_POINT('Ctrl Pts',(-4.36460260997581,-0.739166555623858,
34.6782207132379));
#65057=CARTESIAN_POINT('Ctrl Pts',(-3.83552704168218,-2.93813387262851,
34.7579515724629));
#65058=CARTESIAN_POINT('Ctrl Pts',(-0.350623086089188,-5.15549385292585,
34.8906026857698));
#65059=CARTESIAN_POINT('Ctrl Pts',(4.14111364246891,-3.09083018236409,35.0493634480157));
#65060=CARTESIAN_POINT('Ctrl Pts',(4.84277667347619,1.80265568173448,35.2081242102616));
#65061=CARTESIAN_POINT('Ctrl Pts',(1.11218256837853,5.0462960030749,35.3668849725075));
#65062=CARTESIAN_POINT('Ctrl Pts',(-3.30734354987895,3.76666274637145,35.5146469384519));
#65063=CARTESIAN_POINT('Ctrl Pts',(-4.36249672862818,1.14658859078299,35.6094886503144));
#65064=CARTESIAN_POINT('Ctrl Pts',(-4.37311107145795,-0.00391014173522778,
35.651410108095));
#65065=CARTESIAN_POINT('Ctrl Pts',(-4.37381658707025,-0.00380592486605963,
34.848589891905));
#65066=CARTESIAN_POINT('Ctrl Pts',(-4.37636167316891,-0.282199643018631,
34.8587381135445));
#65067=CARTESIAN_POINT('Ctrl Pts',(-4.22532647145104,-2.00959079533273,
34.921806589266));
#65068=CARTESIAN_POINT('Ctrl Pts',(-1.92621049372714,-4.7949731289833,35.0377953190694));
#65069=CARTESIAN_POINT('Ctrl Pts',(2.98365473640471,-4.21898786295316,35.1965560813153));
#65070=CARTESIAN_POINT('Ctrl Pts',(5.16278801485838,0.21834396591395,35.3553168435612));
#65071=CARTESIAN_POINT('Ctrl Pts',(2.61678000270041,4.45584072777334,35.514077605807));
#65072=CARTESIAN_POINT('Ctrl Pts',(-2.32418499851494,4.61521595014736,35.672838368053));
#65073=CARTESIAN_POINT('Ctrl Pts',(-4.30043031041834,1.76047520998047,35.7843424634189));
#65074=CARTESIAN_POINT('Ctrl Pts',(-4.37827205266511,0.157677555053939,
35.842926304703));
#65075=CARTESIAN_POINT('Ctrl Pts',(-4.3771739373938,0.00261949572194524,
35.848589891905));
#65076=CARTESIAN_POINT('Origin',(0.,0.,24.1514101080949));
#65077=CARTESIAN_POINT('',(-4.37369305382679,0.00382718076316987,33.651410108095));
#65078=CARTESIAN_POINT('',(-4.36484727915486,-0.000226203520788115,33.848589891905));
#65079=CARTESIAN_POINT('',(-4.372,3.82579154166093E-12,24.1514101080949));
#65080=CARTESIAN_POINT('Ctrl Pts',(-4.37369305382679,0.00382718076316957,
33.651410108095));
#65081=CARTESIAN_POINT('Ctrl Pts',(-4.36297801900768,-1.16550827733193,
33.6940325220795));
#65082=CARTESIAN_POINT('Ctrl Pts',(-3.27833228748252,-3.80423885928109,
33.789575190146));
#65083=CARTESIAN_POINT('Ctrl Pts',(1.17875881138994,-5.0311610072254,33.9380381122944));
#65084=CARTESIAN_POINT('Ctrl Pts',(4.86617124330449,-1.73851397661661,34.0967988745404));
#65085=CARTESIAN_POINT('Ctrl Pts',(4.09991511421076,3.14527414899259,34.2555596367862));
#65086=CARTESIAN_POINT('Ctrl Pts',(-0.418708560946466,5.15041129979394,
34.4143203990322));
#65087=CARTESIAN_POINT('Ctrl Pts',(-3.85575329743435,2.89916044399897,34.5462705561351));
#65088=CARTESIAN_POINT('Ctrl Pts',(-4.36507476723817,0.720154234863851,
34.625300459156));
#65089=CARTESIAN_POINT('Ctrl Pts',(-4.36484181559087,0.000158569877717965,
34.651410108095));
#65090=CARTESIAN_POINT('Ctrl Pts',(-4.36484727915486,-0.000226203520787838,
33.848589891905));
#65091=CARTESIAN_POINT('Ctrl Pts',(-4.36517770844991,-0.716093813355663,
33.8745499223861));
#65092=CARTESIAN_POINT('Ctrl Pts',(-3.86002428520416,-2.89083849180258,
33.9534302069491));
#65093=CARTESIAN_POINT('Ctrl Pts',(-0.433232286323001,-5.1492100326073,
34.085230745594));
#65094=CARTESIAN_POINT('Ctrl Pts',(4.0910284465022,-3.15682442079478,34.24399150784));
#65095=CARTESIAN_POINT('Ctrl Pts',(4.87105498299758,1.72478332738662,34.4027522700858));
#65096=CARTESIAN_POINT('Ctrl Pts',(1.1929432107418,5.02781669015105,34.5615130323318));
#65097=CARTESIAN_POINT('Ctrl Pts',(-3.27208568972255,3.81224566198089,34.7101255729381));
#65098=CARTESIAN_POINT('Ctrl Pts',(-4.36308973176021,1.16954893154173,34.8058178594626));
#65099=CARTESIAN_POINT('Ctrl Pts',(-4.37381658707025,-0.00380592486605963,
34.848589891905));
#65100=CARTESIAN_POINT('Origin',(0.,0.,24.1514101080949));
#65101=CARTESIAN_POINT('',(-4.37726747931578,-0.00256312102853162,32.651410108095));
#65102=CARTESIAN_POINT('',(-4.37298639645094,0.00392429018828133,32.848589891905));
#65103=CARTESIAN_POINT('',(-4.372,3.82579154166093E-12,24.1514101080949));
#65104=CARTESIAN_POINT('Ctrl Pts',(-4.37726747931578,-0.0025631210285324,
32.651410108095));
#65105=CARTESIAN_POINT('Ctrl Pts',(-4.37831848753371,-0.153516427525766,
32.6569240768391));
#65106=CARTESIAN_POINT('Ctrl Pts',(-4.30273715326605,-1.7521779604483,32.7153582996652));
#65107=CARTESIAN_POINT('Ctrl Pts',(-2.33719172860392,-4.60864277632799,
32.8267127765732));
#65108=CARTESIAN_POINT('Ctrl Pts',(2.60420302889879,-4.4632028858578,32.9854735388192));
#65109=CARTESIAN_POINT('Ctrl Pts',(5.16215162793603,-0.232903383943239,
33.144234301065));
#65110=CARTESIAN_POINT('Ctrl Pts',(2.99554137711165,4.21055640908263,33.302995063311));
#65111=CARTESIAN_POINT('Ctrl Pts',(-1.91267984204806,4.80038636339596,33.4617558255568));
#65112=CARTESIAN_POINT('Ctrl Pts',(-4.22261792613804,2.01791460332865,33.5778941738182));
#65113=CARTESIAN_POINT('Ctrl Pts',(-4.37628187282812,0.286345894322504,
33.6411122679975));
#65114=CARTESIAN_POINT('Ctrl Pts',(-4.37369305382679,0.00382718076316957,
33.651410108095));
#65115=CARTESIAN_POINT('Ctrl Pts',(-4.37298639645094,0.00392429018828126,
32.848589891905));
#65116=CARTESIAN_POINT('Ctrl Pts',(-4.36240284050621,-1.14255230782506,
32.8903617312276));
#65117=CARTESIAN_POINT('Ctrl Pts',(-3.31348194711132,-3.75862865123049,
32.9850538246322));
#65118=CARTESIAN_POINT('Ctrl Pts',(1.09794640645064,-5.04941262548215,33.1326661721187));
#65119=CARTESIAN_POINT('Ctrl Pts',(4.83767356537879,-1.81630632015957,33.2914269343646));
#65120=CARTESIAN_POINT('Ctrl Pts',(4.14981410860918,3.07913900917197,33.4501876966104));
#65121=CARTESIAN_POINT('Ctrl Pts',(-0.336081978081961,5.15646226378366,
33.6089484588564));
#65122=CARTESIAN_POINT('Ctrl Pts',(-3.83116330074657,2.94644944182165,33.7417491906212));
#65123=CARTESIAN_POINT('Ctrl Pts',(-4.36450411901545,0.743222493270702,
33.8216296683041));
#65124=CARTESIAN_POINT('Ctrl Pts',(-4.36484727915486,-0.000226203520787838,
33.848589891905));
#65125=CARTESIAN_POINT('Origin',(0.,0.,24.1514101080949));
#65126=CARTESIAN_POINT('',(-4.36593258301536,-0.00219842154078257,31.651410108095));
#65127=CARTESIAN_POINT('',(-4.37776688532802,-0.00222515354369623,31.848589891905));
#65128=CARTESIAN_POINT('',(-4.372,3.82579154166093E-12,24.1514101080949));
#65129=CARTESIAN_POINT('Ctrl Pts',(-4.36593258301536,-0.00219842154078276,
31.651410108095));
#65130=CARTESIAN_POINT('Ctrl Pts',(-4.36860855649085,-0.589907775928666,
31.6727358856806));
#65131=CARTESIAN_POINT('Ctrl Pts',(-3.98440775127391,-2.63267349583233,
31.7469819173483));
#65132=CARTESIAN_POINT('Ctrl Pts',(-0.880810653343035,-5.09178023966167,
31.8741482030979));
#65133=CARTESIAN_POINT('Ctrl Pts',(3.80002027066033,-3.5016994957634,32.0329089653438));
#65134=CARTESIAN_POINT('Ctrl Pts',(5.00295656982363,1.29324358746212,32.1916697275897));
#65135=CARTESIAN_POINT('Ctrl Pts',(1.62703419898677,4.90457063680218,32.3504304898356));
#65136=CARTESIAN_POINT('Ctrl Pts',(-3.06903058869073,4.05756105615878,32.5036772833373));
#65137=CARTESIAN_POINT('Ctrl Pts',(-4.36823144777778,1.29525626325957,32.6040038227571));
#65138=CARTESIAN_POINT('Ctrl Pts',(-4.37726747931578,-0.0025631210285324,
32.651410108095));
#65139=CARTESIAN_POINT('Ctrl Pts',(-4.37776688532802,-0.00222515354369674,
31.848589891905));
#65140=CARTESIAN_POINT('Ctrl Pts',(-4.37856029699079,-0.129854311945594,
31.8532532859872));
#65141=CARTESIAN_POINT('Ctrl Pts',(-4.31561362407578,-1.70502699061033,
31.9108369341514));
#65142=CARTESIAN_POINT('Ctrl Pts',(-2.41077837014428,-4.57058003144683,
32.0213408363975));
#65143=CARTESIAN_POINT('Ctrl Pts',(2.53231309568674,-4.50438059662262,32.1801015986434));
#65144=CARTESIAN_POINT('Ctrl Pts',(5.15775426583447,-0.31563445167244,32.3388623608893));
#65145=CARTESIAN_POINT('Ctrl Pts',(3.06266118623515,4.16198998462816,32.4976231231351));
#65146=CARTESIAN_POINT('Ctrl Pts',(-1.83547296121064,4.83043405735769,32.6563838853811));
#65147=CARTESIAN_POINT('Ctrl Pts',(-4.20696559908301,2.06524898522119,32.7733728083043));
#65148=CARTESIAN_POINT('Ctrl Pts',(-4.37581102359723,0.309905468748449,
32.8374414771457));
#65149=CARTESIAN_POINT('Ctrl Pts',(-4.37298639645094,0.00392429018828126,
32.848589891905));
#65150=CARTESIAN_POINT('Origin',(0.,0.,24.1514101080949));
#65151=CARTESIAN_POINT('',(-4.36924553642194,0.00375164274966603,30.651410108095));
#65152=CARTESIAN_POINT('',(-4.36631454878401,-0.00251114173366096,30.848589891905));
#65153=CARTESIAN_POINT('',(-4.372,3.82579154166093E-12,24.1514101080949));
#65154=CARTESIAN_POINT('Ctrl Pts',(-4.36924553642194,0.00375164274966585,
30.651410108095));
#65155=CARTESIAN_POINT('Ctrl Pts',(-4.36088767272676,-1.01775802631581,
30.6885476945222));
#65156=CARTESIAN_POINT('Ctrl Pts',(-3.49432807348169,-3.50767273053874,
30.7786055350314));
#65157=CARTESIAN_POINT('Ctrl Pts',(0.653236365857992,-5.12594729451212,
30.9215836296226));
#65158=CARTESIAN_POINT('Ctrl Pts',(4.6607687206244,-2.23143190555148,31.0803443918685));
#65159=CARTESIAN_POINT('Ctrl Pts',(4.4026231771807,2.70535812338375,31.2391051541143));
#65160=CARTESIAN_POINT('Ctrl Pts',(0.115062422136807,5.16612176153803,31.3978659163603));
#65161=CARTESIAN_POINT('Ctrl Pts',(-3.68772820349694,3.20326873769824,31.5353009010205));
#65162=CARTESIAN_POINT('Ctrl Pts',(-4.36196808602404,0.868502274330174,
31.6198156315987));
#65163=CARTESIAN_POINT('Ctrl Pts',(-4.36593258301536,-0.00219842154078276,
31.651410108095));
#65164=CARTESIAN_POINT('Ctrl Pts',(-4.36631454878401,-0.0025111417336611,
30.848589891905));
#65165=CARTESIAN_POINT('Ctrl Pts',(-4.36926463444175,-0.566656242129838,
30.8690650948288));
#65166=CARTESIAN_POINT('Ctrl Pts',(-4.00561083840711,-2.58523495481153,
30.9424605518345));
#65167=CARTESIAN_POINT('Ctrl Pts',(-0.962330244988123,-5.07700449806455,
31.0687762629221));
#65168=CARTESIAN_POINT('Ctrl Pts',(3.74339174195905,-3.56217243267071,31.2275370251681));
#65169=CARTESIAN_POINT('Ctrl Pts',(5.02304726326813,1.21286865108392,31.3862977874139));
#65170=CARTESIAN_POINT('Ctrl Pts',(1.70545649826175,4.87785529780762,31.5450585496599));
#65171=CARTESIAN_POINT('Ctrl Pts',(-3.02972114369421,4.10196041210765,31.6991559178235));
#65172=CARTESIAN_POINT('Ctrl Pts',(-4.36955665156738,1.31848296597982,31.8003330319052));
#65173=CARTESIAN_POINT('Ctrl Pts',(-4.37776688532802,-0.00222515354369674,
31.848589891905));
#65174=CARTESIAN_POINT('Origin',(0.,0.,24.1514101080949));
#65175=CARTESIAN_POINT('',(-4.37917542201394,-1.48878467067329E-5,29.651410108095));
#65176=CARTESIAN_POINT('',(-4.36862654983539,0.00359793095617206,29.848589891905));
#65177=CARTESIAN_POINT('',(-4.372,3.82579154166093E-12,24.1514101080949));
#65178=CARTESIAN_POINT('Ctrl Pts',(-4.3791753974872,-1.48877958181532E-5,
29.651410108095));
#65179=CARTESIAN_POINT('Ctrl Pts',(-4.37917543773958,-0.000811749618496727,
29.6514392492818));
#65180=CARTESIAN_POINT('Ctrl Pts',(-4.37881439934298,-1.44870578249893,
29.7043886445506));
#65181=CARTESIAN_POINT('Ctrl Pts',(-2.80033535833003,-4.34283033250174,
29.8102582939013));
#65182=CARTESIAN_POINT('Ctrl Pts',(2.12968392236957,-4.70813124181331,29.9690190561473));
#65183=CARTESIAN_POINT('Ctrl Pts',(5.11055143098187,-0.764406630547101,
30.1277798183931));
#65184=CARTESIAN_POINT('Ctrl Pts',(3.41408616315334,3.87892628001712,30.286540580639));
#65185=CARTESIAN_POINT('Ctrl Pts',(-1.4070550442568,4.97214737476293,30.4453013428849));
#65186=CARTESIAN_POINT('Ctrl Pts',(-4.11388660080008,2.32347755138503,30.5669245187036));
#65187=CARTESIAN_POINT('Ctrl Pts',(-4.37279744697119,0.437871066329566,
30.6356274404402));
#65188=CARTESIAN_POINT('Ctrl Pts',(-4.36924553642194,0.00375164274966585,
30.651410108095));
#65189=CARTESIAN_POINT('Ctrl Pts',(-4.36862654983539,0.0035979309561724,
29.848589891905));
#65190=CARTESIAN_POINT('Ctrl Pts',(-4.36087365922317,-0.994873321808196,
29.8848769036703));
#65191=CARTESIAN_POINT('Ctrl Pts',(-3.52559867611562,-3.46122138486278,
29.9740841695176));
#65192=CARTESIAN_POINT('Ctrl Pts',(0.570971856938151,-5.13576141485164,
30.1162116894468));
#65193=CARTESIAN_POINT('Ctrl Pts',(4.62439484690811,-2.30586783557282,30.2749724516927));
#65194=CARTESIAN_POINT('Ctrl Pts',(4.44543041863472,2.63442642081081,30.4337332139386));
#65195=CARTESIAN_POINT('Ctrl Pts',(0.1978722839815,5.16361314708889,30.5924939761844));
#65196=CARTESIAN_POINT('Ctrl Pts',(-3.65962554388572,3.25021066517935,30.7307795355066));
#65197=CARTESIAN_POINT('Ctrl Pts',(-4.361639836624,0.891434413344724,30.8161448407468));
#65198=CARTESIAN_POINT('Ctrl Pts',(-4.36631454878401,-0.0025111417336611,
30.848589891905));
#65199=CARTESIAN_POINT('Origin',(0.,0.,24.1514101080949));
#65200=CARTESIAN_POINT('',(-4.36920210772109,-0.00374225457618444,28.651410108095));
#65201=CARTESIAN_POINT('',(-4.379125585284,0.000418740495046069,28.848589891905));
#65202=CARTESIAN_POINT('',(-4.372,3.82579154166093E-12,24.1514101080949));
#65203=CARTESIAN_POINT('Ctrl Pts',(-4.36920210772109,-0.00374225457618473,
28.651410108095));
#65204=CARTESIAN_POINT('Ctrl Pts',(-4.37275566211042,-0.439475723050513,
28.6672510581234));
#65205=CARTESIAN_POINT('Ctrl Pts',(-4.11263026215736,-2.3267277008933,28.7360122622337));
#65206=CARTESIAN_POINT('Ctrl Pts',(-1.40159165779937,-4.9736902589037,28.857693720426));
#65207=CARTESIAN_POINT('Ctrl Pts',(3.41834539873403,-3.87517318393326,29.0164544826719));
#65208=CARTESIAN_POINT('Ctrl Pts',(5.10970861334159,0.770020576487015,29.1752152449178));
#65209=CARTESIAN_POINT('Ctrl Pts',(2.12451027984608,4.71046807932676,29.3339760071637));
#65210=CARTESIAN_POINT('Ctrl Pts',(-2.80419982800075,4.33981931003669,29.4927076282227));
#65211=CARTESIAN_POINT('Ctrl Pts',(-4.37910233962271,1.44628545901738,29.5985189951998));
#65212=CARTESIAN_POINT('Ctrl Pts',(-4.3791753974872,-1.48877958181532E-5,
29.651410108095));
#65213=CARTESIAN_POINT('Ctrl Pts',(-4.379125585284,0.000418740495045835,
28.848589891905));
#65214=CARTESIAN_POINT('Ctrl Pts',(-4.37717920749743,-1.42426027511931,
28.9006887125119));
#65215=CARTESIAN_POINT('Ctrl Pts',(-2.84412638479826,-4.2996753084771,29.0057077872007));
#65216=CARTESIAN_POINT('Ctrl Pts',(2.05392820456428,-4.74166985111631,29.1636471159715));
#65217=CARTESIAN_POINT('Ctrl Pts',(5.09763950196961,-0.846242130327758,
29.3224078782173));
#65218=CARTESIAN_POINT('Ctrl Pts',(3.47583539931961,3.82369225364773,29.4811686404633));
#65219=CARTESIAN_POINT('Ctrl Pts',(-1.32715942194175,4.9940666821606,29.6399294027091));
#65220=CARTESIAN_POINT('Ctrl Pts',(-4.09533214146315,2.37091623060187,29.7624031531897));
#65221=CARTESIAN_POINT('Ctrl Pts',(-4.37218032023241,0.461277235079317,
29.8319566495884));
#65222=CARTESIAN_POINT('Ctrl Pts',(-4.36862654983539,0.0035979309561724,
29.848589891905));
#65223=CARTESIAN_POINT('Origin',(0.,0.,24.1514101080949));
#65224=CARTESIAN_POINT('',(-4.36594998909341,0.00221597220681413,27.651410108095));
#65225=CARTESIAN_POINT('',(-4.36984836444492,-0.00386263586949487,27.848589891905));
#65226=CARTESIAN_POINT('',(-4.372,3.82579154166093E-12,24.1514101080949));
#65227=CARTESIAN_POINT('Ctrl Pts',(-4.36594998909341,0.00221597220681394,
27.651410108095));
#65228=CARTESIAN_POINT('Ctrl Pts',(-4.36193991209169,-0.870076739562532,
27.6830628669649));
#65229=CARTESIAN_POINT('Ctrl Pts',(-3.68583197785541,-3.20648009630763,
27.7676358799168));
#65230=CARTESIAN_POINT('Ctrl Pts',(0.12074539761077,-5.16599709979471,27.9051291469506));
#65231=CARTESIAN_POINT('Ctrl Pts',(4.40558866999103,-2.70051724468854,28.0638899091966));
#65232=CARTESIAN_POINT('Ctrl Pts',(4.65831652566081,2.23654953809766,28.2226506714425));
#65233=CARTESIAN_POINT('Ctrl Pts',(0.647603546994949,5.12666253671564,28.3814114336883));
#65234=CARTESIAN_POINT('Ctrl Pts',(-3.49648913171247,3.50449301705117,28.5243312459059));
#65235=CARTESIAN_POINT('Ctrl Pts',(-4.36088421495349,1.0161898665986,28.6143308040414));
#65236=CARTESIAN_POINT('Ctrl Pts',(-4.36920210772109,-0.00374225457618473,
28.651410108095));
#65237=CARTESIAN_POINT('Ctrl Pts',(-4.36984836444492,-0.00386263586949508,
27.848589891905));
#65238=CARTESIAN_POINT('Ctrl Pts',(-4.37335795381477,-0.41604489030568,
27.8635802672715));
#65239=CARTESIAN_POINT('Ctrl Pts',(-4.13075387899131,-2.27929715120676,
27.9314908967199));
#65240=CARTESIAN_POINT('Ctrl Pts',(-1.48115027726835,-4.95058115072351,
28.0523217802503));
#65241=CARTESIAN_POINT('Ctrl Pts',(3.35577787359124,-3.92947861571792,28.2110825424961));
#65242=CARTESIAN_POINT('Ctrl Pts',(5.12139735341277,0.688001195909337,28.369843304742));
#65243=CARTESIAN_POINT('Ctrl Pts',(2.1997566305386,4.67580212267651,28.5286040669879));
#65244=CARTESIAN_POINT('Ctrl Pts',(-2.7351680780718,4.38416569184913,28.6873648292338));
#65245=CARTESIAN_POINT('Ctrl Pts',(-4.36882639464741,1.49245678983841,28.7940267708728));
#65246=CARTESIAN_POINT('Ctrl Pts',(-4.37915627350017,0.0228814185571984,
28.8477684584299));
#65247=CARTESIAN_POINT('Ctrl Pts',(-4.379125585284,0.000418740495045835,
28.848589891905));
#65248=CARTESIAN_POINT('Origin',(0.,0.,24.1514101080949));
#65249=CARTESIAN_POINT('',(-4.37688026104952,0.00226901643694793,26.651410108095));
#65250=CARTESIAN_POINT('',(-4.36558297706963,0.00185075076461538,26.848589891905));
#65251=CARTESIAN_POINT('',(-4.372,3.82579154166093E-12,24.1514101080949));
#65252=CARTESIAN_POINT('Ctrl Pts',(-4.37688026104952,0.00226901643694839,
26.651410108095));
#65253=CARTESIAN_POINT('Ctrl Pts',(-4.36778028862692,-1.29719233300268,
26.6988746758065));
#65254=CARTESIAN_POINT('Ctrl Pts',(-3.06703503858937,-4.06017418671544,
26.7992594975999));
#65255=CARTESIAN_POINT('Ctrl Pts',(1.63279456941769,-4.90302026906412,26.9525645734753));
#65256=CARTESIAN_POINT('Ctrl Pts',(5.00417945325775,-1.28762125191842,27.1113253357213));
#65257=CARTESIAN_POINT('Ctrl Pts',(3.79627275763131,3.50580663842047,27.2700860979671));
#65258=CARTESIAN_POINT('Ctrl Pts',(-0.886457053099411,5.09084367591115,
27.428846860213));
#65259=CARTESIAN_POINT('Ctrl Pts',(-3.98586478860146,2.62941579049566,27.5559548635889));
#65260=CARTESIAN_POINT('Ctrl Pts',(-4.3686443606578,0.588309625125352,27.6301426128829));
#65261=CARTESIAN_POINT('Ctrl Pts',(-4.36594998909341,0.00221597220681394,
27.651410108095));
#65262=CARTESIAN_POINT('Ctrl Pts',(-4.36558297706963,0.00185075076461511,
26.848589891905));
#65263=CARTESIAN_POINT('Ctrl Pts',(-4.36229437398082,-0.847147845875526,
26.879392076113));
#65264=CARTESIAN_POINT('Ctrl Pts',(-3.7134735047561,-3.15941742864277,26.963114514403));
#65265=CARTESIAN_POINT('Ctrl Pts',(0.037946527963305,-5.16730646950401,
27.0997572067749));
#65266=CARTESIAN_POINT('Ctrl Pts',(4.36170657063856,-2.77078223288025,27.2585179690208));
#65267=CARTESIAN_POINT('Ctrl Pts',(4.69358555482947,2.16156853417802,27.4172787312667));
#65268=CARTESIAN_POINT('Ctrl Pts',(0.729706757950081,5.11562647870316,27.5760394935125));
#65269=CARTESIAN_POINT('Ctrl Pts',(-3.46466751885718,3.55083973542589,27.719809880392));
#65270=CARTESIAN_POINT('Ctrl Pts',(-4.36096811322469,1.03907475143884,27.8106600131895));
#65271=CARTESIAN_POINT('Ctrl Pts',(-4.36984836444492,-0.00386263586949508,
27.848589891905));
#65272=CARTESIAN_POINT('Ctrl Pts',(-1.91898364243938,3.92834389788497,25.6709103465619));
#65273=CARTESIAN_POINT('Ctrl Pts',(-2.57208606313318,3.60930541889036,25.6973704736029));
#65274=CARTESIAN_POINT('Ctrl Pts',(-3.70615701990389,2.63929385761509,25.7502907276849));
#65275=CARTESIAN_POINT('Ctrl Pts',(-4.81803798679934,-0.15958129715831,
25.8561312358487));
#65276=CARTESIAN_POINT('Ctrl Pts',(-3.30234769881301,-3.97407004593024,
25.9884318710537));
#65277=CARTESIAN_POINT('Ctrl Pts',(1.55593458522165,-4.93043777696371,26.1471926332996));
#65278=CARTESIAN_POINT('Ctrl Pts',(4.98187809541805,-1.36671674862893,26.3059533955455));
#65279=CARTESIAN_POINT('Ctrl Pts',(3.85252000415521,3.44398917781397,26.4647141577913));
#65280=CARTESIAN_POINT('Ctrl Pts',(-0.805001512196143,5.10466442465425,
26.6234749200372));
#65281=CARTESIAN_POINT('Ctrl Pts',(-4.72460311480109,2.09234479401288,26.7822356822831));
#65282=CARTESIAN_POINT('Ctrl Pts',(-4.32070810303542,-2.83440458431113,
26.940996444529));
#65283=CARTESIAN_POINT('Ctrl Pts',(0.037946527963305,-5.16730646950401,
27.0997572067749));
#65284=CARTESIAN_POINT('Ctrl Pts',(4.36170657063856,-2.77078223288025,27.2585179690208));
#65285=CARTESIAN_POINT('Ctrl Pts',(4.69358555482947,2.16156853417802,27.4172787312667));
#65286=CARTESIAN_POINT('Ctrl Pts',(0.729706757950081,5.11562647870316,27.5760394935125));
#65287=CARTESIAN_POINT('Ctrl Pts',(-3.90199850336257,3.38768554797952,27.7348002557585));
#65288=CARTESIAN_POINT('Ctrl Pts',(-4.96248778940575,-1.44075757294651,
27.8935610180043));
#65289=CARTESIAN_POINT('Ctrl Pts',(-1.48115027726835,-4.95058115072351,
28.0523217802503));
#65290=CARTESIAN_POINT('Ctrl Pts',(3.35577787359124,-3.92947861571792,28.2110825424961));
#65291=CARTESIAN_POINT('Ctrl Pts',(5.12139735341277,0.688001195909337,28.369843304742));
#65292=CARTESIAN_POINT('Ctrl Pts',(2.1997566305386,4.67580212267651,28.5286040669879));
#65293=CARTESIAN_POINT('Ctrl Pts',(-2.7351680780718,4.38416569184913,28.6873648292338));
#65294=CARTESIAN_POINT('Ctrl Pts',(-5.16678366281907,0.0800071286185968,
28.8461255914797));
#65295=CARTESIAN_POINT('Ctrl Pts',(-2.86960088841888,-4.29737651997417,
29.0048863537256));
#65296=CARTESIAN_POINT('Ctrl Pts',(2.05392820456428,-4.74166985111631,29.1636471159715));
#65297=CARTESIAN_POINT('Ctrl Pts',(5.09763950196961,-0.846242130327758,
29.3224078782173));
#65298=CARTESIAN_POINT('Ctrl Pts',(3.47583539931961,3.82369225364773,29.4811686404633));
#65299=CARTESIAN_POINT('Ctrl Pts',(-1.32715942194175,4.9940666821606,29.6399294027091));
#65300=CARTESIAN_POINT('Ctrl Pts',(-4.9154974066526,1.59371874196162,29.798690164955));
#65301=CARTESIAN_POINT('Ctrl Pts',(-4.00502201634919,-3.26524927403143,
29.9574509272009));
#65302=CARTESIAN_POINT('Ctrl Pts',(0.570971856938151,-5.13576141485164,
30.1162116894468));
#65303=CARTESIAN_POINT('Ctrl Pts',(4.62439484690811,-2.30586783557282,30.2749724516927));
#65304=CARTESIAN_POINT('Ctrl Pts',(4.44543041863472,2.63442642081081,30.4337332139386));
#65305=CARTESIAN_POINT('Ctrl Pts',(0.1978722839815,5.16361314708889,30.5924939761844));
#65306=CARTESIAN_POINT('Ctrl Pts',(-4.23078460916092,2.96690339662622,30.7512547384304));
#65307=CARTESIAN_POINT('Ctrl Pts',(-4.7872981969476,-1.94520696772118,30.9100155006763));
#65308=CARTESIAN_POINT('Ctrl Pts',(-0.962330244988123,-5.07700449806455,
31.0687762629221));
#65309=CARTESIAN_POINT('Ctrl Pts',(3.74339174195905,-3.56217243267071,31.2275370251681));
#65310=CARTESIAN_POINT('Ctrl Pts',(5.02304726326813,1.21286865108392,31.3862977874139));
#65311=CARTESIAN_POINT('Ctrl Pts',(1.70545649826175,4.87785529780762,31.5450585496599));
#65312=CARTESIAN_POINT('Ctrl Pts',(-3.17302014780288,4.07847977994959,31.7038193119056));
#65313=CARTESIAN_POINT('Ctrl Pts',(-5.14745183343486,-0.453645011306304,
31.8625800741516));
#65314=CARTESIAN_POINT('Ctrl Pts',(-2.41077837014428,-4.57058003144683,
32.0213408363975));
#65315=CARTESIAN_POINT('Ctrl Pts',(2.53231309568674,-4.50438059662262,32.1801015986434));
#65316=CARTESIAN_POINT('Ctrl Pts',(5.15775426583447,-0.31563445167244,32.3388623608893));
#65317=CARTESIAN_POINT('Ctrl Pts',(3.06266118623515,4.16198998462816,32.4976231231351));
#65318=CARTESIAN_POINT('Ctrl Pts',(-1.83547296121064,4.83043405735769,32.6563838853811));
#65319=CARTESIAN_POINT('Ctrl Pts',(-5.05372618930481,1.07791733326401,32.8151446476269));
#65320=CARTESIAN_POINT('Ctrl Pts',(-3.64665484087083,-3.66114225964655,
32.9739054098729));
#65321=CARTESIAN_POINT('Ctrl Pts',(1.09794640645064,-5.04941262548215,33.1326661721187));
#65322=CARTESIAN_POINT('Ctrl Pts',(4.83767356537879,-1.81630632015957,33.2914269343646));
#65323=CARTESIAN_POINT('Ctrl Pts',(4.14981410860918,3.07913900917197,33.4501876966104));
#65324=CARTESIAN_POINT('Ctrl Pts',(-0.336081978081961,5.15646226378366,
33.6089484588564));
#65325=CARTESIAN_POINT('Ctrl Pts',(-4.51438557267483,2.51443374838985,33.7677092211023));
#65326=CARTESIAN_POINT('Ctrl Pts',(-4.56098559745287,-2.42888133790924,
33.9264699833482));
#65327=CARTESIAN_POINT('Ctrl Pts',(-0.433232286323001,-5.1492100326073,
34.085230745594));
#65328=CARTESIAN_POINT('Ctrl Pts',(4.0910284465022,-3.15682442079478,34.24399150784));
#65329=CARTESIAN_POINT('Ctrl Pts',(4.87105498299758,1.72478332738662,34.4027522700858));
#65330=CARTESIAN_POINT('Ctrl Pts',(1.1929432107418,5.02781669015105,34.5615130323318));
#65331=CARTESIAN_POINT('Ctrl Pts',(-3.5769866269097,3.72923864142877,34.7202737945776));
#65332=CARTESIAN_POINT('Ctrl Pts',(-5.07314904313429,-0.982452523006609,
34.8790345568235));
#65333=CARTESIAN_POINT('Ctrl Pts',(-1.92621049372714,-4.7949731289833,35.0377953190694));
#65334=CARTESIAN_POINT('Ctrl Pts',(2.98365473640471,-4.21898786295316,35.1965560813153));
#65335=CARTESIAN_POINT('Ctrl Pts',(5.16278801485838,0.21834396591395,35.3553168435612));
#65336=CARTESIAN_POINT('Ctrl Pts',(2.61678000270041,4.45584072777334,35.514077605807));
#65337=CARTESIAN_POINT('Ctrl Pts',(-2.32418499851494,4.61521595014736,35.672838368053));
#65338=CARTESIAN_POINT('Ctrl Pts',(-5.13798489593422,0.55060456133973,35.8315991302988));
#65339=CARTESIAN_POINT('Ctrl Pts',(-3.24934407480239,-4.01793694044132,
35.9903598925447));
#65340=CARTESIAN_POINT('Ctrl Pts',(1.61319569609569,-4.90913982484862,36.1491206547906));
#65341=CARTESIAN_POINT('Ctrl Pts',(4.99928949022287,-1.30734798992603,36.3078814170365));
#65342=CARTESIAN_POINT('Ctrl Pts',(3.80988083761225,3.49096865884117,36.4666421792824));
#65343=CARTESIAN_POINT('Ctrl Pts',(-0.866447131906533,5.09424415801081,
36.6254029415283));
#65344=CARTESIAN_POINT('Ctrl Pts',(-4.74977622033223,2.03511179805508,36.7841637037742));
#65345=CARTESIAN_POINT('Ctrl Pts',(-4.28596502810612,-2.88661704277997,
36.94292446602));
#65346=CARTESIAN_POINT('Ctrl Pts',(0.100492274349119,-5.16642579319712,
37.101685228266));
#65347=CARTESIAN_POINT('Ctrl Pts',(4.39497597774354,-2.71776384714963,37.2604459905118));
#65348=CARTESIAN_POINT('Ctrl Pts',(4.66704342001788,2.21827858698683,37.4192067527577));
#65349=CARTESIAN_POINT('Ctrl Pts',(0.66769016759438,5.12408470011126,37.5779675150036));
#65350=CARTESIAN_POINT('Ctrl Pts',(-3.9427535210732,3.34017197848871,37.7367282772495));
#65351=CARTESIAN_POINT('Ctrl Pts',(-4.94466875428017,-1.50076816472822,
37.8954890394954));
#65352=CARTESIAN_POINT('Ctrl Pts',(-1.42107210669624,-4.96815944202542,
38.0542498017413));
#65353=CARTESIAN_POINT('Ctrl Pts',(3.40313314014881,-3.88853944357485,38.2130105639872));
#65354=CARTESIAN_POINT('Ctrl Pts',(5.11268698707437,0.749990630619295,38.3717713262331));
#65355=CARTESIAN_POINT('Ctrl Pts',(2.14295353437204,4.70210637090854,38.5305320884789));
#65356=CARTESIAN_POINT('Ctrl Pts',(-2.78807645035559,4.35071073283309,38.6892928507248));
#65357=CARTESIAN_POINT('Ctrl Pts',(-5.16737370481374,0.0174117378790549,
38.8480536129707));
#65358=CARTESIAN_POINT('Ctrl Pts',(-2.81733270514135,-4.33182301143032,
39.0068143752166));
#65359=CARTESIAN_POINT('Ctrl Pts',(2.11121724282438,-4.71644102342194,39.1655751374625));
#65360=CARTESIAN_POINT('Ctrl Pts',(5.10751668218689,-0.784428145210908,
39.3243358997084));
#65361=CARTESIAN_POINT('Ctrl Pts',(3.42926084288352,3.86551733216684,39.4830966619543));
#65362=CARTESIAN_POINT('Ctrl Pts',(-1.38755926796319,4.97762327338117,39.6418574242002));
#65363=CARTESIAN_POINT('Ctrl Pts',(-4.93444275322028,1.53405635131447,39.8006181864461));
#65364=CARTESIAN_POINT('Ctrl Pts',(-3.96517350621375,-3.31352580183661,
39.959378948692));
#65365=CARTESIAN_POINT('Ctrl Pts',(0.6331436514814,-5.12846792818335,40.1181397109379));
#65366=CARTESIAN_POINT('Ctrl Pts',(4.65198839971611,-2.2496795555641,40.2769004731838));
#65367=CARTESIAN_POINT('Ctrl Pts',(4.41319126769477,2.68808426366416,40.4356612354296));
#65368=CARTESIAN_POINT('Ctrl Pts',(0.135306684796697,5.16563125618407,40.5944219976755));
#65369=CARTESIAN_POINT('Ctrl Pts',(-4.26641470902384,2.91543473678309,40.7531827599214));
#65370=CARTESIAN_POINT('Ctrl Pts',(-4.7633830418116,-2.00305670683536,40.9119435221673));
#65371=CARTESIAN_POINT('Ctrl Pts',(-0.90075771530386,-5.08828946819429,
41.0707042844132));
#65372=CARTESIAN_POINT('Ctrl Pts',(3.78626858625262,-3.51656428443629,41.2294650466591));
#65373=CARTESIAN_POINT('Ctrl Pts',(5.00798622459088,1.27362794729248,41.3882258089049));
#65374=CARTESIAN_POINT('Ctrl Pts',(1.64624189925253,4.89815697818699,41.5469865711509));
#65375=CARTESIAN_POINT('Ctrl Pts',(-3.22219329739529,4.03974312649174,41.7057473333967));
#65376=CARTESIAN_POINT('Ctrl Pts',(-5.14157876509112,-0.515967030129218,
41.8645080956427));
#65377=CARTESIAN_POINT('Ctrl Pts',(-2.35523429540729,-4.59944840035779,
42.0232688578885));
#65378=CARTESIAN_POINT('Ctrl Pts',(2.58669254300161,-4.47337410259821,42.1820296201345));
#65379=CARTESIAN_POINT('Ctrl Pts',(5.16119935450289,-0.253131185149624,
42.3407903823802));
#65380=CARTESIAN_POINT('Ctrl Pts',(3.01201886587614,4.19878512494061,42.4995511446263));
#65381=CARTESIAN_POINT('Ctrl Pts',(-1.89385329211466,4.80784503512363,42.6583119068721));
#65382=CARTESIAN_POINT('Ctrl Pts',(-5.0664130686601,1.01661831162269,42.817072669118));
#65383=CARTESIAN_POINT('Ctrl Pts',(-3.6020368491656,-3.70504854368597,42.9758334313639));
#65384=CARTESIAN_POINT('Ctrl Pts',(1.15903352033341,-5.0357417996319,43.1345941936098));
#65385=CARTESIAN_POINT('Ctrl Pts',(4.85932100888344,-1.75757034181863,43.2933549558556));
#65386=CARTESIAN_POINT('Ctrl Pts',(4.11220948021047,3.12918317851219,43.4521157181016));
#65387=CARTESIAN_POINT('Ctrl Pts',(-0.398521773825228,5.15201267172389,
43.6108764803474));
#65388=CARTESIAN_POINT('Ctrl Pts',(-4.54451372744996,2.45956279749778,43.7696372425933));
#65389=CARTESIAN_POINT('Ctrl Pts',(-4.53122790373328,-2.48395407732217,
43.9283980048393));
#65390=CARTESIAN_POINT('Ctrl Pts',(-0.370823894361365,-5.15408030721166,
44.0871587670851));
#65391=CARTESIAN_POINT('Ctrl Pts',(4.12896947009338,-3.10703480650815,44.245919529331));
#65392=CARTESIAN_POINT('Ctrl Pts',(4.84980385450403,1.78366385472551,44.4046802915768));
#65393=CARTESIAN_POINT('Ctrl Pts',(1.13194961208497,5.04189887339256,44.5634410538228));
#65394=CARTESIAN_POINT('Ctrl Pts',(-3.62189949116538,3.68563403632435,44.7222018160687));
#65395=CARTESIAN_POINT('Ctrl Pts',(-5.06087554774066,-1.0438356499454,44.8809625783145));
#65396=CARTESIAN_POINT('Ctrl Pts',(-1.8679837165673,-4.81795506501003,45.0397233405604));
#65397=CARTESIAN_POINT('Ctrl Pts',(3.03454387031403,-4.18253483822383,45.1984841028063));
#65398=CARTESIAN_POINT('Ctrl Pts',(5.15976421573454,0.280869029694986,45.3572448650522));
#65399=CARTESIAN_POINT('Ctrl Pts',(2.56261074386464,4.4872129823807,45.5160056272982));
#65400=CARTESIAN_POINT('Ctrl Pts',(-2.37992235675453,4.58672254988638,45.6747663895439));
#65401=CARTESIAN_POINT('Ctrl Pts',(-5.14427782079704,0.488323536471552,
45.8335271517899));
#65402=CARTESIAN_POINT('Ctrl Pts',(-3.20043308923407,-4.05700409355871,
45.9922879140358));
#65403=CARTESIAN_POINT('Ctrl Pts',(1.67254576409749,-4.88923765436041,46.1510486762816));
#65404=CARTESIAN_POINT('Ctrl Pts',(5.01475964555148,-1.2466915701828,46.3098094385276));
#65405=CARTESIAN_POINT('Ctrl Pts',(3.76731232156889,3.53686471971598,46.4685702007735));
#65406=CARTESIAN_POINT('Ctrl Pts',(-0.928094313166731,5.08337438319113,
46.6273309630193));
#65407=CARTESIAN_POINT('Ctrl Pts',(-4.77408068348225,1.97742453747749,46.7860917252652));
#65408=CARTESIAN_POINT('Ctrl Pts',(-4.25068258608159,-2.93832464615453,
46.9448524875111));
#65409=CARTESIAN_POINT('Ctrl Pts',(0.163070052891163,-5.16482936133098,
47.103613249757));
#65410=CARTESIAN_POINT('Ctrl Pts',(4.42757599841828,-2.66432448325026,47.2623740120029));
#65411=CARTESIAN_POINT('Ctrl Pts',(4.63982914812316,2.27465154475207,47.4211347742487));
#65412=CARTESIAN_POINT('Ctrl Pts',(0.605568936039063,5.13179699886122,47.5798955364947));
#65413=CARTESIAN_POINT('Ctrl Pts',(-3.982926463652,3.29216508683222,47.7386562987406));
#65414=CARTESIAN_POINT('Ctrl Pts',(-4.92612590373581,-1.56055687315755,
47.8974170609864));
#65415=CARTESIAN_POINT('Ctrl Pts',(-1.36078444624568,-4.98500951500319,
48.0561778232324));
#65416=CARTESIAN_POINT('Ctrl Pts',(3.44998850215064,-3.84702917961962,48.2149385854782));
#65417=CARTESIAN_POINT('Ctrl Pts',(5.10322659210776,0.811869769988193,48.3736993477241));
#65418=CARTESIAN_POINT('Ctrl Pts',(2.08583582488191,4.72772070721777,48.53246010997));
#65419=CARTESIAN_POINT('Ctrl Pts',(-2.8405756019607,4.31661724309231,48.6912208722158));
#65420=CARTESIAN_POINT('Ctrl Pts',(-5.16720547137737,-0.0451861747017031,
48.8499816344618));
#65421=CARTESIAN_POINT('Ctrl Pts',(-2.76465105904324,-4.36563382517906,
49.0087423967076));
#65422=CARTESIAN_POINT('Ctrl Pts',(2.16819644989342,-4.69052004883103,49.1675031589536));
#65423=CARTESIAN_POINT('Ctrl Pts',(5.11664433946473,-0.72249904999246,49.3262639211995));
#65424=CARTESIAN_POINT('Ctrl Pts',(3.38218303962157,3.90677514842007,49.4850246834453));
#65425=CARTESIAN_POINT('Ctrl Pts',(-1.44775548820939,4.96044939699782,49.6437854456913));
#65426=CARTESIAN_POINT('Ctrl Pts',(-4.95266397096391,1.47416883854343,49.8025462079371));
#65427=CARTESIAN_POINT('Ctrl Pts',(-3.92474310640146,-3.36131607001936,
49.961306970183));
#65428=CARTESIAN_POINT('Ctrl Pts',(0.695222531978707,-5.12042183856424,
50.1200677324289));
#65429=CARTESIAN_POINT('Ctrl Pts',(4.67889927324325,-2.19316113513354,50.2788284946747));
#65430=CARTESIAN_POINT('Ctrl Pts',(4.38030448079635,2.74134763015048,50.4375892569207));
#65431=CARTESIAN_POINT('Ctrl Pts',(0.0727212293821569,5.16689130876717,
50.5963500191666));
#65432=CARTESIAN_POINT('Ctrl Pts',(-4.30141871246148,2.86353823685011,50.7551107814125));
#65433=CARTESIAN_POINT('Ctrl Pts',(-4.73876886011502,-2.06061249734653,
50.9138715436583));
#65434=CARTESIAN_POINT('Ctrl Pts',(-0.839052999411725,-5.09882773174331,
51.0726323059043));
#65435=CARTESIAN_POINT('Ctrl Pts',(3.82858979556074,-3.47044008032763,51.2313930681501));
#65436=CARTESIAN_POINT('Ctrl Pts',(4.99219026383802,1.33420033857639,51.390153830396));
#65437=CARTESIAN_POINT('Ctrl Pts',(1.58678571421362,4.91773985393535,51.548914592642));
#65438=CARTESIAN_POINT('Ctrl Pts',(-3.27089359005984,4.00041364065291,51.7076753548878));
#65439=CARTESIAN_POINT('Ctrl Pts',(-5.1349511699649,-0.578213330780779,
51.8664361171337));
#65440=CARTESIAN_POINT('Ctrl Pts',(-2.2993445899923,-4.62764180012773,52.0251968793796));
#65441=CARTESIAN_POINT('Ctrl Pts',(2.64069239313623,-4.44171114083851,52.1839576416255));
#65442=CARTESIAN_POINT('Ctrl Pts',(5.16388703706709,-0.190590771620509,
52.3427184038713));
#65443=CARTESIAN_POINT('Ctrl Pts',(2.96093453169081,4.23496409345547,52.5014791661172));
#65444=CARTESIAN_POINT('Ctrl Pts',(-1.95195570001178,4.78455046153847,52.6602399283632));
#65445=CARTESIAN_POINT('Ctrl Pts',(-5.07835645180041,0.955170101224678,
52.819000690609));
#65446=CARTESIAN_POINT('Ctrl Pts',(-3.5568902584837,-3.7484111117806,52.9777614528549));
#65447=CARTESIAN_POINT('Ctrl Pts',(1.21995054602492,-5.021331978576,53.1365222151008));
#65448=CARTESIAN_POINT('Ctrl Pts',(4.88025534693686,-1.69857643999627,53.2952829773467));
#65449=CARTESIAN_POINT('Ctrl Pts',(4.07400138499168,3.17876814016096,53.4540437395925));
#65450=CARTESIAN_POINT('Ctrl Pts',(-0.460903086490536,5.14680702170578,
53.6128045018385));
#65451=CARTESIAN_POINT('Ctrl Pts',(-4.57397497474849,2.404330905718,53.7715652640843));
#65452=CARTESIAN_POINT('Ctrl Pts',(-4.5008052522319,-2.53866229642665,53.9303260263303));
#65453=CARTESIAN_POINT('Ctrl Pts',(-0.308361083986154,-5.15819422043212,
54.0890867885761));
#65454=CARTESIAN_POINT('Ctrl Pts',(4.16630456733569,-3.05678923480409,54.2478475508221));
#65455=CARTESIAN_POINT('Ctrl Pts',(4.82784101720183,1.84228262935957,54.4066083130679));
#65456=CARTESIAN_POINT('Ctrl Pts',(1.07078989980086,5.0552411578777,54.5653690753139));
#65457=CARTESIAN_POINT('Ctrl Pts',(-3.66628084160122,3.64148856435446,54.7241298375597));
#65458=CARTESIAN_POINT('Ctrl Pts',(-5.04785936876341,-1.10506559398251,
54.8828905998056));
#65459=CARTESIAN_POINT('Ctrl Pts',(-1.80948281276126,-4.84022996603858,
55.0416513620516));
#65460=CARTESIAN_POINT('Ctrl Pts',(3.08498768485217,-4.1454680264268,55.2004121242973));
#65461=CARTESIAN_POINT('Ctrl Pts',(5.15598322111311,0.34335287594041,55.3591728865433));
#65462=CARTESIAN_POINT('Ctrl Pts',(2.50806542185317,4.51792673839683,55.5179336487891));
#65463=CARTESIAN_POINT('Ctrl Pts',(-2.43531046134262,4.55755604800332,55.6766944110351));
#65464=CARTESIAN_POINT('Ctrl Pts',(-5.14981582279099,0.425970850115064,
55.8354551732808));
#65465=CARTESIAN_POINT('Ctrl Pts',(-3.15105244004859,-4.09547588124754,
55.9942159355269));
#65466=CARTESIAN_POINT('Ctrl Pts',(1.73165038597632,-4.86861798815274,56.1529766977727));
#65467=CARTESIAN_POINT('Ctrl Pts',(5.02949388480597,-1.18585219842773,56.3117374600186));
#65468=CARTESIAN_POINT('Ctrl Pts',(3.72419095237009,3.58224174562538,56.4704982222645));
#65469=CARTESIAN_POINT('Ctrl Pts',(-0.989605296568694,5.07175862308326,
56.6292589845104));
#65470=CARTESIAN_POINT('Ctrl Pts',(-4.79768455020047,1.91944708981109,56.7880197467563));
#65471=CARTESIAN_POINT('Ctrl Pts',(-4.21477635630603,-2.98960105033098,
56.9467805090022));
#65472=CARTESIAN_POINT('Ctrl Pts',(0.225623900899773,-5.162474990657,57.1055412712481));
#65473=CARTESIAN_POINT('Ctrl Pts',(4.45952627223033,-2.61049412968195,57.2643020334939));
#65474=CARTESIAN_POINT('Ctrl Pts',(4.61193398121205,2.33069069735948,57.4230627957398));
#65475=CARTESIAN_POINT('Ctrl Pts',(0.543358837230748,5.13875620630321,57.5818235579857));
#65476=CARTESIAN_POINT('Ctrl Pts',(-4.02251491169591,3.24367506988608,57.7405843202316));
#65477=CARTESIAN_POINT('Ctrl Pts',(-4.90686014412063,-1.62011656983585,
57.8993450824775));
#65478=CARTESIAN_POINT('Ctrl Pts',(-1.30029709065152,-5.00112803773905,
58.0581058447233));
#65479=CARTESIAN_POINT('Ctrl Pts',(3.49633757827368,-3.80495436405849,58.2168666069693));
#65480=CARTESIAN_POINT('Ctrl Pts',(5.09301729854088,0.873629767452735,58.3756273692151));
#65481=CARTESIAN_POINT('Ctrl Pts',(2.02841201894453,4.75264125042254,58.5343881314611));
#65482=CARTESIAN_POINT('Ctrl Pts',(-2.89265789904175,4.2818902896884,58.6931488937069));
#65483=CARTESIAN_POINT('Ctrl Pts',(-5.16627895043901,-0.107777456210482,
58.8519096559528));
#65484=CARTESIAN_POINT('Ctrl Pts',(-2.71156370034918,-4.39880398208026,
59.0106704181988));
#65485=CARTESIAN_POINT('Ctrl Pts',(2.22485747409188,-4.66391074033302,59.1694311804446));
#65486=CARTESIAN_POINT('Ctrl Pts',(5.12502112908765,-0.660463928024547,
59.3281919426906));
#65487=CARTESIAN_POINT('Ctrl Pts',(3.33460890093368,3.94745964534539,59.4869527049363));
#65488=CARTESIAN_POINT('Ctrl Pts',(-1.5077392503099,4.94254757457034,59.6457134671823));
#65489=CARTESIAN_POINT('Ctrl Pts',(-4.97015838517481,1.41406499146713,59.8044742294282));
#65490=CARTESIAN_POINT('Ctrl Pts',(-3.88373675046313,-3.40861306500439,
59.963234991674));
#65491=CARTESIAN_POINT('Ctrl Pts',(0.757199388556149,-5.11162432694214,
60.12199575392));
#65492=CARTESIAN_POINT('Ctrl Pts',(4.70512351821232,-2.13632086826434,60.2807565161658));
#65493=CARTESIAN_POINT('Ctrl Pts',(4.34677488413138,2.79420870381954,60.4395172784118));
#65494=CARTESIAN_POINT('Ctrl Pts',(0.0101251021257834,5.16739311995163,
60.5982780406576));
#65495=CARTESIAN_POINT('Ctrl Pts',(-4.33579148262063,2.81122151262594,60.7570388029036));
#65496=CARTESIAN_POINT('Ctrl Pts',(-4.71345926399734,-2.11786589293417,
60.9157995651493));
#65497=CARTESIAN_POINT('Ctrl Pts',(-0.777225152475865,-5.10861774222493,
61.0745603273954));
#65498=CARTESIAN_POINT('Ctrl Pts',(3.87034915924295,-3.42380658907068,61.2333210896411));
#65499=CARTESIAN_POINT('Ctrl Pts',(4.97566169906822,1.39457693593507,61.3920818518871));
#65500=CARTESIAN_POINT('Ctrl Pts',(1.52709666834069,4.93660105126586,61.550842614133));
#65501=CARTESIAN_POINT('Ctrl Pts',(-3.3191138790273,3.96049709403562,61.7096033763789));
#65502=CARTESIAN_POINT('Ctrl Pts',(-5.12757002065602,-0.640374778614905,
61.8683641386248));
#65503=CARTESIAN_POINT('Ctrl Pts',(-2.24311745571471,-4.65515609337478,
62.0271249008706));
#65504=CARTESIAN_POINT('Ctrl Pts',(2.69430472161155,-4.40939635788372,62.1858856631165));
#65505=CARTESIAN_POINT('Ctrl Pts',(5.16581691910958,-0.128022388891978,
62.3446464253625));
#65506=CARTESIAN_POINT('Ctrl Pts',(2.90941568030617,4.27052158090844,62.5034071876082));
#65507=CARTESIAN_POINT('Ctrl Pts',(-2.00977165837252,4.76055375508134,62.6621679498542));
#65508=CARTESIAN_POINT('Ctrl Pts',(-5.08955458603407,0.893581719595941,
62.8209287121001));
#65509=CARTESIAN_POINT('Ctrl Pts',(-3.51122169408817,-3.79122360047265,
62.9796894743459));
#65510=CARTESIAN_POINT('Ctrl Pts',(1.28068854395033,-5.00618527695598,63.1384502365919));
#65511=CARTESIAN_POINT('Ctrl Pts',(4.90047350742458,-1.63933327204883,63.2972109988377));
#65512=CARTESIAN_POINT('Ctrl Pts',(4.03519542999152,3.22788661752423,63.4559717610837));
#65513=CARTESIAN_POINT('Ctrl Pts',(-0.523216761619089,5.14084607765855,
63.6147325233295));
#65514=CARTESIAN_POINT('Ctrl Pts',(-4.60276499113179,2.34874617833169,63.7734932855755));
#65515=CARTESIAN_POINT('Ctrl Pts',(-4.46972210747346,-2.59299796679048,
63.9322540478212));
#65516=CARTESIAN_POINT('Ctrl Pts',(-0.245853021615901,-5.16155116855183,
64.0910148100673));
#65517=CARTESIAN_POINT('Ctrl Pts',(4.20302825930282,-3.00609507922124,64.249775572313));
#65518=CARTESIAN_POINT('Ctrl Pts',(4.80516969413782,1.90063104898239,64.408536334559));
#65519=CARTESIAN_POINT('Ctrl Pts',(1.00947304907845,5.06784158562605,64.5672970968048));
#65520=CARTESIAN_POINT('Ctrl Pts',(-3.71012416525332,3.59680870386789,64.7260578590508));
#65521=CARTESIAN_POINT('Ctrl Pts',(-5.03410241632698,-1.16613336962256,
64.8848186212966));
#65522=CARTESIAN_POINT('Ctrl Pts',(-1.75071636731768,-4.86179456322688,
65.0435793835425));
#65523=CARTESIAN_POINT('Ctrl Pts',(3.1349787773885,-4.10779286711735,65.2023401457884));
#65524=CARTESIAN_POINT('Ctrl Pts',(5.15144558585509,0.405786335144852,65.3611009080343));
#65525=CARTESIAN_POINT('Ctrl Pts',(2.45315204119292,4.54797748857745,65.5198616702802));
#65526=CARTESIAN_POINT('Ctrl Pts',(-2.49034118407384,4.52772072468283,65.6786224325261));
#65527=CARTESIAN_POINT('Ctrl Pts',(-5.15459808921429,0.363555652528053,
65.837383194772));
#65528=CARTESIAN_POINT('Ctrl Pts',(-3.10120937385697,-4.13334665777235,
65.9961439570178));
#65529=CARTESIAN_POINT('Ctrl Pts',(1.79050088812788,-4.84728385216189,66.1549047192638));
#65530=CARTESIAN_POINT('Ctrl Pts',(5.04349004573647,-1.12483880283976,66.3136654815096));
#65531=CARTESIAN_POINT('Ctrl Pts',(3.68052305807757,3.62709307749002,66.4724262437556));
#65532=CARTESIAN_POINT('Ctrl Pts',(-1.05097105537457,5.05939858230018,66.6311870060014));
#65533=CARTESIAN_POINT('Ctrl Pts',(-4.82058435661895,1.86118796324735,66.7899477682473));
#65534=CARTESIAN_POINT('Ctrl Pts',(-4.17825160801934,-3.04043873049599,
66.9487085304932));
#65535=CARTESIAN_POINT('Ctrl Pts',(0.288144638596748,-5.15936302667923,
67.1074692927391));
#65536=CARTESIAN_POINT('Ctrl Pts',(4.49082211047655,-2.55628068604989,67.266230054985));
#65537=CARTESIAN_POINT('Ctrl Pts',(4.58336201290063,2.38638782106256,67.4249908172308));
#65538=CARTESIAN_POINT('Ctrl Pts',(0.481069000502546,5.14496130117338,67.5837515794768));
#65539=CARTESIAN_POINT('Ctrl Pts',(-4.06151305559941,3.19470904356121,67.7425123417227));
#65540=CARTESIAN_POINT('Ctrl Pts',(-4.88687430268524,-1.67943851437657,
67.9012731039685));
#65541=CARTESIAN_POINT('Ctrl Pts',(-1.23961891643423,-5.01651264483955,
68.0600338662145));
#65542=CARTESIAN_POINT('Ctrl Pts',(3.54217356679019,-3.76232117137135,68.2187946284603));
#65543=CARTESIAN_POINT('Ctrl Pts',(5.08206060458778,0.935261559732356,68.3775553907062));
#65544=CARTESIAN_POINT('Ctrl Pts',(1.97069054350433,4.77686434343271,68.5363161529522));
#65545=CARTESIAN_POINT('Ctrl Pts',(-2.9443156985208,4.2465349688023,68.695076915198));
#65546=CARTESIAN_POINT('Ctrl Pts',(-5.16459427796565,-0.170352921375672,
68.8538376774439));
#65547=CARTESIAN_POINT('Ctrl Pts',(-2.65807841962993,-4.43132861441282,
69.0125984396897));
#65548=CARTESIAN_POINT('Ctrl Pts',(2.2811920004135,-4.63661700284439,69.1713592019357));
#65549=CARTESIAN_POINT('Ctrl Pts',(5.1326458217616,-0.598331882962418,69.3301199641815));
#65550=CARTESIAN_POINT('Ctrl Pts',(3.28654540832559,3.98756485249208,69.4888807264275));
#65551=CARTESIAN_POINT('Ctrl Pts',(-1.56750175164667,4.92392043319156,69.6476414886732));
#65552=CARTESIAN_POINT('Ctrl Pts',(-4.98692342854749,1.35375363032602,69.8064022509193));
#65553=CARTESIAN_POINT('Ctrl Pts',(-3.84216045608199,-3.45540984595692,
69.965163013165));
#65554=CARTESIAN_POINT('Ctrl Pts',(0.819065126108891,-5.102076684352,70.1239237754111));
#65555=CARTESIAN_POINT('Ctrl Pts',(4.73065728621489,-2.07916709626671,70.2826845376568));
#65556=CARTESIAN_POINT('Ctrl Pts',(4.31260739816882,2.84665972730784,70.4414452999028));
#65557=CARTESIAN_POINT('Ctrl Pts',(-0.0524725109896868,5.16713661609669,
70.6002060621488));
#65558=CARTESIAN_POINT('Ctrl Pts',(-4.36952797529665,2.75849224159072,70.7589668243945));
#65559=CARTESIAN_POINT('Ctrl Pts',(-4.68745796764224,-2.17480849166161,
70.9177275866405));
#65560=CARTESIAN_POINT('Ctrl Pts',(-0.715283247733823,-5.11765806295492,
71.0764883488864));
#65561=CARTESIAN_POINT('Ctrl Pts',(3.91154054911197,-3.37667065413102,71.2352491111322));
#65562=CARTESIAN_POINT('Ctrl Pts',(4.95840295584866,1.45474887910182,71.3940098733782));
#65563=CARTESIAN_POINT('Ctrl Pts',(1.46718352100222,4.95473780229749,71.552770635624));
#65564=CARTESIAN_POINT('Ctrl Pts',(-3.36684708796952,3.91999934439373,71.7115313978699));
#65565=CARTESIAN_POINT('Ctrl Pts',(-5.11943640034826,-0.702442251438138,
71.8702921601158));
#65566=CARTESIAN_POINT('Ctrl Pts',(-2.18656114390733,-4.68198724237597,
72.0290529223616));
#65567=CARTESIAN_POINT('Ctrl Pts',(2.74752166081747,-4.3764344959288,72.1878136846077));
#65568=CARTESIAN_POINT('Ctrl Pts',(5.16698871742013,-0.0654352188752399,
72.3465744468534));
#65569=CARTESIAN_POINT('Ctrl Pts',(2.85746987211454,4.30545236923763,72.5053352090995));
#65570=CARTESIAN_POINT('Ctrl Pts',(-2.06729268270395,4.73585843726931,72.6640959713451));
#65571=CARTESIAN_POINT('Ctrl Pts',(-5.10000582803462,0.831862204832684,
72.8228567335913));
#65572=CARTESIAN_POINT('Ctrl Pts',(-3.46503785784167,-3.83347972702879,
72.9816174958369));
#65573=CARTESIAN_POINT('Ctrl Pts',(1.34123860080759,-4.99030391755056,73.140378258083));
#65574=CARTESIAN_POINT('Ctrl Pts',(4.91997252333115,-1.57984953191204,73.2991390203287));
#65575=CARTESIAN_POINT('Ctrl Pts',(3.99579730998455,3.27653140246455,73.4578997825747));
#65576=CARTESIAN_POINT('Ctrl Pts',(-0.585453654677876,5.13413071435083,
73.6166605448206));
#65577=CARTESIAN_POINT('Ctrl Pts',(-4.63087955166449,2.29281677239862,73.7754213070665));
#65578=CARTESIAN_POINT('Ctrl Pts',(-4.43798303090997,-2.64695311465312,
73.9341820693124));
#65579=CARTESIAN_POINT('Ctrl Pts',(-0.183308880309829,-5.16415065893858,
74.0929428315583));
#65580=CARTESIAN_POINT('Ctrl Pts',(4.23913515679244,-2.95495977912772,74.2517035938041));
#65581=CARTESIAN_POINT('Ctrl Pts',(4.78179321232898,1.95870055096247,74.4104643560501));
#65582=CARTESIAN_POINT('Ctrl Pts',(0.948008058166557,5.07969830752458,74.5692251182959));
#65583=CARTESIAN_POINT('Ctrl Pts',(-3.75342302811316,3.55160101163497,74.7279858805418));
#65584=CARTESIAN_POINT('Ctrl Pts',(-5.01960670926438,-1.22703001516843,
74.8867466427878));
#65585=CARTESIAN_POINT('Ctrl Pts',(-1.69169300421356,-4.88264569196979,
75.0455074050335));
#65586=CARTESIAN_POINT('Ctrl Pts',(3.18450981172911,-4.06951488912588,75.2042681672795));
#65587=CARTESIAN_POINT('Ctrl Pts',(5.14615197585861,0.468160245196775,75.3630289295254));
#65588=CARTESIAN_POINT('Ctrl Pts',(2.39787866042351,4.57736082297456,75.5217896917712));
#65589=CARTESIAN_POINT('Ctrl Pts',(-2.54500644918866,4.49722095825909,75.6805504540172));
#65590=CARTESIAN_POINT('Ctrl Pts',(-5.15862391826907,0.301087103142032,
75.839311216263));
#65591=CARTESIAN_POINT('Ctrl Pts',(-3.05091120513038,-4.17061086559584,
75.9980719785089));
#65592=CARTESIAN_POINT('Ctrl Pts',(1.84908863423975,-4.82523837717284,76.1568327407549));
#65593=CARTESIAN_POINT('Ctrl Pts',(5.05674607440601,-1.06366033713594,76.3155935030006));
#65594=CARTESIAN_POINT('Ctrl Pts',(3.63631504695578,3.6714121333759,76.4743542652466));
#65595=CARTESIAN_POINT('Ctrl Pts',(-1.11218258415778,5.04629607467818,76.6331150274925));
#65596=CARTESIAN_POINT('Ctrl Pts',(-4.84277674219067,1.80265570731443,76.7918757897383));
#65597=CARTESIAN_POINT('Ctrl Pts',(-4.1411137012291,-3.09083022621898,76.9506365519843));
#65598=CARTESIAN_POINT('Ctrl Pts',(0.350623091062388,-5.15549392607834,
77.1093973142301));
#65599=CARTESIAN_POINT('Ctrl Pts',(4.52145892049186,-2.50169210817825,77.268158076476));
#65600=CARTESIAN_POINT('Ctrl Pts',(4.55411743612604,2.44173474230699,77.4269188387219));
#65601=CARTESIAN_POINT('Ctrl Pts',(0.4187085668894,5.15041137287398,77.5856796009678));
#65602=CARTESIAN_POINT('Ctrl Pts',(-4.09991517238411,3.14527419362299,77.7444403632137));
#65603=CARTESIAN_POINT('Ctrl Pts',(-4.86617131235222,-1.738514001283,77.9032011254596));
#65604=CARTESIAN_POINT('Ctrl Pts',(-1.17875882811733,-5.03116107861318,
78.0619618877055));
#65605=CARTESIAN_POINT('Ctrl Pts',(3.58748974126774,-3.71913585798031,78.2207226499514));
#65606=CARTESIAN_POINT('Ctrl Pts',(5.07035811814355,0.996756102360001,78.3794834121972));
#65607=CARTESIAN_POINT('Ctrl Pts',(1.91267986918918,4.80038643150889,78.5382441744432));
#65608=CARTESIAN_POINT('Ctrl Pts',(-2.99554141961442,4.21055646882815,78.697004936689));
#65609=CARTESIAN_POINT('Ctrl Pts',(-5.16215170118294,-0.232903387246084,
78.855765698935));
#65610=CARTESIAN_POINT('Ctrl Pts',(-2.60420306585193,-4.46320294918618,
79.0145264611808));
#65611=CARTESIAN_POINT('Ctrl Pts',(2.33719176176521,-4.60864284172174,79.1732872234268));
#65612=CARTESIAN_POINT('Ctrl Pts',(5.13951729856278,-0.536112032685121,
79.3320479856725));
#65613=CARTESIAN_POINT('Ctrl Pts',(3.23799961511593,4.02708488442023,79.4908087479186));
#65614=CARTESIAN_POINT('Ctrl Pts',(-1.62703422207133,4.90457070639472,79.6495695101643));
#65615=CARTESIAN_POINT('Ctrl Pts',(-5.00295664081116,1.29324360581397,79.8083302724103));
#65616=CARTESIAN_POINT('Ctrl Pts',(-3.80002032458076,-3.5016995454484,79.9670910346561));
#65617=CARTESIAN_POINT('Ctrl Pts',(0.880810665839244,-5.09178031191025,
80.125851796902));
#65618=CARTESIAN_POINT('Ctrl Pts',(4.75549683016874,-2.02170820645871,80.2846125591479));
#65619=CARTESIAN_POINT('Ctrl Pts',(4.27780703699033,2.89869300342805,80.4433733213939));
#65620=CARTESIAN_POINT('Ctrl Pts',(-0.11506242376767,5.16612183484124,80.6021340836397));
#65621=CARTESIAN_POINT('Ctrl Pts',(-4.40262323964949,2.70535816177208,80.7608948458856));
#65622=CARTESIAN_POINT('Ctrl Pts',(-4.66076878675771,-2.23143193721207,
80.9196556081315));
#65623=CARTESIAN_POINT('Ctrl Pts',(-0.653236375128765,-5.12594736724498,
81.0784163703773));
#65624=CARTESIAN_POINT('Ctrl Pts',(3.95215792026738,-3.32903919274863,81.2371771326234));
#65625=CARTESIAN_POINT('Ctrl Pts',(4.94041656702063,1.51470733791976,81.3959378948691));
#65626=CARTESIAN_POINT('Ctrl Pts',(1.40705506422376,4.97214744531344,81.5546986571151));
#65627=CARTESIAN_POINT('Ctrl Pts',(-3.41408621159557,3.87892633505682,81.713459419361));
#65628=CARTESIAN_POINT('Ctrl Pts',(-5.11055150349599,-0.76440664139103,
81.8722201816067));
#65629=CARTESIAN_POINT('Ctrl Pts',(-2.12968395259116,-4.7081313086182,82.0309809438528));
#65630=CARTESIAN_POINT('Ctrl Pts',(2.80033539806548,-4.3428303941221,82.1897417060986));
#65631=CARTESIAN_POINT('Ctrl Pts',(5.16740226597732,-0.00283844241944707,
82.3485024683445));
#65632=CARTESIAN_POINT('Ctrl Pts',(2.80510471878759,4.33975132503298,82.5072632305904));
#65633=CARTESIAN_POINT('Ctrl Pts',(-2.12451031000386,4.71046814615349,82.6660239928362));
#65634=CARTESIAN_POINT('Ctrl Pts',(-5.10970868581842,0.770020587436124,
82.8247847550823));
#65635=CARTESIAN_POINT('Ctrl Pts',(-3.41834544728425,-3.87517323895607,
82.983545517328));
#65636=CARTESIAN_POINT('Ctrl Pts',(1.40159167776471,-4.9736903294079,83.142306279574));
#65637=CARTESIAN_POINT('Ctrl Pts',(4.93874982643145,-1.52013376024582,83.3010670418199));
#65638=CARTESIAN_POINT('Ctrl Pts',(3.95581224496304,3.32469499516411,83.4598278040656));
#65639=CARTESIAN_POINT('Ctrl Pts',(-0.647603556591826,5.12666260907039,
83.6185885663118));
#65640=CARTESIAN_POINT('Ctrl Pts',(-4.65831659106839,2.23654957051732,83.7773493285574));
#65641=CARTESIAN_POINT('Ctrl Pts',(-4.40558873364168,-2.70051728419629,
83.9361100908035));
#65642=CARTESIAN_POINT('Ctrl Pts',(-0.120745397495975,-5.1659971710397,
84.0948708530492));
#65643=CARTESIAN_POINT('Ctrl Pts',(4.27463443926266,-2.90338152834273,84.2536316152952));
#65644=CARTESIAN_POINT('Ctrl Pts',(4.75768727179541,2.01646478129229,84.412392377541));
#65645=CARTESIAN_POINT('Ctrl Pts',(0.886457060193665,5.09084373843816,84.571153139787));
#65646=CARTESIAN_POINT('Ctrl Pts',(-3.79627280569434,3.50580670373394,84.7299139020329));
#65647=CARTESIAN_POINT('Ctrl Pts',(-5.00417952636703,-1.28762129421282,
84.8886746642788));
#65648=CARTESIAN_POINT('Ctrl Pts',(-1.63279460579437,-4.90302030367583,
85.0474354265246));
#65649=CARTESIAN_POINT('Ctrl Pts',(3.23428855022947,-4.03017982392474,85.2061961887705));
#65650=CARTESIAN_POINT('Ctrl Pts',(5.13873193725801,0.529582954402255,85.3649569510164));
#65651=CARTESIAN_POINT('Ctrl Pts',(2.34489518331184,4.6077777382683,85.5237177132623));
#65652=CARTESIAN_POINT('Ctrl Pts',(-2.60449736313211,4.46265913321349,85.6824784755082));
#65653=CARTESIAN_POINT('Ctrl Pts',(-4.72633661207834,0.94905134843793,85.8147791107131));
#65654=CARTESIAN_POINT('Ctrl Pts',(-4.08944266318188,-1.99447502555823,
85.9206196188771));
#65655=CARTESIAN_POINT('Ctrl Pts',(-3.130164636136,-3.13763950664809,85.973539872959));
#65656=CARTESIAN_POINT('Ctrl Pts',(-2.53835875722777,-3.5596515025498,86.));
#65657=CARTESIAN_POINT('Ctrl Pts',(-2.00237954638818,4.09906332620103,25.7806068977079));
#65658=CARTESIAN_POINT('Ctrl Pts',(-2.68386473467845,3.76615995447791,25.8070670247489));
#65659=CARTESIAN_POINT('Ctrl Pts',(-3.86722056834447,2.75399327045732,25.8599872788309));
#65660=CARTESIAN_POINT('Ctrl Pts',(-5.02742207131257,-0.166516440447624,
25.9658277869948));
#65661=CARTESIAN_POINT('Ctrl Pts',(-3.44586235178049,-4.14677665817345,
26.0981284221997));
#65662=CARTESIAN_POINT('Ctrl Pts',(1.62355296838563,-5.14470657330929,26.2568891844456));
#65663=CARTESIAN_POINT('Ctrl Pts',(5.19838240423087,-1.42611203276403,26.4156499466915));
#65664=CARTESIAN_POINT('Ctrl Pts',(4.01994424953236,3.59365933878956,26.5744107089374));
#65665=CARTESIAN_POINT('Ctrl Pts',(-0.839985566934964,5.3265048273725,26.7331714711833));
#65666=CARTESIAN_POINT('Ctrl Pts',(-4.92992667194028,2.18327469128225,26.8919322334291));
#65667=CARTESIAN_POINT('Ctrl Pts',(-4.50847904072441,-2.95758319158922,
27.050692995675));
#65668=CARTESIAN_POINT('Ctrl Pts',(0.0395956222711487,-5.39186919347605,
27.2094537579209));
#65669=CARTESIAN_POINT('Ctrl Pts',(4.55125923496193,-2.89119591637671,27.3682145201668));
#65670=CARTESIAN_POINT('Ctrl Pts',(4.89756113932563,2.25550678246132,27.5269752824127));
#65671=CARTESIAN_POINT('Ctrl Pts',(0.761418625289898,5.33794327443822,27.6857360446586));
#65672=CARTESIAN_POINT('Ctrl Pts',(-4.07157300373756,3.53490884489523,27.8444968069045));
#65673=CARTESIAN_POINT('Ctrl Pts',(-5.17814942709716,-1.503370550728,28.0032575691504));
#65674=CARTESIAN_POINT('Ctrl Pts',(-1.54551865619794,-5.1657253452884,28.1620183313962));
#65675=CARTESIAN_POINT('Ctrl Pts',(3.50161451494142,-4.10024735702302,28.3207790936422));
#65676=CARTESIAN_POINT('Ctrl Pts',(5.34396494196453,0.717900607442646,28.479539855888));
#65677=CARTESIAN_POINT('Ctrl Pts',(2.29535447129834,4.8790048681726,28.6383006181339));
#65678=CARTESIAN_POINT('Ctrl Pts',(-2.85403402839988,4.57469439300441,28.7970613803798));
#65679=CARTESIAN_POINT('Ctrl Pts',(-5.391323666464,0.0834841081329312,28.9558221426257));
#65680=CARTESIAN_POINT('Ctrl Pts',(-2.99430906975439,-4.48413350506007,
29.1145829048716));
#65681=CARTESIAN_POINT('Ctrl Pts',(2.14318857941972,-4.94773510082165,29.2733436671175));
#65682=CARTESIAN_POINT('Ctrl Pts',(5.31917461298845,-0.88301843516797,29.4321044293634));
#65683=CARTESIAN_POINT('Ctrl Pts',(3.62688954521853,3.98986369193538,29.5908651916093));
#65684=CARTESIAN_POINT('Ctrl Pts',(-1.3848356090803,5.21110068710349,29.7496259538552));
#65685=CARTESIAN_POINT('Ctrl Pts',(-5.12911691883564,1.66297916304394,29.9083867161011));
#65686=CARTESIAN_POINT('Ctrl Pts',(-4.17907375081987,-3.40715168987467,
30.0671474783469));
#65687=CARTESIAN_POINT('Ctrl Pts',(0.595785363987352,-5.35895324212101,
30.2259082405928));
#65688=CARTESIAN_POINT('Ctrl Pts',(4.82536351591838,-2.40607709649645,30.3846690028387));
#65689=CARTESIAN_POINT('Ctrl Pts',(4.63862158504372,2.74891430277669,30.5434297650846));
#65690=CARTESIAN_POINT('Ctrl Pts',(0.206471491199163,5.38801536528353,30.7021905273305));
#65691=CARTESIAN_POINT('Ctrl Pts',(-4.41464761825083,3.09584018650688,30.8609512895764));
#65692=CARTESIAN_POINT('Ctrl Pts',(-4.99534638025495,-2.02974249468088,
31.0197120518223));
#65693=CARTESIAN_POINT('Ctrl Pts',(-1.00415155023673,-5.29764284541871,
31.1784728140681));
#65694=CARTESIAN_POINT('Ctrl Pts',(3.90607345078174,-3.71697864543531,31.3372335763141));
#65695=CARTESIAN_POINT('Ctrl Pts',(5.24134071706976,1.26557794744869,31.4959943385599));
#65696=CARTESIAN_POINT('Ctrl Pts',(1.77957286026287,5.08983894524214,31.6547551008058));
#65697=CARTESIAN_POINT('Ctrl Pts',(-3.31091443601954,4.25572386919705,31.8135158630518));
#65698=CARTESIAN_POINT('Ctrl Pts',(-5.37115170725749,-0.473359684716424,
31.9722766252976));
#65699=CARTESIAN_POINT('Ctrl Pts',(-2.51554687204882,-4.76920999621703,
32.1310373875435));
#65700=CARTESIAN_POINT('Ctrl Pts',(2.6423632988389,-4.70013364176394,32.2897981497894));
#65701=CARTESIAN_POINT('Ctrl Pts',(5.38190186659124,-0.329351410916935,
32.4485589120353));
#65702=CARTESIAN_POINT('Ctrl Pts',(3.19575945370633,4.34286329137105,32.6073196742812));
#65703=CARTESIAN_POINT('Ctrl Pts',(-1.91523962695419,5.04035685490976,32.7660804365271));
#65704=CARTESIAN_POINT('Ctrl Pts',(-5.27335289927007,1.12476186513028,32.9248411987729));
#65705=CARTESIAN_POINT('Ctrl Pts',(-3.80513252151237,-3.82024953991496,
33.0836019610189));
#65706=CARTESIAN_POINT('Ctrl Pts',(1.14566136921973,-5.26885187498842,33.2423627232647));
#65707=CARTESIAN_POINT('Ctrl Pts',(5.04791098015974,-1.89524003489642,33.4011234855106));
#65708=CARTESIAN_POINT('Ctrl Pts',(4.330158271609,3.21295337599341,33.5598842477565));
#65709=CARTESIAN_POINT('Ctrl Pts',(-0.350687553524876,5.38055371623537,
33.7186450100024));
#65710=CARTESIAN_POINT('Ctrl Pts',(-4.71057341778202,2.62370694422547,33.8774057722483));
#65711=CARTESIAN_POINT('Ctrl Pts',(-4.75919860374648,-2.53443656531169,
34.0361665344942));
#65712=CARTESIAN_POINT('Ctrl Pts',(-0.452059855948003,-5.3729863149027,
34.19492729674));
#65713=CARTESIAN_POINT('Ctrl Pts',(4.2688178803622,-3.29401486909083,34.353688058986));
#65714=CARTESIAN_POINT('Ctrl Pts',(5.08274309982495,1.79973960190727,34.5124488212318));
#65715=CARTESIAN_POINT('Ctrl Pts',(1.2447865799184,5.24631741547787,34.6712095834778));
#65716=CARTESIAN_POINT('Ctrl Pts',(-3.73243664043062,3.89130527955111,34.8299703457236));
#65717=CARTESIAN_POINT('Ctrl Pts',(-5.2936198386959,-1.02514830968824,34.9887311079695));
#65718=CARTESIAN_POINT('Ctrl Pts',(-2.00992046486332,-5.00335485233809,
35.1474918702154));
#65719=CARTESIAN_POINT('Ctrl Pts',(3.11331951223216,-4.40233820466419,35.3062526324613));
#65720=CARTESIAN_POINT('Ctrl Pts',(5.38715437415002,0.227832839089729,35.4650133947072));
#65721=CARTESIAN_POINT('Ctrl Pts',(2.73050100007286,4.64948430926405,35.6237741569531));
#65722=CARTESIAN_POINT('Ctrl Pts',(-2.42519029351004,4.81578571925249,35.782534919199));
#65723=CARTESIAN_POINT('Ctrl Pts',(-5.36127335207045,0.574532938890892,
35.9412956814449));
#65724=CARTESIAN_POINT('Ctrl Pts',(-3.39055527658917,-4.19254993648074,
36.1000564436907));
#65725=CARTESIAN_POINT('Ctrl Pts',(1.68330255388594,-5.12248304687996,36.2588172059367));
#65726=CARTESIAN_POINT('Ctrl Pts',(5.21655046989866,-1.36416320449261,36.4175779681825));
#65727=CARTESIAN_POINT('Ctrl Pts',(3.97545205425126,3.64268047155399,36.5763387304284));
#65728=CARTESIAN_POINT('Ctrl Pts',(-0.904101513210989,5.31563171291061,
36.7350994926743));
#65729=CARTESIAN_POINT('Ctrl Pts',(-4.95619375964226,2.12355444252664,36.8938602549202));
#65730=CARTESIAN_POINT('Ctrl Pts',(-4.47222608833935,-3.01206471847277,
37.0526210171661));
#65731=CARTESIAN_POINT('Ctrl Pts',(0.10485950493631,-5.39095024441108,37.211381779412));
#65732=CARTESIAN_POINT('Ctrl Pts',(4.58597447631896,-2.83587343794507,37.3701425416579));
#65733=CARTESIAN_POINT('Ctrl Pts',(4.8698655265602,2.31468136181031,37.5289033039037));
#65734=CARTESIAN_POINT('Ctrl Pts',(0.696706894914159,5.34676907637412,37.6876640661497));
#65735=CARTESIAN_POINT('Ctrl Pts',(-4.1140991681465,3.48533041305234,37.8464248283955));
#65736=CARTESIAN_POINT('Ctrl Pts',(-5.15955600572413,-1.56598910509857,
38.0051855906414));
#65737=CARTESIAN_POINT('Ctrl Pts',(-1.48282958617279,-5.18406756050325,
38.1639463528873));
#65738=CARTESIAN_POINT('Ctrl Pts',(3.55102776426338,-4.05752903512989,38.3227071151332));
#65739=CARTESIAN_POINT('Ctrl Pts',(5.33487603729029,0.782584002032494,38.4814678773791));
#65740=CARTESIAN_POINT('Ctrl Pts',(2.23608280507879,4.90645225619513,38.640228639625));
#65741=CARTESIAN_POINT('Ctrl Pts',(-2.90924171237944,4.53978553595244,38.7989894018709));
#65742=CARTESIAN_POINT('Ctrl Pts',(-5.39193935072285,0.0181684236512802,
38.9577501641167));
#65743=CARTESIAN_POINT('Ctrl Pts',(-2.93976939635272,-4.52007698493724,
39.1165109263627));
#65744=CARTESIAN_POINT('Ctrl Pts',(2.20296730598482,-4.92140986936197,39.2752716886085));
#65745=CARTESIAN_POINT('Ctrl Pts',(5.32948103937253,-0.818518114924823,
39.4340324508545));
#65746=CARTESIAN_POINT('Ctrl Pts',(3.5782909344085,4.03350642025291,39.5927932131003));
#65747=CARTESIAN_POINT('Ctrl Pts',(-1.44786033404595,5.19394267455733,39.7515539753462));
#65748=CARTESIAN_POINT('Ctrl Pts',(-5.14888559931178,1.60072394206216,39.9103147375921));
#65749=CARTESIAN_POINT('Ctrl Pts',(-4.13749348932905,-3.45752623695775,
40.069075499838));
#65750=CARTESIAN_POINT('Ctrl Pts',(0.660659043471872,-5.3513427923999,40.2278362620838));
#65751=CARTESIAN_POINT('Ctrl Pts',(4.85415623959407,-2.3474469653437,40.3865970243298));
#65752=CARTESIAN_POINT('Ctrl Pts',(4.60498137310684,2.80490402809622,40.5453577865757));
#65753=CARTESIAN_POINT('Ctrl Pts',(0.141186892964701,5.39012117811339,40.7041185488216));
#65754=CARTESIAN_POINT('Ctrl Pts',(-4.45182614422856,3.04213478252601,40.8628793110674));
#65755=CARTESIAN_POINT('Ctrl Pts',(-4.97039191142365,-2.09010628924604,
41.0216400733134));
#65756=CARTESIAN_POINT('Ctrl Pts',(-0.939903178686041,-5.30941824197221,
41.1804008355592));
#65757=CARTESIAN_POINT('Ctrl Pts',(3.95081365290143,-3.66938844135355,41.3391615978052));
#65758=CARTESIAN_POINT('Ctrl Pts',(5.22562515017917,1.32897774372121,41.497922360051));
#65759=CARTESIAN_POINT('Ctrl Pts',(1.71778489121437,5.11102290358859,41.6566831222969));
#65760=CARTESIAN_POINT('Ctrl Pts',(-3.36222457061253,4.21530378386431,41.8154438845428));
#65761=CARTESIAN_POINT('Ctrl Pts',(-5.36502340492809,-0.538390116983158,
41.9742046467887));
#65762=CARTESIAN_POINT('Ctrl Pts',(-2.4575889422798,-4.7993329374274,42.1329654090346));
#65763=CARTESIAN_POINT('Ctrl Pts',(2.69910598837468,-4.66777965600471,42.2917261712804));
#65764=CARTESIAN_POINT('Ctrl Pts',(5.38549667320271,-0.26413185422043,42.4504869335264));
#65765=CARTESIAN_POINT('Ctrl Pts',(3.14291630057783,4.38125748855891,42.6092476957722));
#65766=CARTESIAN_POINT('Ctrl Pts',(-1.97615707196429,5.01678615055665,42.7680084580181));
#65767=CARTESIAN_POINT('Ctrl Pts',(-5.28659112974097,1.06079888783667,42.926769220264));
#65768=CARTESIAN_POINT('Ctrl Pts',(-3.75857550455005,-3.86606391955536,
43.0855299825098));
#65769=CARTESIAN_POINT('Ctrl Pts',(1.20940322958872,-5.25458693731027,43.2442907447559));
#65770=CARTESIAN_POINT('Ctrl Pts',(5.07049918630525,-1.83395148659098,43.4030515070016));
#65771=CARTESIAN_POINT('Ctrl Pts',(4.29091940730092,3.26517238343396,43.5618122692476));
#65772=CARTESIAN_POINT('Ctrl Pts',(-0.41584088110511,5.37591075215103,43.7205730314935));
#65773=CARTESIAN_POINT('Ctrl Pts',(-4.74201089309862,2.56645139116746,43.8793337937394));
#65774=CARTESIAN_POINT('Ctrl Pts',(-4.72814768911957,-2.59190267629106,
44.0380945559852));
#65775=CARTESIAN_POINT('Ctrl Pts',(-0.386939296906612,-5.3780682437099,
44.1968553182311));
#65776=CARTESIAN_POINT('Ctrl Pts',(4.30840775904998,-3.24206147925195,44.3556160804771));
#65777=CARTESIAN_POINT('Ctrl Pts',(5.06056843189549,1.86117898107469,44.5143768427229));
#65778=CARTESIAN_POINT('Ctrl Pts',(1.18114229879479,5.26101158746959,44.6731376049688));
#65779=CARTESIAN_POINT('Ctrl Pts',(-3.77930134462421,3.84580568932092,44.8318983672147));
#65780=CARTESIAN_POINT('Ctrl Pts',(-5.2808129571804,-1.08919904735859,44.9906591294605));
#65781=CARTESIAN_POINT('Ctrl Pts',(-1.94916324679306,-5.02733554587743,
45.1494198917065));
#65782=CARTESIAN_POINT('Ctrl Pts',(3.16642020502591,-4.36430099084551,45.3081806539524));
#65783=CARTESIAN_POINT('Ctrl Pts',(5.38399916564066,0.293075140317788,45.4669414161982));
#65784=CARTESIAN_POINT('Ctrl Pts',(2.67397763346517,4.68221995096551,45.6257021784443));
#65785=CARTESIAN_POINT('Ctrl Pts',(-2.48334990656791,4.78605404221895,45.7844629406899));
#65786=CARTESIAN_POINT('Ctrl Pts',(-5.3678397571995,0.509545282109415,45.9432237029359));
#65787=CARTESIAN_POINT('Ctrl Pts',(-3.3395186992418,-4.23331488444999,46.1019844651818));
#65788=CARTESIAN_POINT('Ctrl Pts',(1.74523187918884,-5.10171596047391,46.2607452274276));
#65789=CARTESIAN_POINT('Ctrl Pts',(5.232692932984,-1.30087075552908,46.4195059896737));
#65790=CARTESIAN_POINT('Ctrl Pts',(3.93103357982541,3.69057110049061,46.5782667519194));
#65791=CARTESIAN_POINT('Ctrl Pts',(-0.96842778057353,5.30428955537918,46.7370275141654));
#65792=CARTESIAN_POINT('Ctrl Pts',(-4.98155445517987,2.06336018755066,46.8957882764112));
#65793=CARTESIAN_POINT('Ctrl Pts',(-4.43541032884349,-3.06601945008181,
47.0545490386572));
#65794=CARTESIAN_POINT('Ctrl Pts',(0.170156811823045,-5.3892844342159,47.213309800903));
#65795=CARTESIAN_POINT('Ctrl Pts',(4.61999124080161,-2.78011168631907,47.3720705631489));
#65796=CARTESIAN_POINT('Ctrl Pts',(4.8414685667286,2.37350419651411,47.5308313253948));
#65797=CARTESIAN_POINT('Ctrl Pts',(0.631885975802691,5.35481653906792,47.6895920876407));
#65798=CARTESIAN_POINT('Ctrl Pts',(-4.15601796138632,3.43523722006585,47.8483528498866));
#65799=CARTESIAN_POINT('Ctrl Pts',(-5.14020731309298,-1.62837613342762,
48.0071136121325));
#65800=CARTESIAN_POINT('Ctrl Pts',(-1.41992192218023,-5.20164991021152,
48.1658743743783));
#65801=CARTESIAN_POINT('Ctrl Pts',(3.59991938399174,-4.01421480270452,48.3246351366243));
#65802=CARTESIAN_POINT('Ctrl Pts',(5.32500450896511,0.847152308025391,48.4833958988701));
#65803=CARTESIAN_POINT('Ctrl Pts',(2.17648285295299,4.93317974984624,48.642156661116));
#65804=CARTESIAN_POINT('Ctrl Pts',(-2.96402239161607,4.50421039867032,48.800917423362));
#65805=CARTESIAN_POINT('Ctrl Pts',(-5.39176380613531,-0.0471498922667038,
48.9596781856078));
#65806=CARTESIAN_POINT('Ctrl Pts',(-2.88479829170963,-4.55535716158905,
49.1184389478537));
#65807=CARTESIAN_POINT('Ctrl Pts',(2.26242273659985,-4.89436241142882,49.2771997100995));
#65808=CARTESIAN_POINT('Ctrl Pts',(5.33900536977086,-0.753897682082513,
49.4359604723455));
#65809=CARTESIAN_POINT('Ctrl Pts',(3.52916720648512,4.07655723401027,49.5947212345913));
#65810=CARTESIAN_POINT('Ctrl Pts',(-1.51067258399179,5.1760224494748,49.7534819968373));
#65811=CARTESIAN_POINT('Ctrl Pts',(-5.16789868150448,1.53823381551562,49.9122427590831));
#65812=CARTESIAN_POINT('Ctrl Pts',(-4.09530605018365,-3.5073933923671,50.0710035213291));
#65813=CARTESIAN_POINT('Ctrl Pts',(0.72543577101732,-5.34294703282935,50.2297642835748));
#65814=CARTESIAN_POINT('Ctrl Pts',(4.88223661585912,-2.28847234640404,50.3885250458209));
#65815=CARTESIAN_POINT('Ctrl Pts',(4.57066538000743,2.86048213374822,50.5472858080667));
#65816=CARTESIAN_POINT('Ctrl Pts',(0.0758815755810925,5.39143599052969,
50.7060465703126));
#65817=CARTESIAN_POINT('Ctrl Pts',(-4.48835136464999,2.98798294522175,50.8648073325585));
#65818=CARTESIAN_POINT('Ctrl Pts',(-4.94470803747584,-2.15016336068061,
51.0235680948044));
#65819=CARTESIAN_POINT('Ctrl Pts',(-0.875516876330153,-5.32041448129303,
51.1823288570502));
#65820=CARTESIAN_POINT('Ctrl Pts',(3.99497407304406,-3.62125975444968,51.3410896192962));
#65821=CARTESIAN_POINT('Ctrl Pts',(5.20914272269644,1.39218251248544,51.499850381542));
#65822=CARTESIAN_POINT('Ctrl Pts',(1.65574483720076,5.13145681922537,51.658611143788));
#65823=CARTESIAN_POINT('Ctrl Pts',(-3.41304129868565,4.17426510262078,51.8173719060338));
#65824=CARTESIAN_POINT('Ctrl Pts',(-5.35810778531101,-0.603341540490118,
51.9761326682797));
#65825=CARTESIAN_POINT('Ctrl Pts',(-2.39927036128639,-4.82875157643711,
52.1348934305256));
#65826=CARTESIAN_POINT('Ctrl Pts',(2.75545258405494,-4.6347406734915,52.2936541927715));
#65827=CARTESIAN_POINT('Ctrl Pts',(5.38830115807414,-0.198873536169234,
52.4524149550174));
#65828=CARTESIAN_POINT('Ctrl Pts',(3.08961192442195,4.41900873612634,52.6111757172633));
#65829=CARTESIAN_POINT('Ctrl Pts',(-2.03678451588621,4.99247923273975,52.7699364795092));
#65830=CARTESIAN_POINT('Ctrl Pts',(-5.29905355286222,0.996680238285941,
52.928697241755));
#65831=CARTESIAN_POINT('Ctrl Pts',(-3.71146691656038,-3.91131095424147,
53.087458004001));
#65832=CARTESIAN_POINT('Ctrl Pts',(1.27296761001063,-5.23955088889833,53.2462187662468));
#65833=CARTESIAN_POINT('Ctrl Pts',(5.09234329659795,-1.77239380586966,53.4049795284928));
#65834=CARTESIAN_POINT('Ctrl Pts',(4.25105085048754,3.31691222676463,53.5637402907385));
#65835=CARTESIAN_POINT('Ctrl Pts',(-0.48093318402806,5.37047887306077,53.7225010529846));
#65836=CARTESIAN_POINT('Ctrl Pts',(-4.77275247822576,2.50881921131856,53.8812618152303));
#65837=CARTESIAN_POINT('Ctrl Pts',(-4.69640291872861,-2.64898842550301,
54.0400225774763));
#65838=CARTESIAN_POINT('Ctrl Pts',(-0.321761954516003,-5.38236094089921,
54.1987833397221));
#65839=CARTESIAN_POINT('Ctrl Pts',(4.34736537881655,-3.18963231682882,54.3575441019682));
#65840=CARTESIAN_POINT('Ctrl Pts',(5.03765112545161,1.92234523219103,54.5163048642139));
#65841=CARTESIAN_POINT('Ctrl Pts',(1.11732468501616,5.27493370590994,54.6750656264599));
#65842=CARTESIAN_POINT('Ctrl Pts',(-3.82561143627296,3.79974172703212,54.8338263887057));
#65843=CARTESIAN_POINT('Ctrl Pts',(-5.26723111626224,-1.15308994504782,
54.9925871509516));
#65844=CARTESIAN_POINT('Ctrl Pts',(-1.88811998897897,-5.05057847782898,
55.1513479131975));
#65845=CARTESIAN_POINT('Ctrl Pts',(3.21905622559384,-4.32562331577277,55.3101086754434));
#65846=CARTESIAN_POINT('Ctrl Pts',(5.38005385515049,0.358274432763269,55.4688694376893));
#65847=CARTESIAN_POINT('Ctrl Pts',(2.61706186058861,4.71426847679935,55.6276301999351));
#65848=CARTESIAN_POINT('Ctrl Pts',(-2.54114508797937,4.75562001166302,55.7863909621812));
#65849=CARTESIAN_POINT('Ctrl Pts',(-5.37361843174121,0.444482849548049,
55.9451517244269));
#65850=CARTESIAN_POINT('Ctrl Pts',(-3.28799204746135,-4.27345859337873,
56.1039124866729));
#65851=CARTESIAN_POINT('Ctrl Pts',(1.80690509167997,-5.08020019715291,56.2626732489186));
#65852=CARTESIAN_POINT('Ctrl Pts',(5.24806749828111,-1.23738740375719,56.4214340111647));
#65853=CARTESIAN_POINT('Ctrl Pts',(3.88603822614634,3.73792013804749,56.5801947734104));
#65854=CARTESIAN_POINT('Ctrl Pts',(-1.03261193114073,5.2921689932538,56.7389555356565));
#65855=CARTESIAN_POINT('Ctrl Pts',(-5.00618410750568,2.00286313442759,56.8977162979023));
#65856=CARTESIAN_POINT('Ctrl Pts',(-4.3979436727968,-3.11952424327782,57.0564770601482));
#65857=CARTESIAN_POINT('Ctrl Pts',(0.235429148194338,-5.38682774642662,
57.2152378223941));
#65858=CARTESIAN_POINT('Ctrl Pts',(4.65333002148106,-2.72394195324985,57.37399858464));
#65859=CARTESIAN_POINT('Ctrl Pts',(4.81236112129208,2.43197871943155,57.5327593468858));
#65860=CARTESIAN_POINT('Ctrl Pts',(0.566972327412124,5.36207818233195,57.6915201091318));
#65861=CARTESIAN_POINT('Ctrl Pts',(-4.19732685891063,3.38463990595143,57.8502808713776));
#65862=CARTESIAN_POINT('Ctrl Pts',(-5.12010429494008,-1.6905241975279,58.0090416336235));
#65863=CARTESIAN_POINT('Ctrl Pts',(-1.35680588461835,-5.21846891769574,
58.1678023958695));
#65864=CARTESIAN_POINT('Ctrl Pts',(3.64828271548151,-3.97031148417985,58.3265631581153));
#65865=CARTESIAN_POINT('Ctrl Pts',(5.31435153612611,0.911596294400786,58.4853239203612));
#65866=CARTESIAN_POINT('Ctrl Pts',(2.11656350192684,4.95918329927446,58.6440846826071));
#65867=CARTESIAN_POINT('Ctrl Pts',(-3.01836810050987,4.46797426842589,58.8028454448529));
#65868=CARTESIAN_POINT('Ctrl Pts',(-5.39079702010585,-0.112461288937121,
58.9616062070989));
#65869=CARTESIAN_POINT('Ctrl Pts',(-2.8294038428619,-4.58996883949007,59.1203669693448));
#65870=CARTESIAN_POINT('Ctrl Pts',(2.32154615663493,-4.86659670571795,59.2791277315906));
#65871=CARTESIAN_POINT('Ctrl Pts',(5.34774620102881,-0.689166614740877,
59.4378884938366));
#65872=CARTESIAN_POINT('Ctrl Pts',(3.47952557320649,4.11900981291542,59.5966492560824));
#65873=CARTESIAN_POINT('Ctrl Pts',(-1.5732631427069,5.15734264299855,59.7554100183284));
#65874=CARTESIAN_POINT('Ctrl Pts',(-5.18615337446655,1.47551795312722,59.9141707805741));
#65875=CARTESIAN_POINT('Ctrl Pts',(-4.05251762479693,-3.55674583772888,
60.0729315428202));
#65876=CARTESIAN_POINT('Ctrl Pts',(0.790106040849496,-5.33376719567931,
60.2316923050659));
#65877=CARTESIAN_POINT('Ctrl Pts',(4.90960052380718,-2.22916189410365,60.3904530673119));
#65878=CARTESIAN_POINT('Ctrl Pts',(4.53567864167587,2.91564046359228,60.5492138295578));
#65879=CARTESIAN_POINT('Ctrl Pts',(0.0105651225747838,5.39195960961101,
60.7079745918036));
#65880=CARTESIAN_POINT('Ctrl Pts',(-4.52421791942263,2.93339262136295,60.8667353540496));
#65881=CARTESIAN_POINT('Ctrl Pts',(-4.91829852752871,-2.20990489560075,
61.0254961162954));
#65882=CARTESIAN_POINT('Ctrl Pts',(-0.811002091855911,-5.3306299496867,
61.1842568785414));
#65883=CARTESIAN_POINT('Ctrl Pts',(4.03854823066489,-3.57259964760746,61.3430176407872));
#65884=CARTESIAN_POINT('Ctrl Pts',(5.19189585341926,1.4551829784393,61.5017784030331));
#65885=CARTESIAN_POINT('Ctrl Pts',(1.5934618026005,5.15113769347555,61.660539165279));
#65886=CARTESIAN_POINT('Ctrl Pts',(-3.4633571628827,4.1326138478934,61.8192999275249));
#65887=CARTESIAN_POINT('Ctrl Pts',(-5.35040586327371,-0.668204423614378,
61.9780606897707));
#65888=CARTESIAN_POINT('Ctrl Pts',(-2.34059968732153,-4.85746159606041,
62.1368214520167));
#65889=CARTESIAN_POINT('Ctrl Pts',(2.81139481701569,-4.60102154269558,62.2955822142625));
#65890=CARTESIAN_POINT('Ctrl Pts',(5.39031490964729,-0.133586033422769,
62.4543429765085));
#65891=CARTESIAN_POINT('Ctrl Pts',(3.03585414765692,4.45611149407704,62.6131037387543));
#65892=CARTESIAN_POINT('Ctrl Pts',(-2.09711306164141,4.96743966849971,62.7718645010003));
#65893=CARTESIAN_POINT('Ctrl Pts',(-5.310738339773,0.932415325891086,62.930625263246));
#65894=CARTESIAN_POINT('Ctrl Pts',(-3.66381367072956,-3.95598400396999,
63.089386025492));
#65895=CARTESIAN_POINT('Ctrl Pts',(1.33634518241131,-5.223745936293,63.2481467877379));
#65896=CARTESIAN_POINT('Ctrl Pts',(5.11344010541426,-1.71057602632341,63.4069075499838));
#65897=CARTESIAN_POINT('Ctrl Pts',(4.21055845188033,3.36816531316245,63.5656683122297));
#65898=CARTESIAN_POINT('Ctrl Pts',(-0.545954909997053,5.36425887609291,
63.7244290744756));
#65899=CARTESIAN_POINT('Ctrl Pts',(-4.80279366183524,2.45081886220229,63.8831898367214));
#65900=CARTESIAN_POINT('Ctrl Pts',(-4.66396895111927,-2.70568543561274,
64.0419505989674));
#65901=CARTESIAN_POINT('Ctrl Pts',(-0.256537393552353,-5.38586377651727,
64.2007113612132));
#65902=CARTESIAN_POINT('Ctrl Pts',(4.38568502263036,-3.13673507580205,64.3594721234591));
#65903=CARTESIAN_POINT('Ctrl Pts',(5.01399454360851,1.98322937910761,64.5182328857051));
#65904=CARTESIAN_POINT('Ctrl Pts',(1.05334310381863,5.28808172772786,64.6769936479507));
#65905=CARTESIAN_POINT('Ctrl Pts',(-3.87136011937014,3.75312015257198,64.8357544101969));
#65906=CARTESIAN_POINT('Ctrl Pts',(-5.25287630907674,-1.21681162676554,
64.9945151724425));
#65907=CARTESIAN_POINT('Ctrl Pts',(-1.82679964952023,-5.07308023729216,
65.1532759346887));
#65908=CARTESIAN_POINT('Ctrl Pts',(3.27121984959904,-4.28631085539543,65.3120366969344));
#65909=CARTESIAN_POINT('Ctrl Pts',(5.3753190216539,0.423421148429019,65.4707974591804));
#65910=CARTESIAN_POINT('Ctrl Pts',(2.55976203383379,4.7456251836438,65.6295582214262));
#65911=CARTESIAN_POINT('Ctrl Pts',(-2.59856735630046,4.7244880937792,65.7883189836722));
#65912=CARTESIAN_POINT('Ctrl Pts',(-5.37860852767513,0.379355189119878,
65.947079745918));
#65913=CARTESIAN_POINT('Ctrl Pts',(-3.23598288278473,-4.31297517217702,
66.1058405081639));
#65914=CARTESIAN_POINT('Ctrl Pts',(1.86831314081432,-5.05793891435551,66.2646012704098));
#65915=CARTESIAN_POINT('Ctrl Pts',(5.26267190957225,-1.17372246536004,66.4233620326557));
#65916=CARTESIAN_POINT('Ctrl Pts',(3.84047259628301,3.78472063575253,66.5821227949015));
#65917=CARTESIAN_POINT('Ctrl Pts',(-1.09664454588739,5.27927180522719,66.7408835571475));
#65918=CARTESIAN_POINT('Ctrl Pts',(-5.03007910221774,1.94207216110101,66.8996443193933));
#65919=CARTESIAN_POINT('Ctrl Pts',(-4.35983161843177,-3.17257124623133,
67.0584050816393));
#65920=CARTESIAN_POINT('Ctrl Pts',(0.300666935333765,-5.38358054156236,
67.2171658438851));
#65921=CARTESIAN_POINT('Ctrl Pts',(4.68598592589077,-2.66737248164657,67.375926606131));
#65922=CARTESIAN_POINT('Ctrl Pts',(4.78254746176859,2.49009634942548,67.534687368377));
#65923=CARTESIAN_POINT('Ctrl Pts',(0.50197547582154,5.3685529405199,67.6934481306227));
#65924=CARTESIAN_POINT('Ctrl Pts',(-4.23801979863793,3.33354589586587,67.8522088928688));
#65925=CARTESIAN_POINT('Ctrl Pts',(-5.09924990138375,-1.75242417716988,
68.0109696551145));
#65926=CARTESIAN_POINT('Ctrl Pts',(-1.29349073576672,-5.2345221147663,68.1697304173606));
#65927=CARTESIAN_POINT('Ctrl Pts',(3.69611066141296,-3.92582552236859,68.3284911796063));
#65928=CARTESIAN_POINT('Ctrl Pts',(5.30291868209728,0.975906504002708,68.4872519418522));
#65929=CARTESIAN_POINT('Ctrl Pts',(2.05633354516605,4.98445908845845,68.6460127040982));
#65930=CARTESIAN_POINT('Ctrl Pts',(-3.07227086382722,4.43108246287181,68.804773466344));
#65931=CARTESIAN_POINT('Ctrl Pts',(-5.38903913451035,-0.177756181911403,
68.96353422859));
#65932=CARTESIAN_POINT('Ctrl Pts',(-2.77359417894579,-4.62390693937597,
69.1222949908358));
#65933=CARTESIAN_POINT('Ctrl Pts',(2.38032888972716,-4.83811682684714,69.2810557530817));
#65934=CARTESIAN_POINT('Ctrl Pts',(5.35570225042921,-0.624334412185203,
69.4398165153275));
#65935=CARTESIAN_POINT('Ctrl Pts',(3.42937331948324,4.16085792705156,69.5985772775736));
#65936=CARTESIAN_POINT('Ctrl Pts',(-1.63562282502583,5.13790599639058,69.7573380398193));
#65937=CARTESIAN_POINT('Ctrl Pts',(-5.20364699932156,1.4125855584507,69.9160988020653));
#65938=CARTESIAN_POINT('Ctrl Pts',(-4.00913449237088,-3.60557633057093,
70.0748595643111));
#65939=CARTESIAN_POINT('Ctrl Pts',(0.854660362605124,-5.32380462809097,
70.233620326557));
#65940=CARTESIAN_POINT('Ctrl Pts',(4.93624394778424,-2.1695243122525,70.392381088803));
#65941=CARTESIAN_POINT('Ctrl Pts',(4.50002629241666,2.97037092314251,70.5511418510488));
#65942=CARTESIAN_POINT('Ctrl Pts',(-0.0547528808636342,5.39169195851627,
70.7099026132947));
#65943=CARTESIAN_POINT('Ctrl Pts',(-4.55942054512895,2.87837182208054,70.8686633755406));
#65944=CARTESIAN_POINT('Ctrl Pts',(-4.89116725717831,-2.26932212693528,
71.0274241377865));
#65945=CARTESIAN_POINT('Ctrl Pts',(-0.746368292808977,-5.34006314803305,
71.1861849000323));
#65946=CARTESIAN_POINT('Ctrl Pts',(4.08152973125557,-3.52341526169831,71.3449456622782));
#65947=CARTESIAN_POINT('Ctrl Pts',(5.17388707332602,1.51796989626334,71.5037064245242));
#65948=CARTESIAN_POINT('Ctrl Pts',(1.53094492744998,5.1700626381705,71.66246718677));
#65949=CARTESIAN_POINT('Ctrl Pts',(-3.51316477934987,4.09035613200449,71.8212279490159));
#65950=CARTESIAN_POINT('Ctrl Pts',(-5.34191876907334,-0.732969247726808,
71.9799887112618));
#65951=CARTESIAN_POINT('Ctrl Pts',(-2.28158553030752,-4.88545878310146,
72.1387494735077));
#65952=CARTESIAN_POINT('Ctrl Pts',(2.86692447773331,-4.56662721189998,72.2975102357536));
#65953=CARTESIAN_POINT('Ctrl Pts',(5.39153763240408,-0.0682789269231456,
72.4562709979995));
#65954=CARTESIAN_POINT('Ctrl Pts',(2.98165085923738,4.49256031758063,72.6150317602455));
#65955=CARTESIAN_POINT('Ctrl Pts',(-2.15713385601469,4.94167113239301,72.7737925224911));
#65956=CARTESIAN_POINT('Ctrl Pts',(-5.32164377573057,0.868013581529248,
72.9325532847373));
#65957=CARTESIAN_POINT('Ctrl Pts',(-3.61562276017225,-4.00007651297025,
73.091314046983));
#65958=CARTESIAN_POINT('Ctrl Pts',(1.39952664613108,-5.20717439887132,73.250074809229));
#65959=CARTESIAN_POINT('Ctrl Pts',(5.13378651679711,-1.64850721971224,73.4088355714748));
#65960=CARTESIAN_POINT('Ctrl Pts',(4.16944815373948,3.41892412123604,73.5675963337207));
#65961=CARTESIAN_POINT('Ctrl Pts',(-0.610896517072584,5.35725167403211,
73.7263570959665));
#65962=CARTESIAN_POINT('Ctrl Pts',(-4.83213003538284,2.39245885537094,73.8851178582126));
#65963=CARTESIAN_POINT('Ctrl Pts',(-4.63085054597687,-2.76198538633308,
74.0438786204583));
#65964=CARTESIAN_POINT('Ctrl Pts',(-0.191275185721079,-5.38857623652284,
74.2026393827044));
#65965=CARTESIAN_POINT('Ctrl Pts',(4.42336106708315,-3.08337751884262,74.3614001449501));
#65966=CARTESIAN_POINT('Ctrl Pts',(4.98960215796993,2.04382248707493,74.5201609071961));
#65967=CARTESIAN_POINT('Ctrl Pts',(0.989206944500219,5.30045372345089,74.678921669442));
#65968=CARTESIAN_POINT('Ctrl Pts',(-3.9165406802957,3.70594780765739,74.8376824316877));
#65969=CARTESIAN_POINT('Ctrl Pts',(-5.23775064219211,-1.2803547413539,74.9964431939339));
#65970=CARTESIAN_POINT('Ctrl Pts',(-1.76521122717783,-5.09483752213321,
75.1552039561795));
#65971=CARTESIAN_POINT('Ctrl Pts',(3.32290342202856,-4.24636937881787,75.3139647184255));
#65972=CARTESIAN_POINT('Ctrl Pts',(5.36979535998785,0.488505727033064,75.4727254806714));
#65973=CARTESIAN_POINT('Ctrl Pts',(2.50208656195135,4.77628546990172,75.6314862429173));
#65974=CARTESIAN_POINT('Ctrl Pts',(-2.65560828481232,4.69266285717694,75.7902470051632));
#65975=CARTESIAN_POINT('Ctrl Pts',(-5.38280931270438,0.314171858310403,
75.9490077674091));
#65976=CARTESIAN_POINT('Ctrl Pts',(-3.18349883755812,-4.35185882178607,
76.107768529655));
#65977=CARTESIAN_POINT('Ctrl Pts',(1.92944701495941,-5.03493537892548,76.2665292919008));
#65978=CARTESIAN_POINT('Ctrl Pts',(5.27650402365974,-1.10988528316864,76.4252900541468));
#65979=CARTESIAN_POINT('Ctrl Pts',(3.7943433769926,3.83096572563162,76.5840508163925));
#65980=CARTESIAN_POINT('Ctrl Pts',(-1.16051622802576,5.26559988396195,76.7428115786386));
#65981=CARTESIAN_POINT('Ctrl Pts',(-5.0532359327251,1.88099618864767,76.9015723408843));
#65982=CARTESIAN_POINT('Ctrl Pts',(-4.32107975869319,-3.22515267429361,
77.0603331031303));
#65983=CARTESIAN_POINT('Ctrl Pts',(0.365860599594574,-5.37954329615034,
77.2190938653761));
#65984=CARTESIAN_POINT('Ctrl Pts',(4.7179541617759,-2.61041157308061,77.3778546276221));
#65985=CARTESIAN_POINT('Ctrl Pts',(4.75203196331349,2.54784855773221,77.5366153898679));
#65986=CARTESIAN_POINT('Ctrl Pts',(0.436904959320356,5.37423986346092,77.6953761521139));
#65987=CARTESIAN_POINT('Ctrl Pts',(-4.27809080887851,3.28196268785622,77.8541369143598));
#65988=CARTESIAN_POINT('Ctrl Pts',(-5.07764719280662,-1.81406698853016,
78.0128976766055));
#65989=CARTESIAN_POINT('Ctrl Pts',(-1.22998576712498,-5.24980714561609,
78.1716584388517));
#65990=CARTESIAN_POINT('Ctrl Pts',(3.74339620303386,-3.88076344558682,78.3304192010973));
#65991=CARTESIAN_POINT('Ctrl Pts',(5.29070762465021,1.0400734993063,78.4891799633433));
#65992=CARTESIAN_POINT('Ctrl Pts',(1.99580182141817,5.00900340817564,78.6479407255891));
#65993=CARTESIAN_POINT('Ctrl Pts',(-3.12572277133616,4.39354039588141,78.8067014878351));
#65994=CARTESIAN_POINT('Ctrl Pts',(-5.38649040731852,-0.243024989162281,
78.965462250081));
#65995=CARTESIAN_POINT('Ctrl Pts',(-2.71737749003105,-4.65716648082978,
79.1242230123268));
#65996=CARTESIAN_POINT('Ctrl Pts',(2.43876230950906,-4.8089269542393,79.2829837745728));
#65997=CARTESIAN_POINT('Ctrl Pts',(5.36287235042167,-0.559410588542699,
79.4417445368186));
#65998=CARTESIAN_POINT('Ctrl Pts',(3.37871780515969,4.20209543520715,79.6005052990646));
#65999=CARTESIAN_POINT('Ctrl Pts',(-1.69774247966381,5.11771536197905,79.7592660613104));
#66000=CARTESIAN_POINT('Ctrl Pts',(-5.2203769888794,1.34944586681667,79.9180268235563));
#66001=CARTESIAN_POINT('Ctrl Pts',(-3.96516301938171,-3.65387770501744,
80.0767875858022));
#66002=CARTESIAN_POINT('Ctrl Pts',(0.91908926293675,-5.31306079207099,80.235548348048));
#66003=CARTESIAN_POINT('Ctrl Pts',(4.96216297786599,-2.10956835266785,80.3943091102941));
#66004=CARTESIAN_POINT('Ctrl Pts',(4.46371356421533,3.02466548070436,80.5530698725397));
#66005=CARTESIAN_POINT('Ctrl Pts',(-0.120062849320441,5.39063307652007,
80.7118306347859));
#66006=CARTESIAN_POINT('Ctrl Pts',(-4.59395407577343,2.82292862168424,80.8705913970315));
#66007=CARTESIAN_POINT('Ctrl Pts',(-4.86331820795707,-2.32840633521552,
81.0293521592777));
#66008=CARTESIAN_POINT('Ctrl Pts',(-0.681624964166643,-5.34871269198804,
81.1881129215234));
#66009=CARTESIAN_POINT('Ctrl Pts',(4.12391226721417,-3.47371381457424,81.3468736837694));
#66010=CARTESIAN_POINT('Ctrl Pts',(5.15511902533117,1.58053405205645,81.5056344460152));
#66011=CARTESIAN_POINT('Ctrl Pts',(1.46820338586184,5.18822887591951,81.6643952082611));
#66012=CARTESIAN_POINT('Ctrl Pts',(-3.56245683835765,4.04749815657105,81.823155970507));
#66013=CARTESIAN_POINT('Ctrl Pts',(-5.33264774907332,-0.797626509155247,
81.9819167327528));
#66014=CARTESIAN_POINT('Ctrl Pts',(-2.22223654888384,-4.91273902788576,
82.1406774949988));
#66015=CARTESIAN_POINT('Ctrl Pts',(2.92203341399256,-4.53156273055457,82.2994382572446));
#66016=CARTESIAN_POINT('Ctrl Pts',(5.39196915310808,-0.0029617965042665,
82.4581990194906));
#66017=CARTESIAN_POINT('Ctrl Pts',(2.92701000162586,4.52834985013744,82.6169597817364));
#66018=CARTESIAN_POINT('Ctrl Pts',(-2.21683806821556,4.91517742057454,82.7757205439824));
#66019=CARTESIAN_POINT('Ctrl Pts',(-5.33176830391211,0.803484428152502,
82.9344813062282));
#66020=CARTESIAN_POINT('Ctrl Pts',(-3.56690117349271,-4.04358195702611,
83.0932420684741));
#66021=CARTESIAN_POINT('Ctrl Pts',(1.46250256952503,-5.18983881124397,83.2520028307201));
#66022=CARTESIAN_POINT('Ctrl Pts',(5.15337985091046,-1.58619629785924,83.4107635929658));
#66023=CARTESIAN_POINT('Ctrl Pts',(4.12772540290961,3.46918082523772,83.5695243552118));
#66024=CARTESIAN_POINT('Ctrl Pts',(-0.675747352509778,5.34945901705833,
83.7282851174576));
#66025=CARTESIAN_POINT('Ctrl Pts',(-4.86075944383677,2.33374637252957,83.8870458797035));
#66026=CARTESIAN_POINT('Ctrl Pts',(-4.59704844530487,-2.81787736745293,
84.0458066419496));
#66027=CARTESIAN_POINT('Ctrl Pts',(-0.125992795831606,-5.39050299503273,
84.2045674041953));
#66028=CARTESIAN_POINT('Ctrl Pts',(4.46040309055735,-3.02955776127604,84.3633281664412));
#66029=CARTESIAN_POINT('Ctrl Pts',(4.96444861251837,2.10409705678322,84.5220889286871));
#66030=CARTESIAN_POINT('Ctrl Pts',(0.924981040394022,5.31208351664113,84.6808496909329));
#66031=CARTESIAN_POINT('Ctrl Pts',(-3.96125263942776,3.65816335371309,84.8396104531789));
#66032=CARTESIAN_POINT('Ctrl Pts',(-5.22165301904991,-1.3435792187099,84.9983712154247));
#66033=CARTESIAN_POINT('Ctrl Pts',(-1.70375320028204,-5.11609758128303,
85.1571319776708));
#66034=CARTESIAN_POINT('Ctrl Pts',(3.37484546343723,-4.20532487574203,85.3158927399164));
#66035=CARTESIAN_POINT('Ctrl Pts',(5.36205285859353,0.552597767150946,85.4746535021625));
#66036=CARTESIAN_POINT('Ctrl Pts',(2.4468005092104,4.80802425479881,85.6334142644084));
#66037=CARTESIAN_POINT('Ctrl Pts',(-2.7176845769921,4.65659903150035,85.7921750266542));
#66038=CARTESIAN_POINT('Ctrl Pts',(-4.93173550418608,0.99029557446776,85.9244756618591));
#66039=CARTESIAN_POINT('Ctrl Pts',(-4.26716318148111,-2.08115166207624,
86.0303161700231));
#66040=CARTESIAN_POINT('Ctrl Pts',(-3.26619649360748,-3.2739962098191,86.083236424105));
#66041=CARTESIAN_POINT('Ctrl Pts',(-2.64867169498456,-3.71434815979703,
86.109696551146));
#66042=CARTESIAN_POINT('Ctrl Pts',(-2.08577545033697,4.2697827545171,25.890303448854));
#66043=CARTESIAN_POINT('Ctrl Pts',(-2.79564340622372,3.92301449006545,25.9167635758949));
#66044=CARTESIAN_POINT('Ctrl Pts',(-4.02828411678504,2.86869268329956,25.9696838299769));
#66045=CARTESIAN_POINT('Ctrl Pts',(-5.2368061558258,-0.173451583736938,
26.0755243381408));
#66046=CARTESIAN_POINT('Ctrl Pts',(-3.58937700474797,-4.31948327041665,
26.2078249733457));
#66047=CARTESIAN_POINT('Ctrl Pts',(1.69117135154962,-5.35897536965486,26.3665857355916));
#66048=CARTESIAN_POINT('Ctrl Pts',(5.4148867130437,-1.48550731689914,26.5253464978375));
#66049=CARTESIAN_POINT('Ctrl Pts',(4.18736849490951,3.74332949976516,26.6841072600834));
#66050=CARTESIAN_POINT('Ctrl Pts',(-0.874969621673782,5.54834523009075,
26.8428680223293));
#66051=CARTESIAN_POINT('Ctrl Pts',(-5.13525022907948,2.27420458855161,27.0016287845751));
#66052=CARTESIAN_POINT('Ctrl Pts',(-4.6962499784134,-3.08076179886732,27.1603895468211));
#66053=CARTESIAN_POINT('Ctrl Pts',(0.0412447165789918,-5.61643191744809,
27.319150309067));
#66054=CARTESIAN_POINT('Ctrl Pts',(4.7408118992853,-3.01160959987317,27.4779110713129));
#66055=CARTESIAN_POINT('Ctrl Pts',(5.1015367238218,2.34944503074463,27.6366718335587));
#66056=CARTESIAN_POINT('Ctrl Pts',(0.793130492629709,5.56026007017329,27.7954325958046));
#66057=CARTESIAN_POINT('Ctrl Pts',(-4.24114750411255,3.68213214181093,27.9541933580505));
#66058=CARTESIAN_POINT('Ctrl Pts',(-5.39381106478857,-1.56598352850948,
28.1129541202964));
#66059=CARTESIAN_POINT('Ctrl Pts',(-1.60988703512753,-5.3808695398533,28.2717148825423));
#66060=CARTESIAN_POINT('Ctrl Pts',(3.6474511562916,-4.2710160983281,28.4304756447882));
#66061=CARTESIAN_POINT('Ctrl Pts',(5.5665325305163,0.747800018975952,28.5892364070341));
#66062=CARTESIAN_POINT('Ctrl Pts',(2.39095231205807,5.08220761366869,28.74799716928));
#66063=CARTESIAN_POINT('Ctrl Pts',(-2.97289997872796,4.76522309415968,28.9067579315259));
#66064=CARTESIAN_POINT('Ctrl Pts',(-5.61586367010893,0.0869610876472672,
29.0655186937718));
#66065=CARTESIAN_POINT('Ctrl Pts',(-3.11901725108991,-4.67089049014597,
29.2242794560176));
#66066=CARTESIAN_POINT('Ctrl Pts',(2.23244895427517,-5.15380035052699,29.3830402182635));
#66067=CARTESIAN_POINT('Ctrl Pts',(5.54070972400729,-0.91979474000819,29.5418009805094));
#66068=CARTESIAN_POINT('Ctrl Pts',(3.77794369111745,4.15603513022305,29.7005617427553));
#66069=CARTESIAN_POINT('Ctrl Pts',(-1.44251179621886,5.42813469204637,29.8593225050012));
#66070=CARTESIAN_POINT('Ctrl Pts',(-5.34273643101869,1.73223958412626,30.0180832672471));
#66071=CARTESIAN_POINT('Ctrl Pts',(-4.35312548529055,-3.54905410571791,
30.176844029493));
#66072=CARTESIAN_POINT('Ctrl Pts',(0.620598871036556,-5.58214506939038,
30.3356047917389));
#66073=CARTESIAN_POINT('Ctrl Pts',(5.02633218492865,-2.50628635742007,30.4943655539847));
#66074=CARTESIAN_POINT('Ctrl Pts',(4.83181275145273,2.86340218474256,30.6531263162307));
#66075=CARTESIAN_POINT('Ctrl Pts',(0.215070698416827,5.61241758347815,30.8118870784765));
#66076=CARTESIAN_POINT('Ctrl Pts',(-4.59851062734073,3.22477697638755,30.9706478407224));
#66077=CARTESIAN_POINT('Ctrl Pts',(-5.2033945635623,-2.11427802164059,31.1294086029683));
#66078=CARTESIAN_POINT('Ctrl Pts',(-1.04597285548533,-5.51828119277288,
31.2881693652142));
#66079=CARTESIAN_POINT('Ctrl Pts',(4.06875515960443,-3.87178485819991,31.4469301274601));
#66080=CARTESIAN_POINT('Ctrl Pts',(5.4596341708714,1.31828724381346,31.605690889706));
#66081=CARTESIAN_POINT('Ctrl Pts',(1.853689222264,5.30182259267667,31.7644516519519));
#66082=CARTESIAN_POINT('Ctrl Pts',(-3.4488087242362,4.43296795844451,31.9232124141977));
#66083=CARTESIAN_POINT('Ctrl Pts',(-5.59485158108012,-0.493074358126545,
32.0819731764437));
#66084=CARTESIAN_POINT('Ctrl Pts',(-2.62031537395337,-4.96783996098723,
32.2407339386895));
#66085=CARTESIAN_POINT('Ctrl Pts',(2.75241350199106,-4.89588668690527,32.3994947009355));
#66086=CARTESIAN_POINT('Ctrl Pts',(5.60604946734801,-0.343068370161422,
32.5582554631813));
#66087=CARTESIAN_POINT('Ctrl Pts',(3.3288577211775,4.52373659811392,32.7170162254272));
#66088=CARTESIAN_POINT('Ctrl Pts',(-1.99500629269775,5.25027965246184,32.8757769876731));
#66089=CARTESIAN_POINT('Ctrl Pts',(-5.49297960923532,1.17160639699654,33.034537749919));
#66090=CARTESIAN_POINT('Ctrl Pts',(-3.96361020215392,-3.97935682018335,
33.1932985121649));
#66091=CARTESIAN_POINT('Ctrl Pts',(1.19337633198882,-5.48829112449471,33.3520592744107));
#66092=CARTESIAN_POINT('Ctrl Pts',(5.25814839494067,-1.97417374963327,33.5108200366567));
#66093=CARTESIAN_POINT('Ctrl Pts',(4.51050243460883,3.34676774281486,33.6695807989025));
#66094=CARTESIAN_POINT('Ctrl Pts',(-0.365293128967798,5.60464516868708,
33.8283415611484));
#66095=CARTESIAN_POINT('Ctrl Pts',(-4.9067612628892,2.73298014006108,33.9871023233943));
#66096=CARTESIAN_POINT('Ctrl Pts',(-4.95741161004009,-2.63999179271414,
34.1458630856402));
#66097=CARTESIAN_POINT('Ctrl Pts',(-0.470887425572999,-5.59676259719809,
34.3046238478861));
#66098=CARTESIAN_POINT('Ctrl Pts',(4.4466073142222,-3.43120531738688,34.463384610132));
#66099=CARTESIAN_POINT('Ctrl Pts',(5.29443121665232,1.87469587642792,34.6221453723779));
#66100=CARTESIAN_POINT('Ctrl Pts',(1.296629949095,5.4648181408047,34.7809061346238));
#66101=CARTESIAN_POINT('Ctrl Pts',(-3.88788665395154,4.05337191767345,34.9396668968696));
#66102=CARTESIAN_POINT('Ctrl Pts',(-5.51409063425751,-1.06784409636987,
35.0984276591156));
#66103=CARTESIAN_POINT('Ctrl Pts',(-2.09363043599948,-5.21173657569289,
35.2571884213614));
#66104=CARTESIAN_POINT('Ctrl Pts',(3.2429842880596,-4.58568854637521,35.4159491836074));
#66105=CARTESIAN_POINT('Ctrl Pts',(5.61152073344166,0.237321712265504,35.5747099458532));
#66106=CARTESIAN_POINT('Ctrl Pts',(2.8442219974453,4.84312789075476,35.7334707080991));
#66107=CARTESIAN_POINT('Ctrl Pts',(-2.52619558850515,5.01635548835761,35.892231470345));
#66108=CARTESIAN_POINT('Ctrl Pts',(-5.58456180820669,0.598461316442061,
36.0509922325909));
#66109=CARTESIAN_POINT('Ctrl Pts',(-3.53176647837594,-4.36716293252018,
36.2097529948368));
#66110=CARTESIAN_POINT('Ctrl Pts',(1.7534094116762,-5.33582626891128,36.3685137570827));
#66111=CARTESIAN_POINT('Ctrl Pts',(5.43381144957445,-1.4209784190592,36.5272745193285));
#66112=CARTESIAN_POINT('Ctrl Pts',(4.14102327089027,3.79439228426682,36.6860352815745));
#66113=CARTESIAN_POINT('Ctrl Pts',(-0.941755894515449,5.5370192678104,36.8447960438203));
#66114=CARTESIAN_POINT('Ctrl Pts',(-5.16261129895229,2.2119970869982,37.0035568060662));
#66115=CARTESIAN_POINT('Ctrl Pts',(-4.65848714857258,-3.13751239416556,
37.1623175683121));
#66116=CARTESIAN_POINT('Ctrl Pts',(0.109226735523501,-5.61547469562505,
37.321078330558));
#66117=CARTESIAN_POINT('Ctrl Pts',(4.77697297489437,-2.95398302874052,37.4798390928039));
#66118=CARTESIAN_POINT('Ctrl Pts',(5.07268763310252,2.4110841366338,37.6385998550498));
#66119=CARTESIAN_POINT('Ctrl Pts',(0.725723622233936,5.56945345263699,37.7973606172957));
#66120=CARTESIAN_POINT('Ctrl Pts',(-4.2854448152198,3.63048884761598,37.9561213795416));
#66121=CARTESIAN_POINT('Ctrl Pts',(-5.37444325716809,-1.63121004546892,
38.1148821417874));
#66122=CARTESIAN_POINT('Ctrl Pts',(-1.54458706564933,-5.39997567898108,
38.2736429040334));
#66123=CARTESIAN_POINT('Ctrl Pts',(3.69892238837796,-4.22651862668493,38.4324036662792));
#66124=CARTESIAN_POINT('Ctrl Pts',(5.55706508750621,0.815177373445694,38.5911644285252));
#66125=CARTESIAN_POINT('Ctrl Pts',(2.32921207578554,5.11079814148172,38.749925190771));
#66126=CARTESIAN_POINT('Ctrl Pts',(-3.0304069744033,4.7288603390718,38.908685953017));
#66127=CARTESIAN_POINT('Ctrl Pts',(-5.61650499663195,0.0189251094235045,
39.0674467152627));
#66128=CARTESIAN_POINT('Ctrl Pts',(-3.0622060875641,-4.70833095844415,39.2262074775087));
#66129=CARTESIAN_POINT('Ctrl Pts',(2.29471736914525,-5.126378715302,39.3849682397545));
#66130=CARTESIAN_POINT('Ctrl Pts',(5.55144539655818,-0.852608084638733,
39.5437290020005));
#66131=CARTESIAN_POINT('Ctrl Pts',(3.72732102593349,4.20149550833897,39.7024897642464));
#66132=CARTESIAN_POINT('Ctrl Pts',(-1.50816140012871,5.41026207573349,39.8612505264922));
#66133=CARTESIAN_POINT('Ctrl Pts',(-5.3633284454033,1.66739153280986,40.0200112887382));
#66134=CARTESIAN_POINT('Ctrl Pts',(-4.30981347244434,-3.60152667207889,
40.178772050984));
#66135=CARTESIAN_POINT('Ctrl Pts',(0.688174435462339,-5.57421765661644,
40.3375328132299));
#66136=CARTESIAN_POINT('Ctrl Pts',(5.05632407947203,-2.4452143751233,40.4962935754758));
#66137=CARTESIAN_POINT('Ctrl Pts',(4.79677147851891,2.92172379252827,40.6550543377217));
#66138=CARTESIAN_POINT('Ctrl Pts',(0.147067101132706,5.61461110004271,40.8138150999676));
#66139=CARTESIAN_POINT('Ctrl Pts',(-4.63723757943327,3.16883482826894,40.9725758622135));
#66140=CARTESIAN_POINT('Ctrl Pts',(-5.1774007810357,-2.17715587165673,41.1313366244594));
#66141=CARTESIAN_POINT('Ctrl Pts',(-0.979048642068222,-5.53054701575012,
41.2900973867053));
#66142=CARTESIAN_POINT('Ctrl Pts',(4.11535871955024,-3.82221259827082,41.4488581489512));
#66143=CARTESIAN_POINT('Ctrl Pts',(5.44326407576748,1.38432754014994,41.607618911197));
#66144=CARTESIAN_POINT('Ctrl Pts',(1.7893278831762,5.32388882899019,41.7663796734429));
#66145=CARTESIAN_POINT('Ctrl Pts',(-3.50225584382976,4.39086444123689,41.9251404356888));
#66146=CARTESIAN_POINT('Ctrl Pts',(-5.58846804476507,-0.560813203837097,
42.0839011979347));
#66147=CARTESIAN_POINT('Ctrl Pts',(-2.55994358915231,-4.99921747449702,
42.2426619601806));
#66148=CARTESIAN_POINT('Ctrl Pts',(2.81151943374774,-4.86218520941121,42.4014227224265));
#66149=CARTESIAN_POINT('Ctrl Pts',(5.60979399190252,-0.275132523291236,
42.5601834846724));
#66150=CARTESIAN_POINT('Ctrl Pts',(3.27381373527952,4.56372985217721,42.7189442469183));
#66151=CARTESIAN_POINT('Ctrl Pts',(-2.05846085181392,5.22572726598967,42.8777050091642));
#66152=CARTESIAN_POINT('Ctrl Pts',(-5.50676919082185,1.10497946405063,43.03646577141));
#66153=CARTESIAN_POINT('Ctrl Pts',(-3.91511415993451,-4.02707929542473,
43.1952265336559));
#66154=CARTESIAN_POINT('Ctrl Pts',(1.25977293884402,-5.47343207498865,43.3539872959018));
#66155=CARTESIAN_POINT('Ctrl Pts',(5.28167736372706,-1.91033263136333,43.5127480581477));
#66156=CARTESIAN_POINT('Ctrl Pts',(4.46962933439137,3.40116158835573,43.6715088203935));
#66157=CARTESIAN_POINT('Ctrl Pts',(-0.433159988384986,5.59980883257818,
43.8302695826396));
#66158=CARTESIAN_POINT('Ctrl Pts',(-4.93950805874728,2.67333998483713,43.9890303448854));
#66159=CARTESIAN_POINT('Ctrl Pts',(-4.92506747450587,-2.69985127525994,
44.1477911071313));
#66160=CARTESIAN_POINT('Ctrl Pts',(-0.403054699451855,-5.60205618020814,
44.3065518693771));
#66161=CARTESIAN_POINT('Ctrl Pts',(4.48784604800658,-3.37708815199574,44.4653126316231));
#66162=CARTESIAN_POINT('Ctrl Pts',(5.27133300928694,1.93869410742388,44.6240733938689));
#66163=CARTESIAN_POINT('Ctrl Pts',(1.2303349855046,5.48012430154663,44.7828341561148));
#66164=CARTESIAN_POINT('Ctrl Pts',(-3.93670319808305,4.00597734231749,44.9415949183607));
#66165=CARTESIAN_POINT('Ctrl Pts',(-5.50075036662014,-1.13456244477178,
45.1003556806066));
#66166=CARTESIAN_POINT('Ctrl Pts',(-2.03034277701881,-5.23671602674481,
45.2591164428525));
#66167=CARTESIAN_POINT('Ctrl Pts',(3.2982965397378,-4.5460671434672,45.4178772050984));
#66168=CARTESIAN_POINT('Ctrl Pts',(5.60823411554676,0.305281250940591,45.5766379673442));
#66169=CARTESIAN_POINT('Ctrl Pts',(2.78534452306571,4.87722691955032,45.7353987295903));
#66170=CARTESIAN_POINT('Ctrl Pts',(-2.5867774563813,4.98538553455152,45.894159491836));
#66171=CARTESIAN_POINT('Ctrl Pts',(-5.59140169360195,0.53076702774728,46.052920254082));
#66172=CARTESIAN_POINT('Ctrl Pts',(-3.47860430924953,-4.40962567534128,
46.2116810163279));
#66173=CARTESIAN_POINT('Ctrl Pts',(1.81791799428017,-5.3141942665874,46.3704417785737));
#66174=CARTESIAN_POINT('Ctrl Pts',(5.45062622041652,-1.35504994087535,46.5292025408197));
#66175=CARTESIAN_POINT('Ctrl Pts',(4.09475483808194,3.84427748126524,46.6879633030655));
#66176=CARTESIAN_POINT('Ctrl Pts',(-1.00876124798033,5.52520472756723,46.8467240653114));
#66177=CARTESIAN_POINT('Ctrl Pts',(-5.18902822687748,2.14929583762384,47.0054848275573));
#66178=CARTESIAN_POINT('Ctrl Pts',(-4.62013807160538,-3.19371425400909,
47.1642455898032));
#66179=CARTESIAN_POINT('Ctrl Pts',(0.177243570754919,-5.61373950710082,
47.3230063520491));
#66180=CARTESIAN_POINT('Ctrl Pts',(4.81240648318495,-2.89589888938787,47.4817671142949));
#66181=CARTESIAN_POINT('Ctrl Pts',(5.04310798533405,2.47235684827615,47.6405278765409));
#66182=CARTESIAN_POINT('Ctrl Pts',(0.658203015566318,5.57783607927463,47.7992886387866));
#66183=CARTESIAN_POINT('Ctrl Pts',(-4.32910945912064,3.57830935329949,47.9580494010327));
#66184=CARTESIAN_POINT('Ctrl Pts',(-5.35428872245015,-1.69619539369769,
48.1168101632785));
#66185=CARTESIAN_POINT('Ctrl Pts',(-1.47905939811478,-5.41829030541985,
48.2755709255244));
#66186=CARTESIAN_POINT('Ctrl Pts',(3.74985026583283,-4.18140042578941,48.4343316877703));
#66187=CARTESIAN_POINT('Ctrl Pts',(5.54678242582246,0.882434846062579,48.5930924500162));
#66188=CARTESIAN_POINT('Ctrl Pts',(2.26712988102407,5.13863879247473,48.7518532122621));
#66189=CARTESIAN_POINT('Ctrl Pts',(-3.08746918127143,4.69180355424833,48.9106139745079));
#66190=CARTESIAN_POINT('Ctrl Pts',(-5.61632214089325,-0.0491136098317049,
49.0693747367539));
#66191=CARTESIAN_POINT('Ctrl Pts',(-3.00494552437603,-4.74508049799904,
49.2281354989997));
#66192=CARTESIAN_POINT('Ctrl Pts',(2.35664902330628,-5.09820477402661,49.3868962612456));
#66193=CARTESIAN_POINT('Ctrl Pts',(5.561366400077,-0.785296314172567,49.5456570234916));
#66194=CARTESIAN_POINT('Ctrl Pts',(3.67615137334867,4.24633931960047,49.7044177857373));
#66195=CARTESIAN_POINT('Ctrl Pts',(-1.57358967977417,5.39159550195178,49.8631785479833));
#66196=CARTESIAN_POINT('Ctrl Pts',(-5.38313339204505,1.60229879248781,50.0219393102291));
#66197=CARTESIAN_POINT('Ctrl Pts',(-4.26586899396583,-3.65347071471485,
50.1807000724751));
#66198=CARTESIAN_POINT('Ctrl Pts',(0.755649010055931,-5.56547222709447,
50.339460834721));
#66199=CARTESIAN_POINT('Ctrl Pts',(5.08557395847498,-2.38378355767454,50.4982215969668));
#66200=CARTESIAN_POINT('Ctrl Pts',(4.76102627921851,2.97961663734597,50.6569823592128));
#66201=CARTESIAN_POINT('Ctrl Pts',(0.0790419217800287,5.61598067229221,
50.8157431214586));
#66202=CARTESIAN_POINT('Ctrl Pts',(-4.6752840168385,3.11242765359339,50.9745038837046));
#66203=CARTESIAN_POINT('Ctrl Pts',(-5.15064721483666,-2.2397142240147,51.1332646459504));
#66204=CARTESIAN_POINT('Ctrl Pts',(-0.911980753248584,-5.54200123084275,
51.2920254081963));
#66205=CARTESIAN_POINT('Ctrl Pts',(4.16135835052739,-3.77207942857173,51.4507861704422));
#66206=CARTESIAN_POINT('Ctrl Pts',(5.42609518155485,1.45016468639448,51.6095469326881));
#66207=CARTESIAN_POINT('Ctrl Pts',(1.72470396018791,5.34517378451539,51.768307694934));
#66208=CARTESIAN_POINT('Ctrl Pts',(-3.55518900731147,4.34811656458864,51.9270684571799));
#66209=CARTESIAN_POINT('Ctrl Pts',(-5.58126440065713,-0.62846975019945,
52.0858292194257));
#66210=CARTESIAN_POINT('Ctrl Pts',(-2.49919613258049,-5.0298613527465,52.2445899816716));
#66211=CARTESIAN_POINT('Ctrl Pts',(2.87021277497366,-4.82777020614449,52.4033507439175));
#66212=CARTESIAN_POINT('Ctrl Pts',(5.61271527908117,-0.207156300717966,
52.5621115061634));
#66213=CARTESIAN_POINT('Ctrl Pts',(3.2182893171531,4.60305337879721,52.7208722684093));
#66214=CARTESIAN_POINT('Ctrl Pts',(-2.12161333176065,5.20040800394102,52.8796330306552));
#66215=CARTESIAN_POINT('Ctrl Pts',(-5.51975065392403,1.03819037534721,53.038393792901));
#66216=CARTESIAN_POINT('Ctrl Pts',(-3.86604357463707,-4.07421079670234,
53.197154555147));
#66217=CARTESIAN_POINT('Ctrl Pts',(1.32598467399636,-5.45776979922066,53.3559153173929));
#66218=CARTESIAN_POINT('Ctrl Pts',(5.30443124625904,-1.84621117174306,53.5146760796387));
#66219=CARTESIAN_POINT('Ctrl Pts',(4.4281003159834,3.4550563133683,53.6734368418847));
#66220=CARTESIAN_POINT('Ctrl Pts',(-0.500963281565584,5.59415072441577,
53.8321976041305));
#66221=CARTESIAN_POINT('Ctrl Pts',(-4.97152998170303,2.61330751691913,53.9909583663765));
#66222=CARTESIAN_POINT('Ctrl Pts',(-4.89200058522532,-2.75931455457936,
54.1497191286223));
#66223=CARTESIAN_POINT('Ctrl Pts',(-0.33516282504586,-5.60652766136632,
54.3084798908682));
#66224=CARTESIAN_POINT('Ctrl Pts',(4.5284261902974,-3.32247539885354,54.4672406531142));
#66225=CARTESIAN_POINT('Ctrl Pts',(5.24746123370139,2.00240783502248,54.6260014153599));
#66226=CARTESIAN_POINT('Ctrl Pts',(1.16385947023147,5.49462625394218,54.7847621776059));
#66227=CARTESIAN_POINT('Ctrl Pts',(-3.9849420309447,3.95799488970978,54.9435229398517));
#66228=CARTESIAN_POINT('Ctrl Pts',(-5.48660286376106,-1.20111429611312,
55.1022837020977));
#66229=CARTESIAN_POINT('Ctrl Pts',(-1.96675716519669,-5.26092698961938,
55.2610444643435));
#66230=CARTESIAN_POINT('Ctrl Pts',(3.35312476633552,-4.50577860511874,55.4198052265895));
#66231=CARTESIAN_POINT('Ctrl Pts',(5.60412448918787,0.373195989586127,55.5785659888352));
#66232=CARTESIAN_POINT('Ctrl Pts',(2.72605829932405,4.91061021520187,55.7373267510813));
#66233=CARTESIAN_POINT('Ctrl Pts',(-2.64697971461612,4.95368397532273,55.8960875133271));
#66234=CARTESIAN_POINT('Ctrl Pts',(-5.59742104069143,0.462994848981032,
56.054848275573));
#66235=CARTESIAN_POINT('Ctrl Pts',(-3.4249316548741,-4.45144130550992,56.2136090378189));
#66236=CARTESIAN_POINT('Ctrl Pts',(1.88215979738361,-5.29178240615308,56.3723698000648));
#66237=CARTESIAN_POINT('Ctrl Pts',(5.46664111175626,-1.28892260908666,56.5311305623107));
#66238=CARTESIAN_POINT('Ctrl Pts',(4.04788549992257,3.8935985304696,56.6898913245566));
#66239=CARTESIAN_POINT('Ctrl Pts',(-1.07561856571275,5.51257936342436,56.8486520868024));
#66240=CARTESIAN_POINT('Ctrl Pts',(-5.21468366481089,2.08627917904408,57.0074128490483));
#66241=CARTESIAN_POINT('Ctrl Pts',(-4.58111098928757,-3.24944743622466,
57.1661736112942));
#66242=CARTESIAN_POINT('Ctrl Pts',(0.245234395488895,-5.61118050219625,
57.3249343735402));
#66243=CARTESIAN_POINT('Ctrl Pts',(4.84713377073179,-2.83738977681774,57.4836951357859));
#66244=CARTESIAN_POINT('Ctrl Pts',(5.01278826137211,2.53326674150361,57.6424558980319));
#66245=CARTESIAN_POINT('Ctrl Pts',(0.590585817593506,5.58540015836071,57.8012166602777));
#66246=CARTESIAN_POINT('Ctrl Pts',(-4.37213880612535,3.52560474201678,57.9599774225237));
#66247=CARTESIAN_POINT('Ctrl Pts',(-5.33334844575954,-1.76093182521995,
58.1187381847696));
#66248=CARTESIAN_POINT('Ctrl Pts',(-1.41331467858517,-5.43580979765242,
58.2774989470154));
#66249=CARTESIAN_POINT('Ctrl Pts',(3.80022785268933,-4.1356686043012,58.4362597092614));
#66250=CARTESIAN_POINT('Ctrl Pts',(5.53568577371134,0.949562821348838,58.5950204715072));
#66251=CARTESIAN_POINT('Ctrl Pts',(2.20471498490915,5.16572534812638,58.7537812337531));
#66252=CARTESIAN_POINT('Ctrl Pts',(-3.144078301978,4.65405824716339,58.9125419959989));
#66253=CARTESIAN_POINT('Ctrl Pts',(-5.61531508977269,-0.117145121663757,
59.071302758245));
#66254=CARTESIAN_POINT('Ctrl Pts',(-2.94724398537462,-4.78113369689988,
59.2300635204908));
#66255=CARTESIAN_POINT('Ctrl Pts',(2.41823483917798,-5.06928267110287,59.3888242827367));
#66256=CARTESIAN_POINT('Ctrl Pts',(5.57047127296998,-0.717869301457213,
59.5475850449825));
#66257=CARTESIAN_POINT('Ctrl Pts',(3.6244422454793,4.29055998048545,59.7063458072285));
#66258=CARTESIAN_POINT('Ctrl Pts',(-1.63878703510391,5.37213771142675,59.8651065694744));
#66259=CARTESIAN_POINT('Ctrl Pts',(-5.40214836375828,1.53697091478732,60.0238673317203));
#66260=CARTESIAN_POINT('Ctrl Pts',(-4.22129849913074,-3.70487861045338,
60.1826280939661));
#66261=CARTESIAN_POINT('Ctrl Pts',(0.823012693142843,-5.55591006441646,
60.3413888562121));
#66262=CARTESIAN_POINT('Ctrl Pts',(5.11407752940203,-2.32200291994295,60.5001496184578));
#66263=CARTESIAN_POINT('Ctrl Pts',(4.72458239922035,3.03707222336503,60.6589103807039));
#66264=CARTESIAN_POINT('Ctrl Pts',(0.0110051430237869,5.61652609927038,
60.8176711429496));
#66265=CARTESIAN_POINT('Ctrl Pts',(-4.71264435622464,3.05556373009997,60.9764319051957));
#66266=CARTESIAN_POINT('Ctrl Pts',(-5.12313779106008,-2.30194389826733,
61.1351926674413));
#66267=CARTESIAN_POINT('Ctrl Pts',(-0.844779031235954,-5.55264215714847,
61.2939534296875));
#66268=CARTESIAN_POINT('Ctrl Pts',(4.20674730208683,-3.72139270614424,61.4527141919332));
#66269=CARTESIAN_POINT('Ctrl Pts',(5.4081300077703,1.51578902094353,61.6114749541792));
#66270=CARTESIAN_POINT('Ctrl Pts',(1.65982693686032,5.36567433568524,61.770235716425));
#66271=CARTESIAN_POINT('Ctrl Pts',(-3.60760044673811,4.30473060175118,61.9289964786709));
#66272=CARTESIAN_POINT('Ctrl Pts',(-5.5732417058914,-0.696034068613847,
62.0877572409168));
#66273=CARTESIAN_POINT('Ctrl Pts',(-2.43808191892836,-5.05976709874605,
62.2465180031627));
#66274=CARTESIAN_POINT('Ctrl Pts',(2.92848491241984,-4.79264672750744,62.4052787654085));
#66275=CARTESIAN_POINT('Ctrl Pts',(5.61481290018499,-0.139149677953565,
62.5640395276545));
#66276=CARTESIAN_POINT('Ctrl Pts',(3.16229261500766,4.64170140724564,62.7228002899003));
#66277=CARTESIAN_POINT('Ctrl Pts',(-2.18445446491029,5.17432558191808,62.8815610521463));
#66278=CARTESIAN_POINT('Ctrl Pts',(-5.53192209351194,0.97124893218624,63.0403218143921));
#66279=CARTESIAN_POINT('Ctrl Pts',(-3.81640564737093,-4.12074440746734,
63.199082576638));
#66280=CARTESIAN_POINT('Ctrl Pts',(1.39200182087229,-5.44130659563001,63.357843338884));
#66281=CARTESIAN_POINT('Ctrl Pts',(5.32640670340396,-1.78181878059799,63.5166041011298));
#66282=CARTESIAN_POINT('Ctrl Pts',(4.38592147376913,3.50844400880067,63.6753648633758));
#66283=CARTESIAN_POINT('Ctrl Pts',(-0.568693058375023,5.58767167452727,
63.8341256256215));
#66284=CARTESIAN_POINT('Ctrl Pts',(-5.00282233253868,2.55289154607289,63.9928863878675));
#66285=CARTESIAN_POINT('Ctrl Pts',(-4.85821579476509,-2.818372904435,64.1516471501133));
#66286=CARTESIAN_POINT('Ctrl Pts',(-0.267221765488804,-5.61017638448271,
64.3104079123593));
#66287=CARTESIAN_POINT('Ctrl Pts',(4.56834178595791,-3.26737507238287,64.4691686746051));
#66288=CARTESIAN_POINT('Ctrl Pts',(5.2228193930792,2.06582770923283,64.6279294368511));
#66289=CARTESIAN_POINT('Ctrl Pts',(1.0972131585588,5.50832186982966,64.7866901990968));
#66290=CARTESIAN_POINT('Ctrl Pts',(-4.03259607348695,3.90943160127608,64.9454509613429));
#66291=CARTESIAN_POINT('Ctrl Pts',(-5.4716502018265,-1.26748988390853,65.1042117235886));
#66292=CARTESIAN_POINT('Ctrl Pts',(-1.90288293172278,-5.28436591135743,
65.2629724858347));
#66293=CARTESIAN_POINT('Ctrl Pts',(3.40746092180959,-4.46482884367352,65.4217332480805));
#66294=CARTESIAN_POINT('Ctrl Pts',(5.59919245745271,0.441055961713188,65.5804940103263));
#66295=CARTESIAN_POINT('Ctrl Pts',(2.66637202647467,4.94327287871016,65.7392547725723));
#66296=CARTESIAN_POINT('Ctrl Pts',(-2.70679352852708,4.92125546287557,65.8980155348181));
#66297=CARTESIAN_POINT('Ctrl Pts',(-5.60261896613596,0.395154725711709,
66.0567762970641));
#66298=CARTESIAN_POINT('Ctrl Pts',(-3.37075639171248,-4.49260368658171,
66.2155370593099));
#66299=CARTESIAN_POINT('Ctrl Pts',(1.94612539350076,-5.26859397654912,66.3742978215559));
#66300=CARTESIAN_POINT('Ctrl Pts',(5.48185377340806,-1.22260612788034,66.5330585838017));
#66301=CARTESIAN_POINT('Ctrl Pts',(4.00042213448843,3.94234819401505,66.6918193460476));
#66302=CARTESIAN_POINT('Ctrl Pts',(-1.1423180364002,5.49914502815419,66.8505801082935));
#66303=CARTESIAN_POINT('Ctrl Pts',(-5.23957384781653,2.02295635895467,67.0093408705393));
#66304=CARTESIAN_POINT('Ctrl Pts',(-4.54141162884421,-3.30470376196668,
67.1681016327853));
#66305=CARTESIAN_POINT('Ctrl Pts',(0.31318923207078,-5.60779805644547,67.3268623950311));
#66306=CARTESIAN_POINT('Ctrl Pts',(4.88114974130499,-2.77846427724327,67.4856231572771));
#66307=CARTESIAN_POINT('Ctrl Pts',(4.98173291063654,2.59380487778839,67.6443839195229));
#66308=CARTESIAN_POINT('Ctrl Pts',(0.522881951140529,5.59214457986643,67.8031446817689));
#66309=CARTESIAN_POINT('Ctrl Pts',(-4.41452654167645,3.47238274817052,67.9619054440147));
#66310=CARTESIAN_POINT('Ctrl Pts',(-5.31162550008227,-1.82540983996319,
68.1206662062607));
#66311=CARTESIAN_POINT('Ctrl Pts',(-1.34736255509922,-5.45253158469304,
68.2794269685065));
#66312=CARTESIAN_POINT('Ctrl Pts',(3.85004775603573,-4.08932987336585,68.4381877307524));
#66313=CARTESIAN_POINT('Ctrl Pts',(5.52377675960678,1.01655144827307,68.5969484929983));
#66314=CARTESIAN_POINT('Ctrl Pts',(2.14197654682777,5.19205383348419,68.7557092552442));
#66315=CARTESIAN_POINT('Ctrl Pts',(-3.20022602913364,4.61562995694134,68.9144700174901));
#66316=CARTESIAN_POINT('Ctrl Pts',(-5.61348399105505,-0.185159442447144,
69.073230779736));
#66317=CARTESIAN_POINT('Ctrl Pts',(-2.88910993826166,-4.81648526433911,
69.2319915419818));
#66318=CARTESIAN_POINT('Ctrl Pts',(2.47946577904082,-5.0396166508499,69.3907523042278));
#66319=CARTESIAN_POINT('Ctrl Pts',(5.57875867909682,-0.650336941407984,
69.5495130664736));
#66320=CARTESIAN_POINT('Ctrl Pts',(3.57220123064088,4.33415100161104,69.7082738287195));
#66321=CARTESIAN_POINT('Ctrl Pts',(-1.70374389840499,5.35189155958961,69.8670345909654));
#66322=CARTESIAN_POINT('Ctrl Pts',(-5.42037057009564,1.47141748657539,70.0257953532113));
#66323=CARTESIAN_POINT('Ctrl Pts',(-4.17610852865976,-3.75574281518495,
70.1845561154572));
#66324=CARTESIAN_POINT('Ctrl Pts',(0.89025559910136,-5.54553257182993,70.343316877703));
#66325=CARTESIAN_POINT('Ctrl Pts',(5.14183060935358,-2.2598815282383,70.5020776399489));
#66326=CARTESIAN_POINT('Ctrl Pts',(4.68744518666451,3.09408211897719,70.6608384021949));
#66327=CARTESIAN_POINT('Ctrl Pts',(-0.0570332507375796,5.61624730093583,
70.8195991644407));
#66328=CARTESIAN_POINT('Ctrl Pts',(-4.74931311496125,2.99825140257037,70.9783599266866));
#66329=CARTESIAN_POINT('Ctrl Pts',(-5.09487654671437,-2.36383576220895,
71.1371206889325));
#66330=CARTESIAN_POINT('Ctrl Pts',(-0.777453337884133,-5.56246823311117,
71.2958814511784));
#66331=CARTESIAN_POINT('Ctrl Pts',(4.25151891339917,-3.67015986926562,71.4546422134243));
#66332=CARTESIAN_POINT('Ctrl Pts',(5.38937119080337,1.58119091342487,71.6134029756702));
#66333=CARTESIAN_POINT('Ctrl Pts',(1.59470633389773,5.38538747404349,71.7721637379161));
#66334=CARTESIAN_POINT('Ctrl Pts',(-3.65948247073021,4.26071291961525,71.9309245001618));
#66335=CARTESIAN_POINT('Ctrl Pts',(-5.56440113779842,-0.763496244015491,
72.089685262408));
#66336=CARTESIAN_POINT('Ctrl Pts',(-2.3766099167077,-5.08893032382693,72.2484460246537));
#66337=CARTESIAN_POINT('Ctrl Pts',(2.98632729464914,-4.75681992787116,72.4072067868998));
#66338=CARTESIAN_POINT('Ctrl Pts',(5.61608654738804,-0.0711226349710497,
72.5659675491454));
#66339=CARTESIAN_POINT('Ctrl Pts',(3.10583184636022,4.67966826592364,72.7247283113916));
#66340=CARTESIAN_POINT('Ctrl Pts',(-2.24697502932542,5.14748382751671,72.8834890736371));
#66341=CARTESIAN_POINT('Ctrl Pts',(-5.54328172342653,0.904164958225804,
73.0422498358833));
#66342=CARTESIAN_POINT('Ctrl Pts',(-3.76620766250282,-4.1666732989117,73.2010105981289));
#66343=CARTESIAN_POINT('Ctrl Pts',(1.45781469145456,-5.42404488019209,73.3597713603751));
#66344=CARTESIAN_POINT('Ctrl Pts',(5.34760051026307,-1.71716490751244,73.5185321226207));
#66345=CARTESIAN_POINT('Ctrl Pts',(4.3430989974944,3.56131684000752,73.6772928848668));
#66346=CARTESIAN_POINT('Ctrl Pts',(-0.636339379467287,5.58037263371339,
73.8360536471125));
#66347=CARTESIAN_POINT('Ctrl Pts',(-5.03338051910119,2.49210093834326,73.9948144093586));
#66348=CARTESIAN_POINT('Ctrl Pts',(-4.82371806104376,-2.87701765801306,
74.1535751716043));
#66349=CARTESIAN_POINT('Ctrl Pts',(-0.199241491132339,-5.61300181410709,
74.3123359338505));
#66350=CARTESIAN_POINT('Ctrl Pts',(4.60758697737389,-3.21179525855753,74.4710966960961));
#66351=CARTESIAN_POINT('Ctrl Pts',(5.19741110361085,2.12894442318739,74.6298574583422));
#66352=CARTESIAN_POINT('Ctrl Pts',(1.0304058308339,5.52120913937719,74.7886182205879));
#66353=CARTESIAN_POINT('Ctrl Pts',(-4.07965833247825,3.86029460367982,74.9473789828338));
#66354=CARTESIAN_POINT('Ctrl Pts',(-5.45589457511983,-1.33367946753936,
75.1061397450798));
#66355=CARTESIAN_POINT('Ctrl Pts',(-1.8387294501421,-5.30702935229665,75.2649005073255));
#66356=CARTESIAN_POINT('Ctrl Pts',(3.46129703232802,-4.42322386850986,75.4236612695716));
#66357=CARTESIAN_POINT('Ctrl Pts',(5.5934387441171,0.508851208869345,75.5824220318174));
#66358=CARTESIAN_POINT('Ctrl Pts',(2.60629446347919,4.97521011682889,75.7411827940634));
#66359=CARTESIAN_POINT('Ctrl Pts',(-2.76621012043596,4.88810475609477,75.8999435563092));
#66360=CARTESIAN_POINT('Ctrl Pts',(-5.60699470713969,0.327256613478776,
76.0587043185551));
#66361=CARTESIAN_POINT('Ctrl Pts',(-3.31608646998587,-4.53310677797631,
76.2174650808009));
#66362=CARTESIAN_POINT('Ctrl Pts',(2.00980539567907,-5.24463238067812,76.3762258430469));
#66363=CARTESIAN_POINT('Ctrl Pts',(5.49626197291347,-1.15611022920134,76.5349866052928));
#66364=CARTESIAN_POINT('Ctrl Pts',(3.95237170702942,3.99051931788734,76.6937473675386));
#66365=CARTESIAN_POINT('Ctrl Pts',(-1.20884987189374,5.48490369324573,76.8525081297847));
#66366=CARTESIAN_POINT('Ctrl Pts',(-5.26369512325953,1.95933666998091,77.0112688920303));
#66367=CARTESIAN_POINT('Ctrl Pts',(-4.50104581615728,-3.35947512236825,
77.1700296542764));
#66368=CARTESIAN_POINT('Ctrl Pts',(0.381098108126755,-5.60359266622235,
77.3287904165222));
#66369=CARTESIAN_POINT('Ctrl Pts',(4.91444940305996,-2.71913103798297,77.4875511787681));
#66370=CARTESIAN_POINT('Ctrl Pts',(4.94994649050095,2.65396237315744,77.646311941014));
#66371=CARTESIAN_POINT('Ctrl Pts',(0.455101351751309,5.59806835404786,77.8050727032599));
#66372=CARTESIAN_POINT('Ctrl Pts',(-4.45626644537291,3.41865118208945,77.9638334655057));
#66373=CARTESIAN_POINT('Ctrl Pts',(-5.28912307326102,-1.88961997577731,
78.1225942277517));
#66374=CARTESIAN_POINT('Ctrl Pts',(-1.28121270613263,-5.468453212619,78.2813549899975));
#66375=CARTESIAN_POINT('Ctrl Pts',(3.89930266479998,-4.04239103319333,78.4401157522435));
#66376=CARTESIAN_POINT('Ctrl Pts',(5.51105713115687,1.08339089625261,78.5988765144893));
#66377=CARTESIAN_POINT('Ctrl Pts',(2.07892377364716,5.21762038484239,78.7576372767352));
#66378=CARTESIAN_POINT('Ctrl Pts',(-3.2559041230579,4.57652432293467,78.9163980389812));
#66379=CARTESIAN_POINT('Ctrl Pts',(-5.61082911345409,-0.253146591078478,
79.0751588012269));
#66380=CARTESIAN_POINT('Ctrl Pts',(-2.83055191421017,-4.85113001247338,
79.2339195634729));
#66381=CARTESIAN_POINT('Ctrl Pts',(2.54033285725292,-5.00921106675685,79.3926803257188));
#66382=CARTESIAN_POINT('Ctrl Pts',(5.58622740228054,-0.582709144400273,
79.5514410879646));
#66383=CARTESIAN_POINT('Ctrl Pts',(3.51943599520346,4.37710598599406,79.7102018502106));
#66384=CARTESIAN_POINT('Ctrl Pts',(-1.7684507372563,5.33086001756339,79.8689626124564));
#66385=CARTESIAN_POINT('Ctrl Pts',(-5.43779733694764,1.40564812781938,80.0277233747023));
#66386=CARTESIAN_POINT('Ctrl Pts',(-4.13030571418267,-3.80605586458648,
80.1864841369483));
#66387=CARTESIAN_POINT('Ctrl Pts',(0.95736786003426,-5.53434127223174,80.345244899194));
#66388=CARTESIAN_POINT('Ctrl Pts',(5.16882912556325,-2.19742849887699,80.5040056614401));
#66389=CARTESIAN_POINT('Ctrl Pts',(4.64962009144032,3.15063795798068,80.6627664236858));
#66390=CARTESIAN_POINT('Ctrl Pts',(-0.125063274873211,5.61514431819889,
80.8215271859319));
#66391=CARTESIAN_POINT('Ctrl Pts',(-4.78528491189737,2.9404990815964,80.9802879481776));
#66392=CARTESIAN_POINT('Ctrl Pts',(-5.06586762915643,-2.42538073321897,
81.1390487104236));
#66393=CARTESIAN_POINT('Ctrl Pts',(-0.710013553204522,-5.5714780167311,
81.2978094726694));
#66394=CARTESIAN_POINT('Ctrl Pts',(4.29566661416096,-3.61838843639986,81.4565702349154));
#66395=CARTESIAN_POINT('Ctrl Pts',(5.36982148364171,1.64636076619313,81.6153309971612));
#66396=CARTESIAN_POINT('Ctrl Pts',(1.52935170749991,5.4043103065256,81.7740917594071));
#66397=CARTESIAN_POINT('Ctrl Pts',(-3.71082746511973,4.21606997808528,81.932852521653));
#66398=CARTESIAN_POINT('Ctrl Pts',(-5.55474399465067,-0.830846376919461,
82.0916132838989));
#66399=CARTESIAN_POINT('Ctrl Pts',(-2.3147891451765,-5.11734674715333,82.2503740461448));
#66400=CARTESIAN_POINT('Ctrl Pts',(3.04373142991963,-4.72029506698704,82.4091348083907));
#66401=CARTESIAN_POINT('Ctrl Pts',(5.61653604023885,-0.00308515058908493,
82.5678955706366));
#66402=CARTESIAN_POINT('Ctrl Pts',(3.04891528446413,4.71694837524191,82.7266563328824));
#66403=CARTESIAN_POINT('Ctrl Pts',(-2.30916582642725,5.11988669499558,82.8854170951283));
#66404=CARTESIAN_POINT('Ctrl Pts',(-5.55382792200581,0.836948268868883,
83.0441778573743));
#66405=CARTESIAN_POINT('Ctrl Pts',(-3.71545689970117,-4.21199067509615,
83.2029386196201));
#66406=CARTESIAN_POINT('Ctrl Pts',(1.52341346128536,-5.40598729308003,83.3616993818661));
#66407=CARTESIAN_POINT('Ctrl Pts',(5.36800987538946,-1.65225883547266,83.5204601441119));
#66408=CARTESIAN_POINT('Ctrl Pts',(4.29963856085619,3.61366665531133,83.6792209063577));
#66409=CARTESIAN_POINT('Ctrl Pts',(-0.703891148427739,5.57225542504627,
83.8379816686037));
#66410=CARTESIAN_POINT('Ctrl Pts',(-5.06320229660515,2.43094317454181,83.9967424308495));
#66411=CARTESIAN_POINT('Ctrl Pts',(-4.78850815696806,-2.93523745070957,
84.1555031930955));
#66412=CARTESIAN_POINT('Ctrl Pts',(-0.131240194167233,-5.61500881902578,
84.3142639553413));
#66413=CARTESIAN_POINT('Ctrl Pts',(4.64617174185204,-3.15573399420934,84.4730247175873));
#66414=CARTESIAN_POINT('Ctrl Pts',(5.17120995324134,2.19172933227414,84.6317854798331));
#66415=CARTESIAN_POINT('Ctrl Pts',(0.963505020594375,5.53332329484411,84.790546242079));
#66416=CARTESIAN_POINT('Ctrl Pts',(-4.12623247316118,3.81052000369223,84.949307004325));
#66417=CARTESIAN_POINT('Ctrl Pts',(-5.43912651173278,-1.39953714320699,
85.1080677665708));
#66418=CARTESIAN_POINT('Ctrl Pts',(-1.77471179476972,-5.32917485889023,
85.2668285288167));
#66419=CARTESIAN_POINT('Ctrl Pts',(3.51540237664497,-4.38046992755931,85.4255892910626));
#66420=CARTESIAN_POINT('Ctrl Pts',(5.58537377992907,0.575612579899635,85.5843500533083));
#66421=CARTESIAN_POINT('Ctrl Pts',(2.54870583510895,5.00827077132932,85.7431108155546));
#66422=CARTESIAN_POINT('Ctrl Pts',(-2.83087179085208,4.8505389297872,85.9018715778));
#66423=CARTESIAN_POINT('Ctrl Pts',(-5.13713439629382,1.0315398004976,86.0341722130053));
#66424=CARTESIAN_POINT('Ctrl Pts',(-4.44488369978034,-2.16782829859426,
86.140012721169));
#66425=CARTESIAN_POINT('Ctrl Pts',(-3.40222835107896,-3.41035291299011,
86.1929329752511));
#66426=CARTESIAN_POINT('Ctrl Pts',(-2.75898463274135,-3.86904481704426,
86.219393102292));
#66427=CARTESIAN_POINT('Ctrl Pts',(-2.16917135428577,4.44050218283316,26.));
#66428=CARTESIAN_POINT('Ctrl Pts',(-2.90742207776898,4.07986902565299,26.026460127041));
#66429=CARTESIAN_POINT('Ctrl Pts',(-4.18934766522561,2.98339209614179,26.0793803811229));
#66430=CARTESIAN_POINT('Ctrl Pts',(-5.44619024033903,-0.180386727026251,
26.1852208892869));
#66431=CARTESIAN_POINT('Ctrl Pts',(-3.73289165771545,-4.49218988265986,
26.3175215244917));
#66432=CARTESIAN_POINT('Ctrl Pts',(1.7587897347136,-5.57324416600043,26.4762822867377));
#66433=CARTESIAN_POINT('Ctrl Pts',(5.63139102185651,-1.54490260103424,26.6350430489835));
#66434=CARTESIAN_POINT('Ctrl Pts',(4.35479274028667,3.89299966074075,26.7938038112295));
#66435=CARTESIAN_POINT('Ctrl Pts',(-0.909953676412603,5.770185632809,26.9525645734753));
#66436=CARTESIAN_POINT('Ctrl Pts',(-5.34057378621867,2.36513448582097,27.1113253357212));
#66437=CARTESIAN_POINT('Ctrl Pts',(-4.88402091610239,-3.20394040614541,
27.2700860979671));
#66438=CARTESIAN_POINT('Ctrl Pts',(0.0428938108868349,-5.84099464142013,
27.428846860213));
#66439=CARTESIAN_POINT('Ctrl Pts',(4.93036456360867,-3.13202328336963,27.5876076224589));
#66440=CARTESIAN_POINT('Ctrl Pts',(5.30551230831797,2.44338327902792,27.7463683847048));
#66441=CARTESIAN_POINT('Ctrl Pts',(0.824842359969521,5.78257686590837,27.9051291469507));
#66442=CARTESIAN_POINT('Ctrl Pts',(-4.41072200448754,3.82935543872663,28.0638899091965));
#66443=CARTESIAN_POINT('Ctrl Pts',(-5.60947270247999,-1.62859650629097,
28.2226506714425));
#66444=CARTESIAN_POINT('Ctrl Pts',(-1.67425541405712,-5.59601373441819,
28.3814114336883));
#66445=CARTESIAN_POINT('Ctrl Pts',(3.79328779764178,-4.44178483963319,28.5401721959342));
#66446=CARTESIAN_POINT('Ctrl Pts',(5.78910011906805,0.777699430509262,28.6989329581801));
#66447=CARTESIAN_POINT('Ctrl Pts',(2.48655015281781,5.28541035916478,28.8576937204261));
#66448=CARTESIAN_POINT('Ctrl Pts',(-3.09176592905605,4.95575179531496,29.0164544826718));
#66449=CARTESIAN_POINT('Ctrl Pts',(-5.84040367375386,0.0904380671616019,
29.1752152449178));
#66450=CARTESIAN_POINT('Ctrl Pts',(-3.24372543242543,-4.85764747523187,
29.3339760071636));
#66451=CARTESIAN_POINT('Ctrl Pts',(2.32170932913062,-5.35986560023234,29.4927367694096));
#66452=CARTESIAN_POINT('Ctrl Pts',(5.76224483502612,-0.956571044848404,
29.6514975316554));
#66453=CARTESIAN_POINT('Ctrl Pts',(3.92899783701638,4.32220656851071,29.8102582939014));
#66454=CARTESIAN_POINT('Ctrl Pts',(-1.50018798335741,5.64516869698926,29.9690190561472));
#66455=CARTESIAN_POINT('Ctrl Pts',(-5.55635594320173,1.80150000520858,30.1277798183931));
#66456=CARTESIAN_POINT('Ctrl Pts',(-4.52717721976122,-3.69095652156115,
30.286540580639));
#66457=CARTESIAN_POINT('Ctrl Pts',(0.645412378085751,-5.80533689665976,
30.4453013428849));
#66458=CARTESIAN_POINT('Ctrl Pts',(5.22730085393893,-2.60649561834369,30.6040621051308));
#66459=CARTESIAN_POINT('Ctrl Pts',(5.02500391786172,2.97789006670843,30.7628228673767));
#66460=CARTESIAN_POINT('Ctrl Pts',(0.223669905634492,5.83681980167278,30.9215836296225));
#66461=CARTESIAN_POINT('Ctrl Pts',(-4.78237363643064,3.35371376626822,31.0803443918685));
#66462=CARTESIAN_POINT('Ctrl Pts',(-5.41144274686964,-2.19881354860029,
31.2391051541144));
#66463=CARTESIAN_POINT('Ctrl Pts',(-1.08779416073393,-5.73891954012705,
31.3978659163602));
#66464=CARTESIAN_POINT('Ctrl Pts',(4.23143686842713,-4.0265910709645,31.5566266786062));
#66465=CARTESIAN_POINT('Ctrl Pts',(5.67792762467303,1.37099654017823,31.715387440852));
#66466=CARTESIAN_POINT('Ctrl Pts',(1.92780558426513,5.51380624011119,31.8741482030979));
#66467=CARTESIAN_POINT('Ctrl Pts',(-3.58670301245285,4.61021204769197,32.0329089653438));
#66468=CARTESIAN_POINT('Ctrl Pts',(-5.81855145490275,-0.512789031536669,
32.1916697275897));
#66469=CARTESIAN_POINT('Ctrl Pts',(-2.72508387585791,-5.16646992575742,
32.3504304898355));
#66470=CARTESIAN_POINT('Ctrl Pts',(2.86246370514321,-5.09163973204659,32.5091912520815));
#66471=CARTESIAN_POINT('Ctrl Pts',(5.83019706810478,-0.35678532940591,32.6679520143274));
#66472=CARTESIAN_POINT('Ctrl Pts',(3.46195598864868,4.7046099048568,32.8267127765732));
#66473=CARTESIAN_POINT('Ctrl Pts',(-2.0747729584413,5.46020245001391,32.9854735388191));
#66474=CARTESIAN_POINT('Ctrl Pts',(-5.71260631920057,1.21845092886281,33.144234301065));
#66475=CARTESIAN_POINT('Ctrl Pts',(-4.12208788279547,-4.13846410045175,
33.3029950633109));
#66476=CARTESIAN_POINT('Ctrl Pts',(1.24109129475792,-5.70773037400097,33.4617558255568));
#66477=CARTESIAN_POINT('Ctrl Pts',(5.46838580972161,-2.05310746437012,33.6205165878027));
#66478=CARTESIAN_POINT('Ctrl Pts',(4.69084659760865,3.48058210963631,33.7792773500486));
#66479=CARTESIAN_POINT('Ctrl Pts',(-0.379898704410712,5.82873662113877,
33.9380381122945));
#66480=CARTESIAN_POINT('Ctrl Pts',(-5.1029491079964,2.8422533358967,34.0967988745404));
#66481=CARTESIAN_POINT('Ctrl Pts',(-5.15562461633369,-2.74554702011659,
34.2555596367863));
#66482=CARTESIAN_POINT('Ctrl Pts',(-0.489714995198005,-5.82053887949348,
34.4143203990321));
#66483=CARTESIAN_POINT('Ctrl Pts',(4.62439674808221,-3.56839576568293,34.573081161278));
#66484=CARTESIAN_POINT('Ctrl Pts',(5.50611933347969,1.94965215094856,34.7318419235239));
#66485=CARTESIAN_POINT('Ctrl Pts',(1.3484733182716,5.68331886613153,34.8906026857698));
#66486=CARTESIAN_POINT('Ctrl Pts',(-4.04333666747246,4.2154385557958,35.0493634480157));
#66487=CARTESIAN_POINT('Ctrl Pts',(-5.73456142981912,-1.11053988305151,
35.2081242102616));
#66488=CARTESIAN_POINT('Ctrl Pts',(-2.17734040713567,-5.42011829904768,
35.3668849725075));
#66489=CARTESIAN_POINT('Ctrl Pts',(3.37264906388706,-4.76903888808624,35.5256457347534));
#66490=CARTESIAN_POINT('Ctrl Pts',(5.83588709273329,0.246810585441287,35.6844064969993));
#66491=CARTESIAN_POINT('Ctrl Pts',(2.95794299481775,5.03677147224547,35.8431672592451));
#66492=CARTESIAN_POINT('Ctrl Pts',(-2.62720088350026,5.21692525746274,36.001928021491));
#66493=CARTESIAN_POINT('Ctrl Pts',(-5.80785026434291,0.622389693993225,
36.160688783737));
#66494=CARTESIAN_POINT('Ctrl Pts',(-3.67297768016272,-4.54177592855961,
36.3194495459828));
#66495=CARTESIAN_POINT('Ctrl Pts',(1.82351626946645,-5.54916949094261,36.4782103082287));
#66496=CARTESIAN_POINT('Ctrl Pts',(5.65107242925025,-1.47779363362579,36.6369710704746));
#66497=CARTESIAN_POINT('Ctrl Pts',(4.30659448752927,3.94610409697964,36.7957318327205));
#66498=CARTESIAN_POINT('Ctrl Pts',(-0.979410275819905,5.7584068227102,36.9544925949664));
#66499=CARTESIAN_POINT('Ctrl Pts',(-5.36902883826232,2.30043973146977,37.1132533572123));
#66500=CARTESIAN_POINT('Ctrl Pts',(-4.84474820880581,-3.26296006985836,
37.2720141194581));
#66501=CARTESIAN_POINT('Ctrl Pts',(0.113593966110691,-5.839999146839,37.4307748817041));
#66502=CARTESIAN_POINT('Ctrl Pts',(4.96797147346979,-3.07209261953597,37.5895356439499));
#66503=CARTESIAN_POINT('Ctrl Pts',(5.27550973964484,2.50748691145728,37.7482964061959));
#66504=CARTESIAN_POINT('Ctrl Pts',(0.754740349553719,5.79213782889985,37.9070571684417));
#66505=CARTESIAN_POINT('Ctrl Pts',(-4.4567904622931,3.77564728217961,38.0658179306876));
#66506=CARTESIAN_POINT('Ctrl Pts',(-5.58933050861204,-1.69643098583928,
38.2245786929334));
#66507=CARTESIAN_POINT('Ctrl Pts',(-1.60634454512588,-5.6158837974589,38.3833394551794));
#66508=CARTESIAN_POINT('Ctrl Pts',(3.84681701249253,-4.39550821823998,38.5421002174252));
#66509=CARTESIAN_POINT('Ctrl Pts',(5.77925413772213,0.847770744858901,38.7008609796712));
#66510=CARTESIAN_POINT('Ctrl Pts',(2.42234134649229,5.31514402676831,38.859621741917));
#66511=CARTESIAN_POINT('Ctrl Pts',(-3.15157223642715,4.91793514219116,39.018382504163));
#66512=CARTESIAN_POINT('Ctrl Pts',(-5.84107064254106,0.0196817951957224,
39.1771432664088));
#66513=CARTESIAN_POINT('Ctrl Pts',(-3.18464277877548,-4.89658493195106,
39.3359040286547));
#66514=CARTESIAN_POINT('Ctrl Pts',(2.38646743230569,-5.33134756124203,39.4946647909006));
#66515=CARTESIAN_POINT('Ctrl Pts',(5.77340975374383,-0.886698054352646,
39.6534255531465));
#66516=CARTESIAN_POINT('Ctrl Pts',(3.87635111745847,4.36948459642503,39.8121863153924));
#66517=CARTESIAN_POINT('Ctrl Pts',(-1.56846246621147,5.62658147690965,39.9709470776383));
#66518=CARTESIAN_POINT('Ctrl Pts',(-5.57777129149482,1.73405912355756,40.1297078398841));
#66519=CARTESIAN_POINT('Ctrl Pts',(-4.48213345555963,-3.74552710720003,
40.2884686021301));
#66520=CARTESIAN_POINT('Ctrl Pts',(0.7156898274528,-5.79709252083298,40.4472293643759));
#66521=CARTESIAN_POINT('Ctrl Pts',(5.25849191934999,-2.5429817849029,40.6059901266219));
#66522=CARTESIAN_POINT('Ctrl Pts',(4.98856158393098,3.03854355696032,40.7647508888677));
#66523=CARTESIAN_POINT('Ctrl Pts',(0.152947309300711,5.83910102197203,40.9235116511136));
#66524=CARTESIAN_POINT('Ctrl Pts',(-4.82264901463799,3.29553487401187,41.0822724133595));
#66525=CARTESIAN_POINT('Ctrl Pts',(-5.38440965064774,-2.26420545406742,
41.2410331756054));
#66526=CARTESIAN_POINT('Ctrl Pts',(-1.0181941054504,-5.75167578952804,41.3997939378513));
#66527=CARTESIAN_POINT('Ctrl Pts',(4.27990378619904,-3.97503675518808,41.5585547000972));
#66528=CARTESIAN_POINT('Ctrl Pts',(5.66090300135578,1.43967733657867,41.7173154623431));
#66529=CARTESIAN_POINT('Ctrl Pts',(1.86087087513805,5.53675475439179,41.8760762245889));
#66530=CARTESIAN_POINT('Ctrl Pts',(-3.64228711704701,4.56642509860946,42.0348369868349));
#66531=CARTESIAN_POINT('Ctrl Pts',(-5.81191268460203,-0.583236290691027,
42.1935977490807));
#66532=CARTESIAN_POINT('Ctrl Pts',(-2.66229823602482,-5.19910201156664,
42.3523585113267));
#66533=CARTESIAN_POINT('Ctrl Pts',(2.92393287912081,-5.05659076281771,42.5111192735725));
#66534=CARTESIAN_POINT('Ctrl Pts',(5.83409131060233,-0.286133192362046,
42.6698800358184));
#66535=CARTESIAN_POINT('Ctrl Pts',(3.4047111699812,4.74620221579552,42.8286407980643));
#66536=CARTESIAN_POINT('Ctrl Pts',(-2.14076463166355,5.43466838142269,42.9874015603102));
#66537=CARTESIAN_POINT('Ctrl Pts',(-5.72694725190272,1.1491600402646,43.1461623225561));
#66538=CARTESIAN_POINT('Ctrl Pts',(-4.07165281531897,-4.18809467129411,
43.3049230848019));
#66539=CARTESIAN_POINT('Ctrl Pts',(1.31014264809932,-5.69227721266703,43.4636838470478));
#66540=CARTESIAN_POINT('Ctrl Pts',(5.49285554114887,-1.98671377613569,43.6224446092938));
#66541=CARTESIAN_POINT('Ctrl Pts',(4.64833926148183,3.53715079327751,43.7812053715396));
#66542=CARTESIAN_POINT('Ctrl Pts',(-0.450479095664875,5.82370691300532,
43.9399661337855));
#66543=CARTESIAN_POINT('Ctrl Pts',(-5.13700522439592,2.78022857850681,44.0987268960314));
#66544=CARTESIAN_POINT('Ctrl Pts',(-5.12198725989218,-2.80779987422883,
44.2574876582773));
#66545=CARTESIAN_POINT('Ctrl Pts',(-0.419170101997096,-5.82604411670637,
44.4162484205232));
#66546=CARTESIAN_POINT('Ctrl Pts',(4.66728433696318,-3.51211482473953,44.575009182769));
#66547=CARTESIAN_POINT('Ctrl Pts',(5.48209758667841,2.01620923377307,44.733769945015));
#66548=CARTESIAN_POINT('Ctrl Pts',(1.27952767221442,5.69923701562366,44.8925307072609));
#66549=CARTESIAN_POINT('Ctrl Pts',(-4.09410505154189,4.16614899531406,45.0512914695068));
#66550=CARTESIAN_POINT('Ctrl Pts',(-5.72068777605988,-1.17992584218497,
45.2100522317526));
#66551=CARTESIAN_POINT('Ctrl Pts',(-2.11152230724456,-5.4460965076122,45.3688129939986));
#66552=CARTESIAN_POINT('Ctrl Pts',(3.43017287444968,-4.72783329608889,45.5275737562444));
#66553=CARTESIAN_POINT('Ctrl Pts',(5.83246906545287,0.317487361563403,45.6863345184903));
#66554=CARTESIAN_POINT('Ctrl Pts',(2.89671141266624,5.07223388813511,45.8450952807362));
#66555=CARTESIAN_POINT('Ctrl Pts',(-2.69020500619468,5.1847170268841,46.003856042982));
#66556=CARTESIAN_POINT('Ctrl Pts',(-5.8149636300044,0.551988773385138,46.162616805228));
#66557=CARTESIAN_POINT('Ctrl Pts',(-3.61768991925726,-4.58593646623255,
46.3213775674738));
#66558=CARTESIAN_POINT('Ctrl Pts',(1.89060410937151,-5.5266725727009,46.4801383297198));
#66559=CARTESIAN_POINT('Ctrl Pts',(5.66855950784905,-1.40922912622162,46.6388990919655));
#66560=CARTESIAN_POINT('Ctrl Pts',(4.25847609633845,3.99798386203986,46.7976598542116));
#66561=CARTESIAN_POINT('Ctrl Pts',(-1.04909471538713,5.74611989975528,46.9564206164574));
#66562=CARTESIAN_POINT('Ctrl Pts',(-5.39650199857509,2.23523148769702,47.1151813787033));
#66563=CARTESIAN_POINT('Ctrl Pts',(-4.80486581436728,-3.32140905793637,
47.2739421409491));
#66564=CARTESIAN_POINT('Ctrl Pts',(0.184330329686807,-5.83819457998573,
47.4327029031951));
#66565=CARTESIAN_POINT('Ctrl Pts',(5.00482172556827,-3.01168609245668,47.5914636654409));
#66566=CARTESIAN_POINT('Ctrl Pts',(5.24474740393951,2.5712095000382,47.7502244276869));
#66567=CARTESIAN_POINT('Ctrl Pts',(0.684520055329939,5.80085561948134,47.9089851899327));
#66568=CARTESIAN_POINT('Ctrl Pts',(-4.50220095685495,3.72138148653313,48.0677459521787));
#66569=CARTESIAN_POINT('Ctrl Pts',(-5.56837013180732,-1.76401465396777,
48.2265067144245));
#66570=CARTESIAN_POINT('Ctrl Pts',(-1.53819687404933,-5.63493070062818,
48.3852674766705));
#66571=CARTESIAN_POINT('Ctrl Pts',(3.89978114767392,-4.3485860488743,48.5440282389163));
#66572=CARTESIAN_POINT('Ctrl Pts',(5.76856034267981,0.917717384099773,48.7027890011622));
#66573=CARTESIAN_POINT('Ctrl Pts',(2.35777690909515,5.34409783510322,48.8615497634081));
#66574=CARTESIAN_POINT('Ctrl Pts',(-3.21091597092679,4.87939670982634,49.020310525654));
#66575=CARTESIAN_POINT('Ctrl Pts',(-5.84088047565118,-0.0510773273967016,
49.1790712878999));
#66576=CARTESIAN_POINT('Ctrl Pts',(-3.12509275704243,-4.93480383440904,
49.3378320501458));
#66577=CARTESIAN_POINT('Ctrl Pts',(2.45087531001271,-5.3020471366244,49.4965928123917));
#66578=CARTESIAN_POINT('Ctrl Pts',(5.78372743038313,-0.816694946262622,
49.6553535746376));
#66579=CARTESIAN_POINT('Ctrl Pts',(3.82313554021223,4.41612140519068,49.8141143368834));
#66580=CARTESIAN_POINT('Ctrl Pts',(-1.63650677555656,5.60716855442876,49.9728750991293));
#66581=CARTESIAN_POINT('Ctrl Pts',(-5.59836810258563,1.66636376946,50.1316358613752));
#66582=CARTESIAN_POINT('Ctrl Pts',(-4.43643193774801,-3.79954803706259,
50.2903966236211));
#66583=CARTESIAN_POINT('Ctrl Pts',(0.785862249094534,-5.78799742135959,
50.4491573858669));
#66584=CARTESIAN_POINT('Ctrl Pts',(5.28891130109086,-2.47909476894502,50.6079181481129));
#66585=CARTESIAN_POINT('Ctrl Pts',(4.95138717842959,3.0987511409437,50.7666789103587));
#66586=CARTESIAN_POINT('Ctrl Pts',(0.0822022679789686,5.84052535405474,
50.9254396726047));
#66587=CARTESIAN_POINT('Ctrl Pts',(-4.86221666902701,3.23687236196503,51.0842004348505));
#66588=CARTESIAN_POINT('Ctrl Pts',(-5.35658639219748,-2.32926508734879,
51.2429611970965));
#66589=CARTESIAN_POINT('Ctrl Pts',(-0.948444630167017,-5.76358798039247,
51.4017219593423));
#66590=CARTESIAN_POINT('Ctrl Pts',(4.32774262801073,-3.92289910269379,51.5604827215883));
#66591=CARTESIAN_POINT('Ctrl Pts',(5.64304764041327,1.50814686030353,51.7192434838341));
#66592=CARTESIAN_POINT('Ctrl Pts',(1.79366308317505,5.55889074980541,51.87800424608));
#66593=CARTESIAN_POINT('Ctrl Pts',(-3.69733671593728,4.52196802655651,52.0367650083259));
#66594=CARTESIAN_POINT('Ctrl Pts',(-5.80442101600325,-0.653597959908777,
52.1955257705718));
#66595=CARTESIAN_POINT('Ctrl Pts',(-2.59912190387458,-5.2309711290559,52.3542865328177));
#66596=CARTESIAN_POINT('Ctrl Pts',(2.98497296589237,-5.02079973879747,52.5130472950635));
#66597=CARTESIAN_POINT('Ctrl Pts',(5.83712940008821,-0.215439065266698,
52.6718080573094));
#66598=CARTESIAN_POINT('Ctrl Pts',(3.34696670988424,4.78709802146808,52.8305688195553));
#66599=CARTESIAN_POINT('Ctrl Pts',(-2.20644214763509,5.4083367751423,52.9893295818012));
#66600=CARTESIAN_POINT('Ctrl Pts',(-5.74044775498584,1.07970051240847,53.1480903440471));
#66601=CARTESIAN_POINT('Ctrl Pts',(-4.02062023271376,-4.2371106391632,53.306851106293));
#66602=CARTESIAN_POINT('Ctrl Pts',(1.37900173798208,-5.675988709543,53.4656118685389));
#66603=CARTESIAN_POINT('Ctrl Pts',(5.51651919592013,-1.92002853761645,53.6243726307848));
#66604=CARTESIAN_POINT('Ctrl Pts',(4.60514978147925,3.59320039997198,53.7831333930307));
#66605=CARTESIAN_POINT('Ctrl Pts',(-0.520993379103106,5.81782257577076,
53.9418941552766));
#66606=CARTESIAN_POINT('Ctrl Pts',(-5.1703074851803,2.71779582251969,54.1006549175224));
#66607=CARTESIAN_POINT('Ctrl Pts',(-5.08759825172204,-2.86964068365571,
54.2594156797684));
#66608=CARTESIAN_POINT('Ctrl Pts',(-0.348563695575712,-5.83069438183342,
54.4181764420142));
#66609=CARTESIAN_POINT('Ctrl Pts',(4.70948700177826,-3.45531848087826,54.5769372042601));
#66610=CARTESIAN_POINT('Ctrl Pts',(5.45727134195117,2.08247043785393,54.735697966506));
#66611=CARTESIAN_POINT('Ctrl Pts',(1.21039425544677,5.71431880197442,54.8944587287519));
#66612=CARTESIAN_POINT('Ctrl Pts',(-4.14427262561643,4.11624805238744,55.0532194909978));
#66613=CARTESIAN_POINT('Ctrl Pts',(-5.70597461125989,-1.24913864717843,
55.2119802532437));
#66614=CARTESIAN_POINT('Ctrl Pts',(-2.04539434141439,-5.47127550140978,
55.3707410154896));
#66615=CARTESIAN_POINT('Ctrl Pts',(3.48719330707719,-4.68593389446471,55.5295017777355));
#66616=CARTESIAN_POINT('Ctrl Pts',(5.82819512322526,0.388117546408988,55.6882625399813));
#66617=CARTESIAN_POINT('Ctrl Pts',(2.83505473805949,5.10695195360438,55.8470233022273));
#66618=CARTESIAN_POINT('Ctrl Pts',(-2.75281434125286,5.15174793898243,56.0057840644731));
#66619=CARTESIAN_POINT('Ctrl Pts',(-5.82122364964165,0.481506848414017,
56.1645448267191));
#66620=CARTESIAN_POINT('Ctrl Pts',(-3.56187126228685,-4.6294240176411,56.3233055889649));
#66621=CARTESIAN_POINT('Ctrl Pts',(1.95741450308725,-5.50336461515325,56.4820663512108));
#66622=CARTESIAN_POINT('Ctrl Pts',(5.6852147252314,-1.34045781441613,56.6408271134567));
#66623=CARTESIAN_POINT('Ctrl Pts',(4.20973277369882,4.0492769228917,56.7995878757026));
#66624=CARTESIAN_POINT('Ctrl Pts',(-1.11862520028478,5.73298973359492,56.9583486379484));
#66625=CARTESIAN_POINT('Ctrl Pts',(-5.42318322211612,2.16969522366057,57.1171094001944));
#66626=CARTESIAN_POINT('Ctrl Pts',(-4.76427830577834,-3.3793706291715,57.2758701624402));
#66627=CARTESIAN_POINT('Ctrl Pts',(0.255039642783455,-5.83553325796587,
57.4346309246862));
#66628=CARTESIAN_POINT('Ctrl Pts',(5.04093751998252,-2.95083760038564,57.593391686932));
#66629=CARTESIAN_POINT('Ctrl Pts',(5.21321540145215,2.63455476357568,57.7521524491779));
#66630=CARTESIAN_POINT('Ctrl Pts',(0.614199307774883,5.80872213438946,57.9109132114238));
#66631=CARTESIAN_POINT('Ctrl Pts',(-4.54695075334007,3.66656957808212,58.0696739736697));
#66632=CARTESIAN_POINT('Ctrl Pts',(-5.54659259657899,-1.83133945291199,
58.2284347359156));
#66633=CARTESIAN_POINT('Ctrl Pts',(-1.469823472552,-5.65315067760911,58.3871954981615));
#66634=CARTESIAN_POINT('Ctrl Pts',(3.95217298989717,-4.30102572442254,58.5459562604074));
#66635=CARTESIAN_POINT('Ctrl Pts',(5.75702001129657,0.987529348296885,58.7047170226532));
#66636=CARTESIAN_POINT('Ctrl Pts',(2.29286646789146,5.37226739697831,58.8634777848992));
#66637=CARTESIAN_POINT('Ctrl Pts',(-3.26978850344612,4.84014222590088,59.022238547145));
#66638=CARTESIAN_POINT('Ctrl Pts',(-5.83983315943952,-0.121828954390395,
59.180999309391));
#66639=CARTESIAN_POINT('Ctrl Pts',(-3.06508412788734,-4.97229855430969,
59.3397600716368));
#66640=CARTESIAN_POINT('Ctrl Pts',(2.51492352172104,-5.27196863648781,59.4985208338828));
#66641=CARTESIAN_POINT('Ctrl Pts',(5.79319634491114,-0.746571988173542,
59.6572815961285));
#66642=CARTESIAN_POINT('Ctrl Pts',(3.76935891775212,4.46211014805548,59.8160423583745));
#66643=CARTESIAN_POINT('Ctrl Pts',(-1.70431092750091,5.58693277985496,59.9748031206203));
#66644=CARTESIAN_POINT('Ctrl Pts',(-5.61814335305001,1.59842387644741,60.1335638828663));
#66645=CARTESIAN_POINT('Ctrl Pts',(-4.39007937346456,-3.85301138317786,
60.2923246451121));
#66646=CARTESIAN_POINT('Ctrl Pts',(0.85591934543619,-5.77805293315363,60.451085407358));
#66647=CARTESIAN_POINT('Ctrl Pts',(5.31855453499689,-2.41484394578226,60.609846169604));
#66648=CARTESIAN_POINT('Ctrl Pts',(4.91348615676483,3.15850398313777,60.7686069318498));
#66649=CARTESIAN_POINT('Ctrl Pts',(0.0114451634727917,5.84109258892977,
60.9273676940957));
#66650=CARTESIAN_POINT('Ctrl Pts',(-4.90107079302665,3.17773483883697,61.0861284563416));
#66651=CARTESIAN_POINT('Ctrl Pts',(-5.32797705459145,-2.3939829009339,61.2448892185875));
#66652=CARTESIAN_POINT('Ctrl Pts',(-0.878555970616003,-5.77465436461024,
61.4036499808334));
#66653=CARTESIAN_POINT('Ctrl Pts',(4.37494637350877,-3.87018576468102,61.5624107430792));
#66654=CARTESIAN_POINT('Ctrl Pts',(5.62436416212133,1.57639506344776,61.7211715053253));
#66655=CARTESIAN_POINT('Ctrl Pts',(1.72619207112014,5.58021097789493,61.879932267571));
#66656=CARTESIAN_POINT('Ctrl Pts',(-3.75184373059352,4.47684735560896,62.038693029817));
#66657=CARTESIAN_POINT('Ctrl Pts',(-5.79607754850909,-0.723863713613315,
62.1974537920628));
#66658=CARTESIAN_POINT('Ctrl Pts',(-2.53556415053518,-5.26207260143168,
62.3562145543087));
#66659=CARTESIAN_POINT('Ctrl Pts',(3.04557500782399,-4.9842719123193,62.5149753165546));
#66660=CARTESIAN_POINT('Ctrl Pts',(5.8393108907227,-0.144713322484355,62.6737360788005));
#66661=CARTESIAN_POINT('Ctrl Pts',(3.28873108235841,4.82729132041423,62.8324968410464));
#66662=CARTESIAN_POINT('Ctrl Pts',(-2.27179586817918,5.38121149533645,62.9912576032922));
#66663=CARTESIAN_POINT('Ctrl Pts',(-5.75310584725087,1.01008253848138,63.1500183655383));
#66664=CARTESIAN_POINT('Ctrl Pts',(-3.96899762401232,-4.28550481096468,
63.3087791277839));
#66665=CARTESIAN_POINT('Ctrl Pts',(1.44765845933327,-5.65886725496703,63.4675398900301));
#66666=CARTESIAN_POINT('Ctrl Pts',(5.53937330139366,-1.85306153487257,63.6263006522757));
#66667=CARTESIAN_POINT('Ctrl Pts',(4.56128449565793,3.64872270443888,63.7850614145219));
#66668=CARTESIAN_POINT('Ctrl Pts',(-0.591431206752995,5.81108447296164,
63.9438221767675));
#66669=CARTESIAN_POINT('Ctrl Pts',(-5.20285100324211,2.65496422994348,64.1025829390136));
#66670=CARTESIAN_POINT('Ctrl Pts',(-5.05246263841092,-2.93106037325727,
64.2613437012593));
#66671=CARTESIAN_POINT('Ctrl Pts',(-0.277906137425253,-5.83448899244814,
64.4201044635054));
#66672=CARTESIAN_POINT('Ctrl Pts',(4.75099854928546,-3.3980150689637,64.5788652257511));
#66673=CARTESIAN_POINT('Ctrl Pts',(5.4316442425499,2.14842603935805,64.7376259879971));
#66674=CARTESIAN_POINT('Ctrl Pts',(1.14108321329899,5.72856201193147,64.896386750243));
#66675=CARTESIAN_POINT('Ctrl Pts',(-4.19383202760378,4.06574304998017,65.0551475124888));
#66676=CARTESIAN_POINT('Ctrl Pts',(-5.69042409457625,-1.31816814105151,
65.2139082747347));
#66677=CARTESIAN_POINT('Ctrl Pts',(-1.97896621392534,-5.49565158542271,
65.3726690369806));
#66678=CARTESIAN_POINT('Ctrl Pts',(3.54370199402013,-4.6433468319516,65.5314297992266));
#66679=CARTESIAN_POINT('Ctrl Pts',(5.82306589325152,0.458690774997357,65.6901905614723));
#66680=CARTESIAN_POINT('Ctrl Pts',(2.77298201911554,5.14092057377652,65.8489513237183));
#66681=CARTESIAN_POINT('Ctrl Pts',(-2.8150197007537,5.11802283197194,66.0077120859641));
#66682=CARTESIAN_POINT('Ctrl Pts',(-5.8266294045968,0.410954262303533,66.1664728482102));
#66683=CARTESIAN_POINT('Ctrl Pts',(-3.50552990064023,-4.67223220098639,
66.3252336104559));
#66684=CARTESIAN_POINT('Ctrl Pts',(2.0239376461872,-5.47924903874272,66.483994372702));
#66685=CARTESIAN_POINT('Ctrl Pts',(5.70103563724385,-1.27148979040063,66.6427551349476));
#66686=CARTESIAN_POINT('Ctrl Pts',(4.16037167269387,4.09997575227756,66.8015158971937));
#66687=CARTESIAN_POINT('Ctrl Pts',(-1.18799152691301,5.71901825108119,66.9602766594395));
#66688=CARTESIAN_POINT('Ctrl Pts',(-5.44906859341531,2.10384055680833,67.1190374216854));
#66689=CARTESIAN_POINT('Ctrl Pts',(-4.72299163925665,-3.43683627770202,
67.2777981839313));
#66690=CARTESIAN_POINT('Ctrl Pts',(0.325711528807802,-5.8320155713286,67.4365589461772));
#66691=CARTESIAN_POINT('Ctrl Pts',(5.07631355671921,-2.88955607283996,67.5953197084231));
#66692=CARTESIAN_POINT('Ctrl Pts',(5.18091835950451,2.6975134061513,67.754080470669));
#66693=CARTESIAN_POINT('Ctrl Pts',(0.54378842645952,5.81573621921296,67.9128412329148));
#66694=CARTESIAN_POINT('Ctrl Pts',(-4.59103328471497,3.61121960047518,68.0716019951608));
#66695=CARTESIAN_POINT('Ctrl Pts',(-5.52400109878079,-1.8983955027565,68.2303627574066));
#66696=CARTESIAN_POINT('Ctrl Pts',(-1.40123437443171,-5.67054105461978,
68.3891235196526));
#66697=CARTESIAN_POINT('Ctrl Pts',(4.00398485065851,-4.2528342243631,68.5478842818984));
#66698=CARTESIAN_POINT('Ctrl Pts',(5.74463483711628,1.05719639254342,68.7066450441444));
#66699=CARTESIAN_POINT('Ctrl Pts',(2.22761954848948,5.39964857850993,68.8654058063901));
#66700=CARTESIAN_POINT('Ctrl Pts',(-3.32818119444006,4.80017745101086,69.0241665686361));
#66701=CARTESIAN_POINT('Ctrl Pts',(-5.83792884759976,-0.192562702982879,
69.182927330882));
#66702=CARTESIAN_POINT('Ctrl Pts',(-3.00462569757752,-5.00906358930226,
69.3416880931278));
#66703=CARTESIAN_POINT('Ctrl Pts',(2.57860266835449,-5.24111647485266,69.5004488553739));
#66704=CARTESIAN_POINT('Ctrl Pts',(5.80181510776444,-0.676339470630766,
69.6592096176196));
#66705=CARTESIAN_POINT('Ctrl Pts',(3.71502914179852,4.50744407617051,69.8179703798656));
#66706=CARTESIAN_POINT('Ctrl Pts',(-1.77186497178415,5.56587712278864,69.9767311421114));
#66707=CARTESIAN_POINT('Ctrl Pts',(-5.63709414086971,1.53024941470006,70.1354919043573));
#66708=CARTESIAN_POINT('Ctrl Pts',(-4.34308256494864,-3.90590929979895,
70.2942526666033));
#66709=CARTESIAN_POINT('Ctrl Pts',(0.925850835597592,-5.7672605155689,70.453013428849));
#66710=CARTESIAN_POINT('Ctrl Pts',(5.34741727092293,-2.35023874422409,70.6117741910951));
#66711=CARTESIAN_POINT('Ctrl Pts',(4.87486408091236,3.21779331481187,70.7705349533408));
#66712=CARTESIAN_POINT('Ctrl Pts',(-0.0593136206115266,5.8408026433554,
70.9292957155867));
#66713=CARTESIAN_POINT('Ctrl Pts',(-4.93920568479356,3.11813098306019,71.0880564778327));
#66714=CARTESIAN_POINT('Ctrl Pts',(-5.29858583625043,-2.45834939748262,
71.2468172400784));
#66715=CARTESIAN_POINT('Ctrl Pts',(-0.808538382959287,-5.78487331818929,
71.4055780023245));
#66716=CARTESIAN_POINT('Ctrl Pts',(4.42150809554277,-3.81690447683292,71.5643387645703));
#66717=CARTESIAN_POINT('Ctrl Pts',(5.60485530828073,1.64441193058638,71.7230995268162));
#66718=CARTESIAN_POINT('Ctrl Pts',(1.65846774034549,5.6007123099165,71.8818602890621));
#66719=CARTESIAN_POINT('Ctrl Pts',(-3.80580016211055,4.43106970722601,72.040621051308));
#66720=CARTESIAN_POINT('Ctrl Pts',(-5.78688350652351,-0.794023240304163,
72.1993818135539));
#66721=CARTESIAN_POINT('Ctrl Pts',(-2.47163430310789,-5.29240186455242,
72.3581425757998));
#66722=CARTESIAN_POINT('Ctrl Pts',(3.10573011156498,-4.94701264384235,72.5169033380457));
#66723=CARTESIAN_POINT('Ctrl Pts',(5.84063546237199,-0.0739663430189528,
72.6756641002916));
#66724=CARTESIAN_POINT('Ctrl Pts',(3.23001283348305,4.86677621426665,72.8344248625374));
#66725=CARTESIAN_POINT('Ctrl Pts',(-2.33681620263615,5.35329652264041,72.9931856247833));
#66726=CARTESIAN_POINT('Ctrl Pts',(-5.76491967112249,0.940316334922364,
73.1519463870293));
#66727=CARTESIAN_POINT('Ctrl Pts',(-3.9167925648334,-4.33327008485316,73.3107071492751));
#66728=CARTESIAN_POINT('Ctrl Pts',(1.51610273677804,-5.64091536151285,73.469467911521));
#66729=CARTESIAN_POINT('Ctrl Pts',(5.56141450372903,-1.78582259531264,73.6282286737669));
#66730=CARTESIAN_POINT('Ctrl Pts',(4.51674984124932,3.70370955877901,73.7869894360128));
#66731=CARTESIAN_POINT('Ctrl Pts',(-0.661782241861996,5.80349359339467,
73.9457501982587));
#66732=CARTESIAN_POINT('Ctrl Pts',(-5.23463100281954,2.59174302131558,74.1045109605046));
#66733=CARTESIAN_POINT('Ctrl Pts',(-5.01658557611066,-2.99204992969303,
74.2632717227504));
#66734=CARTESIAN_POINT('Ctrl Pts',(-0.207207796543587,-5.83742739169134,
74.4220324849964));
#66735=CARTESIAN_POINT('Ctrl Pts',(4.79181288766461,-3.34021299827244,74.5807932472422));
#66736=CARTESIAN_POINT('Ctrl Pts',(5.4052200492518,2.21406635929985,74.7395540094881));
#66737=CARTESIAN_POINT('Ctrl Pts',(1.07160471716756,5.7419645553035,74.8983147717341));
#66738=CARTESIAN_POINT('Ctrl Pts',(-4.2427759846608,4.01464139970224,75.0570755339798));
#66739=CARTESIAN_POINT('Ctrl Pts',(-5.67403850804756,-1.38700419372482,
75.2158362962259));
#66740=CARTESIAN_POINT('Ctrl Pts',(-1.91224767310636,-5.51922118246009,
75.3745970584716));
#66741=CARTESIAN_POINT('Ctrl Pts',(3.59969064262747,-4.60007835820185,75.5333578207176));
#66742=CARTESIAN_POINT('Ctrl Pts',(5.81708212824635,0.529196690705634,75.6921185829634));
#66743=CARTESIAN_POINT('Ctrl Pts',(2.71050236500702,5.17413476375605,75.8508793452094));
#66744=CARTESIAN_POINT('Ctrl Pts',(-2.87681195605961,5.08354665501262,76.0096401074552));
#66745=CARTESIAN_POINT('Ctrl Pts',(-5.83118010157501,0.340341368647152,
76.1684008697012));
#66746=CARTESIAN_POINT('Ctrl Pts',(-3.4486741024136,-4.71435473416655,76.327161631947));
#66747=CARTESIAN_POINT('Ctrl Pts',(2.09016377639872,-5.45432938243075,76.4859223941929));
#66748=CARTESIAN_POINT('Ctrl Pts',(5.71601992216721,-1.20233517523405,76.6446831564388));
#66749=CARTESIAN_POINT('Ctrl Pts',(4.11040003706624,4.15007291014307,76.8034439186847));
#66750=CARTESIAN_POINT('Ctrl Pts',(-1.25718351576172,5.7042075025295,76.9622046809306));
#66751=CARTESIAN_POINT('Ctrl Pts',(-5.47415431379396,2.03767715131415,77.1209654431764));
#66752=CARTESIAN_POINT('Ctrl Pts',(-4.68101187362137,-3.49379757044288,
77.2797262054223));
#66753=CARTESIAN_POINT('Ctrl Pts',(0.39633561665894,-5.82764203629436,77.4384869676682));
#66754=CARTESIAN_POINT('Ctrl Pts',(5.11094464434401,-2.82785050288533,77.5972477299141));
#66755=CARTESIAN_POINT('Ctrl Pts',(5.1478610176884,2.76007618858267,77.75600849216));
#66756=CARTESIAN_POINT('Ctrl Pts',(0.473297744182263,5.82189684463481,77.9147692544059));
#66757=CARTESIAN_POINT('Ctrl Pts',(-4.63444208186731,3.55533967632268,78.0735300166519));
#66758=CARTESIAN_POINT('Ctrl Pts',(-5.50059895371541,-1.96517296302448,
78.2322907788976));
#66759=CARTESIAN_POINT('Ctrl Pts',(-1.33243964514028,-5.6870992796219,78.3910515411437));
#66760=CARTESIAN_POINT('Ctrl Pts',(4.0552091265661,-4.20401862079985,78.5498123033894));
#66761=CARTESIAN_POINT('Ctrl Pts',(5.73140663766353,1.12670829319891,78.7085730656353));
#66762=CARTESIAN_POINT('Ctrl Pts',(2.16204572587615,5.42623736150913,78.8673338278812));
#66763=CARTESIAN_POINT('Ctrl Pts',(-3.38608547477963,4.75950824998793,79.0260945901272));
#66764=CARTESIAN_POINT('Ctrl Pts',(-5.83516781958967,-0.263268192994679,
79.184855352373));
#66765=CARTESIAN_POINT('Ctrl Pts',(-2.94372633838929,-5.04509354411697,
79.3436161146189));
#66766=CARTESIAN_POINT('Ctrl Pts',(2.64190340499678,-5.2094951792744,79.5023768768649));
#66767=CARTESIAN_POINT('Ctrl Pts',(5.80958245413942,-0.606007700257848,
79.6611376391106));
#66768=CARTESIAN_POINT('Ctrl Pts',(3.66015418524723,4.55211653678098,79.8198984013567));
#66769=CARTESIAN_POINT('Ctrl Pts',(-1.8391589948488,5.54400467314773,79.9786591636023));
#66770=CARTESIAN_POINT('Ctrl Pts',(-5.65521768501588,1.46185038882208,80.1374199258485));
#66771=CARTESIAN_POINT('Ctrl Pts',(-4.29544840898361,-3.95823402415551,
80.2961806880941));
#66772=CARTESIAN_POINT('Ctrl Pts',(0.995646457131763,-5.7556217523925,80.4549414503402));
#66773=CARTESIAN_POINT('Ctrl Pts',(5.3754952732605,-2.28528864508612,80.613702212586));
#66774=CARTESIAN_POINT('Ctrl Pts',(4.83552661866532,3.27661043525698,80.7724629748319));
#66775=CARTESIAN_POINT('Ctrl Pts',(-0.130063700425983,5.83965555987772,
80.9312237370779));
#66776=CARTESIAN_POINT('Ctrl Pts',(-4.9766157480213,3.05806954150856,81.0899844993236));
#66777=CARTESIAN_POINT('Ctrl Pts',(-5.26841705035579,-2.52235513122241,
81.2487452615697));
#66778=CARTESIAN_POINT('Ctrl Pts',(-0.738402142242399,-5.79424334147416,
81.4075060238153));
#66779=CARTESIAN_POINT('Ctrl Pts',(4.46742096110774,-3.76306305822547,81.5662667860616));
#66780=CARTESIAN_POINT('Ctrl Pts',(5.58452394195224,1.71218748032981,81.7250275483071));
#66781=CARTESIAN_POINT('Ctrl Pts',(1.590500029138,5.62039173713168,81.8837883105533));
#66782=CARTESIAN_POINT('Ctrl Pts',(-3.85919809188181,4.38464179959952,82.0425490727989));
#66783=CARTESIAN_POINT('Ctrl Pts',(-5.776840240228,-0.864066244683674,82.201309835045));
#66784=CARTESIAN_POINT('Ctrl Pts',(-2.40734174146917,-5.3219544664209,82.3600705972908));
#66785=CARTESIAN_POINT('Ctrl Pts',(3.16542944584671,-4.9090274034195,82.5188313595367));
#66786=CARTESIAN_POINT('Ctrl Pts',(5.84110292736961,-0.00320850467390637,
82.6775921217826));
#66787=CARTESIAN_POINT('Ctrl Pts',(3.1708205673024,4.90554690034638,82.8363528840285));
#66788=CARTESIAN_POINT('Ctrl Pts',(-2.40149358463894,5.32459596941663,82.9951136462743));
#66789=CARTESIAN_POINT('Ctrl Pts',(-5.7758875400995,0.870412109585264,83.1538744085203));
#66790=CARTESIAN_POINT('Ctrl Pts',(-3.86401262590961,-4.3803993931662,83.3126351707661));
#66791=CARTESIAN_POINT('Ctrl Pts',(1.58432435304567,-5.62213577491609,83.4713959330121));
#66792=CARTESIAN_POINT('Ctrl Pts',(5.58263989986849,-1.71832137308609,83.6301566952579));
#66793=CARTESIAN_POINT('Ctrl Pts',(4.47155171880276,3.75815248538495,83.7889174575037));
#66794=CARTESIAN_POINT('Ctrl Pts',(-0.732034944345687,5.79505183303421,
83.9476782197497));
#66795=CARTESIAN_POINT('Ctrl Pts',(-5.26564514937354,2.52813997655405,84.1064389819955));
#66796=CARTESIAN_POINT('Ctrl Pts',(-4.97996786863125,-3.05259753396621,
84.2651997442416));
#66797=CARTESIAN_POINT('Ctrl Pts',(-0.136487592502867,-5.83951464301881,
84.4239605064873));
#66798=CARTESIAN_POINT('Ctrl Pts',(4.83194039314673,-3.28191022714265,84.5827212687333));
#66799=CARTESIAN_POINT('Ctrl Pts',(5.3779712939643,2.27936160776507,84.7414820309791));
#66800=CARTESIAN_POINT('Ctrl Pts',(1.00202900079473,5.75456307304708,84.9002427932251));
#66801=CARTESIAN_POINT('Ctrl Pts',(-4.29121230689459,3.96287665367137,85.059003555471));
#66802=CARTESIAN_POINT('Ctrl Pts',(-5.65660000441566,-1.45549506770408,
85.2177643177168));
#66803=CARTESIAN_POINT('Ctrl Pts',(-1.84567038925739,-5.54225213649743,
85.3765250799627));
#66804=CARTESIAN_POINT('Ctrl Pts',(3.65595928985271,-4.55561497937659,85.5352858422086));
#66805=CARTESIAN_POINT('Ctrl Pts',(5.8086947012646,0.598627392648328,85.6940466044544));
#66806=CARTESIAN_POINT('Ctrl Pts',(2.65061116100751,5.20851728785982,85.8528073667005));
#66807=CARTESIAN_POINT('Ctrl Pts',(-2.94405900471206,5.04447882807405,86.0115681289463));
#66808=CARTESIAN_POINT('Ctrl Pts',(-5.34253328840157,1.07278402652743,86.1438687641512));
#66809=CARTESIAN_POINT('Ctrl Pts',(-4.62260421807956,-2.25450493511227,
86.2497092723151));
#66810=CARTESIAN_POINT('Ctrl Pts',(-3.53826020855044,-3.54670961616112,
86.3026295263971));
#66811=CARTESIAN_POINT('Ctrl Pts',(-2.86929757049814,-4.02374147429149,
86.3290896534381));
#66812=CARTESIAN_POINT('',(-2.16917135428524,4.44050218283342,86.));
#66813=CARTESIAN_POINT('Ctrl Pts',(-2.17574227734826,4.44486702454923,86.));
#66814=CARTESIAN_POINT('Ctrl Pts',(-2.28013295862628,4.38716599510334,86.));
#66815=CARTESIAN_POINT('Ctrl Pts',(-2.38203491056673,4.32558764363711,86.));
#66816=CARTESIAN_POINT('Ctrl Pts',(-2.48120820121107,4.26013722079047,86.));
#66817=CARTESIAN_POINT('Ctrl Pts',(-2.60006688906204,4.18169521963978,86.));
#66818=CARTESIAN_POINT('Ctrl Pts',(-2.7150074127347,4.09769239705542,86.));
#66819=CARTESIAN_POINT('Ctrl Pts',(-2.825877147636,4.00855468944723,86.));
#66820=CARTESIAN_POINT('Ctrl Pts',(-2.93875239431318,3.9178045785764,86.));
#66821=CARTESIAN_POINT('Ctrl Pts',(-3.04740870522866,3.82173148785291,86.));
#66822=CARTESIAN_POINT('Ctrl Pts',(-3.15164741290182,3.72074618418362,86.));
#66823=CARTESIAN_POINT('Ctrl Pts',(-3.25648521909179,3.61918048051708,86.));
#66824=CARTESIAN_POINT('Ctrl Pts',(-3.35685490813916,3.51264518527105,86.));
#66825=CARTESIAN_POINT('Ctrl Pts',(-3.45251018852357,3.40153010769327,86.));
#66826=CARTESIAN_POINT('Ctrl Pts',(-3.48145067837577,3.36791225866138,86.));
#66827=CARTESIAN_POINT('Ctrl Pts',(-3.50995929996644,3.33387504208837,86.));
#66828=CARTESIAN_POINT('Ctrl Pts',(-3.53802835306874,3.2994289123823,86.));
#66829=CARTESIAN_POINT('Ctrl Pts',(-3.55893895860226,3.27376757539972,86.));
#66830=CARTESIAN_POINT('Ctrl Pts',(-3.57960560368256,3.24787929661303,86.));
#66831=CARTESIAN_POINT('Ctrl Pts',(-3.60002494885949,3.22176835839145,86.));
#66832=CARTESIAN_POINT('Ctrl Pts',(-3.61193639941707,3.20653676565705,86.));
#66833=CARTESIAN_POINT('Ctrl Pts',(-3.62375830311465,3.19123627397227,86.));
#66834=CARTESIAN_POINT('Ctrl Pts',(-3.63548790188773,3.17587102356872,86.));
#66835=CARTESIAN_POINT('Ctrl Pts',(-3.72304104356389,3.06118031918079,86.));
#66836=CARTESIAN_POINT('Ctrl Pts',(-3.80549810494951,2.94282892853622,86.));
#66837=CARTESIAN_POINT('Ctrl Pts',(-3.88269282098784,2.82123575460696,86.));
#66838=CARTESIAN_POINT('Ctrl Pts',(-3.96010237178875,2.69930418393253,86.));
#66839=CARTESIAN_POINT('Ctrl Pts',(-4.03222060518193,2.57411198603205,86.));
#66840=CARTESIAN_POINT('Ctrl Pts',(-4.09883515477919,2.44605409339683,86.));
#66841=CARTESIAN_POINT('Ctrl Pts',(-4.16485320331115,2.31914289723916,86.));
#66842=CARTESIAN_POINT('Ctrl Pts',(-4.2254659552961,2.18941632853557,86.));
#66843=CARTESIAN_POINT('Ctrl Pts',(-4.28041834739517,2.05724343991072,86.));
#66844=CARTESIAN_POINT('Ctrl Pts',(-4.33438117280193,1.92745068221766,86.));
#66845=CARTESIAN_POINT('Ctrl Pts',(-4.38288583069982,1.79529822126205,86.));
#66846=CARTESIAN_POINT('Ctrl Pts',(-4.42564090526442,1.66113144401598,86.));
#66847=CARTESIAN_POINT('Ctrl Pts',(-4.43255967958786,1.63942011119941,86.));
#66848=CARTESIAN_POINT('Ctrl Pts',(-4.43932777954855,1.61765603376178,86.));
#66849=CARTESIAN_POINT('Ctrl Pts',(-4.4459438397712,1.59584068384471,86.));
#66850=CARTESIAN_POINT('Ctrl Pts',(-4.45171251084707,1.57681945764039,86.));
#66851=CARTESIAN_POINT('Ctrl Pts',(-4.45736585345657,1.55775815091916,86.));
#66852=CARTESIAN_POINT('Ctrl Pts',(-4.46289825998277,1.53867450299572,86.));
#66853=CARTESIAN_POINT('Ctrl Pts',(-4.50224730205451,1.40294274476988,86.));
#66854=CARTESIAN_POINT('Ctrl Pts',(-4.53554254717084,1.2658880814313,86.));
#66855=CARTESIAN_POINT('Ctrl Pts',(-4.56258502829437,1.12787819891714,86.));
#66856=CARTESIAN_POINT('Ctrl Pts',(-4.58931759393923,0.991449953775849,
86.));
#66857=CARTESIAN_POINT('Ctrl Pts',(-4.60994008626122,0.854087541637941,
86.));
#66858=CARTESIAN_POINT('Ctrl Pts',(-4.62421031200347,0.716138535076822,
86.));
#66859=CARTESIAN_POINT('Ctrl Pts',(-4.63813932416541,0.581488009932714,
86.));
#66860=CARTESIAN_POINT('Ctrl Pts',(-4.64601628194546,0.446277995360083,
86.));
#66861=CARTESIAN_POINT('Ctrl Pts',(-4.64756630557454,0.310834136529796,
86.));
#66862=CARTESIAN_POINT('Ctrl Pts',(-4.64793240287716,0.278843894287929,
86.));
#66863=CARTESIAN_POINT('Ctrl Pts',(-4.6479453277195,0.246840640295154,86.));
#66864=CARTESIAN_POINT('Ctrl Pts',(-4.64760103388387,0.214828741346587,
86.));
#66865=CARTESIAN_POINT('Ctrl Pts',(-4.64657805635091,0.119713900408526,
86.));
#66866=CARTESIAN_POINT('Ctrl Pts',(-4.64240219271064,0.0245223992060761,
86.));
#66867=CARTESIAN_POINT('Ctrl Pts',(-4.63512171526216,-0.0706009649893001,
86.));
#66868=CARTESIAN_POINT('Ctrl Pts',(-4.63272301775774,-0.101941241491998,
86.));
#66869=CARTESIAN_POINT('Ctrl Pts',(-4.62998723239254,-0.133274083991166,
86.));
#66870=CARTESIAN_POINT('Ctrl Pts',(-4.62691585213729,-0.16459419159554,
86.));
#66871=CARTESIAN_POINT('Ctrl Pts',(-4.62511596030474,-0.182948417118559,
86.));
#66872=CARTESIAN_POINT('Ctrl Pts',(-4.62320081633973,-0.201298267969776,
86.));
#66873=CARTESIAN_POINT('Ctrl Pts',(-4.62117070299388,-0.21964266601306,
86.));
#66874=CARTESIAN_POINT('Ctrl Pts',(-4.61910605502354,-0.238299123921961,
86.));
#66875=CARTESIAN_POINT('Ctrl Pts',(-4.6169235721841,-0.256940116225532,
86.));
#66876=CARTESIAN_POINT('Ctrl Pts',(-4.61462417515337,-0.275562596752177,
86.));
#66877=CARTESIAN_POINT('Ctrl Pts',(-4.59791089402231,-0.410921018216574,
86.));
#66878=CARTESIAN_POINT('Ctrl Pts',(-4.57502130177171,-0.545336418557933,
86.));
#66879=CARTESIAN_POINT('Ctrl Pts',(-4.54619383694625,-0.678403869974182,
86.));
#66880=CARTESIAN_POINT('Ctrl Pts',(-4.51690235263596,-0.81361323330078,
86.));
#66881=CARTESIAN_POINT('Ctrl Pts',(-4.48148002405017,-0.947431726142265,
86.));
#66882=CARTESIAN_POINT('Ctrl Pts',(-4.44012512005541,-1.07942238906511,
86.));
#66883=CARTESIAN_POINT('Ctrl Pts',(-4.39891579514076,-1.21094841351862,
86.));
#66884=CARTESIAN_POINT('Ctrl Pts',(-4.35181516564808,-1.34066022876501,
86.));
#66885=CARTESIAN_POINT('Ctrl Pts',(-4.29897383984103,-1.46810153698611,
86.));
#66886=CARTESIAN_POINT('Ctrl Pts',(-4.26316764637209,-1.55445796480857,
86.));
#66887=CARTESIAN_POINT('Ctrl Pts',(-4.22472458946287,-1.639771352916,86.));
#66888=CARTESIAN_POINT('Ctrl Pts',(-4.18368102987994,-1.72389071907676,
86.));
#66889=CARTESIAN_POINT('Ctrl Pts',(-4.16189573536735,-1.76853999376555,
86.));
#66890=CARTESIAN_POINT('Ctrl Pts',(-4.13937765883534,-1.81285273679093,
86.));
#66891=CARTESIAN_POINT('Ctrl Pts',(-4.11613135978827,-1.85680534418916,
86.));
#66892=CARTESIAN_POINT('Ctrl Pts',(-4.10598652796122,-1.87598653985015,
86.));
#66893=CARTESIAN_POINT('Ctrl Pts',(-4.09570182816448,-1.8951012704791,86.));
#66894=CARTESIAN_POINT('Ctrl Pts',(-4.08528136703263,-1.91414066944428,
86.));
#66895=CARTESIAN_POINT('Ctrl Pts',(-4.07459370444932,-1.93366827665418,
86.));
#66896=CARTESIAN_POINT('Ctrl Pts',(-4.06376686324371,-1.95311008122927,
86.));
#66897=CARTESIAN_POINT('Ctrl Pts',(-4.05280165642382,-1.97246424292779,
86.));
#66898=CARTESIAN_POINT('Ctrl Pts',(-3.98545341209713,-2.09133740530588,
86.));
#66899=CARTESIAN_POINT('Ctrl Pts',(-3.91288886269624,-2.20690686036164,
86.));
#66900=CARTESIAN_POINT('Ctrl Pts',(-3.83535609314517,-2.31888838615919,
86.));
#66901=CARTESIAN_POINT('Ctrl Pts',(-3.75793727989042,-2.43070532348649,
86.));
#66902=CARTESIAN_POINT('Ctrl Pts',(-3.67556431499777,-2.53894540267671,
86.));
#66903=CARTESIAN_POINT('Ctrl Pts',(-3.58844692437017,-2.6432897533722,86.));
#66904=CARTESIAN_POINT('Ctrl Pts',(-3.55106838804729,-2.68805967903758,
86.));
#66905=CARTESIAN_POINT('Ctrl Pts',(-3.51281602034817,-2.7321119355856,86.));
#66906=CARTESIAN_POINT('Ctrl Pts',(-3.47370464217661,-2.77541893263456,
86.));
#66907=CARTESIAN_POINT('Ctrl Pts',(-3.45527487716358,-2.79582572514213,
86.));
#66908=CARTESIAN_POINT('Ctrl Pts',(-3.43665436275494,-2.81606701722102,
86.));
#66909=CARTESIAN_POINT('Ctrl Pts',(-3.41784457942235,-2.83613979970913,
86.));
#66910=CARTESIAN_POINT('Ctrl Pts',(-3.40161580152966,-2.85345827291681,
86.));
#66911=CARTESIAN_POINT('Ctrl Pts',(-3.38525177230088,-2.87064524159307,
86.));
#66912=CARTESIAN_POINT('Ctrl Pts',(-3.36875789576418,-2.88769480011766,
86.));
#66913=CARTESIAN_POINT('Ctrl Pts',(-3.27548691461708,-2.98410809920928,
86.));
#66914=CARTESIAN_POINT('Ctrl Pts',(-3.1780247285723,-3.07617507300169,86.));
#66915=CARTESIAN_POINT('Ctrl Pts',(-3.07658549505738,-3.16359906081916,
86.));
#66916=CARTESIAN_POINT('Ctrl Pts',(-2.97674507744291,-3.24964513146433,
86.));
#66917=CARTESIAN_POINT('Ctrl Pts',(-2.87305144560376,-3.33119379608769,
86.));
#66918=CARTESIAN_POINT('Ctrl Pts',(-2.76568166074672,-3.40792026882373,
86.));
#66919=CARTESIAN_POINT('Ctrl Pts',(-2.691638695275,-3.46083138882947,86.));
#66920=CARTESIAN_POINT('Ctrl Pts',(-2.61584694697416,-3.51144841450292,
86.));
#66921=CARTESIAN_POINT('Ctrl Pts',(-2.53835875722777,-3.5596515025498,86.));
#66922=CARTESIAN_POINT('Ctrl Pts',(-4.94096920053978,-0.0044629540342261,
85.1776795453431));
#66923=CARTESIAN_POINT('Ctrl Pts',(-4.94470425404279,-0.419442432737937,
85.1910411361343));
#66924=CARTESIAN_POINT('Ctrl Pts',(-4.89679105157154,-0.83357493998294,
85.2044027269256));
#66925=CARTESIAN_POINT('Ctrl Pts',(-4.79388045230233,-1.23355929227409,
85.2177643177168));
#66926=CARTESIAN_POINT('Ctrl Pts',(-4.38629013269605,-2.81774742396872,
85.2706845717988));
#66927=CARTESIAN_POINT('Ctrl Pts',(-3.11598026097668,-4.17999978023304,
85.3236048258808));
#66928=CARTESIAN_POINT('Ctrl Pts',(-1.5638870452654,-4.69668643217841,85.3765250799627));
#66929=CARTESIAN_POINT('Ctrl Pts',(-0.0117938295540432,-5.21337308412381,
85.4294453340447));
#66930=CARTESIAN_POINT('Ctrl Pts',(1.82208273014937,-4.88449403175019,85.4823655881266));
#66931=CARTESIAN_POINT('Ctrl Pts',(3.09781024523634,-3.86101411022591,85.5352858422086));
#66932=CARTESIAN_POINT('Ctrl Pts',(4.37353776032332,-2.83753418870164,85.5882060962905));
#66933=CARTESIAN_POINT('Ctrl Pts',(5.0911162307939,-1.11945339802691,85.6411263503725));
#66934=CARTESIAN_POINT('Ctrl Pts',(4.92355820931981,0.507901979845797,85.6940466044544));
#66935=CARTESIAN_POINT('Ctrl Pts',(4.75600018784572,2.1352573577185,85.7469668585364));
#66936=CARTESIAN_POINT('Ctrl Pts',(3.70330567442676,3.67188732278906,85.7998871126184));
#66937=CARTESIAN_POINT('Ctrl Pts',(2.24451339009742,4.41286256202677,85.8528073667004));
#66938=CARTESIAN_POINT('Ctrl Pts',(0.892016244518137,5.09984651908455,85.9018715778003));
#66939=CARTESIAN_POINT('Ctrl Pts',(-0.809554018707134,5.10290237899098,
85.9509357889001));
#66940=CARTESIAN_POINT('Ctrl Pts',(-2.17574227734751,4.44486702454959,86.));
#66941=CARTESIAN_POINT('',(-2.53835875722709,-3.55965150255029,26.));
#66942=CARTESIAN_POINT('Ctrl Pts',(-2.54472725763298,-3.56250530678305,
26.));
#66943=CARTESIAN_POINT('Ctrl Pts',(-2.63508309937759,-3.50703322951937,
26.));
#66944=CARTESIAN_POINT('Ctrl Pts',(-2.72311007746572,-3.44818980724315,
26.));
#66945=CARTESIAN_POINT('Ctrl Pts',(-2.80858488092082,-3.38601400346164,
26.));
#66946=CARTESIAN_POINT('Ctrl Pts',(-2.91385291450225,-3.30944027253914,
26.));
#66947=CARTESIAN_POINT('Ctrl Pts',(-3.01525129898596,-3.22781364096124,
26.));
#66948=CARTESIAN_POINT('Ctrl Pts',(-3.11268784287649,-3.1415518359691,26.));
#66949=CARTESIAN_POINT('Ctrl Pts',(-3.17680627098234,-3.08478698039414,
26.));
#66950=CARTESIAN_POINT('Ctrl Pts',(-3.23920859831056,-3.02601391139215,
26.));
#66951=CARTESIAN_POINT('Ctrl Pts',(-3.29986195943645,-2.96534150637499,
26.));
#66952=CARTESIAN_POINT('Ctrl Pts',(-3.33570437568566,-2.9294878363541,26.));
#66953=CARTESIAN_POINT('Ctrl Pts',(-3.37093593415121,-2.89297075792499,
26.));
#66954=CARTESIAN_POINT('Ctrl Pts',(-3.40554888779674,-2.85581160143786,
26.));
#66955=CARTESIAN_POINT('Ctrl Pts',(-3.4189115430604,-2.84146596069563,26.));
#66956=CARTESIAN_POINT('Ctrl Pts',(-3.43218080021828,-2.82702583304496,
26.));
#66957=CARTESIAN_POINT('Ctrl Pts',(-3.44534999888201,-2.81249952818835,
26.));
#66958=CARTESIAN_POINT('Ctrl Pts',(-3.53470458244056,-2.71393681725578,
26.));
#66959=CARTESIAN_POINT('Ctrl Pts',(-3.61953742655147,-2.6113223183339,26.));
#66960=CARTESIAN_POINT('Ctrl Pts',(-3.69975229053408,-2.50508736800556,
26.));
#66961=CARTESIAN_POINT('Ctrl Pts',(-3.78158309623279,-2.39671229701354,
26.));
#66962=CARTESIAN_POINT('Ctrl Pts',(-3.85860846570253,-2.28456889207013,
26.));
#66963=CARTESIAN_POINT('Ctrl Pts',(-3.93069241652625,-2.16907329602735,
26.));
#66964=CARTESIAN_POINT('Ctrl Pts',(-3.96222914501164,-2.11854397275863,
26.));
#66965=CARTESIAN_POINT('Ctrl Pts',(-3.99281958123178,-2.06737253695488,
26.));
#66966=CARTESIAN_POINT('Ctrl Pts',(-4.02244999738294,-2.01559181929177,
26.));
#66967=CARTESIAN_POINT('Ctrl Pts',(-4.03719360535128,-1.98982658543039,
26.));
#66968=CARTESIAN_POINT('Ctrl Pts',(-4.05169949925962,-1.96391048284628,
26.));
#66969=CARTESIAN_POINT('Ctrl Pts',(-4.06596584566683,-1.93784746217908,
26.));
#66970=CARTESIAN_POINT('Ctrl Pts',(-4.07831325232761,-1.91529012999318,
26.));
#66971=CARTESIAN_POINT('Ctrl Pts',(-4.09048280358417,-1.89261955019595,
26.));
#66972=CARTESIAN_POINT('Ctrl Pts',(-4.10246124623198,-1.86986160408455,
26.));
#66973=CARTESIAN_POINT('Ctrl Pts',(-4.16682782765767,-1.74757098296373,
26.));
#66974=CARTESIAN_POINT('Ctrl Pts',(-4.22575033277333,-1.62263418183686,
26.));
#66975=CARTESIAN_POINT('Ctrl Pts',(-4.27912376767658,-1.49549834075104,
26.));
#66976=CARTESIAN_POINT('Ctrl Pts',(-4.333101839857,-1.36692225005554,26.));
#66977=CARTESIAN_POINT('Ctrl Pts',(-4.38140486252481,-1.23609633060621,
26.));
#66978=CARTESIAN_POINT('Ctrl Pts',(-4.42388482122499,-1.10344716235086,
26.));
#66979=CARTESIAN_POINT('Ctrl Pts',(-4.46661826556875,-0.970006452370537,
26.));
#66980=CARTESIAN_POINT('Ctrl Pts',(-4.50345940350737,-0.83471991605117,
26.));
#66981=CARTESIAN_POINT('Ctrl Pts',(-4.53421101307421,-0.697996575960625,
26.));
#66982=CARTESIAN_POINT('Ctrl Pts',(-4.55727472024934,-0.595454070892716,
26.));
#66983=CARTESIAN_POINT('Ctrl Pts',(-4.57691215392772,-0.492102769524819,
26.));
#66984=CARTESIAN_POINT('Ctrl Pts',(-4.59302069983613,-0.388109915197262,
26.));
#66985=CARTESIAN_POINT('Ctrl Pts',(-4.59983051322201,-0.344147416318648,
26.));
#66986=CARTESIAN_POINT('Ctrl Pts',(-4.60600945165704,-0.300070227388598,
26.));
#66987=CARTESIAN_POINT('Ctrl Pts',(-4.61154878947915,-0.25589088056297,
26.));
#66988=CARTESIAN_POINT('Ctrl Pts',(-4.6146089290101,-0.231484539947162,
26.));
#66989=CARTESIAN_POINT('Ctrl Pts',(-4.61747426508659,-0.207042538674214,
26.));
#66990=CARTESIAN_POINT('Ctrl Pts',(-4.62014035545176,-0.182595807090288,
26.));
#66991=CARTESIAN_POINT('Ctrl Pts',(-4.6355064624287,-0.0416961970611351,
26.));
#66992=CARTESIAN_POINT('Ctrl Pts',(-4.64428121342256,0.099526957690747,
26.));
#66993=CARTESIAN_POINT('Ctrl Pts',(-4.64631642071577,0.240645210364403,
26.));
#66994=CARTESIAN_POINT('Ctrl Pts',(-4.64782495501833,0.345244739654039,
26.));
#66995=CARTESIAN_POINT('Ctrl Pts',(-4.64562987589745,0.449787288147385,
26.));
#66996=CARTESIAN_POINT('Ctrl Pts',(-4.6396534459514,0.554104703798643,26.));
#66997=CARTESIAN_POINT('Ctrl Pts',(-4.63179775743763,0.691224210145253,
26.));
#66998=CARTESIAN_POINT('Ctrl Pts',(-4.61741097334291,0.827954978565883,
26.));
#66999=CARTESIAN_POINT('Ctrl Pts',(-4.59676076751363,0.963919018344825,
26.));
#67000=CARTESIAN_POINT('Ctrl Pts',(-4.57581741441672,1.1018131835223,26.));
#67001=CARTESIAN_POINT('Ctrl Pts',(-4.54843137134414,1.23891944459888,26.));
#67002=CARTESIAN_POINT('Ctrl Pts',(-4.51482841662203,1.3748401921847,26.));
#67003=CARTESIAN_POINT('Ctrl Pts',(-4.50509310232456,1.41421861019102,26.));
#67004=CARTESIAN_POINT('Ctrl Pts',(-4.49483564045414,1.45349746044631,26.));
#67005=CARTESIAN_POINT('Ctrl Pts',(-4.48406073341117,1.49266688179373,26.));
#67006=CARTESIAN_POINT('Ctrl Pts',(-4.47783668509381,1.51529281908091,26.));
#67007=CARTESIAN_POINT('Ctrl Pts',(-4.47143997379187,1.53788224103568,26.));
#67008=CARTESIAN_POINT('Ctrl Pts',(-4.46487145429867,1.56043322804307,26.));
#67009=CARTESIAN_POINT('Ctrl Pts',(-4.45973334069111,1.57807335734872,26.));
#67010=CARTESIAN_POINT('Ctrl Pts',(-4.45449021537901,1.59568938184522,26.));
#67011=CARTESIAN_POINT('Ctrl Pts',(-4.44914654369818,1.61326759097873,26.));
#67012=CARTESIAN_POINT('Ctrl Pts',(-4.40827604464057,1.7477126360219,26.));
#67013=CARTESIAN_POINT('Ctrl Pts',(-4.36147201478811,1.88014056905998,26.));
#67014=CARTESIAN_POINT('Ctrl Pts',(-4.30904356529584,2.01016709268461,26.));
#67015=CARTESIAN_POINT('Ctrl Pts',(-4.25484746504965,2.14457752399178,26.));
#67016=CARTESIAN_POINT('Ctrl Pts',(-4.19464124103037,2.27642270082558,26.));
#67017=CARTESIAN_POINT('Ctrl Pts',(-4.12870910753944,2.4052752225727,26.));
#67018=CARTESIAN_POINT('Ctrl Pts',(-4.06277697404851,2.53412774431982,26.));
#67019=CARTESIAN_POINT('Ctrl Pts',(-3.991118562445,2.65998845878048,26.));
#67020=CARTESIAN_POINT('Ctrl Pts',(-3.91396546539836,2.78241449550764,26.));
#67021=CARTESIAN_POINT('Ctrl Pts',(-3.8599022254897,2.86820169586649,26.));
#67022=CARTESIAN_POINT('Ctrl Pts',(-3.80313988532888,2.95230207537908,26.));
#67023=CARTESIAN_POINT('Ctrl Pts',(-3.74376497539126,3.03461721426763,26.));
#67024=CARTESIAN_POINT('Ctrl Pts',(-3.71778845229355,3.07063008753137,26.));
#67025=CARTESIAN_POINT('Ctrl Pts',(-3.69131172751679,3.10630115823714,26.));
#67026=CARTESIAN_POINT('Ctrl Pts',(-3.66434142116742,3.1416216999591,26.));
#67027=CARTESIAN_POINT('Ctrl Pts',(-3.64886736739569,3.16188665189447,26.));
#67028=CARTESIAN_POINT('Ctrl Pts',(-3.63323082853231,3.18203621015477,26.));
#67029=CARTESIAN_POINT('Ctrl Pts',(-3.61743300165625,3.20206867796743,26.));
#67030=CARTESIAN_POINT('Ctrl Pts',(-3.60562290128194,3.21704450074792,26.));
#67031=CARTESIAN_POINT('Ctrl Pts',(-3.59372248215876,3.23195501636103,26.));
#67032=CARTESIAN_POINT('Ctrl Pts',(-3.58174179779154,3.24678792441536,26.));
#67033=CARTESIAN_POINT('Ctrl Pts',(-3.49102566491969,3.35910071195637,26.));
#67034=CARTESIAN_POINT('Ctrl Pts',(-3.39558140635013,3.46713215575717,26.));
#67035=CARTESIAN_POINT('Ctrl Pts',(-3.29573453983928,3.57065014592309,26.));
#67036=CARTESIAN_POINT('Ctrl Pts',(-3.19481521819522,3.67528002275919,26.));
#67037=CARTESIAN_POINT('Ctrl Pts',(-3.08939783097439,3.77529957447928,26.));
#67038=CARTESIAN_POINT('Ctrl Pts',(-2.97977151694561,3.87044492257043,26.));
#67039=CARTESIAN_POINT('Ctrl Pts',(-2.87044051512184,3.9653339673936,26.));
#67040=CARTESIAN_POINT('Ctrl Pts',(-2.75692276267532,4.05537559850027,26.));
#67041=CARTESIAN_POINT('Ctrl Pts',(-2.63946507568592,4.14027538885812,26.));
#67042=CARTESIAN_POINT('Ctrl Pts',(-2.52377549108901,4.22389717412067,26.));
#67043=CARTESIAN_POINT('Ctrl Pts',(-2.40426319127569,4.30253122094905,26.));
#67044=CARTESIAN_POINT('Ctrl Pts',(-2.28113248745318,4.37585694114117,26.));
#67045=CARTESIAN_POINT('Ctrl Pts',(-2.24413725288456,4.39788801977718,26.));
#67046=CARTESIAN_POINT('Ctrl Pts',(-2.20681518281834,4.41943960051781,26.));
#67047=CARTESIAN_POINT('Ctrl Pts',(-2.16917135428626,4.44050218283292,26.));
#67048=CARTESIAN_POINT('Ctrl Pts',(-2.54472725763282,-3.56250530678316,
26.));
#67049=CARTESIAN_POINT('Ctrl Pts',(-1.44818804155806,-4.33531677513798,
26.0490642110999));
#67050=CARTESIAN_POINT('Ctrl Pts',(1.63914523023693,-4.84388073813931,26.1510486762817));
#67051=CARTESIAN_POINT('Ctrl Pts',(4.98187809541805,-1.36671674862893,26.3059533955455));
#67052=CARTESIAN_POINT('Ctrl Pts',(3.85252000415521,3.44398917781397,26.4647141577913));
#67053=CARTESIAN_POINT('Ctrl Pts',(-0.805001512196143,5.10466442465425,
26.6234749200372));
#67054=CARTESIAN_POINT('Ctrl Pts',(-3.96413630374849,2.67678406505067,26.7514334980751));
#67055=CARTESIAN_POINT('Ctrl Pts',(-4.3679444184666,0.611489669763926,26.826471822031));
#67056=CARTESIAN_POINT('Ctrl Pts',(-4.36558297706963,0.00185075076461511,
26.848589891905));
#67057=CARTESIAN_POINT('Origin',(0.,0.,24.1514101080949));
#67058=CARTESIAN_POINT('',(2.5383587572269,-3.55965150255042,26.));
#67059=CARTESIAN_POINT('Origin',(0.,0.,26.));
#67060=CARTESIAN_POINT('Ctrl Pts',(2.53835875722654,-3.55965150255068,26.));
#67061=CARTESIAN_POINT('Ctrl Pts',(3.13016463613492,-3.13763950664917,26.026460127041));
#67062=CARTESIAN_POINT('Ctrl Pts',(4.08944058768451,-1.99447514282845,26.079380381123));
#67063=CARTESIAN_POINT('Ctrl Pts',(4.72633908941221,0.949051473338421,26.1852208892869));
#67064=CARTESIAN_POINT('Ctrl Pts',(2.60449620246589,4.46265906441401,26.3175215244918));
#67065=CARTESIAN_POINT('Ctrl Pts',(-2.34489469821123,4.60777770546463,26.4762822867377));
#67066=CARTESIAN_POINT('Ctrl Pts',(-4.30346090622908,1.74883727013167,26.5875784812721));
#67067=CARTESIAN_POINT('Ctrl Pts',(-4.3779262327693,0.151632086931482,26.6459544217245));
#67068=CARTESIAN_POINT('Ctrl Pts',(-4.37688026104952,0.00226901643694839,
26.651410108095));
#67069=CARTESIAN_POINT('Ctrl Pts',(2.86929757049756,-4.02374147429191,25.6709103465619));
#67070=CARTESIAN_POINT('Ctrl Pts',(3.53826020854994,-3.54670961616163,25.6973704736029));
#67071=CARTESIAN_POINT('Ctrl Pts',(4.62260187198943,-2.25450506767067,25.7502907276849));
#67072=CARTESIAN_POINT('Ctrl Pts',(5.34253608871791,1.0727841677129,25.8561312358488));
#67073=CARTESIAN_POINT('Ctrl Pts',(2.94405769272283,5.04447875030544,25.9884318710537));
#67074=CARTESIAN_POINT('Ctrl Pts',(-2.65061061266289,5.20851725077882,26.1471926332996));
#67075=CARTESIAN_POINT('Ctrl Pts',(-5.80869481541901,0.598627327994403,
26.3059533955455));
#67076=CARTESIAN_POINT('Ctrl Pts',(-3.6559591721986,-4.55561486272761,26.4647141577913));
#67077=CARTESIAN_POINT('Ctrl Pts',(1.84567034813922,-5.54225209737284,26.6234749200373));
#67078=CARTESIAN_POINT('Ctrl Pts',(5.65659992177503,-1.45549501989441,26.7822356822831));
#67079=CARTESIAN_POINT('Ctrl Pts',(4.29121225256454,3.96287657984353,26.940996444529));
#67080=CARTESIAN_POINT('Ctrl Pts',(-1.00202899277672,5.75456300236789,27.0997572067749));
#67081=CARTESIAN_POINT('Ctrl Pts',(-5.37797121296738,2.27936156876184,27.2585179690208));
#67082=CARTESIAN_POINT('Ctrl Pts',(-4.83194032779028,-3.28191017660925,
27.4172787312667));
#67083=CARTESIAN_POINT('Ctrl Pts',(0.136487592633803,-5.83951456248522,
27.5760394935126));
#67084=CARTESIAN_POINT('Ctrl Pts',(4.97996779668276,-3.05259748930662,27.7348002557585));
#67085=CARTESIAN_POINT('Ctrl Pts',(5.26564507543792,2.52813993990873,27.8935610180044));
#67086=CARTESIAN_POINT('Ctrl Pts',(0.732034933496452,5.79505175124635,28.0523217802503));
#67087=CARTESIAN_POINT('Ctrl Pts',(-4.47155165508331,3.75815243181214,28.2110825424962));
#67088=CARTESIAN_POINT('Ctrl Pts',(-5.58263982081247,-1.71832134856424,
28.369843304742));
#67089=CARTESIAN_POINT('Ctrl Pts',(-1.58432433047622,-5.62213569522022,
28.5286040669879));
#67090=CARTESIAN_POINT('Ctrl Pts',(3.86401257103054,-4.38039933096899,28.6873648292338));
#67091=CARTESIAN_POINT('Ctrl Pts',(5.77588745817332,0.870412097209825,28.8461255914797));
#67092=CARTESIAN_POINT('Ctrl Pts',(2.40149355054825,5.32459589387785,29.0048863537256));
#67093=CARTESIAN_POINT('Ctrl Pts',(-3.17082052230127,4.90554683073371,29.1636471159715));
#67094=CARTESIAN_POINT('Ctrl Pts',(-5.84110284449404,-0.00320850462351047,
29.3224078782174));
#67095=CARTESIAN_POINT('Ctrl Pts',(-3.16542940092975,-4.90902733376601,
29.4811686404633));
#67096=CARTESIAN_POINT('Ctrl Pts',(2.40734170730851,-5.32195439090584,29.6399294027091));
#67097=CARTESIAN_POINT('Ctrl Pts',(5.77684015826,-0.8640662324248,29.7986901649551));
#67098=CARTESIAN_POINT('Ctrl Pts',(3.85919803712304,4.38464173738479,29.9574509272009));
#67099=CARTESIAN_POINT('Ctrl Pts',(-1.59050000656898,5.62039165738282,30.1162116894468));
#67100=CARTESIAN_POINT('Ctrl Pts',(-5.58452386271215,1.71218745603623,30.2749724516927));
#67101=CARTESIAN_POINT('Ctrl Pts',(-4.46742089771919,-3.76306300482994,
30.4337332139386));
#67102=CARTESIAN_POINT('Ctrl Pts',(0.738402131764131,-5.79424325925859,
30.5924939761845));
#67103=CARTESIAN_POINT('Ctrl Pts',(5.26841697560084,-2.522355095433,30.7512547384304));
#67104=CARTESIAN_POINT('Ctrl Pts',(4.97661567740753,3.05806949811635,30.9100155006762));
#67105=CARTESIAN_POINT('Ctrl Pts',(0.130063698581311,5.83965547701761,31.0687762629222));
#67106=CARTESIAN_POINT('Ctrl Pts',(-4.83552655005252,3.27661038876524,31.227537025168));
#67107=CARTESIAN_POINT('Ctrl Pts',(-5.37549519698693,-2.28528861265885,
31.386297787414));
#67108=CARTESIAN_POINT('Ctrl Pts',(-0.995646443005195,-5.75562167072471,
31.5450585496598));
#67109=CARTESIAN_POINT('Ctrl Pts',(4.2954483480341,-3.95823396799194,31.7038193119058));
#67110=CARTESIAN_POINT('Ctrl Pts',(5.65521760477304,1.46185036807875,31.8625800741516));
#67111=CARTESIAN_POINT('Ctrl Pts',(1.83915896875347,5.54400459448242,32.0213408363975));
#67112=CARTESIAN_POINT('Ctrl Pts',(-3.66015413331184,4.5521164721907,32.1801015986434));
#67113=CARTESIAN_POINT('Ctrl Pts',(-5.80958237170622,-0.606007691658192,
32.3388623608893));
#67114=CARTESIAN_POINT('Ctrl Pts',(-2.64190336751104,-5.20949510535547,
32.4976231231352));
#67115=CARTESIAN_POINT('Ctrl Pts',(2.9437262966194,-5.04509347253155,32.6563838853811));
#67116=CARTESIAN_POINT('Ctrl Pts',(5.83516773679323,-0.263268189260048,
32.8151446476269));
#67117=CARTESIAN_POINT('Ctrl Pts',(3.3860854267346,4.75950818245377,32.9739054098728));
#67118=CARTESIAN_POINT('Ctrl Pts',(-2.1620456951976,5.42623728451552,33.1326661721187));
#67119=CARTESIAN_POINT('Ctrl Pts',(-5.73140655633933,1.12670827721268,33.2914269343647));
#67120=CARTESIAN_POINT('Ctrl Pts',(-4.0552090690265,-4.20401856114767,33.4501876966105));
#67121=CARTESIAN_POINT('Ctrl Pts',(1.33243962623321,-5.68709919892666,33.6089484588564));
#67122=CARTESIAN_POINT('Ctrl Pts',(5.50059887566598,-1.96517293514109,33.7677092211022));
#67123=CARTESIAN_POINT('Ctrl Pts',(4.63444201610888,3.55533962587452,33.9264699833482));
#67124=CARTESIAN_POINT('Ctrl Pts',(-0.473297737465698,5.82189676202686,
34.0852307455941));
#67125=CARTESIAN_POINT('Ctrl Pts',(-5.14786094464401,2.7600761494201,34.24399150784));
#67126=CARTESIAN_POINT('Ctrl Pts',(-5.11094457182416,-2.82785046275963,
34.4027522700858));
#67127=CARTESIAN_POINT('Ctrl Pts',(-0.396335611036177,-5.82764195360469,
34.5615130323317));
#67128=CARTESIAN_POINT('Ctrl Pts',(4.68101180720102,-3.49379752086946,34.7202737945776));
#67129=CARTESIAN_POINT('Ctrl Pts',(5.47415423612042,2.03767712240033,34.8790345568235));
#67130=CARTESIAN_POINT('Ctrl Pts',(1.2571834979241,5.7042074215912,35.0377953190694));
#67131=CARTESIAN_POINT('Ctrl Pts',(-4.11039997874232,4.15007285125745,35.1965560813153));
#67132=CARTESIAN_POINT('Ctrl Pts',(-5.71601984106162,-1.20233515817297,
35.3553168435612));
#67133=CARTESIAN_POINT('Ctrl Pts',(-2.09016374674189,-5.45432930503785,
35.5140776058071));
#67134=CARTESIAN_POINT('Ctrl Pts',(3.44867405347895,-4.71435466727419,35.6728383680529));
#67135=CARTESIAN_POINT('Ctrl Pts',(5.8311800188353,0.340341363817132,35.8315991302989));
#67136=CARTESIAN_POINT('Ctrl Pts',(2.87681191524069,5.0835465828807,35.9903598925447));
#67137=CARTESIAN_POINT('Ctrl Pts',(-2.7105023265463,5.17413469033962,36.1491206547906));
#67138=CARTESIAN_POINT('Ctrl Pts',(-5.81708204570653,0.529196683197753,
36.3078814170365));
#67139=CARTESIAN_POINT('Ctrl Pts',(-3.5996905915515,-4.60007829292986,36.4666421792824));
#67140=CARTESIAN_POINT('Ctrl Pts',(1.91224764597227,-5.51922110414707,36.6254029415283));
#67141=CARTESIAN_POINT('Ctrl Pts',(5.67403842753732,-1.38700417404515,36.7841637037742));
#67142=CARTESIAN_POINT('Ctrl Pts',(4.24277592445978,4.01464134273703,36.9429244660201));
#67143=CARTESIAN_POINT('Ctrl Pts',(-1.07160470196143,5.74196447382976,37.1016852282659));
#67144=CARTESIAN_POINT('Ctrl Pts',(-5.40521997255572,2.2140663278849,37.2604459905119));
#67145=CARTESIAN_POINT('Ctrl Pts',(-4.79181281967314,-3.34021295087678,
37.4192067527577));
#67146=CARTESIAN_POINT('Ctrl Pts',(0.207207793602656,-5.83742730886296,
37.5779675150036));
#67147=CARTESIAN_POINT('Ctrl Pts',(5.01658550492884,-2.99204988723897,37.7367282772495));
#67148=CARTESIAN_POINT('Ctrl Pts',(5.23463092854471,2.59174298453994,37.8954890394954));
#67149=CARTESIAN_POINT('Ctrl Pts',(0.661782232472825,5.80349351104764,38.0542498017413));
#67150=CARTESIAN_POINT('Ctrl Pts',(-4.51674977715968,3.70370950622708,38.2130105639872));
#67151=CARTESIAN_POINT('Ctrl Pts',(-5.5614144248173,-1.78582256997244,38.371771326233));
#67152=CARTESIAN_POINT('Ctrl Pts',(-1.51610271526659,-5.64091528147253,
38.530532088479));
#67153=CARTESIAN_POINT('Ctrl Pts',(3.91679250925652,-4.33327002336813,38.6892928507249));
#67154=CARTESIAN_POINT('Ctrl Pts',(5.76491958932306,0.940316321579044,38.8480536129708));
#67155=CARTESIAN_POINT('Ctrl Pts',(2.33681616947948,5.35329644668107,39.0068143752167));
#67156=CARTESIAN_POINT('Ctrl Pts',(-3.23001278765103,4.86677614521149,39.1655751374625));
#67157=CARTESIAN_POINT('Ctrl Pts',(-5.84063537949807,-0.0739663419686063,
39.3243358997085));
#67158=CARTESIAN_POINT('Ctrl Pts',(-3.10573006749788,-4.94701257364771,
39.4830966619543));
#67159=CARTESIAN_POINT('Ctrl Pts',(2.47163426803653,-5.29240178945783,39.6418574242002));
#67160=CARTESIAN_POINT('Ctrl Pts',(5.78688342441216,-0.794023229038551,
39.8006181864461));
#67161=CARTESIAN_POINT('Ctrl Pts',(3.80580010810998,4.43106964435213,39.959378948692));
#67162=CARTESIAN_POINT('Ctrl Pts',(-1.65846771681237,5.60071223044711,40.1181397109378));
#67163=CARTESIAN_POINT('Ctrl Pts',(-5.60485522875205,1.64441190725433,40.2769004731838));
#67164=CARTESIAN_POINT('Ctrl Pts',(-4.4215080328057,-3.81690442267336,40.4356612354296));
#67165=CARTESIAN_POINT('Ctrl Pts',(0.808538371485783,-5.78487323610672,
40.5944219976756));
#67166=CARTESIAN_POINT('Ctrl Pts',(5.29858576106737,-2.45834936260147,40.7531827599214));
#67167=CARTESIAN_POINT('Ctrl Pts',(4.93920561471065,3.1181309388157,40.9119435221673));
#67168=CARTESIAN_POINT('Ctrl Pts',(0.0593136197707885,5.84080256047905,
41.0707042844132));
#67169=CARTESIAN_POINT('Ctrl Pts',(-4.87486401174139,3.21779326915472,41.2294650466591));
#67170=CARTESIAN_POINT('Ctrl Pts',(-5.34741719504777,-2.35023871087517,
41.388225808905));
#67171=CARTESIAN_POINT('Ctrl Pts',(-0.925850822461446,-5.76726043373597,
41.5469865711509));
#67172=CARTESIAN_POINT('Ctrl Pts',(4.34308250332321,-3.90590924437788,41.7057473333967));
#67173=CARTESIAN_POINT('Ctrl Pts',(5.63709406088405,1.53024939298615,41.8645080956427));
#67174=CARTESIAN_POINT('Ctrl Pts',(1.77186494664376,5.56587704381296,42.0232688578886));
#67175=CARTESIAN_POINT('Ctrl Pts',(-3.71502908908446,4.50744401221416,42.1820296201344));
#67176=CARTESIAN_POINT('Ctrl Pts',(-5.80181502544146,-0.676339461033121,
42.3407903823803));
#67177=CARTESIAN_POINT('Ctrl Pts',(-2.57860263176698,-5.24111640048504,
42.4995511446262));
#67178=CARTESIAN_POINT('Ctrl Pts',(3.00462565494359,-5.00906351822809,42.6583119068721));
#67179=CARTESIAN_POINT('Ctrl Pts',(5.83792876476416,-0.192562700251437,
42.817072669118));
#67180=CARTESIAN_POINT('Ctrl Pts',(3.32818114721658,4.80017738289961,42.9758334313639));
#67181=CARTESIAN_POINT('Ctrl Pts',(-2.22761951688042,5.39964850189364,43.1345941936098));
#67182=CARTESIAN_POINT('Ctrl Pts',(-5.74463475560437,1.05719637754358,43.2933549558557));
#67183=CARTESIAN_POINT('Ctrl Pts',(-4.0039847938458,-4.25283416401821,43.4521157181015));
#67184=CARTESIAN_POINT('Ctrl Pts',(1.40123435454846,-5.67054097415953,43.6108764803475));
#67185=CARTESIAN_POINT('Ctrl Pts',(5.5240010203993,-1.89839547582067,43.7696372425933));
#67186=CARTESIAN_POINT('Ctrl Pts',(4.59103321957251,3.61121954923408,43.9283980048393));
#67187=CARTESIAN_POINT('Ctrl Pts',(-0.543788418742688,5.81573613669244,
44.0871587670851));
#67188=CARTESIAN_POINT('Ctrl Pts',(-5.18091828599107,2.69751336787648,44.245919529331));
#67189=CARTESIAN_POINT('Ctrl Pts',(-5.07631348469077,-2.88955603183869,
44.4046802915769));
#67190=CARTESIAN_POINT('Ctrl Pts',(-0.325711524187161,-5.83201548857688,
44.5634410538228));
#67191=CARTESIAN_POINT('Ctrl Pts',(4.7229915722406,-3.43683622893689,44.7222018160687));
#67192=CARTESIAN_POINT('Ctrl Pts',(5.44906851609775,2.1038405269557,44.8809625783145));
#67193=CARTESIAN_POINT('Ctrl Pts',(1.18799151005716,5.71901816993276,45.0397233405605));
#67194=CARTESIAN_POINT('Ctrl Pts',(-4.16037161366087,4.09997569410277,45.1984841028063));
#67195=CARTESIAN_POINT('Ctrl Pts',(-5.70103555635091,-1.27148977235826,
45.3572448650522));
#67196=CARTESIAN_POINT('Ctrl Pts',(-2.02393761747008,-5.47924896099626,
45.5160056272981));
#67197=CARTESIAN_POINT('Ctrl Pts',(3.50552985089882,-4.67223213469171,45.674766389544));
#67198=CARTESIAN_POINT('Ctrl Pts',(5.82662932192163,0.410954256471436,45.8335271517899));
#67199=CARTESIAN_POINT('Ctrl Pts',(2.81501966081174,5.11802275935076,45.9922879140358));
#67200=CARTESIAN_POINT('Ctrl Pts',(-2.77298197976823,5.1409205008315,46.1510486762817));
#67201=CARTESIAN_POINT('Ctrl Pts',(-5.82306581062682,0.458690768489886,
46.3098094385276));
#67202=CARTESIAN_POINT('Ctrl Pts',(-3.54370194373858,-4.64334676606566,
46.4685702007734));
#67203=CARTESIAN_POINT('Ctrl Pts',(1.97896618584451,-5.49565150744413,46.6273309630194));
#67204=CARTESIAN_POINT('Ctrl Pts',(5.69042401383344,-1.31816812234872,46.7860917252652));
#67205=CARTESIAN_POINT('Ctrl Pts',(4.19383196809736,4.0657429922898,46.9448524875111));
#67206=CARTESIAN_POINT('Ctrl Pts',(-1.14108319710691,5.72856193064797,47.103613249757));
#67207=CARTESIAN_POINT('Ctrl Pts',(-5.4316441654788,2.14842600887457,47.2623740120029));
#67208=CARTESIAN_POINT('Ctrl Pts',(-4.75099848187323,-3.39801502074773,
47.4211347742488));
#67209=CARTESIAN_POINT('Ctrl Pts',(0.277906133480956,-5.83448890966147,
47.5798955364947));
#67210=CARTESIAN_POINT('Ctrl Pts',(5.05246256671996,-2.93106033166876,47.7386562987406));
#67211=CARTESIAN_POINT('Ctrl Pts',(5.20285092941832,2.65496419227074,47.8974170609865));
#67212=CARTESIAN_POINT('Ctrl Pts',(0.591431198362095,5.8110843905069,48.0561778232323));
#67213=CARTESIAN_POINT('Ctrl Pts',(-4.56128443093633,3.6487226526672,48.2149385854782));
#67214=CARTESIAN_POINT('Ctrl Pts',(-5.53937322279471,-1.85306150857812,
48.3736993477241));
#67215=CARTESIAN_POINT('Ctrl Pts',(-1.44765843879317,-5.65886717467194,
48.53246010997));
#67216=CARTESIAN_POINT('Ctrl Pts',(3.96899756769466,-4.28550475015754,48.6912208722159));
#67217=CARTESIAN_POINT('Ctrl Pts',(5.75310576561908,1.01008252414809,48.8499816344618));
#67218=CARTESIAN_POINT('Ctrl Pts',(2.27179583594514,5.38121141898098,49.0087423967076));
#67219=CARTESIAN_POINT('Ctrl Pts',(-3.28873103569315,4.8272912519194,49.1675031589537));
#67220=CARTESIAN_POINT('Ctrl Pts',(-5.83931080786754,-0.144713320429998,
49.3262639211994));
#67221=CARTESIAN_POINT('Ctrl Pts',(-3.04557496461057,-4.98427184159595,
49.4850246834454));
#67222=CARTESIAN_POINT('Ctrl Pts',(2.53556411455661,-5.26207252676754,49.6437854456913));
#67223=CARTESIAN_POINT('Ctrl Pts',(5.79607746626723,-0.72386370334331,49.8025462079371));
#67224=CARTESIAN_POINT('Ctrl Pts',(3.75184367735869,4.47684729208542,49.961306970183));
#67225=CARTESIAN_POINT('Ctrl Pts',(-1.72619204662586,5.58021089871651,50.120067732429));
#67226=CARTESIAN_POINT('Ctrl Pts',(-5.62436408231579,1.57639504108098,50.2788284946748));
#67227=CARTESIAN_POINT('Ctrl Pts',(-4.37494631143252,-3.87018570976535,
50.4375892569207));
#67228=CARTESIAN_POINT('Ctrl Pts',(0.878555958148904,-5.77465428267269,
50.5963500191666));
#67229=CARTESIAN_POINT('Ctrl Pts',(5.32797697899131,-2.39398286696617,50.7551107814125));
#67230=CARTESIAN_POINT('Ctrl Pts',(4.90107072348494,3.17773479374659,50.9138715436583));
#67231=CARTESIAN_POINT('Ctrl Pts',(-0.0114451633093337,5.84109250604932,
51.0726323059043));
#67232=CARTESIAN_POINT('Ctrl Pts',(-4.91348608704586,3.15850393832203,51.2313930681501));
#67233=CARTESIAN_POINT('Ctrl Pts',(-5.31855445953128,-2.4148439115166,51.3901538303961));
#67234=CARTESIAN_POINT('Ctrl Pts',(-0.855919333292373,-5.77805285116754,
51.5489145926419));
#67235=CARTESIAN_POINT('Ctrl Pts',(4.39007931117216,-3.85301132850749,51.7076753548878));
#67236=CARTESIAN_POINT('Ctrl Pts',(5.61814327333331,1.59842385376603,51.8664361171337));
#67237=CARTESIAN_POINT('Ctrl Pts',(1.70431090331913,5.58693270058057,52.0251968793796));
#67238=CARTESIAN_POINT('Ctrl Pts',(-3.76935886426715,4.46211008474238,52.1839576416255));
#67239=CARTESIAN_POINT('Ctrl Pts',(-5.79319626271042,-0.746571977579234,
52.3427184038713));
#67240=CARTESIAN_POINT('Ctrl Pts',(-2.51492348603726,-5.27196856168236,
52.5014791661173));
#67241=CARTESIAN_POINT('Ctrl Pts',(3.06508408439537,-4.9722984837573,52.6602399283631));
#67242=CARTESIAN_POINT('Ctrl Pts',(5.83983307657691,-0.121828952662795,
52.8190006906091));
#67243=CARTESIAN_POINT('Ctrl Pts',(3.26978845705136,4.84014215722252,52.9777614528549));
#67244=CARTESIAN_POINT('Ctrl Pts',(-2.29286643535651,5.37226732075056,53.1365222151009));
#67245=CARTESIAN_POINT('Ctrl Pts',(-5.75701992960891,0.98752933428568,53.2952829773466));
#67246=CARTESIAN_POINT('Ctrl Pts',(-3.95217293381976,-4.30102566339373,
53.4540437395927));
#67247=CARTESIAN_POINT('Ctrl Pts',(1.46982345169535,-5.65315059739567,53.6128045018384));
#67248=CARTESIAN_POINT('Ctrl Pts',(5.54659251787697,-1.83133942692776,53.7715652640845));
#67249=CARTESIAN_POINT('Ctrl Pts',(4.54695068882314,3.66656952605562,53.9303260263302));
#67250=CARTESIAN_POINT('Ctrl Pts',(-0.61419929905889,5.80872205196845,54.0890867885762));
#67251=CARTESIAN_POINT('Ctrl Pts',(-5.21321532748033,2.63455472619438,54.2478475508221));
#67252=CARTESIAN_POINT('Ctrl Pts',(-5.04093744845616,-2.95083755851469,
54.4066083130679));
#67253=CARTESIAN_POINT('Ctrl Pts',(-0.255039639165707,-5.8355331751643,
54.5653690753139));
#67254=CARTESIAN_POINT('Ctrl Pts',(4.76427823817645,-3.37937058122179,54.7241298375597));
#67255=CARTESIAN_POINT('Ctrl Pts',(5.42318314516584,2.16969519287334,54.8828905998057));
#67256=CARTESIAN_POINT('Ctrl Pts',(1.11862518441343,5.7329896522482,55.0416513620514));
#67257=CARTESIAN_POINT('Ctrl Pts',(-4.20973271396536,4.04927686543645,55.2004121242976));
#67258=CARTESIAN_POINT('Ctrl Pts',(-5.68521464456297,-1.34045779539507,
55.3591728865431));
#67259=CARTESIAN_POINT('Ctrl Pts',(-1.95741447531414,-5.50336453706454,
55.5179336487893));
#67260=CARTESIAN_POINT('Ctrl Pts',(3.56187121174587,-4.62942395195395,55.676694411035));
#67261=CARTESIAN_POINT('Ctrl Pts',(5.82122356704326,0.481506841580768,55.835455173281));
#67262=CARTESIAN_POINT('Ctrl Pts',(2.75281430219354,5.15174786588276,55.9942159355268));
#67263=CARTESIAN_POINT('Ctrl Pts',(-2.83505469783139,5.10695188114131,56.1529766977728));
#67264=CARTESIAN_POINT('Ctrl Pts',(-5.82819504052776,0.388117540903014,
56.3117374600186));
#67265=CARTESIAN_POINT('Ctrl Pts',(-3.48719325759759,-4.6859338279744,56.4704982222645));
#67266=CARTESIAN_POINT('Ctrl Pts',(2.04539431239091,-5.47127542377716,56.6292589845104));
#67267=CARTESIAN_POINT('Ctrl Pts',(5.70597453029646,-1.24913862945516,56.7880197467563));
#67268=CARTESIAN_POINT('Ctrl Pts',(4.14427256681325,4.11624799398041,56.9467805090021));
#67269=CARTESIAN_POINT('Ctrl Pts',(-1.21039423827122,5.71431872089305,57.1055412712481));
#67270=CARTESIAN_POINT('Ctrl Pts',(-5.4572712645165,2.08247040830632,57.2643020334939));
#67271=CARTESIAN_POINT('Ctrl Pts',(-4.709486934955,-3.45531843184919,57.4230627957399));
#67272=CARTESIAN_POINT('Ctrl Pts',(0.348563690628765,-5.8306942991006,57.5818235579858));
#67273=CARTESIAN_POINT('Ctrl Pts',(5.08759817953255,-2.86964064293877,57.7405843202316));
#67274=CARTESIAN_POINT('Ctrl Pts',(5.17030741181829,2.71779578395536,57.8993450824775));
#67275=CARTESIAN_POINT('Ctrl Pts',(0.520993371711727,5.81782249322041,58.0581058447234));
#67276=CARTESIAN_POINT('Ctrl Pts',(-4.60514971613518,3.59320034898822,58.2168666069693));
#67277=CARTESIAN_POINT('Ctrl Pts',(-5.51651911764551,-1.9200285103718,58.3756273692151));
#67278=CARTESIAN_POINT('Ctrl Pts',(-1.37900171841615,-5.67598862900501,
58.5343881314612));
#67279=CARTESIAN_POINT('Ctrl Pts',(4.02062017566359,-4.23711057904269,58.6931488937069));
#67280=CARTESIAN_POINT('Ctrl Pts',(5.74044767353369,1.07970049708729,58.8519096559529));
#67281=CARTESIAN_POINT('Ctrl Pts',(2.20644211632846,5.40833669840192,59.0106704181987));
#67282=CARTESIAN_POINT('Ctrl Pts',(-3.34696666239261,4.78709795354361,59.1694311804446));
#67283=CARTESIAN_POINT('Ctrl Pts',(-5.83712931726406,-0.215439062208749,
59.3281919426906));
#67284=CARTESIAN_POINT('Ctrl Pts',(-2.98497292353889,-5.02079966755579,
59.4869527049364));
#67285=CARTESIAN_POINT('Ctrl Pts',(2.59912186699419,-5.23097105483309,59.6457134671823));
#67286=CARTESIAN_POINT('Ctrl Pts',(5.80442093364305,-0.653597950635783,
59.8044742294282));
#67287=CARTESIAN_POINT('Ctrl Pts',(3.69733666347582,4.52196796239271,59.9632349916741));
#67288=CARTESIAN_POINT('Ctrl Pts',(-1.79366305772334,5.55889067092954,60.1219957539199));
#67289=CARTESIAN_POINT('Ctrl Pts',(-5.64304756034266,1.5081468389052,60.2807565161659));
#67290=CARTESIAN_POINT('Ctrl Pts',(-4.32774256660426,-3.92289904703017,
60.4395172784117));
#67291=CARTESIAN_POINT('Ctrl Pts',(0.948444616708253,-5.76358789861195,
60.5982780406577));
#67292=CARTESIAN_POINT('Ctrl Pts',(5.35658631619137,-2.32926505429939,60.7570388029035));
#67293=CARTESIAN_POINT('Ctrl Pts',(4.86221660003666,3.23687231603548,60.9157995651494));
#67294=CARTESIAN_POINT('Ctrl Pts',(-0.0822022668114812,5.84052527118238,
61.0745603273953));
#67295=CARTESIAN_POINT('Ctrl Pts',(-4.95138710817278,3.09875109697584,61.2333210896412));
#67296=CARTESIAN_POINT('Ctrl Pts',(-5.28891122604591,-2.47909473376766,
61.3920818518871));
#67297=CARTESIAN_POINT('Ctrl Pts',(-0.785862237944882,-5.78799733923239,
61.5508426141331));
#67298=CARTESIAN_POINT('Ctrl Pts',(4.43643187479794,-3.79954798315087,61.7096033763787));
#67299=CARTESIAN_POINT('Ctrl Pts',(5.59836802314956,1.66636374581465,61.8683641386249));
#67300=CARTESIAN_POINT('Ctrl Pts',(1.63650675233685,5.6071684748672,62.0271249008705));
#67301=CARTESIAN_POINT('Ctrl Pts',(-3.82313548596416,4.41612134253018,62.1858856631167));
#67302=CARTESIAN_POINT('Ctrl Pts',(-5.78372734831682,-0.816694934673283,
62.3446464253623));
#67303=CARTESIAN_POINT('Ctrl Pts',(-2.45087527523776,-5.30204706139213,
62.5034071876083));
#67304=CARTESIAN_POINT('Ctrl Pts',(3.12509271269893,-4.93480376438871,62.6621679498542));
#67305=CARTESIAN_POINT('Ctrl Pts',(5.84088039277376,-0.0510773266730637,
62.8209287121001));
#67306=CARTESIAN_POINT('Ctrl Pts',(3.21091592536738,4.879396640591,62.979689474346));
#67307=CARTESIAN_POINT('Ctrl Pts',(-2.35777687563918,5.34409775927519,63.1384502365919));
#67308=CARTESIAN_POINT('Ctrl Pts',(-5.76856026082839,0.917717371079188,
63.2972109988377));
#67309=CARTESIAN_POINT('Ctrl Pts',(-3.89978109233997,-4.34858598717061,
63.4559717610837));
#67310=CARTESIAN_POINT('Ctrl Pts',(1.53819685222249,-5.63493062067332,63.6147325233296));
#67311=CARTESIAN_POINT('Ctrl Pts',(5.56837005279627,-1.76401462893886,63.7734932855754));
#67312=CARTESIAN_POINT('Ctrl Pts',(4.50220089297303,3.72138143372885,63.9322540478213));
#67313=CARTESIAN_POINT('Ctrl Pts',(-0.684520045616047,5.80085553717197,
64.0910148100672));
#67314=CARTESIAN_POINT('Ctrl Pts',(-5.2447473295203,2.57120946355576,64.2497755723131));
#67315=CARTESIAN_POINT('Ctrl Pts',(-5.00482165455439,-3.01168604972238,
64.408536334559));
#67316=CARTESIAN_POINT('Ctrl Pts',(-0.184330327072359,-5.83819449714635,
64.5672970968048));
#67317=CARTESIAN_POINT('Ctrl Pts',(4.80486574618941,-3.32140901080918,64.7260578590508));
#67318=CARTESIAN_POINT('Ctrl Pts',(5.39650192200348,2.23523145597974,64.8848186212967));
#67319=CARTESIAN_POINT('Ctrl Pts',(1.04909470050257,5.74611981822221,65.0435793835425));
#67320=CARTESIAN_POINT('Ctrl Pts',(-4.25847603591327,3.99798380531258,65.2023401457885));
#67321=CARTESIAN_POINT('Ctrl Pts',(-5.66855942741703,-1.40922910622467,
65.3611009080343));
#67322=CARTESIAN_POINT('Ctrl Pts',(-1.8906040825464,-5.52667249428149,65.5198616702802));
#67323=CARTESIAN_POINT('Ctrl Pts',(3.61768986792422,-4.58593640116248,65.6786224325261));
#67324=CARTESIAN_POINT('Ctrl Pts',(5.8149635474948,0.551988765551636,65.8373831947719));
#67325=CARTESIAN_POINT('Ctrl Pts',(2.6902049680239,5.18471695331663,65.996143957018));
#67326=CARTESIAN_POINT('Ctrl Pts',(-2.89671137156331,5.07223381616474,66.1549047192637));
#67327=CARTESIAN_POINT('Ctrl Pts',(-5.83246898269471,0.317487357059558,
66.3136654815097));
#67328=CARTESIAN_POINT('Ctrl Pts',(-3.4301728257792,-4.72783322900402,66.4724262437555));
#67329=CARTESIAN_POINT('Ctrl Pts',(2.11152227728272,-5.44609643033688,66.6311870060015));
#67330=CARTESIAN_POINT('Ctrl Pts',(5.72068769488774,-1.1799258254438,66.7899477682473));
#67331=CARTESIAN_POINT('Ctrl Pts',(4.0941049934505,4.16614893619904,66.9487085304932));
#67332=CARTESIAN_POINT('Ctrl Pts',(-1.27952765405788,5.69923693475624,67.1074692927391));
#67333=CARTESIAN_POINT('Ctrl Pts',(-5.48209750889141,2.01620920516577,67.266230054985));
#67334=CARTESIAN_POINT('Ctrl Pts',(-4.66728427073886,-3.51211477490457,
67.4249908172309));
#67335=CARTESIAN_POINT('Ctrl Pts',(0.419170096048379,-5.82604403403957,
67.5837515794768));
#67336=CARTESIAN_POINT('Ctrl Pts',(5.12198718721476,-2.80779983438927,67.7425123417226));
#67337=CARTESIAN_POINT('Ctrl Pts',(5.13700515150643,2.78022853905663,67.9012731039686));
#67338=CARTESIAN_POINT('Ctrl Pts',(0.45047908927406,5.82370683037148,68.0600338662144));
#67339=CARTESIAN_POINT('Ctrl Pts',(-4.64833919552487,3.53715074308911,68.2187946284603));
#67340=CARTESIAN_POINT('Ctrl Pts',(-5.49285546321007,-1.98671374794472,
68.3775553907063));
#67341=CARTESIAN_POINT('Ctrl Pts',(-1.31014262951052,-5.69227713189796,
68.5363161529521));
#67342=CARTESIAN_POINT('Ctrl Pts',(4.07165275754471,-4.18809461186912,68.6950769151981));
#67343=CARTESIAN_POINT('Ctrl Pts',(5.72694717064212,1.14916002395785,68.8538376774439));
#67344=CARTESIAN_POINT('Ctrl Pts',(2.14076460128891,5.43466830430864,69.0125984396898));
#67345=CARTESIAN_POINT('Ctrl Pts',(-3.40471112167017,4.74620214845141,69.1713592019357));
#67346=CARTESIAN_POINT('Ctrl Pts',(-5.83409122782134,-0.28613318830099,
69.3301199641816));
#67347=CARTESIAN_POINT('Ctrl Pts',(-2.92393283763341,-5.0565906910682,69.4888807264275));
#67348=CARTESIAN_POINT('Ctrl Pts',(2.66229819824794,-5.19910193779603,69.6476414886733));
#67349=CARTESIAN_POINT('Ctrl Pts',(5.81191260213551,-0.583236282416525,
69.8064022509193));
#67350=CARTESIAN_POINT('Ctrl Pts',(3.64228706536681,4.56642503381477,69.9651630131651));
#67351=CARTESIAN_POINT('Ctrl Pts',(-1.86087084873268,5.53675467583008,70.123923775411));
#67352=CARTESIAN_POINT('Ctrl Pts',(-5.66090292103185,1.43967731615189,70.282684537657));
#67353=CARTESIAN_POINT('Ctrl Pts',(-4.27990372547136,-3.97503669878468,
70.4414452999028));
#67354=CARTESIAN_POINT('Ctrl Pts',(1.01819409100193,-5.75167570791655,70.6002060621487));
#67355=CARTESIAN_POINT('Ctrl Pts',(5.38440957424679,-2.26420542194124,70.7589668243946));
#67356=CARTESIAN_POINT('Ctrl Pts',(4.82264894620915,3.29553482724991,70.9177275866405));
#67357=CARTESIAN_POINT('Ctrl Pts',(-0.152947307129394,5.83910093911992,
71.0764883488863));
#67358=CARTESIAN_POINT('Ctrl Pts',(-4.98856151314671,3.03854351384673,71.2352491111322));
#67359=CARTESIAN_POINT('Ctrl Pts',(-5.25849184473667,-2.542981748819,71.3940098733781));
#67360=CARTESIAN_POINT('Ctrl Pts',(-0.71568981729892,-5.79709243857671,
71.5527706356241));
#67361=CARTESIAN_POINT('Ctrl Pts',(4.48213339196102,-3.74552705405491,71.7115313978699));
#67362=CARTESIAN_POINT('Ctrl Pts',(5.57777121235107,1.73405909895161,71.8702921601158));
#67363=CARTESIAN_POINT('Ctrl Pts',(1.56846244395725,5.62658139707268,72.0290529223617));
#67364=CARTESIAN_POINT('Ctrl Pts',(-3.87635106245531,4.36948453442625,72.1878136846075));
#67365=CARTESIAN_POINT('Ctrl Pts',(-5.77340967182392,-0.88669804176993,
72.3465744468535));
#67366=CARTESIAN_POINT('Ctrl Pts',(-2.38646739844469,-5.33134748559404,
72.5053352090994));
#67367=CARTESIAN_POINT('Ctrl Pts',(3.18464273358708,-4.89658486247307,72.6640959713453));
#67368=CARTESIAN_POINT('Ctrl Pts',(5.84107055966092,0.0196817949154431,
72.8228567335911));
#67369=CARTESIAN_POINT('Ctrl Pts',(3.15157219170978,4.91793507240897,72.9816174958371));
#67370=CARTESIAN_POINT('Ctrl Pts',(-2.42234131212014,5.31514395135115,73.1403782580829));
#67371=CARTESIAN_POINT('Ctrl Pts',(-5.77925405571895,0.847770732830903,
73.2991390203289));
#67372=CARTESIAN_POINT('Ctrl Pts',(-3.84681695791018,-4.39550815587048,
73.4578997825747));
#67373=CARTESIAN_POINT('Ctrl Pts',(1.60634452233207,-5.61588371777435,73.6166605448206));
#67374=CARTESIAN_POINT('Ctrl Pts',(5.58933042930359,-1.6964309617693,73.7754213070665));
#67375=CARTESIAN_POINT('Ctrl Pts',(4.45679039905553,3.77564722860532,73.9341820693123));
#67376=CARTESIAN_POINT('Ctrl Pts',(-0.754740338843374,5.79213774671418,
74.0929428315583));
#67377=CARTESIAN_POINT('Ctrl Pts',(-5.2755096647891,2.50748687587913,74.2517035938041));
#67378=CARTESIAN_POINT('Ctrl Pts',(-4.96797140297887,-3.07209257594453,
74.4104643560501));
#67379=CARTESIAN_POINT('Ctrl Pts',(-0.113593964499922,-5.83999906397405,
74.5692251182959));
#67380=CARTESIAN_POINT('Ctrl Pts',(4.84474814006207,-3.26296002356047,74.7279858805419));
#67381=CARTESIAN_POINT('Ctrl Pts',(5.36902876208054,2.30043969882727,74.8867466427877));
#67382=CARTESIAN_POINT('Ctrl Pts',(0.979410261924092,5.75840674100279,75.0455074050336));
#67383=CARTESIAN_POINT('Ctrl Pts',(-4.30659442642138,3.94610404098849,75.2042681672795));
#67384=CARTESIAN_POINT('Ctrl Pts',(-5.65107234906636,-1.477793612656,75.3630289295254));
#67385=CARTESIAN_POINT('Ctrl Pts',(-1.82351624359326,-5.54916941220397,
75.5217896917713));
#67386=CARTESIAN_POINT('Ctrl Pts',(3.6729776280452,-4.54177586411616,75.6805504540171));
#67387=CARTESIAN_POINT('Ctrl Pts',(5.80785018193428,0.622389685160801,75.8393112162631));
#67388=CARTESIAN_POINT('Ctrl Pts',(2.62720084622344,5.21692518343825,75.9980719785088));
#67389=CARTESIAN_POINT('Ctrl Pts',(-2.95794295284595,5.0367714007783,76.1568327407549));
#67390=CARTESIAN_POINT('Ctrl Pts',(-5.83588700992668,0.246810581940319,
76.3155935030007));
#67391=CARTESIAN_POINT('Ctrl Pts',(-3.37264901603277,-4.76903882041673,
76.4743542652466));
#67392=CARTESIAN_POINT('Ctrl Pts',(2.17734037623983,-5.42011822214095,76.6331150274925));
#67393=CARTESIAN_POINT('Ctrl Pts',(5.73456134845009,-1.110539867295,76.7918757897384));
#67394=CARTESIAN_POINT('Ctrl Pts',(4.04333661010157,4.21543849598137,76.9506365519843));
#67395=CARTESIAN_POINT('Ctrl Pts',(-1.34847329913683,5.68331878549001,77.1093973142302));
#67396=CARTESIAN_POINT('Ctrl Pts',(-5.50611925535187,1.94965212328559,77.2681580764761));
#67397=CARTESIAN_POINT('Ctrl Pts',(-4.62439668246642,-3.56839571504929,
77.4269188387219));
#67398=CARTESIAN_POINT('Ctrl Pts',(0.489714988248199,-5.82053879690483,
77.5856796009679));
#67399=CARTESIAN_POINT('Ctrl Pts',(5.15562454317905,-2.74554698116043,77.7444403632137));
#67400=CARTESIAN_POINT('Ctrl Pts',(5.1029490355901,2.8422532955665,77.9032011254596));
#67401=CARTESIAN_POINT('Ctrl Pts',(0.379898699021361,5.82873653843356,78.0619618877055));
#67402=CARTESIAN_POINT('Ctrl Pts',(-4.69084653104859,3.48058206025056,78.2207226499513));
#67403=CARTESIAN_POINT('Ctrl Pts',(-5.46838573213,-2.05310743523703,78.3794834121973));
#67404=CARTESIAN_POINT('Ctrl Pts',(-1.24109127714898,-5.70773029301263,
78.5382441744431));
#67405=CARTESIAN_POINT('Ctrl Pts',(4.12208782430557,-4.13846404173107,78.6970049366891));
#67406=CARTESIAN_POINT('Ctrl Pts',(5.71260623814347,1.21845091157291,78.8557656989349));
#67407=CARTESIAN_POINT('Ctrl Pts',(2.07477292900298,5.46020237253759,79.0145264611808));
#67408=CARTESIAN_POINT('Ctrl Pts',(-3.46195593952531,4.70460983810283,79.1732872234267));
#67409=CARTESIAN_POINT('Ctrl Pts',(-5.83019698537905,-0.356785324342241,
79.3320479856726));
#67410=CARTESIAN_POINT('Ctrl Pts',(-2.86246366452812,-5.09163965979981,
79.4908087479185));
#67411=CARTESIAN_POINT('Ctrl Pts',(2.72508383719022,-5.16646985244982,79.6495695101644));
#67412=CARTESIAN_POINT('Ctrl Pts',(5.81855137234204,-0.512789024261698,
79.8083302724102));
#67413=CARTESIAN_POINT('Ctrl Pts',(3.58670296156134,4.61021198227599,79.9670910346562));
#67414=CARTESIAN_POINT('Ctrl Pts',(-1.92780555690993,5.51380616187509,80.1258517969019));
#67415=CARTESIAN_POINT('Ctrl Pts',(-5.67792754410753,1.37099652072606,80.2846125591481));
#67416=CARTESIAN_POINT('Ctrl Pts',(-4.23143680838723,-4.02659101382961,
80.4433733213938));
#67417=CARTESIAN_POINT('Ctrl Pts',(1.08779414529793,-5.73891945869655,80.6021340836398));
#67418=CARTESIAN_POINT('Ctrl Pts',(5.41144267008512,-2.19881351740198,80.7608948458856));
#67419=CARTESIAN_POINT('Ctrl Pts',(4.7823735685733,3.3537137186807,80.9196556081314));
#67420=CARTESIAN_POINT('Ctrl Pts',(-0.223669902459649,5.83681971885304,
81.0784163703775));
#67421=CARTESIAN_POINT('Ctrl Pts',(-5.02500384656033,2.97789002445559,81.2371771326232));
#67422=CARTESIAN_POINT('Ctrl Pts',(-5.22730077976831,-2.60649558135874,
81.3959378948693));
#67423=CARTESIAN_POINT('Ctrl Pts',(-0.645412368928784,-5.8053368142863,
81.5546986571149));
#67424=CARTESIAN_POINT('Ctrl Pts',(4.52717715552302,-3.69095646919078,81.713459419361));
#67425=CARTESIAN_POINT('Ctrl Pts',(5.5563558643626,1.80149997964642,81.8722201816067));
#67426=CARTESIAN_POINT('Ctrl Pts',(1.5001879620707,5.64516861688714,82.0309809438528));
#67427=CARTESIAN_POINT('Ctrl Pts',(-3.92899778126385,4.3222065071854,82.1897417060986));
#67428=CARTESIAN_POINT('Ctrl Pts',(-5.76224475326896,-0.956571031279116,
82.3485024683446));
#67429=CARTESIAN_POINT('Ctrl Pts',(-2.32170929618077,-5.35986552417092,
82.5072632305903));
#67430=CARTESIAN_POINT('Ctrl Pts',(3.24372538638481,-4.8576474063222,82.6660239928364));
#67431=CARTESIAN_POINT('Ctrl Pts',(5.8404035909078,0.0904380659057711,82.8247847550821));
#67432=CARTESIAN_POINT('Ctrl Pts',(3.09176588514392,4.95575172494502,82.9835455173283));
#67433=CARTESIAN_POINT('Ctrl Pts',(-2.48655011745873,5.28541028426119,83.1423062795738));
#67434=CARTESIAN_POINT('Ctrl Pts',(-5.78910003705706,0.777699419312094,
83.30106704182));
#67435=CARTESIAN_POINT('Ctrl Pts',(-3.79328774359228,-4.44178477631751,
83.4598278040656));
#67436=CARTESIAN_POINT('Ctrl Pts',(1.67425538991496,-5.59601365552512,83.6185885663117));
#67437=CARTESIAN_POINT('Ctrl Pts',(5.60947262352764,-1.6285964822938,83.7773493285575));
#67438=CARTESIAN_POINT('Ctrl Pts',(4.41072194085603,3.82935538285094,83.9361100908034));
#67439=CARTESIAN_POINT('Ctrl Pts',(-0.8248423466062,5.78257678649102,84.0948708530494));
#67440=CARTESIAN_POINT('Ctrl Pts',(-5.30551223554587,2.44338323992171,84.253631615295));
#67441=CARTESIAN_POINT('Ctrl Pts',(-4.9303644901222,-3.13202323158636,84.4123923775413));
#67442=CARTESIAN_POINT('Ctrl Pts',(-0.0428938145929691,-5.84099457038411,
84.5711531397868));
#67443=CARTESIAN_POINT('Ctrl Pts',(4.88402085037918,-3.20394034224944,84.729913902033));
#67444=CARTESIAN_POINT('Ctrl Pts',(5.3405737125575,2.36513442508082,84.8886746642787));
#67445=CARTESIAN_POINT('Ctrl Pts',(0.90995364228369,5.77018558745976,85.0474354265247));
#67446=CARTESIAN_POINT('Ctrl Pts',(-4.35479260506382,3.89299956501012,85.2061961887705));
#67447=CARTESIAN_POINT('Ctrl Pts',(-5.63139114508318,-1.54490255601334,
85.3649569510165));
#67448=CARTESIAN_POINT('Ctrl Pts',(-1.75878919991609,-5.5732440393258,85.5237177132622));
#67449=CARTESIAN_POINT('Ctrl Pts',(3.73289035077776,-4.49219002151886,85.6824784755083));
#67450=CARTESIAN_POINT('Ctrl Pts',(5.44619302579455,-0.180386406182261,
85.814779110713));
#67451=CARTESIAN_POINT('Ctrl Pts',(4.18934532924144,2.98339184141738,85.9206196188771));
#67452=CARTESIAN_POINT('Ctrl Pts',(2.90742207776985,4.07986902565238,85.973539872959));
#67453=CARTESIAN_POINT('Ctrl Pts',(2.16917135428672,4.4405021828327,86.));
#67454=CARTESIAN_POINT('Ctrl Pts',(2.75898463274055,-3.86904481704483,25.7806068977079));
#67455=CARTESIAN_POINT('Ctrl Pts',(3.40222835107826,-3.41035291299081,25.8070670247489));
#67456=CARTESIAN_POINT('Ctrl Pts',(4.44488144388779,-2.1678284260566,25.8599872788309));
#67457=CARTESIAN_POINT('Ctrl Pts',(5.13713708894935,1.03153993625474,25.9658277869948));
#67458=CARTESIAN_POINT('Ctrl Pts',(2.83087052930385,4.85053885500829,26.0981284221998));
#67459=CARTESIAN_POINT('Ctrl Pts',(-2.54870530784567,5.00827073567408,26.2568891844456));
#67460=CARTESIAN_POINT('Ctrl Pts',(-5.58537388969466,0.575612517731738,
26.4156499466916));
#67461=CARTESIAN_POINT('Ctrl Pts',(-3.51540226351445,-4.38046981539479,
26.5744107089373));
#67462=CARTESIAN_POINT('Ctrl Pts',(1.77471175523205,-5.32917482126994,26.7331714711833));
#67463=CARTESIAN_POINT('Ctrl Pts',(5.43912643226927,-1.39953709723575,26.8919322334291));
#67464=CARTESIAN_POINT('Ctrl Pts',(4.12623242092013,3.81051993270251,27.0506929956751));
#67465=CARTESIAN_POINT('Ctrl Pts',(-0.963505012884285,5.53332322688231,
27.2094537579209));
#67466=CARTESIAN_POINT('Ctrl Pts',(-5.17120987535828,2.19172929477075,27.3682145201668));
#67467=CARTESIAN_POINT('Ctrl Pts',(-4.64617167900849,-3.15573394561846,
27.5269752824127));
#67468=CARTESIAN_POINT('Ctrl Pts',(0.131240194292791,-5.61500874158838,
27.6857360446586));
#67469=CARTESIAN_POINT('Ctrl Pts',(4.78850808778552,-2.93523740776727,27.8444968069045));
#67470=CARTESIAN_POINT('Ctrl Pts',(5.06320222551221,2.43094313930505,28.0032575691504));
#67471=CARTESIAN_POINT('Ctrl Pts',(0.703891137995956,5.57225534640277,28.1620183313963));
#67472=CARTESIAN_POINT('Ctrl Pts',(-4.29963849958627,3.61366660379846,28.3207790936422));
#67473=CARTESIAN_POINT('Ctrl Pts',(-5.36800979937294,-1.65225881189325,
28.4795398558881));
#67474=CARTESIAN_POINT('Ctrl Pts',(-1.52341343958394,-5.40598721644804,
28.638300618134));
#67475=CARTESIAN_POINT('Ctrl Pts',(3.7154568469317,-4.21199061529042,28.7970613803798));
#67476=CARTESIAN_POINT('Ctrl Pts',(5.55382784322941,0.836948256968893,28.9558221426258));
#67477=CARTESIAN_POINT('Ctrl Pts',(2.30916579364752,5.11988662236081,29.1145829048716));
#67478=CARTESIAN_POINT('Ctrl Pts',(-3.04891524119282,4.71694830830577,29.2733436671175));
#67479=CARTESIAN_POINT('Ctrl Pts',(-5.61653596054952,-0.00308515054028371,
29.4321044293634));
#67480=CARTESIAN_POINT('Ctrl Pts',(-3.04373138672984,-4.72029500001125,
29.5908651916093));
#67481=CARTESIAN_POINT('Ctrl Pts',(2.31478911232886,-5.11734667454166,29.7496259538552));
#67482=CARTESIAN_POINT('Ctrl Pts',(5.55474391583396,-0.830846365132238,
29.908386716101));
#67483=CARTESIAN_POINT('Ctrl Pts',(3.71082741246647,4.21606991826224,30.067147478347));
#67484=CARTESIAN_POINT('Ctrl Pts',(-1.52935168579825,5.40431022984286,30.2259082405928));
#67485=CARTESIAN_POINT('Ctrl Pts',(-5.36982140744797,1.64636074283387,30.3846690028388));
#67486=CARTESIAN_POINT('Ctrl Pts',(-4.29566655320965,-3.61838838505691,
30.5434297650846));
#67487=CARTESIAN_POINT('Ctrl Pts',(0.710013543128747,-5.57147793767643,
30.7021905273306));
#67488=CARTESIAN_POINT('Ctrl Pts',(5.06586755727536,-2.42538069880583,30.8609512895764));
#67489=CARTESIAN_POINT('Ctrl Pts',(4.78528484399858,2.94049903987215,31.0197120518223));
#67490=CARTESIAN_POINT('Ctrl Pts',(0.125063273099813,5.61514423852442,31.1784728140682));
#67491=CARTESIAN_POINT('Ctrl Pts',(-4.64962002546522,3.15063791327663,31.3372335763141));
#67492=CARTESIAN_POINT('Ctrl Pts',(-5.16882905222222,-2.19742846769609,
31.49599433856));
#67493=CARTESIAN_POINT('Ctrl Pts',(-0.957367846451143,-5.5343411937037,
31.6547551008058));
#67494=CARTESIAN_POINT('Ctrl Pts',(4.13030565557618,-3.80605581058243,31.8135158630518));
#67495=CARTESIAN_POINT('Ctrl Pts',(5.4377972597899,1.40564810787321,31.9722766252976));
#67496=CARTESIAN_POINT('Ctrl Pts',(1.76845071216457,5.33085994192234,32.1310373875435));
#67497=CARTESIAN_POINT('Ctrl Pts',(-3.51943594526451,4.37710592388724,32.2897981497894));
#67498=CARTESIAN_POINT('Ctrl Pts',(-5.58622732301659,-0.582709136130893,
32.4485589120353));
#67499=CARTESIAN_POINT('Ctrl Pts',(-2.54033282120867,-5.00921099567965,
32.6073196742812));
#67500=CARTESIAN_POINT('Ctrl Pts',(2.83055187404587,-4.8511299436403,32.7660804365271));
#67501=CARTESIAN_POINT('Ctrl Pts',(5.61082903384082,-0.253146587487778,
32.9248411987729));
#67502=CARTESIAN_POINT('Ctrl Pts',(3.25590407686029,4.57652425799672,33.0836019610189));
#67503=CARTESIAN_POINT('Ctrl Pts',(-2.07892374414776,5.217620310809,33.2423627232647));
#67504=CARTESIAN_POINT('Ctrl Pts',(-5.51105705295918,1.08339088088132,33.4011234855107));
#67505=CARTESIAN_POINT('Ctrl Pts',(-3.8993026094728,-4.0423909758343,33.5598842477566));
#67506=CARTESIAN_POINT('Ctrl Pts',(1.28121268795212,-5.46845313502624,33.7186450100024));
#67507=CARTESIAN_POINT('Ctrl Pts',(5.28912299821215,-1.88961994896626,33.8774057722484));
#67508=CARTESIAN_POINT('Ctrl Pts',(4.45626638214284,3.41865113358054,34.0361665344941));
#67509=CARTESIAN_POINT('Ctrl Pts',(-0.455101345292619,5.59806827461589,
34.1949272967401));
#67510=CARTESIAN_POINT('Ctrl Pts',(-4.94994642026466,2.65396233550082,34.353688058986));
#67511=CARTESIAN_POINT('Ctrl Pts',(-4.91444933332838,-2.71913099939964,
34.5124488212319));
#67512=CARTESIAN_POINT('Ctrl Pts',(-0.381098102720512,-5.60359258671175,
34.6712095834778));
#67513=CARTESIAN_POINT('Ctrl Pts',(4.50104575229031,-3.35947507470101,34.8299703457236));
#67514=CARTESIAN_POINT('Ctrl Pts',(5.26369504857235,1.95933664217838,34.9887311079696));
#67515=CARTESIAN_POINT('Ctrl Pts',(1.20884985474224,5.48490361541909,35.1474918702154));
#67516=CARTESIAN_POINT('Ctrl Pts',(-3.95237165094757,3.99051926126589,35.3062526324614));
#67517=CARTESIAN_POINT('Ctrl Pts',(-5.49626189492614,-1.15611021279586,
35.4650133947072));
#67518=CARTESIAN_POINT('Ctrl Pts',(-2.00980536716273,-5.24463230626054,
35.6237741569531));
#67519=CARTESIAN_POINT('Ctrl Pts',(3.31608642293227,-4.53310671365589,35.782534919199));
#67520=CARTESIAN_POINT('Ctrl Pts',(5.60699462758102,0.327256608834102,35.9412956814449));
#67521=CARTESIAN_POINT('Ctrl Pts',(2.76621008118667,4.88810468673588,36.1000564436907));
#67522=CARTESIAN_POINT('Ctrl Pts',(-2.60629442649681,4.97521004623518,36.2588172059367));
#67523=CARTESIAN_POINT('Ctrl Pts',(-5.59343866475058,0.508851201650464,
36.4175779681825));
#67524=CARTESIAN_POINT('Ctrl Pts',(-3.46129698321598,-4.42322380574711,
36.5763387304285));
#67525=CARTESIAN_POINT('Ctrl Pts',(1.83872942405087,-5.30702927699456,36.7350994926743));
#67526=CARTESIAN_POINT('Ctrl Pts',(5.4558944977048,-1.33367944861663,36.8938602549202));
#67527=CARTESIAN_POINT('Ctrl Pts',(4.07965827459196,3.86029454890444,37.0526210171661));
#67528=CARTESIAN_POINT('Ctrl Pts',(-1.03040581621204,5.52120906103586,37.211381779412));
#67529=CARTESIAN_POINT('Ctrl Pts',(-5.1974110298633,2.12894439298054,37.3701425416579));
#67530=CARTESIAN_POINT('Ctrl Pts',(-4.60758691199661,-3.21179521298375,
37.5289033039038));
#67531=CARTESIAN_POINT('Ctrl Pts',(0.199241488304119,-5.61300173446314,
37.6876640661497));
#67532=CARTESIAN_POINT('Ctrl Pts',(4.82371799259843,-2.87701761719148,37.8464248283956));
#67533=CARTESIAN_POINT('Ctrl Pts',(5.03338044768208,2.49210090298119,38.0051855906414));
#67534=CARTESIAN_POINT('Ctrl Pts',(0.636339370439441,5.58037255453223,38.1639463528873));
#67535=CARTESIAN_POINT('Ctrl Pts',(-4.34309893586852,3.56131678947628,38.3227071151332));
#67536=CARTESIAN_POINT('Ctrl Pts',(-5.34760043438529,-1.71716488314614,
38.4814678773791));
#67537=CARTESIAN_POINT('Ctrl Pts',(-1.45781467077047,-5.4240448032289,38.640228639625));
#67538=CARTESIAN_POINT('Ctrl Pts',(3.76620760906239,-4.16667323979076,38.7989894018709));
#67539=CARTESIAN_POINT('Ctrl Pts',(5.54328164477202,0.904164945395139,38.9577501641167));
#67540=CARTESIAN_POINT('Ctrl Pts',(2.2469749974438,5.14748375447756,39.1165109263627));
#67541=CARTESIAN_POINT('Ctrl Pts',(-3.10583180228996,4.67966819952357,39.2752716886085));
#67542=CARTESIAN_POINT('Ctrl Pts',(-5.61608646770029,-0.0711226339607316,
39.4340324508545));
#67543=CARTESIAN_POINT('Ctrl Pts',(-2.98632725227654,-4.75681986037505,
39.5927932131003));
#67544=CARTESIAN_POINT('Ctrl Pts',(2.37660988298438,-5.08893025161958,39.7515539753462));
#67545=CARTESIAN_POINT('Ctrl Pts',(5.56440105884388,-0.763496233183334,
39.9103147375921));
#67546=CARTESIAN_POINT('Ctrl Pts',(3.65948241880601,4.26071285915838,40.069075499838));
#67547=CARTESIAN_POINT('Ctrl Pts',(-1.59470631126904,5.3853873976295,40.2278362620839));
#67548=CARTESIAN_POINT('Ctrl Pts',(-5.38937111433215,1.58119089099016,40.3865970243298));
#67549=CARTESIAN_POINT('Ctrl Pts',(-4.25151885307432,-3.67015981718801,
40.5453577865757));
#67550=CARTESIAN_POINT('Ctrl Pts',(0.777453326851397,-5.56246815418439,
40.7041185488216));
#67551=CARTESIAN_POINT('Ctrl Pts',(5.09487647442165,-2.36383572866916,40.8628793110675));
#67552=CARTESIAN_POINT('Ctrl Pts',(4.74931304757294,2.9982513600266,41.0216400733133));
#67553=CARTESIAN_POINT('Ctrl Pts',(0.0570332499295138,5.61624722124574,
41.1804008355593));
#67554=CARTESIAN_POINT('Ctrl Pts',(-4.6874451201527,3.09408207507567,41.3391615978051));
#67555=CARTESIAN_POINT('Ctrl Pts',(-5.14183053639566,-2.25988149617119,
41.497922360051));
#67556=CARTESIAN_POINT('Ctrl Pts',(-0.89025558647059,-5.5455324931431,41.6566831222969));
#67557=CARTESIAN_POINT('Ctrl Pts',(4.17610846940334,-3.75574276189485,41.8154438845428));
#67558=CARTESIAN_POINT('Ctrl Pts',(5.4203704931852,1.47141746569594,41.9742046467887));
#67559=CARTESIAN_POINT('Ctrl Pts',(1.70374387423147,5.35189148365012,42.1329654090346));
#67560=CARTESIAN_POINT('Ctrl Pts',(-3.57220117995318,4.33415094011377,42.2917261712804));
#67561=CARTESIAN_POINT('Ctrl Pts',(-5.57875859993888,-0.65033693217899,
42.4504869335264));
#67562=CARTESIAN_POINT('Ctrl Pts',(-2.47946574386026,-5.03961657934126,
42.6092476957722));
#67563=CARTESIAN_POINT('Ctrl Pts',(2.88910989726652,-4.81648519599765,42.7680084580182));
#67564=CARTESIAN_POINT('Ctrl Pts',(5.61348391140414,-0.185159439821055,
42.926769220264));
#67565=CARTESIAN_POINT('Ctrl Pts',(3.200225983726,4.61562989144849,43.0855299825099));
#67566=CARTESIAN_POINT('Ctrl Pts',(-2.14197651643363,5.19205375981362,43.2442907447558));
#67567=CARTESIAN_POINT('Ctrl Pts',(-5.52377668122861,1.01655143385025,43.4030515070017));
#67568=CARTESIAN_POINT('Ctrl Pts',(-3.8500477014075,-4.08932981534074,43.5618122692476));
#67569=CARTESIAN_POINT('Ctrl Pts',(1.34736253598006,-5.45253150732624,43.7205730314935));
#67570=CARTESIAN_POINT('Ctrl Pts',(5.31162542471411,-1.82540981406326,43.8793337937394));
#67571=CARTESIAN_POINT('Ctrl Pts',(4.41452647903867,3.47238269889917,44.0380945559852));
#67572=CARTESIAN_POINT('Ctrl Pts',(-0.522881943720034,5.59214450051854,
44.1968553182311));
#67573=CARTESIAN_POINT('Ctrl Pts',(-4.98173283994925,2.59380484098539,44.355616080477));
#67574=CARTESIAN_POINT('Ctrl Pts',(-4.88114967204592,-2.77846423781803,
44.5143768427229));
#67575=CARTESIAN_POINT('Ctrl Pts',(-0.313189227628139,-5.60779797687521,
44.6731376049688));
#67576=CARTESIAN_POINT('Ctrl Pts',(4.54141156440446,-3.30470371507665,44.8318983672147));
#67577=CARTESIAN_POINT('Ctrl Pts',(5.23957377347164,2.02295633024942,44.9906591294605));
#67578=CARTESIAN_POINT('Ctrl Pts',(1.14231802019273,5.49914495012552,45.1494198917065));
#67579=CARTESIAN_POINT('Ctrl Pts',(-4.00042207772478,3.94234813807709,45.3081806539523));
#67580=CARTESIAN_POINT('Ctrl Pts',(-5.48185369562519,-1.22260611053129,
45.4669414161983));
#67581=CARTESIAN_POINT('Ctrl Pts',(-1.94612536588803,-5.26859390179156,
45.6257021784441));
#67582=CARTESIAN_POINT('Ctrl Pts',(3.37075634388315,-4.492603622836,45.7844629406901));
#67583=CARTESIAN_POINT('Ctrl Pts',(5.60261888663935,0.395154720103479,45.9432237029359));
#67584=CARTESIAN_POINT('Ctrl Pts',(2.70679349012103,4.92125539304622,46.1019844651818));
#67585=CARTESIAN_POINT('Ctrl Pts',(-2.66637198863979,4.94327280856975,46.2607452274277));
#67586=CARTESIAN_POINT('Ctrl Pts',(-5.59919237800458,0.441055955456253,
46.4195059896736));
#67587=CARTESIAN_POINT('Ctrl Pts',(-3.40746087346144,-4.46482878032041,
46.5782667519195));
#67588=CARTESIAN_POINT('Ctrl Pts',(1.90288290472123,-5.28436583637694,46.7370275141654));
#67589=CARTESIAN_POINT('Ctrl Pts',(5.47165012418784,-1.26748986592512,46.8957882764113));
#67590=CARTESIAN_POINT('Ctrl Pts',(4.03259601626857,3.90943154580342,47.0545490386571));
#67591=CARTESIAN_POINT('Ctrl Pts',(-1.09721314298891,5.50832179167125,47.2133098009031));
#67592=CARTESIAN_POINT('Ctrl Pts',(-5.22281931897105,2.06582767992164,47.3720705631488));
#67593=CARTESIAN_POINT('Ctrl Pts',(-4.56834172113761,-3.26737502602034,
47.5308313253949));
#67594=CARTESIAN_POINT('Ctrl Pts',(0.267221761695801,-5.61017630487886,
47.6895920876407));
#67595=CARTESIAN_POINT('Ctrl Pts',(4.85821572583019,-2.81837286444571,47.8483528498866));
#67596=CARTESIAN_POINT('Ctrl Pts',(5.00282226155327,2.5528915098482,48.0071136121325));
#67597=CARTESIAN_POINT('Ctrl Pts',(0.568693050307066,5.58767159524255,48.1658743743783));
#67598=CARTESIAN_POINT('Ctrl Pts',(-4.38592141153559,3.50844395901968,48.3246351366243));
#67599=CARTESIAN_POINT('Ctrl Pts',(-5.32640662782695,-1.78181875531413,
48.4833958988701));
#67600=CARTESIAN_POINT('Ctrl Pts',(-1.39200180112221,-5.44130651842186,
48.6421566611161));
#67601=CARTESIAN_POINT('Ctrl Pts',(3.81640559321821,-4.12074434899823,48.8009174233619));
#67602=CARTESIAN_POINT('Ctrl Pts',(5.53192201501862,0.971248918403669,48.9596781856079));
#67603=CARTESIAN_POINT('Ctrl Pts',(2.18445443391585,5.17432550849803,49.1184389478537));
#67604=CARTESIAN_POINT('Ctrl Pts',(-3.16229257013621,4.64170134138436,49.2771997100997));
#67605=CARTESIAN_POINT('Ctrl Pts',(-5.61481282051529,-0.139149675977844,
49.4359604723455));
#67606=CARTESIAN_POINT('Ctrl Pts',(-2.92848487086811,-4.79264665950293,
49.5947212345914));
#67607=CARTESIAN_POINT('Ctrl Pts',(2.43808188433272,-5.05976702695259,49.7534819968373));
#67608=CARTESIAN_POINT('Ctrl Pts',(5.57324162681136,-0.696034058739029,
49.9122427590832));
#67609=CARTESIAN_POINT('Ctrl Pts',(3.60760039555022,4.30473054066965,50.0710035213291));
#67610=CARTESIAN_POINT('Ctrl Pts',(-1.65982691330743,5.36567425955101,50.229764283575));
#67611=CARTESIAN_POINT('Ctrl Pts',(-5.40812993103286,1.515788999437,50.3885250458208));
#67612=CARTESIAN_POINT('Ctrl Pts',(-4.20674724239739,-3.7213926533396,50.5472858080668));
#67613=CARTESIAN_POINT('Ctrl Pts',(0.844779019247828,-5.55264207836113,
50.7060465703126));
#67614=CARTESIAN_POINT('Ctrl Pts',(5.12313771836632,-2.30194386560584,50.8648073325585));
#67615=CARTESIAN_POINT('Ctrl Pts',(4.71264428935673,3.05556368674283,51.0235680948044));
#67616=CARTESIAN_POINT('Ctrl Pts',(-0.0110051428662697,5.61652601957635,
51.1823288570503));
#67617=CARTESIAN_POINT('Ctrl Pts',(-4.7245823321816,3.03707218027256,51.3410896192961));
#67618=CARTESIAN_POINT('Ctrl Pts',(-5.11407745683792,-2.32200288699436,
51.4998503815421));
#67619=CARTESIAN_POINT('Ctrl Pts',(-0.82301268146625,-5.55590998558236,
51.6586111437879));
#67620=CARTESIAN_POINT('Ctrl Pts',(4.22129843923301,-3.70487855788512,51.8173719060339));
#67621=CARTESIAN_POINT('Ctrl Pts',(5.40214828710646,1.53697089297761,51.9761326682797));
#67622=CARTESIAN_POINT('Ctrl Pts',(1.63878701185215,5.37213763520004,52.1348934305256));
#67623=CARTESIAN_POINT('Ctrl Pts',(-3.62444219405034,4.29055991960671,52.2936541927716));
#67624=CARTESIAN_POINT('Ctrl Pts',(-5.57047119392959,-0.717869291269865,
52.4524149550173));
#67625=CARTESIAN_POINT('Ctrl Pts',(-2.41823480486641,-5.06928259917325,
52.6111757172634));
#67626=CARTESIAN_POINT('Ctrl Pts',(2.94724394355444,-4.78113362906013,52.7699364795091));
#67627=CARTESIAN_POINT('Ctrl Pts',(5.6153150100958,-0.117145120002924,52.9286972417552));
#67628=CARTESIAN_POINT('Ctrl Pts',(3.14407825736721,4.65405818112524,53.0874580040009));
#67629=CARTESIAN_POINT('Ctrl Pts',(-2.20471495362471,5.16572527482943,53.2462187662469));
#67630=CARTESIAN_POINT('Ctrl Pts',(-5.53568569516419,0.949562807876645,
53.4049795284926));
#67631=CARTESIAN_POINT('Ctrl Pts',(-3.80022779876814,-4.13566854561846,
53.5637402907387));
#67632=CARTESIAN_POINT('Ctrl Pts',(1.41331465853004,-5.43580972052295,53.7225010529844));
#67633=CARTESIAN_POINT('Ctrl Pts',(5.33334837008319,-1.76093180023503,53.8812618152305));
#67634=CARTESIAN_POINT('Ctrl Pts',(4.37213874408905,3.52560469199021,54.0400225774763));
#67635=CARTESIAN_POINT('Ctrl Pts',(-0.590585809212258,5.58540007910849,
54.1987833397222));
#67636=CARTESIAN_POINT('Ctrl Pts',(-5.01278819024406,2.53326670555979,54.3575441019681));
#67637=CARTESIAN_POINT('Ctrl Pts',(-4.8471337019555,-2.83738973655626,54.516304864214));
#67638=CARTESIAN_POINT('Ctrl Pts',(-0.245234392010581,-5.61118042257805,
54.6750656264598));
#67639=CARTESIAN_POINT('Ctrl Pts',(4.58111092428449,-3.2494473901187,54.8338263887058));
#67640=CARTESIAN_POINT('Ctrl Pts',(5.21468359081919,2.08627914944017,54.9925871509516));
#67641=CARTESIAN_POINT('Ctrl Pts',(1.07561855045193,5.51257928520504,55.1513479131975));
#67642=CARTESIAN_POINT('Ctrl Pts',(-4.04788544248539,3.89359847522351,55.3101086754434));
#67643=CARTESIAN_POINT('Ctrl Pts',(-5.46664103418928,-1.28892259079655,
55.4688694376893));
#67644=CARTESIAN_POINT('Ctrl Pts',(-1.88215977067859,-5.29178233106645,
55.6276301999352));
#67645=CARTESIAN_POINT('Ctrl Pts',(3.42493160627594,-4.45144124234838,55.7863909621811));
#67646=CARTESIAN_POINT('Ctrl Pts',(5.59742096126865,0.46299484241015,55.9451517244269));
#67647=CARTESIAN_POINT('Ctrl Pts',(2.64697967705877,4.95368390503328,56.1039124866729));
#67648=CARTESIAN_POINT('Ctrl Pts',(-2.72605826064226,4.91061014552488,56.2626732489187));
#67649=CARTESIAN_POINT('Ctrl Pts',(-5.60412440966974,0.373195984292183,
56.4214340111647));
#67650=CARTESIAN_POINT('Ctrl Pts',(-3.35312471875849,-4.5057785411845,56.5801947734105));
#67651=CARTESIAN_POINT('Ctrl Pts',(1.96675713728871,-5.26092691497154,56.7389555356564));
#67652=CARTESIAN_POINT('Ctrl Pts',(5.48660278591027,-1.20111427907158,56.8977162979024));
#67653=CARTESIAN_POINT('Ctrl Pts',(3.9849419744025,3.95799483354801,57.0564770601482));
#67654=CARTESIAN_POINT('Ctrl Pts',(-1.1638594537159,5.49462617597814,57.2152378223941));
#67655=CARTESIAN_POINT('Ctrl Pts',(-5.24746115924365,2.00240780661117,57.37399858464));
#67656=CARTESIAN_POINT('Ctrl Pts',(-4.52842612604344,-3.32247535170916,
57.5327593468859));
#67657=CARTESIAN_POINT('Ctrl Pts',(0.335162820288752,-5.60652758181426,
57.6915201091317));
#67658=CARTESIAN_POINT('Ctrl Pts',(4.89200051581106,-2.75931451542811,57.8502808713777));
#67659=CARTESIAN_POINT('Ctrl Pts',(4.97152991116165,2.61330747983713,58.0090416336235));
#67660=CARTESIAN_POINT('Ctrl Pts',(0.500963274458718,5.59415064503912,58.1678023958695));
#67661=CARTESIAN_POINT('Ctrl Pts',(-4.42810025315133,3.45505626434493,58.3265631581152));
#67662=CARTESIAN_POINT('Ctrl Pts',(-5.30443117099388,-1.84621114554552,
58.4853239203613));
#67663=CARTESIAN_POINT('Ctrl Pts',(-1.325984655183,-5.45776972177896,58.644084682607));
#67664=CARTESIAN_POINT('Ctrl Pts',(3.86604351978,-4.07421073889346,58.802845444853));
#67665=CARTESIAN_POINT('Ctrl Pts',(5.51975057560345,1.03819036061473,58.9616062070988));
#67666=CARTESIAN_POINT('Ctrl Pts',(2.12161330165796,5.20040793015086,59.1203669693448));
#67667=CARTESIAN_POINT('Ctrl Pts',(-3.21828927148705,4.60305331348437,59.2791277315906));
#67668=CARTESIAN_POINT('Ctrl Pts',(-5.61271519944128,-0.207156297777243,
59.4378884938366));
#67669=CARTESIAN_POINT('Ctrl Pts',(-2.8702127342488,-4.82777013764157,59.5966492560824));
#67670=CARTESIAN_POINT('Ctrl Pts',(2.49919609711769,-5.02986128137743,59.7554100183283));
#67671=CARTESIAN_POINT('Ctrl Pts',(5.58126432146331,-0.6284697412833,59.9141707805742));
#67672=CARTESIAN_POINT('Ctrl Pts',(3.55518895686721,4.34811650289146,60.0729315428202));
#67673=CARTESIAN_POINT('Ctrl Pts',(-1.72470393571439,5.34517370867209,60.2316923050659));
#67674=CARTESIAN_POINT('Ctrl Pts',(-5.42609510456254,1.45016466581917,60.3904530673119));
#67675=CARTESIAN_POINT('Ctrl Pts',(-4.161358291482,-3.7720793750479,60.5492138295578));
#67676=CARTESIAN_POINT('Ctrl Pts',(0.911980740306919,-5.54200115220642,
60.7079745918037));
#67677=CARTESIAN_POINT('Ctrl Pts',(5.15064714175253,-2.23971419223624,60.8667353540495));
#67678=CARTESIAN_POINT('Ctrl Pts',(4.67528395050075,3.11242760942936,61.0254961162954));
#67679=CARTESIAN_POINT('Ctrl Pts',(-0.0790419206570804,5.61598059260596,
61.1842568785413));
#67680=CARTESIAN_POINT('Ctrl Pts',(-4.76102621166261,2.97961659506878,61.3430176407873));
#67681=CARTESIAN_POINT('Ctrl Pts',(-5.08557388631535,-2.38378352384928,
61.5017784030331));
#67682=CARTESIAN_POINT('Ctrl Pts',(-0.75564899933528,-5.56547214812468,
61.660539165279));
#67683=CARTESIAN_POINT('Ctrl Pts',(4.26586893343571,-3.65347066287608,61.8192999275249));
#67684=CARTESIAN_POINT('Ctrl Pts',(5.38313331566308,1.60229876975119,61.9780606897708));
#67685=CARTESIAN_POINT('Ctrl Pts',(1.5735896574475,5.39159542544895,62.1368214520167));
#67686=CARTESIAN_POINT('Ctrl Pts',(-3.67615132118597,4.24633925934925,62.2955822142625));
#67687=CARTESIAN_POINT('Ctrl Pts',(-5.56136632116585,-0.785296303028447,
62.4543429765086));
#67688=CARTESIAN_POINT('Ctrl Pts',(-2.3566489898686,-5.09820470168657,62.6131037387542));
#67689=CARTESIAN_POINT('Ctrl Pts',(3.00494548173707,-4.7450804306709,62.7718645010003));
#67690=CARTESIAN_POINT('Ctrl Pts',(5.61632206120212,-0.0491136091362308,
62.930625263246));
#67691=CARTESIAN_POINT('Ctrl Pts',(3.08746913746389,4.69180348767462,63.0893860254921));
#67692=CARTESIAN_POINT('Ctrl Pts',(-2.26712984885402,5.13863871956213,63.2481467877378));
#67693=CARTESIAN_POINT('Ctrl Pts',(-5.54678234711784,0.882434833542929,
63.4069075499838));
#67694=CARTESIAN_POINT('Ctrl Pts',(-3.74985021262651,-4.18140036645774,
63.5656683122296));
#67695=CARTESIAN_POINT('Ctrl Pts',(1.47905937712676,-5.41829022853902,63.7244290744757));
#67696=CARTESIAN_POINT('Ctrl Pts',(5.35428864647665,-1.69619536963139,63.8831898367214));
#67697=CARTESIAN_POINT('Ctrl Pts',(4.32910939769494,3.57830930252506,64.0419505989674));
#67698=CARTESIAN_POINT('Ctrl Pts',(-0.658203006225538,5.57783600012977,
64.2007113612132));
#67699=CARTESIAN_POINT('Ctrl Pts',(-5.04310791377582,2.47235681319663,64.3594721234592));
#67700=CARTESIAN_POINT('Ctrl Pts',(-4.81240641490144,-2.89589884829624,
64.518232885705));
#67701=CARTESIAN_POINT('Ctrl Pts',(-0.177243568241342,-5.61373942744627,
64.676993647951));
#67702=CARTESIAN_POINT('Ctrl Pts',(4.62013800604848,-3.19371420869404,64.8357544101967));
#67703=CARTESIAN_POINT('Ctrl Pts',(5.18902815324987,2.14929580712564,64.9945151724427));
#67704=CARTESIAN_POINT('Ctrl Pts',(1.00876123366836,5.52520464916871,65.1532759346885));
#67705=CARTESIAN_POINT('Ctrl Pts',(-4.09475477997962,3.84427742671915,65.3120366969346));
#67706=CARTESIAN_POINT('Ctrl Pts',(-5.45062614307688,-1.35504992164687,
65.4707974591803));
#67707=CARTESIAN_POINT('Ctrl Pts',(-1.81791796848671,-5.31419419118279,
65.6295582214263));
#67708=CARTESIAN_POINT('Ctrl Pts',(3.47860425988976,-4.40962561277309,65.7883189836721));
#67709=CARTESIAN_POINT('Ctrl Pts',(5.59140161426455,0.530767020214592,65.947079745918));
#67710=CARTESIAN_POINT('Ctrl Pts',(2.58677741967834,4.98538546381227,66.1058405081639));
#67711=CARTESIAN_POINT('Ctrl Pts',(-2.78534448354271,4.87722685034708,66.2646012704098));
#67712=CARTESIAN_POINT('Ctrl Pts',(-5.6082340359703,0.305281246610254,66.4233620326558));
#67713=CARTESIAN_POINT('Ctrl Pts',(-3.29829649293878,-4.54606707896127,
66.5821227949015));
#67714=CARTESIAN_POINT('Ctrl Pts',(2.03034274820855,-5.23671595244054,66.7408835571475));
#67715=CARTESIAN_POINT('Ctrl Pts',(5.50075028856868,-1.13456242867458,66.8996443193933));
#67716=CARTESIAN_POINT('Ctrl Pts',(3.93670314222528,4.00597728547496,67.0584050816393));
#67717=CARTESIAN_POINT('Ctrl Pts',(-1.23033496804577,5.48012422378831,67.2171658438851));
#67718=CARTESIAN_POINT('Ctrl Pts',(-5.27133293449043,1.93869407991674,67.375926606131));
#67719=CARTESIAN_POINT('Ctrl Pts',(-4.48784598432852,-3.37708810407645,
67.534687368377));
#67720=CARTESIAN_POINT('Ctrl Pts',(0.403054693731489,-5.60205610071956,
67.6934481306228));
#67721=CARTESIAN_POINT('Ctrl Pts',(4.92506740462245,-2.69985123695237,67.8522088928687));
#67722=CARTESIAN_POINT('Ctrl Pts',(4.93950798866025,2.67333994690335,68.0109696551146));
#67723=CARTESIAN_POINT('Ctrl Pts',(0.433159982240225,5.59980875312125,68.1697304173605));
#67724=CARTESIAN_POINT('Ctrl Pts',(-4.46962927096998,3.40116154009715,68.3284911796064));
#67725=CARTESIAN_POINT('Ctrl Pts',(-5.28167728878481,-1.91033260425587,
68.4872519418522));
#67726=CARTESIAN_POINT('Ctrl Pts',(-1.25977292097022,-5.47343199732475,
68.6460127040982));
#67727=CARTESIAN_POINT('Ctrl Pts',(3.9151141043812,-4.02707923828464,68.804773466344));
#67728=CARTESIAN_POINT('Ctrl Pts',(5.50676911268545,1.10497944837047,68.96353422859));
#67729=CARTESIAN_POINT('Ctrl Pts',(2.05846082260739,5.22572719184021,69.1222949908358));
#67730=CARTESIAN_POINT('Ctrl Pts',(-3.27381368882556,4.56372978742243,69.2810557530818));
#67731=CARTESIAN_POINT('Ctrl Pts',(-5.60979391230414,-0.27513251938597,
69.4398165153275));
#67732=CARTESIAN_POINT('Ctrl Pts',(-2.81151939385567,-4.86218514042,69.5985772775736));
#67733=CARTESIAN_POINT('Ctrl Pts',(2.55994355282749,-4.99921740356275,69.7573380398193));
#67734=CARTESIAN_POINT('Ctrl Pts',(5.58846796546901,-0.560813195881055,
69.9160988020653));
#67735=CARTESIAN_POINT('Ctrl Pts',(3.50225579413674,4.39086437893307,70.074859564311));
#67736=CARTESIAN_POINT('Ctrl Pts',(-1.78932785778569,5.32388875344897,70.2336203265571));
#67737=CARTESIAN_POINT('Ctrl Pts',(-5.4432639985316,1.38432752050883,70.3923810888029));
#67738=CARTESIAN_POINT('Ctrl Pts',(-4.11535866115752,-3.82221254403565,
70.5511418510488));
#67739=CARTESIAN_POINT('Ctrl Pts',(0.979048628174891,-5.53054693727633,
70.7099026132948));
#67740=CARTESIAN_POINT('Ctrl Pts',(5.17740070757192,-2.17715584076599,70.8686633755405));
#67741=CARTESIAN_POINT('Ctrl Pts',(4.63723751363544,3.16883478330451,71.0274241377865));
#67742=CARTESIAN_POINT('Ctrl Pts',(-0.14706709904452,5.61461102037593,71.1861849000324));
#67743=CARTESIAN_POINT('Ctrl Pts',(-4.79677141045583,2.92172375107252,71.3449456622783));
#67744=CARTESIAN_POINT('Ctrl Pts',(-5.05632400772744,-2.44521434042637,
71.5037064245242));
#67745=CARTESIAN_POINT('Ctrl Pts',(-0.688174425699173,-5.57421757752254,
71.6624671867701));
#67746=CARTESIAN_POINT('Ctrl Pts',(4.30981341129062,-3.60152662097726,71.8212279490159));
#67747=CARTESIAN_POINT('Ctrl Pts',(5.36332836930242,1.66739150914959,71.9799887112618));
#67748=CARTESIAN_POINT('Ctrl Pts',(1.50816137873041,5.41026199896583,72.1387494735078));
#67749=CARTESIAN_POINT('Ctrl Pts',(-3.72732097304471,4.20149544872403,72.2975102357535));
#67750=CARTESIAN_POINT('Ctrl Pts',(-5.55144531778782,-0.85260807253943,
72.4562709979996));
#67751=CARTESIAN_POINT('Ctrl Pts',(-2.29471733658639,-5.12637864256223,
72.6150317602453));
#67752=CARTESIAN_POINT('Ctrl Pts',(3.06220604411272,-4.70833089163749,72.7737925224914));
#67753=CARTESIAN_POINT('Ctrl Pts',(5.61650491693822,0.0189251091536447,
72.9325532847371));
#67754=CARTESIAN_POINT('Ctrl Pts',(3.03040693140542,4.72886027197227,73.0913140469831));
#67755=CARTESIAN_POINT('Ctrl Pts',(-2.32921204273454,5.11079806896419,73.2500748092289));
#67756=CARTESIAN_POINT('Ctrl Pts',(-5.55706500865567,0.815177361880478,
73.4088355714748));
#67757=CARTESIAN_POINT('Ctrl Pts',(-3.69892233589434,-4.22651856671307,
73.5675963337208));
#67758=CARTESIAN_POINT('Ctrl Pts',(1.54458704373152,-5.39997560236016,73.7263570959665));
#67759=CARTESIAN_POINT('Ctrl Pts',(5.37444318090863,-1.63121002232468,73.8851178582126));
#67760=CARTESIAN_POINT('Ctrl Pts',(4.28544475441368,3.63048879610115,74.0438786204583));
#67761=CARTESIAN_POINT('Ctrl Pts',(-0.725723611935015,5.56945337361106,
74.2026393827042));
#67762=CARTESIAN_POINT('Ctrl Pts',(-5.07268756112454,2.41108410242379,74.3614001449502));
#67763=CARTESIAN_POINT('Ctrl Pts',(-4.77697290711372,-2.9539829868247,74.5201609071961));
#67764=CARTESIAN_POINT('Ctrl Pts',(-0.109226733975009,-5.61547461594591,
74.6789216694419));
#67765=CARTESIAN_POINT('Ctrl Pts',(4.65848708247156,-3.13751234964793,74.8376824316879));
#67766=CARTESIAN_POINT('Ctrl Pts',(5.16261122569953,2.21199705561036,74.9964431939337));
#67767=CARTESIAN_POINT('Ctrl Pts',(0.94175588115421,5.53701918924425,75.1552039561797));
#67768=CARTESIAN_POINT('Ctrl Pts',(-4.14102321213148,3.79439223042856,75.3139647184255));
#67769=CARTESIAN_POINT('Ctrl Pts',(-5.43381137247341,-1.42097839889528,
75.4727254806715));
#67770=CARTESIAN_POINT('Ctrl Pts',(-1.75340938679805,-5.33582619319972,
75.6314862429172));
#67771=CARTESIAN_POINT('Ctrl Pts',(3.53176642826186,-4.36716287055454,75.7902470051633));
#67772=CARTESIAN_POINT('Ctrl Pts',(5.58456172896637,0.598461307948863,75.949007767409));
#67773=CARTESIAN_POINT('Ctrl Pts',(2.52619555266178,5.0163554171789,76.107768529655));
#67774=CARTESIAN_POINT('Ctrl Pts',(-2.84422195708685,4.8431278220354,76.2665292919008));
#67775=CARTESIAN_POINT('Ctrl Pts',(-5.61152065381861,0.23732170889948,76.4252900541468));
#67776=CARTESIAN_POINT('Ctrl Pts',(-3.24298424204541,-4.58568848130712,
76.5840508163926));
#67777=CARTESIAN_POINT('Ctrl Pts',(2.09363040629115,-5.21173650174305,76.7428115786384));
#67778=CARTESIAN_POINT('Ctrl Pts',(5.51409055601673,-1.06784408121947,76.9015723408844));
#67779=CARTESIAN_POINT('Ctrl Pts',(3.88788659878658,4.05337186015841,77.0603331031303));
#67780=CARTESIAN_POINT('Ctrl Pts',(-1.29662993069554,5.46481806326361,77.2190938653762));
#67781=CARTESIAN_POINT('Ctrl Pts',(-5.29443114152808,1.8746958498288,77.377854627622));
#67782=CARTESIAN_POINT('Ctrl Pts',(-4.44660725112929,-3.43120526869962,
77.5366153898679));
#67783=CARTESIAN_POINT('Ctrl Pts',(0.470887418890042,-5.59676251778467,
77.6953761521139));
#67784=CARTESIAN_POINT('Ctrl Pts',(4.95741153969778,-2.63999175525599,77.8541369143597));
#67785=CARTESIAN_POINT('Ctrl Pts',(4.90676119326682,2.73298010128111,78.0128976766056));
#67786=CARTESIAN_POINT('Ctrl Pts',(0.365293123785983,5.60464508916152,78.1716584388516));
#67787=CARTESIAN_POINT('Ctrl Pts',(-4.51050237060752,3.34676769532807,78.3304192010974));
#67788=CARTESIAN_POINT('Ctrl Pts',(-5.25814832033228,-1.9741737216199,78.4891799633432));
#67789=CARTESIAN_POINT('Ctrl Pts',(-1.19337631505721,-5.48829104661996,
78.6479407255893));
#67790=CARTESIAN_POINT('Ctrl Pts',(3.96361014591247,-3.97935676372049,78.806701487835));
#67791=CARTESIAN_POINT('Ctrl Pts',(5.49297953129461,1.17160638037103,78.9654622500811));
#67792=CARTESIAN_POINT('Ctrl Pts',(1.99500626439154,5.25027957796405,79.1242230123267));
#67793=CARTESIAN_POINT('Ctrl Pts',(-3.32885767394246,4.52373653392658,79.2829837745728));
#67794=CARTESIAN_POINT('Ctrl Pts',(-5.60604938780277,-0.34306836529208,
79.4417445368186));
#67795=CARTESIAN_POINT('Ctrl Pts',(-2.75241346293775,-4.89588661743591,
79.6005052990645));
#67796=CARTESIAN_POINT('Ctrl Pts',(2.62031533677199,-4.96783989049817,79.7592660613105));
#67797=CARTESIAN_POINT('Ctrl Pts',(5.59485150169351,-0.493074351131619,
79.9180268235562));
#67798=CARTESIAN_POINT('Ctrl Pts',(3.44880867530152,4.43296789554331,80.0767875858023));
#67799=CARTESIAN_POINT('Ctrl Pts',(-1.85368919596017,5.30182251744854,80.235548348048));
#67800=CARTESIAN_POINT('Ctrl Pts',(-5.45963409340325,1.31828722510949,80.3943091102941));
#67801=CARTESIAN_POINT('Ctrl Pts',(-4.06875510187306,-3.87178480326137,
80.5530698725397));
#67802=CARTESIAN_POINT('Ctrl Pts',(1.04597284064243,-5.51828111447312,80.7118306347859));
#67803=CARTESIAN_POINT('Ctrl Pts',(5.20339448972971,-2.11427799164205,80.8705913970315));
#67804=CARTESIAN_POINT('Ctrl Pts',(4.59851056209243,3.2247769306293,81.0293521592777));
#67805=CARTESIAN_POINT('Ctrl Pts',(-0.215070695363695,5.6124175038425,81.1881129215234));
#67806=CARTESIAN_POINT('Ctrl Pts',(-4.8318126828924,2.86340214411448,81.3468736837694));
#67807=CARTESIAN_POINT('Ctrl Pts',(-5.02633211360974,-2.50628632185673,
81.5056344460153));
#67808=CARTESIAN_POINT('Ctrl Pts',(-0.62059886223198,-5.58214499018382,
81.664395208261));
#67809=CARTESIAN_POINT('Ctrl Pts',(4.35312542352183,-3.54905405536124,81.823155970507));
#67810=CARTESIAN_POINT('Ctrl Pts',(5.34273635521072,1.73223955954653,81.9819167327528));
#67811=CARTESIAN_POINT('Ctrl Pts',(1.44251177575087,5.42813461502377,82.1406774949988));
#67812=CARTESIAN_POINT('Ctrl Pts',(-3.77794363750813,4.15603507125568,82.2994382572446));
#67813=CARTESIAN_POINT('Ctrl Pts',(-5.54070964539341,-0.919794726960242,
82.4581990194906));
#67814=CARTESIAN_POINT('Ctrl Pts',(-2.23244892259243,-5.15380027738969,
82.6169597817364));
#67815=CARTESIAN_POINT('Ctrl Pts',(3.11901720681907,-4.6708904238858,82.7757205439823));
#67816=CARTESIAN_POINT('Ctrl Pts',(5.61586359044797,0.0869610864393738,
82.9344813062282));
#67817=CARTESIAN_POINT('Ctrl Pts',(2.97289993650437,4.765223026495,83.0932420684742));
#67818=CARTESIAN_POINT('Ctrl Pts',(-2.39095227805809,5.08220754164499,83.2520028307198));
#67819=CARTESIAN_POINT('Ctrl Pts',(-5.56653245165825,0.747800008209614,
83.4107635929661));
#67820=CARTESIAN_POINT('Ctrl Pts',(-3.64745110432035,-4.27101603744643,
83.5695243552116));
#67821=CARTESIAN_POINT('Ctrl Pts',(1.60988701191321,-5.38086946399345,83.7282851174578));
#67822=CARTESIAN_POINT('Ctrl Pts',(5.39381098887153,-1.56598350543525,83.8870458797035));
#67823=CARTESIAN_POINT('Ctrl Pts',(4.24114744292764,3.68213208808317,84.0458066419495));
#67824=CARTESIAN_POINT('Ctrl Pts',(-0.793130479779808,5.56025999380927,
84.2045674041954));
#67825=CARTESIAN_POINT('Ctrl Pts',(-5.10153665384735,2.3494449931422,84.3633281664411));
#67826=CARTESIAN_POINT('Ctrl Pts',(-4.74081182862427,-3.01160955008047,
84.5220889286872));
#67827=CARTESIAN_POINT('Ctrl Pts',(-0.0412447201429887,-5.61643184914312,
84.680849690933));
#67828=CARTESIAN_POINT('Ctrl Pts',(4.6962499152168,-3.08076173742818,84.8396104531789));
#67829=CARTESIAN_POINT('Ctrl Pts',(5.13525015825041,2.27420453014635,84.9983712154247));
#67830=CARTESIAN_POINT('Ctrl Pts',(0.874969588857335,5.54834518648496,85.1571319776707));
#67831=CARTESIAN_POINT('Ctrl Pts',(-4.1873683648852,3.74332940771524,85.3158927399165));
#67832=CARTESIAN_POINT('Ctrl Pts',(-5.41488683153288,-1.48550727360877,
85.4746535021625));
#67833=CARTESIAN_POINT('Ctrl Pts',(-1.69117083731324,-5.35897524785026,
85.6334142644083));
#67834=CARTESIAN_POINT('Ctrl Pts',(3.58937574805651,-4.3194834039373,85.7921750266543));
#67835=CARTESIAN_POINT('Ctrl Pts',(5.23680883419176,-0.173451275228434,
85.9244756618591));
#67836=CARTESIAN_POINT('Ctrl Pts',(4.02828187061023,2.86869243836803,86.0303161700231));
#67837=CARTESIAN_POINT('Ctrl Pts',(2.79564340622479,3.92301449006468,86.083236424105));
#67838=CARTESIAN_POINT('Ctrl Pts',(2.08577545033815,4.26978275451652,86.109696551146));
#67839=CARTESIAN_POINT('Ctrl Pts',(2.64867169498355,-3.71434815979776,25.890303448854));
#67840=CARTESIAN_POINT('Ctrl Pts',(3.26619649360659,-3.27399620981999,25.916763575895));
#67841=CARTESIAN_POINT('Ctrl Pts',(4.26716101578614,-2.08115178444252,25.9696838299769));
#67842=CARTESIAN_POINT('Ctrl Pts',(4.93173808918078,0.990295704796579,26.0755243381408));
#67843=CARTESIAN_POINT('Ctrl Pts',(2.71768336588486,4.65659895971115,26.2078249733458));
#67844=CARTESIAN_POINT('Ctrl Pts',(-2.44680000302844,4.80802422056935,26.3665857355916));
#67845=CARTESIAN_POINT('Ctrl Pts',(-5.36205296397033,0.552597707469077,
26.5253464978375));
#67846=CARTESIAN_POINT('Ctrl Pts',(-3.3748453548303,-4.20532476806197,26.6841072600834));
#67847=CARTESIAN_POINT('Ctrl Pts',(1.70375316232487,-5.11609754516703,26.8428680223293));
#67848=CARTESIAN_POINT('Ctrl Pts',(5.22165294276351,-1.34357917457709,27.0016287845752));
#67849=CARTESIAN_POINT('Ctrl Pts',(3.96125258927572,3.65816328556149,27.1603895468211));
#67850=CARTESIAN_POINT('Ctrl Pts',(-0.924981032991848,5.31208345139673,
27.319150309067));
#67851=CARTESIAN_POINT('Ctrl Pts',(-4.96444853774918,2.10409702077966,27.4779110713129));
#67852=CARTESIAN_POINT('Ctrl Pts',(-4.46040303022669,-3.02955771462767,
27.6366718335588));
#67853=CARTESIAN_POINT('Ctrl Pts',(0.125992795951784,-5.39050292069155,
27.7954325958046));
#67854=CARTESIAN_POINT('Ctrl Pts',(4.59704837888827,-2.8178773262279,27.9541933580506));
#67855=CARTESIAN_POINT('Ctrl Pts',(4.86075937558651,2.33374633870135,28.1129541202964));
#67856=CARTESIAN_POINT('Ctrl Pts',(0.67574734249545,5.34945894155921,28.2717148825423));
#67857=CARTESIAN_POINT('Ctrl Pts',(-4.12772534408922,3.46918077578477,28.4304756447882));
#67858=CARTESIAN_POINT('Ctrl Pts',(-5.15337977793343,-1.58619627522226,
28.5892364070341));
#67859=CARTESIAN_POINT('Ctrl Pts',(-1.46250254869165,-5.18983873767588,
28.74799716928));
#67860=CARTESIAN_POINT('Ctrl Pts',(3.56690112283287,-4.04358189961183,28.9067579315259));
#67861=CARTESIAN_POINT('Ctrl Pts',(5.3317682282855,0.803484416727951,29.0655186937718));
#67862=CARTESIAN_POINT('Ctrl Pts',(2.2168380367468,4.91517735084379,29.2242794560177));
#67863=CARTESIAN_POINT('Ctrl Pts',(-2.92700996008437,4.52834978587781,29.3830402182635));
#67864=CARTESIAN_POINT('Ctrl Pts',(-5.39196907660498,-0.00296179645705061,
29.5418009805095));
#67865=CARTESIAN_POINT('Ctrl Pts',(-2.92203337252994,-4.5315626662565,29.7005617427553));
#67866=CARTESIAN_POINT('Ctrl Pts',(2.22223651734922,-4.91273895817748,29.8593225050013));
#67867=CARTESIAN_POINT('Ctrl Pts',(5.33264767340791,-0.797626497839672,
30.0180832672471));
#67868=CARTESIAN_POINT('Ctrl Pts',(3.56245678780991,4.04749809913968,30.176844029493));
#67869=CARTESIAN_POINT('Ctrl Pts',(-1.46820336502753,5.18822880230289,30.3356047917389));
#67870=CARTESIAN_POINT('Ctrl Pts',(-5.15511895218379,1.58053402963151,30.4943655539848));
#67871=CARTESIAN_POINT('Ctrl Pts',(-4.12391220870013,-3.47371376528387,
30.6531263162307));
#67872=CARTESIAN_POINT('Ctrl Pts',(0.681624954493375,-5.34871261609428,
30.8118870784765));
#67873=CARTESIAN_POINT('Ctrl Pts',(4.86331813894988,-2.32840630217865,30.9706478407225));
#67874=CARTESIAN_POINT('Ctrl Pts',(4.59395401058964,2.82292858162795,31.1294086029683));
#67875=CARTESIAN_POINT('Ctrl Pts',(0.120062847618306,5.39063300003123,31.2881693652142));
#67876=CARTESIAN_POINT('Ctrl Pts',(-4.46371350087791,3.02466543778803,31.4469301274601));
#67877=CARTESIAN_POINT('Ctrl Pts',(-4.96216290745751,-2.10956832273333,
31.605690889706));
#67878=CARTESIAN_POINT('Ctrl Pts',(-0.919089249897086,-5.31306071668268,
31.7644516519519));
#67879=CARTESIAN_POINT('Ctrl Pts',(3.96516296311825,-3.65387765317291,31.9232124141978));
#67880=CARTESIAN_POINT('Ctrl Pts',(5.22037691480677,1.34944584766767,32.0819731764437));
#67881=CARTESIAN_POINT('Ctrl Pts',(1.69774245557567,5.11771528936226,32.2407339386896));
#67882=CARTESIAN_POINT('Ctrl Pts',(-3.37871775721717,4.20209537558378,32.3994947009355));
#67883=CARTESIAN_POINT('Ctrl Pts',(-5.36287227432698,-0.559410580603594,
32.5582554631813));
#67884=CARTESIAN_POINT('Ctrl Pts',(-2.43876227490629,-4.80892688600382,
32.7170162254272));
#67885=CARTESIAN_POINT('Ctrl Pts',(2.71737745147233,-4.65716641474905,32.8757769876731));
#67886=CARTESIAN_POINT('Ctrl Pts',(5.38649033088843,-0.24302498571551,33.034537749919));
#67887=CARTESIAN_POINT('Ctrl Pts',(3.12572272698597,4.39354033353968,33.1932985121649));
#67888=CARTESIAN_POINT('Ctrl Pts',(-1.99580179309791,5.00900333710248,33.3520592744107));
#67889=CARTESIAN_POINT('Ctrl Pts',(-5.29070754957905,1.04007348454996,33.5108200366567));
#67890=CARTESIAN_POINT('Ctrl Pts',(-3.74339614991909,-3.88076339052093,
33.6695807989025));
#67891=CARTESIAN_POINT('Ctrl Pts',(1.22998574967103,-5.24980707112582,33.8283415611485));
#67892=CARTESIAN_POINT('Ctrl Pts',(5.07764712075832,-1.81406696279143,33.9871023233943));
#67893=CARTESIAN_POINT('Ctrl Pts',(4.2780907481768,3.28196264128657,34.1458630856403));
#67894=CARTESIAN_POINT('Ctrl Pts',(-0.436904953119544,5.37423978720491,
34.3046238478861));
#67895=CARTESIAN_POINT('Ctrl Pts',(-4.75203189588531,2.54784852158155,34.463384610132));
#67896=CARTESIAN_POINT('Ctrl Pts',(-4.71795409483259,-2.61041153603965,
34.6221453723779));
#67897=CARTESIAN_POINT('Ctrl Pts',(-0.36586059440485,-5.3795432198188,34.7809061346238));
#67898=CARTESIAN_POINT('Ctrl Pts',(4.32107969737961,-3.22515262853255,34.9396668968697));
#67899=CARTESIAN_POINT('Ctrl Pts',(5.05323586102427,1.88099616195643,35.0984276591155));
#67900=CARTESIAN_POINT('Ctrl Pts',(1.16051621156039,5.265599809247,35.2571884213615));
#67901=CARTESIAN_POINT('Ctrl Pts',(-3.79434332315281,3.83096567127432,35.4159491836074));
#67902=CARTESIAN_POINT('Ctrl Pts',(-5.27650394879067,-1.10988526741874,
35.5747099458532));
#67903=CARTESIAN_POINT('Ctrl Pts',(-1.92944698758358,-5.03493530748322,
35.7334707080991));
#67904=CARTESIAN_POINT('Ctrl Pts',(3.18349879238559,-4.3518587600376,35.892231470345));
#67905=CARTESIAN_POINT('Ctrl Pts',(5.38280923632674,0.314171853851074,36.0509922325909));
#67906=CARTESIAN_POINT('Ctrl Pts',(2.65560824713265,4.69266279059105,36.2097529948368));
#67907=CARTESIAN_POINT('Ctrl Pts',(-2.50208652644733,4.77628540213074,36.3685137570827));
#67908=CARTESIAN_POINT('Ctrl Pts',(-5.36979528379463,0.488505720103176,
36.5272745193286));
#67909=CARTESIAN_POINT('Ctrl Pts',(-3.32290337488047,-4.24636931856435,
36.6860352815745));
#67910=CARTESIAN_POINT('Ctrl Pts',(1.76521120212947,-5.09483744984206,36.8447960438204));
#67911=CARTESIAN_POINT('Ctrl Pts',(5.23775056787229,-1.28035472318811,37.0035568060662));
#67912=CARTESIAN_POINT('Ctrl Pts',(3.91654062472413,3.70594775507185,37.1623175683121));
#67913=CARTESIAN_POINT('Ctrl Pts',(-0.98920693046264,5.30045364824194,37.321078330558));
#67914=CARTESIAN_POINT('Ctrl Pts',(-4.98960208717089,2.04382245807619,37.4798390928039));
#67915=CARTESIAN_POINT('Ctrl Pts',(-4.42336100432008,-3.08337747509074,
37.6385998550498));
#67916=CARTESIAN_POINT('Ctrl Pts',(0.191275183005581,-5.38857616006331,
37.7973606172957));
#67917=CARTESIAN_POINT('Ctrl Pts',(4.63085048026802,-2.761985347144,37.9561213795416));
#67918=CARTESIAN_POINT('Ctrl Pts',(4.83212996681944,2.39245882142244,38.1148821417875));
#67919=CARTESIAN_POINT('Ctrl Pts',(0.610896508406062,5.35725159801683,38.2736429040334));
#67920=CARTESIAN_POINT('Ctrl Pts',(-4.16944809457737,3.41892407272547,38.4324036662793));
#67921=CARTESIAN_POINT('Ctrl Pts',(-5.13378644395327,-1.64850719631984,
38.5911644285251));
#67922=CARTESIAN_POINT('Ctrl Pts',(-1.39952662627435,-5.20717432498527,
38.7499251907711));
#67923=CARTESIAN_POINT('Ctrl Pts',(3.61562270886826,-4.00007645621339,38.9086859530169));
#67924=CARTESIAN_POINT('Ctrl Pts',(5.32164370022099,0.868013569211233,39.0674467152629));
#67925=CARTESIAN_POINT('Ctrl Pts',(2.15713382540813,4.94167106227405,39.2262074775087));
#67926=CARTESIAN_POINT('Ctrl Pts',(-2.98165081692889,4.49256025383564,39.3849682397546));
#67927=CARTESIAN_POINT('Ctrl Pts',(-5.39153755590251,-0.0682789259528612,
39.5437290020005));
#67928=CARTESIAN_POINT('Ctrl Pts',(-2.8669244370552,-4.56662714710238,39.7024897642464));
#67929=CARTESIAN_POINT('Ctrl Pts',(2.28158549793223,-4.88545871378134,39.8612505264922));
#67930=CARTESIAN_POINT('Ctrl Pts',(5.3419186932756,-0.732969237328121,40.0200112887382));
#67931=CARTESIAN_POINT('Ctrl Pts',(3.51316472950203,4.09035607396464,40.1787720509841));
#67932=CARTESIAN_POINT('Ctrl Pts',(-1.53094490572569,5.17006256481187,40.3375328132299));
#67933=CARTESIAN_POINT('Ctrl Pts',(-5.17388699991225,1.517969874726,40.4962935754758));
#67934=CARTESIAN_POINT('Ctrl Pts',(-4.08152967334293,-3.52341521170266,
40.6550543377217));
#67935=CARTESIAN_POINT('Ctrl Pts',(0.746368282217007,-5.34006307226206,
40.8138150999676));
#67936=CARTESIAN_POINT('Ctrl Pts',(4.89116718777592,-2.26932209473684,40.9725758622135));
#67937=CARTESIAN_POINT('Ctrl Pts',(4.55942048043523,2.87837178123751,41.1313366244594));
#67938=CARTESIAN_POINT('Ctrl Pts',(0.054752880088232,5.39169188201243,41.2900973867052));
#67939=CARTESIAN_POINT('Ctrl Pts',(-4.50002622856399,2.97037088099662,41.4488581489512));
#67940=CARTESIAN_POINT('Ctrl Pts',(-4.93624387774355,-2.16952428146721,
41.607618911197));
#67941=CARTESIAN_POINT('Ctrl Pts',(-0.854660350479725,-5.32380455255023,
41.766379673443));
#67942=CARTESIAN_POINT('Ctrl Pts',(4.00913443548347,-3.60557627941182,41.9251404356888));
#67943=CARTESIAN_POINT('Ctrl Pts',(5.20364692548634,1.41258553840574,42.0839011979347));
#67944=CARTESIAN_POINT('Ctrl Pts',(1.63562280181919,5.13790592348729,42.2426619601806));
#67945=CARTESIAN_POINT('Ctrl Pts',(-3.42937327082192,4.16085786801338,42.4014227224264));
#67946=CARTESIAN_POINT('Ctrl Pts',(-5.3557021744363,-0.62433440332485,42.5601834846724));
#67947=CARTESIAN_POINT('Ctrl Pts',(-2.38032885595355,-4.83811675819748,
42.7189442469182));
#67948=CARTESIAN_POINT('Ctrl Pts',(2.77359413958947,-4.62390687376719,42.8777050091642));
#67949=CARTESIAN_POINT('Ctrl Pts',(5.38903905804413,-0.177756179390683,
43.03646577141));
#67950=CARTESIAN_POINT('Ctrl Pts',(3.07227082023542,4.43108239999738,43.195226533656));
#67951=CARTESIAN_POINT('Ctrl Pts',(-2.05633351598682,4.9844590177336,43.3539872959018));
#67952=CARTESIAN_POINT('Ctrl Pts',(-5.30291860685286,0.975906490156919,
43.5127480581477));
#67953=CARTESIAN_POINT('Ctrl Pts',(-3.6961106089692,-3.92582546666328,43.6715088203936));
#67954=CARTESIAN_POINT('Ctrl Pts',(1.29349071741166,-5.23452204049296,43.8302695826395));
#67955=CARTESIAN_POINT('Ctrl Pts',(5.09924982902894,-1.75242415230585,43.9890303448854));
#67956=CARTESIAN_POINT('Ctrl Pts',(4.23801973850483,3.33354584856425,44.1477911071313));
#67957=CARTESIAN_POINT('Ctrl Pts',(-0.501975468697378,5.36855286434462,
44.3065518693772));
#67958=CARTESIAN_POINT('Ctrl Pts',(-4.78254739390742,2.4900963140943,44.4653126316231));
#67959=CARTESIAN_POINT('Ctrl Pts',(-4.68598585940108,-2.66737244379737,
44.624073393869));
#67960=CARTESIAN_POINT('Ctrl Pts',(-0.300666931069113,-5.38358046517354,
44.7828341561148));
#67961=CARTESIAN_POINT('Ctrl Pts',(4.35983155656832,-3.1725712012164,44.9415949183607));
#67962=CARTESIAN_POINT('Ctrl Pts',(5.03007903084552,1.94207213354316,45.1003556806066));
#67963=CARTESIAN_POINT('Ctrl Pts',(1.0966445303283,5.27927173031827,45.2591164428526));
#67964=CARTESIAN_POINT('Ctrl Pts',(-3.84047254178868,3.78472058205141,45.4178772050983));
#67965=CARTESIAN_POINT('Ctrl Pts',(-5.26267183489948,-1.17372244870432,
45.5766379673443));
#67966=CARTESIAN_POINT('Ctrl Pts',(-1.86831311430597,-5.05793884258687,
45.7353987295902));
#67967=CARTESIAN_POINT('Ctrl Pts',(3.23598283686748,-4.3129751109803,45.8941594918361));
#67968=CARTESIAN_POINT('Ctrl Pts',(5.37860845135706,0.379355183735526,46.052920254082));
#67969=CARTESIAN_POINT('Ctrl Pts',(2.59856731943033,4.72448802674167,46.2116810163278));
#67970=CARTESIAN_POINT('Ctrl Pts',(-2.55976199751136,4.745625116308,46.3704417785738));
#67971=CARTESIAN_POINT('Ctrl Pts',(-5.37531894538233,0.423421142422616,
46.5292025408196));
#67972=CARTESIAN_POINT('Ctrl Pts',(-3.27121980318429,-4.28631079457517,
46.6879633030656));
#67973=CARTESIAN_POINT('Ctrl Pts',(1.82679962359794,-5.07308016530974,46.8467240653114));
#67974=CARTESIAN_POINT('Ctrl Pts',(5.25287623454225,-1.21681160950152,47.0054848275573));
#67975=CARTESIAN_POINT('Ctrl Pts',(3.87136006443976,3.75312009931705,47.1642455898032));
#67976=CARTESIAN_POINT('Ctrl Pts',(-1.05334308887091,5.28808165269453,47.3230063520491));
#67977=CARTESIAN_POINT('Ctrl Pts',(-5.01399447246331,1.98322935096872,47.4817671142949));
#67978=CARTESIAN_POINT('Ctrl Pts',(-4.38568496040199,-3.13673503129295,
47.6405278765409));
#67979=CARTESIAN_POINT('Ctrl Pts',(0.256537389910642,-5.38586370009625,
47.7992886387868));
#67980=CARTESIAN_POINT('Ctrl Pts',(4.66396888494043,-2.70568539722266,47.9580494010326));
#67981=CARTESIAN_POINT('Ctrl Pts',(4.80279359368822,2.45081882742566,48.1168101632785));
#67982=CARTESIAN_POINT('Ctrl Pts',(0.545954902252042,5.3642587999782,48.2755709255244));
#67983=CARTESIAN_POINT('Ctrl Pts',(-4.21055839213486,3.36816526537215,48.4343316877703));
#67984=CARTESIAN_POINT('Ctrl Pts',(-5.11344003285917,-1.71057600205014,
48.5930924500163));
#67985=CARTESIAN_POINT('Ctrl Pts',(-1.33634516345125,-5.22374586217178,
48.751853212262));
#67986=CARTESIAN_POINT('Ctrl Pts',(3.66381361874176,-3.9559839478389,48.910613974508));
#67987=CARTESIAN_POINT('Ctrl Pts',(5.31073826441816,0.932415312659234,49.0693747367539));
#67988=CARTESIAN_POINT('Ctrl Pts',(2.09711303188655,4.96743959801509,49.2281354989997));
#67989=CARTESIAN_POINT('Ctrl Pts',(-3.03585410457926,4.45611143084931,49.3868962612457));
#67990=CARTESIAN_POINT('Ctrl Pts',(-5.39031483316305,-0.133586031525688,
49.5456570234915));
#67991=CARTESIAN_POINT('Ctrl Pts',(-2.81139477712564,-4.60102147740992,
49.7044177857375));
#67992=CARTESIAN_POINT('Ctrl Pts',(2.34059965410881,-4.85746152713764,49.8631785479833));
#67993=CARTESIAN_POINT('Ctrl Pts',(5.35040578735549,-0.668204414134744,
50.0219393102293));
#67994=CARTESIAN_POINT('Ctrl Pts',(3.46335711374174,4.13261378925387,50.180700072475));
#67995=CARTESIAN_POINT('Ctrl Pts',(-1.59346177998899,5.15113762038552,50.339460834721));
#67996=CARTESIAN_POINT('Ctrl Pts',(-5.19189577974993,1.45518295779302,50.4982215969668));
#67997=CARTESIAN_POINT('Ctrl Pts',(-4.03854817336226,-3.57259959691384,
50.6569823592128));
#67998=CARTESIAN_POINT('Ctrl Pts',(0.811002080346741,-5.33062987404959,
50.8157431214586));
#67999=CARTESIAN_POINT('Ctrl Pts',(4.91829845774134,-2.2099048642455,50.9745038837045));
#68000=CARTESIAN_POINT('Ctrl Pts',(4.5242178552285,2.93339257973907,51.1332646459504));
#68001=CARTESIAN_POINT('Ctrl Pts',(-0.0105651224232033,5.3919595331034,
51.2920254081963));
#68002=CARTESIAN_POINT('Ctrl Pts',(-4.53567857731733,2.91564042222309,51.4507861704422));
#68003=CARTESIAN_POINT('Ctrl Pts',(-4.90960045414457,-2.22916186247211,
51.6095469326881));
#68004=CARTESIAN_POINT('Ctrl Pts',(-0.790106029640123,-5.33376711999718,
51.7683076949339));
#68005=CARTESIAN_POINT('Ctrl Pts',(4.05251756729386,-3.55674578726275,51.92706845718));
#68006=CARTESIAN_POINT('Ctrl Pts',(5.18615330087962,1.47551793218919,52.0858292194257));
#68007=CARTESIAN_POINT('Ctrl Pts',(1.57326312038517,5.15734256981952,52.2445899816717));
#68008=CARTESIAN_POINT('Ctrl Pts',(-3.47952552383355,4.11900975447104,52.4033507439175));
#68009=CARTESIAN_POINT('Ctrl Pts',(-5.34774612514876,-0.689166604960497,
52.5621115061635));
#68010=CARTESIAN_POINT('Ctrl Pts',(-2.32154612369557,-4.86659663666414,
52.7208722684093));
#68011=CARTESIAN_POINT('Ctrl Pts',(2.82940380271352,-4.58996877436295,52.8796330306552));
#68012=CARTESIAN_POINT('Ctrl Pts',(5.39079694361469,-0.112461287343052,
53.0383937929012));
#68013=CARTESIAN_POINT('Ctrl Pts',(3.01836805768307,4.46797420502795,53.1971545551469));
#68014=CARTESIAN_POINT('Ctrl Pts',(-2.11656347189292,4.95918322890829,53.355915317393));
#68015=CARTESIAN_POINT('Ctrl Pts',(-5.31435146071946,0.911596281467614,
53.5146760796387));
#68016=CARTESIAN_POINT('Ctrl Pts',(-3.64828266371651,-3.97031142784319,
53.6734368418848));
#68017=CARTESIAN_POINT('Ctrl Pts',(1.35680586536473,-5.21846884365023,53.8321976041305));
#68018=CARTESIAN_POINT('Ctrl Pts',(5.1201042222894,-1.69052417354231,53.9909583663765));
#68019=CARTESIAN_POINT('Ctrl Pts',(4.19732679935496,3.38463985792481,54.1497191286223));
#68020=CARTESIAN_POINT('Ctrl Pts',(-0.56697231936563,5.36207810624853,54.3084798908682));
#68021=CARTESIAN_POINT('Ctrl Pts',(-4.81236105300778,2.43197868492519,54.4672406531142));
#68022=CARTESIAN_POINT('Ctrl Pts',(-4.65332995545485,-2.72394191459784,
54.6260014153599));
#68023=CARTESIAN_POINT('Ctrl Pts',(-0.235429144855458,-5.3868276699918,
54.784762177606));
#68024=CARTESIAN_POINT('Ctrl Pts',(4.39794361039255,-3.11952419901562,54.9435229398517));
#68025=CARTESIAN_POINT('Ctrl Pts',(5.00618403647253,2.002863106007,55.1022837020977));
#68026=CARTESIAN_POINT('Ctrl Pts',(1.03261191649043,5.29216891816187,55.2610444643436));
#68027=CARTESIAN_POINT('Ctrl Pts',(-3.88603817100542,3.73792008501059,55.4198052265894));
#68028=CARTESIAN_POINT('Ctrl Pts',(-5.24806742381559,-1.23738738619803,
55.5785659888354));
#68029=CARTESIAN_POINT('Ctrl Pts',(-1.80690506604304,-5.08020012506836,
55.7373267510812));
#68030=CARTESIAN_POINT('Ctrl Pts',(3.287992000806,-4.27345853274282,55.8960875133271));
#68031=CARTESIAN_POINT('Ctrl Pts',(5.37361835549403,0.444482843239534,56.054848275573));
#68032=CARTESIAN_POINT('Ctrl Pts',(2.54114505192401,4.7556199441838,56.2136090378189));
#68033=CARTESIAN_POINT('Ctrl Pts',(-2.61706182345312,4.71426840990844,56.3723698000648));
#68034=CARTESIAN_POINT('Ctrl Pts',(-5.38005377881171,0.358274427681354,
56.5311305623107));
#68035=CARTESIAN_POINT('Ctrl Pts',(-3.21905617991939,-4.32562325439461,
56.6898913245565));
#68036=CARTESIAN_POINT('Ctrl Pts',(1.88811996218651,-5.05057840616592,56.8486520868024));
#68037=CARTESIAN_POINT('Ctrl Pts',(5.26723104152409,-1.15308992868801,57.0074128490484));
#68038=CARTESIAN_POINT('Ctrl Pts',(3.82561138199176,3.79974167311562,57.1661736112942));
#68039=CARTESIAN_POINT('Ctrl Pts',(-1.11732466916059,5.27493363106322,57.3249343735401));
#68040=CARTESIAN_POINT('Ctrl Pts',(-5.03765105397079,1.92234520491603,57.4836951357861));
#68041=CARTESIAN_POINT('Ctrl Pts',(-4.34736531713187,-3.18963227156913,
57.6424558980318));
#68042=CARTESIAN_POINT('Ctrl Pts',(0.321761949948743,-5.38236086452793,
57.8012166602778));
#68043=CARTESIAN_POINT('Ctrl Pts',(4.69640285208957,-2.64898838791747,57.9599774225237));
#68044=CARTESIAN_POINT('Ctrl Pts',(4.77275241050502,2.50881917571891,58.1187381847696));
#68045=CARTESIAN_POINT('Ctrl Pts',(0.480933177205712,5.37047879685782,58.2774989470154));
#68046=CARTESIAN_POINT('Ctrl Pts',(-4.25105079016747,3.31691217970165,58.4362597092614));
#68047=CARTESIAN_POINT('Ctrl Pts',(-5.09234322434225,-1.77239378071924,
58.5950204715072));
#68048=CARTESIAN_POINT('Ctrl Pts',(-1.27296759194985,-5.23955081455291,
58.7537812337532));
#68049=CARTESIAN_POINT('Ctrl Pts',(3.71146686389641,-3.91131089874422,58.912541995999));
#68050=CARTESIAN_POINT('Ctrl Pts',(5.29905347767321,0.996680224142156,59.071302758245));
#68051=CARTESIAN_POINT('Ctrl Pts',(2.03678448698746,4.99247916189982,59.2300635204907));
#68052=CARTESIAN_POINT('Ctrl Pts',(-3.08961188058148,4.41900867342512,59.3888242827367));
#68053=CARTESIAN_POINT('Ctrl Pts',(-5.38830108161851,-0.198873533345728,
59.5475850449826));
#68054=CARTESIAN_POINT('Ctrl Pts',(-2.7554525449587,-4.63474060772737,59.7063458072284));
#68055=CARTESIAN_POINT('Ctrl Pts',(2.39927032724118,-4.82875150792175,59.8651065694744));
#68056=CARTESIAN_POINT('Ctrl Pts',(5.35810770928357,-0.603341531930828,
60.0238673317202));
#68057=CARTESIAN_POINT('Ctrl Pts',(3.4130412502586,4.17426504339022,60.1826280939662));
#68058=CARTESIAN_POINT('Ctrl Pts',(-1.65574481370544,5.13145674641463,60.341388856212));
#68059=CARTESIAN_POINT('Ctrl Pts',(-5.20914264878242,1.39218249273314,60.500149618458));
#68060=CARTESIAN_POINT('Ctrl Pts',(-3.99497401635973,-3.62125970306563,
60.6589103807038));
#68061=CARTESIAN_POINT('Ctrl Pts',(0.875516863905577,-5.32041440580089,
60.8176711429497));
#68062=CARTESIAN_POINT('Ctrl Pts',(4.94470796731371,-2.15016333017309,60.9764319051956));
#68063=CARTESIAN_POINT('Ctrl Pts',(4.48835130096483,2.98798290282324,61.1351926674415));
#68064=CARTESIAN_POINT('Ctrl Pts',(-0.0758815745026817,5.39143591402955,
61.2939534296874));
#68065=CARTESIAN_POINT('Ctrl Pts',(-4.57066531515243,2.86048209316173,61.4527141919332));
#68066=CARTESIAN_POINT('Ctrl Pts',(-4.88223654658481,-2.2884723139309,61.6114749541792));
#68067=CARTESIAN_POINT('Ctrl Pts',(-0.725435760725668,-5.34294695701698,
61.770235716425));
#68068=CARTESIAN_POINT('Ctrl Pts',(4.09530599207347,-3.50739334260129,61.9289964786709));
#68069=CARTESIAN_POINT('Ctrl Pts',(5.16789860817661,1.53823379368774,62.0877572409168));
#68070=CARTESIAN_POINT('Ctrl Pts',(1.51067256255815,5.17602237603069,62.2465180031627));
#68071=CARTESIAN_POINT('Ctrl Pts',(-3.52916715640777,4.07655717616831,62.4052787654086));
#68072=CARTESIAN_POINT('Ctrl Pts',(-5.33900529401489,-0.75389767138361,
62.5640395276545));
#68073=CARTESIAN_POINT('Ctrl Pts',(-2.26242270449944,-4.89436234198102,
62.7228002899004));
#68074=CARTESIAN_POINT('Ctrl Pts',(2.88479825077521,-4.5553570969531,62.8815610521463));
#68075=CARTESIAN_POINT('Ctrl Pts',(5.39176372963048,-0.0471498915993996,
63.0403218143921));
#68076=CARTESIAN_POINT('Ctrl Pts',(2.96402234956039,4.50421033475823,63.1990825766381));
#68077=CARTESIAN_POINT('Ctrl Pts',(-2.17648282206887,4.93317967984907,63.3578433388838));
#68078=CARTESIAN_POINT('Ctrl Pts',(-5.32500443340729,0.847152296006667,
63.5166041011299));
#68079=CARTESIAN_POINT('Ctrl Pts',(-3.59991933291304,-4.01421474574488,
63.6753648633757));
#68080=CARTESIAN_POINT('Ctrl Pts',(1.41992190203103,-5.20164983640472,63.8341256256216));
#68081=CARTESIAN_POINT('Ctrl Pts',(5.14020724015703,-1.62837611032391,63.9928863878675));
#68082=CARTESIAN_POINT('Ctrl Pts',(4.15601790241685,3.43523717132127,64.1516471501133));
#68083=CARTESIAN_POINT('Ctrl Pts',(-0.631885966835028,5.35481646308756,
64.3104079123593));
#68084=CARTESIAN_POINT('Ctrl Pts',(-4.84146849803133,2.3735041628375,64.4691686746051));
#68085=CARTESIAN_POINT('Ctrl Pts',(-4.61999117524849,-2.7801116468701,64.6279294368511));
#68086=CARTESIAN_POINT('Ctrl Pts',(-0.170156809410319,-5.38928435774618,
64.7866901990969));
#68087=CARTESIAN_POINT('Ctrl Pts',(4.43541026590754,-3.06601940657889,64.9454509613428));
#68088=CARTESIAN_POINT('Ctrl Pts',(4.98155438449627,2.06336015827155,65.1042117235887));
#68089=CARTESIAN_POINT('Ctrl Pts',(0.968427766834154,5.30428948011521,65.2629724858346));
#68090=CARTESIAN_POINT('Ctrl Pts',(-3.93103352404596,3.69057104812572,65.4217332480805));
#68091=CARTESIAN_POINT('Ctrl Pts',(-5.23269285873673,-1.30087073706907,
65.5804940103263));
#68092=CARTESIAN_POINT('Ctrl Pts',(-1.74523185442701,-5.10171588808409,
65.7392547725724));
#68093=CARTESIAN_POINT('Ctrl Pts',(3.33951865185531,-4.23331482438371,65.8980155348181));
#68094=CARTESIAN_POINT('Ctrl Pts',(5.36783968103429,0.50954527487755,66.0567762970641));
#68095=CARTESIAN_POINT('Ctrl Pts',(2.48334987133277,4.78605397430791,66.2155370593099));
#68096=CARTESIAN_POINT('Ctrl Pts',(-2.67397759552212,4.68221988452942,66.3742978215559));
#68097=CARTESIAN_POINT('Ctrl Pts',(-5.38399908924589,0.29307513616095,66.5330585838017));
#68098=CARTESIAN_POINT('Ctrl Pts',(-3.16642016009836,-4.36430092891852,
66.6918193460477));
#68099=CARTESIAN_POINT('Ctrl Pts',(1.94916321913439,-5.0273354745442,66.8505801082934));
#68100=CARTESIAN_POINT('Ctrl Pts',(5.2808128822496,-1.08919903190536,67.0093408705395));
#68101=CARTESIAN_POINT('Ctrl Pts',(3.77930129100008,3.84580563475087,67.1681016327852));
#68102=CARTESIAN_POINT('Ctrl Pts',(-1.18114228203367,5.26101151282039,67.3268623950312));
#68103=CARTESIAN_POINT('Ctrl Pts',(-5.06056836008944,1.86117895466771,67.485623157277));
#68104=CARTESIAN_POINT('Ctrl Pts',(-4.30840769791819,-3.24206143324834,
67.644383919523));
#68105=CARTESIAN_POINT('Ctrl Pts',(0.386939291414611,-5.37806816739956,
67.8031446817688));
#68106=CARTESIAN_POINT('Ctrl Pts',(4.72814762203013,-2.59190263951545,67.9619054440148));
#68107=CARTESIAN_POINT('Ctrl Pts',(4.74201082581408,2.56645135475007,68.1206662062606));
#68108=CARTESIAN_POINT('Ctrl Pts',(0.415840875206383,5.37591067587102,68.2794269685066));
#68109=CARTESIAN_POINT('Ctrl Pts',(-4.29091934641509,3.26517233710519,68.4381877307524));
#68110=CARTESIAN_POINT('Ctrl Pts',(-5.07049911435956,-1.83395146056701,
68.5969484929983));
#68111=CARTESIAN_POINT('Ctrl Pts',(-1.20940321242992,-5.25458686275155,
68.7557092552442));
#68112=CARTESIAN_POINT('Ctrl Pts',(3.75857545121767,-3.86606386470014,68.9144700174901));
#68113=CARTESIAN_POINT('Ctrl Pts',(5.28659105472879,1.06079887278309,69.073230779736));
#68114=CARTESIAN_POINT('Ctrl Pts',(1.97615704392586,5.01678607937179,69.2319915419818));
#68115=CARTESIAN_POINT('Ctrl Pts',(-3.14291625598096,4.38125742639343,69.3907523042277));
#68116=CARTESIAN_POINT('Ctrl Pts',(-5.38549659678694,-0.264131850470941,
69.5495130664737));
#68117=CARTESIAN_POINT('Ctrl Pts',(-2.69910595007792,-4.66777958977181,
69.7082738287194));
#68118=CARTESIAN_POINT('Ctrl Pts',(2.45758890740704,-4.79933286932947,69.8670345909655));
#68119=CARTESIAN_POINT('Ctrl Pts',(5.36502332880251,-0.538390109345589,
70.0257953532112));
#68120=CARTESIAN_POINT('Ctrl Pts',(3.36222452290666,4.21530372405138,70.1845561154571));
#68121=CARTESIAN_POINT('Ctrl Pts',(-1.7177848668387,5.11102283106786,70.3433168777031));
#68122=CARTESIAN_POINT('Ctrl Pts',(-5.22562507603134,1.32897772486576,70.5020776399489));
#68123=CARTESIAN_POINT('Ctrl Pts',(-3.95081359684368,-3.66938838928662,
70.6608384021949));
#68124=CARTESIAN_POINT('Ctrl Pts',(0.939903165347853,-5.3094181666361,70.8195991644408));
#68125=CARTESIAN_POINT('Ctrl Pts',(4.97039184089704,-2.09010625959075,70.9783599266866));
#68126=CARTESIAN_POINT('Ctrl Pts',(4.45182608106173,3.0421347393591,71.1371206889325));
#68127=CARTESIAN_POINT('Ctrl Pts',(-0.141186890959645,5.39012110163196,
71.2958814511784));
#68128=CARTESIAN_POINT('Ctrl Pts',(-4.60498130776496,2.80490398829831,71.4546422134243));
#68129=CARTESIAN_POINT('Ctrl Pts',(-4.85415617071822,-2.34744693203373,
71.6134029756702));
#68130=CARTESIAN_POINT('Ctrl Pts',(-0.660659034099426,-5.35134271646838,
71.7721637379161));
#68131=CARTESIAN_POINT('Ctrl Pts',(4.13749343062021,-3.4575261878996,71.9309245001619));
#68132=CARTESIAN_POINT('Ctrl Pts',(5.14888552625377,1.60072391934755,72.0896852624079));
#68133=CARTESIAN_POINT('Ctrl Pts',(1.44786031350356,5.19394260085899,72.2484460246537));
#68134=CARTESIAN_POINT('Ctrl Pts',(-3.57829088363412,4.03350636302179,72.4072067868997));
#68135=CARTESIAN_POINT('Ctrl Pts',(-5.32948096375172,-0.818518103308924,
72.5659675491455));
#68136=CARTESIAN_POINT('Ctrl Pts',(-2.20296727472809,-4.92140979953042,
72.7247283113914));
#68137=CARTESIAN_POINT('Ctrl Pts',(2.93976935463837,-4.52007692080191,72.8834890736374));
#68138=CARTESIAN_POINT('Ctrl Pts',(5.39193927421552,0.0181684233918482,
73.0422498358832));
#68139=CARTESIAN_POINT('Ctrl Pts',(2.90924167110106,4.53978547153557,73.201010598129));
#68140=CARTESIAN_POINT('Ctrl Pts',(-2.23608277334895,4.90645218657722,73.359771360375));
#68141=CARTESIAN_POINT('Ctrl Pts',(-5.33487596159239,0.782583990930051,
73.5185321226207));
#68142=CARTESIAN_POINT('Ctrl Pts',(-3.5510277138785,-4.05752897755565,73.6772928848669));
#68143=CARTESIAN_POINT('Ctrl Pts',(1.48282956513097,-5.18406748694598,73.8360536471125));
#68144=CARTESIAN_POINT('Ctrl Pts',(5.15955593251365,-1.56598908288006,73.9948144093587));
#68145=CARTESIAN_POINT('Ctrl Pts',(4.11409910977184,3.48533036359696,74.1535751716043));
#68146=CARTESIAN_POINT('Ctrl Pts',(-0.696706885026663,5.34676900050795,
74.3123359338504));
#68147=CARTESIAN_POINT('Ctrl Pts',(-4.86986545745996,2.31468132896846,74.4710966960961));
#68148=CARTESIAN_POINT('Ctrl Pts',(-4.58597441124858,-2.83587339770487,
74.6298574583422));
#68149=CARTESIAN_POINT('Ctrl Pts',(-0.104859503450096,-5.39095016791776,
74.7886182205879));
#68150=CARTESIAN_POINT('Ctrl Pts',(4.47222602488106,-3.01206467573539,74.9473789828339));
#68151=CARTESIAN_POINT('Ctrl Pts',(4.95619368931852,2.12355441239345,75.1061397450797));
#68152=CARTESIAN_POINT('Ctrl Pts',(0.904101500384337,5.31563163748572,75.2649005073256));
#68153=CARTESIAN_POINT('Ctrl Pts',(-3.97545199784159,3.64268041986863,75.4236612695716));
#68154=CARTESIAN_POINT('Ctrl Pts',(-5.21655039588045,-1.36416318513457,
75.5824220318174));
#68155=CARTESIAN_POINT('Ctrl Pts',(-1.68330253000285,-5.12248297419546,
75.7411827940633));
#68156=CARTESIAN_POINT('Ctrl Pts',(3.39055522847852,-4.19254987699292,75.8999435563093));
#68157=CARTESIAN_POINT('Ctrl Pts',(5.36127327599845,0.574532930736923,76.058704318555));
#68158=CARTESIAN_POINT('Ctrl Pts',(2.42519025910013,4.81578565091957,76.217465080801));
#68159=CARTESIAN_POINT('Ctrl Pts',(-2.73050096132775,4.64948424329249,76.3762258430469));
#68160=CARTESIAN_POINT('Ctrl Pts',(-5.38715429771053,0.227832835858649,
76.5349866052928));
#68161=CARTESIAN_POINT('Ctrl Pts',(-3.11331946805805,-4.40233814219751,
76.6937473675387));
#68162=CARTESIAN_POINT('Ctrl Pts',(2.00992043634247,-5.00335478134514,76.8525081297845));
#68163=CARTESIAN_POINT('Ctrl Pts',(5.29361976358337,-1.02514829514396,77.0112688920305));
#68164=CARTESIAN_POINT('Ctrl Pts',(3.73243658747159,3.89130522433545,77.1700296542762));
#68165=CARTESIAN_POINT('Ctrl Pts',(-1.24478656225425,5.2463173410372,77.3287904165223));
#68166=CARTESIAN_POINT('Ctrl Pts',(-5.0827430277043,1.79973957637201,77.4875511787681));
#68167=CARTESIAN_POINT('Ctrl Pts',(-4.26881781979216,-3.29401482234996,
77.646311941014));
#68168=CARTESIAN_POINT('Ctrl Pts',(0.452059849531884,-5.3729862386645,77.8050727032599));
#68169=CARTESIAN_POINT('Ctrl Pts',(4.75919853621651,-2.53443652935156,77.9638334655057));
#68170=CARTESIAN_POINT('Ctrl Pts',(4.71057335094352,2.62370690699572,78.1225942277518));
#68171=CARTESIAN_POINT('Ctrl Pts',(0.350687548550617,5.38055363988948,78.2813549899974));
#68172=CARTESIAN_POINT('Ctrl Pts',(-4.33015821016646,3.21295333040559,78.4401157522436));
#68173=CARTESIAN_POINT('Ctrl Pts',(-5.04791090853454,-1.89524000800277,
78.5988765144892));
#68174=CARTESIAN_POINT('Ctrl Pts',(-1.14566135296546,-5.26885180022729,
78.7576372767353));
#68175=CARTESIAN_POINT('Ctrl Pts',(3.80513246751939,-3.82024948570991,78.916398038981));
#68176=CARTESIAN_POINT('Ctrl Pts',(5.27335282444574,1.12476184916915,79.0751588012271));
#68177=CARTESIAN_POINT('Ctrl Pts',(1.91523959978009,5.0403567833905,79.2339195634728));
#68178=CARTESIAN_POINT('Ctrl Pts',(-3.19575940835959,4.34286322975033,79.3926803257188));
#68179=CARTESIAN_POINT('Ctrl Pts',(-5.3819017902265,-0.329351406241924,
79.5514410879647));
#68180=CARTESIAN_POINT('Ctrl Pts',(-2.64236326134738,-4.70013357507201,
79.7102018502106));
#68181=CARTESIAN_POINT('Ctrl Pts',(2.51554683635375,-4.76920992854652,79.8689626124565));
#68182=CARTESIAN_POINT('Ctrl Pts',(5.37115163104497,-0.473359678001532,
80.0277233747023));
#68183=CARTESIAN_POINT('Ctrl Pts',(3.31091438904171,4.25572380881061,80.1864841369483));
#68184=CARTESIAN_POINT('Ctrl Pts',(-1.77957283501041,5.089838873022,80.3452448991941));
#68185=CARTESIAN_POINT('Ctrl Pts',(-5.24134064269895,1.26557792949291,80.50400566144));
#68186=CARTESIAN_POINT('Ctrl Pts',(-3.9060733953589,-3.71697859269313,80.6627664236859));
#68187=CARTESIAN_POINT('Ctrl Pts',(1.00415153598694,-5.29764277024969,80.8215271859318));
#68188=CARTESIAN_POINT('Ctrl Pts',(4.99534630937428,-2.02974246588212,80.9802879481777));
#68189=CARTESIAN_POINT('Ctrl Pts',(4.41464755561157,3.0958401425779,81.1390487104235));
#68190=CARTESIAN_POINT('Ctrl Pts',(-0.206471488267744,5.38801528883197,
81.2978094726694));
#68191=CARTESIAN_POINT('Ctrl Pts',(-4.63862151922447,2.74891426377335,81.4565702349153));
#68192=CARTESIAN_POINT('Ctrl Pts',(-4.82536344745119,-2.40607706235473,
81.6153309971613));
#68193=CARTESIAN_POINT('Ctrl Pts',(-0.595785355535171,-5.35895316608133,
81.7740917594071));
#68194=CARTESIAN_POINT('Ctrl Pts',(4.17907369152063,-3.4071516415317,81.932852521653));
#68195=CARTESIAN_POINT('Ctrl Pts',(5.12911684605883,1.66297913944664,82.0916132838989));
#68196=CARTESIAN_POINT('Ctrl Pts',(1.38483558943104,5.2111006131604,82.2503740461447));
#68197=CARTESIAN_POINT('Ctrl Pts',(-3.62688949375241,3.98986363532597,82.4091348083908));
#68198=CARTESIAN_POINT('Ctrl Pts',(-5.31917453751786,-0.883018422641366,
82.5678955706364));
#68199=CARTESIAN_POINT('Ctrl Pts',(-2.1431885490041,-4.94773503060847,82.7266563328826));
#68200=CARTESIAN_POINT('Ctrl Pts',(2.99430902725335,-4.48413344144938,82.8854170951283));
#68201=CARTESIAN_POINT('Ctrl Pts',(5.39132358998814,0.0834841069729651,
83.0441778573743));
#68202=CARTESIAN_POINT('Ctrl Pts',(2.85403398786483,4.57469432804498,83.20293861962));
#68203=CARTESIAN_POINT('Ctrl Pts',(-2.29535443865746,4.87900479902879,83.3616993818661));
#68204=CARTESIAN_POINT('Ctrl Pts',(-5.34396486625942,0.717900597107141,
83.5204601441119));
#68205=CARTESIAN_POINT('Ctrl Pts',(-3.50161446504842,-4.10024729857536,
83.6792209063577));
#68206=CARTESIAN_POINT('Ctrl Pts',(1.54551863391146,-5.16572527246177,83.8379816686037));
#68207=CARTESIAN_POINT('Ctrl Pts',(5.17814935421542,-1.50337052857669,83.9967424308496));
#68208=CARTESIAN_POINT('Ctrl Pts',(4.07157294499926,3.5349087933154,84.1555031930955));
#68209=CARTESIAN_POINT('Ctrl Pts',(-0.761418612953421,5.33794320112753,
84.3142639553413));
#68210=CARTESIAN_POINT('Ctrl Pts',(-4.89756107214883,2.25550674636269,84.4730247175872));
#68211=CARTESIAN_POINT('Ctrl Pts',(-4.55125916712634,-2.89119586857457,
84.6317854798332));
#68212=CARTESIAN_POINT('Ctrl Pts',(-0.0395956256930076,-5.39186912790212,
84.7905462420789));
#68213=CARTESIAN_POINT('Ctrl Pts',(4.50847898005441,-2.95758313260692,84.949307004325));
#68214=CARTESIAN_POINT('Ctrl Pts',(4.92992660394334,2.18327463521188,85.1080677665708));
#68215=CARTESIAN_POINT('Ctrl Pts',(0.83998553543098,5.32650478551015,85.2668285288166));
#68216=CARTESIAN_POINT('Ctrl Pts',(-4.0199441247066,3.59365925042037,85.4255892910627));
#68217=CARTESIAN_POINT('Ctrl Pts',(-5.19838251798258,-1.4261119912042,85.5843500533084));
#68218=CARTESIAN_POINT('Ctrl Pts',(-1.62355247471041,-5.1447064563747,85.7431108155544));
#68219=CARTESIAN_POINT('Ctrl Pts',(3.44586114533526,-4.14677678635576,85.9018715778002));
#68220=CARTESIAN_POINT('Ctrl Pts',(5.02742464258896,-0.1665161442746,86.0341722130051));
#68221=CARTESIAN_POINT('Ctrl Pts',(3.86721841197903,2.75399303531867,86.1400127211691));
#68222=CARTESIAN_POINT('Ctrl Pts',(2.68386473467973,3.76615995447699,86.192932975251));
#68223=CARTESIAN_POINT('Ctrl Pts',(2.00237954638958,4.09906332620035,86.219393102292));
#68224=CARTESIAN_POINT('Ctrl Pts',(2.53835875722654,-3.55965150255068,26.));
#68225=CARTESIAN_POINT('Ctrl Pts',(3.13016463613492,-3.13763950664917,26.026460127041));
#68226=CARTESIAN_POINT('Ctrl Pts',(4.08944058768451,-1.99447514282845,26.079380381123));
#68227=CARTESIAN_POINT('Ctrl Pts',(4.72633908941221,0.949051473338421,26.1852208892869));
#68228=CARTESIAN_POINT('Ctrl Pts',(2.60449620246589,4.46265906441401,26.3175215244918));
#68229=CARTESIAN_POINT('Ctrl Pts',(-2.34489469821123,4.60777770546463,26.4762822867377));
#68230=CARTESIAN_POINT('Ctrl Pts',(-5.13873203824598,0.529582897206408,
26.6350430489835));
#68231=CARTESIAN_POINT('Ctrl Pts',(-3.23428844614615,-4.03017972072915,
26.7938038112295));
#68232=CARTESIAN_POINT('Ctrl Pts',(1.63279456941769,-4.90302026906412,26.9525645734753));
#68233=CARTESIAN_POINT('Ctrl Pts',(5.00417945325775,-1.28762125191842,27.1113253357213));
#68234=CARTESIAN_POINT('Ctrl Pts',(3.79627275763131,3.50580663842047,27.2700860979671));
#68235=CARTESIAN_POINT('Ctrl Pts',(-0.886457053099411,5.09084367591115,
27.428846860213));
#68236=CARTESIAN_POINT('Ctrl Pts',(-4.75768720014009,2.01646474678857,27.5876076224589));
#68237=CARTESIAN_POINT('Ctrl Pts',(-4.27463438144488,-2.90338148363688,
27.7463683847048));
#68238=CARTESIAN_POINT('Ctrl Pts',(0.12074539761077,-5.16599709979471,27.9051291469506));
#68239=CARTESIAN_POINT('Ctrl Pts',(4.40558866999103,-2.70051724468854,28.0638899091966));
#68240=CARTESIAN_POINT('Ctrl Pts',(4.65831652566081,2.23654953809766,28.2226506714425));
#68241=CARTESIAN_POINT('Ctrl Pts',(0.647603546994949,5.12666253671564,28.3814114336883));
#68242=CARTESIAN_POINT('Ctrl Pts',(-3.95581218859218,3.32469494777108,28.5401721959342));
#68243=CARTESIAN_POINT('Ctrl Pts',(-4.93874975649391,-1.52013373855127,
28.6989329581801));
#68244=CARTESIAN_POINT('Ctrl Pts',(-1.40159165779937,-4.9736902589037,28.857693720426));
#68245=CARTESIAN_POINT('Ctrl Pts',(3.41834539873403,-3.87517318393326,29.0164544826719));
#68246=CARTESIAN_POINT('Ctrl Pts',(5.10970861334159,0.770020576487015,29.1752152449178));
#68247=CARTESIAN_POINT('Ctrl Pts',(2.12451027984608,4.71046807932676,29.3339760071637));
#68248=CARTESIAN_POINT('Ctrl Pts',(-2.80510467897592,4.33975126344986,29.4927367694096));
#68249=CARTESIAN_POINT('Ctrl Pts',(-5.16740219266045,-0.00283844237382118,
29.6514975316555));
#68250=CARTESIAN_POINT('Ctrl Pts',(-2.80033535833003,-4.34283033250174,
29.8102582939013));
#68251=CARTESIAN_POINT('Ctrl Pts',(2.12968392236957,-4.70813124181331,29.9690190561473));
#68252=CARTESIAN_POINT('Ctrl Pts',(5.11055143098187,-0.764406630547101,
30.1277798183931));
#68253=CARTESIAN_POINT('Ctrl Pts',(3.41408616315334,3.87892628001712,30.286540580639));
#68254=CARTESIAN_POINT('Ctrl Pts',(-1.4070550442568,4.97214737476293,30.4453013428849));
#68255=CARTESIAN_POINT('Ctrl Pts',(-4.94041649691963,1.51470731642915,30.6040621051308));
#68256=CARTESIAN_POINT('Ctrl Pts',(-3.95215786419059,-3.32903914551084,
30.7628228673767));
#68257=CARTESIAN_POINT('Ctrl Pts',(0.653236365857992,-5.12594729451212,
30.9215836296226));
#68258=CARTESIAN_POINT('Ctrl Pts',(4.6607687206244,-2.23143190555148,31.0803443918685));
#68259=CARTESIAN_POINT('Ctrl Pts',(4.4026231771807,2.70535812338375,31.2391051541143));
#68260=CARTESIAN_POINT('Ctrl Pts',(0.115062422136807,5.16612176153803,31.3978659163603));
#68261=CARTESIAN_POINT('Ctrl Pts',(-4.27780697629061,2.89869296229943,31.5566266786061));
#68262=CARTESIAN_POINT('Ctrl Pts',(-4.7554967626928,-2.02170817777057,31.715387440852));
#68263=CARTESIAN_POINT('Ctrl Pts',(-0.880810653343035,-5.09178023966167,
31.8741482030979));
#68264=CARTESIAN_POINT('Ctrl Pts',(3.80002027066033,-3.5016994957634,32.0329089653438));
#68265=CARTESIAN_POINT('Ctrl Pts',(5.00295656982363,1.29324358746212,32.1916697275897));
#68266=CARTESIAN_POINT('Ctrl Pts',(1.62703419898677,4.90457063680218,32.3504304898356));
#68267=CARTESIAN_POINT('Ctrl Pts',(-3.23799956916984,4.02708482728032,32.5091912520815));
#68268=CARTESIAN_POINT('Ctrl Pts',(-5.13951722563736,-0.536112025076297,
32.6679520143274));
#68269=CARTESIAN_POINT('Ctrl Pts',(-2.33719172860392,-4.60864277632799,
32.8267127765732));
#68270=CARTESIAN_POINT('Ctrl Pts',(2.60420302889879,-4.4632028858578,32.9854735388192));
#68271=CARTESIAN_POINT('Ctrl Pts',(5.16215162793603,-0.232903383943239,
33.144234301065));
#68272=CARTESIAN_POINT('Ctrl Pts',(2.99554137711165,4.21055640908263,33.302995063311));
#68273=CARTESIAN_POINT('Ctrl Pts',(-1.91267984204806,4.80038636339596,33.4617558255568));
#68274=CARTESIAN_POINT('Ctrl Pts',(-5.07035804619892,0.996756088218607,
33.6205165878027));
#68275=CARTESIAN_POINT('Ctrl Pts',(-3.58748969036538,-3.71913580520757,
33.7792773500486));
#68276=CARTESIAN_POINT('Ctrl Pts',(1.17875881138994,-5.0311610072254,33.9380381122944));
#68277=CARTESIAN_POINT('Ctrl Pts',(4.86617124330449,-1.73851397661661,34.0967988745404));
#68278=CARTESIAN_POINT('Ctrl Pts',(4.09991511421076,3.14527414899259,34.2555596367862));
#68279=CARTESIAN_POINT('Ctrl Pts',(-0.418708560946466,5.15041129979394,
34.4143203990322));
#68280=CARTESIAN_POINT('Ctrl Pts',(-4.55411737150595,2.44173470766227,34.5730811612781));
#68281=CARTESIAN_POINT('Ctrl Pts',(-4.5214588563368,-2.50169207267966,34.7318419235239));
#68282=CARTESIAN_POINT('Ctrl Pts',(-0.350623086089188,-5.15549385292585,
34.8906026857698));
#68283=CARTESIAN_POINT('Ctrl Pts',(4.14111364246891,-3.09083018236409,35.0493634480157));
#68284=CARTESIAN_POINT('Ctrl Pts',(4.84277667347619,1.80265568173448,35.2081242102616));
#68285=CARTESIAN_POINT('Ctrl Pts',(1.11218256837853,5.0462960030749,35.3668849725075));
#68286=CARTESIAN_POINT('Ctrl Pts',(-3.63631499535807,3.67141208128276,35.5256457347534));
#68287=CARTESIAN_POINT('Ctrl Pts',(-5.05674600265519,-1.06366032204162,
35.6844064969993));
#68288=CARTESIAN_POINT('Ctrl Pts',(-1.84908860800444,-4.8252383087059,35.8431672592452));
#68289=CARTESIAN_POINT('Ctrl Pts',(3.05091116183891,-4.17061080641931,36.0019280214911));
#68290=CARTESIAN_POINT('Ctrl Pts',(5.15862384507246,0.301087098868051,36.1606887837369));
#68291=CARTESIAN_POINT('Ctrl Pts',(2.54500641307862,4.49722089444621,36.3194495459828));
#68292=CARTESIAN_POINT('Ctrl Pts',(-2.39787862639785,4.5773607580263,36.4782103082287));
#68293=CARTESIAN_POINT('Ctrl Pts',(-5.14615190283867,0.468160238555881,
36.6369710704746));
#68294=CARTESIAN_POINT('Ctrl Pts',(-3.18450976654496,-4.06951483138158,
36.7957318327205));
#68295=CARTESIAN_POINT('Ctrl Pts',(1.69169298020808,-4.88264562268956,36.9544925949664));
#68296=CARTESIAN_POINT('Ctrl Pts',(5.01960663803976,-1.22702999775959,37.1132533572123));
#68297=CARTESIAN_POINT('Ctrl Pts',(3.75342297485632,3.55160096123927,37.2720141194582));
#68298=CARTESIAN_POINT('Ctrl Pts',(-0.94800804471325,5.07969823544803,37.430774881704));
#68299=CARTESIAN_POINT('Ctrl Pts',(-4.78179314447847,1.95870052317183,37.58953564395));
#68300=CARTESIAN_POINT('Ctrl Pts',(-4.23913509664356,-2.95495973719773,
37.7482964061958));
#68301=CARTESIAN_POINT('Ctrl Pts',(0.183308877707052,-5.16415058566349,
37.9070571684418));
#68302=CARTESIAN_POINT('Ctrl Pts',(4.43798296793759,-2.64695307709652,38.0658179306876));
#68303=CARTESIAN_POINT('Ctrl Pts',(4.63087948595682,2.29281673986369,38.2245786929335));
#68304=CARTESIAN_POINT('Ctrl Pts',(0.585453646372677,5.13413064150142,38.3833394551794));
#68305=CARTESIAN_POINT('Ctrl Pts',(-3.99579725328622,3.27653135597467,38.5421002174253));
#68306=CARTESIAN_POINT('Ctrl Pts',(-4.91997245352125,-1.57984950949354,
38.7008609796712));
#68307=CARTESIAN_POINT('Ctrl Pts',(-1.34123858177823,-4.99030384674165,
38.8596217419171));
#68308=CARTESIAN_POINT('Ctrl Pts',(3.46503780867414,-3.83347967263602,39.0183825041629));
#68309=CARTESIAN_POINT('Ctrl Pts',(5.10000575566994,0.831862193027325,39.1771432664089));
#68310=CARTESIAN_POINT('Ctrl Pts',(2.06729265337245,4.73585837007054,39.3359040286547));
#68311=CARTESIAN_POINT('Ctrl Pts',(-2.85746983156782,4.30545230814772,39.4946647909006));
#68312=CARTESIAN_POINT('Ctrl Pts',(-5.16698864410473,-0.0654352179449955,
39.6534255531465));
#68313=CARTESIAN_POINT('Ctrl Pts',(-2.74752162183386,-4.3764344338297,39.8121863153924));
#68314=CARTESIAN_POINT('Ctrl Pts',(2.18656111288008,-4.68198717594309,39.9709470776383));
#68315=CARTESIAN_POINT('Ctrl Pts',(5.11943632770732,-0.702442241472902,
40.1297078398842));
#68316=CARTESIAN_POINT('Ctrl Pts',(3.36684704019806,3.9199992887709,40.2884686021301));
#68317=CARTESIAN_POINT('Ctrl Pts',(-1.46718350018236,4.95473773199425,40.4472293643759));
#68318=CARTESIAN_POINT('Ctrl Pts',(-4.95840288549236,1.45474885846183,40.6059901266218));
#68319=CARTESIAN_POINT('Ctrl Pts',(-3.91154049361154,-3.37667060621731,
40.7647508888677));
#68320=CARTESIAN_POINT('Ctrl Pts',(0.715283237582617,-5.11765799033974,
40.9235116511136));
#68321=CARTESIAN_POINT('Ctrl Pts',(4.6874579011302,-2.17480846080452,41.0822724133595));
#68322=CARTESIAN_POINT('Ctrl Pts',(4.36952791329752,2.75849220244841,41.2410331756054));
#68323=CARTESIAN_POINT('Ctrl Pts',(0.052472510246957,5.16713654277911,41.3997939378513));
#68324=CARTESIAN_POINT('Ctrl Pts',(-4.3126073369753,2.84665968691757,41.5585547000972));
#68325=CARTESIAN_POINT('Ctrl Pts',(-4.73065721909144,-2.07916706676323,
41.7173154623431));
#68326=CARTESIAN_POINT('Ctrl Pts',(-0.819065114488867,-5.10207661195736,
41.8760762245889));
#68327=CARTESIAN_POINT('Ctrl Pts',(3.8421604015636,-3.45540979692878,42.0348369868349));
#68328=CARTESIAN_POINT('Ctrl Pts',(4.98692335778749,1.35375361111553,42.1935977490807));
#68329=CARTESIAN_POINT('Ctrl Pts',(1.56750172940691,4.92392036332446,42.3523585113267));
#68330=CARTESIAN_POINT('Ctrl Pts',(-3.28654536169065,3.98756479591298,42.5111192735724));
#68331=CARTESIAN_POINT('Ctrl Pts',(-5.13264574893371,-0.59833187447071,
42.6698800358185));
#68332=CARTESIAN_POINT('Ctrl Pts',(-2.28119196804685,-4.63661693705371,
42.8286407980642));
#68333=CARTESIAN_POINT('Ctrl Pts',(2.65807838191241,-4.43132855153674,42.9874015603103));
#68334=CARTESIAN_POINT('Ctrl Pts',(5.1645942046841,-0.170352918960309,43.146162322556));
#68335=CARTESIAN_POINT('Ctrl Pts',(2.94431565674484,4.24653490854626,43.304923084802));
#68336=CARTESIAN_POINT('Ctrl Pts',(-1.97069051554003,4.77686427565358,43.4636838470478));
#68337=CARTESIAN_POINT('Ctrl Pts',(-5.0820605324771,0.935261546463589,43.6224446092938));
#68338=CARTESIAN_POINT('Ctrl Pts',(-3.54217351653091,-3.76232111798581,
43.7812053715396));
#68339=CARTESIAN_POINT('Ctrl Pts',(1.23961889884326,-5.01651257365967,43.9399661337855));
#68340=CARTESIAN_POINT('Ctrl Pts',(4.88687423334376,-1.67943849054845,44.0987268960314));
#68341=CARTESIAN_POINT('Ctrl Pts',(4.06151299797099,3.19470899822934,44.2574876582773));
#68342=CARTESIAN_POINT('Ctrl Pts',(-0.481068993674721,5.1449612281707,44.4162484205232));
#68343=CARTESIAN_POINT('Ctrl Pts',(-4.5833619478656,2.38638778720321,44.5750091827691));
#68344=CARTESIAN_POINT('Ctrl Pts',(-4.49082204675623,-2.55628064977671,
44.733769945015));
#68345=CARTESIAN_POINT('Ctrl Pts',(-0.288144634510089,-5.15936295347187,
44.8925307072609));
#68346=CARTESIAN_POINT('Ctrl Pts',(4.17825154873217,-3.04043868735616,45.0512914695067));
#68347=CARTESIAN_POINT('Ctrl Pts',(4.8205842882194,1.86118793683688,45.2100522317526));
#68348=CARTESIAN_POINT('Ctrl Pts',(1.05097104046387,5.05939851051103,45.3688129939986));
#68349=CARTESIAN_POINT('Ctrl Pts',(-3.68052300585259,3.62709302602572,45.5275737562444));
#68350=CARTESIAN_POINT('Ctrl Pts',(-5.04348997417376,-1.12483878687734,
45.6863345184903));
#68351=CARTESIAN_POINT('Ctrl Pts',(-1.79050086272392,-4.84728378338218,
45.8450952807362));
#68352=CARTESIAN_POINT('Ctrl Pts',(3.1012093298518,-4.13334659912459,46.0038560429821));
#68353=CARTESIAN_POINT('Ctrl Pts',(5.15459801607478,0.363555647367575,46.162616805228));
#68354=CARTESIAN_POINT('Ctrl Pts',(2.49034114873962,4.52772066043712,46.3213775674739));
#68355=CARTESIAN_POINT('Ctrl Pts',(-2.45315200638293,4.54797742404625,46.4801383297198));
#68356=CARTESIAN_POINT('Ctrl Pts',(-5.15144551276008,0.405786329388982,
46.6388990919657));
#68357=CARTESIAN_POINT('Ctrl Pts',(-3.13497873290715,-4.10779280882992,
46.7976598542116));
#68358=CARTESIAN_POINT('Ctrl Pts',(1.75071634247466,-4.86179449424254,46.9564206164574));
#68359=CARTESIAN_POINT('Ctrl Pts',(5.03410234489664,-1.16613335307792,47.1151813787034));
#68360=CARTESIAN_POINT('Ctrl Pts',(3.71012411261097,3.59680865283067,47.2739421409492));
#68361=CARTESIAN_POINT('Ctrl Pts',(-1.00947303475291,5.06784151371782,47.4327029031951));
#68362=CARTESIAN_POINT('Ctrl Pts',(-4.80516962595556,1.90063102201579,47.5914636654409));
#68363=CARTESIAN_POINT('Ctrl Pts',(-4.20302819966638,-3.00609503656556,
47.750224427687));
#68364=CARTESIAN_POINT('Ctrl Pts',(0.245853018125491,-5.16155109531365,
47.9089851899327));
#68365=CARTESIAN_POINT('Ctrl Pts',(4.46972204405066,-2.59299792999961,48.0677459521787));
#68366=CARTESIAN_POINT('Ctrl Pts',(4.60276492582317,2.34874614500311,48.2265067144246));
#68367=CARTESIAN_POINT('Ctrl Pts',(0.523216754197009,5.14084600471386,48.3852674766704));
#68368=CARTESIAN_POINT('Ctrl Pts',(-4.03519537273411,3.22788657172462,48.5440282389163));
#68369=CARTESIAN_POINT('Ctrl Pts',(-4.9004734378914,-1.63933324878614,48.7027890011622));
#68370=CARTESIAN_POINT('Ctrl Pts',(-1.2806885257803,-5.00618520592171,48.8615497634081));
#68371=CARTESIAN_POINT('Ctrl Pts',(3.51122164426531,-3.79122354667958,49.020310525654));
#68372=CARTESIAN_POINT('Ctrl Pts',(5.0895545138177,0.893581706914796,49.1790712878999));
#68373=CARTESIAN_POINT('Ctrl Pts',(2.00977162985725,4.76055368753214,49.3378320501457));
#68374=CARTESIAN_POINT('Ctrl Pts',(-2.90941563902232,4.27052152031426,49.4965928123917));
#68375=CARTESIAN_POINT('Ctrl Pts',(-5.1658168458108,-0.128022387073527,
49.6553535746375));
#68376=CARTESIAN_POINT('Ctrl Pts',(-2.69430468338317,-4.40939629531691,
49.8141143368835));
#68377=CARTESIAN_POINT('Ctrl Pts',(2.2431174238849,-4.6551560273227,49.9728750991294));
#68378=CARTESIAN_POINT('Ctrl Pts',(5.12756994789964,-0.640374769530455,
50.1316358613752));
#68379=CARTESIAN_POINT('Ctrl Pts',(3.31911383193326,3.96049703783808,50.2903966236212));
#68380=CARTESIAN_POINT('Ctrl Pts',(-1.52709664667054,4.93660098122003,50.4491573858669));
#68381=CARTESIAN_POINT('Ctrl Pts',(-4.975661628467,1.39457691614903,50.607918148113));
#68382=CARTESIAN_POINT('Ctrl Pts',(-3.87034910432713,-3.42380654048809,
50.7666789103588));
#68383=CARTESIAN_POINT('Ctrl Pts',(0.777225141445664,-5.10861766973804,
50.9254396726047));
#68384=CARTESIAN_POINT('Ctrl Pts',(4.71345919711634,-2.11786586288516,51.0842004348506));
#68385=CARTESIAN_POINT('Ctrl Pts',(4.33579142110028,2.81122147273531,51.2429611970965));
#68386=CARTESIAN_POINT('Ctrl Pts',(-0.0101251019801382,5.16739304663044,
51.4017219593423));
#68387=CARTESIAN_POINT('Ctrl Pts',(-4.34677482245307,2.79420866417363,51.5604827215882));
#68388=CARTESIAN_POINT('Ctrl Pts',(-4.7051234514512,-2.13632083794987,51.7192434838341));
#68389=CARTESIAN_POINT('Ctrl Pts',(-0.757199377814005,-5.111624254412,51.87800424608));
#68390=CARTESIAN_POINT('Ctrl Pts',(3.88373669535471,-3.40861301664037,52.0367650083259));
#68391=CARTESIAN_POINT('Ctrl Pts',(4.97015831465276,1.41406497140078,52.1955257705718));
#68392=CARTESIAN_POINT('Ctrl Pts',(1.50773922891819,4.94254750443899,52.3542865328176));
#68393=CARTESIAN_POINT('Ctrl Pts',(-3.33460885361675,3.94745958933536,52.5130472950636));
#68394=CARTESIAN_POINT('Ctrl Pts',(-5.12502105636793,-0.660463918651125,
52.6718080573094));
#68395=CARTESIAN_POINT('Ctrl Pts',(-2.22485744252472,-4.66391067415503,
52.8305688195554));
#68396=CARTESIAN_POINT('Ctrl Pts',(2.71156366187259,-4.39880391966578,52.9893295818012));
#68397=CARTESIAN_POINT('Ctrl Pts',(5.16627887713359,-0.107777454683187,
53.1480903440472));
#68398=CARTESIAN_POINT('Ctrl Pts',(2.89265785799892,4.28189022893068,53.306851106293));
#68399=CARTESIAN_POINT('Ctrl Pts',(-2.02841199016113,4.75264118298715,53.4656118685389));
#68400=CARTESIAN_POINT('Ctrl Pts',(-5.09301722627474,0.873629755058583,
53.6243726307848));
#68401=CARTESIAN_POINT('Ctrl Pts',(-3.49633752866489,-3.80495431006791,
53.7831333930307));
#68402=CARTESIAN_POINT('Ctrl Pts',(1.30029707219943,-5.00112796677752,53.9418941552766));
#68403=CARTESIAN_POINT('Ctrl Pts',(4.90686007449561,-1.62011654684958,54.1006549175225));
#68404=CARTESIAN_POINT('Ctrl Pts',(4.02251485462088,3.2436750238594,54.2594156797684));
#68405=CARTESIAN_POINT('Ctrl Pts',(-0.543358829519001,5.13875613338857,
54.4181764420142));
#68406=CARTESIAN_POINT('Ctrl Pts',(-4.61193391577151,2.33069066429059,54.5769372042602));
#68407=CARTESIAN_POINT('Ctrl Pts',(-4.4595262089542,-2.61049409263942,54.735697966506));
#68408=CARTESIAN_POINT('Ctrl Pts',(-0.22562389770033,-5.16247491740555,
54.8944587287519));
#68409=CARTESIAN_POINT('Ctrl Pts',(4.21477629650059,-2.98960100791253,55.0532194909978));
#68410=CARTESIAN_POINT('Ctrl Pts',(4.79768448212587,1.91944706257383,55.2119802532437));
#68411=CARTESIAN_POINT('Ctrl Pts',(0.989605282528937,5.07175855111871,55.3707410154895));
#68412=CARTESIAN_POINT('Ctrl Pts',(-3.72419089952545,3.58224169479765,55.5295017777355));
#68413=CARTESIAN_POINT('Ctrl Pts',(-5.0294938134419,-1.1858521815995,55.6882625399813));
#68414=CARTESIAN_POINT('Ctrl Pts',(-1.7316503614075,-4.86861791907028,55.8470233022273));
#68415=CARTESIAN_POINT('Ctrl Pts',(3.15105239533607,-4.09547582313724,56.0057840644731));
#68416=CARTESIAN_POINT('Ctrl Pts',(5.14981574971942,0.425970844068908,56.1645448267191));
#68417=CARTESIAN_POINT('Ctrl Pts',(2.43531042678924,4.55755598333432,56.3233055889649));
#68418=CARTESIAN_POINT('Ctrl Pts',(-2.50806538626398,4.517926674292,56.4820663512109));
#68419=CARTESIAN_POINT('Ctrl Pts',(-5.1559831479537,0.343352871070528,56.6408271134567));
#68420=CARTESIAN_POINT('Ctrl Pts',(-3.08498764108028,-4.14546796760472,
56.7995878757026));
#68421=CARTESIAN_POINT('Ctrl Pts',(1.8094827870843,-4.8402298973603,56.9583486379485));
#68422=CARTESIAN_POINT('Ctrl Pts',(5.04785929713791,-1.10506557830443,57.1171094001944));
#68423=CARTESIAN_POINT('Ctrl Pts',(3.66628078958101,3.64148851268323,57.2758701624403));
#68424=CARTESIAN_POINT('Ctrl Pts',(-1.07078988460527,5.05524108614831,57.4346309246862));
#68425=CARTESIAN_POINT('Ctrl Pts',(-4.82784094869794,1.84228260322088,57.593391686932));
#68426=CARTESIAN_POINT('Ctrl Pts',(-4.16630450822031,-3.05678919142909,
57.7521524491779));
#68427=CARTESIAN_POINT('Ctrl Pts',(0.308361079608735,-5.1581941472416,57.9109132114238));
#68428=CARTESIAN_POINT('Ctrl Pts',(4.50080518836808,-2.53866226040682,58.0696739736697));
#68429=CARTESIAN_POINT('Ctrl Pts',(4.57397490984839,2.40433087160068,58.2284347359156));
#68430=CARTESIAN_POINT('Ctrl Pts',(0.460903079952699,5.14680694867653,58.3871954981615));
#68431=CARTESIAN_POINT('Ctrl Pts',(-4.07400132718361,3.17876809505837,58.5459562604074));
#68432=CARTESIAN_POINT('Ctrl Pts',(-4.88025527769062,-1.69857641589297,
58.7047170226532));
#68433=CARTESIAN_POINT('Ctrl Pts',(-1.21995052871669,-5.02133190732686,
58.8634777848992));
#68434=CARTESIAN_POINT('Ctrl Pts',(3.55689020801282,-3.74841105859499,59.022238547145));
#68435=CARTESIAN_POINT('Ctrl Pts',(5.07835637974298,0.955170087669591,59.1809993093909));
#68436=CARTESIAN_POINT('Ctrl Pts',(1.95195567231696,4.78455039364876,59.3397600716368));
#68437=CARTESIAN_POINT('Ctrl Pts',(-2.96093448967591,4.23496403336588,59.4985208338827));
#68438=CARTESIAN_POINT('Ctrl Pts',(-5.16388696379574,-0.190590768914221,
59.6572815961286));
#68439=CARTESIAN_POINT('Ctrl Pts',(-2.6406923556686,-4.44171107781315,59.8160423583745));
#68440=CARTESIAN_POINT('Ctrl Pts',(2.29934455736468,-4.62764173446609,59.9748031206204));
#68441=CARTESIAN_POINT('Ctrl Pts',(5.13495109710383,-0.578213322578349,
60.1335638828663));
#68442=CARTESIAN_POINT('Ctrl Pts',(3.27089354364999,4.00041358388897,60.2923246451122));
#68443=CARTESIAN_POINT('Ctrl Pts',(-1.58678569169648,4.91773978415717,60.451085407358));
#68444=CARTESIAN_POINT('Ctrl Pts',(-4.99219019300232,1.33420031964711,60.6098461696039));
#68445=CARTESIAN_POINT('Ctrl Pts',(-3.82858974123746,-3.47044003108337,
60.7686069318499));
#68446=CARTESIAN_POINT('Ctrl Pts',(0.839052987504236,-5.09882765939536,
60.9273676940957));
#68447=CARTESIAN_POINT('Ctrl Pts',(4.73876879287487,-2.06061246810993,61.0861284563416));
#68448=CARTESIAN_POINT('Ctrl Pts',(4.30141865142892,2.86353819621711,61.2448892185875));
#68449=CARTESIAN_POINT('Ctrl Pts',(-0.0727212283482856,5.16689123545314,
61.4036499808334));
#68450=CARTESIAN_POINT('Ctrl Pts',(-4.38030441864225,2.74134759125467,61.5624107430792));
#68451=CARTESIAN_POINT('Ctrl Pts',(-4.67889920685427,-2.19316110401252,
61.7211715053253));
#68452=CARTESIAN_POINT('Ctrl Pts',(-0.695222522116061,-5.12042176590928,
61.879932267571));
#68453=CARTESIAN_POINT('Ctrl Pts',(3.92474305071123,-3.3613160223265,62.038693029817));
#68454=CARTESIAN_POINT('Ctrl Pts',(4.95266390069012,1.47416881762428,62.1974537920629));
#68455=CARTESIAN_POINT('Ctrl Pts',(1.4477554676688,4.96044932661243,62.3562145543087));
#68456=CARTESIAN_POINT('Ctrl Pts',(-3.38218299162958,3.90677509298738,62.5149753165547));
#68457=CARTESIAN_POINT('Ctrl Pts',(-5.11664426686392,-0.722499039738782,
62.6737360788005));
#68458=CARTESIAN_POINT('Ctrl Pts',(-2.16819641913028,-4.69051998227545,
62.8324968410464));
#68459=CARTESIAN_POINT('Ctrl Pts',(2.76465101981334,-4.3656337632353,62.9912576032923));
#68460=CARTESIAN_POINT('Ctrl Pts',(5.16720539805885,-0.0451861740625634,
63.1500183655382));
#68461=CARTESIAN_POINT('Ctrl Pts',(2.8405755616569,4.31661718184185,63.308779127784));
#68462=CARTESIAN_POINT('Ctrl Pts',(-2.08583579528372,4.72772064013601,63.46753989003));
#68463=CARTESIAN_POINT('Ctrl Pts',(-5.10322651969674,0.811869758470405,
63.6263006522758));
#68464=CARTESIAN_POINT('Ctrl Pts',(-3.44998845319957,-3.847029125032,63.7850614145218));
#68465=CARTESIAN_POINT('Ctrl Pts',(1.36078442693529,-4.98500944427043,63.9438221767676));
#68466=CARTESIAN_POINT('Ctrl Pts',(4.92612583383742,-1.56055685101642,64.1025829390136));
#68467=CARTESIAN_POINT('Ctrl Pts',(3.98292640713875,3.29216504011747,64.2613437012594));
#68468=CARTESIAN_POINT('Ctrl Pts',(-0.605568927444514,5.13179692604536,
64.4201044635054));
#68469=CARTESIAN_POINT('Ctrl Pts',(-4.63982908228685,2.27465151247837,64.5788652257511));
#68470=CARTESIAN_POINT('Ctrl Pts',(-4.42757593559553,-2.66432444544396,
64.7376259879972));
#68471=CARTESIAN_POINT('Ctrl Pts',(-0.163070050579303,-5.16482928804609,
64.8963867502428));
#68472=CARTESIAN_POINT('Ctrl Pts',(4.25068252576661,-2.93832460446375,65.0551475124889));
#68473=CARTESIAN_POINT('Ctrl Pts',(4.77408061574266,1.97742450941745,65.2139082747347));
#68474=CARTESIAN_POINT('Ctrl Pts',(0.928094299999949,5.08337431106172,65.3726690369806));
#68475=CARTESIAN_POINT('Ctrl Pts',(-3.76731226811231,3.53686466953228,65.5314297992265));
#68476=CARTESIAN_POINT('Ctrl Pts',(-5.01475957439658,-1.24669155249126,
65.6901905614724));
#68477=CARTESIAN_POINT('Ctrl Pts',(-1.67254574036732,-4.88923758498539,
65.8489513237183));
#68478=CARTESIAN_POINT('Ctrl Pts',(3.20043304382085,-4.05700403599433,66.0077120859643));
#68479=CARTESIAN_POINT('Ctrl Pts',(5.14427774780404,0.488323529540513,66.16647284821));
#68480=CARTESIAN_POINT('Ctrl Pts',(2.3799223229872,4.58672248480354,66.3252336104561));
#68481=CARTESIAN_POINT('Ctrl Pts',(-2.56261070750152,4.48721291871176,66.4839943727018));
#68482=CARTESIAN_POINT('Ctrl Pts',(-5.15976414252148,0.280869025711643,
66.6427551349478));
#68483=CARTESIAN_POINT('Ctrl Pts',(-3.03454382725794,-4.18253477887576,
66.8015158971936));
#68484=CARTESIAN_POINT('Ctrl Pts',(1.86798369006022,-4.81795499664787,66.9602766594396));
#68485=CARTESIAN_POINT('Ctrl Pts',(5.06087547593053,-1.04383563513614,67.1190374216854));
#68486=CARTESIAN_POINT('Ctrl Pts',(3.62189943977487,3.68563398402679,67.2777981839313));
#68487=CARTESIAN_POINT('Ctrl Pts',(-1.13194959602156,5.04189880185246,67.4365589461772));
#68488=CARTESIAN_POINT('Ctrl Pts',(-4.84980378568845,1.78366382941869,67.5953197084231));
#68489=CARTESIAN_POINT('Ctrl Pts',(-4.12896941150786,-3.10703476242022,
67.754080470669));
#68490=CARTESIAN_POINT('Ctrl Pts',(0.370823889097725,-5.15408023407956,
67.9128412329148));
#68491=CARTESIAN_POINT('Ctrl Pts',(4.53122783943781,-2.48395404207855,68.0716019951608));
#68492=CARTESIAN_POINT('Ctrl Pts',(4.5445136629679,2.45956276259679,68.2303627574067));
#68493=CARTESIAN_POINT('Ctrl Pts',(0.398521768172548,5.15201259862078,68.3891235196525));
#68494=CARTESIAN_POINT('Ctrl Pts',(-4.11220942186021,3.12918313411324,68.5478842818985));
#68495=CARTESIAN_POINT('Ctrl Pts',(-4.85932093993431,-1.75757031687816,
68.7066450441443));
#68496=CARTESIAN_POINT('Ctrl Pts',(-1.15903350388962,-5.03574172817834,
68.8654058063903));
#68497=CARTESIAN_POINT('Ctrl Pts',(3.60203679805415,-3.70504849111566,69.0241665686361));
#68498=CARTESIAN_POINT('Ctrl Pts',(5.06641299677213,1.01661829719571,69.182927330882));
#68499=CARTESIAN_POINT('Ctrl Pts',(1.89385326524434,4.80784496690336,69.3416880931279));
#68500=CARTESIAN_POINT('Ctrl Pts',(-3.01201882313635,4.19878506536444,69.5004488553738));
#68501=CARTESIAN_POINT('Ctrl Pts',(-5.16119928126974,-0.25313118155592,
69.6592096176196));
#68502=CARTESIAN_POINT('Ctrl Pts',(-2.58669250630018,-4.47337403912361,
69.8179703798655));
#68503=CARTESIAN_POINT('Ctrl Pts',(2.35523426198658,-4.5994483350962,69.9767311421114));
#68504=CARTESIAN_POINT('Ctrl Pts',(5.14157869213602,-0.51596702281012,70.1354919043573));
#68505=CARTESIAN_POINT('Ctrl Pts',(3.22219325167658,4.03974306916968,70.2942526666032));
#68506=CARTESIAN_POINT('Ctrl Pts',(-1.6462418758917,4.89815690868675,70.4530134288491));
#68507=CARTESIAN_POINT('Ctrl Pts',(-5.00798615353109,1.2736279292227,70.611774191095));
#68508=CARTESIAN_POINT('Ctrl Pts',(-3.78626853252985,-3.51656423453759,
70.7705349533408));
#68509=CARTESIAN_POINT('Ctrl Pts',(0.900757702520816,-5.08828939599587,
70.9292957155868));
#68510=CARTESIAN_POINT('Ctrl Pts',(4.76338297422217,-2.00305667841551,71.0880564778326));
#68511=CARTESIAN_POINT('Ctrl Pts',(4.26641464848803,2.9154346954137,71.2468172400786));
#68512=CARTESIAN_POINT('Ctrl Pts',(-0.135306682874774,5.16563118288797,
71.4055780023244));
#68513=CARTESIAN_POINT('Ctrl Pts',(-4.41319120507407,2.6880842255241,71.5643387645703));
#68514=CARTESIAN_POINT('Ctrl Pts',(-4.65198833370899,-2.24967952364111,
71.7230995268162));
#68515=CARTESIAN_POINT('Ctrl Pts',(-0.63314364249968,-5.12846785541421,
71.8818602890621));
#68516=CARTESIAN_POINT('Ctrl Pts',(3.9651734499498,-3.31352575482195,72.040621051308));
#68517=CARTESIAN_POINT('Ctrl Pts',(4.93444268320512,1.53405632954553,72.1993818135539));
#68518=CARTESIAN_POINT('Ctrl Pts',(1.38755924827672,4.97762320275213,72.3581425757998));
#68519=CARTESIAN_POINT('Ctrl Pts',(-3.42926079422353,3.86551727731956,72.5169033380456));
#68520=CARTESIAN_POINT('Ctrl Pts',(-5.10751660971561,-0.784428134078424,
72.6756641002916));
#68521=CARTESIAN_POINT('Ctrl Pts',(-2.1112172128698,-4.71644095649861,72.8344248625374));
#68522=CARTESIAN_POINT('Ctrl Pts',(2.81733266516402,-4.33182294996633,72.9931856247833));
#68523=CARTESIAN_POINT('Ctrl Pts',(5.16737363149282,0.0174117376300544,
73.1519463870293));
#68524=CARTESIAN_POINT('Ctrl Pts',(2.78807641079671,4.35071067109887,73.3107071492751));
#68525=CARTESIAN_POINT('Ctrl Pts',(-2.14295350396336,4.70210630419026,73.469467911521));
#68526=CARTESIAN_POINT('Ctrl Pts',(-5.11268691452911,0.749990619979619,
73.6282286737669));
#68527=CARTESIAN_POINT('Ctrl Pts',(-3.40313309186266,-3.88853938839824,
73.7869894360128));
#68528=CARTESIAN_POINT('Ctrl Pts',(1.42107208653042,-4.9681593715318,73.9457501982587));
#68529=CARTESIAN_POINT('Ctrl Pts',(4.94466868411869,-1.50076814343543,74.1045109605046));
#68530=CARTESIAN_POINT('Ctrl Pts',(3.94275346512999,3.34017193109278,74.2632717227505));
#68531=CARTESIAN_POINT('Ctrl Pts',(-0.667690158118302,5.12408462740484,
74.4220324849963));
#68532=CARTESIAN_POINT('Ctrl Pts',(-4.6670433537954,2.21827855551313,74.5807932472423));
#68533=CARTESIAN_POINT('Ctrl Pts',(-4.39497591538344,-2.71776380858505,
74.7395540094881));
#68534=CARTESIAN_POINT('Ctrl Pts',(-0.100492272925181,-5.16642571988962,
74.898314771734));
#68535=CARTESIAN_POINT('Ctrl Pts',(4.28596496729055,-2.88661700182285,75.0570755339799));
#68536=CARTESIAN_POINT('Ctrl Pts',(4.74977615293751,2.03511176917654,75.2158362962258));
#68537=CARTESIAN_POINT('Ctrl Pts',(0.866447119614458,5.09424408572719,75.3745970584717));
#68538=CARTESIAN_POINT('Ctrl Pts',(-3.8098807835517,3.4909686093087,75.5333578207175));
#68539=CARTESIAN_POINT('Ctrl Pts',(-4.99928941928749,-1.30734797137385,
75.6921185829635));
#68540=CARTESIAN_POINT('Ctrl Pts',(-1.61319567320764,-4.90913975519121,
75.8508793452094));
#68541=CARTESIAN_POINT('Ctrl Pts',(3.24934402869518,-4.01793688343129,76.0096401074552));
#68542=CARTESIAN_POINT('Ctrl Pts',(5.13798482303055,0.550604553524979,76.1684008697012));
#68543=CARTESIAN_POINT('Ctrl Pts',(2.32418496553848,4.61521588466023,76.3271616319469));
#68544=CARTESIAN_POINT('Ctrl Pts',(-2.61677996556865,4.45584066454958,76.485922394193));
#68545=CARTESIAN_POINT('Ctrl Pts',(-5.16278794160245,0.218343962817818,
76.6446831564387));
#68546=CARTESIAN_POINT('Ctrl Pts',(-2.98365469407069,-4.21898780308791,
76.8034439186847));
#68547=CARTESIAN_POINT('Ctrl Pts',(1.92621046639379,-4.79497306094723,76.9622046809306));
#68548=CARTESIAN_POINT('Ctrl Pts',(5.07314897115,-0.982452509068445,77.1209654431764));
#68549=CARTESIAN_POINT('Ctrl Pts',(3.5769865761566,3.7292385885125,77.2797262054224));
#68550=CARTESIAN_POINT('Ctrl Pts',(-1.19294319381297,5.02781661881079,77.4384869676682));
#68551=CARTESIAN_POINT('Ctrl Pts',(-4.87105491388051,1.72478330291522,77.5972477299142));
#68552=CARTESIAN_POINT('Ctrl Pts',(-4.09102838845504,-3.1568243760003,77.75600849216));
#68553=CARTESIAN_POINT('Ctrl Pts',(0.433232280173729,-5.14920995954434,
77.9147692544059));
#68554=CARTESIAN_POINT('Ctrl Pts',(4.56098553273524,-2.42888130344712,78.0735300166518));
#68555=CARTESIAN_POINT('Ctrl Pts',(4.51438550862023,2.51443371271033,78.2322907788977));
#68556=CARTESIAN_POINT('Ctrl Pts',(0.336081973315249,5.15646219061744,78.3910515411436));
#68557=CARTESIAN_POINT('Ctrl Pts',(-4.1498140497254,3.0791389654831,78.5498123033895));
#68558=CARTESIAN_POINT('Ctrl Pts',(-4.8376734967368,-1.81630629438564,78.7085730656354));
#68559=CARTESIAN_POINT('Ctrl Pts',(-1.0979463908737,-5.04941255383462,78.8673338278812));
#68560=CARTESIAN_POINT('Ctrl Pts',(3.64665478912629,-3.66114220769932,79.0260945901272));
#68561=CARTESIAN_POINT('Ctrl Pts',(5.05372611759689,1.07791731796727,79.184855352373));
#68562=CARTESIAN_POINT('Ctrl Pts',(1.83547293516864,4.83043398881696,79.3436161146189));
#68563=CARTESIAN_POINT('Ctrl Pts',(-3.06266114277673,4.16198992557408,79.5023768768648));
#68564=CARTESIAN_POINT('Ctrl Pts',(-5.15775419265022,-0.315634447191765,
79.6611376391107));
#68565=CARTESIAN_POINT('Ctrl Pts',(-2.53231305975701,-4.50438053270811,
79.8198984013567));
#68566=CARTESIAN_POINT('Ctrl Pts',(2.41077833593552,-4.57057996659486,79.9786591636024));
#68567=CARTESIAN_POINT('Ctrl Pts',(5.14745176039643,-0.453645004871452,
80.1374199258484));
#68568=CARTESIAN_POINT('Ctrl Pts',(3.1730201027819,4.07847972207792,80.2961806880942));
#68569=CARTESIAN_POINT('Ctrl Pts',(-1.70545647406065,4.87785522859546,80.4549414503402));
#68570=CARTESIAN_POINT('Ctrl Pts',(-5.02304719199465,1.21286863387634,80.613702212586));
#68571=CARTESIAN_POINT('Ctrl Pts',(-3.74339168884474,-3.56217238212488,
80.7724629748319));
#68572=CARTESIAN_POINT('Ctrl Pts',(0.962330231331446,-5.07700442602626,
80.9312237370778));
#68573=CARTESIAN_POINT('Ctrl Pts',(4.78729812901886,-1.94520694012218,81.0899844993237));
#68574=CARTESIAN_POINT('Ctrl Pts',(4.2307845491307,2.96690335452649,81.2487452615696));
#68575=CARTESIAN_POINT('Ctrl Pts',(-0.19787228117179,5.16361307382143,81.4075060238155));
#68576=CARTESIAN_POINT('Ctrl Pts',(-4.44543035555655,2.63442638343223,81.5662667860614));
#68577=CARTESIAN_POINT('Ctrl Pts',(-4.62439478129263,-2.30586780285272,
81.7250275483072));
#68578=CARTESIAN_POINT('Ctrl Pts',(-0.57097184883837,-5.13576134197884,
81.8837883105532));
#68579=CARTESIAN_POINT('Ctrl Pts',(4.00502195951943,-3.26524922770216,82.0425490727989));
#68580=CARTESIAN_POINT('Ctrl Pts',(4.91549733690694,1.59371871934676,82.2013098350451));
#68581=CARTESIAN_POINT('Ctrl Pts',(1.32715940311121,4.99406661129702,82.3600705972907));
#68582=CARTESIAN_POINT('Ctrl Pts',(-3.47583534999669,3.82369219939626,82.5188313595369));
#68583=CARTESIAN_POINT('Ctrl Pts',(-5.09763942964231,-0.846242118322492,
82.6775921217824));
#68584=CARTESIAN_POINT('Ctrl Pts',(-2.05392817541576,-4.74166978382725,
82.8363528840287));
#68585=CARTESIAN_POINT('Ctrl Pts',(2.86960084768762,-4.29737645901297,82.9951136462743));
#68586=CARTESIAN_POINT('Ctrl Pts',(5.16678358952832,0.0800071275065655,
83.1538744085204));
#68587=CARTESIAN_POINT('Ctrl Pts',(2.73516803922529,4.38416562959496,83.312635170766));
#68588=CARTESIAN_POINT('Ctrl Pts',(-2.19975659925683,4.67580205641259,83.4713959330121));
#68589=CARTESIAN_POINT('Ctrl Pts',(-5.1213972808606,0.688001186004659,83.6301566952579));
#68590=CARTESIAN_POINT('Ctrl Pts',(-3.35577782577649,-3.92947855970427,
83.7889174575038));
#68591=CARTESIAN_POINT('Ctrl Pts',(1.4811502559097,-4.9505810809301,83.9476782197498));
#68592=CARTESIAN_POINT('Ctrl Pts',(4.96248771955931,-1.44075755171813,84.1064389819956));
#68593=CARTESIAN_POINT('Ctrl Pts',(3.90199844707087,3.38768549854763,84.2651997442416));
#68594=CARTESIAN_POINT('Ctrl Pts',(-0.729706746127024,5.11562640844579,
84.4239605064874));
#68595=CARTESIAN_POINT('Ctrl Pts',(-4.69358549045032,2.16156849958318,84.5827212687333));
#68596=CARTESIAN_POINT('Ctrl Pts',(-4.36170650562841,-2.77078218706868,
84.7414820309791));
#68597=CARTESIAN_POINT('Ctrl Pts',(-0.0379465312430282,-5.16730640666113,
84.9002427932251));
#68598=CARTESIAN_POINT('Ctrl Pts',(4.32070804489202,-2.83440452778566,85.059003555471));
#68599=CARTESIAN_POINT('Ctrl Pts',(4.72460304963626,2.09234474027741,85.2177643177169));
#68600=CARTESIAN_POINT('Ctrl Pts',(0.805001482004623,5.10466438453535,85.3765250799626));
#68601=CARTESIAN_POINT('Ctrl Pts',(-3.85251988452798,3.44398909312549,85.5352858422087));
#68602=CARTESIAN_POINT('Ctrl Pts',(-4.98187820443228,-1.36671670879964,
85.6940466044544));
#68603=CARTESIAN_POINT('Ctrl Pts',(-1.55593411210757,-4.93043766489916,
85.8528073667005));
#68604=CARTESIAN_POINT('Ctrl Pts',(3.302346542614,-3.9740701687742,86.0115681289462));
#68605=CARTESIAN_POINT('Ctrl Pts',(4.81804045098618,-0.159581013320771,
86.1438687641512));
#68606=CARTESIAN_POINT('Ctrl Pts',(3.70615495334781,2.63929363226931,86.2497092723151));
#68607=CARTESIAN_POINT('Ctrl Pts',(2.57208606313468,3.6093054188893,86.3026295263971));
#68608=CARTESIAN_POINT('Ctrl Pts',(1.91898364244101,3.92834389788417,86.329089653438));
#68609=CARTESIAN_POINT('',(2.16917135428672,4.4405021828327,86.));
#68610=CARTESIAN_POINT('Ctrl Pts',(2.54472701347473,-3.56250531650751,85.9999999999999));
#68611=CARTESIAN_POINT('Ctrl Pts',(2.63513329971733,-3.50700228194743,85.9999999999999));
#68612=CARTESIAN_POINT('Ctrl Pts',(2.72315806304114,-3.44815476600379,86.));
#68613=CARTESIAN_POINT('Ctrl Pts',(2.80858471961567,-3.38601400582831,86.));
#68614=CARTESIAN_POINT('Ctrl Pts',(2.91292188753961,-3.31011742753144,86.));
#68615=CARTESIAN_POINT('Ctrl Pts',(3.01338478767473,-3.22930990203852,85.9999999999999));
#68616=CARTESIAN_POINT('Ctrl Pts',(3.1098984160813,-3.14401909712343,85.9999999999999));
#68617=CARTESIAN_POINT('Ctrl Pts',(3.20859981088314,-3.05679492424881,85.9999999999999));
#68618=CARTESIAN_POINT('Ctrl Pts',(3.30317129552995,-2.96488147836652,85.9999999999999));
#68619=CARTESIAN_POINT('Ctrl Pts',(3.39350543356314,-2.86868861821106,85.9999999999999));
#68620=CARTESIAN_POINT('Ctrl Pts',(3.48531110601377,-2.77092878561846,85.9999999999999));
#68621=CARTESIAN_POINT('Ctrl Pts',(3.57274072745551,-2.66874842101355,86.));
#68622=CARTESIAN_POINT('Ctrl Pts',(3.65564683072142,-2.56253686518592,86.));
#68623=CARTESIAN_POINT('Ctrl Pts',(3.68584784338838,-2.52384614862143,86.));
#68624=CARTESIAN_POINT('Ctrl Pts',(3.71544822227817,-2.48462014936941,86.));
#68625=CARTESIAN_POINT('Ctrl Pts',(3.74443952828415,-2.44487660282335,86.));
#68626=CARTESIAN_POINT('Ctrl Pts',(3.75595083040377,-2.42909601082439,86.));
#68627=CARTESIAN_POINT('Ctrl Pts',(3.76736609971463,-2.41323381819194,86.));
#68628=CARTESIAN_POINT('Ctrl Pts',(3.77868477502221,-2.39729111372332,86.));
#68629=CARTESIAN_POINT('Ctrl Pts',(3.78947724093788,-2.38208959146869,86.));
#68630=CARTESIAN_POINT('Ctrl Pts',(3.80017685936615,-2.36682191965604,86.));
#68631=CARTESIAN_POINT('Ctrl Pts',(3.81078105898287,-2.35149266837476,86.));
#68632=CARTESIAN_POINT('Ctrl Pts',(3.88827217096444,-2.23947282995537,86.));
#68633=CARTESIAN_POINT('Ctrl Pts',(3.96071122105411,-2.12411080348259,86.));
#68634=CARTESIAN_POINT('Ctrl Pts',(4.02800505520053,-2.00585829504273,86.));
#68635=CARTESIAN_POINT('Ctrl Pts',(4.09627718657597,-1.88588666771479,86.));
#68636=CARTESIAN_POINT('Ctrl Pts',(4.15925387587574,-1.76293927819734,86.));
#68637=CARTESIAN_POINT('Ctrl Pts',(4.21680206540741,-1.63744665973299,86.));
#68638=CARTESIAN_POINT('Ctrl Pts',(4.27457311504665,-1.5114680607595,86.));
#68639=CARTESIAN_POINT('Ctrl Pts',(4.32687396830893,-1.38292375176368,86.));
#68640=CARTESIAN_POINT('Ctrl Pts',(4.37352758038542,-1.25221847894515,86.));
#68641=CARTESIAN_POINT('Ctrl Pts',(4.41978765417706,-1.1226157473147,86.));
#68642=CARTESIAN_POINT('Ctrl Pts',(4.46049570285582,-0.990887588742712,
86.));
#68643=CARTESIAN_POINT('Ctrl Pts',(4.49543183958698,-0.857409609773572,
86.));
#68644=CARTESIAN_POINT('Ctrl Pts',(4.5001149290464,-0.839517267492425,86.));
#68645=CARTESIAN_POINT('Ctrl Pts',(4.50469423047283,-0.821593465132248,
86.));
#68646=CARTESIAN_POINT('Ctrl Pts',(4.50916914362169,-0.803639092756939,
86.));
#68647=CARTESIAN_POINT('Ctrl Pts',(4.51380380131252,-0.785043788838134,
86.));
#68648=CARTESIAN_POINT('Ctrl Pts',(4.5183245524103,-0.76642335069997,86.));
#68649=CARTESIAN_POINT('Ctrl Pts',(4.52272974339821,-0.747784414927894,
86.));
#68650=CARTESIAN_POINT('Ctrl Pts',(4.55525927718291,-0.610147728443155,
86.));
#68651=CARTESIAN_POINT('Ctrl Pts',(4.58151477805167,-0.471409643850918,
86.));
#68652=CARTESIAN_POINT('Ctrl Pts',(4.60136007125311,-0.332008493005429,
86.));
#68653=CARTESIAN_POINT('Ctrl Pts',(4.6211606972018,-0.19292110252501,86.));
#68654=CARTESIAN_POINT('Ctrl Pts',(4.63458031267456,-0.0531728409362625,
86.));
#68655=CARTESIAN_POINT('Ctrl Pts',(4.64143733545588,0.0868237683291349,
86.));
#68656=CARTESIAN_POINT('Ctrl Pts',(4.64817665416128,0.224417268832664,86.));
#68657=CARTESIAN_POINT('Ctrl Pts',(4.64857698604029,0.362251427033831,86.));
#68658=CARTESIAN_POINT('Ctrl Pts',(4.64241679650986,0.499945184924937,86.));
#68659=CARTESIAN_POINT('Ctrl Pts',(4.64160900570028,0.518001082655194,86.));
#68660=CARTESIAN_POINT('Ctrl Pts',(4.64068833141729,0.536054571915867,86.));
#68661=CARTESIAN_POINT('Ctrl Pts',(4.63965420661563,0.554104796667351,86.));
#68662=CARTESIAN_POINT('Ctrl Pts',(4.63402930249198,0.65228519372856,86.));
#68663=CARTESIAN_POINT('Ctrl Pts',(4.62504894974127,0.750369112179832,86.));
#68664=CARTESIAN_POINT('Ctrl Pts',(4.61279339604946,0.848217515281527,86.));
#68665=CARTESIAN_POINT('Ctrl Pts',(4.6078781705278,0.887460700883271,86.));
#68666=CARTESIAN_POINT('Ctrl Pts',(4.60243597814028,0.926665987486628,86.));
#68667=CARTESIAN_POINT('Ctrl Pts',(4.59647140132863,0.965824309598894,86.));
#68668=CARTESIAN_POINT('Ctrl Pts',(4.59357119157143,0.984864612281179,86.));
#68669=CARTESIAN_POINT('Ctrl Pts',(4.59054712512505,1.00389559177027,86.));
#68670=CARTESIAN_POINT('Ctrl Pts',(4.58740263898465,1.02289935437782,86.));
#68671=CARTESIAN_POINT('Ctrl Pts',(4.56506277525981,1.15791075145704,86.));
#68672=CARTESIAN_POINT('Ctrl Pts',(4.53662319345842,1.29172741325957,86.));
#68673=CARTESIAN_POINT('Ctrl Pts',(4.50239447214487,1.42398414516775,86.));
#68674=CARTESIAN_POINT('Ctrl Pts',(4.46711335178721,1.56030725329147,86.));
#68675=CARTESIAN_POINT('Ctrl Pts',(4.42568158764605,1.6949737254632,86.));
#68676=CARTESIAN_POINT('Ctrl Pts',(4.3783840316949,1.82758749733868,86.));
#68677=CARTESIAN_POINT('Ctrl Pts',(4.33065091250152,1.96142250957807,86.));
#68678=CARTESIAN_POINT('Ctrl Pts',(4.27694321392572,2.09316762674784,86.));
#68679=CARTESIAN_POINT('Ctrl Pts',(4.21750086301315,2.22240829814259,86.));
#68680=CARTESIAN_POINT('Ctrl Pts',(4.17317829962387,2.31877524464499,86.));
#68681=CARTESIAN_POINT('Ctrl Pts',(4.12566627444568,2.41374969077583,86.));
#68682=CARTESIAN_POINT('Ctrl Pts',(4.07504671027994,2.5071531160556,86.));
#68683=CARTESIAN_POINT('Ctrl Pts',(4.04973692819707,2.55385482869548,86.));
#68684=CARTESIAN_POINT('Ctrl Pts',(4.02365003622111,2.60016367547768,86.));
#68685=CARTESIAN_POINT('Ctrl Pts',(3.99679497172134,2.64605655812716,86.));
#68686=CARTESIAN_POINT('Ctrl Pts',(3.98389889010003,2.66809479826952,86.));
#68687=CARTESIAN_POINT('Ctrl Pts',(3.97082565386207,2.69003710756834,86.));
#68688=CARTESIAN_POINT('Ctrl Pts',(3.95757618483902,2.71188087703549,86.));
#68689=CARTESIAN_POINT('Ctrl Pts',(3.94694273066632,2.72941174722991,86.));
#68690=CARTESIAN_POINT('Ctrl Pts',(3.93620106712467,2.74687039690698,86.));
#68691=CARTESIAN_POINT('Ctrl Pts',(3.92535253208302,2.76425480853107,86.));
#68692=CARTESIAN_POINT('Ctrl Pts',(3.92156948774113,2.770317009536,86.));
#68693=CARTESIAN_POINT('Ctrl Pts',(3.91777342701665,2.77637021666335,86.));
#68694=CARTESIAN_POINT('Ctrl Pts',(3.91396438452183,2.78241437972366,86.));
#68695=CARTESIAN_POINT('Ctrl Pts',(3.83729807392157,2.90406796671591,86.));
#68696=CARTESIAN_POINT('Ctrl Pts',(3.7553768005218,3.02205919675202,86.));
#68697=CARTESIAN_POINT('Ctrl Pts',(3.66851542581977,3.13614597147405,86.));
#68698=CARTESIAN_POINT('Ctrl Pts',(3.58104093093735,3.25103803973578,86.));
#68699=CARTESIAN_POINT('Ctrl Pts',(3.48855596305165,3.36197093402805,86.));
#68700=CARTESIAN_POINT('Ctrl Pts',(3.39133507740585,3.46867352459105,86.));
#68701=CARTESIAN_POINT('Ctrl Pts',(3.34733743007933,3.51696215020099,86.));
#68702=CARTESIAN_POINT('Ctrl Pts',(3.30236924503015,3.56438401262811,86.));
#68703=CARTESIAN_POINT('Ctrl Pts',(3.25645316546651,3.61091188198635,86.));
#68704=CARTESIAN_POINT('Ctrl Pts',(3.23459379362241,3.63306250998163,86.));
#68705=CARTESIAN_POINT('Ctrl Pts',(3.21251956234251,3.65501049805194,86.));
#68706=CARTESIAN_POINT('Ctrl Pts',(3.19023278769809,3.67675278772905,86.));
#68707=CARTESIAN_POINT('Ctrl Pts',(3.1754125274436,3.69121097634916,86.));
#68708=CARTESIAN_POINT('Ctrl Pts',(3.16050000228347,3.70557647179484,86.));
#68709=CARTESIAN_POINT('Ctrl Pts',(3.14550229693264,3.71984252397241,86.));
#68710=CARTESIAN_POINT('Ctrl Pts',(3.03965115782958,3.82052978500174,86.));
#68711=CARTESIAN_POINT('Ctrl Pts',(2.92947196960907,3.91635255577481,86.));
#68712=CARTESIAN_POINT('Ctrl Pts',(2.81526020000344,4.00704611824462,86.));
#68713=CARTESIAN_POINT('Ctrl Pts',(2.7017209514917,4.09720564351275,86.));
#68714=CARTESIAN_POINT('Ctrl Pts',(2.58419598194515,4.18229672829323,86.));
#68715=CARTESIAN_POINT('Ctrl Pts',(2.46293629783775,4.26202671871549,86.));
#68716=CARTESIAN_POINT('Ctrl Pts',(2.3673022580591,4.32490747856343,86.));
#68717=CARTESIAN_POINT('Ctrl Pts',(2.26934437440973,4.38445308888104,86.));
#68718=CARTESIAN_POINT('Ctrl Pts',(2.16917135428672,4.4405021828327,86.));
#68719=CARTESIAN_POINT('Ctrl Pts',(2.17574200330365,4.44486699004439,26.));
#68720=CARTESIAN_POINT('Ctrl Pts',(2.28006508424018,4.38720334283182,26.));
#68721=CARTESIAN_POINT('Ctrl Pts',(2.38197081280219,4.32562977310065,26.));
#68722=CARTESIAN_POINT('Ctrl Pts',(2.48120802246663,4.26013719370393,26.));
#68723=CARTESIAN_POINT('Ctrl Pts',(2.60168389996394,4.18062794511602,26.));
#68724=CARTESIAN_POINT('Ctrl Pts',(2.71822805906223,4.09534340135309,26.));
#68725=CARTESIAN_POINT('Ctrl Pts',(2.83065917997165,4.00470474933307,26.));
#68726=CARTESIAN_POINT('Ctrl Pts',(2.90083958424456,3.94812737831637,26.));
#68727=CARTESIAN_POINT('Ctrl Pts',(2.96941670994451,3.88946302886519,26.));
#68728=CARTESIAN_POINT('Ctrl Pts',(3.03633883105725,3.82880744415046,26.));
#68729=CARTESIAN_POINT('Ctrl Pts',(3.07291548330716,3.79565580173034,26.));
#68730=CARTESIAN_POINT('Ctrl Pts',(3.10899764098955,3.76190925146565,26.));
#68731=CARTESIAN_POINT('Ctrl Pts',(3.14457605294962,3.72758291425312,26.));
#68732=CARTESIAN_POINT('Ctrl Pts',(3.16870678245731,3.70430139288574,26.));
#68733=CARTESIAN_POINT('Ctrl Pts',(3.19260993644808,3.68074881011364,26.));
#68734=CARTESIAN_POINT('Ctrl Pts',(3.21625888633569,3.65695400262287,26.));
#68735=CARTESIAN_POINT('Ctrl Pts',(3.31788256697706,3.55470354630845,26.));
#68736=CARTESIAN_POINT('Ctrl Pts',(3.41488652713577,3.44791753206169,26.));
#68737=CARTESIAN_POINT('Ctrl Pts',(3.50709206651038,3.33701451625688,26.));
#68738=CARTESIAN_POINT('Ctrl Pts',(3.59746145912339,3.2283199817939,26.));
#68739=CARTESIAN_POINT('Ctrl Pts',(3.6832218206498,3.11566998580718,26.));
#68740=CARTESIAN_POINT('Ctrl Pts',(3.76416544626806,2.99943221817338,26.));
#68741=CARTESIAN_POINT('Ctrl Pts',(3.79957828247605,2.94857819483358,26.));
#68742=CARTESIAN_POINT('Ctrl Pts',(3.83406863332226,2.89703717531663,26.));
#68743=CARTESIAN_POINT('Ctrl Pts',(3.86761651871398,2.84483889381663,26.));
#68744=CARTESIAN_POINT('Ctrl Pts',(3.89532327236222,2.80172902535561,26.));
#68745=CARTESIAN_POINT('Ctrl Pts',(3.92238715315105,2.75817083249342,26.));
#68746=CARTESIAN_POINT('Ctrl Pts',(3.94879604378199,2.71418084548941,26.));
#68747=CARTESIAN_POINT('Ctrl Pts',(3.95941005243527,2.69650081079038,26.));
#68748=CARTESIAN_POINT('Ctrl Pts',(3.96991386666906,2.6787582983834,26.));
#68749=CARTESIAN_POINT('Ctrl Pts',(3.98030512442337,2.6609577203422,26.));
#68750=CARTESIAN_POINT('Ctrl Pts',(4.05292301831336,2.53656079766556,26.));
#68751=CARTESIAN_POINT('Ctrl Pts',(4.12007774857859,2.40928022608588,26.));
#68752=CARTESIAN_POINT('Ctrl Pts',(4.18159035621228,2.27951928558395,26.));
#68753=CARTESIAN_POINT('Ctrl Pts',(4.24297458767659,2.15002915480893,26.));
#68754=CARTESIAN_POINT('Ctrl Pts',(4.29874053362767,2.01806821927191,26.));
#68755=CARTESIAN_POINT('Ctrl Pts',(4.34866300062458,1.88401668144009,26.));
#68756=CARTESIAN_POINT('Ctrl Pts',(4.39830723531613,1.75071225148679,26.));
#68757=CARTESIAN_POINT('Ctrl Pts',(4.44217322437405,1.61533971306916,26.));
#68758=CARTESIAN_POINT('Ctrl Pts',(4.47998827572883,1.47826395773052,26.));
#68759=CARTESIAN_POINT('Ctrl Pts',(4.50834956424491,1.37545714122654,26.));
#68760=CARTESIAN_POINT('Ctrl Pts',(4.53330618455047,1.27169201598405,26.));
#68761=CARTESIAN_POINT('Ctrl Pts',(4.55472254010161,1.16712293514026,26.));
#68762=CARTESIAN_POINT('Ctrl Pts',(4.5633703360405,1.12489856739035,26.));
#68763=CARTESIAN_POINT('Ctrl Pts',(4.57144068485198,1.0825431363053,26.));
#68764=CARTESIAN_POINT('Ctrl Pts',(4.57892379357549,1.04006693008015,26.));
#68765=CARTESIAN_POINT('Ctrl Pts',(4.58238261217842,1.02043371376567,26.));
#68766=CARTESIAN_POINT('Ctrl Pts',(4.58571635833316,1.00077225530923,26.));
#68767=CARTESIAN_POINT('Ctrl Pts',(4.58892275403614,0.98109144089082,26.));
#68768=CARTESIAN_POINT('Ctrl Pts',(4.6112579051569,0.843998578707096,26.));
#68769=CARTESIAN_POINT('Ctrl Pts',(4.62736483254579,0.706302385469903,26.));
#68770=CARTESIAN_POINT('Ctrl Pts',(4.63704039371253,0.568349643633761,26.));
#68771=CARTESIAN_POINT('Ctrl Pts',(4.64529719664733,0.450625350021645,26.));
#68772=CARTESIAN_POINT('Ctrl Pts',(4.64886975587046,0.332713782967315,26.));
#68773=CARTESIAN_POINT('Ctrl Pts',(4.64760179618238,0.214828774577272,26.));
#68774=CARTESIAN_POINT('Ctrl Pts',(4.64610810169851,0.0759567044171535,
26.));
#68775=CARTESIAN_POINT('Ctrl Pts',(4.63789790766952,-0.0628793196366818,
26.));
#68776=CARTESIAN_POINT('Ctrl Pts',(4.62316922884463,-0.20123695388626,26.));
#68777=CARTESIAN_POINT('Ctrl Pts',(4.60840903270106,-0.339890654178337,
26.));
#68778=CARTESIAN_POINT('Ctrl Pts',(4.58710205140909,-0.478064733297057,
26.));
#68779=CARTESIAN_POINT('Ctrl Pts',(4.55939920087044,-0.615294818730504,
26.));
#68780=CARTESIAN_POINT('Ctrl Pts',(4.54980593455313,-0.66281645389487,26.));
#68781=CARTESIAN_POINT('Ctrl Pts',(4.53944529005038,-0.710224661945217,
26.));
#68782=CARTESIAN_POINT('Ctrl Pts',(4.52832231101321,-0.757499347947085,
26.));
#68783=CARTESIAN_POINT('Ctrl Pts',(4.52204558440698,-0.784176578789409,
26.));
#68784=CARTESIAN_POINT('Ctrl Pts',(4.51552434543633,-0.81081776400017,26.));
#68785=CARTESIAN_POINT('Ctrl Pts',(4.50876854798769,-0.837384466189193,
26.));
#68786=CARTESIAN_POINT('Ctrl Pts',(4.47488762719443,-0.97061882370914,26.));
#68787=CARTESIAN_POINT('Ctrl Pts',(4.43508456291388,-1.10210853291686,26.));
#68788=CARTESIAN_POINT('Ctrl Pts',(4.38958618794437,-1.2314396670372,26.));
#68789=CARTESIAN_POINT('Ctrl Pts',(4.34401166128567,-1.36098726568698,26.));
#68790=CARTESIAN_POINT('Ctrl Pts',(4.29272234355304,-1.48836984485114,26.));
#68791=CARTESIAN_POINT('Ctrl Pts',(4.23589771868779,-1.61315285151403,26.));
#68792=CARTESIAN_POINT('Ctrl Pts',(4.18015009153959,-1.73557084452973,26.));
#68793=CARTESIAN_POINT('Ctrl Pts',(4.11907449353476,-1.85548750502406,26.));
#68794=CARTESIAN_POINT('Ctrl Pts',(4.05280063784894,-1.97246430242313,26.));
#68795=CARTESIAN_POINT('Ctrl Pts',(4.0071971296468,-2.0529568629426,26.));
#68796=CARTESIAN_POINT('Ctrl Pts',(3.95913143391569,-2.13205676654158,26.));
#68797=CARTESIAN_POINT('Ctrl Pts',(3.90866288715487,-2.2096607611529,26.));
#68798=CARTESIAN_POINT('Ctrl Pts',(3.88457170018092,-2.24670506823327,26.));
#68799=CARTESIAN_POINT('Ctrl Pts',(3.85993289144,-2.28340838898037,26.));
#68800=CARTESIAN_POINT('Ctrl Pts',(3.83475240364166,-2.31975877789511,26.));
#68801=CARTESIAN_POINT('Ctrl Pts',(3.81911152043036,-2.34233785548306,26.));
#68802=CARTESIAN_POINT('Ctrl Pts',(3.80326163575805,-2.36478075250477,26.));
#68803=CARTESIAN_POINT('Ctrl Pts',(3.78720411571068,-2.38708450953735,26.));
#68804=CARTESIAN_POINT('Ctrl Pts',(3.77570997324099,-2.40304977442168,26.));
#68805=CARTESIAN_POINT('Ctrl Pts',(3.76411377204687,-2.41893767166227,26.));
#68806=CARTESIAN_POINT('Ctrl Pts',(3.75242084457745,-2.43474120045983,26.));
#68807=CARTESIAN_POINT('Ctrl Pts',(3.66959100122522,-2.54668954001269,26.));
#68808=CARTESIAN_POINT('Ctrl Pts',(3.58184107407233,-2.65450498805187,26.));
#68809=CARTESIAN_POINT('Ctrl Pts',(3.48944434360053,-2.75789800803035,26.));
#68810=CARTESIAN_POINT('Ctrl Pts',(3.40008035358429,-2.85789735603679,26.));
#68811=CARTESIAN_POINT('Ctrl Pts',(3.3063688476751,-2.95376016129811,26.));
#68812=CARTESIAN_POINT('Ctrl Pts',(3.20852006341883,-3.04518760514634,26.));
#68813=CARTESIAN_POINT('Ctrl Pts',(3.11161693078311,-3.13573145589637,26.));
#68814=CARTESIAN_POINT('Ctrl Pts',(3.01065557724222,-3.2219256920299,26.));
#68815=CARTESIAN_POINT('Ctrl Pts',(2.90581240538358,-3.30343749134566,26.));
#68816=CARTESIAN_POINT('Ctrl Pts',(2.80309976478498,-3.38329287915244,26.));
#68817=CARTESIAN_POINT('Ctrl Pts',(2.69666097167601,-3.45865450573126,26.));
#68818=CARTESIAN_POINT('Ctrl Pts',(2.58664264704464,-3.52916309203659,26.));
#68819=CARTESIAN_POINT('Ctrl Pts',(2.57062378681069,-3.53942926535911,26.));
#68820=CARTESIAN_POINT('Ctrl Pts',(2.55452901448013,-3.54959246856517,26.));
#68821=CARTESIAN_POINT('Ctrl Pts',(2.53835875722658,-3.55965150255066,26.));
#68822=CARTESIAN_POINT('Ctrl Pts',(2.16917135428672,4.4405021828327,86.));
#68823=CARTESIAN_POINT('Ctrl Pts',(2.90742207776984,4.07986902565238,85.973539872959));
#68824=CARTESIAN_POINT('Ctrl Pts',(3.54838370350565,3.53163043353487,85.947079745918));
#68825=CARTESIAN_POINT('Ctrl Pts',(4.02597047844268,2.86203885652618,85.9206196188771));
#68826=CARTESIAN_POINT('Ctrl Pts',(4.50355725337971,2.19244727951748,85.894159491836));
#68827=CARTESIAN_POINT('Ctrl Pts',(4.817769177518,1.40150271761755,85.8676993647951));
#68828=CARTESIAN_POINT('Ctrl Pts',(4.91302361527573,0.586752768661848,85.8412392377541));
#68829=CARTESIAN_POINT('Ctrl Pts',(5.10353249079119,-1.04274712924955,85.7883189836721));
#68830=CARTESIAN_POINT('Ctrl Pts',(4.41821142078444,-2.76746857538425,85.7353987295902));
#68831=CARTESIAN_POINT('Ctrl Pts',(3.16027096066549,-3.81000496808603,85.6824784755082));
#68832=CARTESIAN_POINT('Ctrl Pts',(1.90233050054647,-4.85254136078787,85.6295582214263));
#68833=CARTESIAN_POINT('Ctrl Pts',(0.071770650315324,-5.21289270005682,
85.5766379673442));
#68834=CARTESIAN_POINT('Ctrl Pts',(-1.4889429323282,-4.72167812247258,85.5237177132623));
#68835=CARTESIAN_POINT('Ctrl Pts',(-3.04965651497173,-4.23046354488835,
85.4707974591803));
#68836=CARTESIAN_POINT('Ctrl Pts',(-4.34052383002751,-2.88768305045078,
85.4178772050984));
#68837=CARTESIAN_POINT('Ctrl Pts',(-4.77319106421879,-1.30997578306141,
85.3649569510165));
#68838=CARTESIAN_POINT('Ctrl Pts',(-4.88938737554012,-0.886269640491669,
85.3507447855632));
#68839=CARTESIAN_POINT('Ctrl Pts',(-4.94368731125384,-0.445619761719663,
85.33653262011));
#68840=CARTESIAN_POINT('Ctrl Pts',(-4.93983901057914,-0.00407131671605609,
85.3223204546568));
#68841=CARTESIAN_POINT('Origin',(0.,0.,16.));
#68842=CARTESIAN_POINT('Origin',(0.,0.,86.));
#68843=CARTESIAN_POINT('Origin',(0.,0.,26.));
#68844=CARTESIAN_POINT('',(4.61880215351701,-8.,26.));
#68845=CARTESIAN_POINT('',(9.23760430703401,0.,26.));
#68846=CARTESIAN_POINT('',(4.61880215351701,-8.,26.));
#68847=CARTESIAN_POINT('',(4.61880215351701,8.,26.));
#68848=CARTESIAN_POINT('',(9.23760430703401,0.,26.));
#68849=CARTESIAN_POINT('',(-4.61880215351701,8.,26.));
#68850=CARTESIAN_POINT('',(4.61880215351701,8.,26.));
#68851=CARTESIAN_POINT('',(-9.23760430703401,1.11022302462516E-15,26.));
#68852=CARTESIAN_POINT('',(-4.618802153517,8.,26.));
#68853=CARTESIAN_POINT('',(-4.61880215351701,-8.,26.));
#68854=CARTESIAN_POINT('',(-9.23760430703401,1.1312802546399E-15,26.));
#68855=CARTESIAN_POINT('',(-4.61880215351701,-8.,26.));
#68856=CARTESIAN_POINT('Origin',(0.,0.,20.));
#68857=CARTESIAN_POINT('',(4.61880215351701,-8.,20.));
#68858=CARTESIAN_POINT('',(9.23760430703401,0.,20.));
#68859=CARTESIAN_POINT('',(4.61880215351701,-8.,20.));
#68860=CARTESIAN_POINT('',(-4.61880215351701,-8.,20.));
#68861=CARTESIAN_POINT('',(-4.61880215351701,-8.,20.));
#68862=CARTESIAN_POINT('',(-9.23760430703401,1.1312802546399E-15,20.));
#68863=CARTESIAN_POINT('',(-9.23760430703401,1.1312802546399E-15,20.));
#68864=CARTESIAN_POINT('',(-4.618802153517,8.,20.));
#68865=CARTESIAN_POINT('',(-4.618802153517,8.,20.));
#68866=CARTESIAN_POINT('',(4.61880215351701,8.,20.));
#68867=CARTESIAN_POINT('',(4.61880215351701,8.,20.));
#68868=CARTESIAN_POINT('',(9.23760430703401,0.,20.));
#68869=CARTESIAN_POINT('',(-5.,6.12323399573677E-16,20.));
#68870=CARTESIAN_POINT('Origin',(0.,0.,20.));
#68871=CARTESIAN_POINT('Origin',(-4.61880215351701,-8.,20.));
#68872=CARTESIAN_POINT('',(4.61880215351701,-8.,20.));
#68873=CARTESIAN_POINT('',(-4.61880215351701,-8.,20.));
#68874=CARTESIAN_POINT('Origin',(-9.23760430703401,1.1312802546399E-15,
20.));
#68875=CARTESIAN_POINT('',(-9.23760430703401,1.1312802546399E-15,20.));
#68876=CARTESIAN_POINT('Origin',(-4.618802153517,8.,20.));
#68877=CARTESIAN_POINT('',(-4.618802153517,8.,20.));
#68878=CARTESIAN_POINT('Origin',(4.61880215351701,8.,20.));
#68879=CARTESIAN_POINT('',(4.61880215351701,8.,20.));
#68880=CARTESIAN_POINT('Origin',(9.23760430703401,0.,20.));
#68881=CARTESIAN_POINT('',(9.23760430703401,0.,20.));
#68882=CARTESIAN_POINT('Origin',(4.61880215351701,-8.,20.));
#68883=CARTESIAN_POINT('Origin',(0.,0.,16.));
#68884=CARTESIAN_POINT('',(-5.,6.12323399573677E-16,17.3166247903554));
#68885=CARTESIAN_POINT('',(-5.,-6.12323399573677E-16,16.));
#68886=CARTESIAN_POINT('Origin',(0.,0.,17.3166247903554));
#68887=CARTESIAN_POINT('Origin',(0.,0.,86.));
#68888=CARTESIAN_POINT('Origin',(5.55111512312578E-16,0.,14.));
#68889=CARTESIAN_POINT('',(1.87717472568372E-16,-4.49927934798557E-32,8.));
#68890=CARTESIAN_POINT('Origin',(5.55111512312578E-16,0.,14.));
#68891=CARTESIAN_POINT('',(0.,0.,0.));
#68892=CARTESIAN_POINT('Origin',(0.,0.,4.));
#68893=CARTESIAN_POINT('',(-4.51054691465169,-0.000515110389415763,0.38741669750802));
#68894=CARTESIAN_POINT('',(-4.51874859034235,-0.000597354552748235,0.112583302491978));
#68895=CARTESIAN_POINT('',(-4.51775,5.53264807684796E-16,4.));
#68896=CARTESIAN_POINT('',(-3.43378788736191,2.93584158412995,0.));
#68897=CARTESIAN_POINT('Ctrl Pts',(-4.51874859034235,-0.000597354552748235,
0.112583302491978));
#68898=CARTESIAN_POINT('Ctrl Pts',(-4.51722457181931,0.322607764342177,
0.101221950551661));
#68899=CARTESIAN_POINT('Ctrl Pts',(-4.48139903614817,0.645891255334514,
0.0898605986113441));
#68900=CARTESIAN_POINT('Ctrl Pts',(-4.41220310426637,0.961201691623003,
0.0784992466710271));
#68901=CARTESIAN_POINT('Ctrl Pts',(-4.25283743035848,1.68739554150353,0.0523328311140182));
#68902=CARTESIAN_POINT('Ctrl Pts',(-3.91646501574702,2.37129788193745,0.0261664155570086));
#68903=CARTESIAN_POINT('Ctrl Pts',(-3.43378788736191,2.93584158412995,-2.08166817117217E-16));
#68904=CARTESIAN_POINT('',(3.44055068766013,2.93810645203836,-8.32667268468867E-16));
#68905=CARTESIAN_POINT('Origin',(0.,0.,0.));
#68906=CARTESIAN_POINT('Ctrl Pts',(3.44055068766013,2.93810645203836,-8.32667268468867E-16));
#68907=CARTESIAN_POINT('Ctrl Pts',(2.51857754810217,4.00873567447971,0.0500251109657056));
#68908=CARTESIAN_POINT('Ctrl Pts',(1.04980798302248,4.62287274287841,0.10005022193141));
#68909=CARTESIAN_POINT('Ctrl Pts',(-0.359976603224271,4.51112404046721,
0.150075332897117));
#68910=CARTESIAN_POINT('Ctrl Pts',(-1.83479629347494,4.39422023240758,0.202408164011137));
#68911=CARTESIAN_POINT('Ctrl Pts',(-3.24506337966313,3.48291388857057,0.254740995125157));
#68912=CARTESIAN_POINT('Ctrl Pts',(-3.96016577839605,2.18804786800098,0.307073826239177));
#68913=CARTESIAN_POINT('Ctrl Pts',(-4.32611438556047,1.52540931786942,0.333854783328791));
#68914=CARTESIAN_POINT('Ctrl Pts',(-4.5100126795522,0.762323836917479,0.360635740418406));
#68915=CARTESIAN_POINT('Ctrl Pts',(-4.51054691465169,-0.000515110389415763,
0.38741669750802));
#68916=CARTESIAN_POINT('Origin',(0.,0.,4.));
#68917=CARTESIAN_POINT('',(-4.52244050167421,-0.00276900106626683,1.38741669750802));
#68918=CARTESIAN_POINT('',(-4.5233994151039,0.0021134167823725,1.11258330249198));
#68919=CARTESIAN_POINT('',(-4.51775,5.53264807684796E-16,4.));
#68920=CARTESIAN_POINT('Ctrl Pts',(-4.5233994151039,0.0021134167823725,
1.11258330249198));
#68921=CARTESIAN_POINT('Ctrl Pts',(-4.52416026905118,0.130280331830068,
1.10805201945945));
#68922=CARTESIAN_POINT('Ctrl Pts',(-4.51917716893618,0.258387747461467,
1.10352073642693));
#68923=CARTESIAN_POINT('Ctrl Pts',(-4.50825644670978,0.385987082702882,
1.0989894533944));
#68924=CARTESIAN_POINT('Ctrl Pts',(-4.38213051111597,1.85966118637707,1.04665662228038));
#68925=CARTESIAN_POINT('Ctrl Pts',(-3.46401651516602,3.2655651297045,0.994323791166365));
#68926=CARTESIAN_POINT('Ctrl Pts',(-2.16517718342927,3.97324079579977,0.941990960052346));
#68927=CARTESIAN_POINT('Ctrl Pts',(-0.866337851692522,4.68091646189503,
0.889658128938326));
#68928=CARTESIAN_POINT('Ctrl Pts',(0.813226815831038,4.69036385075812,0.837325297824306));
#68929=CARTESIAN_POINT('Ctrl Pts',(2.11977950774785,3.99758999513324,0.784992466710287));
#68930=CARTESIAN_POINT('Ctrl Pts',(3.42633219966466,3.30481613950837,0.732659635596268));
#68931=CARTESIAN_POINT('Ctrl Pts',(4.35987291597477,1.90982103939552,0.680326804482248));
#68932=CARTESIAN_POINT('Ctrl Pts',(4.50321991349222,0.437577595733461,0.627993973368229));
#68933=CARTESIAN_POINT('Ctrl Pts',(4.64656691100967,-1.0346658479286,0.57566114225421));
#68934=CARTESIAN_POINT('Ctrl Pts',(3.99972018973448,-2.58415763513987,0.523328311140192));
#68935=CARTESIAN_POINT('Ctrl Pts',(2.85003205531654,-3.51527160715898,0.470995480026173));
#68936=CARTESIAN_POINT('Ctrl Pts',(1.7003439208986,-4.4463855791781,0.418662648912154));
#68937=CARTESIAN_POINT('Ctrl Pts',(0.0478143733379097,-4.75912173600502,
0.366329817798135));
#68938=CARTESIAN_POINT('Ctrl Pts',(-1.36123648115533,-4.3152078830999,0.313996986684115));
#68939=CARTESIAN_POINT('Ctrl Pts',(-2.77028733564855,-3.87129403019478,
0.261664155570096));
#68940=CARTESIAN_POINT('Ctrl Pts',(-3.93585949707434,-2.67073016755762,
0.209331324456076));
#68941=CARTESIAN_POINT('Ctrl Pts',(-4.34790497327718,-1.24589506757571,
0.156998493342058));
#68942=CARTESIAN_POINT('Ctrl Pts',(-4.46447347068682,-0.842806340108052,
0.142193429725364));
#68943=CARTESIAN_POINT('Ctrl Pts',(-4.52073455040284,-0.421768388741025,
0.127388366108671));
#68944=CARTESIAN_POINT('Ctrl Pts',(-4.51874859034235,-0.000597354552748235,
0.112583302491978));
#68945=CARTESIAN_POINT('Ctrl Pts',(-4.51054691465169,-0.000515110389415763,
0.38741669750802));
#68946=CARTESIAN_POINT('Ctrl Pts',(-4.51105663160901,-0.728344389129203,
0.412968571532425));
#68947=CARTESIAN_POINT('Ctrl Pts',(-4.3446466691941,-1.4559492437521,0.438520445556829));
#68948=CARTESIAN_POINT('Ctrl Pts',(-4.01017598625922,-2.09587333886935,
0.464072319581234));
#68949=CARTESIAN_POINT('Ctrl Pts',(-3.32514608411178,-3.40650282786799,
0.516405150695253));
#68950=CARTESIAN_POINT('Ctrl Pts',(-1.9351485685392,-4.34933610856308,0.568737981809272));
#68951=CARTESIAN_POINT('Ctrl Pts',(-0.463832664911,-4.50105515886306,0.621070812923292));
#68952=CARTESIAN_POINT('Ctrl Pts',(1.00748323871719,-4.65277420916302,0.673403644037311));
#68953=CARTESIAN_POINT('Ctrl Pts',(2.560117530401,-4.01337902906788,0.725736475151331));
#68954=CARTESIAN_POINT('Ctrl Pts',(3.49818631344856,-2.86985357730659,0.77806930626535));
#68955=CARTESIAN_POINT('Ctrl Pts',(4.43625509649613,-1.7263281255453,0.830402137379369));
#68956=CARTESIAN_POINT('Ctrl Pts',(4.75975837090746,-0.0786724021178761,
0.882734968493387));
#68957=CARTESIAN_POINT('Ctrl Pts',(4.32353285348464,1.33455667095541,0.935067799607406));
#68958=CARTESIAN_POINT('Ctrl Pts',(3.88730733606183,2.7477857440287,0.987400630721425));
#68959=CARTESIAN_POINT('Ctrl Pts',(2.69135302680487,3.92658816674785,1.03973346183545));
#68960=CARTESIAN_POINT('Ctrl Pts',(1.27193499135498,4.34236723513978,1.09206629294946));
#68961=CARTESIAN_POINT('Ctrl Pts',(-0.147483044094926,4.7581463035317,1.14439912406348));
#68962=CARTESIAN_POINT('Ctrl Pts',(-1.79036480573777,4.41090201759639,1.1967319551775));
#68963=CARTESIAN_POINT('Ctrl Pts',(-2.92016350112278,3.45636436650575,1.24906478629152));
#68964=CARTESIAN_POINT('Ctrl Pts',(-3.91577693325848,2.61519636835964,1.29518209003036));
#68965=CARTESIAN_POINT('Ctrl Pts',(-4.51294659780824,1.30242392182032,1.34129939376919));
#68966=CARTESIAN_POINT('Ctrl Pts',(-4.52244050167421,-0.00276900106626683,
1.38741669750802));
#68967=CARTESIAN_POINT('Origin',(0.,0.,4.));
#68968=CARTESIAN_POINT('',(-4.51698911071085,0.00388851918503852,2.38741669750802));
#68969=CARTESIAN_POINT('',(-4.51093362149631,0.00101330851266679,2.11258330249198));
#68970=CARTESIAN_POINT('',(-4.51775,5.53264807684796E-16,4.));
#68971=CARTESIAN_POINT('Ctrl Pts',(-4.51093362149631,0.00101330851266679,
2.11258330249198));
#68972=CARTESIAN_POINT('Ctrl Pts',(-4.51232811703185,0.680923530020972,
2.08871567281024));
#68973=CARTESIAN_POINT('Ctrl Pts',(-4.36790019846314,1.36027124256301,2.06484804312849));
#68974=CARTESIAN_POINT('Ctrl Pts',(-4.07455659430891,1.96770381197164,2.04098041344675));
#68975=CARTESIAN_POINT('Ctrl Pts',(-3.43136321904367,3.29957742036487,1.98864758233273));
#68976=CARTESIAN_POINT('Ctrl Pts',(-2.07224023608874,4.28571055146719,1.93631475121871));
#68977=CARTESIAN_POINT('Ctrl Pts',(-0.606537899693793,4.48397159897241,
1.88398192010469));
#68978=CARTESIAN_POINT('Ctrl Pts',(0.859164436701136,4.68223264647763,1.83164908899067));
#68979=CARTESIAN_POINT('Ctrl Pts',(2.43144612653608,4.09262161038578,1.77931625787665));
#68980=CARTESIAN_POINT('Ctrl Pts',(3.40536636602181,2.97949323501332,1.72698342676264));
#68981=CARTESIAN_POINT('Ctrl Pts',(4.37928660550757,1.86636485964083,1.67465059564862));
#68982=CARTESIAN_POINT('Ctrl Pts',(4.75484539464409,0.229719144987712,1.6223177645346));
#68983=CARTESIAN_POINT('Ctrl Pts',(4.36368967023442,-1.19666928711504,1.56998493342058));
#68984=CARTESIAN_POINT('Ctrl Pts',(3.97253394582476,-2.62305771921779,1.51765210230656));
#68985=CARTESIAN_POINT('Ctrl Pts',(2.81466370786892,-3.83918886877017,1.46531927119254));
#68986=CARTESIAN_POINT('Ctrl Pts',(1.40915332177568,-4.29979703199479,1.41298644007852));
#68987=CARTESIAN_POINT('Ctrl Pts',(0.00364293568242802,-4.76040519521942,
1.3606536089645));
#68988=CARTESIAN_POINT('Ctrl Pts',(-1.64950759854823,-4.46549037211628,
1.30832077785048));
#68989=CARTESIAN_POINT('Ctrl Pts',(-2.80901392804473,-3.54731082855424,
1.25598794673646));
#68990=CARTESIAN_POINT('Ctrl Pts',(-3.86812340827646,-2.70863264767388,
1.20818639865497));
#68991=CARTESIAN_POINT('Ctrl Pts',(-4.51537299162016,-1.34994888171753,
1.16038485057347));
#68992=CARTESIAN_POINT('Ctrl Pts',(-4.5233994151039,0.0021134167823725,
1.11258330249198));
#68993=CARTESIAN_POINT('Ctrl Pts',(-4.52244050167421,-0.00276900106626683,
1.38741669750802));
#68994=CARTESIAN_POINT('Ctrl Pts',(-4.52372005651789,-0.178678295071038,
1.39363222488321));
#68995=CARTESIAN_POINT('Ctrl Pts',(-4.51432465941186,-0.35444990932754,
1.39984775225839));
#68996=CARTESIAN_POINT('Ctrl Pts',(-4.49379103756964,-0.528910718243546,
1.40606327963358));
#68997=CARTESIAN_POINT('Ctrl Pts',(-4.32090424950433,-1.99781713565632,
1.4583961107476));
#68998=CARTESIAN_POINT('Ctrl Pts',(-3.3584150442465,-3.37379895423595,1.51072894186162));
#68999=CARTESIAN_POINT('Ctrl Pts',(-2.037860803389,-4.0399278796399,1.56306177297564));
#69000=CARTESIAN_POINT('Ctrl Pts',(-0.717306562531505,-4.70605680504386,
1.61539460408966));
#69001=CARTESIAN_POINT('Ctrl Pts',(0.961312713925656,-4.66233283727215,
1.66772743520368));
#69002=CARTESIAN_POINT('Ctrl Pts',(2.24539906972787,-3.92836571897045,1.72006026631769));
#69003=CARTESIAN_POINT('Ctrl Pts',(3.52948542553009,-3.19439860066874,1.77239309743171));
#69004=CARTESIAN_POINT('Ctrl Pts',(4.41903886067735,-1.77018833183704,1.82472592854573));
#69005=CARTESIAN_POINT('Ctrl Pts',(4.51522900816629,-0.294270957708535,
1.87705875965975));
#69006=CARTESIAN_POINT('Ctrl Pts',(4.61141915565522,1.18164641641996,1.92939159077377));
#69007=CARTESIAN_POINT('Ctrl Pts',(3.91424601548584,2.70927089584527,1.98172442188779));
#69008=CARTESIAN_POINT('Ctrl Pts',(2.73628580760446,3.60369609834798,2.03405725300181));
#69009=CARTESIAN_POINT('Ctrl Pts',(1.55832559972309,4.4981213008507,2.08639008411583));
#69010=CARTESIAN_POINT('Ctrl Pts',(-0.100421675870265,4.75934722643081,
2.13872291522985));
#69011=CARTESIAN_POINT('Ctrl Pts',(-1.49626358664302,4.2702551012346,2.19105574634387));
#69012=CARTESIAN_POINT('Ctrl Pts',(-2.89210549741577,3.78116297603839,2.24338857745789));
#69013=CARTESIAN_POINT('Ctrl Pts',(-4.02504204336792,2.54175280006585,2.29572140857191));
#69014=CARTESIAN_POINT('Ctrl Pts',(-4.38712504707582,1.10770899592287,2.34805423968593));
#69015=CARTESIAN_POINT('Ctrl Pts',(-4.47790602629514,0.748167400624681,
2.36117505895996));
#69016=CARTESIAN_POINT('Ctrl Pts',(-4.52023125554896,0.376391161643011,
2.37429587823399));
#69017=CARTESIAN_POINT('Ctrl Pts',(-4.51698911071085,0.00388851918503852,
2.38741669750802));
#69018=CARTESIAN_POINT('Origin',(0.,0.,4.));
#69019=CARTESIAN_POINT('',(-4.51234492774861,-0.00257476452032779,3.38741669750802));
#69020=CARTESIAN_POINT('',(-4.52027081060448,-0.00355576929457683,3.11258330249198));
#69021=CARTESIAN_POINT('',(-4.51775,5.53264807684796E-16,4.));
#69022=CARTESIAN_POINT('Ctrl Pts',(-4.52027081060448,-0.00355576929457683,
3.11258330249198));
#69023=CARTESIAN_POINT('Ctrl Pts',(-4.50971003274407,1.22072076070225,3.06937932616102));
#69024=CARTESIAN_POINT('Ctrl Pts',(-3.99354051828841,2.45284880293372,3.02617534983006));
#69025=CARTESIAN_POINT('Ctrl Pts',(-3.10547711214626,3.29088013555457,2.9829713734991));
#69026=CARTESIAN_POINT('Ctrl Pts',(-2.02976889732455,4.30598466811756,2.93063854238508));
#69027=CARTESIAN_POINT('Ctrl Pts',(-0.408403261408893,4.74285492731681,
2.87830571127106));
#69028=CARTESIAN_POINT('Ctrl Pts',(1.03168676818161,4.40562172719721,2.82597288015704));
#69029=CARTESIAN_POINT('Ctrl Pts',(2.4717767977721,4.06838852707761,2.77364004904302));
#69030=CARTESIAN_POINT('Ctrl Pts',(3.73059122103745,2.95705186763916,2.721307217929));
#69031=CARTESIAN_POINT('Ctrl Pts',(4.2437450475446,1.56987545160024,2.66897438681498));
#69032=CARTESIAN_POINT('Ctrl Pts',(4.75689887405174,0.182699035561331,2.61664155570096));
#69033=CARTESIAN_POINT('Ctrl Pts',(4.5243921038007,-1.48031713707804,2.56430872458694));
#69034=CARTESIAN_POINT('Ctrl Pts',(3.65046881853353,-2.67356621578173,2.51197589347292));
#69035=CARTESIAN_POINT('Ctrl Pts',(2.77654553326636,-3.86681529448543,2.4596430623589));
#69036=CARTESIAN_POINT('Ctrl Pts',(1.26120573298304,-4.59029727925343,2.40731023124489));
#69037=CARTESIAN_POINT('Ctrl Pts',(-0.216154740062777,-4.51964138893216,
2.35497740013087));
#69038=CARTESIAN_POINT('Ctrl Pts',(-1.69351521310859,-4.44898549861089,
2.30264456901685));
#69039=CARTESIAN_POINT('Ctrl Pts',(-3.1328963589169,-3.58419173320037,2.25031173790283));
#69040=CARTESIAN_POINT('Ctrl Pts',(-3.88895504803329,-2.31298780765304,
2.19797890678881));
#69041=CARTESIAN_POINT('Ctrl Pts',(-4.30019522790109,-1.62154660273587,
2.16951370535653));
#69042=CARTESIAN_POINT('Ctrl Pts',(-4.50927050719276,-0.809866601606811,
2.14104850392425));
#69043=CARTESIAN_POINT('Ctrl Pts',(-4.51093362149631,0.00101330851266679,
2.11258330249198));
#69044=CARTESIAN_POINT('Ctrl Pts',(-4.51698911071085,0.00388851918503852,
2.38741669750802));
#69045=CARTESIAN_POINT('Ctrl Pts',(-4.50729985128856,-1.10934821713655,
2.42662870934801));
#69046=CARTESIAN_POINT('Ctrl Pts',(-4.09063314279102,-2.22907270570801,
2.465840721188));
#69047=CARTESIAN_POINT('Ctrl Pts',(-3.34408434212355,-3.04811166820345,
2.50505273302798));
#69048=CARTESIAN_POINT('Ctrl Pts',(-2.34773117199973,-4.14121109587334,
2.557385564142));
#69049=CARTESIAN_POINT('Ctrl Pts',(-0.763795370288439,-4.69873251889968,
2.60971839525602));
#69050=CARTESIAN_POINT('Ctrl Pts',(0.697571505631126,-4.4707134324377,2.66205122637004));
#69051=CARTESIAN_POINT('Ctrl Pts',(2.15893838155069,-4.24269434597572,2.71438405748406));
#69052=CARTESIAN_POINT('Ctrl Pts',(3.49773633167853,-3.2291347500254,2.76671688859808));
#69053=CARTESIAN_POINT('Ctrl Pts',(4.11372028899329,-1.88446020659954,2.8190497197121));
#69054=CARTESIAN_POINT('Ctrl Pts',(4.72970424630805,-0.539785663173669,
2.87138255082612));
#69055=CARTESIAN_POINT('Ctrl Pts',(4.62287421080972,1.13600382772776,2.92371538194014));
#69056=CARTESIAN_POINT('Ctrl Pts',(3.84112705187867,2.39157432571858,2.97604821305416));
#69057=CARTESIAN_POINT('Ctrl Pts',(3.05937989294762,3.6471448237094,3.02838104416818));
#69058=CARTESIAN_POINT('Ctrl Pts',(1.60271561058387,4.48249632878962,3.08071387528219));
#69059=CARTESIAN_POINT('Ctrl Pts',(0.124224136080841,4.52310215772866,3.13304670639621));
#69060=CARTESIAN_POINT('Ctrl Pts',(-1.35426733842219,4.56370798666771,3.18537953751023));
#69061=CARTESIAN_POINT('Ctrl Pts',(-2.85458600506451,3.80956813946558,3.23771236862425));
#69062=CARTESIAN_POINT('Ctrl Pts',(-3.70406963378462,2.5987983669013,3.29004519973827));
#69063=CARTESIAN_POINT('Ctrl Pts',(-4.2309249653141,1.84787099365534,3.32250236566152));
#69064=CARTESIAN_POINT('Ctrl Pts',(-4.50743256748542,0.921298090727453,
3.35495953158477));
#69065=CARTESIAN_POINT('Ctrl Pts',(-4.51234492774861,-0.00257476452032779,
3.38741669750802));
#69066=CARTESIAN_POINT('Origin',(0.,0.,4.));
#69067=CARTESIAN_POINT('',(-4.52478583629221,-0.000271302356462328,4.38741669750802));
#69068=CARTESIAN_POINT('',(-4.51939464917808,0.00373292266216646,4.11258330249198));
#69069=CARTESIAN_POINT('',(-4.51775,5.53264807684796E-16,4.));
#69070=CARTESIAN_POINT('Ctrl Pts',(-4.51939464917808,0.00373292266216647,
4.11258330249198));
#69071=CARTESIAN_POINT('Ctrl Pts',(-4.52195179175284,0.293129143485266,
4.10237581062582));
#69072=CARTESIAN_POINT('Ctrl Pts',(-4.49647546580418,0.582077227182858,
4.09216831875966));
#69073=CARTESIAN_POINT('Ctrl Pts',(-4.44131034778915,0.865241438283023,
4.0819608268935));
#69074=CARTESIAN_POINT('Ctrl Pts',(-4.15848408230504,2.31699717136045,4.02962799577948));
#69075=CARTESIAN_POINT('Ctrl Pts',(-3.09528361658689,3.61672297535275,3.97729516466546));
#69076=CARTESIAN_POINT('Ctrl Pts',(-1.72839087618034,4.18169168234348,3.92496233355144));
#69077=CARTESIAN_POINT('Ctrl Pts',(-0.361498135773788,4.7466603893342,3.87262950243742));
#69078=CARTESIAN_POINT('Ctrl Pts',(1.30908687932117,4.57687199932334,3.8202966713234));
#69079=CARTESIAN_POINT('Ctrl Pts',(2.5343636726828,3.74845049626232,3.76796384020938));
#69080=CARTESIAN_POINT('Ctrl Pts',(3.75964046604444,2.9200289932013,3.71563100909536));
#69081=CARTESIAN_POINT('Ctrl Pts',(4.53960903767275,1.43297437709012,3.66329817798134));
#69082=CARTESIAN_POINT('Ctrl Pts',(4.52457341059044,-0.0459980138823182,
3.61096534686733));
#69083=CARTESIAN_POINT('Ctrl Pts',(4.50953778350813,-1.52497040485477,3.55863251575331));
#69084=CARTESIAN_POINT('Ctrl Pts',(3.69949795771518,-2.99586057068848,3.50629968463929));
#69085=CARTESIAN_POINT('Ctrl Pts',(2.45763224901275,-3.79920044943065,3.45396685352527));
#69086=CARTESIAN_POINT('Ctrl Pts',(1.21576654031032,-4.60254032817281,3.40163402241125));
#69087=CARTESIAN_POINT('Ctrl Pts',(-0.457925051301578,-4.73832991982345,
3.34930119129723));
#69088=CARTESIAN_POINT('Ctrl Pts',(-1.81304922569253,-4.1456884652134,3.29696836018321));
#69089=CARTESIAN_POINT('Ctrl Pts',(-3.16817340008348,-3.55304701060334,
3.24463552906919));
#69090=CARTESIAN_POINT('Ctrl Pts',(-4.20473015725347,-2.23197450973259,
3.19230269795517));
#69091=CARTESIAN_POINT('Ctrl Pts',(-4.45798313897459,-0.774768856333857,
3.13996986684115));
#69092=CARTESIAN_POINT('Ctrl Pts',(-4.50216018126897,-0.520576248830078,
3.1308410120581));
#69093=CARTESIAN_POINT('Ctrl Pts',(-4.52250226742098,-0.262241279420579,
3.12171215727504));
#69094=CARTESIAN_POINT('Ctrl Pts',(-4.52027081060448,-0.00355576929457683,
3.11258330249198));
#69095=CARTESIAN_POINT('Ctrl Pts',(-4.51234492774861,-0.00257476452032779,
3.38741669750802));
#69096=CARTESIAN_POINT('Ctrl Pts',(-4.51535309020244,-0.568323098591327,
3.40729236269879));
#69097=CARTESIAN_POINT('Ctrl Pts',(-4.41651517435603,-1.13305893603127,
3.42716802788956));
#69098=CARTESIAN_POINT('Ctrl Pts',(-4.21095206217547,-1.65582834772821,
3.44704369308033));
#69099=CARTESIAN_POINT('Ctrl Pts',(-3.66970227104832,-3.032285591867,3.49937652419435));
#69100=CARTESIAN_POINT('Ctrl Pts',(-2.3885540979961,-4.11780038221814,3.55170935530837));
#69101=CARTESIAN_POINT('Ctrl Pts',(-0.941905499312602,-4.42568625369714,
3.60404218642239));
#69102=CARTESIAN_POINT('Ctrl Pts',(0.504743099370899,-4.73357212517614,
3.65637501753641));
#69103=CARTESIAN_POINT('Ctrl Pts',(2.11689212368568,-4.263829077783,3.70870784865043));
#69104=CARTESIAN_POINT('Ctrl Pts',(3.17174063018436,-3.22706463608245,3.76104067976445));
#69105=CARTESIAN_POINT('Ctrl Pts',(4.22658913668306,-2.19030019438189,3.81337351087847));
#69106=CARTESIAN_POINT('Ctrl Pts',(4.72413712536563,-0.586514358373886,
3.86570634199248));
#69107=CARTESIAN_POINT('Ctrl Pts',(4.44131082922502,0.865241532073468,3.9180391731065));
#69108=CARTESIAN_POINT('Ctrl Pts',(4.15848453308441,2.31699742252081,3.97037200422052));
#69109=CARTESIAN_POINT('Ctrl Pts',(3.09528395212065,3.61672336740751,4.02270483533454));
#69110=CARTESIAN_POINT('Ctrl Pts',(1.7283910635404,4.18169213563993,4.07503766644856));
#69111=CARTESIAN_POINT('Ctrl Pts',(0.361498174960155,4.74666090387236,4.12737049756258));
#69112=CARTESIAN_POINT('Ctrl Pts',(-1.30908702123658,4.5768724954505,4.1797033286766));
#69113=CARTESIAN_POINT('Ctrl Pts',(-2.5343639474132,3.74845090259061,4.23203615979062));
#69114=CARTESIAN_POINT('Ctrl Pts',(-3.74701372251171,2.9285666488301,4.28382967236309));
#69115=CARTESIAN_POINT('Ctrl Pts',(-4.52348622608021,1.46355441369542,4.33562318493555));
#69116=CARTESIAN_POINT('Ctrl Pts',(-4.52478583629221,-0.000271302356462328,
4.38741669750802));
#69117=CARTESIAN_POINT('Origin',(0.,0.,4.));
#69118=CARTESIAN_POINT('',(-4.51292607061429,0.0029183530353194,5.38741669750802));
#69119=CARTESIAN_POINT('',(-4.51119223387812,-0.00146992377155156,5.11258330249198));
#69120=CARTESIAN_POINT('',(-4.51775,5.53264807684796E-16,4.));
#69121=CARTESIAN_POINT('Ctrl Pts',(-4.51119223387812,-0.00146992377155156,
5.11258330249198));
#69122=CARTESIAN_POINT('Ctrl Pts',(-4.50867979289825,0.840016500418339,
5.0830394639766));
#69123=CARTESIAN_POINT('Ctrl Pts',(-4.28245206788243,1.68275768437228,5.05349562546122));
#69124=CARTESIAN_POINT('Ctrl Pts',(-3.84112663548136,2.39157406650585,5.02395178694585));
#69125=CARTESIAN_POINT('Ctrl Pts',(-3.05937956127687,3.64714442841863,4.97161895583183));
#69126=CARTESIAN_POINT('Ctrl Pts',(-1.60271543685273,4.48249584288365,4.9192861247178));
#69127=CARTESIAN_POINT('Ctrl Pts',(-0.124224122626221,4.52310166740692,
4.86695329360379));
#69128=CARTESIAN_POINT('Ctrl Pts',(1.3542671916003,4.56370749193019,4.81462046248977));
#69129=CARTESIAN_POINT('Ctrl Pts',(2.85458569562921,3.80956772651169,4.76228763137575));
#69130=CARTESIAN_POINT('Ctrl Pts',(3.70406923227031,2.59879808520239,4.70995480026173));
#69131=CARTESIAN_POINT('Ctrl Pts',(4.5535527689114,1.3880284438931,4.65762196914771));
#69132=CARTESIAN_POINT('Ctrl Pts',(4.7522013381647,-0.279371073306991,4.60528913803369));
#69133=CARTESIAN_POINT('Ctrl Pts',(4.21095160570608,-1.65582816824236,4.55295630691967));
#69134=CARTESIAN_POINT('Ctrl Pts',(3.66970187324747,-3.03228526317774,4.50062347580565));
#69135=CARTESIAN_POINT('Ctrl Pts',(2.38855383907694,-4.11779993584839,4.44829064469163));
#69136=CARTESIAN_POINT('Ctrl Pts',(0.94190539721171,-4.42568577395046,4.39595781357761));
#69137=CARTESIAN_POINT('Ctrl Pts',(-0.50474304465354,-4.73357161205254,
4.34362498246359));
#69138=CARTESIAN_POINT('Ctrl Pts',(-2.11689189421349,-4.263828615586,4.29129215134958));
#69139=CARTESIAN_POINT('Ctrl Pts',(-3.17174028636843,-3.22706428627144,
4.23895932023556));
#69140=CARTESIAN_POINT('Ctrl Pts',(-4.02084104068784,-2.3925203076111,4.1968339809877));
#69141=CARTESIAN_POINT('Ctrl Pts',(-4.50884156719875,-1.19057750531243,
4.15470864173984));
#69142=CARTESIAN_POINT('Ctrl Pts',(-4.51939464917808,0.00373292266216647,
4.11258330249198));
#69143=CARTESIAN_POINT('Ctrl Pts',(-4.52478583629221,-0.000271302356462328,
4.38741669750802));
#69144=CARTESIAN_POINT('Ctrl Pts',(-4.52479936895005,-0.0155139130822968,
4.38795601604957));
#69145=CARTESIAN_POINT('Ctrl Pts',(-4.52472885144687,-0.030756395156677,
4.38849533459112));
#69146=CARTESIAN_POINT('Ctrl Pts',(-4.52457390104248,-0.0459980188636215,
4.38903465313267));
#69147=CARTESIAN_POINT('Ctrl Pts',(-4.50953827233865,-1.52497057016008,
4.44136748424669));
#69148=CARTESIAN_POINT('Ctrl Pts',(-3.69949835877446,-2.99586089545507,
4.49370031536071));
#69149=CARTESIAN_POINT('Ctrl Pts',(-2.45763251543912,-3.79920086127216,
4.54603314647473));
#69150=CARTESIAN_POINT('Ctrl Pts',(-1.21576667210378,-4.60254082708924,
4.59836597758875));
#69151=CARTESIAN_POINT('Ctrl Pts',(0.45792510100271,-4.73833043342844,4.65069880870277));
#69152=CARTESIAN_POINT('Ctrl Pts',(1.81304942226226,-4.14568891458885,4.70303163981679));
#69153=CARTESIAN_POINT('Ctrl Pts',(3.16817374352182,-3.55304739574926,4.75536447093081));
#69154=CARTESIAN_POINT('Ctrl Pts',(4.20473061293445,-2.23197475173087,4.80769730204483));
#69155=CARTESIAN_POINT('Ctrl Pts',(4.45798362215519,-0.774768940348221,
4.86003013315885));
#69156=CARTESIAN_POINT('Ctrl Pts',(4.71123663137592,0.682436871034428,4.91236296427287));
#69157=CARTESIAN_POINT('Ctrl Pts',(4.18118578040478,2.27577584978132,4.96469579538688));
#69158=CARTESIAN_POINT('Ctrl Pts',(3.10547744889356,3.29088049233953,5.0170286265009));
#69159=CARTESIAN_POINT('Ctrl Pts',(2.02976911738235,4.30598513489774,5.06936145761492));
#69160=CARTESIAN_POINT('Ctrl Pts',(0.408403305331062,4.74285544126724,5.12169428872895));
#69161=CARTESIAN_POINT('Ctrl Pts',(-1.03168688021991,4.40562220466712,5.17402711984297));
#69162=CARTESIAN_POINT('Ctrl Pts',(-2.47177706577088,4.068388968067,5.22635995095699));
#69163=CARTESIAN_POINT('Ctrl Pts',(-3.73059162482154,2.95705218849725,5.278692782071));
#69164=CARTESIAN_POINT('Ctrl Pts',(-4.2437455072054,1.56987562195304,5.33102561318502));
#69165=CARTESIAN_POINT('Ctrl Pts',(-4.42806131327582,1.07162631350615,5.34982264129268));
#69166=CARTESIAN_POINT('Ctrl Pts',(-4.51617798535533,0.537790377713164,
5.36861966940035));
#69167=CARTESIAN_POINT('Ctrl Pts',(-4.51292607061429,0.0029183530353194,
5.38741669750802));
#69168=CARTESIAN_POINT('Origin',(0.,0.,4.));
#69169=CARTESIAN_POINT('',(-4.51611343680291,-0.0038242599945422,6.38741669750802));
#69170=CARTESIAN_POINT('',(-4.52399690261043,-0.00167256832429505,6.11258330249198));
#69171=CARTESIAN_POINT('',(-4.51775,5.53264807684796E-16,4.));
#69172=CARTESIAN_POINT('Ctrl Pts',(-4.52399690261043,-0.00167256832429505,
6.11258330249198));
#69173=CARTESIAN_POINT('Ctrl Pts',(-4.5173342997898,1.3804594726294,6.06370311732738));
#69174=CARTESIAN_POINT('Ctrl Pts',(-3.83652995787924,2.76828008382611,6.01482293216279));
#69175=CARTESIAN_POINT('Ctrl Pts',(-2.73628551041168,3.60369570881218,5.96594274699819));
#69176=CARTESIAN_POINT('Ctrl Pts',(-1.55832542986843,4.49812081512447,5.91360991588417));
#69177=CARTESIAN_POINT('Ctrl Pts',(0.100421664862097,4.75934671033683,5.86127708477015));
#69178=CARTESIAN_POINT('Ctrl Pts',(1.49626342410919,4.27025463771519,5.80894425365613));
#69179=CARTESIAN_POINT('Ctrl Pts',(2.89210518335629,3.78116256509354,5.75661142254211));
#69180=CARTESIAN_POINT('Ctrl Pts',(4.02504160711995,2.54175252463788,5.7042785914281));
#69181=CARTESIAN_POINT('Ctrl Pts',(4.3871245717083,1.10770887619882,5.65194576031408));
#69182=CARTESIAN_POINT('Ctrl Pts',(4.74920753629665,-0.326334772240243,
5.59961292920006));
#69183=CARTESIAN_POINT('Ctrl Pts',(4.34043704170966,-1.95501202866272,5.54728009808604));
#69184=CARTESIAN_POINT('Ctrl Pts',(3.34408397951354,-3.04811133798521,5.49494726697202));
#69185=CARTESIAN_POINT('Ctrl Pts',(2.34773091731743,-4.14121064730769,5.442614435858));
#69186=CARTESIAN_POINT('Ctrl Pts',(0.763795287512193,-4.6987320095302,5.39028160474398));
#69187=CARTESIAN_POINT('Ctrl Pts',(-0.697571429950846,-4.47071294770401,
5.33794877362996));
#69188=CARTESIAN_POINT('Ctrl Pts',(-2.15893814741389,-4.24269388587781,
5.28561594251594));
#69189=CARTESIAN_POINT('Ctrl Pts',(-3.49773595253472,-3.22913440000291,
5.23328311140192));
#69190=CARTESIAN_POINT('Ctrl Pts',(-4.11371984310272,-1.88446000238519,
5.1809502802879));
#69191=CARTESIAN_POINT('Ctrl Pts',(-4.3819578119688,-1.29890454431857,5.15816128768926));
#69192=CARTESIAN_POINT('Ctrl Pts',(-4.51313023522704,-0.650560524599824,
5.13537229509062));
#69193=CARTESIAN_POINT('Ctrl Pts',(-4.51119223387812,-0.00146992377155156,
5.11258330249198));
#69194=CARTESIAN_POINT('Ctrl Pts',(-4.51292607061429,0.0029183530353194,
5.38741669750802));
#69195=CARTESIAN_POINT('Ctrl Pts',(-4.50712432517217,-0.95134754210846,
5.42095250051437));
#69196=CARTESIAN_POINT('Ctrl Pts',(-4.21049476107502,-1.90891132639337,
5.45448830352073));
#69197=CARTESIAN_POINT('Ctrl Pts',(-3.65046921487666,-2.67356650591896,
5.48802410652708));
#69198=CARTESIAN_POINT('Ctrl Pts',(-2.776545834447,-3.86681571372806,5.5403569376411));
#69199=CARTESIAN_POINT('Ctrl Pts',(-1.26120586787061,-4.5902977758276,5.59268976875511));
#69200=CARTESIAN_POINT('Ctrl Pts',(0.216154764597121,-4.51964187827841,
5.64502259986913));
#69201=CARTESIAN_POINT('Ctrl Pts',(1.69351539706486,-4.44898598072923,5.69735543098315));
#69202=CARTESIAN_POINT('Ctrl Pts',(3.13289669542393,-3.58419212353131,5.74968826209718));
#69203=CARTESIAN_POINT('Ctrl Pts',(3.88895546769304,-2.31298805942388,5.8020210932112));
#69204=CARTESIAN_POINT('Ctrl Pts',(4.64501423996215,-1.04178399531645,5.85435392432522));
#69205=CARTESIAN_POINT('Ctrl Pts',(4.71775048614129,0.635830275700497,5.90668675543923));
#69206=CARTESIAN_POINT('Ctrl Pts',(4.07455703922814,1.96770402713248,5.95901958655325));
#69207=CARTESIAN_POINT('Ctrl Pts',(3.43136359231499,3.29957777856446,6.01135241766727));
#69208=CARTESIAN_POINT('Ctrl Pts',(2.07224045230956,4.28571101041149,6.0636852487813));
#69209=CARTESIAN_POINT('Ctrl Pts',(0.606537960019231,4.4839720817303,6.11601807989532));
#69210=CARTESIAN_POINT('Ctrl Pts',(-0.859164532271093,4.68223315304911,
6.16835091100933));
#69211=CARTESIAN_POINT('Ctrl Pts',(-2.43144637684631,4.0926220638397,6.22068374212335));
#69212=CARTESIAN_POINT('Ctrl Pts',(-3.4053667262744,2.97949356381203,6.27301657323736));
#69213=CARTESIAN_POINT('Ctrl Pts',(-4.11503346658856,2.16838999191388,6.31114994799425));
#69214=CARTESIAN_POINT('Ctrl Pts',(-4.506994027605,1.07931947572563,6.34928332275114));
#69215=CARTESIAN_POINT('Ctrl Pts',(-4.51611343680291,-0.0038242599945422,
6.38741669750802));
#69216=CARTESIAN_POINT('Origin',(0.,0.,4.));
#69217=CARTESIAN_POINT('',(-4.52286359173795,0.00246468782935438,7.38741669750802));
#69218=CARTESIAN_POINT('',(-4.51483246697105,0.00361950456559231,7.11258330249198));
#69219=CARTESIAN_POINT('',(-4.51775,5.53264807684796E-16,4.));
#69220=CARTESIAN_POINT('',(3.43378788736184,2.93584158413003,8.));
#69221=CARTESIAN_POINT('Ctrl Pts',(-4.52286359173795,0.00246468782935438,
7.38741669750802));
#69222=CARTESIAN_POINT('Ctrl Pts',(-4.514736621556,-1.33289820095304,7.43461263832996));
#69223=CARTESIAN_POINT('Ctrl Pts',(-3.88687106704568,-2.67555385687553,
7.48180857915189));
#69224=CARTESIAN_POINT('Ctrl Pts',(-2.85003294005483,-3.51527175392636,
7.52900451997383));
#69225=CARTESIAN_POINT('Ctrl Pts',(-1.70034350389957,-4.44638604308903,
7.58133735108785));
#69226=CARTESIAN_POINT('Ctrl Pts',(-0.0478099810187527,-4.759123220785,
7.63367018220187));
#69227=CARTESIAN_POINT('Ctrl Pts',(1.3612375474742,-4.31520832020808,7.68600301331589));
#69228=CARTESIAN_POINT('Ctrl Pts',(2.77028507596716,-3.87129341963115,7.73833584442991));
#69229=CARTESIAN_POINT('Ctrl Pts',(3.93584661007225,-2.67072644078133,7.79066867554392));
#69230=CARTESIAN_POINT('Ctrl Pts',(4.34789968202776,-1.24589357093064,7.84300150665794));
#69231=CARTESIAN_POINT('Ctrl Pts',(4.55392621800552,-0.533477136005289,
7.86916792221495));
#69232=CARTESIAN_POINT('Ctrl Pts',(4.57157563844588,0.235005771670285,7.89533433777196));
#69233=CARTESIAN_POINT('Ctrl Pts',(4.41221033788124,0.961199526155991,7.92150075332897));
#69234=CARTESIAN_POINT('Ctrl Pts',(4.2528450373166,1.6873932806417,7.94766716888598));
#69235=CARTESIAN_POINT('Ctrl Pts',(3.91646501574697,2.37129788193754,7.97383358444299));
#69236=CARTESIAN_POINT('Ctrl Pts',(3.43378788736183,2.93584158413004,8.));
#69237=CARTESIAN_POINT('',(-3.44054916109511,2.9381068161154,8.));
#69238=CARTESIAN_POINT('Origin',(0.,0.,8.));
#69239=CARTESIAN_POINT('Ctrl Pts',(-3.44054916109511,2.9381068161154,8.));
#69240=CARTESIAN_POINT('Ctrl Pts',(-2.51857342159112,4.00873681403696,7.94997488903429));
#69241=CARTESIAN_POINT('Ctrl Pts',(-1.04980743191293,4.62287257548397,7.89994977806859));
#69242=CARTESIAN_POINT('Ctrl Pts',(0.359975956906261,4.51112341871505,7.84992466710289));
#69243=CARTESIAN_POINT('Ctrl Pts',(1.83479439449057,4.39421913533762,7.79759183598887));
#69244=CARTESIAN_POINT('Ctrl Pts',(3.24506283044465,3.48291324925361,7.74525900487485));
#69245=CARTESIAN_POINT('Ctrl Pts',(3.96016560277148,2.18804756351099,7.69292617376083));
#69246=CARTESIAN_POINT('Ctrl Pts',(4.67526837509831,0.893181877768381,7.64059334264681));
#69247=CARTESIAN_POINT('Ctrl Pts',(4.69520548379788,-0.785243607632836,
7.58826051153279));
#69248=CARTESIAN_POINT('Ctrl Pts',(4.01017546547555,-2.09587300826054,7.53592768041877));
#69249=CARTESIAN_POINT('Ctrl Pts',(3.32514544715321,-3.40650240888826,7.48359484930475));
#69250=CARTESIAN_POINT('Ctrl Pts',(1.93514830180898,-4.34933572474246,7.43126201819073));
#69251=CARTESIAN_POINT('Ctrl Pts',(0.463832634566904,-4.50105475907159,
7.37892918707671));
#69252=CARTESIAN_POINT('Ctrl Pts',(-1.00748303267517,-4.65277379340072,
7.32659635596269));
#69253=CARTESIAN_POINT('Ctrl Pts',(-2.56011722181508,-4.01337854620477,
7.27426352484867));
#69254=CARTESIAN_POINT('Ctrl Pts',(-3.49818593160913,-2.86985320272758,
7.22193069373465));
#69255=CARTESIAN_POINT('Ctrl Pts',(-4.15153848320893,-2.0734028007694,7.18548156332043));
#69256=CARTESIAN_POINT('Ctrl Pts',(-4.50676902168756,-1.0324019249735,7.14903243290621));
#69257=CARTESIAN_POINT('Ctrl Pts',(-4.51483246697105,0.00361950456559231,
7.11258330249198));
#69258=CARTESIAN_POINT('Origin',(0.,0.,10.2083368446371));
#69259=CARTESIAN_POINT('',(-5.0799445016814,0.00237344505285342,0.791663155362921));
#69260=CARTESIAN_POINT('',(-5.06551066928822,-0.000578487979983568,0.708336844637072));
#69261=CARTESIAN_POINT('',(-5.0736,1.10600941455115E-13,10.2083368446371));
#69262=CARTESIAN_POINT('',(1.31303618635654,-4.9007502418832,0.));
#69263=CARTESIAN_POINT('Ctrl Pts',(-5.06551066928822,-0.000578487979984235,
0.708336844637072));
#69264=CARTESIAN_POINT('Ctrl Pts',(-5.06491070355288,0.856117806205452,
0.681555887547458));
#69265=CARTESIAN_POINT('Ctrl Pts',(-4.45481520994778,3.38770743142078,0.602442099343825));
#69266=CARTESIAN_POINT('Ctrl Pts',(-0.476761969141785,5.95830217192949,
0.470995480026171));
#69267=CARTESIAN_POINT('Ctrl Pts',(4.70955374493753,3.67573393888292,0.313996986684114));
#69268=CARTESIAN_POINT('Ctrl Pts',(5.49957691269067,-0.955274817987675,
0.183164908899066));
#69269=CARTESIAN_POINT('Ctrl Pts',(3.61105296193539,-3.84612671226304,0.0784992466710263));
#69270=CARTESIAN_POINT('Ctrl Pts',(2.11876087752236,-4.68487601374969,0.0261664155570096));
#69271=CARTESIAN_POINT('Ctrl Pts',(1.31303618635654,-4.90075024188321,0.));
#69272=CARTESIAN_POINT('',(-1.31785621200034,-4.9071451662202,1.75207071073658E-15));
#69273=CARTESIAN_POINT('Origin',(0.,0.,0.));
#69274=CARTESIAN_POINT('Ctrl Pts',(-5.0799445016814,0.00237344505285278,
0.791663155362921));
#69275=CARTESIAN_POINT('Ctrl Pts',(-5.08079896874729,0.146309621287887,
0.787131872330397));
#69276=CARTESIAN_POINT('Ctrl Pts',(-5.01057089916491,1.95175929947146,0.730267758183854));
#69277=CARTESIAN_POINT('Ctrl Pts',(-2.85914249825567,5.24623219278067,0.621070812923292));
#69278=CARTESIAN_POINT('Ctrl Pts',(2.79949684465664,5.27806149196883,0.464072319581235));
#69279=CARTESIAN_POINT('Ctrl Pts',(5.94469888877439,0.578168532022547,0.307073826239177));
#69280=CARTESIAN_POINT('Ctrl Pts',(3.79743415440745,-4.56550609975241,0.152383053045432));
#69281=CARTESIAN_POINT('Ctrl Pts',(0.216274136307286,-5.31234397836678,
0.0500251109657079));
#69282=CARTESIAN_POINT('Ctrl Pts',(-1.31785621200034,-4.9071451662202,1.74231289118421E-15));
#69283=CARTESIAN_POINT('Origin',(0.,0.,10.2083368446371));
#69284=CARTESIAN_POINT('',(-5.06594495534805,0.00113798286105304,1.79166315536292));
#69285=CARTESIAN_POINT('',(-5.0788676065064,-0.0031096904011537,1.70833684463707));
#69286=CARTESIAN_POINT('',(-5.0736,1.10600941455115E-13,10.2083368446371));
#69287=CARTESIAN_POINT('Ctrl Pts',(-5.0788676065064,-0.00310969040115398,
1.70833684463707));
#69288=CARTESIAN_POINT('Ctrl Pts',(-5.06820560204524,1.46267013662722,1.66221954089824));
#69289=CARTESIAN_POINT('Ctrl Pts',(-3.63653147921883,4.60995381904077,1.56376940604539));
#69290=CARTESIAN_POINT('Ctrl Pts',(1.67938795492248,5.73354207176578,1.41298644007852));
#69291=CARTESIAN_POINT('Ctrl Pts',(5.70869045070874,1.76202618095205,1.25598794673646));
#69292=CARTESIAN_POINT('Ctrl Pts',(4.61877209773216,-3.78910839602635,1.0989894533944));
#69293=CARTESIAN_POINT('Ctrl Pts',(-0.612224753988487,-5.94330155793046,
0.941990960052346));
#69294=CARTESIAN_POINT('Ctrl Pts',(-4.49644008704084,-3.30864398166895,
0.811773423799902));
#69295=CARTESIAN_POINT('Ctrl Pts',(-5.06608310024492,-0.817957632158887,
0.733888718661477));
#69296=CARTESIAN_POINT('Ctrl Pts',(-5.06551066928822,-0.000578487979984235,
0.708336844637072));
#69297=CARTESIAN_POINT('Ctrl Pts',(-5.06594495534805,0.00113798286105242,
1.79166315536292));
#69298=CARTESIAN_POINT('Ctrl Pts',(-5.06751102530523,0.764702257078156,
1.76779552568118));
#69299=CARTESIAN_POINT('Ctrl Pts',(-4.54967353500429,3.20046203254748,1.69159506488542));
#69300=CARTESIAN_POINT('Ctrl Pts',(-0.800856996403053,5.92047503909791,
1.56306177297564));
#69301=CARTESIAN_POINT('Ctrl Pts',(4.49633411524324,3.93401017093414,1.40606327963358));
#69302=CARTESIAN_POINT('Ctrl Pts',(5.76163326143087,-1.58003046734643,1.24906478629152));
#69303=CARTESIAN_POINT('Ctrl Pts',(1.86064021890344,-5.67731097226746,1.09206629294947));
#69304=CARTESIAN_POINT('Ctrl Pts',(-3.54825609197855,-4.71238753324782,
0.939599082639932));
#69305=CARTESIAN_POINT('Ctrl Pts',(-5.07093053185417,-1.51604242073639,
0.839464703444417));
#69306=CARTESIAN_POINT('Ctrl Pts',(-5.0799445016814,0.00237344505285278,
0.791663155362921));
#69307=CARTESIAN_POINT('Origin',(0.,0.,10.2083368446371));
#69308=CARTESIAN_POINT('',(-5.07643096335186,-0.00399326016102722,2.79166315536292));
#69309=CARTESIAN_POINT('',(-5.07274549324388,0.00436695056987321,2.70833684463708));
#69310=CARTESIAN_POINT('',(-5.0736,1.10600941455115E-13,10.2083368446371));
#69311=CARTESIAN_POINT('Ctrl Pts',(-5.07274549324388,0.00436695056987284,
2.70833684463708));
#69312=CARTESIAN_POINT('Ctrl Pts',(-5.07638654156454,0.422701167110148,
2.69521602536304));
#69313=CARTESIAN_POINT('Ctrl Pts',(-4.83926758888069,2.50550600890858,2.62976237497499));
#69314=CARTESIAN_POINT('Ctrl Pts',(-1.97561166336026,5.63828895889383,2.51197589347292));
#69315=CARTESIAN_POINT('Ctrl Pts',(3.6128915810316,4.75818989009414,2.35497740013087));
#69316=CARTESIAN_POINT('Ctrl Pts',(5.96174508817349,-0.388546134793637,
2.19797890678881));
#69317=CARTESIAN_POINT('Ctrl Pts',(2.96474106500057,-5.18686823314646,2.04098041344675));
#69318=CARTESIAN_POINT('Ctrl Pts',(-2.69071315072611,-5.33417912211988,
1.88398192010469));
#69319=CARTESIAN_POINT('Ctrl Pts',(-4.98091385691211,-2.06009093973243,
1.77310073050147));
#69320=CARTESIAN_POINT('Ctrl Pts',(-5.08030459382418,-0.200662320374615,
1.71455237201226));
#69321=CARTESIAN_POINT('Ctrl Pts',(-5.0788676065064,-0.00310969040115398,
1.70833684463707));
#69322=CARTESIAN_POINT('Ctrl Pts',(-5.07643096335186,-0.00399326016102722,
2.79166315536292));
#69323=CARTESIAN_POINT('Ctrl Pts',(-5.06457082001664,1.37091447103077,2.74845917903196));
#69324=CARTESIAN_POINT('Ctrl Pts',(-3.7827320999117,4.43074150154599,2.65292237158698));
#69325=CARTESIAN_POINT('Ctrl Pts',(1.36220151697138,5.81702256793933,2.50505273302799));
#69326=CARTESIAN_POINT('Ctrl Pts',(5.60328669734595,2.07280630409542,2.34805423968593));
#69327=CARTESIAN_POINT('Ctrl Pts',(4.81994564291905,-3.53007932713903,2.19105574634387));
#69328=CARTESIAN_POINT('Ctrl Pts',(-0.285401937658034,-5.96757024490932,
2.03405725300181));
#69329=CARTESIAN_POINT('Ctrl Pts',(-4.39760317314566,-3.49692096558582,
1.90092638934149));
#69330=CARTESIAN_POINT('Ctrl Pts',(-5.0640772165997,-0.90951008575328,1.8201283567952));
#69331=CARTESIAN_POINT('Ctrl Pts',(-5.06594495534805,0.00113798286105242,
1.79166315536292));
#69332=CARTESIAN_POINT('Origin',(0.,0.,10.2083368446371));
#69333=CARTESIAN_POINT('',(-5.07544700173093,0.00419220993169878,3.79166315536292));
#69334=CARTESIAN_POINT('',(-5.06752990436066,-0.00289155559083432,3.70833684463708));
#69335=CARTESIAN_POINT('',(-5.0736,1.10600941455115E-13,10.2083368446371));
#69336=CARTESIAN_POINT('Ctrl Pts',(-5.06752990436066,-0.00289155559083445,
3.70833684463708));
#69337=CARTESIAN_POINT('Ctrl Pts',(-5.06201314247005,1.03465176096834,3.67587967871383));
#69338=CARTESIAN_POINT('Ctrl Pts',(-4.25079971500112,3.75301601020252,3.59108968167655));
#69339=CARTESIAN_POINT('Ctrl Pts',(0.164021032340792,5.97213939901987,3.45396685352527));
#69340=CARTESIAN_POINT('Ctrl Pts',(5.07168429591276,3.15774768001703,3.29696836018321));
#69341=CARTESIAN_POINT('Ctrl Pts',(5.43160651478565,-2.48817267483047,3.13996986684115));
#69342=CARTESIAN_POINT('Ctrl Pts',(0.921047975843499,-5.90296718493849,
2.9829713734991));
#69343=CARTESIAN_POINT('Ctrl Pts',(-3.96942410407231,-4.18159504957827,
2.83909369943107));
#69344=CARTESIAN_POINT('Ctrl Pts',(-5.06186409728241,-1.24583899384963,
2.74754885647706));
#69345=CARTESIAN_POINT('Ctrl Pts',(-5.07274549324388,0.00436695056987284,
2.70833684463708));
#69346=CARTESIAN_POINT('Ctrl Pts',(-5.07544700173093,0.00419220993169878,
3.79166315536292));
#69347=CARTESIAN_POINT('Ctrl Pts',(-5.07831876722643,0.329194847520769,
3.78145566349676));
#69348=CARTESIAN_POINT('Ctrl Pts',(-4.90302280847942,2.31737130051307,3.71891534051658));
#69349=CARTESIAN_POINT('Ctrl Pts',(-2.2821043825461,5.52135344516299,3.60404218642239));
#69350=CARTESIAN_POINT('Ctrl Pts',(3.34628151701835,4.94931755856517,3.44704369308033));
#69351=CARTESIAN_POINT('Ctrl Pts',(5.9740820006751,-0.0607341045204584,
3.29004519973827));
#69352=CARTESIAN_POINT('Ctrl Pts',(3.24496813195078,-5.01632594473331,3.13304670639622));
#69353=CARTESIAN_POINT('Ctrl Pts',(-2.39388416789017,-5.47381611497205,
2.97604821305415));
#69354=CARTESIAN_POINT('Ctrl Pts',(-4.9251294092353,-2.24779066275208,2.86225369604306));
#69355=CARTESIAN_POINT('Ctrl Pts',(-5.0789369717198,-0.294506636106011,
2.80079201014598));
#69356=CARTESIAN_POINT('Ctrl Pts',(-5.07643096335186,-0.00399326016102722,
2.79166315536292));
#69357=CARTESIAN_POINT('Origin',(0.,0.,10.2083368446371));
#69358=CARTESIAN_POINT('',(-5.06623538659821,-0.00165077865025204,4.79166315536292));
#69359=CARTESIAN_POINT('',(-5.08150150384863,-0.000304682560140652,4.70833684463708));
#69360=CARTESIAN_POINT('',(-5.0736,1.10600941455115E-13,10.2083368446371));
#69361=CARTESIAN_POINT('Ctrl Pts',(-5.08150150384863,-0.000304682560140828,
4.70833684463708));
#69362=CARTESIAN_POINT('Ctrl Pts',(-5.08004199361202,1.64362562632391,4.65654333206461));
#69363=CARTESIAN_POINT('Ctrl Pts',(-3.32694734261784,4.95128314317388,4.55241698837811));
#69364=CARTESIAN_POINT('Ctrl Pts',(2.28210462993784,5.52135404368456,4.39595781357762));
#69365=CARTESIAN_POINT('Ctrl Pts',(5.86414511529741,1.14243341683897,4.23895932023555));
#69366=CARTESIAN_POINT('Ctrl Pts',(4.18785084798745,-4.2608986517151,4.0819608268935));
#69367=CARTESIAN_POINT('Ctrl Pts',(-1.24365772802729,-5.8435149929827,3.92496233355144));
#69368=CARTESIAN_POINT('Ctrl Pts',(-4.66764902476596,-2.94237266391977,
3.80042100613263));
#69369=CARTESIAN_POINT('Ctrl Pts',(-5.07090818182747,-0.638247816504467,
3.72821250982785));
#69370=CARTESIAN_POINT('Ctrl Pts',(-5.06752990436066,-0.00289155559083445,
3.70833684463708));
#69371=CARTESIAN_POINT('Ctrl Pts',(-5.06623538659821,-0.00165077865025218,
4.79166315536292));
#69372=CARTESIAN_POINT('Ctrl Pts',(-5.06341382264369,0.943369534950495,
4.76211931684755));
#69373=CARTESIAN_POINT('Ctrl Pts',(-4.35931582912874,3.56626810599387,4.68024264721815));
#69374=CARTESIAN_POINT('Ctrl Pts',(-0.164021014606317,5.97213875156532,
4.54603314647473));
#69375=CARTESIAN_POINT('Ctrl Pts',(4.89071815558305,3.43135837605058,4.38903465313268));
#69376=CARTESIAN_POINT('Ctrl Pts',(5.55998718173337,-2.18629522837624,4.23203615979062));
#69377=CARTESIAN_POINT('Ctrl Pts',(1.24365759322077,-5.84351435953346,4.07503766644856));
#69378=CARTESIAN_POINT('Ctrl Pts',(-3.83471277836695,-4.36379434722342,
3.92824666497267));
#69379=CARTESIAN_POINT('Ctrl Pts',(-5.06359550115425,-1.33706248264138,
3.83378849461079));
#69380=CARTESIAN_POINT('Ctrl Pts',(-5.07544700173093,0.00419220993169878,
3.79166315536292));
#69381=CARTESIAN_POINT('Origin',(0.,0.,10.2083368446371));
#69382=CARTESIAN_POINT('',(-5.08061550220448,-0.00187835596255306,5.79166315536292));
#69383=CARTESIAN_POINT('',(-5.06818254924878,0.00327741817492065,5.70833684463708));
#69384=CARTESIAN_POINT('',(-5.0736,1.10600941455115E-13,10.2083368446371));
#69385=CARTESIAN_POINT('Ctrl Pts',(-5.06818254924878,0.00327741817492046,
5.70833684463708));
#69386=CARTESIAN_POINT('Ctrl Pts',(-5.07183456953104,0.603958443996534,
5.68953981652941));
#69387=CARTESIAN_POINT('Ctrl Pts',(-4.69736642816282,2.87259326592426,5.61840995730772));
#69388=CARTESIAN_POINT('Ctrl Pts',(-1.36220166545199,5.81702319809857,5.49494726697201));
#69389=CARTESIAN_POINT('Ctrl Pts',(4.10035928902097,4.34515876133492,5.33794877362997));
#69390=CARTESIAN_POINT('Ctrl Pts',(5.88615929841981,-1.02297668832719,5.1809502802879));
#69391=CARTESIAN_POINT('Ctrl Pts',(2.3938844275315,-5.47381670826519,5.02395178694585));
#69392=CARTESIAN_POINT('Ctrl Pts',(-3.24496848378481,-5.01632648853908,
4.86695329360378));
#69393=CARTESIAN_POINT('Ctrl Pts',(-5.07375293308448,-1.69557487064781,
4.7617483128342));
#69394=CARTESIAN_POINT('Ctrl Pts',(-5.08151670152288,-0.0174226970094883,
4.70887616317863));
#69395=CARTESIAN_POINT('Ctrl Pts',(-5.08150150384863,-0.000304682560140828,
4.70833684463708));
#69396=CARTESIAN_POINT('Ctrl Pts',(-5.08061550220448,-0.00187835596255308,
5.79166315536293));
#69397=CARTESIAN_POINT('Ctrl Pts',(-5.07313315332044,1.5503069404754,5.74278297019833));
#69398=CARTESIAN_POINT('Ctrl Pts',(-3.48999114796195,4.77754415127511,5.64156995391971));
#69399=CARTESIAN_POINT('Ctrl Pts',(1.97561144788205,5.63828834519714,5.48802410652708));
#69400=CARTESIAN_POINT('Ctrl Pts',(5.79259970947732,1.46257867915377,5.33102561318502));
#69401=CARTESIAN_POINT('Ctrl Pts',(4.41540665009831,-4.0246153410012,5.17402711984296));
#69402=CARTESIAN_POINT('Ctrl Pts',(-0.92104787574744,-5.90296654461282,
5.01702862650091));
#69403=CARTESIAN_POINT('Ctrl Pts',(-4.58281307585404,-3.13076536575022,
4.88957397167423));
#69404=CARTESIAN_POINT('Ctrl Pts',(-5.0684118336446,-0.730603481292581,
4.81445214796157));
#69405=CARTESIAN_POINT('Ctrl Pts',(-5.06623538659821,-0.00165077865025218,
4.79166315536292));
#69406=CARTESIAN_POINT('Origin',(0.,0.,10.2083368446371));
#69407=CARTESIAN_POINT('',(-5.07032350272244,0.00406483722298734,6.79166315536293));
#69408=CARTESIAN_POINT('',(-5.07176207912418,-0.00429478512726797,6.70833684463708));
#69409=CARTESIAN_POINT('',(-5.0736,1.10600941455115E-13,10.2083368446371));
#69410=CARTESIAN_POINT('Ctrl Pts',(-5.07176207912418,-0.00429478512726802,
6.70833684463708));
#69411=CARTESIAN_POINT('Ctrl Pts',(-5.06152064599786,1.21211560888524,6.67020346988019));
#69412=CARTESIAN_POINT('Ctrl Pts',(-4.01723926286446,4.11367300543969,6.57973726400929));
#69413=CARTESIAN_POINT('Ctrl Pts',(0.800857062853464,5.92047566764934,6.43693822702436));
#69414=CARTESIAN_POINT('Ctrl Pts',(5.37989341709942,2.59808361512381,6.27993973368231));
#69415=CARTESIAN_POINT('Ctrl Pts',(5.13483694964473,-3.0539846259906,6.12294124034024));
#69416=CARTESIAN_POINT('Ctrl Pts',(0.285401972927619,-5.96757088942664,
5.96594274699819));
#69417=CARTESIAN_POINT('Ctrl Pts',(-4.20869589117159,-3.8219142963774,5.8277412817638));
#69418=CARTESIAN_POINT('Ctrl Pts',(-5.06166697497504,-1.0683984039935,5.74187264764343));
#69419=CARTESIAN_POINT('Ctrl Pts',(-5.06818254924878,0.00327741817492046,
5.70833684463708));
#69420=CARTESIAN_POINT('Ctrl Pts',(-5.07032350272244,0.00406483722298713,
6.79166315536293));
#69421=CARTESIAN_POINT('Ctrl Pts',(-5.07426970367213,0.511087407033013,
6.77577945466313));
#69422=CARTESIAN_POINT('Ctrl Pts',(-4.77323782375589,2.68406204063008,6.70756292284932));
#69423=CARTESIAN_POINT('Ctrl Pts',(-1.67938775292856,5.73354154736347,6.58701355992148));
#69424=CARTESIAN_POINT('Ctrl Pts',(3.85566217988192,4.56363706615652,6.43001506657943));
#69425=CARTESIAN_POINT('Ctrl Pts',(5.93344523009267,-0.69834389981148,6.27301657323736));
#69426=CARTESIAN_POINT('Ctrl Pts',(2.69071284975304,-5.33417856632519,6.11601807989532));
#69427=CARTESIAN_POINT('Ctrl Pts',(-2.96474073765194,-5.18686765769478,
5.95901958655325));
#69428=CARTESIAN_POINT('Ctrl Pts',(-5.0286520759667,-1.88246391579033,5.85090127837579));
#69429=CARTESIAN_POINT('Ctrl Pts',(-5.08114401701022,-0.111516776080137,
5.79511580131235));
#69430=CARTESIAN_POINT('Ctrl Pts',(-5.08061550220448,-0.00187835596255308,
5.79166315536293));
#69431=CARTESIAN_POINT('Origin',(0.,0.,10.2083368446371));
#69432=CARTESIAN_POINT('',(-5.0667809979009,-0.000656412822606089,7.79166315536293));
#69433=CARTESIAN_POINT('',(-5.07934275226421,0.00276793540382957,7.70833684463708));
#69434=CARTESIAN_POINT('',(-5.0736,1.10600941455115E-13,10.2083368446371));
#69435=CARTESIAN_POINT('',(-1.31303618635646,-4.90075024188322,8.));
#69436=CARTESIAN_POINT('Ctrl Pts',(-1.31303618635644,-4.90075024188323,
8.));
#69437=CARTESIAN_POINT('Ctrl Pts',(-2.11876087752226,-4.68487601374973,
7.97383358444299));
#69438=CARTESIAN_POINT('Ctrl Pts',(-3.61103600209076,-3.84612122823184,
7.92150075332897));
#69439=CARTESIAN_POINT('Ctrl Pts',(-4.8640953672922,-1.92805050100101,7.85205513844995));
#69440=CARTESIAN_POINT('Ctrl Pts',(-5.07037793642002,-0.54712311490011,
7.80877593912793));
#69441=CARTESIAN_POINT('Ctrl Pts',(-5.0667809979009,-0.000656412822605951,
7.79166315536293));
#69442=CARTESIAN_POINT('',(1.31785785677863,-4.90714579947409,8.00000000000001));
#69443=CARTESIAN_POINT('Origin',(0.,0.,8.));
#69444=CARTESIAN_POINT('Ctrl Pts',(1.31785785677863,-4.90714579947409,8.00000000000001));
#69445=CARTESIAN_POINT('Ctrl Pts',(-0.216269591468087,-5.31234554625424,
7.9499748890343));
#69446=CARTESIAN_POINT('Ctrl Pts',(-3.61771514871704,-4.60298607712906,
7.85275383724664));
#69447=CARTESIAN_POINT('Ctrl Pts',(-5.07021586478366,-1.49689387689792,
7.75553278545901));
#69448=CARTESIAN_POINT('Ctrl Pts',(-5.07934275226421,0.00276793540382986,
7.70833684463708));
#69449=CARTESIAN_POINT('Origin',(0.,0.,10.2083368446371));
#69450=CARTESIAN_POINT('Ctrl Pts',(-5.07934275226421,0.00276793540383012,
7.70833684463708));
#69451=CARTESIAN_POINT('Ctrl Pts',(-5.08033613895975,0.165993799129837,
7.70319995434499));
#69452=CARTESIAN_POINT('Ctrl Pts',(-4.99920696262547,1.99102187228673,7.64573023293889));
#69453=CARTESIAN_POINT('Ctrl Pts',(-2.799497488489,5.27806255262917,7.53592768041876));
#69454=CARTESIAN_POINT('Ctrl Pts',(2.8591428156985,5.24623244979999,7.37892918707671));
#69455=CARTESIAN_POINT('Ctrl Pts',(5.95237094349663,0.509586379962791,7.22193069373465));
#69456=CARTESIAN_POINT('Ctrl Pts',(3.70900729550924,-4.68371090122276,7.06493220039259));
#69457=CARTESIAN_POINT('Ctrl Pts',(-1.86064034918539,-5.67731151891722,
6.90793370705054));
#69458=CARTESIAN_POINT('Ctrl Pts',(-4.81412133745352,-2.5752195014975,6.78906858846536));
#69459=CARTESIAN_POINT('Ctrl Pts',(-5.07557560949328,-0.457240961862529,
6.72253630099421));
#69460=CARTESIAN_POINT('Ctrl Pts',(-5.07176207912418,-0.00429478512726802,
6.70833684463708));
#69461=CARTESIAN_POINT('Ctrl Pts',(-5.0667809979009,-0.000656412822605951,
7.79166315536293));
#69462=CARTESIAN_POINT('Ctrl Pts',(-5.05937809100424,1.12403395819613,7.75644310801391));
#69463=CARTESIAN_POINT('Ctrl Pts',(-4.14423912611421,3.92453560182124,7.66889022955088));
#69464=CARTESIAN_POINT('Ctrl Pts',(0.476758320675261,5.95830042580594,7.52900451997384));
#69465=CARTESIAN_POINT('Ctrl Pts',(5.22810884028568,2.88800998678043,7.37200602663177));
#69466=CARTESIAN_POINT('Ctrl Pts',(5.29527916712856,-2.76679132542031,7.21500753328971));
#69467=CARTESIAN_POINT('Ctrl Pts',(0.612224870220684,-5.9433011663707,7.05800903994766));
#69468=CARTESIAN_POINT('Ctrl Pts',(-4.08954628424525,-4.00704976176015,
6.91689424730539));
#69469=CARTESIAN_POINT('Ctrl Pts',(-5.0612679560476,-1.15942546766541,6.82811228577715));
#69470=CARTESIAN_POINT('Ctrl Pts',(-5.07032350272244,0.00406483722298713,
6.79166315536293));
#69471=CARTESIAN_POINT('Ctrl Pts',(3.43378788736183,2.93584158413004,8.));
#69472=CARTESIAN_POINT('Ctrl Pts',(3.91646501574697,2.37129788193754,7.97383358444299));
#69473=CARTESIAN_POINT('Ctrl Pts',(4.58922505888624,1.00348867934585,7.92150075332897));
#69474=CARTESIAN_POINT('Ctrl Pts',(4.5186273771248,-2.07044295135642,7.81683509110093));
#69475=CARTESIAN_POINT('Ctrl Pts',(1.60472354186206,-5.07186039848098,7.68600301331589));
#69476=CARTESIAN_POINT('Ctrl Pts',(-3.35287702678038,-4.13364886539305,
7.52900451997383));
#69477=CARTESIAN_POINT('Ctrl Pts',(-5.29341307506948,0.514825336495039,
7.37200602663177));
#69478=CARTESIAN_POINT('Ctrl Pts',(-2.49279205665034,4.69981218407846,7.21500753328972));
#69479=CARTESIAN_POINT('Ctrl Pts',(2.5459028018807,4.67146930189292,7.05800903994766));
#69480=CARTESIAN_POINT('Ctrl Pts',(5.3002451572812,0.453757463748993,6.90101054660559));
#69481=CARTESIAN_POINT('Ctrl Pts',(3.30265841006127,-4.17057610454098,6.74401205326355));
#69482=CARTESIAN_POINT('Ctrl Pts',(-1.6567935859217,-5.05532050508283,6.58701355992147));
#69483=CARTESIAN_POINT('Ctrl Pts',(-5.13040478426442,-1.40692675790748,
6.43001506657944));
#69484=CARTESIAN_POINT('Ctrl Pts',(-4.00372822142153,3.50301097463029,6.27301657323735));
#69485=CARTESIAN_POINT('Ctrl Pts',(0.713117312304132,5.27184424225852,6.11601807989532));
#69486=CARTESIAN_POINT('Ctrl Pts',(4.79048673232043,2.31344454671744,5.95901958655324));
#69487=CARTESIAN_POINT('Ctrl Pts',(4.57227799378301,-2.71939826633338,5.8020210932112));
#69488=CARTESIAN_POINT('Ctrl Pts',(0.254134098705802,-5.31377983792714,
5.64502259986913));
#69489=CARTESIAN_POINT('Ctrl Pts',(-4.2918858010234,-3.14333365162852,5.48802410652709));
#69490=CARTESIAN_POINT('Ctrl Pts',(-4.98940618387219,1.8457154089275,5.33102561318501));
#69491=CARTESIAN_POINT('Ctrl Pts',(-1.21296250672023,5.17972574763675,5.17402711984298));
#69492=CARTESIAN_POINT('Ctrl Pts',(3.65113492943364,3.86911482852823,5.0170286265009));
#69493=CARTESIAN_POINT('Ctrl Pts',(5.24128748234707,-0.910902107712505,
4.86003013315885));
#69494=CARTESIAN_POINT('Ctrl Pts',(2.13161687410921,-4.87412003976763,4.70303163981679));
#69495=CARTESIAN_POINT('Ctrl Pts',(-2.88945844521027,-4.46675122075005,
4.54603314647474));
#69496=CARTESIAN_POINT('Ctrl Pts',(-5.31957818590282,-0.0540802448651307,
4.38903465313267));
#69497=CARTESIAN_POINT('Ctrl Pts',(-2.97967221743332,4.40708408702865,4.23203615979062));
#69498=CARTESIAN_POINT('Ctrl Pts',(2.0320833711569,4.91644931229421,4.07503766644856));
#69499=CARTESIAN_POINT('Ctrl Pts',(5.22168511404818,1.01727147763408,3.9180391731065));
#69500=CARTESIAN_POINT('Ctrl Pts',(3.7290411480005,-3.79408603038985,3.76104067976445));
#69501=CARTESIAN_POINT('Ctrl Pts',(-1.10740592494388,-5.20331517256929,
3.60404218642238));
#69502=CARTESIAN_POINT('Ctrl Pts',(-4.95085044410053,-1.94677080151586,
3.44704369308033));
#69503=CARTESIAN_POINT('Ctrl Pts',(-4.35490467170682,3.05542829226346,3.29004519973827));
#69504=CARTESIAN_POINT('Ctrl Pts',(0.146051328220124,5.31784783386984,3.13304670639621));
#69505=CARTESIAN_POINT('Ctrl Pts',(4.51604417531138,2.81179331862917,2.97604821305416));
#69506=CARTESIAN_POINT('Ctrl Pts',(4.83653428180639,-2.21557515407508,2.8190497197121));
#69507=CARTESIAN_POINT('Ctrl Pts',(0.820140431422849,-5.25625394192603,
2.66205122637004));
#69508=CARTESIAN_POINT('Ctrl Pts',(-3.93166697371103,-3.58368967284698,
2.50505273302798));
#69509=CARTESIAN_POINT('Ctrl Pts',(-5.15797858932007,1.30234262409331,2.34805423968593));
#69510=CARTESIAN_POINT('Ctrl Pts',(-1.75916895146362,5.02057315201092,2.19105574634387));
#69511=CARTESIAN_POINT('Ctrl Pts',(3.21707287531645,4.23689537527058,2.03405725300181));
#69512=CARTESIAN_POINT('Ctrl Pts',(5.30859229582462,-0.345978063005356,
1.87705875965975));
#69513=CARTESIAN_POINT('Ctrl Pts',(2.63993199038283,-4.61860886950043,1.7200602663177));
#69514=CARTESIAN_POINT('Ctrl Pts',(-2.39592583898866,-4.74978077281557,
1.56306177297564));
#69515=CARTESIAN_POINT('Ctrl Pts',(-5.28339345476216,-0.621835317076693,
1.40606327963358));
#69516=CARTESIAN_POINT('Ctrl Pts',(-3.43324656738056,4.06365773166108,1.24906478629152));
#69517=CARTESIAN_POINT('Ctrl Pts',(1.4953987175479,5.10539058946701,1.09206629294947));
#69518=CARTESIAN_POINT('Ctrl Pts',(5.08326164531879,1.56898332130955,0.935067799607405));
#69519=CARTESIAN_POINT('Ctrl Pts',(4.1127518220848,-3.37398384897273,0.778069306265351));
#69520=CARTESIAN_POINT('Ctrl Pts',(-0.545151052966628,-5.29216938925817,
0.621070812923291));
#69521=CARTESIAN_POINT('Ctrl Pts',(-4.71514359968435,-2.4636695471729,0.464072319581234));
#69522=CARTESIAN_POINT('Ctrl Pts',(-4.65533046585126,2.57160754473359,0.307073826239176));
#69523=CARTESIAN_POINT('Ctrl Pts',(-0.424529207286798,5.30552657624457,
0.150075332897118));
#69524=CARTESIAN_POINT('Ctrl Pts',(4.1935876756527,3.27303039309136,-0.00692316044493899));
#69525=CARTESIAN_POINT('Ctrl Pts',(4.89705802532881,-0.850617472596149,
-0.137755238229987));
#69526=CARTESIAN_POINT('Ctrl Pts',(3.21543569039412,-3.42475539150235,-0.242420900458027));
#69527=CARTESIAN_POINT('Ctrl Pts',(1.88663512189109,-4.17161357046627,-0.294753731572044));
#69528=CARTESIAN_POINT('Ctrl Pts',(1.16918346556927,-4.36383719750628,-0.320920147129053));
#69529=CARTESIAN_POINT('Ctrl Pts',(3.574615437742,3.05624720968396,8.10697338237635));
#69530=CARTESIAN_POINT('Ctrl Pts',(4.0770882669231,2.46855026993857,8.08080696681934));
#69531=CARTESIAN_POINT('Ctrl Pts',(4.77743974901458,1.04464406144345,8.02847413570532));
#69532=CARTESIAN_POINT('Ctrl Pts',(4.7039466937149,-2.15535658568851,7.92380847347729));
#69533=CARTESIAN_POINT('Ctrl Pts',(1.67053695050899,-5.27986907555073,7.79297639569223));
#69534=CARTESIAN_POINT('Ctrl Pts',(-3.49038623640434,-4.30317932648753,
7.63597790235018));
#69535=CARTESIAN_POINT('Ctrl Pts',(-5.51050813771329,0.535939509353267,
7.47897940900812));
#69536=CARTESIAN_POINT('Ctrl Pts',(-2.59502720059656,4.8925623069287,7.32198091566607));
#69537=CARTESIAN_POINT('Ctrl Pts',(2.65031613981997,4.86305701786194,7.16498242232401));
#69538=CARTESIAN_POINT('Ctrl Pts',(5.51762041935301,0.472367102486928,7.00798392898195));
#69539=CARTESIAN_POINT('Ctrl Pts',(3.43810803854393,-4.34162103676824,6.85098543563989));
#69540=CARTESIAN_POINT('Ctrl Pts',(-1.72474250700959,-5.26265084302763,
6.69398694229783));
#69541=CARTESIAN_POINT('Ctrl Pts',(-5.34081450144173,-1.46462806485474,
6.53698844895577));
#69542=CARTESIAN_POINT('Ctrl Pts',(-4.16793033765764,3.64667752326241,6.37998995561372));
#69543=CARTESIAN_POINT('Ctrl Pts',(0.742363895820577,5.48805471738879,6.22299146227166));
#69544=CARTESIAN_POINT('Ctrl Pts',(4.98695562724675,2.40832423618623,6.0659929689296));
#69545=CARTESIAN_POINT('Ctrl Pts',(4.75979764573692,-2.83092705288579,5.90899447558755));
#69546=CARTESIAN_POINT('Ctrl Pts',(0.264556723446406,-5.53171018842698,
5.75199598224549));
#69547=CARTESIAN_POINT('Ctrl Pts',(-4.4679059233187,-3.27224900479161,5.59499748890343));
#69548=CARTESIAN_POINT('Ctrl Pts',(-5.19403322368223,1.92141244912467,5.43799899556137));
#69549=CARTESIAN_POINT('Ctrl Pts',(-1.26270889296415,5.39215823112403,5.28100050221931));
#69550=CARTESIAN_POINT('Ctrl Pts',(3.80087638262942,4.02779613946379,5.12400200887726));
#69551=CARTESIAN_POINT('Ctrl Pts',(5.45624475437132,-0.948260301250735,
4.96700351553519));
#69552=CARTESIAN_POINT('Ctrl Pts',(2.21903939191664,-5.07401892926682,4.81000502219315));
#69553=CARTESIAN_POINT('Ctrl Pts',(-3.00796179140179,-4.64994297667973,
4.65300652885108));
#69554=CARTESIAN_POINT('Ctrl Pts',(-5.53774634000859,-0.05629820027127,
4.49600803550903));
#69555=CARTESIAN_POINT('Ctrl Pts',(-3.10187543821507,4.58782875637178,4.33900954216697));
#69556=CARTESIAN_POINT('Ctrl Pts',(2.11542379075055,5.11808422275766,4.18201104882491));
#69557=CARTESIAN_POINT('Ctrl Pts',(5.43583844779792,1.05899212403571,4.02501255548285));
#69558=CARTESIAN_POINT('Ctrl Pts',(3.88197771466281,-3.94969023749826,3.8680140621408));
#69559=CARTESIAN_POINT('Ctrl Pts',(-1.15282319263835,-5.4167151127071,3.71101556879874));
#69560=CARTESIAN_POINT('Ctrl Pts',(-5.15389622421624,-2.0266123561262,3.55401707545668));
#69561=CARTESIAN_POINT('Ctrl Pts',(-4.53350934304161,3.18073844416463,3.39701858211462));
#69562=CARTESIAN_POINT('Ctrl Pts',(0.152041229593681,5.53594502225318,3.24002008877256));
#69563=CARTESIAN_POINT('Ctrl Pts',(4.70125754884517,2.92711143909179,3.08302159543051));
#69564=CARTESIAN_POINT('Ctrl Pts',(5.03489169279947,-2.30644099432688,2.92602310208845));
#69565=CARTESIAN_POINT('Ctrl Pts',(0.853776279563064,-5.47182502293018,
2.7690246087464));
#69566=CARTESIAN_POINT('Ctrl Pts',(-4.09291369219827,-3.730665040722,2.61202611540433));
#69567=CARTESIAN_POINT('Ctrl Pts',(-5.36951917175407,1.3557546948219,2.45502762206228));
#69568=CARTESIAN_POINT('Ctrl Pts',(-1.83131652209583,5.22647842097189,2.29802912872022));
#69569=CARTESIAN_POINT('Ctrl Pts',(3.34901244388816,4.41066021354511,2.14103063537816));
#69570=CARTESIAN_POINT('Ctrl Pts',(5.52630989327424,-0.360167420268118,
1.9840321420361));
#69571=CARTESIAN_POINT('Ctrl Pts',(2.74820168192207,-4.80802865738244,1.82703364869405));
#69572=CARTESIAN_POINT('Ctrl Pts',(-2.49418827623448,-4.94458022258368,
1.67003515535199));
#69573=CARTESIAN_POINT('Ctrl Pts',(-5.50007758969876,-0.647338215717022,
1.51303666200993));
#69574=CARTESIAN_POINT('Ctrl Pts',(-3.57405191698147,4.23031769514908,1.35603816866787));
#69575=CARTESIAN_POINT('Ctrl Pts',(1.55672846333943,5.31477441689994,1.19903967532582));
#69576=CARTESIAN_POINT('Ctrl Pts',(5.2917379137821,1.63333094119038,1.04204118198376));
#69577=CARTESIAN_POINT('Ctrl Pts',(4.28142524730059,-3.5123586979906,0.885042688641701));
#69578=CARTESIAN_POINT('Ctrl Pts',(-0.567508953307252,-5.50921344548227,
0.728044195299643));
#69579=CARTESIAN_POINT('Ctrl Pts',(-4.90852249920177,-2.56471030992692,
0.571045701957585));
#69580=CARTESIAN_POINT('Ctrl Pts',(-4.84625629098129,2.67707509338356,0.414047208615528));
#69581=CARTESIAN_POINT('Ctrl Pts',(-0.441940127905122,5.52311844147288,
0.257048715273468));
#69582=CARTESIAN_POINT('Ctrl Pts',(4.3655763654143,3.40726490835521,0.100050221931412));
#69583=CARTESIAN_POINT('Ctrl Pts',(5.09789765444943,-0.885503254393324,
-0.0307818558536364));
#69584=CARTESIAN_POINT('Ctrl Pts',(3.3473081142412,-3.56521249842258,-0.135447518081676));
#69585=CARTESIAN_POINT('Ctrl Pts',(1.96401037376818,-4.34270105156074,-0.187780349195693));
#69586=CARTESIAN_POINT('Ctrl Pts',(1.21713437249836,-4.54280821229859,-0.213946764752702));
#69587=CARTESIAN_POINT('Ctrl Pts',(3.71544298812217,3.17665283523789,8.21394676475271));
#69588=CARTESIAN_POINT('Ctrl Pts',(4.23771151809924,2.5658026579396,8.1877803491957));
#69589=CARTESIAN_POINT('Ctrl Pts',(4.96565443914292,1.08579944354106,8.13544751808168));
#69590=CARTESIAN_POINT('Ctrl Pts',(4.889266010305,-2.24027022002061,8.03078185585363));
#69591=CARTESIAN_POINT('Ctrl Pts',(1.73635035915592,-5.48787775262049,7.89994977806859));
#69592=CARTESIAN_POINT('Ctrl Pts',(-3.62789544602829,-4.472709787582,7.74295128472654));
#69593=CARTESIAN_POINT('Ctrl Pts',(-5.72760320035712,0.557053682211493,
7.58595279138447));
#69594=CARTESIAN_POINT('Ctrl Pts',(-2.69726234454278,5.08531242977894,7.42895429804241));
#69595=CARTESIAN_POINT('Ctrl Pts',(2.75472947775923,5.05464473383097,7.27195580470038));
#69596=CARTESIAN_POINT('Ctrl Pts',(5.73499568142482,0.490976741224864,7.11495731135828));
#69597=CARTESIAN_POINT('Ctrl Pts',(3.57355766702658,-4.5126659689955,6.95795881801627));
#69598=CARTESIAN_POINT('Ctrl Pts',(-1.7926914280975,-5.46998118097242,6.80096032467417));
#69599=CARTESIAN_POINT('Ctrl Pts',(-5.55122421861904,-1.522329371802,6.64396183133214));
#69600=CARTESIAN_POINT('Ctrl Pts',(-4.33213245389376,3.79034407189453,6.48696333799006));
#69601=CARTESIAN_POINT('Ctrl Pts',(0.771610479337022,5.70426519251906,6.32996484464802));
#69602=CARTESIAN_POINT('Ctrl Pts',(5.18342452217309,2.50320392565502,6.17296635130595));
#69603=CARTESIAN_POINT('Ctrl Pts',(4.94731729769082,-2.9424558394382,6.01596785796391));
#69604=CARTESIAN_POINT('Ctrl Pts',(0.274979348187014,-5.7496405389268,5.85896936462183));
#69605=CARTESIAN_POINT('Ctrl Pts',(-4.64392604561401,-3.40116435795471,
5.70197087127979));
#69606=CARTESIAN_POINT('Ctrl Pts',(-5.39866026349227,1.99710948932185,5.54497237793772));
#69607=CARTESIAN_POINT('Ctrl Pts',(-1.31245527920807,5.6045907146113,5.38797388459567));
#69608=CARTESIAN_POINT('Ctrl Pts',(3.95061783582519,4.18647745039935,5.23097539125361));
#69609=CARTESIAN_POINT('Ctrl Pts',(5.67120202639557,-0.985618494788963,
5.07397689791155));
#69610=CARTESIAN_POINT('Ctrl Pts',(2.30646190972407,-5.273917818766,4.9169784045695));
#69611=CARTESIAN_POINT('Ctrl Pts',(-3.1264651375933,-4.83313473260941,4.75997991122743));
#69612=CARTESIAN_POINT('Ctrl Pts',(-5.75591449411437,-0.058516155677411,
4.60298141788538));
#69613=CARTESIAN_POINT('Ctrl Pts',(-3.22407865899683,4.76857342571492,4.44598292454332));
#69614=CARTESIAN_POINT('Ctrl Pts',(2.19876421034419,5.31971913322111,4.28898443120126));
#69615=CARTESIAN_POINT('Ctrl Pts',(5.64999178154766,1.10071277043733,4.1319859378592));
#69616=CARTESIAN_POINT('Ctrl Pts',(4.03491428132513,-4.10529444460668,3.97498744451715));
#69617=CARTESIAN_POINT('Ctrl Pts',(-1.19824046033282,-5.6301150528449,3.81798895117509));
#69618=CARTESIAN_POINT('Ctrl Pts',(-5.35694200433196,-2.10645391073654,
3.66099045783303));
#69619=CARTESIAN_POINT('Ctrl Pts',(-4.7121140143764,3.30604859606581,3.50399196449097));
#69620=CARTESIAN_POINT('Ctrl Pts',(0.158031130967237,5.75404221063653,3.34699347114891));
#69621=CARTESIAN_POINT('Ctrl Pts',(4.88647092237896,3.04242955955441,3.18999497780686));
#69622=CARTESIAN_POINT('Ctrl Pts',(5.23324910379256,-2.39730683457867,3.0329964844648));
#69623=CARTESIAN_POINT('Ctrl Pts',(0.887412127703281,-5.68739610393434,
2.87599799112275));
#69624=CARTESIAN_POINT('Ctrl Pts',(-4.25416041068552,-3.87764040859701,
2.71899949778068));
#69625=CARTESIAN_POINT('Ctrl Pts',(-5.58105975418807,1.40916676555049,2.56200100443863));
#69626=CARTESIAN_POINT('Ctrl Pts',(-1.90346409272805,5.43238368993286,2.40500251109657));
#69627=CARTESIAN_POINT('Ctrl Pts',(3.48095201245988,4.58442505181962,2.24800401775452));
#69628=CARTESIAN_POINT('Ctrl Pts',(5.74402749072386,-0.374356777530876,
2.09100552441245));
#69629=CARTESIAN_POINT('Ctrl Pts',(2.85647137346132,-4.99744844526445,1.9340070310704));
#69630=CARTESIAN_POINT('Ctrl Pts',(-2.5924507134803,-5.13937967235178,1.77700853772834));
#69631=CARTESIAN_POINT('Ctrl Pts',(-5.71676172463537,-0.672841114357358,
1.62001004438628));
#69632=CARTESIAN_POINT('Ctrl Pts',(-3.71485726658238,4.39697765863709,1.46301155104423));
#69633=CARTESIAN_POINT('Ctrl Pts',(1.61805820913096,5.52415824433286,1.30601305770217));
#69634=CARTESIAN_POINT('Ctrl Pts',(5.50021418224542,1.69767856107122,1.14901456436011));
#69635=CARTESIAN_POINT('Ctrl Pts',(4.45009867251637,-3.65073354700848,0.992016071018051));
#69636=CARTESIAN_POINT('Ctrl Pts',(-0.589866853647869,-5.72625750170636,
0.835017577675995));
#69637=CARTESIAN_POINT('Ctrl Pts',(-5.1019013987192,-2.66575107268096,0.678019084333936));
#69638=CARTESIAN_POINT('Ctrl Pts',(-5.0371821161113,2.78254264203352,0.521020590991878));
#69639=CARTESIAN_POINT('Ctrl Pts',(-0.459351048523452,5.74071030670118,
0.36402209764982));
#69640=CARTESIAN_POINT('Ctrl Pts',(4.53756505517591,3.54149942361907,0.207023604307763));
#69641=CARTESIAN_POINT('Ctrl Pts',(5.29873728357006,-0.920389036190499,
0.076191526522715));
#69642=CARTESIAN_POINT('Ctrl Pts',(3.47918053808829,-3.70566960534281,-0.0284741357053249));
#69643=CARTESIAN_POINT('Ctrl Pts',(2.04138562564527,-4.51378853265522,-0.0808069668193416));
#69644=CARTESIAN_POINT('Ctrl Pts',(1.26508527942745,-4.7217792270909,-0.106973382376351));
#69645=CARTESIAN_POINT('Ctrl Pts',(3.85627053850235,3.29705846079181,8.32092014712906));
#69646=CARTESIAN_POINT('Ctrl Pts',(4.39833476927537,2.66305504594064,8.29475373157205));
#69647=CARTESIAN_POINT('Ctrl Pts',(5.15386912927126,1.12695482563867,8.24242090045804));
#69648=CARTESIAN_POINT('Ctrl Pts',(5.0745853268951,-2.3251838543527,8.13775523822997));
#69649=CARTESIAN_POINT('Ctrl Pts',(1.80216376780286,-5.69588642969024,8.00692316044496));
#69650=CARTESIAN_POINT('Ctrl Pts',(-3.76540465565226,-4.64224024867649,
7.84992466710287));
#69651=CARTESIAN_POINT('Ctrl Pts',(-5.94469826300093,0.578167855069724,
7.69292617376083));
#69652=CARTESIAN_POINT('Ctrl Pts',(-2.799497488489,5.27806255262917,7.53592768041876));
#69653=CARTESIAN_POINT('Ctrl Pts',(2.8591428156985,5.24623244979999,7.37892918707671));
#69654=CARTESIAN_POINT('Ctrl Pts',(5.95237094349663,0.509586379962791,7.22193069373465));
#69655=CARTESIAN_POINT('Ctrl Pts',(3.70900729550924,-4.68371090122276,7.06493220039259));
#69656=CARTESIAN_POINT('Ctrl Pts',(-1.86064034918539,-5.67731151891722,
6.90793370705054));
#69657=CARTESIAN_POINT('Ctrl Pts',(-5.76163393579635,-1.58003067874924,
6.75093521370848));
#69658=CARTESIAN_POINT('Ctrl Pts',(-4.49633457012987,3.93401062052664,6.59393672036642));
#69659=CARTESIAN_POINT('Ctrl Pts',(0.800857062853464,5.92047566764934,6.43693822702436));
#69660=CARTESIAN_POINT('Ctrl Pts',(5.37989341709942,2.59808361512381,6.27993973368231));
#69661=CARTESIAN_POINT('Ctrl Pts',(5.13483694964473,-3.0539846259906,6.12294124034024));
#69662=CARTESIAN_POINT('Ctrl Pts',(0.285401972927619,-5.96757088942664,
5.96594274699819));
#69663=CARTESIAN_POINT('Ctrl Pts',(-4.81994616790931,-3.5300797111178,5.80894425365613));
#69664=CARTESIAN_POINT('Ctrl Pts',(-5.6032873033023,2.07280652951902,5.65194576031408));
#69665=CARTESIAN_POINT('Ctrl Pts',(-1.36220166545199,5.81702319809857,5.49494726697201));
#69666=CARTESIAN_POINT('Ctrl Pts',(4.10035928902097,4.34515876133492,5.33794877362997));
#69667=CARTESIAN_POINT('Ctrl Pts',(5.88615929841981,-1.02297668832719,5.1809502802879));
#69668=CARTESIAN_POINT('Ctrl Pts',(2.3938844275315,-5.47381670826519,5.02395178694585));
#69669=CARTESIAN_POINT('Ctrl Pts',(-3.24496848378481,-5.01632648853908,
4.86695329360378));
#69670=CARTESIAN_POINT('Ctrl Pts',(-5.97408264822014,-0.0607341110835563,
4.70995480026174));
#69671=CARTESIAN_POINT('Ctrl Pts',(-3.34628187977858,4.94931809505806,4.55295630691966));
#69672=CARTESIAN_POINT('Ctrl Pts',(2.28210462993784,5.52135404368456,4.39595781357762));
#69673=CARTESIAN_POINT('Ctrl Pts',(5.86414511529741,1.14243341683897,4.23895932023555));
#69674=CARTESIAN_POINT('Ctrl Pts',(4.18785084798745,-4.2608986517151,4.0819608268935));
#69675=CARTESIAN_POINT('Ctrl Pts',(-1.24365772802729,-5.8435149929827,3.92496233355144));
#69676=CARTESIAN_POINT('Ctrl Pts',(-5.55998778444767,-2.18629546534688,
3.76796384020939));
#69677=CARTESIAN_POINT('Ctrl Pts',(-4.89071868571119,3.43135874796699,3.61096534686732));
#69678=CARTESIAN_POINT('Ctrl Pts',(0.164021032340792,5.97213939901987,3.45396685352527));
#69679=CARTESIAN_POINT('Ctrl Pts',(5.07168429591276,3.15774768001703,3.29696836018321));
#69680=CARTESIAN_POINT('Ctrl Pts',(5.43160651478565,-2.48817267483047,3.13996986684115));
#69681=CARTESIAN_POINT('Ctrl Pts',(0.921047975843499,-5.90296718493849,
2.9829713734991));
#69682=CARTESIAN_POINT('Ctrl Pts',(-4.41540712917277,-4.02461577647203,
2.82597288015704));
#69683=CARTESIAN_POINT('Ctrl Pts',(-5.79260033662206,1.46257883627908,2.66897438681498));
#69684=CARTESIAN_POINT('Ctrl Pts',(-1.97561166336026,5.63828895889383,2.51197589347292));
#69685=CARTESIAN_POINT('Ctrl Pts',(3.6128915810316,4.75818989009414,2.35497740013087));
#69686=CARTESIAN_POINT('Ctrl Pts',(5.96174508817349,-0.388546134793637,
2.19797890678881));
#69687=CARTESIAN_POINT('Ctrl Pts',(2.96474106500057,-5.18686823314646,2.04098041344675));
#69688=CARTESIAN_POINT('Ctrl Pts',(-2.69071315072611,-5.33417912211988,
1.88398192010469));
#69689=CARTESIAN_POINT('Ctrl Pts',(-5.93344585957197,-0.698344012997689,
1.72698342676263));
#69690=CARTESIAN_POINT('Ctrl Pts',(-3.85566261618328,4.5636376221251,1.56998493342058));
#69691=CARTESIAN_POINT('Ctrl Pts',(1.67938795492248,5.73354207176578,1.41298644007852));
#69692=CARTESIAN_POINT('Ctrl Pts',(5.70869045070874,1.76202618095205,1.25598794673646));
#69693=CARTESIAN_POINT('Ctrl Pts',(4.61877209773216,-3.78910839602635,1.0989894533944));
#69694=CARTESIAN_POINT('Ctrl Pts',(-0.612224753988487,-5.94330155793046,
0.941990960052346));
#69695=CARTESIAN_POINT('Ctrl Pts',(-5.29528029823663,-2.76679183543498,
0.784992466710288));
#69696=CARTESIAN_POINT('Ctrl Pts',(-5.22810794124132,2.88801019068349,0.62799397336823));
#69697=CARTESIAN_POINT('Ctrl Pts',(-0.476761969141785,5.95830217192949,
0.470995480026171));
#69698=CARTESIAN_POINT('Ctrl Pts',(4.70955374493753,3.67573393888292,0.313996986684114));
#69699=CARTESIAN_POINT('Ctrl Pts',(5.49957691269067,-0.955274817987675,
0.183164908899066));
#69700=CARTESIAN_POINT('Ctrl Pts',(3.61105296193539,-3.84612671226304,0.0784992466710263));
#69701=CARTESIAN_POINT('Ctrl Pts',(2.11876087752236,-4.68487601374969,0.0261664155570096));
#69702=CARTESIAN_POINT('Ctrl Pts',(1.31303618635654,-4.90075024188321,0.));
#69703=CARTESIAN_POINT('Ctrl Pts',(1.31303618635654,-4.90075024188321,0.));
#69704=CARTESIAN_POINT('Ctrl Pts',(1.45239813196613,-4.85517621763986,-2.47434559251786E-16));
#69705=CARTESIAN_POINT('Ctrl Pts',(1.58927692318379,-4.80351009978137,-1.74819720228364E-15));
#69706=CARTESIAN_POINT('Ctrl Pts',(1.72341090925204,-4.74604460400692,-1.88737914186277E-15));
#69707=CARTESIAN_POINT('Ctrl Pts',(1.85925417986306,-4.68784681892573,-2.02833469262672E-15));
#69708=CARTESIAN_POINT('Ctrl Pts',(1.99228283138741,-4.62370052461763,2.98138735348004E-16));
#69709=CARTESIAN_POINT('Ctrl Pts',(2.12220346118141,-4.55386096654418,1.11022302462516E-16));
#69710=CARTESIAN_POINT('Ctrl Pts',(2.25247560296862,-4.48383245124121,-7.66003908251115E-17));
#69711=CARTESIAN_POINT('Ctrl Pts',(2.37962344910693,-4.40807936214696,-4.32517766211178E-16));
#69712=CARTESIAN_POINT('Ctrl Pts',(2.50332095055395,-4.32681677710386,-4.44089209850063E-16));
#69713=CARTESIAN_POINT('Ctrl Pts',(2.62609735089877,-4.24615930579203,-4.55574487888469E-16));
#69714=CARTESIAN_POINT('Ctrl Pts',(2.74547509807873,-4.16007358686041,1.08564249317406E-16));
#69715=CARTESIAN_POINT('Ctrl Pts',(2.86109774307792,-4.06873562676994,-5.55111512312578E-17));
#69716=CARTESIAN_POINT('Ctrl Pts',(2.90211866182286,-4.03633049506564,-1.13722271327984E-16));
#69717=CARTESIAN_POINT('Ctrl Pts',(2.94266654026491,-4.00326397860027,-2.92134559916121E-15));
#69718=CARTESIAN_POINT('Ctrl Pts',(2.98272412781597,-3.96954306736407,-2.99760216648792E-15));
#69719=CARTESIAN_POINT('Ctrl Pts',(2.99979215651063,-3.95517501587181,-3.03009412016909E-15));
#69720=CARTESIAN_POINT('Ctrl Pts',(3.01677225892353,-3.94068710954429,-2.12566972362838E-15));
#69721=CARTESIAN_POINT('Ctrl Pts',(3.03364729547102,-3.92609378878367,-2.1094237467878E-15));
#69722=CARTESIAN_POINT('Ctrl Pts',(3.14433957478624,-3.83036848867988,-2.00285780240447E-15));
#69723=CARTESIAN_POINT('Ctrl Pts',(3.25067225380611,-3.72997908311154,-3.12896148123733E-15));
#69724=CARTESIAN_POINT('Ctrl Pts',(3.35235973413124,-3.62516300488518,-3.10862446895044E-15));
#69725=CARTESIAN_POINT('Ctrl Pts',(3.36192986162372,-3.61529843523825,-3.10671048898182E-15));
#69726=CARTESIAN_POINT('Ctrl Pts',(3.37145882014037,-3.60539462864919,-2.66105468162811E-15));
#69727=CARTESIAN_POINT('Ctrl Pts',(3.38094635546186,-3.59545176562119,-2.692290834716E-15));
#69728=CARTESIAN_POINT('Ctrl Pts',(3.48180408426425,-3.48975365237926,-3.02597608841997E-15));
#69729=CARTESIAN_POINT('Ctrl Pts',(3.57798405787049,-3.37964444416285,-3.04382432431275E-15));
#69730=CARTESIAN_POINT('Ctrl Pts',(3.66918347167548,-3.26550314479251,-2.94209101525666E-15));
#69731=CARTESIAN_POINT('Ctrl Pts',(3.75971565071324,-3.15219692801907,-2.84110200923889E-15));
#69732=CARTESIAN_POINT('Ctrl Pts',(3.84534031026112,-3.03491668112307,-1.42999735083781E-15));
#69733=CARTESIAN_POINT('Ctrl Pts',(3.92571655230007,-2.91400844798661,-1.72084568816899E-15));
#69734=CARTESIAN_POINT('Ctrl Pts',(3.99657720672258,-2.80741430638731,-1.97726105417974E-15));
#69735=CARTESIAN_POINT('Ctrl Pts',(4.06335815473368,-2.69799970084542,-4.7182430533371E-15));
#69736=CARTESIAN_POINT('Ctrl Pts',(4.12579259176727,-2.58599222827228,-4.96824803519758E-15));
#69737=CARTESIAN_POINT('Ctrl Pts',(4.14218217787996,-2.55658928649489,-5.03387653084013E-15));
#69738=CARTESIAN_POINT('Ctrl Pts',(4.15827206325859,-2.52700763769101,-2.22246092678142E-15));
#69739=CARTESIAN_POINT('Ctrl Pts',(4.17405702945515,-2.49725134739943,-2.08166817117217E-15));
#69740=CARTESIAN_POINT('Ctrl Pts',(4.18546582852437,-2.47574458376403,-1.97990829160411E-15));
#69741=CARTESIAN_POINT('Ctrl Pts',(4.1967169159508,-2.45414332829404,-3.10559938199478E-15));
#69742=CARTESIAN_POINT('Ctrl Pts',(4.20779634099434,-2.4324729617879,-3.08086889333481E-15));
#69743=CARTESIAN_POINT('Ctrl Pts',(4.27314972651924,-2.30464757272886,-2.93499298792804E-15));
#69744=CARTESIAN_POINT('Ctrl Pts',(4.3326198595779,-2.17426195525281,-5.03888835755339E-15));
#69745=CARTESIAN_POINT('Ctrl Pts',(4.38592260758549,-2.04167340157391,-4.413136522885E-15));
#69746=CARTESIAN_POINT('Ctrl Pts',(4.43841100193019,-1.9111105215869,-3.79694485758248E-15));
#69747=CARTESIAN_POINT('Ctrl Pts',(4.48491932736646,-1.77841080748911,-3.47246432590996E-15));
#69748=CARTESIAN_POINT('Ctrl Pts',(4.52512906800885,-1.64389810614591,-3.30291349825984E-15));
#69749=CARTESIAN_POINT('Ctrl Pts',(4.53704337373435,-1.60404145892158,-3.25267491516128E-15));
#69750=CARTESIAN_POINT('Ctrl Pts',(4.54840435272953,-1.56402555907027,-1.86047514559207E-15));
#69751=CARTESIAN_POINT('Ctrl Pts',(4.55920284487768,-1.52385866802948,-1.74860126378462E-15));
#69752=CARTESIAN_POINT('Ctrl Pts',(4.59648625924208,-1.38517645000696,-1.33619040184573E-15));
#69753=CARTESIAN_POINT('Ctrl Pts',(4.62706837090021,-1.24469418107576,-3.1405520603229E-15));
#69754=CARTESIAN_POINT('Ctrl Pts',(4.6510479415724,-1.1028549274787,-3.44169137633799E-15));
#69755=CARTESIAN_POINT('Ctrl Pts',(4.66553556506662,-1.0171605782801,-3.62362928879583E-15));
#69756=CARTESIAN_POINT('Ctrl Pts',(4.67761212738266,-0.93097088404131,-3.48256637849421E-15));
#69757=CARTESIAN_POINT('Ctrl Pts',(4.68729033896278,-0.844384764732073,
-3.60822483003176E-15));
#69758=CARTESIAN_POINT('Ctrl Pts',(4.69282045363923,-0.794909594117687,
-3.68002586902689E-15));
#69759=CARTESIAN_POINT('Ctrl Pts',(4.6975673931995,-0.74530501799734,-2.90670583210387E-15));
#69760=CARTESIAN_POINT('Ctrl Pts',(4.70153256693874,-0.695589781678817,
-3.02535774210355E-15));
#69761=CARTESIAN_POINT('Ctrl Pts',(4.70300273002319,-0.67715691846114,-3.06935017962366E-15));
#69762=CARTESIAN_POINT('Ctrl Pts',(4.70436508297707,-0.658712562708346,
-1.39035176949888E-15));
#69763=CARTESIAN_POINT('Ctrl Pts',(4.70561925922056,-0.640267374588028,
-1.41553435639707E-15));
#69764=CARTESIAN_POINT('Ctrl Pts',(4.71515008316959,-0.500097409167311,
-1.60690363448191E-15));
#69765=CARTESIAN_POINT('Ctrl Pts',(4.71845154780466,-0.359714693128242,
-6.98970443009747E-16));
#69766=CARTESIAN_POINT('Ctrl Pts',(4.71567835888356,-0.219533504962576,
-9.0205620750794E-16));
#69767=CARTESIAN_POINT('Ctrl Pts',(4.71285964179518,-0.0770509255950372,
-1.1084760840775E-15));
#69768=CARTESIAN_POINT('Ctrl Pts',(4.70376507114378,0.065224279671225,-2.40577940367026E-15));
#69769=CARTESIAN_POINT('Ctrl Pts',(4.68850374693714,0.206855299208619,-2.26207941267376E-15));
#69770=CARTESIAN_POINT('Ctrl Pts',(4.67332604169022,0.347710302303635,-2.11916677430768E-15));
#69771=CARTESIAN_POINT('Ctrl Pts',(4.65204869880232,0.487928957857132,-3.70693630030531E-15));
#69772=CARTESIAN_POINT('Ctrl Pts',(4.62472984685344,0.627067645312151,-4.06619182768964E-15));
#69773=CARTESIAN_POINT('Ctrl Pts',(4.60512526025429,0.72691651350792,-4.32400120090221E-15));
#69774=CARTESIAN_POINT('Ctrl Pts',(4.58240838869996,0.826208961746935,-2.80327058352682E-15));
#69775=CARTESIAN_POINT('Ctrl Pts',(4.55658611607818,0.924773126569175,-2.94209101525666E-15));
#69776=CARTESIAN_POINT('Ctrl Pts',(4.54451163215688,0.970861688981747,-3.00700339130591E-15));
#69777=CARTESIAN_POINT('Ctrl Pts',(4.53175798542344,1.01679090044476,-4.8702446610021E-15));
#69778=CARTESIAN_POINT('Ctrl Pts',(4.51832500803005,1.062542528366,-4.8988590961585E-15));
#69779=CARTESIAN_POINT('Ctrl Pts',(4.51266846717592,1.08180824622589,-4.91090845176596E-15));
#69780=CARTESIAN_POINT('Ctrl Pts',(4.50689146090876,1.10104246936981,-1.58247074004002E-15));
#69781=CARTESIAN_POINT('Ctrl Pts',(4.50099394804091,1.12024381085806,-1.56819002228303E-15));
#69782=CARTESIAN_POINT('Ctrl Pts',(4.49471177106765,1.14069755603102,-1.55297784754686E-15));
#69783=CARTESIAN_POINT('Ctrl Pts',(4.48829554526876,1.1611051847425,-3.02768046308214E-15));
#69784=CARTESIAN_POINT('Ctrl Pts',(4.48174652480305,1.18146221251882,-3.05311331771918E-15));
#69785=CARTESIAN_POINT('Ctrl Pts',(4.4388367801027,1.31484320732769,-3.21975156617037E-15));
#69786=CARTESIAN_POINT('Ctrl Pts',(4.3902172033679,1.44609540153194,-2.42101694317024E-15));
#69787=CARTESIAN_POINT('Ctrl Pts',(4.33595560037894,1.57478564497199,-2.33146835171283E-15));
#69788=CARTESIAN_POINT('Ctrl Pts',(4.28905400984558,1.68602041819998,-2.25406607942409E-15));
#69789=CARTESIAN_POINT('Ctrl Pts',(4.23793630897375,1.79534112442678,-2.09120843630436E-15));
#69790=CARTESIAN_POINT('Ctrl Pts',(4.18261934387559,1.90245063170277,-1.54737334057131E-15));
#69791=CARTESIAN_POINT('Ctrl Pts',(4.15876651886949,1.94863654101668,-1.31287017598733E-15));
#69792=CARTESIAN_POINT('Ctrl Pts',(4.13413259613109,1.99441106904023,-3.34114378130206E-15));
#69793=CARTESIAN_POINT('Ctrl Pts',(4.1087175751394,2.03974918362091,-3.32373017997156E-15));
#69794=CARTESIAN_POINT('Ctrl Pts',(4.09757084929567,2.05963394128716,-3.31609278159812E-15));
#69795=CARTESIAN_POINT('Ctrl Pts',(4.08627386148571,2.07943474030452,-3.10826804513356E-15));
#69796=CARTESIAN_POINT('Ctrl Pts',(4.07482656400744,2.09914941832117,-3.21964677141295E-15));
#69797=CARTESIAN_POINT('Ctrl Pts',(4.06286705490573,2.11974623356295,-3.33600916115644E-15));
#69798=CARTESIAN_POINT('Ctrl Pts',(4.05074796307183,2.14024130439856,-5.56609850953026E-16));
#69799=CARTESIAN_POINT('Ctrl Pts',(4.03847105489573,2.16062996612303,-7.21644966006352E-16));
#69800=CARTESIAN_POINT('Ctrl Pts',(3.96920184151707,2.27566760746066,-1.65281203475204E-15));
#69801=CARTESIAN_POINT('Ctrl Pts',(3.89489673126452,2.38734604756407,-5.44084181235126E-15));
#69802=CARTESIAN_POINT('Ctrl Pts',(3.81559015152877,2.49525778868992,-3.92741394961149E-15));
#69803=CARTESIAN_POINT('Ctrl Pts',(3.73966418517796,2.5985695599563,-2.47849920176032E-15));
#69804=CARTESIAN_POINT('Ctrl Pts',(3.65915364949516,2.69842924853399,9.77632756533034E-16));
#69805=CARTESIAN_POINT('Ctrl Pts',(3.57405694815596,2.79444772885285,1.90646110009851E-15));
#69806=CARTESIAN_POINT('Ctrl Pts',(3.53072890723773,2.84333672899846,2.33391700333807E-15));
#69807=CARTESIAN_POINT('Ctrl Pts',(3.48621138925297,2.89122932971802,2.44271821993007E-16));
#69808=CARTESIAN_POINT('Ctrl Pts',(3.44055068766011,2.93810645203839,2.77555756156289E-16));
#69809=CARTESIAN_POINT('Ctrl Pts',(3.43378788736183,2.93584158413004,8.));
#69810=CARTESIAN_POINT('Ctrl Pts',(3.52723828091404,2.83914431545175,8.));
#69811=CARTESIAN_POINT('Ctrl Pts',(3.61594081851665,2.73846055769803,8.));
#69812=CARTESIAN_POINT('Ctrl Pts',(3.69984090589852,2.63418809372837,8.));
#69813=CARTESIAN_POINT('Ctrl Pts',(3.78516287227981,2.52814849421259,8.));
#69814=CARTESIAN_POINT('Ctrl Pts',(3.86551863442571,2.41839706286655,8.));
#69815=CARTESIAN_POINT('Ctrl Pts',(3.94081955158113,2.30530820215193,8.));
#69816=CARTESIAN_POINT('Ctrl Pts',(4.01714046916727,2.19068747846675,8.));
#69817=CARTESIAN_POINT('Ctrl Pts',(4.08826910733635,2.07263776324572,8.));
#69818=CARTESIAN_POINT('Ctrl Pts',(4.15407500660322,1.95151170764482,8.));
#69819=CARTESIAN_POINT('Ctrl Pts',(4.2198164513151,1.83050429073889,8.));
#69820=CARTESIAN_POINT('Ctrl Pts',(4.28024594506117,1.70642592249187,8.));
#69821=CARTESIAN_POINT('Ctrl Pts',(4.33518967485951,1.57960030623271,8.));
#69822=CARTESIAN_POINT('Ctrl Pts',(4.35307625782352,1.53831303076909,8.));
#69823=CARTESIAN_POINT('Ctrl Pts',(4.37038109771682,1.49673442540794,8.));
#69824=CARTESIAN_POINT('Ctrl Pts',(4.3870970941841,1.45487519313349,8.));
#69825=CARTESIAN_POINT('Ctrl Pts',(4.39376575085273,1.43817592851012,8.));
#69826=CARTESIAN_POINT('Ctrl Pts',(4.40033736934907,1.42144028204873,8.));
#69827=CARTESIAN_POINT('Ctrl Pts',(4.40681102745828,1.40467100393547,8.));
#69828=CARTESIAN_POINT('Ctrl Pts',(4.45934053196233,1.26859927210788,8.));
#69829=CARTESIAN_POINT('Ctrl Pts',(4.50544025366947,1.13027539792009,8.));
#69830=CARTESIAN_POINT('Ctrl Pts',(4.54499873531868,0.990127463611741,8.));
#69831=CARTESIAN_POINT('Ctrl Pts',(4.58299050839006,0.855530070216331,8.));
#69832=CARTESIAN_POINT('Ctrl Pts',(4.61494911931547,0.719249512352558,8.));
#69833=CARTESIAN_POINT('Ctrl Pts',(4.64085249468742,0.581767615475945,8.));
#69834=CARTESIAN_POINT('Ctrl Pts',(4.66691769963291,0.443426809811538,8.));
#69835=CARTESIAN_POINT('Ctrl Pts',(4.68685201899535,0.303868786404607,8.));
#69836=CARTESIAN_POINT('Ctrl Pts',(4.70058414747143,0.163565049614876,8.));
#69837=CARTESIAN_POINT('Ctrl Pts',(4.71271762019861,0.0395950789853681,
8.));
#69838=CARTESIAN_POINT('Ctrl Pts',(4.72000832561645,-0.0849577470138994,
8.));
#69839=CARTESIAN_POINT('Ctrl Pts',(4.7223733384523,-0.209772800136726,8.));
#69840=CARTESIAN_POINT('Ctrl Pts',(4.72292943816615,-0.239121315406544,
8.));
#69841=CARTESIAN_POINT('Ctrl Pts',(4.7232130590816,-0.268484329285888,8.));
#69842=CARTESIAN_POINT('Ctrl Pts',(4.72322285747563,-0.297857662780827,
8.));
#69843=CARTESIAN_POINT('Ctrl Pts',(4.72323033779459,-0.320281939952091,
8.));
#69844=CARTESIAN_POINT('Ctrl Pts',(4.72307812055779,-0.342714494826838,
8.));
#69845=CARTESIAN_POINT('Ctrl Pts',(4.72276611337907,-0.365130653249834,
8.));
#69846=CARTESIAN_POINT('Ctrl Pts',(4.72077139214363,-0.508441417465993,
8.));
#69847=CARTESIAN_POINT('Ctrl Pts',(4.71225120797944,-0.651280085007766,
8.));
#69848=CARTESIAN_POINT('Ctrl Pts',(4.69718547532262,-0.793154607131843,
8.));
#69849=CARTESIAN_POINT('Ctrl Pts',(4.68212772666397,-0.934953943670782,
8.));
#69850=CARTESIAN_POINT('Ctrl Pts',(4.66053153776914,-1.07579102267899,8.));
#69851=CARTESIAN_POINT('Ctrl Pts',(4.63232650453452,-1.21518583219434,8.));
#69852=CARTESIAN_POINT('Ctrl Pts',(4.62517817164043,-1.25051429622537,8.));
#69853=CARTESIAN_POINT('Ctrl Pts',(4.6176050749471,-1.28575013896589,8.));
#69854=CARTESIAN_POINT('Ctrl Pts',(4.60960553319191,-1.32088555816255,8.));
#69855=CARTESIAN_POINT('Ctrl Pts',(4.57835655312357,-1.45813667176012,8.));
#69856=CARTESIAN_POINT('Ctrl Pts',(4.54060431924761,-1.59385616146054,8.));
#69857=CARTESIAN_POINT('Ctrl Pts',(4.49667031501799,-1.72776662727194,8.));
#69858=CARTESIAN_POINT('Ctrl Pts',(4.46792000249182,-1.81539733178229,8.));
#69859=CARTESIAN_POINT('Ctrl Pts',(4.43652132007444,-1.90225320075805,8.));
#69860=CARTESIAN_POINT('Ctrl Pts',(4.4025528899726,-1.98825323145006,8.));
#69861=CARTESIAN_POINT('Ctrl Pts',(4.39064088821649,-2.01841160243036,8.));
#69862=CARTESIAN_POINT('Ctrl Pts',(4.37841279355623,-2.04846469658551,8.));
#69863=CARTESIAN_POINT('Ctrl Pts',(4.36587175340618,-2.07840891566329,8.));
#69864=CARTESIAN_POINT('Ctrl Pts',(4.35885849939885,-2.09515444968045,8.));
#69865=CARTESIAN_POINT('Ctrl Pts',(4.35174737519127,-2.11186593393486,8.));
#69866=CARTESIAN_POINT('Ctrl Pts',(4.34453891478344,-2.12854273059161,8.));
#69867=CARTESIAN_POINT('Ctrl Pts',(4.33664233992457,-2.14681148227446,8.));
#69868=CARTESIAN_POINT('Ctrl Pts',(4.32863248368416,-2.16503040522278,8.));
#69869=CARTESIAN_POINT('Ctrl Pts',(4.32051229345552,-2.18319454758947,8.));
#69870=CARTESIAN_POINT('Ctrl Pts',(4.26271734267779,-2.31247670532764,8.));
#69871=CARTESIAN_POINT('Ctrl Pts',(4.19930769062008,-2.43905306787665,8.));
#69872=CARTESIAN_POINT('Ctrl Pts',(4.1306563766664,-2.56266246904431,8.));
#69873=CARTESIAN_POINT('Ctrl Pts',(4.05932719227651,-2.69109348165625,8.));
#69874=CARTESIAN_POINT('Ctrl Pts',(3.98233931388035,-2.81632224208436,8.));
#69875=CARTESIAN_POINT('Ctrl Pts',(3.90005514682149,-2.93804448640157,8.));
#69876=CARTESIAN_POINT('Ctrl Pts',(3.81788412514087,-3.05959935575629,8.));
#69877=CARTESIAN_POINT('Ctrl Pts',(3.73043085662906,-3.17765799919859,8.));
#69878=CARTESIAN_POINT('Ctrl Pts',(3.63800695579095,-3.29189623321801,8.));
#69879=CARTESIAN_POINT('Ctrl Pts',(3.56857767496828,-3.37771254651463,8.));
#69880=CARTESIAN_POINT('Ctrl Pts',(3.49634236728105,-3.46137260211582,8.));
#69881=CARTESIAN_POINT('Ctrl Pts',(3.42141741611953,-3.54272769601374,8.));
#69882=CARTESIAN_POINT('Ctrl Pts',(3.38628453897598,-3.58087571579362,8.));
#69883=CARTESIAN_POINT('Ctrl Pts',(3.35056009922657,-3.61851677693959,8.));
#69884=CARTESIAN_POINT('Ctrl Pts',(3.3142552023334,-3.65563464117867,8.));
#69885=CARTESIAN_POINT('Ctrl Pts',(3.299200603776,-3.67102635395701,8.));
#69886=CARTESIAN_POINT('Ctrl Pts',(3.28404454782071,-3.68632972667595,8.));
#69887=CARTESIAN_POINT('Ctrl Pts',(3.26879310797022,-3.70153828550149,8.));
#69888=CARTESIAN_POINT('Ctrl Pts',(3.16313496534899,-3.80689935915782,8.));
#69889=CARTESIAN_POINT('Ctrl Pts',(3.05310906400962,-3.90750842604698,8.));
#69890=CARTESIAN_POINT('Ctrl Pts',(2.93905349297435,-4.00304219163214,8.));
#69891=CARTESIAN_POINT('Ctrl Pts',(2.83343523748027,-4.09150880111292,8.));
#69892=CARTESIAN_POINT('Ctrl Pts',(2.72436063892977,-4.17562341526862,8.));
#69893=CARTESIAN_POINT('Ctrl Pts',(2.61206707761722,-4.25510461849443,8.));
#69894=CARTESIAN_POINT('Ctrl Pts',(2.56057116079448,-4.29155334611912,8.));
#69895=CARTESIAN_POINT('Ctrl Pts',(2.50839792228814,-4.3270273021059,8.));
#69896=CARTESIAN_POINT('Ctrl Pts',(2.45556847535629,-4.3614972584752,8.));
#69897=CARTESIAN_POINT('Ctrl Pts',(2.42827791858812,-4.37930369703788,8.));
#69898=CARTESIAN_POINT('Ctrl Pts',(2.40081223344856,-4.39684219182932,8.));
#69899=CARTESIAN_POINT('Ctrl Pts',(2.37317422709578,-4.41410855841438,8.));
#69900=CARTESIAN_POINT('Ctrl Pts',(2.35241127848289,-4.42707985155184,8.));
#69901=CARTESIAN_POINT('Ctrl Pts',(2.33155925321721,-4.43989244410762,8.));
#69902=CARTESIAN_POINT('Ctrl Pts',(2.31062069154639,-4.45254421740167,8.));
#69903=CARTESIAN_POINT('Ctrl Pts',(2.18359867140573,-4.52929513408044,8.));
#69904=CARTESIAN_POINT('Ctrl Pts',(2.05338150515115,-4.60013897577206,8.00000000000001));
#69905=CARTESIAN_POINT('Ctrl Pts',(1.9202708514578,-4.66473499429566,8.00000000000001));
#69906=CARTESIAN_POINT('Ctrl Pts',(1.79118849882964,-4.72737615644222,8.00000000000001));
#69907=CARTESIAN_POINT('Ctrl Pts',(1.65938453798209,-4.78414231274042,8.00000000000001));
#69908=CARTESIAN_POINT('Ctrl Pts',(1.52510693593821,-4.83468454964306,8.00000000000001));
#69909=CARTESIAN_POINT('Ctrl Pts',(1.45664940136588,-4.86045204085127,8.00000000000001));
#69910=CARTESIAN_POINT('Ctrl Pts',(1.38754853402863,-4.88460115986285,8.00000000000001));
#69911=CARTESIAN_POINT('Ctrl Pts',(1.31785785677859,-4.9071457994741,8.00000000000001));
#69912=CARTESIAN_POINT('Ctrl Pts',(-4.51611343680291,-0.0038242599945422,
6.38741669750802));
#69913=CARTESIAN_POINT('Ctrl Pts',(-4.51950916701914,-0.407146869176555,
6.40161615386516));
#69914=CARTESIAN_POINT('Ctrl Pts',(-4.46982237313174,-0.809647705501708,
6.41581561022229));
#69915=CARTESIAN_POINT('Ctrl Pts',(-4.36369015740015,-1.19666942701374,
6.43001506657943));
#69916=CARTESIAN_POINT('Ctrl Pts',(-3.97253438481685,-2.62305800696593,
6.48234789769345));
#69917=CARTESIAN_POINT('Ctrl Pts',(-2.81466398536927,-3.83918925602438,
6.53468072880746));
#69918=CARTESIAN_POINT('Ctrl Pts',(-1.40915345298166,-4.2997974804633,6.58701355992148));
#69919=CARTESIAN_POINT('Ctrl Pts',(-0.0036429205940397,-4.76040570490222,
6.6393463910355));
#69920=CARTESIAN_POINT('Ctrl Pts',(1.64950774473362,-4.4654909047216,6.69167922214952));
#69921=CARTESIAN_POINT('Ctrl Pts',(2.8090142019341,-3.54731124324962,6.74401205326355));
#69922=CARTESIAN_POINT('Ctrl Pts',(3.96852065913458,-2.62913158177766,6.79634488437757));
#69923=CARTESIAN_POINT('Ctrl Pts',(4.63438290820789,-1.08768705901433,6.84867771549158));
#69924=CARTESIAN_POINT('Ctrl Pts',(4.50825697351113,0.385987175391315,6.9010105466056));
#69925=CARTESIAN_POINT('Ctrl Pts',(4.38213103881437,1.85966140979697,6.95334337771962));
#69926=CARTESIAN_POINT('Ctrl Pts',(3.46401692034753,3.26556535584495,7.00567620883364));
#69927=CARTESIAN_POINT('Ctrl Pts',(2.16517738469227,3.97324114256653,7.05800903994766));
#69928=CARTESIAN_POINT('Ctrl Pts',(0.866337849037014,4.6809169292881,7.11034187106168));
#69929=CARTESIAN_POINT('Ctrl Pts',(-0.81322710380666,4.69036455668328,7.1626747021757));
#69930=CARTESIAN_POINT('Ctrl Pts',(-2.11977974996502,3.9975905624503,7.21500753328971));
#69931=CARTESIAN_POINT('Ctrl Pts',(-3.42633239612339,3.30481656821732,7.26734036440373));
#69932=CARTESIAN_POINT('Ctrl Pts',(-4.35987273559643,1.90982095235617,7.31967319551775));
#69933=CARTESIAN_POINT('Ctrl Pts',(-4.50322023061811,0.437577444110917,
7.37200602663177));
#69934=CARTESIAN_POINT('Ctrl Pts',(-4.51729094569115,0.293064846108908,
7.37714291692385));
#69935=CARTESIAN_POINT('Ctrl Pts',(-4.52374814565307,0.14780796397411,7.38227980721594));
#69936=CARTESIAN_POINT('Ctrl Pts',(-4.52286359173795,0.00246468782935438,
7.38741669750802));
#69937=CARTESIAN_POINT('Ctrl Pts',(-1.31303618635644,-4.90075024188323,
8.));
#69938=CARTESIAN_POINT('Ctrl Pts',(-2.11876087752226,-4.68487601374973,
7.97383358444299));
#69939=CARTESIAN_POINT('Ctrl Pts',(-3.61103600209076,-3.84612122823184,
7.92150075332897));
#69940=CARTESIAN_POINT('Ctrl Pts',(-5.49959712288033,-0.955281493922513,
7.81683509110094));
#69941=CARTESIAN_POINT('Ctrl Pts',(-4.70954440514987,3.67573693777646,7.68600301331588));
#69942=CARTESIAN_POINT('Ctrl Pts',(0.476758320675261,5.95830042580594,7.52900451997384));
#69943=CARTESIAN_POINT('Ctrl Pts',(5.22810884028568,2.88800998678043,7.37200602663177));
#69944=CARTESIAN_POINT('Ctrl Pts',(5.29527916712856,-2.76679132542031,7.21500753328971));
#69945=CARTESIAN_POINT('Ctrl Pts',(0.612224870220684,-5.9433011663707,7.05800903994766));
#69946=CARTESIAN_POINT('Ctrl Pts',(-4.61877163601819,-3.7891077783966,6.90101054660559));
#69947=CARTESIAN_POINT('Ctrl Pts',(-5.70868984087812,1.76202584286959,6.74401205326355));
#69948=CARTESIAN_POINT('Ctrl Pts',(-1.67938775292856,5.73354154736347,6.58701355992148));
#69949=CARTESIAN_POINT('Ctrl Pts',(3.85566217988192,4.56363706615652,6.43001506657943));
#69950=CARTESIAN_POINT('Ctrl Pts',(5.93344523009267,-0.69834389981148,6.27301657323736));
#69951=CARTESIAN_POINT('Ctrl Pts',(2.69071284975304,-5.33417856632519,6.11601807989532));
#69952=CARTESIAN_POINT('Ctrl Pts',(-2.96474073765194,-5.18686765769478,
5.95901958655325));
#69953=CARTESIAN_POINT('Ctrl Pts',(-5.96174444561926,-0.38854610033802,
5.8020210932112));
#69954=CARTESIAN_POINT('Ctrl Pts',(-3.61289118716291,4.75818937870979,5.64502259986913));
#69955=CARTESIAN_POINT('Ctrl Pts',(1.97561144788205,5.63828834519714,5.48802410652708));
#69956=CARTESIAN_POINT('Ctrl Pts',(5.79259970947732,1.46257867915377,5.33102561318502));
#69957=CARTESIAN_POINT('Ctrl Pts',(4.41540665009831,-4.0246153410012,5.17402711984296));
#69958=CARTESIAN_POINT('Ctrl Pts',(-0.92104787574744,-5.90296654461282,
5.01702862650091));
#69959=CARTESIAN_POINT('Ctrl Pts',(-5.43160592614493,-2.48817240536104,
4.86003013315885));
#69960=CARTESIAN_POINT('Ctrl Pts',(-5.07168374606222,3.15774733785514,4.70303163981679));
#69961=CARTESIAN_POINT('Ctrl Pts',(-0.164021014606317,5.97213875156532,
4.54603314647473));
#69962=CARTESIAN_POINT('Ctrl Pts',(4.89071815558305,3.43135837605058,4.38903465313268));
#69963=CARTESIAN_POINT('Ctrl Pts',(5.55998718173337,-2.18629522837624,4.23203615979062));
#69964=CARTESIAN_POINT('Ctrl Pts',(1.24365759322077,-5.84351435953346,4.07503766644856));
#69965=CARTESIAN_POINT('Ctrl Pts',(-4.1878503940255,-4.26089818984331,3.91803917310651));
#69966=CARTESIAN_POINT('Ctrl Pts',(-5.86414447963045,1.14243329300625,3.76104067976444));
#69967=CARTESIAN_POINT('Ctrl Pts',(-2.2821043825461,5.52135344516299,3.60404218642239));
#69968=CARTESIAN_POINT('Ctrl Pts',(3.34628151701835,4.94931755856517,3.44704369308033));
#69969=CARTESIAN_POINT('Ctrl Pts',(5.9740820006751,-0.0607341045204584,
3.29004519973827));
#69970=CARTESIAN_POINT('Ctrl Pts',(3.24496813195078,-5.01632594473331,3.13304670639622));
#69971=CARTESIAN_POINT('Ctrl Pts',(-2.39388416789017,-5.47381611497205,
2.97604821305415));
#69972=CARTESIAN_POINT('Ctrl Pts',(-5.88615866062065,-1.02297657731424,
2.8190497197121));
#69973=CARTESIAN_POINT('Ctrl Pts',(-4.10035884408111,4.34515829009749,2.66205122637004));
#69974=CARTESIAN_POINT('Ctrl Pts',(1.36220151697138,5.81702256793933,2.50505273302799));
#69975=CARTESIAN_POINT('Ctrl Pts',(5.60328669734595,2.07280630409542,2.34805423968593));
#69976=CARTESIAN_POINT('Ctrl Pts',(4.81994564291905,-3.53007932713903,2.19105574634387));
#69977=CARTESIAN_POINT('Ctrl Pts',(-0.285401937658034,-5.96757024490932,
2.03405725300181));
#69978=CARTESIAN_POINT('Ctrl Pts',(-5.13483640041478,-3.05398429071519,
1.87705875965975));
#69979=CARTESIAN_POINT('Ctrl Pts',(-5.37989282152843,2.59808332599247,1.7200602663177));
#69980=CARTESIAN_POINT('Ctrl Pts',(-0.800856996403053,5.92047503909791,
1.56306177297564));
#69981=CARTESIAN_POINT('Ctrl Pts',(4.49633411524324,3.93401017093414,1.40606327963358));
#69982=CARTESIAN_POINT('Ctrl Pts',(5.76163326143087,-1.58003046734643,1.24906478629152));
#69983=CARTESIAN_POINT('Ctrl Pts',(1.86064021890344,-5.67731097226746,1.09206629294947));
#69984=CARTESIAN_POINT('Ctrl Pts',(-3.70900698411085,-4.68371027734449,
0.935067799607409));
#69985=CARTESIAN_POINT('Ctrl Pts',(-5.9523702132809,0.509586132109229,0.77806930626535));
#69986=CARTESIAN_POINT('Ctrl Pts',(-2.85914249825567,5.24623219278067,0.621070812923292));
#69987=CARTESIAN_POINT('Ctrl Pts',(2.79949684465664,5.27806149196883,0.464072319581235));
#69988=CARTESIAN_POINT('Ctrl Pts',(5.94469888877439,0.578168532022547,0.307073826239177));
#69989=CARTESIAN_POINT('Ctrl Pts',(3.76540065952631,-4.64224087416102,0.150075332897119));
#69990=CARTESIAN_POINT('Ctrl Pts',(-1.80215437063507,-5.69588361575389,
-0.00692316044493745));
#69991=CARTESIAN_POINT('Ctrl Pts',(-5.07460576691081,-2.32518978947096,
-0.137755238229986));
#69992=CARTESIAN_POINT('Ctrl Pts',(-5.15385204348173,1.12695990370127,-0.242420900458024));
#69993=CARTESIAN_POINT('Ctrl Pts',(-4.39833476927544,2.66305504594052,-0.294753731572044));
#69994=CARTESIAN_POINT('Ctrl Pts',(-3.85627053850243,3.2970584607917,-0.320920147129053));
#69995=CARTESIAN_POINT('Ctrl Pts',(-1.26508527942735,-4.72177922709092,
8.10697338237635));
#69996=CARTESIAN_POINT('Ctrl Pts',(-2.04138562564518,-4.51378853265526,
8.08080696681934));
#69997=CARTESIAN_POINT('Ctrl Pts',(-3.47916419760203,-3.70566432158352,
8.02847413570533));
#69998=CARTESIAN_POINT('Ctrl Pts',(-5.29875675570167,-0.920395468326166,
7.92380847347728));
#69999=CARTESIAN_POINT('Ctrl Pts',(-4.53755605646894,3.54150231299569,7.79297639569223));
#70000=CARTESIAN_POINT('Ctrl Pts',(0.459347533295664,5.74070862434451,7.63597790235019));
#70001=CARTESIAN_POINT('Ctrl Pts',(5.03718298232336,2.78254244557681,7.47897940900812));
#70002=CARTESIAN_POINT('Ctrl Pts',(5.10190030891819,-2.66575058129155,7.32198091566607));
#70003=CARTESIAN_POINT('Ctrl Pts',(0.589866965635366,-5.72625712444602,
7.16498242232401));
#70004=CARTESIAN_POINT('Ctrl Pts',(-4.45009822766378,-3.650732951934,7.00798392898195));
#70005=CARTESIAN_POINT('Ctrl Pts',(-5.50021359468528,1.69767823533522,6.8509854356399));
#70006=CARTESIAN_POINT('Ctrl Pts',(-1.61805801451367,5.52415773908126,6.69398694229783));
#70007=CARTESIAN_POINT('Ctrl Pts',(3.71485684621434,4.39697712297199,6.53698844895578));
#70008=CARTESIAN_POINT('Ctrl Pts',(5.71676111814409,-0.672841005304612,
6.37998995561372));
#70009=CARTESIAN_POINT('Ctrl Pts',(2.5924504234985,-5.13937913685421,6.22299146227166));
#70010=CARTESIAN_POINT('Ctrl Pts',(-2.85647105806718,-4.99744789082776,
6.0659929689296));
#70011=CARTESIAN_POINT('Ctrl Pts',(-5.74402687163513,-0.374356744333544,
5.90899447558755));
#70012=CARTESIAN_POINT('Ctrl Pts',(-3.48095163297493,4.58442455911056,5.75199598224549));
#70013=CARTESIAN_POINT('Ctrl Pts',(1.90346388511891,5.43238309864782,5.59499748890343));
#70014=CARTESIAN_POINT('Ctrl Pts',(5.58105914994609,1.40916661416325,5.43799899556138));
#70015=CARTESIAN_POINT('Ctrl Pts',(4.25415994910644,-3.8776399890292,5.28100050221931));
#70016=CARTESIAN_POINT('Ctrl Pts',(-0.887412031262641,-5.68739548699278,
5.12400200887726));
#70017=CARTESIAN_POINT('Ctrl Pts',(-5.23324853664848,-2.39730657495003,
4.9670035155352));
#70018=CARTESIAN_POINT('Ctrl Pts',(-4.88647039260848,3.04242922988797,4.81000502219315));
#70019=CARTESIAN_POINT('Ctrl Pts',(-0.15803111388041,5.75404158682643,4.65300652885108));
#70020=CARTESIAN_POINT('Ctrl Pts',(4.71211350360807,3.30604823773145,4.49600803550903));
#70021=CARTESIAN_POINT('Ctrl Pts',(5.35694142362824,-2.10645368241985,4.33900954216697));
#70022=CARTESIAN_POINT('Ctrl Pts',(1.19824033044931,-5.63011444252866,4.18201104882491));
#70023=CARTESIAN_POINT('Ctrl Pts',(-4.03491384394147,-4.10529399960203,
4.02501255548286));
#70024=CARTESIAN_POINT('Ctrl Pts',(-5.6499911690947,1.10071265112688,3.86801406214079));
#70025=CARTESIAN_POINT('Ctrl Pts',(-2.19876397198699,5.31971855655701,3.71101556879874));
#70026=CARTESIAN_POINT('Ctrl Pts',(3.22407830948427,4.76857290881427,3.55401707545668));
#70027=CARTESIAN_POINT('Ctrl Pts',(5.75591387021709,-0.0585161493539971,
3.39701858211462));
#70028=CARTESIAN_POINT('Ctrl Pts',(3.12646479860794,-4.83313420866293,3.24002008877257));
#70029=CARTESIAN_POINT('Ctrl Pts',(-2.30646165956461,-5.27391724713939,
3.08302159543051));
#70030=CARTESIAN_POINT('Ctrl Pts',(-5.67120141188825,-0.985618387830106,
2.92602310208845));
#70031=CARTESIAN_POINT('Ctrl Pts',(-3.95061740713414,4.18647699637109,2.76902460874639));
#70032=CARTESIAN_POINT('Ctrl Pts',(1.31245513614984,5.60459010746491,2.61202611540434));
#70033=CARTESIAN_POINT('Ctrl Pts',(5.39865967966489,1.99710927213052,2.45502762206228));
#70034=CARTESIAN_POINT('Ctrl Pts',(4.64392553979592,-3.4011639879985,2.29802912872022));
#70035=CARTESIAN_POINT('Ctrl Pts',(-0.274979314205441,-5.74963991794669,
2.14103063537816));
#70036=CARTESIAN_POINT('Ctrl Pts',(-4.94731676851826,-2.94245551640673,
1.9840321420361));
#70037=CARTESIAN_POINT('Ctrl Pts',(-5.18342394835182,2.50320364708249,1.82703364869405));
#70038=CARTESIAN_POINT('Ctrl Pts',(-0.771610415313318,5.70426458692177,
1.67003515535199));
#70039=CARTESIAN_POINT('Ctrl Pts',(4.33213201561917,3.79034363872074,1.51303666200993));
#70040=CARTESIAN_POINT('Ctrl Pts',(5.55122356888078,-1.52232916811941,1.35603816866787));
#70041=CARTESIAN_POINT('Ctrl Pts',(1.79269130257332,-5.46998065428583,1.19903967532582));
#70042=CARTESIAN_POINT('Ctrl Pts',(-3.57355736700018,-4.5126653679007,1.04204118198376));
#70043=CARTESIAN_POINT('Ctrl Pts',(-5.73499497787591,0.490976502422684,
0.885042688641701));
#70044=CARTESIAN_POINT('Ctrl Pts',(-2.75472917190912,5.05464448619777,0.728044195299644));
#70045=CARTESIAN_POINT('Ctrl Pts',(2.6972617242226,5.08531140785296,0.571045701957586));
#70046=CARTESIAN_POINT('Ctrl Pts',(5.72760380327789,0.557054334442611,0.414047208615528));
#70047=CARTESIAN_POINT('Ctrl Pts',(3.62789159583729,-4.47271039022441,0.25704871527347));
#70048=CARTESIAN_POINT('Ctrl Pts',(-1.7363413051643,-5.48787504144657,0.100050221931414));
#70049=CARTESIAN_POINT('Ctrl Pts',(-4.88928570386961,-2.24027593839366,
-0.0307818558536355));
#70050=CARTESIAN_POINT('Ctrl Pts',(-4.96563797731115,1.08580433615736,-0.135447518081672));
#70051=CARTESIAN_POINT('Ctrl Pts',(-4.2377115180993,2.56580265793949,-0.187780349195693));
#70052=CARTESIAN_POINT('Ctrl Pts',(-3.71544298812226,3.17665283523778,-0.213946764752702));
#70053=CARTESIAN_POINT('Ctrl Pts',(-1.21713437249827,-4.54280821229861,
8.21394676475271));
#70054=CARTESIAN_POINT('Ctrl Pts',(-1.96401037376809,-4.34270105156078,
8.1877803491957));
#70055=CARTESIAN_POINT('Ctrl Pts',(-3.34729239311329,-3.56520741493521,
8.13544751808168));
#70056=CARTESIAN_POINT('Ctrl Pts',(-5.097916388523,-0.88550944272982,8.03078185585364));
#70057=CARTESIAN_POINT('Ctrl Pts',(-4.36556770778803,3.40726768821492,7.89994977806859));
#70058=CARTESIAN_POINT('Ctrl Pts',(0.441936745916073,5.52311682288307,7.74295128472654));
#70059=CARTESIAN_POINT('Ctrl Pts',(4.84625712436104,2.6770749043732,7.58595279138447));
#70060=CARTESIAN_POINT('Ctrl Pts',(4.90852145070782,-2.56470983716281,7.42895429804242));
#70061=CARTESIAN_POINT('Ctrl Pts',(0.567509061050049,-5.50921308252134,
7.27195580470035));
#70062=CARTESIAN_POINT('Ctrl Pts',(-4.28142481930937,-3.51235812547142,
7.11495731135831));
#70063=CARTESIAN_POINT('Ctrl Pts',(-5.29173734849243,1.63333062780086,6.95795881801624));
#70064=CARTESIAN_POINT('Ctrl Pts',(-1.55672827609878,5.31477393079903,6.80096032467419));
#70065=CARTESIAN_POINT('Ctrl Pts',(3.57405151254677,4.23031717978746,6.64396183133213));
#70066=CARTESIAN_POINT('Ctrl Pts',(5.50007700619551,-0.647338110797742,
6.48696333799007));
#70067=CARTESIAN_POINT('Ctrl Pts',(2.49418799724395,-4.94457970738323,6.32996484464802));
#70068=CARTESIAN_POINT('Ctrl Pts',(-2.74820137848241,-4.80802812396074,
6.17296635130595));
#70069=CARTESIAN_POINT('Ctrl Pts',(-5.52630929765102,-0.360167388329068,
6.0159678579639));
#70070=CARTESIAN_POINT('Ctrl Pts',(-3.34901207878694,4.41065973951134,5.85896936462184));
#70071=CARTESIAN_POINT('Ctrl Pts',(1.83131632235576,5.22647785209851,5.70197087127978));
#70072=CARTESIAN_POINT('Ctrl Pts',(5.36951859041486,1.35575454917273,5.54497237793772));
#70073=CARTESIAN_POINT('Ctrl Pts',(4.09291324811456,-3.73066463705719,5.38797388459567));
#70074=CARTESIAN_POINT('Ctrl Pts',(-0.853776186777843,-5.47182442937275,
5.23097539125361));
#70075=CARTESIAN_POINT('Ctrl Pts',(-5.03489114715202,-2.30644074453902,
5.07397689791155));
#70076=CARTESIAN_POINT('Ctrl Pts',(-4.70125703915474,2.92711112192079,4.91697840456949));
#70077=CARTESIAN_POINT('Ctrl Pts',(-0.1520412131545,5.53594442208755,4.75997991122743));
#70078=CARTESIAN_POINT('Ctrl Pts',(4.53350885163308,3.18073809941233,4.60298141788538));
#70079=CARTESIAN_POINT('Ctrl Pts',(5.15389566552312,-2.02661213646347,4.44598292454332));
#70080=CARTESIAN_POINT('Ctrl Pts',(1.15282306767785,-5.41671452552386,4.28898443120126));
#70081=CARTESIAN_POINT('Ctrl Pts',(-3.88197729385743,-3.94968980936076,
4.13198593785921));
#70082=CARTESIAN_POINT('Ctrl Pts',(-5.43583785855895,1.05899200924751,3.97498744451714));
#70083=CARTESIAN_POINT('Ctrl Pts',(-2.11542356142786,5.11808366795104,3.81798895117509));
#70084=CARTESIAN_POINT('Ctrl Pts',(3.1018751019502,4.58782825906337,3.66099045783304));
#70085=CARTESIAN_POINT('Ctrl Pts',(5.53774573975908,-0.0562981941875292,
3.50399196449097));
#70086=CARTESIAN_POINT('Ctrl Pts',(3.00796146526509,-4.64994247259256,3.34699347114892));
#70087=CARTESIAN_POINT('Ctrl Pts',(-2.21903915123905,-5.07401837930674,
3.18999497780685));
#70088=CARTESIAN_POINT('Ctrl Pts',(-5.45624416315586,-0.948260198345973,
3.03299648446481));
#70089=CARTESIAN_POINT('Ctrl Pts',(-3.80087597018717,4.0277957026447,2.87599799112274));
#70090=CARTESIAN_POINT('Ctrl Pts',(1.26270875532829,5.39215764699048,2.71899949778069));
#70091=CARTESIAN_POINT('Ctrl Pts',(5.19403266198385,1.92141224016561,2.56200100443863));
#70092=CARTESIAN_POINT('Ctrl Pts',(4.46790543667278,-3.27224864885797,2.40500251109657));
#70093=CARTESIAN_POINT('Ctrl Pts',(-0.264556690752847,-5.53170959098406,
2.24800401775451));
#70094=CARTESIAN_POINT('Ctrl Pts',(-4.75979713662174,-2.83092674209829,
2.09100552441246));
#70095=CARTESIAN_POINT('Ctrl Pts',(-4.9869550751752,2.40832396817252,1.9340070310704));
#70096=CARTESIAN_POINT('Ctrl Pts',(-0.742363834223583,5.48805413474563,
1.77700853772834));
#70097=CARTESIAN_POINT('Ctrl Pts',(4.16792991599511,3.64667710650734,1.62001004438628));
#70098=CARTESIAN_POINT('Ctrl Pts',(5.3408138763307,-1.4646278688924,1.46301155104423));
#70099=CARTESIAN_POINT('Ctrl Pts',(1.7247423862432,-5.26265033630419,1.30601305770217));
#70100=CARTESIAN_POINT('Ctrl Pts',(-3.43810774988952,-4.34162045845692,
1.14901456436011));
#70101=CARTESIAN_POINT('Ctrl Pts',(-5.51761974247093,0.472366872736146,
0.992016071018053));
#70102=CARTESIAN_POINT('Ctrl Pts',(-2.65031584556259,4.86305677961485,0.835017577675994));
#70103=CARTESIAN_POINT('Ctrl Pts',(2.59502660378856,4.89256132373709,0.678019084333937));
#70104=CARTESIAN_POINT('Ctrl Pts',(5.51050871778138,0.535940136862668,0.521020590991879));
#70105=CARTESIAN_POINT('Ctrl Pts',(3.49038253214829,-4.30317990628779,0.364022097649821));
#70106=CARTESIAN_POINT('Ctrl Pts',(-1.67052823969354,-5.27986646713926,
0.207023604307765));
#70107=CARTESIAN_POINT('Ctrl Pts',(-4.70396564082841,-2.15536208731635,
0.0761915265227156));
#70108=CARTESIAN_POINT('Ctrl Pts',(-4.77742391114056,1.04464876861345,-0.0284741357053212));
#70109=CARTESIAN_POINT('Ctrl Pts',(-4.07708826692317,2.46855026993846,-0.0808069668193416));
#70110=CARTESIAN_POINT('Ctrl Pts',(-3.57461543774208,3.05624720968387,-0.106973382376351));
#70111=CARTESIAN_POINT('Ctrl Pts',(-1.16918346556918,-4.3638371975063,8.32092014712906));
#70112=CARTESIAN_POINT('Ctrl Pts',(-1.886635121891,-4.17161357046631,8.29475373157205));
#70113=CARTESIAN_POINT('Ctrl Pts',(-3.21542058862456,-3.4247505082869,8.24242090045803));
#70114=CARTESIAN_POINT('Ctrl Pts',(-4.89707602134433,-0.850623417133479,
8.13775523822999));
#70115=CARTESIAN_POINT('Ctrl Pts',(-4.19357935910711,3.27303306343417,8.00692316044493));
#70116=CARTESIAN_POINT('Ctrl Pts',(0.424525958536476,5.30552502142163,7.84992466710289));
#70117=CARTESIAN_POINT('Ctrl Pts',(4.65533126639873,2.5716073631696,7.69292617376082));
#70118=CARTESIAN_POINT('Ctrl Pts',(4.71514259249745,-2.46366909303406,7.53592768041877));
#70119=CARTESIAN_POINT('Ctrl Pts',(0.545151156464739,-5.29216904059666,
7.3789291870767));
#70120=CARTESIAN_POINT('Ctrl Pts',(-4.11275141095498,-3.37398329900883,
7.22193069373466));
#70121=CARTESIAN_POINT('Ctrl Pts',(-5.08326110229957,1.56898302026649,7.06493220039259));
#70122=CARTESIAN_POINT('Ctrl Pts',(-1.4953985376839,5.10539012251682,6.90793370705054));
#70123=CARTESIAN_POINT('Ctrl Pts',(3.4332461788792,4.06365723660293,6.75093521370847));
#70124=CARTESIAN_POINT('Ctrl Pts',(5.28339289424692,-0.621835216290863,
6.59393672036643));
#70125=CARTESIAN_POINT('Ctrl Pts',(2.3959255709894,-4.74978027791225,6.43693822702436));
#70126=CARTESIAN_POINT('Ctrl Pts',(-2.63993169889764,-4.61860835709371,
6.27993973368231));
#70127=CARTESIAN_POINT('Ctrl Pts',(-5.3085917236669,-0.345978032324596,
6.12294124034025));
#70128=CARTESIAN_POINT('Ctrl Pts',(-3.21707252459896,4.23689491991211,5.96594274699819));
#70129=CARTESIAN_POINT('Ctrl Pts',(1.75916875959262,5.0205726055492,5.80894425365613));
#70130=CARTESIAN_POINT('Ctrl Pts',(5.15797803088363,1.30234248418222,5.65194576031408));
#70131=CARTESIAN_POINT('Ctrl Pts',(3.93166654712268,-3.58368928508518,5.49494726697202));
#70132=CARTESIAN_POINT('Ctrl Pts',(-0.820140342293046,-5.25625337175271,
5.33794877362996));
#70133=CARTESIAN_POINT('Ctrl Pts',(-4.83653375765556,-2.215574914128,5.1809502802879));
#70134=CARTESIAN_POINT('Ctrl Pts',(-4.516043685701,2.81179301395361,5.02395178694585));
#70135=CARTESIAN_POINT('Ctrl Pts',(-0.14605131242859,5.31784725734868,4.86695329360378));
#70136=CARTESIAN_POINT('Ctrl Pts',(4.3549041996581,3.0554279610932,4.70995480026174));
#70137=CARTESIAN_POINT('Ctrl Pts',(4.95084990741799,-1.94677059050708,4.55295630691967));
#70138=CARTESIAN_POINT('Ctrl Pts',(1.1074058049064,-5.20331460851906,4.39595781357761));
#70139=CARTESIAN_POINT('Ctrl Pts',(-3.7290407437734,-3.79408561911948,4.23895932023556));
#70140=CARTESIAN_POINT('Ctrl Pts',(-5.22168454802319,1.01727136736814,4.08196082689349));
#70141=CARTESIAN_POINT('Ctrl Pts',(-2.03208315086874,4.91644877934506,3.92496233355144));
#70142=CARTESIAN_POINT('Ctrl Pts',(2.97967189441612,4.40708360931248,3.76796384020938));
#70143=CARTESIAN_POINT('Ctrl Pts',(5.31957760930108,-0.0540802390210696,
3.61096534686732));
#70144=CARTESIAN_POINT('Ctrl Pts',(2.88945813192224,-4.46675073652217,3.45396685352527));
#70145=CARTESIAN_POINT('Ctrl Pts',(-2.13161664291348,-4.87411951147409,
3.29696836018321));
#70146=CARTESIAN_POINT('Ctrl Pts',(-5.24128691442347,-0.910902008861835,
3.13996986684115));
#70147=CARTESIAN_POINT('Ctrl Pts',(-3.6511345332402,3.86911440891831,2.9829713734991));
#70148=CARTESIAN_POINT('Ctrl Pts',(1.21296237450675,5.17972518651607,2.82597288015703));
#70149=CARTESIAN_POINT('Ctrl Pts',(4.98940564430279,1.8457152082007,2.66897438681498));
#70150=CARTESIAN_POINT('Ctrl Pts',(4.29188533354966,-3.14333330971743,2.51197589347292));
#70151=CARTESIAN_POINT('Ctrl Pts',(-0.254134067300259,-5.31377926402143,
2.35497740013087));
#70152=CARTESIAN_POINT('Ctrl Pts',(-4.57227750472522,-2.71939796778984,
2.1979789067888));
#70153=CARTESIAN_POINT('Ctrl Pts',(-4.79048620199859,2.31344428926255,2.04098041344675));
#70154=CARTESIAN_POINT('Ctrl Pts',(-0.713117253133846,5.27184368256949,
1.88398192010469));
#70155=CARTESIAN_POINT('Ctrl Pts',(4.00372781637104,3.50301057429394,1.72698342676264));
#70156=CARTESIAN_POINT('Ctrl Pts',(5.13040418378061,-1.40692656966539,1.56998493342058));
#70157=CARTESIAN_POINT('Ctrl Pts',(1.65679346991308,-5.05532001832255,1.41298644007852));
#70158=CARTESIAN_POINT('Ctrl Pts',(-3.30265813277885,-4.17057554901314,
1.25598794673646));
#70159=CARTESIAN_POINT('Ctrl Pts',(-5.30024450706594,0.453757243049607,
1.0989894533944));
#70160=CARTESIAN_POINT('Ctrl Pts',(-2.54590251921605,4.67146907303194,0.941990960052346));
#70161=CARTESIAN_POINT('Ctrl Pts',(2.49279148335452,4.69981123962122,0.784992466710289));
#70162=CARTESIAN_POINT('Ctrl Pts',(5.29341363228488,0.514825939282724,0.62799397336823));
#70163=CARTESIAN_POINT('Ctrl Pts',(3.35287346845927,-4.13364942235117,0.470995480026172));
#70164=CARTESIAN_POINT('Ctrl Pts',(-1.60471517422276,-5.07185789283195,
0.313996986684116));
#70165=CARTESIAN_POINT('Ctrl Pts',(-4.51864557778723,-2.07044823623904,
0.183164908899067));
#70166=CARTESIAN_POINT('Ctrl Pts',(-4.58920984496997,1.00349320106954,0.07849924667103));
#70167=CARTESIAN_POINT('Ctrl Pts',(-3.91646501574703,2.37129788193743,0.0261664155570096));
#70168=CARTESIAN_POINT('Ctrl Pts',(-3.43378788736191,2.93584158412995,0.));
#70169=CARTESIAN_POINT('Ctrl Pts',(-3.43378788736191,2.93584158412995,0.));
#70170=CARTESIAN_POINT('Ctrl Pts',(-3.52723777670969,2.83914483717434,2.20957577510153E-16));
#70171=CARTESIAN_POINT('Ctrl Pts',(-3.61593961326928,2.73846171784274,-1.95102593779902E-16));
#70172=CARTESIAN_POINT('Ctrl Pts',(-3.69983889649088,2.63418997519716,-5.55111512312578E-17));
#70173=CARTESIAN_POINT('Ctrl Pts',(-3.78516004991503,2.5281511032253,8.64459958272222E-17));
#70174=CARTESIAN_POINT('Ctrl Pts',(-3.86551489177621,2.41840048478536,3.57207213678775E-15));
#70175=CARTESIAN_POINT('Ctrl Pts',(-3.9408148769991,2.30531248881791,3.33066907387547E-15));
#70176=CARTESIAN_POINT('Ctrl Pts',(-4.01713525064214,2.19069203993958,3.08599476344226E-15));
#70177=CARTESIAN_POINT('Ctrl Pts',(-4.08826327828892,2.07264261686327,1.15541512747695E-15));
#70178=CARTESIAN_POINT('Ctrl Pts',(-4.15406859699169,1.95151684254046,1.38777878078145E-15));
#70179=CARTESIAN_POINT('Ctrl Pts',(-4.21980984783224,1.8305089959106,1.61991620552547E-15));
#70180=CARTESIAN_POINT('Ctrl Pts',(-4.28023911511666,1.70643015108279,2.039107624704E-15));
#70181=CARTESIAN_POINT('Ctrl Pts',(-4.33518267922297,1.57960398874639,2.4980018054066E-15));
#70182=CARTESIAN_POINT('Ctrl Pts',(-4.35306946209471,1.53831594955441,2.64739401730341E-15));
#70183=CARTESIAN_POINT('Ctrl Pts',(-4.37037449182742,1.49673656482301,-1.24977233183131E-15));
#70184=CARTESIAN_POINT('Ctrl Pts',(-4.38709067099901,1.45487653718474,-1.55431223447522E-15));
#70185=CARTESIAN_POINT('Ctrl Pts',(-4.39375920070266,1.43817745572383,-1.67580132393046E-15));
#70186=CARTESIAN_POINT('Ctrl Pts',(-4.40033069663165,1.42144199284245,2.13318250051857E-15));
#70187=CARTESIAN_POINT('Ctrl Pts',(-4.40680423707264,1.40467289792598,2.1094237467878E-15));
#70188=CARTESIAN_POINT('Ctrl Pts',(-4.45933329243635,1.26860134275516,1.91663513266347E-15));
#70189=CARTESIAN_POINT('Ctrl Pts',(-4.50543275765374,1.13027759164836,2.92434253228364E-15));
#70190=CARTESIAN_POINT('Ctrl Pts',(-4.54499128400339,0.990129694249863,
2.63677968348475E-15));
#70191=CARTESIAN_POINT('Ctrl Pts',(-4.58298351161253,0.855530878059325,
2.35904680574097E-15));
#70192=CARTESIAN_POINT('Ctrl Pts',(-4.61494272389214,0.719248781594657,
4.48491542532579E-15));
#70193=CARTESIAN_POINT('Ctrl Pts',(-4.64084676847695,0.58176526830246,3.3584246494911E-15));
#70194=CARTESIAN_POINT('Ctrl Pts',(-4.66691254514768,0.44342337572085,2.22490062051545E-15));
#70195=CARTESIAN_POINT('Ctrl Pts',(-4.68684755285248,0.303864196021266,
1.79312284184644E-16));
#70196=CARTESIAN_POINT('Ctrl Pts',(-4.70058040711193,0.163559265384357,
-6.66133814775094E-16));
#70197=CARTESIAN_POINT('Ctrl Pts',(-4.71271438319262,0.0395896491496948,
-1.41314696648225E-15));
#70198=CARTESIAN_POINT('Ctrl Pts',(-4.72000573130037,-0.0849628385647041,
1.44014651394631E-16));
#70199=CARTESIAN_POINT('Ctrl Pts',(-4.7223714742082,-0.209777558646538,
-3.88578058618805E-16));
#70200=CARTESIAN_POINT('Ctrl Pts',(-4.72292774412613,-0.239125918464476,
-5.13809461450429E-16));
#70201=CARTESIAN_POINT('Ctrl Pts',(-4.72321154151185,-0.268488777105225,
3.0010215925102E-15));
#70202=CARTESIAN_POINT('Ctrl Pts',(-4.72322152198113,-0.297861955465308,
2.91433543964104E-15));
#70203=CARTESIAN_POINT('Ctrl Pts',(-4.72322914092456,-0.320285007726138,
2.84816050575247E-15));
#70204=CARTESIAN_POINT('Ctrl Pts',(-4.72307708136321,-0.342716335801155,
3.67219762837691E-17));
#70205=CARTESIAN_POINT('Ctrl Pts',(-4.72276525050185,-0.365131269043745,
1.38777878078145E-16));
#70206=CARTESIAN_POINT('Ctrl Pts',(-4.72077152616445,-0.508443568958217,
7.91283323787342E-16));
#70207=CARTESIAN_POINT('Ctrl Pts',(-4.71225224775121,-0.651283769357607,
4.69641391259678E-15));
#70208=CARTESIAN_POINT('Ctrl Pts',(-4.69718724960338,-0.793159785562181,
4.52415882534751E-15));
#70209=CARTESIAN_POINT('Ctrl Pts',(-4.68213033873543,-0.934959639059055,
4.35199620907545E-15));
#70210=CARTESIAN_POINT('Ctrl Pts',(-4.66053490666648,-1.07579720961356,
2.29755459169068E-15));
#70211=CARTESIAN_POINT('Ctrl Pts',(-4.63233047059339,-1.21519245994795,
1.88737914186277E-15));
#70212=CARTESIAN_POINT('Ctrl Pts',(-4.62518265294206,-1.25051923720629,
1.78342885146082E-15));
#70213=CARTESIAN_POINT('Ctrl Pts',(-4.61761010448178,-1.28575339934606,
3.86113148383421E-16));
#70214=CARTESIAN_POINT('Ctrl Pts',(-4.60961114292865,-1.32088714489269,
2.22044604925031E-16));
#70215=CARTESIAN_POINT('Ctrl Pts',(-4.57836306126197,-1.45813772958496,
-4.20462921062943E-16));
#70216=CARTESIAN_POINT('Ctrl Pts',(-4.54061164386395,-1.59385666227503,
-3.37562086541692E-16));
#70217=CARTESIAN_POINT('Ctrl Pts',(-4.49667838831439,-1.72776655308613,
-8.04911692853238E-16));
#70218=CARTESIAN_POINT('Ctrl Pts',(-4.46792839524171,-1.81539740094895,
-1.11074602668306E-15));
#70219=CARTESIAN_POINT('Ctrl Pts',(-4.43652997184098,-1.90225339638272,
9.54490265544014E-16));
#70220=CARTESIAN_POINT('Ctrl Pts',(-4.40256174565587,-1.98825353803286,
7.21644966006352E-16));
#70221=CARTESIAN_POINT('Ctrl Pts',(-4.39065014752274,-2.01841110708421,
6.3999337724903E-16));
#70222=CARTESIAN_POINT('Ctrl Pts',(-4.37842246733328,-2.04846340327406,
1.30054899424822E-15));
#70223=CARTESIAN_POINT('Ctrl Pts',(-4.3658818524655,-2.07840682871088,1.27675647831893E-15));
#70224=CARTESIAN_POINT('Ctrl Pts',(-4.35886905063707,-2.09515140709612,
1.26345153267066E-15));
#70225=CARTESIAN_POINT('Ctrl Pts',(-4.35175838797214,-2.11186193915223,
-4.29181623021427E-15));
#70226=CARTESIAN_POINT('Ctrl Pts',(-4.34455039841696,-2.12853778716716,
-4.44089209850063E-15));
#70227=CARTESIAN_POINT('Ctrl Pts',(-4.33665307152192,-2.14680843281913,
-4.60422486348398E-15));
#70228=CARTESIAN_POINT('Ctrl Pts',(-4.3286424353965,-2.16502924396809,5.30168465333661E-15));
#70229=CARTESIAN_POINT('Ctrl Pts',(-4.32052144132994,-2.18319526042712,
5.16253706450698E-15));
#70230=CARTESIAN_POINT('Ctrl Pts',(-4.26272706163057,-2.31247668142725,
4.17227053836974E-15));
#70231=CARTESIAN_POINT('Ctrl Pts',(-4.19931793630604,-2.4390523089761,-3.17224447424671E-16));
#70232=CARTESIAN_POINT('Ctrl Pts',(-4.1306671181063,-2.56266098762457,-5.55111512312578E-17));
#70233=CARTESIAN_POINT('Ctrl Pts',(-4.0593379123478,-2.69109221545352,2.16412797287518E-16));
#70234=CARTESIAN_POINT('Ctrl Pts',(-3.9823498940757,-2.81632115639891,3.16344549884833E-15));
#70235=CARTESIAN_POINT('Ctrl Pts',(-3.90006549167258,-2.93804355166681,
2.74780198594726E-15));
#70236=CARTESIAN_POINT('Ctrl Pts',(-3.81789453604086,-3.05959812639587,
2.33273152715138E-15));
#70237=CARTESIAN_POINT('Ctrl Pts',(-3.73044127702168,-3.17765647132671,
1.52792430062925E-15));
#70238=CARTESIAN_POINT('Ctrl Pts',(-3.63801734753769,-3.29189441139934,
2.04003480774873E-15));
#70239=CARTESIAN_POINT('Ctrl Pts',(-3.56858774848175,-3.37771087062696,
2.42473633883647E-15));
#70240=CARTESIAN_POINT('Ctrl Pts',(-3.49635207705255,-3.46137105631218,
2.6380387160668E-15));
#70241=CARTESIAN_POINT('Ctrl Pts',(-3.42142672585507,-3.54272626619495,
2.95596880306448E-15));
#70242=CARTESIAN_POINT('Ctrl Pts',(-3.38629422705786,-3.58087372586878,
3.10504622773483E-15));
#70243=CARTESIAN_POINT('Ctrl Pts',(-3.3505701767281,-3.61851424013804,2.76570113010457E-15));
#70244=CARTESIAN_POINT('Ctrl Pts',(-3.31426568073248,-3.6556315716941,2.76167977375508E-15));
#70245=CARTESIAN_POINT('Ctrl Pts',(-3.29921135129803,-3.67102295839838,
2.76001224411176E-15));
#70246=CARTESIAN_POINT('Ctrl Pts',(-3.2840555690535,-3.68632600746954,3.617329513469E-16));
#70247=CARTESIAN_POINT('Ctrl Pts',(-3.26880440302003,-3.70153424964867,
5.13478148889135E-16));
#70248=CARTESIAN_POINT('Ctrl Pts',(-3.16314622619418,-3.8068950553632,1.56474995848081E-15));
#70249=CARTESIAN_POINT('Ctrl Pts',(-3.05312027550677,-3.90750387615403,
1.50739186887073E-15));
#70250=CARTESIAN_POINT('Ctrl Pts',(-2.93906465882528,-4.00303742675364,
1.35308431126191E-15));
#70251=CARTESIAN_POINT('Ctrl Pts',(-2.83344548104308,-4.09150457426047,
1.21019053860593E-15));
#70252=CARTESIAN_POINT('Ctrl Pts',(-2.72436990580127,-4.17561968062982,
2.13759783489021E-15));
#70253=CARTESIAN_POINT('Ctrl Pts',(-2.61207533410326,-4.25510133080791,
2.0122792321331E-15));
#70254=CARTESIAN_POINT('Ctrl Pts',(-2.56057702495619,-4.29155162872077,
1.95480810018898E-15));
#70255=CARTESIAN_POINT('Ctrl Pts',(-2.50840133628958,-4.32702707245024,
2.36751160669112E-15));
#70256=CARTESIAN_POINT('Ctrl Pts',(-2.45556938566372,-4.36149843071932,
2.75474087985117E-15));
#70257=CARTESIAN_POINT('Ctrl Pts',(-2.42827777589571,-4.37930543664865,
2.95477343758642E-15));
#70258=CARTESIAN_POINT('Ctrl Pts',(-2.40081102655259,-4.39684448061502,
1.19861602340893E-15));
#70259=CARTESIAN_POINT('Ctrl Pts',(-2.3731719452944,-4.41411137781326,1.24206200879939E-15));
#70260=CARTESIAN_POINT('Ctrl Pts',(-2.35240993886931,-4.42708197648195,
1.27469789200386E-15));
#70261=CARTESIAN_POINT('Ctrl Pts',(-2.3315588675056,-4.43989388919032,-2.42681870829991E-15));
#70262=CARTESIAN_POINT('Ctrl Pts',(-2.310621268056,-4.45254499954709,-2.38004060904018E-15));
#70263=CARTESIAN_POINT('Ctrl Pts',(-2.18359867883944,-4.52929576545271,
-2.09625089852901E-15));
#70264=CARTESIAN_POINT('Ctrl Pts',(-2.0533809663479,-4.60013945799199,1.86447051626453E-17));
#70265=CARTESIAN_POINT('Ctrl Pts',(-1.92026980955225,-4.66473533433833,
-1.2490009027033E-16));
#70266=CARTESIAN_POINT('Ctrl Pts',(-1.7911873441691,-4.72737617657195,-2.64100413770296E-16));
#70267=CARTESIAN_POINT('Ctrl Pts',(-1.65938332691157,-4.78414205363558,
1.04097051092433E-15));
#70268=CARTESIAN_POINT('Ctrl Pts',(-1.52510574125302,-4.83468405991464,
1.71217207078911E-15));
#70269=CARTESIAN_POINT('Ctrl Pts',(-1.45664804130053,-4.8604514989394,2.07094871730909E-15));
#70270=CARTESIAN_POINT('Ctrl Pts',(-1.38754702424773,-4.88460057019718,
-4.86141022577448E-16));
#70271=CARTESIAN_POINT('Ctrl Pts',(-1.31785621200041,-4.90714516622019,
-4.9960036108132E-16));
#70272=CARTESIAN_POINT('Ctrl Pts',(-4.51483246697105,0.00361950456559231,
7.11258330249198));
#70273=CARTESIAN_POINT('Ctrl Pts',(-4.5183463327351,0.455094042321683,7.09669960179219));
#70274=CARTESIAN_POINT('Ctrl Pts',(-4.45593254783999,0.905622974345749,
7.08081590109239));
#70275=CARTESIAN_POINT('Ctrl Pts',(-4.32353239297286,1.33455648409566,7.0649322003926));
#70276=CARTESIAN_POINT('Ctrl Pts',(-3.88730691409435,2.74778538768327,7.01259936927858));
#70277=CARTESIAN_POINT('Ctrl Pts',(-2.69135272588913,3.92658775510004,6.96026653816456));
#70278=CARTESIAN_POINT('Ctrl Pts',(-1.27193484569267,4.34236679115612,6.90793370705054));
#70279=CARTESIAN_POINT('Ctrl Pts',(0.147483034503799,4.75814582721219,6.85560087593652));
#70280=CARTESIAN_POINT('Ctrl Pts',(1.7903646066915,4.41090153190756,6.8032680448225));
#70281=CARTESIAN_POINT('Ctrl Pts',(2.92016317867997,3.45636397543961,6.75093521370848));
#70282=CARTESIAN_POINT('Ctrl Pts',(4.04996175066844,2.50182641897166,6.69860238259446));
#70283=CARTESIAN_POINT('Ctrl Pts',(4.66667732245768,0.939995601340394,6.64626955148044));
#70284=CARTESIAN_POINT('Ctrl Pts',(4.49379055447605,-0.528910651078803,
6.59393672036643));
#70285=CARTESIAN_POINT('Ctrl Pts',(4.32090378649441,-1.997816903498,6.54160388925241));
#70286=CARTESIAN_POINT('Ctrl Pts',(3.35841467874189,-3.37379859070514,6.48927105813838));
#70287=CARTESIAN_POINT('Ctrl Pts',(2.03786057988447,-4.03992744750561,6.43693822702436));
#70288=CARTESIAN_POINT('Ctrl Pts',(0.717306481027035,-4.70605630430607,
6.38460539591034));
#70289=CARTESIAN_POINT('Ctrl Pts',(-0.961312608935302,-4.66233233069989,
6.33227256479632));
#70290=CARTESIAN_POINT('Ctrl Pts',(-2.24539882471135,-3.92836528976861,
6.27993973368231));
#70291=CARTESIAN_POINT('Ctrl Pts',(-3.5294850404874,-3.19439824883733,6.22760690256829));
#70292=CARTESIAN_POINT('Ctrl Pts',(-4.41903838207715,-1.77018814058096,
6.17527407145427));
#70293=CARTESIAN_POINT('Ctrl Pts',(-4.51522851969403,-0.294270927746662,
6.12294124034025));
#70294=CARTESIAN_POINT('Ctrl Pts',(-4.52157464089458,-0.196897644511263,
6.11948859439083));
#70295=CARTESIAN_POINT('Ctrl Pts',(-4.52446751475242,-0.0992992973699645,
6.1160359484414));
#70296=CARTESIAN_POINT('Ctrl Pts',(-4.52399690261043,-0.00167256832429505,
6.11258330249198));
#70297=CARTESIAN_POINT('Ctrl Pts',(-1.31303618635644,-4.90075024188323,
8.));
#70298=CARTESIAN_POINT('Ctrl Pts',(-1.45239709211802,-4.85517655769009,
8.));
#70299=CARTESIAN_POINT('Ctrl Pts',(-1.58927461952972,-4.80351078633936,
8.));
#70300=CARTESIAN_POINT('Ctrl Pts',(-1.72340721958534,-4.74604566824414,
8.));
#70301=CARTESIAN_POINT('Ctrl Pts',(-1.85924970425712,-4.68784800100459,
8.));
#70302=CARTESIAN_POINT('Ctrl Pts',(-1.99227741877149,-4.62370180241543,
8.));
#70303=CARTESIAN_POINT('Ctrl Pts',(-2.1221970609313,-4.55386234778148,8.));
#70304=CARTESIAN_POINT('Ctrl Pts',(-2.25246970806005,-4.48383313219911,
8.));
#70305=CARTESIAN_POINT('Ctrl Pts',(-2.37961793682551,-4.40807921917534,
8.));
#70306=CARTESIAN_POINT('Ctrl Pts',(-2.50331578855033,-4.32681572428032,
8.));
#70307=CARTESIAN_POINT('Ctrl Pts',(-2.62609342189428,-4.24615676827303,
8.));
#70308=CARTESIAN_POINT('Ctrl Pts',(-2.74547232113475,-4.16006940168606,
8.));
#70309=CARTESIAN_POINT('Ctrl Pts',(-2.86109611850811,-4.06872967104376,
8.));
#70310=CARTESIAN_POINT('Ctrl Pts',(-2.9021226048247,-4.0363198359191,8.));
#70311=CARTESIAN_POINT('Ctrl Pts',(-2.94267593191283,-4.00324843420239,
8.));
#70312=CARTESIAN_POINT('Ctrl Pts',(-2.98273884627905,-3.96952246026761,
8.));
#70313=CARTESIAN_POINT('Ctrl Pts',(-2.99980179304064,-3.95515844040447,
8.));
#70314=CARTESIAN_POINT('Ctrl Pts',(-3.01677686159523,-3.94067464141144,
8.));
#70315=CARTESIAN_POINT('Ctrl Pts',(-3.03364692784275,-3.92608549145045,
8.));
#70316=CARTESIAN_POINT('Ctrl Pts',(-3.14433906287484,-3.83035947983968,
8.));
#70317=CARTESIAN_POINT('Ctrl Pts',(-3.25067173076357,-3.72996938710921,
8.));
#70318=CARTESIAN_POINT('Ctrl Pts',(-3.35235942406226,-3.62515267891276,
8.));
#70319=CARTESIAN_POINT('Ctrl Pts',(-3.36192701172294,-3.61529068862227,
8.));
#70320=CARTESIAN_POINT('Ctrl Pts',(-3.37145345441303,-3.60538948288356,
8.));
#70321=CARTESIAN_POINT('Ctrl Pts',(-3.38093849819353,-3.5954492420827,8.));
#70322=CARTESIAN_POINT('Ctrl Pts',(-3.48179697338609,-3.48975046478426,
8.));
#70323=CARTESIAN_POINT('Ctrl Pts',(-3.57797791034191,-3.37964062514819,
8.));
#70324=CARTESIAN_POINT('Ctrl Pts',(-3.6691784190789,-3.26549870852508,8.));
#70325=CARTESIAN_POINT('Ctrl Pts',(-3.75971104108468,-3.1521926849539,8.));
#70326=CARTESIAN_POINT('Ctrl Pts',(-3.84533634314077,-3.03491270174392,
8.));
#70327=CARTESIAN_POINT('Ctrl Pts',(-3.92571335075401,-2.91400477707446,
8.));
#70328=CARTESIAN_POINT('Ctrl Pts',(-3.99657459670685,-2.80741103289235,
8.));
#70329=CARTESIAN_POINT('Ctrl Pts',(-4.06335624155544,-2.69799686623316,
8.));
#70330=CARTESIAN_POINT('Ctrl Pts',(-4.12579142887319,-2.5859898555039,8.));
#70331=CARTESIAN_POINT('Ctrl Pts',(-4.14218052019666,-2.55658827593677,
8.));
#70332=CARTESIAN_POINT('Ctrl Pts',(-4.15826993976141,-2.52700800600865,
8.));
#70333=CARTESIAN_POINT('Ctrl Pts',(-4.17405446883537,-2.49725311040552,
8.));
#70334=CARTESIAN_POINT('Ctrl Pts',(-4.18546373911311,-2.47574587097943,
8.));
#70335=CARTESIAN_POINT('Ctrl Pts',(-4.19671529109329,-2.45414413479639,
8.));
#70336=CARTESIAN_POINT('Ctrl Pts',(-4.20779517261687,-2.4324732839539,8.));
#70337=CARTESIAN_POINT('Ctrl Pts',(-4.27314976421176,-2.30464794545096,
8.));
#70338=CARTESIAN_POINT('Ctrl Pts',(-4.33262109126524,-2.17426237076666,
8.));
#70339=CARTESIAN_POINT('Ctrl Pts',(-4.38592494350939,-2.0416738299269,8.));
#70340=CARTESIAN_POINT('Ctrl Pts',(-4.43841400089354,-1.91111201805743,
8.));
#70341=CARTESIAN_POINT('Ctrl Pts',(-4.48492299905459,-1.7784133775905,8.));
#70342=CARTESIAN_POINT('Ctrl Pts',(-4.52513335521759,-1.64390172617838,
8.));
#70343=CARTESIAN_POINT('Ctrl Pts',(-4.537048107786,-1.60404450537571,8.));
#70344=CARTESIAN_POINT('Ctrl Pts',(-4.54840950403996,-1.5640280227951,8.));
#70345=CARTESIAN_POINT('Ctrl Pts',(-4.55920838150573,-1.52386053965931,
8.));
#70346=CARTESIAN_POINT('Ctrl Pts',(-4.59649237875198,-1.385179057684,8.));
#70347=CARTESIAN_POINT('Ctrl Pts',(-4.62707496138222,-1.24469748534875,
8.));
#70348=CARTESIAN_POINT('Ctrl Pts',(-4.65105491040296,-1.10285889077504,
8.));
#70349=CARTESIAN_POINT('Ctrl Pts',(-4.66554282028716,-1.017164597826,8.));
#70350=CARTESIAN_POINT('Ctrl Pts',(-4.67761961594462,-0.930974942162248,
8.));
#70351=CARTESIAN_POINT('Ctrl Pts',(-4.68729801221865,-0.844388845291519,
8.));
#70352=CARTESIAN_POINT('Ctrl Pts',(-4.69282817886049,-0.794914166739051,
8.));
#70353=CARTESIAN_POINT('Ctrl Pts',(-4.69757516967293,-0.745310079919106,
8.));
#70354=CARTESIAN_POINT('Ctrl Pts',(-4.70154039472519,-0.695595329877529,
8.));
#70355=CARTESIAN_POINT('Ctrl Pts',(-4.70301053775668,-0.677163136906814,
8.));
#70356=CARTESIAN_POINT('Ctrl Pts',(-4.70437287652954,-0.658719449757616,
8.));
#70357=CARTESIAN_POINT('Ctrl Pts',(-4.70562704431493,-0.64027493011297,
8.));
#70358=CARTESIAN_POINT('Ctrl Pts',(-4.71515809633756,-0.500105745165328,
8.));
#70359=CARTESIAN_POINT('Ctrl Pts',(-4.71845973908213,-0.359723770205855,
8.));
#70360=CARTESIAN_POINT('Ctrl Pts',(-4.71568669686701,-0.219543283976319,
8.));
#70361=CARTESIAN_POINT('Ctrl Pts',(-4.71286811953556,-0.0770609450327588,
8.));
#70362=CARTESIAN_POINT('Ctrl Pts',(-4.70377361453064,0.0652140588645918,
8.));
#70363=CARTESIAN_POINT('Ctrl Pts',(-4.68851230252744,0.206844911988138,
8.));
#70364=CARTESIAN_POINT('Ctrl Pts',(-4.67333458060724,0.347700016947462,
8.));
#70365=CARTESIAN_POINT('Ctrl Pts',(-4.65205714501789,0.487918806531984,
8.));
#70366=CARTESIAN_POINT('Ctrl Pts',(-4.62473814484182,0.627057654071025,
8.));
#70367=CARTESIAN_POINT('Ctrl Pts',(-4.605133388788,0.726906958439074,8.));
#70368=CARTESIAN_POINT('Ctrl Pts',(-4.5824162991499,0.826199852698566,8.));
#70369=CARTESIAN_POINT('Ctrl Pts',(-4.55659376741278,0.92476446952987,8.));
#70370=CARTESIAN_POINT('Ctrl Pts',(-4.54451944953447,0.97085214703918,8.));
#70371=CARTESIAN_POINT('Ctrl Pts',(-4.53176599217756,1.01678048248609,8.));
#70372=CARTESIAN_POINT('Ctrl Pts',(-4.5183332282825,1.06253124418397,8.));
#70373=CARTESIAN_POINT('Ctrl Pts',(-4.51267692512135,1.08179609392292,8.));
#70374=CARTESIAN_POINT('Ctrl Pts',(-4.50690016711964,1.10102945232834,8.));
#70375=CARTESIAN_POINT('Ctrl Pts',(-4.50100291315461,1.12022993263941,8.));
#70376=CARTESIAN_POINT('Ctrl Pts',(-4.49471977615854,1.14068678406554,8.));
#70377=CARTESIAN_POINT('Ctrl Pts',(-4.48830254703555,1.16109751332069,8.));
#70378=CARTESIAN_POINT('Ctrl Pts',(-4.48175248385615,1.18145762320509,8.));
#70379=CARTESIAN_POINT('Ctrl Pts',(-4.43884234970562,1.31483878649018,8.));
#70380=CARTESIAN_POINT('Ctrl Pts',(-4.39022235830023,1.4460911608231,8.));
#70381=CARTESIAN_POINT('Ctrl Pts',(-4.33596033524399,1.57478158992507,8.));
#70382=CARTESIAN_POINT('Ctrl Pts',(-4.28905827705606,1.68601677162324,8.));
#70383=CARTESIAN_POINT('Ctrl Pts',(-4.23794008569217,1.79533788193322,8.));
#70384=CARTESIAN_POINT('Ctrl Pts',(-4.18262262022186,1.90244778297798,8.));
#70385=CARTESIAN_POINT('Ctrl Pts',(-4.15876953368252,1.94863395071215,8.));
#70386=CARTESIAN_POINT('Ctrl Pts',(-4.13413534457581,1.9944087336574,8.));
#70387=CARTESIAN_POINT('Ctrl Pts',(-4.10872005342092,2.03974709902823,8.));
#70388=CARTESIAN_POINT('Ctrl Pts',(-4.09757333138634,2.05963174851782,8.));
#70389=CARTESIAN_POINT('Ctrl Pts',(-4.08627634995272,2.07943244040586,8.));
#70390=CARTESIAN_POINT('Ctrl Pts',(-4.0748290615074,2.09914701235749,8.));
#70391=CARTESIAN_POINT('Ctrl Pts',(-4.06286920268517,2.11974433533126,8.));
#70392=CARTESIAN_POINT('Ctrl Pts',(-4.05074975381766,2.1402399100487,8.));
#70393=CARTESIAN_POINT('Ctrl Pts',(-4.0384724823486,2.16062907002492,8.));
#70394=CARTESIAN_POINT('Ctrl Pts',(-3.96920273979072,2.27566699731059,8.));
#70395=CARTESIAN_POINT('Ctrl Pts',(-3.89489711290362,2.38734570786034,8.));
#70396=CARTESIAN_POINT('Ctrl Pts',(-3.81559004701476,2.49525769668179,8.));
#70397=CARTESIAN_POINT('Ctrl Pts',(-3.739663695997,2.59856959519238,8.));
#70398=CARTESIAN_POINT('Ctrl Pts',(-3.65915281331369,2.69842939750744,8.));
#70399=CARTESIAN_POINT('Ctrl Pts',(-3.57405581868196,2.79444797267076,8.));
#70400=CARTESIAN_POINT('Ctrl Pts',(-3.53072763156913,2.8433370175658,8.));
#70401=CARTESIAN_POINT('Ctrl Pts',(-3.48620998149697,2.89122965827726,8.));
#70402=CARTESIAN_POINT('Ctrl Pts',(-3.44054916109509,2.93810681611542,8.));
#70403=CARTESIAN_POINT('Origin',(-1.11022302462516E-15,0.,8.));
#70404=CARTESIAN_POINT('',(4.90747728811182,-8.5,8.));
#70405=CARTESIAN_POINT('',(9.81495457622364,0.,8.));
#70406=CARTESIAN_POINT('',(4.90747728811182,-8.5,8.));
#70407=CARTESIAN_POINT('',(4.90747728811182,8.5,8.));
#70408=CARTESIAN_POINT('',(9.81495457622364,0.,8.));
#70409=CARTESIAN_POINT('',(-4.90747728811182,8.5,8.));
#70410=CARTESIAN_POINT('',(4.90747728811182,8.5,8.));
#70411=CARTESIAN_POINT('',(-9.81495457622364,1.11022302462516E-15,8.));
#70412=CARTESIAN_POINT('',(-4.90747728811182,8.5,8.));
#70413=CARTESIAN_POINT('',(-4.90747728811182,-8.5,8.));
#70414=CARTESIAN_POINT('',(-9.81495457622364,1.20198527055489E-15,8.));
#70415=CARTESIAN_POINT('',(-4.90747728811182,-8.5,8.));
#70416=CARTESIAN_POINT('Origin',(0.,0.,4.));
#70417=CARTESIAN_POINT('Origin',(-4.90747728811182,-8.5,0.));
#70418=CARTESIAN_POINT('',(-4.90747728811182,-8.5,0.));
#70419=CARTESIAN_POINT('',(4.90747728811182,-8.5,0.));
#70420=CARTESIAN_POINT('',(-4.90747728811182,-8.5,0.));
#70421=CARTESIAN_POINT('',(4.90747728811182,-8.5,0.));
#70422=CARTESIAN_POINT('',(-4.90747728811182,-8.5,0.));
#70423=CARTESIAN_POINT('Origin',(-9.81495457622364,1.20198527055489E-15,
0.));
#70424=CARTESIAN_POINT('',(-9.81495457622364,1.20198527055489E-15,0.));
#70425=CARTESIAN_POINT('',(-9.81495457622364,1.20198527055489E-15,0.));
#70426=CARTESIAN_POINT('',(-9.81495457622364,1.20198527055489E-15,0.));
#70427=CARTESIAN_POINT('Origin',(-4.90747728811182,8.5,0.));
#70428=CARTESIAN_POINT('',(-4.90747728811182,8.5,0.));
#70429=CARTESIAN_POINT('',(-4.90747728811182,8.5,0.));
#70430=CARTESIAN_POINT('',(-4.90747728811182,8.5,0.));
#70431=CARTESIAN_POINT('Origin',(4.90747728811182,8.5,0.));
#70432=CARTESIAN_POINT('',(4.90747728811182,8.5,0.));
#70433=CARTESIAN_POINT('',(4.90747728811182,8.5,0.));
#70434=CARTESIAN_POINT('',(4.90747728811182,8.5,0.));
#70435=CARTESIAN_POINT('Origin',(9.81495457622364,0.,0.));
#70436=CARTESIAN_POINT('',(9.81495457622364,0.,0.));
#70437=CARTESIAN_POINT('',(9.81495457622364,0.,0.));
#70438=CARTESIAN_POINT('',(9.81495457622364,0.,0.));
#70439=CARTESIAN_POINT('Origin',(4.90747728811182,-8.5,0.));
#70440=CARTESIAN_POINT('',(4.90747728811182,-8.5,0.));
#70441=CARTESIAN_POINT('Origin',(-1.11022302462516E-15,0.,0.));
#70442=CARTESIAN_POINT('',(0.,0.,0.));
#70443=CARTESIAN_POINT('Origin',(0.,0.,0.));
#70444=CARTESIAN_POINT('',(-5.5,-6.73555739531044E-16,2.));
#70445=CARTESIAN_POINT('Origin',(0.,0.,2.));
#70446=CARTESIAN_POINT('',(-5.5,-6.73555739531044E-16,0.));
#70447=CARTESIAN_POINT('',(-5.5,-6.73555739531044E-16,0.));
#70448=CARTESIAN_POINT('Origin',(0.,0.,0.));
#70449=CARTESIAN_POINT('Origin',(0.,0.,0.));
#70450=CARTESIAN_POINT('',(-11.,-1.34711147906209E-15,2.));
#70451=CARTESIAN_POINT('Origin',(0.,0.,2.));
#70452=CARTESIAN_POINT('',(-11.,-1.34711147906209E-15,0.));
#70453=CARTESIAN_POINT('',(-11.,-1.34711147906209E-15,0.));
#70454=CARTESIAN_POINT('Origin',(0.,0.,0.));
#70455=CARTESIAN_POINT('Origin',(0.,0.,2.));
#70456=CARTESIAN_POINT('Origin',(0.,0.,0.));
#70457=CARTESIAN_POINT('',(0.,0.,0.));
#70458=CARTESIAN_POINT('Origin',(0.,0.,0.));
#70459=CARTESIAN_POINT('',(-2.94490570994055,0.00214417779480537,0.322176117089595));
#70460=CARTESIAN_POINT('',(-2.94453111094736,0.00313617179185542,0.177823882910391));
#70461=CARTESIAN_POINT('',(-2.942,-3.60291088309151E-16,0.));
#70462=CARTESIAN_POINT('',(1.28892185405323,2.64462557919718,0.));
#70463=CARTESIAN_POINT('Ctrl Pts',(-2.94490570994055,0.00214417779480537,
0.322176117089595));
#70464=CARTESIAN_POINT('Ctrl Pts',(-2.94584715833611,0.124808428590093,
0.315520895872749));
#70465=CARTESIAN_POINT('Ctrl Pts',(-2.93884007386573,0.247358426874668,
0.308865674655903));
#70466=CARTESIAN_POINT('Ctrl Pts',(-2.92351947045398,0.368852411761562,
0.302210453439057));
#70467=CARTESIAN_POINT('Ctrl Pts',(-2.80238513102988,1.32946037267173,0.249590083068687));
#70468=CARTESIAN_POINT('Ctrl Pts',(-2.16153286152783,2.22405187279705,0.196969712698316));
#70469=CARTESIAN_POINT('Ctrl Pts',(-1.29099252632988,2.64857098947325,0.144349342327946));
#70470=CARTESIAN_POINT('Ctrl Pts',(-0.494964144347145,3.03675434170317,
0.0962328948852971));
#70471=CARTESIAN_POINT('Ctrl Pts',(0.493115753268411,3.03189109212113,0.0481164474426485));
#70472=CARTESIAN_POINT('Ctrl Pts',(1.29200104020318,2.64812001020929,-1.63834222883338E-16));
#70473=CARTESIAN_POINT('',(-1.28892185405328,2.64462557919715,0.));
#70474=CARTESIAN_POINT('Origin',(0.,0.,0.));
#70475=CARTESIAN_POINT('Ctrl Pts',(-1.28892185405328,2.64462557919715,2.08166817117217E-15));
#70476=CARTESIAN_POINT('Ctrl Pts',(-2.16403831185616,2.21811653527939,0.0526649636666859));
#70477=CARTESIAN_POINT('Ctrl Pts',(-2.80357657272064,1.32706756586464,0.10532992733337));
#70478=CARTESIAN_POINT('Ctrl Pts',(-2.92355402589586,0.366959843828546,
0.157994891000053));
#70479=CARTESIAN_POINT('Ctrl Pts',(-2.93861167702227,0.246462477535227,
0.164604554970166));
#70480=CARTESIAN_POINT('Ctrl Pts',(-2.94548559297357,0.124877349165528,
0.171214218940278));
#70481=CARTESIAN_POINT('Ctrl Pts',(-2.94453111094736,0.00313617179185542,
0.177823882910391));
#70482=CARTESIAN_POINT('Origin',(0.,0.,0.));
#70483=CARTESIAN_POINT('',(-2.93741501075088,0.000605053430647595,1.3221761170896));
#70484=CARTESIAN_POINT('',(-2.93743260967528,0.000720687897601403,1.17782388291039));
#70485=CARTESIAN_POINT('',(-2.942,-3.60291088309151E-16,0.));
#70486=CARTESIAN_POINT('Ctrl Pts',(-2.93741501075088,0.000605053430647595,
1.3221761170896));
#70487=CARTESIAN_POINT('Ctrl Pts',(-2.9382479568139,0.450815163107398,1.29790978476164));
#70488=CARTESIAN_POINT('Ctrl Pts',(-2.84099804532476,0.900683451883265,
1.27364345243368));
#70489=CARTESIAN_POINT('Ctrl Pts',(-2.64378204823906,1.30134356458571,1.24937712010572));
#70490=CARTESIAN_POINT('Ctrl Pts',(-2.21612867774369,2.17015567999336,1.19675674973535));
#70491=CARTESIAN_POINT('Ctrl Pts',(-1.31841648749453,2.80758195059898,1.14413637936498));
#70492=CARTESIAN_POINT('Ctrl Pts',(-0.357192829781819,2.92497002089294,
1.09151600899461));
#70493=CARTESIAN_POINT('Ctrl Pts',(0.604030827930888,3.04235809118689,1.03889563862424));
#70494=CARTESIAN_POINT('Ctrl Pts',(1.62876595310715,2.63970796116917,0.986275268253872));
#70495=CARTESIAN_POINT('Ctrl Pts',(2.25292793158662,1.89932766827126,0.933654897883501));
#70496=CARTESIAN_POINT('Ctrl Pts',(2.8770899100661,1.15894737537334,0.881034527513131));
#70497=CARTESIAN_POINT('Ctrl Pts',(3.1006787418488,0.0808369195952267,0.828414157142761));
#70498=CARTESIAN_POINT('Ctrl Pts',(2.82245137682484,-0.846673957408537,
0.775793786772391));
#70499=CARTESIAN_POINT('Ctrl Pts',(2.54422401180089,-1.7741848344123,0.72317341640202));
#70500=CARTESIAN_POINT('Ctrl Pts',(1.76418044997028,-2.55109613264171,0.67055304603165));
#70501=CARTESIAN_POINT('Ctrl Pts',(0.835554749603298,-2.82571794203434,
0.617932675661279));
#70502=CARTESIAN_POINT('Ctrl Pts',(-0.0930709507636752,-3.10033975142697,
0.565312305290909));
#70503=CARTESIAN_POINT('Ctrl Pts',(-1.17027878966702,-2.87267207198282,
0.512691934920538));
#70504=CARTESIAN_POINT('Ctrl Pts',(-1.90817450444562,-2.24552602141323,
0.460071564550168));
#70505=CARTESIAN_POINT('Ctrl Pts',(-2.55274401908064,-1.69769898118953,
0.414106415396644));
#70506=CARTESIAN_POINT('Ctrl Pts',(-2.93840347440061,-0.845052391620324,
0.368141266243119));
#70507=CARTESIAN_POINT('Ctrl Pts',(-2.94490570994055,0.00214417779480537,
0.322176117089595));
#70508=CARTESIAN_POINT('Ctrl Pts',(-2.94453111094736,0.00313617179185542,
0.177823882910391));
#70509=CARTESIAN_POINT('Ctrl Pts',(-2.93788040132423,-0.845140901703999,
0.223879182606963));
#70510=CARTESIAN_POINT('Ctrl Pts',(-2.55115114237882,-1.7009943502416,0.269934482303535));
#70511=CARTESIAN_POINT('Ctrl Pts',(-1.90455354763271,-2.24922658650796,
0.315989782000107));
#70512=CARTESIAN_POINT('Ctrl Pts',(-1.16515897070839,-2.87613882015091,
0.368654745666792));
#70513=CARTESIAN_POINT('Ctrl Pts',(-0.0859531713737992,-3.10079681277935,
0.421319709333476));
#70514=CARTESIAN_POINT('Ctrl Pts',(0.842833952810694,-2.82335342322726,
0.473984673000161));
#70515=CARTESIAN_POINT('Ctrl Pts',(1.77162107699519,-2.54591003367518,0.526649636666845));
#70516=CARTESIAN_POINT('Ctrl Pts',(2.54998952602959,-1.76636526194256,0.57931460033353));
#70517=CARTESIAN_POINT('Ctrl Pts',(2.82526196809064,-0.837265996441287,
0.631979564000215));
#70518=CARTESIAN_POINT('Ctrl Pts',(3.1005344101517,0.0918332690599885,0.684644527666899));
#70519=CARTESIAN_POINT('Ctrl Pts',(2.87271084523941,1.17048702832993,0.737309491333584));
#70520=CARTESIAN_POINT('Ctrl Pts',(2.2449320231631,1.90890163868963,0.789974455000268));
#70521=CARTESIAN_POINT('Ctrl Pts',(1.61715320108678,2.64731624904933,0.842639418666953));
#70522=CARTESIAN_POINT('Ctrl Pts',(0.589419121846451,3.0454917104988,0.895304382333637));
#70523=CARTESIAN_POINT('Ctrl Pts',(-0.37200976733393,2.9231058378395,0.947969346000322));
#70524=CARTESIAN_POINT('Ctrl Pts',(-1.33343865651431,2.8007199651802,1.00063430966701));
#70525=CARTESIAN_POINT('Ctrl Pts',(-2.22856235563474,2.15777275841214,1.05329927333369));
#70526=CARTESIAN_POINT('Ctrl Pts',(-2.6514251854394,1.28574400496261,1.10596423700038));
#70527=CARTESIAN_POINT('Ctrl Pts',(-2.8437527539192,0.889125626674557,1.12991745230371));
#70528=CARTESIAN_POINT('Ctrl Pts',(-2.93838674329414,0.445118617110292,
1.15387066760705));
#70529=CARTESIAN_POINT('Ctrl Pts',(-2.93743260967528,0.000720687897601403,
1.17782388291039));
#70530=CARTESIAN_POINT('Origin',(0.,0.,0.));
#70531=CARTESIAN_POINT('',(-2.94283216929169,-0.00254059509496668,2.3221761170896));
#70532=CARTESIAN_POINT('',(-2.94249560619114,-0.00258942729680482,2.17782388291039));
#70533=CARTESIAN_POINT('',(-2.942,-3.60291088309151E-16,0.));
#70534=CARTESIAN_POINT('Ctrl Pts',(-2.94283216929169,-0.00254059509496668,
2.3221761170896));
#70535=CARTESIAN_POINT('Ctrl Pts',(-2.93583836831966,0.770783310741536,
2.28029867365053));
#70536=CARTESIAN_POINT('Ctrl Pts',(-2.62244249954969,1.54912568223824,2.23842123021146));
#70537=CARTESIAN_POINT('Ctrl Pts',(-2.07534059520784,2.09189740289201,2.19654378677239));
#70538=CARTESIAN_POINT('Ctrl Pts',(-1.38788924974329,2.77390773164861,2.14392341640202));
#70539=CARTESIAN_POINT('Ctrl Pts',(-0.331445515483537,3.08398167899393,
2.09130304603165));
#70540=CARTESIAN_POINT('Ctrl Pts',(0.615553755286461,2.88169496582278,2.03868267566128));
#70541=CARTESIAN_POINT('Ctrl Pts',(1.56255302605646,2.67940825265162,1.98606230529091));
#70542=CARTESIAN_POINT('Ctrl Pts',(2.40010783333669,1.96476087896396,1.93344193492054));
#70543=CARTESIAN_POINT('Ctrl Pts',(2.74891040156469,1.06139789331815,1.88082156455017));
#70544=CARTESIAN_POINT('Ctrl Pts',(3.09771296979268,0.158034907672333,1.8282011941798));
#70545=CARTESIAN_POINT('Ctrl Pts',(2.95776329896845,-0.934043689931643,
1.77558082380943));
#70546=CARTESIAN_POINT('Ctrl Pts',(2.39244139669332,-1.72026117030417,1.72296045343906));
#70547=CARTESIAN_POINT('Ctrl Pts',(1.82711949441818,-2.50647865067671,1.67034008306869));
#70548=CARTESIAN_POINT('Ctrl Pts',(0.836425360692154,-2.9868350138178,1.61771971269832));
#70549=CARTESIAN_POINT('Ctrl Pts',(-0.130980997368149,-2.9437920444354,
1.56509934232795));
#70550=CARTESIAN_POINT('Ctrl Pts',(-1.09838735542844,-2.90074907505299,
1.51247897195758));
#70551=CARTESIAN_POINT('Ctrl Pts',(-2.04250593782301,-2.33430677314711,
1.45985860158721));
#70552=CARTESIAN_POINT('Ctrl Pts',(-2.5357679536495,-1.50098664208934,1.40723823121684));
#70553=CARTESIAN_POINT('Ctrl Pts',(-2.80155798635321,-1.05195919262036,
1.37888419317442));
#70554=CARTESIAN_POINT('Ctrl Pts',(-2.93644175348072,-0.525443729069001,
1.35053015513201));
#70555=CARTESIAN_POINT('Ctrl Pts',(-2.93741501075088,0.000605053430647595,
1.3221761170896));
#70556=CARTESIAN_POINT('Ctrl Pts',(-2.93743260967528,0.000720687897601403,
1.17782388291039));
#70557=CARTESIAN_POINT('Ctrl Pts',(-2.93628892837727,-0.53196109845813,
1.20653563127374));
#70558=CARTESIAN_POINT('Ctrl Pts',(-2.79780571115684,-1.06520455211536,
1.23524737963708));
#70559=CARTESIAN_POINT('Ctrl Pts',(-2.52560900690579,-1.51806949138664,
1.26395912800043));
#70560=CARTESIAN_POINT('Ctrl Pts',(-2.02632803807862,-2.34874393415536,
1.31662409166711));
#70561=CARTESIAN_POINT('Ctrl Pts',(-1.07716413993538,-2.9089825195618,1.3692890553338));
#70562=CARTESIAN_POINT('Ctrl Pts',(-0.108652539320438,-2.94471329972367,
1.42195401900048));
#70563=CARTESIAN_POINT('Ctrl Pts',(0.85985906129451,-2.98044407988555,1.47461898266717));
#70564=CARTESIAN_POINT('Ctrl Pts',(1.84771836438116,-2.49166705480286,1.52728394633385));
#70565=CARTESIAN_POINT('Ctrl Pts',(2.40686102399513,-1.70005997098112,1.57994891000054));
#70566=CARTESIAN_POINT('Ctrl Pts',(2.9660036836091,-0.908452887159384,1.63261387366722));
#70567=CARTESIAN_POINT('Ctrl Pts',(3.09642969975039,0.185984255401396,1.68527883733391));
#70568=CARTESIAN_POINT('Ctrl Pts',(2.73897659148843,1.08682694396802,1.73794380100059));
#70569=CARTESIAN_POINT('Ctrl Pts',(2.38152348322647,1.98766963253464,1.79060876466727));
#70570=CARTESIAN_POINT('Ctrl Pts',(1.53619125056127,2.69491786710711,1.84327372833396));
#70571=CARTESIAN_POINT('Ctrl Pts',(0.586406744725485,2.88778465426983,1.89593869200064));
#70572=CARTESIAN_POINT('Ctrl Pts',(-0.363377761110303,3.08065144143255,
1.94860365566733));
#70573=CARTESIAN_POINT('Ctrl Pts',(-1.41761454011667,2.75913678118554,2.00126861933401));
#70574=CARTESIAN_POINT('Ctrl Pts',(-2.09812527093809,2.0690698668059,2.0539335830007));
#70575=CARTESIAN_POINT('Ctrl Pts',(-2.63174175688638,1.52795998382732,2.09523034963726));
#70576=CARTESIAN_POINT('Ctrl Pts',(-2.93556254699721,0.76023565397735,2.13652711627383));
#70577=CARTESIAN_POINT('Ctrl Pts',(-2.94249560619114,-0.00258942729680482,
2.17782388291039));
#70578=CARTESIAN_POINT('Origin',(0.,0.,0.));
#70579=CARTESIAN_POINT('',(-2.94484294150901,0.00199174253909633,3.3221761170896));
#70580=CARTESIAN_POINT('',(-2.94526037616607,0.00180040430511289,3.17782388291039));
#70581=CARTESIAN_POINT('',(-2.942,-3.60291088309151E-16,0.));
#70582=CARTESIAN_POINT('Ctrl Pts',(-2.94484294150901,0.00199174253909633,
3.3221761170896));
#70583=CARTESIAN_POINT('Ctrl Pts',(-2.94583002736539,0.128597483532049,
3.31530793290979));
#70584=CARTESIAN_POINT('Ctrl Pts',(-2.93836342958051,0.255086036799256,
3.30843974872998));
#70585=CARTESIAN_POINT('Ctrl Pts',(-2.92204585589404,0.380422278131109,
3.30157156455017));
#70586=CARTESIAN_POINT('Ctrl Pts',(-2.79702929424561,1.34068182665933,3.2489511941798));
#70587=CARTESIAN_POINT('Ctrl Pts',(-2.15247739366928,2.23330287085301,3.19633082380943));
#70588=CARTESIAN_POINT('Ctrl Pts',(-1.28029158434589,2.65403966800756,3.14371045343906));
#70589=CARTESIAN_POINT('Ctrl Pts',(-0.4081057750225,3.0747764651621,3.09109008306869));
#70590=CARTESIAN_POINT('Ctrl Pts',(0.69171394304795,3.0236290152775,3.03846971269832));
#70591=CARTESIAN_POINT('Ctrl Pts',(1.5210867384019,2.5237607280468,2.98584934232795));
#70592=CARTESIAN_POINT('Ctrl Pts',(2.35045953375586,2.0238924408161,2.93322897195758));
#70593=CARTESIAN_POINT('Ctrl Pts',(2.90938540639331,1.07530331623929,2.8806086015872));
#70594=CARTESIAN_POINT('Ctrl Pts',(2.94474080948057,0.107585617606989,2.82798823121683));
#70595=CARTESIAN_POINT('Ctrl Pts',(2.98009621256783,-0.860132081025304,
2.77536786084646));
#70596=CARTESIAN_POINT('Ctrl Pts',(2.49188114610491,-1.84697835371309,2.7227474904761));
#70597=CARTESIAN_POINT('Ctrl Pts',(1.70119600494326,-2.40603518007504,2.67012712010573));
#70598=CARTESIAN_POINT('Ctrl Pts',(0.91051086378161,-2.965092006437,2.61750674973535));
#70599=CARTESIAN_POINT('Ctrl Pts',(-0.182644352078765,-3.09635938647313,
2.56488637936498));
#70600=CARTESIAN_POINT('Ctrl Pts',(-1.08320700768761,-2.74038967310636,
2.51226600899461));
#70601=CARTESIAN_POINT('Ctrl Pts',(-1.98376966329644,-2.3844199597396,2.45964563862424));
#70602=CARTESIAN_POINT('Ctrl Pts',(-2.69173975865374,-1.54121315296996,
2.40702526825387));
#70603=CARTESIAN_POINT('Ctrl Pts',(-2.88649532799773,-0.59263639450121,
2.3544048978835));
#70604=CARTESIAN_POINT('Ctrl Pts',(-2.92625644781122,-0.398975826678611,
2.3436619709522));
#70605=CARTESIAN_POINT('Ctrl Pts',(-2.94462630681883,-0.200923340849699,
2.3329190440209));
#70606=CARTESIAN_POINT('Ctrl Pts',(-2.94283216929169,-0.00254059509496668,
2.3221761170896));
#70607=CARTESIAN_POINT('Ctrl Pts',(-2.94249560619114,-0.00258942729680482,
2.17782388291039));
#70608=CARTESIAN_POINT('Ctrl Pts',(-2.94440414260591,-0.212580342560449,
2.18919207994051));
#70609=CARTESIAN_POINT('Ctrl Pts',(-2.92381470891138,-0.422199995772688,
2.20056027697063));
#70610=CARTESIAN_POINT('Ctrl Pts',(-2.87932772554241,-0.626618874207943,
2.21192847400075));
#70611=CARTESIAN_POINT('Ctrl Pts',(-2.67323476668884,-1.57362153232989,
2.26459343766743));
#70612=CARTESIAN_POINT('Ctrl Pts',(-1.95426416634525,-2.40900768006153,
2.31725840133412));
#70613=CARTESIAN_POINT('Ctrl Pts',(-1.04852602468143,-2.75386472764491,
2.3699233650008));
#70614=CARTESIAN_POINT('Ctrl Pts',(-0.142787883017607,-3.09872177522829,
2.42258832866749));
#70615=CARTESIAN_POINT('Ctrl Pts',(0.949717799966449,-2.95304972266342,
2.47525329233417));
#70616=CARTESIAN_POINT('Ctrl Pts',(1.7334537997702,-2.38292188563198,2.52791825600086));
#70617=CARTESIAN_POINT('Ctrl Pts',(2.51718979957395,-1.81279404860055,2.58058321966754));
#70618=CARTESIAN_POINT('Ctrl Pts',(2.99215611619739,-0.818210427102559,
2.63324818333423));
#70619=CARTESIAN_POINT('Ctrl Pts',(2.94291803037279,0.149706737509724,2.68591314700091));
#70620=CARTESIAN_POINT('Ctrl Pts',(2.89367994454819,1.11762390212201,2.7385781106676));
#70621=CARTESIAN_POINT('Ctrl Pts',(2.32023745627556,2.05887460984858,2.79124307433428));
#70622=CARTESIAN_POINT('Ctrl Pts',(1.4826919461771,2.54652764310569,2.84390803800096));
#70623=CARTESIAN_POINT('Ctrl Pts',(0.645146436078633,3.03418067636279,2.89657300166765));
#70624=CARTESIAN_POINT('Ctrl Pts',(-0.456502095845658,3.06823603515044,
2.94923796533433));
#70625=CARTESIAN_POINT('Ctrl Pts',(-1.32256928803916,2.63324686948073,3.00190292900102));
#70626=CARTESIAN_POINT('Ctrl Pts',(-2.18863648023266,2.19825770381101,3.0545678926677));
#70627=CARTESIAN_POINT('Ctrl Pts',(-2.81912233269536,1.29422401368392,3.10723285633439));
#70628=CARTESIAN_POINT('Ctrl Pts',(-2.92805183726137,0.331196319314338,
3.15989782000107));
#70629=CARTESIAN_POINT('Ctrl Pts',(-2.94041095304778,0.221931425219236,
3.16587317430418));
#70630=CARTESIAN_POINT('Ctrl Pts',(-2.94605601250203,0.111907094355046,
3.17184852860728));
#70631=CARTESIAN_POINT('Ctrl Pts',(-2.94526037616607,0.00180040430511289,
3.17782388291039));
#70632=CARTESIAN_POINT('Origin',(0.,0.,0.));
#70633=CARTESIAN_POINT('',(-2.93739242931988,0.000540407572186541,4.3221761170896));
#70634=CARTESIAN_POINT('',(-2.93753500859377,0.000882026442511373,4.17782388291039));
#70635=CARTESIAN_POINT('',(-2.942,-3.60291088309151E-16,0.));
#70636=CARTESIAN_POINT('Ctrl Pts',(-2.93739242931988,0.000540407572186541,
4.3221761170896));
#70637=CARTESIAN_POINT('Ctrl Pts',(-2.93814630501522,0.454709257120266,
4.29769682179868));
#70638=CARTESIAN_POINT('Ctrl Pts',(-2.83910536028106,0.908566671316128,
4.27321752650776));
#70639=CARTESIAN_POINT('Ctrl Pts',(-2.6385374625564,1.31194251096478,4.24873823121684));
#70640=CARTESIAN_POINT('Ctrl Pts',(-2.20739935432037,2.17903389691023,4.19611786084646));
#70641=CARTESIAN_POINT('Ctrl Pts',(-1.30713327152341,2.8128638865229,4.14349749047609));
#70642=CARTESIAN_POINT('Ctrl Pts',(-0.345447198709921,2.92638673563265,
4.09087712010572));
#70643=CARTESIAN_POINT('Ctrl Pts',(0.616238874103564,3.0399095847424,4.03825674973536));
#70644=CARTESIAN_POINT('Ctrl Pts',(1.63934493693357,2.63312529334921,3.98563637936499));
#70645=CARTESIAN_POINT('Ctrl Pts',(2.26053185174972,1.89025628960273,3.93301600899462));
#70646=CARTESIAN_POINT('Ctrl Pts',(2.88171876656588,1.14738728585625,3.88039563862425));
#70647=CARTESIAN_POINT('Ctrl Pts',(3.10098653336818,0.0684335697564567,
3.82777526825387));
#70648=CARTESIAN_POINT('Ctrl Pts',(2.8190342665149,-0.857973716122647,3.7751548978835));
#70649=CARTESIAN_POINT('Ctrl Pts',(2.53708199966161,-1.78438100200175,3.72253452751313));
#70650=CARTESIAN_POINT('Ctrl Pts',(1.75390969915275,-2.55824185766015,3.66991415714276));
#70651=CARTESIAN_POINT('Ctrl Pts',(0.824196505293748,-2.82909406262337,
3.61729378677239));
#70652=CARTESIAN_POINT('Ctrl Pts',(-0.105516688565254,-3.09994626758658,
3.56467341640202));
#70653=CARTESIAN_POINT('Ctrl Pts',(-1.18177077577439,-2.86778982185459,
3.51205304603165));
#70654=CARTESIAN_POINT('Ctrl Pts',(-1.91715720801869,-2.23776257255722,
3.45943267566128));
#70655=CARTESIAN_POINT('Ctrl Pts',(-2.55655857926025,-1.68996855643583,
3.41368048947072));
#70656=CARTESIAN_POINT('Ctrl Pts',(-2.93826750108625,-0.841388295482023,
3.36792830328016));
#70657=CARTESIAN_POINT('Ctrl Pts',(-2.94484294150901,0.00199174253909633,
3.3221761170896));
#70658=CARTESIAN_POINT('Ctrl Pts',(-2.94526037616607,0.00180040430511289,
3.17782388291039));
#70659=CARTESIAN_POINT('Ctrl Pts',(-2.93904351473207,-0.858539934689441,
3.22451349227397));
#70660=CARTESIAN_POINT('Ctrl Pts',(-2.53959728591596,-1.72390862024193,
3.27120310163755));
#70661=CARTESIAN_POINT('Ctrl Pts',(-1.87733008879233,-2.27130145042432,
3.31789271100113));
#70662=CARTESIAN_POINT('Ctrl Pts',(-1.13030567908798,-2.88874982718133,
3.37055767466781));
#70663=CARTESIAN_POINT('Ctrl Pts',(-0.0488837030099704,-3.10162488208327,
3.4232226383345));
#70664=CARTESIAN_POINT('Ctrl Pts',(0.876425794829888,-2.81337100100799,
3.47588760200118));
#70665=CARTESIAN_POINT('Ctrl Pts',(1.80173529266975,-2.5251171199327,3.52855256566786));
#70666=CARTESIAN_POINT('Ctrl Pts',(2.57093231227146,-1.73573430288019,3.58121752933455));
#70667=CARTESIAN_POINT('Ctrl Pts',(2.83512541526138,-0.803269840348294,
3.63388249300123));
#70668=CARTESIAN_POINT('Ctrl Pts',(3.0993185182513,0.129194622183599,3.68654745666792));
#70669=CARTESIAN_POINT('Ctrl Pts',(2.85850770462944,1.20474073019488,3.7392124203346));
#70670=CARTESIAN_POINT('Ctrl Pts',(2.22191964750238,1.93552360728328,3.79187738400129));
#70671=CARTESIAN_POINT('Ctrl Pts',(1.58533159037532,2.66630648437168,3.84454234766797));
#70672=CARTESIAN_POINT('Ctrl Pts',(0.552966289743035,3.05232613053722,3.89720731133465));
#70673=CARTESIAN_POINT('Ctrl Pts',(-0.406917273431679,2.91849222887777,
3.94987227500134));
#70674=CARTESIAN_POINT('Ctrl Pts',(-1.36680083660641,2.78465832721833,4.00253723866802));
#70675=CARTESIAN_POINT('Ctrl Pts',(-2.25420266232356,2.13097087773392,4.05520220233471));
#70676=CARTESIAN_POINT('Ctrl Pts',(-2.666616123304,1.25392862924115,4.10786716600139));
#70677=CARTESIAN_POINT('Ctrl Pts',(-2.84922387445754,0.865593310885713,
4.13118607163773));
#70678=CARTESIAN_POINT('Ctrl Pts',(-2.9387088904313,0.433468688742346,4.15450497727406));
#70679=CARTESIAN_POINT('Ctrl Pts',(-2.93753500859377,0.000882026442511374,
4.17782388291039));
#70680=CARTESIAN_POINT('Origin',(0.,0.,0.));
#70681=CARTESIAN_POINT('',(-2.94294893056736,-0.00252441656932667,5.3221761170896));
#70682=CARTESIAN_POINT('',(-2.94214529852914,-0.00261326515612426,5.1778238829104));
#70683=CARTESIAN_POINT('',(-2.942,-3.60291088309151E-16,0.));
#70684=CARTESIAN_POINT('Ctrl Pts',(-2.94294893056736,-0.00252441656932667,
5.3221761170896));
#70685=CARTESIAN_POINT('Ctrl Pts',(-2.93593381851913,0.774652637504292,
5.28008571068756));
#70686=CARTESIAN_POINT('Ctrl Pts',(-2.61899610205614,1.55689120032164,5.23799530428553));
#70687=CARTESIAN_POINT('Ctrl Pts',(-2.06692649506365,2.10021140779169,5.1959048978835));
#70688=CARTESIAN_POINT('Ctrl Pts',(-1.37674291943613,2.77945670358908,5.14328452751313));
#70689=CARTESIAN_POINT('Ctrl Pts',(-0.31906293568821,3.08528758407071,5.09066415714276));
#70690=CARTESIAN_POINT('Ctrl Pts',(0.627116654359043,2.8792008952563,5.03804378677239));
#70691=CARTESIAN_POINT('Ctrl Pts',(1.5732962444063,2.67311420644189,4.98542341640202));
#70692=CARTESIAN_POINT('Ctrl Pts',(2.4079754407529,1.95510994833143,4.93280304603165));
#70693=CARTESIAN_POINT('Ctrl Pts',(2.75314891878373,1.05035428518759,4.88018267566128));
#70694=CARTESIAN_POINT('Ctrl Pts',(3.09832239681456,0.145598622043775,4.82756230529091));
#70695=CARTESIAN_POINT('Ctrl Pts',(2.95399015652965,-0.945908446133409,
4.77494193492054));
#70696=CARTESIAN_POINT('Ctrl Pts',(2.38551665840565,-1.72985067733577,4.72232156455017));
#70697=CARTESIAN_POINT('Ctrl Pts',(1.81704316028163,-2.51379290853814,4.6697011941798));
#70698=CARTESIAN_POINT('Ctrl Pts',(0.824428404318513,-2.99017030276568,
4.61708082380943));
#70699=CARTESIAN_POINT('Ctrl Pts',(-0.142797221412707,-2.9432434569701,
4.56446045343906));
#70700=CARTESIAN_POINT('Ctrl Pts',(-1.11002284714393,-2.89631661117452,
4.51184008306869));
#70701=CARTESIAN_POINT('Ctrl Pts',(-2.05185934264326,-2.32608552535581,
4.45921971269832));
#70702=CARTESIAN_POINT('Ctrl Pts',(-2.54177252355539,-1.49079359130735,
4.40659934232795));
#70703=CARTESIAN_POINT('Ctrl Pts',(-2.80377530896762,-1.04408421119714,
4.3784582672485));
#70704=CARTESIAN_POINT('Ctrl Pts',(-2.93652578376122,-0.52156611314212,
4.35031719216905));
#70705=CARTESIAN_POINT('Ctrl Pts',(-2.93739242931988,0.000540407572186541,
4.3221761170896));
#70706=CARTESIAN_POINT('Ctrl Pts',(-2.93753500859377,0.000882026442511374,
4.17782388291039));
#70707=CARTESIAN_POINT('Ctrl Pts',(-2.93605771780397,-0.543513730930775,
4.20716994094074));
#70708=CARTESIAN_POINT('Ctrl Pts',(-2.79100052624987,-1.08864123864977,
4.23651599897109));
#70709=CARTESIAN_POINT('Ctrl Pts',(-2.50727405993036,-1.54814577624058,
4.26586205700145));
#70710=CARTESIAN_POINT('Ctrl Pts',(-1.99809343933257,-2.37278088572845,
4.31852702066813));
#70711=CARTESIAN_POINT('Ctrl Pts',(-1.04230710189327,-2.92165405720309,
4.37119198433482));
#70712=CARTESIAN_POINT('Ctrl Pts',(-0.0734394371752462,-2.94580807344744,
4.4238569480015));
#70713=CARTESIAN_POINT('Ctrl Pts',(0.895428227542791,-2.9699620896918,4.47652191166818));
#70714=CARTESIAN_POINT('Ctrl Pts',(1.87737721953956,-2.46939695070584,4.52918687533487));
#70715=CARTESIAN_POINT('Ctrl Pts',(2.427016324523,-1.67115837574717,4.58185183900155));
#70716=CARTESIAN_POINT('Ctrl Pts',(2.97665542950643,-0.872919800788501,
4.63451680266824));
#70717=CARTESIAN_POINT('Ctrl Pts',(3.09398464747655,0.22299221014288,4.68718176633492));
#70718=CARTESIAN_POINT('Ctrl Pts',(2.725785936287,1.11949523708763,4.73984673000161));
#70719=CARTESIAN_POINT('Ctrl Pts',(2.35758722509745,2.01599826403239,4.79251169366829));
#70720=CARTESIAN_POINT('Ctrl Pts',(1.50386058474821,2.71309230699052,4.84517665733498));
#70721=CARTESIAN_POINT('Ctrl Pts',(0.551838293166775,2.8945903085884,4.89784162100166));
#70722=CARTESIAN_POINT('Ctrl Pts',(-0.400183998414646,3.07608831018627,
4.95050658466835));
#70723=CARTESIAN_POINT('Ctrl Pts',(-1.45050194122825,2.74199027042391,5.00317154833503));
#70724=CARTESIAN_POINT('Ctrl Pts',(-2.12271361651498,2.04383596665945,5.05583651200172));
#70725=CARTESIAN_POINT('Ctrl Pts',(-2.64172618991724,1.50479316935294,5.09649896897128));
#70726=CARTESIAN_POINT('Ctrl Pts',(-2.93533688440644,0.748724173372516,
5.13716142594084));
#70727=CARTESIAN_POINT('Ctrl Pts',(-2.94214529852914,-0.00261326515612426,
5.1778238829104));
#70728=CARTESIAN_POINT('Origin',(0.,0.,0.));
#70729=CARTESIAN_POINT('',(-2.94474230559933,0.0020353165097306,6.3221761170896));
#70730=CARTESIAN_POINT('',(-2.94552589459255,0.00164462538419303,6.1778238829104));
#70731=CARTESIAN_POINT('',(-2.942,-3.60291088309151E-16,0.));
#70732=CARTESIAN_POINT('Ctrl Pts',(-2.94474230559933,0.0020353165097306,
6.3221761170896));
#70733=CARTESIAN_POINT('Ctrl Pts',(-2.94577608567865,0.132578411608025,
6.31509496994683));
#70734=CARTESIAN_POINT('Ctrl Pts',(-2.93783733482844,0.262995037552802,
6.30801382280405));
#70735=CARTESIAN_POINT('Ctrl Pts',(-2.92049520368276,0.39214902611321,6.30093267566128));
#70736=CARTESIAN_POINT('Ctrl Pts',(-2.79162493090094,1.35189898976081,6.24831230529091));
#70737=CARTESIAN_POINT('Ctrl Pts',(-2.1434950231737,2.24192544902223,6.19569193492054));
#70738=CARTESIAN_POINT('Ctrl Pts',(-1.26962729970534,2.65915768867859,6.14307156455017));
#70739=CARTESIAN_POINT('Ctrl Pts',(-0.395759576236975,3.07638992833495,
6.0904511941798));
#70740=CARTESIAN_POINT('Ctrl Pts',(0.70384596297251,3.02082794838624,6.03783082380943));
#70741=CARTESIAN_POINT('Ctrl Pts',(1.53120548099802,2.51763437940803,5.98521045343906));
#70742=CARTESIAN_POINT('Ctrl Pts',(2.35856499902354,2.0144408104298,5.93259008306869));
#70743=CARTESIAN_POINT('Ctrl Pts',(2.91367849586509,1.06361565242206,5.87996971269832));
#70744=CARTESIAN_POINT('Ctrl Pts',(2.9451489575673,0.0957638301017936,5.82734934232795));
#70745=CARTESIAN_POINT('Ctrl Pts',(2.97661941926951,-0.872087992218468,
5.77472897195758));
#70746=CARTESIAN_POINT('Ctrl Pts',(2.48444684583239,-1.85696647885126,5.72210860158721));
#70747=CARTESIAN_POINT('Ctrl Pts',(1.69152388176343,-2.41284480454905,5.66948823121684));
#70748=CARTESIAN_POINT('Ctrl Pts',(0.898600917694462,-2.96872313024685,
5.61686786084646));
#70749=CARTESIAN_POINT('Ctrl Pts',(-0.19507243700635,-3.09560129500965,
5.56424749047609));
#70750=CARTESIAN_POINT('Ctrl Pts',(-1.09419888335647,-2.73601935246765,
5.51162712010572));
#70751=CARTESIAN_POINT('Ctrl Pts',(-1.9933253297066,-2.37643740992565,5.45900674973535));
#70752=CARTESIAN_POINT('Ctrl Pts',(-2.69790486770603,-1.53039536007885,
5.40638637936499));
#70753=CARTESIAN_POINT('Ctrl Pts',(-2.88885105295217,-0.581044479598858,
5.35376600899461));
#70754=CARTESIAN_POINT('Ctrl Pts',(-2.92706166295704,-0.391068040923041,
5.34323604502627));
#70755=CARTESIAN_POINT('Ctrl Pts',(-2.94470393564848,-0.196954622309047,
5.33270608105794));
#70756=CARTESIAN_POINT('Ctrl Pts',(-2.94294893056736,-0.00252441656932667,
5.3221761170896));
#70757=CARTESIAN_POINT('Ctrl Pts',(-2.94214529852914,-0.00261326515612426,
5.1778238829104));
#70758=CARTESIAN_POINT('Ctrl Pts',(-2.94415496646843,-0.224388664623296,
5.18982638960752));
#70759=CARTESIAN_POINT('Ctrl Pts',(-2.92117618657372,-0.445751813963285,
5.20182889630465));
#70760=CARTESIAN_POINT('Ctrl Pts',(-2.87162987121487,-0.660999575716158,
5.21383140300177));
#70761=CARTESIAN_POINT('Ctrl Pts',(-2.65422904286817,-1.60547024656074,
5.26649636666845));
#70762=CARTESIAN_POINT('Ctrl Pts',(-1.92532197841492,-2.43220102048334,
5.31916133033513));
#70763=CARTESIAN_POINT('Ctrl Pts',(-1.01552544630456,-2.76620437138433,
5.37182629400182));
#70764=CARTESIAN_POINT('Ctrl Pts',(-0.105728914194198,-3.10020772228531,
5.4244912576685));
#70765=CARTESIAN_POINT('Ctrl Pts',(0.984957085573281,-2.94148365016469,
5.47715622133519));
#70766=CARTESIAN_POINT('Ctrl Pts',(1.761820540694,-2.36202602414577,5.52982118500188));
#70767=CARTESIAN_POINT('Ctrl Pts',(2.53868399581473,-1.78256839812686,5.58248614866856));
#70768=CARTESIAN_POINT('Ctrl Pts',(3.0017249062887,-0.782377218209647,5.63515111233524));
#70769=CARTESIAN_POINT('Ctrl Pts',(2.94091774630216,0.184882032222853,5.68781607600193));
#70770=CARTESIAN_POINT('Ctrl Pts',(2.88011058631563,1.15214128265535,5.74048103966861));
#70771=CARTESIAN_POINT('Ctrl Pts',(2.2954553558686,2.08646860360313,5.7931460033353));
#70772=CARTESIAN_POINT('Ctrl Pts',(1.45213925422783,2.56407295970403,5.84581096700198));
#70773=CARTESIAN_POINT('Ctrl Pts',(0.60882315258705,3.04167731580494,5.89847593066867));
#70774=CARTESIAN_POINT('Ctrl Pts',(-0.493153820247473,3.06255870705896,
5.95114089433535));
#70775=CARTESIAN_POINT('Ctrl Pts',(-1.35395830631657,2.6172457777424,6.00380585800203));
#70776=CARTESIAN_POINT('Ctrl Pts',(-2.21476279238567,2.17193284842583,6.05647082166872));
#70777=CARTESIAN_POINT('Ctrl Pts',(-2.83439479168936,1.26042559853868,6.10913578533541));
#70778=CARTESIAN_POINT('Ctrl Pts',(-2.93180238522596,0.296164363719765,
6.16180074900209));
#70779=CARTESIAN_POINT('Ctrl Pts',(-2.94168102690256,0.198373309905978,
6.1671417936382));
#70780=CARTESIAN_POINT('Ctrl Pts',(-2.94618853440423,0.100039675683843,
6.1724828382743));
#70781=CARTESIAN_POINT('Ctrl Pts',(-2.94552589459255,0.00164462538419303,
6.1778238829104));
#70782=CARTESIAN_POINT('Origin',(0.,0.,0.));
#70783=CARTESIAN_POINT('',(-2.93737184280031,0.000478285809368539,7.32217611708959));
#70784=CARTESIAN_POINT('',(-2.93765213932985,0.00105817779144944,7.17782388291039));
#70785=CARTESIAN_POINT('',(-2.942,-3.60291088309151E-16,0.));
#70786=CARTESIAN_POINT('Ctrl Pts',(-2.93737184280031,0.000478285809368539,
7.32217611708959));
#70787=CARTESIAN_POINT('Ctrl Pts',(-2.93804459091945,0.458606303769958,
7.29748385883571));
#70788=CARTESIAN_POINT('Ctrl Pts',(-2.83719423177179,0.916453996322869,
7.27279160058183));
#70789=CARTESIAN_POINT('Ctrl Pts',(-2.63324974290992,1.32252368027208,7.24809934232795));
#70790=CARTESIAN_POINT('Ctrl Pts',(-2.198634389848,2.18787738530332,7.19547897195758));
#70791=CARTESIAN_POINT('Ctrl Pts',(-1.29583121079705,2.81808837804428,7.14285860158721));
#70792=CARTESIAN_POINT('Ctrl Pts',(-0.333697177699206,2.92774986756231,
7.09023823121684));
#70793=CARTESIAN_POINT('Ctrl Pts',(0.628436855398639,3.03741135708034,7.03761786084647));
#70794=CARTESIAN_POINT('Ctrl Pts',(1.64990174254338,2.62652334337548,6.9849974904761));
#70795=CARTESIAN_POINT('Ctrl Pts',(2.26810159307568,1.88116672756646,6.93237712010573));
#70796=CARTESIAN_POINT('Ctrl Pts',(2.886301443608,1.13581011175742,6.87975674973536));
#70797=CARTESIAN_POINT('Ctrl Pts',(3.10123625752784,0.055984893844227,6.82713637936498));
#70798=CARTESIAN_POINT('Ctrl Pts',(2.81556743521199,-0.869283101865742,
6.77451600899461));
#70799=CARTESIAN_POINT('Ctrl Pts',(2.52989861289615,-1.7945510975757,6.72189563862424));
#70800=CARTESIAN_POINT('Ctrl Pts',(1.74362615434463,-2.56526187108243,6.66927526825387));
#70801=CARTESIAN_POINT('Ctrl Pts',(0.812833183747132,-2.8323797960046,6.6166548978835));
#70802=CARTESIAN_POINT('Ctrl Pts',(-0.117959786850361,-3.09949772092676,
6.56403452751313));
#70803=CARTESIAN_POINT('Ctrl Pts',(-1.19327326949384,-2.86302279726437,
6.51141415714276));
#70804=CARTESIAN_POINT('Ctrl Pts',(-1.92612469189739,-2.23004860141629,
6.45879378677239));
#70805=CARTESIAN_POINT('Ctrl Pts',(-2.56035596550109,-1.68225403062272,
6.41325456354479));
#70806=CARTESIAN_POINT('Ctrl Pts',(-2.93809401248361,-0.83749407451141,
6.3677153403172));
#70807=CARTESIAN_POINT('Ctrl Pts',(-2.94474230559933,0.0020353165097306,
6.3221761170896));
#70808=CARTESIAN_POINT('Ctrl Pts',(-2.94552589459255,0.00164462538419303,
6.1778238829104));
#70809=CARTESIAN_POINT('Ctrl Pts',(-2.93965462503178,-0.87017722046166,
6.22514780194098));
#70810=CARTESIAN_POINT('Ctrl Pts',(-2.52789003171806,-1.74682066505967,
6.27247172097156));
#70811=CARTESIAN_POINT('Ctrl Pts',(-1.85003983495055,-2.2935847848838,6.31979564000214));
#70812=CARTESIAN_POINT('Ctrl Pts',(-1.095686503369,-2.90205747891776,6.37246060366883));
#70813=CARTESIAN_POINT('Ctrl Pts',(-0.0117966524363787,-3.10198764723502,
6.42512556733551));
#70814=CARTESIAN_POINT('Ctrl Pts',(0.910000294361383,-2.80269121035772,
6.4777905310022));
#70815=CARTESIAN_POINT('Ctrl Pts',(1.83179724115916,-2.50339477348041,6.53045549466888));
#70816=CARTESIAN_POINT('Ctrl Pts',(2.59150128382206,-1.70487173140855,6.58312045833556));
#70817=CARTESIAN_POINT('Ctrl Pts',(2.8445267984577,-0.769315181970455,6.63578542200225));
#70818=CARTESIAN_POINT('Ctrl Pts',(3.09755231309333,0.166241367467632,6.68845038566893));
#70819=CARTESIAN_POINT('Ctrl Pts',(2.84389929970168,1.23883142427194,6.74111534933562));
#70820=CARTESIAN_POINT('Ctrl Pts',(2.19861937965545,1.96195091165853,6.79378031300231));
#70821=CARTESIAN_POINT('Ctrl Pts',(1.55333945960922,2.68507039904512,6.84644527666899));
#70822=CARTESIAN_POINT('Ctrl Pts',(0.51643263290838,3.05871931701401,6.89911024033567));
#70823=CARTESIAN_POINT('Ctrl Pts',(-0.441782179220013,2.91341844960141,
6.95177520400236));
#70824=CARTESIAN_POINT('Ctrl Pts',(-1.39999699134843,2.76811758218879,7.00444016766904));
#70825=CARTESIAN_POINT('Ctrl Pts',(-2.2795197889044,2.10386692939468,7.05710513133573));
#70826=CARTESIAN_POINT('Ctrl Pts',(-2.68141770473996,1.22195648411116,7.10977009500241));
#70827=CARTESIAN_POINT('Ctrl Pts',(-2.85452884366231,0.842087578115104,
7.13245469097174));
#70828=CARTESIAN_POINT('Ctrl Pts',(-2.93902534565796,0.421835844039577,
7.15513928694107));
#70829=CARTESIAN_POINT('Ctrl Pts',(-2.93765213932985,0.00105817779144944,
7.17782388291039));
#70830=CARTESIAN_POINT('Origin',(0.,0.,0.));
#70831=CARTESIAN_POINT('',(-2.94306537549688,-0.00250657139928612,8.3221761170896));
#70832=CARTESIAN_POINT('',(-2.94179645842688,-0.00262223567938445,8.17782388291039));
#70833=CARTESIAN_POINT('',(-2.942,-3.60291088309151E-16,0.));
#70834=CARTESIAN_POINT('Ctrl Pts',(-2.94306537549688,-0.00250657139928612,
8.3221761170896));
#70835=CARTESIAN_POINT('Ctrl Pts',(-2.93603346312234,0.778523040326291,
8.2798727477246));
#70836=CARTESIAN_POINT('Ctrl Pts',(-2.6155295502631,1.5646541741046,8.23756937835961));
#70837=CARTESIAN_POINT('Ctrl Pts',(-2.0584790752992,2.10849163858216,8.19526600899462));
#70838=CARTESIAN_POINT('Ctrl Pts',(-1.36557440251332,2.78496089461673,8.14264563862425));
#70839=CARTESIAN_POINT('Ctrl Pts',(-0.306675260078988,3.08654352280986,
8.09002526825387));
#70840=CARTESIAN_POINT('Ctrl Pts',(0.638669423716989,2.87666029635488,8.0374048978835));
#70841=CARTESIAN_POINT('Ctrl Pts',(1.58401410751295,2.66677706989991,7.98478452751313));
#70842=CARTESIAN_POINT('Ctrl Pts',(2.41580433267058,1.94542798879682,7.93216415714276));
#70843=CARTESIAN_POINT('Ctrl Pts',(2.75734311734437,1.03929400395132,7.87954378677239));
#70844=CARTESIAN_POINT('Ctrl Pts',(3.09888190201817,0.133160019105817,7.82692341640202));
#70845=CARTESIAN_POINT('Ctrl Pts',(2.95016924620815,-0.957758869482093,
7.77430304603165));
#70846=CARTESIAN_POINT('Ctrl Pts',(2.37855339098706,-1.73941279161662,7.72168267566128));
#70847=CARTESIAN_POINT('Ctrl Pts',(1.80693753576595,-2.52106671375116,7.66906230529091));
#70848=CARTESIAN_POINT('Ctrl Pts',(0.812418481133763,-2.99345566943229,
7.61644193492054));
#70849=CARTESIAN_POINT('Ctrl Pts',(-0.154610975618871,-2.94264651965433,
7.56382156455017));
#70850=CARTESIAN_POINT('Ctrl Pts',(-1.1216404323715,-2.89183736987637,7.5112011941798));
#70851=CARTESIAN_POINT('Ctrl Pts',(-2.06118029124457,-2.31783011463932,
7.45858082380943));
#70852=CARTESIAN_POINT('Ctrl Pts',(-2.54773645714466,-1.48057827836003,
7.40596045343906));
#70853=CARTESIAN_POINT('Ctrl Pts',(-2.80597476023112,-1.03620924430037,
7.37803234132257));
#70854=CARTESIAN_POINT('Ctrl Pts',(-2.93661093285418,-0.517686173583286,
7.35010422920608));
#70855=CARTESIAN_POINT('Ctrl Pts',(-2.93737184280031,0.000478285809368539,
7.32217611708959));
#70856=CARTESIAN_POINT('Ctrl Pts',(-2.93765213932985,0.00105817779144944,
7.17782388291039));
#70857=CARTESIAN_POINT('Ctrl Pts',(-2.93583728528984,-0.555049110608679,
7.20780425060775));
#70858=CARTESIAN_POINT('Ctrl Pts',(-2.78403605908896,-1.11207503097007,
7.23778461830511));
#70859=CARTESIAN_POINT('Ctrl Pts',(-2.48858495099342,-1.57801251517323,
7.26776498600247));
#70860=CARTESIAN_POINT('Ctrl Pts',(-1.96958124729618,-2.39650083140119,
7.32042994966915));
#70861=CARTESIAN_POINT('Ctrl Pts',(-1.00730080578659,-2.93390722608419,
7.37309491333584));
#70862=CARTESIAN_POINT('Ctrl Pts',(-0.0382136038189444,-2.94647556868157,
7.42575987700252));
#70863=CARTESIAN_POINT('Ctrl Pts',(0.930873598148709,-2.95904391127895,
7.47842484066921));
#70864=CARTESIAN_POINT('Ctrl Pts',(1.90676756057442,-2.44677420179069,7.53108980433588));
#70865=CARTESIAN_POINT('Ctrl Pts',(2.44682350205541,-1.64202110404938,7.58375476800257));
#70866=CARTESIAN_POINT('Ctrl Pts',(2.98687944353639,-0.837268006308086,
7.63641973166925));
#70867=CARTESIAN_POINT('Ctrl Pts',(3.09109736407267,0.25996847968624,7.68908469533594));
#70868=CARTESIAN_POINT('Ctrl Pts',(2.71220622763963,1.15200518015635,7.74174965900263));
#70869=CARTESIAN_POINT('Ctrl Pts',(2.33331509120659,2.04404188062646,7.79441462266931));
#70870=CARTESIAN_POINT('Ctrl Pts',(1.47131489780423,2.73087879557235,7.84707958633599));
#70871=CARTESIAN_POINT('Ctrl Pts',(0.517190633372317,2.90098128313613,7.89974455000268));
#70872=CARTESIAN_POINT('Ctrl Pts',(-0.436933631059594,3.07108377069992,
7.95240951366936));
#70873=CARTESIAN_POINT('Ctrl Pts',(-1.48318196652107,2.72445183088159,8.00507447733605));
#70874=CARTESIAN_POINT('Ctrl Pts',(-2.14699834174799,2.01831035197405,8.05773944100273));
#70875=CARTESIAN_POINT('Ctrl Pts',(-2.65153376339188,1.48160562142403,8.09776758830529));
#70876=CARTESIAN_POINT('Ctrl Pts',(-2.93514585523751,0.737219387421443,
8.13779573560784));
#70877=CARTESIAN_POINT('Ctrl Pts',(-2.94179645842688,-0.00262223567938445,
8.17782388291039));
#70878=CARTESIAN_POINT('Origin',(0.,0.,0.));
#70879=CARTESIAN_POINT('',(-2.94464008512449,0.00207742171232136,9.3221761170896));
#70880=CARTESIAN_POINT('',(-2.94577110767244,0.00147777103002609,9.1778238829104));
#70881=CARTESIAN_POINT('',(-2.942,-3.60291088309151E-16,0.));
#70882=CARTESIAN_POINT('Ctrl Pts',(-2.94464008512449,0.00207742171232136,
9.3221761170896));
#70883=CARTESIAN_POINT('Ctrl Pts',(-2.94572064417758,0.136558752036829,
9.31488200698387));
#70884=CARTESIAN_POINT('Ctrl Pts',(-2.93729508396668,0.270903986837675,
9.30758789687813));
#70885=CARTESIAN_POINT('Ctrl Pts',(-2.91889749004766,0.4038694541666,9.3002937867724));
#70886=CARTESIAN_POINT('Ctrl Pts',(-2.7861755826581,1.3630943679524,9.24767341640203));
#70887=CARTESIAN_POINT('Ctrl Pts',(-2.1344781113937,2.25051190295123,9.19505304603165));
#70888=CARTESIAN_POINT('Ctrl Pts',(-1.25894255572533,2.66423286046833,9.14243267566128));
#70889=CARTESIAN_POINT('Ctrl Pts',(-0.383407000056953,3.07795381798544,
9.08981230529091));
#70890=CARTESIAN_POINT('Ctrl Pts',(0.715966640015389,3.01797819802083,9.03719193492054));
#70891=CARTESIAN_POINT('Ctrl Pts',(1.54129954888374,2.51146745828537,8.98457156455017));
#70892=CARTESIAN_POINT('Ctrl Pts',(2.3666324577521,2.00495671854991,8.9319511941798));
#70893=CARTESIAN_POINT('Ctrl Pts',(2.91792463541645,1.05191085904358,8.87933082380943));
#70894=CARTESIAN_POINT('Ctrl Pts',(2.94550964776859,0.0839405046308018,
8.82671045343906));
#70895=CARTESIAN_POINT('Ctrl Pts',(2.97309466012074,-0.884029849781979,
8.77409008306869));
#70896=CARTESIAN_POINT('Ctrl Pts',(2.47697250716068,-1.86692469910122,8.72146971269832));
#70897=CARTESIAN_POINT('Ctrl Pts',(1.68182449914462,-2.41961555778857,8.66884934232795));
#70898=CARTESIAN_POINT('Ctrl Pts',(0.886676491128584,-2.97230641647591,
8.61622897195757));
#70899=CARTESIAN_POINT('Ctrl Pts',(-0.207497371943416,-3.09479328453138,
8.56360860158721));
#70900=CARTESIAN_POINT('Ctrl Pts',(-1.10517312337017,-2.73160492399537,
8.51098823121684));
#70901=CARTESIAN_POINT('Ctrl Pts',(-2.00284887479693,-2.36841656345936,
8.45836786084647));
#70902=CARTESIAN_POINT('Ctrl Pts',(-2.70402651457844,-1.51955297433185,
8.4057474904761));
#70903=CARTESIAN_POINT('Ctrl Pts',(-2.89116023290047,-0.56944323783011,
8.35312712010573));
#70904=CARTESIAN_POINT('Ctrl Pts',(-2.92785056302318,-0.383160187412328,
8.34281011910035));
#70905=CARTESIAN_POINT('Ctrl Pts',(-2.94478032747652,-0.192985093804385,
8.33249311809497));
#70906=CARTESIAN_POINT('Ctrl Pts',(-2.94306537549688,-0.00250657139928612,
8.3221761170896));
#70907=CARTESIAN_POINT('Ctrl Pts',(-2.94179645842688,-0.00262223567938445,
8.17782388291039));
#70908=CARTESIAN_POINT('Ctrl Pts',(-2.94389604226671,-0.236188947098698,
8.19046069927452));
#70909=CARTESIAN_POINT('Ctrl Pts',(-2.91839215134056,-0.469302718100354,
8.20309751563865));
#70910=CARTESIAN_POINT('Ctrl Pts',(-2.86352159037298,-0.695286025907358,
8.21573433200279));
#70911=CARTESIAN_POINT('Ctrl Pts',(-2.63484404877868,-1.63708990688444,
8.26839929566947));
#70912=CARTESIAN_POINT('Ctrl Pts',(-1.89610455059774,-2.45504665084187,
8.32106425933616));
#70913=CARTESIAN_POINT('Ctrl Pts',(-0.982379647459882,-2.77814844538783,
8.37372922300284));
#70914=CARTESIAN_POINT('Ctrl Pts',(-0.068654744322021,-3.1012502399338,
8.42639418666953));
#70915=CARTESIAN_POINT('Ctrl Pts',(1.02005556377276,-2.92949708506828,8.47905915033621));
#70916=CARTESIAN_POINT('Ctrl Pts',(1.78993539631662,-2.34079256521527,8.53172411400289));
#70917=CARTESIAN_POINT('Ctrl Pts',(2.55981522886048,-1.75208804536226,8.58438907766958));
#70918=CARTESIAN_POINT('Ctrl Pts',(3.01086458585342,-0.746432160521719,
8.63705404133626));
#70919=CARTESIAN_POINT('Ctrl Pts',(2.93849705553841,0.220030931794408,8.68971900500295));
#70920=CARTESIAN_POINT('Ctrl Pts',(2.86612952522341,1.18649402411053,8.74238396866963));
#70921=CARTESIAN_POINT('Ctrl Pts',(2.27034510760049,2.11376432390223,8.79504893233632));
#70922=CARTESIAN_POINT('Ctrl Pts',(1.42137896494728,2.58125171077128,8.847713896003));
#70923=CARTESIAN_POINT('Ctrl Pts',(0.572412822294062,3.04873909764032,8.90037885966968));
#70924=CARTESIAN_POINT('Ctrl Pts',(-0.529735045389435,3.05644357158669,
8.95304382333637));
#70925=CARTESIAN_POINT('Ctrl Pts',(-1.38515376586909,2.60087054680792,9.00570878700305));
#70926=CARTESIAN_POINT('Ctrl Pts',(-2.24057248634875,2.14529752202914,9.05837375066974));
#70927=CARTESIAN_POINT('Ctrl Pts',(-2.84926205962455,1.2264469985252,9.11103871433643));
#70928=CARTESIAN_POINT('Ctrl Pts',(-2.93513381881397,0.261090064936974,
9.16370367800311));
#70929=CARTESIAN_POINT('Ctrl Pts',(-2.94280828744918,0.174814884615283,
9.16841041297221));
#70930=CARTESIAN_POINT('Ctrl Pts',(-2.94630689264378,0.0881682471389342,
9.1731171479413));
#70931=CARTESIAN_POINT('Ctrl Pts',(-2.94577110767244,0.00147777103002609,
9.1778238829104));
#70932=CARTESIAN_POINT('Origin',(0.,0.,0.));
#70933=CARTESIAN_POINT('',(-2.93735377875815,0.0004158914717875,10.3221761170896));
#70934=CARTESIAN_POINT('',(-2.93779053274574,0.00122895754932335,10.1778238829104));
#70935=CARTESIAN_POINT('',(-2.942,-3.60291088309151E-16,0.));
#70936=CARTESIAN_POINT('Ctrl Pts',(-2.93735377875815,0.0004158914717875,
10.3221761170896));
#70937=CARTESIAN_POINT('Ctrl Pts',(-2.93794360094505,0.462502223744089,
10.2972708958728));
#70938=CARTESIAN_POINT('Ctrl Pts',(-2.83526550161259,0.924340675123848,
10.2723656746559));
#70939=CARTESIAN_POINT('Ctrl Pts',(-2.6279195904465,1.33308353810155,10.2474604534391));
#70940=CARTESIAN_POINT('Ctrl Pts',(-2.18983399605069,2.19668561771623,10.1948400830687));
#70941=CARTESIAN_POINT('Ctrl Pts',(-1.28450826872579,2.82326745826868,10.1422197126983));
#70942=CARTESIAN_POINT('Ctrl Pts',(-0.321941779407734,2.9290658210569,10.0895993423279));
#70943=CARTESIAN_POINT('Ctrl Pts',(0.640624709910309,3.03486418384512,10.0369789719576));
#70944=CARTESIAN_POINT('Ctrl Pts',(1.66043196122149,2.61987906886913,9.98435860158721));
#70945=CARTESIAN_POINT('Ctrl Pts',(2.27563478565877,1.87204685190273,9.93173823121684));
#70946=CARTESIAN_POINT('Ctrl Pts',(2.89083761009605,1.12421463493634,9.87911786084647));
#70947=CARTESIAN_POINT('Ctrl Pts',(3.10143600765941,0.0435353159795382,
9.82649749047609));
#70948=CARTESIAN_POINT('Ctrl Pts',(2.8120552331994,-0.880578479665677,9.77387712010572));
#70949=CARTESIAN_POINT('Ctrl Pts',(2.52267445873939,-1.8046922753109,9.72125674973535));
#70950=CARTESIAN_POINT('Ctrl Pts',(1.733314512256,-2.57224054764455,9.66863637936499));
#70951=CARTESIAN_POINT('Ctrl Pts',(0.801456763974427,-2.83561988794246,
9.61601600899462));
#70952=CARTESIAN_POINT('Ctrl Pts',(-0.130400984307143,-3.09899922824038,
9.56339563862425));
#70953=CARTESIAN_POINT('Ctrl Pts',(-1.20475653438691,-2.85820963650256,
9.51077526825387));
#70954=CARTESIAN_POINT('Ctrl Pts',(-1.93506113766943,-2.22229869434726,
9.4581548978835));
#70955=CARTESIAN_POINT('Ctrl Pts',(-2.5641326605009,-1.67453620870937,9.41282863761886));
#70956=CARTESIAN_POINT('Ctrl Pts',(-2.93792539338528,-0.833601734574448,
9.36750237735423));
#70957=CARTESIAN_POINT('Ctrl Pts',(-2.94464008512449,0.00207742171232136,
9.3221761170896));
#70958=CARTESIAN_POINT('Ctrl Pts',(-2.94577110767244,0.00147777103002609,
9.1778238829104));
#70959=CARTESIAN_POINT('Ctrl Pts',(-2.94031184592155,-0.881835546255158,
9.22578211160798));
#70960=CARTESIAN_POINT('Ctrl Pts',(-2.51599664630944,-1.76970025068938,
9.27374034030557));
#70961=CARTESIAN_POINT('Ctrl Pts',(-1.82248510748737,-2.31554023703778,
9.32169856900316));
#70962=CARTESIAN_POINT('Ctrl Pts',(-1.06091069186834,-2.91495026175178,
9.37436353266984));
#70963=CARTESIAN_POINT('Ctrl Pts',(0.0252920844727601,-3.1019069675073,
9.42702849633653));
#70964=CARTESIAN_POINT('Ctrl Pts',(0.943444704192239,-2.79161076199491,
9.47969346000322));
#70965=CARTESIAN_POINT('Ctrl Pts',(1.86159732391172,-2.48131455648253,9.5323584236699));
#70966=CARTESIAN_POINT('Ctrl Pts',(2.61169978700958,-1.67376543970224,9.58502338733658));
#70967=CARTESIAN_POINT('Ctrl Pts',(2.85352154222556,-0.735250545330611,
9.63768835100327));
#70968=CARTESIAN_POINT('Ctrl Pts',(3.09534329744155,0.203264349041017,9.69035331466995));
#70969=CARTESIAN_POINT('Ctrl Pts',(2.82888434477565,1.27274502100399,9.74301827833664));
#70970=CARTESIAN_POINT('Ctrl Pts',(2.17500480776272,1.98809774472063,9.79568324200333));
#70971=CARTESIAN_POINT('Ctrl Pts',(1.52112527074978,2.70345046843728,9.84834820567001));
#70972=CARTESIAN_POINT('Ctrl Pts',(0.479825149389799,3.06467524390761,9.90101316933669));
#70973=CARTESIAN_POINT('Ctrl Pts',(-0.476583929910364,2.90792818241875,
9.95367813300337));
#70974=CARTESIAN_POINT('Ctrl Pts',(-1.43299300921054,2.75118112092989,10.0063430966701));
#70975=CARTESIAN_POINT('Ctrl Pts',(-2.3045110464509,2.07646222248183,10.0590080603367));
#70976=CARTESIAN_POINT('Ctrl Pts',(-2.69583596380714,1.18980965393578,10.1116730240034));
#70977=CARTESIAN_POINT('Ctrl Pts',(-2.85967973895049,0.818577213506006,
10.1337233103058));
#70978=CARTESIAN_POINT('Ctrl Pts',(-2.93934508420187,0.410192546500391,
10.1557735966081));
#70979=CARTESIAN_POINT('Ctrl Pts',(-2.93779053274574,0.00122895754932335,
10.1778238829104));
#70980=CARTESIAN_POINT('Origin',(0.,0.,0.));
#70981=CARTESIAN_POINT('',(-2.94318142996902,-0.00248705772575741,11.3221761170896));
#70982=CARTESIAN_POINT('',(-2.94145083142593,-0.00261642954227547,11.1778238829104));
#70983=CARTESIAN_POINT('',(-2.942,-3.60291088309151E-16,0.));
#70984=CARTESIAN_POINT('Ctrl Pts',(-2.94318142996902,-0.00248705772575741,
11.3221761170896));
#70985=CARTESIAN_POINT('Ctrl Pts',(-2.93613735245544,0.782394524444463,
11.2796597847616));
#70986=CARTESIAN_POINT('Ctrl Pts',(-2.61204283140731,1.57241444895454,11.2371434524337));
#70987=CARTESIAN_POINT('Ctrl Pts',(-2.04999848462302,2.11673789269853,11.1946271201057));
#70988=CARTESIAN_POINT('Ctrl Pts',(-1.35438388023453,2.79042020824128,11.1420067497354));
#70989=CARTESIAN_POINT('Ctrl Pts',(-0.294282642636005,3.08774972424349,
11.089386379365));
#70990=CARTESIAN_POINT('Ctrl Pts',(0.65021190135765,2.87407334222539,11.0367660089946));
#70991=CARTESIAN_POINT('Ctrl Pts',(1.59470644535131,2.66039696020728,10.9841456386242));
#70992=CARTESIAN_POINT('Ctrl Pts',(2.42359429574009,1.93571468016887,10.9315252682539));
#70993=CARTESIAN_POINT('Ctrl Pts',(2.76149288344003,1.02821697529914,10.8789048978835));
#70994=CARTESIAN_POINT('Ctrl Pts',(3.09939147113997,0.120719270429434,10.8262845275131));
#70995=CARTESIAN_POINT('Ctrl Pts',(2.9463007961511,-0.969593859271576,10.7736641571428));
#70996=CARTESIAN_POINT('Ctrl Pts',(2.37155179497663,-1.74894687658982,10.7210437867724));
#70997=CARTESIAN_POINT('Ctrl Pts',(1.79680279380215,-2.52829989390807,10.668423416402));
#70998=CARTESIAN_POINT('Ctrl Pts',(0.800395466442055,-2.99669279884355,
10.6158030460317));
#70999=CARTESIAN_POINT('Ctrl Pts',(-0.166422238380945,-2.94200216382593,
10.5631826756613));
#71000=CARTESIAN_POINT('Ctrl Pts',(-1.13323994320395,-2.8873115288083,10.5105623052909));
#71001=CARTESIAN_POINT('Ctrl Pts',(-2.07046802548985,-2.30953735383759,
10.4579419349205));
#71002=CARTESIAN_POINT('Ctrl Pts',(-2.55365933589945,-1.47033910701379,
10.4053215645502));
#71003=CARTESIAN_POINT('Ctrl Pts',(-2.80815619982173,-1.02833338914462,
10.3776064153966));
#71004=CARTESIAN_POINT('Ctrl Pts',(-2.93669740996939,-0.513805263571333,
10.3498912662431));
#71005=CARTESIAN_POINT('Ctrl Pts',(-2.93735377875815,0.0004158914717875,
10.3221761170896));
#71006=CARTESIAN_POINT('Ctrl Pts',(-2.93779053274574,0.00122895754932335,
10.1778238829104));
#71007=CARTESIAN_POINT('Ctrl Pts',(-2.93563218928374,-0.566577199606596,
10.2084385602748));
#71008=CARTESIAN_POINT('Ctrl Pts',(-2.77690932929649,-1.13549932265473,
10.2390532376391));
#71009=CARTESIAN_POINT('Ctrl Pts',(-2.46954008606165,-1.60765366907442,
10.2696679150035));
#71010=CARTESIAN_POINT('Ctrl Pts',(-1.94078749348779,-2.41987818489459,
10.3223328786702));
#71011=CARTESIAN_POINT('Ctrl Pts',(-0.972150510867944,-2.9457409778909,
10.3749978423368));
#71012=CARTESIAN_POINT('Ctrl Pts',(-0.00298230764251388,-2.94672185015728,
10.4276628060035));
#71013=CARTESIAN_POINT('Ctrl Pts',(0.966185895582889,-2.94770272242366,
10.4803277696702));
#71014=CARTESIAN_POINT('Ctrl Pts',(1.93588531941386,-2.42380167396015,10.5329927333369));
#71015=CARTESIAN_POINT('Ctrl Pts',(2.46628089363149,-1.61264909700348,10.5856576970036));
#71016=CARTESIAN_POINT('Ctrl Pts',(2.99667646784912,-0.801496520046785,
10.6383226606703));
#71017=CARTESIAN_POINT('Ctrl Pts',(3.08776819245338,0.296907585403119,10.690987624337));
#71018=CARTESIAN_POINT('Ctrl Pts',(2.69823879520542,1.18435043817229,10.7436525880036));
#71019=CARTESIAN_POINT('Ctrl Pts',(2.30870939795745,2.07179329094149,10.7963175516703));
#71020=CARTESIAN_POINT('Ctrl Pts',(1.43855887885726,2.74827489102996,10.848982515337));
#71021=CARTESIAN_POINT('Ctrl Pts',(0.482469038528927,2.90695754754173,10.9016474790037));
#71022=CARTESIAN_POINT('Ctrl Pts',(-0.473620801799363,3.0656402040535,10.9543124426704));
#71023=CARTESIAN_POINT('Ctrl Pts',(-1.51564996335577,2.70652391698861,11.0069774063371));
#71024=CARTESIAN_POINT('Ctrl Pts',(-2.17097614256679,1.99249620947818,11.0596423700038));
#71025=CARTESIAN_POINT('Ctrl Pts',(-2.66116565955863,1.45839745352016,11.0990362076393));
#71026=CARTESIAN_POINT('Ctrl Pts',(-2.93498842496261,0.725719853723158,
11.1384300452748));
#71027=CARTESIAN_POINT('Ctrl Pts',(-2.94145083142593,-0.00261642954227547,
11.1778238829104));
#71028=CARTESIAN_POINT('Origin',(0.,0.,0.));
#71029=CARTESIAN_POINT('',(-2.9445363666432,0.00211803469319205,12.3221761170896));
#71030=CARTESIAN_POINT('',(-2.94599368555865,0.00130075687149912,12.1778238829104));
#71031=CARTESIAN_POINT('',(-2.942,-3.60291088309151E-16,0.));
#71032=CARTESIAN_POINT('Ctrl Pts',(-2.9445363666432,0.00211803469319205,
12.3221761170896));
#71033=CARTESIAN_POINT('Ctrl Pts',(-2.9456637214079,0.140538485345201,12.3146690440209));
#71034=CARTESIAN_POINT('Ctrl Pts',(-2.93673667551181,0.278812877817704,
12.3071619709522));
#71035=CARTESIAN_POINT('Ctrl Pts',(-2.91725274860024,0.415583368023806,
12.2996548978835));
#71036=CARTESIAN_POINT('Ctrl Pts',(-2.78068135240184,1.37426776932391,12.2470345275131));
#71037=CARTESIAN_POINT('Ctrl Pts',(-2.12542680364205,2.25906209195984,12.1944141571428));
#71038=CARTESIAN_POINT('Ctrl Pts',(-1.24823752065428,2.66926510338839,12.1417937867724));
#71039=CARTESIAN_POINT('Ctrl Pts',(-0.371048237666502,3.07946811481694,
12.089173416402));
#71040=CARTESIAN_POINT('Ctrl Pts',(0.728075779549269,3.01507981503809,12.0365530460316));
#71041=CARTESIAN_POINT('Ctrl Pts',(1.55136877770631,2.50526006508935,11.9839326756613));
#71042=CARTESIAN_POINT('Ctrl Pts',(2.37466177586334,1.99544031514062,11.9313123052909));
#71043=CARTESIAN_POINT('Ctrl Pts',(2.92212375496165,1.04018911502201,11.8786919349205));
#71044=CARTESIAN_POINT('Ctrl Pts',(2.9458228744686,0.0721158274039949,11.8260715645502));
#71045=CARTESIAN_POINT('Ctrl Pts',(2.96952199397554,-0.895957460214037,
11.7734511941798));
#71046=CARTESIAN_POINT('Ctrl Pts',(2.4694582538911,-1.87685283533148,11.7208308238094));
#71047=CARTESIAN_POINT('Ctrl Pts',(1.67209801460167,-2.42634732122405,11.6682104534391));
#71048=CARTESIAN_POINT('Ctrl Pts',(0.874737775312261,-2.9758418071166,11.6155900830687));
#71049=CARTESIAN_POINT('Ctrl Pts',(-0.219918963182118,-3.09393540378431,
11.5629697126983));
#71050=CARTESIAN_POINT('Ctrl Pts',(-1.11612955404462,-2.72714647754463,
11.510349342328));
#71051=CARTESIAN_POINT('Ctrl Pts',(-2.01234014490716,-2.36035755130494,
11.4577289719576));
#71052=CARTESIAN_POINT('Ctrl Pts',(-2.7101045881378,-1.50868610215784,11.4051086015872));
#71053=CARTESIAN_POINT('Ctrl Pts',(-2.89342282416388,-0.557832820042644,
11.3524882312168));
#71054=CARTESIAN_POINT('Ctrl Pts',(-2.9286231547134,-0.375252240171749,
11.3423841931744));
#71055=CARTESIAN_POINT('Ctrl Pts',(-2.94485546023631,-0.189014750280763,
11.332280155132));
#71056=CARTESIAN_POINT('Ctrl Pts',(-2.94318142996902,-0.00248705772575741,
11.3221761170896));
#71057=CARTESIAN_POINT('Ctrl Pts',(-2.94145083142593,-0.00261642954227547,
11.1778238829104));
#71058=CARTESIAN_POINT('Ctrl Pts',(-2.94362790824268,-0.247980760321293,
11.1910950089415));
#71059=CARTESIAN_POINT('Ctrl Pts',(-2.9154621622164,-0.492852393533084,
11.2043661349727));
#71060=CARTESIAN_POINT('Ctrl Pts',(-2.85500395443405,-0.729473081400432,
11.2176372610038));
#71061=CARTESIAN_POINT('Ctrl Pts',(-2.61508239022462,-1.6684755368126,11.2703022246705));
#71062=CARTESIAN_POINT('Ctrl Pts',(-1.86661606494013,-2.4775413196809,11.3229671883372));
#71063=CARTESIAN_POINT('Ctrl Pts',(-0.949093412422085,-2.7896953688222,
11.3756321520039));
#71064=CARTESIAN_POINT('Ctrl Pts',(-0.0315707599040525,-3.10184941796349,
11.4282971156705));
#71065=CARTESIAN_POINT('Ctrl Pts',(1.05500821984753,-2.91709173337779,11.4809620793372));
#71066=CARTESIAN_POINT('Ctrl Pts',(1.81779437152408,-2.31922447800469,11.5336270430039));
#71067=CARTESIAN_POINT('Ctrl Pts',(2.58058052320064,-1.7213572226316,11.5862920066706));
#71068=CARTESIAN_POINT('Ctrl Pts',(3.01957384680218,-0.710380396471107,
11.6389569703373));
#71069=CARTESIAN_POINT('Ctrl Pts',(2.93565629151018,0.255148376847553,11.691621934004));
#71070=CARTESIAN_POINT('Ctrl Pts',(2.85173873621817,1.22067715016623,11.7442868976707));
#71071=CARTESIAN_POINT('Ctrl Pts',(2.24491030203262,2.14075787064307,11.7969518613373));
#71072=CARTESIAN_POINT('Ctrl Pts',(1.39041548234847,2.59806145861508,11.849616825004));
#71073=CARTESIAN_POINT('Ctrl Pts',(0.535920662664327,3.05536504658708,11.9022817886707));
#71074=CARTESIAN_POINT('Ctrl Pts',(-0.566240542518395,3.04989150205426,
11.9549467523374));
#71075=CARTESIAN_POINT('Ctrl Pts',(-1.41615121076395,2.58412350821102,12.0076117160041));
#71076=CARTESIAN_POINT('Ctrl Pts',(-2.26606187900951,2.11835551436778,12.0602766796708));
#71077=CARTESIAN_POINT('Ctrl Pts',(-2.86372201031791,1.19229307121411,12.1129416433374));
#71078=CARTESIAN_POINT('Ctrl Pts',(-2.93804565964555,0.22597844177242,12.1656066070041));
#71079=CARTESIAN_POINT('Ctrl Pts',(-2.94379288681505,0.151256200025011,
12.1696790323062));
#71080=CARTESIAN_POINT('Ctrl Pts',(-2.94641083929854,0.0762932715455572,
12.1737514576083));
#71081=CARTESIAN_POINT('Ctrl Pts',(-2.94599368555865,0.00130075687149912,
12.1778238829104));
#71082=CARTESIAN_POINT('Origin',(0.,0.,0.));
#71083=CARTESIAN_POINT('',(-2.93733773658367,0.000353650820144602,13.3221761170896));
#71084=CARTESIAN_POINT('',(-2.93794966127546,0.0013934910171998,13.1778238829104));
#71085=CARTESIAN_POINT('',(-2.942,-3.60291088309151E-16,0.));
#71086=CARTESIAN_POINT('Ctrl Pts',(-2.93733773658367,0.000353650820144602,
13.3221761170896));
#71087=CARTESIAN_POINT('Ctrl Pts',(-2.93784318272048,0.466397170874405,
13.2970579329098));
#71088=CARTESIAN_POINT('Ctrl Pts',(-2.8333193685149,0.932226520914598,13.27193974873));
#71089=CARTESIAN_POINT('Ctrl Pts',(-2.62254748003497,1.34362161549686,13.2468215645502));
#71090=CARTESIAN_POINT('Ctrl Pts',(-2.18099904818651,2.20545788879211,13.1942011941798));
#71091=CARTESIAN_POINT('Ctrl Pts',(-1.27316460447925,2.82840106158337,13.1415808238094));
#71092=CARTESIAN_POINT('Ctrl Pts',(-0.31018098965669,2.93033473129373,13.0889604534391));
#71093=CARTESIAN_POINT('Ctrl Pts',(0.652802625165875,3.03226840100409,13.0363400830687));
#71094=CARTESIAN_POINT('Ctrl Pts',(1.67093541110377,2.61319256763355,12.9837197126983));
#71095=CARTESIAN_POINT('Ctrl Pts',(2.28313120153524,1.86289672775273,12.9310993423279));
#71096=CARTESIAN_POINT('Ctrl Pts',(2.89532699196672,1.1126008878719,12.8784789719576));
#71097=CARTESIAN_POINT('Ctrl Pts',(3.10158578689178,0.0310850414808014,
12.8258586015872));
#71098=CARTESIAN_POINT('Ctrl Pts',(2.80849777284497,-0.891859624755379,
12.7732382312168));
#71099=CARTESIAN_POINT('Ctrl Pts',(2.51540975879817,-1.81480429099155,12.7206178608465));
#71100=CARTESIAN_POINT('Ctrl Pts',(1.72297493577951,-2.57917777707278,12.6679974904761));
#71101=CARTESIAN_POINT('Ctrl Pts',(0.790067400131255,-2.83881430845519,
12.6153771201057));
#71102=CARTESIAN_POINT('Ctrl Pts',(-0.142840135516982,-3.0984508398376,
12.5627567497353));
#71103=CARTESIAN_POINT('Ctrl Pts',(-1.21622038379481,-2.85335041652122,
12.510136379365));
#71104=CARTESIAN_POINT('Ctrl Pts',(-1.94396638611522,-2.21451296488091,
12.4575160089946));
#71105=CARTESIAN_POINT('Ctrl Pts',(-2.56788867194677,-1.66681511174075,
12.4124027116929));
#71106=CARTESIAN_POINT('Ctrl Pts',(-2.93776159700942,-0.829711212970877,
12.3672894143913));
#71107=CARTESIAN_POINT('Ctrl Pts',(-2.9445363666432,0.00211803469319205,
12.3221761170896));
#71108=CARTESIAN_POINT('Ctrl Pts',(-2.94599368555865,0.00130075687149912,
12.1778238829104));
#71109=CARTESIAN_POINT('Ctrl Pts',(-2.94101617029297,-0.893516551252978,
12.226416421275));
#71110=CARTESIAN_POINT('Ctrl Pts',(-2.50391622116005,-1.79254618589271,
12.2750089596396));
#71111=CARTESIAN_POINT('Ctrl Pts',(-1.79466984706922,-2.33716467042755,
12.3236014980042));
#71112=CARTESIAN_POINT('Ctrl Pts',(-1.02598321781837,-2.92742633745608,
12.3762664616709));
#71113=CARTESIAN_POINT('Ctrl Pts',(0.0623772080302214,-3.10138285578342,
12.4289314253375));
#71114=CARTESIAN_POINT('Ctrl Pts',(0.976754244976282,-2.78013123936204,
12.4815963890042));
#71115=CARTESIAN_POINT('Ctrl Pts',(1.89113128192235,-2.45887962294065,12.5342613526709));
#71116=CARTESIAN_POINT('Ctrl Pts',(2.6315249299659,-1.64241987177053,12.5869263163376));
#71117=CARTESIAN_POINT('Ctrl Pts',(2.86210835815027,-0.701080799331296,
12.6395912800043));
#71118=CARTESIAN_POINT('Ctrl Pts',(3.09269178633465,0.240258273107937,12.692256243671));
#71119=CARTESIAN_POINT('Ctrl Pts',(2.81346499465986,1.30647666681628,12.7449212073377));
#71120=CARTESIAN_POINT('Ctrl Pts',(2.15107931219979,2.01396036610533,12.7975861710043));
#71121=CARTESIAN_POINT('Ctrl Pts',(1.48869362973973,2.72144406539436,12.850251134671));
#71122=CARTESIAN_POINT('Ctrl Pts',(0.443149056494409,3.07019307026412,12.9029160983377));
#71123=CARTESIAN_POINT('Ctrl Pts',(-0.511317558922748,2.90202221756343,
12.9555810620044));
#71124=CARTESIAN_POINT('Ctrl Pts',(-1.46578417433991,2.73385136486274,13.0082460256711));
#71125=CARTESIAN_POINT('Ctrl Pts',(-2.3291728319289,2.04876065459161,13.0609109893378));
#71126=CARTESIAN_POINT('Ctrl Pts',(-2.7098688231833,1.1574927237348,13.1135759530044));
#71127=CARTESIAN_POINT('Ctrl Pts',(-2.86467717936984,0.795062526234979,
13.1349919296398));
#71128=CARTESIAN_POINT('Ctrl Pts',(-2.93966715879244,0.398538727939818,
13.1564079062751));
#71129=CARTESIAN_POINT('Ctrl Pts',(-2.93794966127546,0.0013934910171998,
13.1778238829104));
#71130=CARTESIAN_POINT('Origin',(0.,0.,0.));
#71131=CARTESIAN_POINT('',(-2.94325266537063,-0.0024318079996577,14.3221761170896));
#71132=CARTESIAN_POINT('',(-2.94111188951679,-0.00259486169482749,14.1778238829104));
#71133=CARTESIAN_POINT('',(-2.942,-3.60291088309151E-16,0.));
#71134=CARTESIAN_POINT('Ctrl Pts',(-2.94325266537063,-0.0024318079996577,
14.3221761170896));
#71135=CARTESIAN_POINT('Ctrl Pts',(-2.93620194204164,0.786300619982285,
14.2794468217987));
#71136=CARTESIAN_POINT('Ctrl Pts',(-2.60854122084458,1.58016790859219,14.2367175265078));
#71137=CARTESIAN_POINT('Ctrl Pts',(-2.04150376744995,2.12493551247607,14.1939882312168));
#71138=CARTESIAN_POINT('Ctrl Pts',(-1.34320718641939,2.79580716825642,14.1413678608465));
#71139=CARTESIAN_POINT('Ctrl Pts',(-0.281884150596186,3.08890703892681,
14.0887474904761));
#71140=CARTESIAN_POINT('Ctrl Pts',(0.661753798897932,2.87144767774516,14.0361271201057));
#71141=CARTESIAN_POINT('Ctrl Pts',(1.60539174839208,2.65398831656351,13.9835067497354));
#71142=CARTESIAN_POINT('Ctrl Pts',(2.43134461155714,1.92596972352975,13.930886379365));
#71143=CARTESIAN_POINT('Ctrl Pts',(2.76559296922098,1.01711939779235,13.8782660089946));
#71144=CARTESIAN_POINT('Ctrl Pts',(3.09984132688481,0.108269072054953,13.8256456386242));
#71145=CARTESIAN_POINT('Ctrl Pts',(2.94238517904746,-0.981412986386104,
13.7730252682539));
#71146=CARTESIAN_POINT('Ctrl Pts',(2.36451469520878,-1.75845069530582,13.7204048978835));
#71147=CARTESIAN_POINT('Ctrl Pts',(1.7866442113701,-2.53548840422553,13.6677845275131));
#71148=CARTESIAN_POINT('Ctrl Pts',(0.788359391530092,-2.99988176362388,
13.6151641571428));
#71149=CARTESIAN_POINT('Ctrl Pts',(-0.178232238982059,-2.94131149038551,
13.5625437867724));
#71150=CARTESIAN_POINT('Ctrl Pts',(-1.14482386949421,-2.88274121714715,
13.509923416402));
#71151=CARTESIAN_POINT('Ctrl Pts',(-2.07972231067849,-2.30120731127206,
13.4573030460317));
#71152=CARTESIAN_POINT('Ctrl Pts',(-2.5595403212758,-1.46007567143488,13.4046826756613));
#71153=CARTESIAN_POINT('Ctrl Pts',(-2.81031856879004,-1.02045582826861,
13.3771804894707));
#71154=CARTESIAN_POINT('Ctrl Pts',(-2.9367843178467,-0.509922711901109,
13.3496783032802));
#71155=CARTESIAN_POINT('Ctrl Pts',(-2.93733773658367,0.000353650820144602,
13.3221761170896));
#71156=CARTESIAN_POINT('Ctrl Pts',(-2.93794966127546,0.0013934910171998,
13.1778238829104));
#71157=CARTESIAN_POINT('Ctrl Pts',(-2.9354435856223,-0.578098472832708,
13.2090728699418));
#71158=CARTESIAN_POINT('Ctrl Pts',(-2.76961959866241,-1.15891354184382,
13.2403218569731));
#71159=CARTESIAN_POINT('Ctrl Pts',(-2.45014221851649,-1.63706498032062,
13.2715708440045));
#71160=CARTESIAN_POINT('Ctrl Pts',(-1.91171629767549,-2.44290960207673,
13.3242358076712));
#71161=CARTESIAN_POINT('Ctrl Pts',(-0.936861131073665,-2.95715369414646,
13.3769007713379));
#71162=CARTESIAN_POINT('Ctrl Pts',(0.032249473718084,-2.94654692146698,
13.4295657350046));
#71163=CARTESIAN_POINT('Ctrl Pts',(1.00136007850986,-2.9359401487875,13.4822306986712));
#71164=CARTESIAN_POINT('Ctrl Pts',(1.96472612149158,-2.40048251135878,13.5348956623379));
#71165=CARTESIAN_POINT('Ctrl Pts',(2.48538560527679,-1.58304647931889,13.5875606260046));
#71166=CARTESIAN_POINT('Ctrl Pts',(3.00604508906198,-0.765610447279041,
13.6402255896713));
#71167=CARTESIAN_POINT('Ctrl Pts',(3.08399801365073,0.333803979371919,13.692890553338));
#71168=CARTESIAN_POINT('Ctrl Pts',(2.68388585052197,1.21652624548705,13.7455555170047));
#71169=CARTESIAN_POINT('Ctrl Pts',(2.28377368739319,2.0992485116022,13.7982204806713));
#71170=CARTESIAN_POINT('Ctrl Pts',(1.40559643654686,2.76527861718149,13.850885444338));
#71171=CARTESIAN_POINT('Ctrl Pts',(0.447678061833244,2.91251851826326,13.9035504080047));
#71172=CARTESIAN_POINT('Ctrl Pts',(-0.510240312880357,3.05975841934504,
13.9562153716714));
#71173=CARTESIAN_POINT('Ctrl Pts',(-1.54789981146125,2.68820811592931,14.0088803353381));
#71174=CARTESIAN_POINT('Ctrl Pts',(-2.1946428070508,1.96639671204873,14.0615452990048));
#71175=CARTESIAN_POINT('Ctrl Pts',(-2.67062249982462,1.435169358057,14.1003048269733));
#71176=CARTESIAN_POINT('Ctrl Pts',(-2.93486488519192,0.714225423327012,
14.1390643549419));
#71177=CARTESIAN_POINT('Ctrl Pts',(-2.94111188951679,-0.00259486169482749,
14.1778238829104));
#71178=CARTESIAN_POINT('Origin',(0.,0.,-1.84858989190501));
#71179=CARTESIAN_POINT('',(-2.37275986033066,-0.00196044888638088,14.651410108095));
#71180=CARTESIAN_POINT('',(-2.37517539399571,0.0009292342096269,14.848589891905));
#71181=CARTESIAN_POINT('',(-2.37175,-2.62313128856983E-13,-1.84858989190501));
#71182=CARTESIAN_POINT('',(-2.34668236863853,0.343918483395512,15.62825));
#71183=CARTESIAN_POINT('Ctrl Pts',(-2.37275986033066,-0.00196044888638126,
14.651410108095));
#71184=CARTESIAN_POINT('Ctrl Pts',(-2.37407562336888,-0.149148890039704,
14.6613011831744));
#71185=CARTESIAN_POINT('Ctrl Pts',(-2.29486163858049,-1.07797575416432,
14.7238126286243));
#71186=CARTESIAN_POINT('Ctrl Pts',(-1.07036982067409,-2.58532778276268,
14.8389444444444));
#71187=CARTESIAN_POINT('Ctrl Pts',(1.57881200919325,-2.30987053095853,14.9968055555556));
#71188=CARTESIAN_POINT('Ctrl Pts',(2.79654399706859,0.0566462213665858,
15.1546666666667));
#71189=CARTESIAN_POINT('Ctrl Pts',(1.48409012818578,2.37398300468726,15.3125277777778));
#71190=CARTESIAN_POINT('Ctrl Pts',(-1.17817012667699,2.53688639776398,15.4703888888889));
#71191=CARTESIAN_POINT('Ctrl Pts',(-2.23297482288527,1.11978691060522,15.5756296296296));
#71192=CARTESIAN_POINT('Ctrl Pts',(-2.34668236863854,0.343918483395395,
15.62825));
#71193=CARTESIAN_POINT('',(-0.439445221994505,2.33068358199182,15.62825));
#71194=CARTESIAN_POINT('Origin',(0.,0.,15.62825));
#71195=CARTESIAN_POINT('Ctrl Pts',(-2.37517539399571,0.000929234209626874,
14.848589891905));
#71196=CARTESIAN_POINT('Ctrl Pts',(-2.37154287511732,-0.72977569986937,
14.8978167399366));
#71197=CARTESIAN_POINT('Ctrl Pts',(-1.620069408967,-2.24871933567263,14.9997085516349));
#71198=CARTESIAN_POINT('Ctrl Pts',(0.958368222991996,-2.62865236842956,
15.1542653269999));
#71199=CARTESIAN_POINT('Ctrl Pts',(2.7277014223945,-0.634378452891388,15.3122602179999));
#71200=CARTESIAN_POINT('Ctrl Pts',(2.01676643438217,1.93930517753648,15.470255109));
#71201=CARTESIAN_POINT('Ctrl Pts',(0.331786659212352,2.47609764328476,15.5755850363333));
#71202=CARTESIAN_POINT('Ctrl Pts',(-0.439445221994538,2.33068358199181,
15.62825));
#71203=CARTESIAN_POINT('Origin',(0.,0.,-1.84858989190501));
#71204=CARTESIAN_POINT('',(-2.36799142649297,0.000285102424211894,13.651410108095));
#71205=CARTESIAN_POINT('',(-2.37103403261776,-0.00209189776527924,13.848589891905));
#71206=CARTESIAN_POINT('',(-2.37175,-2.62313128856983E-13,-1.84858989190501));
#71207=CARTESIAN_POINT('Ctrl Pts',(-2.36799142649297,0.000285102424211897,
13.651410108095));
#71208=CARTESIAN_POINT('Ctrl Pts',(-2.36754527731231,-0.41108402173757,
13.6789122942855));
#71209=CARTESIAN_POINT('Ctrl Pts',(-2.07052456040773,-1.61013525385437,
13.7590348508465));
#71210=CARTESIAN_POINT('Ctrl Pts',(-0.16923542984156,-2.79279215602584,
13.8917777777778));
#71211=CARTESIAN_POINT('Ctrl Pts',(2.24512421134353,-1.66965318578134,14.0496388888889));
#71212=CARTESIAN_POINT('Ctrl Pts',(2.62593313585052,0.965751391486786,14.2075));
#71213=CARTESIAN_POINT('Ctrl Pts',(0.628359679142483,2.72647005025058,14.3653611111111));
#71214=CARTESIAN_POINT('Ctrl Pts',(-1.77762972544941,2.06202090562868,14.5133311471428));
#71215=CARTESIAN_POINT('Ctrl Pts',(-2.36707578383325,0.633891398858792,
14.6086808128041));
#71216=CARTESIAN_POINT('Ctrl Pts',(-2.37275986033066,-0.00196044888638126,
14.651410108095));
#71217=CARTESIAN_POINT('Ctrl Pts',(-2.37103403261776,-0.00209189776527889,
13.848589891905));
#71218=CARTESIAN_POINT('Ctrl Pts',(-2.37284080801943,-0.20941258958213,
13.8624953276032));
#71219=CARTESIAN_POINT('Ctrl Pts',(-2.25333213139831,-1.19988405133594,
13.929065726968));
#71220=CARTESIAN_POINT('Ctrl Pts',(-0.869666078203209,-2.66015561356989,
14.0483010899995));
#71221=CARTESIAN_POINT('Ctrl Pts',(1.75267763866885,-2.18191305067097,14.2062959809995));
#71222=CARTESIAN_POINT('Ctrl Pts',(2.78512620401791,0.275629071355557,14.3642908719996));
#71223=CARTESIAN_POINT('Ctrl Pts',(1.29091271455523,2.48320730756548,14.5222857629997));
#71224=CARTESIAN_POINT('Ctrl Pts',(-1.37414448785656,2.43798182357128,14.6802806539997));
#71225=CARTESIAN_POINT('Ctrl Pts',(-2.35095938458833,0.884486526760038,
14.7890486969682));
#71226=CARTESIAN_POINT('Ctrl Pts',(-2.37542909742077,0.0519633377314283,
14.8451517762699));
#71227=CARTESIAN_POINT('Ctrl Pts',(-2.37517539399571,0.000929234209626874,
14.848589891905));
#71228=CARTESIAN_POINT('Origin',(0.,0.,-1.84858989190501));
#71229=CARTESIAN_POINT('',(-2.3737947408518,0.00170749448784205,12.651410108095));
#71230=CARTESIAN_POINT('',(-2.36848474137664,0.00112338963946246,12.848589891905));
#71231=CARTESIAN_POINT('',(-2.37175,-2.62313128856983E-13,-1.84858989190501));
#71232=CARTESIAN_POINT('Ctrl Pts',(-2.3737947408518,0.00170749448784207,
12.651410108095));
#71233=CARTESIAN_POINT('Ctrl Pts',(-2.36833312974404,-0.668887685031927,
12.6965234053967));
#71234=CARTESIAN_POINT('Ctrl Pts',(-1.72235411599047,-2.13088047848934,
12.7942570730687));
#71235=CARTESIAN_POINT('Ctrl Pts',(0.750172845833004,-2.69546828972993,
12.9446111111111));
#71236=CARTESIAN_POINT('Ctrl Pts',(2.66668266040929,-0.846825037914988,
13.1024722222222));
#71237=CARTESIAN_POINT('Ctrl Pts',(2.16784415239069,1.76882949166842,13.2603333333333));
#71238=CARTESIAN_POINT('Ctrl Pts',(-0.294517949969841,2.78236767093066,
13.4181944444444));
#71239=CARTESIAN_POINT('Ctrl Pts',(-2.10760963637491,1.5382497642797,13.548553369365));
#71240=CARTESIAN_POINT('Ctrl Pts',(-2.36839890163746,0.375995067988055,
13.6262919239152));
#71241=CARTESIAN_POINT('Ctrl Pts',(-2.36799142649297,0.000285102424211897,
13.651410108095));
#71242=CARTESIAN_POINT('Ctrl Pts',(-2.36848474137664,0.00112338963946246,
12.848589891905));
#71243=CARTESIAN_POINT('Ctrl Pts',(-2.36646442019019,-0.466045225337024,
12.8798388789364));
#71244=CARTESIAN_POINT('Ctrl Pts',(-2.00748312661735,-1.72341304420753,
12.9637528296344));
#71245=CARTESIAN_POINT('Ctrl Pts',(0.0306296239850783,-2.7985342282319,
13.1003317439992));
#71246=CARTESIAN_POINT('Ctrl Pts',(2.36053793034993,-1.50352574600393,13.2583266349992));
#71247=CARTESIAN_POINT('Ctrl Pts',(2.54906768788899,1.15541663986578,13.4163215259993));
#71248=CARTESIAN_POINT('Ctrl Pts',(0.42518914129335,2.76621565710669,13.5743164169993));
#71249=CARTESIAN_POINT('Ctrl Pts',(-1.86352481270074,1.94670562977947,13.7184058723013));
#71250=CARTESIAN_POINT('Ctrl Pts',(-2.36599788968529,0.57578658999839,13.8098303639365));
#71251=CARTESIAN_POINT('Ctrl Pts',(-2.37103403261776,-0.00209189776527889,
13.848589891905));
#71252=CARTESIAN_POINT('Origin',(0.,0.,-1.84858989190501));
#71253=CARTESIAN_POINT('',(-2.37270243253876,-0.00200498951788303,11.651410108095));
#71254=CARTESIAN_POINT('',(-2.37496958658182,0.00104863022067879,11.848589891905));
#71255=CARTESIAN_POINT('',(-2.37175,-2.62313128856983E-13,-1.84858989190501));
#71256=CARTESIAN_POINT('Ctrl Pts',(-2.37270243253876,-0.00200498951788284,
11.651410108095));
#71257=CARTESIAN_POINT('Ctrl Pts',(-2.37405198430164,-0.152377883745359,
11.6615141461374));
#71258=CARTESIAN_POINT('Ctrl Pts',(-2.29281607417404,-1.08441874324097,
11.7242385545502));
#71259=CARTESIAN_POINT('Ctrl Pts',(-1.05977053720295,-2.58943908287633,
11.8395833333333));
#71260=CARTESIAN_POINT('Ctrl Pts',(1.58766534266525,-2.30382879610199,11.9974444444444));
#71261=CARTESIAN_POINT('Ctrl Pts',(2.79707340746319,0.0684743370742143,
12.1553055555555));
#71262=CARTESIAN_POINT('Ctrl Pts',(1.47303233105958,2.37875683253439,12.3131666666667));
#71263=CARTESIAN_POINT('Ctrl Pts',(-1.18520769732058,2.53448043892505,12.4710277777778));
#71264=CARTESIAN_POINT('Ctrl Pts',(-2.31706196946124,1.00613052370996,12.5837755915872));
#71265=CARTESIAN_POINT('Ctrl Pts',(-2.37470357962243,0.113297808503467,
12.6439030350263));
#71266=CARTESIAN_POINT('Ctrl Pts',(-2.3737947408518,0.00170749448784207,
12.651410108095));
#71267=CARTESIAN_POINT('Ctrl Pts',(-2.37496958658182,0.00104863022067909,
11.848589891905));
#71268=CARTESIAN_POINT('Ctrl Pts',(-2.37095686672064,-0.72032558818314,
11.8971824302696));
#71269=CARTESIAN_POINT('Ctrl Pts',(-1.63667192852724,-2.23060698037937,
11.9984399323009));
#71270=CARTESIAN_POINT('Ctrl Pts',(0.927689321261817,-2.64047796075702,
12.1523623979988));
#71271=CARTESIAN_POINT('Ctrl Pts',(2.71833714731268,-0.66586366962402,12.3103572889989));
#71272=CARTESIAN_POINT('Ctrl Pts',(2.04302496870488,1.91279385105346,12.468352179999));
#71273=CARTESIAN_POINT('Ctrl Pts',(-0.48563275555883,2.75624604578475,12.626347070999));
#71274=CARTESIAN_POINT('Ctrl Pts',(-2.16074812800628,1.4270578867686,12.7530929749677));
#71275=CARTESIAN_POINT('Ctrl Pts',(-2.36986933510064,0.32128967640745,12.8271739152697));
#71276=CARTESIAN_POINT('Ctrl Pts',(-2.36848474137664,0.00112338963946246,
12.848589891905));
#71277=CARTESIAN_POINT('Origin',(0.,0.,-1.84858989190501));
#71278=CARTESIAN_POINT('',(-2.3680043592011,0.000335278925106314,10.651410108095));
#71279=CARTESIAN_POINT('',(-2.37130727717011,-0.00210928510120167,10.848589891905));
#71280=CARTESIAN_POINT('',(-2.37175,-2.62313128856983E-13,-1.84858989190501));
#71281=CARTESIAN_POINT('Ctrl Pts',(-2.3680043592011,0.000335278925106194,
10.651410108095));
#71282=CARTESIAN_POINT('Ctrl Pts',(-2.36747521485208,-0.414214015593381,
10.6791252572485));
#71283=CARTESIAN_POINT('Ctrl Pts',(-2.06710351553143,-1.61654972761244,
10.7594607767724));
#71284=CARTESIAN_POINT('Ctrl Pts',(-0.158018739337926,-2.79344562132492,
10.8924166666667));
#71285=CARTESIAN_POINT('Ctrl Pts',(2.25180017160661,-1.66063371893121,11.0502777777778));
#71286=CARTESIAN_POINT('Ctrl Pts',(2.62205116590109,0.976297109112734,11.2081388888889));
#71287=CARTESIAN_POINT('Ctrl Pts',(0.617379419647229,2.72894686881467,11.366));
#71288=CARTESIAN_POINT('Ctrl Pts',(-1.78238141625357,2.05587933285381,11.5137570730687));
#71289=CARTESIAN_POINT('Ctrl Pts',(-2.36702371369352,0.630742424660346,
11.608893775767));
#71290=CARTESIAN_POINT('Ctrl Pts',(-2.37270243253876,-0.00200498951788284,
11.651410108095));
#71291=CARTESIAN_POINT('Ctrl Pts',(-2.37130727717011,-0.00210928510120129,
10.848589891905));
#71292=CARTESIAN_POINT('Ctrl Pts',(-2.37306236960384,-0.199914469168129,
10.8618610179362));
#71293=CARTESIAN_POINT('Ctrl Pts',(-2.26024839139859,-1.18071373741556,
10.927797107634));
#71294=CARTESIAN_POINT('Ctrl Pts',(-0.90141796228012,-2.64956165719617,
11.0463981609985));
#71295=CARTESIAN_POINT('Ctrl Pts',(1.72648179491819,-2.20272375262492,11.2043930519985));
#71296=CARTESIAN_POINT('Ctrl Pts',(2.7881905800153,0.242331605070017,11.3623879429986));
#71297=CARTESIAN_POINT('Ctrl Pts',(1.32057126786748,2.46755402056041,11.5203828339987));
#71298=CARTESIAN_POINT('Ctrl Pts',(-1.34501422335496,2.45431621031658,11.6783777249987));
#71299=CARTESIAN_POINT('Ctrl Pts',(-2.34590203170026,0.903460530701682,
11.7877800776342));
#71300=CARTESIAN_POINT('Ctrl Pts',(-2.37530588310888,0.0615052912262518,
11.8445174666029));
#71301=CARTESIAN_POINT('Ctrl Pts',(-2.37496958658182,0.00104863022067909,
11.848589891905));
#71302=CARTESIAN_POINT('Origin',(0.,0.,-1.84858989190501));
#71303=CARTESIAN_POINT('',(-2.37387835550442,0.0016747535505271,9.65141010809499));
#71304=CARTESIAN_POINT('',(-2.36835645684558,0.000990747813277848,9.84858989190503));
#71305=CARTESIAN_POINT('',(-2.37175,-2.62313128856983E-13,-1.84858989190501));
#71306=CARTESIAN_POINT('Ctrl Pts',(-2.37387835550442,0.00167475355052717,
9.65141010809499));
#71307=CARTESIAN_POINT('Ctrl Pts',(-2.36846517734921,-0.672024104003181,
9.69673636835963));
#71308=CARTESIAN_POINT('Ctrl Pts',(-1.71729169385484,-2.1369916722257,9.79468299899462));
#71309=CARTESIAN_POINT('Ctrl Pts',(0.760987165659879,-2.69243512365168,
9.94525));
#71310=CARTESIAN_POINT('Ctrl Pts',(2.6700603672968,-0.836113626465368,10.1031111111111));
#71311=CARTESIAN_POINT('Ctrl Pts',(2.16072649637127,1.7775177549783,10.2609722222222));
#71312=CARTESIAN_POINT('Ctrl Pts',(-0.305685313585232,2.78116249982291,
10.4188333333333));
#71313=CARTESIAN_POINT('Ctrl Pts',(-2.11081288774265,1.53182193243431,10.5489792952909));
#71314=CARTESIAN_POINT('Ctrl Pts',(-2.36847985572451,0.37285508129321,10.6265048868781));
#71315=CARTESIAN_POINT('Ctrl Pts',(-2.3680043592011,0.000335278925106194,
10.651410108095));
#71316=CARTESIAN_POINT('Ctrl Pts',(-2.36835645684558,0.00099074781327764,
9.84858989190503));
#71317=CARTESIAN_POINT('Ctrl Pts',(-2.36661646666674,-0.456757128880904,
9.87920456926939));
#71318=CARTESIAN_POINT('Ctrl Pts',(-2.01853982608692,-1.70439405627733,
9.96248421030043));
#71319=CARTESIAN_POINT('Ctrl Pts',(-0.00283249851198579,-2.79870028674429,
10.0984288149982));
#71320=CARTESIAN_POINT('Ctrl Pts',(2.34239313895008,-1.53164150527581,10.2564237059982));
#71321=CARTESIAN_POINT('Ctrl Pts',(2.56269918704329,1.12485741087042,10.4144185969983));
#71322=CARTESIAN_POINT('Ctrl Pts',(0.458233353927178,2.76093344928963,10.5724134879983));
#71323=CARTESIAN_POINT('Ctrl Pts',(-1.85023633825226,1.96536160231837,10.7171372529672));
#71324=CARTESIAN_POINT('Ctrl Pts',(-2.36609748365237,0.585053046589831,
10.8091960542695));
#71325=CARTESIAN_POINT('Ctrl Pts',(-2.37130727717011,-0.00210928510120129,
10.848589891905));
#71326=CARTESIAN_POINT('Origin',(0.,0.,-1.84858989190501));
#71327=CARTESIAN_POINT('',(-2.37260887298938,-0.00202072084187682,8.65141010809499));
#71328=CARTESIAN_POINT('',(-2.3747901511292,0.00119133359606532,8.84858989190503));
#71329=CARTESIAN_POINT('',(-2.37175,-2.62313128856983E-13,-1.84858989190501));
#71330=CARTESIAN_POINT('Ctrl Pts',(-2.37260887298937,-0.00202072084187674,
8.65141010809499));
#71331=CARTESIAN_POINT('Ctrl Pts',(-2.37399141457934,-0.155578652695773,
8.66172710910036));
#71332=CARTESIAN_POINT('Ctrl Pts',(-2.29073220490892,-1.09084435213441,
8.72466448047611));
#71333=CARTESIAN_POINT('Ctrl Pts',(-1.04936735270146,-2.59367240037321,
8.84022222222223));
#71334=CARTESIAN_POINT('Ctrl Pts',(1.59690068918271,-2.29743695240177,8.99808333333332));
#71335=CARTESIAN_POINT('Ctrl Pts',(2.79677599470576,0.0797019247629725,
9.15594444444445));
#71336=CARTESIAN_POINT('Ctrl Pts',(1.46347155312646,2.38465078671139,9.31380555555555));
#71337=CARTESIAN_POINT('Ctrl Pts',(-1.19537219008389,2.52970229247383,9.47166666666666));
#71338=CARTESIAN_POINT('Ctrl Pts',(-2.31895585283185,0.999716542450464,
9.58420151751315));
#71339=CARTESIAN_POINT('Ctrl Pts',(-2.37474946901026,0.110089469797055,
9.64411599798926));
#71340=CARTESIAN_POINT('Ctrl Pts',(-2.37387835550442,0.00167475355052717,
9.65141010809499));
#71341=CARTESIAN_POINT('Ctrl Pts',(-2.3747901511292,0.00119133359606537,
8.84858989190503));
#71342=CARTESIAN_POINT('Ctrl Pts',(-2.37038906205444,-0.71090872088079,
8.89654812060261));
#71343=CARTESIAN_POINT('Ctrl Pts',(-1.65267775677864,-2.21269450774448,
8.99717131296688));
#71344=CARTESIAN_POINT('Ctrl Pts',(0.896053003445084,-2.6513808351669,9.15045946899784));
#71345=CARTESIAN_POINT('Ctrl Pts',(2.71018167460651,-0.698316982967359,
9.30845435999788));
#71346=CARTESIAN_POINT('Ctrl Pts',(2.06574861445826,1.88823038317285,9.46644925099794));
#71347=CARTESIAN_POINT('Ctrl Pts',(-0.45264386973844,2.76185532663481,9.62444414199799));
#71348=CARTESIAN_POINT('Ctrl Pts',(-2.15199374797492,1.44623886325989,9.75182435563369));
#71349=CARTESIAN_POINT('Ctrl Pts',(-2.36960968846224,0.330684626839437,
9.8265396056027));
#71350=CARTESIAN_POINT('Ctrl Pts',(-2.36835645684558,0.00099074781327764,
9.84858989190503));
#71351=CARTESIAN_POINT('Origin',(0.,0.,-1.84858989190501));
#71352=CARTESIAN_POINT('',(-2.36801892187683,0.000385579322849399,7.65141010809499));
#71353=CARTESIAN_POINT('',(-2.37158591103805,-0.00211396583053219,7.84858989190503));
#71354=CARTESIAN_POINT('',(-2.37175,-2.62313128856983E-13,-1.84858989190501));
#71355=CARTESIAN_POINT('Ctrl Pts',(-2.36801892187683,0.000385579322849869,
7.65141010809499));
#71356=CARTESIAN_POINT('Ctrl Pts',(-2.36740549965901,-0.417342685994756,
7.67933822021147));
#71357=CARTESIAN_POINT('Ctrl Pts',(-2.06366306314178,-1.62296175556451,
7.75988670269832));
#71358=CARTESIAN_POINT('Ctrl Pts',(-0.146803886877873,-2.79405744038503,
7.89305555555557));
#71359=CARTESIAN_POINT('Ctrl Pts',(2.25844822171206,-1.65158105802259,8.05091666666665));
#71360=CARTESIAN_POINT('Ctrl Pts',(2.61811094239596,0.986814802625037,8.20877777777778));
#71361=CARTESIAN_POINT('Ctrl Pts',(0.606419780073446,2.73140319464357,8.36663888888888));
#71362=CARTESIAN_POINT('Ctrl Pts',(-1.7871649975578,2.04969182184781,8.51418299899463));
#71363=CARTESIAN_POINT('Ctrl Pts',(-2.36693996130543,0.627621353124904,
8.60910673873));
#71364=CARTESIAN_POINT('Ctrl Pts',(-2.37260887298937,-0.00202072084187674,
8.65141010809499));
#71365=CARTESIAN_POINT('Ctrl Pts',(-2.37158591103805,-0.002113965830532,
7.84858989190503));
#71366=CARTESIAN_POINT('Ctrl Pts',(-2.37327853101496,-0.190408271679788,
7.86122670826915));
#71367=CARTESIAN_POINT('Ctrl Pts',(-2.26703071089283,-1.16154754141212,
7.92652848829996));
#71368=CARTESIAN_POINT('Ctrl Pts',(-0.9330321424437,-2.63859476601473,8.04449523199746));
#71369=CARTESIAN_POINT('Ctrl Pts',(1.70002224901497,-2.22320841823872,8.2024901229975));
#71370=CARTESIAN_POINT('Ctrl Pts',(2.79088864512093,0.208978201275766,8.36048501399757));
#71371=CARTESIAN_POINT('Ctrl Pts',(1.34997937336987,2.45158867054595,8.51847990499762));
#71372=CARTESIAN_POINT('Ctrl Pts',(-1.31557386100644,2.47022200101732,8.67647479599767));
#71373=CARTESIAN_POINT('Ctrl Pts',(-2.34084261733164,0.922522196646213,
8.78651145830014));
#71374=CARTESIAN_POINT('Ctrl Pts',(-2.37522208450983,0.0710785316625285,
8.84388315693593));
#71375=CARTESIAN_POINT('Ctrl Pts',(-2.3747901511292,0.00119133359606537,
8.84858989190503));
#71376=CARTESIAN_POINT('Origin',(0.,0.,-1.84858989190501));
#71377=CARTESIAN_POINT('',(-2.37396076251026,0.0016408096299993,6.65141010809499));
#71378=CARTESIAN_POINT('',(-2.36824488832617,0.00085307042009708,6.84858989190503));
#71379=CARTESIAN_POINT('',(-2.37175,-2.62313128856983E-13,-1.84858989190501));
#71380=CARTESIAN_POINT('Ctrl Pts',(-2.37396076251026,0.00164080962999946,
6.65141010809499));
#71381=CARTESIAN_POINT('Ctrl Pts',(-2.36860111288507,-0.675161988858878,
6.69694933132258));
#71382=CARTESIAN_POINT('Ctrl Pts',(-1.71220786555833,-2.14309654094568,
6.79510892492056));
#71383=CARTESIAN_POINT('Ctrl Pts',(0.771789132562049,-2.68935864031417,
6.94588888888888));
#71384=CARTESIAN_POINT('Ctrl Pts',(2.67339522049833,-0.825388609316905,
7.10375));
#71385=CARTESIAN_POINT('Ctrl Pts',(2.15357369271338,1.7861771220756,7.26161111111111));
#71386=CARTESIAN_POINT('Ctrl Pts',(-0.3168471224657,2.77991299546561,7.41947222222222));
#71387=CARTESIAN_POINT('Ctrl Pts',(-2.11399942046796,1.52539245310181,7.54940522121685));
#71388=CARTESIAN_POINT('Ctrl Pts',(-2.36856127073871,0.369714310321545,
7.62671784984111));
#71389=CARTESIAN_POINT('Ctrl Pts',(-2.36801892187683,0.000385579322849869,
7.65141010809499));
#71390=CARTESIAN_POINT('Ctrl Pts',(-2.36824488832617,0.000853070420097184,
6.84858989190503));
#71391=CARTESIAN_POINT('Ctrl Pts',(-2.36678180876479,-0.447463537758943,
6.87857025960238));
#71392=CARTESIAN_POINT('Ctrl Pts',(-2.02943011823198,-1.68535627820218,
6.96121559096642));
#71393=CARTESIAN_POINT('Ctrl Pts',(-0.0362940343214689,-2.79846637663312,
7.09652588599712));
#71394=CARTESIAN_POINT('Ctrl Pts',(2.32391314315961,-1.55953807940794,7.2545207769972));
#71395=CARTESIAN_POINT('Ctrl Pts',(2.57596499873257,1.09413693995685,7.41251566799723));
#71396=CARTESIAN_POINT('Ctrl Pts',(0.491210792034311,2.75525738831465,7.5705105589973));
#71397=CARTESIAN_POINT('Ctrl Pts',(-1.83676464589149,1.98397717256952,7.71586863363322));
#71398=CARTESIAN_POINT('Ctrl Pts',(-2.36622439910258,0.594323617306658,
7.80856174460247));
#71399=CARTESIAN_POINT('Ctrl Pts',(-2.37158591103805,-0.002113965830532,
7.84858989190503));
#71400=CARTESIAN_POINT('Origin',(0.,0.,-1.84858989190501));
#71401=CARTESIAN_POINT('',(-2.37251499866524,-0.00203510706959473,5.65141010809499));
#71402=CARTESIAN_POINT('',(-2.37459246787895,0.00132584644941116,5.84858989190502));
#71403=CARTESIAN_POINT('',(-2.37175,-2.62313128856983E-13,-1.84858989190501));
#71404=CARTESIAN_POINT('Ctrl Pts',(-2.37251499866524,-0.00203510706959476,
5.65141010809499));
#71405=CARTESIAN_POINT('Ctrl Pts',(-2.37392982983489,-0.158778764602934,
5.66194007206332));
#71406=CARTESIAN_POINT('Ctrl Pts',(-2.28863365792017,-1.09727074999648,
5.72509040640203));
#71407=CARTESIAN_POINT('Ctrl Pts',(-1.03894725747156,-2.59786392206505,
5.84086111111111));
#71408=CARTESIAN_POINT('Ctrl Pts',(1.60611030100396,-2.29100808867664,5.99872222222222));
#71409=CARTESIAN_POINT('Ctrl Pts',(2.79643351757374,0.090928230838667,6.15658333333333));
#71410=CARTESIAN_POINT('Ctrl Pts',(1.45388718569001,2.39050630885174,6.31444444444444));
#71411=CARTESIAN_POINT('Ctrl Pts',(-1.20551740739643,2.52488339173069,6.47230555555556));
#71412=CARTESIAN_POINT('Ctrl Pts',(-2.3208356274226,0.99330351170231,6.58462744343907));
#71413=CARTESIAN_POINT('Ctrl Pts',(-2.37479416424485,0.106880641648857,
6.64432896095221));
#71414=CARTESIAN_POINT('Ctrl Pts',(-2.37396076251026,0.00164080962999946,
6.65141010809499));
#71415=CARTESIAN_POINT('Ctrl Pts',(-2.37459246787895,0.00132584644941126,
5.84858989190502));
#71416=CARTESIAN_POINT('Ctrl Pts',(-2.3698592307678,-0.701510136856058,
5.8959138109356));
#71417=CARTESIAN_POINT('Ctrl Pts',(-1.6684907359976,-2.19471791424095,5.99590269363287));
#71418=CARTESIAN_POINT('Ctrl Pts',(0.864288593995119,-2.66190468356086,
6.14855653999681));
#71419=CARTESIAN_POINT('Ctrl Pts',(2.70163876039796,-0.730670463607777,
6.30655143099686));
#71420=CARTESIAN_POINT('Ctrl Pts',(2.08817696449889,1.86339697407977,6.46454632199692));
#71421=CARTESIAN_POINT('Ctrl Pts',(-0.419590302218696,2.76706980330411,
6.62254121299697));
#71422=CARTESIAN_POINT('Ctrl Pts',(-2.14308835195883,1.46541542002878,6.75055573629967));
#71423=CARTESIAN_POINT('Ctrl Pts',(-2.36935192507288,0.340071095547311,
6.82590529593569));
#71424=CARTESIAN_POINT('Ctrl Pts',(-2.36824488832617,0.000853070420097184,
6.84858989190503));
#71425=CARTESIAN_POINT('Origin',(0.,0.,-1.84858989190501));
#71426=CARTESIAN_POINT('',(-2.36803551809634,0.000435659979227324,4.65141010809499));
#71427=CARTESIAN_POINT('',(-2.37186713520955,-0.00210673407030348,4.84858989190502));
#71428=CARTESIAN_POINT('',(-2.37175,-2.62313128856983E-13,-1.84858989190501));
#71429=CARTESIAN_POINT('Ctrl Pts',(-2.36803551809634,0.000435659979227676,
4.65141010809499));
#71430=CARTESIAN_POINT('Ctrl Pts',(-2.36733685507668,-0.420470574046625,
4.67955118317444));
#71431=CARTESIAN_POINT('Ctrl Pts',(-2.06020439223756,-1.62937224150312,
4.76031262862425));
#71432=CARTESIAN_POINT('Ctrl Pts',(-0.135586668767159,-2.79462423533096,
4.89369444444444));
#71433=CARTESIAN_POINT('Ctrl Pts',(2.2650598786042,-1.64250178316317,5.05155555555556));
#71434=CARTESIAN_POINT('Ctrl Pts',(2.61412853009539,0.997316594419356,5.20941666666666));
#71435=CARTESIAN_POINT('Ctrl Pts',(0.595450368366912,2.73381550588105,5.36727777777778));
#71436=CARTESIAN_POINT('Ctrl Pts',(-1.79192767962886,2.0434990191552,5.51460892492054));
#71437=CARTESIAN_POINT('Ctrl Pts',(-2.36685963088812,0.624501153297232,
5.60931970169295));
#71438=CARTESIAN_POINT('Ctrl Pts',(-2.37251499866524,-0.00203510706959476,
5.65141010809499));
#71439=CARTESIAN_POINT('Ctrl Pts',(-2.37186713520955,-0.00210673407030307,
4.84858989190502));
#71440=CARTESIAN_POINT('Ctrl Pts',(-2.37348726775032,-0.180895246540068,
4.86059239860214));
#71441=CARTESIAN_POINT('Ctrl Pts',(-2.27367886126175,-1.14238681798702,
4.92525986896595));
#71442=CARTESIAN_POINT('Ctrl Pts',(-0.964512940920624,-2.62725067416123,
5.04259230299644));
#71443=CARTESIAN_POINT('Ctrl Pts',(1.67331967629405,-2.24337526486265,5.20058719399648));
#71444=CARTESIAN_POINT('Ctrl Pts',(2.79318773824162,0.175594923072764,5.35858208499656));
#71445=CARTESIAN_POINT('Ctrl Pts',(1.37919449268132,2.43527285317938,5.51657697599659));
#71446=CARTESIAN_POINT('Ctrl Pts',(-1.28594543116668,2.48577466117395,5.67457186699666));
#71447=CARTESIAN_POINT('Ctrl Pts',(-2.33566190719347,0.94159330950118,5.78524283896613));
#71448=CARTESIAN_POINT('Ctrl Pts',(-2.37512666773395,0.0806489125773547,
5.84324884726892));
#71449=CARTESIAN_POINT('Ctrl Pts',(-2.37459246787895,0.00132584644941126,
5.84858989190502));
#71450=CARTESIAN_POINT('Origin',(0.,0.,-1.84858989190501));
#71451=CARTESIAN_POINT('',(-2.37404189208837,0.00160568163382189,3.65141010809499));
#71452=CARTESIAN_POINT('',(-2.36815046112586,0.00071106261527204,3.84858989190502));
#71453=CARTESIAN_POINT('',(-2.37175,-2.62313128856983E-13,-1.84858989190501));
#71454=CARTESIAN_POINT('Ctrl Pts',(-2.37404189208837,0.0016056816338219,
3.65141010809499));
#71455=CARTESIAN_POINT('Ctrl Pts',(-2.36874097406567,-0.678301390146093,
3.69716229428555));
#71456=CARTESIAN_POINT('Ctrl Pts',(-1.70710264047504,-2.14919504149034,
3.79553485084648));
#71457=CARTESIAN_POINT('Ctrl Pts',(0.782578662553965,-2.68623882063674,
3.94652777777777));
#71458=CARTESIAN_POINT('Ctrl Pts',(2.67668699402767,-0.814650291328897,
4.10438888888889));
#71459=CARTESIAN_POINT('Ctrl Pts',(2.14638618582228,1.79480770611467,4.26225));
#71460=CARTESIAN_POINT('Ctrl Pts',(-0.328003825581952,2.77861869501174,
4.42011111111111));
#71461=CARTESIAN_POINT('Ctrl Pts',(-2.1171683957745,1.51896204170615,4.54983114714277));
#71462=CARTESIAN_POINT('Ctrl Pts',(-2.3686432695173,0.366572631058683,4.62693081280407));
#71463=CARTESIAN_POINT('Ctrl Pts',(-2.36803551809634,0.000435659979227676,
4.65141010809499));
#71464=CARTESIAN_POINT('Ctrl Pts',(-2.36815046112586,0.000711062615271901,
3.84858989190502));
#71465=CARTESIAN_POINT('Ctrl Pts',(-2.36695951468436,-0.438164069114789,
3.87793594993537));
#71466=CARTESIAN_POINT('Ctrl Pts',(-2.04015506879268,-1.66630099353556,
3.9599469716324));
#71467=CARTESIAN_POINT('Ctrl Pts',(-0.0697503817448946,-2.79783241149437,
4.09462295699612));
#71468=CARTESIAN_POINT('Ctrl Pts',(2.30510093209087,-1.58721170953314,4.25261784799616));
#71469=CARTESIAN_POINT('Ctrl Pts',(2.5888625630092,1.06326005653742,4.41061273899623));
#71470=CARTESIAN_POINT('Ctrl Pts',(0.524118009051023,2.74918744918107,4.56860762999628));
#71471=CARTESIAN_POINT('Ctrl Pts',(-1.82311086019465,2.00255204277458,4.71460001429921));
#71472=CARTESIAN_POINT('Ctrl Pts',(-2.36637840094874,0.603598422228309,
4.80792743493546));
#71473=CARTESIAN_POINT('Ctrl Pts',(-2.37186713520955,-0.00210673407030307,
4.84858989190502));
#71474=CARTESIAN_POINT('Origin',(0.,0.,-1.84858989190501));
#71475=CARTESIAN_POINT('',(-2.37242086931256,-0.00204814969984112,2.65141010809499));
#71476=CARTESIAN_POINT('',(-2.37437841508221,0.00145143062880153,2.84858989190502));
#71477=CARTESIAN_POINT('',(-2.37175,-2.62313128856983E-13,-1.84858989190501));
#71478=CARTESIAN_POINT('Ctrl Pts',(-2.37242086931256,-0.00204814969984169,
2.65141010809499));
#71479=CARTESIAN_POINT('Ctrl Pts',(-2.37386724785776,-0.161978223542019,
2.66215303502629));
#71480=CARTESIAN_POINT('Ctrl Pts',(-2.28652040521148,-1.10369798895945,
2.72551633232796));
#71481=CARTESIAN_POINT('Ctrl Pts',(-1.02851040967351,-2.60201352259292,
2.84149999999999));
#71482=CARTESIAN_POINT('Ctrl Pts',(1.61529402596567,-2.28454233775194,2.99936111111111));
#71483=CARTESIAN_POINT('Ctrl Pts',(2.79604598097933,0.102153087721166,3.15722222222222));
#71484=CARTESIAN_POINT('Ctrl Pts',(1.44427938842878,2.39632330140064,3.31508333333333));
#71485=CARTESIAN_POINT('Ctrl Pts',(-1.21564319790733,2.5200238088076,3.47294444444445));
#71486=CARTESIAN_POINT('Ctrl Pts',(-2.32270131739363,0.986891451715146,
3.58505336936499));
#71487=CARTESIAN_POINT('Ctrl Pts',(-2.37483765037521,0.103671339757588,
3.64454192391517));
#71488=CARTESIAN_POINT('Ctrl Pts',(-2.37404189208837,0.0016056816338219,
3.65141010809499));
#71489=CARTESIAN_POINT('Ctrl Pts',(-2.37437841508221,0.00145143062880148,
2.84858989190502));
#71490=CARTESIAN_POINT('Ctrl Pts',(-2.36936657242201,-0.69212851464997,
2.89527950126859));
#71491=CARTESIAN_POINT('Ctrl Pts',(-1.68411161328175,-2.17667922631145,
2.99463407429885));
#71492=CARTESIAN_POINT('Ctrl Pts',(0.832400628534772,-2.67204800324426,
3.1466536109958));
#71493=CARTESIAN_POINT('Ctrl Pts',(2.69270963387839,-0.762919488957052,
3.30464850199585));
#71494=CARTESIAN_POINT('Ctrl Pts',(2.11030679852043,1.83829718168443,3.4626433929959));
#71495=CARTESIAN_POINT('Ctrl Pts',(-0.386476751895552,2.77188871376435,
3.62063828399595));
#71496=CARTESIAN_POINT('Ctrl Pts',(-2.13403081733917,1.48458669705641,3.74928711696566));
#71497=CARTESIAN_POINT('Ctrl Pts',(-2.36909680859298,0.349449137499666,
3.82527098626868));
#71498=CARTESIAN_POINT('Ctrl Pts',(-2.36815046112586,0.000711062615271901,
3.84858989190502));
#71499=CARTESIAN_POINT('Origin',(0.,0.,-1.84858989190501));
#71500=CARTESIAN_POINT('',(-2.36805372255214,0.000487775483918624,1.65141010809499));
#71501=CARTESIAN_POINT('',(-2.37214954248261,-0.00208751672060303,1.84858989190502));
#71502=CARTESIAN_POINT('',(-2.37175,-2.62313128856983E-13,-1.84858989190501));
#71503=CARTESIAN_POINT('Ctrl Pts',(-2.36805372255214,0.000487775483918769,
1.65141010809499));
#71504=CARTESIAN_POINT('Ctrl Pts',(-2.36726911244657,-0.423596588857836,
1.6797641461374));
#71505=CARTESIAN_POINT('Ctrl Pts',(-2.0567282222087,-1.63578530702029,1.76073855455018));
#71506=CARTESIAN_POINT('Ctrl Pts',(-0.124366744542119,-2.79514315034066,
1.89433333333333));
#71507=CARTESIAN_POINT('Ctrl Pts',(2.27163476293377,-1.63339753074864,2.05219444444444));
#71508=CARTESIAN_POINT('Ctrl Pts',(2.61010413592219,1.00780309522069,2.21005555555555));
#71509=CARTESIAN_POINT('Ctrl Pts',(0.584471286669745,2.73618335546233,2.36791666666667));
#71510=CARTESIAN_POINT('Ctrl Pts',(-1.79666946585791,2.03730116384381,2.51503485084647));
#71511=CARTESIAN_POINT('Ctrl Pts',(-2.36678268187025,0.621381820955435,
2.60953266465592));
#71512=CARTESIAN_POINT('Ctrl Pts',(-2.37242086931256,-0.00204814969984169,
2.65141010809499));
#71513=CARTESIAN_POINT('Ctrl Pts',(-2.37214954248261,-0.00208751672060286,
1.84858989190502));
#71514=CARTESIAN_POINT('Ctrl Pts',(-2.37368814589582,-0.171375740131997,
1.85995808893514));
#71515=CARTESIAN_POINT('Ctrl Pts',(-2.28019409230745,-1.12323247312203,
1.92399124963194));
#71516=CARTESIAN_POINT('Ctrl Pts',(-0.995855715555496,-2.61553061219188,
2.04068937399542));
#71517=CARTESIAN_POINT('Ctrl Pts',(1.64637781974439,-2.26322161422709,2.19868426499547));
#71518=CARTESIAN_POINT('Ctrl Pts',(2.79508756969503,0.142186649832604,2.35667915599553));
#71519=CARTESIAN_POINT('Ctrl Pts',(1.40821242874264,2.41860884498944,2.51467404699558));
#71520=CARTESIAN_POINT('Ctrl Pts',(-1.25613315819632,2.50097199645567,2.67266893799564));
#71521=CARTESIAN_POINT('Ctrl Pts',(-2.33035893824447,0.960673681793537,
2.78397421963211));
#71522=CARTESIAN_POINT('Ctrl Pts',(-2.37501983264844,0.0902160608552179,
2.84261453760191));
#71523=CARTESIAN_POINT('Ctrl Pts',(-2.37437841508221,0.00145143062880148,
2.84858989190502));
#71524=CARTESIAN_POINT('Origin',(0.,0.,-1.84858989190501));
#71525=CARTESIAN_POINT('',(-2.37409249406917,0.00172857025301859,0.651410108094985));
#71526=CARTESIAN_POINT('',(-2.36806791026422,0.000580996437929415,0.848589891905023));
#71527=CARTESIAN_POINT('',(-2.37175,-2.62313128856983E-13,-1.84858989190501));
#71528=CARTESIAN_POINT('Ctrl Pts',(-2.37409249406917,0.00172857025301858,
0.651410108094986));
#71529=CARTESIAN_POINT('Ctrl Pts',(-2.36885059157359,-0.681255271864669,
0.697375257248508));
#71530=CARTESIAN_POINT('Ctrl Pts',(-1.70202128243095,-2.15553453151225,
0.7959607767724));
#71531=CARTESIAN_POINT('Ctrl Pts',(0.793380919254056,-2.68293732976497,
0.947166666666663));
#71532=CARTESIAN_POINT('Ctrl Pts',(2.67992237177449,-0.803971281251394,
1.10502777777777));
#71533=CARTESIAN_POINT('Ctrl Pts',(2.13917103413275,1.80344728451176,1.26288888888888));
#71534=CARTESIAN_POINT('Ctrl Pts',(-0.339158877291603,2.77725977180218,
1.42075));
#71535=CARTESIAN_POINT('Ctrl Pts',(-2.12031894951391,1.51253569372851,1.5502570730687));
#71536=CARTESIAN_POINT('Ctrl Pts',(-2.36872521807391,0.363433332120877,
1.62714377576703));
#71537=CARTESIAN_POINT('Ctrl Pts',(-2.36805372255214,0.000487775483918769,
1.65141010809499));
#71538=CARTESIAN_POINT('Ctrl Pts',(-2.36806791026422,0.000580996437929554,
0.848589891905023));
#71539=CARTESIAN_POINT('Ctrl Pts',(-2.36714590954407,-0.428850691797627,
0.877301640268363));
#71540=CARTESIAN_POINT('Ctrl Pts',(-2.05072593975983,-1.64725737587436,
0.958678352298389));
#71541=CARTESIAN_POINT('Ctrl Pts',(-0.103189861818606,-2.79677945469355,
1.0927200279951));
#71542=CARTESIAN_POINT('Ctrl Pts',(2.28595558559378,-1.6146683983646,1.25071491899515));
#71543=CARTESIAN_POINT('Ctrl Pts',(2.60139192527736,1.0322363870214,1.4087098099952));
#71544=CARTESIAN_POINT('Ctrl Pts',(0.556949311928898,2.7427217714679,1.56670470099526));
#71545=CARTESIAN_POINT('Ctrl Pts',(-1.80927361374524,2.02108563130788,1.7133313949652));
#71546=CARTESIAN_POINT('Ctrl Pts',(-2.36656032319539,0.612878624174093,
1.80729312526845));
#71547=CARTESIAN_POINT('Ctrl Pts',(-2.37214954248261,-0.00208751672060286,
1.84858989190502));
#71548=CARTESIAN_POINT('Origin',(0.,0.,15.5));
#71549=CARTESIAN_POINT('',(-2.86987326377042,0.00104132824445593,15.1339652973708));
#71550=CARTESIAN_POINT('Ctrl Pts',(-0.439445221994174,2.33068358199188,
15.62825));
#71551=CARTESIAN_POINT('Ctrl Pts',(-0.359491362851287,2.34930954683752,
15.6247606402091));
#71552=CARTESIAN_POINT('Ctrl Pts',(-0.27873128971825,2.36341107797762,15.6212855109979));
#71553=CARTESIAN_POINT('Ctrl Pts',(-0.197490043658781,2.37317361481181,
15.6178198845782));
#71554=CARTESIAN_POINT('Ctrl Pts',(-0.114097433923979,2.38319467509491,
15.6142624842978));
#71555=CARTESIAN_POINT('Ctrl Pts',(-0.0301970746788968,2.38864392614809,
15.610715096763));
#71556=CARTESIAN_POINT('Ctrl Pts',(0.0538748377108959,2.38966967391038,
15.6071726085593));
#71557=CARTESIAN_POINT('Ctrl Pts',(0.0936167287327529,2.39015455827456,
15.6054980281181));
#71558=CARTESIAN_POINT('Ctrl Pts',(0.133397101437596,2.38965022998153,15.6038245424699));
#71559=CARTESIAN_POINT('Ctrl Pts',(0.17318082101162,2.38816842541213,15.6021516114778));
#71560=CARTESIAN_POINT('Ctrl Pts',(0.19744268730314,2.38726475565179,15.601131384398));
#71561=CARTESIAN_POINT('Ctrl Pts',(0.221705799792773,2.38599750448324,15.6001113636003));
#71562=CARTESIAN_POINT('Ctrl Pts',(0.245962166148401,2.38436888753973,15.5990914265778));
#71563=CARTESIAN_POINT('Ctrl Pts',(0.26185491634123,2.38330181913124,15.5984231647255));
#71564=CARTESIAN_POINT('Ctrl Pts',(0.277745619245824,2.38207945021967,15.597754902985));
#71565=CARTESIAN_POINT('Ctrl Pts',(0.293615508622687,2.38070402970992,15.5970873017022));
#71566=CARTESIAN_POINT('Ctrl Pts',(0.379355905904818,2.37327303267301,15.5934804461119));
#71567=CARTESIAN_POINT('Ctrl Pts',(0.46460122999168,2.36137220783444,15.5898881158652));
#71568=CARTESIAN_POINT('Ctrl Pts',(0.548999070996607,2.3451645872232,15.5863050764217));
#71569=CARTESIAN_POINT('Ctrl Pts',(0.634137600151781,2.32881472609505,15.582690591685));
#71570=CARTESIAN_POINT('Ctrl Pts',(0.718414656351904,2.30808199543454,15.5790855615419));
#71571=CARTESIAN_POINT('Ctrl Pts',(0.801467682213623,2.28308069981211,15.5754846124216));
#71572=CARTESIAN_POINT('Ctrl Pts',(0.852459500288906,2.26773072905791,15.573273748452));
#71573=CARTESIAN_POINT('Ctrl Pts',(0.902989840792886,2.2507706713731,15.5710644228464));
#71574=CARTESIAN_POINT('Ctrl Pts',(0.952972256247749,2.23221757070223,15.5688553919549));
#71575=CARTESIAN_POINT('Ctrl Pts',(0.964785636442244,2.22783253188374,15.5683332858993));
#71576=CARTESIAN_POINT('Ctrl Pts',(0.976567164733754,2.22335887755768,15.5678112499871));
#71577=CARTESIAN_POINT('Ctrl Pts',(0.98830665315667,2.21880049805757,15.5672896716409));
#71578=CARTESIAN_POINT('Ctrl Pts',(1.07009362440554,2.18704306198486,15.5636559261431));
#71579=CARTESIAN_POINT('Ctrl Pts',(1.14996182974845,2.15113305037133,15.5600390318413));
#71580=CARTESIAN_POINT('Ctrl Pts',(1.22755227573139,2.11121890826833,15.5564336755567));
#71581=CARTESIAN_POINT('Ctrl Pts',(1.30476387614222,2.07149965222131,15.552845922899));
#71582=CARTESIAN_POINT('Ctrl Pts',(1.37972085381243,2.02781498993708,15.5492695958616));
#71583=CARTESIAN_POINT('Ctrl Pts',(1.45205674723287,1.98026157738062,15.5456994587133));
#71584=CARTESIAN_POINT('Ctrl Pts',(1.51163119176407,1.94109750537355,15.5427591627211));
#71585=CARTESIAN_POINT('Ctrl Pts',(1.56942781249227,1.89930836286272,15.5398230652386));
#71586=CARTESIAN_POINT('Ctrl Pts',(1.62522850219512,1.85492460083693,15.5368882414682));
#71587=CARTESIAN_POINT('Ctrl Pts',(1.65312884704655,1.83273271982404,15.5354208295831));
#71588=CARTESIAN_POINT('Ctrl Pts',(1.68052998038672,1.80989186082895,15.5339537361259));
#71589=CARTESIAN_POINT('Ctrl Pts',(1.70740302888556,1.78640394209333,15.532486595497));
#71590=CARTESIAN_POINT('Ctrl Pts',(1.72592667853778,1.77021366960761,15.5314752923321));
#71591=CARTESIAN_POINT('Ctrl Pts',(1.74419939199006,1.753715928893,15.5304639667541));
#71592=CARTESIAN_POINT('Ctrl Pts',(1.76221135665739,1.73691101229318,15.5294524990243));
#71593=CARTESIAN_POINT('Ctrl Pts',(1.77033011726031,1.72933631972932,15.528996587384));
#71594=CARTESIAN_POINT('Ctrl Pts',(1.77839409985328,1.72170084478485,15.5285407465195));
#71595=CARTESIAN_POINT('Ctrl Pts',(1.78639747681482,1.71400960641012,15.5280852527741));
#71596=CARTESIAN_POINT('Ctrl Pts',(1.84657495109044,1.65617910540199,15.5246603905846));
#71597=CARTESIAN_POINT('Ctrl Pts',(1.90341295390484,1.59512114682347,15.5212504095826));
#71598=CARTESIAN_POINT('Ctrl Pts',(1.95689046613085,1.53122773141625,15.5178508639384));
#71599=CARTESIAN_POINT('Ctrl Pts',(2.01194103421405,1.46545487347031,15.5143513197161));
#71600=CARTESIAN_POINT('Ctrl Pts',(2.06343093897923,1.39667671283205,15.5108628337987));
#71601=CARTESIAN_POINT('Ctrl Pts',(2.11130423046702,1.3252770563036,15.507380556377));
#71602=CARTESIAN_POINT('Ctrl Pts',(2.15745742078722,1.25644281002257,15.5040233981871));
#71603=CARTESIAN_POINT('Ctrl Pts',(2.20024928268006,1.18517117106803,15.500672010362));
#71604=CARTESIAN_POINT('Ctrl Pts',(2.23959635988792,1.11177753196584,15.4973220472993));
#71605=CARTESIAN_POINT('Ctrl Pts',(2.25681070616636,1.07966781485864,15.4958564384594));
#71606=CARTESIAN_POINT('Ctrl Pts',(2.27336525378777,1.04715163497876,15.4943911023279));
#71607=CARTESIAN_POINT('Ctrl Pts',(2.28925084670373,1.0142542353915,15.4929256750031));
#71608=CARTESIAN_POINT('Ctrl Pts',(2.29885484868501,0.994365352899876,15.4920397170785));
#71609=CARTESIAN_POINT('Ctrl Pts',(2.30821431569525,0.974337119524171,15.491153725822));
#71610=CARTESIAN_POINT('Ctrl Pts',(2.3173269757796,0.954175024263046,15.4902676208197));
#71611=CARTESIAN_POINT('Ctrl Pts',(2.32227232757467,0.943233251710468,15.4897867402729));
#71612=CARTESIAN_POINT('Ctrl Pts',(2.32714420559321,0.932253683866113,15.4893058986854));
#71613=CARTESIAN_POINT('Ctrl Pts',(2.33193873109372,0.921245710398884,15.4888254510349));
#71614=CARTESIAN_POINT('Ctrl Pts',(2.36754247444614,0.839501424730483,15.4852576871677));
#71615=CARTESIAN_POINT('Ctrl Pts',(2.39894281260828,0.756064329075142,15.4817059560376));
#71616=CARTESIAN_POINT('Ctrl Pts',(2.42608268559146,0.671340103595013,15.4781652340513));
#71617=CARTESIAN_POINT('Ctrl Pts',(2.453534139292,0.58564319725637,15.4745838626229));
#71618=CARTESIAN_POINT('Ctrl Pts',(2.47662715562456,0.498628540954889,15.4710137545713));
#71619=CARTESIAN_POINT('Ctrl Pts',(2.49525785992387,0.410687466692489,15.4674497112883));
#71620=CARTESIAN_POINT('Ctrl Pts',(2.51258257274376,0.328910963121187,15.4641355034428));
#71621=CARTESIAN_POINT('Ctrl Pts',(2.52604844140045,0.24633247953868,15.4608265399003));
#71622=CARTESIAN_POINT('Ctrl Pts',(2.53553303361489,0.163255416668028,15.4575186404574));
#71623=CARTESIAN_POINT('Ctrl Pts',(2.53942998139287,0.129121426694033,15.4561595191486));
#71624=CARTESIAN_POINT('Ctrl Pts',(2.54265436806282,0.0949032017028567,
15.4548005774761));
#71625=CARTESIAN_POINT('Ctrl Pts',(2.54519570834653,0.0606216731012661,
15.4534415254952));
#71626=CARTESIAN_POINT('Ctrl Pts',(2.54650804671318,0.0429188233335401,
15.4527397162695));
#71627=CARTESIAN_POINT('Ctrl Pts',(2.5476382209856,0.0251990932110098,15.4520378776284));
#71628=CARTESIAN_POINT('Ctrl Pts',(2.54858465973821,0.00746537430393359,
15.4513359696452));
#71629=CARTESIAN_POINT('Ctrl Pts',(2.54936740774304,-0.00720121986763361,
15.4507554597369));
#71630=CARTESIAN_POINT('Ctrl Pts',(2.55002444266908,-0.0218786230829287,
15.4501748534934));
#71631=CARTESIAN_POINT('Ctrl Pts',(2.55055443165925,-0.0365475000712079,
15.4495948274855));
#71632=CARTESIAN_POINT('Ctrl Pts',(2.55387898415761,-0.128563471239416,
15.4459563992365));
#71633=CARTESIAN_POINT('Ctrl Pts',(2.55221836548087,-0.22040066645441,15.4423345418383));
#71634=CARTESIAN_POINT('Ctrl Pts',(2.5454697064449,-0.311650010793409,15.4387239299593));
#71635=CARTESIAN_POINT('Ctrl Pts',(2.53872104740894,-0.402899355132408,
15.4351133180804));
#71636=CARTESIAN_POINT('Ctrl Pts',(2.52688470709894,-0.49356189746232,15.4315139517205));
#71637=CARTESIAN_POINT('Ctrl Pts',(2.50980235603637,-0.583236219097685,
15.4279205055482));
#71638=CARTESIAN_POINT('Ctrl Pts',(2.49326213150481,-0.670064631014266,
15.424441101202));
#71639=CARTESIAN_POINT('Ctrl Pts',(2.47180332144007,-0.755967381987536,
15.420967247239));
#71640=CARTESIAN_POINT('Ctrl Pts',(2.44569482135312,-0.840684658565203,
15.4174941094224));
#71641=CARTESIAN_POINT('Ctrl Pts',(2.43658807165331,-0.870234384917672,
15.4162826650015));
#71642=CARTESIAN_POINT('Ctrl Pts',(2.42691516765274,-0.899639766052948,
15.41507130771));
#71643=CARTESIAN_POINT('Ctrl Pts',(2.41668612527745,-0.928889320342703,
15.4138598323975));
#71644=CARTESIAN_POINT('Ctrl Pts',(2.41079789512425,-0.945726488595391,
15.4131624606198));
#71645=CARTESIAN_POINT('Ctrl Pts',(2.40472537046329,-0.962512016907764,
15.4124650497348));
#71646=CARTESIAN_POINT('Ctrl Pts',(2.39847036187175,-0.979243667871416,
15.4117675606113));
#71647=CARTESIAN_POINT('Ctrl Pts',(2.39421301098727,-0.990631743201221,
15.4112928281));
#71648=CARTESIAN_POINT('Ctrl Pts',(2.38987156242605,-1.0019935463669,15.4108181134517));
#71649=CARTESIAN_POINT('Ctrl Pts',(2.38545028303317,-1.01331939423191,15.4103437824454));
#71650=CARTESIAN_POINT('Ctrl Pts',(2.35279097735238,-1.09698167717045,15.4068399728119));
#71651=CARTESIAN_POINT('Ctrl Pts',(2.31572987674733,-1.17881857921774,15.4033514296728));
#71652=CARTESIAN_POINT('Ctrl Pts',(2.27459874133947,-1.25857844945699,15.3998733992833));
#71653=CARTESIAN_POINT('Ctrl Pts',(2.23281288372258,-1.33960793109688,15.396340005877));
#71654=CARTESIAN_POINT('Ctrl Pts',(2.18682594253521,-1.41849449977561,15.3928174625663));
#71655=CARTESIAN_POINT('Ctrl Pts',(2.13693151879332,-1.49496175096055,15.3893007849646));
#71656=CARTESIAN_POINT('Ctrl Pts',(2.08679723793274,-1.57179660263405,15.385767201663));
#71657=CARTESIAN_POINT('Ctrl Pts',(2.03271725897117,-1.64618961960946,15.3822395406022));
#71658=CARTESIAN_POINT('Ctrl Pts',(1.97494281786374,-1.71783598585985,15.3787127451654));
#71659=CARTESIAN_POINT('Ctrl Pts',(1.95216878512211,-1.74607817495815,15.3773225222016));
#71660=CARTESIAN_POINT('Ctrl Pts',(1.92882022676702,-1.77389324483966,15.3759324337425));
#71661=CARTESIAN_POINT('Ctrl Pts',(1.90491084697345,-1.80126106485015,15.3745421700657));
#71662=CARTESIAN_POINT('Ctrl Pts',(1.89303589564547,-1.8148537022746,15.3738516748025));
#71663=CARTESIAN_POINT('Ctrl Pts',(1.88102258946071,-1.82833599951471,15.3731611363172));
#71664=CARTESIAN_POINT('Ctrl Pts',(1.86887253021617,-1.84170540057035,15.3724705166642));
#71665=CARTESIAN_POINT('Ctrl Pts',(1.86055716973053,-1.85085526453538,15.3719978645349));
#71666=CARTESIAN_POINT('Ctrl Pts',(1.8521789913077,-1.85995082597714,15.3715252464369));
#71667=CARTESIAN_POINT('Ctrl Pts',(1.84374494253208,-1.86898463564396,15.3710530027583));
#71668=CARTESIAN_POINT('Ctrl Pts',(1.77862481272331,-1.93873557897155,15.3674067623267));
#71669=CARTESIAN_POINT('Ctrl Pts',(1.71007452953627,-2.00492197279666,15.3637769310107));
#71670=CARTESIAN_POINT('Ctrl Pts',(1.63841756617314,-2.06724394639147,15.3601581531957));
#71671=CARTESIAN_POINT('Ctrl Pts',(1.56864469297252,-2.1279272764847,15.3566345245939));
#71672=CARTESIAN_POINT('Ctrl Pts',(1.49592552744324,-2.18494739655425,15.3531213758712));
#71673=CARTESIAN_POINT('Ctrl Pts',(1.42051657448793,-2.237996979208,15.3496137628515));
#71674=CARTESIAN_POINT('Ctrl Pts',(1.34626553575621,-2.29023197866037,15.3461600096832));
#71675=CARTESIAN_POINT('Ctrl Pts',(1.26940602418092,-2.33861808827242,15.3427116235202));
#71676=CARTESIAN_POINT('Ctrl Pts',(1.19015227451303,-2.38282228508801,15.3392638844625));
#71677=CARTESIAN_POINT('Ctrl Pts',(1.16438136391748,-2.39719614637352,15.3381427845096));
#71678=CARTESIAN_POINT('Ctrl Pts',(1.1383570943619,-2.4111274748391,15.3370217529787));
#71679=CARTESIAN_POINT('Ctrl Pts',(1.11208629310672,-2.42460372067378,15.3359006275904));
#71680=CARTESIAN_POINT('Ctrl Pts',(1.09252404263768,-2.4346386523776,15.3350657944447));
#71681=CARTESIAN_POINT('Ctrl Pts',(1.07282508844486,-2.44442123549769,15.3342309092564));
#71682=CARTESIAN_POINT('Ctrl Pts',(1.05299217133848,-2.4539460706498,15.3333959050218));
#71683=CARTESIAN_POINT('Ctrl Pts',(1.04038456497523,-2.46000092237074,15.3328651003678));
#71684=CARTESIAN_POINT('Ctrl Pts',(1.02772285622574,-2.46595150778408,15.3323342505181));
#71685=CARTESIAN_POINT('Ctrl Pts',(1.01502087310116,-2.47179063085649,15.3318038822616));
#71686=CARTESIAN_POINT('Ctrl Pts',(0.982652722257195,-2.48667032440912,
15.3304523578927));
#71687=CARTESIAN_POINT('Ctrl Pts',(0.950002091670773,-2.50083650005249,
15.3291030741213));
#71688=CARTESIAN_POINT('Ctrl Pts',(0.917084170499721,-2.5142729570447,15.3277557583224));
#71689=CARTESIAN_POINT('Ctrl Pts',(0.834495683370104,-2.5479839757206,15.3243754484619));
#71690=CARTESIAN_POINT('Ctrl Pts',(0.750226663082229,-2.57710500546031,
15.3210075263739));
#71691=CARTESIAN_POINT('Ctrl Pts',(0.664646844355562,-2.60177034865307,
15.317647686521));
#71692=CARTESIAN_POINT('Ctrl Pts',(0.576787650214132,-2.6270926408521,15.3141983590239));
#71693=CARTESIAN_POINT('Ctrl Pts',(0.487546169865586,-2.64771888106776,
15.3107575500279));
#71694=CARTESIAN_POINT('Ctrl Pts',(0.397298853288816,-2.66374516605354,
15.3073206007236));
#71695=CARTESIAN_POINT('Ctrl Pts',(0.308910977458226,-2.67944124812091,
15.3039544657529));
#71696=CARTESIAN_POINT('Ctrl Pts',(0.219557440695963,-2.69072476824651,
15.3005920330634));
#71697=CARTESIAN_POINT('Ctrl Pts',(0.129581594551193,-2.69764046998944,
15.2972289259214));
#71698=CARTESIAN_POINT('Ctrl Pts',(0.0974227261046785,-2.7001122571645,
15.2960268953233));
#71699=CARTESIAN_POINT('Ctrl Pts',(0.0651843226484069,-2.70202565483482,
15.2948247785662));
#71700=CARTESIAN_POINT('Ctrl Pts',(0.0328820436324132,-2.7033813247538,
15.2936223758136));
#71701=CARTESIAN_POINT('Ctrl Pts',(0.0192199250543532,-2.70395469987624,
15.2931138244208));
#71702=CARTESIAN_POINT('Ctrl Pts',(0.00555605037576419,-2.70442788901379,
15.2926055817652));
#71703=CARTESIAN_POINT('Ctrl Pts',(-0.00810768527292701,-2.70480131817288,
15.2920976575977));
#71704=CARTESIAN_POINT('Ctrl Pts',(-0.102177189495074,-2.70737223265483,
15.2886007973064));
#71705=CARTESIAN_POINT('Ctrl Pts',(-0.196248953232544,-2.705219350857,15.2851186519246));
#71706=CARTESIAN_POINT('Ctrl Pts',(-0.28992790026966,-2.69846111693802,
15.2816464960614));
#71707=CARTESIAN_POINT('Ctrl Pts',(-0.384721183626751,-2.69162249200534,
15.2781330379685));
#71708=CARTESIAN_POINT('Ctrl Pts',(-0.479113197863739,-2.68006831395088,
15.2746298084638));
#71709=CARTESIAN_POINT('Ctrl Pts',(-0.572703609774366,-2.66386867615587,
15.2711319115131));
#71710=CARTESIAN_POINT('Ctrl Pts',(-0.670406973022026,-2.64695712438838,
15.2674802949704));
#71711=CARTESIAN_POINT('Ctrl Pts',(-0.767237930320469,-2.62498318167097,
15.2638344899723));
#71712=CARTESIAN_POINT('Ctrl Pts',(-0.862734200133818,-2.5979664405403,
15.2601889262148));
#71713=CARTESIAN_POINT('Ctrl Pts',(-0.899309423475345,-2.58761898568426,
15.258792669493));
#71714=CARTESIAN_POINT('Ctrl Pts',(-0.935688693950487,-2.57653116703875,
15.2573964481588));
#71715=CARTESIAN_POINT('Ctrl Pts',(-0.971845190453781,-2.56470173355219,
15.2559999492582));
#71716=CARTESIAN_POINT('Ctrl Pts',(-0.985718422450195,-2.56016278506391,
15.2554641132369));
#71717=CARTESIAN_POINT('Ctrl Pts',(-0.999558849945709,-2.55551463851664,
15.2549282363508));
#71718=CARTESIAN_POINT('Ctrl Pts',(-1.01336493152648,-2.55075717270086,
15.254392300921));
#71719=CARTESIAN_POINT('Ctrl Pts',(-1.02713823497804,-2.5460110019675,15.2538576378986));
#71720=CARTESIAN_POINT('Ctrl Pts',(-1.0408680078023,-2.54115923920241,15.2533232792799));
#71721=CARTESIAN_POINT('Ctrl Pts',(-1.05455083068562,-2.53620294641156,
15.2527892870021));
#71722=CARTESIAN_POINT('Ctrl Pts',(-1.14480706402235,-2.50350966941525,
15.2492669048126));
#71723=CARTESIAN_POINT('Ctrl Pts',(-1.23304972084596,-2.46626241239109,
15.2457593395817));
#71724=CARTESIAN_POINT('Ctrl Pts',(-1.3188786706842,-2.42453542284507,15.242261762893));
#71725=CARTESIAN_POINT('Ctrl Pts',(-1.40341018907482,-2.38343919842613,
15.238817057246));
#71726=CARTESIAN_POINT('Ctrl Pts',(-1.48560133565556,-2.33799743942912,
15.2353820404405));
#71727=CARTESIAN_POINT('Ctrl Pts',(-1.56505752288372,-2.28823266258407,
15.2319520997326));
#71728=CARTESIAN_POINT('Ctrl Pts',(-1.59875150777533,-2.26712954025155,
15.2304976079627));
#71729=CARTESIAN_POINT('Ctrl Pts',(-1.63195344745741,-2.24524844976825,
15.2290440290004));
#71730=CARTESIAN_POINT('Ctrl Pts',(-1.66463195977674,-2.22258855435451,
15.2275910110965));
#71731=CARTESIAN_POINT('Ctrl Pts',(-1.74176819837999,-2.16910083489293,
15.2241612241271));
#71732=CARTESIAN_POINT('Ctrl Pts',(-1.81599039866318,-2.11127647963352,
15.2207345632396));
#71733=CARTESIAN_POINT('Ctrl Pts',(-1.88715256813859,-2.04946422501414,
15.2173064022613));
#71734=CARTESIAN_POINT('Ctrl Pts',(-1.90164577925548,-2.03687526008497,
15.2166082074035));
#71735=CARTESIAN_POINT('Ctrl Pts',(-1.91601194648249,-2.02412075255685,
15.215909950323));
#71736=CARTESIAN_POINT('Ctrl Pts',(-1.9302496520377,-2.01120346334021,15.2152115919387));
#71737=CARTESIAN_POINT('Ctrl Pts',(-1.94128816753001,-2.0011886687103,15.2146701535858));
#71738=CARTESIAN_POINT('Ctrl Pts',(-1.95224352654855,-1.99108137253609,
15.2141289446068));
#71739=CARTESIAN_POINT('Ctrl Pts',(-1.96311133771197,-1.98088698275119,
15.2135881466736));
#71740=CARTESIAN_POINT('Ctrl Pts',(-2.03178675603926,-1.91646702066845,
15.2101707589647));
#71741=CARTESIAN_POINT('Ctrl Pts',(-2.09701995613675,-1.8485265277173,15.2067672577273));
#71742=CARTESIAN_POINT('Ctrl Pts',(-2.15871310631003,-1.77747212767664,
15.2033732357386));
#71743=CARTESIAN_POINT('Ctrl Pts',(-2.22164945390415,-1.7049858888237,15.1999108197811));
#71744=CARTESIAN_POINT('Ctrl Pts',(-2.28090217022322,-1.62925832538052,
15.19645826896));
#71745=CARTESIAN_POINT('Ctrl Pts',(-2.33633512040192,-1.55067589533689,
15.1930109042136));
#71746=CARTESIAN_POINT('Ctrl Pts',(-2.39218601791983,-1.47150097801918,
15.1895375474008));
#71747=CARTESIAN_POINT('Ctrl Pts',(-2.44415984798534,-1.38942718616138,
15.1860694551604));
#71748=CARTESIAN_POINT('Ctrl Pts',(-2.49207710040016,-1.30481547317471,
15.1826018417945));
#71749=CARTESIAN_POINT('Ctrl Pts',(-2.52022211747796,-1.25511733759765,
15.1805650798249));
#71750=CARTESIAN_POINT('Ctrl Pts',(-2.54696681998739,-1.20454303320315,
15.1785284830672));
#71751=CARTESIAN_POINT('Ctrl Pts',(-2.57226731600719,-1.15316195438398,
15.1764910817393));
#71752=CARTESIAN_POINT('Ctrl Pts',(-2.57933924906923,-1.13880004030214,
15.1759215922795));
#71753=CARTESIAN_POINT('Ctrl Pts',(-2.58629893239321,-1.12437358425022,
15.1753519825172));
#71754=CARTESIAN_POINT('Ctrl Pts',(-2.59313735551554,-1.10990147500019,
15.1747829112963));
#71755=CARTESIAN_POINT('Ctrl Pts',(-2.63517066423893,-1.02094666405867,
15.1712850367298));
#71756=CARTESIAN_POINT('Ctrl Pts',(-2.6726976453638,-0.930127060905838,
15.167801819036));
#71757=CARTESIAN_POINT('Ctrl Pts',(-2.70558302354023,-0.837840896222647,
15.1643285389057));
#71758=CARTESIAN_POINT('Ctrl Pts',(-2.73847376195491,-0.745539689114618,
15.1608546926391));
#71759=CARTESIAN_POINT('Ctrl Pts',(-2.76672184052432,-0.651770570287676,
15.1573907871758));
#71760=CARTESIAN_POINT('Ctrl Pts',(-2.79014819101862,-0.556903769359717,
15.1539321008988));
#71761=CARTESIAN_POINT('Ctrl Pts',(-2.81305355218475,-0.464146754627161,
15.1505503339286));
#71762=CARTESIAN_POINT('Ctrl Pts',(-2.83134952927604,-0.370339481518358,
15.1471735565822));
#71763=CARTESIAN_POINT('Ctrl Pts',(-2.8448219024633,-0.275813943398833,
15.1437973553073));
#71764=CARTESIAN_POINT('Ctrl Pts',(-2.85447686455589,-0.208072315799913,
15.1413778042102));
#71765=CARTESIAN_POINT('Ctrl Pts',(-2.86165354894421,-0.139961477196466,
15.1389585489751));
#71766=CARTESIAN_POINT('Ctrl Pts',(-2.86625656775569,-0.071602632167948,
15.1365379651471));
#71767=CARTESIAN_POINT('Ctrl Pts',(-2.8678889837078,-0.0473598311579388,
15.1356795285827));
#71768=CARTESIAN_POINT('Ctrl Pts',(-2.86919553394546,-0.0231160969724086,
15.1348219958471));
#71769=CARTESIAN_POINT('Ctrl Pts',(-2.87017396612668,0.00112290304428943,
15.1339652973708));
#71770=CARTESIAN_POINT('',(0.261080338132197,2.92584241055005,15.058));
#71771=CARTESIAN_POINT('Ctrl Pts',(0.260984867623723,2.92515103163649,15.058));
#71772=CARTESIAN_POINT('Ctrl Pts',(0.163110290089364,2.92129299518303,15.0703787026841));
#71773=CARTESIAN_POINT('Ctrl Pts',(0.0656985383021158,2.91278590387498,
15.0828015605825));
#71774=CARTESIAN_POINT('Ctrl Pts',(-0.0308724856851826,2.89964343902045,
15.0952881213498));
#71775=CARTESIAN_POINT('Ctrl Pts',(-0.13093434020212,2.88602590291106,15.1082260438789));
#71776=CARTESIAN_POINT('Ctrl Pts',(-0.230094798512676,2.86743186329655,
15.121232357953));
#71777=CARTESIAN_POINT('Ctrl Pts',(-0.327908726704405,2.84382209488468,
15.1343288085909));
#71778=CARTESIAN_POINT('Ctrl Pts',(-0.401269172848201,2.82611476857578,
15.1441511465694));
#71779=CARTESIAN_POINT('Ctrl Pts',(-0.473871776581697,2.80558493098147,
15.154024186365));
#71780=CARTESIAN_POINT('Ctrl Pts',(-0.54551386023679,2.78219703023119,15.1639571016578));
#71781=CARTESIAN_POINT('Ctrl Pts',(-0.599245422978111,2.76465610466849,
15.1714067881273));
#71782=CARTESIAN_POINT('Ctrl Pts',(-0.652436445713434,2.74550717996222,
15.178890154564));
#71783=CARTESIAN_POINT('Ctrl Pts',(-0.704995275147146,2.7247296345796,15.186411071114));
#71784=CARTESIAN_POINT('Ctrl Pts',(-0.720729468886594,2.71850959642421,
15.1886625588158));
#71785=CARTESIAN_POINT('Ctrl Pts',(-0.736406966678059,2.71214357207348,
15.1909174117022));
#71786=CARTESIAN_POINT('Ctrl Pts',(-0.752025204049111,2.70563092815761,
15.1931757336031));
#71787=CARTESIAN_POINT('Ctrl Pts',(-0.764775912501757,2.70031401422844,
15.1950194246335));
#71788=CARTESIAN_POINT('Ctrl Pts',(-0.777478081511626,2.69490314594757,
15.196864120682));
#71789=CARTESIAN_POINT('Ctrl Pts',(-0.790130440968904,2.6893983882733,15.1987098648068));
#71790=CARTESIAN_POINT('Ctrl Pts',(-0.873485337988913,2.65313254310755,
15.2108697952897));
#71791=CARTESIAN_POINT('Ctrl Pts',(-0.954683148186728,2.61279395749136,
15.2230755503321));
#71792=CARTESIAN_POINT('Ctrl Pts',(-1.0333900295422,2.56835839969231,15.2353460721376));
#71793=CARTESIAN_POINT('Ctrl Pts',(-1.07474974365993,2.54500793864519,15.2417941141031));
#71794=CARTESIAN_POINT('Ctrl Pts',(-1.11542111238663,2.52052546068703,15.2482600407761));
#71795=CARTESIAN_POINT('Ctrl Pts',(-1.15535178122673,2.49490314259947,15.2547466008415));
#71796=CARTESIAN_POINT('Ctrl Pts',(-1.23327915249916,2.44489947493076,15.2674055567063));
#71797=CARTESIAN_POINT('Ctrl Pts',(-1.30838829429154,2.39055588937394,15.2801430971848));
#71798=CARTESIAN_POINT('Ctrl Pts',(-1.38046450469962,2.33219918561456,15.2929796526032));
#71799=CARTESIAN_POINT('Ctrl Pts',(-1.45426350057602,2.27244762382022,15.3061230309111));
#71800=CARTESIAN_POINT('Ctrl Pts',(-1.52488347180723,2.20848778279982,15.3193702140928));
#71801=CARTESIAN_POINT('Ctrl Pts',(-1.59204074405781,2.14065188994946,15.332743132764));
#71802=CARTESIAN_POINT('Ctrl Pts',(-1.60237109058904,2.13021715582588,15.3348001979094));
#71803=CARTESIAN_POINT('Ctrl Pts',(-1.61262065491134,2.1196893711682,15.3368604944486));
#71804=CARTESIAN_POINT('Ctrl Pts',(-1.62278430900332,2.10907388768773,15.3389232952054));
#71805=CARTESIAN_POINT('Ctrl Pts',(-1.68486768809848,2.04423056665054,15.3515236493914));
#71806=CARTESIAN_POINT('Ctrl Pts',(-1.74353795945352,1.97633977637267,15.3641743680265));
#71807=CARTESIAN_POINT('Ctrl Pts',(-1.79863355499942,1.90572574364455,15.3768970731667));
#71808=CARTESIAN_POINT('Ctrl Pts',(-1.8536060338742,1.83526950510231,15.3895913481376));
#71809=CARTESIAN_POINT('Ctrl Pts',(-1.90502010402237,1.76210117952091,15.4023572882508));
#71810=CARTESIAN_POINT('Ctrl Pts',(-1.95266740197694,1.68652354076833,15.4152163709358));
#71811=CARTESIAN_POINT('Ctrl Pts',(-1.999553014057,1.61215408007279,15.4278698893587));
#71812=CARTESIAN_POINT('Ctrl Pts',(-2.04279147033365,1.53545080587127,15.4406135962167));
#71813=CARTESIAN_POINT('Ctrl Pts',(-2.08213462636226,1.45669772176484,15.4534679553077));
#71814=CARTESIAN_POINT('Ctrl Pts',(-2.10370638024081,1.41351760306046,15.4605159681915));
#71815=CARTESIAN_POINT('Ctrl Pts',(-2.12410620181193,1.36972125073741,15.4675972464718));
#71816=CARTESIAN_POINT('Ctrl Pts',(-2.14328646703913,1.32535636167276,15.4747151632939));
#71817=CARTESIAN_POINT('Ctrl Pts',(-2.15012579550102,1.30953666132481,15.4772532810172));
#71818=CARTESIAN_POINT('Ctrl Pts',(-2.15681001155505,1.29364468163272,15.4797960573454));
#71819=CARTESIAN_POINT('Ctrl Pts',(-2.16333680365848,1.27768262506038,15.4823436452153));
#71820=CARTESIAN_POINT('Ctrl Pts',(-2.16791412260327,1.2664882400105,15.4841302996752));
#71821=CARTESIAN_POINT('Ctrl Pts',(-2.17241292255598,1.25526195256421,15.4859189101699));
#71822=CARTESIAN_POINT('Ctrl Pts',(-2.17682958710993,1.24401228867859,15.4877083034276));
#71823=CARTESIAN_POINT('Ctrl Pts',(-2.20791015801245,1.16484712416239,15.5003004673422));
#71824=CARTESIAN_POINT('Ctrl Pts',(-2.2349734122897,1.08441291813616,15.5129492481641));
#71825=CARTESIAN_POINT('Ctrl Pts',(-2.25783961089921,1.00297802743715,15.5256767231474));
#71826=CARTESIAN_POINT('Ctrl Pts',(-2.28035828534265,0.922780797311416,
15.5382107639178));
#71827=CARTESIAN_POINT('Ctrl Pts',(-2.29880657051476,0.841612257746407,
15.5508211250137));
#71828=CARTESIAN_POINT('Ctrl Pts',(-2.31296316132111,0.759731453145844,
15.5635288923091));
#71829=CARTESIAN_POINT('Ctrl Pts',(-2.32670958827523,0.680223009708963,
15.5758684730222));
#71830=CARTESIAN_POINT('Ctrl Pts',(-2.33640931253598,0.600042348520933,
15.5882998973352));
#71831=CARTESIAN_POINT('Ctrl Pts',(-2.34181299591968,0.519439649300842,
15.6008424709262));
#71832=CARTESIAN_POINT('Ctrl Pts',(-2.34572284670801,0.461119332452094,
15.609917686434));
#71833=CARTESIAN_POINT('Ctrl Pts',(-2.34738263953658,0.402578305857885,
15.6190510917899));
#71834=CARTESIAN_POINT('Ctrl Pts',(-2.34668236863854,0.343918483395394,
15.62825));
#71835=CARTESIAN_POINT('',(-2.14373220034752,2.0119373894844,15.058));
#71836=CARTESIAN_POINT('Origin',(0.,0.,15.058));
#71837=CARTESIAN_POINT('Ctrl Pts',(-2.87017396612668,0.00112290304428943,
15.1339652973708));
#71838=CARTESIAN_POINT('Ctrl Pts',(-2.87266912500978,0.0629362380616879,
15.1317805789463));
#71839=CARTESIAN_POINT('Ctrl Pts',(-2.87303098230106,0.124718621761705,
15.1296012856735));
#71840=CARTESIAN_POINT('Ctrl Pts',(-2.87121685856479,0.18637804904607,15.1274262638706));
#71841=CARTESIAN_POINT('Ctrl Pts',(-2.86841400163638,0.281643079490827,
15.1240658123162));
#71842=CARTESIAN_POINT('Ctrl Pts',(-2.86041988710444,0.376614623554742,
15.1207155571276));
#71843=CARTESIAN_POINT('Ctrl Pts',(-2.84750858059062,0.47099184224787,15.1173712434175));
#71844=CARTESIAN_POINT('Ctrl Pts',(-2.83433033308302,0.567320307975548,
15.1139577860911));
#71845=CARTESIAN_POINT('Ctrl Pts',(-2.81602924148459,0.663030385704492,
15.1105505184628));
#71846=CARTESIAN_POINT('Ctrl Pts',(-2.79284156103339,0.757800921120369,
15.1071449162423));
#71847=CARTESIAN_POINT('Ctrl Pts',(-2.77879319434313,0.815218101582043,
15.1050816159094));
#71848=CARTESIAN_POINT('Ctrl Pts',(-2.76295010551778,0.872290339259573,
15.1030189268812));
#71849=CARTESIAN_POINT('Ctrl Pts',(-2.74535586092349,0.928944130664371,
15.100955843023));
#71850=CARTESIAN_POINT('Ctrl Pts',(-2.7354097693855,0.960970728468381,15.099789574088));
#71851=CARTESIAN_POINT('Ctrl Pts',(-2.72490394590206,0.992863566804536,
15.098623178978));
#71852=CARTESIAN_POINT('Ctrl Pts',(-2.7138453785436,1.0246089965303,15.0974564759315));
#71853=CARTESIAN_POINT('Ctrl Pts',(-2.70868377697821,1.03942621963478,15.0969119156755));
#71854=CARTESIAN_POINT('Ctrl Pts',(-2.7034040983514,1.05420445638712,15.0963675402945));
#71855=CARTESIAN_POINT('Ctrl Pts',(-2.69801003661965,1.06893536837389,15.0958235919881));
#71856=CARTESIAN_POINT('Ctrl Pts',(-2.66394262772994,1.16197175299988,15.0923881642358));
#71857=CARTESIAN_POINT('Ctrl Pts',(-2.62528653689294,1.25320878716493,15.0889665364856));
#71858=CARTESIAN_POINT('Ctrl Pts',(-2.58232115247044,1.34232723597939,15.0855542358814));
#71859=CARTESIAN_POINT('Ctrl Pts',(-2.53887733631532,1.43243804397901,15.0821039383428));
#71860=CARTESIAN_POINT('Ctrl Pts',(-2.49102735184572,1.52038366982231,15.0786631768276));
#71861=CARTESIAN_POINT('Ctrl Pts',(-2.43900735397324,1.60582293428401,15.0752273273902));
#71862=CARTESIAN_POINT('Ctrl Pts',(-2.38725398360023,1.69082428143753,15.071809088333));
#71863=CARTESIAN_POINT('Ctrl Pts',(-2.33137274895099,1.77334571203064,15.0683957111292));
#71864=CARTESIAN_POINT('Ctrl Pts',(-2.27155099682431,1.8530278346518,15.064982642569));
#71865=CARTESIAN_POINT('Ctrl Pts',(-2.23076137590659,1.90735930205439,15.0626554326866));
#71866=CARTESIAN_POINT('Ctrl Pts',(-2.18813878650124,1.96037022431859,15.0603283662998));
#71867=CARTESIAN_POINT('Ctrl Pts',(-2.14373220034752,2.0119373894844,15.058));
#71868=CARTESIAN_POINT('',(-2.,-2.44929359829471E-16,16.));
#71869=CARTESIAN_POINT('',(-2.5,-3.06161699786838E-16,15.5));
#71870=CARTESIAN_POINT('Origin',(0.,0.,16.));
#71871=CARTESIAN_POINT('Ctrl Pts',(1.70810875200393,-2.39535560853239,-0.329233991005387));
#71872=CARTESIAN_POINT('Ctrl Pts',(2.5000696979919,-1.83061464970825,-0.276613620635017));
#71873=CARTESIAN_POINT('Ctrl Pts',(3.46698259537958,0.135843711197753,-0.171372879894276));
#71874=CARTESIAN_POINT('Ctrl Pts',(1.78000461065578,2.98198357260362,-0.013511768783165));
#71875=CARTESIAN_POINT('Ctrl Pts',(-1.52068059202578,3.11864337292237,0.144349342327946));
#71876=CARTESIAN_POINT('Ctrl Pts',(-3.44323740053193,0.434868872546417,
0.302210453439058));
#71877=CARTESIAN_POINT('Ctrl Pts',(-2.24748662857037,-2.64500439253867,
0.460071564550167));
#71878=CARTESIAN_POINT('Ctrl Pts',(0.98413688813967,-3.32800743087112,0.61793267566128));
#71879=CARTESIAN_POINT('Ctrl Pts',(3.3242675736315,-0.997273536182889,0.775793786772391));
#71880=CARTESIAN_POINT('Ctrl Pts',(2.65350107828341,2.23705783115145,0.933654897883501));
#71881=CARTESIAN_POINT('Ctrl Pts',(-0.420704297245377,3.44500822120461,
1.09151600899461));
#71882=CARTESIAN_POINT('Ctrl Pts',(-3.11384086799285,1.53272940938773,1.24937712010572));
#71883=CARTESIAN_POINT('Ctrl Pts',(-2.98662452021757,-1.76786447124123,
1.40723823121684));
#71884=CARTESIAN_POINT('Ctrl Pts',(-0.154268773033873,-3.46719137695888,
1.56509934232795));
#71885=CARTESIAN_POINT('Ctrl Pts',(2.81781362814421,-2.02612228753563,1.72296045343906));
#71886=CARTESIAN_POINT('Ctrl Pts',(3.23766264061691,1.25011350527631,1.88082156455017));
#71887=CARTESIAN_POINT('Ctrl Pts',(0.724998218776244,3.39405562633926,2.03868267566128));
#71888=CARTESIAN_POINT('Ctrl Pts',(-2.44433298400306,2.46383378430329,2.19654378677239));
#71889=CARTESIAN_POINT('Ctrl Pts',(-3.39970985401105,-0.698006346200326,
2.35440489788351));
#71890=CARTESIAN_POINT('Ctrl Pts',(-1.27579956793912,-3.22762676650925,
2.51226600899461));
#71891=CARTESIAN_POINT('Ctrl Pts',(2.00366607964198,-2.83382462640088,2.67012712010573));
#71892=CARTESIAN_POINT('Ctrl Pts',(3.46831127903076,0.12671419166248,2.82798823121683));
#71893=CARTESIAN_POINT('Ctrl Pts',(1.79153366111842,2.9724815653929,2.98584934232795));
#71894=CARTESIAN_POINT('Ctrl Pts',(-1.50792549309295,3.12592391504671,3.14371045343906));
#71895=CARTESIAN_POINT('Ctrl Pts',(-3.44158119482194,0.448060782465637,
3.30157156455017));
#71896=CARTESIAN_POINT('Ctrl Pts',(-2.25802486298351,-2.63563337612261,
3.45943267566128));
#71897=CARTESIAN_POINT('Ctrl Pts',(0.970737398643871,-3.33210271331857,
3.61729378677239));
#71898=CARTESIAN_POINT('Ctrl Pts',(3.32025430017048,-1.01052014634333,3.7751548978835));
#71899=CARTESIAN_POINT('Ctrl Pts',(2.66245099976358,2.22634100195603,3.93301600899462));
#71900=CARTESIAN_POINT('Ctrl Pts',(-0.406867188726441,3.44669387613558,
4.09087712010572));
#71901=CARTESIAN_POINT('Ctrl Pts',(-3.10766543711734,1.54520390729755,4.24873823121684));
#71902=CARTESIAN_POINT('Ctrl Pts',(-2.99369583814259,-1.75585443953709,
4.40659934232795));
#71903=CARTESIAN_POINT('Ctrl Pts',(-0.16818635164463,-3.46654769699322,
4.56446045343906));
#71904=CARTESIAN_POINT('Ctrl Pts',(2.80965791624474,-2.03741551431062,4.72232156455017));
#71905=CARTESIAN_POINT('Ctrl Pts',(3.24265463709948,1.23710569022097,4.88018267566128));
#71906=CARTESIAN_POINT('Ctrl Pts',(0.738617048059715,3.39111846455234,5.0380437867724));
#71907=CARTESIAN_POINT('Ctrl Pts',(-2.43442290318405,2.47362582310745,5.1959048978835));
#71908=CARTESIAN_POINT('Ctrl Pts',(-3.40248440570545,-0.684353310232048,
5.35376600899462));
#71909=CARTESIAN_POINT('Ctrl Pts',(-1.28874579170717,-3.22247945977245,
5.51162712010572));
#71910=CARTESIAN_POINT('Ctrl Pts',(1.99227427239527,-2.84184496548404,5.66948823121683));
#71911=CARTESIAN_POINT('Ctrl Pts',(3.46879199270663,0.112790494414327,5.82734934232795));
#71912=CARTESIAN_POINT('Ctrl Pts',(1.803451502182,2.96526596843754,5.98521045343906));
#71913=CARTESIAN_POINT('Ctrl Pts',(-1.49536511544646,3.13195190828366,6.14307156455017));
#71914=CARTESIAN_POINT('Ctrl Pts',(-3.4397548386282,0.461872530499354,6.30093267566129));
#71915=CARTESIAN_POINT('Ctrl Pts',(-2.26858675213732,-2.62654787360198,
6.45879378677239));
#71916=CARTESIAN_POINT('Ctrl Pts',(0.957353695793138,-3.33597264458916,
6.61665489788351));
#71917=CARTESIAN_POINT('Ctrl Pts',(3.31617107144768,-1.02384032406894,6.77451600899461));
#71918=CARTESIAN_POINT('Ctrl Pts',(2.67136662968815,2.21563532967061,6.93237712010573));
#71919=CARTESIAN_POINT('Ctrl Pts',(-0.393028031746144,3.44829937078522,
7.09023823121684));
#71920=CARTESIAN_POINT('Ctrl Pts',(-3.10143756889894,1.55766639256237,7.24809934232795));
#71921=CARTESIAN_POINT('Ctrl Pts',(-3.00072015011765,-1.74382285940228,
7.40596045343905));
#71922=CARTESIAN_POINT('Ctrl Pts',(-0.182100573498421,-3.46584462511342,
7.56382156455018));
#71923=CARTESIAN_POINT('Ctrl Pts',(2.80145659039814,-2.04867775807003,7.72168267566128));
#71924=CARTESIAN_POINT('Ctrl Pts',(3.24759455782818,1.22407890769377,7.8795437867724));
#71925=CARTESIAN_POINT('Ctrl Pts',(0.752223882355328,3.38812615100299,8.03740489788349));
#71926=CARTESIAN_POINT('Ctrl Pts',(-2.42447354494764,2.4833782664236,8.19526600899462));
#71927=CARTESIAN_POINT('Ctrl Pts',(-3.40520415435994,-0.670689385204343,
8.35312712010572));
#71928=CARTESIAN_POINT('Ctrl Pts',(-1.30167123501543,-3.21728015258687,
8.51098823121684));
#71929=CARTESIAN_POINT('Ctrl Pts',(1.98085035420065,-2.84981954842042,8.66884934232795));
#71930=CARTESIAN_POINT('Ctrl Pts',(3.46921681308078,0.098864999537257,8.82671045343906));
#71931=CARTESIAN_POINT('Ctrl Pts',(1.81534028008778,2.95800257805621,8.98457156455017));
#71932=CARTESIAN_POINT('Ctrl Pts',(-1.4827806401293,3.13792943795007,9.14243267566127));
#71933=CARTESIAN_POINT('Ctrl Pts',(-3.4378730539225,0.475676832953572,9.3002937867724));
#71934=CARTESIAN_POINT('Ctrl Pts',(-2.27911208446667,-2.61742004476474,
9.45815489788349));
#71935=CARTESIAN_POINT('Ctrl Pts',(0.943954565772613,-3.3397888199782,9.61601600899462));
#71936=CARTESIAN_POINT('Ctrl Pts',(3.31203440522278,-1.03714400297725,9.77387712010572));
#71937=CARTESIAN_POINT('Ctrl Pts',(2.68023921253269,2.20489395389312,9.93173823121684));
#71938=CARTESIAN_POINT('Ctrl Pts',(-0.379182541400898,3.44984929882113,
10.0895993423279));
#71939=CARTESIAN_POINT('Ctrl Pts',(-3.09515972337558,1.57010377716378,10.2474604534391));
#71940=CARTESIAN_POINT('Ctrl Pts',(-3.00769610777576,-1.73176317886687,
10.4053215645502));
#71941=CARTESIAN_POINT('Ctrl Pts',(-0.196011860918037,-3.46508570377902,
10.5631826756613));
#71942=CARTESIAN_POINT('Ctrl Pts',(2.79321012116224,-2.05990698897259,10.7210437867724));
#71943=CARTESIAN_POINT('Ctrl Pts',(3.25248214612884,1.2110324001305,10.8789048978835));
#71944=CARTESIAN_POINT('Ctrl Pts',(0.765818594962506,3.38507924024569,11.0367660089946));
#71945=CARTESIAN_POINT('Ctrl Pts',(-2.41448511783304,2.49309069223908,11.1946271201057));
#71946=CARTESIAN_POINT('Ctrl Pts',(-3.40786903136843,-0.657014653010787,
11.3524882312168));
#71947=CARTESIAN_POINT('Ctrl Pts',(-1.3145757016765,-3.21202900045202,11.510349342328));
#71948=CARTESIAN_POINT('Ctrl Pts',(1.96939451380669,-2.85774821044889,11.668210453439));
#71949=CARTESIAN_POINT('Ctrl Pts',(3.46958573405997,0.0849379149034097,
11.8260715645502));
#71950=CARTESIAN_POINT('Ctrl Pts',(1.82719979676502,2.95069151525923,11.9839326756613));
#71951=CARTESIAN_POINT('Ctrl Pts',(-1.47017225488226,3.14385641459579,12.1417937867724));
#71952=CARTESIAN_POINT('Ctrl Pts',(-3.43593590116163,0.489473446687968,
12.2996548978835));
#71953=CARTESIAN_POINT('Ctrl Pts',(-2.28960063207268,-2.60824999320481,
12.4575160089946));
#71954=CARTESIAN_POINT('Ctrl Pts',(0.930540112760845,-3.34355126315401,
12.6153771201057));
#71955=CARTESIAN_POINT('Ctrl Pts',(3.30784458181684,-1.05043080491032,12.7732382312169));
#71956=CARTESIAN_POINT('Ctrl Pts',(2.68906819704165,2.19411673426304,12.9310993423279));
#71957=CARTESIAN_POINT('Ctrl Pts',(-0.365330160772045,3.45134423437463,
13.0889604534391));
#71958=CARTESIAN_POINT('Ctrl Pts',(-3.08883349189378,1.58251471600082,13.2468215645502));
#71959=CARTESIAN_POINT('Ctrl Pts',(-3.01462075186278,-1.71967340539697,
13.4046826756613));
#71960=CARTESIAN_POINT('Ctrl Pts',(-0.209925428309919,-3.46427512302224,
13.5625437867724));
#71961=CARTESIAN_POINT('Ctrl Pts',(2.78492903121011,-2.07109504482717,13.7204048978835));
#71962=CARTESIAN_POINT('Ctrl Pts',(3.25729747472216,1.19795113049603,13.8782660089946));
#71963=CARTESIAN_POINT('Ctrl Pts',(0.779438885227093,3.38200690959721,14.0361271201057));
#71964=CARTESIAN_POINT('Ctrl Pts',(-2.40453022224261,2.50270729758603,14.1939882312168));
#71965=CARTESIAN_POINT('Ctrl Pts',(-3.41034060095634,-0.643223025084935,
14.351849342328));
#71966=CARTESIAN_POINT('Ctrl Pts',(-1.3277234162215,-3.20692920286191,14.5097104534391));
#71967=CARTESIAN_POINT('Ctrl Pts',(1.95841253548915,-2.86524258546647,14.6675715645502));
#71968=CARTESIAN_POINT('Ctrl Pts',(3.46892903525912,0.0702659147297645,
14.8254326756613));
#71969=CARTESIAN_POINT('Ctrl Pts',(1.8409162673649,2.94476989555806,14.9832937867724));
#71970=CARTESIAN_POINT('Ctrl Pts',(-1.46144261101867,3.14684084841223,15.1411548978835));
#71971=CARTESIAN_POINT('Ctrl Pts',(-2.76985851330384,1.3890220685151,15.2463956386242));
#71972=CARTESIAN_POINT('Ctrl Pts',(-2.91090525077878,0.426608275808748,
15.2990160089946));
#71973=CARTESIAN_POINT('Ctrl Pts',(1.59774743137963,-2.24059110187414,-0.219489327336926));
#71974=CARTESIAN_POINT('Ctrl Pts',(2.33853958862414,-1.71233819332979,-0.166868956966556));
#71975=CARTESIAN_POINT('Ctrl Pts',(3.24298000926863,0.127066816079881,-0.061628216225815));
#71976=CARTESIAN_POINT('Ctrl Pts',(1.66499808117169,2.78931689094975,0.0962328948852963));
#71977=CARTESIAN_POINT('Ctrl Pts',(-1.42242905026252,2.9171470684346,0.254094005996407));
#71978=CARTESIAN_POINT('Ctrl Pts',(-3.22076899721748,0.406771889250497,
0.411955117107519));
#71979=CARTESIAN_POINT('Ctrl Pts',(-2.10227597256058,-2.4741100174146,0.56981622821863));
#71980=CARTESIAN_POINT('Ctrl Pts',(0.9205515651778,-3.11298406383574,0.72767733932974));
#71981=CARTESIAN_POINT('Ctrl Pts',(3.10948583967916,-0.932839451205724,
0.885538450440853));
#71982=CARTESIAN_POINT('Ctrl Pts',(2.48205773023319,2.09252098227156,1.04339956155196));
#71983=CARTESIAN_POINT('Ctrl Pts',(-0.393522490594119,3.22242540473713,
1.20126067266308));
#71984=CARTESIAN_POINT('Ctrl Pts',(-2.91265485451303,1.43369939061326,1.35912178377418));
#71985=CARTESIAN_POINT('Ctrl Pts',(-2.79365798581306,-1.65364231910831,
1.5169828948853));
#71986=CARTESIAN_POINT('Ctrl Pts',(-0.144301430203291,-3.24317530141947,
1.67484400599641));
#71987=CARTESIAN_POINT('Ctrl Pts',(2.6357540064074,-1.8952140352733,1.83270511710752));
#71988=CARTESIAN_POINT('Ctrl Pts',(3.02847647238534,1.16934336859111,1.99056622821863));
#71989=CARTESIAN_POINT('Ctrl Pts',(0.67815590807408,3.17476486938028,2.14842733932974));
#71990=CARTESIAN_POINT('Ctrl Pts',(-2.28640403724036,2.30464488610489,2.30628845044085));
#71991=CARTESIAN_POINT('Ctrl Pts',(-3.18005377603123,-0.652907986929923,
2.46414956155196));
#71992=CARTESIAN_POINT('Ctrl Pts',(-1.19336984851725,-3.01908901853714,
2.62201067266307));
#71993=CARTESIAN_POINT('Ctrl Pts',(1.87420872841654,-2.65073053018457,2.77987178377419));
#71994=CARTESIAN_POINT('Ctrl Pts',(3.24422284634695,0.118527157015377,2.9377328948853));
#71995=CARTESIAN_POINT('Ctrl Pts',(1.67578223688854,2.78042881072881,3.09559400599641));
#71996=CARTESIAN_POINT('Ctrl Pts',(-1.41049806136441,2.92395721296701,3.25345511710752));
#71997=CARTESIAN_POINT('Ctrl Pts',(-3.21921979935999,0.419111466671254,
3.41131622821863));
#71998=CARTESIAN_POINT('Ctrl Pts',(-2.11213332909314,-2.46534446464132,
3.56917733932974));
#71999=CARTESIAN_POINT('Ctrl Pts',(0.908017819947236,-3.11681474909129,
3.72703845044085));
#72000=CARTESIAN_POINT('Ctrl Pts',(3.10573186478955,-0.94523019467185,3.88489956155197));
#72001=CARTESIAN_POINT('Ctrl Pts',(2.49042939511648,2.08249657000891,4.04276067266307));
#72002=CARTESIAN_POINT('Ctrl Pts',(-0.380579401011611,3.2240021490943,4.20062178377419));
#72003=CARTESIAN_POINT('Ctrl Pts',(-2.90687841972373,1.44536790818848,4.3584828948853));
#72004=CARTESIAN_POINT('Ctrl Pts',(-2.8002724241724,-1.64240825846459,4.5163440059964));
#72005=CARTESIAN_POINT('Ctrl Pts',(-0.157319790685473,-3.24257320977247,
4.67420511710753));
#72006=CARTESIAN_POINT('Ctrl Pts',(2.62812523703122,-1.90577760392813,4.83206622821863));
#72007=CARTESIAN_POINT('Ctrl Pts',(3.03314593476479,1.15717599162043,4.98992733932975));
#72008=CARTESIAN_POINT('Ctrl Pts',(0.690894821495446,3.17201747832858,5.14778845044085));
#72009=CARTESIAN_POINT('Ctrl Pts',(-2.27713424914591,2.31380425890769,5.30564956155197));
#72010=CARTESIAN_POINT('Ctrl Pts',(-3.18264906326793,-0.640137076925948,
5.46351067266308));
#72011=CARTESIAN_POINT('Ctrl Pts',(-1.20547961362863,-3.01427428053665,
5.62137178377419));
#72012=CARTESIAN_POINT('Ctrl Pts',(1.86355294859817,-2.65823267321491,5.7792328948853));
#72013=CARTESIAN_POINT('Ctrl Pts',(3.24467250099567,0.105503073222438,5.93709400599641));
#72014=CARTESIAN_POINT('Ctrl Pts',(1.68693006335134,2.77367941524228,6.09495511710752));
#72015=CARTESIAN_POINT('Ctrl Pts',(-1.39874921276312,2.92959573609933,6.25281622821863));
#72016=CARTESIAN_POINT('Ctrl Pts',(-3.21751144448276,0.432030834315646,
6.41067733932974));
#72017=CARTESIAN_POINT('Ctrl Pts',(-2.12201281202782,-2.45684597864148,
6.56853845044085));
#72018=CARTESIAN_POINT('Ctrl Pts',(0.895498841382776,-3.12043464316416,
6.72639956155197));
#72019=CARTESIAN_POINT('Ctrl Pts',(3.10191245446456,-0.957689752484927,
6.88426067266308));
#72020=CARTESIAN_POINT('Ctrl Pts',(2.4987689840299,2.07248259380561,7.04212178377418));
#72021=CARTESIAN_POINT('Ctrl Pts',(-0.367634395319329,3.22550391234535,
7.1999828948853));
#72022=CARTESIAN_POINT('Ctrl Pts',(-2.90105293558095,1.45702518925863,7.3578440059964));
#72023=CARTESIAN_POINT('Ctrl Pts',(-2.8068428936476,-1.63115404163953,7.51570511710752));
#72024=CARTESIAN_POINT('Ctrl Pts',(-0.170335011291572,-3.24191556353729,
7.67356622821863));
#72025=CARTESIAN_POINT('Ctrl Pts',(2.62045380083611,-1.91631219138755,7.83142733932975));
#72026=CARTESIAN_POINT('Ctrl Pts',(3.03776668601744,1.14499087267086,7.98928845044085));
#72027=CARTESIAN_POINT('Ctrl Pts',(0.703622514928034,3.16921849888318,8.14714956155197));
#72028=CARTESIAN_POINT('Ctrl Pts',(-2.26782772135753,2.32292659449655,8.30501067266308));
#72029=CARTESIAN_POINT('Ctrl Pts',(-3.18519308830241,-0.627355981407313,
8.46287178377418));
#72030=CARTESIAN_POINT('Ctrl Pts',(-1.21756994091078,-3.00941090184898,
8.62073289488531));
#72031=CARTESIAN_POINT('Ctrl Pts',(1.852867132528,-2.6656920164142,8.77859400599641));
#72032=CARTESIAN_POINT('Ctrl Pts',(3.24506987362244,0.0924773079458306,
8.93645511710752));
#72033=CARTESIAN_POINT('Ctrl Pts',(1.698050704434,2.7668853142746,9.09431622821864));
#72034=CARTESIAN_POINT('Ctrl Pts',(-1.3869778234475,2.93518705612466,9.25217733932973));
#72035=CARTESIAN_POINT('Ctrl Pts',(-3.21575124234316,0.444943237441223,
9.41003845044086));
#72036=CARTESIAN_POINT('Ctrl Pts',(-2.13185810008334,-2.44830790103859,
9.56789956155196));
#72037=CARTESIAN_POINT('Ctrl Pts',(0.882965432401702,-3.12400425453603,
9.72576067266308));
#72038=CARTESIAN_POINT('Ctrl Pts',(3.09804305924746,-0.970133877473286,
9.88362178377418));
#72039=CARTESIAN_POINT('Ctrl Pts',(2.50706830714555,2.06243522092151,10.0414828948853));
#72040=CARTESIAN_POINT('Ctrl Pts',(-0.354683465462343,3.22695369915506,
10.1993440059964));
#72041=CARTESIAN_POINT('Ctrl Pts',(-2.89518070317902,1.4686589914253,10.3572051171075));
#72042=CARTESIAN_POINT('Ctrl Pts',(-2.81336813298999,-1.61987353998757,
10.5150662282186));
#72043=CARTESIAN_POINT('Ctrl Pts',(-0.183347487058001,-3.24120567629433,
10.6729273393297));
#72044=CARTESIAN_POINT('Ctrl Pts',(2.61274013797703,-1.9268158989588,10.8307884504409));
#72045=CARTESIAN_POINT('Ctrl Pts',(3.04233848605292,1.13278730312457,10.988649561552));
#72046=CARTESIAN_POINT('Ctrl Pts',(0.716338869857416,3.16636844976869,11.1465106726631));
#72047=CARTESIAN_POINT('Ctrl Pts',(-2.25848464894066,2.33201149812516,11.3043717837742));
#72048=CARTESIAN_POINT('Ctrl Pts',(-3.18768578696123,-0.61456477697643,
11.4622328948853));
#72049=CARTESIAN_POINT('Ctrl Pts',(-1.22964064685199,-3.00449902792679,
11.6200940059964));
#72050=CARTESIAN_POINT('Ctrl Pts',(1.84215145675955,-2.67310840566659,11.7779551171075));
#72051=CARTESIAN_POINT('Ctrl Pts',(3.24541495852771,0.0794500556270124,
11.9358162282186));
#72052=CARTESIAN_POINT('Ctrl Pts',(1.70914397486321,2.76004662101762,12.0936773393297));
#72053=CARTESIAN_POINT('Ctrl Pts',(-1.37518406902836,2.94073108937221,12.2515384504409));
#72054=CARTESIAN_POINT('Ctrl Pts',(-3.21393924949186,0.457848448617044,
12.409399561552));
#72055=CARTESIAN_POINT('Ctrl Pts',(-2.14166898008542,-2.43973032873338,
12.5672606726631));
#72056=CARTESIAN_POINT('Ctrl Pts',(0.870417690451563,-3.12752360534598,
12.7251217837742));
#72057=CARTESIAN_POINT('Ctrl Pts',(3.09412394134766,-0.98256221591188,12.8829828948853));
#72058=CARTESIAN_POINT('Ctrl Pts',(2.51532684882466,2.05235432006483,13.0408440059964));
#72059=CARTESIAN_POINT('Ctrl Pts',(-0.341726090504644,3.22835204655998,
13.1987051171075));
#72060=CARTESIAN_POINT('Ctrl Pts',(-2.88926321104715,1.48026805649486,13.3565662282186));
#72061=CARTESIAN_POINT('Ctrl Pts',(-2.81984537414356,-1.60856488971291,
13.5144273393297));
#72062=CARTESIAN_POINT('Ctrl Pts',(-0.196362095487134,-3.24044746735677,
13.6722884504409));
#72063=CARTESIAN_POINT('Ctrl Pts',(2.60499409125458,-1.93728109181189,13.830149561552));
#72064=CARTESIAN_POINT('Ctrl Pts',(3.04684269509828,1.12055121749295,13.9880106726631));
#72065=CARTESIAN_POINT('Ctrl Pts',(0.729079149865556,3.16349462314833,14.1458717837742));
#72066=CARTESIAN_POINT('Ctrl Pts',(-2.24917294156805,2.34100677226896,14.3037328948853));
#72067=CARTESIAN_POINT('Ctrl Pts',(-3.1899976678388,-0.601664229474863,
14.4615940059964));
#72068=CARTESIAN_POINT('Ctrl Pts',(-1.24193888437236,-2.9997287294955,14.6194551171075));
#72069=CARTESIAN_POINT('Ctrl Pts',(1.83187902672385,-2.68011856729716,14.7773162282186));
#72070=CARTESIAN_POINT('Ctrl Pts',(3.24480068919561,0.0657260169420378,
14.9351773393297));
#72071=CARTESIAN_POINT('Ctrl Pts',(1.72197422097186,2.75450759860113,15.0930384504409));
#72072=CARTESIAN_POINT('Ctrl Pts',(-1.36701844957144,2.94352269819615,15.250899561552));
#72073=CARTESIAN_POINT('Ctrl Pts',(-2.59089728316432,1.29927701587847,15.3561403022927));
#72074=CARTESIAN_POINT('Ctrl Pts',(-2.72283095673204,0.399045011670964,
15.4087606726631));
#72075=CARTESIAN_POINT('Ctrl Pts',(1.48738611075532,-2.0858265952159,-0.109744663668465));
#72076=CARTESIAN_POINT('Ctrl Pts',(2.17700947925639,-1.59406173695134,-0.0571242932980945));
#72077=CARTESIAN_POINT('Ctrl Pts',(3.01897742315769,0.118289920962009,0.0481164474426461));
#72078=CARTESIAN_POINT('Ctrl Pts',(1.5499915516876,2.59665020929587,0.205977558553758));
#72079=CARTESIAN_POINT('Ctrl Pts',(-1.32417750849926,2.71565076394683,0.363838669664868));
#72080=CARTESIAN_POINT('Ctrl Pts',(-2.99830059390304,0.37867490595458,0.521699780775981));
#72081=CARTESIAN_POINT('Ctrl Pts',(-1.95706531655079,-2.30321564229053,
0.679560891887089));
#72082=CARTESIAN_POINT('Ctrl Pts',(0.856966242215927,-2.89796069680035,
0.837422002998203));
#72083=CARTESIAN_POINT('Ctrl Pts',(2.89470410572683,-0.86840536622856,0.995283114109312));
#72084=CARTESIAN_POINT('Ctrl Pts',(2.31061438218297,1.94798413339166,1.15314422522042));
#72085=CARTESIAN_POINT('Ctrl Pts',(-0.36634068394286,2.99984258826965,1.31100533633153));
#72086=CARTESIAN_POINT('Ctrl Pts',(-2.71146884103322,1.33466937183879,1.46886644744265));
#72087=CARTESIAN_POINT('Ctrl Pts',(-2.60069145140856,-1.53942016697539,
1.62672755855376));
#72088=CARTESIAN_POINT('Ctrl Pts',(-0.134334087372704,-3.01915922588007,
1.78458866966487));
#72089=CARTESIAN_POINT('Ctrl Pts',(2.45369438467058,-1.76430578301097,1.94244978077598));
#72090=CARTESIAN_POINT('Ctrl Pts',(2.81929030415377,1.0885732319059,2.10031089188709));
#72091=CARTESIAN_POINT('Ctrl Pts',(0.63131359737191,2.95547411242131,2.2581720029982));
#72092=CARTESIAN_POINT('Ctrl Pts',(-2.12847509047765,2.14545598790649,2.41603311410931));
#72093=CARTESIAN_POINT('Ctrl Pts',(-2.96039769805142,-0.607809627659522,
2.57389422522043));
#72094=CARTESIAN_POINT('Ctrl Pts',(-1.11094012909538,-2.81055127056503,
2.73175533633153));
#72095=CARTESIAN_POINT('Ctrl Pts',(1.74475137719111,-2.46763643396825,2.88961644744264));
#72096=CARTESIAN_POINT('Ctrl Pts',(3.02013441366314,0.110340122368272,3.04747755855376));
#72097=CARTESIAN_POINT('Ctrl Pts',(1.56003081265866,2.58837605606472,3.20533866966487));
#72098=CARTESIAN_POINT('Ctrl Pts',(-1.31307062963587,2.72199051088731,3.36319978077598));
#72099=CARTESIAN_POINT('Ctrl Pts',(-2.99685840389804,0.390162150876873,
3.52106089188709));
#72100=CARTESIAN_POINT('Ctrl Pts',(-1.96624179520275,-2.29505555316004,
3.6789220029982));
#72101=CARTESIAN_POINT('Ctrl Pts',(0.845298241250599,-2.90152678486402,
3.83678311410932));
#72102=CARTESIAN_POINT('Ctrl Pts',(2.89120942940861,-0.879940243000373,
3.99464422522043));
#72103=CARTESIAN_POINT('Ctrl Pts',(2.31840779046938,1.93865213806179,4.15250533633154));
#72104=CARTESIAN_POINT('Ctrl Pts',(-0.354291613296782,3.00131042205302,
4.31036644744265));
#72105=CARTESIAN_POINT('Ctrl Pts',(-2.70609140233011,1.34553190907942,4.46822755855376));
#72106=CARTESIAN_POINT('Ctrl Pts',(-2.60684901020221,-1.52896207739209,
4.62608866966487));
#72107=CARTESIAN_POINT('Ctrl Pts',(-0.146453229726317,-3.01859872255171,
4.78394978077598));
#72108=CARTESIAN_POINT('Ctrl Pts',(2.44659255781772,-1.77413969354566,4.94181089188709));
#72109=CARTESIAN_POINT('Ctrl Pts',(2.82363723243009,1.07724629301989,5.09967200299821));
#72110=CARTESIAN_POINT('Ctrl Pts',(0.643172594931182,2.95291649210482,5.25753311410931));
#72111=CARTESIAN_POINT('Ctrl Pts',(-2.11984559510778,2.15398269470792,5.41539422522043));
#72112=CARTESIAN_POINT('Ctrl Pts',(-2.96281372083041,-0.595920843619846,
5.57325533633153));
#72113=CARTESIAN_POINT('Ctrl Pts',(-1.12221343555009,-2.80606910130085,
5.73111644744265));
#72114=CARTESIAN_POINT('Ctrl Pts',(1.73483162480106,-2.47462038094578,5.88897755855376));
#72115=CARTESIAN_POINT('Ctrl Pts',(3.02055300928471,0.0982156520305535,
6.04683866966487));
#72116=CARTESIAN_POINT('Ctrl Pts',(1.57040862452068,2.58209286204701,6.20469978077598));
#72117=CARTESIAN_POINT('Ctrl Pts',(-1.30213331007977,2.72723956391501,6.36256089188709));
#72118=CARTESIAN_POINT('Ctrl Pts',(-2.99526805033731,0.402189138131933,
6.52042200299821));
#72119=CARTESIAN_POINT('Ctrl Pts',(-1.97543887191833,-2.28714408368097,
6.67828311410931));
#72120=CARTESIAN_POINT('Ctrl Pts',(0.833643986972413,-2.90489664173917,
6.83614422522043));
#72121=CARTESIAN_POINT('Ctrl Pts',(2.88765383748144,-0.891539180900916,
6.99400533633154));
#72122=CARTESIAN_POINT('Ctrl Pts',(2.32617133837164,1.9293298579406,7.15186644744265));
#72123=CARTESIAN_POINT('Ctrl Pts',(-0.342240758892514,3.00270845390548,
7.30972755855377));
#72124=CARTESIAN_POINT('Ctrl Pts',(-2.70066830226297,1.35638398595488,7.46758866966487));
#72125=CARTESIAN_POINT('Ctrl Pts',(-2.61296563717754,-1.51848522387679,
7.62544978077598));
#72126=CARTESIAN_POINT('Ctrl Pts',(-0.158569449084724,-3.01798650196116,
7.78331089188708));
#72127=CARTESIAN_POINT('Ctrl Pts',(2.43945101127409,-1.78394662470507,7.94117200299821));
#72128=CARTESIAN_POINT('Ctrl Pts',(2.8279388142067,1.06590283764795,8.09903311410931));
#72129=CARTESIAN_POINT('Ctrl Pts',(0.655021147500741,2.95031084676337,8.25689422522044));
#72130=CARTESIAN_POINT('Ctrl Pts',(-2.11118189776743,2.16247492256949,8.41475533633153));
#72131=CARTESIAN_POINT('Ctrl Pts',(-2.96518202224487,-0.584022577610279,
8.57261644744266));
#72132=CARTESIAN_POINT('Ctrl Pts',(-1.13346864680612,-2.8015416511111,8.73047755855375));
#72133=CARTESIAN_POINT('Ctrl Pts',(1.72488391085535,-2.48156448440799,8.88833866966489));
#72134=CARTESIAN_POINT('Ctrl Pts',(3.0209229341641,0.0860896163543999,9.04619978077597));
#72135=CARTESIAN_POINT('Ctrl Pts',(1.58076112878023,2.575768050493,9.2040608918871));
#72136=CARTESIAN_POINT('Ctrl Pts',(-1.2911750067657,2.73244467429924,9.3619220029982));
#72137=CARTESIAN_POINT('Ctrl Pts',(-2.99362943076381,0.414209641928883,
9.51978311410932));
#72138=CARTESIAN_POINT('Ctrl Pts',(-1.98460411570002,-2.27919575731244,
9.67764422522042));
#72139=CARTESIAN_POINT('Ctrl Pts',(0.821976299030791,-2.90821968909385,
9.83550533633154));
#72140=CARTESIAN_POINT('Ctrl Pts',(2.88405171327213,-0.903123751969326,
9.99336644744264));
#72141=CARTESIAN_POINT('Ctrl Pts',(2.33389740175841,1.9199764879499,10.1512275585538));
#72142=CARTESIAN_POINT('Ctrl Pts',(-0.330184389523787,3.00405809948898,
10.3090886696649));
#72143=CARTESIAN_POINT('Ctrl Pts',(-2.69520168298246,1.36721420568682,10.466949780776));
#72144=CARTESIAN_POINT('Ctrl Pts',(-2.61904015820422,-1.50798390110827,
10.6248108918871));
#72145=CARTESIAN_POINT('Ctrl Pts',(-0.170683113197963,-3.01732564880962,
10.7826720029982));
#72146=CARTESIAN_POINT('Ctrl Pts',(2.43227015479182,-1.793724808945,10.9405331141093));
#72147=CARTESIAN_POINT('Ctrl Pts',(2.83219482597701,1.05454220611865,11.0983942252204));
#72148=CARTESIAN_POINT('Ctrl Pts',(0.666859144752323,2.94765765929168,11.2562553363315));
#72149=CARTESIAN_POINT('Ctrl Pts',(-2.10248418004828,2.17093230401124,11.4141164474427));
#72150=CARTESIAN_POINT('Ctrl Pts',(-2.96750254255404,-0.572114900942073,
11.5719775585538));
#72151=CARTESIAN_POINT('Ctrl Pts',(-1.14470559202747,-2.79696905540156,
11.7298386696649));
#72152=CARTESIAN_POINT('Ctrl Pts',(1.7149083997124,-2.48846860088429,11.887699780776));
#72153=CARTESIAN_POINT('Ctrl Pts',(3.02124418299545,0.0739621963506113,
12.0455608918871));
#72154=CARTESIAN_POINT('Ctrl Pts',(1.5910881529614,2.56940172677601,12.2034220029982));
#72155=CARTESIAN_POINT('Ctrl Pts',(-1.28019588317448,2.73760576414863,12.3612831141093));
#72156=CARTESIAN_POINT('Ctrl Pts',(-2.99194259782208,0.42622345054612,12.5191442252204));
#72157=CARTESIAN_POINT('Ctrl Pts',(-1.99373732809816,-2.27121066426194,
12.6770053363315));
#72158=CARTESIAN_POINT('Ctrl Pts',(0.810295268142284,-2.91149594753796,
12.8348664474426));
#72159=CARTESIAN_POINT('Ctrl Pts',(2.88040330087848,-0.914693626913434,
12.9927275585538));
#72160=CARTESIAN_POINT('Ctrl Pts',(2.34158550060768,1.91059190586663,13.1505886696649));
#72161=CARTESIAN_POINT('Ctrl Pts',(-0.318122020237242,3.00535985874532,
13.308449780776));
#72162=CARTESIAN_POINT('Ctrl Pts',(-2.68969293020052,1.37802139698889,13.4663108918871));
#72163=CARTESIAN_POINT('Ctrl Pts',(-2.62506999642434,-1.49745637402886,
13.6241720029982));
#72164=CARTESIAN_POINT('Ctrl Pts',(-0.182798762664348,-3.0166198116913,
13.7820331141093));
#72165=CARTESIAN_POINT('Ctrl Pts',(2.42505915129906,-1.80346713879661,13.9398942252204));
#72166=CARTESIAN_POINT('Ctrl Pts',(2.8363879154744,1.04315130448987,14.0977553363316));
#72167=CARTESIAN_POINT('Ctrl Pts',(0.678719414504022,2.94498233669946,14.2556164474426));
#72168=CARTESIAN_POINT('Ctrl Pts',(-2.09381566089348,2.17930624695187,14.4134775585538));
#72169=CARTESIAN_POINT('Ctrl Pts',(-2.96965473472126,-0.560105433864789,
14.5713386696649));
#72170=CARTESIAN_POINT('Ctrl Pts',(-1.15615435252323,-2.79252825612909,
14.729199780776));
#72171=CARTESIAN_POINT('Ctrl Pts',(1.70534551795855,-2.49499454912784,14.8870608918871));
#72172=CARTESIAN_POINT('Ctrl Pts',(3.0206723431321,0.0611861191543108,15.0449220029982));
#72173=CARTESIAN_POINT('Ctrl Pts',(1.60303217457882,2.56424530164419,15.2027831141093));
#72174=CARTESIAN_POINT('Ctrl Pts',(-1.27259428812422,2.74020454798006,15.3606442252204));
#72175=CARTESIAN_POINT('Ctrl Pts',(-2.41193605302479,1.20953196324185,15.4658849659612));
#72176=CARTESIAN_POINT('Ctrl Pts',(-2.53475666268529,0.371481747533179,
15.5185053363315));
#72177=CARTESIAN_POINT('Ctrl Pts',(1.37702479013102,-1.93106208855765,-3.60822483003176E-15));
#72178=CARTESIAN_POINT('Ctrl Pts',(2.01547936988864,-1.47578528057288,0.0526203703703667));
#72179=CARTESIAN_POINT('Ctrl Pts',(2.79497483704674,0.109513025844136,0.157861111111108));
#72180=CARTESIAN_POINT('Ctrl Pts',(1.4349850222035,2.40398352764199,0.315722222222219));
#72181=CARTESIAN_POINT('Ctrl Pts',(-1.225925966736,2.51415445945906,0.473583333333329));
#72182=CARTESIAN_POINT('Ctrl Pts',(-2.77583219058859,0.350577922658662,
0.631444444444441));
#72183=CARTESIAN_POINT('Ctrl Pts',(-1.811854660541,-2.13232126716645,0.789305555555552));
#72184=CARTESIAN_POINT('Ctrl Pts',(0.793380919254056,-2.68293732976497,
0.947166666666663));
#72185=CARTESIAN_POINT('Ctrl Pts',(2.67992237177449,-0.803971281251394,
1.10502777777777));
#72186=CARTESIAN_POINT('Ctrl Pts',(2.13917103413275,1.80344728451176,1.26288888888888));
#72187=CARTESIAN_POINT('Ctrl Pts',(-0.339158877291603,2.77725977180218,
1.42075));
#72188=CARTESIAN_POINT('Ctrl Pts',(-2.51028282755341,1.23563935306431,1.57861111111111));
#72189=CARTESIAN_POINT('Ctrl Pts',(-2.40772491700405,-1.42519801484247,
1.73647222222222));
#72190=CARTESIAN_POINT('Ctrl Pts',(-0.124366744542119,-2.79514315034066,
1.89433333333333));
#72191=CARTESIAN_POINT('Ctrl Pts',(2.27163476293377,-1.63339753074864,2.05219444444444));
#72192=CARTESIAN_POINT('Ctrl Pts',(2.61010413592219,1.00780309522069,2.21005555555555));
#72193=CARTESIAN_POINT('Ctrl Pts',(0.584471286669745,2.73618335546233,2.36791666666667));
#72194=CARTESIAN_POINT('Ctrl Pts',(-1.97054614371495,1.98626708970809,2.52577777777777));
#72195=CARTESIAN_POINT('Ctrl Pts',(-2.7407416200716,-0.562711268389121,
2.68363888888889));
#72196=CARTESIAN_POINT('Ctrl Pts',(-1.02851040967351,-2.60201352259292,
2.84149999999999));
#72197=CARTESIAN_POINT('Ctrl Pts',(1.61529402596567,-2.28454233775194,2.99936111111111));
#72198=CARTESIAN_POINT('Ctrl Pts',(2.79604598097933,0.102153087721166,3.15722222222222));
#72199=CARTESIAN_POINT('Ctrl Pts',(1.44427938842878,2.39632330140064,3.31508333333333));
#72200=CARTESIAN_POINT('Ctrl Pts',(-1.21564319790733,2.5200238088076,3.47294444444445));
#72201=CARTESIAN_POINT('Ctrl Pts',(-2.77449700843608,0.361212835082494,
3.63080555555555));
#72202=CARTESIAN_POINT('Ctrl Pts',(-1.82035026131238,-2.12476664167876,
3.78866666666667));
#72203=CARTESIAN_POINT('Ctrl Pts',(0.782578662553965,-2.68623882063674,
3.94652777777777));
#72204=CARTESIAN_POINT('Ctrl Pts',(2.67668699402767,-0.814650291328897,
4.10438888888889));
#72205=CARTESIAN_POINT('Ctrl Pts',(2.14638618582228,1.79480770611467,4.26225));
#72206=CARTESIAN_POINT('Ctrl Pts',(-0.328003825581952,2.77861869501174,
4.42011111111111));
#72207=CARTESIAN_POINT('Ctrl Pts',(-2.50530438493649,1.24569590997036,4.57797222222222));
#72208=CARTESIAN_POINT('Ctrl Pts',(-2.41342559623202,-1.41551589631959,
4.73583333333333));
#72209=CARTESIAN_POINT('Ctrl Pts',(-0.135586668767159,-2.79462423533096,
4.89369444444444));
#72210=CARTESIAN_POINT('Ctrl Pts',(2.2650598786042,-1.64250178316317,5.05155555555556));
#72211=CARTESIAN_POINT('Ctrl Pts',(2.61412853009539,0.997316594419356,5.20941666666666));
#72212=CARTESIAN_POINT('Ctrl Pts',(0.595450368366912,2.73381550588105,5.36727777777778));
#72213=CARTESIAN_POINT('Ctrl Pts',(-1.96255694106964,1.99416113050815,5.52513888888888));
#72214=CARTESIAN_POINT('Ctrl Pts',(-2.74297837839289,-0.551704610313744,
5.683));
#72215=CARTESIAN_POINT('Ctrl Pts',(-1.03894725747156,-2.59786392206505,
5.84086111111111));
#72216=CARTESIAN_POINT('Ctrl Pts',(1.60611030100396,-2.29100808867664,5.99872222222222));
#72217=CARTESIAN_POINT('Ctrl Pts',(2.79643351757374,0.090928230838667,6.15658333333333));
#72218=CARTESIAN_POINT('Ctrl Pts',(1.45388718569001,2.39050630885174,6.31444444444444));
#72219=CARTESIAN_POINT('Ctrl Pts',(-1.20551740739643,2.52488339173069,6.47230555555556));
#72220=CARTESIAN_POINT('Ctrl Pts',(-2.77302465619186,0.372347441948222,
6.63016666666666));
#72221=CARTESIAN_POINT('Ctrl Pts',(-1.82886493180883,-2.11744218872047,
6.78802777777778));
#72222=CARTESIAN_POINT('Ctrl Pts',(0.771789132562049,-2.68935864031417,
6.94588888888888));
#72223=CARTESIAN_POINT('Ctrl Pts',(2.67339522049833,-0.825388609316905,
7.10375));
#72224=CARTESIAN_POINT('Ctrl Pts',(2.15357369271338,1.7861771220756,7.26161111111111));
#72225=CARTESIAN_POINT('Ctrl Pts',(-0.3168471224657,2.77991299546561,7.41947222222222));
#72226=CARTESIAN_POINT('Ctrl Pts',(-2.50028366894498,1.25574278265114,7.57733333333334));
#72227=CARTESIAN_POINT('Ctrl Pts',(-2.41908838070749,-1.40581640611404,
7.73519444444443));
#72228=CARTESIAN_POINT('Ctrl Pts',(-0.146803886877873,-2.79405744038503,
7.89305555555557));
#72229=CARTESIAN_POINT('Ctrl Pts',(2.25844822171206,-1.65158105802259,8.05091666666665));
#72230=CARTESIAN_POINT('Ctrl Pts',(2.61811094239596,0.986814802625037,8.20877777777778));
#72231=CARTESIAN_POINT('Ctrl Pts',(0.606419780073446,2.73140319464357,8.36663888888888));
#72232=CARTESIAN_POINT('Ctrl Pts',(-1.95453607417732,2.00202325064244,8.52450000000001));
#72233=CARTESIAN_POINT('Ctrl Pts',(-2.74517095618734,-0.540689173813247,
8.68236111111111));
#72234=CARTESIAN_POINT('Ctrl Pts',(-1.04936735270146,-2.59367240037321,
8.84022222222223));
#72235=CARTESIAN_POINT('Ctrl Pts',(1.59690068918271,-2.29743695240177,8.99808333333332));
#72236=CARTESIAN_POINT('Ctrl Pts',(2.79677599470576,0.0797019247629725,
9.15594444444445));
#72237=CARTESIAN_POINT('Ctrl Pts',(1.46347155312646,2.38465078671139,9.31380555555555));
#72238=CARTESIAN_POINT('Ctrl Pts',(-1.19537219008389,2.52970229247383,9.47166666666666));
#72239=CARTESIAN_POINT('Ctrl Pts',(-2.77150761918447,0.383476046416537,
9.62952777777778));
#72240=CARTESIAN_POINT('Ctrl Pts',(-1.83735013131669,-2.1100836135863,9.78738888888888));
#72241=CARTESIAN_POINT('Ctrl Pts',(0.760987165659879,-2.69243512365168,
9.94525));
#72242=CARTESIAN_POINT('Ctrl Pts',(2.6700603672968,-0.836113626465368,10.1031111111111));
#72243=CARTESIAN_POINT('Ctrl Pts',(2.16072649637127,1.7775177549783,10.2609722222222));
#72244=CARTESIAN_POINT('Ctrl Pts',(-0.305685313585232,2.78116249982291,
10.4188333333333));
#72245=CARTESIAN_POINT('Ctrl Pts',(-2.4952226627859,1.26576941994835,10.5766944444444));
#72246=CARTESIAN_POINT('Ctrl Pts',(-2.42471218341845,-1.39609426222898,
10.7345555555556));
#72247=CARTESIAN_POINT('Ctrl Pts',(-0.158018739337926,-2.79344562132492,
10.8924166666667));
#72248=CARTESIAN_POINT('Ctrl Pts',(2.25180017160661,-1.66063371893121,11.0502777777778));
#72249=CARTESIAN_POINT('Ctrl Pts',(2.62205116590109,0.976297109112734,11.2081388888889));
#72250=CARTESIAN_POINT('Ctrl Pts',(0.617379419647229,2.72894686881467,11.366));
#72251=CARTESIAN_POINT('Ctrl Pts',(-1.9464837111559,2.00985310989732,11.5238611111111));
#72252=CARTESIAN_POINT('Ctrl Pts',(-2.74731929814685,-0.529665024907718,
11.6817222222222));
#72253=CARTESIAN_POINT('Ctrl Pts',(-1.05977053720295,-2.58943908287633,
11.8395833333333));
#72254=CARTESIAN_POINT('Ctrl Pts',(1.58766534266525,-2.30382879610199,11.9974444444444));
#72255=CARTESIAN_POINT('Ctrl Pts',(2.79707340746319,0.0684743370742143,
12.1553055555555));
#72256=CARTESIAN_POINT('Ctrl Pts',(1.47303233105958,2.37875683253439,12.3131666666667));
#72257=CARTESIAN_POINT('Ctrl Pts',(-1.18520769732058,2.53448043892505,12.4710277777778));
#72258=CARTESIAN_POINT('Ctrl Pts',(-2.76994594615232,0.394598452475193,
12.6288888888889));
#72259=CARTESIAN_POINT('Ctrl Pts',(-1.8458056761109,-2.1026909997905,12.78675));
#72260=CARTESIAN_POINT('Ctrl Pts',(0.750172845833004,-2.69546828972993,
12.9446111111111));
#72261=CARTESIAN_POINT('Ctrl Pts',(2.66668266040929,-0.846825037914988,
13.1024722222222));
#72262=CARTESIAN_POINT('Ctrl Pts',(2.16784415239069,1.76882949166842,13.2603333333333));
#72263=CARTESIAN_POINT('Ctrl Pts',(-0.294517949969841,2.78236767093066,
13.4181944444444));
#72264=CARTESIAN_POINT('Ctrl Pts',(-2.49012264935389,1.27577473748293,13.5760555555556));
#72265=CARTESIAN_POINT('Ctrl Pts',(-2.43029461870512,-1.3863478583448,13.7339166666666));
#72266=CARTESIAN_POINT('Ctrl Pts',(-0.16923542984156,-2.79279215602584,
13.8917777777778));
#72267=CARTESIAN_POINT('Ctrl Pts',(2.24512421134353,-1.66965318578134,14.0496388888889));
#72268=CARTESIAN_POINT('Ctrl Pts',(2.62593313585052,0.965751391486786,14.2075));
#72269=CARTESIAN_POINT('Ctrl Pts',(0.628359679142483,2.72647005025058,14.3653611111111));
#72270=CARTESIAN_POINT('Ctrl Pts',(-1.93845838021891,2.01760572163479,14.5232222222222));
#72271=CARTESIAN_POINT('Ctrl Pts',(-2.74931180160372,-0.518546638254714,
14.6810833333333));
#72272=CARTESIAN_POINT('Ctrl Pts',(-1.07036982067409,-2.58532778276268,
14.8389444444444));
#72273=CARTESIAN_POINT('Ctrl Pts',(1.57881200919325,-2.30987053095853,14.9968055555556));
#72274=CARTESIAN_POINT('Ctrl Pts',(2.79654399706859,0.0566462213665858,
15.1546666666667));
#72275=CARTESIAN_POINT('Ctrl Pts',(1.48409012818578,2.37398300468726,15.3125277777778));
#72276=CARTESIAN_POINT('Ctrl Pts',(-1.17817012667699,2.53688639776398,15.4703888888889));
#72277=CARTESIAN_POINT('Ctrl Pts',(-2.23297482288527,1.11978691060522,15.5756296296296));
#72278=CARTESIAN_POINT('Ctrl Pts',(-2.34668236863854,0.343918483395395,
15.62825));
#72279=CARTESIAN_POINT('',(1.37702479013102,-1.93106208855765,0.));
#72280=CARTESIAN_POINT('Ctrl Pts',(1.37702479013102,-1.93106208855765,-3.60822483003176E-15));
#72281=CARTESIAN_POINT('Ctrl Pts',(2.01547936988864,-1.47578528057288,0.0526203703703667));
#72282=CARTESIAN_POINT('Ctrl Pts',(2.79497483704674,0.109513025844136,0.157861111111108));
#72283=CARTESIAN_POINT('Ctrl Pts',(1.4349850222035,2.40398352764199,0.315722222222219));
#72284=CARTESIAN_POINT('Ctrl Pts',(-1.225925966736,2.51415445945906,0.473583333333329));
#72285=CARTESIAN_POINT('Ctrl Pts',(-2.32453883371355,0.980556500150706,
0.585479295290919));
#72286=CARTESIAN_POINT('Ctrl Pts',(-2.37485146083742,0.100616720091163,
0.644754886878137));
#72287=CARTESIAN_POINT('Ctrl Pts',(-2.37409249406917,0.00172857025301858,
0.651410108094986));
#72288=CARTESIAN_POINT('Ctrl Pts',(1.29200104020317,2.64812001020929,8.84708972748172E-17));
#72289=CARTESIAN_POINT('Ctrl Pts',(1.36315737313149,2.60529414881161,1.11522009070411E-16));
#72290=CARTESIAN_POINT('Ctrl Pts',(1.43224767624703,2.55934891308958,-5.0435019692162E-16));
#72291=CARTESIAN_POINT('Ctrl Pts',(1.49903325513988,2.51027466650741,-4.38885039422132E-16));
#72292=CARTESIAN_POINT('Ctrl Pts',(1.57786836962904,2.45234638450537,-3.65724347932505E-16));
#72293=CARTESIAN_POINT('Ctrl Pts',(1.65349331585608,2.39005818913334,-5.19266877679362E-16));
#72294=CARTESIAN_POINT('Ctrl Pts',(1.72573019513852,2.32378926839401,-6.48786580015326E-16));
#72295=CARTESIAN_POINT('Ctrl Pts',(1.76374109312884,2.28891869797108,-7.16939582223243E-16));
#72296=CARTESIAN_POINT('Ctrl Pts',(1.80081318017132,2.2529453987339,-5.63901193634668E-16));
#72297=CARTESIAN_POINT('Ctrl Pts',(1.83691551656788,2.21592189026143,-5.759281940243E-16));
#72298=CARTESIAN_POINT('Ctrl Pts',(1.85077163488616,2.20171222503873,-5.80544170635404E-16));
#72299=CARTESIAN_POINT('Ctrl Pts',(1.86448486767998,2.18734784556943,1.18680337545582E-16));
#72300=CARTESIAN_POINT('Ctrl Pts',(1.87805332095389,2.17283167229843,1.45716771982052E-16));
#72301=CARTESIAN_POINT('Ctrl Pts',(1.88973877018296,2.16033002584437,1.69001141656681E-16));
#72302=CARTESIAN_POINT('Ctrl Pts',(1.90131548250979,2.14771713833219,-1.20552840767492E-16));
#72303=CARTESIAN_POINT('Ctrl Pts',(1.91277473204616,2.1350036118777,-1.04083408558608E-16));
#72304=CARTESIAN_POINT('Ctrl Pts',(1.9778462733255,2.06280963801715,-1.05614606835039E-17));
#72305=CARTESIAN_POINT('Ctrl Pts',(2.03920496551099,1.98729716595704,-4.81412066085989E-16));
#72306=CARTESIAN_POINT('Ctrl Pts',(2.09668120715734,1.90884345828848,-3.33066907387547E-16));
#72307=CARTESIAN_POINT('Ctrl Pts',(2.14417843271961,1.84401087107344,-2.10477411937863E-16));
#72308=CARTESIAN_POINT('Ctrl Pts',(2.18902362087598,1.7771688452355,-1.7119245770294E-16));
#72309=CARTESIAN_POINT('Ctrl Pts',(2.23109606376114,1.7085204430367,-1.94289029309402E-16));
#72310=CARTESIAN_POINT('Ctrl Pts',(2.24950275752339,1.67848676707472,-2.0439377938723E-16));
#72311=CARTESIAN_POINT('Ctrl Pts',(2.26737842523222,1.6481072631063,-4.61788465798711E-16));
#72312=CARTESIAN_POINT('Ctrl Pts',(2.28471149018554,1.61739870311764,-5.13478148889135E-16));
#72313=CARTESIAN_POINT('Ctrl Pts',(2.29518347047447,1.59884575614786,-5.44707094486553E-16));
#72314=CARTESIAN_POINT('Ctrl Pts',(2.30545737670969,1.58017269818218,-5.13081578012294E-16));
#72315=CARTESIAN_POINT('Ctrl Pts',(2.3155304906665,1.56138322284078,-5.55111512312578E-16));
#72316=CARTESIAN_POINT('Ctrl Pts',(2.32274660107223,1.54792294341672,-5.85220637212436E-16));
#72317=CARTESIAN_POINT('Ctrl Pts',(2.32985933504635,1.5344033850802,-2.08590721469464E-17));
#72318=CARTESIAN_POINT('Ctrl Pts',(2.33686168047272,1.52083799385098,-2.77555756156289E-17));
#72319=CARTESIAN_POINT('Ctrl Pts',(2.38047027627073,1.43635663411551,-7.07050181056999E-17));
#72320=CARTESIAN_POINT('Ctrl Pts',(2.41986655819018,1.34997905359849,1.3198210981114E-16));
#72321=CARTESIAN_POINT('Ctrl Pts',(2.45488985599288,1.26205357875123,5.55111512312578E-17));
#72322=CARTESIAN_POINT('Ctrl Pts',(2.48959846523414,1.17491812491653,-2.02727065483809E-17));
#72323=CARTESIAN_POINT('Ctrl Pts',(2.52001253380174,1.08626153918075,-4.44579204063227E-16));
#72324=CARTESIAN_POINT('Ctrl Pts',(2.54592562425351,0.996413712953991,-4.9960036108132E-16));
#72325=CARTESIAN_POINT('Ctrl Pts',(2.57101139534936,0.909434430942866,-5.528648743571E-16));
#72326=CARTESIAN_POINT('Ctrl Pts',(2.59187898968551,0.821337996875181,-7.89241560757653E-18));
#72327=CARTESIAN_POINT('Ctrl Pts',(2.60829286172102,0.732427405689614,-8.32667268468867E-17));
#72328=CARTESIAN_POINT('Ctrl Pts',(2.61783087340729,0.680761945161682,-1.27066328786625E-16));
#72329=CARTESIAN_POINT('Ctrl Pts',(2.62586408863254,0.628821695636964,-4.14952786105416E-17));
#72330=CARTESIAN_POINT('Ctrl Pts',(2.63233843305125,0.576668196894126,-5.55111512312578E-17));
#72331=CARTESIAN_POINT('Ctrl Pts',(2.63414224296016,0.562137768524485,-5.94160979378542E-17));
#72332=CARTESIAN_POINT('Ctrl Pts',(2.63582527555606,0.547588319420663,3.76279563716787E-16));
#72333=CARTESIAN_POINT('Ctrl Pts',(2.63738542604938,0.533029261526728,3.60822483003176E-16));
#72334=CARTESIAN_POINT('Ctrl Pts',(2.64690685377435,0.444176924476997,2.66489610960485E-16));
#72335=CARTESIAN_POINT('Ctrl Pts',(2.65183263786108,0.355196731300303,5.62349138697447E-16));
#72336=CARTESIAN_POINT('Ctrl Pts',(2.65198717743404,0.266381980286723,3.88578058618805E-16));
#72337=CARTESIAN_POINT('Ctrl Pts',(2.65207998114243,0.213047173573617,2.84225494854879E-16));
#72338=CARTESIAN_POINT('Ctrl Pts',(2.65045121279133,0.159772024909719,-3.854419951949E-17));
#72339=CARTESIAN_POINT('Ctrl Pts',(2.64705383408491,0.106621318043217,-8.32667268468867E-17));
#72340=CARTESIAN_POINT('Ctrl Pts',(2.64128166054733,0.0163178428672467,
-1.29468843946197E-16));
#72341=CARTESIAN_POINT('Ctrl Pts',(2.63040647827402,-0.0736278476965388,
-4.84995897836269E-16));
#72342=CARTESIAN_POINT('Ctrl Pts',(2.61462343406994,-0.162881882998066,
-6.10622663543836E-16));
#72343=CARTESIAN_POINT('Ctrl Pts',(2.59852152905154,-0.253939094797703,
-7.38787434739808E-16));
#72344=CARTESIAN_POINT('Ctrl Pts',(2.57731092756958,-0.344277415185344,
-3.0810955291451E-16));
#72345=CARTESIAN_POINT('Ctrl Pts',(2.55115372858487,-0.433510589178544,
-3.60822483003176E-16));
#72346=CARTESIAN_POINT('Ctrl Pts',(2.54730992415644,-0.446623417870874,
-3.68568656216471E-16));
#72347=CARTESIAN_POINT('Ctrl Pts',(2.54335838534963,-0.4597150170452,-1.33461876853334E-16));
#72348=CARTESIAN_POINT('Ctrl Pts',(2.53930241226215,-0.472774949708627,
-1.38777878078145E-16));
#72349=CARTESIAN_POINT('Ctrl Pts',(2.51300579541719,-0.557448106523011,
-1.73243798916645E-16));
#72350=CARTESIAN_POINT('Ctrl Pts',(2.48237490705721,-0.640633082262047,
2.2266366763076E-16));
#72351=CARTESIAN_POINT('Ctrl Pts',(2.4476284488952,-0.722031078376524,1.66533453693773E-16));
#72352=CARTESIAN_POINT('Ctrl Pts',(2.41285997251409,-0.803480654968775,
1.10367671027941E-16));
#72353=CARTESIAN_POINT('Ctrl Pts',(2.37397005509887,-0.883141781461701,
-2.60473824643759E-16));
#72354=CARTESIAN_POINT('Ctrl Pts',(2.33113438836321,-0.960686402199183,
-2.22044604925031E-16));
#72355=CARTESIAN_POINT('Ctrl Pts',(2.28891526223189,-1.03711491080453,-1.84168503113759E-16));
#72356=CARTESIAN_POINT('Ctrl Pts',(2.24286247138705,-1.11148803969701,-4.86311355035046E-16));
#72357=CARTESIAN_POINT('Ctrl Pts',(2.19311210725222,-1.18345333925267,-6.10622663543836E-16));
#72358=CARTESIAN_POINT('Ctrl Pts',(2.16658994742807,-1.22181838863071,-6.76893623556989E-16));
#72359=CARTESIAN_POINT('Ctrl Pts',(2.13901644812981,-1.25949841963374,-1.03661145615814E-16));
#72360=CARTESIAN_POINT('Ctrl Pts',(2.11040940583919,-1.29643454206688,-5.55111512312578E-17));
#72361=CARTESIAN_POINT('Ctrl Pts',(2.10166865720486,-1.30772020237512,-4.0799144537779E-17));
#72362=CARTESIAN_POINT('Ctrl Pts',(2.09283023898332,-1.31893783850973,-3.98702450321844E-16));
#72363=CARTESIAN_POINT('Ctrl Pts',(2.08389831377262,-1.33008110200649,-3.88578058618805E-16));
#72364=CARTESIAN_POINT('Ctrl Pts',(2.03043260129099,-1.39678368942974,-3.27974347428123E-16));
#72365=CARTESIAN_POINT('Ctrl Pts',(1.97380215986925,-1.46059813131217,-2.08556400160018E-16));
#72366=CARTESIAN_POINT('Ctrl Pts',(1.91417150281915,-1.52123259912064,-1.11022302462516E-16));
#72367=CARTESIAN_POINT('Ctrl Pts',(1.85542332105702,-1.58096973622562,-1.49316138302572E-17));
#72368=CARTESIAN_POINT('Ctrl Pts',(1.79376241718216,-1.63762085789259,-5.35520206863283E-16));
#72369=CARTESIAN_POINT('Ctrl Pts',(1.72931881925135,-1.69086532717403,-5.55111512312578E-16));
#72370=CARTESIAN_POINT('Ctrl Pts',(1.66690919772329,-1.7424292882658,-5.74084474679515E-16));
#72371=CARTESIAN_POINT('Ctrl Pts',(1.60188918190129,-1.79079854027645,-4.05239810717764E-16));
#72372=CARTESIAN_POINT('Ctrl Pts',(1.53436012060039,-1.83563678794726,-4.44089209850063E-16));
#72373=CARTESIAN_POINT('Ctrl Pts',(1.48333459704145,-1.8695169429323,-4.73444140786276E-16));
#72374=CARTESIAN_POINT('Ctrl Pts',(1.43087616732457,-1.90138023485661,-2.26823314612322E-16));
#72375=CARTESIAN_POINT('Ctrl Pts',(1.37702479013106,-1.93106208855762,-2.22044604925031E-16));
#72376=CARTESIAN_POINT('Ctrl Pts',(0.260984867623806,2.92515103163649,15.058));
#72377=CARTESIAN_POINT('Ctrl Pts',(0.721611965671866,2.88493263312463,15.0330979289241));
#72378=CARTESIAN_POINT('Ctrl Pts',(1.17298362662806,2.74202417939443,15.0081958578483));
#72379=CARTESIAN_POINT('Ctrl Pts',(1.56185858228333,2.49936439089571,14.9832937867724));
#72380=CARTESIAN_POINT('Ctrl Pts',(2.3835871899963,1.98660190194863,14.930673416402));
#72381=CARTESIAN_POINT('Ctrl Pts',(2.92625811262771,1.02843390833919,14.8780530460316));
#72382=CARTESIAN_POINT('Ctrl Pts',(2.94584082398175,0.0600984948350938,
14.8254326756613));
#72383=CARTESIAN_POINT('Ctrl Pts',(2.96542353533579,-0.90823691866899,14.7728123052909));
#72384=CARTESIAN_POINT('Ctrl Pts',(2.46191803541247,-1.88673975206773,14.7201919349205));
#72385=CARTESIAN_POINT('Ctrl Pts',(1.6624759601657,-2.43293893833301,14.6675715645502));
#72386=CARTESIAN_POINT('Ctrl Pts',(0.863033884918936,-2.97913812459828,
14.6149511941798));
#72387=CARTESIAN_POINT('Ctrl Pts',(-0.232344765651281,-3.0930336637301,
14.5623308238094));
#72388=CARTESIAN_POINT('Ctrl Pts',(-1.12713695505886,-2.72269707033318,
14.5097104534391));
#72389=CARTESIAN_POINT('Ctrl Pts',(-2.02192914446644,-2.35236047693625,
14.4570900830687));
#72390=CARTESIAN_POINT('Ctrl Pts',(-2.71613487271139,-1.49779175101059,
14.4044697126983));
#72391=CARTESIAN_POINT('Ctrl Pts',(-2.89560267371491,-0.546185667602603,
14.351849342328));
#72392=CARTESIAN_POINT('Ctrl Pts',(-2.9293373183321,-0.367311836977727,
14.3419582672485));
#72393=CARTESIAN_POINT('Ctrl Pts',(-2.94488478294563,-0.185009395803266,
14.3320671921691));
#72394=CARTESIAN_POINT('Ctrl Pts',(-2.94325266537063,-0.0024318079996577,
14.3221761170896));
#72395=CARTESIAN_POINT('Origin',(0.,0.,-1.84858989190501));
#72396=CARTESIAN_POINT('',(-1.37702479013098,-1.93106208855768,0.));
#72397=CARTESIAN_POINT('Ctrl Pts',(-1.37994859234593,-1.93347131995891,
-1.03866568124111E-15));
#72398=CARTESIAN_POINT('Ctrl Pts',(-0.794305021574331,-2.34617453422284,
0.0482502273315914));
#72399=CARTESIAN_POINT('Ctrl Pts',(0.853330802601401,-2.62819893329841,
0.149165418329868));
#72400=CARTESIAN_POINT('Ctrl Pts',(2.68321992772198,-0.795544356782894,
0.30274557299483));
#72401=CARTESIAN_POINT('Ctrl Pts',(2.13222685489998,1.81318819272267,0.460740463994884));
#72402=CARTESIAN_POINT('Ctrl Pts',(-0.353356050373597,2.77617865909866,
0.618735354994938));
#72403=CARTESIAN_POINT('Ctrl Pts',(-2.12480812784407,1.50378450145058,0.74801849763165));
#72404=CARTESIAN_POINT('Ctrl Pts',(-2.36883710346974,0.358840951777969,
0.824636676601679));
#72405=CARTESIAN_POINT('Ctrl Pts',(-2.36806791026422,0.000580996437929554,
0.848589891905023));
#72406=CARTESIAN_POINT('Origin',(0.,0.,0.));
#72407=CARTESIAN_POINT('Ctrl Pts',(-1.03908919352511,2.13201587949043,-0.329233991005384));
#72408=CARTESIAN_POINT('Ctrl Pts',(-1.74458119175558,1.78817739379635,-0.2765690273387));
#72409=CARTESIAN_POINT('Ctrl Pts',(-2.77573338088225,0.351504794741619,
-0.171239100005331));
#72410=CARTESIAN_POINT('Ctrl Pts',(-1.80933791412281,-2.1375423700464,-0.013244209005277));
#72411=CARTESIAN_POINT('Ctrl Pts',(0.800729748594893,-2.68087948155196,
0.144750681994776));
#72412=CARTESIAN_POINT('Ctrl Pts',(2.68321992772198,-0.795544356782894,
0.30274557299483));
#72413=CARTESIAN_POINT('Ctrl Pts',(2.13222685489998,1.81318819272267,0.460740463994884));
#72414=CARTESIAN_POINT('Ctrl Pts',(-0.353356050373597,2.77617865909866,
0.618735354994938));
#72415=CARTESIAN_POINT('Ctrl Pts',(-2.51821971460423,1.2212058130903,0.77673024599499));
#72416=CARTESIAN_POINT('Ctrl Pts',(-2.39875016986203,-1.44183805604875,
0.934725136995045));
#72417=CARTESIAN_POINT('Ctrl Pts',(-0.103189861818606,-2.79677945469355,
1.0927200279951));
#72418=CARTESIAN_POINT('Ctrl Pts',(2.28595558559378,-1.6146683983646,1.25071491899515));
#72419=CARTESIAN_POINT('Ctrl Pts',(2.60139192527736,1.0322363870214,1.4087098099952));
#72420=CARTESIAN_POINT('Ctrl Pts',(0.556949311928898,2.7427217714679,1.56670470099526));
#72421=CARTESIAN_POINT('Ctrl Pts',(-1.99273057992189,1.96513605211958,1.72469959199531));
#72422=CARTESIAN_POINT('Ctrl Pts',(-2.73469173326279,-0.595142683011921,
1.88269448299537));
#72423=CARTESIAN_POINT('Ctrl Pts',(-0.995855715555496,-2.61553061219188,
2.04068937399542));
#72424=CARTESIAN_POINT('Ctrl Pts',(1.64637781974439,-2.26322161422709,2.19868426499547));
#72425=CARTESIAN_POINT('Ctrl Pts',(2.79508756969503,0.142186649832604,2.35667915599553));
#72426=CARTESIAN_POINT('Ctrl Pts',(1.40821242874264,2.41860884498944,2.51467404699558));
#72427=CARTESIAN_POINT('Ctrl Pts',(-1.25613315819632,2.50097199645567,2.67266893799564));
#72428=CARTESIAN_POINT('Ctrl Pts',(-2.78096812139655,0.314559449318749,
2.83066382899569));
#72429=CARTESIAN_POINT('Ctrl Pts',(-1.78302687496254,-2.15720801874703,
2.98865871999574));
#72430=CARTESIAN_POINT('Ctrl Pts',(0.832400628534772,-2.67204800324426,
3.1466536109958));
#72431=CARTESIAN_POINT('Ctrl Pts',(2.69270963387839,-0.762919488957052,
3.30464850199585));
#72432=CARTESIAN_POINT('Ctrl Pts',(2.11030679852043,1.83829718168443,3.4626433929959));
#72433=CARTESIAN_POINT('Ctrl Pts',(-0.386476751895552,2.77188871376435,
3.62063828399595));
#72434=CARTESIAN_POINT('Ctrl Pts',(-2.53266500493224,1.1909405067813,3.77863317499601));
#72435=CARTESIAN_POINT('Ctrl Pts',(-2.38132711099884,-1.47037835529628,
3.93662806599605));
#72436=CARTESIAN_POINT('Ctrl Pts',(-0.0697503817448946,-2.79783241149437,
4.09462295699612));
#72437=CARTESIAN_POINT('Ctrl Pts',(2.30510093209087,-1.58721170953314,4.25261784799616));
#72438=CARTESIAN_POINT('Ctrl Pts',(2.5888625630092,1.06326005653742,4.41061273899623));
#72439=CARTESIAN_POINT('Ctrl Pts',(0.524118009051023,2.74918744918107,4.56860762999628));
#72440=CARTESIAN_POINT('Ctrl Pts',(-2.01608414683087,1.9411687281004,4.72660252099633));
#72441=CARTESIAN_POINT('Ctrl Pts',(-2.72738037475851,-0.627795834204506,
4.88459741199638));
#72442=CARTESIAN_POINT('Ctrl Pts',(-0.964512940920624,-2.62725067416123,
5.04259230299644));
#72443=CARTESIAN_POINT('Ctrl Pts',(1.67331967629405,-2.24337526486265,5.20058719399648));
#72444=CARTESIAN_POINT('Ctrl Pts',(2.79318773824162,0.175594923072764,5.35858208499656));
#72445=CARTESIAN_POINT('Ctrl Pts',(1.37919449268132,2.43527285317938,5.51657697599659));
#72446=CARTESIAN_POINT('Ctrl Pts',(-1.28594543116668,2.48577466117395,5.67457186699666));
#72447=CARTESIAN_POINT('Ctrl Pts',(-2.78453026564846,0.281287251330417,
5.8325667579967));
#72448=CARTESIAN_POINT('Ctrl Pts',(-1.75710748413146,-2.17837200846936,
5.99056164899676));
#72449=CARTESIAN_POINT('Ctrl Pts',(0.864288593995119,-2.66190468356086,
6.14855653999681));
#72450=CARTESIAN_POINT('Ctrl Pts',(2.70163876039796,-0.730670463607777,
6.30655143099686));
#72451=CARTESIAN_POINT('Ctrl Pts',(2.08817696449889,1.86339697407977,6.46454632199692));
#72452=CARTESIAN_POINT('Ctrl Pts',(-0.419590302218696,2.76706980330411,
6.62254121299697));
#72453=CARTESIAN_POINT('Ctrl Pts',(-2.54672306405081,1.16057440653543,6.78053610399702));
#72454=CARTESIAN_POINT('Ctrl Pts',(-2.3635768050391,-1.49874480975067,6.93853099499709));
#72455=CARTESIAN_POINT('Ctrl Pts',(-0.0362940343214689,-2.79846637663312,
7.09652588599712));
#72456=CARTESIAN_POINT('Ctrl Pts',(2.32391314315961,-1.55953807940794,7.2545207769972));
#72457=CARTESIAN_POINT('Ctrl Pts',(2.57596499873257,1.09413693995685,7.41251566799723));
#72458=CARTESIAN_POINT('Ctrl Pts',(0.491210792034311,2.75525738831465,7.5705105589973));
#72459=CARTESIAN_POINT('Ctrl Pts',(-2.03914898665099,1.91692533196097,7.72850544999735));
#72460=CARTESIAN_POINT('Ctrl Pts',(-2.71967939412015,-0.66035998612245,
7.8865003409974));
#72461=CARTESIAN_POINT('Ctrl Pts',(-0.9330321424437,-2.63859476601473,8.04449523199746));
#72462=CARTESIAN_POINT('Ctrl Pts',(1.70002224901497,-2.22320841823872,8.2024901229975));
#72463=CARTESIAN_POINT('Ctrl Pts',(2.79088864512093,0.208978201275766,8.36048501399757));
#72464=CARTESIAN_POINT('Ctrl Pts',(1.34997937336987,2.45158867054595,8.51847990499762));
#72465=CARTESIAN_POINT('Ctrl Pts',(-1.31557386100644,2.47022200101732,8.67647479599767));
#72466=CARTESIAN_POINT('Ctrl Pts',(-2.78769435259396,0.247974826523285,
8.83446968699772));
#72467=CARTESIAN_POINT('Ctrl Pts',(-1.73093690286391,-2.19922458070505,
8.99246457799778));
#72468=CARTESIAN_POINT('Ctrl Pts',(0.896053003445084,-2.6513808351669,9.15045946899784));
#72469=CARTESIAN_POINT('Ctrl Pts',(2.71018167460651,-0.698316982967359,
9.30845435999788));
#72470=CARTESIAN_POINT('Ctrl Pts',(2.06574861445826,1.88823038317285,9.46644925099794));
#72471=CARTESIAN_POINT('Ctrl Pts',(-0.45264386973844,2.76185532663481,9.62444414199799));
#72472=CARTESIAN_POINT('Ctrl Pts',(-2.5604170561675,1.13004239591331,9.78243903299804));
#72473=CARTESIAN_POINT('Ctrl Pts',(-2.34548861359897,-1.52689701078686,
9.9404339239981));
#72474=CARTESIAN_POINT('Ctrl Pts',(-0.00283249851198579,-2.79870028674429,
10.0984288149982));
#72475=CARTESIAN_POINT('Ctrl Pts',(2.34239313895008,-1.53164150527581,10.2564237059982));
#72476=CARTESIAN_POINT('Ctrl Pts',(2.56269918704329,1.12485741087042,10.4144185969983));
#72477=CARTESIAN_POINT('Ctrl Pts',(0.458233353927178,2.76093344928963,10.5724134879983));
#72478=CARTESIAN_POINT('Ctrl Pts',(-2.06192231968409,1.89240790151988,10.7304083789984));
#72479=CARTESIAN_POINT('Ctrl Pts',(-2.71158962134898,-0.692829736205835,
10.8884032699984));
#72480=CARTESIAN_POINT('Ctrl Pts',(-0.90141796228012,-2.64956165719617,
11.0463981609985));
#72481=CARTESIAN_POINT('Ctrl Pts',(1.72648179491819,-2.20272375262492,11.2043930519985));
#72482=CARTESIAN_POINT('Ctrl Pts',(2.7881905800153,0.242331605070017,11.3623879429986));
#72483=CARTESIAN_POINT('Ctrl Pts',(1.32057126786748,2.46755402056041,11.5203828339987));
#72484=CARTESIAN_POINT('Ctrl Pts',(-1.34501422335496,2.45431621031658,11.6783777249987));
#72485=CARTESIAN_POINT('Ctrl Pts',(-2.79045992331823,0.214626951768239,
11.8363726159988));
#72486=CARTESIAN_POINT('Ctrl Pts',(-1.70451887724915,-2.21976276122321,
11.9943675069988));
#72487=CARTESIAN_POINT('Ctrl Pts',(0.927689321261817,-2.64047796075702,
12.1523623979988));
#72488=CARTESIAN_POINT('Ctrl Pts',(2.71833714731268,-0.66586366962402,12.3103572889989));
#72489=CARTESIAN_POINT('Ctrl Pts',(2.04302496870488,1.91279385105346,12.468352179999));
#72490=CARTESIAN_POINT('Ctrl Pts',(-0.48563275555883,2.75624604578475,12.626347070999));
#72491=CARTESIAN_POINT('Ctrl Pts',(-2.57374497374716,1.09934880708429,12.7843419619991));
#72492=CARTESIAN_POINT('Ctrl Pts',(-2.32706521767492,-1.55483087129818,
12.9423368529991));
#72493=CARTESIAN_POINT('Ctrl Pts',(0.0306296239850783,-2.7985342282319,
13.1003317439992));
#72494=CARTESIAN_POINT('Ctrl Pts',(2.36053793034993,-1.50352574600393,13.2583266349992));
#72495=CARTESIAN_POINT('Ctrl Pts',(2.54906768788899,1.15541663986578,13.4163215259993));
#72496=CARTESIAN_POINT('Ctrl Pts',(0.42518914129335,2.76621565710669,13.5743164169993));
#72497=CARTESIAN_POINT('Ctrl Pts',(-2.08439846825039,1.86761834358563,13.7323113079994));
#72498=CARTESIAN_POINT('Ctrl Pts',(-2.7031168406022,-0.725197389434075,
13.8903061989994));
#72499=CARTESIAN_POINT('Ctrl Pts',(-0.869666078203209,-2.66015561356989,
14.0483010899995));
#72500=CARTESIAN_POINT('Ctrl Pts',(1.75267763866885,-2.18191305067097,14.2062959809995));
#72501=CARTESIAN_POINT('Ctrl Pts',(2.78512620401791,0.275629071355557,14.3642908719996));
#72502=CARTESIAN_POINT('Ctrl Pts',(1.29091271455523,2.48320730756548,14.5222857629997));
#72503=CARTESIAN_POINT('Ctrl Pts',(-1.37414448785656,2.43798182357128,14.6802806539997));
#72504=CARTESIAN_POINT('Ctrl Pts',(-2.79305172314729,0.181396953694044,
14.8382755449998));
#72505=CARTESIAN_POINT('Ctrl Pts',(-1.67742675687761,-2.24026772494819,
14.9962704359998));
#72506=CARTESIAN_POINT('Ctrl Pts',(0.958368222991996,-2.62865236842956,
15.1542653269999));
#72507=CARTESIAN_POINT('Ctrl Pts',(2.7277014223945,-0.634378452891388,15.3122602179999));
#72508=CARTESIAN_POINT('Ctrl Pts',(2.01676643438217,1.93930517753648,15.470255109));
#72509=CARTESIAN_POINT('Ctrl Pts',(0.331786659212352,2.47609764328476,15.5755850363333));
#72510=CARTESIAN_POINT('Ctrl Pts',(-0.439445221994538,2.33068358199181,
15.62825));
#72511=CARTESIAN_POINT('Ctrl Pts',(-1.12236674703448,2.30288577939268,-0.219489327336923));
#72512=CARTESIAN_POINT('Ctrl Pts',(-1.88440023178909,1.93149044095738,-0.166824363670239));
#72513=CARTESIAN_POINT('Ctrl Pts',(-2.99819386511655,0.37967606197771,-0.0614944363368692));
#72514=CARTESIAN_POINT('Ctrl Pts',(-1.9543468660962,-2.30885518920509,0.096500454663184));
#72515=CARTESIAN_POINT('Ctrl Pts',(0.864904041716857,-2.89573792283723,
0.254495345663238));
#72516=CARTESIAN_POINT('Ctrl Pts',(2.89826594350265,-0.859303067925248,
0.412490236663291));
#72517=CARTESIAN_POINT('Ctrl Pts',(2.30311366337569,1.95850572434841,0.570485127663346));
#72518=CARTESIAN_POINT('Ctrl Pts',(-0.381675686047029,2.99867483004853,
0.728480018663398));
#72519=CARTESIAN_POINT('Ctrl Pts',(-2.72004182798788,1.31907905927489,0.886474909663454));
#72520=CARTESIAN_POINT('Ctrl Pts',(-2.59099742531531,-1.55739382028214,
1.0444698006635));
#72521=CARTESIAN_POINT('Ctrl Pts',(-0.111459988476451,-3.02092667145178,
1.20246469166356));
#72522=CARTESIAN_POINT('Ctrl Pts',(2.46916294621846,-1.74407560881646,1.36045958266361));
#72523=CARTESIAN_POINT('Ctrl Pts',(2.80987985548213,1.11496472400166,1.51845447366367));
#72524=CARTESIAN_POINT('Ctrl Pts',(0.60158588058462,2.96253654820512,1.67644936466372));
#72525=CARTESIAN_POINT('Ctrl Pts',(-2.15243749298894,2.12263140839256,1.83444425566377));
#72526=CARTESIAN_POINT('Ctrl Pts',(-2.95386294451934,-0.642840250207365,
1.99243914666383));
#72527=CARTESIAN_POINT('Ctrl Pts',(-1.07566833237088,-2.82515168405898,
2.15043403766388));
#72528=CARTESIAN_POINT('Ctrl Pts',(1.77832637414643,-2.44460696618424,2.30842892866393));
#72529=CARTESIAN_POINT('Ctrl Pts',(3.01909919073696,0.153582164686878,2.46642381966399));
#72530=CARTESIAN_POINT('Ctrl Pts',(1.52107327516274,2.61244766918467,2.62441871066404));
#72531=CARTESIAN_POINT('Ctrl Pts',(-1.35680564805421,2.70141179561648,2.7824136016641));
#72532=CARTESIAN_POINT('Ctrl Pts',(-3.00384814265038,0.339769740731444,
2.94040849266415));
#72533=CARTESIAN_POINT('Ctrl Pts',(-1.92592713503036,-2.33009693659115,
3.0984033836642));
#72534=CARTESIAN_POINT('Ctrl Pts',(0.899113176712534,-2.88619864782458,
3.25639827466426));
#72535=CARTESIAN_POINT('Ctrl Pts',(2.90851619987664,-0.824063487913928,
3.41439316566431));
#72536=CARTESIAN_POINT('Ctrl Pts',(2.27943682934948,1.98562706719167,3.57238805666436));
#72537=CARTESIAN_POINT('Ctrl Pts',(-0.417450838226782,2.99404106807715,
3.73038294766441));
#72538=CARTESIAN_POINT('Ctrl Pts',(-2.73564483263507,1.2863881472707,3.88837783866447));
#72539=CARTESIAN_POINT('Ctrl Pts',(-2.57217799958985,-1.5882214749488,4.04637272966452));
#72540=CARTESIAN_POINT('Ctrl Pts',(-0.0753405093145775,-3.02206401722216,
4.20436762066458));
#72541=CARTESIAN_POINT('Ctrl Pts',(2.48984269190601,-1.71441841026206,4.36236251166463));
#72542=CARTESIAN_POINT('Ctrl Pts',(2.79634633048836,1.1484747780497,4.52035740266469));
#72543=CARTESIAN_POINT('Ctrl Pts',(0.566123320833673,2.9695204161036,4.67835229366474));
#72544=CARTESIAN_POINT('Ctrl Pts',(-2.1776627259012,2.09674322895411,4.83634718466479));
#72545=CARTESIAN_POINT('Ctrl Pts',(-2.94596561894615,-0.678110380349046,
4.99434207566485));
#72546=CARTESIAN_POINT('Ctrl Pts',(-1.04181359860098,-2.83781104757613,
5.1523369666649));
#72547=CARTESIAN_POINT('Ctrl Pts',(1.80742747930962,-2.42317003592312,5.31033185766495));
#72548=CARTESIAN_POINT('Ctrl Pts',(3.01704709774863,0.189667935951029,5.46832674866501));
#72549=CARTESIAN_POINT('Ctrl Pts',(1.48972970359473,2.63044721030322,5.62632163966506));
#72550=CARTESIAN_POINT('Ctrl Pts',(-1.38900721847178,2.68499647355363,5.78431653066512));
#72551=CARTESIAN_POINT('Ctrl Pts',(-3.00769577409666,0.303830950437453,
5.94231142166516));
#72552=CARTESIAN_POINT('Ctrl Pts',(-1.89793044085485,-2.35295710917974,
6.10030631266523));
#72553=CARTESIAN_POINT('Ctrl Pts',(0.933556795495496,-2.87524239422467,
6.25830120366527));
#72554=CARTESIAN_POINT('Ctrl Pts',(2.91816094909363,-0.789229872184075,
6.41629609466533));
#72555=CARTESIAN_POINT('Ctrl Pts',(2.25553340510261,2.01273847641193,6.57429098566538));
#72556=CARTESIAN_POINT('Ctrl Pts',(-0.453218266076613,2.98883594719704,
6.73228587666544));
#72557=CARTESIAN_POINT('Ctrl Pts',(-2.75082957152067,1.25358836322381,6.89028076766548));
#72558=CARTESIAN_POINT('Ctrl Pts',(-2.55300509962799,-1.61886135207317,
7.04827565866555));
#72559=CARTESIAN_POINT('Ctrl Pts',(-0.0392028109733089,-3.02274879134448,
7.20627054966559));
#72560=CARTESIAN_POINT('Ctrl Pts',(2.51016260310644,-1.68452688370611,7.36426544066566));
#72561=CARTESIAN_POINT('Ctrl Pts',(2.78241509402469,1.18182628186475,7.5222603316657));
#72562=CARTESIAN_POINT('Ctrl Pts',(0.530578762823495,2.97607682904918,7.68025522266576));
#72563=CARTESIAN_POINT('Ctrl Pts',(-2.2025760917615,2.07055685166173,7.83825011366581));
#72564=CARTESIAN_POINT('Ctrl Pts',(-2.93764744506665,-0.713284378390626,
7.99624500466586));
#72565=CARTESIAN_POINT('Ctrl Pts',(-1.0078097791014,-2.85006430894292,8.15423989566592));
#72566=CARTESIAN_POINT('Ctrl Pts',(1.83627012329917,-2.40138692222673,8.31223478666596));
#72567=CARTESIAN_POINT('Ctrl Pts',(3.01456374436274,0.225726708956776,8.47022967766603));
#72568=CARTESIAN_POINT('Ctrl Pts',(1.45817314557243,2.64807065492862,8.62822456866608));
#72569=CARTESIAN_POINT('Ctrl Pts',(-1.42101021169528,2.66819734918923,8.78621945966612));
#72570=CARTESIAN_POINT('Ctrl Pts',(-3.01111344602942,0.267848709355943,
8.9442143506662));
#72571=CARTESIAN_POINT('Ctrl Pts',(-1.86966242464576,-2.37548090580212,
9.10220924166623));
#72572=CARTESIAN_POINT('Ctrl Pts',(0.967866955901341,-2.86387511453221,
9.26020413266631));
#72573=CARTESIAN_POINT('Ctrl Pts',(2.92738853310682,-0.754283429618888,
9.41819902366633));
#72574=CARTESIAN_POINT('Ctrl Pts',(2.23130754034209,2.03956215310421,9.57619391466641));
#72575=CARTESIAN_POINT('Ctrl Pts',(-0.488920903815691,2.98320355754919,
9.73418880566644));
#72576=CARTESIAN_POINT('Ctrl Pts',(-2.76562106534208,1.22060937195346,9.89218369666651));
#72577=CARTESIAN_POINT('Ctrl Pts',(-2.53346723443519,-1.64926980449067,
10.0501785876666));
#72578=CARTESIAN_POINT('Ctrl Pts',(-0.00305950842402692,-3.02300144812525,
10.2081734786666));
#72579=CARTESIAN_POINT('Ctrl Pts',(2.53012367371502,-1.65439454534941,10.3661683696667));
#72580=CARTESIAN_POINT('Ctrl Pts',(2.76808609704807,1.21500883753128,10.5241632606667));
#72581=CARTESIAN_POINT('Ctrl Pts',(0.494958355870487,2.98220779656589,10.6821581516668));
#72582=CARTESIAN_POINT('Ctrl Pts',(-2.22717458809345,2.0440744776545,10.8401530426668));
#72583=CARTESIAN_POINT('Ctrl Pts',(-2.92890931940236,-0.748356408785326,
10.9981479336669));
#72584=CARTESIAN_POINT('Ctrl Pts',(-0.973661888071959,-2.86191013898051,
11.1561428246669));
#72585=CARTESIAN_POINT('Ctrl Pts',(1.86485026314516,-2.37926051801397,11.314137715667));
#72586=CARTESIAN_POINT('Ctrl Pts',(3.01164944347811,0.261753213276476,11.472132606667));
#72587=CARTESIAN_POINT('Ctrl Pts',(1.42640813452734,2.66531554408024,11.6301274976671));
#72588=CARTESIAN_POINT('Ctrl Pts',(-1.45281006480367,2.6510167927182,11.7881223886671));
#72589=CARTESIAN_POINT('Ctrl Pts',(-3.01410066275426,0.231828177198969,
11.9461172796672));
#72590=CARTESIAN_POINT('Ctrl Pts',(-1.84112713272175,-2.39766511385838,
12.1041121706673));
#72591=CARTESIAN_POINT('Ctrl Pts',(1.00203875880082,-2.85209843187493,12.2621070616673));
#72592=CARTESIAN_POINT('Ctrl Pts',(2.9361976242116,-0.71922915328282,12.4201019526674));
#72593=CARTESIAN_POINT('Ctrl Pts',(2.20676271346495,2.0660942542105,12.5780968436674));
#72594=CARTESIAN_POINT('Ctrl Pts',(-0.52455367595618,2.97714472223446,12.7360917346675));
#72595=CARTESIAN_POINT('Ctrl Pts',(-2.78001714567073,1.1874558528297,12.8940866256675));
#72596=CARTESIAN_POINT('Ctrl Pts',(-2.51356729987571,-1.67944241753446,
13.0520815166676));
#72597=CARTESIAN_POINT('Ctrl Pts',(0.0330844278327718,-3.02282208089334,
13.2100764076676));
#72598=CARTESIAN_POINT('Ctrl Pts',(2.5497226750577,-1.62402545531265,13.3680712986677));
#72599=CARTESIAN_POINT('Ctrl Pts',(2.75336210467249,1.24801722858484,13.5260661896677));
#72600=CARTESIAN_POINT('Ctrl Pts',(0.459265822762407,2.98791334565805,13.6840610806678));
#72601=CARTESIAN_POINT('Ctrl Pts',(-2.25145208218098,2.01729816656161,13.8420559716679));
#72602=CARTESIAN_POINT('Ctrl Pts',(-2.91975748968037,-0.78331815979697,
14.0000508626679));
#72603=CARTESIAN_POINT('Ctrl Pts',(-0.939365256882179,-2.87335314543991,
14.158045753668));
#72604=CARTESIAN_POINT('Ctrl Pts',(1.893145566493,-2.35678194735699,14.316040644668));
#72605=CARTESIAN_POINT('Ctrl Pts',(3.0083394738034,0.297719296989276,14.4740355356681));
#72606=CARTESIAN_POINT('Ctrl Pts',(1.3943726035929,2.68222336000765,14.6320304266681));
#72607=CARTESIAN_POINT('Ctrl Pts',(-1.4842749673478,2.63337329047569,14.7900253176682));
#72608=CARTESIAN_POINT('Ctrl Pts',(-3.01690018175728,0.195934968921086,
14.9480202086682));
#72609=CARTESIAN_POINT('Ctrl Pts',(-1.81186372087882,-2.41981344296957,
15.1060150996683));
#72610=CARTESIAN_POINT('Ctrl Pts',(1.03517641373175,-2.8393250802945,15.2640099906683));
#72611=CARTESIAN_POINT('Ctrl Pts',(2.94631239686769,-0.685220561427491,
15.4220048816684));
#72612=CARTESIAN_POINT('Ctrl Pts',(2.17839969522424,2.09473032457841,15.5799997726684));
#72613=CARTESIAN_POINT('Ctrl Pts',(0.358377621218746,2.67454389339306,15.6853297000018));
#72614=CARTESIAN_POINT('Ctrl Pts',(-0.474664453622694,2.51747565713054,
15.7379946636685));
#72615=CARTESIAN_POINT('Ctrl Pts',(-1.20564430054385,2.47375567929493,-0.109744663668462));
#72616=CARTESIAN_POINT('Ctrl Pts',(-2.02421927182262,2.0748034881184,-0.057079700001777));
#72617=CARTESIAN_POINT('Ctrl Pts',(-3.22065434935084,0.407847329213798,
0.0482502273315919));
#72618=CARTESIAN_POINT('Ctrl Pts',(-2.09935581806959,-2.48016800836378,
0.206245118331646));
#72619=CARTESIAN_POINT('Ctrl Pts',(0.929078334838823,-3.11059636412251,
0.364240009331699));
#72620=CARTESIAN_POINT('Ctrl Pts',(3.11331195928332,-0.923061779067598,
0.522234900331752));
#72621=CARTESIAN_POINT('Ctrl Pts',(2.4740004718514,2.10382325597413,0.680229791331807));
#72622=CARTESIAN_POINT('Ctrl Pts',(-0.409995321720456,3.2211710009984,0.83822468233186));
#72623=CARTESIAN_POINT('Ctrl Pts',(-2.92186394137152,1.41695230545948,0.996219573331913));
#72624=CARTESIAN_POINT('Ctrl Pts',(-2.78324468076858,-1.67294958451553,
1.15421446433197));
#72625=CARTESIAN_POINT('Ctrl Pts',(-0.119730115134298,-3.24507388821001,
1.31220935533202));
#72626=CARTESIAN_POINT('Ctrl Pts',(2.65237030684314,-1.87348281926831,1.47020424633207));
#72627=CARTESIAN_POINT('Ctrl Pts',(3.0183677856869,1.19769306098192,1.62819913733213));
#72628=CARTESIAN_POINT('Ctrl Pts',(0.646222449240343,3.18235132494235,1.78619402833218));
#72629=CARTESIAN_POINT('Ctrl Pts',(-2.31214440605599,2.28012676466554,1.94418891933223));
#72630=CARTESIAN_POINT('Ctrl Pts',(-3.17303415577589,-0.690537817402807,
2.10218381033229));
#72631=CARTESIAN_POINT('Ctrl Pts',(-1.15548094918627,-3.03477275592607,
2.26017870133234));
#72632=CARTESIAN_POINT('Ctrl Pts',(1.91027492854846,-2.62599231814139,2.4181735923324));
#72633=CARTESIAN_POINT('Ctrl Pts',(3.24311081177889,0.16497767954115,2.57616848333245));
#72634=CARTESIAN_POINT('Ctrl Pts',(1.63393412158284,2.80628649337991,2.7341633743325));
#72635=CARTESIAN_POINT('Ctrl Pts',(-1.45747813791209,2.90185159477728,2.89215826533256));
#72636=CARTESIAN_POINT('Ctrl Pts',(-3.22672816390422,0.364980032144142,
3.05015315633261));
#72637=CARTESIAN_POINT('Ctrl Pts',(-2.06882739509817,-2.50298585443527,
3.20814804733266));
#72638=CARTESIAN_POINT('Ctrl Pts',(0.965825724890286,-3.10034929240489,
3.36614293833272));
#72639=CARTESIAN_POINT('Ctrl Pts',(3.1243227658749,-0.885207486870811,3.52413782933277));
#72640=CARTESIAN_POINT('Ctrl Pts',(2.44856686017853,2.13295695269892,3.68213272033283));
#72641=CARTESIAN_POINT('Ctrl Pts',(-0.448424924558006,3.21619342238995,
3.84012761133287));
#72642=CARTESIAN_POINT('Ctrl Pts',(-2.9386246603379,1.3818357877601,3.99812250233293));
#72643=CARTESIAN_POINT('Ctrl Pts',(-2.76302888818086,-1.70606459460131,
4.15611739333298));
#72644=CARTESIAN_POINT('Ctrl Pts',(-0.0809306368842651,-3.24629562294995,
4.31411228433304));
#72645=CARTESIAN_POINT('Ctrl Pts',(2.67458445172116,-1.84162511099097,4.47210717533309));
#72646=CARTESIAN_POINT('Ctrl Pts',(3.00383009796752,1.23368949956199,4.63010206633314));
#72647=CARTESIAN_POINT('Ctrl Pts',(0.608128632616327,3.18985338302612,4.7880969573332));
#72648=CARTESIAN_POINT('Ctrl Pts',(-2.33924130497153,2.25231772980782,4.94609184833325));
#72649=CARTESIAN_POINT('Ctrl Pts',(-3.16455086313379,-0.728424926493586,
5.10408673933331));
#72650=CARTESIAN_POINT('Ctrl Pts',(-1.11911425628133,-3.04837142099104,
5.26208163033336));
#72651=CARTESIAN_POINT('Ctrl Pts',(1.94153528232519,-2.60296480698359,5.42007652133342));
#72652=CARTESIAN_POINT('Ctrl Pts',(3.24090645725565,0.20374094882929,5.57807141233347));
#72653=CARTESIAN_POINT('Ctrl Pts',(1.60026491450814,2.82562156742707,5.73606630333352));
#72654=CARTESIAN_POINT('Ctrl Pts',(-1.49206900577688,2.8842182859333,5.89406119433358));
#72655=CARTESIAN_POINT('Ctrl Pts',(-3.23086128254485,0.326374649544494,
6.05205608533362));
#72656=CARTESIAN_POINT('Ctrl Pts',(-2.03875339757824,-2.52754220989012,
6.21005097633369));
#72657=CARTESIAN_POINT('Ctrl Pts',(1.00282499699587,-3.08858010488847,6.36804586733373));
#72658=CARTESIAN_POINT('Ctrl Pts',(3.1346831377893,-0.847789280760374,6.52604075833379));
#72659=CARTESIAN_POINT('Ctrl Pts',(2.42288984570632,2.16207997874408,6.68403564933384));
#72660=CARTESIAN_POINT('Ctrl Pts',(-0.486846229934527,3.21060209108997,
6.8420305403339));
#72661=CARTESIAN_POINT('Ctrl Pts',(-2.95493607899053,1.34660231991219,7.00002543133394));
#72662=CARTESIAN_POINT('Ctrl Pts',(-2.74243339421689,-1.73897789439567,
7.15802032233401));
#72663=CARTESIAN_POINT('Ctrl Pts',(-0.042111587625147,-3.24703120605584,
7.31601521333405));
#72664=CARTESIAN_POINT('Ctrl Pts',(2.69641206305327,-1.80951568800428,7.47401010433411));
#72665=CARTESIAN_POINT('Ctrl Pts',(2.98886518931682,1.26951562377266,7.63200499533417));
#72666=CARTESIAN_POINT('Ctrl Pts',(0.56994673361268,3.19689626978371,7.78999988633422));
#72667=CARTESIAN_POINT('Ctrl Pts',(-2.36600319687202,2.2241883713625,7.94799477733426));
#72668=CARTESIAN_POINT('Ctrl Pts',(-3.15561549601314,-0.766208770658805,
8.10598966833433));
#72669=CARTESIAN_POINT('Ctrl Pts',(-1.0825874157591,-3.06153385187112,8.26398455933438));
#72670=CARTESIAN_POINT('Ctrl Pts',(1.97251799758337,-2.57956542621475,8.42197945033443));
#72671=CARTESIAN_POINT('Ctrl Pts',(3.23823884360454,0.242475216637791,8.57997434133449));
#72672=CARTESIAN_POINT('Ctrl Pts',(1.566366917775,2.84455263931128,8.73796923233454));
#72673=CARTESIAN_POINT('Ctrl Pts',(-1.52644656238412,2.86617269736115,8.89596412333459));
#72674=CARTESIAN_POINT('Ctrl Pts',(-3.23453253946489,0.287722592188601,
9.05395901433465));
#72675=CARTESIAN_POINT('Ctrl Pts',(-2.0083879464276,-2.55173723089919,9.21195390533469));
#72676=CARTESIAN_POINT('Ctrl Pts',(1.0396809083576,-3.07636939389751,9.36994879633477));
#72677=CARTESIAN_POINT('Ctrl Pts',(3.14459539160713,-0.810249876270418,
9.5279436873348));
#72678=CARTESIAN_POINT('Ctrl Pts',(2.39686646622593,2.19089392303558,9.68593857833487));
#72679=CARTESIAN_POINT('Ctrl Pts',(-0.525197937892946,3.20455178846357,
9.8439334693349));
#72680=CARTESIAN_POINT('Ctrl Pts',(-2.97082507451666,1.31117634799362,10.001928360335));
#72681=CARTESIAN_POINT('Ctrl Pts',(-2.72144585527141,-1.77164259819448,
10.159923251335));
#72682=CARTESIAN_POINT('Ctrl Pts',(-0.00328651833606387,-3.24730260950622,
10.3179181423351));
#72683=CARTESIAN_POINT('Ctrl Pts',(2.71785420847995,-1.77714758542301,10.4759130333351));
#72684=CARTESIAN_POINT('Ctrl Pts',(2.97347300705285,1.30516026419214,10.6339079243352));
#72685=CARTESIAN_POINT('Ctrl Pts',(0.531683357813799,3.20348214384215,10.7919028153352));
#72686=CARTESIAN_POINT('Ctrl Pts',(-2.39242685650282,2.19574105378912,10.9498977063353));
#72687=CARTESIAN_POINT('Ctrl Pts',(-3.14622901745573,-0.803883081364814,
11.1078925973353));
#72688=CARTESIAN_POINT('Ctrl Pts',(-1.0459058138638,-3.07425862076485,11.2658874883354));
#72689=CARTESIAN_POINT('Ctrl Pts',(2.00321873137213,-2.55579728340303,11.4238823793354));
#72690=CARTESIAN_POINT('Ctrl Pts',(3.23510830694092,0.281174821482934,11.5818772703355));
#72691=CARTESIAN_POINT('Ctrl Pts',(1.5322450011872,2.86307706760007,11.7398721613356));
#72692=CARTESIAN_POINT('Ctrl Pts',(-1.56060590625239,2.84771737511982,11.8978670523356));
#72693=CARTESIAN_POINT('Ctrl Pts',(-3.23774140219028,0.2490294026297,12.0558619433357));
#72694=CARTESIAN_POINT('Ctrl Pts',(-1.97773538819436,-2.57556746649356,
12.2138568343357));
#72695=CARTESIAN_POINT('Ctrl Pts',(1.07638819633982,-3.06371890299285,12.3718517253358));
#72696=CARTESIAN_POINT('Ctrl Pts',(3.15405810111051,-0.772594636941618,
12.5298466163358));
#72697=CARTESIAN_POINT('Ctrl Pts',(2.37050045822502,2.21939465736754,12.6878415073359));
#72698=CARTESIAN_POINT('Ctrl Pts',(-0.563474596353531,3.19804339868417,
12.8458363983359));
#72699=CARTESIAN_POINT('Ctrl Pts',(-2.98628931759431,1.2755628985751,13.003831289336));
#72700=CARTESIAN_POINT('Ctrl Pts',(-2.70006938207651,-1.80405396377073,
13.161826180336));
#72701=CARTESIAN_POINT('Ctrl Pts',(0.0355392316804697,-3.24710993355476,
13.3198210713361));
#72702=CARTESIAN_POINT('Ctrl Pts',(2.73890741976546,-1.74452516462138,13.4778159623361));
#72703=CARTESIAN_POINT('Ctrl Pts',(2.95765652145599,1.3406178173039,13.6358108533362));
#72704=CARTESIAN_POINT('Ctrl Pts',(0.493342504231463,3.20961103420941,13.7938057443362));
#72705=CARTESIAN_POINT('Ctrl Pts',(-2.41850569611158,2.16697798953759,13.9518006353363));
#72706=CARTESIAN_POINT('Ctrl Pts',(-3.13639813875855,-0.841438930159867,
14.1097955263364));
#72707=CARTESIAN_POINT('Ctrl Pts',(-1.00906443556115,-3.08655067730993,
14.2677904173364));
#72708=CARTESIAN_POINT('Ctrl Pts',(2.03361349431715,-2.53165084404301,14.4257853083365));
#72709=CARTESIAN_POINT('Ctrl Pts',(3.23155274358889,0.319809522622996,14.5837801993365));
#72710=CARTESIAN_POINT('Ctrl Pts',(1.49783249263057,2.88123941244982,14.7417750903366));
#72711=CARTESIAN_POINT('Ctrl Pts',(-1.59440544683904,2.8287647573801,14.8997699813366));
#72712=CARTESIAN_POINT('Ctrl Pts',(-3.24074864036727,0.210472984148126,
15.0577648723367));
#72713=CARTESIAN_POINT('Ctrl Pts',(-1.94630068488002,-2.59935916099094,
15.2157597633367));
#72714=CARTESIAN_POINT('Ctrl Pts',(1.1119846044715,-3.04999779215944,15.3737546543368));
#72715=CARTESIAN_POINT('Ctrl Pts',(3.16492337134089,-0.73606266996359,15.5317495453368));
#72716=CARTESIAN_POINT('Ctrl Pts',(2.34003295606631,2.25015547162033,15.6897444363369));
#72717=CARTESIAN_POINT('Ctrl Pts',(0.384968583225142,2.87299014350137,15.7950743636703));
#72718=CARTESIAN_POINT('Ctrl Pts',(-0.50988368525085,2.70426773226927,15.847739327337));
#72719=CARTESIAN_POINT('Ctrl Pts',(-1.28892185405322,2.64462557919718,-2.77555756156289E-16));
#72720=CARTESIAN_POINT('Ctrl Pts',(-2.16403831185614,2.21811653527943,0.0526649636666843));
#72721=CARTESIAN_POINT('Ctrl Pts',(-3.44311483358514,0.436018596449888,
0.157994891000053));
#72722=CARTESIAN_POINT('Ctrl Pts',(-2.24436477004298,-2.65148082752247,
0.315989782000107));
#72723=CARTESIAN_POINT('Ctrl Pts',(0.99325262796079,-3.32545480540779,0.47398467300016));
#72724=CARTESIAN_POINT('Ctrl Pts',(3.32835797506399,-0.986820490209951,
0.631979564000214));
#72725=CARTESIAN_POINT('Ctrl Pts',(2.64488728032712,2.24914078759987,0.789974455000268));
#72726=CARTESIAN_POINT('Ctrl Pts',(-0.438314957393884,3.44366717194826,
0.947969346000321));
#72727=CARTESIAN_POINT('Ctrl Pts',(-3.12368605475517,1.51482555164407,1.10596423700038));
#72728=CARTESIAN_POINT('Ctrl Pts',(-2.97549193622185,-1.78850534874892,
1.26395912800043));
#72729=CARTESIAN_POINT('Ctrl Pts',(-0.128000241792142,-3.46922110496824,
1.42195401900048));
#72730=CARTESIAN_POINT('Ctrl Pts',(2.83557766746782,-2.00289002972017,1.57994891000054));
#72731=CARTESIAN_POINT('Ctrl Pts',(3.22685571589167,1.28042139796218,1.73794380100059));
#72732=CARTESIAN_POINT('Ctrl Pts',(0.690859017896064,3.40216610167957,1.89593869200064));
#72733=CARTESIAN_POINT('Ctrl Pts',(-2.47185131912304,2.43762212093852,2.0539335830007));
#72734=CARTESIAN_POINT('Ctrl Pts',(-3.39220536703243,-0.738235384598252,
2.21192847400075));
#72735=CARTESIAN_POINT('Ctrl Pts',(-1.23529356600166,-3.24439382779317,
2.3699233650008));
#72736=CARTESIAN_POINT('Ctrl Pts',(2.0422234829505,-2.80737767009854,2.52791825600086));
#72737=CARTESIAN_POINT('Ctrl Pts',(3.46712243282082,0.176373194395425,2.68591314700091));
#72738=CARTESIAN_POINT('Ctrl Pts',(1.74679496800295,3.00012531757514,2.84390803800096));
#72739=CARTESIAN_POINT('Ctrl Pts',(-1.55815062776997,3.10229139393809,3.00190292900102));
#72740=CARTESIAN_POINT('Ctrl Pts',(-3.44960818515806,0.390190323556838,
3.15989782000107));
#72741=CARTESIAN_POINT('Ctrl Pts',(-2.21172765516599,-2.67587477227939,
3.31789271100113));
#72742=CARTESIAN_POINT('Ctrl Pts',(1.03253827306805,-3.31449993698521,3.47588760200118));
#72743=CARTESIAN_POINT('Ctrl Pts',(3.34012933187316,-0.946351485827688,
3.63388249300123));
#72744=CARTESIAN_POINT('Ctrl Pts',(2.61769689100758,2.28028683820616,3.79187738400129));
#72745=CARTESIAN_POINT('Ctrl Pts',(-0.479399010889233,3.43834577670275,
3.94987227500134));
#72746=CARTESIAN_POINT('Ctrl Pts',(-3.14160448804072,1.4772834282495,4.1078671660014));
#72747=CARTESIAN_POINT('Ctrl Pts',(-2.95387977677187,-1.82390771425382,
4.26586205700145));
#72748=CARTESIAN_POINT('Ctrl Pts',(-0.0865207644539496,-3.47052722867774,
4.4238569480015));
#72749=CARTESIAN_POINT('Ctrl Pts',(2.85932621153631,-1.96883181171989,4.58185183900155));
#72750=CARTESIAN_POINT('Ctrl Pts',(3.21131386544667,1.31890422107427,4.73984673000161));
#72751=CARTESIAN_POINT('Ctrl Pts',(0.65013394439898,3.41018634994864,4.89784162100166));
#72752=CARTESIAN_POINT('Ctrl Pts',(-2.50081988404187,2.40789223066154,5.05583651200171));
#72753=CARTESIAN_POINT('Ctrl Pts',(-3.38313610732142,-0.77873947263813,
5.21383140300178));
#72754=CARTESIAN_POINT('Ctrl Pts',(-1.19641491396169,-3.25893179440594,
5.37182629400181));
#72755=CARTESIAN_POINT('Ctrl Pts',(2.07564308534076,-2.78275957804407,5.52982118500188));
#72756=CARTESIAN_POINT('Ctrl Pts',(3.46476581676266,0.217813961707557,5.68781607600192));
#72757=CARTESIAN_POINT('Ctrl Pts',(1.71080012542156,3.02079592455092,5.84581096700199));
#72758=CARTESIAN_POINT('Ctrl Pts',(-1.59513079308199,3.08344009831299,6.00380585800203));
#72759=CARTESIAN_POINT('Ctrl Pts',(-3.45402679099304,0.348918348651528,
6.1618007490021));
#72760=CARTESIAN_POINT('Ctrl Pts',(-2.17957635430163,-2.7021273106005,6.31979564000214));
#72761=CARTESIAN_POINT('Ctrl Pts',(1.07209319849625,-3.30191781555228,6.4777905310022));
#72762=CARTESIAN_POINT('Ctrl Pts',(3.35120532648497,-0.906348689336672,
6.63578542200224));
#72763=CARTESIAN_POINT('Ctrl Pts',(2.59024628631004,2.31142148107623,6.79378031300231));
#72764=CARTESIAN_POINT('Ctrl Pts',(-0.520474193792445,3.4323682349829,6.95177520400236));
#72765=CARTESIAN_POINT('Ctrl Pts',(-3.15904258646038,1.43961627660056,7.10977009500241));
#72766=CARTESIAN_POINT('Ctrl Pts',(-2.93186168880579,-1.85909443671817,
7.26776498600247));
#72767=CARTESIAN_POINT('Ctrl Pts',(-0.0450203642769841,-3.47131362076721,
7.42575987700253));
#72768=CARTESIAN_POINT('Ctrl Pts',(2.8826615230001,-1.93450449230244,7.58375476800256));
#72769=CARTESIAN_POINT('Ctrl Pts',(3.19531528460895,1.35720496568057,7.74174965900264));
#72770=CARTESIAN_POINT('Ctrl Pts',(0.609314704401862,3.41771571051825,7.89974455000267));
#72771=CARTESIAN_POINT('Ctrl Pts',(-2.52943030198254,2.37781989106326,8.05773944100274));
#72772=CARTESIAN_POINT('Ctrl Pts',(-3.37358354695964,-0.819133162926983,
8.21573433200278));
#72773=CARTESIAN_POINT('Ctrl Pts',(-1.15736505241679,-3.27300339479932,
8.37372922300284));
#72774=CARTESIAN_POINT('Ctrl Pts',(2.10876587186757,-2.75774393020277,8.53172411400289));
#72775=CARTESIAN_POINT('Ctrl Pts',(3.46191394284634,0.259223724318805,8.68971900500295));
#72776=CARTESIAN_POINT('Ctrl Pts',(1.67456068997757,3.04103462369395,8.847713896003));
#72777=CARTESIAN_POINT('Ctrl Pts',(-1.63188291307296,3.06414804553306,9.00570878700305));
#72778=CARTESIAN_POINT('Ctrl Pts',(-3.45795163290035,0.307596475021262,
9.16370367800311));
#72779=CARTESIAN_POINT('Ctrl Pts',(-2.14711346820945,-2.72799355599627,
9.32169856900316));
#72780=CARTESIAN_POINT('Ctrl Pts',(1.11149486081386,-3.28886367326282,9.47969346000322));
#72781=CARTESIAN_POINT('Ctrl Pts',(3.36180225010744,-0.866216322921951,
9.63768835100326));
#72782=CARTESIAN_POINT('Ctrl Pts',(2.56242539210976,2.34222569296695,9.79568324200333));
#72783=CARTESIAN_POINT('Ctrl Pts',(-0.561474971970195,3.42590001937795,
9.95367813300337));
#72784=CARTESIAN_POINT('Ctrl Pts',(-3.17602908369125,1.40174332403378,10.1116730240034));
#72785=CARTESIAN_POINT('Ctrl Pts',(-2.90942447610763,-1.8940153918983,10.2696679150035));
#72786=CARTESIAN_POINT('Ctrl Pts',(-0.0035135282481055,-3.47160377088719,
10.4276628060035));
#72787=CARTESIAN_POINT('Ctrl Pts',(2.90558474324488,-1.89990062549661,10.5856576970036));
#72788=CARTESIAN_POINT('Ctrl Pts',(3.17885991705762,1.39531169085301,10.7436525880036));
#72789=CARTESIAN_POINT('Ctrl Pts',(0.568408359757113,3.4247564911184,10.9016474790037));
#72790=CARTESIAN_POINT('Ctrl Pts',(-2.55767912491219,2.34740762992373,11.0596423700038));
#72791=CARTESIAN_POINT('Ctrl Pts',(-3.36354871550911,-0.859409753944302,
11.2176372610038));
#72792=CARTESIAN_POINT('Ctrl Pts',(-1.11814973965565,-3.2866071025492,11.3756321520039));
#72793=CARTESIAN_POINT('Ctrl Pts',(2.14158719959911,-2.73233404879208,11.5336270430039));
#72794=CARTESIAN_POINT('Ctrl Pts',(3.45856717040372,0.300596429689395,11.691621934004));
#72795=CARTESIAN_POINT('Ctrl Pts',(1.63808186784707,3.0608385911199,11.849616825004));
#72796=CARTESIAN_POINT('Ctrl Pts',(-1.66840174770112,3.04441795752144,12.0076117160041));
#72797=CARTESIAN_POINT('Ctrl Pts',(-3.46138214162631,0.266230628060431,
12.1656066070041));
#72798=CARTESIAN_POINT('Ctrl Pts',(-2.11434364366697,-2.75346981912873,
12.3236014980042));
#72799=CARTESIAN_POINT('Ctrl Pts',(1.15073763387882,-3.27533937411076,12.4815963890042));
#72800=CARTESIAN_POINT('Ctrl Pts',(3.37191857800943,-0.825960120600417,
12.6395912800043));
#72801=CARTESIAN_POINT('Ctrl Pts',(2.53423820298509,2.37269506052457,12.7975861710043));
#72802=CARTESIAN_POINT('Ctrl Pts',(-0.602395516750883,3.41894207513388,
12.9555810620044));
#72803=CARTESIAN_POINT('Ctrl Pts',(-3.19256148951789,1.3636699443205,13.1135759530045));
#72804=CARTESIAN_POINT('Ctrl Pts',(-2.8865714642773,-1.928665510007,13.2715708440045));
#72805=CARTESIAN_POINT('Ctrl Pts',(0.0379940355281645,-3.4713977862162,
13.4295657350046));
#72806=CARTESIAN_POINT('Ctrl Pts',(2.92809216447323,-1.8650248739301,13.5875606260046));
#72807=CARTESIAN_POINT('Ctrl Pts',(3.16195093823948,1.43321840602296,13.7455555170047));
#72808=CARTESIAN_POINT('Ctrl Pts',(0.527419185700519,3.43130872276077,13.9035504080047));
#72809=CARTESIAN_POINT('Ctrl Pts',(-2.58555931004217,2.31665781251357,14.0615452990048));
#72810=CARTESIAN_POINT('Ctrl Pts',(-3.35303878783672,-0.89955970052277,
14.2195401900048));
#72811=CARTESIAN_POINT('Ctrl Pts',(-1.07876361424012,-3.29974820917995,
14.3775350810049));
#72812=CARTESIAN_POINT('Ctrl Pts',(2.1740814221413,-2.70651974072904,14.5355299720049));
#72813=CARTESIAN_POINT('Ctrl Pts',(3.45476601337439,0.341899748256715,14.693524863005));
#72814=CARTESIAN_POINT('Ctrl Pts',(1.60129238166824,3.08025546489199,14.851519754005));
#72815=CARTESIAN_POINT('Ctrl Pts',(-1.70453592633028,3.02415622428451,15.0095146450051));
#72816=CARTESIAN_POINT('Ctrl Pts',(-3.46459709897726,0.225010999375169,
15.1675095360052));
#72817=CARTESIAN_POINT('Ctrl Pts',(-2.08073764888123,-2.77890487901232,
15.3255044270052));
#72818=CARTESIAN_POINT('Ctrl Pts',(1.18879279521126,-3.26067050402438,15.4834993180053));
#72819=CARTESIAN_POINT('Ctrl Pts',(3.38353434581409,-0.786904778499691,
15.6414942090053));
#72820=CARTESIAN_POINT('Ctrl Pts',(2.50166621690838,2.40558061866225,15.7994891000054));
#72821=CARTESIAN_POINT('Ctrl Pts',(0.411559545231536,3.07143639360967,15.9048190273387));
#72822=CARTESIAN_POINT('Ctrl Pts',(-0.545102916879006,2.891059807408,15.9574839910054));
#72823=CARTESIAN_POINT('Ctrl Pts',(-2.94111188951679,-0.00259486169482749,
14.1778238829104));
#72824=CARTESIAN_POINT('Ctrl Pts',(-2.94335307565858,-0.259762554464039,
14.1917293186085));
#72825=CARTESIAN_POINT('Ctrl Pts',(-2.91238767988341,-0.516399492336486,
14.2056347543067));
#72826=CARTESIAN_POINT('Ctrl Pts',(-2.84607967927153,-0.763554866459577,
14.2195401900048));
#72827=CARTESIAN_POINT('Ctrl Pts',(-2.59494706330453,-1.69962253674182,
14.2722051536715));
#72828=CARTESIAN_POINT('Ctrl Pts',(-1.83685533877235,-2.49968537296086,
14.3248701173382));
#72829=CARTESIAN_POINT('Ctrl Pts',(-0.915668637109368,-2.80084537966192,
14.3775350810049));
#72830=CARTESIAN_POINT('Ctrl Pts',(0.00551806455364026,-3.10200538636298,
14.4302000446716));
#72831=CARTESIAN_POINT('Ctrl Pts',(1.0897997433475,-2.90426256354601,14.4828650083382));
#72832=CARTESIAN_POINT('Ctrl Pts',(1.84538801461659,-2.29732123730656,14.5355299720049));
#72833=CARTESIAN_POINT('Ctrl Pts',(2.60097628588567,-1.6903799110671,14.5881949356716));
#72834=CARTESIAN_POINT('Ctrl Pts',(3.02787114963004,-0.674240081405173,
14.6408598993383));
#72835=CARTESIAN_POINT('Ctrl Pts',(2.93240630955118,0.29022245286501,14.693524863005));
#72836=CARTESIAN_POINT('Ctrl Pts',(2.83694146947232,1.25468498713517,14.7461898266717));
#72837=CARTESIAN_POINT('Ctrl Pts',(2.21911692557029,2.16747022601356,14.7988547903384));
#72838=CARTESIAN_POINT('Ctrl Pts',(1.35923326895286,2.61451297201819,14.851519754005));
#72839=CARTESIAN_POINT('Ctrl Pts',(0.499349612335403,3.06155571802283,14.9041847176717));
#72840=CARTESIAN_POINT('Ctrl Pts',(-0.602593156997484,3.04285597115367,
14.9568496813384));
#72841=CARTESIAN_POINT('Ctrl Pts',(-1.4469080704384,2.56698189356751,15.0095146450051));
#72842=CARTESIAN_POINT('Ctrl Pts',(-1.70601080500511,2.42094600950443,15.0256764300034));
#72843=CARTESIAN_POINT('Ctrl Pts',(-1.94085146734146,2.2318557880317,15.0418382150017));
#72844=CARTESIAN_POINT('Ctrl Pts',(-2.14373220034761,2.01193738948431,15.058));
#72845=CARTESIAN_POINT('Ctrl Pts',(-1.37994859234592,-1.93347131995891,
-1.83880688453542E-16));
#72846=CARTESIAN_POINT('Ctrl Pts',(-1.43831895271373,-1.90176082500493,
-1.96503831907269E-16));
#72847=CARTESIAN_POINT('Ctrl Pts',(-1.49514575458196,-1.86752259046863,
-3.60259795903682E-17));
#72848=CARTESIAN_POINT('Ctrl Pts',(-1.55024291463987,-1.83079524515745,
-1.11022302462516E-16));
#72849=CARTESIAN_POINT('Ctrl Pts',(-1.61820139003649,-1.78549464545158,
-1.89647209120044E-16));
#72850=CARTESIAN_POINT('Ctrl Pts',(-1.68352982136479,-1.73640902813589,
4.37133882625492E-17));
#72851=CARTESIAN_POINT('Ctrl Pts',(-1.74614398662112,-1.68389593204229,
2.08166817117217E-17));
#72852=CARTESIAN_POINT('Ctrl Pts',(-1.78291149355231,-1.65305984859862,
7.3715640875763E-18));
#72853=CARTESIAN_POINT('Ctrl Pts',(-1.81874277362574,-1.62104095184393,
-1.13501056944751E-16));
#72854=CARTESIAN_POINT('Ctrl Pts',(-1.85361742493061,-1.58790418430478,
-1.38777878078145E-16));
#72855=CARTESIAN_POINT('Ctrl Pts',(-1.86599100473682,-1.57614720832583,
-1.47746133009421E-16));
#72856=CARTESIAN_POINT('Ctrl Pts',(-1.87824533378606,-1.56424827137885,
6.18933070998169E-17));
#72857=CARTESIAN_POINT('Ctrl Pts',(-1.89037564784625,-1.55221386701801,
6.93889390390723E-18));
#72858=CARTESIAN_POINT('Ctrl Pts',(-1.9520612058093,-1.49101603289205,-2.72517484859507E-16));
#72859=CARTESIAN_POINT('Ctrl Pts',(-2.01038866542646,-1.42647262579372,
-5.93465220813464E-16));
#72860=CARTESIAN_POINT('Ctrl Pts',(-2.06526482907838,-1.35900295762991,
-3.95516952522712E-16));
#72861=CARTESIAN_POINT('Ctrl Pts',(-2.11328147227381,-1.29996699798658,
-2.22312217768304E-16));
#72862=CARTESIAN_POINT('Ctrl Pts',(-2.15865566139155,-1.2386893890933,-3.33360010116584E-16));
#72863=CARTESIAN_POINT('Ctrl Pts',(-2.20130818996771,-1.17541961668097,
-3.46944695195361E-16));
#72864=CARTESIAN_POINT('Ctrl Pts',(-2.22006840714514,-1.1475911452903,-3.52919760469855E-16));
#72865=CARTESIAN_POINT('Ctrl Pts',(-2.23830186692143,-1.11937693173939,
-3.24730293914024E-16));
#72866=CARTESIAN_POINT('Ctrl Pts',(-2.25600064404541,-1.09079672684346,
-3.05311331771918E-16));
#72867=CARTESIAN_POINT('Ctrl Pts',(-2.26668277274188,-1.07354709288677,
-2.93590982320615E-16));
#72868=CARTESIAN_POINT('Ctrl Pts',(-2.27717011522814,-1.05616412126237,
7.72460434588031E-17));
#72869=CARTESIAN_POINT('Ctrl Pts',(-2.28746078556243,-1.03865201740679,
1.38777878078145E-16));
#72870=CARTESIAN_POINT('Ctrl Pts',(-2.2952947631346,-1.02532057986291,1.85620211640871E-16));
#72871=CARTESIAN_POINT('Ctrl Pts',(-2.30301001735291,-1.01192234024488,
-2.74638834286083E-16));
#72872=CARTESIAN_POINT('Ctrl Pts',(-2.31060459934883,-0.99846213025753,
-2.77555756156289E-16));
#72873=CARTESIAN_POINT('Ctrl Pts',(-2.35418081118604,-0.921230103254969,
-2.94292477860916E-16));
#72874=CARTESIAN_POINT('Ctrl Pts',(-2.39380271969424,-0.841933889485626,
-3.78845217127159E-17));
#72875=CARTESIAN_POINT('Ctrl Pts',(-2.42937389319446,-0.760969916140703,
-6.93889390390723E-17));
#72876=CARTESIAN_POINT('Ctrl Pts',(-2.46720610926394,-0.674859556767564,
-1.02895900045749E-16));
#72877=CARTESIAN_POINT('Ctrl Pts',(-2.5004573035107,-0.586862180324133,
-9.42383278312778E-17));
#72878=CARTESIAN_POINT('Ctrl Pts',(-2.52897137574918,-0.497406668002497,
0.));
#72879=CARTESIAN_POINT('Ctrl Pts',(-2.55035692992803,-0.430315033761271,
7.06787458734584E-17));
#72880=CARTESIAN_POINT('Ctrl Pts',(-2.56907707912655,-0.362402071614612,
2.24154037051898E-16));
#72881=CARTESIAN_POINT('Ctrl Pts',(-2.58504714386116,-0.293835873442853,
2.77555756156289E-16));
#72882=CARTESIAN_POINT('Ctrl Pts',(-2.59702469241211,-0.242411224814034,
3.17607045484582E-16));
#72883=CARTESIAN_POINT('Ctrl Pts',(-2.60745499960513,-0.1906188874626,1.72939271916983E-16));
#72884=CARTESIAN_POINT('Ctrl Pts',(-2.61629539664834,-0.138527206391925,
1.38777878078145E-16));
#72885=CARTESIAN_POINT('Ctrl Pts',(-2.61869711284596,-0.124375191094725,
1.29497076264031E-16));
#72886=CARTESIAN_POINT('Ctrl Pts',(-2.62098183196127,-0.110198515695441,
1.70346493820844E-17));
#72887=CARTESIAN_POINT('Ctrl Pts',(-2.62314735205575,-0.0960068887486099,
2.77555756156289E-17));
#72888=CARTESIAN_POINT('Ctrl Pts',(-2.63712677206149,-0.00439346333649258,
9.69640447732094E-17));
#72889=CARTESIAN_POINT('Ctrl Pts',(-2.64610759043344,0.0876011416361361,
-2.12521409618605E-16));
#72890=CARTESIAN_POINT('Ctrl Pts',(-2.64996359474771,0.179577964648124,
-5.55111512312578E-17));
#72891=CARTESIAN_POINT('Ctrl Pts',(-2.65210628483955,0.230687302523444,
3.17357233945851E-17));
#72892=CARTESIAN_POINT('Ctrl Pts',(-2.65266584064783,0.281791760322423,
2.25858622101648E-16));
#72893=CARTESIAN_POINT('Ctrl Pts',(-2.65161463128253,0.332826444242184,
1.94289029309402E-16));
#72894=CARTESIAN_POINT('Ctrl Pts',(-2.64978728963931,0.421541220055518,
1.40408657934648E-16));
#72895=CARTESIAN_POINT('Ctrl Pts',(-2.6430958113368,0.510044886368098,1.72520161624302E-16));
#72896=CARTESIAN_POINT('Ctrl Pts',(-2.63178393076928,0.598076371345786,
1.66533453693773E-16));
#72897=CARTESIAN_POINT('Ctrl Pts',(-2.62024798910265,0.687851547937211,
1.60428163503557E-16));
#72898=CARTESIAN_POINT('Ctrl Pts',(-2.60390669120625,0.777136386959749,
-1.34425914858345E-16));
#72899=CARTESIAN_POINT('Ctrl Pts',(-2.58296460883121,0.865656938831555,
-1.11022302462516E-16));
#72900=CARTESIAN_POINT('Ctrl Pts',(-2.57869408333521,0.883708117645516,
-1.06249819877211E-16));
#72901=CARTESIAN_POINT('Ctrl Pts',(-2.57423206760738,0.901727502426255,
-4.70036822748448E-17));
#72902=CARTESIAN_POINT('Ctrl Pts',(-2.56958003501042,0.919712740461561,
-5.55111512312578E-17));
#72903=CARTESIAN_POINT('Ctrl Pts',(-2.56604635272843,0.933374320783267,
-6.19734215806574E-17));
#72904=CARTESIAN_POINT('Ctrl Pts',(-2.56240532303519,0.947007284078113,
8.26362614469453E-17));
#72905=CARTESIAN_POINT('Ctrl Pts',(-2.5586586911495,0.960608258314244,8.32667268468867E-17));
#72906=CARTESIAN_POINT('Ctrl Pts',(-2.53407091484386,1.04986648337083,8.74042409382574E-17));
#72907=CARTESIAN_POINT('Ctrl Pts',(-2.504930952964,1.13777933274063,7.81122475311754E-16));
#72908=CARTESIAN_POINT('Ctrl Pts',(-2.47152838793823,1.2240648243653,6.38378239159465E-16));
#72909=CARTESIAN_POINT('Ctrl Pts',(-2.43748524526305,1.31200505589874,4.92896525595146E-16));
#72910=CARTESIAN_POINT('Ctrl Pts',(-2.39901427145562,1.39825569878996,-4.49689980744232E-17));
#72911=CARTESIAN_POINT('Ctrl Pts',(-2.35636659634517,1.48252101187545,-5.55111512312578E-17));
#72912=CARTESIAN_POINT('Ctrl Pts',(-2.31336109209446,1.56749334086406,-6.61417567970626E-17));
#72913=CARTESIAN_POINT('Ctrl Pts',(-2.26610821171127,1.65044775809861,-5.44480906746773E-17));
#72914=CARTESIAN_POINT('Ctrl Pts',(-2.21481327415801,1.731071203515,-5.55111512312578E-17));
#72915=CARTESIAN_POINT('Ctrl Pts',(-2.18401751630642,1.77947481253834,-5.61493770883036E-17));
#72916=CARTESIAN_POINT('Ctrl Pts',(-2.15176385823466,1.82703799978858,3.67516605336294E-16));
#72917=CARTESIAN_POINT('Ctrl Pts',(-2.11808850376184,1.87368930169054,3.88578058618805E-16));
#72918=CARTESIAN_POINT('Ctrl Pts',(-2.1089145366433,1.88639822536441,3.94315699184355E-16));
#72919=CARTESIAN_POINT('Ctrl Pts',(-2.09963412322397,1.89904053530927,1.84615714870052E-16));
#72920=CARTESIAN_POINT('Ctrl Pts',(-2.09025911328956,1.91160012317952,1.66533453693773E-16));
#72921=CARTESIAN_POINT('Ctrl Pts',(-2.03145402967869,1.99038058527982,5.31118266465956E-17));
#72922=CARTESIAN_POINT('Ctrl Pts',(-1.96883756375661,2.06603912302101,4.62847422951145E-16));
#72923=CARTESIAN_POINT('Ctrl Pts',(-1.90268196527442,2.13826743811961,3.33066907387547E-16));
#72924=CARTESIAN_POINT('Ctrl Pts',(-1.83635976195865,2.21067765145044,2.0295955537029E-16));
#72925=CARTESIAN_POINT('Ctrl Pts',(-1.76648017672323,2.2796412428746,3.28001727774597E-18));
#72926=CARTESIAN_POINT('Ctrl Pts',(-1.6932675195623,2.34483179093341,0.));
#72927=CARTESIAN_POINT('Ctrl Pts',(-1.62146081066126,2.40877044429043,-3.21702906282713E-18));
#72928=CARTESIAN_POINT('Ctrl Pts',(-1.54644728359632,2.46908034426641,-8.3280583097932E-18));
#72929=CARTESIAN_POINT('Ctrl Pts',(-1.46839770082455,2.52542611967769,-5.55111512312578E-17));
#72930=CARTESIAN_POINT('Ctrl Pts',(-1.41023968234018,2.56741172077267,-9.06692532072844E-17));
#72931=CARTESIAN_POINT('Ctrl Pts',(-1.35039506896231,2.60719581243537,-1.11866688105539E-17));
#72932=CARTESIAN_POINT('Ctrl Pts',(-1.28892185405323,2.64462557919718,0.));
#72933=CARTESIAN_POINT('Origin',(0.,0.,0.));
#72934=CARTESIAN_POINT('Origin',(-1.44337567297407,-2.5,-6.));
#72935=CARTESIAN_POINT('',(-1.44337567297407,-2.5,-6.));
#72936=CARTESIAN_POINT('',(1.44337567297406,-2.5,-6.));
#72937=CARTESIAN_POINT('',(-0.721687836487033,-2.5,-6.));
#72938=CARTESIAN_POINT('',(-1.44337567297407,-2.5,-3.));
#72939=CARTESIAN_POINT('',(-1.44337567297407,-2.5,-6.));
#72940=CARTESIAN_POINT('',(1.44337567297406,-2.5,-3.));
#72941=CARTESIAN_POINT('',(-1.44337567297407,-2.5,-3.));
#72942=CARTESIAN_POINT('',(1.44337567297406,-2.5,-6.));
#72943=CARTESIAN_POINT('Origin',(-2.88675134594813,3.53525079574969E-16,
-6.));
#72944=CARTESIAN_POINT('',(-2.88675134594813,3.53525079574969E-16,-6.));
#72945=CARTESIAN_POINT('',(-2.52590742770461,-0.625,-6.));
#72946=CARTESIAN_POINT('',(-2.88675134594813,5.55111512312578E-16,-3.));
#72947=CARTESIAN_POINT('',(-2.88675134594813,3.53525079574969E-16,-6.));
#72948=CARTESIAN_POINT('',(-2.88675134594813,3.53525079574969E-16,-3.));
#72949=CARTESIAN_POINT('Origin',(-1.44337567297406,2.5,-6.));
#72950=CARTESIAN_POINT('',(-1.44337567297406,2.5,-6.));
#72951=CARTESIAN_POINT('',(-1.80421959121758,1.875,-6.));
#72952=CARTESIAN_POINT('',(-1.44337567297406,2.5,-3.));
#72953=CARTESIAN_POINT('',(-1.44337567297406,2.5,-6.));
#72954=CARTESIAN_POINT('',(-1.44337567297406,2.5,-3.));
#72955=CARTESIAN_POINT('Origin',(1.44337567297406,2.5,-6.));
#72956=CARTESIAN_POINT('',(1.44337567297406,2.5,-6.));
#72957=CARTESIAN_POINT('',(0.721687836487033,2.5,-6.));
#72958=CARTESIAN_POINT('',(1.44337567297406,2.5,-3.));
#72959=CARTESIAN_POINT('',(1.44337567297406,2.5,-6.));
#72960=CARTESIAN_POINT('',(1.44337567297406,2.5,-3.));
#72961=CARTESIAN_POINT('Origin',(2.88675134594813,0.,-6.));
#72962=CARTESIAN_POINT('',(2.88675134594813,0.,-6.));
#72963=CARTESIAN_POINT('',(2.52590742770461,0.625,-6.));
#72964=CARTESIAN_POINT('',(2.88675134594813,0.,-3.));
#72965=CARTESIAN_POINT('',(2.88675134594813,0.,-6.));
#72966=CARTESIAN_POINT('',(2.88675134594813,0.,-3.));
#72967=CARTESIAN_POINT('Origin',(1.44337567297406,-2.5,-6.));
#72968=CARTESIAN_POINT('',(1.80421959121758,-1.875,-6.));
#72969=CARTESIAN_POINT('',(1.44337567297406,-2.5,-3.));
#72970=CARTESIAN_POINT('Origin',(0.,0.,-3.));
#72971=CARTESIAN_POINT('Origin',(0.,0.,0.));
#72972=CARTESIAN_POINT('',(-5.,-6.12323399573677E-16,0.));
#72973=CARTESIAN_POINT('Origin',(0.,0.,0.));
#72974=CARTESIAN_POINT('Origin',(0.,0.,-6.));
#72975=CARTESIAN_POINT('',(-5.,-6.12323399573677E-16,-6.));
#72976=CARTESIAN_POINT('',(-5.,-6.12323399573677E-16,-6.));
#72977=CARTESIAN_POINT('Origin',(0.,0.,-6.));
#72978=CARTESIAN_POINT('Origin',(0.,0.,-6.));
#72979=CARTESIAN_POINT('Origin',(0.,0.,16.));
#72980=CARTESIAN_POINT('',(0.,0.,0.));
#72981=CARTESIAN_POINT('Origin',(160.,225.,10.));
#72982=CARTESIAN_POINT('',(157.486483939918,225.000575042283,0.387416697507991));
#72983=CARTESIAN_POINT('',(157.48459726363,224.996259956084,0.112583302491957));
#72984=CARTESIAN_POINT('',(157.4825,225.,10.));
#72985=CARTESIAN_POINT('',(158.086534003335,226.635987203375,0.));
#72986=CARTESIAN_POINT('Ctrl Pts',(157.48459726363,224.996259956084,0.112583302491957));
#72987=CARTESIAN_POINT('Ctrl Pts',(157.489762449105,225.588952407467,0.0750555349946362));
#72988=CARTESIAN_POINT('Ctrl Pts',(157.700778171916,226.184803560304,0.0375277674973158));
#72989=CARTESIAN_POINT('Ctrl Pts',(158.086534003335,226.635987203375,-4.09394740330526E-15));
#72990=CARTESIAN_POINT('',(161.917152715742,226.638755029745,8.50380292826545E-15));
#72991=CARTESIAN_POINT('Origin',(160.,225.,0.));
#72992=CARTESIAN_POINT('Ctrl Pts',(161.917156415839,226.638757807614,5.95993938154068E-15));
#72993=CARTESIAN_POINT('Ctrl Pts',(161.386618674923,227.257451018951,0.0517556153419846));
#72994=CARTESIAN_POINT('Ctrl Pts',(160.527623995925,227.597124544241,0.103511230683961));
#72995=CARTESIAN_POINT('Ctrl Pts',(159.717628701157,227.505772300943,0.15526684602594));
#72996=CARTESIAN_POINT('Ctrl Pts',(158.889421475104,227.412366094136,0.208186134436534));
#72997=CARTESIAN_POINT('Ctrl Pts',(158.112441807901,226.868333858592,0.261105422847131));
#72998=CARTESIAN_POINT('Ctrl Pts',(157.741727721422,226.12214743685,0.314024711257726));
#72999=CARTESIAN_POINT('Ctrl Pts',(157.570350743671,225.77719379613,0.338488706674481));
#73000=CARTESIAN_POINT('Ctrl Pts',(157.485797170545,225.389037591527,0.362952702091236));
#73001=CARTESIAN_POINT('Ctrl Pts',(157.486483939918,225.000575042283,0.387416697507991));
#73002=CARTESIAN_POINT('Origin',(160.,225.,10.));
#73003=CARTESIAN_POINT('',(157.482539767498,224.997698761652,1.38741669750799));
#73004=CARTESIAN_POINT('',(157.478271555719,225.000135319788,1.11258330249196));
#73005=CARTESIAN_POINT('',(157.4825,225.,10.));
#73006=CARTESIAN_POINT('Ctrl Pts',(157.478271555719,225.000135319788,1.11258330249196));
#73007=CARTESIAN_POINT('Ctrl Pts',(157.478266683081,225.006844587079,1.11215722053548));
#73008=CARTESIAN_POINT('Ctrl Pts',(157.478291126166,225.013553815972,1.11173113857901));
#73009=CARTESIAN_POINT('Ctrl Pts',(157.478344991774,225.020262806545,1.11130505662253));
#73010=CARTESIAN_POINT('Ctrl Pts',(157.485035088855,225.85351800941,1.05838576821194));
#73011=CARTESIAN_POINT('Ctrl Pts',(157.945584889413,226.683097001022,1.00546647980134));
#73012=CARTESIAN_POINT('Ctrl Pts',(158.649263586559,227.129460441397,0.952547191390747));
#73013=CARTESIAN_POINT('Ctrl Pts',(159.352942283705,227.575823881771,0.899627902980148));
#73014=CARTESIAN_POINT('Ctrl Pts',(160.299749877437,227.638971770909,0.84670861456955));
#73015=CARTESIAN_POINT('Ctrl Pts',(161.056392441986,227.289849947809,0.793789326158952));
#73016=CARTESIAN_POINT('Ctrl Pts',(161.813035006535,226.940728124708,0.740870037748355));
#73017=CARTESIAN_POINT('Ctrl Pts',(162.3795125419,226.179336589369,0.687950749337759));
#73018=CARTESIAN_POINT('Ctrl Pts',(162.496677259461,225.354415175787,0.635031460927162));
#73019=CARTESIAN_POINT('Ctrl Pts',(162.613841977023,224.529493762204,0.582112172516563));
#73020=CARTESIAN_POINT('Ctrl Pts',(162.281693876781,223.641042470379,0.529192884105964));
#73021=CARTESIAN_POINT('Ctrl Pts',(161.65207595311,223.09493528623,0.476273595695365));
#73022=CARTESIAN_POINT('Ctrl Pts',(161.022458029439,222.548828102082,0.423354307284768));
#73023=CARTESIAN_POINT('Ctrl Pts',(160.09537028234,222.34506502561,0.370435018874173));
#73024=CARTESIAN_POINT('Ctrl Pts',(159.295373479341,222.578292580861,0.317515730463577));
#73025=CARTESIAN_POINT('Ctrl Pts',(158.495376676342,222.811520136111,0.264596442052982));
#73026=CARTESIAN_POINT('Ctrl Pts',(157.822470817444,223.481738323085,0.211677153642386));
#73027=CARTESIAN_POINT('Ctrl Pts',(157.584268019495,224.278797417901,0.158757865231791));
#73028=CARTESIAN_POINT('Ctrl Pts',(157.514986979324,224.510621240471,0.143366344318513));
#73029=CARTESIAN_POINT('Ctrl Pts',(157.482478830652,224.753174932141,0.127974823405235));
#73030=CARTESIAN_POINT('Ctrl Pts',(157.48459726363,224.996259956084,0.112583302491957));
#73031=CARTESIAN_POINT('Ctrl Pts',(157.486483939918,225.000575042283,0.387416697507991));
#73032=CARTESIAN_POINT('Ctrl Pts',(157.487282755622,224.548734880137,0.415871990501833));
#73033=CARTESIAN_POINT('Ctrl Pts',(157.603404731867,224.096480258932,0.444327283495675));
#73034=CARTESIAN_POINT('Ctrl Pts',(157.832358689369,223.711314639842,0.472782576489517));
#73035=CARTESIAN_POINT('Ctrl Pts',(158.258152249548,222.995008872516,0.525701864900114));
#73036=CARTESIAN_POINT('Ctrl Pts',(159.07418787566,222.510737945805,0.578621153310711));
#73037=CARTESIAN_POINT('Ctrl Pts',(159.906929713407,222.479994087708,0.631540441721308));
#73038=CARTESIAN_POINT('Ctrl Pts',(160.739671551153,222.449250229612,0.684459730131907));
#73039=CARTESIAN_POINT('Ctrl Pts',(161.589119600533,222.872033440131,0.737379018542505));
#73040=CARTESIAN_POINT('Ctrl Pts',(162.066623300567,223.5549311968,0.790298306953104));
#73041=CARTESIAN_POINT('Ctrl Pts',(162.544127000601,224.237828953469,0.843217595363701));
#73042=CARTESIAN_POINT('Ctrl Pts',(162.649686351289,225.180841256288,0.896136883774297));
#73043=CARTESIAN_POINT('Ctrl Pts',(162.334970000144,225.952420120802,0.949056172184893));
#73044=CARTESIAN_POINT('Ctrl Pts',(162.020253649,226.723998985317,1.00197546059549));
#73045=CARTESIAN_POINT('Ctrl Pts',(161.285261596023,227.324144411527,1.05489474900609));
#73046=CARTESIAN_POINT('Ctrl Pts',(160.466339392169,227.478242187855,1.10781403741669));
#73047=CARTESIAN_POINT('Ctrl Pts',(159.647417188314,227.632339964183,1.16073332582729));
#73048=CARTESIAN_POINT('Ctrl Pts',(158.744564833583,227.34039009063,1.21365261423788));
#73049=CARTESIAN_POINT('Ctrl Pts',(158.170921185734,226.735982884831,1.26657190264848));
#73050=CARTESIAN_POINT('Ctrl Pts',(157.734269755296,226.275914561981,1.30685350093498));
#73051=CARTESIAN_POINT('Ctrl Pts',(157.488364882719,225.634805582068,1.34713509922148));
#73052=CARTESIAN_POINT('Ctrl Pts',(157.482539767498,224.997698761652,1.38741669750799));
#73053=CARTESIAN_POINT('Origin',(160.,225.,10.));
#73054=CARTESIAN_POINT('',(157.478659078657,225.000905528694,2.38741669750799));
#73055=CARTESIAN_POINT('',(157.484174776371,225.002114825273,2.11258330249196));
#73056=CARTESIAN_POINT('',(157.4825,225.,10.));
#73057=CARTESIAN_POINT('Ctrl Pts',(157.484174776371,225.002114825273,2.11258330249196));
#73058=CARTESIAN_POINT('Ctrl Pts',(157.48212567403,225.259454343706,2.09633961766574));
#73059=CARTESIAN_POINT('Ctrl Pts',(157.518448799924,225.516229216226,2.08009593283951));
#73060=CARTESIAN_POINT('Ctrl Pts',(157.59554743232,225.760113789415,2.06385224801329));
#73061=CARTESIAN_POINT('Ctrl Pts',(157.846722261643,226.554650140346,2.0109329596027));
#73062=CARTESIAN_POINT('Ctrl Pts',(158.530668186833,227.212375217892,1.9580136711921));
#73063=CARTESIAN_POINT('Ctrl Pts',(159.334411776144,227.432314991755,1.9050943827815));
#73064=CARTESIAN_POINT('Ctrl Pts',(160.138155365455,227.652254765619,1.8521750943709));
#73065=CARTESIAN_POINT('Ctrl Pts',(161.061696618887,227.4344092358,1.7992558059603));
#73066=CARTESIAN_POINT('Ctrl Pts',(161.682422640936,226.878462536606,1.74633651754971));
#73067=CARTESIAN_POINT('Ctrl Pts',(162.303148662985,226.322515837411,1.69341722913911));
#73068=CARTESIAN_POINT('Ctrl Pts',(162.621059453651,225.428467968842,1.64049794072851));
#73069=CARTESIAN_POINT('Ctrl Pts',(162.490679946232,224.605439317717,1.58757865231791));
#73070=CARTESIAN_POINT('Ctrl Pts',(162.360300438814,223.782410666591,1.53465936390732));
#73071=CARTESIAN_POINT('Ctrl Pts',(161.78163063331,223.03040123291,1.48174007549672));
#73072=CARTESIAN_POINT('Ctrl Pts',(161.019467943839,222.693522012104,1.42882078708612));
#73073=CARTESIAN_POINT('Ctrl Pts',(160.257305254368,222.356642791298,1.37590149867553));
#73074=CARTESIAN_POINT('Ctrl Pts',(159.311649680928,222.434893783368,1.32298221026493));
#73075=CARTESIAN_POINT('Ctrl Pts',(158.615237091009,222.892484986464,1.27006292185433));
#73076=CARTESIAN_POINT('Ctrl Pts',(157.924431697403,223.346391874048,1.21756971540021));
#73077=CARTESIAN_POINT('Ctrl Pts',(157.478871863597,224.173555015805,1.16507650894608));
#73078=CARTESIAN_POINT('Ctrl Pts',(157.478271555719,225.000135319788,1.11258330249196));
#73079=CARTESIAN_POINT('Ctrl Pts',(157.482539767498,224.997698761652,1.38741669750799));
#73080=CARTESIAN_POINT('Ctrl Pts',(157.480712233233,224.797816956687,1.40005438763208));
#73081=CARTESIAN_POINT('Ctrl Pts',(157.502515451918,224.598329079321,1.41269207775617));
#73082=CARTESIAN_POINT('Ctrl Pts',(157.549472852864,224.404949327159,1.42532976788027));
#73083=CARTESIAN_POINT('Ctrl Pts',(157.746103108808,223.595187513332,1.47824905629087));
#73084=CARTESIAN_POINT('Ctrl Pts',(158.383798561664,222.892528423726,1.53116834470147));
#73085=CARTESIAN_POINT('Ctrl Pts',(159.170748307313,222.618507464788,1.58408763311207));
#73086=CARTESIAN_POINT('Ctrl Pts',(159.957698052962,222.34448650585,1.63700692152266));
#73087=CARTESIAN_POINT('Ctrl Pts',(160.893902091404,222.499103677581,1.68992620993326));
#73088=CARTESIAN_POINT('Ctrl Pts',(161.550954185028,223.011606829843,1.74284549834386));
#73089=CARTESIAN_POINT('Ctrl Pts',(162.208006278652,223.524109982105,1.79576478675445));
#73090=CARTESIAN_POINT('Ctrl Pts',(162.585906427457,224.394499114897,1.84868407516505));
#73091=CARTESIAN_POINT('Ctrl Pts',(162.511727187682,225.224483857895,1.90160336357565));
#73092=CARTESIAN_POINT('Ctrl Pts',(162.437547947907,226.054468600893,1.95452265198625));
#73093=CARTESIAN_POINT('Ctrl Pts',(161.911289319553,226.844048954097,2.00744194039685));
#73094=CARTESIAN_POINT('Ctrl Pts',(161.173767405945,227.231913117744,2.06036122880744));
#73095=CARTESIAN_POINT('Ctrl Pts',(160.436245492337,227.619777281391,2.11328051721804));
#73096=CARTESIAN_POINT('Ctrl Pts',(159.487460293475,227.605925255482,2.16619980562864));
#73097=CARTESIAN_POINT('Ctrl Pts',(158.761575818028,227.196695652424,2.21911909403924));
#73098=CARTESIAN_POINT('Ctrl Pts',(158.03569134258,226.787466049366,2.27203838244983));
#73099=CARTESIAN_POINT('Ctrl Pts',(157.532707590547,225.982858869159,2.32495767086043));
#73100=CARTESIAN_POINT('Ctrl Pts',(157.482789955364,225.151062377488,2.37787695927103));
#73101=CARTESIAN_POINT('Ctrl Pts',(157.479790411547,225.101079840967,2.38105687201668));
#73102=CARTESIAN_POINT('Ctrl Pts',(157.478426795029,225.05099912951,2.38423678476234));
#73103=CARTESIAN_POINT('Ctrl Pts',(157.478659078657,225.000905528694,2.38741669750799));
#73104=CARTESIAN_POINT('Origin',(160.,225.,10.));
#73105=CARTESIAN_POINT('',(157.485215863135,225.001726236658,3.38741669750799));
#73106=CARTESIAN_POINT('',(157.485769661895,224.998633683171,3.11258330249196));
#73107=CARTESIAN_POINT('',(157.4825,225.,10.));
#73108=CARTESIAN_POINT('Ctrl Pts',(157.485769661895,224.998633683171,3.11258330249196));
#73109=CARTESIAN_POINT('Ctrl Pts',(157.488277019004,225.507373471095,3.08052201479599));
#73110=CARTESIAN_POINT('Ctrl Pts',(157.638052762054,226.017470645054,3.04846072710002));
#73111=CARTESIAN_POINT('Ctrl Pts',(157.924920111362,226.432902133972,3.01639943940405));
#73112=CARTESIAN_POINT('Ctrl Pts',(158.398413756956,227.118599445487,2.96348015099345));
#73113=CARTESIAN_POINT('Ctrl Pts',(159.245395644497,227.546392416654,2.91056086258285));
#73114=CARTESIAN_POINT('Ctrl Pts',(160.078286881534,227.520523004211,2.85764157417226));
#73115=CARTESIAN_POINT('Ctrl Pts',(160.911178118571,227.494653591767,2.80472228576166));
#73116=CARTESIAN_POINT('Ctrl Pts',(161.729978705104,227.015121795713,2.75180299735106));
#73117=CARTESIAN_POINT('Ctrl Pts',(162.160005503369,226.301361331734,2.69888370894047));
#73118=CARTESIAN_POINT('Ctrl Pts',(162.590032301635,225.587600867755,2.64596442052987));
#73119=CARTESIAN_POINT('Ctrl Pts',(162.631285311633,224.639611735851,2.59304513211927));
#73120=CARTESIAN_POINT('Ctrl Pts',(162.26488716814,223.891193795518,2.54012584370867));
#73121=CARTESIAN_POINT('Ctrl Pts',(161.898489024646,223.142775855184,2.48720655529807));
#73122=CARTESIAN_POINT('Ctrl Pts',(161.124439727659,222.593929106419,2.43428726688747));
#73123=CARTESIAN_POINT('Ctrl Pts',(160.296944196735,222.49580570407,2.38136797847687));
#73124=CARTESIAN_POINT('Ctrl Pts',(159.469448665811,222.39768230172,2.32844869006628));
#73125=CARTESIAN_POINT('Ctrl Pts',(158.588506900948,222.750282245786,2.27552940165568));
#73126=CARTESIAN_POINT('Ctrl Pts',(158.057237885245,223.392256029976,2.22261011324508));
#73127=CARTESIAN_POINT('Ctrl Pts',(157.689042990683,223.837174635795,2.18593450966071));
#73128=CARTESIAN_POINT('Ctrl Pts',(157.488801316835,224.421083965243,2.14925890607633));
#73129=CARTESIAN_POINT('Ctrl Pts',(157.484174776371,225.002114825273,2.11258330249196));
#73130=CARTESIAN_POINT('Ctrl Pts',(157.478659078657,225.000905528694,2.38741669750799));
#73131=CARTESIAN_POINT('Ctrl Pts',(157.482292399308,224.217354334461,2.43715607317293));
#73132=CARTESIAN_POINT('Ctrl Pts',(157.876385195861,223.430649576648,2.48689544883788));
#73133=CARTESIAN_POINT('Ctrl Pts',(158.507754644582,222.967176837434,2.53663482450282));
#73134=CARTESIAN_POINT('Ctrl Pts',(159.179488487313,222.474073592187,2.58955411291342));
#73135=CARTESIAN_POINT('Ctrl Pts',(160.119807691108,222.346852904829,2.64247340132401));
#73136=CARTESIAN_POINT('Ctrl Pts',(160.898422215714,222.643730967717,2.69539268973461));
#73137=CARTESIAN_POINT('Ctrl Pts',(161.677036740321,222.940609030605,2.74831197814521));
#73138=CARTESIAN_POINT('Ctrl Pts',(162.293946585739,223.661585843738,2.80123126655581));
#73139=CARTESIAN_POINT('Ctrl Pts',(162.466853814539,224.476742427593,2.8541505549664));
#73140=CARTESIAN_POINT('Ctrl Pts',(162.639761043338,225.291899011447,2.907069843377));
#73141=CARTESIAN_POINT('Ctrl Pts',(162.368665655519,226.201235366023,2.9599891317876));
#73142=CARTESIAN_POINT('Ctrl Pts',(161.777620897288,226.788639195277,3.0129084201982));
#73143=CARTESIAN_POINT('Ctrl Pts',(161.186576139056,227.376043024532,3.0658277086088));
#73144=CARTESIAN_POINT('Ctrl Pts',(160.275582010412,227.641514328466,3.11874699701939));
#73145=CARTESIAN_POINT('Ctrl Pts',(159.461509405714,227.463573442687,3.17166628542999));
#73146=CARTESIAN_POINT('Ctrl Pts',(158.647436801015,227.285632556909,3.22458557384059));
#73147=CARTESIAN_POINT('Ctrl Pts',(157.930285720262,226.664279481418,3.27750486225119));
#73148=CARTESIAN_POINT('Ctrl Pts',(157.638224484387,225.883845371791,3.33042415066178));
#73149=CARTESIAN_POINT('Ctrl Pts',(157.533377309456,225.603677031858,3.34942166627719));
#73150=CARTESIAN_POINT('Ctrl Pts',(157.483313203619,225.303007267603,3.36841918189259));
#73151=CARTESIAN_POINT('Ctrl Pts',(157.485215863135,225.001726236658,3.38741669750799));
#73152=CARTESIAN_POINT('Origin',(160.,225.,10.));
#73153=CARTESIAN_POINT('',(157.484904367492,224.998127113727,4.38741669750799));
#73154=CARTESIAN_POINT('',(157.479195958542,224.99863044174,4.11258330249196));
#73155=CARTESIAN_POINT('',(157.4825,225.,10.));
#73156=CARTESIAN_POINT('Ctrl Pts',(157.479195958542,224.99863044174,4.11258330249196));
#73157=CARTESIAN_POINT('Ctrl Pts',(157.484147283841,225.753298234935,4.06470441192624));
#73158=CARTESIAN_POINT('Ctrl Pts',(157.845660169901,226.512080307909,4.01682552136052));
#73159=CARTESIAN_POINT('Ctrl Pts',(158.437397204933,226.979251770666,3.9689466307948));
#73160=CARTESIAN_POINT('Ctrl Pts',(159.091428709216,227.495604198275,3.9160273423842));
#73161=CARTESIAN_POINT('Ctrl Pts',(160.026709034588,227.655716237085,3.8631080539736));
#73162=CARTESIAN_POINT('Ctrl Pts',(160.815253922581,227.386320621434,3.81018876556301));
#73163=CARTESIAN_POINT('Ctrl Pts',(161.603798810575,227.116925005784,3.75726947715241));
#73164=CARTESIAN_POINT('Ctrl Pts',(162.245608261189,226.418021735672,3.70435018874181));
#73165=CARTESIAN_POINT('Ctrl Pts',(162.446990282374,225.609428933451,3.65143090033122));
#73166=CARTESIAN_POINT('Ctrl Pts',(162.64837230356,224.80083613123,3.59851161192062));
#73167=CARTESIAN_POINT('Ctrl Pts',(162.409326895316,223.882553796899,3.54559232351002));
#73168=CARTESIAN_POINT('Ctrl Pts',(161.839241231897,223.274787909237,3.49267303509942));
#73169=CARTESIAN_POINT('Ctrl Pts',(161.269155568478,222.667022021574,3.43975374668882));
#73170=CARTESIAN_POINT('Ctrl Pts',(160.368029649885,222.369772580581,3.38683445827823));
#73171=CARTESIAN_POINT('Ctrl Pts',(159.548218678452,222.519060923273,3.33391516986763));
#73172=CARTESIAN_POINT('Ctrl Pts',(158.72840770702,222.668349265967,3.28099588145703));
#73173=CARTESIAN_POINT('Ctrl Pts',(157.989911682748,223.264175392347,3.22807659304644));
#73174=CARTESIAN_POINT('Ctrl Pts',(157.670666372435,224.033889281469,3.17515730463584));
#73175=CARTESIAN_POINT('Ctrl Pts',(157.544836658721,224.337270020922,3.15429930392121));
#73176=CARTESIAN_POINT('Ctrl Pts',(157.484138459279,224.667664604178,3.13344130320659));
#73177=CARTESIAN_POINT('Ctrl Pts',(157.485769661895,224.998633683171,3.11258330249196));
#73178=CARTESIAN_POINT('Ctrl Pts',(157.485215863135,225.001726236658,3.38741669750799));
#73179=CARTESIAN_POINT('Ctrl Pts',(157.488613232829,224.463761858256,3.42133847030319));
#73180=CARTESIAN_POINT('Ctrl Pts',(157.657697874279,223.923848559047,3.45526024309838));
#73181=CARTESIAN_POINT('Ctrl Pts',(157.9764364223,223.495222051598,3.48918201589358));
#73182=CARTESIAN_POINT('Ctrl Pts',(158.473680987085,222.826547984796,3.54210130430417));
#73183=CARTESIAN_POINT('Ctrl Pts',(159.335141507653,222.428714994955,3.59502059271477));
#73184=CARTESIAN_POINT('Ctrl Pts',(160.166613666841,222.483771450508,3.64793988112537));
#73185=CARTESIAN_POINT('Ctrl Pts',(160.998085826029,222.538827906061,3.70085916953596));
#73186=CARTESIAN_POINT('Ctrl Pts',(161.799569623837,223.046773807008,3.75377845794656));
#73187=CARTESIAN_POINT('Ctrl Pts',(162.204306090093,223.775173119013,3.80669774635716));
#73188=CARTESIAN_POINT('Ctrl Pts',(162.60904255635,224.503572431018,3.85961703476776));
#73189=CARTESIAN_POINT('Ctrl Pts',(162.617031691054,225.452425154081,3.91253632317835));
#73190=CARTESIAN_POINT('Ctrl Pts',(162.224617666349,226.187536300809,3.96545561158895));
#73191=CARTESIAN_POINT('Ctrl Pts',(161.832203641644,226.922647447537,4.01837489999955));
#73192=CARTESIAN_POINT('Ctrl Pts',(161.03938645753,227.444017017929,4.07129418841015));
#73193=CARTESIAN_POINT('Ctrl Pts',(160.208959241856,227.513066306815,4.12421347682075));
#73194=CARTESIAN_POINT('Ctrl Pts',(159.378532026181,227.5821155957,4.17713276523135));
#73195=CARTESIAN_POINT('Ctrl Pts',(158.510494778948,227.198844603078,4.23005205364194));
#73196=CARTESIAN_POINT('Ctrl Pts',(158.002061327427,226.538638127642,4.28297134205254));
#73197=CARTESIAN_POINT('Ctrl Pts',(157.667567584443,226.10429429277,4.31778646053769));
#73198=CARTESIAN_POINT('Ctrl Pts',(157.488717715052,225.550087119984,4.35260157902284));
#73199=CARTESIAN_POINT('Ctrl Pts',(157.484904367492,224.998127113727,4.38741669750799));
#73200=CARTESIAN_POINT('Origin',(160.,225.,10.));
#73201=CARTESIAN_POINT('',(157.478473441424,224.999338730904,5.38741669750799));
#73202=CARTESIAN_POINT('',(157.481647251813,225.00223805178,5.11258330249196));
#73203=CARTESIAN_POINT('',(157.4825,225.,10.));
#73204=CARTESIAN_POINT('Ctrl Pts',(157.481647251813,225.00223805178,5.11258330249196));
#73205=CARTESIAN_POINT('Ctrl Pts',(157.480078416762,225.172538839621,5.10180609746709));
#73206=CARTESIAN_POINT('Ctrl Pts',(157.495878683591,225.342550212557,5.09102889244222));
#73207=CARTESIAN_POINT('Ctrl Pts',(157.530116486515,225.508763694247,5.08025168741734));
#73208=CARTESIAN_POINT('Ctrl Pts',(157.698234302151,226.32492142299,5.02733239900675));
#73209=CARTESIAN_POINT('Ctrl Pts',(158.310900040407,227.049508094982,4.97441311059615));
#73210=CARTESIAN_POINT('Ctrl Pts',(159.087757871502,227.350952863366,4.92149382218556));
#73211=CARTESIAN_POINT('Ctrl Pts',(159.864615702598,227.652397631749,4.86857453377496));
#73212=CARTESIAN_POINT('Ctrl Pts',(160.805665626533,227.530700496525,4.81565524536436));
#73213=CARTESIAN_POINT('Ctrl Pts',(161.480283216618,227.04155006438,4.76273595695376));
#73214=CARTESIAN_POINT('Ctrl Pts',(162.154900806703,226.552399632235,4.70981666854317));
#73215=CARTESIAN_POINT('Ctrl Pts',(162.563086062939,225.695795903169,4.65689738013257));
#73216=CARTESIAN_POINT('Ctrl Pts',(162.518053420096,224.863720726757,4.60397809172197));
#73217=CARTESIAN_POINT('Ctrl Pts',(162.473020777253,224.031645550345,4.55105880331137));
#73218=CARTESIAN_POINT('Ctrl Pts',(161.974770235332,223.224098926587,4.49813951490078));
#73219=CARTESIAN_POINT('Ctrl Pts',(161.251301232521,222.810614174644,4.44522022649018));
#73220=CARTESIAN_POINT('Ctrl Pts',(160.52783222971,222.397129422701,4.39230093807958));
#73221=CARTESIAN_POINT('Ctrl Pts',(159.579144766009,222.377706542573,4.33938164966898));
#73222=CARTESIAN_POINT('Ctrl Pts',(158.839358206151,222.761233443809,4.28646236125838));
#73223=CARTESIAN_POINT('Ctrl Pts',(158.099571646293,223.144760345044,4.23354307284779));
#73224=CARTESIAN_POINT('Ctrl Pts',(157.568685990277,223.931237027643,4.18062378443719));
#73225=CARTESIAN_POINT('Ctrl Pts',(157.489634503867,224.760771777146,4.12770449602659));
#73226=CARTESIAN_POINT('Ctrl Pts',(157.482105095333,224.839782385362,4.12266409818172));
#73227=CARTESIAN_POINT('Ctrl Pts',(157.478674713186,224.919183615102,4.11762370033684));
#73228=CARTESIAN_POINT('Ctrl Pts',(157.479195958542,224.99863044174,4.11258330249196));
#73229=CARTESIAN_POINT('Ctrl Pts',(157.484904367492,224.998127113727,4.38741669750799));
#73230=CARTESIAN_POINT('Ctrl Pts',(157.482921392991,224.711103022467,4.40552086743344));
#73231=CARTESIAN_POINT('Ctrl Pts',(157.528269906085,224.424686585732,4.42362503735889));
#73232=CARTESIAN_POINT('Ctrl Pts',(157.623676807573,224.156048394559,4.44172920728433));
#73233=CARTESIAN_POINT('Ctrl Pts',(157.902555395047,223.370807095162,4.49464849569493));
#73234=CARTESIAN_POINT('Ctrl Pts',(158.609142225803,222.737466454618,4.54756778410552));
#73235=CARTESIAN_POINT('Ctrl Pts',(159.42010317998,222.545843137587,4.60048707251612));
#73236=CARTESIAN_POINT('Ctrl Pts',(160.231064134158,222.354219820557,4.65340636092672));
#73237=CARTESIAN_POINT('Ctrl Pts',(161.146399211757,222.604313827041,4.70632564933731));
#73238=CARTESIAN_POINT('Ctrl Pts',(161.747251099266,223.181682144589,4.75924493774791));
#73239=CARTESIAN_POINT('Ctrl Pts',(162.348102986775,223.759050462136,4.81216422615851));
#73240=CARTESIAN_POINT('Ctrl Pts',(162.634471684193,224.663693090748,4.86508351456911));
#73241=CARTESIAN_POINT('Ctrl Pts',(162.475314881213,225.481645581359,4.91800280297971));
#73242=CARTESIAN_POINT('Ctrl Pts',(162.316158078232,226.299598071969,4.9709220913903));
#73243=CARTESIAN_POINT('Ctrl Pts',(161.711475774853,227.030860424578,5.0238413798009));
#73244=CARTESIAN_POINT('Ctrl Pts',(160.937970581213,227.340807001009,5.0767606682115));
#73245=CARTESIAN_POINT('Ctrl Pts',(160.164465387572,227.650753577441,5.1296799566221));
#73246=CARTESIAN_POINT('Ctrl Pts',(159.22213730367,227.539384377695,5.1825992450327));
#73247=CARTESIAN_POINT('Ctrl Pts',(158.542195642172,227.057661945386,5.23551853344329));
#73248=CARTESIAN_POINT('Ctrl Pts',(157.891633291123,226.596754053046,5.28615125479819));
#73249=CARTESIAN_POINT('Ctrl Pts',(157.48127254598,225.796806356742,5.33678397615309));
#73250=CARTESIAN_POINT('Ctrl Pts',(157.478473441424,224.999338730904,5.38741669750799));
#73251=CARTESIAN_POINT('Origin',(160.,225.,10.));
#73252=CARTESIAN_POINT('',(157.482962656938,225.002292268722,6.38741669750799));
#73253=CARTESIAN_POINT('',(157.486517381253,224.999964780133,6.11258330249196));
#73254=CARTESIAN_POINT('',(157.4825,225.,10.));
#73255=CARTESIAN_POINT('Ctrl Pts',(157.486517381253,224.999964780133,6.11258330249196));
#73256=CARTESIAN_POINT('Ctrl Pts',(157.486570082313,225.422277771847,6.08598849459734));
#73257=CARTESIAN_POINT('Ctrl Pts',(157.587291160886,225.844614382724,6.05939368670272));
#73258=CARTESIAN_POINT('Ctrl Pts',(157.788540203288,226.211862465092,6.0327988788081));
#73259=CARTESIAN_POINT('Ctrl Pts',(158.188992658498,226.942625675193,5.97987959039751));
#73260=CARTESIAN_POINT('Ctrl Pts',(158.987480022325,227.455268905782,5.92696030198691));
#73261=CARTESIAN_POINT('Ctrl Pts',(159.818614492781,227.515206624622,5.87404101357631));
#73262=CARTESIAN_POINT('Ctrl Pts',(160.649748963237,227.575144343462,5.82112172516571));
#73263=CARTESIAN_POINT('Ctrl Pts',(161.513530540323,227.182376550552,5.76820243675512));
#73264=CARTESIAN_POINT('Ctrl Pts',(162.014692791348,226.516633780206,5.71528314834452));
#73265=CARTESIAN_POINT('Ctrl Pts',(162.515855042373,225.85089100986,5.66236385993392));
#73266=CARTESIAN_POINT('Ctrl Pts',(162.654397967336,224.912173262077,5.60944457152333));
#73267=CARTESIAN_POINT('Ctrl Pts',(162.366924326499,224.130037759786,5.55652528311273));
#73268=CARTESIAN_POINT('Ctrl Pts',(162.079450685662,223.347902257495,5.50360599470213));
#73269=CARTESIAN_POINT('Ctrl Pts',(161.365960479025,222.722349000695,5.45068670629153));
#73270=CARTESIAN_POINT('Ctrl Pts',(160.552946811115,222.539631147399,5.39776741788093));
#73271=CARTESIAN_POINT('Ctrl Pts',(159.739933143206,222.356913294103,5.34484812947034));
#73272=CARTESIAN_POINT('Ctrl Pts',(158.827396014025,222.617030844311,5.29192884105974));
#73273=CARTESIAN_POINT('Ctrl Pts',(158.232912395943,223.200954012161,5.23900955264914));
#73274=CARTESIAN_POINT('Ctrl Pts',(157.759497522896,223.66595910897,5.19686746926341));
#73275=CARTESIAN_POINT('Ctrl Pts',(157.487781864395,224.336311219614,5.15472538587769));
#73276=CARTESIAN_POINT('Ctrl Pts',(157.481647251813,225.00223805178,5.11258330249196));
#73277=CARTESIAN_POINT('Ctrl Pts',(157.478473441424,224.999338730904,5.38741669750799));
#73278=CARTESIAN_POINT('Ctrl Pts',(157.478347034229,224.963325197512,5.38970326456369));
#73279=CARTESIAN_POINT('Ctrl Pts',(157.47905181385,224.92731672201,5.39198983161939));
#73280=CARTESIAN_POINT('Ctrl Pts',(157.480603194088,224.891344758261,5.39427639867509));
#73281=CARTESIAN_POINT('Ctrl Pts',(157.516507646598,224.058825668318,5.44719568708568));
#73282=CARTESIAN_POINT('Ctrl Pts',(158.00587179071,223.245863153303,5.50011497549628));
#73283=CARTESIAN_POINT('Ctrl Pts',(158.724762603703,222.824468844103,5.55303426390688));
#73284=CARTESIAN_POINT('Ctrl Pts',(159.443653416695,222.403074534903,5.60595355231748));
#73285=CARTESIAN_POINT('Ctrl Pts',(160.392070898566,222.373248431518,5.65887284072807));
#73286=CARTESIAN_POINT('Ctrl Pts',(161.136019228261,222.748638958271,5.71179212913867));
#73287=CARTESIAN_POINT('Ctrl Pts',(161.879967557955,223.124029485023,5.76471141754927));
#73288=CARTESIAN_POINT('Ctrl Pts',(162.419446735472,223.904636641913,5.81763070595987));
#73289=CARTESIAN_POINT('Ctrl Pts',(162.507591099788,224.733254609297,5.87054999437046));
#73290=CARTESIAN_POINT('Ctrl Pts',(162.595735464103,225.56187257668,5.92346928278106));
#73291=CARTESIAN_POINT('Ctrl Pts',(162.232545015216,226.438501354556,5.97638857119166));
#73292=CARTESIAN_POINT('Ctrl Pts',(161.584215695397,226.961995631405,6.02930785960225));
#73293=CARTESIAN_POINT('Ctrl Pts',(160.935886375578,227.485489908254,6.08222714801285));
#73294=CARTESIAN_POINT('Ctrl Pts',(160.002418184827,227.655849684076,6.13514643642345));
#73295=CARTESIAN_POINT('Ctrl Pts',(159.210966148877,227.395118328805,6.18806572483405));
#73296=CARTESIAN_POINT('Ctrl Pts',(158.419514112928,227.134386973534,6.24098501324465));
#73297=CARTESIAN_POINT('Ctrl Pts',(157.770078231779,226.442564487169,6.29390430165524));
#73298=CARTESIAN_POINT('Ctrl Pts',(157.559840351877,225.636228825869,6.34682359006584));
#73299=CARTESIAN_POINT('Ctrl Pts',(157.506084219323,225.430055291815,6.36035462587989));
#73300=CARTESIAN_POINT('Ctrl Pts',(157.48104213666,225.216395072921,6.37388566169394));
#73301=CARTESIAN_POINT('Ctrl Pts',(157.482962656938,225.002292268722,6.38741669750799));
#73302=CARTESIAN_POINT('Origin',(160.,225.,10.));
#73303=CARTESIAN_POINT('',(157.486314893834,224.999260124597,7.38741669750799));
#73304=CARTESIAN_POINT('',(157.481517992965,224.997780425011,7.11258330249197));
#73305=CARTESIAN_POINT('',(157.4825,225.,10.));
#73306=CARTESIAN_POINT('Ctrl Pts',(157.481517992965,224.997780425011,7.11258330249197));
#73307=CARTESIAN_POINT('Ctrl Pts',(157.487674873099,225.667890457605,7.0701708917276));
#73308=CARTESIAN_POINT('Ctrl Pts',(157.763272295833,226.342472777999,7.02775848096323));
#73309=CARTESIAN_POINT('Ctrl Pts',(158.242102427776,226.808026878213,6.98534607019886));
#73310=CARTESIAN_POINT('Ctrl Pts',(158.839553725528,227.388913256892,6.93242678178826));
#73311=CARTESIAN_POINT('Ctrl Pts',(159.753404444403,227.644377570781,6.87950749337766));
#73312=CARTESIAN_POINT('Ctrl Pts',(160.565476513413,227.457519354868,6.82658820496707));
#73313=CARTESIAN_POINT('Ctrl Pts',(161.377548582423,227.270661138954,6.77366891655647));
#73314=CARTESIAN_POINT('Ctrl Pts',(162.087842001567,226.641480393238,6.72074962814587));
#73315=CARTESIAN_POINT('Ctrl Pts',(162.371326516211,225.857890214587,6.66783033973528));
#73316=CARTESIAN_POINT('Ctrl Pts',(162.654811030855,225.074300035937,6.61491105132468));
#73317=CARTESIAN_POINT('Ctrl Pts',(162.511486640999,224.136300424352,6.56199176291408));
#73318=CARTESIAN_POINT('Ctrl Pts',(162.006938584623,223.473119983652,6.50907247450348));
#73319=CARTESIAN_POINT('Ctrl Pts',(161.502390528247,222.809939542952,6.45615318609288));
#73320=CARTESIAN_POINT('Ctrl Pts',(160.636618805351,222.421578273136,6.40323389768229));
#73321=CARTESIAN_POINT('Ctrl Pts',(159.805800539309,222.485750283635,6.35031460927169));
#73322=CARTESIAN_POINT('Ctrl Pts',(158.974982273267,222.549922294135,6.29739532086109));
#73323=CARTESIAN_POINT('Ctrl Pts',(158.17911746408,223.066627584951,6.24447603245049));
#73324=CARTESIAN_POINT('Ctrl Pts',(157.782393832782,223.799421825165,6.19155674403989));
#73325=CARTESIAN_POINT('Ctrl Pts',(157.585045307963,224.163947280403,6.16523226352392));
#73326=CARTESIAN_POINT('Ctrl Pts',(157.486465215882,224.581944459547,6.13890778300794));
#73327=CARTESIAN_POINT('Ctrl Pts',(157.486517381253,224.999964780133,6.11258330249196));
#73328=CARTESIAN_POINT('Ctrl Pts',(157.482962656938,225.002292268722,6.38741669750799));
#73329=CARTESIAN_POINT('Ctrl Pts',(157.488553207347,224.379048383382,6.42680495010454));
#73330=CARTESIAN_POINT('Ctrl Pts',(157.722615849539,223.752054177995,6.46619320270109));
#73331=CARTESIAN_POINT('Ctrl Pts',(158.141948568882,223.295062726516,6.50558145529763));
#73332=CARTESIAN_POINT('Ctrl Pts',(158.705334544446,222.681081124701,6.55850074370823));
#73333=CARTESIAN_POINT('Ctrl Pts',(159.603146374231,222.373966757305,6.61142003211883));
#73334=CARTESIAN_POINT('Ctrl Pts',(160.42454538258,222.514255152811,6.66433932052943));
#73335=CARTESIAN_POINT('Ctrl Pts',(161.245944390929,222.654543548318,6.71725860894002));
#73336=CARTESIAN_POINT('Ctrl Pts',(161.990930577842,223.242234706726,6.77017789735062));
#73337=CARTESIAN_POINT('Ctrl Pts',(162.318598278836,224.008401165504,6.82309718576122));
#73338=CARTESIAN_POINT('Ctrl Pts',(162.64626597983,224.774567624282,6.87601647417181));
#73339=CARTESIAN_POINT('Ctrl Pts',(162.556615194904,225.719209383429,6.92893576258241));
#73340=CARTESIAN_POINT('Ctrl Pts',(162.090670121478,226.410058392533,6.98185505099301));
#73341=CARTESIAN_POINT('Ctrl Pts',(161.624725048052,227.100907401638,7.03477433940361));
#73342=CARTESIAN_POINT('Ctrl Pts',(160.782485686126,227.5379636607,7.0876936278142));
#73343=CARTESIAN_POINT('Ctrl Pts',(159.949360751157,227.521230234166,7.1406129162248));
#73344=CARTESIAN_POINT('Ctrl Pts',(159.116235816188,227.504496807632,7.1935322046354));
#73345=CARTESIAN_POINT('Ctrl Pts',(158.292225308176,227.033973695501,7.246451493046));
#73346=CARTESIAN_POINT('Ctrl Pts',(157.854396419386,226.324972264635,7.29937078145659));
#73347=CARTESIAN_POINT('Ctrl Pts',(157.611579816057,225.931765412355,7.32871942014039));
#73348=CARTESIAN_POINT('Ctrl Pts',(157.487542176156,225.465209114919,7.35806805882419));
#73349=CARTESIAN_POINT('Ctrl Pts',(157.486314893834,224.999260124597,7.38741669750799));
#73350=CARTESIAN_POINT('Origin',(160.,225.,10.));
#73351=CARTESIAN_POINT('',(157.480251844254,224.998100046348,8.387416697508));
#73352=CARTESIAN_POINT('',(157.479288468299,225.001430882652,8.11258330249197));
#73353=CARTESIAN_POINT('',(157.4825,225.,10.));
#73354=CARTESIAN_POINT('Ctrl Pts',(157.479288468299,225.001430882652,8.11258330249197));
#73355=CARTESIAN_POINT('Ctrl Pts',(157.478719681623,225.085146706162,8.10727257726844));
#73356=CARTESIAN_POINT('Ctrl Pts',(157.4825287714,225.168810144924,8.10196185204492));
#73357=CARTESIAN_POINT('Ctrl Pts',(157.490886088512,225.252016757275,8.0966511268214));
#73358=CARTESIAN_POINT('Ctrl Pts',(157.57416346702,226.081137928365,8.0437318384108));
#73359=CARTESIAN_POINT('Ctrl Pts',(158.109049745654,226.864899257462,7.99081255000021));
#73360=CARTESIAN_POINT('Ctrl Pts',(158.85078097383,227.244651575782,7.93789326158961));
#73361=CARTESIAN_POINT('Ctrl Pts',(159.592512202006,227.624403894102,7.88497397317902));
#73362=CARTESIAN_POINT('Ctrl Pts',(160.541088379722,227.600147201645,7.83205468476842));
#73363=CARTESIAN_POINT('Ctrl Pts',(161.262441066707,227.182981360402,7.77913539635782));
#73364=CARTESIAN_POINT('Ctrl Pts',(161.983793753692,226.765815519159,7.72621610794722));
#73365=CARTESIAN_POINT('Ctrl Pts',(162.477922949946,225.955740529131,7.67329681953663));
#73366=CARTESIAN_POINT('Ctrl Pts',(162.518715144978,225.123446689826,7.62037753112603));
#73367=CARTESIAN_POINT('Ctrl Pts',(162.55950734001,224.291152850521,7.56745824271543));
#73368=CARTESIAN_POINT('Ctrl Pts',(162.146962533821,223.43664016194,7.51453895430483));
#73369=CARTESIAN_POINT('Ctrl Pts',(161.469861221611,222.950933613575,7.46161966589423));
#73370=CARTESIAN_POINT('Ctrl Pts',(160.792759909401,222.465227065211,7.40870037748364));
#73371=CARTESIAN_POINT('Ctrl Pts',(159.85110209117,222.348326657064,7.35578108907304));
#73372=CARTESIAN_POINT('Ctrl Pts',(159.075790366026,222.653726013603,7.30286180066244));
#73373=CARTESIAN_POINT('Ctrl Pts',(158.300478640882,222.959125370143,7.24994251225184));
#73374=CARTESIAN_POINT('Ctrl Pts',(157.691513008825,223.686824491369,7.19702322384125));
#73375=CARTESIAN_POINT('Ctrl Pts',(157.527556131111,224.503828273716,7.14410393543065));
#73376=CARTESIAN_POINT('Ctrl Pts',(157.495003258517,224.666040560303,7.13359705778442));
#73377=CARTESIAN_POINT('Ctrl Pts',(157.479992741628,224.831773258829,7.12309018013819));
#73378=CARTESIAN_POINT('Ctrl Pts',(157.481517992965,224.997780425011,7.11258330249197));
#73379=CARTESIAN_POINT('Ctrl Pts',(157.486314893834,224.999260124597,7.38741669750799));
#73380=CARTESIAN_POINT('Ctrl Pts',(157.485329231704,224.625044456207,7.41098734723479));
#73381=CARTESIAN_POINT('Ctrl Pts',(157.563557612755,224.251220507643,7.43455799696159));
#73382=CARTESIAN_POINT('Ctrl Pts',(157.723088400219,223.916099730613,7.45812864668839));
#73383=CARTESIAN_POINT('Ctrl Pts',(158.081256539411,223.163708377062,7.51104793509899));
#73384=CARTESIAN_POINT('Ctrl Pts',(158.849240087364,222.606405419563,7.56396722350959));
#73385=CARTESIAN_POINT('Ctrl Pts',(159.675609787634,222.499212680511,7.61688651192018));
#73386=CARTESIAN_POINT('Ctrl Pts',(160.501979487905,222.392019941459,7.66980580033078));
#73387=CARTESIAN_POINT('Ctrl Pts',(161.386735340493,222.734937420853,7.72272508874138));
#73388=CARTESIAN_POINT('Ctrl Pts',(161.92501308465,223.371046086864,7.77564437715197));
#73389=CARTESIAN_POINT('Ctrl Pts',(162.463290828808,224.007154752876,7.82856366556257));
#73390=CARTESIAN_POINT('Ctrl Pts',(162.655090464535,224.936454605506,7.88148295397317));
#73391=CARTESIAN_POINT('Ctrl Pts',(162.412644482294,225.733698050462,7.93440224238377));
#73392=CARTESIAN_POINT('Ctrl Pts',(162.170198500053,226.530941495419,7.98732153079436));
#73393=CARTESIAN_POINT('Ctrl Pts',(161.493506899843,227.196128532701,8.04024081920496));
#73394=CARTESIAN_POINT('Ctrl Pts',(160.692223744617,227.424869587129,8.09316010761556));
#73395=CARTESIAN_POINT('Ctrl Pts',(159.89094058939,227.653610641557,8.14607939602615));
#73396=CARTESIAN_POINT('Ctrl Pts',(158.965065879146,227.445905713129,8.19899868443675));
#73397=CARTESIAN_POINT('Ctrl Pts',(158.338279863088,226.896800573011,8.25191797284735));
#73398=CARTESIAN_POINT('Ctrl Pts',(157.803322393818,226.428143186607,8.2970842144009));
#73399=CARTESIAN_POINT('Ctrl Pts',(157.486236167406,225.710792720596,8.34225045595445));
#73400=CARTESIAN_POINT('Ctrl Pts',(157.480251844254,224.998100046348,8.387416697508));
#73401=CARTESIAN_POINT('Origin',(160.,225.,10.));
#73402=CARTESIAN_POINT('',(157.480388031054,225.001947791586,9.387416697508));
#73403=CARTESIAN_POINT('',(157.485838515826,225.001308641677,9.11258330249197));
#73404=CARTESIAN_POINT('',(157.4825,225.,10.));
#73405=CARTESIAN_POINT('Ctrl Pts',(157.485838515826,225.001308641677,9.11258330249197));
#73406=CARTESIAN_POINT('Ctrl Pts',(157.484258502333,225.336590190805,9.0914549743987));
#73407=CARTESIAN_POINT('Ctrl Pts',(157.546594678729,225.671308165495,9.07032664630543));
#73408=CARTESIAN_POINT('Ctrl Pts',(157.675619457858,225.977967362484,9.04919831821216));
#73409=CARTESIAN_POINT('Ctrl Pts',(157.998782723248,226.746044534403,8.99627902980156));
#73410=CARTESIAN_POINT('Ctrl Pts',(158.74030520912,227.338099899218,8.94335974139096));
#73411=CARTESIAN_POINT('Ctrl Pts',(159.560866240521,227.483208933629,8.89044045298036));
#73412=CARTESIAN_POINT('Ctrl Pts',(160.381427271921,227.628317968041,8.83752116456977));
#73413=CARTESIAN_POINT('Ctrl Pts',(161.281026848849,227.32648067205,8.78460187615917));
#73414=CARTESIAN_POINT('Ctrl Pts',(161.84800822259,226.715817786367,8.73168258774858));
#73415=CARTESIAN_POINT('Ctrl Pts',(162.414989596331,226.105154900683,8.67876329933798));
#73416=CARTESIAN_POINT('Ctrl Pts',(162.649352766886,225.185666425308,8.62584401092738));
#73417=CARTESIAN_POINT('Ctrl Pts',(162.443853152016,224.378110268494,8.57292472251678));
#73418=CARTESIAN_POINT('Ctrl Pts',(162.238353537146,223.570554111679,8.52000543410618));
#73419=CARTESIAN_POINT('Ctrl Pts',(161.592991136852,222.874930273426,8.46708614569558));
#73420=CARTESIAN_POINT('Ctrl Pts',(160.803083772819,222.60955620844,8.41416685728498));
#73421=CARTESIAN_POINT('Ctrl Pts',(160.013176408786,222.344182143455,8.36124756887439));
#73422=CARTESIAN_POINT('Ctrl Pts',(159.078724081015,222.509057851738,8.30832828046379));
#73423=CARTESIAN_POINT('Ctrl Pts',(158.427332156319,223.02873621242,8.2554089920532));
#73424=CARTESIAN_POINT('Ctrl Pts',(157.841310791749,223.49626215267,8.20780042886612));
#73425=CARTESIAN_POINT('Ctrl Pts',(157.484387417167,224.250951446125,8.16019186567904));
#73426=CARTESIAN_POINT('Ctrl Pts',(157.479288468299,225.001430882652,8.11258330249197));
#73427=CARTESIAN_POINT('Ctrl Pts',(157.480251844254,224.998100046348,8.387416697508));
#73428=CARTESIAN_POINT('Ctrl Pts',(157.479224600539,224.875762222609,8.39516974436504));
#73429=CARTESIAN_POINT('Ctrl Pts',(157.487364195317,224.753561644012,8.40292279122209));
#73430=CARTESIAN_POINT('Ctrl Pts',(157.505142185515,224.632779749063,8.41067583807914));
#73431=CARTESIAN_POINT('Ctrl Pts',(157.626487845874,223.808369417042,8.46359512648974));
#73432=CARTESIAN_POINT('Ctrl Pts',(158.196876488464,223.050054104809,8.51651441490034));
#73433=CARTESIAN_POINT('Ctrl Pts',(158.955298281651,222.704838884332,8.56943370331093));
#73434=CARTESIAN_POINT('Ctrl Pts',(159.713720074839,222.359623663855,8.62235299172153));
#73435=CARTESIAN_POINT('Ctrl Pts',(160.660175018623,222.427508535133,8.67527228013213));
#73436=CARTESIAN_POINT('Ctrl Pts',(161.361565349338,222.877429382405,8.72819156854273));
#73437=CARTESIAN_POINT('Ctrl Pts',(162.062955680054,223.327350229677,8.78111085695333));
#73438=CARTESIAN_POINT('Ctrl Pts',(162.519281397699,224.159307052943,8.83403014536392));
#73439=CARTESIAN_POINT('Ctrl Pts',(162.521727862853,224.992596426233,8.88694943377452));
#73440=CARTESIAN_POINT('Ctrl Pts',(162.524174328007,225.825885799524,8.93986872218511));
#73441=CARTESIAN_POINT('Ctrl Pts',(162.072741540669,226.660507722839,8.99278801059571));
#73442=CARTESIAN_POINT('Ctrl Pts',(161.374005135449,227.114539220481,9.04570729900631));
#73443=CARTESIAN_POINT('Ctrl Pts',(160.67526873023,227.568570718123,9.09862658741691));
#73444=CARTESIAN_POINT('Ctrl Pts',(159.729228707127,227.642011790091,9.15154587582751));
#73445=CARTESIAN_POINT('Ctrl Pts',(158.968792962114,227.301255803297,9.2044651642381));
#73446=CARTESIAN_POINT('Ctrl Pts',(158.2083572171,226.960499816503,9.2573844526487));
#73447=CARTESIAN_POINT('Ctrl Pts',(157.633525750175,226.205546770946,9.3103037410593));
#73448=CARTESIAN_POINT('Ctrl Pts',(157.5073414293,225.38186316543,9.3632230294699));
#73449=CARTESIAN_POINT('Ctrl Pts',(157.488111757962,225.256339131133,9.3712875854826));
#73450=CARTESIAN_POINT('Ctrl Pts',(157.479301369843,225.12921891334,9.3793521414953));
#73451=CARTESIAN_POINT('Ctrl Pts',(157.480388031054,225.001947791586,9.387416697508));
#73452=CARTESIAN_POINT('Origin',(160.,225.,10.));
#73453=CARTESIAN_POINT('',(157.486356032508,225.000662446517,10.387416697508));
#73454=CARTESIAN_POINT('',(157.484060754376,224.997857937859,10.112583302492));
#73455=CARTESIAN_POINT('',(157.4825,225.,10.));
#73456=CARTESIAN_POINT('Ctrl Pts',(157.484060754376,224.997857937859,10.112583302492));
#73457=CARTESIAN_POINT('Ctrl Pts',(157.488797168304,225.583104362717,10.0756373715289));
#73458=CARTESIAN_POINT('Ctrl Pts',(157.692267651195,226.171320282162,10.0386914405659));
#73459=CARTESIAN_POINT('Ctrl Pts',(158.06545542551,226.617622439287,10.0017455096029));
#73460=CARTESIAN_POINT('Ctrl Pts',(158.599988754229,227.256880727156,9.94882622119231));
#73461=CARTESIAN_POINT('Ctrl Pts',(159.482715739494,227.604987350972,9.89590693278172));
#73462=CARTESIAN_POINT('Ctrl Pts',(160.309700530204,227.502648726522,9.84298764437112));
#73463=CARTESIAN_POINT('Ctrl Pts',(161.136685320915,227.400310102072,9.79006835596053));
#73464=CARTESIAN_POINT('Ctrl Pts',(161.90792791707,226.847526229355,9.73714906754993));
#73465=CARTESIAN_POINT('Ctrl Pts',(162.270507721834,226.097250997659,9.68422977913933));
#73466=CARTESIAN_POINT('Ctrl Pts',(162.633087526598,225.346975765962,9.63131049072873));
#73467=CARTESIAN_POINT('Ctrl Pts',(162.587004539971,224.399209175285,9.57839120231813));
#73468=CARTESIAN_POINT('Ctrl Pts',(162.153346335727,223.687649198886,9.52547191390753));
#73469=CARTESIAN_POINT('Ctrl Pts',(161.719688131483,222.976089222488,9.47255262549694));
#73470=CARTESIAN_POINT('Ctrl Pts',(160.898454709622,222.500735860368,9.41963333708634));
#73471=CARTESIAN_POINT('Ctrl Pts',(160.065442467841,222.479110801686,9.36671404867574));
#73472=CARTESIAN_POINT('Ctrl Pts',(159.232430226059,222.457485743005,9.31379476026514));
#73473=CARTESIAN_POINT('Ctrl Pts',(158.387639164358,222.889588987761,9.26087547185455));
#73474=CARTESIAN_POINT('Ctrl Pts',(157.91764565596,223.577690099652,9.20795618344395));
#73475=CARTESIAN_POINT('Ctrl Pts',(157.635299739686,223.991062913221,9.17616522312662));
#73476=CARTESIAN_POINT('Ctrl Pts',(157.488215899689,224.496823744605,9.14437426280929));
#73477=CARTESIAN_POINT('Ctrl Pts',(157.485838515826,225.001308641677,9.11258330249197));
#73478=CARTESIAN_POINT('Ctrl Pts',(157.480388031054,225.001947791586,9.387416697508));
#73479=CARTESIAN_POINT('Ctrl Pts',(157.486431996492,224.29407099102,9.4322714299059));
#73480=CARTESIAN_POINT('Ctrl Pts',(157.798645056327,223.581525917367,9.4771261623038));
#73481=CARTESIAN_POINT('Ctrl Pts',(158.32717092237,223.112989373578,9.5219808947017));
#73482=CARTESIAN_POINT('Ctrl Pts',(158.950721911137,222.560213352718,9.57490018311229));
#73483=CARTESIAN_POINT('Ctrl Pts',(159.875361063495,222.347075476473,9.62781947152289));
#73484=CARTESIAN_POINT('Ctrl Pts',(160.677973521504,222.571107632822,9.68073875993348));
#73485=CARTESIAN_POINT('Ctrl Pts',(161.480585979514,222.795139789172,9.73365804834408));
#73486=CARTESIAN_POINT('Ctrl Pts',(162.161171743175,223.456341978116,9.78657733675468));
#73487=CARTESIAN_POINT('Ctrl Pts',(162.408294780418,224.252148090994,9.83949662516527));
#73488=CARTESIAN_POINT('Ctrl Pts',(162.655417817662,225.047954203872,9.89241591357587));
#73489=CARTESIAN_POINT('Ctrl Pts',(162.469078128488,225.978364240684,9.94533520198646));
#73490=CARTESIAN_POINT('Ctrl Pts',(161.934544750998,226.617622586879,9.99825449039706));
#73491=CARTESIAN_POINT('Ctrl Pts',(161.400011373508,227.256880933074,10.0511737788077));
#73492=CARTESIAN_POINT('Ctrl Pts',(160.517284307703,227.604987588652,10.1040930672183));
#73493=CARTESIAN_POINT('Ctrl Pts',(159.690299441538,227.502648954864,10.1570123556289));
#73494=CARTESIAN_POINT('Ctrl Pts',(158.863314575373,227.400310321077,10.2099316440395));
#73495=CARTESIAN_POINT('Ctrl Pts',(158.09207190885,226.847526397924,10.26285093245));
#73496=CARTESIAN_POINT('Ctrl Pts',(157.729492071004,226.097251097772,10.3157702208606));
#73497=CARTESIAN_POINT('Ctrl Pts',(157.565861955122,225.758656334653,10.3396523797431));
#73498=CARTESIAN_POINT('Ctrl Pts',(157.485462685781,225.379839233365,10.3635345386255));
#73499=CARTESIAN_POINT('Ctrl Pts',(157.486356032508,225.000662446517,10.387416697508));
#73500=CARTESIAN_POINT('Origin',(160.,225.,10.));
#73501=CARTESIAN_POINT('',(157.482816018711,224.997701707894,11.387416697508));
#73502=CARTESIAN_POINT('',(157.478262151323,224.999954178036,11.112583302492));
#73503=CARTESIAN_POINT('',(157.4825,225.,10.));
#73504=CARTESIAN_POINT('Ctrl Pts',(157.478262555774,224.999954182409,11.112583302492));
#73505=CARTESIAN_POINT('Ctrl Pts',(157.478485401468,225.830795425014,11.0598197686592));
#73506=CARTESIAN_POINT('Ctrl Pts',(157.92931520263,226.661843898407,11.0070562348264));
#73507=CARTESIAN_POINT('Ctrl Pts',(158.625994989915,227.11453902755,10.9542927009937));
#73508=CARTESIAN_POINT('Ctrl Pts',(159.324731331382,227.568570483766,10.9013734125831));
#73509=CARTESIAN_POINT('Ctrl Pts',(160.270771268167,227.642011549034,10.8484541241725));
#73510=CARTESIAN_POINT('Ctrl Pts',(161.031206943798,227.30125559333,10.7955348357619));
#73511=CARTESIAN_POINT('Ctrl Pts',(161.79164261943,226.960499637627,10.7426155473513));
#73512=CARTESIAN_POINT('Ctrl Pts',(162.366474033907,226.205546660952,10.6896962589407));
#73513=CARTESIAN_POINT('Ctrl Pts',(162.492658343269,225.381863130589,10.6367769705301));
#73514=CARTESIAN_POINT('Ctrl Pts',(162.61884265263,224.558179600226,10.5838576821195));
#73515=CARTESIAN_POINT('Ctrl Pts',(162.296379856875,223.665765516174,10.5309383937089));
#73516=CARTESIAN_POINT('Ctrl Pts',(161.672828925001,223.112989545749,10.4780191052983));
#73517=CARTESIAN_POINT('Ctrl Pts',(161.049277993127,222.560213575324,10.4250998168877));
#73518=CARTESIAN_POINT('Ctrl Pts',(160.124638925134,222.347075718526,10.3721805284771));
#73519=CARTESIAN_POINT('Ctrl Pts',(159.322026540355,222.571107854435,10.3192612400665));
#73520=CARTESIAN_POINT('Ctrl Pts',(158.519414155576,222.795139990344,10.2663419516559));
#73521=CARTESIAN_POINT('Ctrl Pts',(157.838828454011,223.456342118959,10.2134226632453));
#73522=CARTESIAN_POINT('Ctrl Pts',(157.591705439315,224.252148159228,10.1605033748347));
#73523=CARTESIAN_POINT('Ctrl Pts',(157.517112897242,224.492357253528,10.1445300173871));
#73524=CARTESIAN_POINT('Ctrl Pts',(157.48201299348,224.744830064544,10.1285566599395));
#73525=CARTESIAN_POINT('Ctrl Pts',(157.484060754376,224.997857937859,10.112583302492));
#73526=CARTESIAN_POINT('Ctrl Pts',(157.486356032508,225.000662446517,10.387416697508));
#73527=CARTESIAN_POINT('Ctrl Pts',(157.487442208375,224.53964024463,10.4164538270362));
#73528=CARTESIAN_POINT('Ctrl Pts',(157.60870260008,224.078086322494,10.4454909565643));
#73529=CARTESIAN_POINT('Ctrl Pts',(157.846653467802,223.687649079147,10.4745280860924));
#73530=CARTESIAN_POINT('Ctrl Pts',(158.280311711613,222.976089037826,10.527447374503));
#73531=CARTESIAN_POINT('Ctrl Pts',(159.101545208403,222.500735632334,10.5803666629136));
#73532=CARTESIAN_POINT('Ctrl Pts',(159.934557526189,222.47911057168,10.6332859513242));
#73533=CARTESIAN_POINT('Ctrl Pts',(160.767569843974,222.457485511025,10.6862052397348));
#73534=CARTESIAN_POINT('Ctrl Pts',(161.612360982755,222.889588795207,10.7391245281454));
#73535=CARTESIAN_POINT('Ctrl Pts',(162.082354534035,223.57768996988,10.792043816556));
#73536=CARTESIAN_POINT('Ctrl Pts',(162.552348085314,224.265791144553,10.8449631049666));
#73537=CARTESIAN_POINT('Ctrl Pts',(162.647544049094,225.209890209716,10.8978823933772));
#73538=CARTESIAN_POINT('Ctrl Pts',(162.324380754219,225.977967451715,10.9508016817878));
#73539=CARTESIAN_POINT('Ctrl Pts',(162.001217459344,226.746044693713,11.0037209701984));
#73540=CARTESIAN_POINT('Ctrl Pts',(161.259694905814,227.338100112547,11.056640258609));
#73541=CARTESIAN_POINT('Ctrl Pts',(160.439133799546,227.483209160198,11.1095595470196));
#73542=CARTESIAN_POINT('Ctrl Pts',(159.618572693277,227.628318207849,11.1624788354302));
#73543=CARTESIAN_POINT('Ctrl Pts',(158.71897303427,227.326480884318,11.2153981238408));
#73544=CARTESIAN_POINT('Ctrl Pts',(158.151991608797,226.715817942918,11.2683174122514));
#73545=CARTESIAN_POINT('Ctrl Pts',(157.726645233492,226.257701932431,11.3080171740036));
#73546=CARTESIAN_POINT('Ctrl Pts',(157.488493693424,225.625781377196,11.3477169357558));
#73547=CARTESIAN_POINT('Ctrl Pts',(157.482816018711,224.997701707894,11.387416697508));
#73548=CARTESIAN_POINT('Origin',(160.,225.,10.));
#73549=CARTESIAN_POINT('',(157.478532268341,225.000747722968,12.387416697508));
#73550=CARTESIAN_POINT('',(157.483927228124,225.002171058717,12.112583302492));
#73551=CARTESIAN_POINT('',(157.4825,225.,10.));
#73552=CARTESIAN_POINT('Ctrl Pts',(157.483927228124,225.002171058717,12.112583302492));
#73553=CARTESIAN_POINT('Ctrl Pts',(157.481884324812,225.250231121536,12.0969214542001));
#73554=CARTESIAN_POINT('Ctrl Pts',(157.515602092607,225.497748009088,12.0812596059081));
#73555=CARTESIAN_POINT('Ctrl Pts',(157.587355737836,225.733697983519,12.0655977576162));
#73556=CARTESIAN_POINT('Ctrl Pts',(157.829801697957,226.530941355735,12.0126784692056));
#73557=CARTESIAN_POINT('Ctrl Pts',(158.506493236424,227.196128332326,11.959759180795));
#73558=CARTESIAN_POINT('Ctrl Pts',(159.307776318542,227.424869365883,11.9068398923844));
#73559=CARTESIAN_POINT('Ctrl Pts',(160.109059400659,227.653610399441,11.8539206039738));
#73560=CARTESIAN_POINT('Ctrl Pts',(161.034934026426,227.445905489964,11.8010013155632));
#73561=CARTESIAN_POINT('Ctrl Pts',(161.661719985296,226.896800399947,11.7480820271526));
#73562=CARTESIAN_POINT('Ctrl Pts',(162.288505944167,226.347695309929,11.695162738742));
#73563=CARTESIAN_POINT('Ctrl Pts',(162.616203236141,225.45719003937,11.6422434503314));
#73564=CARTESIAN_POINT('Ctrl Pts',(162.494857586854,224.632779782569,11.5893241619208));
#73565=CARTESIAN_POINT('Ctrl Pts',(162.373511937567,223.808369525767,11.5364048735102));
#73566=CARTESIAN_POINT('Ctrl Pts',(161.803123347019,223.050054282723,11.4834855850996));
#73567=CARTESIAN_POINT('Ctrl Pts',(161.04470162303,222.704839093743,11.430566296689));
#73568=CARTESIAN_POINT('Ctrl Pts',(160.286279899042,222.359623904763,11.3776470082784));
#73569=CARTESIAN_POINT('Ctrl Pts',(159.339825041612,222.427508769848,11.3247277198678));
#73570=CARTESIAN_POINT('Ctrl Pts',(158.638434774892,222.877429576069,11.2718084314573));
#73571=CARTESIAN_POINT('Ctrl Pts',(157.937044508171,223.32735038229,11.2188891430467));
#73572=CARTESIAN_POINT('Ctrl Pts',(157.480718832161,224.159307129647,11.1659698546361));
#73573=CARTESIAN_POINT('Ctrl Pts',(157.47827236723,224.992596426908,11.1130505662255));
#73574=CARTESIAN_POINT('Ctrl Pts',(157.478265166677,224.995049003778,11.1128948116476));
#73575=CARTESIAN_POINT('Ctrl Pts',(157.478261897948,224.997501592191,11.1127390570698));
#73576=CARTESIAN_POINT('Ctrl Pts',(157.478262555774,224.999954182409,11.112583302492));
#73577=CARTESIAN_POINT('Ctrl Pts',(157.482816018711,224.997701707894,11.387416697508));
#73578=CARTESIAN_POINT('Ctrl Pts',(157.480925423682,224.788558993543,11.4006362241664));
#73579=CARTESIAN_POINT('Ctrl Pts',(157.504811696542,224.579842159362,11.4138557508248));
#73580=CARTESIAN_POINT('Ctrl Pts',(157.556146625006,224.378110211752,11.4270752774832));
#73581=CARTESIAN_POINT('Ctrl Pts',(157.761646258626,223.570553981256,11.4799945658938));
#73582=CARTESIAN_POINT('Ctrl Pts',(158.407008717803,222.874930079534,11.5329138543044));
#73583=CARTESIAN_POINT('Ctrl Pts',(159.196916153907,222.609555990336,11.585833142715));
#73584=CARTESIAN_POINT('Ctrl Pts',(159.986823590012,222.344181901138,11.6387524311256));
#73585=CARTESIAN_POINT('Ctrl Pts',(160.921276003043,222.509057624464,11.6916717195362));
#73586=CARTESIAN_POINT('Ctrl Pts',(161.572667987172,223.028736032562,11.7445910079468));
#73587=CARTESIAN_POINT('Ctrl Pts',(162.224059971301,223.54841444066,11.7975102963574));
#73588=CARTESIAN_POINT('Ctrl Pts',(162.592391526527,224.422895533531,11.850429584768));
#73589=CARTESIAN_POINT('Ctrl Pts',(162.50911414042,225.25201678027,11.9033488731786));
#73590=CARTESIAN_POINT('Ctrl Pts',(162.425836754314,226.081138027009,11.9562681615892));
#73591=CARTESIAN_POINT('Ctrl Pts',(161.890950426876,226.864899427616,12.0091874499998));
#73592=CARTESIAN_POINT('Ctrl Pts',(161.149219131025,227.244651780585,12.0621067384104));
#73593=CARTESIAN_POINT('Ctrl Pts',(160.407487835173,227.624404133553,12.115026026821));
#73594=CARTESIAN_POINT('Ctrl Pts',(159.458911570908,227.600147438883,12.1679453152316));
#73595=CARTESIAN_POINT('Ctrl Pts',(158.737558818107,227.182981559578,12.2208646036422));
#73596=CARTESIAN_POINT('Ctrl Pts',(158.016206065306,226.765815680272,12.2737838920528));
#73597=CARTESIAN_POINT('Ctrl Pts',(157.522076823968,225.955740616332,12.3267031804634));
#73598=CARTESIAN_POINT('Ctrl Pts',(157.481284625214,225.123446701089,12.379622468874));
#73599=CARTESIAN_POINT('Ctrl Pts',(157.479281929328,225.082585172391,12.3822205450853));
#73600=CARTESIAN_POINT('Ctrl Pts',(157.478371923492,225.041670089019,12.3848186212967));
#73601=CARTESIAN_POINT('Ctrl Pts',(157.478532268341,225.000747722968,12.387416697508));
#73602=CARTESIAN_POINT('Origin',(160.,225.,10.));
#73603=CARTESIAN_POINT('',(157.485016106425,225.001823857836,13.387416697508));
#73604=CARTESIAN_POINT('',(157.485914018718,224.998759312188,13.112583302492));
#73605=CARTESIAN_POINT('',(157.4825,225.,10.));
#73606=CARTESIAN_POINT('Ctrl Pts',(157.485914018718,224.998759312188,13.112583302492));
#73607=CARTESIAN_POINT('Ctrl Pts',(157.488141905361,225.4983384767,13.0811038513303));
#73608=CARTESIAN_POINT('Ctrl Pts',(157.632159036081,225.999101383862,13.0496244001686));
#73609=CARTESIAN_POINT('Ctrl Pts',(157.909330069275,226.410058263879,13.018144949007));
#73610=CARTESIAN_POINT('Ctrl Pts',(158.375275100188,227.100907209951,12.9652256605964));
#73611=CARTESIAN_POINT('Ctrl Pts',(159.217514385268,227.537963429135,12.9123063721858));
#73612=CARTESIAN_POINT('Ctrl Pts',(160.050639244222,227.521230004128,12.8593870837752));
#73613=CARTESIAN_POINT('Ctrl Pts',(160.883764103177,227.504496579121,12.8064677953646));
#73614=CARTESIAN_POINT('Ctrl Pts',(161.707774536006,227.033973509921,12.753548506954));
#73615=CARTESIAN_POINT('Ctrl Pts',(162.145603384849,226.324972143744,12.7006292185434));
#73616=CARTESIAN_POINT('Ctrl Pts',(162.583432233691,225.615970777567,12.6477099301328));
#73617=CARTESIAN_POINT('Ctrl Pts',(162.635079498548,224.668491114411,12.5947906417222));
#73618=CARTESIAN_POINT('Ctrl Pts',(162.276911392035,223.916099829509,12.5418713533116));
#73619=CARTESIAN_POINT('Ctrl Pts',(161.918743285523,223.163708544606,12.488952064901));
#73620=CARTESIAN_POINT('Ctrl Pts',(161.150759807641,222.606405637956,12.4360327764904));
#73621=CARTESIAN_POINT('Ctrl Pts',(160.324390182769,222.499212908684,12.3831134880798));
#73622=CARTESIAN_POINT('Ctrl Pts',(159.498020557896,222.392020179412,12.3301941996692));
#73623=CARTESIAN_POINT('Ctrl Pts',(158.613264786033,222.734937627517,12.2772749112586));
#73624=CARTESIAN_POINT('Ctrl Pts',(158.074987090988,223.37104623549,12.224355622848));
#73625=CARTESIAN_POINT('Ctrl Pts',(157.696016594735,223.818893874458,12.1870981827293));
#73626=CARTESIAN_POINT('Ctrl Pts',(157.488787021577,224.412069382079,12.1498407426106));
#73627=CARTESIAN_POINT('Ctrl Pts',(157.483927228124,225.002171058717,12.112583302492));
#73628=CARTESIAN_POINT('Ctrl Pts',(157.478532268341,225.000747722968,12.387416697508));
#73629=CARTESIAN_POINT('Ctrl Pts',(157.481637930571,224.208136999396,12.4377379097073));
#73630=CARTESIAN_POINT('Ctrl Pts',(157.886279610186,223.412794219741,12.4880591219065));
#73631=CARTESIAN_POINT('Ctrl Pts',(158.530138644279,222.950933426618,12.5383803341057));
#73632=CARTESIAN_POINT('Ctrl Pts',(159.207240018268,222.465226833938,12.5912996225163));
#73633=CARTESIAN_POINT('Ctrl Pts',(160.148897922415,222.348326415125,12.6442189109269));
#73634=CARTESIAN_POINT('Ctrl Pts',(160.924209718299,222.653725799529,12.6971381993375));
#73635=CARTESIAN_POINT('Ctrl Pts',(161.699521514183,222.959125183933,12.7500574877481));
#73636=CARTESIAN_POINT('Ctrl Pts',(162.308487201802,223.686824371555,12.8029767761587));
#73637=CARTESIAN_POINT('Ctrl Pts',(162.472444094476,224.503828228446,12.8558960645693));
#73638=CARTESIAN_POINT('Ctrl Pts',(162.63640098715,225.320832085337,12.9088153529799));
#73639=CARTESIAN_POINT('Ctrl Pts',(162.355349084878,226.227140611498,12.9617346413905));
#73640=CARTESIAN_POINT('Ctrl Pts',(161.757897732615,226.808027043178,13.0146539298011));
#73641=CARTESIAN_POINT('Ctrl Pts',(161.160446380351,227.388913474857,13.0675732182117));
#73642=CARTESIAN_POINT('Ctrl Pts',(160.246595578096,227.644377812055,13.1204925066223));
#73643=CARTESIAN_POINT('Ctrl Pts',(159.434523434992,227.457519579092,13.1734117950329));
#73644=CARTESIAN_POINT('Ctrl Pts',(158.622451291889,227.27066134613,13.2263310834435));
#73645=CARTESIAN_POINT('Ctrl Pts',(157.912157807938,226.641480543007,13.2792503718541));
#73646=CARTESIAN_POINT('Ctrl Pts',(157.628673267428,225.857890292861,13.3321696602647));
#73647=CARTESIAN_POINT('Ctrl Pts',(157.530021897025,225.585204340136,13.3505853393458));
#73648=CARTESIAN_POINT('Ctrl Pts',(157.483057487382,225.293819259495,13.3690010184269));
#73649=CARTESIAN_POINT('Ctrl Pts',(157.485016106425,225.001823857836,13.387416697508));
#73650=CARTESIAN_POINT('Origin',(160.,225.,10.));
#73651=CARTESIAN_POINT('',(157.485110394447,224.998220537442,14.387416697508));
#73652=CARTESIAN_POINT('',(157.479399062161,224.998500607783,14.112583302492));
#73653=CARTESIAN_POINT('',(157.4825,225.,10.));
#73654=CARTESIAN_POINT('Ctrl Pts',(157.479399062161,224.998500607783,14.112583302492));
#73655=CARTESIAN_POINT('Ctrl Pts',(157.484655142802,225.744155612533,14.0652862484606));
#73656=CARTESIAN_POINT('Ctrl Pts',(157.836334781685,226.494118132385,14.0179891944291));
#73657=CARTESIAN_POINT('Ctrl Pts',(158.415784449147,226.961995452392,13.9706921403977));
#73658=CARTESIAN_POINT('Ctrl Pts',(159.064113709812,227.485489681477,13.9177728519871));
#73659=CARTESIAN_POINT('Ctrl Pts',(159.997581815393,227.655849441756,13.8648535635765));
#73660=CARTESIAN_POINT('Ctrl Pts',(160.789033779131,227.395118110274,13.8119342751659));
#73661=CARTESIAN_POINT('Ctrl Pts',(161.580485742868,227.134386778792,13.7590149867553));
#73662=CARTESIAN_POINT('Ctrl Pts',(162.229921564762,226.442564355549,13.7060956983447));
#73663=CARTESIAN_POINT('Ctrl Pts',(162.440159425482,225.636228767819,13.6531764099341));
#73664=CARTESIAN_POINT('Ctrl Pts',(162.650397286203,224.829893180089,13.6002571215235));
#73665=CARTESIAN_POINT('Ctrl Pts',(162.42143718575,223.909044427871,13.5473378331129));
#73666=CARTESIAN_POINT('Ctrl Pts',(161.85805126159,223.295062882075,13.4944185447023));
#73667=CARTESIAN_POINT('Ctrl Pts',(161.294665337429,222.681081336279,13.4414992562918));
#73668=CARTESIAN_POINT('Ctrl Pts',(160.396853589561,222.373966996905,13.3885799678811));
#73669=CARTESIAN_POINT('Ctrl Pts',(159.575454656156,222.514255379611,13.3356606794705));
#73670=CARTESIAN_POINT('Ctrl Pts',(158.754055722752,222.654543762317,13.28274139106));
#73671=CARTESIAN_POINT('Ctrl Pts',(158.009069603811,223.242234867105,13.2298221026494));
#73672=CARTESIAN_POINT('Ctrl Pts',(157.681401932714,224.008401255977,13.1769028142388));
#73673=CARTESIAN_POINT('Ctrl Pts',(157.548649929596,224.318807596962,13.1554629769898));
#73674=CARTESIAN_POINT('Ctrl Pts',(157.484396662942,224.658508908041,13.1340231397409));
#73675=CARTESIAN_POINT('Ctrl Pts',(157.485914018718,224.998759312188,13.112583302492));
#73676=CARTESIAN_POINT('Ctrl Pts',(157.485016106425,225.001823857836,13.387416697508));
#73677=CARTESIAN_POINT('Ctrl Pts',(157.48868577432,224.454741384228,13.4219203068375));
#73678=CARTESIAN_POINT('Ctrl Pts',(157.664093645276,223.905516454647,13.456423916167));
#73679=CARTESIAN_POINT('Ctrl Pts',(157.993061232263,223.473119844339,13.4909275254965));
#73680=CARTESIAN_POINT('Ctrl Pts',(158.497609334675,222.80993934313,13.5438468139071));
#73681=CARTESIAN_POINT('Ctrl Pts',(159.363381136564,222.42157803788,13.5967661023177));
#73682=CARTESIAN_POINT('Ctrl Pts',(160.19419947841,222.485750054235,13.6496853907283));
#73683=CARTESIAN_POINT('Ctrl Pts',(161.025017820256,222.54992207059,13.7026046791389));
#73684=CARTESIAN_POINT('Ctrl Pts',(161.820882702058,223.06662740855,13.7555239675495));
#73685=CARTESIAN_POINT('Ctrl Pts',(162.217606369553,223.799421715624,13.8084432559601));
#73686=CARTESIAN_POINT('Ctrl Pts',(162.614330037047,224.532216022699,13.8613625443707));
#73687=CARTESIAN_POINT('Ctrl Pts',(162.611912490233,225.481099298887,13.9142818327813));
#73688=CARTESIAN_POINT('Ctrl Pts',(162.211459998486,226.211862575663,13.9672011211919));
#73689=CARTESIAN_POINT('Ctrl Pts',(161.811007506738,226.942625852439,14.0201204096025));
#73690=CARTESIAN_POINT('Ctrl Pts',(161.012520070057,227.455269129802,14.0730396980131));
#73691=CARTESIAN_POINT('Ctrl Pts',(160.181385523768,227.51520685411,14.1259589864237));
#73692=CARTESIAN_POINT('Ctrl Pts',(159.350250977479,227.575144578419,14.1788782748343));
#73693=CARTESIAN_POINT('Ctrl Pts',(158.486469321582,227.182376749673,14.2317975632449));
#73694=CARTESIAN_POINT('Ctrl Pts',(157.985307024831,226.516633918584,14.2847168516555));
#73695=CARTESIAN_POINT('Ctrl Pts',(157.661107083314,226.085967469206,14.3189501336063));
#73696=CARTESIAN_POINT('Ctrl Pts',(157.488654125966,225.541067920259,14.3531834155572));
#73697=CARTESIAN_POINT('Ctrl Pts',(157.485110394447,224.998220537442,14.387416697508));
#73698=CARTESIAN_POINT('Origin',(160.,225.,10.));
#73699=CARTESIAN_POINT('',(157.47858851104,224.999178326175,15.387416697508));
#73700=CARTESIAN_POINT('',(157.481369652601,225.002195372979,15.112583302492));
#73701=CARTESIAN_POINT('',(157.4825,225.,10.));
#73702=CARTESIAN_POINT('Ctrl Pts',(157.481369652601,225.002195372979,15.112583302492));
#73703=CARTESIAN_POINT('Ctrl Pts',(157.479896180238,225.16325630262,15.1023879340014));
#73704=CARTESIAN_POINT('Ctrl Pts',(157.494022383079,225.324059777303,15.0921925655108));
#73705=CARTESIAN_POINT('Ctrl Pts',(157.524685344636,225.481645537413,15.0819971970203));
#73706=CARTESIAN_POINT('Ctrl Pts',(157.683842133094,226.299597953393,15.0290779086097));
#73707=CARTESIAN_POINT('Ctrl Pts',(158.288524381302,227.030860239281,14.9761586201991));
#73708=CARTESIAN_POINT('Ctrl Pts',(159.062029504368,227.340806787434,14.9232393317885));
#73709=CARTESIAN_POINT('Ctrl Pts',(159.835534627433,227.650753335586,14.8703200433779));
#73710=CARTESIAN_POINT('Ctrl Pts',(160.777862625357,227.539384146001,14.8174007549673));
#73711=CARTESIAN_POINT('Ctrl Pts',(161.457804224818,227.057661757645,14.7644814665567));
#73712=CARTESIAN_POINT('Ctrl Pts',(162.137745824278,226.575939369289,14.7115621781461));
#73713=CARTESIAN_POINT('Ctrl Pts',(162.555301025275,225.72386378216,14.6586428897355));
#73714=CARTESIAN_POINT('Ctrl Pts',(162.519396576041,224.891344768175,14.6057236013249));
#73715=CARTESIAN_POINT('Ctrl Pts',(162.483492126808,224.058825754191,14.5528043129143));
#73716=CARTESIAN_POINT('Ctrl Pts',(161.994128027345,223.245863313351,14.4998850245037));
#73717=CARTESIAN_POINT('Ctrl Pts',(161.275237279945,222.824469042599,14.4469657360931));
#73718=CARTESIAN_POINT('Ctrl Pts',(160.556346532544,222.403074771847,14.3940464476825));
#73719=CARTESIAN_POINT('Ctrl Pts',(159.607929137207,222.373248671183,14.3411271592719));
#73720=CARTESIAN_POINT('Ctrl Pts',(158.86398087539,222.748639163685,14.2882078708613));
#73721=CARTESIAN_POINT('Ctrl Pts',(158.120032613574,223.124029656187,14.2352885824507));
#73722=CARTESIAN_POINT('Ctrl Pts',(157.580553485279,223.904636741854,14.1823692940401));
#73723=CARTESIAN_POINT('Ctrl Pts',(157.492409129006,224.733254633634,14.1294500056295));
#73724=CARTESIAN_POINT('Ctrl Pts',(157.483044524056,224.821288394826,14.1238277712503));
#73725=CARTESIAN_POINT('Ctrl Pts',(157.478774268125,224.909864068181,14.1182055368711));
#73726=CARTESIAN_POINT('Ctrl Pts',(157.479399062161,224.998500607783,14.112583302492));
#73727=CARTESIAN_POINT('Ctrl Pts',(157.485110394447,224.998220537442,14.387416697508));
#73728=CARTESIAN_POINT('Ctrl Pts',(157.483176072458,224.70191094853,14.4061027039678));
#73729=CARTESIAN_POINT('Ctrl Pts',(157.531567388157,224.406212791993,14.4247887104275));
#73730=CARTESIAN_POINT('Ctrl Pts',(157.633075457542,224.13003768041,14.4434747168873));
#73731=CARTESIAN_POINT('Ctrl Pts',(157.920549124609,223.347902106756,14.4963940052978));
#73732=CARTESIAN_POINT('Ctrl Pts',(158.634039396345,222.722348792881,14.5493132937084));
#73733=CARTESIAN_POINT('Ctrl Pts',(159.447053138434,222.539630922914,14.602232582119));
#73734=CARTESIAN_POINT('Ctrl Pts',(160.260066880523,222.356913052947,14.6551518705296));
#73735=CARTESIAN_POINT('Ctrl Pts',(161.172604092964,222.617030626888,14.7080711589402));
#73736=CARTESIAN_POINT('Ctrl Pts',(161.767087765287,223.200953848016,14.7609904473508));
#73737=CARTESIAN_POINT('Ctrl Pts',(162.36157143761,223.784877069144,14.8139097357614));
#73738=CARTESIAN_POINT('Ctrl Pts',(162.638001569814,224.692605937458,14.866829024172));
#73739=CARTESIAN_POINT('Ctrl Pts',(162.469883738838,225.508763740667,14.9197483125826));
#73740=CARTESIAN_POINT('Ctrl Pts',(162.301765907862,226.324921543876,14.9726676009932));
#73741=CARTESIAN_POINT('Ctrl Pts',(161.689100113707,227.04950828198,15.0255868894038));
#73742=CARTESIAN_POINT('Ctrl Pts',(160.912242211731,227.350953077867,15.0785061778144));
#73743=CARTESIAN_POINT('Ctrl Pts',(160.135384309754,227.652397873755,15.131425466225));
#73744=CARTESIAN_POINT('Ctrl Pts',(159.194334299958,227.530700727426,15.1843447546356));
#73745=CARTESIAN_POINT('Ctrl Pts',(158.51971664832,227.041550250651,15.2372640430462));
#73746=CARTESIAN_POINT('Ctrl Pts',(157.88166554457,226.578913376491,15.2873149278668));
#73747=CARTESIAN_POINT('Ctrl Pts',(157.481946516999,225.787578007339,15.3373658126874));
#73748=CARTESIAN_POINT('Ctrl Pts',(157.47858851104,224.999178326175,15.387416697508));
#73749=CARTESIAN_POINT('Origin',(160.,225.,10.));
#73750=CARTESIAN_POINT('',(157.482687981659,225.002301033995,16.387416697508));
#73751=CARTESIAN_POINT('',(157.486512950876,225.000116346801,16.112583302492));
#73752=CARTESIAN_POINT('',(157.4825,225.,10.));
#73753=CARTESIAN_POINT('Ctrl Pts',(157.486512950876,225.000116346801,16.112583302492));
#73754=CARTESIAN_POINT('Ctrl Pts',(157.486342648081,225.413188232998,16.0865703311317));
#73755=CARTESIAN_POINT('Ctrl Pts',(157.582487768739,225.826185463148,16.0605573597713));
#73756=CARTESIAN_POINT('Ctrl Pts',(157.775382536625,226.187536192458,16.034544388411));
#73757=CARTESIAN_POINT('Ctrl Pts',(158.167796525526,226.922647272114,15.9816251000004));
#73758=CARTESIAN_POINT('Ctrl Pts',(158.960613637304,227.444016794936,15.9287058115898));
#73759=CARTESIAN_POINT('Ctrl Pts',(159.79104077721,227.513066077522,15.8757865231792));
#73760=CARTESIAN_POINT('Ctrl Pts',(160.621467917115,227.582115360107,15.8228672347686));
#73761=CARTESIAN_POINT('Ctrl Pts',(161.489505085149,227.198844402455,15.769947946358));
#73762=CARTESIAN_POINT('Ctrl Pts',(161.99793849028,226.538637987256,15.7170286579474));
#73763=CARTESIAN_POINT('Ctrl Pts',(162.506371895412,225.878431572058,15.6641093695368));
#73764=CARTESIAN_POINT('Ctrl Pts',(162.65520153764,224.941289699314,15.6111900811262));
#73765=CARTESIAN_POINT('Ctrl Pts',(162.376322975611,224.156048471562,15.5582707927157));
#73766=CARTESIAN_POINT('Ctrl Pts',(162.097444413582,223.370807243811,15.5053515043051));
#73767=CARTESIAN_POINT('Ctrl Pts',(161.390857647295,222.737466661052,15.4524322158944));
#73768=CARTESIAN_POINT('Ctrl Pts',(160.57989676711,222.545843361505,15.3995129274839));
#73769=CARTESIAN_POINT('Ctrl Pts',(159.768935886925,222.354220061959,15.3465936390733));
#73770=CARTESIAN_POINT('Ctrl Pts',(158.853600892841,222.604314045624,15.2936743506627));
#73771=CARTESIAN_POINT('Ctrl Pts',(158.252749060154,223.181682310492,15.2407550622521));
#73772=CARTESIAN_POINT('Ctrl Pts',(157.767656641972,223.647815477689,15.198031142332));
#73773=CARTESIAN_POINT('Ctrl Pts',(157.487544271528,224.327265941386,15.155307222412));
#73774=CARTESIAN_POINT('Ctrl Pts',(157.481369652601,225.002195372979,15.112583302492));
#73775=CARTESIAN_POINT('Ctrl Pts',(157.47858851104,224.999178326175,15.387416697508));
#73776=CARTESIAN_POINT('Ctrl Pts',(157.478396064566,224.953995339222,15.390285101098));
#73777=CARTESIAN_POINT('Ctrl Pts',(157.479505429084,224.908821994265,15.393153504688));
#73778=CARTESIAN_POINT('Ctrl Pts',(157.481946350156,224.863720714323,15.396021908278));
#73779=CARTESIAN_POINT('Ctrl Pts',(157.526978997108,224.031645461992,15.4489411966886));
#73780=CARTESIAN_POINT('Ctrl Pts',(158.025229584489,223.224098764553,15.5018604850992));
#73781=CARTESIAN_POINT('Ctrl Pts',(158.74869865331,222.810613974884,15.5547797735098));
#73782=CARTESIAN_POINT('Ctrl Pts',(159.472167722131,222.397129185214,15.6076990619204));
#73783=CARTESIAN_POINT('Ctrl Pts',(160.42085527239,222.377706303315,15.660618350331));
#73784=CARTESIAN_POINT('Ctrl Pts',(161.160641899746,222.761233239543,15.7135376387416));
#73785=CARTESIAN_POINT('Ctrl Pts',(161.900428527103,223.144760175772,15.7664569271522));
#73786=CARTESIAN_POINT('Ctrl Pts',(162.431314231556,223.931236930129,15.8193762155628));
#73787=CARTESIAN_POINT('Ctrl Pts',(162.51036572518,224.760771755319,15.8722955039734));
#73788=CARTESIAN_POINT('Ctrl Pts',(162.589417218803,225.590306580509,15.925214792384));
#73789=CARTESIAN_POINT('Ctrl Pts',(162.216634501596,226.462899476532,15.9781340807946));
#73790=CARTESIAN_POINT('Ctrl Pts',(161.562602937639,226.979251951253,16.0310533692052));
#73791=CARTESIAN_POINT('Ctrl Pts',(160.908571373682,227.495604425974,16.0839726576158));
#73792=CARTESIAN_POINT('Ctrl Pts',(159.973290962974,227.655716479393,16.1368919460264));
#73793=CARTESIAN_POINT('Ctrl Pts',(159.184746003034,227.386320839163,16.189811234437));
#73794=CARTESIAN_POINT('Ctrl Pts',(158.396201043094,227.116925198932,16.2427305228476));
#73795=CARTESIAN_POINT('Ctrl Pts',(157.754391533921,226.418021865052,16.2956498112582));
#73796=CARTESIAN_POINT('Ctrl Pts',(157.553009494362,225.609428989055,16.3485690996688));
#73797=CARTESIAN_POINT('Ctrl Pts',(157.503731882362,225.41156861334,16.3615182989485));
#73798=CARTESIAN_POINT('Ctrl Pts',(157.480825612644,225.207140390115,16.3744674982282));
#73799=CARTESIAN_POINT('Ctrl Pts',(157.482687981659,225.002301033995,16.387416697508));
#73800=CARTESIAN_POINT('Origin',(160.,225.,10.));
#73801=CARTESIAN_POINT('',(157.486388012783,224.99940538485,17.387416697508));
#73802=CARTESIAN_POINT('',(157.481796636001,224.997743576325,17.112583302492));
#73803=CARTESIAN_POINT('',(157.4825,225.,10.));
#73804=CARTESIAN_POINT('Ctrl Pts',(157.481796636001,224.997743576325,17.112583302492));
#73805=CARTESIAN_POINT('Ctrl Pts',(157.48789794461,225.658848742086,17.0707527282619));
#73806=CARTESIAN_POINT('Ctrl Pts',(157.75518214039,226.324319915578,17.0289221540318));
#73807=CARTESIAN_POINT('Ctrl Pts',(158.222379264903,226.78863903208,16.9870915798018));
#73808=CARTESIAN_POINT('Ctrl Pts',(158.813423969208,227.376042807739,16.9341722913912));
#73809=CARTESIAN_POINT('Ctrl Pts',(159.724418014731,227.641514087453,16.8812530029806));
#73810=CARTESIAN_POINT('Ctrl Pts',(160.538490545154,227.463573217911,16.82833371457));
#73811=CARTESIAN_POINT('Ctrl Pts',(161.352563075576,227.285632348368,16.7754144261594));
#73812=CARTESIAN_POINT('Ctrl Pts',(162.069714090897,226.664279329569,16.7224951377488));
#73813=CARTESIAN_POINT('Ctrl Pts',(162.361775300124,225.883845291148,16.6695758493382));
#73814=CARTESIAN_POINT('Ctrl Pts',(162.653836509352,225.103411252728,16.6166565609276));
#73815=CARTESIAN_POINT('Ctrl Pts',(162.520807912486,224.163896194687,16.563737272517));
#73816=CARTESIAN_POINT('Ctrl Pts',(162.02356339307,223.495222188895,16.5108179841064));
#73817=CARTESIAN_POINT('Ctrl Pts',(161.526318873653,222.826548183103,16.4578986956958));
#73818=CARTESIAN_POINT('Ctrl Pts',(160.664858431685,222.428715229559,16.4049794072852));
#73819=CARTESIAN_POINT('Ctrl Pts',(159.833386348361,222.483771680089,16.3520601188746));
#73820=CARTESIAN_POINT('Ctrl Pts',(159.001914265037,222.538828130619,16.299140830464));
#73821=CARTESIAN_POINT('Ctrl Pts',(158.200430540357,223.046773985221,16.2462215420534));
#73822=CARTESIAN_POINT('Ctrl Pts',(157.795694111028,223.775173230767,16.1933022536428));
#73823=CARTESIAN_POINT('Ctrl Pts',(157.589909660474,224.145521011859,16.1663959365925));
#73824=CARTESIAN_POINT('Ctrl Pts',(157.486689102264,224.57285861524,16.1394896195422));
#73825=CARTESIAN_POINT('Ctrl Pts',(157.486512950876,225.000116346801,16.112583302492));
#73826=CARTESIAN_POINT('Ctrl Pts',(157.482687981659,225.002301033995,16.387416697508));
#73827=CARTESIAN_POINT('Ctrl Pts',(157.488436526714,224.370026624993,16.4273867866388));
#73828=CARTESIAN_POINT('Ctrl Pts',(157.73017123711,223.733835098205,16.4673568757697));
#73829=CARTESIAN_POINT('Ctrl Pts',(158.16075860029,223.274787751828,16.5073269649006));
#73830=CARTESIAN_POINT('Ctrl Pts',(158.730844315724,222.667021808713,16.5602462533112));
#73831=CARTESIAN_POINT('Ctrl Pts',(159.631970316536,222.369772340596,16.6131655417218));
#73832=CARTESIAN_POINT('Ctrl Pts',(160.451781362769,222.519060696911,16.6660848301324));
#73833=CARTESIAN_POINT('Ctrl Pts',(161.271592409001,222.668349053226,16.719004118543));
#73834=CARTESIAN_POINT('Ctrl Pts',(162.010088500653,223.264175233973,16.7719234069535));
#73835=CARTESIAN_POINT('Ctrl Pts',(162.329333840094,224.033889193323,16.8248426953641));
#73836=CARTESIAN_POINT('Ctrl Pts',(162.648579179535,224.803603152672,16.8777619837747));
#73837=CARTESIAN_POINT('Ctrl Pts',(162.548573766764,225.747204890625,16.9306812721853));
#73838=CARTESIAN_POINT('Ctrl Pts',(162.075080077969,226.432902264707,16.9836005605959));
#73839=CARTESIAN_POINT('Ctrl Pts',(161.601586389173,227.118599638789,17.0365198490065));
#73840=CARTESIAN_POINT('Ctrl Pts',(160.754604424353,227.546392649001,17.0894391374171));
#73841=CARTESIAN_POINT('Ctrl Pts',(159.921713111323,227.52052323419,17.1423584258277));
#73842=CARTESIAN_POINT('Ctrl Pts',(159.088821798293,227.49465381938,17.1952777142383));
#73843=CARTESIAN_POINT('Ctrl Pts',(158.270021137053,227.015121979548,17.2481970026489));
#73844=CARTESIAN_POINT('Ctrl Pts',(157.839994299551,226.301361450457,17.3011162910595));
#73845=CARTESIAN_POINT('Ctrl Pts',(157.606232710443,225.913362886245,17.329883093209));
#73846=CARTESIAN_POINT('Ctrl Pts',(157.487353176809,225.456150111532,17.3586498953585));
#73847=CARTESIAN_POINT('Ctrl Pts',(157.486388012783,224.99940538485,17.387416697508));
#73848=CARTESIAN_POINT('Origin',(160.,225.,10.));
#73849=CARTESIAN_POINT('',(157.480508380744,224.998011611683,18.387416697508));
#73850=CARTESIAN_POINT('',(157.479093530148,225.001296842243,18.112583302492));
#73851=CARTESIAN_POINT('',(157.4825,225.,10.));
#73852=CARTESIAN_POINT('Ctrl Pts',(157.479093530148,225.001296842243,18.112583302492));
#73853=CARTESIAN_POINT('Ctrl Pts',(157.478625650357,225.075825676239,18.1078544138028));
#73854=CARTESIAN_POINT('Ctrl Pts',(157.481644355634,225.150316077051,18.1031255251135));
#73855=CARTESIAN_POINT('Ctrl Pts',(157.488273041435,225.224483837494,18.0983966364243));
#73856=CARTESIAN_POINT('Ctrl Pts',(157.562452274396,226.054468504842,18.0454773480137));
#73857=CARTESIAN_POINT('Ctrl Pts',(158.088710854837,226.844048785844,17.9925580596031));
#73858=CARTESIAN_POINT('Ctrl Pts',(158.826232701178,227.231912914062,17.9396387711925));
#73859=CARTESIAN_POINT('Ctrl Pts',(159.563754547518,227.619777042281,17.8867194827819));
#73860=CARTESIAN_POINT('Ctrl Pts',(160.512539659759,227.605925017717,17.8338001943713));
#73861=CARTESIAN_POINT('Ctrl Pts',(161.238424068964,227.196695452017,17.7808809059607));
#73862=CARTESIAN_POINT('Ctrl Pts',(161.964308478168,226.787465886318,17.7279616175501));
#73863=CARTESIAN_POINT('Ctrl Pts',(162.467292184337,225.982858779483,17.6750423291395));
#73864=CARTESIAN_POINT('Ctrl Pts',(162.517209814972,225.151062363695,17.622123040729));
#73865=CARTESIAN_POINT('Ctrl Pts',(162.567127445607,224.319265947907,17.5692037523184));
#73866=CARTESIAN_POINT('Ctrl Pts',(162.163979000708,223.460280223166,17.5162844639078));
#73867=CARTESIAN_POINT('Ctrl Pts',(161.492245219262,222.967177022915,17.4633651754972));
#73868=CARTESIAN_POINT('Ctrl Pts',(160.820511437816,222.474073822664,17.4104458870866));
#73869=CARTESIAN_POINT('Ctrl Pts',(159.880192319824,222.346853146903,17.357526598676));
#73870=CARTESIAN_POINT('Ctrl Pts',(159.10157786626,222.643731182701,17.3046073102654));
#73871=CARTESIAN_POINT('Ctrl Pts',(158.322963412696,222.940609218499,17.2516880218548));
#73872=CARTESIAN_POINT('Ctrl Pts',(157.706053623561,223.661585965856,17.1987687334442));
#73873=CARTESIAN_POINT('Ctrl Pts',(157.533146410537,224.476742475336,17.1458494450336));
#73874=CARTESIAN_POINT('Ctrl Pts',(157.496915411924,224.647550470257,17.134760730853));
#73875=CARTESIAN_POINT('Ctrl Pts',(157.48017926238,224.822493621923,17.1236720166725));
#73876=CARTESIAN_POINT('Ctrl Pts',(157.481796636001,224.997743576325,17.112583302492));
#73877=CARTESIAN_POINT('Ctrl Pts',(157.486388012783,224.99940538485,17.387416697508));
#73878=CARTESIAN_POINT('Ctrl Pts',(157.48557766512,224.615924430704,17.4115691837691));
#73879=CARTESIAN_POINT('Ctrl Pts',(157.567887645435,224.232773413495,17.4357216700302));
#73880=CARTESIAN_POINT('Ctrl Pts',(157.735112625212,223.891193694375,17.4598741562913));
#73881=CARTESIAN_POINT('Ctrl Pts',(158.101510802135,223.142775685731,17.5127934447019));
#73882=CARTESIAN_POINT('Ctrl Pts',(158.875560169744,222.593928886793,17.5657127331125));
#73883=CARTESIAN_POINT('Ctrl Pts',(159.703055776172,222.495805475537,17.6186320215231));
#73884=CARTESIAN_POINT('Ctrl Pts',(160.530551382599,222.397682064281,17.6715513099337));
#73885=CARTESIAN_POINT('Ctrl Pts',(161.411493227846,222.750282040708,17.7244705983443));
#73886=CARTESIAN_POINT('Ctrl Pts',(161.942762292016,223.392255883383,17.7773898867549));
#73887=CARTESIAN_POINT('Ctrl Pts',(162.474031356186,224.034229726058,17.8303091751655));
#73888=CARTESIAN_POINT('Ctrl Pts',(162.65562763928,224.965577434981,17.8832284635761));
#73889=CARTESIAN_POINT('Ctrl Pts',(162.404452787055,225.760113858579,17.9361477519867));
#73890=CARTESIAN_POINT('Ctrl Pts',(162.153277934831,226.554650282177,17.9890670403973));
#73891=CARTESIAN_POINT('Ctrl Pts',(161.46933194729,227.212375420449,18.0419863288079));
#73892=CARTESIAN_POINT('Ctrl Pts',(160.665588284605,227.432315214048,18.0949056172185));
#73893=CARTESIAN_POINT('Ctrl Pts',(159.861844621921,227.652255007647,18.1478249056291));
#73894=CARTESIAN_POINT('Ctrl Pts',(158.938303284093,227.434409456573,18.2007441940397));
#73895=CARTESIAN_POINT('Ctrl Pts',(158.317577205504,226.878462707285,18.2536634824503));
#73896=CARTESIAN_POINT('Ctrl Pts',(157.794616604086,226.410078573941,18.2982478874695));
#73897=CARTESIAN_POINT('Ctrl Pts',(157.48659524579,225.701709124714,18.3428322924888));
#73898=CARTESIAN_POINT('Ctrl Pts',(157.480508380744,224.998011611683,18.387416697508));
#73899=CARTESIAN_POINT('Origin',(160.,225.,10.));
#73900=CARTESIAN_POINT('',(157.480142558574,225.001823580074,19.387416697508));
#73901=CARTESIAN_POINT('',(157.485690591028,225.001427433753,19.112583302492));
#73902=CARTESIAN_POINT('',(157.4825,225.,10.));
#73903=CARTESIAN_POINT('',(161.913465996665,226.635987203375,20.));
#73904=CARTESIAN_POINT('Ctrl Pts',(157.480142558574,225.001823580074,19.387416697508));
#73905=CARTESIAN_POINT('Ctrl Pts',(157.486035875252,224.285086609627,19.4328532664402));
#73906=CARTESIAN_POINT('Ctrl Pts',(157.807332972564,223.563823321433,19.4782898353724));
#73907=CARTESIAN_POINT('Ctrl Pts',(158.347923825584,223.094934991001,19.5237264043046));
#73908=CARTESIAN_POINT('Ctrl Pts',(158.977541860912,222.548827805233,19.5766456927152));
#73909=CARTESIAN_POINT('Ctrl Pts',(159.904629913844,222.345064991681,19.6295649811258));
#73910=CARTESIAN_POINT('Ctrl Pts',(160.704626516463,222.578292344923,19.6824842695364));
#73911=CARTESIAN_POINT('Ctrl Pts',(161.504623119081,222.811519698165,19.735403557947));
#73912=CARTESIAN_POINT('Ctrl Pts',(162.177528271386,223.481737218202,19.7883228463576));
#73913=CARTESIAN_POINT('Ctrl Pts',(162.415731120478,224.278796422505,19.8412421347682));
#73914=CARTESIAN_POINT('Ctrl Pts',(162.653933969571,225.075855626809,19.8941614231788));
#73915=CARTESIAN_POINT('Ctrl Pts',(162.457434515453,225.999756515379,19.9470807115894));
#73916=CARTESIAN_POINT('Ctrl Pts',(161.913465996665,226.635987203375,20.));
#73917=CARTESIAN_POINT('',(158.082847419036,226.638754849416,20.));
#73918=CARTESIAN_POINT('Origin',(160.,225.,20.));
#73919=CARTESIAN_POINT('Ctrl Pts',(158.082843717471,226.638757628308,20.));
#73920=CARTESIAN_POINT('Ctrl Pts',(158.613381501441,227.257451085127,19.948244384658));
#73921=CARTESIAN_POINT('Ctrl Pts',(159.472376079816,227.597124236137,19.896488769316));
#73922=CARTESIAN_POINT('Ctrl Pts',(160.282371283694,227.505771932288,19.844733153974));
#73923=CARTESIAN_POINT('Ctrl Pts',(161.110578416814,227.412365663568,19.7918138655635));
#73924=CARTESIAN_POINT('Ctrl Pts',(161.887558001259,226.868333694107,19.7388945771529));
#73925=CARTESIAN_POINT('Ctrl Pts',(162.258272057625,226.122147391606,19.6859752887423));
#73926=CARTESIAN_POINT('Ctrl Pts',(162.628986113992,225.375961089105,19.6330560003317));
#73927=CARTESIAN_POINT('Ctrl Pts',(162.59343464228,224.427620453564,19.5801367119211));
#73928=CARTESIAN_POINT('Ctrl Pts',(162.167641122797,223.711314725108,19.5272174235105));
#73929=CARTESIAN_POINT('Ctrl Pts',(161.741847603315,222.995008996652,19.4742981350999));
#73930=CARTESIAN_POINT('Ctrl Pts',(160.925812036062,222.510738175281,19.4213788466893));
#73931=CARTESIAN_POINT('Ctrl Pts',(160.093070271787,222.479994334415,19.3684595582787));
#73932=CARTESIAN_POINT('Ctrl Pts',(159.260328507511,222.44925049355,19.3155402698681));
#73933=CARTESIAN_POINT('Ctrl Pts',(158.410880546213,222.87203363319,19.2626209814575));
#73934=CARTESIAN_POINT('Ctrl Pts',(157.93337689175,223.554931319872,19.2097016930469));
#73935=CARTESIAN_POINT('Ctrl Pts',(157.641269245065,223.972686523039,19.1773288961952));
#73936=CARTESIAN_POINT('Ctrl Pts',(157.488352346154,224.48778301533,19.1449560993436));
#73937=CARTESIAN_POINT('Ctrl Pts',(157.485690591028,225.001427433753,19.112583302492));
#73938=CARTESIAN_POINT('Origin',(-160.,225.,10.));
#73939=CARTESIAN_POINT('',(-162.513515873292,225.000575080101,0.387416697508026));
#73940=CARTESIAN_POINT('',(-162.515402535198,224.996259729968,0.112583302491934));
#73941=CARTESIAN_POINT('',(-162.5175,225.,10.));
#73942=CARTESIAN_POINT('',(-161.913465996665,226.635987203375,0.));
#73943=CARTESIAN_POINT('Ctrl Pts',(-162.515402535198,224.996259729968,0.112583302491934));
#73944=CARTESIAN_POINT('Ctrl Pts',(-162.51023742721,225.58895227201,0.0750555349946119));
#73945=CARTESIAN_POINT('Ctrl Pts',(-162.299221828084,226.184803560304,0.0375277674972904));
#73946=CARTESIAN_POINT('Ctrl Pts',(-161.913465996665,226.635987203375,-3.15025783237388E-14));
#73947=CARTESIAN_POINT('',(-158.082847392586,226.638754884714,3.03954323567685E-15));
#73948=CARTESIAN_POINT('Origin',(-160.,225.,0.));
#73949=CARTESIAN_POINT('Ctrl Pts',(-158.082843691308,226.638757663408,2.26599577176544E-15));
#73950=CARTESIAN_POINT('Ctrl Pts',(-158.613381466828,227.257451072063,0.0517556153419928));
#73951=CARTESIAN_POINT('Ctrl Pts',(-159.47237606495,227.597124296558,0.103511230683983));
#73952=CARTESIAN_POINT('Ctrl Pts',(-160.282371286662,227.505772004605,0.155266846025974));
#73953=CARTESIAN_POINT('Ctrl Pts',(-161.110578438016,227.412365748049,0.20818613443657));
#73954=CARTESIAN_POINT('Ctrl Pts',(-161.887558038694,226.868333726363,0.261105422847168));
#73955=CARTESIAN_POINT('Ctrl Pts',(-162.258272100966,226.122147400466,0.314024711257765));
#73956=CARTESIAN_POINT('Ctrl Pts',(-162.429649067526,225.777193804055,0.338488706674519));
#73957=CARTESIAN_POINT('Ctrl Pts',(-162.514202638506,225.38903761854,0.362952702091273));
#73958=CARTESIAN_POINT('Ctrl Pts',(-162.513515873292,225.000575080101,0.387416697508026));
#73959=CARTESIAN_POINT('Origin',(-160.,225.,10.));
#73960=CARTESIAN_POINT('',(-162.517460047887,224.997698761843,1.38741669750802));
#73961=CARTESIAN_POINT('',(-162.521728513626,225.00013531689,1.11258330249193));
#73962=CARTESIAN_POINT('',(-162.5175,225.,10.));
#73963=CARTESIAN_POINT('Ctrl Pts',(-162.521728513626,225.00013531689,1.11258330249193));
#73964=CARTESIAN_POINT('Ctrl Pts',(-162.52173338627,225.006844584385,1.11215722053546));
#73965=CARTESIAN_POINT('Ctrl Pts',(-162.521708943191,225.013553813481,1.11173113857898));
#73966=CARTESIAN_POINT('Ctrl Pts',(-162.521655077588,225.020262804259,1.11130505662251));
#73967=CARTESIAN_POINT('Ctrl Pts',(-162.514964981143,225.853518032503,1.05838576821191));
#73968=CARTESIAN_POINT('Ctrl Pts',(-162.054415170727,226.683097057043,1.00546647980131));
#73969=CARTESIAN_POINT('Ctrl Pts',(-161.35073645221,227.129460505748,0.952547191390717));
#73970=CARTESIAN_POINT('Ctrl Pts',(-160.647057733692,227.575823954453,0.899627902980116));
#73971=CARTESIAN_POINT('Ctrl Pts',(-159.700250107072,227.638971827323,0.846708614569517));
#73972=CARTESIAN_POINT('Ctrl Pts',(-158.943607525641,227.289850001498,0.793789326158917));
#73973=CARTESIAN_POINT('Ctrl Pts',(-158.186964944209,226.940728175673,0.740870037748322));
#73974=CARTESIAN_POINT('Ctrl Pts',(-157.620487407966,226.179336651153,0.687950749337727));
#73975=CARTESIAN_POINT('Ctrl Pts',(-157.503322677412,225.354415202511,0.635031460927131));
#73976=CARTESIAN_POINT('Ctrl Pts',(-157.386157946857,224.529493753869,0.582112172516532));
#73977=CARTESIAN_POINT('Ctrl Pts',(-157.718306021991,223.641042381106,0.529192884105933));
#73978=CARTESIAN_POINT('Ctrl Pts',(-158.347923979622,223.094935196484,0.476273595695335));
#73979=CARTESIAN_POINT('Ctrl Pts',(-158.977541937253,222.548828011861,0.423354307284738));
#73980=CARTESIAN_POINT('Ctrl Pts',(-159.90462977738,222.345065015378,0.370435018874142));
#73981=CARTESIAN_POINT('Ctrl Pts',(-160.704626519453,222.578292509213,0.317515730463546));
#73982=CARTESIAN_POINT('Ctrl Pts',(-161.504623261526,222.811520003047,0.264596442052949));
#73983=CARTESIAN_POINT('Ctrl Pts',(-162.177528905544,223.481737987198,0.211677153642351));
#73984=CARTESIAN_POINT('Ctrl Pts',(-162.415731719026,224.278797115281,0.158757865231754));
#73985=CARTESIAN_POINT('Ctrl Pts',(-162.485012763715,224.510620947525,0.14336634431848));
#73986=CARTESIAN_POINT('Ctrl Pts',(-162.517520936396,224.753174668843,0.127974823405207));
#73987=CARTESIAN_POINT('Ctrl Pts',(-162.515402535198,224.996259729968,0.112583302491934));
#73988=CARTESIAN_POINT('Ctrl Pts',(-162.513515873292,225.000575080101,0.387416697508026));
#73989=CARTESIAN_POINT('Ctrl Pts',(-162.512717062425,224.548734930521,0.415871990501868));
#73990=CARTESIAN_POINT('Ctrl Pts',(-162.396595099549,224.096480310675,0.444327283495711));
#73991=CARTESIAN_POINT('Ctrl Pts',(-162.167641159638,223.711314708389,0.472782576489553));
#73992=CARTESIAN_POINT('Ctrl Pts',(-161.741847632174,222.995008972314,0.525701864900151));
#73993=CARTESIAN_POINT('Ctrl Pts',(-160.925812053378,222.510738130269,0.578621153310749));
#73994=CARTESIAN_POINT('Ctrl Pts',(-160.093070274692,222.479994286021,0.631540441721348));
#73995=CARTESIAN_POINT('Ctrl Pts',(-159.260328496006,222.449250441774,0.684459730131945));
#73996=CARTESIAN_POINT('Ctrl Pts',(-158.410880517429,222.872033595323,0.737379018542543));
#73997=CARTESIAN_POINT('Ctrl Pts',(-157.933376854027,223.554931295734,0.790298306953139));
#73998=CARTESIAN_POINT('Ctrl Pts',(-157.455873190625,224.237828996146,0.843217595363738));
#73999=CARTESIAN_POINT('Ctrl Pts',(-157.350313842398,225.18084124342,0.896136883774334));
#74000=CARTESIAN_POINT('Ctrl Pts',(-157.665030169378,225.952420054605,0.949056172184933));
#74001=CARTESIAN_POINT('Ctrl Pts',(-157.979746496357,226.72399886579,1.00197546059553));
#74002=CARTESIAN_POINT('Ctrl Pts',(-158.714738498543,227.324144240887,1.05489474900613));
#74003=CARTESIAN_POINT('Ctrl Pts',(-159.533660643004,227.478242004204,1.10781403741672));
#74004=CARTESIAN_POINT('Ctrl Pts',(-160.352582787465,227.63233976752,1.16073332582732));
#74005=CARTESIAN_POINT('Ctrl Pts',(-161.255435074201,227.340389919056,1.21365261423792));
#74006=CARTESIAN_POINT('Ctrl Pts',(-161.829078679583,226.735982758477,1.26657190264851));
#74007=CARTESIAN_POINT('Ctrl Pts',(-162.265730077695,226.275914470048,1.30685350093502));
#74008=CARTESIAN_POINT('Ctrl Pts',(-162.511634932737,225.634805536221,1.34713509922152));
#74009=CARTESIAN_POINT('Ctrl Pts',(-162.517460047887,224.997698761843,1.38741669750802));
#74010=CARTESIAN_POINT('Origin',(-160.,225.,10.));
#74011=CARTESIAN_POINT('',(-162.521340736424,225.000905528618,2.38741669750802));
#74012=CARTESIAN_POINT('',(-162.515825293396,225.002114825265,2.11258330249193));
#74013=CARTESIAN_POINT('',(-162.5175,225.,10.));
#74014=CARTESIAN_POINT('Ctrl Pts',(-162.515825293396,225.002114825265,2.11258330249193));
#74015=CARTESIAN_POINT('Ctrl Pts',(-162.517874395793,225.259454350827,2.09633961766571));
#74016=CARTESIAN_POINT('Ctrl Pts',(-162.481551268892,225.516229230468,2.08009593283949));
#74017=CARTESIAN_POINT('Ctrl Pts',(-162.40445263436,225.760113810438,2.06385224801326));
#74018=CARTESIAN_POINT('Ctrl Pts',(-162.153277798076,226.554650183456,2.01093295960267));
#74019=CARTESIAN_POINT('Ctrl Pts',(-161.469331853934,227.21237527946,1.95801367119207));
#74020=CARTESIAN_POINT('Ctrl Pts',(-160.665588242321,227.432315059322,1.90509438278147));
#74021=CARTESIAN_POINT('Ctrl Pts',(-159.861844630708,227.652254839184,1.85217509437087));
#74022=CARTESIAN_POINT('Ctrl Pts',(-158.938303351623,227.434409302904,1.79925580596027));
#74023=CARTESIAN_POINT('Ctrl Pts',(-158.317577312389,226.878462588484,1.74633651754968));
#74024=CARTESIAN_POINT('Ctrl Pts',(-157.696851273154,226.322515874064,1.69341722913908));
#74025=CARTESIAN_POINT('Ctrl Pts',(-157.37894047377,225.428467981504,1.64049794072848));
#74026=CARTESIAN_POINT('Ctrl Pts',(-157.509319984736,224.605439307191,1.58757865231788));
#74027=CARTESIAN_POINT('Ctrl Pts',(-157.639699495703,223.782410632878,1.53465936390729));
#74028=CARTESIAN_POINT('Ctrl Pts',(-158.21836931702,223.030401176814,1.48174007549669));
#74029=CARTESIAN_POINT('Ctrl Pts',(-158.980532027786,222.693521947342,1.42882078708609));
#74030=CARTESIAN_POINT('Ctrl Pts',(-159.742694738552,222.356642717871,1.37590149867549));
#74031=CARTESIAN_POINT('Ctrl Pts',(-160.688350338767,222.434893714993,1.3229822102649));
#74032=CARTESIAN_POINT('Ctrl Pts',(-161.384762947637,222.892484929529,1.2700629218543));
#74033=CARTESIAN_POINT('Ctrl Pts',(-162.075568360043,223.346391828462,1.21756971540018));
#74034=CARTESIAN_POINT('Ctrl Pts',(-162.52112820495,224.173554987853,1.16507650894606));
#74035=CARTESIAN_POINT('Ctrl Pts',(-162.521728513626,225.00013531689,1.11258330249193));
#74036=CARTESIAN_POINT('Ctrl Pts',(-162.517460047887,224.997698761843,1.38741669750802));
#74037=CARTESIAN_POINT('Ctrl Pts',(-162.51928758213,224.797816971322,1.40005438763212));
#74038=CARTESIAN_POINT('Ctrl Pts',(-162.497484365141,224.598329108395,1.41269207775621));
#74039=CARTESIAN_POINT('Ctrl Pts',(-162.450526967693,224.404949370306,1.42532976788031));
#74040=CARTESIAN_POINT('Ctrl Pts',(-162.253896726394,223.595187615409,1.47824905629091));
#74041=CARTESIAN_POINT('Ctrl Pts',(-161.616201319768,222.892528578311,1.5311683447015));
#74042=CARTESIAN_POINT('Ctrl Pts',(-160.829251631713,222.618507639709,1.5840876331121));
#74043=CARTESIAN_POINT('Ctrl Pts',(-160.042301943657,222.344486701107,1.6370069215227));
#74044=CARTESIAN_POINT('Ctrl Pts',(-159.106097974171,222.499103861,1.68992620993329));
#74045=CARTESIAN_POINT('Ctrl Pts',(-158.449045928806,223.011606975551,1.74284549834389));
#74046=CARTESIAN_POINT('Ctrl Pts',(-157.791993883441,223.524110090102,1.79576478675449));
#74047=CARTESIAN_POINT('Ctrl Pts',(-157.414093762197,224.39449915931,1.84868407516509));
#74048=CARTESIAN_POINT('Ctrl Pts',(-157.488272996495,225.224483841496,1.90160336357569));
#74049=CARTESIAN_POINT('Ctrl Pts',(-157.562452230793,226.054468523682,1.95452265198628));
#74050=CARTESIAN_POINT('Ctrl Pts',(-158.088710820631,226.844048818846,2.00744194039688));
#74051=CARTESIAN_POINT('Ctrl Pts',(-158.826232680166,227.231912954014,2.06036122880748));
#74052=CARTESIAN_POINT('Ctrl Pts',(-159.563754539701,227.619777089181,2.11328051721807));
#74053=CARTESIAN_POINT('Ctrl Pts',(-160.512539668932,227.605925064353,2.16619980562867));
#74054=CARTESIAN_POINT('Ctrl Pts',(-161.23842409113,227.196695491326,2.21911909403927));
#74055=CARTESIAN_POINT('Ctrl Pts',(-161.964308513328,226.787465918299,2.27203838244987));
#74056=CARTESIAN_POINT('Ctrl Pts',(-162.467292228493,225.982858797072,2.32495767086046));
#74057=CARTESIAN_POINT('Ctrl Pts',(-162.517209860019,225.1510623664,2.37787695927106));
#74058=CARTESIAN_POINT('Ctrl Pts',(-162.520209403617,225.101079833544,2.38105687201672));
#74059=CARTESIAN_POINT('Ctrl Pts',(-162.521573020035,225.05099912576,2.38423678476237));
#74060=CARTESIAN_POINT('Ctrl Pts',(-162.521340736424,225.000905528618,2.38741669750802));
#74061=CARTESIAN_POINT('Origin',(-160.,225.,10.));
#74062=CARTESIAN_POINT('',(-162.514783952421,225.001726236531,3.38741669750803));
#74063=CARTESIAN_POINT('',(-162.514230407831,224.998633683133,3.11258330249194));
#74064=CARTESIAN_POINT('',(-162.5175,225.,10.));
#74065=CARTESIAN_POINT('Ctrl Pts',(-162.514230407831,224.998633683133,3.11258330249194));
#74066=CARTESIAN_POINT('Ctrl Pts',(-162.511723050653,225.507373485165,3.08052201479596));
#74067=CARTESIAN_POINT('Ctrl Pts',(-162.361947303449,226.01747067327,3.04846072709999));
#74068=CARTESIAN_POINT('Ctrl Pts',(-162.075079946186,226.432902173709,3.01639943940401));
#74069=CARTESIAN_POINT('Ctrl Pts',(-161.601586287461,227.118599504242,2.96348015099342));
#74070=CARTESIAN_POINT('Ctrl Pts',(-160.75460437643,227.546392487277,2.91056086258282));
#74071=CARTESIAN_POINT('Ctrl Pts',(-159.921713116295,227.520523074114,2.85764157417222));
#74072=CARTESIAN_POINT('Ctrl Pts',(-159.08882185616,227.494653660951,2.80472228576163));
#74073=CARTESIAN_POINT('Ctrl Pts',(-158.270021246919,227.01512185159,2.75180299735103));
#74074=CARTESIAN_POINT('Ctrl Pts',(-157.839994436728,226.30136136782,2.69888370894043));
#74075=CARTESIAN_POINT('Ctrl Pts',(-157.409967626536,225.58760088405,2.64596442052983));
#74076=CARTESIAN_POINT('Ctrl Pts',(-157.368714615394,224.639611725872,2.59304513211924));
#74077=CARTESIAN_POINT('Ctrl Pts',(-157.735112769049,223.891193764775,2.54012584370864));
#74078=CARTESIAN_POINT('Ctrl Pts',(-158.101510922704,223.142775803678,2.48720655529804));
#74079=CARTESIAN_POINT('Ctrl Pts',(-158.875560241156,222.593929039663,2.43428726688744));
#74080=CARTESIAN_POINT('Ctrl Pts',(-159.70305579503,222.495805634607,2.38136797847684));
#74081=CARTESIAN_POINT('Ctrl Pts',(-160.530551348904,222.39768222955,2.32844869006625));
#74082=CARTESIAN_POINT('Ctrl Pts',(-161.411493138199,222.750282183452,2.27552940165565));
#74083=CARTESIAN_POINT('Ctrl Pts',(-161.942762168634,223.392255985419,2.22261011324505));
#74084=CARTESIAN_POINT('Ctrl Pts',(-162.310957073405,223.837174603557,2.18593450966068));
#74085=CARTESIAN_POINT('Ctrl Pts',(-162.511198752803,224.421083949139,2.14925890607631));
#74086=CARTESIAN_POINT('Ctrl Pts',(-162.515825293396,225.002114825265,2.11258330249193));
#74087=CARTESIAN_POINT('Ctrl Pts',(-162.521340736424,225.000905528618,2.38741669750802));
#74088=CARTESIAN_POINT('Ctrl Pts',(-162.517707416043,224.217354391848,2.43715607317297));
#74089=CARTESIAN_POINT('Ctrl Pts',(-162.123614648384,223.430649691751,2.48689544883791));
#74090=CARTESIAN_POINT('Ctrl Pts',(-161.492245245968,222.967176986533,2.53663482450285));
#74091=CARTESIAN_POINT('Ctrl Pts',(-160.820511452501,222.474073777457,2.58955411291345));
#74092=CARTESIAN_POINT('Ctrl Pts',(-159.880192317679,222.346853099421,2.64247340132405));
#74093=CARTESIAN_POINT('Ctrl Pts',(-159.101577850181,222.643731140533,2.69539268973465));
#74094=CARTESIAN_POINT('Ctrl Pts',(-158.322963382683,222.940609181644,2.74831197814524));
#74095=CARTESIAN_POINT('Ctrl Pts',(-157.706053582508,223.661585941903,2.80123126655584));
#74096=CARTESIAN_POINT('Ctrl Pts',(-157.533146366389,224.476742465972,2.85415055496644));
#74097=CARTESIAN_POINT('Ctrl Pts',(-157.36023915027,225.291898990041,2.90706984337704));
#74098=CARTESIAN_POINT('Ctrl Pts',(-157.631334518208,226.201235277919,2.95998913178763));
#74099=CARTESIAN_POINT('Ctrl Pts',(-158.22237923309,226.788639064091,3.01290842019823));
#74100=CARTESIAN_POINT('Ctrl Pts',(-158.813423947973,227.376042850262,3.06582770860883));
#74101=CARTESIAN_POINT('Ctrl Pts',(-159.7244180098,227.641514134727,3.11874699701942));
#74102=CARTESIAN_POINT('Ctrl Pts',(-160.538490554791,227.463573261999,3.17166628543002));
#74103=CARTESIAN_POINT('Ctrl Pts',(-161.352563099782,227.285632389272,3.22458557384062));
#74104=CARTESIAN_POINT('Ctrl Pts',(-162.069714127937,226.664279359353,3.27750486225122));
#74105=CARTESIAN_POINT('Ctrl Pts',(-162.361775342391,225.883845306966,3.33042415066182));
#74106=CARTESIAN_POINT('Ctrl Pts',(-162.466622509632,225.603676987581,3.34942166627722));
#74107=CARTESIAN_POINT('Ctrl Pts',(-162.516686611797,225.303007245379,3.36841918189262));
#74108=CARTESIAN_POINT('Ctrl Pts',(-162.514783952421,225.001726236531,3.38741669750803));
#74109=CARTESIAN_POINT('Origin',(-160.,225.,10.));
#74110=CARTESIAN_POINT('',(-162.515095448041,224.998127113865,4.38741669750803));
#74111=CARTESIAN_POINT('',(-162.520804111367,224.998630441702,4.11258330249194));
#74112=CARTESIAN_POINT('',(-162.5175,225.,10.));
#74113=CARTESIAN_POINT('Ctrl Pts',(-162.520804111367,224.998630441702,4.11258330249194));
#74114=CARTESIAN_POINT('Ctrl Pts',(-162.515852785931,225.753298255826,4.06470441192622));
#74115=CARTESIAN_POINT('Ctrl Pts',(-162.154339889845,226.512080349843,4.01682552136049));
#74116=CARTESIAN_POINT('Ctrl Pts',(-161.562602838402,226.979251825556,3.96894663079477));
#74117=CARTESIAN_POINT('Ctrl Pts',(-160.908571315981,227.495604267485,3.91602734238417));
#74118=CARTESIAN_POINT('Ctrl Pts',(-159.973290964671,227.655716310735,3.86310805397357));
#74119=CARTESIAN_POINT('Ctrl Pts',(-159.184746054809,227.386320687613,3.81018876556298));
#74120=CARTESIAN_POINT('Ctrl Pts',(-158.396201144947,227.116925064492,3.75726947715238));
#74121=CARTESIAN_POINT('Ctrl Pts',(-157.754391676534,226.418021774998,3.70435018874178));
#74122=CARTESIAN_POINT('Ctrl Pts',(-157.553009649764,225.609428950352,3.65143090033119));
#74123=CARTESIAN_POINT('Ctrl Pts',(-157.351627622994,224.800836125707,3.59851161192059));
#74124=CARTESIAN_POINT('Ctrl Pts',(-157.590673037867,223.88255376591,3.54559232350999));
#74125=CARTESIAN_POINT('Ctrl Pts',(-158.160758717096,223.274787861392,3.49267303509939));
#74126=CARTESIAN_POINT('Ctrl Pts',(-158.730844396324,222.667021956874,3.43975374668879));
#74127=CARTESIAN_POINT('Ctrl Pts',(-159.631970339908,222.369772507636,3.3868344582782));
#74128=CARTESIAN_POINT('Ctrl Pts',(-160.451781334077,222.51906085447,3.3339151698676));
#74129=CARTESIAN_POINT('Ctrl Pts',(-161.271592328245,222.668349201303,3.28099588145701));
#74130=CARTESIAN_POINT('Ctrl Pts',(-162.010088372997,223.264175344208,3.22807659304641));
#74131=CARTESIAN_POINT('Ctrl Pts',(-162.329333692164,224.033889254676,3.17515730463581));
#74132=CARTESIAN_POINT('Ctrl Pts',(-162.455163409367,224.337270002544,3.15429930392119));
#74133=CARTESIAN_POINT('Ctrl Pts',(-162.515861610493,224.667664594961,3.13344130320656));
#74134=CARTESIAN_POINT('Ctrl Pts',(-162.514230407831,224.998633683133,3.11258330249194));
#74135=CARTESIAN_POINT('Ctrl Pts',(-162.514783952421,225.001726236531,3.38741669750803));
#74136=CARTESIAN_POINT('Ctrl Pts',(-162.511386582976,224.463761897586,3.42133847030322));
#74137=CARTESIAN_POINT('Ctrl Pts',(-162.342301953927,223.923848637976,3.45526024309842));
#74138=CARTESIAN_POINT('Ctrl Pts',(-162.023563429284,223.495222161964,3.48918201589361));
#74139=CARTESIAN_POINT('Ctrl Pts',(-161.526318900968,222.826548144206,3.54210130430421));
#74140=CARTESIAN_POINT('Ctrl Pts',(-160.664858443584,222.428715183543,3.5950205927148));
#74141=CARTESIAN_POINT('Ctrl Pts',(-159.833386345379,222.483771635058,3.6479398811254));
#74142=CARTESIAN_POINT('Ctrl Pts',(-159.001914247175,222.538828086573,3.700859169536));
#74143=CARTESIAN_POINT('Ctrl Pts',(-158.200430508151,223.046773950265,3.7537784579466));
#74144=CARTESIAN_POINT('Ctrl Pts',(-157.795694071579,223.775173208847,3.80669774635719));
#74145=CARTESIAN_POINT('Ctrl Pts',(-157.390957635008,224.503572467428,3.85961703476779));
#74146=CARTESIAN_POINT('Ctrl Pts',(-157.382968500889,225.452425120899,3.91253632317839));
#74147=CARTESIAN_POINT('Ctrl Pts',(-157.775382496813,226.18753621371,3.96545561158898));
#74148=CARTESIAN_POINT('Ctrl Pts',(-158.167796492737,226.922647306522,4.01837489999958));
#74149=CARTESIAN_POINT('Ctrl Pts',(-158.960613618703,227.444016838676,4.07129418841018));
#74150=CARTESIAN_POINT('Ctrl Pts',(-159.79104077347,227.513066122497,4.12421347682078));
#74151=CARTESIAN_POINT('Ctrl Pts',(-160.621467928238,227.582115406317,4.17713276523138));
#74152=CARTESIAN_POINT('Ctrl Pts',(-161.489505111806,227.198844441806,4.23005205364197));
#74153=CARTESIAN_POINT('Ctrl Pts',(-161.997938526036,226.538638014792,4.28297134205257));
#74154=CARTESIAN_POINT('Ctrl Pts',(-162.332432244487,226.104294211776,4.31778646053772));
#74155=CARTESIAN_POINT('Ctrl Pts',(-162.511282100761,225.550087079639,4.35260157902287));
#74156=CARTESIAN_POINT('Ctrl Pts',(-162.515095448041,224.998127113865,4.38741669750803));
#74157=CARTESIAN_POINT('Origin',(-160.,225.,10.));
#74158=CARTESIAN_POINT('',(-162.521526373637,224.999338730952,5.38741669750803));
#74159=CARTESIAN_POINT('',(-162.518352818028,225.002238051842,5.11258330249194));
#74160=CARTESIAN_POINT('',(-162.5175,225.,10.));
#74161=CARTESIAN_POINT('Ctrl Pts',(-162.518352818028,225.002238051842,5.11258330249194));
#74162=CARTESIAN_POINT('Ctrl Pts',(-162.519921653123,225.172538844406,5.10180609746706));
#74163=CARTESIAN_POINT('Ctrl Pts',(-162.504121385855,225.342550222057,5.09102889244219));
#74164=CARTESIAN_POINT('Ctrl Pts',(-162.469883581982,225.508763708357,5.08025168741732));
#74165=CARTESIAN_POINT('Ctrl Pts',(-162.301765761683,226.324921459734,5.02733239900672));
#74166=CARTESIAN_POINT('Ctrl Pts',(-161.689100006436,227.049508151821,4.97441311059612));
#74167=CARTESIAN_POINT('Ctrl Pts',(-160.912242153797,227.350952928564,4.92149382218553));
#74168=CARTESIAN_POINT('Ctrl Pts',(-160.135384301157,227.652397705307,4.86857453377493));
#74169=CARTESIAN_POINT('Ctrl Pts',(-159.194334351124,227.530700566708,4.81565524536433));
#74170=CARTESIAN_POINT('Ctrl Pts',(-158.51971674233,227.041550120997,4.76273595695374));
#74171=CARTESIAN_POINT('Ctrl Pts',(-157.845099133535,226.552399675287,4.70981666854314));
#74172=CARTESIAN_POINT('Ctrl Pts',(-157.43691386598,225.695795922466,4.65689738013254));
#74173=CARTESIAN_POINT('Ctrl Pts',(-157.481946510071,224.863720722978,4.60397809172194));
#74174=CARTESIAN_POINT('Ctrl Pts',(-157.526979154163,224.03164552349,4.55105880331134));
#74175=CARTESIAN_POINT('Ctrl Pts',(-158.025229709902,223.224098877336,4.49813951490075));
#74176=CARTESIAN_POINT('Ctrl Pts',(-158.748698732777,222.810614113926,4.44522022649015));
#74177=CARTESIAN_POINT('Ctrl Pts',(-159.472167755651,222.397129350516,4.39230093807955));
#74178=CARTESIAN_POINT('Ctrl Pts',(-160.420855245662,222.37770646985,4.33938164966895));
#74179=CARTESIAN_POINT('Ctrl Pts',(-161.160641826037,222.761233381722,4.28646236125835));
#74180=CARTESIAN_POINT('Ctrl Pts',(-161.900428406411,223.144760293593,4.23354307284776));
#74181=CARTESIAN_POINT('Ctrl Pts',(-162.43131407715,223.931236998003,4.18062378443716));
#74182=CARTESIAN_POINT('Ctrl Pts',(-162.510365565753,224.760771770512,4.12770449602657));
#74183=CARTESIAN_POINT('Ctrl Pts',(-162.517894974495,224.839782380918,4.12266409818169));
#74184=CARTESIAN_POINT('Ctrl Pts',(-162.521325356737,224.919183612861,4.11762370033681));
#74185=CARTESIAN_POINT('Ctrl Pts',(-162.520804111367,224.998630441702,4.11258330249194));
#74186=CARTESIAN_POINT('Ctrl Pts',(-162.515095448041,224.998127113865,4.38741669750803));
#74187=CARTESIAN_POINT('Ctrl Pts',(-162.517078422397,224.711103043656,4.40552086743347));
#74188=CARTESIAN_POINT('Ctrl Pts',(-162.471729912629,224.424686627928,4.42362503735892));
#74189=CARTESIAN_POINT('Ctrl Pts',(-162.376323018138,224.156048456458,4.44172920728436));
#74190=CARTESIAN_POINT('Ctrl Pts',(-162.097444451118,223.370807214654,4.49464849569496));
#74191=CARTESIAN_POINT('Ctrl Pts',(-161.390857672187,222.737466620561,4.54756778410556));
#74192=CARTESIAN_POINT('Ctrl Pts',(-160.579896777488,222.545843317585,4.60048707251616));
#74193=CARTESIAN_POINT('Ctrl Pts',(-159.768935882789,222.354220014609,4.65340636092675));
#74194=CARTESIAN_POINT('Ctrl Pts',(-158.853600872324,222.60431400275,4.70632564933735));
#74195=CARTESIAN_POINT('Ctrl Pts',(-158.252749028884,223.181682277951,4.75924493774795));
#74196=CARTESIAN_POINT('Ctrl Pts',(-157.651897185444,223.759050553152,4.81216422615854));
#74197=CARTESIAN_POINT('Ctrl Pts',(-157.365528509029,224.663693115414,4.86508351456914));
#74198=CARTESIAN_POINT('Ctrl Pts',(-157.524685300337,225.481645546033,4.91800280297974));
#74199=CARTESIAN_POINT('Ctrl Pts',(-157.683842091644,226.299597976651,4.97092209139034));
#74200=CARTESIAN_POINT('Ctrl Pts',(-158.288524350673,227.030860275626,5.02384137980094));
#74201=CARTESIAN_POINT('Ctrl Pts',(-159.062029487582,227.340806829325,5.07676066821153));
#74202=CARTESIAN_POINT('Ctrl Pts',(-159.83553462449,227.650753383024,5.12967995662213));
#74203=CARTESIAN_POINT('Ctrl Pts',(-160.777862639279,227.539384191447,5.18259924503273));
#74204=CARTESIAN_POINT('Ctrl Pts',(-161.457804250907,227.05766179447,5.23551853344333));
#74205=CARTESIAN_POINT('Ctrl Pts',(-162.108366554241,226.596753935934,5.28615125479823));
#74206=CARTESIAN_POINT('Ctrl Pts',(-162.518727269286,225.796806298301,5.33678397615313));
#74207=CARTESIAN_POINT('Ctrl Pts',(-162.521526373637,224.999338730952,5.38741669750803));
#74208=CARTESIAN_POINT('Origin',(-160.,225.,10.));
#74209=CARTESIAN_POINT('',(-162.517037158453,225.002292268554,6.38741669750803));
#74210=CARTESIAN_POINT('',(-162.513482688453,224.999964780132,6.11258330249194));
#74211=CARTESIAN_POINT('',(-162.5175,225.,10.));
#74212=CARTESIAN_POINT('Ctrl Pts',(-162.513482688453,224.999964780132,6.11258330249194));
#74213=CARTESIAN_POINT('Ctrl Pts',(-162.513429987392,225.422277783558,6.08598849459732));
#74214=CARTESIAN_POINT('Ctrl Pts',(-162.412708906025,225.844614406147,6.05939368670269));
#74215=CARTESIAN_POINT('Ctrl Pts',(-162.211459858042,226.2118624987,6.03279887880807));
#74216=CARTESIAN_POINT('Ctrl Pts',(-161.811007391726,226.942625729067,5.97987959039748));
#74217=CARTESIAN_POINT('Ctrl Pts',(-161.012520005755,227.455268973874,5.92696030198688));
#74218=CARTESIAN_POINT('Ctrl Pts',(-160.181385512249,227.515206694376,5.87404101357628));
#74219=CARTESIAN_POINT('Ctrl Pts',(-159.350251018743,227.575144414878,5.82112172516568));
#74220=CARTESIAN_POINT('Ctrl Pts',(-158.486469417702,227.182376611076,5.76820243675509));
#74221=CARTESIAN_POINT('Ctrl Pts',(-157.985307152779,226.516633822266,5.71528314834449));
#74222=CARTESIAN_POINT('Ctrl Pts',(-157.484144887856,225.850891033457,5.66236385993389));
#74223=CARTESIAN_POINT('Ctrl Pts',(-157.34560195905,224.912173259641,5.60944457152329));
#74224=CARTESIAN_POINT('Ctrl Pts',(-157.63307560786,224.130037735659,5.5565252831127));
#74225=CARTESIAN_POINT('Ctrl Pts',(-157.920549256669,223.347902211677,5.5036059947021));
#74226=CARTESIAN_POINT('Ctrl Pts',(-158.634039483094,222.722348937529,5.4506867062915));
#74227=CARTESIAN_POINT('Ctrl Pts',(-159.44705317355,222.539631079166,5.3977674178809));
#74228=CARTESIAN_POINT('Ctrl Pts',(-160.260066864006,222.356913220803,5.3448481294703));
#74229=CARTESIAN_POINT('Ctrl Pts',(-161.172604018495,222.617030778224,5.29192884105971));
#74230=CARTESIAN_POINT('Ctrl Pts',(-161.767087653063,223.200953962269,5.23900955264911));
#74231=CARTESIAN_POINT('Ctrl Pts',(-162.24050253924,223.665959071973,5.19686746926338));
#74232=CARTESIAN_POINT('Ctrl Pts',(-162.512218205276,224.336311201209,5.15472538587766));
#74233=CARTESIAN_POINT('Ctrl Pts',(-162.518352818028,225.002238051842,5.11258330249194));
#74234=CARTESIAN_POINT('Ctrl Pts',(-162.521526373637,224.999338730952,5.38741669750803));
#74235=CARTESIAN_POINT('Ctrl Pts',(-162.521652780823,224.963325200202,5.38970326456372));
#74236=CARTESIAN_POINT('Ctrl Pts',(-162.520948001254,224.927316727341,5.39198983161942));
#74237=CARTESIAN_POINT('Ctrl Pts',(-162.519396621129,224.891344766231,5.39427639867511));
#74238=CARTESIAN_POINT('Ctrl Pts',(-162.483492171253,224.058825737347,5.44719568708571));
#74239=CARTESIAN_POINT('Ctrl Pts',(-161.994128063033,223.245863281958,5.50011497549631));
#74240=CARTESIAN_POINT('Ctrl Pts',(-161.275237302767,222.824469003665,5.55303426390691));
#74241=CARTESIAN_POINT('Ctrl Pts',(-160.556346542501,222.403074725371,5.60595355231751));
#74242=CARTESIAN_POINT('Ctrl Pts',(-159.60792913019,222.373248624174,5.65887284072811));
#74243=CARTESIAN_POINT('Ctrl Pts',(-158.863980855059,222.748639123394,5.7117921291387));
#74244=CARTESIAN_POINT('Ctrl Pts',(-158.120032579929,223.124029622614,5.7647114175493));
#74245=CARTESIAN_POINT('Ctrl Pts',(-157.580553441979,223.904636722252,5.81763070595989));
#74246=CARTESIAN_POINT('Ctrl Pts',(-157.492409084129,224.733254628861,5.87054999437049));
#74247=CARTESIAN_POINT('Ctrl Pts',(-157.404264726278,225.56187253547,5.92346928278109));
#74248=CARTESIAN_POINT('Ctrl Pts',(-157.767455148527,226.43850124905,5.97638857119169));
#74249=CARTESIAN_POINT('Ctrl Pts',(-158.415784420795,226.961995487504,6.02930785960229));
#74250=CARTESIAN_POINT('Ctrl Pts',(-159.064113693063,227.485489725958,6.08222714801289));
#74251=CARTESIAN_POINT('Ctrl Pts',(-159.99758181535,227.655849489286,6.13514643642348));
#74252=CARTESIAN_POINT('Ctrl Pts',(-160.789033793252,227.395118153138,6.18806572483408));
#74253=CARTESIAN_POINT('Ctrl Pts',(-161.580485771153,227.13438681699,6.24098501324468));
#74254=CARTESIAN_POINT('Ctrl Pts',(-162.22992160467,226.442564381366,6.29390430165527));
#74255=CARTESIAN_POINT('Ctrl Pts',(-162.440159469152,225.636228779205,6.34682359006587));
#74256=CARTESIAN_POINT('Ctrl Pts',(-162.493915597763,225.430055260273,6.36035462587993));
#74257=CARTESIAN_POINT('Ctrl Pts',(-162.51895767859,225.21639505705,6.37388566169398));
#74258=CARTESIAN_POINT('Ctrl Pts',(-162.517037158453,225.002292268554,6.38741669750803));
#74259=CARTESIAN_POINT('Origin',(-160.,225.,10.));
#74260=CARTESIAN_POINT('',(-162.513684921802,224.999260124652,7.38741669750803));
#74261=CARTESIAN_POINT('',(-162.518482076879,224.99778042495,7.11258330249194));
#74262=CARTESIAN_POINT('',(-162.5175,225.,10.));
#74263=CARTESIAN_POINT('Ctrl Pts',(-162.518482076879,224.99778042495,7.11258330249194));
#74264=CARTESIAN_POINT('Ctrl Pts',(-162.512325196575,225.667890476128,7.07017089172757));
#74265=CARTESIAN_POINT('Ctrl Pts',(-162.236727766197,226.342472815229,7.0277584809632));
#74266=CARTESIAN_POINT('Ctrl Pts',(-161.757897620975,226.808026928355,6.98534607019882));
#74267=CARTESIAN_POINT('Ctrl Pts',(-161.160446306655,227.388913323143,6.93242678178823));
#74268=CARTESIAN_POINT('Ctrl Pts',(-160.246595562436,227.644377644117,6.87950749337763));
#74269=CARTESIAN_POINT('Ctrl Pts',(-159.434523470905,227.457519423022,6.82658820496703));
#74270=CARTESIAN_POINT('Ctrl Pts',(-158.622451379374,227.270661201926,6.77366891655644));
#74271=CARTESIAN_POINT('Ctrl Pts',(-157.912157940531,226.641480438761,6.72074962814584));
#74272=CARTESIAN_POINT('Ctrl Pts',(-157.628673418025,225.857890238379,6.66783033973525));
#74273=CARTESIAN_POINT('Ctrl Pts',(-157.345188895519,225.074300037998,6.61491105132465));
#74274=CARTESIAN_POINT('Ctrl Pts',(-157.48851328935,224.1363004004,6.56199176291404));
#74275=CARTESIAN_POINT('Ctrl Pts',(-157.993061359719,223.473119941308,6.50907247450345));
#74276=CARTESIAN_POINT('Ctrl Pts',(-158.497609430088,222.809939482215,6.45615318609285));
#74277=CARTESIAN_POINT('Ctrl Pts',(-159.363381176994,222.421578201629,6.40323389768225));
#74278=CARTESIAN_POINT('Ctrl Pts',(-160.194199466077,222.485750213908,6.35031460927166));
#74279=CARTESIAN_POINT('Ctrl Pts',(-161.02501775516,222.549922226188,6.29739532086106));
#74280=CARTESIAN_POINT('Ctrl Pts',(-161.820882586419,223.066627531333,6.24447603245046));
#74281=CARTESIAN_POINT('Ctrl Pts',(-162.217606228718,223.79942179187,6.19155674403986));
#74282=CARTESIAN_POINT('Ctrl Pts',(-162.41495475901,224.163947257217,6.16523226352389));
#74283=CARTESIAN_POINT('Ctrl Pts',(-162.513534853826,224.581944447954,6.13890778300791));
#74284=CARTESIAN_POINT('Ctrl Pts',(-162.513482688453,224.999964780132,6.11258330249194));
#74285=CARTESIAN_POINT('Ctrl Pts',(-162.517037158453,225.002292268554,6.38741669750803));
#74286=CARTESIAN_POINT('Ctrl Pts',(-162.511446608453,224.379048428925,6.42680495010458));
#74287=CARTESIAN_POINT('Ctrl Pts',(-162.277383983428,223.752054269524,6.46619320270112));
#74288=CARTESIAN_POINT('Ctrl Pts',(-161.858051294842,223.295062851563,6.50558145529767));
#74289=CARTESIAN_POINT('Ctrl Pts',(-161.294665360598,222.681081294779,6.55850074370826));
#74290=CARTESIAN_POINT('Ctrl Pts',(-160.396853596663,222.373966949908,6.61142003211886));
#74291=CARTESIAN_POINT('Ctrl Pts',(-159.575454648558,222.514255335125,6.66433932052946));
#74292=CARTESIAN_POINT('Ctrl Pts',(-158.754055700454,222.654543720342,6.71725860894005));
#74293=CARTESIAN_POINT('Ctrl Pts',(-158.009069568181,223.242234835647,6.77017789735065));
#74294=CARTESIAN_POINT('Ctrl Pts',(-157.681401891219,224.008401238231,6.82309718576125));
#74295=CARTESIAN_POINT('Ctrl Pts',(-157.353734214258,224.774567640816,6.87601647417185));
#74296=CARTESIAN_POINT('Ctrl Pts',(-157.443384992608,225.719209330679,6.92893576258244));
#74297=CARTESIAN_POINT('Ctrl Pts',(-157.90933003186,226.410058289114,6.98185505099304));
#74298=CARTESIAN_POINT('Ctrl Pts',(-158.375275071111,227.100907247549,7.03477433940364));
#74299=CARTESIAN_POINT('Ctrl Pts',(-159.217514371264,227.537963474556,7.08769362781424));
#74300=CARTESIAN_POINT('Ctrl Pts',(-160.050639245129,227.521230049249,7.14061291622484));
#74301=CARTESIAN_POINT('Ctrl Pts',(-160.883764118993,227.504496623942,7.19353220463543));
#74302=CARTESIAN_POINT('Ctrl Pts',(-161.707774566569,227.033973546322,7.24645149304603));
#74303=CARTESIAN_POINT('Ctrl Pts',(-162.145603423247,226.324972167456,7.29937078145663));
#74304=CARTESIAN_POINT('Ctrl Pts',(-162.388420008767,225.931765344016,7.32871942014043));
#74305=CARTESIAN_POINT('Ctrl Pts',(-162.51245763957,225.465209080798,7.35806805882423));
#74306=CARTESIAN_POINT('Ctrl Pts',(-162.513684921802,224.999260124652,7.38741669750803));
#74307=CARTESIAN_POINT('Origin',(-160.,225.,10.));
#74308=CARTESIAN_POINT('',(-162.519747970937,224.998100046487,8.38741669750803));
#74309=CARTESIAN_POINT('',(-162.520711601608,225.001430882692,8.11258330249194));
#74310=CARTESIAN_POINT('',(-162.5175,225.,10.));
#74311=CARTESIAN_POINT('Ctrl Pts',(-162.520711601608,225.001430882692,8.11258330249194));
#74312=CARTESIAN_POINT('Ctrl Pts',(-162.521280388299,225.085146708523,8.10727257726842));
#74313=CARTESIAN_POINT('Ctrl Pts',(-162.517471298417,225.168810149606,8.10196185204489));
#74314=CARTESIAN_POINT('Ctrl Pts',(-162.509113981073,225.252016764264,8.09665112682137));
#74315=CARTESIAN_POINT('Ctrl Pts',(-162.425836600256,226.081137958348,8.04373183841077));
#74316=CARTESIAN_POINT('Ctrl Pts',(-161.890950306787,226.864899309181,7.99081255000018));
#74317=CARTESIAN_POINT('Ctrl Pts',(-161.149219058041,227.244651638032,7.93789326158958));
#74318=CARTESIAN_POINT('Ctrl Pts',(-160.407487809295,227.624403966884,7.88497397317899));
#74319=CARTESIAN_POINT('Ctrl Pts',(-159.458911605272,227.600147273754,7.83205468476839));
#74320=CARTESIAN_POINT('Ctrl Pts',(-158.737558898282,227.182981420942,7.77913539635779));
#74321=CARTESIAN_POINT('Ctrl Pts',(-158.016206191292,226.76581556813,7.72621610794719));
#74322=CARTESIAN_POINT('Ctrl Pts',(-157.522076981334,225.955740555636,7.67329681953659));
#74323=CARTESIAN_POINT('Ctrl Pts',(-157.481284785171,225.123446693249,7.620377531126));
#74324=CARTESIAN_POINT('Ctrl Pts',(-157.440492589007,224.291152830862,7.5674582427154));
#74325=CARTESIAN_POINT('Ctrl Pts',(-157.853037406638,223.436640118583,7.5145389543048));
#74326=CARTESIAN_POINT('Ctrl Pts',(-158.530138737626,222.950933556749,7.46161966589421));
#74327=CARTESIAN_POINT('Ctrl Pts',(-159.207240068613,222.465226994915,7.40870037748361));
#74328=CARTESIAN_POINT('Ctrl Pts',(-160.148897912959,222.348326583526,7.35578108907301));
#74329=CARTESIAN_POINT('Ctrl Pts',(-160.924209659605,222.653725948535,7.30286180066241));
#74330=CARTESIAN_POINT('Ctrl Pts',(-161.69952140625,222.959125313544,7.24994251225181));
#74331=CARTESIAN_POINT('Ctrl Pts',(-162.308487055195,223.686824454951,7.19702322384122));
#74332=CARTESIAN_POINT('Ctrl Pts',(-162.472443937457,224.503828259956,7.14410393543062));
#74333=CARTESIAN_POINT('Ctrl Pts',(-162.504996810954,224.666040551042,7.13359705778439));
#74334=CARTESIAN_POINT('Ctrl Pts',(-162.520007328259,224.831773254163,7.12309018013817));
#74335=CARTESIAN_POINT('Ctrl Pts',(-162.518482076879,224.99778042495,7.11258330249194));
#74336=CARTESIAN_POINT('Ctrl Pts',(-162.513684921802,224.999260124652,7.38741669750803));
#74337=CARTESIAN_POINT('Ctrl Pts',(-162.51467058386,224.625044483707,7.41098734723483));
#74338=CARTESIAN_POINT('Ctrl Pts',(-162.436442208547,224.251220562561,7.43455799696162));
#74339=CARTESIAN_POINT('Ctrl Pts',(-162.276911432784,223.91609981011,7.45812864668842));
#74340=CARTESIAN_POINT('Ctrl Pts',(-161.918743319861,223.163708511743,7.51104793509902));
#74341=CARTESIAN_POINT('Ctrl Pts',(-161.150759828235,222.606405595119,7.56396722350962));
#74342=CARTESIAN_POINT('Ctrl Pts',(-160.324390188574,222.499212863929,7.61688651192021));
#74343=CARTESIAN_POINT('Ctrl Pts',(-159.498020548912,222.392020132738,7.66980580033081));
#74344=CARTESIAN_POINT('Ctrl Pts',(-158.613264761216,222.734937586981,7.72272508874141));
#74345=CARTESIAN_POINT('Ctrl Pts',(-158.074987056538,223.371046206338,7.775644377152));
#74346=CARTESIAN_POINT('Ctrl Pts',(-157.536709351859,224.007154825695,7.8285636655626));
#74347=CARTESIAN_POINT('Ctrl Pts',(-157.3449097302,224.936454610167,7.88148295397319));
#74348=CARTESIAN_POINT('Ctrl Pts',(-157.587355694659,225.73369799665,7.93440224238379));
#74349=CARTESIAN_POINT('Ctrl Pts',(-157.829801659118,226.530941383133,7.98732153079439));
#74350=CARTESIAN_POINT('Ctrl Pts',(-158.506493209696,227.196128371629,8.04024081920499));
#74351=CARTESIAN_POINT('Ctrl Pts',(-159.307776306153,227.42486940928,8.09316010761559));
#74352=CARTESIAN_POINT('Ctrl Pts',(-160.109059402611,227.653610446931,8.14607939602619));
#74353=CARTESIAN_POINT('Ctrl Pts',(-161.034934044948,227.445905533737,8.19899868443678));
#74354=CARTESIAN_POINT('Ctrl Pts',(-161.661720015035,226.896800433892,8.25191797284738));
#74355=CARTESIAN_POINT('Ctrl Pts',(-162.196677445069,226.428143081861,8.29708421440093));
#74356=CARTESIAN_POINT('Ctrl Pts',(-162.513763648225,225.710792668463,8.34225045595448));
#74357=CARTESIAN_POINT('Ctrl Pts',(-162.519747970937,224.998100046487,8.38741669750803));
#74358=CARTESIAN_POINT('Origin',(-160.,225.,10.));
#74359=CARTESIAN_POINT('',(-162.519611784148,225.001947791443,9.38741669750804));
#74360=CARTESIAN_POINT('',(-162.514161553899,225.001308641714,9.11258330249194));
#74361=CARTESIAN_POINT('',(-162.5175,225.,10.));
#74362=CARTESIAN_POINT('Ctrl Pts',(-162.514161553899,225.001308641714,9.11258330249194));
#74363=CARTESIAN_POINT('Ctrl Pts',(-162.515741567435,225.33659020014,9.09145497439867));
#74364=CARTESIAN_POINT('Ctrl Pts',(-162.45340538931,225.671308184112,9.0703266463054));
#74365=CARTESIAN_POINT('Ctrl Pts',(-162.324380606603,225.977967389606,9.04919831821213));
#74366=CARTESIAN_POINT('Ctrl Pts',(-162.001217332251,226.746044582826,8.99627902980153));
#74367=CARTESIAN_POINT('Ctrl Pts',(-161.259694825814,227.33809996406,8.94335974139093));
#74368=CARTESIAN_POINT('Ctrl Pts',(-160.439133771658,227.483209002496,8.89044045298033));
#74369=CARTESIAN_POINT('Ctrl Pts',(-159.618572717501,227.628318040932,8.83752116456974));
#74370=CARTESIAN_POINT('Ctrl Pts',(-158.718973115625,227.326480736569,8.78460187615914));
#74371=CARTESIAN_POINT('Ctrl Pts',(-158.15199172616,226.715817833951,8.73168258774854));
#74372=CARTESIAN_POINT('Ctrl Pts',(-157.585010336694,226.105154931332,8.67876329933794));
#74373=CARTESIAN_POINT('Ctrl Pts',(-157.35064715964,225.185666430457,8.62584401092735));
#74374=CARTESIAN_POINT('Ctrl Pts',(-157.556146780209,224.378110251247,8.57292472251675));
#74375=CARTESIAN_POINT('Ctrl Pts',(-157.761646400778,223.570554072037,8.52000543410616));
#74376=CARTESIAN_POINT('Ctrl Pts',(-158.40700881897,222.874930214492,8.46708614569555));
#74377=CARTESIAN_POINT('Ctrl Pts',(-159.196916204909,222.609556142147,8.41416685728496));
#74378=CARTESIAN_POINT('Ctrl Pts',(-159.986823590848,222.344182069802,8.36124756887436));
#74379=CARTESIAN_POINT('Ctrl Pts',(-160.921275944535,222.509057782657,8.30832828046377));
#74380=CARTESIAN_POINT('Ctrl Pts',(-161.572667887295,223.028736157752,8.25540899205317));
#74381=CARTESIAN_POINT('Ctrl Pts',(-162.158689268117,223.496262110967,8.20780042886609));
#74382=CARTESIAN_POINT('Ctrl Pts',(-162.515612652598,224.250951425351,8.16019186567902));
#74383=CARTESIAN_POINT('Ctrl Pts',(-162.520711601608,225.001430882692,8.11258330249194));
#74384=CARTESIAN_POINT('Ctrl Pts',(-162.519747970937,224.998100046487,8.38741669750803));
#74385=CARTESIAN_POINT('Ctrl Pts',(-162.520775214578,224.875762231721,8.39516974436508));
#74386=CARTESIAN_POINT('Ctrl Pts',(-162.512635620397,224.753561662087,8.40292279122213));
#74387=CARTESIAN_POINT('Ctrl Pts',(-162.494857631502,224.632779775997,8.41067583807918));
#74388=CARTESIAN_POINT('Ctrl Pts',(-162.373511980044,223.808369504441,8.46359512648977));
#74389=CARTESIAN_POINT('Ctrl Pts',(-161.803123379288,223.050054247826,8.51651441490037));
#74390=CARTESIAN_POINT('Ctrl Pts',(-161.044701641726,222.704839052668,8.56943370331096));
#74391=CARTESIAN_POINT('Ctrl Pts',(-160.286279904165,222.35962385751,8.62235299172156));
#74392=CARTESIAN_POINT('Ctrl Pts',(-159.339825029797,222.42750872381,8.67527228013216));
#74393=CARTESIAN_POINT('Ctrl Pts',(-158.638434750524,222.877429538083,8.72819156854276));
#74394=CARTESIAN_POINT('Ctrl Pts',(-157.937044471252,223.327350352356,8.78111085695335));
#74395=CARTESIAN_POINT('Ctrl Pts',(-157.480718787075,224.159307114602,8.83403014536395));
#74396=CARTESIAN_POINT('Ctrl Pts',(-157.4782723221,224.992596426776,8.88694943377455));
#74397=CARTESIAN_POINT('Ctrl Pts',(-157.475825857125,225.82588573895,8.93986872218515));
#74398=CARTESIAN_POINT('Ctrl Pts',(-157.927258611353,226.660507601051,8.99278801059575));
#74399=CARTESIAN_POINT('Ctrl Pts',(-158.625994965325,227.114539065393,9.04570729900634));
#74400=CARTESIAN_POINT('Ctrl Pts',(-159.324731319297,227.568570529734,9.09862658741694));
#74401=CARTESIAN_POINT('Ctrl Pts',(-160.270771273013,227.642011596316,9.15154587582754));
#74402=CARTESIAN_POINT('Ctrl Pts',(-161.031206962253,227.301255634514,9.20446516423813));
#74403=CARTESIAN_POINT('Ctrl Pts',(-161.791642651494,226.960499672712,9.25738445264873));
#74404=CARTESIAN_POINT('Ctrl Pts',(-162.366474076259,226.205546682527,9.31030374105933));
#74405=CARTESIAN_POINT('Ctrl Pts',(-162.492658387878,225.381863137423,9.36322302946993));
#74406=CARTESIAN_POINT('Ctrl Pts',(-162.511888057807,225.256339112332,9.37128758548263));
#74407=CARTESIAN_POINT('Ctrl Pts',(-162.520698445279,225.129218903863,9.37935214149533));
#74408=CARTESIAN_POINT('Ctrl Pts',(-162.519611784148,225.001947791443,9.38741669750804));
#74409=CARTESIAN_POINT('Origin',(-160.,225.,10.));
#74410=CARTESIAN_POINT('',(-162.513643783132,225.000662446468,10.387416697508));
#74411=CARTESIAN_POINT('',(-162.515939315398,224.997857937799,10.1125833024919));
#74412=CARTESIAN_POINT('',(-162.5175,225.,10.));
#74413=CARTESIAN_POINT('Ctrl Pts',(-162.515939315398,224.997857937799,10.1125833024919));
#74414=CARTESIAN_POINT('Ctrl Pts',(-162.511202901338,225.583104378889,10.0756373715289));
#74415=CARTESIAN_POINT('Ctrl Pts',(-162.307732412804,226.171320314646,10.0386914405659));
#74416=CARTESIAN_POINT('Ctrl Pts',(-161.93454462814,226.617622484148,10.0017455096029));
#74417=CARTESIAN_POINT('Ctrl Pts',(-161.400011284597,227.256880789745,9.94882622119229));
#74418=CARTESIAN_POINT('Ctrl Pts',(-160.517284274851,227.604987423216,9.89590693278168));
#74419=CARTESIAN_POINT('Ctrl Pts',(-159.690299461207,227.502648795927,9.84298764437109));
#74420=CARTESIAN_POINT('Ctrl Pts',(-158.863314647562,227.400310168639,9.79006835596049));
#74421=CARTESIAN_POINT('Ctrl Pts',(-158.092072030018,226.847526280592,9.7371490675499));
#74422=CARTESIAN_POINT('Ctrl Pts',(-157.729492215198,226.097251028089,9.6842297791393));
#74423=CARTESIAN_POINT('Ctrl Pts',(-157.366912400379,225.346975775584,9.6313104907287));
#74424=CARTESIAN_POINT('Ctrl Pts',(-157.412995388284,224.399209158623,9.5783912023181));
#74425=CARTESIAN_POINT('Ctrl Pts',(-157.846653604555,223.687649162491,9.5254719139075));
#74426=CARTESIAN_POINT('Ctrl Pts',(-158.280311820826,222.976089166359,9.4725526254969));
#74427=CARTESIAN_POINT('Ctrl Pts',(-159.101545265462,222.500735791056,9.41963333708631));
#74428=CARTESIAN_POINT('Ctrl Pts',(-159.934557530345,222.479110731775,9.36671404867571));
#74429=CARTESIAN_POINT('Ctrl Pts',(-160.767569795228,222.457485672494,9.31379476026512));
#74430=CARTESIAN_POINT('Ctrl Pts',(-161.612360880358,222.889588929234,9.26087547185452));
#74431=CARTESIAN_POINT('Ctrl Pts',(-162.082354401789,223.577690060207,9.20795618344392));
#74432=CARTESIAN_POINT('Ctrl Pts',(-162.364700325894,223.991062885241,9.17616522312659));
#74433=CARTESIAN_POINT('Ctrl Pts',(-162.51178416997,224.49682373065,9.14437426280927));
#74434=CARTESIAN_POINT('Ctrl Pts',(-162.514161553899,225.001308641714,9.11258330249194));
#74435=CARTESIAN_POINT('Ctrl Pts',(-162.519611784148,225.001947791443,9.38741669750804));
#74436=CARTESIAN_POINT('Ctrl Pts',(-162.513567819153,224.294071042795,9.43227142990593));
#74437=CARTESIAN_POINT('Ctrl Pts',(-162.201354782218,223.581526021403,9.47712616230383));
#74438=CARTESIAN_POINT('Ctrl Pts',(-161.672828954939,223.112989511979,9.52198089470172));
#74439=CARTESIAN_POINT('Ctrl Pts',(-161.049278011905,222.560213531661,9.57490018311232));
#74440=CARTESIAN_POINT('Ctrl Pts',(-160.124638927364,222.347075671048,9.62781947152292));
#74441=CARTESIAN_POINT('Ctrl Pts',(-159.322026528221,222.571107810967,9.68073875993352));
#74442=CARTESIAN_POINT('Ctrl Pts',(-158.519414129078,222.795139950885,9.73365804834411));
#74443=CARTESIAN_POINT('Ctrl Pts',(-157.838828415334,223.456342091334,9.78657733675471));
#74444=CARTESIAN_POINT('Ctrl Pts',(-157.591705396215,224.252148145844,9.8394966251653));
#74445=CARTESIAN_POINT('Ctrl Pts',(-157.344582377097,225.047954200355,9.8924159135759));
#74446=CARTESIAN_POINT('Ctrl Pts',(-157.530922052604,225.978364168927,9.9453352019865));
#74447=CARTESIAN_POINT('Ctrl Pts',(-158.065455390889,226.617622468237,9.9982544903971));
#74448=CARTESIAN_POINT('Ctrl Pts',(-158.599988729174,227.256880767546,10.0511737788077));
#74449=CARTESIAN_POINT('Ctrl Pts',(-159.482715730237,227.604987397592,10.1040930672183));
#74450=CARTESIAN_POINT('Ctrl Pts',(-160.309700535747,227.50264877131,10.1570123556289));
#74451=CARTESIAN_POINT('Ctrl Pts',(-161.136685341257,227.400310145029,10.2099316440395));
#74452=CARTESIAN_POINT('Ctrl Pts',(-161.907927951215,226.847526262419,10.2628509324501));
#74453=CARTESIAN_POINT('Ctrl Pts',(-162.270507762468,226.097251017295,10.3157702208607));
#74454=CARTESIAN_POINT('Ctrl Pts',(-162.434137866349,225.75865627901,10.3396523797431));
#74455=CARTESIAN_POINT('Ctrl Pts',(-162.514537129793,225.379839205506,10.3635345386256));
#74456=CARTESIAN_POINT('Ctrl Pts',(-162.513643783132,225.000662446468,10.387416697508));
#74457=CARTESIAN_POINT('Origin',(-160.,225.,10.));
#74458=CARTESIAN_POINT('',(-162.517183796669,224.997701708063,11.387416697508));
#74459=CARTESIAN_POINT('',(-162.521737918614,224.999954178035,11.1125833024919));
#74460=CARTESIAN_POINT('',(-162.5175,225.,10.));
#74461=CARTESIAN_POINT('Ctrl Pts',(-162.521737514161,224.999954182408,11.1125833024919));
#74462=CARTESIAN_POINT('Ctrl Pts',(-162.52151466846,225.830795448054,11.0598197686592));
#74463=CARTESIAN_POINT('Ctrl Pts',(-162.070684854796,226.661843944495,11.0070562348264));
#74464=CARTESIAN_POINT('Ctrl Pts',(-161.37400504819,227.114539086192,10.9542927009936));
#74465=CARTESIAN_POINT('Ctrl Pts',(-160.675268687345,227.568570555,10.901373412583));
#74466=CARTESIAN_POINT('Ctrl Pts',(-159.729228724324,227.642011622304,10.8484541241724));
#74467=CARTESIAN_POINT('Ctrl Pts',(-158.968793027603,227.30125565715,10.7955348357618));
#74468=CARTESIAN_POINT('Ctrl Pts',(-158.208357330883,226.960499691997,10.7426155473512));
#74469=CARTESIAN_POINT('Ctrl Pts',(-157.633525900464,226.205546694385,10.6896962589407));
#74470=CARTESIAN_POINT('Ctrl Pts',(-157.507341587603,225.381863141179,10.6367769705301));
#74471=CARTESIAN_POINT('Ctrl Pts',(-157.381157274742,224.558179587973,10.5838576821195));
#74472=CARTESIAN_POINT('Ctrl Pts',(-157.70362007944,223.665765479172,10.5309383937089));
#74473=CARTESIAN_POINT('Ctrl Pts',(-158.327171028607,223.112989493417,10.4780191052983));
#74474=CARTESIAN_POINT('Ctrl Pts',(-158.950721977774,222.560213507662,10.4250998168877));
#74475=CARTESIAN_POINT('Ctrl Pts',(-159.87536107141,222.347075644953,10.3721805284771));
#74476=CARTESIAN_POINT('Ctrl Pts',(-160.677973478447,222.571107787075,10.3192612400665));
#74477=CARTESIAN_POINT('Ctrl Pts',(-161.480585885485,222.795139929197,10.2663419516559));
#74478=CARTESIAN_POINT('Ctrl Pts',(-162.161171605924,223.456342076149,10.2134226632453));
#74479=CARTESIAN_POINT('Ctrl Pts',(-162.408294627474,224.252148138488,10.1605033748347));
#74480=CARTESIAN_POINT('Ctrl Pts',(-162.482887171616,224.49235723945,10.1445300173871));
#74481=CARTESIAN_POINT('Ctrl Pts',(-162.51798707635,224.744830057468,10.1285566599395));
#74482=CARTESIAN_POINT('Ctrl Pts',(-162.515939315398,224.997857937799,10.1125833024919));
#74483=CARTESIAN_POINT('Ctrl Pts',(-162.513643783132,225.000662446468,10.387416697508));
#74484=CARTESIAN_POINT('Ctrl Pts',(-162.512557607345,224.539640278395,10.4164538270362));
#74485=CARTESIAN_POINT('Ctrl Pts',(-162.391297224533,224.07808639011,10.4454909565643));
#74486=CARTESIAN_POINT('Ctrl Pts',(-162.153346374264,223.6876491754,10.4745280860925));
#74487=CARTESIAN_POINT('Ctrl Pts',(-161.719688162259,222.976089186267,10.5274473745031));
#74488=CARTESIAN_POINT('Ctrl Pts',(-160.898454725701,222.50073581564,10.5803666629137));
#74489=CARTESIAN_POINT('Ctrl Pts',(-160.065442469011,222.479110756572,10.6332859513243));
#74490=CARTESIAN_POINT('Ctrl Pts',(-159.232430212322,222.457485697503,10.6862052397349));
#74491=CARTESIAN_POINT('Ctrl Pts',(-158.387639135502,222.889588949993,10.7391245281455));
#74492=CARTESIAN_POINT('Ctrl Pts',(-157.917645618693,223.577690074197,10.7920438165561));
#74493=CARTESIAN_POINT('Ctrl Pts',(-157.447652101885,224.265791198402,10.8449631049667));
#74494=CARTESIAN_POINT('Ctrl Pts',(-157.352456145088,225.209890194322,10.8978823933773));
#74495=CARTESIAN_POINT('Ctrl Pts',(-157.675619416261,225.977967379987,10.9508016817879));
#74496=CARTESIAN_POINT('Ctrl Pts',(-157.998782687434,226.746044565652,11.0037209701985));
#74497=CARTESIAN_POINT('Ctrl Pts',(-158.740305186577,227.338099941062,11.0566402586091));
#74498=CARTESIAN_POINT('Ctrl Pts',(-159.560866232662,227.48320897807,11.1095595470196));
#74499=CARTESIAN_POINT('Ctrl Pts',(-160.381427278747,227.628318015078,11.1624788354302));
#74500=CARTESIAN_POINT('Ctrl Pts',(-161.281026871775,227.326480713685,11.2153981238408));
#74501=CARTESIAN_POINT('Ctrl Pts',(-161.848008255663,226.715817817073,11.2683174122514));
#74502=CARTESIAN_POINT('Ctrl Pts',(-162.273354599771,226.257701840186,11.3080171740036));
#74503=CARTESIAN_POINT('Ctrl Pts',(-162.511506122372,225.625781331299,11.3477169357558));
#74504=CARTESIAN_POINT('Ctrl Pts',(-162.517183796669,224.997701708063,11.387416697508));
#74505=CARTESIAN_POINT('Origin',(-160.,225.,10.));
#74506=CARTESIAN_POINT('',(-162.521467546725,225.000747722913,12.387416697508));
#74507=CARTESIAN_POINT('',(-162.516072841654,225.002171058777,12.1125833024919));
#74508=CARTESIAN_POINT('',(-162.5175,225.,10.));
#74509=CARTESIAN_POINT('Ctrl Pts',(-162.516072841654,225.002171058777,12.1125833024919));
#74510=CARTESIAN_POINT('Ctrl Pts',(-162.518115745022,225.250231128475,12.0969214542));
#74511=CARTESIAN_POINT('Ctrl Pts',(-162.484397976292,225.497748022892,12.0812596059081));
#74512=CARTESIAN_POINT('Ctrl Pts',(-162.412644329073,225.733698003867,12.0655977576162));
#74513=CARTESIAN_POINT('Ctrl Pts',(-162.170198362229,226.530941398192,12.0126784692056));
#74514=CARTESIAN_POINT('Ctrl Pts',(-161.493506804995,227.196128393231,11.959759180795));
#74515=CARTESIAN_POINT('Ctrl Pts',(-160.692223700656,227.424869433132,11.9068398923844));
#74516=CARTESIAN_POINT('Ctrl Pts',(-159.890940596317,227.653610473033,11.8539206039738));
#74517=CARTESIAN_POINT('Ctrl Pts',(-158.965065944872,227.445905557796,11.8010013155632));
#74518=CARTESIAN_POINT('Ctrl Pts',(-158.338279968619,226.89680045255,11.7480820271526));
#74519=CARTESIAN_POINT('Ctrl Pts',(-157.711493992366,226.347695347304,11.695162738742));
#74520=CARTESIAN_POINT('Ctrl Pts',(-157.383796691305,225.457190052049,11.6422434503314));
#74521=CARTESIAN_POINT('Ctrl Pts',(-157.505142343957,224.632779772385,11.5893241619208));
#74522=CARTESIAN_POINT('Ctrl Pts',(-157.626487996609,223.80836949272,11.5364048735102));
#74523=CARTESIAN_POINT('Ctrl Pts',(-158.196876602975,223.050054228646,11.4834855850996));
#74524=CARTESIAN_POINT('Ctrl Pts',(-158.955298347997,222.704839030092,11.430566296689));
#74525=CARTESIAN_POINT('Ctrl Pts',(-159.713720093019,222.359623831538,11.3776470082784));
#74526=CARTESIAN_POINT('Ctrl Pts',(-160.660174976697,222.427508698506,11.3247277198678));
#74527=CARTESIAN_POINT('Ctrl Pts',(-161.361565262868,222.877429517204,11.2718084314572));
#74528=CARTESIAN_POINT('Ctrl Pts',(-162.06295554904,223.327350335903,11.2188891430466));
#74529=CARTESIAN_POINT('Ctrl Pts',(-162.519281237706,224.159307106333,11.165969854636));
#74530=CARTESIAN_POINT('Ctrl Pts',(-162.521727702705,224.992596426703,11.1130505662254));
#74531=CARTESIAN_POINT('Ctrl Pts',(-162.521734903257,224.995049003641,11.1128948116476));
#74532=CARTESIAN_POINT('Ctrl Pts',(-162.521738171987,224.997501592121,11.1127390570698));
#74533=CARTESIAN_POINT('Ctrl Pts',(-162.521737514161,224.999954182408,11.1125833024919));
#74534=CARTESIAN_POINT('Ctrl Pts',(-162.517183796669,224.997701708063,11.387416697508));
#74535=CARTESIAN_POINT('Ctrl Pts',(-162.51907439156,224.788559009051,11.4006362241664));
#74536=CARTESIAN_POINT('Ctrl Pts',(-162.495188120451,224.579842190178,11.4138557508248));
#74537=CARTESIAN_POINT('Ctrl Pts',(-162.443853195752,224.378110257364,11.4270752774832));
#74538=CARTESIAN_POINT('Ctrl Pts',(-162.238353577205,223.570554086097,11.4799945658938));
#74539=CARTESIAN_POINT('Ctrl Pts',(-161.592991165361,222.874930235395,11.5329138543044));
#74540=CARTESIAN_POINT('Ctrl Pts',(-160.803083787191,222.60955616566,11.585833142715));
#74541=CARTESIAN_POINT('Ctrl Pts',(-160.013176409022,222.344182095926,11.6387524311256));
#74542=CARTESIAN_POINT('Ctrl Pts',(-159.078724064527,222.509057807159,11.6916717195362));
#74543=CARTESIAN_POINT('Ctrl Pts',(-158.427332128174,223.028736177142,11.7445910079468));
#74544=CARTESIAN_POINT('Ctrl Pts',(-157.775940191821,223.548414547125,11.7975102963574));
#74545=CARTESIAN_POINT('Ctrl Pts',(-157.407608663609,224.422895575858,11.850429584768));
#74546=CARTESIAN_POINT('Ctrl Pts',(-157.490886043608,225.252016761786,11.9033488731786));
#74547=CARTESIAN_POINT('Ctrl Pts',(-157.574163423606,226.081137947714,11.9562681615892));
#74548=CARTESIAN_POINT('Ctrl Pts',(-158.109049711814,226.864899290837,12.0091874499998));
#74549=CARTESIAN_POINT('Ctrl Pts',(-158.850780953264,227.244651615953,12.0621067384104));
#74550=CARTESIAN_POINT('Ctrl Pts',(-159.592512194714,227.624403941069,12.115026026821));
#74551=CARTESIAN_POINT('Ctrl Pts',(-160.541088389406,227.600147248178,12.1679453152316));
#74552=CARTESIAN_POINT('Ctrl Pts',(-161.262441089301,227.182981399469,12.2208646036422));
#74553=CARTESIAN_POINT('Ctrl Pts',(-161.983793789195,226.765815550761,12.2737838920528));
#74554=CARTESIAN_POINT('Ctrl Pts',(-162.477922994292,225.955740546234,12.3267031804634));
#74555=CARTESIAN_POINT('Ctrl Pts',(-162.518715190054,225.123446692035,12.379622468874));
#74556=CARTESIAN_POINT('Ctrl Pts',(-162.520717885793,225.082585166334,12.3822205450853));
#74557=CARTESIAN_POINT('Ctrl Pts',(-162.521627891562,225.041670085963,12.3848186212967));
#74558=CARTESIAN_POINT('Ctrl Pts',(-162.521467546725,225.000747722913,12.387416697508));
#74559=CARTESIAN_POINT('Origin',(-160.,225.,10.));
#74560=CARTESIAN_POINT('',(-162.514983709116,225.001823857702,13.387416697508));
#74561=CARTESIAN_POINT('',(-162.514086051005,224.998759312154,13.1125833024919));
#74562=CARTESIAN_POINT('',(-162.5175,225.,10.));
#74563=CARTESIAN_POINT('Ctrl Pts',(-162.514086051005,224.998759312154,13.1125833024919));
#74564=CARTESIAN_POINT('Ctrl Pts',(-162.511858164299,225.49833849052,13.0811038513303));
#74565=CARTESIAN_POINT('Ctrl Pts',(-162.367841029585,225.99910141157,13.0496244001686));
#74566=CARTESIAN_POINT('Ctrl Pts',(-162.090669988705,226.410058302984,13.0181449490069));
#74567=CARTESIAN_POINT('Ctrl Pts',(-161.62472494487,227.100907268215,12.9652256605963));
#74568=CARTESIAN_POINT('Ctrl Pts',(-160.782485636433,227.53796349952,12.9123063721857));
#74569=CARTESIAN_POINT('Ctrl Pts',(-159.949360754373,227.521230074049,12.8593870837751));
#74570=CARTESIAN_POINT('Ctrl Pts',(-159.116235872314,227.504496648577,12.8064677953645));
#74571=CARTESIAN_POINT('Ctrl Pts',(-158.292225416633,227.033973566329,12.753548506954));
#74572=CARTESIAN_POINT('Ctrl Pts',(-157.854396555648,226.324972180489,12.7006292185434));
#74573=CARTESIAN_POINT('Ctrl Pts',(-157.416567694663,225.615970794649,12.6477099301328));
#74574=CARTESIAN_POINT('Ctrl Pts',(-157.364920428374,224.668491105218,12.5947906417222));
#74575=CARTESIAN_POINT('Ctrl Pts',(-157.72308854482,223.916099799449,12.5418713533116));
#74576=CARTESIAN_POINT('Ctrl Pts',(-158.081256661265,223.16370849368,12.488952064901));
#74577=CARTESIAN_POINT('Ctrl Pts',(-158.849240160445,222.606405571575,12.4360327764904));
#74578=CARTESIAN_POINT('Ctrl Pts',(-159.675609808235,222.49921283933,12.3831134880798));
#74579=CARTESIAN_POINT('Ctrl Pts',(-160.501979456025,222.392020107085,12.3301941996692));
#74580=CARTESIAN_POINT('Ctrl Pts',(-161.386735252425,222.734937564701,12.2772749112586));
#74581=CARTESIAN_POINT('Ctrl Pts',(-161.925012962398,223.371046190315,12.224355622848));
#74582=CARTESIAN_POINT('Ctrl Pts',(-162.303983469161,223.818893841703,12.1870981827293));
#74583=CARTESIAN_POINT('Ctrl Pts',(-162.511213048066,224.412069365775,12.1498407426106));
#74584=CARTESIAN_POINT('Ctrl Pts',(-162.516072841654,225.002171058777,12.1125833024919));
#74585=CARTESIAN_POINT('Ctrl Pts',(-162.521467546725,225.000747722913,12.387416697508));
#74586=CARTESIAN_POINT('Ctrl Pts',(-162.518361884723,224.208137057474,12.4377379097073));
#74587=CARTESIAN_POINT('Ctrl Pts',(-162.113720234785,223.412794336153,12.4880591219065));
#74588=CARTESIAN_POINT('Ctrl Pts',(-161.469861247916,222.950933576905,12.5383803341058));
#74589=CARTESIAN_POINT('Ctrl Pts',(-160.792759923588,222.465227019848,12.5912996225164));
#74590=CARTESIAN_POINT('Ctrl Pts',(-159.851102088505,222.348326609609,12.644218910927));
#74591=CARTESIAN_POINT('Ctrl Pts',(-159.075790349486,222.653725971614,12.6971381993376));
#74592=CARTESIAN_POINT('Ctrl Pts',(-158.300478610467,222.959125333619,12.7500574877482));
#74593=CARTESIAN_POINT('Ctrl Pts',(-157.691512967512,223.686824467868,12.8029767761588));
#74594=CARTESIAN_POINT('Ctrl Pts',(-157.527556086863,224.503828264837,12.8558960645694));
#74595=CARTESIAN_POINT('Ctrl Pts',(-157.363599206214,225.320832061806,12.90881535298));
#74596=CARTESIAN_POINT('Ctrl Pts',(-157.644651087872,226.227140521495,12.9617346413906));
#74597=CARTESIAN_POINT('Ctrl Pts',(-158.242102396316,226.80802691057,13.0146539298012));
#74598=CARTESIAN_POINT('Ctrl Pts',(-158.83955370476,227.388913299645,13.0675732182118));
#74599=CARTESIAN_POINT('Ctrl Pts',(-159.75340443999,227.644377618106,13.1204925066223));
#74600=CARTESIAN_POINT('Ctrl Pts',(-160.565476523533,227.457519398848,13.1734117950329));
#74601=CARTESIAN_POINT('Ctrl Pts',(-161.377548607076,227.270661179591,13.2263310834435));
#74602=CARTESIAN_POINT('Ctrl Pts',(-162.087842038932,226.641480422614,13.2792503718541));
#74603=CARTESIAN_POINT('Ctrl Pts',(-162.371326558649,225.85789022994,13.3321696602647));
#74604=CARTESIAN_POINT('Ctrl Pts',(-162.469977921817,225.585204297215,13.3505853393458));
#74605=CARTESIAN_POINT('Ctrl Pts',(-162.516942328016,225.293819237946,13.3690010184269));
#74606=CARTESIAN_POINT('Ctrl Pts',(-162.514983709116,225.001823857702,13.387416697508));
#74607=CARTESIAN_POINT('Origin',(-160.,225.,10.));
#74608=CARTESIAN_POINT('',(-162.514889421101,224.998220537573,14.387416697508));
#74609=CARTESIAN_POINT('',(-162.520601007743,224.998500607742,14.1125833024919));
#74610=CARTESIAN_POINT('',(-162.5175,225.,10.));
#74611=CARTESIAN_POINT('Ctrl Pts',(-162.520601007743,224.998500607742,14.1125833024919));
#74612=CARTESIAN_POINT('Ctrl Pts',(-162.515344926956,225.74415563317,14.0652862484605));
#74613=CARTESIAN_POINT('Ctrl Pts',(-162.163665278319,226.494118173821,14.0179891944291));
#74614=CARTESIAN_POINT('Ctrl Pts',(-161.584215594788,226.961995506803,13.9706921403977));
#74615=CARTESIAN_POINT('Ctrl Pts',(-160.935886316143,227.485489750407,13.9177728519871));
#74616=CARTESIAN_POINT('Ctrl Pts',(-160.002418184674,227.65584951541,13.8648535635765));
#74617=CARTESIAN_POINT('Ctrl Pts',(-159.210966198987,227.395118176697,13.8119342751659));
#74618=CARTESIAN_POINT('Ctrl Pts',(-158.4195142133,227.134386837984,13.7590149867553));
#74619=CARTESIAN_POINT('Ctrl Pts',(-157.770078373396,226.442564395556,13.7060956983447));
#74620=CARTESIAN_POINT('Ctrl Pts',(-157.559840506845,225.636228785463,13.6531764099341));
#74621=CARTESIAN_POINT('Ctrl Pts',(-157.349602640294,224.829893175371,13.6002571215235));
#74622=CARTESIAN_POINT('Ctrl Pts',(-157.578562747097,223.909044397616,13.5473378331129));
#74623=CARTESIAN_POINT('Ctrl Pts',(-158.141948686882,223.295062834793,13.4944185447023));
#74624=CARTESIAN_POINT('Ctrl Pts',(-158.705334626666,222.681081271969,13.4414992562917));
#74625=CARTESIAN_POINT('Ctrl Pts',(-159.603146399434,222.373966924078,13.3885799678811));
#74626=CARTESIAN_POINT('Ctrl Pts',(-160.424545355618,222.514255310675,13.3356606794705));
#74627=CARTESIAN_POINT('Ctrl Pts',(-161.245944311802,222.654543697272,13.2827413910599));
#74628=CARTESIAN_POINT('Ctrl Pts',(-161.990930451403,223.242234818357,13.2298221026493));
#74629=CARTESIAN_POINT('Ctrl Pts',(-162.318598131587,224.008401228477,13.1769028142387));
#74630=CARTESIAN_POINT('Ctrl Pts',(-162.451350138387,224.31880757807,13.1554629769898));
#74631=CARTESIAN_POINT('Ctrl Pts',(-162.515603406823,224.658508898571,13.1340231397409));
#74632=CARTESIAN_POINT('Ctrl Pts',(-162.514086051005,224.998759312154,13.1125833024919));
#74633=CARTESIAN_POINT('Ctrl Pts',(-162.514983709116,225.001823857702,13.387416697508));
#74634=CARTESIAN_POINT('Ctrl Pts',(-162.511314041491,224.454741424219,13.4219203068375));
#74635=CARTESIAN_POINT('Ctrl Pts',(-162.3359061834,223.905516534921,13.456423916167));
#74636=CARTESIAN_POINT('Ctrl Pts',(-162.00693862054,223.473119956326,13.4909275254965));
#74637=CARTESIAN_POINT('Ctrl Pts',(-161.502390555134,222.809939503758,13.5438468139071));
#74638=CARTESIAN_POINT('Ctrl Pts',(-160.636618816744,222.421578226991,13.5967661023177));
#74639=CARTESIAN_POINT('Ctrl Pts',(-159.805800535833,222.48575023864,13.6496853907283));
#74640=CARTESIAN_POINT('Ctrl Pts',(-158.974982254923,222.549922250288,13.7026046791389));
#74641=CARTESIAN_POINT('Ctrl Pts',(-158.179117431492,223.066627550351,13.7555239675495));
#74642=CARTESIAN_POINT('Ctrl Pts',(-157.782393793095,223.799421803679,13.8084432559601));
#74643=CARTESIAN_POINT('Ctrl Pts',(-157.385670154698,224.532216057008,13.8613625443707));
#74644=CARTESIAN_POINT('Ctrl Pts',(-157.388087701335,225.481099263601,13.9142818327813));
#74645=CARTESIAN_POINT('Ctrl Pts',(-157.788540163711,226.21186248678,13.9672011211919));
#74646=CARTESIAN_POINT('Ctrl Pts',(-158.188992626088,226.942625709959,14.0201204096025));
#74647=CARTESIAN_POINT('Ctrl Pts',(-158.987480004205,227.455268949723,14.0730396980131));
#74648=CARTESIAN_POINT('Ctrl Pts',(-159.818614489535,227.515206669635,14.1259589864237));
#74649=CARTESIAN_POINT('Ctrl Pts',(-160.649748974866,227.575144389548,14.1788782748343));
#74650=CARTESIAN_POINT('Ctrl Pts',(-161.51353056741,227.182376589609,14.2317975632449));
#74651=CARTESIAN_POINT('Ctrl Pts',(-162.014692827404,226.516633807348,14.2847168516555));
#74652=CARTESIAN_POINT('Ctrl Pts',(-162.338892745142,226.085967389556,14.3189501336063));
#74653=CARTESIAN_POINT('Ctrl Pts',(-162.511345689842,225.541067880575,14.3531834155572));
#74654=CARTESIAN_POINT('Ctrl Pts',(-162.514889421101,224.998220537573,14.387416697508));
#74655=CARTESIAN_POINT('Origin',(-160.,225.,10.));
#74656=CARTESIAN_POINT('',(-162.521411304029,224.999178326235,15.387416697508));
#74657=CARTESIAN_POINT('',(-162.518630417247,225.00219537304,15.112583302492));
#74658=CARTESIAN_POINT('',(-162.5175,225.,10.));
#74659=CARTESIAN_POINT('Ctrl Pts',(-162.518630417247,225.00219537304,15.112583302492));
#74660=CARTESIAN_POINT('Ctrl Pts',(-162.520103889651,225.163256307148,15.1023879340014));
#74661=CARTESIAN_POINT('Ctrl Pts',(-162.505977686418,225.32405978629,15.0921925655108));
#74662=CARTESIAN_POINT('Ctrl Pts',(-162.475314724012,225.48164555077,15.0819971970202));
#74663=CARTESIAN_POINT('Ctrl Pts',(-162.316157931139,226.299597989434,15.0290779086096));
#74664=CARTESIAN_POINT('Ctrl Pts',(-161.711475666162,227.030860295603,14.9761586201991));
#74665=CARTESIAN_POINT('Ctrl Pts',(-160.937970521645,227.340806852351,14.9232393317885));
#74666=CARTESIAN_POINT('Ctrl Pts',(-160.164465377128,227.650753409099,14.8703200433779));
#74667=CARTESIAN_POINT('Ctrl Pts',(-159.22213735307,227.539384216426,14.8174007549673));
#74668=CARTESIAN_POINT('Ctrl Pts',(-158.542195734753,227.05766181471,14.7644814665567));
#74669=CARTESIAN_POINT('Ctrl Pts',(-157.862254116436,226.575939412994,14.7115621781461));
#74670=CARTESIAN_POINT('Ctrl Pts',(-157.44469890386,225.723863802235,14.6586428897355));
#74671=CARTESIAN_POINT('Ctrl Pts',(-157.480603354089,224.891344765162,14.6057236013249));
#74672=CARTESIAN_POINT('Ctrl Pts',(-157.516507804318,224.05882572809,14.5528043129143));
#74673=CARTESIAN_POINT('Ctrl Pts',(-158.005871917352,223.245863264704,14.4998850245037));
#74674=CARTESIAN_POINT('Ctrl Pts',(-158.724762684689,222.824468982265,14.4469657360931));
#74675=CARTESIAN_POINT('Ctrl Pts',(-159.443653452027,222.403074699827,14.3940464476825));
#74676=CARTESIAN_POINT('Ctrl Pts',(-160.392070873667,222.373248598336,14.3411271592719));
#74677=CARTESIAN_POINT('Ctrl Pts',(-161.136019156115,222.748639101249,14.2882078708613));
#74678=CARTESIAN_POINT('Ctrl Pts',(-161.879967438563,223.124029604161,14.2352885824507));
#74679=CARTESIAN_POINT('Ctrl Pts',(-162.419446581819,223.904636711477,14.1823692940401));
#74680=CARTESIAN_POINT('Ctrl Pts',(-162.507590940537,224.733254626237,14.1294500056295));
#74681=CARTESIAN_POINT('Ctrl Pts',(-162.516955545746,224.82128838987,14.1238277712503));
#74682=CARTESIAN_POINT('Ctrl Pts',(-162.521225801796,224.909864065682,14.1182055368711));
#74683=CARTESIAN_POINT('Ctrl Pts',(-162.520601007743,224.998500607742,14.1125833024919));
#74684=CARTESIAN_POINT('Ctrl Pts',(-162.514889421101,224.998220537573,14.387416697508));
#74685=CARTESIAN_POINT('Ctrl Pts',(-162.516823742949,224.701910970393,14.4061027039678));
#74686=CARTESIAN_POINT('Ctrl Pts',(-162.468432430799,224.406212835544,14.4247887104275));
#74687=CARTESIAN_POINT('Ctrl Pts',(-162.366924368858,224.130037744216,14.4434747168873));
#74688=CARTESIAN_POINT('Ctrl Pts',(-162.079450722877,223.347902227928,14.4963940052979));
#74689=CARTESIAN_POINT('Ctrl Pts',(-161.36596050347,222.722348959933,14.5493132937085));
#74690=CARTESIAN_POINT('Ctrl Pts',(-160.552946821011,222.539631103367,14.6022325821191));
#74691=CARTESIAN_POINT('Ctrl Pts',(-159.739933138551,222.356913246801,14.6551518705297));
#74692=CARTESIAN_POINT('Ctrl Pts',(-158.827395993039,222.617030801664,14.7080711589403));
#74693=CARTESIAN_POINT('Ctrl Pts',(-158.232912364318,223.200953979965,14.7609904473509));
#74694=CARTESIAN_POINT('Ctrl Pts',(-157.638428735597,223.784877158266,14.8139097357615));
#74695=CARTESIAN_POINT('Ctrl Pts',(-157.361998623667,224.692605960004,14.8668290241721));
#74696=CARTESIAN_POINT('Ctrl Pts',(-157.530116442313,225.508763703353,14.9197483125827));
#74697=CARTESIAN_POINT('Ctrl Pts',(-157.698234260958,226.324921446702,14.9726676009933));
#74698=CARTESIAN_POINT('Ctrl Pts',(-158.310900010178,227.049508131661,15.0255868894039));
#74699=CARTESIAN_POINT('Ctrl Pts',(-159.087757855177,227.350952905439,15.0785061778145));
#74700=CARTESIAN_POINT('Ctrl Pts',(-159.864615700175,227.652397679217,15.131425466225));
#74701=CARTESIAN_POINT('Ctrl Pts',(-160.805665640952,227.530700541815,15.1843447546356));
#74702=CARTESIAN_POINT('Ctrl Pts',(-161.48028324311,227.041550100916,15.2372640430462));
#74703=CARTESIAN_POINT('Ctrl Pts',(-162.118334300063,226.578913260688,15.2873149278668));
#74704=CARTESIAN_POINT('Ctrl Pts',(-162.518053298317,225.787577949575,15.3373658126874));
#74705=CARTESIAN_POINT('Ctrl Pts',(-162.521411304029,224.999178326235,15.387416697508));
#74706=CARTESIAN_POINT('Origin',(-160.,225.,10.));
#74707=CARTESIAN_POINT('',(-162.517311833712,225.002301033826,16.387416697508));
#74708=CARTESIAN_POINT('',(-162.51348711883,225.000116346804,16.1125833024919));
#74709=CARTESIAN_POINT('',(-162.5175,225.,10.));
#74710=CARTESIAN_POINT('Ctrl Pts',(-162.51348711883,225.000116346804,16.1125833024919));
#74711=CARTESIAN_POINT('Ctrl Pts',(-162.513657421629,225.413188244457,16.0865703311316));
#74712=CARTESIAN_POINT('Ctrl Pts',(-162.417512298305,225.82618548606,16.0605573597713));
#74713=CARTESIAN_POINT('Ctrl Pts',(-162.22461752507,226.187536225391,16.034544388411));
#74714=CARTESIAN_POINT('Ctrl Pts',(-161.832203525286,226.922647325434,15.9816251000004));
#74715=CARTESIAN_POINT('Ctrl Pts',(-161.039386391521,227.444016862716,15.9287058115898));
#74716=CARTESIAN_POINT('Ctrl Pts',(-160.208959228585,227.513066147216,15.8757865231792));
#74717=CARTESIAN_POINT('Ctrl Pts',(-159.37853206565,227.582115431716,15.8228672347686));
#74718=CARTESIAN_POINT('Ctrl Pts',(-158.510494873542,227.198844463435,15.769947946358));
#74719=CARTESIAN_POINT('Ctrl Pts',(-158.002061454311,226.538638029927,15.7170286579474));
#74720=CARTESIAN_POINT('Ctrl Pts',(-157.49362803508,225.878431596419,15.6641093695368));
#74721=CARTESIAN_POINT('Ctrl Pts',(-157.344798388724,224.941289697685,15.6111900811262));
#74722=CARTESIAN_POINT('Ctrl Pts',(-157.623676958487,224.156048448157,15.5582707927156));
#74723=CARTESIAN_POINT('Ctrl Pts',(-157.90255552825,223.370807198628,15.505351504305));
#74724=CARTESIAN_POINT('Ctrl Pts',(-158.609142314132,222.737466598306,15.4524322158944));
#74725=CARTESIAN_POINT('Ctrl Pts',(-159.420103216808,222.545843293445,15.3995129274838));
#74726=CARTESIAN_POINT('Ctrl Pts',(-160.231064119483,222.354219988584,15.3465936390732));
#74727=CARTESIAN_POINT('Ctrl Pts',(-161.146399138952,222.604313979185,15.2936743506626));
#74728=CARTESIAN_POINT('Ctrl Pts',(-161.747250988303,223.181682260065,15.240755062252));
#74729=CARTESIAN_POINT('Ctrl Pts',(-162.232343419937,223.647815440189,15.198031142332));
#74730=CARTESIAN_POINT('Ctrl Pts',(-162.512455798149,224.327265922729,15.155307222412));
#74731=CARTESIAN_POINT('Ctrl Pts',(-162.518630417247,225.00219537304,15.112583302492));
#74732=CARTESIAN_POINT('Ctrl Pts',(-162.521411304029,224.999178326235,15.387416697508));
#74733=CARTESIAN_POINT('Ctrl Pts',(-162.52160375049,224.953995342597,15.390285101098));
#74734=CARTESIAN_POINT('Ctrl Pts',(-162.520494386053,224.908822000952,15.393153504688));
#74735=CARTESIAN_POINT('Ctrl Pts',(-162.51805346516,224.863720724318,15.396021908278));
#74736=CARTESIAN_POINT('Ctrl Pts',(-162.473020821511,224.031645533015,15.4489411966886));
#74737=CARTESIAN_POINT('Ctrl Pts',(-161.974770270673,223.224098894804,15.5018604850992));
#74738=CARTESIAN_POINT('Ctrl Pts',(-161.251301254915,222.810614135462,15.5547797735098));
#74739=CARTESIAN_POINT('Ctrl Pts',(-160.527832239156,222.397129376119,15.6076990619204));
#74740=CARTESIAN_POINT('Ctrl Pts',(-159.579144758477,222.377706495644,15.660618350331));
#74741=CARTESIAN_POINT('Ctrl Pts',(-158.83935818538,222.761233403743,15.7135376387416));
#74742=CARTESIAN_POINT('Ctrl Pts',(-158.099571612282,223.144760311842,15.7664569271522));
#74743=CARTESIAN_POINT('Ctrl Pts',(-157.568685946766,223.931237008516,15.8193762155628));
#74744=CARTESIAN_POINT('Ctrl Pts',(-157.48963445894,224.760771772865,15.8722955039734));
#74745=CARTESIAN_POINT('Ctrl Pts',(-157.410582971115,225.590306537214,15.925214792384));
#74746=CARTESIAN_POINT('Ctrl Pts',(-157.783365660981,226.462899369238,15.9781340807946));
#74747=CARTESIAN_POINT('Ctrl Pts',(-158.437397176969,226.979251806087,16.0310533692052));
#74748=CARTESIAN_POINT('Ctrl Pts',(-159.091428692956,227.495604242937,16.0839726576158));
#74749=CARTESIAN_POINT('Ctrl Pts',(-160.026709035066,227.655716284612,16.1368919460264));
#74750=CARTESIAN_POINT('Ctrl Pts',(-160.815253937172,227.38632066414,16.189811234437));
#74751=CARTESIAN_POINT('Ctrl Pts',(-161.603798839277,227.116925043669,16.2427305228476));
#74752=CARTESIAN_POINT('Ctrl Pts',(-162.245608301378,226.418021761049,16.2956498112582));
#74753=CARTESIAN_POINT('Ctrl Pts',(-162.446990326167,225.609428944358,16.3485690996688));
#74754=CARTESIAN_POINT('Ctrl Pts',(-162.496267934553,225.411568583155,16.3615182989485));
#74755=CARTESIAN_POINT('Ctrl Pts',(-162.51917420259,225.207140374923,16.3744674982283));
#74756=CARTESIAN_POINT('Ctrl Pts',(-162.517311833712,225.002301033826,16.387416697508));
#74757=CARTESIAN_POINT('Origin',(-160.,225.,10.));
#74758=CARTESIAN_POINT('',(-162.51361180286,224.999405384875,17.387416697508));
#74759=CARTESIAN_POINT('',(-162.518203433835,224.997743576262,17.1125833024919));
#74760=CARTESIAN_POINT('',(-162.5175,225.,10.));
#74761=CARTESIAN_POINT('Ctrl Pts',(-162.518203433835,224.997743576262,17.1125833024919));
#74762=CARTESIAN_POINT('Ctrl Pts',(-162.512102125057,225.658848760357,17.0707527282619));
#74763=CARTESIAN_POINT('Ctrl Pts',(-162.244817921865,226.324319952305,17.0289221540318));
#74764=CARTESIAN_POINT('Ctrl Pts',(-161.777620784395,226.788639081685,16.9870915798017));
#74765=CARTESIAN_POINT('Ctrl Pts',(-161.186576063699,227.376042873634,16.9341722913911));
#74766=CARTESIAN_POINT('Ctrl Pts',(-160.275581992911,227.64151416071,16.8812530029806));
#74767=CARTESIAN_POINT('Ctrl Pts',(-159.461509439912,227.463573286232,16.82833371457));
#74768=CARTESIAN_POINT('Ctrl Pts',(-158.647436886914,227.285632411754,16.7754144261594));
#74769=CARTESIAN_POINT('Ctrl Pts',(-157.930285851704,226.664279375724,16.7224951377488));
#74770=CARTESIAN_POINT('Ctrl Pts',(-157.638224634377,225.88384531566,16.6695758493382));
#74771=CARTESIAN_POINT('Ctrl Pts',(-157.34616341705,225.103411255596,16.6166565609276));
#74772=CARTESIAN_POINT('Ctrl Pts',(-157.479192017605,224.163896171499,16.563737272517));
#74773=CARTESIAN_POINT('Ctrl Pts',(-157.976436550811,223.495222147163,16.5108179841064));
#74774=CARTESIAN_POINT('Ctrl Pts',(-158.473681084018,222.826548122827,16.4578986956958));
#74775=CARTESIAN_POINT('Ctrl Pts',(-159.335141549876,222.428715158251,16.4049794072852));
#74776=CARTESIAN_POINT('Ctrl Pts',(-160.166613656259,222.483771610307,16.3520601188746));
#74777=CARTESIAN_POINT('Ctrl Pts',(-160.998085762643,222.538828062363,16.299140830464));
#74778=CARTESIAN_POINT('Ctrl Pts',(-161.799569509551,223.046773931052,16.2462215420534));
#74779=CARTESIAN_POINT('Ctrl Pts',(-162.204305950103,223.775173196799,16.1933022536428));
#74780=CARTESIAN_POINT('Ctrl Pts',(-162.410090406365,224.145520988162,16.1663959365925));
#74781=CARTESIAN_POINT('Ctrl Pts',(-162.513310967437,224.572858603394,16.1394896195422));
#74782=CARTESIAN_POINT('Ctrl Pts',(-162.51348711883,225.000116346804,16.1125833024919));
#74783=CARTESIAN_POINT('Ctrl Pts',(-162.517311833712,225.002301033826,16.387416697508));
#74784=CARTESIAN_POINT('Ctrl Pts',(-162.511563289078,224.370026671198,16.4273867866389));
#74785=CARTESIAN_POINT('Ctrl Pts',(-162.269828596412,223.73383519107,16.4673568757697));
#74786=CARTESIAN_POINT('Ctrl Pts',(-161.839241264813,223.274787878362,16.5073269649006));
#74787=CARTESIAN_POINT('Ctrl Pts',(-161.269155591191,222.667021979822,16.5602462533112));
#74788=CARTESIAN_POINT('Ctrl Pts',(-160.368029656471,222.369772533509,16.6131655417218));
#74789=CARTESIAN_POINT('Ctrl Pts',(-159.548218670367,222.519060878874,16.6660848301324));
#74790=CARTESIAN_POINT('Ctrl Pts',(-158.728407684263,222.668349224239,16.719004118543));
#74791=CARTESIAN_POINT('Ctrl Pts',(-157.989911646774,223.264175361282,16.7719234069536));
#74792=CARTESIAN_POINT('Ctrl Pts',(-157.670666330748,224.03388926418,16.8248426953642));
#74793=CARTESIAN_POINT('Ctrl Pts',(-157.351421014722,224.803603167077,16.8777619837748));
#74794=CARTESIAN_POINT('Ctrl Pts',(-157.451426420158,225.747204835827,16.9306812721854));
#74795=CARTESIAN_POINT('Ctrl Pts',(-157.924920074226,226.432902159615,16.983600560596));
#74796=CARTESIAN_POINT('Ctrl Pts',(-158.398413728293,227.118599483403,17.0365198490066));
#74797=CARTESIAN_POINT('Ctrl Pts',(-159.245395630993,227.546392462228,17.0894391374172));
#74798=CARTESIAN_POINT('Ctrl Pts',(-160.078286882935,227.52052304932,17.1423584258278));
#74799=CARTESIAN_POINT('Ctrl Pts',(-160.911178134878,227.494653636412,17.1952777142384));
#74800=CARTESIAN_POINT('Ctrl Pts',(-161.729978736064,227.015121831771,17.248197002649));
#74801=CARTESIAN_POINT('Ctrl Pts',(-162.160005542026,226.301361355021,17.3011162910596));
#74802=CARTESIAN_POINT('Ctrl Pts',(-162.393767113989,225.91336281926,17.329883093209));
#74803=CARTESIAN_POINT('Ctrl Pts',(-162.512646638904,225.456150078067,17.3586498953585));
#74804=CARTESIAN_POINT('Ctrl Pts',(-162.51361180286,224.999405384875,17.387416697508));
#74805=CARTESIAN_POINT('Origin',(-160.,225.,10.));
#74806=CARTESIAN_POINT('',(-162.519491434632,224.998011610487,18.387416697508));
#74807=CARTESIAN_POINT('',(-162.520906539752,225.001296842262,18.1125833024919));
#74808=CARTESIAN_POINT('',(-162.5175,225.,10.));
#74809=CARTESIAN_POINT('Ctrl Pts',(-162.520906539752,225.001296842262,18.1125833024919));
#74810=CARTESIAN_POINT('Ctrl Pts',(-162.521374419554,225.075825678322,18.1078544138027));
#74811=CARTESIAN_POINT('Ctrl Pts',(-162.518355714192,225.150316081198,18.1031255251135));
#74812=CARTESIAN_POINT('Ctrl Pts',(-162.511727028206,225.224483843695,18.0983966364243));
#74813=CARTESIAN_POINT('Ctrl Pts',(-162.437547793174,226.054468534037,18.0454773480137));
#74814=CARTESIAN_POINT('Ctrl Pts',(-161.911289198169,226.844048836985,17.9925580596031));
#74815=CARTESIAN_POINT('Ctrl Pts',(-161.173767331383,227.231912975972,17.9396387711925));
#74816=CARTESIAN_POINT('Ctrl Pts',(-160.436245464596,227.619777114959,17.8867194827819));
#74817=CARTESIAN_POINT('Ctrl Pts',(-159.487460326027,227.605925089986,17.8338001943713));
#74818=CARTESIAN_POINT('Ctrl Pts',(-158.761575896687,227.196695512932,17.7808809059607));
#74819=CARTESIAN_POINT('Ctrl Pts',(-158.035691467348,226.787465935877,17.7279616175501));
#74820=CARTESIAN_POINT('Ctrl Pts',(-157.532707747238,225.98285880674,17.6750423291395));
#74821=CARTESIAN_POINT('Ctrl Pts',(-157.482790115221,225.151062367887,17.6221230407289));
#74822=CARTESIAN_POINT('Ctrl Pts',(-157.432872483204,224.319265929034,17.5692037523183));
#74823=CARTESIAN_POINT('Ctrl Pts',(-157.836020939279,223.460280180465,17.5162844639077));
#74824=CARTESIAN_POINT('Ctrl Pts',(-158.507754739353,222.967176966537,17.4633651754971));
#74825=CARTESIAN_POINT('Ctrl Pts',(-159.179488539427,222.47407375261,17.4104458870865));
#74826=CARTESIAN_POINT('Ctrl Pts',(-160.119807683499,222.346853073324,17.3575265986759));
#74827=CARTESIAN_POINT('Ctrl Pts',(-160.898422158656,222.643731117356,17.3046073102653));
#74828=CARTESIAN_POINT('Ctrl Pts',(-161.677036633814,222.940609161388,17.2516880218547));
#74829=CARTESIAN_POINT('Ctrl Pts',(-162.293946440056,223.661585928738,17.1987687334441));
#74830=CARTESIAN_POINT('Ctrl Pts',(-162.466853657876,224.476742460824,17.1458494450335));
#74831=CARTESIAN_POINT('Ctrl Pts',(-162.503084657493,224.647550460482,17.134760730853));
#74832=CARTESIAN_POINT('Ctrl Pts',(-162.519820807501,224.822493617,17.1236720166725));
#74833=CARTESIAN_POINT('Ctrl Pts',(-162.518203433835,224.997743576262,17.1125833024919));
#74834=CARTESIAN_POINT('Ctrl Pts',(-162.51361180286,224.999405384875,17.387416697508));
#74835=CARTESIAN_POINT('Ctrl Pts',(-162.514422150463,224.615924458848,17.4115691837691));
#74836=CARTESIAN_POINT('Ctrl Pts',(-162.432112176184,224.232773469737,17.4357216700302));
#74837=CARTESIAN_POINT('Ctrl Pts',(-162.264887208673,223.891193775679,17.4598741562913));
#74838=CARTESIAN_POINT('Ctrl Pts',(-161.898489058622,223.142775821946,17.5127934447019));
#74839=CARTESIAN_POINT('Ctrl Pts',(-161.124439747783,222.593929063341,17.5657127331125));
#74840=CARTESIAN_POINT('Ctrl Pts',(-160.296944202049,222.495805659244,17.6186320215231));
#74841=CARTESIAN_POINT('Ctrl Pts',(-159.469448656315,222.397682255148,17.6715513099337));
#74842=CARTESIAN_POINT('Ctrl Pts',(-158.588506875685,222.750282205561,17.7244705983443));
#74843=CARTESIAN_POINT('Ctrl Pts',(-158.057237850476,223.392256001223,17.7773898867549));
#74844=CARTESIAN_POINT('Ctrl Pts',(-157.525968825266,224.034229796885,17.8303091751655));
#74845=CARTESIAN_POINT('Ctrl Pts',(-157.344372555475,224.965577437797,17.8832284635761));
#74846=CARTESIAN_POINT('Ctrl Pts',(-157.59554738929,225.760113802981,17.9361477519867));
#74847=CARTESIAN_POINT('Ctrl Pts',(-157.846722223105,226.554650168166,17.9890670403973));
#74848=CARTESIAN_POINT('Ctrl Pts',(-158.530668160525,227.212375257623,18.0419863288079));
#74849=CARTESIAN_POINT('Ctrl Pts',(-159.334411764228,227.432315035357,18.0949056172185));
#74850=CARTESIAN_POINT('Ctrl Pts',(-160.138155367931,227.652254813092,18.1478249056291));
#74851=CARTESIAN_POINT('Ctrl Pts',(-161.061696637917,227.434409279103,18.2007441940397));
#74852=CARTESIAN_POINT('Ctrl Pts',(-161.682422671056,226.878462570083,18.2536634824503));
#74853=CARTESIAN_POINT('Ctrl Pts',(-162.205383234183,226.410078470665,18.2982478874695));
#74854=CARTESIAN_POINT('Ctrl Pts',(-162.513404570081,225.701709071819,18.3428322924888));
#74855=CARTESIAN_POINT('Ctrl Pts',(-162.519491434632,224.998011610487,18.387416697508));
#74856=CARTESIAN_POINT('Origin',(-160.,225.,10.));
#74857=CARTESIAN_POINT('',(-162.519857258493,225.0018235551,19.387416697508));
#74858=CARTESIAN_POINT('',(-162.514309478995,225.001427434952,19.112583302492));
#74859=CARTESIAN_POINT('',(-162.5175,225.,10.));
#74860=CARTESIAN_POINT('',(-158.086534003335,226.635987203375,20.));
#74861=CARTESIAN_POINT('Ctrl Pts',(-162.519857258493,225.0018235551,19.387416697508));
#74862=CARTESIAN_POINT('Ctrl Pts',(-162.513963907793,224.285086687949,19.4328532664402));
#74863=CARTESIAN_POINT('Ctrl Pts',(-162.192666772489,223.563823557618,19.4782898353725));
#74864=CARTESIAN_POINT('Ctrl Pts',(-161.652075996519,223.094935228314,19.5237264043047));
#74865=CARTESIAN_POINT('Ctrl Pts',(-161.022458050931,222.548828043862,19.5766456927152));
#74866=CARTESIAN_POINT('Ctrl Pts',(-160.095370243792,222.345065019015,19.6295649811258));
#74867=CARTESIAN_POINT('Ctrl Pts',(-159.295373480112,222.578292534632,19.6824842695364));
#74868=CARTESIAN_POINT('Ctrl Pts',(-158.495376716432,222.811520050248,19.735403557947));
#74869=CARTESIAN_POINT('Ctrl Pts',(-157.82247099621,223.481738106327,19.7883228463576));
#74870=CARTESIAN_POINT('Ctrl Pts',(-157.584268188238,224.278797222609,19.8412421347682));
#74871=CARTESIAN_POINT('Ctrl Pts',(-157.346065380267,225.075856338892,19.8941614231788));
#74872=CARTESIAN_POINT('Ctrl Pts',(-157.542565484547,225.999756515379,19.9470807115894));
#74873=CARTESIAN_POINT('Ctrl Pts',(-158.086534003335,226.635987203375,20.));
#74874=CARTESIAN_POINT('',(-161.917152621948,226.63875490413,20.));
#74875=CARTESIAN_POINT('Origin',(-160.,225.,20.));
#74876=CARTESIAN_POINT('Ctrl Pts',(-161.917156323069,226.638757682714,20.));
#74877=CARTESIAN_POINT('Ctrl Pts',(-161.386618552193,227.2574510649,19.948244384658));
#74878=CARTESIAN_POINT('Ctrl Pts',(-160.527623943219,227.59712432977,19.896488769316));
#74879=CARTESIAN_POINT('Ctrl Pts',(-159.717628711707,227.505772044351,19.844733153974));
#74880=CARTESIAN_POINT('Ctrl Pts',(-158.889421550332,227.412365794477,19.7918138655634));
#74881=CARTESIAN_POINT('Ctrl Pts',(-158.112441940732,226.868333744093,19.7388945771528));
#74882=CARTESIAN_POINT('Ctrl Pts',(-157.741727875214,226.12214740534,19.6859752887422));
#74883=CARTESIAN_POINT('Ctrl Pts',(-157.371013809696,225.375961066586,19.6330560003316));
#74884=CARTESIAN_POINT('Ctrl Pts',(-157.40656528826,224.427620439464,19.580136711921));
#74885=CARTESIAN_POINT('Ctrl Pts',(-157.832358820112,223.7113146992,19.5272174235104));
#74886=CARTESIAN_POINT('Ctrl Pts',(-158.258152351964,222.995008958935,19.4742981350998));
#74887=CARTESIAN_POINT('Ctrl Pts',(-159.074187937105,222.51073810553,19.4213788466892));
#74888=CARTESIAN_POINT('Ctrl Pts',(-159.906929723711,222.479994259423,19.3684595582786));
#74889=CARTESIAN_POINT('Ctrl Pts',(-160.739671510318,222.449250413317,19.315540269868));
#74890=CARTESIAN_POINT('Ctrl Pts',(-161.589119498392,222.872033574509,19.2626209814574));
#74891=CARTESIAN_POINT('Ctrl Pts',(-162.066623166706,223.554931282467,19.2097016930469));
#74892=CARTESIAN_POINT('Ctrl Pts',(-162.358730821865,223.972686498648,19.1773288961952));
#74893=CARTESIAN_POINT('Ctrl Pts',(-162.511647724414,224.487783003849,19.1449560993436));
#74894=CARTESIAN_POINT('Ctrl Pts',(-162.514309478995,225.001427434952,19.112583302492));
#74895=CARTESIAN_POINT('Origin',(0.,-225.,10.));
#74896=CARTESIAN_POINT('',(-2.5134738280043,-224.999414148646,0.387416697508012));
#74897=CARTESIAN_POINT('',(-2.51553384111454,-225.003594604017,0.112583302491983));
#74898=CARTESIAN_POINT('',(-2.5175,-225.,10.));
#74899=CARTESIAN_POINT('',(-1.91346599666507,-223.364012796625,0.));
#74900=CARTESIAN_POINT('Ctrl Pts',(-2.51553384111454,-225.003594604017,
0.112583302491983));
#74901=CARTESIAN_POINT('Ctrl Pts',(-2.510318857578,-224.410959591099,0.0750555349946555));
#74902=CARTESIAN_POINT('Ctrl Pts',(-2.29922182808404,-223.815196439696,
0.037527767497328));
#74903=CARTESIAN_POINT('Ctrl Pts',(-1.91346599666507,-223.364012796625,
0.));
#74904=CARTESIAN_POINT('',(1.91712505749227,-223.361260570198,1.64203312618124E-15));
#74905=CARTESIAN_POINT('Origin',(0.,-225.,0.));
#74906=CARTESIAN_POINT('Ctrl Pts',(1.91712862604369,-223.36125788605,1.4081598368354E-15));
#74907=CARTESIAN_POINT('Ctrl Pts',(1.38658196318478,-222.742517051696,0.0517556153419835));
#74908=CARTESIAN_POINT('Ctrl Pts',(0.527608265094371,-222.402929728057,
0.103511230683964));
#74909=CARTESIAN_POINT('Ctrl Pts',(-0.282369175077661,-222.49429768012,
0.155266846025946));
#74910=CARTESIAN_POINT('Ctrl Pts',(-1.11055814509214,-222.587719948888,
0.208186134436544));
#74911=CARTESIAN_POINT('Ctrl Pts',(-1.88752282473288,-223.131694547948,
0.261105422847144));
#74912=CARTESIAN_POINT('Ctrl Pts',(-2.25823169761475,-223.877857467097,
0.314024711257743));
#74913=CARTESIAN_POINT('Ctrl Pts',(-2.42960626517823,-224.222800242831,
0.3384887066745));
#74914=CARTESIAN_POINT('Ctrl Pts',(-2.51415951692064,-224.610952877235,
0.362952702091256));
#74915=CARTESIAN_POINT('Ctrl Pts',(-2.5134738280043,-224.999414148646,0.387416697508012));
#74916=CARTESIAN_POINT('Origin',(0.,-225.,10.));
#74917=CARTESIAN_POINT('',(-2.5174184095497,-225.002301197522,1.38741669750801));
#74918=CARTESIAN_POINT('',(-2.52168724981252,-224.999862409999,1.11258330249199));
#74919=CARTESIAN_POINT('',(-2.5175,-225.,10.));
#74920=CARTESIAN_POINT('Ctrl Pts',(-2.52168724981252,-224.999862409999,
1.11258330249199));
#74921=CARTESIAN_POINT('Ctrl Pts',(-2.52169211725575,-224.99315326678,1.11215722053551));
#74922=CARTESIAN_POINT('Ctrl Pts',(-2.52166766934934,-224.986444162339,
1.11173113857903));
#74923=CARTESIAN_POINT('Ctrl Pts',(-2.52161379929192,-224.979735296596,
1.11130505662256));
#74924=CARTESIAN_POINT('Ctrl Pts',(-2.514923149613,-224.146495597611,1.05838576821196));
#74925=CARTESIAN_POINT('Ctrl Pts',(-2.05437854416698,-223.316937960849,
1.00546647980136));
#74926=CARTESIAN_POINT('Ctrl Pts',(-1.35071294162604,-222.870578888206,
0.952547191390766));
#74927=CARTESIAN_POINT('Ctrl Pts',(-0.647047339085058,-222.424219815563,
0.899627902980166));
#74928=CARTESIAN_POINT('Ctrl Pts',(0.299739260550884,-222.361059307038,
0.846708614569566));
#74929=CARTESIAN_POINT('Ctrl Pts',(1.05637246458552,-222.710180484341,0.793789326158967));
#74930=CARTESIAN_POINT('Ctrl Pts',(1.81300566862008,-223.059301661644,0.740870037748372));
#74931=CARTESIAN_POINT('Ctrl Pts',(2.37948547705339,-223.820704524774,0.687950749337777));
#74932=CARTESIAN_POINT('Ctrl Pts',(2.49664120954915,-224.645603706033,0.635031460927181));
#74933=CARTESIAN_POINT('Ctrl Pts',(2.61379694204491,-225.470502887292,0.582112172516582));
#74934=CARTESIAN_POINT('Ctrl Pts',(2.28162859860309,-226.358898386679,0.529192884105983));
#74935=CARTESIAN_POINT('Ctrl Pts',(1.65203473703061,-226.905008475225,0.476273595695384));
#74936=CARTESIAN_POINT('Ctrl Pts',(1.02244087545817,-227.45111856377,0.423354307284788));
#74937=CARTESIAN_POINT('Ctrl Pts',(0.0954214957550896,-227.654943241475,
0.370435018874193));
#74938=CARTESIAN_POINT('Ctrl Pts',(-0.704614946080803,-227.421676512248,
0.317515730463596));
#74939=CARTESIAN_POINT('Ctrl Pts',(-1.50465138791669,-227.188409783022,
0.264596442052999));
#74940=CARTESIAN_POINT('Ctrl Pts',(-2.17770489188541,-226.518051646864,
0.2116771536424));
#74941=CARTESIAN_POINT('Ctrl Pts',(-2.41590067376944,-225.721010072264,
0.158757865231803));
#74942=CARTESIAN_POINT('Ctrl Pts',(-2.48517967332582,-225.489191345432,
0.14336634431853));
#74943=CARTESIAN_POINT('Ctrl Pts',(-2.51767269811346,-225.246656070328,
0.127974823405257));
#74944=CARTESIAN_POINT('Ctrl Pts',(-2.51553384111454,-225.003594604017,
0.112583302491983));
#74945=CARTESIAN_POINT('Ctrl Pts',(-2.5134738280043,-224.999414148646,0.387416697508012));
#74946=CARTESIAN_POINT('Ctrl Pts',(-2.51267626903306,-225.451252824483,
0.415871990501852));
#74947=CARTESIAN_POINT('Ctrl Pts',(-2.39655744609628,-225.903509060763,
0.444327283495693));
#74948=CARTESIAN_POINT('Ctrl Pts',(-2.16760745744079,-226.288671524275,
0.472782576489533));
#74949=CARTESIAN_POINT('Ctrl Pts',(-1.74182127826191,-227.004971423064,
0.525701864900131));
#74950=CARTESIAN_POINT('Ctrl Pts',(-0.925795853781111,-227.489219981405,
0.578621153310729));
#74951=CARTESIAN_POINT('Ctrl Pts',(-0.0930673405406173,-227.519960009479,
0.631540441721328));
#74952=CARTESIAN_POINT('Ctrl Pts',(0.739661172699829,-227.550700037554,
0.684459730131924));
#74953=CARTESIAN_POINT('Ctrl Pts',(1.58909277469996,-227.127931535363,0.73737901854252));
#74954=CARTESIAN_POINT('Ctrl Pts',(2.0665881116238,-226.445046923735,0.790298306953116));
#74955=CARTESIAN_POINT('Ctrl Pts',(2.54408344854767,-225.762162312107,0.843217595363715));
#74956=CARTESIAN_POINT('Ctrl Pts',(2.64964252039518,-224.819161591042,0.896136883774315));
#74957=CARTESIAN_POINT('Ctrl Pts',(2.33493169451256,-224.047594583661,0.949056172184913));
#74958=CARTESIAN_POINT('Ctrl Pts',(2.02022086862996,-223.27602757628,1.00197546059551));
#74959=CARTESIAN_POINT('Ctrl Pts',(1.28524014501729,-222.675894282583,1.05489474900611));
#74960=CARTESIAN_POINT('Ctrl Pts',(0.466331362713798,-222.521799579672,
1.1078140374167));
#74961=CARTESIAN_POINT('Ctrl Pts',(-0.352577419589698,-222.367704876761,
1.1607333258273));
#74962=CARTESIAN_POINT('Ctrl Pts',(-1.25541426058401,-222.659648764636,
1.2136526142379));
#74963=CARTESIAN_POINT('Ctrl Pts',(-1.82904826482005,-223.264045656224,
1.2665719026485));
#74964=CARTESIAN_POINT('Ctrl Pts',(-2.26569235464287,-223.724106128007,
1.306853500935));
#74965=CARTESIAN_POINT('Ctrl Pts',(-2.51159328780835,-224.365204748859,
1.34713509922151));
#74966=CARTESIAN_POINT('Ctrl Pts',(-2.5174184095497,-225.002301197522,1.38741669750801));
#74967=CARTESIAN_POINT('Origin',(0.,-225.,10.));
#74968=CARTESIAN_POINT('',(-2.52129902664413,-224.999094489651,2.38741669750801));
#74969=CARTESIAN_POINT('',(-2.51578360809179,-224.997885154191,2.11258330249199));
#74970=CARTESIAN_POINT('',(-2.5175,-225.,10.));
#74971=CARTESIAN_POINT('Ctrl Pts',(-2.51578360809179,-224.997885154191,
2.11258330249199));
#74972=CARTESIAN_POINT('Ctrl Pts',(-2.5178326768567,-224.740549886453,2.09633961766576));
#74973=CARTESIAN_POINT('Ctrl Pts',(-2.48151015149358,-224.483779262187,
2.08009593283954));
#74974=CARTESIAN_POINT('Ctrl Pts',(-2.40441279294324,-224.239898736946,
2.06385224801331));
#74975=CARTESIAN_POINT('Ctrl Pts',(-2.15324211360122,-223.445375573575,
2.01093295960272));
#74976=CARTESIAN_POINT('Ctrl Pts',(-1.46930748461902,-222.787661557655,
1.95801367119212));
#74977=CARTESIAN_POINT('Ctrl Pts',(-0.665577204289779,-222.567725340847,
1.90509438278152));
#74978=CARTESIAN_POINT('Ctrl Pts',(0.138153076039436,-222.347789124039,
1.85217509437092));
#74979=CARTESIAN_POINT('Ctrl Pts',(1.06167900771567,-222.565630706345,1.79925580596032));
#74980=CARTESIAN_POINT('Ctrl Pts',(1.6823947882024,-223.121568361418,1.74633651754973));
#74981=CARTESIAN_POINT('Ctrl Pts',(2.30311056868915,-223.677506016492,1.69341722913913));
#74982=CARTESIAN_POINT('Ctrl Pts',(2.62101619798637,-224.571539744334,1.64049794072853));
#74983=CARTESIAN_POINT('Ctrl Pts',(2.49063878605849,-225.394554494071,1.58757865231793));
#74984=CARTESIAN_POINT('Ctrl Pts',(2.36026137413062,-226.217569243809,1.53465936390734));
#74985=CARTESIAN_POINT('Ctrl Pts',(1.78160092097767,-226.969565015442,1.48174007549674));
#74986=CARTESIAN_POINT('Ctrl Pts',(1.01945097696467,-227.306439189746,1.42882078708614));
#74987=CARTESIAN_POINT('Ctrl Pts',(0.257301032951665,-227.643313364049,
1.37590149867554));
#74988=CARTESIAN_POINT('Ctrl Pts',(-0.688338401921387,-227.565065941023,
1.32298221026495));
#74989=CARTESIAN_POINT('Ctrl Pts',(-1.38473977240201,-227.107481348906,
1.27006292185435));
#74990=CARTESIAN_POINT('Ctrl Pts',(-2.07553403690411,-226.65358101907,1.21756971540023));
#74991=CARTESIAN_POINT('Ctrl Pts',(-2.52108758184044,-225.82642742821,1.16507650894611));
#74992=CARTESIAN_POINT('Ctrl Pts',(-2.52168724981252,-224.999862409999,
1.11258330249199));
#74993=CARTESIAN_POINT('Ctrl Pts',(-2.5174184095497,-225.002301197522,1.38741669750801));
#74994=CARTESIAN_POINT('Ctrl Pts',(-2.51924594585992,-225.20217974852,1.4000543876321));
#74995=CARTESIAN_POINT('Ctrl Pts',(-2.49744311761311,-225.401664370669,
1.4126920777562));
#74996=CARTESIAN_POINT('Ctrl Pts',(-2.4504865123205,-225.595040943422,1.42532976788029));
#74997=CARTESIAN_POINT('Ctrl Pts',(-2.25385958810712,-226.404789443731,
1.47824905629089));
#74998=CARTESIAN_POINT('Ctrl Pts',(-1.6161745722026,-227.107436549047,1.53116834470148));
#74999=CARTESIAN_POINT('Ctrl Pts',(-0.829237866958627,-227.381452880329,
1.58408763311208));
#75000=CARTESIAN_POINT('Ctrl Pts',(-0.0423011617146431,-227.65546921161,
1.63700692152268));
#75001=CARTESIAN_POINT('Ctrl Pts',(0.893887232868802,-227.500854768856,
1.68992620993328));
#75002=CARTESIAN_POINT('Ctrl Pts',(1.5509283882814,-226.988360171431,1.74284549834387));
#75003=CARTESIAN_POINT('Ctrl Pts',(2.207969543694,-226.475865574005,1.79576478675447));
#75004=CARTESIAN_POINT('Ctrl Pts',(2.58586345993575,-225.605490821907,1.84868407516507));
#75005=CARTESIAN_POINT('Ctrl Pts',(2.51168546372192,-224.775519850663,1.90160336357567));
#75006=CARTESIAN_POINT('Ctrl Pts',(2.43750746750809,-223.945548879419,1.95452265198626));
#75007=CARTESIAN_POINT('Ctrl Pts',(1.91125755883869,-223.155981689029,2.00744194039686));
#75008=CARTESIAN_POINT('Ctrl Pts',(1.17374789465563,-222.768123980806,2.06036122880746));
#75009=CARTESIAN_POINT('Ctrl Pts',(0.436238230472565,-222.380266272584,
2.11328051721805));
#75010=CARTESIAN_POINT('Ctrl Pts',(-0.512531189224167,-222.394118046529,
2.16619980562865));
#75011=CARTESIAN_POINT('Ctrl Pts',(-1.23840359958205,-222.803340844149,
2.21911909403925));
#75012=CARTESIAN_POINT('Ctrl Pts',(-1.96427600993995,-223.212563641768,
2.27203838244984));
#75013=CARTESIAN_POINT('Ctrl Pts',(-2.46725141095899,-224.017157463062,
2.32495767086044));
#75014=CARTESIAN_POINT('Ctrl Pts',(-2.5171682183347,-224.848940135592,2.37787695927104));
#75015=CARTESIAN_POINT('Ctrl Pts',(-2.52016771240887,-224.898921841723,
2.3810568720167));
#75016=CARTESIAN_POINT('Ctrl Pts',(-2.52153130634907,-224.949001721128,
2.38423678476236));
#75017=CARTESIAN_POINT('Ctrl Pts',(-2.52129902664413,-224.999094489651,
2.38741669750801));
#75018=CARTESIAN_POINT('Origin',(0.,-225.,10.));
#75019=CARTESIAN_POINT('',(-2.51474234901689,-224.998273792081,3.38741669750801));
#75020=CARTESIAN_POINT('',(-2.51418874373752,-225.001366293789,3.11258330249199));
#75021=CARTESIAN_POINT('',(-2.5175,-225.,10.));
#75022=CARTESIAN_POINT('Ctrl Pts',(-2.51418874373752,-225.001366293789,
3.11258330249199));
#75023=CARTESIAN_POINT('Ctrl Pts',(-2.5116814281143,-224.492634921714,3.08052201479602));
#75024=CARTESIAN_POINT('Ctrl Pts',(-2.36190816289223,-223.982546186139,
3.04846072710004));
#75025=CARTESIAN_POINT('Ctrl Pts',(-2.07504555938352,-223.567121570461,
3.01639943940406));
#75026=CARTESIAN_POINT('Ctrl Pts',(-1.60155974704675,-222.881435603683,
2.96348015099347));
#75027=CARTESIAN_POINT('Ctrl Pts',(-0.754591871553214,-222.453649713216,
2.91056086258287));
#75028=CARTESIAN_POINT('Ctrl Pts',(0.0782855864108173,-222.479518696041,
2.85764157417228));
#75029=CARTESIAN_POINT('Ctrl Pts',(0.911163044374884,-222.505387678867,
2.80472228576168));
#75030=CARTESIAN_POINT('Ctrl Pts',(1.72995008480944,-222.984911534986,2.75180299735108));
#75031=CARTESIAN_POINT('Ctrl Pts',(2.15996976906083,-223.698660193995,2.69888370894048));
#75032=CARTESIAN_POINT('Ctrl Pts',(2.5899894533122,-224.412408853004,2.64596442052988));
#75033=CARTESIAN_POINT('Ctrl Pts',(2.63124178138043,-225.360382314904,2.59304513211929));
#75034=CARTESIAN_POINT('Ctrl Pts',(2.26484969900841,-226.108787867573,2.54012584370869));
#75035=CARTESIAN_POINT('Ctrl Pts',(1.89845761663637,-226.857193420243,2.48720655529809));
#75036=CARTESIAN_POINT('Ctrl Pts',(1.12442112382405,-227.406031063681,2.43428726688749));
#75037=CARTESIAN_POINT('Ctrl Pts',(0.296939283634431,-227.50415285454,2.38136797847689));
#75038=CARTESIAN_POINT('Ctrl Pts',(-0.530542556555167,-227.6022746454,2.3284486900663));
#75039=CARTESIAN_POINT('Ctrl Pts',(-1.41146974412205,-227.24968058368,2.2755294016557));
#75040=CARTESIAN_POINT('Ctrl Pts',(-1.94272997305458,-226.60771739741,2.2226101132451));
#75041=CARTESIAN_POINT('Ctrl Pts',(-2.31091877796244,-226.162806136458,
2.18593450966073));
#75042=CARTESIAN_POINT('Ctrl Pts',(-2.51115714343535,-225.57890641684,2.14925890607636));
#75043=CARTESIAN_POINT('Ctrl Pts',(-2.51578360809179,-224.997885154191,
2.11258330249199));
#75044=CARTESIAN_POINT('Ctrl Pts',(-2.52129902664413,-224.999094489651,
2.38741669750801));
#75045=CARTESIAN_POINT('Ctrl Pts',(-2.51766576736073,-225.782632665356,
2.43715607317295));
#75046=CARTESIAN_POINT('Ctrl Pts',(-2.12357951610955,-226.569324345471,
2.4868954488379));
#75047=CARTESIAN_POINT('Ctrl Pts',(-1.49222055795853,-227.032789381898,
2.53663482450284));
#75048=CARTESIAN_POINT('Ctrl Pts',(-0.82049787647425,-227.525884431906,
2.58955411291343));
#75049=CARTESIAN_POINT('Ctrl Pts',(0.119805700226725,-227.653103008158,
2.64247340132403));
#75050=CARTESIAN_POINT('Ctrl Pts',(0.898407286222473,-227.356229879173,
2.69539268973463));
#75051=CARTESIAN_POINT('Ctrl Pts',(1.67700887221823,-227.059356750188,2.74831197814523));
#75052=CARTESIAN_POINT('Ctrl Pts',(2.29390846750877,-226.338391915967,2.80123126655583));
#75053=CARTESIAN_POINT('Ctrl Pts',(2.46681282336827,-225.523248877115,2.85415055496643));
#75054=CARTESIAN_POINT('Ctrl Pts',(2.63971717922775,-224.708105838262,2.90706984337702));
#75055=CARTESIAN_POINT('Ctrl Pts',(2.36862629565625,-223.798784594779,2.95998913178761));
#75056=CARTESIAN_POINT('Ctrl Pts',(1.7775913586249,-223.211390526533,3.01290842019821));
#75057=CARTESIAN_POINT('Ctrl Pts',(1.18655642159351,-222.623996458287,3.06582770860881));
#75058=CARTESIAN_POINT('Ctrl Pts',(0.275577431102228,-222.358529565279,
3.11874699701941));
#75059=CARTESIAN_POINT('Ctrl Pts',(-0.538481646178591,-222.53646749414,
3.17166628543));
#75060=CARTESIAN_POINT('Ctrl Pts',(-1.35254072345939,-222.714405423,3.2245855738406));
#75061=CARTESIAN_POINT('Ctrl Pts',(-2.06967988752974,-223.33574817373,3.2775048622512));
#75062=CARTESIAN_POINT('Ctrl Pts',(-2.36173627028926,-224.116169315018,
3.33042415066179));
#75063=CARTESIAN_POINT('Ctrl Pts',(-2.4665817029981,-224.396332999442,3.3494216662772));
#75064=CARTESIAN_POINT('Ctrl Pts',(-2.51664497692405,-224.696997767499,
3.36841918189261));
#75065=CARTESIAN_POINT('Ctrl Pts',(-2.51474234901689,-224.998273792081,
3.38741669750801));
#75066=CARTESIAN_POINT('Origin',(0.,-225.,10.));
#75067=CARTESIAN_POINT('',(-2.51505383944565,-225.001872855151,4.38741669750802));
#75068=CARTESIAN_POINT('',(-2.52076233832513,-225.001369535607,4.11258330249199));
#75069=CARTESIAN_POINT('',(-2.5175,-225.,10.));
#75070=CARTESIAN_POINT('Ctrl Pts',(-2.52076233832513,-225.001369535607,
4.11258330249199));
#75071=CARTESIAN_POINT('Ctrl Pts',(-2.51581109493886,-224.246714227313,
4.06470441192627));
#75072=CARTESIAN_POINT('Ctrl Pts',(-2.15430418959668,-223.487944707289,
4.01682552136055));
#75073=CARTESIAN_POINT('Ctrl Pts',(-1.56257694401589,-223.020780973236,
3.96894663079482));
#75074=CARTESIAN_POINT('Ctrl Pts',(-0.90855625975808,-222.504437087962,
3.91602734238422));
#75075=CARTESIAN_POINT('Ctrl Pts',(0.0267085927239957,-222.34432769804,
3.86310805397363));
#75076=CARTESIAN_POINT('Ctrl Pts',(0.81524043535916,-222.613718856892,3.81018876556303));
#75077=CARTESIAN_POINT('Ctrl Pts',(1.6037722779943,-222.883110015744,3.75726947715243));
#75078=CARTESIAN_POINT('Ctrl Pts',(2.24557111078254,-223.582001723371,3.70435018874184));
#75079=CARTESIAN_POINT('Ctrl Pts',(2.44694980038708,-224.390581148627,3.65143090033124));
#75080=CARTESIAN_POINT('Ctrl Pts',(2.64832848999163,-225.199160573883,3.59851161192064));
#75081=CARTESIAN_POINT('Ctrl Pts',(2.40928703641246,-226.117427716769,3.54559232351004));
#75082=CARTESIAN_POINT('Ctrl Pts',(1.83921080425351,-226.725183549692,3.49267303509944));
#75083=CARTESIAN_POINT('Ctrl Pts',(1.26913457209457,-227.332939382615,3.43975374668885));
#75084=CARTESIAN_POINT('Ctrl Pts',(0.368023561355883,-227.630183905574,
3.38683445827825));
#75085=CARTESIAN_POINT('Ctrl Pts',(-0.451773847463035,-227.480898032868,
3.33391516986765));
#75086=CARTESIAN_POINT('Ctrl Pts',(-1.27157125628195,-227.331612160162,
3.28099588145706));
#75087=CARTESIAN_POINT('Ctrl Pts',(-2.0100550631811,-226.73579589179,3.22807659304646));
#75088=CARTESIAN_POINT('Ctrl Pts',(-2.32929509204069,-225.966094736059,
3.17515730463586));
#75089=CARTESIAN_POINT('Ctrl Pts',(-2.45512272408338,-225.662719015438,
3.15429930392124));
#75090=CARTESIAN_POINT('Ctrl Pts',(-2.51581991936454,-225.332329897713,
3.13344130320662));
#75091=CARTESIAN_POINT('Ctrl Pts',(-2.51418874373752,-225.001366293789,
3.11258330249199));
#75092=CARTESIAN_POINT('Ctrl Pts',(-2.51474234901689,-224.998273792081,
3.38741669750801));
#75093=CARTESIAN_POINT('Ctrl Pts',(-2.51134503576355,-225.536229231171,
3.4213384703032));
#75094=CARTESIAN_POINT('Ctrl Pts',(-2.3422632039414,-226.076133558656,3.4552602430984));
#75095=CARTESIAN_POINT('Ctrl Pts',(-2.02352995235238,-226.50475294365,3.48918201589359));
#75096=CARTESIAN_POINT('Ctrl Pts',(-1.52629365020732,-227.173415899146,
3.54210130430419));
#75097=CARTESIAN_POINT('Ctrl Pts',(-0.66484744446852,-227.57124227829,3.59502059271479));
#75098=CARTESIAN_POINT('Ctrl Pts',(0.166610898230793,-227.516186737616,
3.64793988112538));
#75099=CARTESIAN_POINT('Ctrl Pts',(0.998069240930105,-227.461131196943,
3.70085916953598));
#75100=CARTESIAN_POINT('Ctrl Pts',(1.79953972058993,-226.953193736451,3.75377845794658));
#75101=CARTESIAN_POINT('Ctrl Pts',(2.20426946139026,-226.224806528169,3.80669774635718));
#75102=CARTESIAN_POINT('Ctrl Pts',(2.60899920219058,-225.496419319888,3.85961703476777));
#75103=CARTESIAN_POINT('Ctrl Pts',(2.61698820413141,-224.547582363817,3.91253632317837));
#75104=CARTESIAN_POINT('Ctrl Pts',(2.22458070012416,-223.812483432352,3.96545561158897));
#75105=CARTESIAN_POINT('Ctrl Pts',(1.83217319611691,-223.077384500887,4.01837489999956));
#75106=CARTESIAN_POINT('Ctrl Pts',(1.03936918616155,-222.556023594028,4.07129418841016));
#75107=CARTESIAN_POINT('Ctrl Pts',(0.208955769604636,-222.486975452526,
4.12421347682076));
#75108=CARTESIAN_POINT('Ctrl Pts',(-0.621457646952277,-222.417927311023,
4.17713276523135));
#75109=CARTESIAN_POINT('Ctrl Pts',(-1.48948047011075,-222.801191934877,
4.23005205364195));
#75110=CARTESIAN_POINT('Ctrl Pts',(-1.99790547305025,-223.461387439737,
4.28297134205255));
#75111=CARTESIAN_POINT('Ctrl Pts',(-2.33239365778951,-223.895724057166,
4.31778646053771));
#75112=CARTESIAN_POINT('Ctrl Pts',(-2.51124055525204,-224.449922020752,
4.35260157902286));
#75113=CARTESIAN_POINT('Ctrl Pts',(-2.51505383944565,-225.001872855151,
4.38741669750802));
#75114=CARTESIAN_POINT('Origin',(0.,-225.,10.));
#75115=CARTESIAN_POINT('',(-2.52148465865137,-225.000661258108,5.38741669750802));
#75116=CARTESIAN_POINT('',(-2.51831108560746,-224.997761985245,5.11258330249199));
#75117=CARTESIAN_POINT('',(-2.5175,-225.,10.));
#75118=CARTESIAN_POINT('Ctrl Pts',(-2.51831108560746,-224.997761985245,
5.11258330249199));
#75119=CARTESIAN_POINT('Ctrl Pts',(-2.51987989470443,-224.82746401479,5.10180609746711));
#75120=CARTESIAN_POINT('Ctrl Pts',(-2.50407988926802,-224.657455454451,
5.09102889244224));
#75121=CARTESIAN_POINT('Ctrl Pts',(-2.46984265276056,-224.491244722527,
5.08025168741736));
#75122=CARTESIAN_POINT('Ctrl Pts',(-2.30172761839515,-223.675100495958,
5.02733239900677));
#75123=CARTESIAN_POINT('Ctrl Pts',(-1.68907201582617,-222.950525811226,
4.97441311059617));
#75124=CARTESIAN_POINT('Ctrl Pts',(-0.912227036743379,-222.64908602982,
4.92149382218558));
#75125=CARTESIAN_POINT('Ctrl Pts',(-0.135382057660579,-222.347646248413,
4.86857453377498));
#75126=CARTESIAN_POINT('Ctrl Pts',(0.805652297936047,-222.469341370332,
4.81565524536438));
#75127=CARTESIAN_POINT('Ctrl Pts',(1.48025872742862,-222.958483710176,4.76273595695379));
#75128=CARTESIAN_POINT('Ctrl Pts',(2.15486515692122,-223.447626050019,4.70981666854319));
#75129=CARTESIAN_POINT('Ctrl Pts',(2.56304366030976,-224.304215607787,4.65689738013259));
#75130=CARTESIAN_POINT('Ctrl Pts',(2.51801176246824,-225.136277018694,4.60397809172199));
#75131=CARTESIAN_POINT('Ctrl Pts',(2.47297986462671,-225.968338429602,4.55105880331139));
#75132=CARTESIAN_POINT('Ctrl Pts',(1.97473756555515,-226.775871693649,4.4981395149008));
#75133=CARTESIAN_POINT('Ctrl Pts',(1.25128053151431,-227.18934960507,4.4452202264902));
#75134=CARTESIAN_POINT('Ctrl Pts',(0.527823497473455,-227.602827516492,
4.3923009380796));
#75135=CARTESIAN_POINT('Ctrl Pts',(-0.420848271536683,-227.622250075287,
4.339381649669));
#75136=CARTESIAN_POINT('Ctrl Pts',(-1.16062259267408,-227.238729518965,
4.2864623612584));
#75137=CARTESIAN_POINT('Ctrl Pts',(-1.90039691381146,-226.855208962643,
4.23354307284781));
#75138=CARTESIAN_POINT('Ctrl Pts',(-2.43127378707612,-226.068745291203,
4.18062378443721));
#75139=CARTESIAN_POINT('Ctrl Pts',(-2.51032396569167,-225.239224265169,
4.12770449602661));
#75140=CARTESIAN_POINT('Ctrl Pts',(-2.51785324966162,-225.160214964072,
4.12266409818174));
#75141=CARTESIAN_POINT('Ctrl Pts',(-2.52128357505804,-225.080815047912,
4.11762370033687));
#75142=CARTESIAN_POINT('Ctrl Pts',(-2.52076233832513,-225.001369535607,
4.11258330249199));
#75143=CARTESIAN_POINT('Ctrl Pts',(-2.51505383944565,-225.001872855151,
4.38741669750802));
#75144=CARTESIAN_POINT('Ctrl Pts',(-2.51703678099574,-225.288892176964,
4.40552086743346));
#75145=CARTESIAN_POINT('Ctrl Pts',(-2.4716890214524,-225.575303854349,4.4236250373589));
#75146=CARTESIAN_POINT('Ctrl Pts',(-2.37628370533025,-225.843937581591,
4.44172920728434));
#75147=CARTESIAN_POINT('Ctrl Pts',(-2.09740975195022,-226.629165832721,
4.49464849569494));
#75148=CARTESIAN_POINT('Ctrl Pts',(-1.39083466246961,-227.262495949115,
4.54756778410554));
#75149=CARTESIAN_POINT('Ctrl Pts',(-0.579887183939557,-227.454116081963,
4.60048707251614));
#75150=CARTESIAN_POINT('Ctrl Pts',(0.231060294590482,-227.64573621481,4.65340636092673));
#75151=CARTESIAN_POINT('Ctrl Pts',(1.14638016216995,-227.39564636411,4.70632564933733));
#75152=CARTESIAN_POINT('Ctrl Pts',(1.74722206539031,-226.818287640627,4.75924493774793));
#75153=CARTESIAN_POINT('Ctrl Pts',(2.34806396861067,-226.240928917144,4.81216422615853));
#75154=CARTESIAN_POINT('Ctrl Pts',(2.63442790747192,-225.336301320878,4.86508351456912));
#75155=CARTESIAN_POINT('Ctrl Pts',(2.47527374918222,-224.518362422092,4.91800280297972));
#75156=CARTESIAN_POINT('Ctrl Pts',(2.31611959089252,-223.700423523307,4.97092209139032));
#75157=CARTESIAN_POINT('Ctrl Pts',(1.71144733545193,-222.969173322003,5.02384137980092));
#75158=CARTESIAN_POINT('Ctrl Pts',(0.937954995060642,-222.659231895919,
5.07676066821151));
#75159=CARTESIAN_POINT('Ctrl Pts',(0.164462654669351,-222.349290469834,
5.12967995662211));
#75160=CARTESIAN_POINT('Ctrl Pts',(-0.777849770672657,-222.460657818971,
5.18259924503271));
#75161=CARTESIAN_POINT('Ctrl Pts',(-1.45778013365644,-222.942372246552,
5.23551853344331));
#75162=CARTESIAN_POINT('Ctrl Pts',(-2.10833167438353,-223.403272480038,
5.28615125479821));
#75163=CARTESIAN_POINT('Ctrl Pts',(-2.51868560060727,-224.2032068837,5.33678397615311));
#75164=CARTESIAN_POINT('Ctrl Pts',(-2.52148465865137,-225.000661258108,
5.38741669750802));
#75165=CARTESIAN_POINT('Origin',(0.,-225.,10.));
#75166=CARTESIAN_POINT('',(-2.51699551773447,-224.997707769369,6.38741669750802));
#75167=CARTESIAN_POINT('',(-2.51344103673693,-225.000035219284,6.11258330249199));
#75168=CARTESIAN_POINT('',(-2.5175,-225.,10.));
#75169=CARTESIAN_POINT('Ctrl Pts',(-2.51344103673693,-225.000035219284,
6.11258330249199));
#75170=CARTESIAN_POINT('Ctrl Pts',(-2.51338833654886,-224.577729214141,
6.08598849459737));
#75171=CARTESIAN_POINT('Ctrl Pts',(-2.41266892426312,-224.155399590225,
6.05939368670275));
#75172=CARTESIAN_POINT('Ctrl Pts',(-2.2114232112413,-223.788157583456,6.03279887880812));
#75173=CARTESIAN_POINT('Ctrl Pts',(-1.8109773809501,-223.057406462798,5.97987959039753));
#75174=CARTESIAN_POINT('Ctrl Pts',(-1.01250322696598,-222.544771713165,
5.92696030198693));
#75175=CARTESIAN_POINT('Ctrl Pts',(-0.181382506452433,-222.48483498591,
5.87404101357633));
#75176=CARTESIAN_POINT('Ctrl Pts',(0.649738214061123,-222.424898258654,
5.82112172516574));
#75177=CARTESIAN_POINT('Ctrl Pts',(1.51350550110408,-222.817659553777,5.76820243675514));
#75178=CARTESIAN_POINT('Ctrl Pts',(2.01465946110902,-223.483391310352,5.71528314834454));
#75179=CARTESIAN_POINT('Ctrl Pts',(2.51581342111396,-224.149123066927,5.66236385993394));
#75180=CARTESIAN_POINT('Ctrl Pts',(2.65435405408086,-225.087825284954,5.60944457152334));
#75181=CARTESIAN_POINT('Ctrl Pts',(2.36688516908806,-225.869947847921,5.55652528311275));
#75182=CARTESIAN_POINT('Ctrl Pts',(2.07941628409525,-226.652070410888,5.50360599470214));
#75183=CARTESIAN_POINT('Ctrl Pts',(1.36593788114273,-227.277613318795,5.45068670629155));
#75184=CARTESIAN_POINT('Ctrl Pts',(0.552937663393149,-227.460328149283,
5.39776741788095));
#75185=CARTESIAN_POINT('Ctrl Pts',(-0.260062554356385,-227.643042979771,
5.34484812947036));
#75186=CARTESIAN_POINT('Ctrl Pts',(-1.17258458690298,-227.382929732839,
5.29192884105976));
#75187=CARTESIAN_POINT('Ctrl Pts',(-1.76705837009536,-226.799016225171,
5.23900955264916));
#75188=CARTESIAN_POINT('Ctrl Pts',(-2.24046541116404,-226.334018821213,
5.19686746926344));
#75189=CARTESIAN_POINT('Ctrl Pts',(-2.51217657451406,-225.663677800595,
5.15472538587771));
#75190=CARTESIAN_POINT('Ctrl Pts',(-2.51831108560746,-224.997761985245,
5.11258330249199));
#75191=CARTESIAN_POINT('Ctrl Pts',(-2.52148465865137,-225.000661258108,
5.38741669750802));
#75192=CARTESIAN_POINT('Ctrl Pts',(-2.52161106374553,-225.036674193067,
5.38970326456371));
#75193=CARTESIAN_POINT('Ctrl Pts',(-2.52090629583595,-225.07268207022,5.39198983161941));
#75194=CARTESIAN_POINT('Ctrl Pts',(-2.51935494137685,-225.108653436226,
5.3942763986751));
#75195=CARTESIAN_POINT('Ctrl Pts',(-2.4834510854879,-225.941158692294,5.4471956870857));
#75196=CARTESIAN_POINT('Ctrl Pts',(-1.99409507308441,-226.754107698402,
5.5001149754963));
#75197=CARTESIAN_POINT('Ctrl Pts',(-1.27521620582045,-227.17549500534,5.55303426390689));
#75198=CARTESIAN_POINT('Ctrl Pts',(-0.556337338556501,-227.596882312277,
5.60595355231749));
#75199=CARTESIAN_POINT('Ctrl Pts',(0.392064383567916,-227.626707920045,
5.65887284072808));
#75200=CARTESIAN_POINT('Ctrl Pts',(1.13600035115615,-227.251323631115,5.71179212913868));
#75201=CARTESIAN_POINT('Ctrl Pts',(1.8799363187444,-226.875939342185,5.76471141754928));
#75202=CARTESIAN_POINT('Ctrl Pts',(2.41940653179646,-226.095345156556,5.81763070595987));
#75203=CARTESIAN_POINT('Ctrl Pts',(2.50754943142679,-225.266740958225,5.87054999437047));
#75204=CARTESIAN_POINT('Ctrl Pts',(2.59569233105713,-224.438136759894,5.92346928278107));
#75205=CARTESIAN_POINT('Ctrl Pts',(2.23250791726574,-223.56152254886,5.97638857119167));
#75206=CARTESIAN_POINT('Ctrl Pts',(1.58418937066262,-223.038036970857,6.02930785960227));
#75207=CARTESIAN_POINT('Ctrl Pts',(0.935870824059497,-222.514551392854,
6.08222714801287));
#75208=CARTESIAN_POINT('Ctrl Pts',(0.00241814464464793,-222.344194447881,
6.13514643642346));
#75209=CARTESIAN_POINT('Ctrl Pts',(-0.789020739835259,-222.604921470608,
6.18806572483406));
#75210=CARTESIAN_POINT('Ctrl Pts',(-1.58045962431517,-222.865648493336,
6.24098501324466));
#75211=CARTESIAN_POINT('Ctrl Pts',(-2.22988471386013,-223.557459483763,
6.29390430165526));
#75212=CARTESIAN_POINT('Ctrl Pts',(-2.44011910026339,-224.363781746274,
6.34682359006585));
#75213=CARTESIAN_POINT('Ctrl Pts',(-2.49387433955717,-224.569951854365,
6.36035462587991));
#75214=CARTESIAN_POINT('Ctrl Pts',(-2.5189160060991,-224.783608522892,6.37388566169396));
#75215=CARTESIAN_POINT('Ctrl Pts',(-2.51699551773447,-224.997707769369,
6.38741669750802));
#75216=CARTESIAN_POINT('Origin',(0.,-225.,10.));
#75217=CARTESIAN_POINT('',(-2.51364333654142,-225.000739863108,7.38741669750802));
#75218=CARTESIAN_POINT('',(-2.5184403423166,-225.002219538269,7.11258330249199));
#75219=CARTESIAN_POINT('',(-2.5175,-225.,10.));
#75220=CARTESIAN_POINT('Ctrl Pts',(-2.5184403423166,-225.002219538269,7.11258330249199));
#75221=CARTESIAN_POINT('Ctrl Pts',(-2.51228356404023,-224.332120591697,
7.07017089172762));
#75222=CARTESIAN_POINT('Ctrl Pts',(-2.23669070067441,-223.657549431312,
7.02775848096325));
#75223=CARTESIAN_POINT('Ctrl Pts',(-1.75786849029817,-223.192003033031,
6.98534607019888));
#75224=CARTESIAN_POINT('Ctrl Pts',(-1.16042707653199,-222.611126264295,
6.93242678178828));
#75225=CARTESIAN_POINT('Ctrl Pts',(-0.246591476022486,-222.355666176701,
6.87950749337768));
#75226=CARTESIAN_POINT('Ctrl Pts',(0.565467158405056,-222.54252130131,6.82658820496709));
#75227=CARTESIAN_POINT('Ctrl Pts',(1.3775257928326,-222.729376425919,6.77366891655649));
#75228=CARTESIAN_POINT('Ctrl Pts',(2.08780746117818,-223.358546762731,6.72074962814589));
#75229=CARTESIAN_POINT('Ctrl Pts',(2.37128728597244,-224.142123977991,6.6678303397353));
#75230=CARTESIAN_POINT('Ctrl Pts',(2.65476711076672,-224.925701193252,6.6149110513247));
#75231=CARTESIAN_POINT('Ctrl Pts',(2.51144509200964,-225.863685286961,6.5619917629141));
#75232=CARTESIAN_POINT('Ctrl Pts',(2.00690538266646,-226.526854756281,6.5090724745035));
#75233=CARTESIAN_POINT('Ctrl Pts',(1.5023656733233,-227.1900242256,6.4561531860929));
#75234=CARTESIAN_POINT('Ctrl Pts',(0.636608273394049,-227.578379070528,
6.4032338976823));
#75235=CARTESIAN_POINT('Ctrl Pts',(-0.194196247936209,-227.514208121664,
6.35031460927171));
#75236=CARTESIAN_POINT('Ctrl Pts',(-1.02500076926649,-227.450037172799,
6.29739532086111));
#75237=CARTESIAN_POINT('Ctrl Pts',(-1.82085241199778,-226.93334043014,6.24447603245051));
#75238=CARTESIAN_POINT('Ctrl Pts',(-2.21756948006428,-226.200558312969,
6.19155674403991));
#75239=CARTESIAN_POINT('Ctrl Pts',(-2.41491474003151,-225.836038888289,
6.16523226352394));
#75240=CARTESIAN_POINT('Ctrl Pts',(-2.51349320124512,-225.418048624316,
6.13890778300797));
#75241=CARTESIAN_POINT('Ctrl Pts',(-2.51344103673693,-225.000035219284,
6.11258330249199));
#75242=CARTESIAN_POINT('Ctrl Pts',(-2.51699551773447,-224.997707769369,
6.38741669750802));
#75243=CARTESIAN_POINT('Ctrl Pts',(-2.51140506022227,-225.620941298335,
6.42680495010456));
#75244=CARTESIAN_POINT('Ctrl Pts',(-2.27734630742311,-226.247925085029,
6.4661932027011));
#75245=CARTESIAN_POINT('Ctrl Pts',(-1.85802055608581,-226.704908942732,
6.50558145529765));
#75246=CARTESIAN_POINT('Ctrl Pts',(-1.29464394224344,-227.318880342084,
6.55850074370824));
#75247=CARTESIAN_POINT('Ctrl Pts',(-0.396847031297126,-227.625989606195,
6.61142003211884));
#75248=CARTESIAN_POINT('Ctrl Pts',(0.424538327956587,-227.485703541845,
6.66433932052944));
#75249=CARTESIAN_POINT('Ctrl Pts',(1.24592368721032,-227.345417477495,6.71725860894004));
#75250=CARTESIAN_POINT('Ctrl Pts',(1.99089749477147,-226.757736084685,6.77017789735063));
#75251=CARTESIAN_POINT('Ctrl Pts',(2.31855975094772,-225.991582357209,6.82309718576123));
#75252=CARTESIAN_POINT('Ctrl Pts',(2.64622200712396,-225.225428629734,6.87601647417183));
#75253=CARTESIAN_POINT('Ctrl Pts',(2.55657271191534,-224.280802567593,6.92893576258243));
#75254=CARTESIAN_POINT('Ctrl Pts',(2.09063538104663,-223.589965038249,6.98185505099302));
#75255=CARTESIAN_POINT('Ctrl Pts',(1.6246980501779,-222.899127508905,7.03477433940362));
#75256=CARTESIAN_POINT('Ctrl Pts',(0.782472683649099,-222.462078512358,
7.08769362781421));
#75257=CARTESIAN_POINT('Ctrl Pts',(-0.0506384073760926,-222.478811660835,
7.14061291622481));
#75258=CARTESIAN_POINT('Ctrl Pts',(-0.883749498401272,-222.495544809311,
7.19353220463541));
#75259=CARTESIAN_POINT('Ctrl Pts',(-1.70774631392282,-222.966060102812,
7.24645149304601));
#75260=CARTESIAN_POINT('Ctrl Pts',(-2.14556792735952,-223.675049752281,
7.29937078145661));
#75261=CARTESIAN_POINT('Ctrl Pts',(-2.388380495832,-224.068250070687,7.32871942014041));
#75262=CARTESIAN_POINT('Ctrl Pts',(-2.51241607461331,-224.534798615409,
7.35806805882421));
#75263=CARTESIAN_POINT('Ctrl Pts',(-2.51364333654142,-225.000739863108,
7.38741669750802));
#75264=CARTESIAN_POINT('Origin',(0.,-225.,10.));
#75265=CARTESIAN_POINT('',(-2.51970628537248,-225.001899922081,8.38741669750802));
#75266=CARTESIAN_POINT('',(-2.52066983009894,-224.998569141019,8.112583302492));
#75267=CARTESIAN_POINT('',(-2.5175,-225.,10.));
#75268=CARTESIAN_POINT('Ctrl Pts',(-2.52066983009894,-224.998569141019,
8.112583302492));
#75269=CARTESIAN_POINT('Ctrl Pts',(-2.52123860736442,-224.91485470247,8.10727257726847));
#75270=CARTESIAN_POINT('Ctrl Pts',(-2.5174295806041,-224.8311926478,8.10196185204495));
#75271=CARTESIAN_POINT('Ctrl Pts',(-2.50907240175204,-224.747987411985,
8.09665112682143));
#75272=CARTESIAN_POINT('Ctrl Pts',(-2.42579640095047,-223.918879957531,
8.04373183841083));
#75273=CARTESIAN_POINT('Ctrl Pts',(-1.89091897125145,-223.135131594655,
7.99081255000023));
#75274=CARTESIAN_POINT('Ctrl Pts',(-1.14920001396848,-222.755385558799,
7.93789326158963));
#75275=CARTESIAN_POINT('Ctrl Pts',(-0.407481056685504,-222.375639522944,
7.88497397317903));
#75276=CARTESIAN_POINT('Ctrl Pts',(0.541079428181421,-222.399895814108,
7.83205468476844));
#75277=CARTESIAN_POINT('Ctrl Pts',(1.26242018140782,-222.817054753933,7.77913539635784));
#75278=CARTESIAN_POINT('Ctrl Pts',(1.98376093463424,-223.234213693758,7.72621610794725));
#75279=CARTESIAN_POINT('Ctrl Pts',(2.47788195622012,-224.044275282243,7.67329681953665));
#75280=CARTESIAN_POINT('Ctrl Pts',(2.51867347640318,-224.876555352425,7.62037753112605));
#75281=CARTESIAN_POINT('Ctrl Pts',(2.55946499658623,-225.708835422607,7.56745824271545));
#75282=CARTESIAN_POINT('Ctrl Pts',(2.14692701536649,-226.563333974486,7.51453895430485));
#75283=CARTESIAN_POINT('Ctrl Pts',(1.46983690483877,-227.049032487523,7.46161966589425));
#75284=CARTESIAN_POINT('Ctrl Pts',(0.792746794311025,-227.534731000561,
7.40870037748366));
#75285=CARTESIAN_POINT('Ctrl Pts',(-0.148895445524709,-227.651629474756,
7.35578108907306));
#75286=CARTESIAN_POINT('Ctrl Pts',(-0.924194344234185,-227.346235170617,
7.30286180066246));
#75287=CARTESIAN_POINT('Ctrl Pts',(-1.69949324294364,-227.040840866477,
7.24994251225187));
#75288=CARTESIAN_POINT('Ctrl Pts',(-2.30844880052685,-226.313153784002,
7.19702322384126));
#75289=CARTESIAN_POINT('Ctrl Pts',(-2.47240296580703,-225.496163517825,
7.14410393543067));
#75290=CARTESIAN_POINT('Ctrl Pts',(-2.50495529986001,-225.333953914811,
7.13359705778444));
#75291=CARTESIAN_POINT('Ctrl Pts',(-2.51996556842092,-225.168223958098,
7.12309018013822));
#75292=CARTESIAN_POINT('Ctrl Pts',(-2.5184403423166,-225.002219538269,7.11258330249199));
#75293=CARTESIAN_POINT('Ctrl Pts',(-2.51364333654142,-225.000739863108,
7.38741669750802));
#75294=CARTESIAN_POINT('Ctrl Pts',(-2.51462898229289,-225.374949313199,
7.41098734723481));
#75295=CARTESIAN_POINT('Ctrl Pts',(-2.43640190115498,-225.748767049972,
7.43455799696161));
#75296=CARTESIAN_POINT('Ctrl Pts',(-2.27687376459592,-226.083882258337,
7.4581286466884));
#75297=CARTESIAN_POINT('Ctrl Pts',(-1.91871157704378,-226.836261109486,
7.511047935099));
#75298=CARTESIAN_POINT('Ctrl Pts',(-1.15074079058765,-227.393554806343,
7.5639672235096));
#75299=CARTESIAN_POINT('Ctrl Pts',(-0.32438482201001,-227.500745764186,
7.61688651192019));
#75300=CARTESIAN_POINT('Ctrl Pts',(0.501971146567617,-227.607936722028,
7.66980580033079));
#75301=CARTESIAN_POINT('Ctrl Pts',(1.38671229726677,-227.265024940856,7.72272508874138));
#75302=CARTESIAN_POINT('Ctrl Pts',(1.92498109692331,-226.628926844991,7.77564437715198));
#75303=CARTESIAN_POINT('Ctrl Pts',(2.46324989657986,-225.992828749126,7.82856366556258));
#75304=CARTESIAN_POINT('Ctrl Pts',(2.6550463451938,-225.063544338567,7.88148295397318));
#75305=CARTESIAN_POINT('Ctrl Pts',(2.4126043916505,-224.266314141316,7.93440224238378));
#75306=CARTESIAN_POINT('Ctrl Pts',(2.1701624381072,-223.469083944065,7.98732153079437));
#75307=CARTESIAN_POINT('Ctrl Pts',(1.49348208240664,-222.803907960121,8.04024081920497));
#75308=CARTESIAN_POINT('Ctrl Pts',(0.692212242012499,-222.575170706658,
8.09316010761557));
#75309=CARTESIAN_POINT('Ctrl Pts',(-0.109057598381629,-222.346433453194,
8.14607939602617));
#75310=CARTESIAN_POINT('Ctrl Pts',(-1.03491692346934,-222.554134930212,
8.19899868443676));
#75311=CARTESIAN_POINT('Ctrl Pts',(-1.66169252429475,-223.103230945912,
8.25191797284736));
#75312=CARTESIAN_POINT('Ctrl Pts',(-2.19664110423604,-223.571880544688,
8.29708421440091));
#75313=CARTESIAN_POINT('Ctrl Pts',(-2.51372206166214,-224.289219090568,
8.34225045595447));
#75314=CARTESIAN_POINT('Ctrl Pts',(-2.51970628537248,-225.001899922081,
8.38741669750802));
#75315=CARTESIAN_POINT('Origin',(0.,-225.,10.));
#75316=CARTESIAN_POINT('',(-2.51957010083597,-224.99805224078,9.38741669750802));
#75317=CARTESIAN_POINT('',(-2.51411989093267,-224.998691379972,9.112583302492));
#75318=CARTESIAN_POINT('',(-2.5175,-225.,10.));
#75319=CARTESIAN_POINT('Ctrl Pts',(-2.51411989093267,-224.998691379972,
9.112583302492));
#75320=CARTESIAN_POINT('Ctrl Pts',(-2.51569987828659,-224.663415377603,
9.09145497439872));
#75321=CARTESIAN_POINT('Ctrl Pts',(-2.45336473315411,-224.328702940348,
9.07032664630545));
#75322=CARTESIAN_POINT('Ctrl Pts',(-2.32434208855732,-224.0220488166,9.04919831821218));
#75323=CARTESIAN_POINT('Ctrl Pts',(-2.00118416944635,-223.25398435143,8.99627902980158));
#75324=CARTESIAN_POINT('Ctrl Pts',(-1.2596739510131,-222.661938781334,8.94335974139098));
#75325=CARTESIAN_POINT('Ctrl Pts',(-0.439126494633056,-222.516832147546,
8.89044045298038));
#75326=CARTESIAN_POINT('Ctrl Pts',(0.381420961746965,-222.371725513758,
8.83752116456979));
#75327=CARTESIAN_POINT('Ctrl Pts',(1.28100565607379,-222.673557816278,8.78460187615919));
#75328=CARTESIAN_POINT('Ctrl Pts',(1.84797764991111,-223.284210599409,8.73168258774859));
#75329=CARTESIAN_POINT('Ctrl Pts',(2.41494964374844,-223.89486338254,8.678763299338));
#75330=CARTESIAN_POINT('Ctrl Pts',(2.64930893709627,-224.81433664628,8.6258440109274));
#75331=CARTESIAN_POINT('Ctrl Pts',(2.44381272192663,-225.621879443221,8.5729247225168));
#75332=CARTESIAN_POINT('Ctrl Pts',(2.23831650675697,-226.429422240163,8.52000543410621));
#75333=CARTESIAN_POINT('Ctrl Pts',(1.59296478306982,-227.125034570305,8.46708614569561));
#75334=CARTESIAN_POINT('Ctrl Pts',(0.803070486935476,-227.390404245053,
8.41416685728501));
#75335=CARTESIAN_POINT('Ctrl Pts',(0.0131761908011642,-227.6557739198,8.36124756887441));
#75336=CARTESIAN_POINT('Ctrl Pts',(-0.921260677780323,-227.490900939152,
8.30832828046381));
#75337=CARTESIAN_POINT('Ctrl Pts',(-1.57264182611901,-226.971231175812,
8.25540899205322));
#75338=CARTESIAN_POINT('Ctrl Pts',(-2.15865349579485,-226.503712970117,
8.20780042886614));
#75339=CARTESIAN_POINT('Ctrl Pts',(-2.51557096558552,-225.749036161928,
8.16019186567907));
#75340=CARTESIAN_POINT('Ctrl Pts',(-2.52066983009894,-224.998569141019,
8.112583302492));
#75341=CARTESIAN_POINT('Ctrl Pts',(-2.51970628537248,-225.001899922081,
8.38741669750802));
#75342=CARTESIAN_POINT('Ctrl Pts',(-2.52073351201861,-225.124235712946,
8.39516974436506));
#75343=CARTESIAN_POINT('Ctrl Pts',(-2.51259405249524,-225.246434260949,
8.40292279122211));
#75344=CARTESIAN_POINT('Ctrl Pts',(-2.4948163577119,-225.367214148879,8.41067583807916));
#75345=CARTESIAN_POINT('Ctrl Pts',(-2.37347271374052,-226.191610781766,
8.46359512648976));
#75346=CARTESIAN_POINT('Ctrl Pts',(-1.80309354923468,-226.949913493158,
8.51651441490035));
#75347=CARTESIAN_POINT('Ctrl Pts',(-1.04468435865743,-227.295122977232,
8.56943370331095));
#75348=CARTESIAN_POINT('Ctrl Pts',(-0.286275168080149,-227.640332461307,
8.62235299172155));
#75349=CARTESIAN_POINT('Ctrl Pts',(0.660164048568542,-227.572448718064,
8.67527228013214));
#75350=CARTESIAN_POINT('Ctrl Pts',(1.36154272435913,-227.122535347076,8.72819156854274));
#75351=CARTESIAN_POINT('Ctrl Pts',(2.0629214001497,-226.672621976089,8.78111085695333));
#75352=CARTESIAN_POINT('Ctrl Pts',(2.51923953508218,-225.840678977357,8.83403014536393));
#75353=CARTESIAN_POINT('Ctrl Pts',(2.52168595958357,-225.007403450743,8.88694943377453));
#75354=CARTESIAN_POINT('Ctrl Pts',(2.52413238408496,-224.174127924128,8.93986872218513));
#75355=CARTESIAN_POINT('Ctrl Pts',(2.07270709815529,-223.339519869632,8.99278801059572));
#75356=CARTESIAN_POINT('Ctrl Pts',(1.37398230376001,-222.88549591658,9.04570729900632));
#75357=CARTESIAN_POINT('Ctrl Pts',(0.675257509364757,-222.431471963529,
9.09862658741692));
#75358=CARTESIAN_POINT('Ctrl Pts',(-0.270766793496115,-222.358032111923,
9.15154587582752));
#75359=CARTESIAN_POINT('Ctrl Pts',(-1.03118990243417,-222.698782436413,
9.20446516423812));
#75360=CARTESIAN_POINT('Ctrl Pts',(-1.79161301137223,-223.039532760903,
9.25738445264872));
#75361=CARTESIAN_POINT('Ctrl Pts',(-2.3664349263875,-223.794473261489,9.31030374105932));
#75362=CARTESIAN_POINT('Ctrl Pts',(-2.49261715047116,-224.618143179947,
9.36322302946991));
#75363=CARTESIAN_POINT('Ctrl Pts',(-2.51184650227261,-224.743665128426,
9.37128758548262));
#75364=CARTESIAN_POINT('Ctrl Pts',(-2.52065674398981,-224.870783233876,
9.37935214149532));
#75365=CARTESIAN_POINT('Ctrl Pts',(-2.51957010083597,-224.99805224078,9.38741669750802));
#75366=CARTESIAN_POINT('Origin',(0.,-225.,10.));
#75367=CARTESIAN_POINT('',(-2.51360219855143,-224.999337564491,10.387416697508));
#75368=CARTESIAN_POINT('',(-2.51589762297194,-225.002142026704,10.112583302492));
#75369=CARTESIAN_POINT('',(-2.5175,-225.,10.));
#75370=CARTESIAN_POINT('Ctrl Pts',(-2.51589762297194,-225.002142026704,
10.112583302492));
#75371=CARTESIAN_POINT('Ctrl Pts',(-2.51116128740118,-224.416905283918,
10.075637371529));
#75372=CARTESIAN_POINT('Ctrl Pts',(-2.30769417064104,-223.828699095673,
10.038691440566));
#75373=CARTESIAN_POINT('Ctrl Pts',(-1.93451257018931,-223.382404321986,
10.0017455096029));
#75374=CARTESIAN_POINT('Ctrl Pts',(-1.39998808456736,-222.74315660974,9.94882622119234));
#75375=CARTESIAN_POINT('Ctrl Pts',(-0.517275702770113,-222.395055744854,
9.89590693278174));
#75376=CARTESIAN_POINT('Ctrl Pts',(0.309695406647945,-222.497392676257,
9.84298764437114));
#75377=CARTESIAN_POINT('Ctrl Pts',(1.136666516066,-222.599729607659,9.79006835596054));
#75378=CARTESIAN_POINT('Ctrl Pts',(1.90789635310486,-223.15250433535,9.73714906754995));
#75379=CARTESIAN_POINT('Ctrl Pts',(2.27047015949948,-223.902767154805,9.68422977913935));
#75380=CARTESIAN_POINT('Ctrl Pts',(2.63304396589411,-224.653029974261,9.63131049072875));
#75381=CARTESIAN_POINT('Ctrl Pts',(2.58696174164449,-225.600780885482,9.57839120231815));
#75382=CARTESIAN_POINT('Ctrl Pts',(2.15331071166118,-226.312329090128,9.52547191390755));
#75383=CARTESIAN_POINT('Ctrl Pts',(1.71965968167787,-227.023877294775,9.47255262549696));
#75384=CARTESIAN_POINT('Ctrl Pts',(0.898439845960882,-227.499222792846,
9.41963333708636));
#75385=CARTESIAN_POINT('Ctrl Pts',(0.0654413851874604,-227.520847493772,
9.36671404867577));
#75386=CARTESIAN_POINT('Ctrl Pts',(-0.767557075585986,-227.542472194698,
9.31379476026517));
#75387=CARTESIAN_POINT('Ctrl Pts',(-1.61233416141586,-227.110376098477,
9.26087547185457));
#75388=CARTESIAN_POINT('Ctrl Pts',(-2.08231989443644,-226.422286370245,
9.20795618344397));
#75389=CARTESIAN_POINT('Ctrl Pts',(-2.36466113969728,-226.008920395343,
9.17616522312665));
#75390=CARTESIAN_POINT('Ctrl Pts',(-2.51174254640032,-225.503167931057,
9.14437426280932));
#75391=CARTESIAN_POINT('Ctrl Pts',(-2.51411989093267,-224.998691379972,
9.112583302492));
#75392=CARTESIAN_POINT('Ctrl Pts',(-2.51957010083597,-224.99805224078,9.38741669750802));
#75393=CARTESIAN_POINT('Ctrl Pts',(-2.51352623582953,-225.705917278637,
9.43227142990591));
#75394=CARTESIAN_POINT('Ctrl Pts',(-2.2013183640046,-226.418450512008,9.4771261623038));
#75395=CARTESIAN_POINT('Ctrl Pts',(-1.67280128041678,-226.886979270178,
9.5219808947017));
#75396=CARTESIAN_POINT('Ctrl Pts',(-1.04926065312667,-227.439746105621,
9.57490018311229));
#75397=CARTESIAN_POINT('Ctrl Pts',(-0.124636865394406,-227.652880440177,
9.62781947152289));
#75398=CARTESIAN_POINT('Ctrl Pts',(0.677962255693717,-227.428852006545,
9.68073875993349));
#75399=CARTESIAN_POINT('Ctrl Pts',(1.48056137678185,-227.204823572913,9.73365804834409));
#75400=CARTESIAN_POINT('Ctrl Pts',(2.16113583122583,-226.543632371092,9.78657733675469));
#75401=CARTESIAN_POINT('Ctrl Pts',(2.40825476205355,-225.747839482035,9.83949662516528));
#75402=CARTESIAN_POINT('Ctrl Pts',(2.65537369288127,-224.952046592978,9.89241591357588));
#75403=CARTESIAN_POINT('Ctrl Pts',(2.46903710009274,-224.021652016685,9.94533520198648));
#75404=CARTESIAN_POINT('Ctrl Pts',(1.93451260488425,-223.382404292974,9.99825449039708));
#75405=CARTESIAN_POINT('Ctrl Pts',(1.39998810967575,-222.743156569264,10.0511737788077));
#75406=CARTESIAN_POINT('Ctrl Pts',(0.517275712047266,-222.395055698135,
10.1040930672183));
#75407=CARTESIAN_POINT('Ctrl Pts',(-0.309695412202296,-222.497392631373,
10.1570123556289));
#75408=CARTESIAN_POINT('Ctrl Pts',(-1.13666653645184,-222.599729564611,
10.2099316440395));
#75409=CARTESIAN_POINT('Ctrl Pts',(-1.90789638732247,-223.152504302215,
10.2628509324501));
#75410=CARTESIAN_POINT('Ctrl Pts',(-2.27047020021974,-223.902767135127,
10.3157702208607));
#75411=CARTESIAN_POINT('Ctrl Pts',(-2.43409759707822,-224.241356271855,
10.3396523797431));
#75412=CARTESIAN_POINT('Ctrl Pts',(-2.51449553043366,-224.620167078381,
10.3635345386256));
#75413=CARTESIAN_POINT('Ctrl Pts',(-2.51360219855143,-224.999337564491,
10.387416697508));
#75414=CARTESIAN_POINT('Origin',(0.,-225.,10.));
#75415=CARTESIAN_POINT('',(-2.51714215352465,-225.002298253916,11.387416697508));
#75416=CARTESIAN_POINT('',(-2.52169612886588,-225.000045821236,11.112583302492));
#75417=CARTESIAN_POINT('',(-2.5175,-225.,10.));
#75418=CARTESIAN_POINT('Ctrl Pts',(-2.5216957256514,-225.000045816832,11.112583302492));
#75419=CARTESIAN_POINT('Ctrl Pts',(-2.52147288364372,-224.169218319319,
11.0598197686592));
#75420=CARTESIAN_POINT('Ctrl Pts',(-2.07065054082289,-223.338183594447,
11.0070562348265));
#75421=CARTESIAN_POINT('Ctrl Pts',(-1.37398227911805,-222.885495954503,
10.9542927009937));
#75422=CARTESIAN_POINT('Ctrl Pts',(-0.675257497254214,-222.431472009595,
10.9013734125831));
#75423=CARTESIAN_POINT('Ctrl Pts',(0.270766788639961,-222.358032159306,
10.8484541241725));
#75424=CARTESIAN_POINT('Ctrl Pts',(1.03118988394006,-222.698782477684,10.7955348357619));
#75425=CARTESIAN_POINT('Ctrl Pts',(1.79161297924015,-223.039532796063,10.7426155473513));
#75426=CARTESIAN_POINT('Ctrl Pts',(2.36643488394616,-223.79447328311,10.6896962589407));
#75427=CARTESIAN_POINT('Ctrl Pts',(2.49261710576678,-224.618143186796,10.6367769705301));
#75428=CARTESIAN_POINT('Ctrl Pts',(2.6187993275874,-225.441813090481,10.5838576821195));
#75429=CARTESIAN_POINT('Ctrl Pts',(2.29634186652262,-226.334212410806,10.5309383937089));
#75430=CARTESIAN_POINT('Ctrl Pts',(1.67280125041553,-226.886979236335,10.4780191052983));
#75431=CARTESIAN_POINT('Ctrl Pts',(1.04926063430843,-227.439746061865,10.4250998168877));
#75432=CARTESIAN_POINT('Ctrl Pts',(0.124636863159021,-227.652880392599,
10.3721805284771));
#75433=CARTESIAN_POINT('Ctrl Pts',(-0.677962243534711,-227.428851962984,
10.3192612400665));
#75434=CARTESIAN_POINT('Ctrl Pts',(-1.48056135022843,-227.20482353337,10.2663419516559));
#75435=CARTESIAN_POINT('Ctrl Pts',(-2.16113579246647,-226.543632343407,
10.2134226632453));
#75436=CARTESIAN_POINT('Ctrl Pts',(-2.40825471886219,-225.747839468623,
10.1605033748347));
#75437=CARTESIAN_POINT('Ctrl Pts',(-2.48284602690762,-225.507634348241,
10.1445300173872));
#75438=CARTESIAN_POINT('Ctrl Pts',(-2.51794534999063,-225.25516571403,10.1285566599396));
#75439=CARTESIAN_POINT('Ctrl Pts',(-2.51589762297194,-225.002142026704,
10.112583302492));
#75440=CARTESIAN_POINT('Ctrl Pts',(-2.51360219855143,-224.999337564491,
10.387416697508));
#75441=CARTESIAN_POINT('Ctrl Pts',(-2.51251604073364,-225.460352105623,
10.4164538270362));
#75442=CARTESIAN_POINT('Ctrl Pts',(-2.39125766399852,-225.92189835817,10.4454909565643));
#75443=CARTESIAN_POINT('Ctrl Pts',(-2.15331075028016,-226.312329113665,
10.4745280860925));
#75444=CARTESIAN_POINT('Ctrl Pts',(-1.71965971251943,-227.023877331072,
10.5274473745031));
#75445=CARTESIAN_POINT('Ctrl Pts',(-0.898439862074109,-227.499222837669,
10.5803666629136));
#75446=CARTESIAN_POINT('Ctrl Pts',(-0.0654413863611154,-227.520847538983,
10.6332859513242));
#75447=CARTESIAN_POINT('Ctrl Pts',(0.767557089351907,-227.542472240296,
10.6862052397348));
#75448=CARTESIAN_POINT('Ctrl Pts',(1.6123341903326,-227.110376136326,10.7391245281454));
#75449=CARTESIAN_POINT('Ctrl Pts',(2.08231993178224,-226.422286395754,10.792043816556));
#75450=CARTESIAN_POINT('Ctrl Pts',(2.55230567323187,-225.734196655181,10.8449631049666));
#75451=CARTESIAN_POINT('Ctrl Pts',(2.64750005515044,-224.790113278006,10.8978823933772));
#75452=CARTESIAN_POINT('Ctrl Pts',(2.32434213024372,-224.022048799061,10.9508016817878));
#75453=CARTESIAN_POINT('Ctrl Pts',(2.001184205337,-223.253984320116,11.0037209701984));
#75454=CARTESIAN_POINT('Ctrl Pts',(1.259673973605,-222.661938739401,11.056640258609));
#75455=CARTESIAN_POINT('Ctrl Pts',(0.439126502508681,-222.516832103011,
11.1095595470196));
#75456=CARTESIAN_POINT('Ctrl Pts',(-0.381420968587641,-222.37172546662,
11.1624788354302));
#75457=CARTESIAN_POINT('Ctrl Pts',(-1.28100567904826,-222.673557774554,
11.2153981238408));
#75458=CARTESIAN_POINT('Ctrl Pts',(-1.84797768305408,-223.284210568637,
11.2683174122514));
#75459=CARTESIAN_POINT('Ctrl Pts',(-2.27331699042637,-223.742318966661,
11.3080171740036));
#75460=CARTESIAN_POINT('Ctrl Pts',(-2.51146457315667,-224.374229021343,
11.3477169357558));
#75461=CARTESIAN_POINT('Ctrl Pts',(-2.51714215352465,-225.002298253916,
11.387416697508));
#75462=CARTESIAN_POINT('Origin',(0.,-225.,10.));
#75463=CARTESIAN_POINT('',(-2.52142583271238,-224.999252289457,12.387416697508));
#75464=CARTESIAN_POINT('',(-2.51603114701545,-224.9978289772,12.112583302492));
#75465=CARTESIAN_POINT('',(-2.5175,-225.,10.));
#75466=CARTESIAN_POINT('Ctrl Pts',(-2.51603114701545,-224.9978289772,12.112583302492));
#75467=CARTESIAN_POINT('Ctrl Pts',(-2.51807401653,-224.749773018184,12.0969214542001));
#75468=CARTESIAN_POINT('Ctrl Pts',(-2.48435680654783,-224.502260225447,
12.0812596059082));
#75469=CARTESIAN_POINT('Ctrl Pts',(-2.41260434838113,-224.266314154475,
12.0655977576162));
#75470=CARTESIAN_POINT('Ctrl Pts',(-2.17016239918595,-223.469083971522,
12.0126784692056));
#75471=CARTESIAN_POINT('Ctrl Pts',(-1.49348205562143,-222.803907999507,
11.959759180795));
#75472=CARTESIAN_POINT('Ctrl Pts',(-0.69221222959782,-222.575170750146,
11.9068398923844));
#75473=CARTESIAN_POINT('Ctrl Pts',(0.109057596425746,-222.346433500785,
11.8539206039738));
#75474=CARTESIAN_POINT('Ctrl Pts',(1.0349169049084,-222.554134974078,11.8010013155632));
#75475=CARTESIAN_POINT('Ctrl Pts',(1.66169249449276,-223.10323097993,11.7480820271526));
#75476=CARTESIAN_POINT('Ctrl Pts',(2.28846808407714,-223.652326985781,11.6951627387421));
#75477=CARTESIAN_POINT('Ctrl Pts',(2.61615995476321,-224.542817524192,11.6422434503315));
#75478=CARTESIAN_POINT('Ctrl Pts',(2.49481631296809,-225.367214142293,11.5893241619209));
#75479=CARTESIAN_POINT('Ctrl Pts',(2.37347267117298,-226.191610760395,11.5364048735103));
#75480=CARTESIAN_POINT('Ctrl Pts',(1.80309351689672,-226.949913458187,11.4834855850997));
#75481=CARTESIAN_POINT('Ctrl Pts',(1.0446843399213,-227.29512293607,11.4305662966891));
#75482=CARTESIAN_POINT('Ctrl Pts',(0.286275162945881,-227.640332413953,
11.3776470082785));
#75483=CARTESIAN_POINT('Ctrl Pts',(-0.660164036728685,-227.572448671928,
11.3247277198679));
#75484=CARTESIAN_POINT('Ctrl Pts',(-1.36154269994023,-227.122535309009,
11.2718084314573));
#75485=CARTESIAN_POINT('Ctrl Pts',(-2.0629213631518,-226.672621946091,11.2188891430467));
#75486=CARTESIAN_POINT('Ctrl Pts',(-2.51923948990035,-225.84067896228,11.1659698546361));
#75487=CARTESIAN_POINT('Ctrl Pts',(-2.52168591435786,-225.00740345061,11.1130505662255));
#75488=CARTESIAN_POINT('Ctrl Pts',(-2.5216931147912,-225.004950914315,11.1128948116477));
#75489=CARTESIAN_POINT('Ctrl Pts',(-2.52169638346675,-225.002498366477,
11.1127390570698));
#75490=CARTESIAN_POINT('Ctrl Pts',(-2.5216957256514,-225.000045816832,11.112583302492));
#75491=CARTESIAN_POINT('Ctrl Pts',(-2.51714215352465,-225.002298253916,
11.387416697508));
#75492=CARTESIAN_POINT('Ctrl Pts',(-2.51903271713805,-225.211437492965,
11.4006362241664));
#75493=CARTESIAN_POINT('Ctrl Pts',(-2.49514684119296,-225.420150858922,
11.4138557508248));
#75494=CARTESIAN_POINT('Ctrl Pts',(-2.44381276575569,-225.621879454375,
11.4270752774832));
#75495=CARTESIAN_POINT('Ctrl Pts',(-2.23831654690051,-226.429422265799,
11.4799945658938));
#75496=CARTESIAN_POINT('Ctrl Pts',(-1.59296481163917,-227.125034608417,
11.5329138543044));
#75497=CARTESIAN_POINT('Ctrl Pts',(-0.803070501338331,-227.390404287924,
11.585833142715));
#75498=CARTESIAN_POINT('Ctrl Pts',(-0.013176191037481,-227.65577396743,
11.6387524311256));
#75499=CARTESIAN_POINT('Ctrl Pts',(0.921260694302875,-227.490900983826,
11.6916717195362));
#75500=CARTESIAN_POINT('Ctrl Pts',(1.5726418543239,-226.971231211165,11.7445910079468));
#75501=CARTESIAN_POINT('Ctrl Pts',(2.22402301434493,-226.451561438505,11.7975102963574));
#75502=CARTESIAN_POINT('Ctrl Pts',(2.59234844904663,-225.577094876789,11.850429584768));
#75503=CARTESIAN_POINT('Ctrl Pts',(2.50907244675153,-224.747987407465,11.9033488731786));
#75504=CARTESIAN_POINT('Ctrl Pts',(2.42579644445644,-223.918879938141,11.9562681615892));
#75505=CARTESIAN_POINT('Ctrl Pts',(1.89091900516453,-223.135131561209,12.0091874499998));
#75506=CARTESIAN_POINT('Ctrl Pts',(1.14920003457903,-222.755385518543,12.0621067384104));
#75507=CARTESIAN_POINT('Ctrl Pts',(0.407481063993527,-222.375639475876,
12.115026026821));
#75508=CARTESIAN_POINT('Ctrl Pts',(-0.541079437885564,-222.399895767476,
12.1679453152316));
#75509=CARTESIAN_POINT('Ctrl Pts',(-1.26242020404901,-222.817054714783,
12.2208646036422));
#75510=CARTESIAN_POINT('Ctrl Pts',(-1.98376097021244,-223.234213662089,
12.2737838920528));
#75511=CARTESIAN_POINT('Ctrl Pts',(-2.47788200066022,-224.044275265102,
12.3267031804634));
#75512=CARTESIAN_POINT('Ctrl Pts',(-2.51867352157486,-224.876555350211,
12.379622468874));
#75513=CARTESIAN_POINT('Ctrl Pts',(-2.52067618418232,-224.917416199917,
12.3822205450853));
#75514=CARTESIAN_POINT('Ctrl Pts',(-2.52158617489675,-224.958330603408,
12.3848186212967));
#75515=CARTESIAN_POINT('Ctrl Pts',(-2.52142583271238,-224.999252289457,
12.387416697508));
#75516=CARTESIAN_POINT('Origin',(0.,-225.,10.));
#75517=CARTESIAN_POINT('',(-2.51494210236921,-224.998176172471,13.387416697508));
#75518=CARTESIAN_POINT('',(-2.51404438929022,-225.001240667286,13.112583302492));
#75519=CARTESIAN_POINT('',(-2.5175,-225.,10.));
#75520=CARTESIAN_POINT('Ctrl Pts',(-2.51404438929022,-225.001240667286,
13.112583302492));
#75521=CARTESIAN_POINT('Ctrl Pts',(-2.51181653950388,-224.501669767605,
13.0811038513303));
#75522=CARTESIAN_POINT('Ctrl Pts',(-2.36780179134328,-224.000915144855,
13.0496244001687));
#75523=CARTESIAN_POINT('Ctrl Pts',(-2.09063534355168,-223.589965063538,
13.018144949007));
#75524=CARTESIAN_POINT('Ctrl Pts',(-1.62469802103941,-222.899127546584,
12.9652256605964));
#75525=CARTESIAN_POINT('Ctrl Pts',(-0.782472669615672,-222.462078557875,
12.9123063721858));
#75526=CARTESIAN_POINT('Ctrl Pts',(0.0506384064679075,-222.478811706052,
12.8593870837752));
#75527=CARTESIAN_POINT('Ctrl Pts',(0.883749482551476,-222.495544854228,
12.8064677953646));
#75528=CARTESIAN_POINT('Ctrl Pts',(1.70774628329489,-222.96606013929,12.753548506954));
#75529=CARTESIAN_POINT('Ctrl Pts',(2.14556788887937,-223.675049776044,12.7006292185434));
#75530=CARTESIAN_POINT('Ctrl Pts',(2.58338949446386,-224.384039412798,12.6477099301328));
#75531=CARTESIAN_POINT('Ctrl Pts',(2.63503590488944,-225.331503401244,12.5947906417222));
#75532=CARTESIAN_POINT('Ctrl Pts',(2.27687372376085,-226.083882238898,12.5418713533116));
#75533=CARTESIAN_POINT('Ctrl Pts',(1.91871154263225,-226.836261076553,12.488952064901));
#75534=CARTESIAN_POINT('Ctrl Pts',(1.15074076994946,-227.393554763416,12.4360327764904));
#75535=CARTESIAN_POINT('Ctrl Pts',(0.32438481619228,-227.500745719336,12.3831134880798));
#75536=CARTESIAN_POINT('Ctrl Pts',(-0.501971137564902,-227.607936675256,
12.3301941996692));
#75537=CARTESIAN_POINT('Ctrl Pts',(-1.38671227239649,-227.265024900234,
12.2772749112586));
#75538=CARTESIAN_POINT('Ctrl Pts',(-1.92498106239934,-226.628926815777,
12.224355622848));
#75539=CARTESIAN_POINT('Ctrl Pts',(-2.30394528912289,-226.181086585814,
12.1870981827293));
#75540=CARTESIAN_POINT('Ctrl Pts',(-2.51117143396052,-225.587920891441,
12.1498407426107));
#75541=CARTESIAN_POINT('Ctrl Pts',(-2.51603114701545,-224.9978289772,12.112583302492));
#75542=CARTESIAN_POINT('Ctrl Pts',(-2.52142583271238,-224.999252289457,
12.387416697508));
#75543=CARTESIAN_POINT('Ctrl Pts',(-2.51832022208835,-225.791849842305,
12.4377379097073));
#75544=CARTESIAN_POINT('Ctrl Pts',(-2.11368526635859,-226.587179405838,
12.4880591219065));
#75545=CARTESIAN_POINT('Ctrl Pts',(-1.46983693119985,-227.049032524272,
12.5383803341058));
#75546=CARTESIAN_POINT('Ctrl Pts',(-0.792746808528703,-227.53473104602,
12.5912996225164));
#75547=CARTESIAN_POINT('Ctrl Pts',(0.148895448195099,-227.651629522312,
12.644218910927));
#75548=CARTESIAN_POINT('Ctrl Pts',(0.92419436080933,-227.346235212695,12.6971381993376));
#75549=CARTESIAN_POINT('Ctrl Pts',(1.69949327342356,-227.040840903079,12.7500574877481));
#75550=CARTESIAN_POINT('Ctrl Pts',(2.30844884192822,-226.313153807553,12.8029767761587));
#75551=CARTESIAN_POINT('Ctrl Pts',(2.47240301014887,-225.496163526723,12.8558960645693));
#75552=CARTESIAN_POINT('Ctrl Pts',(2.63635717836953,-224.679173245894,12.9088153529799));
#75553=CARTESIAN_POINT('Ctrl Pts',(2.35530994630617,-223.77287977976,12.9617346413905));
#75554=CARTESIAN_POINT('Ctrl Pts',(1.75786852182505,-223.192003000605,13.0146539298011));
#75555=CARTESIAN_POINT('Ctrl Pts',(1.16042709734392,-222.611126221451,13.0675732182117));
#75556=CARTESIAN_POINT('Ctrl Pts',(0.246591480445025,-222.355666129275,
13.1204925066223));
#75557=CARTESIAN_POINT('Ctrl Pts',(-0.565467168546566,-222.542521257235,
13.1734117950329));
#75558=CARTESIAN_POINT('Ctrl Pts',(-1.37752581753814,-222.729376385196,
13.2263310834435));
#75559=CARTESIAN_POINT('Ctrl Pts',(-2.08780749862242,-223.358546733292,
13.2792503718541));
#75560=CARTESIAN_POINT('Ctrl Pts',(-2.3712873285008,-224.142123962606,13.3321696602647));
#75561=CARTESIAN_POINT('Ctrl Pts',(-2.46993705962531,-224.414805384138,
13.3505853393458));
#75562=CARTESIAN_POINT('Ctrl Pts',(-2.51690068886609,-224.706185622866,
13.3690010184269));
#75563=CARTESIAN_POINT('Ctrl Pts',(-2.51494210236921,-224.998176172471,
13.387416697508));
#75564=CARTESIAN_POINT('Origin',(0.,-225.,10.));
#75565=CARTESIAN_POINT('',(-2.51484781591379,-225.001779432988,14.387416697508));
#75566=CARTESIAN_POINT('',(-2.52055923806654,-225.001499367411,14.112583302492));
#75567=CARTESIAN_POINT('',(-2.5175,-225.,10.));
#75568=CARTESIAN_POINT('Ctrl Pts',(-2.52055923806654,-225.001499367411,
14.112583302492));
#75569=CARTESIAN_POINT('Ctrl Pts',(-2.51530324437999,-224.255856698468,
14.0652862484606));
#75570=CARTESIAN_POINT('Ctrl Pts',(-2.1636294235382,-223.505906585683,14.0179891944292));
#75571=CARTESIAN_POINT('Ctrl Pts',(-1.58418934225064,-223.038037006044,
13.9706921403977));
#75572=CARTESIAN_POINT('Ctrl Pts',(-0.935870807274923,-222.51455143743,
13.9177728519872));
#75573=CARTESIAN_POINT('Ctrl Pts',(-0.00241814460127818,-222.344194495512,
13.8648535635766));
#75574=CARTESIAN_POINT('Ctrl Pts',(0.789020725684399,-222.604921513563,
13.811934275166));
#75575=CARTESIAN_POINT('Ctrl Pts',(1.58045959597008,-222.865648531615,13.7590149867554));
#75576=CARTESIAN_POINT('Ctrl Pts',(2.22988467386778,-223.557459509635,13.7060956983448));
#75577=CARTESIAN_POINT('Ctrl Pts',(2.44011905650055,-224.363781757685,13.6531764099342));
#75578=CARTESIAN_POINT('Ctrl Pts',(2.65035343913332,-225.170104005735,13.6002571215236));
#75579=CARTESIAN_POINT('Ctrl Pts',(2.42139712650114,-226.090937523814,13.547337833113));
#75580=CARTESIAN_POINT('Ctrl Pts',(1.85802052276276,-226.704908912155,13.4944185447024));
#75581=CARTESIAN_POINT('Ctrl Pts',(1.29464391902438,-227.318880300496,13.4414992562918));
#75582=CARTESIAN_POINT('Ctrl Pts',(0.396847024179783,-227.625989559098,
13.3885799678812));
#75583=CARTESIAN_POINT('Ctrl Pts',(-0.424538320342631,-227.485703497264,
13.3356606794706));
#75584=CARTESIAN_POINT('Ctrl Pts',(-1.24592366486505,-227.345417435431,
13.28274139106));
#75585=CARTESIAN_POINT('Ctrl Pts',(-1.99089745906529,-226.757736053161,
13.2298221026494));
#75586=CARTESIAN_POINT('Ctrl Pts',(-2.31855970936501,-225.991582339426,
13.1769028142388));
#75587=CARTESIAN_POINT('Ctrl Pts',(-2.45130951628865,-225.681181133675,
13.1554629769899));
#75588=CARTESIAN_POINT('Ctrl Pts',(-2.51556171996378,-225.341485442472,
13.1340231397409));
#75589=CARTESIAN_POINT('Ctrl Pts',(-2.51404438929022,-225.001240667286,
13.112583302492));
#75590=CARTESIAN_POINT('Ctrl Pts',(-2.51494210236921,-224.998176172471,
13.387416697508));
#75591=CARTESIAN_POINT('Ctrl Pts',(-2.51127249545279,-225.545249555271,
13.4219203068375));
#75592=CARTESIAN_POINT('Ctrl Pts',(-2.33586753922983,-226.094465358442,
13.456423916167));
#75593=CARTESIAN_POINT('Ctrl Pts',(-2.00690541865975,-226.526854783664,
13.4909275254965));
#75594=CARTESIAN_POINT('Ctrl Pts',(-1.5023657002678,-227.190024264877,13.5438468139071));
#75595=CARTESIAN_POINT('Ctrl Pts',(-0.636608284811431,-227.578379116771,
13.5967661023177));
#75596=CARTESIAN_POINT('Ctrl Pts',(0.19419625141908,-227.514208166755,13.6496853907283));
#75597=CARTESIAN_POINT('Ctrl Pts',(1.02500078764959,-227.450037216739,13.7026046791389));
#75598=CARTESIAN_POINT('Ctrl Pts',(1.82085244465424,-226.933340464814,13.7555239675495));
#75599=CARTESIAN_POINT('Ctrl Pts',(2.21756951983575,-226.200558334501,13.8084432559601));
#75600=CARTESIAN_POINT('Ctrl Pts',(2.61428659501725,-225.467776204187,13.8613625443707));
#75601=CARTESIAN_POINT('Ctrl Pts',(2.61186908837563,-224.518908695486,13.9142818327813));
#75602=CARTESIAN_POINT('Ctrl Pts',(2.21142325090253,-223.788157561722,13.9672011211919));
#75603=CARTESIAN_POINT('Ctrl Pts',(1.81097741342944,-223.057406427958,14.0201204096025));
#75604=CARTESIAN_POINT('Ctrl Pts',(1.01250324512489,-222.544771669131,14.0730396980131));
#75605=CARTESIAN_POINT('Ctrl Pts',(0.181382509705423,-222.484834940801,
14.1259589864237));
#75606=CARTESIAN_POINT('Ctrl Pts',(-0.649738225714033,-222.424898212471,
14.1788782748343));
#75607=CARTESIAN_POINT('Ctrl Pts',(-1.5135055282484,-222.817659514637,14.2317975632449));
#75608=CARTESIAN_POINT('Ctrl Pts',(-2.01465949724137,-223.483391283152,
14.2847168516555));
#75609=CARTESIAN_POINT('Ctrl Pts',(-2.33885405156362,-223.914050576194,
14.3189501336063));
#75610=CARTESIAN_POINT('Ctrl Pts',(-2.51130414328076,-224.458941070606,
14.3531834155572));
#75611=CARTESIAN_POINT('Ctrl Pts',(-2.51484781591379,-225.001779432988,
14.387416697508));
#75612=CARTESIAN_POINT('Origin',(0.,-225.,10.));
#75613=CARTESIAN_POINT('',(-2.52136959094702,-225.00082166017,15.387416697508));
#75614=CARTESIAN_POINT('',(-2.51858868022655,-224.99780466334,15.112583302492));
#75615=CARTESIAN_POINT('',(-2.5175,-225.,10.));
#75616=CARTESIAN_POINT('Ctrl Pts',(-2.51858868022655,-224.99780466334,15.112583302492));
#75617=CARTESIAN_POINT('Ctrl Pts',(-2.52006212821327,-224.836746398224,
15.1023879340014));
#75618=CARTESIAN_POINT('Ctrl Pts',(-2.50593615906982,-224.675945583807,
15.0921925655109));
#75619=CARTESIAN_POINT('Ctrl Pts',(-2.4752737047889,-224.51836243073,15.0819971970203));
#75620=CARTESIAN_POINT('Ctrl Pts',(-2.3161195493536,-223.700423546615,15.0290779086097));
#75621=CARTESIAN_POINT('Ctrl Pts',(-1.71144730475761,-222.969173358425,
14.9761586201991));
#75622=CARTESIAN_POINT('Ctrl Pts',(-0.937954978238689,-222.6592319379,14.9232393317885));
#75623=CARTESIAN_POINT('Ctrl Pts',(-0.164462651719764,-222.349290517374,
14.8703200433779));
#75624=CARTESIAN_POINT('Ctrl Pts',(0.777849756722116,-222.460657864513,
14.8174007549673));
#75625=CARTESIAN_POINT('Ctrl Pts',(1.45778010751154,-222.942372283455,14.7644814665567));
#75626=CARTESIAN_POINT('Ctrl Pts',(2.13771045830097,-223.424086702396,14.7115621781461));
#75627=CARTESIAN_POINT('Ctrl Pts',(2.55525875143796,-224.276148193141,14.6586428897355));
#75628=CARTESIAN_POINT('Ctrl Pts',(2.51935489619294,-225.108653434278,14.6057236013249));
#75629=CARTESIAN_POINT('Ctrl Pts',(2.48345104094792,-225.941158675414,14.5528043129143));
#75630=CARTESIAN_POINT('Ctrl Pts',(1.9940950373209,-226.754107666942,14.4998850245037));
#75631=CARTESIAN_POINT('Ctrl Pts',(1.27521618294983,-227.175494966323,14.4469657360931));
#75632=CARTESIAN_POINT('Ctrl Pts',(0.556337328578752,-227.596882265703,
14.3940464476825));
#75633=CARTESIAN_POINT('Ctrl Pts',(-0.392064376536375,-227.626707872936,
14.3411271592719));
#75634=CARTESIAN_POINT('Ctrl Pts',(-1.13600033078234,-227.251323590738,
14.2882078708613));
#75635=CARTESIAN_POINT('Ctrl Pts',(-1.8799362850283,-226.87593930854,14.2352885824507));
#75636=CARTESIAN_POINT('Ctrl Pts',(-2.41940648840511,-226.095345136912,
14.1823692940401));
#75637=CARTESIAN_POINT('Ctrl Pts',(-2.50754938645462,-225.266740953441,
14.1294500056295));
#75638=CARTESIAN_POINT('Ctrl Pts',(-2.5169138364799,-225.178708648644,14.1238277712504));
#75639=CARTESIAN_POINT('Ctrl Pts',(-2.52118402176622,-225.090134440647,
14.1182055368712));
#75640=CARTESIAN_POINT('Ctrl Pts',(-2.52055923806654,-225.001499367411,
14.112583302492));
#75641=CARTESIAN_POINT('Ctrl Pts',(-2.51484781591379,-225.001779432988,
14.387416697508));
#75642=CARTESIAN_POINT('Ctrl Pts',(-2.51678210576093,-225.298084098157,
14.4061027039678));
#75643=CARTESIAN_POINT('Ctrl Pts',(-2.4683915941746,-225.593777341111,14.4247887104275));
#75644=CARTESIAN_POINT('Ctrl Pts',(-2.36688521153746,-225.869947863523,
14.4434747168873));
#75645=CARTESIAN_POINT('Ctrl Pts',(-2.07941632138898,-226.652070440518,
14.4963940052979));
#75646=CARTESIAN_POINT('Ctrl Pts',(-1.36593790564043,-227.277613359643,
14.5493132937085));
#75647=CARTESIAN_POINT('Ctrl Pts',(-0.552937673309945,-227.460328193408,
14.6022325821191));
#75648=CARTESIAN_POINT('Ctrl Pts',(0.260062559020537,-227.643043027173,
14.6551518705297));
#75649=CARTESIAN_POINT('Ctrl Pts',(1.17258460793295,-227.382929775576,14.7080711589402));
#75650=CARTESIAN_POINT('Ctrl Pts',(1.76705840178706,-226.799016257435,14.7609904473508));
#75651=CARTESIAN_POINT('Ctrl Pts',(2.36153219564117,-226.215102739294,14.8139097357615));
#75652=CARTESIAN_POINT('Ctrl Pts',(2.63795773443698,-225.307388954609,14.8668290241721));
#75653=CARTESIAN_POINT('Ctrl Pts',(2.46984269705649,-224.491244713403,14.9197483125826));
#75654=CARTESIAN_POINT('Ctrl Pts',(2.30172765967599,-223.675100472197,14.9726676009932));
#75655=CARTESIAN_POINT('Ctrl Pts',(1.68907204611922,-222.95052577447,15.0255868894038));
#75656=CARTESIAN_POINT('Ctrl Pts',(0.912227053103926,-222.649085987657,
15.0785061778144));
#75657=CARTESIAN_POINT('Ctrl Pts',(0.135382060088619,-222.347646200844,
15.131425466225));
#75658=CARTESIAN_POINT('Ctrl Pts',(-0.805652312385208,-222.469341324945,
15.1843447546356));
#75659=CARTESIAN_POINT('Ctrl Pts',(-1.48025875397667,-222.958483673561,
15.2372640430462));
#75660=CARTESIAN_POINT('Ctrl Pts',(-2.11829925530295,-223.421112860135,
15.2873149278668));
#75661=CARTESIAN_POINT('Ctrl Pts',(-2.51801164078776,-224.212435079755,
15.3373658126874));
#75662=CARTESIAN_POINT('Ctrl Pts',(-2.52136959094702,-225.00082166017,15.387416697508));
#75663=CARTESIAN_POINT('Origin',(0.,-225.,10.));
#75664=CARTESIAN_POINT('',(-2.51727018845018,-224.997699004247,16.387416697508));
#75665=CARTESIAN_POINT('',(-2.51344546704351,-224.999883655119,16.112583302492));
#75666=CARTESIAN_POINT('',(-2.5175,-225.,10.));
#75667=CARTESIAN_POINT('Ctrl Pts',(-2.51344546704351,-224.999883655119,
16.112583302492));
#75668=CARTESIAN_POINT('Ctrl Pts',(-2.5136157670192,-224.586818602614,16.0865703311317));
#75669=CARTESIAN_POINT('Ctrl Pts',(-2.41747223694359,-224.173828204922,
16.0605573597714));
#75670=CARTESIAN_POINT('Ctrl Pts',(-2.22458066022694,-223.81248345365,16.034544388411));
#75671=CARTESIAN_POINT('Ctrl Pts',(-1.83217316325739,-223.077384535369,
15.9816251000004));
#75672=CARTESIAN_POINT('Ctrl Pts',(-1.03936916752074,-222.55602363786,15.9287058115898));
#75673=CARTESIAN_POINT('Ctrl Pts',(-0.208955765857058,-222.486975497596,
15.8757865231793));
#75674=CARTESIAN_POINT('Ctrl Pts',(0.621457635806621,-222.417927357332,
15.8228672347687));
#75675=CARTESIAN_POINT('Ctrl Pts',(1.48948044339735,-222.801191974312,15.7699479463581));
#75676=CARTESIAN_POINT('Ctrl Pts',(1.99790543721839,-223.461387467331,15.7170286579475));
#75677=CARTESIAN_POINT('Ctrl Pts',(2.50633043103944,-224.12158296035,15.6641093695369));
#75678=CARTESIAN_POINT('Ctrl Pts',(2.6551576110908,-225.058709329408,15.6111900811263));
#75679=CARTESIAN_POINT('Ctrl Pts',(2.37628366271229,-225.843937566455,15.5582707927157));
#75680=CARTESIAN_POINT('Ctrl Pts',(2.09740971433378,-226.629165803502,15.5053515043051));
#75681=CARTESIAN_POINT('Ctrl Pts',(1.3908346375254,-227.262495908538,15.4524322158945));
#75682=CARTESIAN_POINT('Ctrl Pts',(0.579887173539465,-227.454116037949,
15.3995129274839));
#75683=CARTESIAN_POINT('Ctrl Pts',(-0.23106029044647,-227.64573616736,15.3465936390733));
#75684=CARTESIAN_POINT('Ctrl Pts',(-1.14638014160996,-227.395646321145,
15.2936743506627));
#75685=CARTESIAN_POINT('Ctrl Pts',(-1.74722203405439,-226.818287608017,
15.2407550622521));
#75686=CARTESIAN_POINT('Ctrl Pts',(-2.2323064270685,-226.352162152333,15.1980311423321));
#75687=CARTESIAN_POINT('Ctrl Pts',(-2.51241416344975,-225.672722929182,
15.155307222412));
#75688=CARTESIAN_POINT('Ctrl Pts',(-2.51858868022655,-224.99780466334,15.112583302492));
#75689=CARTESIAN_POINT('Ctrl Pts',(-2.52136959094702,-225.00082166017,15.387416697508));
#75690=CARTESIAN_POINT('Ctrl Pts',(-2.52156203422402,-225.046003896322,
15.390285101098));
#75691=CARTESIAN_POINT('Ctrl Pts',(-2.52045268813929,-225.091176490639,
15.393153504688));
#75692=CARTESIAN_POINT('Ctrl Pts',(-2.51801180762806,-225.136277021139,
15.396021908278));
#75693=CARTESIAN_POINT('Ctrl Pts',(-2.4729799089789,-225.968338446969,15.4489411966886));
#75694=CARTESIAN_POINT('Ctrl Pts',(-1.97473760097149,-226.775871725499,
15.5018604850992));
#75695=CARTESIAN_POINT('Ctrl Pts',(-1.25128055395565,-227.189349644336,
15.5547797735098));
#75696=CARTESIAN_POINT('Ctrl Pts',(-0.527823506939808,-227.602827563173,
15.6076990619204));
#75697=CARTESIAN_POINT('Ctrl Pts',(0.420848279084464,-227.622250122317,
15.660618350331));
#75698=CARTESIAN_POINT('Ctrl Pts',(1.1606226134895,-227.238729559116,15.7135376387416));
#75699=CARTESIAN_POINT('Ctrl Pts',(1.90039694789453,-226.855208995915,15.7664569271522));
#75700=CARTESIAN_POINT('Ctrl Pts',(2.43127383068032,-226.06874531037,15.8193762155628));
#75701=CARTESIAN_POINT('Ctrl Pts',(2.51032401071362,-225.23922426946,15.8722955039734));
#75702=CARTESIAN_POINT('Ctrl Pts',(2.58937419074691,-224.409703228549,15.925214792384));
#75703=CARTESIAN_POINT('Ctrl Pts',(2.21659766802771,-223.537124832274,15.9781340807946));
#75704=CARTESIAN_POINT('Ctrl Pts',(1.56257697204023,-223.020780937739,16.0310533692052));
#75705=CARTESIAN_POINT('Ctrl Pts',(0.908556276052754,-222.504437043205,
16.0839726576158));
#75706=CARTESIAN_POINT('Ctrl Pts',(-0.0267085932030033,-222.344327650411,
16.1368919460264));
#75707=CARTESIAN_POINT('Ctrl Pts',(-0.815240449980246,-222.613718814094,
16.189811234437));
#75708=CARTESIAN_POINT('Ctrl Pts',(-1.60377230675749,-222.883109977778,
16.2427305228476));
#75709=CARTESIAN_POINT('Ctrl Pts',(-2.24557115105622,-223.582001697939,
16.2956498112582));
#75710=CARTESIAN_POINT('Ctrl Pts',(-2.44694984427243,-224.390581137697,
16.3485690996688));
#75711=CARTESIAN_POINT('Ctrl Pts',(-2.49622663743184,-224.588438225602,
16.3615182989485));
#75712=CARTESIAN_POINT('Ctrl Pts',(-2.5191325265179,-224.792863051892,16.3744674982283));
#75713=CARTESIAN_POINT('Ctrl Pts',(-2.51727018845018,-224.997699004247,
16.387416697508));
#75714=CARTESIAN_POINT('Origin',(0.,-225.,10.));
#75715=CARTESIAN_POINT('',(-2.51357021912498,-225.000594611151,17.387416697508));
#75716=CARTESIAN_POINT('',(-2.51816170421521,-225.00225638587,17.112583302492));
#75717=CARTESIAN_POINT('',(-2.5175,-225.,10.));
#75718=CARTESIAN_POINT('Ctrl Pts',(-2.51816170421521,-225.00225638587,17.112583302492));
#75719=CARTESIAN_POINT('Ctrl Pts',(-2.51206049652332,-224.34116215718,17.0707527282619));
#75720=CARTESIAN_POINT('Ctrl Pts',(-2.24478072224065,-223.675701993465,
17.0289221540319));
#75721=CARTESIAN_POINT('Ctrl Pts',(-1.77759132674405,-223.211390558611,
16.9870915798018));
#75722=CARTESIAN_POINT('Ctrl Pts',(-1.18655640031251,-222.623996500901,
16.9341722913912));
#75723=CARTESIAN_POINT('Ctrl Pts',(-0.275577426159809,-222.358529612653,
16.8812530029806));
#75724=CARTESIAN_POINT('Ctrl Pts',(0.538481636520985,-222.536467538322,
16.82833371457));
#75725=CARTESIAN_POINT('Ctrl Pts',(1.35254069920178,-222.714405463992,16.7754144261594));
#75726=CARTESIAN_POINT('Ctrl Pts',(2.06967985041067,-223.335748203578,16.7224951377488));
#75727=CARTESIAN_POINT('Ctrl Pts',(2.36173622793228,-224.11616933087,16.6695758493382));
#75728=CARTESIAN_POINT('Ctrl Pts',(2.65379260545388,-224.896590458161,16.6166565609276));
#75729=CARTESIAN_POINT('Ctrl Pts',(2.52076620928823,-225.836089973159,16.563737272517));
#75730=CARTESIAN_POINT('Ctrl Pts',(2.02352991606093,-226.504752916663,16.5108179841064));
#75731=CARTESIAN_POINT('Ctrl Pts',(1.52629362283363,-227.173415860166,16.4578986956958));
#75732=CARTESIAN_POINT('Ctrl Pts',(0.664847432544685,-227.571242232176,
16.4049794072852));
#75733=CARTESIAN_POINT('Ctrl Pts',(-0.16661089524264,-227.516186692489,
16.3520601188746));
#75734=CARTESIAN_POINT('Ctrl Pts',(-0.998069223029971,-227.461131152803,
16.299140830464));
#75735=CARTESIAN_POINT('Ctrl Pts',(-1.79953968831569,-226.953193701421,
16.2462215420534));
#75736=CARTESIAN_POINT('Ctrl Pts',(-2.20426942185732,-226.224806506203,
16.1933022536428));
#75737=CARTESIAN_POINT('Ctrl Pts',(-2.41005046800164,-225.854464851987,
16.1663959365926));
#75738=CARTESIAN_POINT('Ctrl Pts',(-2.5132693185722,-225.427134318303,16.1394896195423));
#75739=CARTESIAN_POINT('Ctrl Pts',(-2.51344546704351,-224.999883655119,
16.112583302492));
#75740=CARTESIAN_POINT('Ctrl Pts',(-2.51727018845018,-224.997699004247,
16.387416697508));
#75741=CARTESIAN_POINT('Ctrl Pts',(-2.51152173891671,-225.629962906901,
16.4273867866389));
#75742=CARTESIAN_POINT('Ctrl Pts',(-2.26979104539765,-226.26614386228,16.4673568757697));
#75743=CARTESIAN_POINT('Ctrl Pts',(-1.83921083723923,-226.725183580632,
16.5073269649006));
#75744=CARTESIAN_POINT('Ctrl Pts',(-1.26913459485615,-227.332939424455,
16.5602462533112));
#75745=CARTESIAN_POINT('Ctrl Pts',(-0.368023567956294,-227.630183952747,
16.6131655417217));
#75746=CARTESIAN_POINT('Ctrl Pts',(0.451773855565479,-227.480898077363,
16.6660848301324));
#75747=CARTESIAN_POINT('Ctrl Pts',(1.27157127908725,-227.331612201979,16.7190041185429));
#75748=CARTESIAN_POINT('Ctrl Pts',(2.01005509923094,-226.735795922919,16.7719234069536));
#75749=CARTESIAN_POINT('Ctrl Pts',(2.32929513381597,-225.966094753385,16.8248426953642));
#75750=CARTESIAN_POINT('Ctrl Pts',(2.64853516840099,-225.19639358385,16.8777619837748));
#75751=CARTESIAN_POINT('Ctrl Pts',(2.54853141742736,-224.252807523841,16.9306812721853));
#75752=CARTESIAN_POINT('Ctrl Pts',(2.07504559659883,-223.567121544764,16.9836005605959));
#75753=CARTESIAN_POINT('Ctrl Pts',(1.60155977577031,-222.881435565687,17.0365198490065));
#75754=CARTESIAN_POINT('Ctrl Pts',(0.754591885086894,-222.453649667542,
17.0894391374171));
#75755=CARTESIAN_POINT('Ctrl Pts',(-0.078285587814752,-222.479518650835,
17.1423584258277));
#75756=CARTESIAN_POINT('Ctrl Pts',(-0.911163060716401,-222.505387634127,
17.1952777142383));
#75757=CARTESIAN_POINT('Ctrl Pts',(-1.72995011583628,-222.984911498856,
17.2481970026489));
#75758=CARTESIAN_POINT('Ctrl Pts',(-2.15996980779954,-223.698660170661,
17.3011162910595));
#75759=CARTESIAN_POINT('Ctrl Pts',(-2.3937275126106,-224.086652289281,17.329883093209));
#75760=CARTESIAN_POINT('Ctrl Pts',(-2.51260507103825,-224.543857471223,
17.3586498953585));
#75761=CARTESIAN_POINT('Ctrl Pts',(-2.51357021912498,-225.000594611151,
17.387416697508));
#75762=CARTESIAN_POINT('Origin',(0.,-225.,10.));
#75763=CARTESIAN_POINT('',(-2.51944981591128,-225.001988766476,18.387416697508));
#75764=CARTESIAN_POINT('',(-2.52086477440939,-224.998703164308,18.112583302492));
#75765=CARTESIAN_POINT('',(-2.5175,-225.,10.));
#75766=CARTESIAN_POINT('Ctrl Pts',(-2.52086477440939,-224.998703164308,
18.112583302492));
#75767=CARTESIAN_POINT('Ctrl Pts',(-2.52133264793523,-224.924175560637,
18.1078544138028));
#75768=CARTESIAN_POINT('Ctrl Pts',(-2.51831399385996,-224.849686389881,
18.1031255251136));
#75769=CARTESIAN_POINT('Ctrl Pts',(-2.51168541869473,-224.775519854655,
18.0983966364243));
#75770=CARTESIAN_POINT('Ctrl Pts',(-2.43750742382676,-223.945548898266,
18.0454773480137));
#75771=CARTESIAN_POINT('Ctrl Pts',(-1.91125752455906,-223.155981722102,
17.9925580596032));
#75772=CARTESIAN_POINT('Ctrl Pts',(-1.17374787359455,-222.768124020852,
17.9396387711926));
#75773=CARTESIAN_POINT('Ctrl Pts',(-0.436238222630047,-222.380266319601,
17.886719482782));
#75774=CARTESIAN_POINT('Ctrl Pts',(0.512531180031255,-222.394118093264,
17.8338001943714));
#75775=CARTESIAN_POINT('Ctrl Pts',(1.23840357736626,-222.803340883536,17.7808809059608));
#75776=CARTESIAN_POINT('Ctrl Pts',(1.96427597470126,-223.212563673808,17.7279616175502));
#75777=CARTESIAN_POINT('Ctrl Pts',(2.46725136670996,-224.01715748069,17.6750423291396));
#75778=CARTESIAN_POINT('Ctrl Pts',(2.51716817319288,-224.848940138306,17.622123040729));
#75779=CARTESIAN_POINT('Ctrl Pts',(2.5670849796758,-225.680722795923,17.5692037523184));
#75780=CARTESIAN_POINT('Ctrl Pts',(2.16394320063292,-226.539694304275,17.5162844639078));
#75781=CARTESIAN_POINT('Ctrl Pts',(1.49222053119448,-227.032789345438,17.4633651754972));
#75782=CARTESIAN_POINT('Ctrl Pts',(0.820497861756054,-227.525884386601,
17.4104458870866));
#75783=CARTESIAN_POINT('Ctrl Pts',(-0.119805698077932,-227.653102960575,
17.357526598676));
#75784=CARTESIAN_POINT('Ctrl Pts',(-0.898407270108993,-227.356229836916,
17.3046073102654));
#75785=CARTESIAN_POINT('Ctrl Pts',(-1.67700884214006,-227.059356713256,
17.2516880218548));
#75786=CARTESIAN_POINT('Ctrl Pts',(-2.2939084263682,-226.338391891963,17.1987687334442));
#75787=CARTESIAN_POINT('Ctrl Pts',(-2.46681277912709,-225.52324886773,17.1458494450336));
#75788=CARTESIAN_POINT('Ctrl Pts',(-2.50304317839922,-225.35244369851,17.1347607308531));
#75789=CARTESIAN_POINT('Ctrl Pts',(-2.51977905108402,-225.177503441002,
17.1236720166725));
#75790=CARTESIAN_POINT('Ctrl Pts',(-2.51816170421521,-225.00225638587,17.112583302492));
#75791=CARTESIAN_POINT('Ctrl Pts',(-2.51357021912498,-225.000594611151,
17.387416697508));
#75792=CARTESIAN_POINT('Ctrl Pts',(-2.51438055340487,-225.38406919549,17.4115691837691));
#75793=CARTESIAN_POINT('Ctrl Pts',(-2.43207194083465,-225.767213847134,
17.4357216700302));
#75794=CARTESIAN_POINT('Ctrl Pts',(-2.26484973962718,-226.108787887449,
17.4598741562913));
#75795=CARTESIAN_POINT('Ctrl Pts',(-1.89845765068491,-226.85719345355,17.5127934447019));
#75796=CARTESIAN_POINT('Ctrl Pts',(-1.12442114399372,-227.40603110687,17.5657127331125));
#75797=CARTESIAN_POINT('Ctrl Pts',(-0.296939288961462,-227.504152899472,
17.6186320215231));
#75798=CARTESIAN_POINT('Ctrl Pts',(0.53054256607079,-227.602274692073,17.6715513099337));
#75799=CARTESIAN_POINT('Ctrl Pts',(1.41146976944411,-227.249680623955,17.7244705983443));
#75800=CARTESIAN_POINT('Ctrl Pts',(1.94273000790024,-226.607717426205,17.7773898867549));
#75801=CARTESIAN_POINT('Ctrl Pts',(2.47399024635636,-225.965754228455,17.8303091751655));
#75802=CARTESIAN_POINT('Ctrl Pts',(2.65558351989528,-225.034421901072,17.8832284635761));
#75803=CARTESIAN_POINT('Ctrl Pts',(2.40441283605821,-224.239898723388,17.9361477519867));
#75804=CARTESIAN_POINT('Ctrl Pts',(2.15324215222114,-223.445375545704,17.9890670403973));
#75805=CARTESIAN_POINT('Ctrl Pts',(1.46930751100809,-222.787661517718,18.0419863288079));
#75806=CARTESIAN_POINT('Ctrl Pts',(0.665577216243244,-222.567725297085,
18.0949056172185));
#75807=CARTESIAN_POINT('Ctrl Pts',(-0.138153078521605,-222.347789076451,
18.1478249056291));
#75808=CARTESIAN_POINT('Ctrl Pts',(-1.06167902683825,-222.565630663171,
18.2007441940397));
#75809=CARTESIAN_POINT('Ctrl Pts',(-1.68239481841196,-223.121568327994,
18.2536634824503));
#75810=CARTESIAN_POINT('Ctrl Pts',(-2.20534675303818,-223.589944807693,
18.2982478874695));
#75811=CARTESIAN_POINT('Ctrl Pts',(-2.51336306631068,-224.298302969004,
18.3428322924888));
#75812=CARTESIAN_POINT('Ctrl Pts',(-2.51944981591128,-225.001988766476,
18.387416697508));
#75813=CARTESIAN_POINT('Origin',(0.,-225.,10.));
#75814=CARTESIAN_POINT('',(-2.51981687702631,-224.998184138844,19.387416697508));
#75815=CARTESIAN_POINT('',(-2.51426761094033,-224.998573473955,19.112583302492));
#75816=CARTESIAN_POINT('',(-2.5175,-225.,10.));
#75817=CARTESIAN_POINT('',(1.91346599666508,-223.364012796625,20.));
#75818=CARTESIAN_POINT('Ctrl Pts',(-2.51981687702631,-224.998184138844,
19.387416697508));
#75819=CARTESIAN_POINT('Ctrl Pts',(-2.51391403651899,-225.714895358089,
19.4328532664402));
#75820=CARTESIAN_POINT('Ctrl Pts',(-2.19260490784885,-226.43611772376,19.4782898353724));
#75821=CARTESIAN_POINT('Ctrl Pts',(-1.6520347840379,-226.905008540457,19.5237264043046));
#75822=CARTESIAN_POINT('Ctrl Pts',(-1.02244089170878,-227.45111862194,19.5766456927152));
#75823=CARTESIAN_POINT('Ctrl Pts',(-0.0954214211907685,-227.65494321484,
19.6295649811258));
#75824=CARTESIAN_POINT('Ctrl Pts',(0.704614973850839,-227.421676530985,
19.6824842695364));
#75825=CARTESIAN_POINT('Ctrl Pts',(1.50465136889245,-227.18840984713,19.735403557947));
#75826=CARTESIAN_POINT('Ctrl Pts',(2.17770468845765,-226.51805188652,19.7883228463576));
#75827=CARTESIAN_POINT('Ctrl Pts',(2.41590047509774,-225.721010295893,19.8412421347682));
#75828=CARTESIAN_POINT('Ctrl Pts',(2.65409626173783,-224.923968705266,19.8941614231788));
#75829=CARTESIAN_POINT('Ctrl Pts',(2.45743451545281,-224.000243484622,19.9470807115894));
#75830=CARTESIAN_POINT('Ctrl Pts',(1.91346599666508,-223.364012796625,20.));
#75831=CARTESIAN_POINT('',(-1.9171250238334,-223.361260565514,20.));
#75832=CARTESIAN_POINT('Origin',(0.,-225.,20.));
#75833=CARTESIAN_POINT('Ctrl Pts',(-1.91712859175364,-223.361257881811,
20.));
#75834=CARTESIAN_POINT('Ctrl Pts',(-1.38658191799954,-222.742516992798,
19.948244384658));
#75835=CARTESIAN_POINT('Ctrl Pts',(-0.527608246006481,-222.40292978571,
19.896488769316));
#75836=CARTESIAN_POINT('Ctrl Pts',(0.28236917328897,-222.494297760505,19.8447331539741));
#75837=CARTESIAN_POINT('Ctrl Pts',(1.1105581219575,-222.587720052515,19.7918138655635));
#75838=CARTESIAN_POINT('Ctrl Pts',(1.88752278571044,-223.131694576731,19.7388945771529));
#75839=CARTESIAN_POINT('Ctrl Pts',(2.25823165337626,-223.877857468017,19.6859752887423));
#75840=CARTESIAN_POINT('Ctrl Pts',(2.62894052104207,-224.624020359302,19.6330560003317));
#75841=CARTESIAN_POINT('Ctrl Pts',(2.59339359262077,-225.572371617659,19.5801367119211));
#75842=CARTESIAN_POINT('Ctrl Pts',(2.16760742134957,-226.288671511728,19.5272174235105));
#75843=CARTESIAN_POINT('Ctrl Pts',(1.74182125007838,-227.004971405797,19.4742981350999));
#75844=CARTESIAN_POINT('Ctrl Pts',(0.925795835957292,-227.489219935578,
19.4213788466893));
#75845=CARTESIAN_POINT('Ctrl Pts',(0.0930673370354757,-227.519959958572,
19.3684595582787));
#75846=CARTESIAN_POINT('Ctrl Pts',(-0.739661161886337,-227.550699981566,
19.3155402698681));
#75847=CARTESIAN_POINT('Ctrl Pts',(-1.58909274560888,-227.127931497772,
19.2626209814575));
#75848=CARTESIAN_POINT('Ctrl Pts',(-2.06658807342754,-226.445046900883,
19.2097016930469));
#75849=CARTESIAN_POINT('Ctrl Pts',(-2.35869062637836,-226.027299705254,
19.1773288961953));
#75850=CARTESIAN_POINT('Ctrl Pts',(-2.51160544441321,-225.512210634445,
19.1449560993436));
#75851=CARTESIAN_POINT('Ctrl Pts',(-2.51426761094033,-224.998573473955,
19.112583302492));
#75852=CARTESIAN_POINT('Origin',(-160.,-225.,10.));
#75853=CARTESIAN_POINT('',(-162.51351594159,-224.999424933735,0.387416697508052));
#75854=CARTESIAN_POINT('',(-162.515402351214,-225.003740476838,0.112583302491938));
#75855=CARTESIAN_POINT('',(-162.5175,-225.,10.));
#75856=CARTESIAN_POINT('',(-161.913465996665,-223.364012796625,0.));
#75857=CARTESIAN_POINT('Ctrl Pts',(-162.515402351214,-225.003740476838,
0.112583302491938));
#75858=CARTESIAN_POINT('Ctrl Pts',(-162.510237314095,-224.411047851875,
0.075055534994612));
#75859=CARTESIAN_POINT('Ctrl Pts',(-162.299221828084,-223.815196439696,
0.0375277674972861));
#75860=CARTESIAN_POINT('Ctrl Pts',(-161.913465996665,-223.364012796625,
-4.02455846426619E-14));
#75861=CARTESIAN_POINT('',(-158.082847352964,-223.361245062325,1.97453514552116E-15));
#75862=CARTESIAN_POINT('Origin',(-160.,-225.,0.));
#75863=CARTESIAN_POINT('Ctrl Pts',(-158.082843652116,-223.361242283932,
1.5839321182582E-15));
#75864=CARTESIAN_POINT('Ctrl Pts',(-158.613381414978,-222.742548947437,
0.0517556153419938));
#75865=CARTESIAN_POINT('Ctrl Pts',(-159.472376042683,-222.40287561289,0.103511230683985));
#75866=CARTESIAN_POINT('Ctrl Pts',(-160.282371291112,-222.494227887034,
0.155266846025977));
#75867=CARTESIAN_POINT('Ctrl Pts',(-161.110578469784,-222.587634125381,
0.208186134436575));
#75868=CARTESIAN_POINT('Ctrl Pts',(-161.887558094787,-223.131666225295,
0.261105422847174));
#75869=CARTESIAN_POINT('Ctrl Pts',(-162.25827216591,-223.877852586243,0.314024711257772));
#75870=CARTESIAN_POINT('Ctrl Pts',(-162.429649136561,-224.222806198858,
0.338488706674532));
#75871=CARTESIAN_POINT('Ctrl Pts',(-162.514202708326,-224.61096239135,0.362952702091292));
#75872=CARTESIAN_POINT('Ctrl Pts',(-162.51351594159,-224.999424933735,0.387416697508052));
#75873=CARTESIAN_POINT('Origin',(-160.,-225.,10.));
#75874=CARTESIAN_POINT('',(-162.517460115391,-225.002301238227,1.38741669750805));
#75875=CARTESIAN_POINT('',(-162.521728577063,-224.999864685758,1.11258330249194));
#75876=CARTESIAN_POINT('',(-162.5175,-225.,10.));
#75877=CARTESIAN_POINT('Ctrl Pts',(-162.521728577063,-224.999864685758,
1.11258330249194));
#75878=CARTESIAN_POINT('Ctrl Pts',(-162.521733449713,-224.993155418077,
1.11215722053546));
#75879=CARTESIAN_POINT('Ctrl Pts',(-162.521709006639,-224.986446188795,
1.11173113857898));
#75880=CARTESIAN_POINT('Ctrl Pts',(-162.521655141041,-224.97973719783,1.11130505662251));
#75881=CARTESIAN_POINT('Ctrl Pts',(-162.514965045176,-224.146481946371,
1.05838576821191));
#75882=CARTESIAN_POINT('Ctrl Pts',(-162.054415225741,-223.316902891715,
1.00546647980131));
#75883=CARTESIAN_POINT('Ctrl Pts',(-161.350736487674,-222.870539435387,
0.952547191390716));
#75884=CARTESIAN_POINT('Ctrl Pts',(-160.647057749606,-222.424175979059,
0.899627902980117));
#75885=CARTESIAN_POINT('Ctrl Pts',(-159.700250092906,-222.361028121059,
0.846708614569519));
#75886=CARTESIAN_POINT('Ctrl Pts',(-158.943607496028,-222.71014994938,0.793789326158921));
#75887=CARTESIAN_POINT('Ctrl Pts',(-158.186964899149,-223.059271777701,
0.740870037748324));
#75888=CARTESIAN_POINT('Ctrl Pts',(-157.620487362092,-223.820663292344,
0.687950749337728));
#75889=CARTESIAN_POINT('Ctrl Pts',(-157.503322619656,-224.645584773054,
0.635031460927131));
#75890=CARTESIAN_POINT('Ctrl Pts',(-157.386157877221,-225.470506253763,
0.582112172516533));
#75891=CARTESIAN_POINT('Ctrl Pts',(-157.718305929406,-226.358957700538,
0.529192884105933));
#75892=CARTESIAN_POINT('Ctrl Pts',(-158.347923918086,-226.905064885608,
0.476273595695335));
#75893=CARTESIAN_POINT('Ctrl Pts',(-158.977541906767,-227.451172070678,
0.423354307284737));
#75894=CARTESIAN_POINT('Ctrl Pts',(-159.904629831943,-227.654934994044,
0.370435018874143));
#75895=CARTESIAN_POINT('Ctrl Pts',(-160.704626518296,-227.421707556381,
0.317515730463546));
#75896=CARTESIAN_POINT('Ctrl Pts',(-161.504623204649,-227.188480118719,
0.264596442052949));
#75897=CARTESIAN_POINT('Ctrl Pts',(-162.177528652179,-226.518262320029,
0.21167715364235));
#75898=CARTESIAN_POINT('Ctrl Pts',(-162.41573147988,-225.721203161505,0.158757865231754));
#75899=CARTESIAN_POINT('Ctrl Pts',(-162.485012528705,-225.489379320406,
0.143366344318482));
#75900=CARTESIAN_POINT('Ctrl Pts',(-162.517520723346,-225.246825571972,
0.12797482340521));
#75901=CARTESIAN_POINT('Ctrl Pts',(-162.515402351214,-225.003740476838,
0.112583302491938));
#75902=CARTESIAN_POINT('Ctrl Pts',(-162.51351594159,-224.999424933735,0.387416697508052));
#75903=CARTESIAN_POINT('Ctrl Pts',(-162.512717128954,-225.451265087905,
0.415871990501891));
#75904=CARTESIAN_POINT('Ctrl Pts',(-162.39659516119,-225.903519708241,0.44432728349573));
#75905=CARTESIAN_POINT('Ctrl Pts',(-162.167641214847,-226.288685316668,
0.472782576489569));
#75906=CARTESIAN_POINT('Ctrl Pts',(-161.74184767542,-227.004991064166,0.525701864900165));
#75907=CARTESIAN_POINT('Ctrl Pts',(-160.925812079326,-227.48926193718,0.578621153310761));
#75908=CARTESIAN_POINT('Ctrl Pts',(-160.093070279045,-227.520005786494,
0.631540441721358));
#75909=CARTESIAN_POINT('Ctrl Pts',(-159.260328478764,-227.550749635808,
0.684459730131956));
#75910=CARTESIAN_POINT('Ctrl Pts',(-158.410880474296,-227.127966461422,
0.737379018542555));
#75911=CARTESIAN_POINT('Ctrl Pts',(-157.9333767975,-226.445068740439,0.790298306953154));
#75912=CARTESIAN_POINT('Ctrl Pts',(-157.455873120704,-225.762171019456,
0.843217595363751));
#75913=CARTESIAN_POINT('Ctrl Pts',(-157.350313771578,-224.819158751875,
0.896136883774348));
#75914=CARTESIAN_POINT('Ctrl Pts',(-157.665030107393,-224.047579921191,
0.949056172184944));
#75915=CARTESIAN_POINT('Ctrl Pts',(-157.979746443209,-223.276001090507,
1.00197546059554));
#75916=CARTESIAN_POINT('Ctrl Pts',(-158.714738463965,-222.67585569672,1.05489474900614));
#75917=CARTESIAN_POINT('Ctrl Pts',(-159.533660630143,-222.521757928645,
1.10781403741674));
#75918=CARTESIAN_POINT('Ctrl Pts',(-160.352582796321,-222.36766016057,1.16073332582734));
#75919=CARTESIAN_POINT('Ctrl Pts',(-161.255435107919,-222.659610018209,
1.21365261423794));
#75920=CARTESIAN_POINT('Ctrl Pts',(-161.829078728829,-223.264017195323,
1.26657190264853));
#75921=CARTESIAN_POINT('Ctrl Pts',(-162.265730138761,-223.724085496338,
1.30685350093504));
#75922=CARTESIAN_POINT('Ctrl Pts',(-162.511635000215,-224.365194447016,
1.34713509922154));
#75923=CARTESIAN_POINT('Ctrl Pts',(-162.517460115391,-225.002301238227,
1.38741669750805));
#75924=CARTESIAN_POINT('Origin',(-160.,-225.,10.));
#75925=CARTESIAN_POINT('',(-162.521340804038,-224.999094471355,2.38741669750805));
#75926=CARTESIAN_POINT('',(-162.515825357218,-224.997885174742,2.11258330249194));
#75927=CARTESIAN_POINT('',(-162.5175,-225.,10.));
#75928=CARTESIAN_POINT('Ctrl Pts',(-162.515825357218,-224.997885174742,
2.11258330249194));
#75929=CARTESIAN_POINT('Ctrl Pts',(-162.517874459667,-224.740545642659,
2.09633961766571));
#75930=CARTESIAN_POINT('Ctrl Pts',(-162.481551331845,-224.483770756502,
2.08009593283949));
#75931=CARTESIAN_POINT('Ctrl Pts',(-162.404452695359,-224.239886170331,
2.06385224801326));
#75932=CARTESIAN_POINT('Ctrl Pts',(-162.153277852707,-223.445349777107,
2.01093295960267));
#75933=CARTESIAN_POINT('Ctrl Pts',(-161.469331891228,-222.787624664217,
1.95801367119207));
#75934=CARTESIAN_POINT('Ctrl Pts',(-160.665588259213,-222.567684878868,
1.90509438278147));
#75935=CARTESIAN_POINT('Ctrl Pts',(-159.861844627198,-222.347745093518,
1.85217509437087));
#75936=CARTESIAN_POINT('Ctrl Pts',(-158.938303324646,-222.565590635709,
1.79925580596027));
#75937=CARTESIAN_POINT('Ctrl Pts',(-158.317577269691,-223.121537364058,
1.74633651754968));
#75938=CARTESIAN_POINT('Ctrl Pts',(-157.696851214735,-223.677484092407,
1.69341722913908));
#75939=CARTESIAN_POINT('Ctrl Pts',(-157.378940407375,-224.571532006914,
1.64049794072848));
#75940=CARTESIAN_POINT('Ctrl Pts',(-157.509319921586,-225.394560702438,
1.58757865231788));
#75941=CARTESIAN_POINT('Ctrl Pts',(-157.639699435798,-226.217589397962,
1.53465936390729));
#75942=CARTESIAN_POINT('Ctrl Pts',(-158.218369271582,-226.969598874502,
1.48174007549669));
#75943=CARTESIAN_POINT('Ctrl Pts',(-158.980532001829,-227.306478111901,
1.42882078708609));
#75944=CARTESIAN_POINT('Ctrl Pts',(-159.742694732075,-227.6433573493,1.37590149867549));
#75945=CARTESIAN_POINT('Ctrl Pts',(-160.688350356784,-227.565106347558,
1.3229822102649));
#75946=CARTESIAN_POINT('Ctrl Pts',(-161.384762982991,-227.107515122556,
1.2700629218543));
#75947=CARTESIAN_POINT('Ctrl Pts',(-162.075568412594,-226.65360821324,1.21756971540018));
#75948=CARTESIAN_POINT('Ctrl Pts',(-162.521128267657,-225.826445037713,
1.16507650894606));
#75949=CARTESIAN_POINT('Ctrl Pts',(-162.521728577063,-224.999864685758,
1.11258330249194));
#75950=CARTESIAN_POINT('Ctrl Pts',(-162.517460115391,-225.002301238227,
1.38741669750805));
#75951=CARTESIAN_POINT('Ctrl Pts',(-162.519287649641,-225.202183034029,
1.40005438763214));
#75952=CARTESIAN_POINT('Ctrl Pts',(-162.497484432032,-225.401670902235,
1.41269207775623));
#75953=CARTESIAN_POINT('Ctrl Pts',(-162.450527033305,-225.595050645471,
1.42532976788032));
#75954=CARTESIAN_POINT('Ctrl Pts',(-162.253896786651,-226.404812421914,
1.47824905629092));
#75955=CARTESIAN_POINT('Ctrl Pts',(-161.616201363122,-227.107471478212,
1.53116834470152));
#75956=CARTESIAN_POINT('Ctrl Pts',(-160.829251654008,-227.38149242425,1.58408763311212));
#75957=CARTESIAN_POINT('Ctrl Pts',(-160.042301944894,-227.655513370288,
1.63700692152271));
#75958=CARTESIAN_POINT('Ctrl Pts',(-159.106097950194,-227.500896206066,
1.68992620993331));
#75959=CARTESIAN_POINT('Ctrl Pts',(-158.449045887184,-226.988393077726,
1.74284549834391));
#75960=CARTESIAN_POINT('Ctrl Pts',(-157.791993824173,-226.475889949387,
1.79576478675451));
#75961=CARTESIAN_POINT('Ctrl Pts',(-157.414093692852,-225.605500856929,
1.84868407516511));
#75962=CARTESIAN_POINT('Ctrl Pts',(-157.488272929152,-224.775516152508,
1.9016033635757));
#75963=CARTESIAN_POINT('Ctrl Pts',(-157.562452165452,-223.945531448086,
1.9545226519863));
#75964=CARTESIAN_POINT('Ctrl Pts',(-158.088710769374,-223.155951131701,
2.0074419403969));
#75965=CARTESIAN_POINT('Ctrl Pts',(-158.82623264868,-222.76808698612,2.0603612288075));
#75966=CARTESIAN_POINT('Ctrl Pts',(-159.563754527987,-222.380222840538,
2.11328051721809));
#75967=CARTESIAN_POINT('Ctrl Pts',(-160.512539682677,-222.394074865762,
2.16619980562869));
#75968=CARTESIAN_POINT('Ctrl Pts',(-161.238424124346,-222.80330444977,2.21911909403929));
#75969=CARTESIAN_POINT('Ctrl Pts',(-161.964308566014,-223.212534033777,
2.27203838244988));
#75970=CARTESIAN_POINT('Ctrl Pts',(-162.46729229466,-224.01714117657,2.32495767086048));
#75971=CARTESIAN_POINT('Ctrl Pts',(-162.517209927523,-224.848937629546,
2.37787695927108));
#75972=CARTESIAN_POINT('Ctrl Pts',(-162.520209471201,-224.898920163742,
2.38105687201674));
#75973=CARTESIAN_POINT('Ctrl Pts',(-162.521573087656,-224.949000872869,
2.3842367847624));
#75974=CARTESIAN_POINT('Ctrl Pts',(-162.521340804038,-224.999094471355,
2.38741669750805));
#75975=CARTESIAN_POINT('Origin',(-160.,-225.,10.));
#75976=CARTESIAN_POINT('',(-162.514784019862,-224.998273763422,3.38741669750805));
#75977=CARTESIAN_POINT('',(-162.514230471617,-225.001366316902,3.11258330249194));
#75978=CARTESIAN_POINT('',(-162.5175,-225.,10.));
#75979=CARTESIAN_POINT('Ctrl Pts',(-162.514230471617,-225.001366316902,
3.11258330249194));
#75980=CARTESIAN_POINT('Ctrl Pts',(-162.511723114375,-224.492626501964,
3.08052201479597));
#75981=CARTESIAN_POINT('Ctrl Pts',(-162.361947363371,-223.982529300918,
3.04846072709999));
#75982=CARTESIAN_POINT('Ctrl Pts',(-162.07507999883,-223.567097789939,3.01639943940401));
#75983=CARTESIAN_POINT('Ctrl Pts',(-161.601586328093,-222.881400442009,
2.96348015099342));
#75984=CARTESIAN_POINT('Ctrl Pts',(-160.754604395574,-222.453607448118,
2.91056086258282));
#75985=CARTESIAN_POINT('Ctrl Pts',(-159.921713114309,-222.479476861939,
2.85764157417222));
#75986=CARTESIAN_POINT('Ctrl Pts',(-159.088821833043,-222.50534627576,2.80472228576163));
#75987=CARTESIAN_POINT('Ctrl Pts',(-158.27002120303,-222.984878097294,2.75180299735103));
#75988=CARTESIAN_POINT('Ctrl Pts',(-157.839994381929,-223.698638599168,
2.69888370894043));
#75989=CARTESIAN_POINT('Ctrl Pts',(-157.409967560828,-224.412399101043,
2.64596442052983));
#75990=CARTESIAN_POINT('Ctrl Pts',(-157.368714548639,-225.360388283258,
2.59304513211923));
#75991=CARTESIAN_POINT('Ctrl Pts',(-157.735112711589,-226.108806263348,
2.54012584370864));
#75992=CARTESIAN_POINT('Ctrl Pts',(-158.101510874539,-226.857224243439,
2.48720655529804));
#75993=CARTESIAN_POINT('Ctrl Pts',(-158.875560212628,-227.406071021405,
2.43428726688744));
#75994=CARTESIAN_POINT('Ctrl Pts',(-159.703055787496,-227.504194428938,
2.38136797847685));
#75995=CARTESIAN_POINT('Ctrl Pts',(-160.530551362364,-227.602317836471,
2.32844869006625));
#75996=CARTESIAN_POINT('Ctrl Pts',(-161.411493174011,-227.249717873572,
2.27552940165565));
#75997=CARTESIAN_POINT('Ctrl Pts',(-161.942762217923,-226.607744055342,
2.22261011324505));
#75998=CARTESIAN_POINT('Ctrl Pts',(-162.310957132034,-226.162825425934,
2.18593450966068));
#75999=CARTESIAN_POINT('Ctrl Pts',(-162.511198816508,-225.578916065593,
2.14925890607631));
#76000=CARTESIAN_POINT('Ctrl Pts',(-162.515825357218,-224.997885174742,
2.11258330249194));
#76001=CARTESIAN_POINT('Ctrl Pts',(-162.521340804038,-224.999094471355,
2.38741669750805));
#76002=CARTESIAN_POINT('Ctrl Pts',(-162.517707483559,-225.782645629135,
2.43715607317299));
#76003=CARTESIAN_POINT('Ctrl Pts',(-162.123614705335,-226.569350350335,
2.48689544883793));
#76004=CARTESIAN_POINT('Ctrl Pts',(-161.492245285988,-227.032823067984,
2.53663482450287));
#76005=CARTESIAN_POINT('Ctrl Pts',(-160.820511474508,-227.525926290286,
2.58955411291347));
#76006=CARTESIAN_POINT('Ctrl Pts',(-159.880192314467,-227.65314697173,2.64247340132407));
#76007=CARTESIAN_POINT('Ctrl Pts',(-159.101577826087,-227.356268922656,
2.69539268973466));
#76008=CARTESIAN_POINT('Ctrl Pts',(-158.322963337707,-227.059390873582,
2.74831197814526));
#76009=CARTESIAN_POINT('Ctrl Pts',(-157.706053520989,-226.33841409399,2.80123126655585));
#76010=CARTESIAN_POINT('Ctrl Pts',(-157.533146300234,-225.523257548061,
2.85415055496645));
#76011=CARTESIAN_POINT('Ctrl Pts',(-157.360239079479,-224.708101002132,
2.90706984337705));
#76012=CARTESIAN_POINT('Ctrl Pts',(-157.631334454686,-223.798764689866,
2.95998913178765));
#76013=CARTESIAN_POINT('Ctrl Pts',(-158.222379185418,-223.211360887942,
3.01290842019825));
#76014=CARTESIAN_POINT('Ctrl Pts',(-158.813423916151,-222.623957086017,
3.06582770860885));
#76015=CARTESIAN_POINT('Ctrl Pts',(-159.724418002409,-222.358485794434,
3.11874699701945));
#76016=CARTESIAN_POINT('Ctrl Pts',(-160.538490569232,-222.536426671933,
3.17166628543004));
#76017=CARTESIAN_POINT('Ctrl Pts',(-161.352563136055,-222.714367549433,
3.22458557384064));
#76018=CARTESIAN_POINT('Ctrl Pts',(-162.069714183442,-223.335720596015,
3.27750486225124));
#76019=CARTESIAN_POINT('Ctrl Pts',(-162.361775405729,-224.116154669331,
3.33042415066184));
#76020=CARTESIAN_POINT('Ctrl Pts',(-162.466622575781,-224.396322996229,
3.34942166627724));
#76021=CARTESIAN_POINT('Ctrl Pts',(-162.516686679289,-224.696992746495,
3.36841918189265));
#76022=CARTESIAN_POINT('Ctrl Pts',(-162.514784019862,-224.998273763422,
3.38741669750805));
#76023=CARTESIAN_POINT('Origin',(-160.,-225.,10.));
#76024=CARTESIAN_POINT('',(-162.51509551549,-225.001872886185,4.38741669750805));
#76025=CARTESIAN_POINT('',(-162.520804175319,-225.001369558332,4.11258330249194));
#76026=CARTESIAN_POINT('',(-162.5175,-225.,10.));
#76027=CARTESIAN_POINT('Ctrl Pts',(-162.520804175319,-225.001369558332,
4.11258330249194));
#76028=CARTESIAN_POINT('Ctrl Pts',(-162.515852849758,-224.246701725063,
4.06470441192622));
#76029=CARTESIAN_POINT('Ctrl Pts',(-162.1543399445,-223.487919611795,4.01682552136049));
#76030=CARTESIAN_POINT('Ctrl Pts',(-161.562602878045,-223.020748124231,
3.96894663079477));
#76031=CARTESIAN_POINT('Ctrl Pts',(-160.908571339031,-222.504395669202,
3.91602734238417));
#76032=CARTESIAN_POINT('Ctrl Pts',(-159.973290963993,-222.34428362189,3.86310805397358));
#76033=CARTESIAN_POINT('Ctrl Pts',(-159.184746034126,-222.613679251846,
3.81018876556298));
#76034=CARTESIAN_POINT('Ctrl Pts',(-158.396201104259,-222.883074881802,
3.75726947715238));
#76035=CARTESIAN_POINT('Ctrl Pts',(-157.754391619563,-223.581978189027,
3.70435018874178));
#76036=CARTESIAN_POINT('Ctrl Pts',(-157.553009587684,-224.390571034187,
3.65143090033118));
#76037=CARTESIAN_POINT('Ctrl Pts',(-157.351627555805,-225.199163879346,
3.59851161192058));
#76038=CARTESIAN_POINT('Ctrl Pts',(-157.590672976743,-226.11744626244,3.54559232350999));
#76039=CARTESIAN_POINT('Ctrl Pts',(-158.160758670434,-226.725212182376,
3.49267303509939));
#76040=CARTESIAN_POINT('Ctrl Pts',(-158.730844364126,-227.332978102313,
3.4397537466888));
#76041=CARTESIAN_POINT('Ctrl Pts',(-159.631970330572,-227.630227559093,
3.3868344582782));
#76042=CARTESIAN_POINT('Ctrl Pts',(-160.451781345539,-227.480939208471,
3.3339151698676));
#76043=CARTESIAN_POINT('Ctrl Pts',(-161.271592360505,-227.33165085785,3.280995881457));
#76044=CARTESIAN_POINT('Ctrl Pts',(-162.010088423993,-226.735824699828,
3.2280765930464));
#76045=CARTESIAN_POINT('Ctrl Pts',(-162.329333751259,-225.966110769833,
3.17515730463581));
#76046=CARTESIAN_POINT('Ctrl Pts',(-162.455163471654,-225.662730014269,
3.15429930392119));
#76047=CARTESIAN_POINT('Ctrl Pts',(-162.51586167432,-225.33233541347,3.13344130320656));
#76048=CARTESIAN_POINT('Ctrl Pts',(-162.514230471617,-225.001366316902,
3.11258330249194));
#76049=CARTESIAN_POINT('Ctrl Pts',(-162.514784019862,-224.998273763422,
3.38741669750805));
#76050=CARTESIAN_POINT('Ctrl Pts',(-162.511386650326,-225.536238116795,
3.42133847030324));
#76051=CARTESIAN_POINT('Ctrl Pts',(-162.342302016743,-226.076151390884,
3.45526024309843));
#76052=CARTESIAN_POINT('Ctrl Pts',(-162.023563483551,-226.50477787839,3.48918201589362));
#76053=CARTESIAN_POINT('Ctrl Pts',(-161.526318941901,-227.173451914081,
3.54210130430422));
#76054=CARTESIAN_POINT('Ctrl Pts',(-160.664858461414,-227.571284885413,
3.59502059271482));
#76055=CARTESIAN_POINT('Ctrl Pts',(-159.833386340911,-227.516228432422,
3.64793988112542));
#76056=CARTESIAN_POINT('Ctrl Pts',(-159.001914220409,-227.46117197943,3.70085916953602));
#76057=CARTESIAN_POINT('Ctrl Pts',(-158.20043045989,-226.953226102116,3.75377845794661));
#76058=CARTESIAN_POINT('Ctrl Pts',(-157.795694012465,-226.224826824,3.80669774635721));
#76059=CARTESIAN_POINT('Ctrl Pts',(-157.390957565039,-225.496427545885,
3.85961703476781));
#76060=CARTESIAN_POINT('Ctrl Pts',(-157.382968430706,-224.547574866968,
3.91253632317841));
#76061=CARTESIAN_POINT('Ctrl Pts',(-157.775382437154,-223.812463754443,
3.965455611589));
#76062=CARTESIAN_POINT('Ctrl Pts',(-158.167796443601,-223.077352641917,
4.0183748999996));
#76063=CARTESIAN_POINT('Ctrl Pts',(-158.960613590829,-222.555983095782,
4.0712941884102));
#76064=CARTESIAN_POINT('Ctrl Pts',(-159.791040767866,-222.486933810109,
4.1242134768208));
#76065=CARTESIAN_POINT('Ctrl Pts',(-160.621467944904,-222.417884524436,
4.17713276523139));
#76066=CARTESIAN_POINT('Ctrl Pts',(-161.489505151751,-222.801155499226,
4.23005205364199));
#76067=CARTESIAN_POINT('Ctrl Pts',(-161.997938579617,-223.461361943945,
4.28297134205259));
#76068=CARTESIAN_POINT('Ctrl Pts',(-162.332432307038,-223.895705758609,
4.31778646053774));
#76069=CARTESIAN_POINT('Ctrl Pts',(-162.511282168108,-224.449912905609,
4.3526015790229));
#76070=CARTESIAN_POINT('Ctrl Pts',(-162.51509551549,-225.001872886185,4.38741669750805));
#76071=CARTESIAN_POINT('Origin',(-160.,-225.,10.));
#76072=CARTESIAN_POINT('',(-162.521526441259,-225.000661269066,5.38741669750805));
#76073=CARTESIAN_POINT('',(-162.518352881918,-224.997761948101,5.11258330249194));
#76074=CARTESIAN_POINT('',(-162.5175,-225.,10.));
#76075=CARTESIAN_POINT('Ctrl Pts',(-162.518352881918,-224.997761948101,
5.11258330249194));
#76076=CARTESIAN_POINT('Ctrl Pts',(-162.519921717053,-224.827461151217,
5.10180609746706));
#76077=CARTESIAN_POINT('Ctrl Pts',(-162.504121449384,-224.657449769252,
5.09102889244219));
#76078=CARTESIAN_POINT('Ctrl Pts',(-162.469883644643,-224.491236278736,
5.08025168741731));
#76079=CARTESIAN_POINT('Ctrl Pts',(-162.301765820079,-223.675078506653,
5.02733239900672));
#76080=CARTESIAN_POINT('Ctrl Pts',(-161.689100049289,-222.950491796184,
4.97441311059612));
#76081=CARTESIAN_POINT('Ctrl Pts',(-160.91224217694,-222.649047011793,4.92149382218553));
#76082=CARTESIAN_POINT('Ctrl Pts',(-160.135384304591,-222.347602227401,
4.86857453377493));
#76083=CARTESIAN_POINT('Ctrl Pts',(-159.194334330684,-222.469299369089,
4.81565524536433));
#76084=CARTESIAN_POINT('Ctrl Pts',(-158.519716704775,-222.958449827209,
4.76273595695373));
#76085=CARTESIAN_POINT('Ctrl Pts',(-157.845099078866,-223.447600285329,
4.70981666854313));
#76086=CARTESIAN_POINT('Ctrl Pts',(-157.436913800955,-224.304204059882,
4.65689738013254));
#76087=CARTESIAN_POINT('Ctrl Pts',(-157.481946446189,-225.13627928048,4.60397809172194));
#76088=CARTESIAN_POINT('Ctrl Pts',(-157.526979091423,-225.968354501077,
4.55105880331134));
#76089=CARTESIAN_POINT('Ctrl Pts',(-158.025229659802,-226.775901167718,
4.49813951490074));
#76090=CARTESIAN_POINT('Ctrl Pts',(-158.748698701031,-227.189385941618,
4.44522022649015));
#76091=CARTESIAN_POINT('Ctrl Pts',(-159.472167742261,-227.602870715519,
4.39230093807955));
#76092=CARTESIAN_POINT('Ctrl Pts',(-160.420855256339,-227.622293596678,
4.33938164966895));
#76093=CARTESIAN_POINT('Ctrl Pts',(-161.160641855482,-227.238766675076,
4.28646236125836));
#76094=CARTESIAN_POINT('Ctrl Pts',(-161.900428454625,-226.855239753474,
4.23354307284776));
#76095=CARTESIAN_POINT('Ctrl Pts',(-162.431314138832,-226.068763029111,
4.18062378443716));
#76096=CARTESIAN_POINT('Ctrl Pts',(-162.51036562944,-225.239228235557,4.12770449602656));
#76097=CARTESIAN_POINT('Ctrl Pts',(-162.517895038374,-225.160217623146,
4.12266409818169));
#76098=CARTESIAN_POINT('Ctrl Pts',(-162.521325420703,-225.08081638919,4.11762370033682));
#76099=CARTESIAN_POINT('Ctrl Pts',(-162.520804175319,-225.001369558332,
4.11258330249194));
#76100=CARTESIAN_POINT('Ctrl Pts',(-162.51509551549,-225.001872886185,4.38741669750805));
#76101=CARTESIAN_POINT('Ctrl Pts',(-162.517078489899,-225.288896964092,
4.4055208674335));
#76102=CARTESIAN_POINT('Ctrl Pts',(-162.471729978915,-225.575313387501,
4.42362503735894));
#76103=CARTESIAN_POINT('Ctrl Pts',(-162.376323081866,-225.843951566175,
4.44172920728438));
#76104=CARTESIAN_POINT('Ctrl Pts',(-162.097444507367,-226.629192829037,
4.49464849569498));
#76105=CARTESIAN_POINT('Ctrl Pts',(-161.390857709486,-227.262533440115,
4.54756778410558));
#76106=CARTESIAN_POINT('Ctrl Pts',(-160.57989679304,-227.45415674823,4.60048707251617));
#76107=CARTESIAN_POINT('Ctrl Pts',(-159.768935876593,-227.645780056345,
4.65340636092677));
#76108=CARTESIAN_POINT('Ctrl Pts',(-158.85360084158,-227.395686061497,4.70632564933737));
#76109=CARTESIAN_POINT('Ctrl Pts',(-158.252748982027,-226.818317770812,
4.75924493774797));
#76110=CARTESIAN_POINT('Ctrl Pts',(-157.651897122473,-226.240949480127,
4.81216422615857));
#76111=CARTESIAN_POINT('Ctrl Pts',(-157.365528438379,-225.336306893605,
4.86508351456916));
#76112=CARTESIAN_POINT('Ctrl Pts',(-157.524685233954,-224.518354441051,
4.91800280297976));
#76113=CARTESIAN_POINT('Ctrl Pts',(-157.68384202953,-223.700401988497,4.97092209139036));
#76114=CARTESIAN_POINT('Ctrl Pts',(-158.288524304775,-222.96913966991,5.02384137980096));
#76115=CARTESIAN_POINT('Ctrl Pts',(-159.062029462427,-222.659193107899,
5.07676066821155));
#76116=CARTESIAN_POINT('Ctrl Pts',(-159.83553462008,-222.349246545888,5.12967995662215));
#76117=CARTESIAN_POINT('Ctrl Pts',(-160.777862660139,-222.460615740452,
5.18259924503275));
#76118=CARTESIAN_POINT('Ctrl Pts',(-161.457804290002,-222.942338150349,
5.23551853344334));
#76119=CARTESIAN_POINT('Ctrl Pts',(-162.108366610783,-223.403246021245,
5.28615125479825));
#76120=CARTESIAN_POINT('Ctrl Pts',(-162.518727336833,-224.20319368033,5.33678397615315));
#76121=CARTESIAN_POINT('Ctrl Pts',(-162.521526441259,-225.000661269066,
5.38741669750805));
#76122=CARTESIAN_POINT('Origin',(-160.,-225.,10.));
#76123=CARTESIAN_POINT('',(-162.517037225954,-224.997707731385,6.38741669750805));
#76124=CARTESIAN_POINT('',(-162.51348275222,-225.000035219869,6.11258330249194));
#76125=CARTESIAN_POINT('',(-162.5175,-225.,10.));
#76126=CARTESIAN_POINT('Ctrl Pts',(-162.51348275222,-225.000035219869,6.11258330249194));
#76127=CARTESIAN_POINT('Ctrl Pts',(-162.513430051157,-224.577722205729,
6.08598849459732));
#76128=CARTESIAN_POINT('Ctrl Pts',(-162.412708967235,-224.155385572425,
6.0593936867027));
#76129=CARTESIAN_POINT('Ctrl Pts',(-162.211459914146,-223.788137470555,
6.03279887880807));
#76130=CARTESIAN_POINT('Ctrl Pts',(-161.811007437671,-223.057374221649,
5.97987959039747));
#76131=CARTESIAN_POINT('Ctrl Pts',(-161.012520031443,-222.544730963836,
5.92696030198687));
#76132=CARTESIAN_POINT('Ctrl Pts',(-160.181385516851,-222.484793241814,
5.87404101357628));
#76133=CARTESIAN_POINT('Ctrl Pts',(-159.350251002259,-222.424855519791,
5.82112172516568));
#76134=CARTESIAN_POINT('Ctrl Pts',(-158.486469379304,-222.817623333558,
5.76820243675509));
#76135=CARTESIAN_POINT('Ctrl Pts',(-157.985307101667,-223.483366139257,
5.71528314834449));
#76136=CARTESIAN_POINT('Ctrl Pts',(-157.484144824029,-224.149108944956,
5.66236385993389));
#76137=CARTESIAN_POINT('Ctrl Pts',(-157.345601891708,-225.087826742587,
5.60944457152329));
#76138=CARTESIAN_POINT('Ctrl Pts',(-157.633075547811,-225.869962286412,
5.55652528311269));
#76139=CARTESIAN_POINT('Ctrl Pts',(-157.920549203914,-226.652097830236,
5.50360599470209));
#76140=CARTESIAN_POINT('Ctrl Pts',(-158.634039448439,-227.277651120254,
5.4506867062915));
#76141=CARTESIAN_POINT('Ctrl Pts',(-159.447053159522,-227.460368983253,
5.3977674178809));
#76142=CARTESIAN_POINT('Ctrl Pts',(-160.260066870604,-227.643086846252,
5.34484812947031));
#76143=CARTESIAN_POINT('Ctrl Pts',(-161.172604048244,-227.382969282231,
5.29192884105971));
#76144=CARTESIAN_POINT('Ctrl Pts',(-161.767087697894,-226.799046083373,
5.23900955264911));
#76145=CARTESIAN_POINT('Ctrl Pts',(-162.240502596081,-226.334040961871,
5.19686746926339));
#76146=CARTESIAN_POINT('Ctrl Pts',(-162.512218269011,-225.663688815629,
5.15472538587766));
#76147=CARTESIAN_POINT('Ctrl Pts',(-162.518352881918,-224.997761948101,
5.11258330249194));
#76148=CARTESIAN_POINT('Ctrl Pts',(-162.521526441259,-225.000661269066,
5.38741669750805));
#76149=CARTESIAN_POINT('Ctrl Pts',(-162.521652848448,-225.036674800782,
5.38970326456375));
#76150=CARTESIAN_POINT('Ctrl Pts',(-162.52094806886,-225.072683274608,5.39198983161944));
#76151=CARTESIAN_POINT('Ctrl Pts',(-162.519396688694,-225.108655236683,
5.39427639867514));
#76152=CARTESIAN_POINT('Ctrl Pts',(-162.483492237855,-225.941174287893,
5.44719568708573));
#76153=CARTESIAN_POINT('Ctrl Pts',(-161.994128116511,-226.754136765084,
5.50011497549633));
#76154=CARTESIAN_POINT('Ctrl Pts',(-161.275237336966,-227.175531054678,
5.55303426390693));
#76155=CARTESIAN_POINT('Ctrl Pts',(-160.556346557421,-227.596925344272,
5.60595355231753));
#76156=CARTESIAN_POINT('Ctrl Pts',(-159.607929119675,-227.626751446269,
5.65887284072812));
#76157=CARTESIAN_POINT('Ctrl Pts',(-158.863980824594,-227.251360936982,
5.71179212913872));
#76158=CARTESIAN_POINT('Ctrl Pts',(-158.120032529513,-226.875970427695,
5.76471141754932));
#76159=CARTESIAN_POINT('Ctrl Pts',(-157.580553377096,-226.095363307124,
5.81763070595992));
#76160=CARTESIAN_POINT('Ctrl Pts',(-157.492409016881,-225.266745378293,
5.87054999437051));
#76161=CARTESIAN_POINT('Ctrl Pts',(-157.404264656667,-224.438127449462,
5.92346928278111));
#76162=CARTESIAN_POINT('Ctrl Pts',(-157.767455088655,-223.561498712372,
5.97638857119171));
#76163=CARTESIAN_POINT('Ctrl Pts',(-158.41578437831,-223.038004459879,6.02930785960231));
#76164=CARTESIAN_POINT('Ctrl Pts',(-159.064113667964,-222.514510207386,
6.0822271480129));
#76165=CARTESIAN_POINT('Ctrl Pts',(-159.997581815285,-222.34415043949,6.1351464364235));
#76166=CARTESIAN_POINT('Ctrl Pts',(-160.789033814412,-222.604881782631,
6.1880657248341));
#76167=CARTESIAN_POINT('Ctrl Pts',(-161.580485813538,-222.865613125771,
6.24098501324469));
#76168=CARTESIAN_POINT('Ctrl Pts',(-162.229921664471,-223.557435579948,
6.29390430165529));
#76169=CARTESIAN_POINT('Ctrl Pts',(-162.440159534592,-224.363771203733,
6.34682359006589));
#76170=CARTESIAN_POINT('Ctrl Pts',(-162.493915664644,-224.569944728194,
6.36035462587995));
#76171=CARTESIAN_POINT('Ctrl Pts',(-162.518957746143,-224.783604937147,
6.373885661694));
#76172=CARTESIAN_POINT('Ctrl Pts',(-162.517037225954,-224.997707731385,
6.38741669750805));
#76173=CARTESIAN_POINT('Origin',(-160.,-225.,10.));
#76174=CARTESIAN_POINT('',(-162.513684989213,-225.000739875368,7.38741669750805));
#76175=CARTESIAN_POINT('',(-162.518482140773,-225.002219575106,7.11258330249195));
#76176=CARTESIAN_POINT('',(-162.5175,-225.,10.));
#76177=CARTESIAN_POINT('Ctrl Pts',(-162.518482140773,-225.002219575106,
7.11258330249195));
#76178=CARTESIAN_POINT('Ctrl Pts',(-162.512325260313,-224.332109506928,
7.07017089172757));
#76179=CARTESIAN_POINT('Ctrl Pts',(-162.236727822943,-223.657527150712,
7.0277584809632));
#76180=CARTESIAN_POINT('Ctrl Pts',(-161.757897665573,-223.191973025776,
6.98534607019882));
#76181=CARTESIAN_POINT('Ctrl Pts',(-161.160446336095,-222.61108661625,6.93242678178823));
#76182=CARTESIAN_POINT('Ctrl Pts',(-160.246595568692,-222.355622288795,
6.87950749337763));
#76183=CARTESIAN_POINT('Ctrl Pts',(-159.434523456559,-222.542480514631,
6.82658820496703));
#76184=CARTESIAN_POINT('Ctrl Pts',(-158.622451344426,-222.729338740468,
6.77366891655644));
#76185=CARTESIAN_POINT('Ctrl Pts',(-157.912157887563,-223.358519519595,
6.72074962814584));
#76186=CARTESIAN_POINT('Ctrl Pts',(-157.628673357865,-224.142109739857,
6.66783033973524));
#76187=CARTESIAN_POINT('Ctrl Pts',(-157.345188828167,-224.925699960118,
6.61491105132465));
#76188=CARTESIAN_POINT('Ctrl Pts',(-157.488513225634,-225.863699621512,
6.56199176291405));
#76189=CARTESIAN_POINT('Ctrl Pts',(-157.993061308803,-226.526880097429,
6.50907247450345));
#76190=CARTESIAN_POINT('Ctrl Pts',(-158.497609391972,-227.190060573346,
6.45615318609285));
#76191=CARTESIAN_POINT('Ctrl Pts',(-159.363381160843,-227.578421863785,
6.40323389768225));
#76192=CARTESIAN_POINT('Ctrl Pts',(-160.194199471004,-227.514249849878,
6.35031460927165));
#76193=CARTESIAN_POINT('Ctrl Pts',(-161.025017781164,-227.45007783597,6.29739532086106));
#76194=CARTESIAN_POINT('Ctrl Pts',(-161.820882632614,-226.933372517716,
6.24447603245046));
#76195=CARTESIAN_POINT('Ctrl Pts',(-162.217606284979,-226.200578238589,
6.19155674403986));
#76196=CARTESIAN_POINT('Ctrl Pts',(-162.414954820277,-225.836052763994,
6.16523226352389));
#76197=CARTESIAN_POINT('Ctrl Pts',(-162.513534917594,-225.418055562652,
6.13890778300792));
#76198=CARTESIAN_POINT('Ctrl Pts',(-162.51348275222,-225.000035219869,6.11258330249194));
#76199=CARTESIAN_POINT('Ctrl Pts',(-162.517037225954,-224.997707731385,
6.38741669750805));
#76200=CARTESIAN_POINT('Ctrl Pts',(-162.511446675805,-225.620951587728,
6.4268049501046));
#76201=CARTESIAN_POINT('Ctrl Pts',(-162.277384044503,-226.247945763943,
6.46619320270114));
#76202=CARTESIAN_POINT('Ctrl Pts',(-161.85805134467,-226.704937194159,6.50558145529768));
#76203=CARTESIAN_POINT('Ctrl Pts',(-161.294665395319,-227.318918767409,
6.55850074370828));
#76204=CARTESIAN_POINT('Ctrl Pts',(-160.396853607305,-227.626033120516,
6.61142003211888));
#76205=CARTESIAN_POINT('Ctrl Pts',(-159.575454637173,-227.485744731537,
6.66433932052947));
#76206=CARTESIAN_POINT('Ctrl Pts',(-158.75405566704,-227.345456342557,6.71725860894007));
#76207=CARTESIAN_POINT('Ctrl Pts',(-158.009069514788,-226.757765211492,
6.77017789735067));
#76208=CARTESIAN_POINT('Ctrl Pts',(-157.68140182904,-225.991598788361,6.82309718576127));
#76209=CARTESIAN_POINT('Ctrl Pts',(-157.353734143291,-225.22543236523,6.87601647417187));
#76210=CARTESIAN_POINT('Ctrl Pts',(-157.443384924046,-224.280790650033,
6.92893576258246));
#76211=CARTESIAN_POINT('Ctrl Pts',(-157.909329975793,-223.589941673071,
6.98185505099306));
#76212=CARTESIAN_POINT('Ctrl Pts',(-158.37527502754,-222.899092696109,7.03477433940366));
#76213=CARTESIAN_POINT('Ctrl Pts',(-159.21751435028,-222.462036457382,7.08769362781425));
#76214=CARTESIAN_POINT('Ctrl Pts',(-160.050639246487,-222.478769883137,
7.14061291622485));
#76215=CARTESIAN_POINT('Ctrl Pts',(-160.883764142694,-222.495503308893,
7.19353220463545));
#76216=CARTESIAN_POINT('Ctrl Pts',(-161.707774612368,-222.966026399131,
7.24645149304605));
#76217=CARTESIAN_POINT('Ctrl Pts',(-162.145603480787,-223.675027797011,
7.29937078145664));
#76218=CARTESIAN_POINT('Ctrl Pts',(-162.388420072819,-224.068234630997,
7.32871942014045));
#76219=CARTESIAN_POINT('Ctrl Pts',(-162.512457706949,-224.534790906726,
7.35806805882425));
#76220=CARTESIAN_POINT('Ctrl Pts',(-162.513684989213,-225.000739875368,
7.38741669750805));
#76221=CARTESIAN_POINT('Origin',(-160.,-225.,10.));
#76222=CARTESIAN_POINT('',(-162.519748038511,-225.001899953564,8.38741669750805));
#76223=CARTESIAN_POINT('',(-162.520711665558,-224.998569117271,8.11258330249194));
#76224=CARTESIAN_POINT('',(-162.5175,-225.,10.));
#76225=CARTESIAN_POINT('Ctrl Pts',(-162.520711665558,-224.998569117271,
8.11258330249194));
#76226=CARTESIAN_POINT('Ctrl Pts',(-162.521280452263,-224.914853289316,
8.10727257726842));
#76227=CARTESIAN_POINT('Ctrl Pts',(-162.517471362285,-224.831189846111,
8.1019618520449));
#76228=CARTESIAN_POINT('Ctrl Pts',(-162.509114044729,-224.747983229342,
8.09665112682137));
#76229=CARTESIAN_POINT('Ctrl Pts',(-162.425836661799,-223.918862014224,
8.04373183841077));
#76230=CARTESIAN_POINT('Ctrl Pts',(-161.89095035476,-223.135100643507,7.99081255000018));
#76231=CARTESIAN_POINT('Ctrl Pts',(-161.149219087196,-222.755348305021,
7.93789326158958));
#76232=CARTESIAN_POINT('Ctrl Pts',(-160.407487819633,-222.375595966535,
7.88497397317898));
#76233=CARTESIAN_POINT('Ctrl Pts',(-159.458911591544,-222.39985266028,7.83205468476838));
#76234=CARTESIAN_POINT('Ctrl Pts',(-158.737558866254,-222.817018523676,
7.77913539635778));
#76235=CARTESIAN_POINT('Ctrl Pts',(-158.016206140963,-223.234184387072,
7.72621610794719));
#76236=CARTESIAN_POINT('Ctrl Pts',(-157.52207691847,-224.044259420117,7.67329681953659));
#76237=CARTESIAN_POINT('Ctrl Pts',(-157.481284721271,-224.876553303619,
7.620377531126));
#76238=CARTESIAN_POINT('Ctrl Pts',(-157.440492524073,-225.708847187121,
7.5674582427154));
#76239=CARTESIAN_POINT('Ctrl Pts',(-157.85303735217,-226.563359921079,7.5145389543048));
#76240=CARTESIAN_POINT('Ctrl Pts',(-158.530138700335,-227.049066495236,
7.4616196658942));
#76241=CARTESIAN_POINT('Ctrl Pts',(-159.207240048501,-227.534773069392,
7.40870037748361));
#76242=CARTESIAN_POINT('Ctrl Pts',(-160.148897916737,-227.651673483747,
7.35578108907301));
#76243=CARTESIAN_POINT('Ctrl Pts',(-160.924209683052,-227.34627411099,7.30286180066241));
#76244=CARTESIAN_POINT('Ctrl Pts',(-161.699521449367,-227.040874738233,
7.24994251225181));
#76245=CARTESIAN_POINT('Ctrl Pts',(-162.308487113762,-226.313175578364,
7.19702322384122));
#76246=CARTESIAN_POINT('Ctrl Pts',(-162.472444000183,-225.496171752631,
7.14410393543062));
#76247=CARTESIAN_POINT('Ctrl Pts',(-162.504996874505,-225.333959457431,
7.13359705778439));
#76248=CARTESIAN_POINT('Ctrl Pts',(-162.520007392191,-225.168226750104,
7.12309018013817));
#76249=CARTESIAN_POINT('Ctrl Pts',(-162.518482140773,-225.002219575106,
7.11258330249195));
#76250=CARTESIAN_POINT('Ctrl Pts',(-162.513684989213,-225.000739875368,
7.38741669750805));
#76251=CARTESIAN_POINT('Ctrl Pts',(-162.514670651298,-225.374955526348,
7.41098734723485));
#76252=CARTESIAN_POINT('Ctrl Pts',(-162.436442273887,-225.748779457519,
7.43455799696164));
#76253=CARTESIAN_POINT('Ctrl Pts',(-162.276911493845,-226.083900218957,
7.45812864668843));
#76254=CARTESIAN_POINT('Ctrl Pts',(-161.918743371317,-226.836291537502,
7.51104793509903));
#76255=CARTESIAN_POINT('Ctrl Pts',(-161.150759859096,-227.393594469072,
7.56396722350963));
#76256=CARTESIAN_POINT('Ctrl Pts',(-160.324390197273,-227.500787203137,
7.61688651192023));
#76257=CARTESIAN_POINT('Ctrl Pts',(-159.498020535451,-227.607979937202,
7.66980580033083));
#76258=CARTESIAN_POINT('Ctrl Pts',(-158.613264724027,-227.265062473763,
7.72272508874142));
#76259=CARTESIAN_POINT('Ctrl Pts',(-158.074987004913,-226.628953837347,
7.77564437715202));
#76260=CARTESIAN_POINT('Ctrl Pts',(-157.5367092858,-225.992845200931,7.82856366556262));
#76261=CARTESIAN_POINT('Ctrl Pts',(-157.344909658996,-225.063545391538,
7.88148295397322));
#76262=CARTESIAN_POINT('Ctrl Pts',(-157.587355629957,-224.266301983674,
7.93440224238382));
#76263=CARTESIAN_POINT('Ctrl Pts',(-157.829801600918,-223.46905857581,7.98732153079441));
#76264=CARTESIAN_POINT('Ctrl Pts',(-158.506493169644,-222.803871569476,
8.040240819205));
#76265=CARTESIAN_POINT('Ctrl Pts',(-159.30777628759,-222.575130525691,8.0931601076156));
#76266=CARTESIAN_POINT('Ctrl Pts',(-160.109059405536,-222.346389481906,
8.1460793960262));
#76267=CARTESIAN_POINT('Ctrl Pts',(-161.034934072702,-222.554094400669,
8.1989986844368));
#76268=CARTESIAN_POINT('Ctrl Pts',(-161.661720059599,-223.10319951524,8.2519179728474));
#76269=CARTESIAN_POINT('Ctrl Pts',(-162.196677503979,-223.571856879839,
8.29708421440095));
#76270=CARTESIAN_POINT('Ctrl Pts',(-162.513763715639,-224.289207312475,
8.3422504559545));
#76271=CARTESIAN_POINT('Ctrl Pts',(-162.519748038511,-225.001899953564,
8.38741669750805));
#76272=CARTESIAN_POINT('Origin',(-160.,-225.,10.));
#76273=CARTESIAN_POINT('',(-162.519611851718,-224.998052208505,9.38741669750806));
#76274=CARTESIAN_POINT('',(-162.514161617683,-224.998691358253,9.11258330249195));
#76275=CARTESIAN_POINT('',(-162.5175,-225.,10.));
#76276=CARTESIAN_POINT('Ctrl Pts',(-162.514161617683,-224.998691358253,
9.11258330249195));
#76277=CARTESIAN_POINT('Ctrl Pts',(-162.515741631259,-224.663409791321,
9.09145497439867));
#76278=CARTESIAN_POINT('Ctrl Pts',(-162.453405451553,-224.328691798857,
9.0703266463054));
#76279=CARTESIAN_POINT('Ctrl Pts',(-162.324380665572,-224.022032585583,
9.04919831821212));
#76280=CARTESIAN_POINT('Ctrl Pts',(-162.001217383022,-223.253955372877,
8.99627902980152));
#76281=CARTESIAN_POINT('Ctrl Pts',(-161.259694857773,-222.661899976623,
8.94335974139093));
#76282=CARTESIAN_POINT('Ctrl Pts',(-160.439133782798,-222.516790934506,
8.89044045298034));
#76283=CARTESIAN_POINT('Ctrl Pts',(-159.618572707824,-222.371681892388,
8.83752116456974));
#76284=CARTESIAN_POINT('Ctrl Pts',(-158.718973083125,-222.673519204408,
8.78460187615914));
#76285=CARTESIAN_POINT('Ctrl Pts',(-158.151991679276,-223.284182122519,
8.73168258774854));
#76286=CARTESIAN_POINT('Ctrl Pts',(-157.585010275426,-223.89484504063,8.67876329933795));
#76287=CARTESIAN_POINT('Ctrl Pts',(-157.350647092427,-224.814333564833,
8.62584401092735));
#76288=CARTESIAN_POINT('Ctrl Pts',(-157.556146718209,-225.62188976453,8.57292472251675));
#76289=CARTESIAN_POINT('Ctrl Pts',(-157.761646343991,-226.429445964228,
8.52000543410615));
#76290=CARTESIAN_POINT('Ctrl Pts',(-158.407008778556,-227.125069839421,
8.46708614569556));
#76291=CARTESIAN_POINT('Ctrl Pts',(-159.196916184535,-227.390443918499,
8.41416685728496));
#76292=CARTESIAN_POINT('Ctrl Pts',(-159.986823590514,-227.655817997576,
8.36124756887436));
#76293=CARTESIAN_POINT('Ctrl Pts',(-160.921275967908,-227.490942280538,
8.30832828046376));
#76294=CARTESIAN_POINT('Ctrl Pts',(-161.572667927194,-226.971263892259,
8.25540899205316));
#76295=CARTESIAN_POINT('Ctrl Pts',(-162.158689322883,-226.503737927182,
8.20780042886609));
#76296=CARTESIAN_POINT('Ctrl Pts',(-162.515612716419,-225.749048593652,
8.16019186567902));
#76297=CARTESIAN_POINT('Ctrl Pts',(-162.520711665558,-224.998569117271,
8.11258330249194));
#76298=CARTESIAN_POINT('Ctrl Pts',(-162.519748038511,-225.001899953564,
8.38741669750805));
#76299=CARTESIAN_POINT('Ctrl Pts',(-162.520775282179,-225.12423777161,8.3951697443651));
#76300=CARTESIAN_POINT('Ctrl Pts',(-162.51263568778,-225.246438344522,8.40292279122215));
#76301=CARTESIAN_POINT('Ctrl Pts',(-162.494857698409,-225.367220233851,
8.41067583807919));
#76302=CARTESIAN_POINT('Ctrl Pts',(-162.373512043696,-226.191630527516,
8.46359512648979));
#76303=CARTESIAN_POINT('Ctrl Pts',(-161.803123427644,-226.949945804467,
8.51651441490039));
#76304=CARTESIAN_POINT('Ctrl Pts',(-161.044701669743,-227.295161008883,
8.56943370331098));
#76305=CARTESIAN_POINT('Ctrl Pts',(-160.286279911842,-227.640376213298,
8.62235299172158));
#76306=CARTESIAN_POINT('Ctrl Pts',(-159.339825012092,-227.572491345178,
8.67527228013218));
#76307=CARTESIAN_POINT('Ctrl Pts',(-158.63843471401,-227.12257051884,8.72819156854278));
#76308=CARTESIAN_POINT('Ctrl Pts',(-157.937044415928,-226.672649692501,
8.78111085695338));
#76309=CARTESIAN_POINT('Ctrl Pts',(-157.480718719513,-225.840692907943,
8.83403014536398));
#76310=CARTESIAN_POINT('Ctrl Pts',(-157.478272254473,-225.007403573423,
8.88694943377457));
#76311=CARTESIAN_POINT('Ctrl Pts',(-157.475825789433,-224.174114238902,
8.93986872218517));
#76312=CARTESIAN_POINT('Ctrl Pts',(-157.927258555767,-223.339492354418,
8.99278801059577));
#76313=CARTESIAN_POINT('Ctrl Pts',(-158.625994928478,-222.8854608779,9.04570729900636));
#76314=CARTESIAN_POINT('Ctrl Pts',(-159.324731301188,-222.431429401383,
9.09862658741696));
#76315=CARTESIAN_POINT('Ctrl Pts',(-160.270771280274,-222.357988332831,
9.15154587582756));
#76316=CARTESIAN_POINT('Ctrl Pts',(-161.031206989908,-222.698744303771,
9.20446516423815));
#76317=CARTESIAN_POINT('Ctrl Pts',(-161.791642699542,-223.039500274711,
9.25738445264875));
#76318=CARTESIAN_POINT('Ctrl Pts',(-162.366474139722,-223.794453285143,
9.31030374105935));
#76319=CARTESIAN_POINT('Ctrl Pts',(-162.492658454726,-224.618136852336,
9.36322302946995));
#76320=CARTESIAN_POINT('Ctrl Pts',(-162.51188812517,-224.743660880793,9.37128758548265));
#76321=CARTESIAN_POINT('Ctrl Pts',(-162.520698512878,-224.870781092672,
9.37935214149535));
#76322=CARTESIAN_POINT('Ctrl Pts',(-162.519611851718,-224.998052208505,
9.38741669750806));
#76323=CARTESIAN_POINT('Origin',(-160.,-225.,10.));
#76324=CARTESIAN_POINT('',(-162.513643850542,-224.999337553514,10.3874166975081));
#76325=CARTESIAN_POINT('',(-162.515939379227,-225.002142062255,10.1125833024919));
#76326=CARTESIAN_POINT('',(-162.5175,-225.,10.));
#76327=CARTESIAN_POINT('Ctrl Pts',(-162.515939379227,-225.002142062255,
10.1125833024919));
#76328=CARTESIAN_POINT('Ctrl Pts',(-162.511202965047,-224.416895606318,
10.0756373715289));
#76329=CARTESIAN_POINT('Ctrl Pts',(-162.307732471351,-223.828679655638,
10.0386914405659));
#76330=CARTESIAN_POINT('Ctrl Pts',(-161.934544677219,-223.382377474813,
10.0017455096029));
#76331=CARTESIAN_POINT('Ctrl Pts',(-161.400011320115,-222.743119152998,
9.94882622119228));
#76332=CARTESIAN_POINT('Ctrl Pts',(-160.517284287975,-222.395012510696,
9.89590693278169));
#76333=CARTESIAN_POINT('Ctrl Pts',(-159.690299453349,-222.497351140581,
9.84298764437109));
#76334=CARTESIAN_POINT('Ctrl Pts',(-158.863314618724,-222.599689770465,
9.79006835596049));
#76335=CARTESIAN_POINT('Ctrl Pts',(-158.092071981614,-223.152473672536,
9.73714906754989));
#76336=CARTESIAN_POINT('Ctrl Pts',(-157.729492157596,-223.902748944075,
9.68422977913929));
#76337=CARTESIAN_POINT('Ctrl Pts',(-157.366912333578,-224.653024215613,
9.6313104907287));
#76338=CARTESIAN_POINT('Ctrl Pts',(-157.412995322652,-225.600790856619,
9.5783912023181));
#76339=CARTESIAN_POINT('Ctrl Pts',(-157.846653549925,-226.312350870803,
9.52547191390751));
#76340=CARTESIAN_POINT('Ctrl Pts',(-158.280311777197,-227.023910884987,
9.47255262549691));
#76341=CARTESIAN_POINT('Ctrl Pts',(-159.101545242668,-227.49926427235,9.41963333708631));
#76342=CARTESIAN_POINT('Ctrl Pts',(-159.934557528684,-227.52088933218,9.36671404867571));
#76343=CARTESIAN_POINT('Ctrl Pts',(-160.767569814701,-227.54251439201,9.31379476026511));
#76344=CARTESIAN_POINT('Ctrl Pts',(-161.612360921263,-227.110411124307,
9.26087547185452));
#76345=CARTESIAN_POINT('Ctrl Pts',(-162.082354454619,-226.422309975877,
9.20795618344392));
#76346=CARTESIAN_POINT('Ctrl Pts',(-162.364700385886,-226.008937140356,
9.1761652231266));
#76347=CARTESIAN_POINT('Ctrl Pts',(-162.511784233693,-225.503176282115,
9.14437426280927));
#76348=CARTESIAN_POINT('Ctrl Pts',(-162.514161617683,-224.998691358253,
9.11258330249195));
#76349=CARTESIAN_POINT('Ctrl Pts',(-162.519611851718,-224.998052208505,
9.38741669750806));
#76350=CARTESIAN_POINT('Ctrl Pts',(-162.513567886561,-225.705928976136,
9.43227142990595));
#76351=CARTESIAN_POINT('Ctrl Pts',(-162.201354841253,-226.418474016637,
9.47712616230385));
#76352=CARTESIAN_POINT('Ctrl Pts',(-161.6728289998,-226.887010538627,9.52198089470174));
#76353=CARTESIAN_POINT('Ctrl Pts',(-161.049278040044,-227.439786533768,
9.57490018311234));
#76354=CARTESIAN_POINT('Ctrl Pts',(-160.124638930707,-227.652924400097,
9.62781947152293));
#76355=CARTESIAN_POINT('Ctrl Pts',(-159.32202651004,-227.428892254171,9.68073875993353));
#76356=CARTESIAN_POINT('Ctrl Pts',(-158.519414089373,-227.204860108245,
9.73365804834413));
#76357=CARTESIAN_POINT('Ctrl Pts',(-157.838828357376,-226.543657950064,
9.78657733675473));
#76358=CARTESIAN_POINT('Ctrl Pts',(-157.59170533163,-225.747851874212,9.83949662516533));
#76359=CARTESIAN_POINT('Ctrl Pts',(-157.344582305884,-224.952045798359,
9.89241591357592));
#76360=CARTESIAN_POINT('Ctrl Pts',(-157.530921986389,-224.021635804835,
9.94533520198652));
#76361=CARTESIAN_POINT('Ctrl Pts',(-158.065455339009,-223.382377488383,
9.99825449039712));
#76362=CARTESIAN_POINT('Ctrl Pts',(-158.599988691629,-222.74311917193,10.0511737788077));
#76363=CARTESIAN_POINT('Ctrl Pts',(-159.482715716365,-222.395012532548,
10.1040930672183));
#76364=CARTESIAN_POINT('Ctrl Pts',(-160.309700544053,-222.497351161574,
10.1570123556289));
#76365=CARTESIAN_POINT('Ctrl Pts',(-161.136685371741,-222.5996897906,10.2099316440395));
#76366=CARTESIAN_POINT('Ctrl Pts',(-161.907928002381,-223.152473688034,
10.2628509324501));
#76367=CARTESIAN_POINT('Ctrl Pts',(-162.270507823358,-223.902748953279,
10.3157702208607));
#76368=CARTESIAN_POINT('Ctrl Pts',(-162.434137931627,-224.241343700644,
10.3396523797432));
#76369=CARTESIAN_POINT('Ctrl Pts',(-162.514537197227,-224.620160784307,
10.3635345386256));
#76370=CARTESIAN_POINT('Ctrl Pts',(-162.513643850542,-224.999337553514,
10.3874166975081));
#76371=CARTESIAN_POINT('Origin',(-160.,-225.,10.));
#76372=CARTESIAN_POINT('',(-162.517183864174,-225.002298291999,11.3874166975081));
#76373=CARTESIAN_POINT('',(-162.521737982592,-225.000045821966,11.112583302492));
#76374=CARTESIAN_POINT('',(-162.5175,-225.,10.));
#76375=CARTESIAN_POINT('Ctrl Pts',(-162.521737578137,-225.000045817593,
11.112583302492));
#76376=CARTESIAN_POINT('Ctrl Pts',(-162.521514732431,-224.169204530868,
11.0598197686592));
#76377=CARTESIAN_POINT('Ctrl Pts',(-162.070684907329,-223.338156013345,
11.0070562348264));
#76378=CARTESIAN_POINT('Ctrl Pts',(-161.374005083048,-222.885460860162,
10.9542927009936));
#76379=CARTESIAN_POINT('Ctrl Pts',(-160.675268704477,-222.431429379836,
10.901373412583));
#76380=CARTESIAN_POINT('Ctrl Pts',(-159.729228717454,-222.357988310668,
10.8484541241724));
#76381=CARTESIAN_POINT('Ctrl Pts',(-158.968793001442,-222.698744284467,
10.7955348357618));
#76382=CARTESIAN_POINT('Ctrl Pts',(-158.208357285429,-223.039500258266,
10.7426155473512));
#76383=CARTESIAN_POINT('Ctrl Pts',(-157.633525840426,-223.79445327503,10.6896962589407));
#76384=CARTESIAN_POINT('Ctrl Pts',(-157.507341524364,-224.618136849133,
10.6367769705301));
#76385=CARTESIAN_POINT('Ctrl Pts',(-157.381157208302,-225.441820423236,
10.5838576821195));
#76386=CARTESIAN_POINT('Ctrl Pts',(-157.703620021181,-226.334234554677,
10.5309383937089));
#76387=CARTESIAN_POINT('Ctrl Pts',(-158.327170986167,-226.887010554456,
10.4780191052983));
#76388=CARTESIAN_POINT('Ctrl Pts',(-158.950721951154,-227.439786554235,
10.4250998168877));
#76389=CARTESIAN_POINT('Ctrl Pts',(-159.875361068248,-227.652924422351,
10.3721805284771));
#76390=CARTESIAN_POINT('Ctrl Pts',(-160.677973495648,-227.428892274546,
10.3192612400665));
#76391=CARTESIAN_POINT('Ctrl Pts',(-161.480585923048,-227.20486012674,10.2663419516559));
#76392=CARTESIAN_POINT('Ctrl Pts',(-162.161171660753,-226.543657963013,
10.2134226632453));
#76393=CARTESIAN_POINT('Ctrl Pts',(-162.408294688572,-225.747851880485,
10.1605033748347));
#76394=CARTESIAN_POINT('Ctrl Pts',(-162.482887234606,-225.507642773429,
10.1445300173871));
#76395=CARTESIAN_POINT('Ctrl Pts',(-162.517987140231,-225.255169949006,
10.1285566599395));
#76396=CARTESIAN_POINT('Ctrl Pts',(-162.515939379227,-225.002142062255,
10.1125833024919));
#76397=CARTESIAN_POINT('Ctrl Pts',(-162.513643850542,-224.999337553514,
10.3874166975081));
#76398=CARTESIAN_POINT('Ctrl Pts',(-162.512557674726,-225.460359733951,
10.4164538270362));
#76399=CARTESIAN_POINT('Ctrl Pts',(-162.391297288662,-225.921913634613,
10.4454909565643));
#76400=CARTESIAN_POINT('Ctrl Pts',(-162.153346432012,-226.312350859794,
10.4745280860925));
#76401=CARTESIAN_POINT('Ctrl Pts',(-161.719688208377,-227.023910868009,
10.5274473745031));
#76402=CARTESIAN_POINT('Ctrl Pts',(-160.898454749795,-227.499264251384,
10.5803666629137));
#76403=CARTESIAN_POINT('Ctrl Pts',(-160.065442470767,-227.520889311033,
10.6332859513243));
#76404=CARTESIAN_POINT('Ctrl Pts',(-159.232430191738,-227.542514370681,
10.6862052397349));
#76405=CARTESIAN_POINT('Ctrl Pts',(-158.387639092262,-227.110411106604,
10.7391245281455));
#76406=CARTESIAN_POINT('Ctrl Pts',(-157.917645562849,-226.422309963946,
10.7920438165561));
#76407=CARTESIAN_POINT('Ctrl Pts',(-157.447652033437,-225.734208821288,
10.8449631049667));
#76408=CARTESIAN_POINT('Ctrl Pts',(-157.352456074086,-224.790109800049,
10.8978823933773));
#76409=CARTESIAN_POINT('Ctrl Pts',(-157.675619353926,-224.022032593786,
10.9508016817879));
#76410=CARTESIAN_POINT('Ctrl Pts',(-157.998782633765,-223.253955387523,
11.0037209701985));
#76411=CARTESIAN_POINT('Ctrl Pts',(-158.740305152795,-222.661899996236,
11.0566402586091));
#76412=CARTESIAN_POINT('Ctrl Pts',(-159.560866220885,-222.516790955336,
11.1095595470197));
#76413=CARTESIAN_POINT('Ctrl Pts',(-160.381427288976,-222.371681914436,
11.1624788354303));
#76414=CARTESIAN_POINT('Ctrl Pts',(-161.281026906129,-222.673519223924,
11.2153981238409));
#76415=CARTESIAN_POINT('Ctrl Pts',(-161.848008305222,-223.284182136912,
11.2683174122515));
#76416=CARTESIAN_POINT('Ctrl Pts',(-162.273354660738,-223.742298126085,
11.3080171740037));
#76417=CARTESIAN_POINT('Ctrl Pts',(-162.511506189725,-224.374218651919,
11.3477169357559));
#76418=CARTESIAN_POINT('Ctrl Pts',(-162.517183864174,-225.002298291999,
11.3874166975081));
#76419=CARTESIAN_POINT('Origin',(-160.,-225.,10.));
#76420=CARTESIAN_POINT('',(-162.521467614345,-224.999252277067,12.3874166975081));
#76421=CARTESIAN_POINT('',(-162.516072905486,-224.997828941168,12.1125833024919));
#76422=CARTESIAN_POINT('',(-162.5175,-225.,10.));
#76423=CARTESIAN_POINT('Ctrl Pts',(-162.516072905486,-224.997828941168,
12.1125833024919));
#76424=CARTESIAN_POINT('Ctrl Pts',(-162.518115808906,-224.749768865176,
12.0969214542));
#76425=CARTESIAN_POINT('Ctrl Pts',(-162.484398039321,-224.50225196448,12.0812596059081));
#76426=CARTESIAN_POINT('Ctrl Pts',(-162.412644390281,-224.266301977519,
12.0655977576162));
#76427=CARTESIAN_POINT('Ctrl Pts',(-162.170198417287,-223.469058562968,
12.0126784692056));
#76428=CARTESIAN_POINT('Ctrl Pts',(-161.493506842885,-222.803871551054,
11.959759180795));
#76429=CARTESIAN_POINT('Ctrl Pts',(-160.692223718217,-222.57513050535,11.9068398923844));
#76430=CARTESIAN_POINT('Ctrl Pts',(-159.89094059355,-222.346389459646,11.8539206039738));
#76431=CARTESIAN_POINT('Ctrl Pts',(-158.965065918616,-222.554094380152,
11.8010013155632));
#76432=CARTESIAN_POINT('Ctrl Pts',(-158.338279926462,-223.103199499328,
11.7480820271526));
#76433=CARTESIAN_POINT('Ctrl Pts',(-157.711493934307,-223.652304618505,
11.695162738742));
#76434=CARTESIAN_POINT('Ctrl Pts',(-157.383796624932,-224.542809936352,
11.6422434503314));
#76435=CARTESIAN_POINT('Ctrl Pts',(-157.505142280663,-225.367220236932,
11.5893241619208));
#76436=CARTESIAN_POINT('Ctrl Pts',(-157.626487936394,-226.191630537512,
11.5364048735102));
#76437=CARTESIAN_POINT('Ctrl Pts',(-158.19687655723,-226.949945820824,11.4834855850996));
#76438=CARTESIAN_POINT('Ctrl Pts',(-158.955298321493,-227.295161028136,
11.430566296689));
#76439=CARTESIAN_POINT('Ctrl Pts',(-159.713720085756,-227.640376235448,
11.3776470082784));
#76440=CARTESIAN_POINT('Ctrl Pts',(-160.660174993445,-227.572491366758,
11.3247277198678));
#76441=CARTESIAN_POINT('Ctrl Pts',(-161.361565297411,-227.122570536645,
11.2718084314572));
#76442=CARTESIAN_POINT('Ctrl Pts',(-162.062955601377,-226.672649706532,
11.2188891430466));
#76443=CARTESIAN_POINT('Ctrl Pts',(-162.51928130162,-225.840692914996,11.165969854636));
#76444=CARTESIAN_POINT('Ctrl Pts',(-162.521727766681,-225.007403573485,
11.1130505662254));
#76445=CARTESIAN_POINT('Ctrl Pts',(-162.521734967233,-225.004950996485,
11.1128948116476));
#76446=CARTESIAN_POINT('Ctrl Pts',(-162.521738235963,-225.002498407942,
11.1127390570698));
#76447=CARTESIAN_POINT('Ctrl Pts',(-162.521737578137,-225.000045817593,
11.112583302492));
#76448=CARTESIAN_POINT('Ctrl Pts',(-162.517183864174,-225.002298291999,
11.3874166975081));
#76449=CARTESIAN_POINT('Ctrl Pts',(-162.519074459115,-225.211440996619,
11.4006362241665));
#76450=CARTESIAN_POINT('Ctrl Pts',(-162.495188187366,-225.42015782109,11.4138557508248));
#76451=CARTESIAN_POINT('Ctrl Pts',(-162.443853261291,-225.621889759314,
11.4270752774832));
#76452=CARTESIAN_POINT('Ctrl Pts',(-162.238353637232,-226.429445952237,
11.4799945658938));
#76453=CARTESIAN_POINT('Ctrl Pts',(-161.592991208081,-227.125069821595,
11.5329138543044));
#76454=CARTESIAN_POINT('Ctrl Pts',(-160.803083808728,-227.390443898446,
11.585833142715));
#76455=CARTESIAN_POINT('Ctrl Pts',(-160.013176409375,-227.655817975297,
11.6387524311256));
#76456=CARTESIAN_POINT('Ctrl Pts',(-159.07872403982,-227.490942259642,11.6916717195362));
#76457=CARTESIAN_POINT('Ctrl Pts',(-158.427332085998,-226.971263875723,
11.7445910079468));
#76458=CARTESIAN_POINT('Ctrl Pts',(-157.775940132176,-226.451585491803,
11.7975102963574));
#76459=CARTESIAN_POINT('Ctrl Pts',(-157.407608594088,-225.577104439619,
11.850429584768));
#76460=CARTESIAN_POINT('Ctrl Pts',(-157.490885976319,-224.747983231456,
11.9033488731786));
#76461=CARTESIAN_POINT('Ctrl Pts',(-157.574163358551,-223.918862023293,
11.9562681615892));
#76462=CARTESIAN_POINT('Ctrl Pts',(-158.109049661103,-223.135100659151,
12.0091874499998));
#76463=CARTESIAN_POINT('Ctrl Pts',(-158.850780922444,-222.75534832385,12.0621067384104));
#76464=CARTESIAN_POINT('Ctrl Pts',(-159.592512183786,-222.37559598855,12.115026026821));
#76465=CARTESIAN_POINT('Ctrl Pts',(-160.541088403917,-222.399852682092,
12.1679453152316));
#76466=CARTESIAN_POINT('Ctrl Pts',(-161.262441123156,-222.817018541988,
12.2208646036422));
#76467=CARTESIAN_POINT('Ctrl Pts',(-161.983793842396,-223.234184401884,
12.2737838920528));
#76468=CARTESIAN_POINT('Ctrl Pts',(-162.477923060744,-224.044259428135,
12.3267031804634));
#76469=CARTESIAN_POINT('Ctrl Pts',(-162.5187152576,-224.876553304655,12.379622468874));
#76470=CARTESIAN_POINT('Ctrl Pts',(-162.520717953393,-224.917414831451,
12.3822205450854));
#76471=CARTESIAN_POINT('Ctrl Pts',(-162.521627959187,-224.95832991292,12.3848186212967));
#76472=CARTESIAN_POINT('Ctrl Pts',(-162.521467614345,-224.999252277067,
12.3874166975081));
#76473=CARTESIAN_POINT('Origin',(-160.,-225.,10.));
#76474=CARTESIAN_POINT('',(-162.514983776563,-224.998176142249,13.3874166975081));
#76475=CARTESIAN_POINT('',(-162.514086114787,-225.001240687878,13.112583302492));
#76476=CARTESIAN_POINT('',(-162.5175,-225.,10.));
#76477=CARTESIAN_POINT('Ctrl Pts',(-162.514086114787,-225.001240687878,
13.112583302492));
#76478=CARTESIAN_POINT('Ctrl Pts',(-162.511858228025,-224.501661496837,
13.0811038513303));
#76479=CARTESIAN_POINT('Ctrl Pts',(-162.367841089657,-224.000898563083,
13.0496244001686));
#76480=CARTESIAN_POINT('Ctrl Pts',(-162.090670041745,-223.589941661243,
13.0181449490069));
#76481=CARTESIAN_POINT('Ctrl Pts',(-161.624724986089,-222.899092678486,
12.9652256605963));
#76482=CARTESIAN_POINT('Ctrl Pts',(-160.782485656284,-222.462036436092,
12.9123063721857));
#76483=CARTESIAN_POINT('Ctrl Pts',(-159.949360753088,-222.478769861988,
12.8593870837751));
#76484=CARTESIAN_POINT('Ctrl Pts',(-159.116235849893,-222.495503287884,
12.8064677953645));
#76485=CARTESIAN_POINT('Ctrl Pts',(-158.292225373307,-222.966026382069,
12.7535485069539));
#76486=CARTESIAN_POINT('Ctrl Pts',(-157.854396501214,-223.675027785897,
12.7006292185434));
#76487=CARTESIAN_POINT('Ctrl Pts',(-157.416567629121,-224.384029189724,
12.6477099301328));
#76488=CARTESIAN_POINT('Ctrl Pts',(-157.364920361522,-225.331508903193,
12.5947906417222));
#76489=CARTESIAN_POINT('Ctrl Pts',(-157.723088487055,-226.083900228049,
12.5418713533116));
#76490=CARTESIAN_POINT('Ctrl Pts',(-158.081256612587,-226.836291552906,
12.488952064901));
#76491=CARTESIAN_POINT('Ctrl Pts',(-158.849240131251,-227.393594489151,
12.4360327764904));
#76492=CARTESIAN_POINT('Ctrl Pts',(-159.675609800005,-227.500787224115,
12.3831134880798));
#76493=CARTESIAN_POINT('Ctrl Pts',(-160.50197946876,-227.607979959079,12.3301941996692));
#76494=CARTESIAN_POINT('Ctrl Pts',(-161.386735287606,-227.265062492763,
12.2772749112586));
#76495=CARTESIAN_POINT('Ctrl Pts',(-161.925013011235,-226.628953851011,
12.224355622848));
#76496=CARTESIAN_POINT('Ctrl Pts',(-162.303983527613,-226.181106188262,
12.1870981827293));
#76497=CARTESIAN_POINT('Ctrl Pts',(-162.511213111775,-225.587930649141,
12.1498407426106));
#76498=CARTESIAN_POINT('Ctrl Pts',(-162.516072905486,-224.997828941168,
12.1125833024919));
#76499=CARTESIAN_POINT('Ctrl Pts',(-162.521467614345,-224.999252277067,
12.3874166975081));
#76500=CARTESIAN_POINT('Ctrl Pts',(-162.518361952259,-225.791862963762,
12.4377379097073));
#76501=CARTESIAN_POINT('Ctrl Pts',(-162.11372029147,-226.587205706412,12.4880591219065));
#76502=CARTESIAN_POINT('Ctrl Pts',(-161.469861287334,-227.049066478047,
12.5383803341058));
#76503=CARTESIAN_POINT('Ctrl Pts',(-160.792759944848,-227.534773048129,
12.5912996225164));
#76504=CARTESIAN_POINT('Ctrl Pts',(-159.851102084512,-227.651673461503,
12.644218910927));
#76505=CARTESIAN_POINT('Ctrl Pts',(-159.075790324701,-227.346274091308,
12.6971381993376));
#76506=CARTESIAN_POINT('Ctrl Pts',(-158.30047856489,-227.040874721113,12.7500574877482));
#76507=CARTESIAN_POINT('Ctrl Pts',(-157.691512905603,-226.313175567348,
12.8029767761588));
#76508=CARTESIAN_POINT('Ctrl Pts',(-157.527556020558,-225.496171748469,
12.8558960645694));
#76509=CARTESIAN_POINT('Ctrl Pts',(-157.363599135512,-224.67916792959,12.90881535298));
#76510=CARTESIAN_POINT('Ctrl Pts',(-157.644651024707,-223.772859445596,
12.9617346413906));
#76511=CARTESIAN_POINT('Ctrl Pts',(-158.242102349173,-223.191973040943,
13.0146539298012));
#76512=CARTESIAN_POINT('Ctrl Pts',(-158.83955367364,-222.61108663629,13.0675732182118));
#76513=CARTESIAN_POINT('Ctrl Pts',(-159.753404433377,-222.355622310978,
13.1204925066224));
#76514=CARTESIAN_POINT('Ctrl Pts',(-160.565476538698,-222.542480535247,
13.173411795033));
#76515=CARTESIAN_POINT('Ctrl Pts',(-161.377548644019,-222.729338759516,
13.2263310834436));
#76516=CARTESIAN_POINT('Ctrl Pts',(-162.087842094923,-223.358519533365,
13.2792503718542));
#76517=CARTESIAN_POINT('Ctrl Pts',(-162.371326622243,-224.142109747053,
13.3321696602648));
#76518=CARTESIAN_POINT('Ctrl Pts',(-162.469977988056,-224.414795687091,
13.3505853393459));
#76519=CARTESIAN_POINT('Ctrl Pts',(-162.516942395514,-224.706180754175,
13.369001018427));
#76520=CARTESIAN_POINT('Ctrl Pts',(-162.514983776563,-224.998176142249,
13.3874166975081));
#76521=CARTESIAN_POINT('Origin',(-160.,-225.,10.));
#76522=CARTESIAN_POINT('',(-162.514889488545,-225.001779462475,14.3874166975081));
#76523=CARTESIAN_POINT('',(-162.52060107169,-225.001499392296,14.112583302492));
#76524=CARTESIAN_POINT('',(-162.5175,-225.,10.));
#76525=CARTESIAN_POINT('Ctrl Pts',(-162.52060107169,-225.001499392296,14.112583302492));
#76526=CARTESIAN_POINT('Ctrl Pts',(-162.51534499077,-224.25584434795,14.0652862484605));
#76527=CARTESIAN_POINT('Ctrl Pts',(-162.163665333211,-223.505881788273,
14.0179891944291));
#76528=CARTESIAN_POINT('Ctrl Pts',(-161.584215634979,-223.038004443421,
13.9706921403977));
#76529=CARTESIAN_POINT('Ctrl Pts',(-160.935886339886,-222.514510186537,
13.9177728519871));
#76530=CARTESIAN_POINT('Ctrl Pts',(-160.002418184735,-222.344150417211,
13.8648535635765));
#76531=CARTESIAN_POINT('Ctrl Pts',(-159.210966178969,-222.604881762539,
13.8119342751659));
#76532=CARTESIAN_POINT('Ctrl Pts',(-158.419514173204,-222.865613107866,
13.7590149867553));
#76533=CARTESIAN_POINT('Ctrl Pts',(-157.770078316823,-223.557435567847,
13.7060956983447));
#76534=CARTESIAN_POINT('Ctrl Pts',(-157.559840444939,-224.363771198395,
13.6531764099341));
#76535=CARTESIAN_POINT('Ctrl Pts',(-157.349602573054,-225.170106828944,
13.6002571215235));
#76536=CARTESIAN_POINT('Ctrl Pts',(-157.578562685665,-226.090955630061,
13.5473378331129));
#76537=CARTESIAN_POINT('Ctrl Pts',(-158.141948639743,-226.704937208461,
13.4944185447023));
#76538=CARTESIAN_POINT('Ctrl Pts',(-158.705334593821,-227.318918786861,
13.4414992562917));
#76539=CARTESIAN_POINT('Ctrl Pts',(-159.603146389366,-227.626033142544,
13.3885799678811));
#76540=CARTESIAN_POINT('Ctrl Pts',(-160.424545366389,-227.485744752388,
13.3356606794705));
#76541=CARTESIAN_POINT('Ctrl Pts',(-161.245944343412,-227.345456362232,
13.2827413910599));
#76542=CARTESIAN_POINT('Ctrl Pts',(-161.990930501913,-226.757765226237,
13.2298221026493));
#76543=CARTESIAN_POINT('Ctrl Pts',(-162.31859819041,-225.991598796679,13.1769028142387));
#76544=CARTESIAN_POINT('Ctrl Pts',(-162.451350200577,-225.681192439211,
13.1554629769898));
#76545=CARTESIAN_POINT('Ctrl Pts',(-162.515603470644,-225.341491110093,
13.1340231397409));
#76546=CARTESIAN_POINT('Ctrl Pts',(-162.514086114787,-225.001240687878,
13.112583302492));
#76547=CARTESIAN_POINT('Ctrl Pts',(-162.514983776563,-224.998176142249,
13.3874166975081));
#76548=CARTESIAN_POINT('Ctrl Pts',(-162.511314108838,-225.545258590403,
13.4219203068376));
#76549=CARTESIAN_POINT('Ctrl Pts',(-162.335906246044,-226.094483494431,
13.4564239161671));
#76550=CARTESIAN_POINT('Ctrl Pts',(-162.006938674362,-226.526880084621,
13.4909275254966));
#76551=CARTESIAN_POINT('Ctrl Pts',(-161.502390595425,-227.190060554975,
13.5438468139071));
#76552=CARTESIAN_POINT('Ctrl Pts',(-160.636618833816,-227.578421842156,
13.5967661023177));
#76553=CARTESIAN_POINT('Ctrl Pts',(-159.805800530625,-227.514249828787,
13.6496853907283));
#76554=CARTESIAN_POINT('Ctrl Pts',(-158.974982227434,-227.450077815418,
13.7026046791389));
#76555=CARTESIAN_POINT('Ctrl Pts',(-158.17911738266,-226.933372501498,13.7555239675495));
#76556=CARTESIAN_POINT('Ctrl Pts',(-157.782393733624,-226.200578228517,
13.8084432559601));
#76557=CARTESIAN_POINT('Ctrl Pts',(-157.385670084588,-225.467783955537,
13.8613625443707));
#76558=CARTESIAN_POINT('Ctrl Pts',(-157.388087631289,-224.518900723497,
13.9142818327813));
#76559=CARTESIAN_POINT('Ctrl Pts',(-157.788540104405,-223.788137480721,
13.9672011211919));
#76560=CARTESIAN_POINT('Ctrl Pts',(-158.188992577521,-223.057374237944,
14.0201204096025));
#76561=CARTESIAN_POINT('Ctrl Pts',(-158.987479977051,-222.544730984433,
14.0730396980131));
#76562=CARTESIAN_POINT('Ctrl Pts',(-159.818614484671,-222.484793262913,
14.1259589864237));
#76563=CARTESIAN_POINT('Ctrl Pts',(-160.649748992291,-222.424855541393,
14.1788782748343));
#76564=CARTESIAN_POINT('Ctrl Pts',(-161.513530608,-222.817623351865,14.2317975632449));
#76565=CARTESIAN_POINT('Ctrl Pts',(-162.014692881433,-223.483366151979,
14.2847168516555));
#76566=CARTESIAN_POINT('Ctrl Pts',(-162.338892807866,-223.91403258132,14.3189501336064));
#76567=CARTESIAN_POINT('Ctrl Pts',(-162.511345757191,-224.458932104915,
14.3531834155572));
#76568=CARTESIAN_POINT('Ctrl Pts',(-162.514889488545,-225.001779462475,
14.3874166975081));
#76569=CARTESIAN_POINT('Origin',(-160.,-225.,10.));
#76570=CARTESIAN_POINT('',(-162.521411371648,-225.000821673787,15.3874166975081));
#76571=CARTESIAN_POINT('',(-162.518630481145,-224.997804626904,15.1125833024919));
#76572=CARTESIAN_POINT('',(-162.5175,-225.,10.));
#76573=CARTESIAN_POINT('Ctrl Pts',(-162.518630481145,-224.997804626904,
15.1125833024919));
#76574=CARTESIAN_POINT('Ctrl Pts',(-162.520103953586,-224.83674368871,15.1023879340014));
#76575=CARTESIAN_POINT('Ctrl Pts',(-162.505977749995,-224.675940205489,
15.0921925655108));
#76576=CARTESIAN_POINT('Ctrl Pts',(-162.47531478681,-224.51835443701,15.0819971970202));
#76577=CARTESIAN_POINT('Ctrl Pts',(-162.316157989899,-223.700401977595,
15.0290779086096));
#76578=CARTESIAN_POINT('Ctrl Pts',(-161.711475709582,-222.969139652874,
14.976158620199));
#76579=CARTESIAN_POINT('Ctrl Pts',(-160.937970545441,-222.659193088263,
14.9232393317885));
#76580=CARTESIAN_POINT('Ctrl Pts',(-160.1644653813,-222.349246523652,14.8703200433779));
#76581=CARTESIAN_POINT('Ctrl Pts',(-159.222137333336,-222.46061571915,14.8174007549673));
#76582=CARTESIAN_POINT('Ctrl Pts',(-158.542195697769,-222.942338133088,
14.7644814665567));
#76583=CARTESIAN_POINT('Ctrl Pts',(-157.862254062202,-223.424060547025,
14.7115621781461));
#76584=CARTESIAN_POINT('Ctrl Pts',(-157.444698839032,-224.276136179401,
14.6586428897355));
#76585=CARTESIAN_POINT('Ctrl Pts',(-157.480603290172,-225.108655237595,
14.6057236013249));
#76586=CARTESIAN_POINT('Ctrl Pts',(-157.516507741312,-225.941174295788,
14.5528043129143));
#76587=CARTESIAN_POINT('Ctrl Pts',(-158.005871866761,-226.754136779799,
14.4998850245037));
#76588=CARTESIAN_POINT('Ctrl Pts',(-158.724762652337,-227.175531072928,
14.4469657360931));
#76589=CARTESIAN_POINT('Ctrl Pts',(-159.443653437912,-227.596925366057,
14.3940464476825));
#76590=CARTESIAN_POINT('Ctrl Pts',(-160.392070883613,-227.626751468304,
14.3411271592719));
#76591=CARTESIAN_POINT('Ctrl Pts',(-161.136019184935,-227.251360955868,
14.2882078708613));
#76592=CARTESIAN_POINT('Ctrl Pts',(-161.879967486257,-226.875970443432,
14.2352885824507));
#76593=CARTESIAN_POINT('Ctrl Pts',(-162.4194466432,-226.095363316312,14.1823692940401));
#76594=CARTESIAN_POINT('Ctrl Pts',(-162.507591004154,-225.266745380531,
14.1294500056295));
#76595=CARTESIAN_POINT('Ctrl Pts',(-162.516955609601,-225.178711614664,
14.1238277712503));
#76596=CARTESIAN_POINT('Ctrl Pts',(-162.521225865759,-225.090135936605,
14.1182055368711));
#76597=CARTESIAN_POINT('Ctrl Pts',(-162.52060107169,-225.001499392296,14.112583302492));
#76598=CARTESIAN_POINT('Ctrl Pts',(-162.514889488545,-225.001779462475,
14.3874166975081));
#76599=CARTESIAN_POINT('Ctrl Pts',(-162.516823810444,-225.298089037601,
14.4061027039678));
#76600=CARTESIAN_POINT('Ctrl Pts',(-162.468432496996,-225.59378718038,14.4247887104276));
#76601=CARTESIAN_POINT('Ctrl Pts',(-162.366924432334,-225.869962279114,
14.4434747168873));
#76602=CARTESIAN_POINT('Ctrl Pts',(-162.079450778643,-226.652097816378,
14.4963940052979));
#76603=CARTESIAN_POINT('Ctrl Pts',(-161.365960540102,-227.277651101148,
14.5493132937085));
#76604=CARTESIAN_POINT('Ctrl Pts',(-160.55294683584,-227.460368962614,14.6022325821191));
#76605=CARTESIAN_POINT('Ctrl Pts',(-159.739933131577,-227.64308682408,14.6551518705297));
#76606=CARTESIAN_POINT('Ctrl Pts',(-158.827395961593,-227.382969262241,
14.7080711589403));
#76607=CARTESIAN_POINT('Ctrl Pts',(-158.232912316929,-226.799046068281,
14.7609904473509));
#76608=CARTESIAN_POINT('Ctrl Pts',(-157.638428672265,-226.215122874321,
14.8139097357615));
#76609=CARTESIAN_POINT('Ctrl Pts',(-157.361998552922,-225.30739404824,14.8668290241721));
#76610=CARTESIAN_POINT('Ctrl Pts',(-157.530116376076,-224.491236283003,
14.9197483125827));
#76611=CARTESIAN_POINT('Ctrl Pts',(-157.69823419923,-223.675078517767,14.9726676009933));
#76612=CARTESIAN_POINT('Ctrl Pts',(-158.310899964881,-222.950491813376,
15.0255868894039));
#76613=CARTESIAN_POINT('Ctrl Pts',(-159.087757830713,-222.649047031514,
15.0785061778145));
#76614=CARTESIAN_POINT('Ctrl Pts',(-159.864615696544,-222.347602249651,
15.1314254662251));
#76615=CARTESIAN_POINT('Ctrl Pts',(-160.805665662558,-222.469299390317,
15.1843447546357));
#76616=CARTESIAN_POINT('Ctrl Pts',(-161.480283282808,-222.958449844334,
15.2372640430463));
#76617=CARTESIAN_POINT('Ctrl Pts',(-162.118334356872,-223.421086696969,
15.2873149278669));
#76618=CARTESIAN_POINT('Ctrl Pts',(-162.518053365845,-224.212422029304,
15.3373658126875));
#76619=CARTESIAN_POINT('Ctrl Pts',(-162.521411371648,-225.000821673787,
15.3874166975081));
#76620=CARTESIAN_POINT('Origin',(-160.,-225.,10.));
#76621=CARTESIAN_POINT('',(-162.517311901221,-224.997698966112,16.3874166975081));
#76622=CARTESIAN_POINT('',(-162.513487182596,-224.999883653193,16.112583302492));
#76623=CARTESIAN_POINT('',(-162.5175,-225.,10.));
#76624=CARTESIAN_POINT('Ctrl Pts',(-162.513487182596,-224.999883653193,
16.112583302492));
#76625=CARTESIAN_POINT('Ctrl Pts',(-162.513657485401,-224.58681174506,16.0865703311316));
#76626=CARTESIAN_POINT('Ctrl Pts',(-162.417512359637,-224.17381449298,16.0605573597713));
#76627=CARTESIAN_POINT('Ctrl Pts',(-162.224617581508,-223.812463744481,
16.034544388411));
#76628=CARTESIAN_POINT('Ctrl Pts',(-161.832203571769,-223.077352625788,
15.9816251000004));
#76629=CARTESIAN_POINT('Ctrl Pts',(-161.03938641789,-222.55598307528,15.9287058115898));
#76630=CARTESIAN_POINT('Ctrl Pts',(-160.208959233887,-222.486933789028,
15.8757865231792));
#76631=CARTESIAN_POINT('Ctrl Pts',(-159.378532049883,-222.417884502776,
15.8228672347686));
#76632=CARTESIAN_POINT('Ctrl Pts',(-158.510494835754,-222.801155480781,
15.769947946358));
#76633=CARTESIAN_POINT('Ctrl Pts',(-158.002061403624,-223.461361931038,
15.7170286579474));
#76634=CARTESIAN_POINT('Ctrl Pts',(-157.493627971493,-224.121568381295,
15.6641093695368));
#76635=CARTESIAN_POINT('Ctrl Pts',(-157.344798321362,-225.058710303804,
15.6111900811262));
#76636=CARTESIAN_POINT('Ctrl Pts',(-157.6236768982,-225.843951573254,15.5582707927156));
#76637=CARTESIAN_POINT('Ctrl Pts',(-157.902555475038,-226.629192842704,
15.505351504305));
#76638=CARTESIAN_POINT('Ctrl Pts',(-158.609142278846,-227.262533459095,
15.4524322158944));
#76639=CARTESIAN_POINT('Ctrl Pts',(-159.420103202096,-227.454156768817,
15.3995129274838));
#76640=CARTESIAN_POINT('Ctrl Pts',(-160.231064125345,-227.645780078539,
15.3465936390732));
#76641=CARTESIAN_POINT('Ctrl Pts',(-161.146399168037,-227.395686081594,
15.2936743506626));
#76642=CARTESIAN_POINT('Ctrl Pts',(-161.74725103263,-226.818317786065,15.240755062252));
#76643=CARTESIAN_POINT('Ctrl Pts',(-162.232343476571,-226.352184594116,
15.198031142332));
#76644=CARTESIAN_POINT('Ctrl Pts',(-162.51245586189,-225.672734094338,15.155307222412));
#76645=CARTESIAN_POINT('Ctrl Pts',(-162.518630481145,-224.997804626904,
15.1125833024919));
#76646=CARTESIAN_POINT('Ctrl Pts',(-162.521411371648,-225.000821673787,
15.3874166975081));
#76647=CARTESIAN_POINT('Ctrl Pts',(-162.521603818114,-225.046004658637,
15.3902851010981));
#76648=CARTESIAN_POINT('Ctrl Pts',(-162.520494453647,-225.091178001493,
15.3931535046881));
#76649=CARTESIAN_POINT('Ctrl Pts',(-162.518053532688,-225.136279279337,
15.3960219082781));
#76650=CARTESIAN_POINT('Ctrl Pts',(-162.473020887832,-225.968354492954,
15.4489411966887));
#76651=CARTESIAN_POINT('Ctrl Pts',(-161.974770323632,-226.775901152821,
15.5018604850993));
#76652=CARTESIAN_POINT('Ctrl Pts',(-161.251301288472,-227.189385923252,
15.5547797735098));
#76653=CARTESIAN_POINT('Ctrl Pts',(-160.527832253312,-227.602870693684,
15.6076990619204));
#76654=CARTESIAN_POINT('Ctrl Pts',(-159.579144747191,-227.62229357468,15.660618350331));
#76655=CARTESIAN_POINT('Ctrl Pts',(-158.839358154254,-227.238766656296,
15.7135376387416));
#76656=CARTESIAN_POINT('Ctrl Pts',(-158.099571561317,-226.855239737911,
15.7664569271522));
#76657=CARTESIAN_POINT('Ctrl Pts',(-157.568685881563,-226.068763020145,
15.8193762155628));
#76658=CARTESIAN_POINT('Ctrl Pts',(-157.489634391618,-225.23922823355,15.8722955039734));
#76659=CARTESIAN_POINT('Ctrl Pts',(-157.410582901673,-224.409693446955,
15.925214792384));
#76660=CARTESIAN_POINT('Ctrl Pts',(-157.783365601536,-223.537100591531,
15.9781340807946));
#76661=CARTESIAN_POINT('Ctrl Pts',(-158.437397135063,-223.020748140834,
16.0310533692052));
#76662=CARTESIAN_POINT('Ctrl Pts',(-159.091428668591,-222.504395690137,
16.0839726576158));
#76663=CARTESIAN_POINT('Ctrl Pts',(-160.026709035783,-222.344283644167,
16.1368919460264));
#76664=CARTESIAN_POINT('Ctrl Pts',(-160.815253959035,-222.613679271864,
16.189811234437));
#76665=CARTESIAN_POINT('Ctrl Pts',(-161.603798882287,-222.88307489956,16.2427305228476));
#76666=CARTESIAN_POINT('Ctrl Pts',(-162.245608361599,-223.581978200923,
16.2956498112582));
#76667=CARTESIAN_POINT('Ctrl Pts',(-162.446990391789,-224.390571039299,
16.3485690996688));
#76668=CARTESIAN_POINT('Ctrl Pts',(-162.496268001497,-224.588431405808,
16.3615182989486));
#76669=CARTESIAN_POINT('Ctrl Pts',(-162.519174270148,-224.792859619522,
16.3744674982283));
#76670=CARTESIAN_POINT('Ctrl Pts',(-162.517311901221,-224.997698966112,
16.3874166975081));
#76671=CARTESIAN_POINT('Origin',(-160.,-225.,10.));
#76672=CARTESIAN_POINT('',(-162.513611870269,-225.000594615134,17.3874166975081));
#76673=CARTESIAN_POINT('',(-162.518203497722,-225.002256423796,17.1125833024919));
#76674=CARTESIAN_POINT('',(-162.5175,-225.,10.));
#76675=CARTESIAN_POINT('Ctrl Pts',(-162.518203497722,-225.002256423796,
17.1125833024919));
#76676=CARTESIAN_POINT('Ctrl Pts',(-162.512102188789,-224.341151222928,
17.0707527282619));
#76677=CARTESIAN_POINT('Ctrl Pts',(-162.244817978816,-223.675680014097,
17.0289221540318));
#76678=CARTESIAN_POINT('Ctrl Pts',(-161.777620829493,-223.211360872938,
16.9870915798017));
#76679=CARTESIAN_POINT('Ctrl Pts',(-161.186576093803,-222.623957066085,
16.9341722913911));
#76680=CARTESIAN_POINT('Ctrl Pts',(-160.275581999903,-222.358485772275,
16.8812530029806));
#76681=CARTESIAN_POINT('Ctrl Pts',(-159.461509426251,-222.536426651267,
16.82833371457));
#76682=CARTESIAN_POINT('Ctrl Pts',(-158.647436852599,-222.71436753026,16.7754144261594));
#76683=CARTESIAN_POINT('Ctrl Pts',(-157.930285799196,-223.335720582054,
16.7224951377488));
#76684=CARTESIAN_POINT('Ctrl Pts',(-157.638224574459,-224.116154661917,
16.6695758493382));
#76685=CARTESIAN_POINT('Ctrl Pts',(-157.346163349722,-224.89658874178,16.6166565609276));
#76686=CARTESIAN_POINT('Ctrl Pts',(-157.479191953652,-225.836103849712,
16.563737272517));
#76687=CARTESIAN_POINT('Ctrl Pts',(-157.976436499474,-226.504777891013,
16.5108179841064));
#76688=CARTESIAN_POINT('Ctrl Pts',(-158.473681045295,-227.173451932314,
16.4578986956958));
#76689=CARTESIAN_POINT('Ctrl Pts',(-159.335141533009,-227.571284906983,
16.4049794072852));
#76690=CARTESIAN_POINT('Ctrl Pts',(-160.166613660486,-227.516228453529,
16.3520601188746));
#76691=CARTESIAN_POINT('Ctrl Pts',(-160.998085787964,-227.461172000076,
16.299140830464));
#76692=CARTESIAN_POINT('Ctrl Pts',(-161.799569555205,-226.953226118501,
16.2462215420534));
#76693=CARTESIAN_POINT('Ctrl Pts',(-162.204306006026,-226.224826834275,
16.1933022536428));
#76694=CARTESIAN_POINT('Ctrl Pts',(-162.410090467508,-225.854479033516,
16.1663959365925));
#76695=CARTESIAN_POINT('Ctrl Pts',(-162.513311031199,-225.427141407443,
16.1394896195422));
#76696=CARTESIAN_POINT('Ctrl Pts',(-162.513487182596,-224.999883653193,
16.112583302492));
#76697=CARTESIAN_POINT('Ctrl Pts',(-162.517311901221,-224.997698966112,
16.3874166975081));
#76698=CARTESIAN_POINT('Ctrl Pts',(-162.511563356433,-225.629973345696,
16.4273867866389));
#76699=CARTESIAN_POINT('Ctrl Pts',(-162.269828657284,-226.266164842886,
16.4673568757698));
#76700=CARTESIAN_POINT('Ctrl Pts',(-161.839241314137,-226.725212167904,
16.5073269649006));
#76701=CARTESIAN_POINT('Ctrl Pts',(-161.269155625227,-227.332978082743,
16.5602462533112));
#76702=CARTESIAN_POINT('Ctrl Pts',(-160.368029666341,-227.630227537028,
16.6131655417218));
#76703=CARTESIAN_POINT('Ctrl Pts',(-159.548218658251,-227.48093918766,16.6660848301324));
#76704=CARTESIAN_POINT('Ctrl Pts',(-158.728407650161,-227.331650838291,
16.719004118543));
#76705=CARTESIAN_POINT('Ctrl Pts',(-157.989911592869,-226.735824685267,
16.7719234069536));
#76706=CARTESIAN_POINT('Ctrl Pts',(-157.670666268281,-225.966110761729,
16.8248426953642));
#76707=CARTESIAN_POINT('Ctrl Pts',(-157.351420943693,-225.19639683819,16.8777619837748));
#76708=CARTESIAN_POINT('Ctrl Pts',(-157.451426351811,-224.252795144137,
16.9306812721854));
#76709=CARTESIAN_POINT('Ctrl Pts',(-157.924920018577,-223.567097801959,
16.983600560596));
#76710=CARTESIAN_POINT('Ctrl Pts',(-158.398413685342,-222.881400459781,
17.0365198490066));
#76711=CARTESIAN_POINT('Ctrl Pts',(-159.245395610756,-222.45360746948,17.0894391374172));
#76712=CARTESIAN_POINT('Ctrl Pts',(-160.078286885035,-222.479476883083,
17.1423584258278));
#76713=CARTESIAN_POINT('Ctrl Pts',(-160.911178159314,-222.505346296687,
17.1952777142384));
#76714=CARTESIAN_POINT('Ctrl Pts',(-161.729978782458,-222.984878114195,
17.248197002649));
#76715=CARTESIAN_POINT('Ctrl Pts',(-162.160005599952,-223.698638610084,
17.3011162910596));
#76716=CARTESIAN_POINT('Ctrl Pts',(-162.393767178185,-224.086637156247,
17.3298830932091));
#76717=CARTESIAN_POINT('Ctrl Pts',(-162.512646706287,-224.543849909697,
17.3586498953586));
#76718=CARTESIAN_POINT('Ctrl Pts',(-162.513611870269,-225.000594615134,
17.3874166975081));
#76719=CARTESIAN_POINT('Origin',(-160.,-225.,10.));
#76720=CARTESIAN_POINT('',(-162.519491502139,-225.001988389076,18.3874166975081));
#76721=CARTESIAN_POINT('',(-162.520906603697,-224.998703157721,18.112583302492));
#76722=CARTESIAN_POINT('',(-162.5175,-225.,10.));
#76723=CARTESIAN_POINT('Ctrl Pts',(-162.520906603697,-224.998703157721,
18.112583302492));
#76724=CARTESIAN_POINT('Ctrl Pts',(-162.521374483509,-224.924174319773,
18.1078544138027));
#76725=CARTESIAN_POINT('Ctrl Pts',(-162.518355778069,-224.84968391501,18.1031255251135));
#76726=CARTESIAN_POINT('Ctrl Pts',(-162.511727091913,-224.775516150632,
18.0983966364243));
#76727=CARTESIAN_POINT('Ctrl Pts',(-162.437547854986,-223.945531439255,
18.0454773480137));
#76728=CARTESIAN_POINT('Ctrl Pts',(-161.911289246659,-223.155951116232,
17.9925580596031));
#76729=CARTESIAN_POINT('Ctrl Pts',(-161.173767361169,-222.768086967393,
17.9396387711925));
#76730=CARTESIAN_POINT('Ctrl Pts',(-160.436245475678,-222.380222818555,
17.8867194827819));
#76731=CARTESIAN_POINT('Ctrl Pts',(-159.487460313023,-222.394074843902,
17.8338001943713));
#76732=CARTESIAN_POINT('Ctrl Pts',(-158.761575865264,-222.803304431344,
17.7808809059607));
#76733=CARTESIAN_POINT('Ctrl Pts',(-158.035691417506,-223.212534018787,
17.7279616175501));
#76734=CARTESIAN_POINT('Ctrl Pts',(-157.532707684643,-224.017141168325,
17.6750423291395));
#76735=CARTESIAN_POINT('Ctrl Pts',(-157.482790051362,-224.848937628277,
17.6221230407289));
#76736=CARTESIAN_POINT('Ctrl Pts',(-157.43287241808,-225.68073408823,17.5692037523183));
#76737=CARTESIAN_POINT('Ctrl Pts',(-157.836020884379,-226.539719858598,
17.5162844639077));
#76738=CARTESIAN_POINT('Ctrl Pts',(-158.507754701494,-227.032823085037,
17.4633651754971));
#76739=CARTESIAN_POINT('Ctrl Pts',(-159.179488518608,-227.525926311476,
17.4104458870865));
#76740=CARTESIAN_POINT('Ctrl Pts',(-160.119807686538,-227.653146993986,
17.3575265986759));
#76741=CARTESIAN_POINT('Ctrl Pts',(-160.89842218145,-227.356268942422,17.3046073102653));
#76742=CARTESIAN_POINT('Ctrl Pts',(-161.677036676361,-227.059390890857,
17.2516880218547));
#76743=CARTESIAN_POINT('Ctrl Pts',(-162.293946498254,-226.338414105218,
17.1987687334441));
#76744=CARTESIAN_POINT('Ctrl Pts',(-162.466853720459,-225.523257552451,
17.1458494450335));
#76745=CARTESIAN_POINT('Ctrl Pts',(-162.503084720996,-225.35244954846,17.134760730853));
#76746=CARTESIAN_POINT('Ctrl Pts',(-162.519820871428,-225.177506387504,
17.1236720166725));
#76747=CARTESIAN_POINT('Ctrl Pts',(-162.518203497722,-225.002256423796,
17.1125833024919));
#76748=CARTESIAN_POINT('Ctrl Pts',(-162.513611870269,-225.000594615134,
17.3874166975081));
#76749=CARTESIAN_POINT('Ctrl Pts',(-162.514422217894,-225.384075551442,
17.4115691837692));
#76750=CARTESIAN_POINT('Ctrl Pts',(-162.432112241408,-225.767226550828,
17.4357216700303));
#76751=CARTESIAN_POINT('Ctrl Pts',(-162.264887269412,-226.10880625405,17.4598741562914));
#76752=CARTESIAN_POINT('Ctrl Pts',(-161.898489109535,-226.85722422786,17.512793444702));
#76753=CARTESIAN_POINT('Ctrl Pts',(-161.124439777939,-227.406071001213,
17.5657127331126));
#76754=CARTESIAN_POINT('Ctrl Pts',(-160.296944210013,-227.504194407927,
17.6186320215232));
#76755=CARTESIAN_POINT('Ctrl Pts',(-159.469448642086,-227.602317814641,
17.6715513099338));
#76756=CARTESIAN_POINT('Ctrl Pts',(-158.58850683783,-227.249717854717,17.7244705983443));
#76757=CARTESIAN_POINT('Ctrl Pts',(-158.057237798374,-226.607744041865,
17.7773898867549));
#76758=CARTESIAN_POINT('Ctrl Pts',(-157.525968758919,-225.965770229013,
17.8303091751655));
#76759=CARTESIAN_POINT('Ctrl Pts',(-157.344372484265,-225.034422563233,
17.8832284635761));
#76760=CARTESIAN_POINT('Ctrl Pts',(-157.595547324811,-224.23988617669,17.9361477519867));
#76761=CARTESIAN_POINT('Ctrl Pts',(-157.846722165357,-223.445349790147,
17.9890670403973));
#76762=CARTESIAN_POINT('Ctrl Pts',(-158.530668121103,-222.78762468284,18.0419863288079));
#76763=CARTESIAN_POINT('Ctrl Pts',(-159.334411746373,-222.567684899305,
18.0949056172185));
#76764=CARTESIAN_POINT('Ctrl Pts',(-160.138155371642,-222.34774511577,18.1478249056291));
#76765=CARTESIAN_POINT('Ctrl Pts',(-161.061696666434,-222.565590656007,
18.2007441940397));
#76766=CARTESIAN_POINT('Ctrl Pts',(-161.682422716191,-223.12153737975,18.2536634824503));
#76767=CARTESIAN_POINT('Ctrl Pts',(-162.205383293319,-223.589921491573,
18.2982478874696));
#76768=CARTESIAN_POINT('Ctrl Pts',(-162.513404637407,-224.29829090884,18.3428322924888));
#76769=CARTESIAN_POINT('Ctrl Pts',(-162.519491502139,-225.001988389076,
18.3874166975081));
#76770=CARTESIAN_POINT('Origin',(-160.,-225.,10.));
#76771=CARTESIAN_POINT('',(-162.519857325378,-224.99817643576,19.3874166975081));
#76772=CARTESIAN_POINT('',(-162.514309543052,-224.998572563953,19.1125833024919));
#76773=CARTESIAN_POINT('',(-162.5175,-225.,10.));
#76774=CARTESIAN_POINT('',(-158.086534003335,-223.364012796625,20.));
#76775=CARTESIAN_POINT('Ctrl Pts',(-162.519857325378,-224.99817643576,19.3874166975081));
#76776=CARTESIAN_POINT('Ctrl Pts',(-162.513963987124,-225.714913340689,
19.4328532664403));
#76777=CARTESIAN_POINT('Ctrl Pts',(-162.192666865723,-226.43617652876,19.4782898353725));
#76778=CARTESIAN_POINT('Ctrl Pts',(-161.652076061567,-226.905064858465,
19.5237264043047));
#76779=CARTESIAN_POINT('Ctrl Pts',(-161.022458083151,-227.451172043386,
19.5766456927153));
#76780=CARTESIAN_POINT('Ctrl Pts',(-160.095370186091,-227.654934990922,
19.6295649811259));
#76781=CARTESIAN_POINT('Ctrl Pts',(-159.295373481316,-227.421707534687,
19.6824842695365));
#76782=CARTESIAN_POINT('Ctrl Pts',(-158.49537677654,-227.188480078453,19.7354035579471));
#76783=CARTESIAN_POINT('Ctrl Pts',(-157.82247126405,-226.518262218448,19.7883228463576));
#76784=CARTESIAN_POINT('Ctrl Pts',(-157.584268441052,-225.721203069991,
19.8412421347682));
#76785=CARTESIAN_POINT('Ctrl Pts',(-157.346065618053,-224.924143921533,
19.8941614231788));
#76786=CARTESIAN_POINT('Ctrl Pts',(-157.542565484547,-224.000243484621,
19.9470807115894));
#76787=CARTESIAN_POINT('Ctrl Pts',(-158.086534003335,-223.364012796625,
20.));
#76788=CARTESIAN_POINT('',(-161.917152659427,-223.361245045743,20.));
#76789=CARTESIAN_POINT('Origin',(-160.,-225.,20.));
#76790=CARTESIAN_POINT('Ctrl Pts',(-161.91715636014,-223.361242267444,20.));
#76791=CARTESIAN_POINT('Ctrl Pts',(-161.386618601236,-222.742548953518,
19.948244384658));
#76792=CARTESIAN_POINT('Ctrl Pts',(-160.527623964281,-222.402875584563,
19.896488769316));
#76793=CARTESIAN_POINT('Ctrl Pts',(-159.717628707495,-222.49422785314,19.844733153974));
#76794=CARTESIAN_POINT('Ctrl Pts',(-158.889421520279,-222.587634085795,
19.7918138655634));
#76795=CARTESIAN_POINT('Ctrl Pts',(-158.112441887667,-223.131666210172,
19.7388945771528));
#76796=CARTESIAN_POINT('Ctrl Pts',(-157.741727813776,-223.877852582083,
19.6859752887422));
#76797=CARTESIAN_POINT('Ctrl Pts',(-157.371013739885,-224.624038953993,
19.6330560003316));
#76798=CARTESIAN_POINT('Ctrl Pts',(-157.406565224716,-225.572379573437,
19.580136711921));
#76799=CARTESIAN_POINT('Ctrl Pts',(-157.832358767884,-226.288685324508,
19.5272174235104));
#76800=CARTESIAN_POINT('Ctrl Pts',(-158.258152311052,-227.004991075579,
19.4742981350998));
#76801=CARTESIAN_POINT('Ctrl Pts',(-159.074187912558,-227.489261958278,
19.4213788466892));
#76802=CARTESIAN_POINT('Ctrl Pts',(-159.906929719594,-227.520005809176,
19.3684595582786));
#76803=CARTESIAN_POINT('Ctrl Pts',(-160.73967152663,-227.550749660074,19.315540269868));
#76804=CARTESIAN_POINT('Ctrl Pts',(-161.589119539195,-227.127966479172,
19.2626209814574));
#76805=CARTESIAN_POINT('Ctrl Pts',(-162.066623220182,-226.445068751754,
19.2097016930468));
#76806=CARTESIAN_POINT('Ctrl Pts',(-162.358730883091,-226.027313523668,
19.1773288961952));
#76807=CARTESIAN_POINT('Ctrl Pts',(-162.511647788968,-225.512217006655,
19.1449560993436));
#76808=CARTESIAN_POINT('Ctrl Pts',(-162.514309543052,-224.998572563953,
19.1125833024919));
#76809=CARTESIAN_POINT('Origin',(160.,-225.,10.));
#76810=CARTESIAN_POINT('',(157.486483996142,-224.999424946341,0.38741669750801));
#76811=CARTESIAN_POINT('',(157.484597045422,-225.003739798663,0.112583302491969));
#76812=CARTESIAN_POINT('',(157.4825,-225.,10.));
#76813=CARTESIAN_POINT('',(158.086534003335,-223.364012796625,0.));
#76814=CARTESIAN_POINT('Ctrl Pts',(157.484597045422,-225.003739798663,0.112583302491969));
#76815=CARTESIAN_POINT('Ctrl Pts',(157.489762314943,-224.411047445606,0.0750555349946397));
#76816=CARTESIAN_POINT('Ctrl Pts',(157.700778171916,-223.815196439696,0.0375277674973106));
#76817=CARTESIAN_POINT('Ctrl Pts',(158.086534003335,-223.364012796625,-1.88044024795886E-14));
#76818=CARTESIAN_POINT('',(161.917152683146,-223.361245013972,6.04505606088546E-15));
#76819=CARTESIAN_POINT('Origin',(160.,-225.,0.));
#76820=CARTESIAN_POINT('Ctrl Pts',(161.9171563836,-223.361242235853,4.27813134826349E-15));
#76821=CARTESIAN_POINT('Ctrl Pts',(161.386618632273,-222.742548965135,0.0517556153419861));
#76822=CARTESIAN_POINT('Ctrl Pts',(160.52762397761,-222.402875530323,0.103511230683966));
#76823=CARTESIAN_POINT('Ctrl Pts',(159.717628704827,-222.494227788249,0.155266846025948));
#76824=CARTESIAN_POINT('Ctrl Pts',(158.889421501254,-222.587634010013,0.208186134436545));
#76825=CARTESIAN_POINT('Ctrl Pts',(158.112441854074,-223.131666181215,0.261105422847145));
#76826=CARTESIAN_POINT('Ctrl Pts',(157.741727774883,-223.877852574113,0.314024711257743));
#76827=CARTESIAN_POINT('Ctrl Pts',(157.5703508005,-224.222806201499,0.338488706674499));
#76828=CARTESIAN_POINT('Ctrl Pts',(157.485797228021,-224.610962400354,0.362952702091254));
#76829=CARTESIAN_POINT('Ctrl Pts',(157.486483996142,-224.999424946341,0.38741669750801));
#76830=CARTESIAN_POINT('Origin',(160.,-225.,10.));
#76831=CARTESIAN_POINT('',(157.482539823067,-225.002301238291,1.38741669750801));
#76832=CARTESIAN_POINT('',(157.478271630914,-224.999864677068,1.11258330249197));
#76833=CARTESIAN_POINT('',(157.4825,-225.,10.));
#76834=CARTESIAN_POINT('Ctrl Pts',(157.478271630914,-224.999864677068,1.11258330249197));
#76835=CARTESIAN_POINT('Ctrl Pts',(157.478266758284,-224.993155409996,1.11215722053549));
#76836=CARTESIAN_POINT('Ctrl Pts',(157.478291201374,-224.986446181325,1.11173113857901));
#76837=CARTESIAN_POINT('Ctrl Pts',(157.478345066988,-224.979737190974,1.11130505662253));
#76838=CARTESIAN_POINT('Ctrl Pts',(157.485035164759,-224.14648201563,1.05838576821194));
#76839=CARTESIAN_POINT('Ctrl Pts',(157.945584954632,-223.316903059734,1.00546647980134));
#76840=CARTESIAN_POINT('Ctrl Pts',(158.649263628601,-222.870539628389,0.952547191390737));
#76841=CARTESIAN_POINT('Ctrl Pts',(159.35294230257,-222.424176197045,0.89962790298014));
#76842=CARTESIAN_POINT('Ctrl Pts',(160.299749860634,-222.361028290252,0.846708614569545));
#76843=CARTESIAN_POINT('Ctrl Pts',(161.056392406879,-222.710150110404,0.793789326158948));
#76844=CARTESIAN_POINT('Ctrl Pts',(161.813034953124,-223.059271930555,0.74087003774835));
#76845=CARTESIAN_POINT('Ctrl Pts',(162.37951248755,-223.820663477651,0.687950749337751));
#76846=CARTESIAN_POINT('Ctrl Pts',(162.496677191016,-224.645584853209,0.635031460927153));
#76847=CARTESIAN_POINT('Ctrl Pts',(162.613841894483,-225.470506228767,0.582112172516556));
#76848=CARTESIAN_POINT('Ctrl Pts',(162.281693766989,-226.358957432787,0.529192884105958));
#76849=CARTESIAN_POINT('Ctrl Pts',(161.652075880165,-226.90506461644,0.476273595695361));
#76850=CARTESIAN_POINT('Ctrl Pts',(161.02245799334,-227.451171800092,0.423354307284765));
#76851=CARTESIAN_POINT('Ctrl Pts',(160.095370347186,-227.654934963376,0.370435018874168));
#76852=CARTESIAN_POINT('Ctrl Pts',(159.295373478101,-227.421707341511,0.317515730463572));
#76853=CARTESIAN_POINT('Ctrl Pts',(158.495376609015,-227.188479719646,0.264596442052972));
#76854=CARTESIAN_POINT('Ctrl Pts',(157.822470517,-226.518261312633,0.211677153642375));
#76855=CARTESIAN_POINT('Ctrl Pts',(157.584267735883,-225.721202253877,0.158757865231775));
#76856=CARTESIAN_POINT('Ctrl Pts',(157.514986700607,-225.489378441796,0.143366344318507));
#76857=CARTESIAN_POINT('Ctrl Pts',(157.482478577974,-225.246824782278,0.127974823405238));
#76858=CARTESIAN_POINT('Ctrl Pts',(157.484597045422,-225.003739798663,0.112583302491969));
#76859=CARTESIAN_POINT('Ctrl Pts',(157.486483996142,-224.999424946341,0.38741669750801));
#76860=CARTESIAN_POINT('Ctrl Pts',(157.487282810391,-225.451265104701,0.415871990501851));
#76861=CARTESIAN_POINT('Ctrl Pts',(157.603404782612,-225.90351972549,0.444327283495692));
#76862=CARTESIAN_POINT('Ctrl Pts',(157.832358734819,-226.28868533952,0.472782576489532));
#76863=CARTESIAN_POINT('Ctrl Pts',(158.258152285151,-227.004991097435,0.52570186490013));
#76864=CARTESIAN_POINT('Ctrl Pts',(159.074187897019,-227.489261998672,0.578621153310728));
#76865=CARTESIAN_POINT('Ctrl Pts',(159.906929716988,-227.520005852602,0.631540441721327));
#76866=CARTESIAN_POINT('Ctrl Pts',(160.739671536957,-227.550749706533,0.684459730131924));
#76867=CARTESIAN_POINT('Ctrl Pts',(161.589119565027,-227.127966513156,0.737379018542522));
#76868=CARTESIAN_POINT('Ctrl Pts',(162.066623254035,-226.445068773419,0.790298306953119));
#76869=CARTESIAN_POINT('Ctrl Pts',(162.544126943043,-225.762171033683,0.843217595363718));
#76870=CARTESIAN_POINT('Ctrl Pts',(162.649686292989,-224.819158747586,0.896136883774314));
#76871=CARTESIAN_POINT('Ctrl Pts',(162.334969949118,-224.047579899124,0.949056172184912));
#76872=CARTESIAN_POINT('Ctrl Pts',(162.020253605247,-223.276001050662,1.00197546059551));
#76873=CARTESIAN_POINT('Ctrl Pts',(161.285261567559,-222.675855639836,1.05489474900611));
#76874=CARTESIAN_POINT('Ctrl Pts',(160.466339381582,-222.521757867424,1.1078140374167));
#76875=CARTESIAN_POINT('Ctrl Pts',(159.647417195605,-222.367660095012,1.1607333258273));
#76876=CARTESIAN_POINT('Ctrl Pts',(158.74456486134,-222.659609961014,1.2136526142379));
#76877=CARTESIAN_POINT('Ctrl Pts',(158.170921226274,-223.264017153202,1.26657190264849));
#76878=CARTESIAN_POINT('Ctrl Pts',(157.734269805566,-223.724085465692,1.306853500935));
#76879=CARTESIAN_POINT('Ctrl Pts',(157.488364938267,-224.365194431732,1.3471350992215));
#76880=CARTESIAN_POINT('Ctrl Pts',(157.482539823067,-225.002301238291,1.38741669750801));
#76881=CARTESIAN_POINT('Origin',(160.,-225.,10.));
#76882=CARTESIAN_POINT('',(157.478659134318,-224.999094471329,2.38741669750801));
#76883=CARTESIAN_POINT('',(157.484174852024,-224.997885174718,2.11258330249197));
#76884=CARTESIAN_POINT('',(157.4825,-225.,10.));
#76885=CARTESIAN_POINT('Ctrl Pts',(157.484174852024,-224.997885174718,2.11258330249197));
#76886=CARTESIAN_POINT('Ctrl Pts',(157.482125749745,-224.740545664016,2.09633961766574));
#76887=CARTESIAN_POINT('Ctrl Pts',(157.518448874547,-224.483770799219,2.08009593283951));
#76888=CARTESIAN_POINT('Ctrl Pts',(157.595547504626,-224.239886233381,2.06385224801329));
#76889=CARTESIAN_POINT('Ctrl Pts',(157.846722326401,-223.445349906401,2.01093295960269));
#76890=CARTESIAN_POINT('Ctrl Pts',(158.53066823104,-222.787624848871,1.95801367119209));
#76891=CARTESIAN_POINT('Ctrl Pts',(159.334411796167,-222.567685081513,1.9050943827815));
#76892=CARTESIAN_POINT('Ctrl Pts',(160.138155361294,-222.347745314154,1.8521750943709));
#76893=CARTESIAN_POINT('Ctrl Pts',(161.061696586909,-222.565590836967,1.7992558059603));
#76894=CARTESIAN_POINT('Ctrl Pts',(161.682422590323,-223.12153751965,1.7463365175497));
#76895=CARTESIAN_POINT('Ctrl Pts',(162.303148593736,-223.677484202334,1.6934172291391));
#76896=CARTESIAN_POINT('Ctrl Pts',(162.621059374948,-224.571532044889,1.64049794072851));
#76897=CARTESIAN_POINT('Ctrl Pts',(162.490679871376,-225.39456067087,1.58757865231791));
#76898=CARTESIAN_POINT('Ctrl Pts',(162.360300367805,-226.217589296851,1.53465936390731));
#76899=CARTESIAN_POINT('Ctrl Pts',(161.781630579449,-226.969598706259,1.48174007549671));
#76900=CARTESIAN_POINT('Ctrl Pts',(161.019467913069,-227.306477917669,1.42882078708612));
#76901=CARTESIAN_POINT('Ctrl Pts',(160.257305246689,-227.643357129078,1.37590149867552));
#76902=CARTESIAN_POINT('Ctrl Pts',(159.311649702285,-227.565106142489,1.32298221026492));
#76903=CARTESIAN_POINT('Ctrl Pts',(158.615237132917,-227.107514951799,1.27006292185432));
#76904=CARTESIAN_POINT('Ctrl Pts',(157.924431759696,-226.653608076519,1.2175697154002));
#76905=CARTESIAN_POINT('Ctrl Pts',(157.478871937926,-225.826444953881,1.16507650894609));
#76906=CARTESIAN_POINT('Ctrl Pts',(157.478271630914,-224.999864677068,1.11258330249197));
#76907=CARTESIAN_POINT('Ctrl Pts',(157.482539823067,-225.002301238291,1.38741669750801));
#76908=CARTESIAN_POINT('Ctrl Pts',(157.480712288809,-225.202183038908,1.4000543876321));
#76909=CARTESIAN_POINT('Ctrl Pts',(157.502515506984,-225.401670911927,1.41269207775619));
#76910=CARTESIAN_POINT('Ctrl Pts',(157.549472906877,-225.595050659854,1.42532976788029));
#76911=CARTESIAN_POINT('Ctrl Pts',(157.746103158413,-226.404812455942,1.47824905629089));
#76912=CARTESIAN_POINT('Ctrl Pts',(158.383798597353,-227.107471529744,1.53116834470148));
#76913=CARTESIAN_POINT('Ctrl Pts',(159.170748325666,-227.381492482561,1.58408763311208));
#76914=CARTESIAN_POINT('Ctrl Pts',(159.95769805398,-227.655513435377,1.63700692152268));
#76915=CARTESIAN_POINT('Ctrl Pts',(160.893902071666,-227.500896267209,1.68992620993327));
#76916=CARTESIAN_POINT('Ctrl Pts',(161.550954150764,-226.988393126299,1.74284549834387));
#76917=CARTESIAN_POINT('Ctrl Pts',(162.208006229861,-226.475889985388,1.79576478675447));
#76918=CARTESIAN_POINT('Ctrl Pts',(162.585906370371,-225.605500871734,1.84868407516507));
#76919=CARTESIAN_POINT('Ctrl Pts',(162.511727132244,-224.775516147041,1.90160336357567));
#76920=CARTESIAN_POINT('Ctrl Pts',(162.437547894118,-223.945531422348,1.95452265198626));
#76921=CARTESIAN_POINT('Ctrl Pts',(161.911289277357,-223.155951086614,2.00744194039686));
#76922=CARTESIAN_POINT('Ctrl Pts',(161.173767380025,-222.768086931539,2.06036122880746));
#76923=CARTESIAN_POINT('Ctrl Pts',(160.436245482693,-222.380222776464,2.11328051721805));
#76924=CARTESIAN_POINT('Ctrl Pts',(159.487460304791,-222.394074802048,2.16619980562865));
#76925=CARTESIAN_POINT('Ctrl Pts',(158.761575845372,-222.803304396067,2.21911909403925));
#76926=CARTESIAN_POINT('Ctrl Pts',(158.035691385952,-223.212533990086,2.27203838244985));
#76927=CARTESIAN_POINT('Ctrl Pts',(157.532707645016,-224.017141152539,2.32495767086044));
#76928=CARTESIAN_POINT('Ctrl Pts',(157.482790010934,-224.84893762585,2.37787695927104));
#76929=CARTESIAN_POINT('Ctrl Pts',(157.479790467183,-224.898920161267,2.3810568720167));
#76930=CARTESIAN_POINT('Ctrl Pts',(157.478426850695,-224.949000871619,2.38423678476235));
#76931=CARTESIAN_POINT('Ctrl Pts',(157.478659134318,-224.999094471329,2.38741669750801));
#76932=CARTESIAN_POINT('Origin',(160.,-225.,10.));
#76933=CARTESIAN_POINT('',(157.485215918653,-224.99827376338,3.38741669750801));
#76934=CARTESIAN_POINT('',(157.485769737505,-225.001366316787,3.11258330249197));
#76935=CARTESIAN_POINT('',(157.4825,-225.,10.));
#76936=CARTESIAN_POINT('Ctrl Pts',(157.485769737505,-225.001366316787,3.11258330249197));
#76937=CARTESIAN_POINT('Ctrl Pts',(157.488277094539,-224.492626544162,3.080522014796));
#76938=CARTESIAN_POINT('Ctrl Pts',(157.638052833085,-223.982529385542,3.04846072710002));
#76939=CARTESIAN_POINT('Ctrl Pts',(157.924920173766,-223.567097909119,3.01639943940404));
#76940=CARTESIAN_POINT('Ctrl Pts',(158.39841380512,-222.881400618225,2.96348015099344));
#76941=CARTESIAN_POINT('Ctrl Pts',(159.24539566719,-222.453607659927,2.91056086258285));
#76942=CARTESIAN_POINT('Ctrl Pts',(160.07828687918,-222.479477071591,2.85764157417225));
#76943=CARTESIAN_POINT('Ctrl Pts',(160.911178091169,-222.505346483254,2.80472228576165));
#76944=CARTESIAN_POINT('Ctrl Pts',(161.729978653078,-222.98487826488,2.75180299735105));
#76945=CARTESIAN_POINT('Ctrl Pts',(162.160005438412,-223.698638707398,2.69888370894046));
#76946=CARTESIAN_POINT('Ctrl Pts',(162.590032223745,-224.412399149916,2.64596442052986));
#76947=CARTESIAN_POINT('Ctrl Pts',(162.631285232503,-225.360388253327,2.59304513211926));
#76948=CARTESIAN_POINT('Ctrl Pts',(162.264887100028,-226.108806171146,2.54012584370867));
#76949=CARTESIAN_POINT('Ctrl Pts',(161.898488967552,-226.857224088965,2.48720655529807));
#76950=CARTESIAN_POINT('Ctrl Pts',(161.124439693843,-227.406070821191,2.43428726688747));
#76951=CARTESIAN_POINT('Ctrl Pts',(160.296944187805,-227.504194220605,2.38136797847687));
#76952=CARTESIAN_POINT('Ctrl Pts',(159.469448681766,-227.602317620019,2.32844869006627));
#76953=CARTESIAN_POINT('Ctrl Pts',(158.588506943398,-227.249717686621,2.27552940165568));
#76954=CARTESIAN_POINT('Ctrl Pts',(158.05723794367,-226.607743921706,2.22261011324508));
#76955=CARTESIAN_POINT('Ctrl Pts',(157.68904306018,-226.162825329247,2.18593450966071));
#76956=CARTESIAN_POINT('Ctrl Pts',(157.48880139235,-225.578916017294,2.14925890607634));
#76957=CARTESIAN_POINT('Ctrl Pts',(157.484174852024,-224.997885174718,2.11258330249197));
#76958=CARTESIAN_POINT('Ctrl Pts',(157.478659134318,-224.999094471329,2.38741669750801));
#76959=CARTESIAN_POINT('Ctrl Pts',(157.482292454888,-225.782645648265,2.43715607317295));
#76960=CARTESIAN_POINT('Ctrl Pts',(157.876385242744,-226.569350388705,2.48689544883789));
#76961=CARTESIAN_POINT('Ctrl Pts',(158.507754677526,-227.032823117687,2.53663482450284));
#76962=CARTESIAN_POINT('Ctrl Pts',(159.179488505429,-227.525926352046,2.58955411291343));
#76963=CARTESIAN_POINT('Ctrl Pts',(160.119807688463,-227.653147036598,2.64247340132403));
#76964=CARTESIAN_POINT('Ctrl Pts',(160.89842219588,-227.356268980265,2.69539268973463));
#76965=CARTESIAN_POINT('Ctrl Pts',(161.677036703297,-227.059390923932,2.74831197814522));
#76966=CARTESIAN_POINT('Ctrl Pts',(162.293946535097,-226.338414126714,2.80123126655582));
#76967=CARTESIAN_POINT('Ctrl Pts',(162.466853760079,-225.523257560855,2.85415055496642));
#76968=CARTESIAN_POINT('Ctrl Pts',(162.639760985062,-224.708100994996,2.90706984337702));
#76969=CARTESIAN_POINT('Ctrl Pts',(162.368665603227,-223.798764660497,2.95998913178761));
#76970=CARTESIAN_POINT('Ctrl Pts',(161.777620858044,-223.21136084421,3.01290842019821));
#76971=CARTESIAN_POINT('Ctrl Pts',(161.186576112861,-222.623957027924,3.06582770860881));
#76972=CARTESIAN_POINT('Ctrl Pts',(160.275582004329,-222.35848572985,3.1187469970194));
#76973=CARTESIAN_POINT('Ctrl Pts',(159.461509417602,-222.5364266117,3.17166628543));
#76974=CARTESIAN_POINT('Ctrl Pts',(158.647436830876,-222.71436749355,3.2245855738406));
#76975=CARTESIAN_POINT('Ctrl Pts',(157.930285765954,-223.335720555324,3.2775048622512));
#76976=CARTESIAN_POINT('Ctrl Pts',(157.638224536527,-224.116154647722,3.3304241506618));
#76977=CARTESIAN_POINT('Ctrl Pts',(157.533377363911,-224.39632298147,3.3494216662772));
#76978=CARTESIAN_POINT('Ctrl Pts',(157.483313259179,-224.696992739086,3.3684191818926));
#76979=CARTESIAN_POINT('Ctrl Pts',(157.485215918653,-224.99827376338,3.38741669750801));
#76980=CARTESIAN_POINT('Origin',(160.,-225.,10.));
#76981=CARTESIAN_POINT('',(157.484904423017,-225.001872886231,4.38741669750801));
#76982=CARTESIAN_POINT('',(157.47919603435,-225.001369558219,4.11258330249197));
#76983=CARTESIAN_POINT('',(157.4825,-225.,10.));
#76984=CARTESIAN_POINT('Ctrl Pts',(157.47919603435,-225.001369558219,4.11258330249197));
#76985=CARTESIAN_POINT('Ctrl Pts',(157.4841473595,-224.246701787719,4.06470441192625));
#76986=CARTESIAN_POINT('Ctrl Pts',(157.845660234688,-223.487919737563,4.01682552136052));
#76987=CARTESIAN_POINT('Ctrl Pts',(158.437397251925,-223.020748288856,3.9689466307948));
#76988=CARTESIAN_POINT('Ctrl Pts',(159.09142873654,-222.504395876775,3.9160273423842));
#76989=CARTESIAN_POINT('Ctrl Pts',(160.026709033785,-222.34428384278,3.8631080539736));
#76990=CARTESIAN_POINT('Ctrl Pts',(160.815253898065,-222.613679450329,3.810188765563));
#76991=CARTESIAN_POINT('Ctrl Pts',(161.603798762344,-222.883075057879,3.75726947715241));
#76992=CARTESIAN_POINT('Ctrl Pts',(162.245608193657,-223.581978306972,3.70435018874181));
#76993=CARTESIAN_POINT('Ctrl Pts',(162.446990208786,-224.390571084876,3.65143090033121));
#76994=CARTESIAN_POINT('Ctrl Pts',(162.648372223916,-225.199163862781,3.59851161192062));
#76995=CARTESIAN_POINT('Ctrl Pts',(162.40932682286,-226.117446169496,3.54559232351002));
#76996=CARTESIAN_POINT('Ctrl Pts',(161.839241176586,-226.725212038881,3.49267303509942));
#76997=CARTESIAN_POINT('Ctrl Pts',(161.269155530311,-227.332977908266,3.43975374668882));
#76998=CARTESIAN_POINT('Ctrl Pts',(160.368029638817,-227.630227340321,3.38683445827822));
#76999=CARTESIAN_POINT('Ctrl Pts',(159.548218692039,-227.480939002117,3.33391516986763));
#77000=CARTESIAN_POINT('Ctrl Pts',(158.72840774526,-227.331650663914,3.28099588145703));
#77001=CARTESIAN_POINT('Ctrl Pts',(157.989911743197,-226.735824555453,3.22807659304643));
#77002=CARTESIAN_POINT('Ctrl Pts',(157.670666442485,-225.966110689478,3.17515730463584));
#77003=CARTESIAN_POINT('Ctrl Pts',(157.544836732555,-225.662729959147,3.15429930392121));
#77004=CARTESIAN_POINT('Ctrl Pts',(157.484138534938,-225.332335385827,3.13344130320659));
#77005=CARTESIAN_POINT('Ctrl Pts',(157.485769737505,-225.001366316787,3.11258330249197));
#77006=CARTESIAN_POINT('Ctrl Pts',(157.485215918653,-224.99827376338,3.38741669750801));
#77007=CARTESIAN_POINT('Ctrl Pts',(157.488613288272,-225.536238129905,3.4213384703032));
#77008=CARTESIAN_POINT('Ctrl Pts',(157.657697925989,-226.076151417195,3.45526024309839));
#77009=CARTESIAN_POINT('Ctrl Pts',(157.976436466973,-226.504777915181,3.48918201589359));
#77010=CARTESIAN_POINT('Ctrl Pts',(158.473681020781,-227.173451967221,3.54210130430419));
#77011=CARTESIAN_POINT('Ctrl Pts',(159.335141522331,-227.57128494828,3.59502059271478));
#77012=CARTESIAN_POINT('Ctrl Pts',(160.166613663162,-227.516228493942,3.64793988112538));
#77013=CARTESIAN_POINT('Ctrl Pts',(160.998085803994,-227.461172039605,3.70085916953598));
#77014=CARTESIAN_POINT('Ctrl Pts',(161.799569584108,-226.953226149871,3.75377845794658));
#77015=CARTESIAN_POINT('Ctrl Pts',(162.20430604143,-226.224826853947,3.80669774635717));
#77016=CARTESIAN_POINT('Ctrl Pts',(162.609042498751,-225.496427558022,3.85961703476777));
#77017=CARTESIAN_POINT('Ctrl Pts',(162.617031633279,-224.547574855907,3.91253632317837));
#77018=CARTESIAN_POINT('Ctrl Pts',(162.224617617237,-223.812463725408,3.96545561158897));
#77019=CARTESIAN_POINT('Ctrl Pts',(161.832203601196,-223.077352594909,4.01837489999956));
#77020=CARTESIAN_POINT('Ctrl Pts',(161.039386434584,-222.555983036026,4.07129418841016));
#77021=CARTESIAN_POINT('Ctrl Pts',(160.208959237243,-222.486933748666,4.12421347682076));
#77022=CARTESIAN_POINT('Ctrl Pts',(159.378532039902,-222.417884461305,4.17713276523136));
#77023=CARTESIAN_POINT('Ctrl Pts',(158.510494811831,-222.801155445465,4.23005205364195));
#77024=CARTESIAN_POINT('Ctrl Pts',(158.002061371535,-223.461361906326,4.28297134205255));
#77025=CARTESIAN_POINT('Ctrl Pts',(157.667567635935,-223.895705731609,4.3177864605377));
#77026=CARTESIAN_POINT('Ctrl Pts',(157.488717770492,-224.44991289216,4.35260157902286));
#77027=CARTESIAN_POINT('Ctrl Pts',(157.484904423017,-225.001872886231,4.38741669750801));
#77028=CARTESIAN_POINT('Origin',(160.,-225.,10.));
#77029=CARTESIAN_POINT('',(157.478473497091,-225.000661269082,5.38741669750801));
#77030=CARTESIAN_POINT('',(157.481647327547,-224.997761948287,5.11258330249197));
#77031=CARTESIAN_POINT('',(157.4825,-225.,10.));
#77032=CARTESIAN_POINT('Ctrl Pts',(157.481647327547,-224.997761948287,5.11258330249197));
#77033=CARTESIAN_POINT('Ctrl Pts',(157.480078492543,-224.827461165568,5.1018060974671));
#77034=CARTESIAN_POINT('Ctrl Pts',(157.495878758897,-224.657449797744,5.09102889244222));
#77035=CARTESIAN_POINT('Ctrl Pts',(157.530116560791,-224.491236321052,5.08025168741734));
#77036=CARTESIAN_POINT('Ctrl Pts',(157.698234371372,-223.675078616854,5.02733239900675));
#77037=CARTESIAN_POINT('Ctrl Pts',(158.310900091203,-222.950491966653,4.97441311059615));
#77038=CARTESIAN_POINT('Ctrl Pts',(159.087757898936,-222.649047207334,4.92149382218555));
#77039=CARTESIAN_POINT('Ctrl Pts',(159.864615706669,-222.347602448016,4.86857453377496));
#77040=CARTESIAN_POINT('Ctrl Pts',(160.805665602304,-222.469299579581,4.81565524536436));
#77041=CARTESIAN_POINT('Ctrl Pts',(161.480283172102,-222.958449997016,4.76273595695376));
#77042=CARTESIAN_POINT('Ctrl Pts',(162.154900741899,-223.447600414451,4.70981666854316));
#77043=CARTESIAN_POINT('Ctrl Pts',(162.563085985859,-224.304204117755,4.65689738013256));
#77044=CARTESIAN_POINT('Ctrl Pts',(162.518053344371,-225.136279269145,4.60397809172197));
#77045=CARTESIAN_POINT('Ctrl Pts',(162.473020702882,-225.968354420534,4.55105880331137));
#77046=CARTESIAN_POINT('Ctrl Pts',(161.974770175945,-226.775901020007,4.49813951490078));
#77047=CARTESIAN_POINT('Ctrl Pts',(161.251301194891,-227.189385759515,4.44522022649018));
#77048=CARTESIAN_POINT('Ctrl Pts',(160.527832213837,-227.602870499024,4.39230093807958));
#77049=CARTESIAN_POINT('Ctrl Pts',(159.579144778666,-227.622293378567,4.33938164966898));
#77050=CARTESIAN_POINT('Ctrl Pts',(158.839358241055,-227.238766488865,4.28646236125838));
#77051=CARTESIAN_POINT('Ctrl Pts',(158.099571703444,-226.855239599163,4.23354307284778));
#77052=CARTESIAN_POINT('Ctrl Pts',(157.568686063394,-226.068762940216,4.18062378443719));
#77053=CARTESIAN_POINT('Ctrl Pts',(157.489634579361,-225.239228215659,4.12770449602659));
#77054=CARTESIAN_POINT('Ctrl Pts',(157.482105171054,-225.16021760982,4.12266409818172));
#77055=CARTESIAN_POINT('Ctrl Pts',(157.47867478901,-225.080816382468,4.11762370033685));
#77056=CARTESIAN_POINT('Ctrl Pts',(157.47919603435,-225.001369558219,4.11258330249197));
#77057=CARTESIAN_POINT('Ctrl Pts',(157.484904423017,-225.001872886231,4.38741669750801));
#77058=CARTESIAN_POINT('Ctrl Pts',(157.482921448559,-225.288896971155,4.40552086743346));
#77059=CARTESIAN_POINT('Ctrl Pts',(157.528269960652,-225.575313401567,4.4236250373589));
#77060=CARTESIAN_POINT('Ctrl Pts',(157.623676860034,-225.843951586809,4.44172920728434));
#77061=CARTESIAN_POINT('Ctrl Pts',(157.902555441351,-226.629192868871,4.49464849569494));
#77062=CARTESIAN_POINT('Ctrl Pts',(158.609142256508,-227.262533495433,4.54756778410554));
#77063=CARTESIAN_POINT('Ctrl Pts',(159.420103192782,-227.454156808233,4.60048707251614));
#77064=CARTESIAN_POINT('Ctrl Pts',(160.231064129057,-227.645780121033,4.65340636092673));
#77065=CARTESIAN_POINT('Ctrl Pts',(161.146399186449,-227.395686120071,4.70632564933733));
#77066=CARTESIAN_POINT('Ctrl Pts',(161.747251060693,-226.818317815269,4.75924493774793));
#77067=CARTESIAN_POINT('Ctrl Pts',(162.348102934937,-226.240949510468,4.81216422615853));
#77068=CARTESIAN_POINT('Ctrl Pts',(162.634471626033,-225.336306901827,4.86508351456912));
#77069=CARTESIAN_POINT('Ctrl Pts',(162.475314826566,-224.518354429275,4.91800280297972));
#77070=CARTESIAN_POINT('Ctrl Pts',(162.316158027099,-223.700401956722,4.97092209139032));
#77071=CARTESIAN_POINT('Ctrl Pts',(161.71147573707,-222.969139620257,5.02384137980092));
#77072=CARTESIAN_POINT('Ctrl Pts',(160.937970560506,-222.659193050668,5.07676066821151));
#77073=CARTESIAN_POINT('Ctrl Pts',(160.164465383941,-222.349246481079,5.12967995662211));
#77074=CARTESIAN_POINT('Ctrl Pts',(159.222137320843,-222.460615678366,5.18259924503271));
#77075=CARTESIAN_POINT('Ctrl Pts',(158.542195674355,-222.94233810004,5.23551853344331));
#77076=CARTESIAN_POINT('Ctrl Pts',(157.891633337668,-223.403245982205,5.28615125479821));
#77077=CARTESIAN_POINT('Ctrl Pts',(157.481272601586,-224.203193660849,5.33678397615311));
#77078=CARTESIAN_POINT('Ctrl Pts',(157.478473497091,-225.000661269082,5.38741669750801));
#77079=CARTESIAN_POINT('Origin',(160.,-225.,10.));
#77080=CARTESIAN_POINT('',(157.482962712505,-224.997707731329,6.38741669750801));
#77081=CARTESIAN_POINT('',(157.48651745684,-225.000035219866,6.11258330249197));
#77082=CARTESIAN_POINT('',(157.4825,-225.,10.));
#77083=CARTESIAN_POINT('Ctrl Pts',(157.48651745684,-225.000035219866,6.11258330249197));
#77084=CARTESIAN_POINT('Ctrl Pts',(157.486570157899,-224.577722240852,6.08598849459735));
#77085=CARTESIAN_POINT('Ctrl Pts',(157.587291233443,-224.155385642676,6.05939368670272));
#77086=CARTESIAN_POINT('Ctrl Pts',(157.788540269793,-223.788137571352,6.0327988788081));
#77087=CARTESIAN_POINT('Ctrl Pts',(158.18899271296,-223.057374383227,5.9798795903975));
#77088=CARTESIAN_POINT('Ctrl Pts',(158.987480052774,-222.544731168055,5.92696030198691));
#77089=CARTESIAN_POINT('Ctrl Pts',(159.818614498236,-222.484793451018,5.87404101357631));
#77090=CARTESIAN_POINT('Ctrl Pts',(160.649748943698,-222.42485573398,5.82112172516571));
#77091=CARTESIAN_POINT('Ctrl Pts',(161.513530494807,-222.817623515078,5.76820243675511));
#77092=CARTESIAN_POINT('Ctrl Pts',(162.01469273076,-223.483366265404,5.71528314834452));
#77093=CARTESIAN_POINT('Ctrl Pts',(162.515854966714,-224.149109015729,5.66236385993392));
#77094=CARTESIAN_POINT('Ctrl Pts',(162.654397887511,-225.087826735282,5.60944457152332));
#77095=CARTESIAN_POINT('Ctrl Pts',(162.366924255319,-225.869962214052,5.55652528311273));
#77096=CARTESIAN_POINT('Ctrl Pts',(162.079450623127,-226.652097692822,5.50360599470213));
#77097=CARTESIAN_POINT('Ctrl Pts',(161.365960437946,-227.27765093081,5.45068670629153));
#77098=CARTESIAN_POINT('Ctrl Pts',(160.552946794486,-227.460368778611,5.39776741788093));
#77099=CARTESIAN_POINT('Ctrl Pts',(159.739933151027,-227.643086626412,5.34484812947033));
#77100=CARTESIAN_POINT('Ctrl Pts',(158.827396049288,-227.382969084027,5.29192884105974));
#77101=CARTESIAN_POINT('Ctrl Pts',(158.232912449084,-226.799045933736,5.23900955264914));
#77102=CARTESIAN_POINT('Ctrl Pts',(157.759497590274,-226.334040850912,5.19686746926341));
#77103=CARTESIAN_POINT('Ctrl Pts',(157.487781939944,-225.663688760426,5.15472538587769));
#77104=CARTESIAN_POINT('Ctrl Pts',(157.481647327547,-224.997761948287,5.11258330249197));
#77105=CARTESIAN_POINT('Ctrl Pts',(157.478473497091,-225.000661269082,5.38741669750801));
#77106=CARTESIAN_POINT('Ctrl Pts',(157.478347089899,-225.036674801679,5.38970326456371));
#77107=CARTESIAN_POINT('Ctrl Pts',(157.479051869504,-225.072683276385,5.3919898316194));
#77108=CARTESIAN_POINT('Ctrl Pts',(157.480603249708,-225.10865523934,5.3942763986751));
#77109=CARTESIAN_POINT('Ctrl Pts',(157.516507701425,-225.941174310904,5.4471956870857));
#77110=CARTESIAN_POINT('Ctrl Pts',(158.005871834734,-226.754136807972,5.50011497549629));
#77111=CARTESIAN_POINT('Ctrl Pts',(158.724762631855,-227.175531107869,5.55303426390689));
#77112=CARTESIAN_POINT('Ctrl Pts',(159.443653428977,-227.596925407766,5.60595355231749));
#77113=CARTESIAN_POINT('Ctrl Pts',(160.392070889911,-227.626751510492,5.65887284072808));
#77114=CARTESIAN_POINT('Ctrl Pts',(161.136019203181,-227.251360992027,5.71179212913868));
#77115=CARTESIAN_POINT('Ctrl Pts',(161.879967516452,-226.875970473562,5.76471141754928));
#77116=CARTESIAN_POINT('Ctrl Pts',(162.419446682059,-226.095363333905,5.81763070595988));
#77117=CARTESIAN_POINT('Ctrl Pts',(162.507591044428,-225.266745384815,5.87054999437047));
#77118=CARTESIAN_POINT('Ctrl Pts',(162.595735406798,-224.438127435725,5.92346928278107));
#77119=CARTESIAN_POINT('Ctrl Pts',(162.232544965929,-223.561498677202,5.97638857119167));
#77120=CARTESIAN_POINT('Ctrl Pts',(161.584215660423,-223.03800441191,6.02930785960226));
#77121=CARTESIAN_POINT('Ctrl Pts',(160.935886354917,-222.514510146617,6.08222714801286));
#77122=CARTESIAN_POINT('Ctrl Pts',(160.002418184774,-222.344150374556,6.13514643642346));
#77123=CARTESIAN_POINT('Ctrl Pts',(159.210966166297,-222.604881724071,6.18806572483406));
#77124=CARTESIAN_POINT('Ctrl Pts',(158.419514147819,-222.865613073586,6.24098501324466));
#77125=CARTESIAN_POINT('Ctrl Pts',(157.770078281009,-223.557435544678,6.29390430165525));
#77126=CARTESIAN_POINT('Ctrl Pts',(157.559840405747,-224.363771188177,6.34682359006585));
#77127=CARTESIAN_POINT('Ctrl Pts',(157.506084274381,-224.569944717679,6.36035462587991));
#77128=CARTESIAN_POINT('Ctrl Pts',(157.48104219227,-224.783604931856,6.37388566169396));
#77129=CARTESIAN_POINT('Ctrl Pts',(157.482962712505,-224.997707731329,6.38741669750801));
#77130=CARTESIAN_POINT('Origin',(160.,-225.,10.));
#77131=CARTESIAN_POINT('',(157.486314949328,-225.000739875386,7.38741669750801));
#77132=CARTESIAN_POINT('',(157.481518068703,-225.002219574922,7.11258330249198));
#77133=CARTESIAN_POINT('',(157.4825,-225.,10.));
#77134=CARTESIAN_POINT('Ctrl Pts',(157.481518068703,-225.002219574922,7.11258330249198));
#77135=CARTESIAN_POINT('Ctrl Pts',(157.487674948651,-224.33210956248,7.0701708917276));
#77136=CARTESIAN_POINT('Ctrl Pts',(157.763272363098,-223.657527262373,7.02775848096323));
#77137=CARTESIAN_POINT('Ctrl Pts',(158.242102480641,-223.191973176159,6.98534607019885));
#77138=CARTESIAN_POINT('Ctrl Pts',(158.839553760426,-222.611086814949,6.93242678178826));
#77139=CARTESIAN_POINT('Ctrl Pts',(159.753404451819,-222.355622508743,6.87950749337766));
#77140=CARTESIAN_POINT('Ctrl Pts',(160.565476496408,-222.542480719037,6.82658820496706));
#77141=CARTESIAN_POINT('Ctrl Pts',(161.377548540996,-222.729338929331,6.77366891655647));
#77142=CARTESIAN_POINT('Ctrl Pts',(162.08784193878,-223.358519656126,6.72074962814587));
#77143=CARTESIAN_POINT('Ctrl Pts',(162.371326444899,-224.142109811212,6.66783033973527));
#77144=CARTESIAN_POINT('Ctrl Pts',(162.654810951018,-224.925699966298,6.61491105132467));
#77145=CARTESIAN_POINT('Ctrl Pts',(162.511486565472,-225.863699549674,6.56199176291407));
#77146=CARTESIAN_POINT('Ctrl Pts',(162.006938524269,-226.52687997043,6.50907247450348));
#77147=CARTESIAN_POINT('Ctrl Pts',(161.502390483066,-227.190060391187,6.45615318609288));
#77148=CARTESIAN_POINT('Ctrl Pts',(160.636618786206,-227.578421649324,6.40323389768228));
#77149=CARTESIAN_POINT('Ctrl Pts',(159.805800545149,-227.514249640754,6.35031460927169));
#77150=CARTESIAN_POINT('Ctrl Pts',(158.974982304092,-227.450077632184,6.29739532086109));
#77151=CARTESIAN_POINT('Ctrl Pts',(158.179117518839,-226.933372356907,6.24447603245049));
#77152=CARTESIAN_POINT('Ctrl Pts',(157.782393899472,-226.20057813873,6.19155674403989));
#77153=CARTESIAN_POINT('Ctrl Pts',(157.585045380588,-225.836052694455,6.16523226352392));
#77154=CARTESIAN_POINT('Ctrl Pts',(157.486465291471,-225.41805552788,6.13890778300795));
#77155=CARTESIAN_POINT('Ctrl Pts',(157.48651745684,-225.000035219866,6.11258330249197));
#77156=CARTESIAN_POINT('Ctrl Pts',(157.482962712505,-224.997707731329,6.38741669750801));
#77157=CARTESIAN_POINT('Ctrl Pts',(157.488553262792,-225.62095160291,6.42680495010456));
#77158=CARTESIAN_POINT('Ctrl Pts',(157.722615899816,-226.247945794455,6.4661932027011));
#77159=CARTESIAN_POINT('Ctrl Pts',(158.141948609901,-226.704937235844,6.50558145529765));
#77160=CARTESIAN_POINT('Ctrl Pts',(158.705334573027,-227.318918824106,6.55850074370824));
#77161=CARTESIAN_POINT('Ctrl Pts',(159.603146382992,-227.626033184721,6.61142003211884));
#77162=CARTESIAN_POINT('Ctrl Pts',(160.424545373207,-227.485744792312,6.66433932052944));
#77163=CARTESIAN_POINT('Ctrl Pts',(161.245944363423,-227.345456399903,6.71725860894004));
#77164=CARTESIAN_POINT('Ctrl Pts',(161.990930533889,-226.757765254469,6.77017789735064));
#77165=CARTESIAN_POINT('Ctrl Pts',(162.318598227649,-225.991598812605,6.82309718576123));
#77166=CARTESIAN_POINT('Ctrl Pts',(162.646265921409,-225.225432370742,6.87601647417183));
#77167=CARTESIAN_POINT('Ctrl Pts',(162.556615138462,-224.280790632449,6.92893576258242));
#77168=CARTESIAN_POINT('Ctrl Pts',(162.090670075323,-223.589941638596,6.98185505099302));
#77169=CARTESIAN_POINT('Ctrl Pts',(161.624725012184,-222.899092644743,7.03477433940362));
#77170=CARTESIAN_POINT('Ctrl Pts',(160.782485668852,-222.46203639533,7.08769362781422));
#77171=CARTESIAN_POINT('Ctrl Pts',(159.949360752275,-222.478769821494,7.14061291622481));
#77172=CARTESIAN_POINT('Ctrl Pts',(159.116235835699,-222.495503247659,7.19353220463541));
#77173=CARTESIAN_POINT('Ctrl Pts',(158.292225345878,-222.966026349402,7.24645149304601));
#77174=CARTESIAN_POINT('Ctrl Pts',(157.854396466754,-223.675027764616,7.29937078145661));
#77175=CARTESIAN_POINT('Ctrl Pts',(157.611579868785,-224.068234608215,7.32871942014041));
#77176=CARTESIAN_POINT('Ctrl Pts',(157.487542231623,-224.534790895352,7.35806805882421));
#77177=CARTESIAN_POINT('Ctrl Pts',(157.486314949328,-225.000739875386,7.38741669750801));
#77178=CARTESIAN_POINT('Origin',(160.,-225.,10.));
#77179=CARTESIAN_POINT('',(157.480251899882,-225.00189995361,8.38741669750802));
#77180=CARTESIAN_POINT('',(157.479288544104,-224.998569117391,8.11258330249198));
#77181=CARTESIAN_POINT('',(157.4825,-225.,10.));
#77182=CARTESIAN_POINT('Ctrl Pts',(157.479288544104,-224.998569117391,8.11258330249198));
#77183=CARTESIAN_POINT('Ctrl Pts',(157.478719757445,-224.914853296399,8.10727257726845));
#77184=CARTESIAN_POINT('Ctrl Pts',(157.482528847107,-224.831189860152,8.10196185204493));
#77185=CARTESIAN_POINT('Ctrl Pts',(157.490886163968,-224.747983250304,8.0966511268214));
#77186=CARTESIAN_POINT('Ctrl Pts',(157.574163539971,-223.918862104148,8.04373183841081));
#77187=CARTESIAN_POINT('Ctrl Pts',(158.109049802521,-223.135100798621,7.99081255000021));
#77188=CARTESIAN_POINT('Ctrl Pts',(158.850781008391,-222.755348491721,7.93789326158961));
#77189=CARTESIAN_POINT('Ctrl Pts',(159.59251221426,-222.375596184821,7.88497397317902));
#77190=CARTESIAN_POINT('Ctrl Pts',(160.54108836345,-222.399852876549,7.83205468476842));
#77191=CARTESIAN_POINT('Ctrl Pts',(161.262441028742,-222.817018705246,7.77913539635782));
#77192=CARTESIAN_POINT('Ctrl Pts',(161.983793694034,-223.234184533944,7.72621610794722));
#77193=CARTESIAN_POINT('Ctrl Pts',(162.477922875428,-224.044259499611,7.67329681953662));
#77194=CARTESIAN_POINT('Ctrl Pts',(162.518715069233,-224.876553313887,7.62037753112602));
#77195=CARTESIAN_POINT('Ctrl Pts',(162.559507263039,-225.708847128162,7.56745824271543));
#77196=CARTESIAN_POINT('Ctrl Pts',(162.146962469256,-226.563359791046,7.51453895430483));
#77197=CARTESIAN_POINT('Ctrl Pts',(161.469861177408,-227.049066324803,7.46161966589423));
#77198=CARTESIAN_POINT('Ctrl Pts',(160.79275988556,-227.534772858561,7.40870037748364));
#77199=CARTESIAN_POINT('Ctrl Pts',(159.851102095648,-227.651673263193,7.35578108907304));
#77200=CARTESIAN_POINT('Ctrl Pts',(159.07579039382,-227.346273915838,7.30286180066244));
#77201=CARTESIAN_POINT('Ctrl Pts',(158.300478691992,-227.040874568482,7.24994251225184));
#77202=CARTESIAN_POINT('Ctrl Pts',(157.691513078248,-226.31317546914,7.19702322384125));
#77203=CARTESIAN_POINT('Ctrl Pts',(157.527556205464,-225.496171711362,7.14410393543065));
#77204=CARTESIAN_POINT('Ctrl Pts',(157.495003333849,-225.333959429654,7.13359705778443));
#77205=CARTESIAN_POINT('Ctrl Pts',(157.479992817412,-225.168226736112,7.1230901801382));
#77206=CARTESIAN_POINT('Ctrl Pts',(157.481518068703,-225.002219574922,7.11258330249198));
#77207=CARTESIAN_POINT('Ctrl Pts',(157.486314949328,-225.000739875386,7.38741669750801));
#77208=CARTESIAN_POINT('Ctrl Pts',(157.48532928722,-225.374955535516,7.41098734723481));
#77209=CARTESIAN_POINT('Ctrl Pts',(157.563557666543,-225.748779475827,7.4345579969616));
#77210=CARTESIAN_POINT('Ctrl Pts',(157.723088450485,-226.083900245458,7.4581286466884));
#77211=CARTESIAN_POINT('Ctrl Pts',(158.08125658177,-226.836291582399,7.511047935099));
#77212=CARTESIAN_POINT('Ctrl Pts',(158.849240112769,-227.393594527594,7.5639672235096));
#77213=CARTESIAN_POINT('Ctrl Pts',(159.675609794796,-227.50078726428,7.6168865119202));
#77214=CARTESIAN_POINT('Ctrl Pts',(160.501979476823,-227.607980000966,7.66980580033079));
#77215=CARTESIAN_POINT('Ctrl Pts',(161.386735309878,-227.265062529142,7.72272508874138));
#77216=CARTESIAN_POINT('Ctrl Pts',(161.925013042153,-226.628953877174,7.77564437715198));
#77217=CARTESIAN_POINT('Ctrl Pts',(162.463290774427,-225.992845225205,7.82856366556258));
#77218=CARTESIAN_POINT('Ctrl Pts',(162.655090405919,-225.063545393091,7.88148295397318));
#77219=CARTESIAN_POINT('Ctrl Pts',(162.412644429031,-224.266301965735,7.93440224238378));
#77220=CARTESIAN_POINT('Ctrl Pts',(162.170198452142,-223.46905853838,7.98732153079438));
#77221=CARTESIAN_POINT('Ctrl Pts',(161.493506866872,-222.803871515782,8.04024081920497));
#77222=CARTESIAN_POINT('Ctrl Pts',(160.692223729335,-222.575130466404,8.09316010761557));
#77223=CARTESIAN_POINT('Ctrl Pts',(159.890940591798,-222.346389417026,8.14607939602616));
#77224=CARTESIAN_POINT('Ctrl Pts',(158.965065901994,-222.554094340868,8.19899868443676));
#77225=CARTESIAN_POINT('Ctrl Pts',(158.338279899773,-223.103199468864,8.25191797284736));
#77226=CARTESIAN_POINT('Ctrl Pts',(157.803322442313,-223.571856844922,8.29708421440091));
#77227=CARTESIAN_POINT('Ctrl Pts',(157.486236222901,-224.289207295096,8.34225045595446));
#77228=CARTESIAN_POINT('Ctrl Pts',(157.480251899882,-225.00189995361,8.38741669750802));
#77229=CARTESIAN_POINT('Origin',(160.,-225.,10.));
#77230=CARTESIAN_POINT('',(157.480388086678,-224.998052208457,9.38741669750802));
#77231=CARTESIAN_POINT('',(157.485838591434,-224.998691358362,9.11258330249198));
#77232=CARTESIAN_POINT('',(157.4825,-225.,10.));
#77233=CARTESIAN_POINT('Ctrl Pts',(157.485838591434,-224.998691358362,9.11258330249198));
#77234=CARTESIAN_POINT('Ctrl Pts',(157.484258577989,-224.663409819317,9.0914549743987));
#77235=CARTESIAN_POINT('Ctrl Pts',(157.54659475251,-224.328691854693,9.07032664630543));
#77236=CARTESIAN_POINT('Ctrl Pts',(157.675619527759,-224.022032666926,9.04919831821216));
#77237=CARTESIAN_POINT('Ctrl Pts',(157.99878278343,-223.253955518105,8.99627902980156));
#77238=CARTESIAN_POINT('Ctrl Pts',(158.740305247003,-222.661900171095,8.94335974139096));
#77239=CARTESIAN_POINT('Ctrl Pts',(159.560866253727,-222.516791141048,8.89044045298036));
#77240=CARTESIAN_POINT('Ctrl Pts',(160.38142726045,-222.371682111,8.83752116456977));
#77241=CARTESIAN_POINT('Ctrl Pts',(161.281026810325,-222.673519397914,8.78460187615917));
#77242=CARTESIAN_POINT('Ctrl Pts',(161.848008167015,-223.284182265233,8.73168258774857));
#77243=CARTESIAN_POINT('Ctrl Pts',(162.414989523706,-223.894845132552,8.67876329933798));
#77244=CARTESIAN_POINT('Ctrl Pts',(162.649352687212,-224.814333580276,8.62584401092738));
#77245=CARTESIAN_POINT('Ctrl Pts',(162.443853078522,-225.621889712804,8.57292472251678));
#77246=CARTESIAN_POINT('Ctrl Pts',(162.238353469833,-226.429445845333,8.52000543410618));
#77247=CARTESIAN_POINT('Ctrl Pts',(161.592991088946,-227.125069662667,8.46708614569559));
#77248=CARTESIAN_POINT('Ctrl Pts',(160.803083748668,-227.390443719672,8.41416685728499));
#77249=CARTESIAN_POINT('Ctrl Pts',(160.01317640839,-227.655817776677,8.36124756887439));
#77250=CARTESIAN_POINT('Ctrl Pts',(159.07872410872,-227.490942073352,8.30832828046379));
#77251=CARTESIAN_POINT('Ctrl Pts',(158.427332203613,-226.971263728298,8.25540899205319));
#77252=CARTESIAN_POINT('Ctrl Pts',(157.841310856667,-226.503737802108,8.20780042886612));
#77253=CARTESIAN_POINT('Ctrl Pts',(157.484387492819,-225.749048531349,8.16019186567905));
#77254=CARTESIAN_POINT('Ctrl Pts',(157.479288544104,-224.998569117391,8.11258330249198));
#77255=CARTESIAN_POINT('Ctrl Pts',(157.480251899882,-225.00189995361,8.38741669750802));
#77256=CARTESIAN_POINT('Ctrl Pts',(157.479224656189,-225.124237774648,8.39516974436506));
#77257=CARTESIAN_POINT('Ctrl Pts',(157.487364250787,-225.246438350547,8.40292279122211));
#77258=CARTESIAN_POINT('Ctrl Pts',(157.505142240593,-225.36722024283,8.41067583807915));
#77259=CARTESIAN_POINT('Ctrl Pts',(157.626487898273,-226.19163055665,8.46359512648975));
#77260=CARTESIAN_POINT('Ctrl Pts',(158.196876528271,-226.949945852142,8.51651441490035));
#77261=CARTESIAN_POINT('Ctrl Pts',(158.955298304715,-227.295161064999,8.56943370331095));
#77262=CARTESIAN_POINT('Ctrl Pts',(159.713720081158,-227.640376277855,8.62235299172154));
#77263=CARTESIAN_POINT('Ctrl Pts',(160.660175004048,-227.572491408075,8.67527228013214));
#77264=CARTESIAN_POINT('Ctrl Pts',(161.361565319279,-227.122570570736,8.72819156854274));
#77265=CARTESIAN_POINT('Ctrl Pts',(162.06295563451,-226.672649733396,8.78111085695333));
#77266=CARTESIAN_POINT('Ctrl Pts',(162.519281342082,-225.840692928498,8.83403014536393));
#77267=CARTESIAN_POINT('Ctrl Pts',(162.521727807182,-225.007403573603,8.88694943377453));
#77268=CARTESIAN_POINT('Ctrl Pts',(162.524174272282,-224.174114218709,8.93986872218513));
#77269=CARTESIAN_POINT('Ctrl Pts',(162.07274149491,-223.339492313819,8.99278801059573));
#77270=CARTESIAN_POINT('Ctrl Pts',(161.374005105116,-222.885460826201,9.04570729900632));
#77271=CARTESIAN_POINT('Ctrl Pts',(160.675268715322,-222.431429338582,9.09862658741692));
#77272=CARTESIAN_POINT('Ctrl Pts',(159.729228713105,-222.357988268235,9.15154587582752));
#77273=CARTESIAN_POINT('Ctrl Pts',(158.968792984879,-222.698744247507,9.20446516423812));
#77274=CARTESIAN_POINT('Ctrl Pts',(158.208357256654,-223.039500226778,9.25738445264872));
#77275=CARTESIAN_POINT('Ctrl Pts',(157.633525802418,-223.794453255668,9.31030374105931));
#77276=CARTESIAN_POINT('Ctrl Pts',(157.50734148433,-224.618136843,9.36322302946991));
#77277=CARTESIAN_POINT('Ctrl Pts',(157.488111813416,-224.743660874526,9.37128758548261));
#77278=CARTESIAN_POINT('Ctrl Pts',(157.479301425492,-224.870781089513,9.37935214149532));
#77279=CARTESIAN_POINT('Ctrl Pts',(157.480388086678,-224.998052208457,9.38741669750802));
#77280=CARTESIAN_POINT('Origin',(160.,-225.,10.));
#77281=CARTESIAN_POINT('',(157.486356088001,-224.999337553498,10.387416697508));
#77282=CARTESIAN_POINT('',(157.484060830038,-225.002142062077,10.112583302492));
#77283=CARTESIAN_POINT('',(157.4825,-225.,10.));
#77284=CARTESIAN_POINT('Ctrl Pts',(157.484060830038,-225.002142062077,10.112583302492));
#77285=CARTESIAN_POINT('Ctrl Pts',(157.488797243823,-224.416895654818,10.075637371529));
#77286=CARTESIAN_POINT('Ctrl Pts',(157.692267720596,-223.828679753063,10.0386914405659));
#77287=CARTESIAN_POINT('Ctrl Pts',(158.065455483688,-223.38237760936,10.0017455096029));
#77288=CARTESIAN_POINT('Ctrl Pts',(158.599988796332,-222.743119340715,9.94882622119231));
#77289=CARTESIAN_POINT('Ctrl Pts',(159.482715755051,-222.395012727367,9.89590693278172));
#77290=CARTESIAN_POINT('Ctrl Pts',(160.309700520891,-222.49735134874,9.84298764437112));
#77291=CARTESIAN_POINT('Ctrl Pts',(161.136685286731,-222.599689970112,9.79006835596052));
#77292=CARTESIAN_POINT('Ctrl Pts',(161.907927859693,-223.152473826205,9.73714906754993));
#77293=CARTESIAN_POINT('Ctrl Pts',(162.270507653554,-223.902749035339,9.68422977913933));
#77294=CARTESIAN_POINT('Ctrl Pts',(162.633087447414,-224.653024244473,9.63131049072873));
#77295=CARTESIAN_POINT('Ctrl Pts',(162.587004462172,-225.600790806648,9.57839120231814));
#77296=CARTESIAN_POINT('Ctrl Pts',(162.153346270969,-226.312350761648,9.52547191390754));
#77297=CARTESIAN_POINT('Ctrl Pts',(161.719688079767,-227.023910716647,9.47255262549694));
#77298=CARTESIAN_POINT('Ctrl Pts',(160.898454682603,-227.499264064472,9.41963333708634));
#77299=CARTESIAN_POINT('Ctrl Pts',(160.065442465872,-227.520889122503,9.36671404867574));
#77300=CARTESIAN_POINT('Ctrl Pts',(159.232430249142,-227.542514180535,9.31379476026514));
#77301=CARTESIAN_POINT('Ctrl Pts',(158.387639212846,-227.110410948773,9.26087547185455));
#77302=CARTESIAN_POINT('Ctrl Pts',(157.917645718582,-226.422309857576,9.20795618344395));
#77303=CARTESIAN_POINT('Ctrl Pts',(157.635299810799,-226.008937056437,9.17616522312663));
#77304=CARTESIAN_POINT('Ctrl Pts',(157.488215975226,-225.503176240263,9.1443742628093));
#77305=CARTESIAN_POINT('Ctrl Pts',(157.485838591434,-224.998691358362,9.11258330249198));
#77306=CARTESIAN_POINT('Ctrl Pts',(157.480388086678,-224.998052208457,9.38741669750802));
#77307=CARTESIAN_POINT('Ctrl Pts',(157.486432051983,-225.705928993396,9.43227142990591));
#77308=CARTESIAN_POINT('Ctrl Pts',(157.798645104925,-226.418474051318,9.47712616230381));
#77309=CARTESIAN_POINT('Ctrl Pts',(158.3271709593,-226.887010584763,9.5219808947017));
#77310=CARTESIAN_POINT('Ctrl Pts',(158.950721934301,-227.43978659342,9.5749001831123));
#77311=CARTESIAN_POINT('Ctrl Pts',(159.875361066246,-227.65292446496,9.62781947152289));
#77312=CARTESIAN_POINT('Ctrl Pts',(160.677973506536,-227.428892313556,9.68073875993349));
#77313=CARTESIAN_POINT('Ctrl Pts',(161.480585946827,-227.204860162152,9.73365804834408));
#77314=CARTESIAN_POINT('Ctrl Pts',(162.161171695463,-226.543657987806,9.78657733675469));
#77315=CARTESIAN_POINT('Ctrl Pts',(162.408294727251,-225.747851892496,9.83949662516529));
#77316=CARTESIAN_POINT('Ctrl Pts',(162.655417759039,-224.952045797187,9.89241591357588));
#77317=CARTESIAN_POINT('Ctrl Pts',(162.469078073979,-224.021635780915,9.94533520198648));
#77318=CARTESIAN_POINT('Ctrl Pts',(161.93454470829,-223.382377448833,9.99825449039708));
#77319=CARTESIAN_POINT('Ctrl Pts',(161.400011342601,-222.74311911675,10.0511737788077));
#77320=CARTESIAN_POINT('Ctrl Pts',(160.517284296283,-222.395012468857,10.1040930672183));
#77321=CARTESIAN_POINT('Ctrl Pts',(159.690299448375,-222.497351100386,10.1570123556289));
#77322=CARTESIAN_POINT('Ctrl Pts',(158.863314600468,-222.599689731914,10.2099316440395));
#77323=CARTESIAN_POINT('Ctrl Pts',(158.092071950971,-223.152473642863,10.2628509324501));
#77324=CARTESIAN_POINT('Ctrl Pts',(157.729492121129,-223.902748926452,10.3157702208607));
#77325=CARTESIAN_POINT('Ctrl Pts',(157.56586200886,-224.241343682096,10.3396523797431));
#77326=CARTESIAN_POINT('Ctrl Pts',(157.485462741294,-224.620160775021,10.3635345386256));
#77327=CARTESIAN_POINT('Ctrl Pts',(157.486356088001,-224.999337553498,10.387416697508));
#77328=CARTESIAN_POINT('Origin',(160.,-225.,10.));
#77329=CARTESIAN_POINT('',(157.482816074282,-225.002298292055,11.387416697508));
#77330=CARTESIAN_POINT('',(157.478262227161,-225.000045821962,11.112583302492));
#77331=CARTESIAN_POINT('',(157.4825,-225.,10.));
#77332=CARTESIAN_POINT('Ctrl Pts',(157.47826263161,-225.000045817589,11.112583302492));
#77333=CARTESIAN_POINT('Ctrl Pts',(157.478485477297,-224.16920459997,11.0598197686592));
#77334=CARTESIAN_POINT('Ctrl Pts',(157.929315264901,-223.338156151569,11.0070562348264));
#77335=CARTESIAN_POINT('Ctrl Pts',(158.625995031235,-222.88546103604,10.9542927009937));
#77336=CARTESIAN_POINT('Ctrl Pts',(159.324731351689,-222.431429593478,10.9013734125831));
#77337=CARTESIAN_POINT('Ctrl Pts',(160.270771260024,-222.357988530419,10.8484541241725));
#77338=CARTESIAN_POINT('Ctrl Pts',(161.031206912787,-222.698744475875,10.7955348357619));
#77339=CARTESIAN_POINT('Ctrl Pts',(161.79164256555,-223.039500421331,10.7426155473513));
#77340=CARTESIAN_POINT('Ctrl Pts',(162.366473962741,-223.794453375302,10.6896962589407));
#77341=CARTESIAN_POINT('Ctrl Pts',(162.492658268308,-224.618136880895,10.6367769705301));
#77342=CARTESIAN_POINT('Ctrl Pts',(162.618842573874,-225.441820386487,10.5838576821195));
#77343=CARTESIAN_POINT('Ctrl Pts',(162.296379787816,-226.334234443702,10.5309383937089));
#77344=CARTESIAN_POINT('Ctrl Pts',(161.672828874694,-226.887010397503,10.4780191052983));
#77345=CARTESIAN_POINT('Ctrl Pts',(161.049277961572,-227.439786351304,10.4250998168877));
#77346=CARTESIAN_POINT('Ctrl Pts',(160.124638921385,-227.652924201693,10.3721805284771));
#77347=CARTESIAN_POINT('Ctrl Pts',(159.322026560743,-227.428892072521,10.3192612400665));
#77348=CARTESIAN_POINT('Ctrl Pts',(158.519414200101,-227.20485994335,10.2663419516559));
#77349=CARTESIAN_POINT('Ctrl Pts',(157.838828519004,-226.543657834619,10.2134226632453));
#77350=CARTESIAN_POINT('Ctrl Pts',(157.591705511739,-225.747851818282,10.1605033748347));
#77351=CARTESIAN_POINT('Ctrl Pts',(157.517112971909,-225.507642731205,10.1445300173871));
#77352=CARTESIAN_POINT('Ctrl Pts',(157.482013069203,-225.255169927782,10.1285566599396));
#77353=CARTESIAN_POINT('Ctrl Pts',(157.484060830038,-225.002142062077,10.112583302492));
#77354=CARTESIAN_POINT('Ctrl Pts',(157.486356088001,-224.999337553498,10.387416697508));
#77355=CARTESIAN_POINT('Ctrl Pts',(157.487442263843,-225.460359745206,10.4164538270362));
#77356=CARTESIAN_POINT('Ctrl Pts',(157.608702652872,-225.921913657154,10.4454909565643));
#77357=CARTESIAN_POINT('Ctrl Pts',(157.84665351534,-226.312350891881,10.4745280860925));
#77358=CARTESIAN_POINT('Ctrl Pts',(158.280311749578,-227.023910917493,10.527447374503));
#77359=CARTESIAN_POINT('Ctrl Pts',(159.101545228238,-227.49926431249,10.5803666629137));
#77360=CARTESIAN_POINT('Ctrl Pts',(159.934557527633,-227.520889372667,10.6332859513243));
#77361=CARTESIAN_POINT('Ctrl Pts',(160.767569827029,-227.542514432845,10.6862052397348));
#77362=CARTESIAN_POINT('Ctrl Pts',(161.612360947159,-227.110411158202,10.7391245281454));
#77363=CARTESIAN_POINT('Ctrl Pts',(162.082354488063,-226.422309998721,10.792043816556));
#77364=CARTESIAN_POINT('Ctrl Pts',(162.552348028967,-225.734208839239,10.8449631049666));
#77365=CARTESIAN_POINT('Ctrl Pts',(162.647543990645,-224.790109794918,10.8978823933772));
#77366=CARTESIAN_POINT('Ctrl Pts',(162.324380702904,-224.022032569876,10.9508016817878));
#77367=CARTESIAN_POINT('Ctrl Pts',(162.001217415163,-223.253955344834,11.0037209701984));
#77368=CARTESIAN_POINT('Ctrl Pts',(161.259694878004,-222.661899939071,11.056640258609));
#77369=CARTESIAN_POINT('Ctrl Pts',(160.439133789851,-222.516790894623,11.1095595470196));
#77370=CARTESIAN_POINT('Ctrl Pts',(159.618572701698,-222.371681850175,11.1624788354302));
#77371=CARTESIAN_POINT('Ctrl Pts',(158.718973062551,-222.673519167043,11.2153981238408));
#77372=CARTESIAN_POINT('Ctrl Pts',(158.151991649595,-223.284182094961,11.2683174122514));
#77373=CARTESIAN_POINT('Ctrl Pts',(157.72664528368,-223.742298095335,11.3080171740036));
#77374=CARTESIAN_POINT('Ctrl Pts',(157.48849374887,-224.374218636619,11.3477169357558));
#77375=CARTESIAN_POINT('Ctrl Pts',(157.482816074282,-225.002298292055,11.387416697508));
#77376=CARTESIAN_POINT('Origin',(160.,-225.,10.));
#77377=CARTESIAN_POINT('',(157.478532324006,-224.999252277049,12.387416697508));
#77378=CARTESIAN_POINT('',(157.483927303789,-224.997828941348,12.112583302492));
#77379=CARTESIAN_POINT('',(157.4825,-225.,10.));
#77380=CARTESIAN_POINT('Ctrl Pts',(157.483927303789,-224.997828941348,12.112583302492));
#77381=CARTESIAN_POINT('Ctrl Pts',(157.481884400539,-224.74976888599,12.0969214542001));
#77382=CARTESIAN_POINT('Ctrl Pts',(157.51560216732,-224.50225200588,12.0812596059081));
#77383=CARTESIAN_POINT('Ctrl Pts',(157.587355810392,-224.266302038545,12.0655977576162));
#77384=CARTESIAN_POINT('Ctrl Pts',(157.829801763221,-223.469058690305,12.0126784692056));
#77385=CARTESIAN_POINT('Ctrl Pts',(158.506493281338,-222.803871733718,11.959759180795));
#77386=CARTESIAN_POINT('Ctrl Pts',(159.307776339359,-222.575130707039,11.9068398923844));
#77387=CARTESIAN_POINT('Ctrl Pts',(160.109059397379,-222.346389680361,11.8539206039738));
#77388=CARTESIAN_POINT('Ctrl Pts',(161.034933995303,-222.554094583591,11.8010013155632));
#77389=CARTESIAN_POINT('Ctrl Pts',(161.661719935324,-223.103199657096,11.7480820271526));
#77390=CARTESIAN_POINT('Ctrl Pts',(162.288505875345,-223.6523047306,11.695162738742));
#77391=CARTESIAN_POINT('Ctrl Pts',(162.616203157464,-224.542809974379,11.6422434503314));
#77392=CARTESIAN_POINT('Ctrl Pts',(162.494857511826,-225.367220206388,11.5893241619208));
#77393=CARTESIAN_POINT('Ctrl Pts',(162.373511866188,-226.191630438397,11.5364048735102));
#77394=CARTESIAN_POINT('Ctrl Pts',(161.803123292794,-226.949945658637,11.4834855850996));
#77395=CARTESIAN_POINT('Ctrl Pts',(161.044701591613,-227.295160837235,11.430566296689));
#77396=CARTESIAN_POINT('Ctrl Pts',(160.286279890432,-227.640376015833,11.3776470082784));
#77397=CARTESIAN_POINT('Ctrl Pts',(159.339825061465,-227.57249115279,11.3247277198679));
#77398=CARTESIAN_POINT('Ctrl Pts',(158.638434815837,-227.122570360099,11.2718084314573));
#77399=CARTESIAN_POINT('Ctrl Pts',(157.93704457021,-226.672649567409,11.2188891430467));
#77400=CARTESIAN_POINT('Ctrl Pts',(157.480718907923,-225.84069284507,11.1659698546361));
#77401=CARTESIAN_POINT('Ctrl Pts',(157.478272443065,-225.007403572869,11.1130505662255));
#77402=CARTESIAN_POINT('Ctrl Pts',(157.478265242513,-225.004950996073,11.1128948116476));
#77403=CARTESIAN_POINT('Ctrl Pts',(157.478261973784,-225.002498407734,11.1127390570698));
#77404=CARTESIAN_POINT('Ctrl Pts',(157.47826263161,-225.000045817589,11.112583302492));
#77405=CARTESIAN_POINT('Ctrl Pts',(157.482816074282,-225.002298292055,11.387416697508));
#77406=CARTESIAN_POINT('Ctrl Pts',(157.480925479294,-225.211441001789,11.4006362241664));
#77407=CARTESIAN_POINT('Ctrl Pts',(157.504811751628,-225.420157831362,11.4138557508248));
#77408=CARTESIAN_POINT('Ctrl Pts',(157.556146678958,-225.621889774519,11.4270752774832));
#77409=CARTESIAN_POINT('Ctrl Pts',(157.761646308041,-226.429445987186,11.4799945658938));
#77410=CARTESIAN_POINT('Ctrl Pts',(158.407008752971,-227.125069873552,11.5329138543044));
#77411=CARTESIAN_POINT('Ctrl Pts',(159.196916171637,-227.390443956891,11.585833142715));
#77412=CARTESIAN_POINT('Ctrl Pts',(159.986823590303,-227.655818040231,11.6387524311256));
#77413=CARTESIAN_POINT('Ctrl Pts',(160.921275982705,-227.490942320545,11.6916717195362));
#77414=CARTESIAN_POINT('Ctrl Pts',(161.572667952453,-226.971263923919,11.7445910079468));
#77415=CARTESIAN_POINT('Ctrl Pts',(162.224059922201,-226.451585527294,11.7975102963574));
#77416=CARTESIAN_POINT('Ctrl Pts',(162.592391469295,-225.577104453729,11.850429584768));
#77417=CARTESIAN_POINT('Ctrl Pts',(162.509114085028,-224.747983225294,11.9033488731786));
#77418=CARTESIAN_POINT('Ctrl Pts',(162.42583670076,-223.91886199686,11.9562681615892));
#77419=CARTESIAN_POINT('Ctrl Pts',(161.89095038513,-223.135100613555,12.0091874499998));
#77420=CARTESIAN_POINT('Ctrl Pts',(161.149219105654,-222.75534826897,12.0621067384104));
#77421=CARTESIAN_POINT('Ctrl Pts',(160.407487826177,-222.375595924385,12.115026026821));
#77422=CARTESIAN_POINT('Ctrl Pts',(159.458911582854,-222.39985261852,12.1679453152316));
#77423=CARTESIAN_POINT('Ctrl Pts',(158.737558845978,-222.817018488615,12.2208646036422));
#77424=CARTESIAN_POINT('Ctrl Pts',(158.016206109101,-223.234184358711,12.2737838920528));
#77425=CARTESIAN_POINT('Ctrl Pts',(157.522076878672,-224.044259404767,12.3267031804634));
#77426=CARTESIAN_POINT('Ctrl Pts',(157.481284680818,-224.876553301636,12.379622468874));
#77427=CARTESIAN_POINT('Ctrl Pts',(157.479281984977,-224.917414829432,12.3822205450853));
#77428=CARTESIAN_POINT('Ctrl Pts',(157.478371979161,-224.958329911901,12.3848186212967));
#77429=CARTESIAN_POINT('Ctrl Pts',(157.478532324006,-224.999252277049,12.387416697508));
#77430=CARTESIAN_POINT('Origin',(160.,-225.,10.));
#77431=CARTESIAN_POINT('',(157.485016161947,-224.998176142204,13.387416697508));
#77432=CARTESIAN_POINT('',(157.485914094323,-225.001240687775,13.112583302492));
#77433=CARTESIAN_POINT('',(157.4825,-225.,10.));
#77434=CARTESIAN_POINT('Ctrl Pts',(157.485914094323,-225.001240687775,13.112583302492));
#77435=CARTESIAN_POINT('Ctrl Pts',(157.4881419809,-224.501661538287,13.0811038513303));
#77436=CARTESIAN_POINT('Ctrl Pts',(157.632159107289,-224.000898646184,13.0496244001686));
#77437=CARTESIAN_POINT('Ctrl Pts',(157.909330132147,-223.589941778525,13.018144949007));
#77438=CARTESIAN_POINT('Ctrl Pts',(158.375275149048,-222.899092853229,12.9652256605964));
#77439=CARTESIAN_POINT('Ctrl Pts',(159.2175144088,-222.462036647188,12.9123063721858));
#77440=CARTESIAN_POINT('Ctrl Pts',(160.0506392427,-222.478770071692,12.8593870837752));
#77441=CARTESIAN_POINT('Ctrl Pts',(160.8837640766,-222.495503496197,12.8064677953646));
#77442=CARTESIAN_POINT('Ctrl Pts',(161.707774484648,-222.966026551246,12.753548506954));
#77443=CARTESIAN_POINT('Ctrl Pts',(162.145603320324,-223.675027896102,12.7006292185434));
#77444=CARTESIAN_POINT('Ctrl Pts',(162.583432156,-224.384029240958,12.6477099301328));
#77445=CARTESIAN_POINT('Ctrl Pts',(162.635079419304,-225.331508875619,12.5947906417222));
#77446=CARTESIAN_POINT('Ctrl Pts',(162.276911323562,-226.083900137896,12.5418713533116));
#77447=CARTESIAN_POINT('Ctrl Pts',(161.91874322782,-226.836291400172,12.488952064901));
#77448=CARTESIAN_POINT('Ctrl Pts',(161.150759773034,-227.393594290062,12.4360327764904));
#77449=CARTESIAN_POINT('Ctrl Pts',(160.324390173013,-227.500787016111,12.3831134880798));
#77450=CARTESIAN_POINT('Ctrl Pts',(159.498020572992,-227.607979742159,12.3301941996692));
#77451=CARTESIAN_POINT('Ctrl Pts',(158.613264827736,-227.265062304366,12.2772749112586));
#77452=CARTESIAN_POINT('Ctrl Pts',(158.074987148879,-226.628953715522,12.224355622848));
#77453=CARTESIAN_POINT('Ctrl Pts',(157.696016664022,-226.181106090023,12.1870981827293));
#77454=CARTESIAN_POINT('Ctrl Pts',(157.488787097096,-225.58793060024,12.1498407426107));
#77455=CARTESIAN_POINT('Ctrl Pts',(157.483927303789,-224.997828941348,12.112583302492));
#77456=CARTESIAN_POINT('Ctrl Pts',(157.478532324006,-224.999252277049,12.387416697508));
#77457=CARTESIAN_POINT('Ctrl Pts',(157.481637986168,-225.791862983123,12.4377379097073));
#77458=CARTESIAN_POINT('Ctrl Pts',(157.88627965685,-226.587205745219,12.4880591219065));
#77459=CARTESIAN_POINT('Ctrl Pts',(158.530138676728,-227.049066528146,12.5383803341058));
#77460=CARTESIAN_POINT('Ctrl Pts',(159.207240035769,-227.534773110103,12.5912996225164));
#77461=CARTESIAN_POINT('Ctrl Pts',(160.148897919128,-227.651673526335,12.644218910927));
#77462=CARTESIAN_POINT('Ctrl Pts',(160.924209697895,-227.346274148673,12.6971381993375));
#77463=CARTESIAN_POINT('Ctrl Pts',(161.699521476663,-227.040874771011,12.7500574877481));
#77464=CARTESIAN_POINT('Ctrl Pts',(162.308487150838,-226.313175599455,12.8029767761587));
#77465=CARTESIAN_POINT('Ctrl Pts',(162.472444039893,-225.4961717606,12.8558960645693));
#77466=CARTESIAN_POINT('Ctrl Pts',(162.636400928947,-224.679167921746,12.9088153529799));
#77467=CARTESIAN_POINT('Ctrl Pts',(162.35534903288,-223.772859415593,12.9617346413905));
#77468=CARTESIAN_POINT('Ctrl Pts',(161.757897693807,-223.191972996737,13.0146539298011));
#77469=CARTESIAN_POINT('Ctrl Pts',(161.160446354733,-222.611086577882,13.0675732182117));
#77470=CARTESIAN_POINT('Ctrl Pts',(160.246595572652,-222.355622246324,13.1204925066223));
#77471=CARTESIAN_POINT('Ctrl Pts',(159.434523447476,-222.542480475161,13.1734117950329));
#77472=CARTESIAN_POINT('Ctrl Pts',(158.622451322301,-222.729338703999,13.2263310834435));
#77473=CARTESIAN_POINT('Ctrl Pts',(157.91215785403,-223.358519493232,13.2792503718541));
#77474=CARTESIAN_POINT('Ctrl Pts',(157.628673319779,-224.142109726078,13.3321696602647));
#77475=CARTESIAN_POINT('Ctrl Pts',(157.530021951554,-224.414795672783,13.3505853393458));
#77476=CARTESIAN_POINT('Ctrl Pts',(157.483057542947,-224.706180746991,13.3690010184269));
#77477=CARTESIAN_POINT('Ctrl Pts',(157.485016161947,-224.998176142204,13.387416697508));
#77478=CARTESIAN_POINT('Origin',(160.,-225.,10.));
#77479=CARTESIAN_POINT('',(157.485110449967,-225.001779462518,14.387416697508));
#77480=CARTESIAN_POINT('',(157.479399137962,-225.001499392172,14.112583302492));
#77481=CARTESIAN_POINT('',(157.4825,-225.,10.));
#77482=CARTESIAN_POINT('Ctrl Pts',(157.479399137962,-225.001499392172,14.112583302492));
#77483=CARTESIAN_POINT('Ctrl Pts',(157.484655218445,-224.255844409846,14.0652862484606));
#77484=CARTESIAN_POINT('Ctrl Pts',(157.836334846753,-223.505881912547,14.0179891944291));
#77485=CARTESIAN_POINT('Ctrl Pts',(158.415784496789,-223.038004606611,13.9706921403977));
#77486=CARTESIAN_POINT('Ctrl Pts',(159.064113737957,-222.514510393269,13.9177728519871));
#77487=CARTESIAN_POINT('Ctrl Pts',(159.997581815466,-222.344150638113,13.8648535635765));
#77488=CARTESIAN_POINT('Ctrl Pts',(160.789033755402,-222.604881961754,13.8119342751659));
#77489=CARTESIAN_POINT('Ctrl Pts',(161.580485695339,-222.865613285395,13.7590149867553));
#77490=CARTESIAN_POINT('Ctrl Pts',(162.229921497702,-223.557435687833,13.7060956983447));
#77491=CARTESIAN_POINT('Ctrl Pts',(162.4401593521,-224.363771251314,13.6531764099341));
#77492=CARTESIAN_POINT('Ctrl Pts',(162.650397206498,-225.170106814795,13.6002571215235));
#77493=CARTESIAN_POINT('Ctrl Pts',(162.421437112931,-226.09095553932,13.5473378331129));
#77494=CARTESIAN_POINT('Ctrl Pts',(161.858051205713,-226.704937066652,13.4944185447023));
#77495=CARTESIAN_POINT('Ctrl Pts',(161.294665298495,-227.318918593984,13.4414992562917));
#77496=CARTESIAN_POINT('Ctrl Pts',(160.396853577626,-227.626032924123,13.3885799678811));
#77497=CARTESIAN_POINT('Ctrl Pts',(159.575454668923,-227.485744545635,13.3356606794706));
#77498=CARTESIAN_POINT('Ctrl Pts',(158.75405576022,-227.345456167148,13.28274139106));
#77499=CARTESIAN_POINT('Ctrl Pts',(158.009069663684,-226.757765080034,13.2298221026494));
#77500=CARTESIAN_POINT('Ctrl Pts',(157.68140200244,-225.991598714202,13.1769028142388));
#77501=CARTESIAN_POINT('Ctrl Pts',(157.548650003315,-225.681192382553,13.1554629769898));
#77502=CARTESIAN_POINT('Ctrl Pts',(157.484396738593,-225.341491081689,13.1340231397409));
#77503=CARTESIAN_POINT('Ctrl Pts',(157.485914094323,-225.001240687775,13.112583302492));
#77504=CARTESIAN_POINT('Ctrl Pts',(157.485016161947,-224.998176142204,13.387416697508));
#77505=CARTESIAN_POINT('Ctrl Pts',(157.488685829761,-225.545258603735,13.4219203068375));
#77506=CARTESIAN_POINT('Ctrl Pts',(157.664093696845,-226.09448352119,13.456423916167));
#77507=CARTESIAN_POINT('Ctrl Pts',(157.99306127657,-226.526880121952,13.4909275254965));
#77508=CARTESIAN_POINT('Ctrl Pts',(158.497609367842,-227.190060608521,13.5438468139071));
#77509=CARTESIAN_POINT('Ctrl Pts',(159.363381150619,-227.578421905197,13.5967661023177));
#77510=CARTESIAN_POINT('Ctrl Pts',(160.194199474123,-227.514249890259,13.6496853907283));
#77511=CARTESIAN_POINT('Ctrl Pts',(161.025017797627,-227.450077875321,13.7026046791389));
#77512=CARTESIAN_POINT('Ctrl Pts',(161.820882661859,-226.933372548768,13.7555239675495));
#77513=CARTESIAN_POINT('Ctrl Pts',(162.217606320595,-226.200578257871,13.8084432559601));
#77514=CARTESIAN_POINT('Ctrl Pts',(162.614329979331,-225.467783966974,13.8613625443707));
#77515=CARTESIAN_POINT('Ctrl Pts',(162.611912432571,-224.518900711734,13.9142818327813));
#77516=CARTESIAN_POINT('Ctrl Pts',(162.211459949664,-223.788137451091,13.9672011211919));
#77517=CARTESIAN_POINT('Ctrl Pts',(161.811007466758,-223.057374190448,14.0201204096025));
#77518=CARTESIAN_POINT('Ctrl Pts',(161.012520047705,-222.544730924403,14.0730396980131));
#77519=CARTESIAN_POINT('Ctrl Pts',(160.181385519764,-222.484793201417,14.1259589864237));
#77520=CARTESIAN_POINT('Ctrl Pts',(159.350250991823,-222.424855478432,14.1788782748343));
#77521=CARTESIAN_POINT('Ctrl Pts',(158.486469354995,-222.817623298507,14.2317975632449));
#77522=CARTESIAN_POINT('Ctrl Pts',(157.985307069309,-223.483366114898,14.2847168516555));
#77523=CARTESIAN_POINT('Ctrl Pts',(157.661107134949,-223.914032554769,14.3189501336063));
#77524=CARTESIAN_POINT('Ctrl Pts',(157.488654181408,-224.458932091686,14.3531834155572));
#77525=CARTESIAN_POINT('Ctrl Pts',(157.485110449967,-225.001779462518,14.387416697508));
#77526=CARTESIAN_POINT('Origin',(160.,-225.,10.));
#77527=CARTESIAN_POINT('',(157.478588566705,-225.000821673807,15.387416697508));
#77528=CARTESIAN_POINT('',(157.481369728344,-224.997804627087,15.112583302492));
#77529=CARTESIAN_POINT('',(157.4825,-225.,10.));
#77530=CARTESIAN_POINT('Ctrl Pts',(157.481369728344,-224.997804627087,15.112583302492));
#77531=CARTESIAN_POINT('Ctrl Pts',(157.479896256025,-224.836743702289,15.1023879340014));
#77532=CARTESIAN_POINT('Ctrl Pts',(157.494022458441,-224.675940232443,15.0921925655108));
#77533=CARTESIAN_POINT('Ctrl Pts',(157.524685419075,-224.518354477072,15.0819971970203));
#77534=CARTESIAN_POINT('Ctrl Pts',(157.683842202748,-223.70040208569,15.0290779086097));
#77535=CARTESIAN_POINT('Ctrl Pts',(158.288524432771,-222.969139821792,14.9761586201991));
#77536=CARTESIAN_POINT('Ctrl Pts',(159.062029532575,-222.659193282961,14.9232393317885));
#77537=CARTESIAN_POINT('Ctrl Pts',(159.835534632379,-222.34924674413,14.8703200433779));
#77538=CARTESIAN_POINT('Ctrl Pts',(160.777862601965,-222.460615930365,14.8174007549673));
#77539=CARTESIAN_POINT('Ctrl Pts',(161.457804180978,-222.942338304235,14.7644814665567));
#77540=CARTESIAN_POINT('Ctrl Pts',(162.13774575999,-223.424060678104,14.7115621781461));
#77541=CARTESIAN_POINT('Ctrl Pts',(162.555300948429,-224.276136239609,14.6586428897355));
#77542=CARTESIAN_POINT('Ctrl Pts',(162.519396500276,-225.108655228557,14.6057236013249));
#77543=CARTESIAN_POINT('Ctrl Pts',(162.483492052122,-225.941174217505,14.5528043129143));
#77544=CARTESIAN_POINT('Ctrl Pts',(161.994127967376,-226.754136633897,14.4998850245037));
#77545=CARTESIAN_POINT('Ctrl Pts',(161.275237241595,-227.175530891977,14.4469657360931));
#77546=CARTESIAN_POINT('Ctrl Pts',(160.556346515813,-227.596925150056,14.3940464476825));
#77547=CARTESIAN_POINT('Ctrl Pts',(159.607929148997,-227.626751249823,14.3411271592719));
#77548=CARTESIAN_POINT('Ctrl Pts',(158.863980909553,-227.25136076861,14.2882078708613));
#77549=CARTESIAN_POINT('Ctrl Pts',(158.12003267011,-226.875970287397,14.2352885824507));
#77550=CARTESIAN_POINT('Ctrl Pts',(157.580553558038,-226.095363225205,14.1823692940401));
#77551=CARTESIAN_POINT('Ctrl Pts',(157.492409204416,-225.266745358344,14.1294500056295));
#77552=CARTESIAN_POINT('Ctrl Pts',(157.483044599748,-225.1787115998,14.1238277712503));
#77553=CARTESIAN_POINT('Ctrl Pts',(157.478774343945,-225.090135929108,14.1182055368712));
#77554=CARTESIAN_POINT('Ctrl Pts',(157.479399137962,-225.001499392172,14.112583302492));
#77555=CARTESIAN_POINT('Ctrl Pts',(157.485110449967,-225.001779462518,14.387416697508));
#77556=CARTESIAN_POINT('Ctrl Pts',(157.483176128021,-225.298089044889,14.4061027039678));
#77557=CARTESIAN_POINT('Ctrl Pts',(157.531567442652,-225.593787194898,14.4247887104275));
#77558=CARTESIAN_POINT('Ctrl Pts',(157.633075509796,-225.869962300384,14.4434747168873));
#77559=CARTESIAN_POINT('Ctrl Pts',(157.920549170516,-226.652097856771,14.4963940052979));
#77560=CARTESIAN_POINT('Ctrl Pts',(158.634039426501,-227.277651156836,14.5493132937085));
#77561=CARTESIAN_POINT('Ctrl Pts',(159.447053150641,-227.460369022769,14.6022325821191));
#77562=CARTESIAN_POINT('Ctrl Pts',(160.260066874781,-227.643086888702,14.6551518705297));
#77563=CARTESIAN_POINT('Ctrl Pts',(161.172604067077,-227.382969320504,14.7080711589403));
#77564=CARTESIAN_POINT('Ctrl Pts',(161.767087726275,-226.799046112267,14.7609904473509));
#77565=CARTESIAN_POINT('Ctrl Pts',(162.361571385474,-226.21512290403,14.8139097357615));
#77566=CARTESIAN_POINT('Ctrl Pts',(162.638001511576,-225.307394055755,14.866829024172));
#77567=CARTESIAN_POINT('Ctrl Pts',(162.469883684311,-224.491236270564,14.9197483125826));
#77568=CARTESIAN_POINT('Ctrl Pts',(162.301765857047,-223.675078485373,14.9726676009932));
#77569=CARTESIAN_POINT('Ctrl Pts',(161.689100076417,-222.950491763267,15.0255868894038));
#77570=CARTESIAN_POINT('Ctrl Pts',(160.912242191591,-222.649046974034,15.0785061778144));
#77571=CARTESIAN_POINT('Ctrl Pts',(160.135384306766,-222.347602184801,15.131425466225));
#77572=CARTESIAN_POINT('Ctrl Pts',(159.194334317744,-222.469299328443,15.1843447546356));
#77573=CARTESIAN_POINT('Ctrl Pts',(158.519716681,-222.95844979442,15.2372640430462));
#77574=CARTESIAN_POINT('Ctrl Pts',(157.881665591336,-223.421086658366,15.2873149278668));
#77575=CARTESIAN_POINT('Ctrl Pts',(157.481946572589,-224.212422010048,15.3373658126874));
#77576=CARTESIAN_POINT('Ctrl Pts',(157.478588566705,-225.000821673807,15.387416697508));
#77577=CARTESIAN_POINT('Origin',(160.,-225.,10.));
#77578=CARTESIAN_POINT('',(157.482688037232,-224.997698966056,16.387416697508));
#77579=CARTESIAN_POINT('',(157.486513026464,-224.999883653202,16.112583302492));
#77580=CARTESIAN_POINT('',(157.4825,-225.,10.));
#77581=CARTESIAN_POINT('Ctrl Pts',(157.486513026464,-224.999883653202,16.112583302492));
#77582=CARTESIAN_POINT('Ctrl Pts',(157.486342723674,-224.586811779428,16.0865703311317));
#77583=CARTESIAN_POINT('Ctrl Pts',(157.58248784144,-224.173814561698,16.0605573597713));
#77584=CARTESIAN_POINT('Ctrl Pts',(157.775382603526,-223.812463843255,16.034544388411));
#77585=CARTESIAN_POINT('Ctrl Pts',(158.167796580626,-223.077352785706,15.9816251000004));
#77586=CARTESIAN_POINT('Ctrl Pts',(158.960613668561,-222.555983278562,15.9287058115898));
#77587=CARTESIAN_POINT('Ctrl Pts',(159.791040783494,-222.486933998053,15.8757865231792));
#77588=CARTESIAN_POINT('Ctrl Pts',(160.621467898426,-222.417884717545,15.8228672347686));
#77589=CARTESIAN_POINT('Ctrl Pts',(161.489505040356,-222.801155663671,15.769947946358));
#77590=CARTESIAN_POINT('Ctrl Pts',(161.997938430197,-223.461362059015,15.7170286579474));
#77591=CARTESIAN_POINT('Ctrl Pts',(162.506371820038,-224.121568454359,15.6641093695368));
#77592=CARTESIAN_POINT('Ctrl Pts',(162.65520145779,-225.058710298921,15.6111900811262));
#77593=CARTESIAN_POINT('Ctrl Pts',(162.376322904148,-225.843951503058,15.5582707927156));
#77594=CARTESIAN_POINT('Ctrl Pts',(162.097444350506,-226.629192707195,15.505351504305));
#77595=CARTESIAN_POINT('Ctrl Pts',(161.390857605468,-227.262533270907,15.4524322158945));
#77596=CARTESIAN_POINT('Ctrl Pts',(160.579896749671,-227.454156564691,15.3995129274839));
#77597=CARTESIAN_POINT('Ctrl Pts',(159.768935893874,-227.645779858475,15.3465936390733));
#77598=CARTESIAN_POINT('Ctrl Pts',(158.853600927316,-227.395685882331,15.2936743506627));
#77599=CARTESIAN_POINT('Ctrl Pts',(158.252749112698,-226.818317634826,15.2407550622521));
#77600=CARTESIAN_POINT('Ctrl Pts',(157.767656709105,-226.352184481647,15.198031142332));
#77601=CARTESIAN_POINT('Ctrl Pts',(157.487544347085,-225.672734038383,15.155307222412));
#77602=CARTESIAN_POINT('Ctrl Pts',(157.481369728344,-224.997804627087,15.112583302492));
#77603=CARTESIAN_POINT('Ctrl Pts',(157.478588566705,-225.000821673807,15.387416697508));
#77604=CARTESIAN_POINT('Ctrl Pts',(157.478396120234,-225.046004659762,15.390285101098));
#77605=CARTESIAN_POINT('Ctrl Pts',(157.479505484729,-225.091178003722,15.393153504688));
#77606=CARTESIAN_POINT('Ctrl Pts',(157.481946405746,-225.136279282669,15.396021908278));
#77607=CARTESIAN_POINT('Ctrl Pts',(157.526979051704,-225.96835451663,15.4489411966886));
#77608=CARTESIAN_POINT('Ctrl Pts',(158.025229628086,-226.775901196241,15.5018604850992));
#77609=CARTESIAN_POINT('Ctrl Pts',(158.748698680934,-227.189385976782,15.5547797735098));
#77610=CARTESIAN_POINT('Ctrl Pts',(159.472167733783,-227.602870757323,15.6076990619204));
#77611=CARTESIAN_POINT('Ctrl Pts',(160.420855263099,-227.622293638794,15.660618350331));
#77612=CARTESIAN_POINT('Ctrl Pts',(161.160641874123,-227.238766711032,15.7135376387416));
#77613=CARTESIAN_POINT('Ctrl Pts',(161.900428485148,-226.855239783271,15.7664569271522));
#77614=CARTESIAN_POINT('Ctrl Pts',(162.431314177881,-226.068763046276,15.8193762155628));
#77615=CARTESIAN_POINT('Ctrl Pts',(162.510365669759,-225.2392282394,15.8722955039734));
#77616=CARTESIAN_POINT('Ctrl Pts',(162.589417161637,-224.409693432523,15.925214792384));
#77617=CARTESIAN_POINT('Ctrl Pts',(162.21663445266,-223.537100555763,15.9781340807946));
#77618=CARTESIAN_POINT('Ctrl Pts',(161.562602903142,-223.020748092442,16.0310533692052));
#77619=CARTESIAN_POINT('Ctrl Pts',(160.908571353624,-222.50439562912,16.0839726576158));
#77620=CARTESIAN_POINT('Ctrl Pts',(159.973290963564,-222.344283579236,16.1368919460264));
#77621=CARTESIAN_POINT('Ctrl Pts',(159.184746021032,-222.613679213519,16.189811234437));
#77622=CARTESIAN_POINT('Ctrl Pts',(158.396201078501,-222.883074847802,16.2427305228476));
#77623=CARTESIAN_POINT('Ctrl Pts',(157.754391583496,-223.581978166253,16.2956498112582));
#77624=CARTESIAN_POINT('Ctrl Pts',(157.553009548383,-224.390571024399,16.3485690996688));
#77625=CARTESIAN_POINT('Ctrl Pts',(157.503731937471,-224.588431395745,16.3615182989485));
#77626=CARTESIAN_POINT('Ctrl Pts',(157.480825668259,-224.792859614458,16.3744674982283));
#77627=CARTESIAN_POINT('Ctrl Pts',(157.482688037232,-224.997698966056,16.387416697508));
#77628=CARTESIAN_POINT('Origin',(160.,-225.,10.));
#77629=CARTESIAN_POINT('',(157.486388068275,-225.000594615142,17.387416697508));
#77630=CARTESIAN_POINT('',(157.48179671173,-225.002256423607,17.112583302492));
#77631=CARTESIAN_POINT('',(157.4825,-225.,10.));
#77632=CARTESIAN_POINT('Ctrl Pts',(157.48179671173,-225.002256423607,17.112583302492));
#77633=CARTESIAN_POINT('Ctrl Pts',(157.487898020156,-224.341151277727,17.0707527282619));
#77634=CARTESIAN_POINT('Ctrl Pts',(157.755182207898,-223.675680124248,17.0289221540319));
#77635=CARTESIAN_POINT('Ctrl Pts',(158.222379318362,-223.211361021709,16.9870915798018));
#77636=CARTESIAN_POINT('Ctrl Pts',(158.813424004892,-222.623957263715,16.9341722913912));
#77637=CARTESIAN_POINT('Ctrl Pts',(159.724418023019,-222.358485991985,16.8812530029806));
#77638=CARTESIAN_POINT('Ctrl Pts',(160.53849052896,-222.536426856176,16.82833371457));
#77639=CARTESIAN_POINT('Ctrl Pts',(161.3525630349,-222.714367720367,16.7754144261594));
#77640=CARTESIAN_POINT('Ctrl Pts',(162.069714028654,-223.335720720481,16.7224951377488));
#77641=CARTESIAN_POINT('Ctrl Pts',(162.361775229099,-224.116154735432,16.6695758493382));
#77642=CARTESIAN_POINT('Ctrl Pts',(162.653836429543,-224.896588750382,16.6166565609276));
#77643=CARTESIAN_POINT('Ctrl Pts',(162.520807836678,-225.836103780169,16.563737272517));
#77644=CARTESIAN_POINT('Ctrl Pts',(162.023563332215,-226.504777765852,16.5108179841064));
#77645=CARTESIAN_POINT('Ctrl Pts',(161.526318827752,-227.173451751535,16.4578986956958));
#77646=CARTESIAN_POINT('Ctrl Pts',(160.664858411691,-227.571284693115,16.4049794072852));
#77647=CARTESIAN_POINT('Ctrl Pts',(159.833386353372,-227.516228244241,16.3520601188746));
#77648=CARTESIAN_POINT('Ctrl Pts',(159.001914295052,-227.461171795367,16.299140830464));
#77649=CARTESIAN_POINT('Ctrl Pts',(158.200430594475,-226.95322595604,16.2462215420534));
#77650=CARTESIAN_POINT('Ctrl Pts',(157.795694177318,-226.224826732399,16.1933022536428));
#77651=CARTESIAN_POINT('Ctrl Pts',(157.589909732952,-225.854478962444,16.1663959365925));
#77652=CARTESIAN_POINT('Ctrl Pts',(157.486689177846,-225.427141371915,16.1394896195423));
#77653=CARTESIAN_POINT('Ctrl Pts',(157.486513026464,-224.999883653202,16.112583302492));
#77654=CARTESIAN_POINT('Ctrl Pts',(157.482688037232,-224.997698966056,16.387416697508));
#77655=CARTESIAN_POINT('Ctrl Pts',(157.488436582161,-225.629973361099,16.4273867866389));
#77656=CARTESIAN_POINT('Ctrl Pts',(157.73017128722,-226.266164873843,16.4673568757697));
#77657=CARTESIAN_POINT('Ctrl Pts',(158.160758640894,-226.725212210085,16.5073269649006));
#77658=CARTESIAN_POINT('Ctrl Pts',(158.730844343742,-227.332978139783,16.5602462533112));
#77659=CARTESIAN_POINT('Ctrl Pts',(159.631970324661,-227.630227601337,16.6131655417218));
#77660=CARTESIAN_POINT('Ctrl Pts',(160.451781352795,-227.480939248318,16.6660848301324));
#77661=CARTESIAN_POINT('Ctrl Pts',(161.271592380928,-227.331650895299,16.719004118543));
#77662=CARTESIAN_POINT('Ctrl Pts',(162.010088456277,-226.735824727707,16.7719234069535));
#77663=CARTESIAN_POINT('Ctrl Pts',(162.32933378867,-225.966110785349,16.8248426953641));
#77664=CARTESIAN_POINT('Ctrl Pts',(162.648579121063,-225.196396842992,16.8777619837747));
#77665=CARTESIAN_POINT('Ctrl Pts',(162.5485737105,-224.252795125869,16.9306812721853));
#77666=CARTESIAN_POINT('Ctrl Pts',(162.075080032158,-223.567097766926,16.9836005605959));
#77667=CARTESIAN_POINT('Ctrl Pts',(161.601586353816,-222.881400407983,17.0365198490065));
#77668=CARTESIAN_POINT('Ctrl Pts',(160.754604407694,-222.453607407218,17.0894391374171));
#77669=CARTESIAN_POINT('Ctrl Pts',(159.921713113051,-222.479476821456,17.1423584258277));
#77670=CARTESIAN_POINT('Ctrl Pts',(159.088821818408,-222.505346235694,17.1952777142383));
#77671=CARTESIAN_POINT('Ctrl Pts',(158.270021175245,-222.984878064933,17.2481970026489));
#77672=CARTESIAN_POINT('Ctrl Pts',(157.839994347237,-223.698638578269,17.3011162910595));
#77673=CARTESIAN_POINT('Ctrl Pts',(157.606232763289,-224.086637133918,17.329883093209));
#77674=CARTESIAN_POINT('Ctrl Pts',(157.48735323228,-224.543849898541,17.3586498953585));
#77675=CARTESIAN_POINT('Ctrl Pts',(157.486388068275,-225.000594615142,17.387416697508));
#77676=CARTESIAN_POINT('Origin',(160.,-225.,10.));
#77677=CARTESIAN_POINT('',(157.480508436316,-225.001988388677,18.387416697508));
#77678=CARTESIAN_POINT('',(157.479093605947,-224.998703157778,18.112583302492));
#77679=CARTESIAN_POINT('',(157.4825,-225.,10.));
#77680=CARTESIAN_POINT('Ctrl Pts',(157.479093605947,-224.998703157778,18.112583302492));
#77681=CARTESIAN_POINT('Ctrl Pts',(157.478625726168,-224.92417432602,18.1078544138028));
#77682=CARTESIAN_POINT('Ctrl Pts',(157.481644431352,-224.849683927444,18.1031255251135));
#77683=CARTESIAN_POINT('Ctrl Pts',(157.488273116953,-224.775516169229,18.0983966364243));
#77684=CARTESIAN_POINT('Ctrl Pts',(157.562452347668,-223.945531526816,18.0454773480137));
#77685=CARTESIAN_POINT('Ctrl Pts',(158.088710912316,-223.155951269613,17.9925580596031));
#77686=CARTESIAN_POINT('Ctrl Pts',(158.826232736485,-222.768087153071,17.9396387711925));
#77687=CARTESIAN_POINT('Ctrl Pts',(159.563754560655,-222.38022303653,17.8867194827819));
#77688=CARTESIAN_POINT('Ctrl Pts',(160.512539644345,-222.39407506065,17.8338001943713));
#77689=CARTESIAN_POINT('Ctrl Pts',(161.238424031716,-222.803304614037,17.7808809059607));
#77690=CARTESIAN_POINT('Ctrl Pts',(161.964308419087,-223.212534167423,17.7279616175502));
#77691=CARTESIAN_POINT('Ctrl Pts',(162.467292110139,-224.017141250075,17.6750423291395));
#77692=CARTESIAN_POINT('Ctrl Pts',(162.517209739275,-224.848937640852,17.6221230407289));
#77693=CARTESIAN_POINT('Ctrl Pts',(162.567127368411,-225.680734031629,17.5692037523183));
#77694=CARTESIAN_POINT('Ctrl Pts',(162.16397893563,-226.539719730531,17.5162844639078));
#77695=CARTESIAN_POINT('Ctrl Pts',(161.492245174384,-227.032822915951,17.4633651754972));
#77696=CARTESIAN_POINT('Ctrl Pts',(160.820511413138,-227.525926101371,17.4104458870866));
#77697=CARTESIAN_POINT('Ctrl Pts',(159.880192323427,-227.653146773309,17.357526598676));
#77698=CARTESIAN_POINT('Ctrl Pts',(159.101577893279,-227.35626874644,17.3046073102654));
#77699=CARTESIAN_POINT('Ctrl Pts',(158.322963463131,-227.059390719571,17.2516880218548));
#77700=CARTESIAN_POINT('Ctrl Pts',(157.706053692547,-226.338413993894,17.1987687334442));
#77701=CARTESIAN_POINT('Ctrl Pts',(157.533146484722,-225.523257508927,17.1458494450336));
#77702=CARTESIAN_POINT('Ctrl Pts',(157.496915487198,-225.352449519144,17.134760730853));
#77703=CARTESIAN_POINT('Ctrl Pts',(157.480179338158,-225.177506372738,17.1236720166725));
#77704=CARTESIAN_POINT('Ctrl Pts',(157.48179671173,-225.002256423607,17.112583302492));
#77705=CARTESIAN_POINT('Ctrl Pts',(157.486388068275,-225.000594615142,17.387416697508));
#77706=CARTESIAN_POINT('Ctrl Pts',(157.48557772063,-225.384075560824,17.4115691837691));
#77707=CARTESIAN_POINT('Ctrl Pts',(157.567887699128,-225.767226569576,17.4357216700302));
#77708=CARTESIAN_POINT('Ctrl Pts',(157.735112675213,-226.108806281153,17.4598741562913));
#77709=CARTESIAN_POINT('Ctrl Pts',(158.101510844047,-226.857224273268,17.5127934447019));
#77710=CARTESIAN_POINT('Ctrl Pts',(158.875560194568,-227.406071060066,17.5657127331125));
#77711=CARTESIAN_POINT('Ctrl Pts',(159.703055782727,-227.504194469167,17.6186320215231));
#77712=CARTESIAN_POINT('Ctrl Pts',(160.530551370886,-227.602317878268,17.6715513099337));
#77713=CARTESIAN_POINT('Ctrl Pts',(161.411493196683,-227.249717909671,17.7244705983443));
#77714=CARTESIAN_POINT('Ctrl Pts',(161.942762249126,-226.607744081147,17.7773898867549));
#77715=CARTESIAN_POINT('Ctrl Pts',(162.474031301569,-225.965770252623,17.8303091751655));
#77716=CARTESIAN_POINT('Ctrl Pts',(162.655627580658,-225.034422564172,17.8832284635761));
#77717=CARTESIAN_POINT('Ctrl Pts',(162.404452733975,-224.239886158156,17.9361477519867));
#77718=CARTESIAN_POINT('Ctrl Pts',(162.153277887292,-223.445349752141,17.9890670403973));
#77719=CARTESIAN_POINT('Ctrl Pts',(161.469331914838,-222.787624628562,18.0419863288079));
#77720=CARTESIAN_POINT('Ctrl Pts',(160.665588269906,-222.567684839738,18.0949056172185));
#77721=CARTESIAN_POINT('Ctrl Pts',(159.861844624975,-222.347745050914,18.1478249056291));
#77722=CARTESIAN_POINT('Ctrl Pts',(158.938303307568,-222.565590596846,18.2007441940397));
#77723=CARTESIAN_POINT('Ctrl Pts',(158.317577242659,-223.121537334013,18.2536634824503));
#77724=CARTESIAN_POINT('Ctrl Pts',(157.794616652767,-223.589921457145,18.2982478874695));
#77725=CARTESIAN_POINT('Ctrl Pts',(157.486595301213,-224.298290891207,18.3428322924888));
#77726=CARTESIAN_POINT('Ctrl Pts',(157.480508436316,-225.001988388677,18.387416697508));
#77727=CARTESIAN_POINT('Origin',(160.,-225.,10.));
#77728=CARTESIAN_POINT('',(157.48014261364,-224.998176427436,19.387416697508));
#77729=CARTESIAN_POINT('',(157.485690666959,-224.998572567547,19.112583302492));
#77730=CARTESIAN_POINT('',(157.4825,-225.,10.));
#77731=CARTESIAN_POINT('',(161.913465996665,-223.364012796625,20.));
#77732=CARTESIAN_POINT('Ctrl Pts',(157.48014261364,-224.998176427436,19.387416697508));
#77733=CARTESIAN_POINT('Ctrl Pts',(157.486035940553,-225.714913366798,19.4328532664402));
#77734=CARTESIAN_POINT('Ctrl Pts',(157.807333049291,-226.436176607492,19.4782898353724));
#77735=CARTESIAN_POINT('Ctrl Pts',(158.347923879131,-226.905064937574,19.5237264043046));
#77736=CARTESIAN_POINT('Ctrl Pts',(158.97754188746,-227.451172122934,19.5766456927152));
#77737=CARTESIAN_POINT('Ctrl Pts',(159.904629866452,-227.654935000039,19.6295649811258));
#77738=CARTESIAN_POINT('Ctrl Pts',(160.704626517538,-227.421707597932,19.6824842695364));
#77739=CARTESIAN_POINT('Ctrl Pts',(161.504623168624,-227.188480195825,19.735403557947));
#77740=CARTESIAN_POINT('Ctrl Pts',(162.177528491803,-226.518262514506,19.7883228463576));
#77741=CARTESIAN_POINT('Ctrl Pts',(162.41573132851,-225.721203336705,19.8412421347682));
#77742=CARTESIAN_POINT('Ctrl Pts',(162.653934165218,-224.924144158904,19.8941614231788));
#77743=CARTESIAN_POINT('Ctrl Pts',(162.457434515453,-224.000243484621,19.9470807115894));
#77744=CARTESIAN_POINT('Ctrl Pts',(161.913465996665,-223.364012796625,20.));
#77745=CARTESIAN_POINT('',(158.082847463497,-223.361245209821,20.));
#77746=CARTESIAN_POINT('Origin',(160.,-225.,20.));
#77747=CARTESIAN_POINT('Ctrl Pts',(158.082843761452,-223.361242430594,20.));
#77748=CARTESIAN_POINT('Ctrl Pts',(158.613381559625,-222.742548892826,19.948244384658));
#77749=CARTESIAN_POINT('Ctrl Pts',(159.472376104806,-222.40287586538,19.896488769316));
#77750=CARTESIAN_POINT('Ctrl Pts',(160.282371278711,-222.494228189242,19.844733153974));
#77751=CARTESIAN_POINT('Ctrl Pts',(161.110578381185,-222.587634478424,19.7918138655634));
#77752=CARTESIAN_POINT('Ctrl Pts',(161.887557938352,-223.131666360088,19.7388945771528));
#77753=CARTESIAN_POINT('Ctrl Pts',(162.258271984796,-223.877852623269,19.6859752887422));
#77754=CARTESIAN_POINT('Ctrl Pts',(162.62898603124,-224.62403888645,19.6330560003316));
#77755=CARTESIAN_POINT('Ctrl Pts',(162.59343456696,-225.572379531148,19.5801367119211));
#77756=CARTESIAN_POINT('Ctrl Pts',(162.167641060891,-226.288685246806,19.5272174235105));
#77757=CARTESIAN_POINT('Ctrl Pts',(161.741847554822,-227.004990962463,19.4742981350999));
#77758=CARTESIAN_POINT('Ctrl Pts',(160.925812006964,-227.489261749081,19.4213788466893));
#77759=CARTESIAN_POINT('Ctrl Pts',(160.093070266903,-227.520005584259,19.3684595582787));
#77760=CARTESIAN_POINT('Ctrl Pts',(159.260328526843,-227.550749419438,19.3155402698681));
#77761=CARTESIAN_POINT('Ctrl Pts',(158.410880594581,-227.127966303179,19.2626209814575));
#77762=CARTESIAN_POINT('Ctrl Pts',(157.933376955139,-226.445068639568,19.2097016930469));
#77763=CARTESIAN_POINT('Ctrl Pts',(157.641269317644,-226.027313450515,19.1773288961952));
#77764=CARTESIAN_POINT('Ctrl Pts',(157.488352422676,-225.512216972223,19.1449560993436));
#77765=CARTESIAN_POINT('Ctrl Pts',(157.485690666959,-224.998572567547,19.112583302492));
#77766=CARTESIAN_POINT('Origin',(0.,225.,10.));
#77767=CARTESIAN_POINT('',(-2.51347389046773,225.0005858313,0.387416697508012));
#77768=CARTESIAN_POINT('',(-2.51553408751311,224.996405665924,0.112583302491965));
#77769=CARTESIAN_POINT('',(-2.5175,225.,10.));
#77770=CARTESIAN_POINT('',(-1.91346599666507,226.635987203375,0.));
#77771=CARTESIAN_POINT('Ctrl Pts',(-2.51553408751311,224.996405665924,0.112583302491965));
#77772=CARTESIAN_POINT('Ctrl Pts',(-2.51031901166848,225.589040573862,0.0750555349946381));
#77773=CARTESIAN_POINT('Ctrl Pts',(-2.29922182808404,226.184803560304,0.0375277674973117));
#77774=CARTESIAN_POINT('Ctrl Pts',(-1.91346599666503,226.635987203375,-1.50573997714787E-14));
#77775=CARTESIAN_POINT('',(1.91712510374251,226.63873942345,1.67669336393566E-15));
#77776=CARTESIAN_POINT('Origin',(0.,225.,0.));
#77777=CARTESIAN_POINT('Ctrl Pts',(1.91712867315962,226.638742108209,1.44285430635494E-15));
#77778=CARTESIAN_POINT('Ctrl Pts',(1.38658202527179,227.257482867444,0.0517556153419835));
#77779=CARTESIAN_POINT('Ctrl Pts',(0.527608291324034,227.597070351188,0.103511230683964));
#77780=CARTESIAN_POINT('Ctrl Pts',(-0.282369177537283,227.505702430347,
0.155266846025946));
#77781=CARTESIAN_POINT('Ctrl Pts',(-1.1105581768861,227.412280193503,0.208186134436544));
#77782=CARTESIAN_POINT('Ctrl Pts',(-1.88752287836714,226.868305491623,0.261105422847144));
#77783=CARTESIAN_POINT('Ctrl Pts',(-2.25823175842065,226.122142534186,0.314024711257743));
#77784=CARTESIAN_POINT('Ctrl Pts',(-2.42960632929949,225.777199740752,0.338488706674499));
#77785=CARTESIAN_POINT('Ctrl Pts',(-2.51415958122241,225.389047102439,0.362952702091256));
#77786=CARTESIAN_POINT('Ctrl Pts',(-2.51347389046773,225.0005858313,0.387416697508012));
#77787=CARTESIAN_POINT('Origin',(0.,225.,10.));
#77788=CARTESIAN_POINT('',(-2.51741847158745,224.997698802423,1.38741669750801));
#77789=CARTESIAN_POINT('',(-2.52168717967801,225.000137595091,1.11258330249197));
#77790=CARTESIAN_POINT('',(-2.5175,225.,10.));
#77791=CARTESIAN_POINT('Ctrl Pts',(-2.52168717967801,225.000137595091,1.11258330249197));
#77792=CARTESIAN_POINT('Ctrl Pts',(-2.52169204710937,225.006846738092,1.11215722053549));
#77793=CARTESIAN_POINT('Ctrl Pts',(-2.52166759919164,225.013555842314,1.11173113857901));
#77794=CARTESIAN_POINT('Ctrl Pts',(-2.52161372912346,225.020264707836,1.11130505662253));
#77795=CARTESIAN_POINT('Ctrl Pts',(-2.51492307810834,225.853504379485,1.05838576821194));
#77796=CARTESIAN_POINT('Ctrl Pts',(-2.05437847998888,226.683061975931,1.00546647980134));
#77797=CARTESIAN_POINT('Ctrl Pts',(-1.3507129006363,227.129421042381,0.952547191390737));
#77798=CARTESIAN_POINT('Ctrl Pts',(-0.647047321283738,227.575780108832,
0.899627902980141));
#77799=CARTESIAN_POINT('Ctrl Pts',(0.299739239301934,227.638940645286,0.846708614569544));
#77800=CARTESIAN_POINT('Ctrl Pts',(1.05637242882409,227.289819467046,0.793789326158948));
#77801=CARTESIAN_POINT('Ctrl Pts',(1.81300561834626,226.940698288805,0.740870037748351));
#77802=CARTESIAN_POINT('Ctrl Pts',(2.37948543680491,226.179295395871,0.687950749337752));
#77803=CARTESIAN_POINT('Ctrl Pts',(2.49664115114991,225.35439625556,0.635031460927153));
#77804=CARTESIAN_POINT('Ctrl Pts',(2.61379686549491,224.52949711525,0.582112172516556));
#77805=CARTESIAN_POINT('Ctrl Pts',(2.28162847572628,223.641101727564,0.529192884105959));
#77806=CARTESIAN_POINT('Ctrl Pts',(1.65203466276087,223.094991627842,0.476273595695361));
#77807=CARTESIAN_POINT('Ctrl Pts',(1.02244084979547,222.548881528121,0.423354307284765));
#77808=CARTESIAN_POINT('Ctrl Pts',(0.0954216136332989,222.345056716363,
0.370435018874169));
#77809=CARTESIAN_POINT('Ctrl Pts',(-0.704614902137573,222.578323517273,
0.317515730463573));
#77810=CARTESIAN_POINT('Ctrl Pts',(-1.50465141790847,222.811590318182,0.264596442052974));
#77811=CARTESIAN_POINT('Ctrl Pts',(-2.17770521328806,223.48194873176,0.211677153642374));
#77812=CARTESIAN_POINT('Ctrl Pts',(-2.41590098767414,224.278990281059,0.158757865231776));
#77813=CARTESIAN_POINT('Ctrl Pts',(-2.48517998504973,224.510809000532,0.143366344318505));
#77814=CARTESIAN_POINT('Ctrl Pts',(-2.51767298237096,224.75334424267,0.127974823405235));
#77815=CARTESIAN_POINT('Ctrl Pts',(-2.51553408751311,224.996405665924,0.112583302491965));
#77816=CARTESIAN_POINT('Ctrl Pts',(-2.51347389046773,225.0005858313,0.387416697508012));
#77817=CARTESIAN_POINT('Ctrl Pts',(-2.51267632935821,224.54874715578,0.415871990501853));
#77818=CARTESIAN_POINT('Ctrl Pts',(-2.39655750155179,224.096490925473,0.444327283495693));
#77819=CARTESIAN_POINT('Ctrl Pts',(-2.16760750705151,223.711328458468,0.472782576489533));
#77820=CARTESIAN_POINT('Ctrl Pts',(-1.74182131700286,222.995028553183,0.525701864900131));
#77821=CARTESIAN_POINT('Ctrl Pts',(-0.925795878279577,222.510779955607,
0.578621153310729));
#77822=CARTESIAN_POINT('Ctrl Pts',(-0.0930673453572587,222.480039920553,
0.631540441721328));
#77823=CARTESIAN_POINT('Ctrl Pts',(0.739661187565012,222.449299885498,0.684459730131924));
#77824=CARTESIAN_POINT('Ctrl Pts',(1.5890928146863,222.872068412965,0.73737901854252));
#77825=CARTESIAN_POINT('Ctrl Pts',(2.06658816412527,223.554953044849,0.790298306953116));
#77826=CARTESIAN_POINT('Ctrl Pts',(2.54408351356428,224.237837676734,0.843217595363715));
#77827=CARTESIAN_POINT('Ctrl Pts',(2.64964258532089,225.180838413036,0.896136883774315));
#77828=CARTESIAN_POINT('Ctrl Pts',(2.33493175115268,225.952405437576,0.949056172184913));
#77829=CARTESIAN_POINT('Ctrl Pts',(2.02022091698448,226.723972462116,1.00197546059551));
#77830=CARTESIAN_POINT('Ctrl Pts',(1.28524017689151,227.324105774894,1.05489474900611));
#77831=CARTESIAN_POINT('Ctrl Pts',(0.466331374739214,227.478200482608,1.1078140374167));
#77832=CARTESIAN_POINT('Ctrl Pts',(-0.352577427413085,227.632295190321,
1.1607333258273));
#77833=CARTESIAN_POINT('Ctrl Pts',(-1.2554142916247,227.34035129297,1.2136526142379));
#77834=CARTESIAN_POINT('Ctrl Pts',(-1.82904831020792,226.735954385945,1.2665719026485));
#77835=CARTESIAN_POINT('Ctrl Pts',(-2.26569241095164,226.275893902412,1.306853500935));
#77836=CARTESIAN_POINT('Ctrl Pts',(-2.5115933498986,225.634795266357,1.34713509922151));
#77837=CARTESIAN_POINT('Ctrl Pts',(-2.51741847158745,224.997698802423,1.38741669750801));
#77838=CARTESIAN_POINT('Origin',(0.,225.,10.));
#77839=CARTESIAN_POINT('',(-2.52129908879481,225.000905510379,2.38741669750801));
#77840=CARTESIAN_POINT('',(-2.51578353683605,225.002114845881,2.11258330249197));
#77841=CARTESIAN_POINT('',(-2.5175,225.,10.));
#77842=CARTESIAN_POINT('Ctrl Pts',(-2.51578353683605,225.002114845881,2.11258330249197));
#77843=CARTESIAN_POINT('Ctrl Pts',(-2.51783260554419,225.259450106344,2.09633961766574));
#77844=CARTESIAN_POINT('Ctrl Pts',(-2.48151008120921,225.516220723336,2.08009593283951));
#77845=CARTESIAN_POINT('Ctrl Pts',(-2.40441272483833,225.760101241637,2.06385224801329));
#77846=CARTESIAN_POINT('Ctrl Pts',(-2.15324205259667,226.554624382399,2.01093295960269));
#77847=CARTESIAN_POINT('Ctrl Pts',(-1.46930744293435,227.21233837926,1.95801367119209));
#77848=CARTESIAN_POINT('Ctrl Pts',(-0.665577185407848,227.432274590025,
1.9050943827815));
#77849=CARTESIAN_POINT('Ctrl Pts',(0.138153072118675,227.65221080079,1.8521750943709));
#77850=CARTESIAN_POINT('Ctrl Pts',(1.06167897750938,227.434369225459,1.7992558059603));
#77851=CARTESIAN_POINT('Ctrl Pts',(1.68239474048309,226.878431585785,1.7463365175497));
#77852=CARTESIAN_POINT('Ctrl Pts',(2.30311050345679,226.322493946112,1.6934172291391));
#77853=CARTESIAN_POINT('Ctrl Pts',(2.62101612401351,225.428460242096,1.64049794072851));
#77854=CARTESIAN_POINT('Ctrl Pts',(2.49063871562429,224.605445516318,1.58757865231791));
#77855=CARTESIAN_POINT('Ctrl Pts',(2.36026130723508,223.78243079054,1.53465936390731));
#77856=CARTESIAN_POINT('Ctrl Pts',(1.78160086989994,223.030435043,1.48174007549672));
#77857=CARTESIAN_POINT('Ctrl Pts',(1.01945094781155,222.693560877067,1.42882078708612));
#77858=CARTESIAN_POINT('Ctrl Pts',(0.257301025723131,222.356686711134,1.37590149867552));
#77859=CARTESIAN_POINT('Ctrl Pts',(-0.688338381118543,222.434934126809,
1.32298221026492));
#77860=CARTESIAN_POINT('Ctrl Pts',(-1.38473973258398,222.892518708072,1.27006292185432));
#77861=CARTESIAN_POINT('Ctrl Pts',(-2.07553397822393,223.346419027141,1.2175697154002));
#77862=CARTESIAN_POINT('Ctrl Pts',(-2.52108751316975,224.173572603789,1.16507650894609));
#77863=CARTESIAN_POINT('Ctrl Pts',(-2.52168717967801,225.000137595091,1.11258330249197));
#77864=CARTESIAN_POINT('Ctrl Pts',(-2.51741847158745,224.997698802423,1.38741669750801));
#77865=CARTESIAN_POINT('Ctrl Pts',(-2.5192460078812,224.797820246635,1.4000543876321));
#77866=CARTESIAN_POINT('Ctrl Pts',(-2.49744317904368,224.598335619689,1.4126920777562));
#77867=CARTESIAN_POINT('Ctrl Pts',(-2.45048657256469,224.404959042237,1.42532976788029));
#77868=CARTESIAN_POINT('Ctrl Pts',(-2.25385964338344,223.595210522252,1.47824905629088));
#77869=CARTESIAN_POINT('Ctrl Pts',(-1.61617461206615,222.892563398979,1.53116834470149));
#77870=CARTESIAN_POINT('Ctrl Pts',(-0.829237887491455,222.618547060792,
1.58408763311208));
#77871=CARTESIAN_POINT('Ctrl Pts',(-0.0423011629167494,222.344530722605,
1.63700692152268));
#77872=CARTESIAN_POINT('Ctrl Pts',(0.893887254915367,222.499145169502,1.68992620993328));
#77873=CARTESIAN_POINT('Ctrl Pts',(1.55092842656392,223.011639779642,1.74284549834387));
#77874=CARTESIAN_POINT('Ctrl Pts',(2.20796959821247,223.524134389781,1.79576478675447));
#77875=CARTESIAN_POINT('Ctrl Pts',(2.58586352367745,224.394509163162,1.84868407516507));
#77876=CARTESIAN_POINT('Ctrl Pts',(2.5116855256137,225.224480154825,1.90160336357567));
#77877=CARTESIAN_POINT('Ctrl Pts',(2.43750752754995,226.054451146488,1.95452265198626));
#77878=CARTESIAN_POINT('Ctrl Pts',(1.91125760595749,226.844018356432,2.00744194039686));
#77879=CARTESIAN_POINT('Ctrl Pts',(1.17374792360493,227.231876074238,2.06036122880746));
#77880=CARTESIAN_POINT('Ctrl Pts',(0.436238241252373,227.619733792044,2.11328051721805));
#77881=CARTESIAN_POINT('Ctrl Pts',(-0.512531201860274,227.60588201771,2.16619980562865));
#77882=CARTESIAN_POINT('Ctrl Pts',(-1.23840363011865,227.196659209991,2.21911909403925));
#77883=CARTESIAN_POINT('Ctrl Pts',(-1.96427605837704,226.787436402272,2.27203838244985));
#77884=CARTESIAN_POINT('Ctrl Pts',(-2.46725147178114,225.982842561167,2.32495767086044));
#77885=CARTESIAN_POINT('Ctrl Pts',(-2.51716828038405,225.151059868138,2.37787695927104));
#77886=CARTESIAN_POINT('Ctrl Pts',(-2.52016777453195,225.101078160775,2.3810568720167));
#77887=CARTESIAN_POINT('Ctrl Pts',(-2.52153136850561,225.050998280136,2.38423678476236));
#77888=CARTESIAN_POINT('Ctrl Pts',(-2.52129908879481,225.000905510379,2.38741669750801));
#77889=CARTESIAN_POINT('Origin',(0.,225.,10.));
#77890=CARTESIAN_POINT('',(-2.51474241101028,225.001726207962,3.38741669750801));
#77891=CARTESIAN_POINT('',(-2.51418867251095,224.99863370625,3.11258330249198));
#77892=CARTESIAN_POINT('',(-2.5175,225.,10.));
#77893=CARTESIAN_POINT('Ctrl Pts',(-2.51418867251095,224.99863370625,3.11258330249198));
#77894=CARTESIAN_POINT('Ctrl Pts',(-2.51168135695882,225.507365063915,3.080522014796));
#77895=CARTESIAN_POINT('Ctrl Pts',(-2.36190809597984,226.01745378504,3.04846072710002));
#77896=CARTESIAN_POINT('Ctrl Pts',(-2.07504550059781,226.432878388949,3.01639943940404));
#77897=CARTESIAN_POINT('Ctrl Pts',(-1.60155970167469,227.118564336299,2.96348015099344));
#77898=CARTESIAN_POINT('Ctrl Pts',(-0.754591850175153,227.546350214638,
2.91056086258285));
#77899=CARTESIAN_POINT('Ctrl Pts',(0.0782855841932958,227.520481232549,
2.85764157417225));
#77900=CARTESIAN_POINT('Ctrl Pts',(0.911163018561756,227.49461225046,2.80472228576165));
#77901=CARTESIAN_POINT('Ctrl Pts',(1.72995003579915,227.015088407943,2.75180299735105));
#77902=CARTESIAN_POINT('Ctrl Pts',(2.15996970786875,226.301339769147,2.69888370894046));
#77903=CARTESIAN_POINT('Ctrl Pts',(2.58998937993835,225.58759113035,2.64596442052986));
#77904=CARTESIAN_POINT('Ctrl Pts',(2.63124170684017,224.639617695274,2.59304513211926));
#77905=CARTESIAN_POINT('Ctrl Pts',(2.26484963484653,223.891212163822,2.54012584370866));
#77906=CARTESIAN_POINT('Ctrl Pts',(1.89845756285288,223.14280663237,2.48720655529807));
#77907=CARTESIAN_POINT('Ctrl Pts',(1.12442109196377,222.593969004542,2.43428726688747));
#77908=CARTESIAN_POINT('Ctrl Pts',(0.296939275219781,222.495847216434,2.38136797847687));
#77909=CARTESIAN_POINT('Ctrl Pts',(-0.530542541524199,222.397725428326,
2.32844869006628));
#77910=CARTESIAN_POINT('Ctrl Pts',(-1.41146970412308,222.750319479939,2.27552940165568));
#77911=CARTESIAN_POINT('Ctrl Pts',(-1.94272991801202,223.392282648076,2.22261011324508));
#77912=CARTESIAN_POINT('Ctrl Pts',(-2.31091871249395,223.83719389646,2.18593450966071));
#77913=CARTESIAN_POINT('Ctrl Pts',(-2.51115707230781,224.421093599656,2.14925890607634));
#77914=CARTESIAN_POINT('Ctrl Pts',(-2.51578353683605,225.002114845881,2.11258330249197));
#77915=CARTESIAN_POINT('Ctrl Pts',(-2.52129908879481,225.000905510379,2.38741669750801));
#77916=CARTESIAN_POINT('Ctrl Pts',(-2.51766582941986,224.217367315361,2.43715607317295));
#77917=CARTESIAN_POINT('Ctrl Pts',(-2.12357956846045,223.430675615842,2.4868954488379));
#77918=CARTESIAN_POINT('Ctrl Pts',(-1.49222059474684,222.967210567987,2.53663482450284));
#77919=CARTESIAN_POINT('Ctrl Pts',(-0.820497896705034,222.474115505819,
2.58955411291343));
#77920=CARTESIAN_POINT('Ctrl Pts',(0.119805703180309,222.346896926438,2.64247340132403));
#77921=CARTESIAN_POINT('Ctrl Pts',(0.898407308371105,222.643770062743,2.69539268973463));
#77922=CARTESIAN_POINT('Ctrl Pts',(1.67700891356191,222.940643199048,2.74831197814523));
#77923=CARTESIAN_POINT('Ctrl Pts',(2.29390852405818,223.661608051039,2.80123126655583));
#77924=CARTESIAN_POINT('Ctrl Pts',(2.46681288417962,224.476751109985,2.85415055496642));
#77925=CARTESIAN_POINT('Ctrl Pts',(2.63971724430104,225.291894168932,2.90706984337702));
#77926=CARTESIAN_POINT('Ctrl Pts',(2.3686263540477,226.201215434834,2.95998913178762));
#77927=CARTESIAN_POINT('Ctrl Pts',(1.7775914024464,226.78860951756,3.01290842019821));
#77928=CARTESIAN_POINT('Ctrl Pts',(1.18655645084507,227.376003600287,3.06582770860881));
#77929=CARTESIAN_POINT('Ctrl Pts',(0.275577437895753,227.641470499838,3.11874699701941));
#77930=CARTESIAN_POINT('Ctrl Pts',(-0.538481659453402,227.463532566591,
3.17166628543));
#77931=CARTESIAN_POINT('Ctrl Pts',(-1.35254075680253,227.285594633344,3.2245855738406));
#77932=CARTESIAN_POINT('Ctrl Pts',(-2.06967993855152,226.664251867297,3.2775048622512));
#77933=CARTESIAN_POINT('Ctrl Pts',(-2.36173632851075,225.88383070677,3.33042415066179));
#77934=CARTESIAN_POINT('Ctrl Pts',(-2.46658176380421,225.603667015439,3.3494216662772));
#77935=CARTESIAN_POINT('Ctrl Pts',(-2.51664503896433,225.30300223997,3.36841918189261));
#77936=CARTESIAN_POINT('Ctrl Pts',(-2.51474241101028,225.001726207962,3.38741669750801));
#77937=CARTESIAN_POINT('Origin',(0.,225.,10.));
#77938=CARTESIAN_POINT('',(-2.5150539014468,224.998127144802,4.38741669750802));
#77939=CARTESIAN_POINT('',(-2.52076226691227,224.998630464431,4.11258330249197));
#77940=CARTESIAN_POINT('',(-2.5175,225.,10.));
#77941=CARTESIAN_POINT('Ctrl Pts',(-2.52076226691227,224.998630464431,4.11258330249197));
#77942=CARTESIAN_POINT('Ctrl Pts',(-2.51581102366626,225.753285751347,4.06470441192625));
#77943=CARTESIAN_POINT('Ctrl Pts',(-2.15430412856549,226.512055249875,4.01682552136052));
#77944=CARTESIAN_POINT('Ctrl Pts',(-1.56257689974821,226.979218970693,3.9689466307948));
#77945=CARTESIAN_POINT('Ctrl Pts',(-0.908556234018705,227.495562841339,
3.9160273423842));
#77946=CARTESIAN_POINT('Ctrl Pts',(0.0267085919674362,227.655672226725,
3.8631080539736));
#77947=CARTESIAN_POINT('Ctrl Pts',(0.815240412263574,227.386281075505,3.810188765563));
#77948=CARTESIAN_POINT('Ctrl Pts',(1.60377223255971,227.116889924285,3.75726947715241));
#77949=CARTESIAN_POINT('Ctrl Pts',(2.24557104716584,226.417998236458,3.70435018874181));
#77950=CARTESIAN_POINT('Ctrl Pts',(2.44694973106533,225.609418834108,3.65143090033121));
#77951=CARTESIAN_POINT('Ctrl Pts',(2.64832841496483,224.800839431759,3.59851161192062));
#77952=CARTESIAN_POINT('Ctrl Pts',(2.40928696815766,223.882572314887,3.54559232351002));
#77953=CARTESIAN_POINT('Ctrl Pts',(1.83921075214889,223.274816499182,3.49267303509942));
#77954=CARTESIAN_POINT('Ctrl Pts',(1.26913453614011,222.667060683477,3.43975374668882));
#77955=CARTESIAN_POINT('Ctrl Pts',(0.368023550929722,222.36981616894,3.38683445827822));
#77956=CARTESIAN_POINT('Ctrl Pts',(-0.451773834664424,222.519102037416,
3.33391516986763));
#77957=CARTESIAN_POINT('Ctrl Pts',(-1.27157122025857,222.668387905892,3.28099588145703));
#77958=CARTESIAN_POINT('Ctrl Pts',(-2.01005500623649,223.264204157383,3.22807659304643));
#77959=CARTESIAN_POINT('Ctrl Pts',(-2.32929502605208,224.033905291309,3.17515730463584));
#77960=CARTESIAN_POINT('Ctrl Pts',(-2.45512265453008,224.337281003336,3.15429930392122));
#77961=CARTESIAN_POINT('Ctrl Pts',(-2.51581984809172,224.667670111702,3.1334413032066));
#77962=CARTESIAN_POINT('Ctrl Pts',(-2.51418867251095,224.99863370625,3.11258330249198));
#77963=CARTESIAN_POINT('Ctrl Pts',(-2.51474241101028,225.001726207962,3.38741669750801));
#77964=CARTESIAN_POINT('Ctrl Pts',(-2.51134509767322,224.46377075561,3.4213384703032));
#77965=CARTESIAN_POINT('Ctrl Pts',(-2.34226326168293,223.923866414815,3.4552602430984));
#77966=CARTESIAN_POINT('Ctrl Pts',(-2.02353000223652,223.495247019255,3.48918201589359));
#77967=CARTESIAN_POINT('Ctrl Pts',(-1.52629368783361,222.826584047275,3.54210130430419));
#77968=CARTESIAN_POINT('Ctrl Pts',(-0.664847460858349,222.428757658323,
3.59502059271478));
#77969=CARTESIAN_POINT('Ctrl Pts',(0.166610902338107,222.483813200354,3.64793988112538));
#77970=CARTESIAN_POINT('Ctrl Pts',(0.998069265534564,222.538868742386,3.70085916953598));
#77971=CARTESIAN_POINT('Ctrl Pts',(1.79953976495221,223.046806215399,3.75377845794658));
#77972=CARTESIAN_POINT('Ctrl Pts',(2.20426951572994,223.775193441637,3.80669774635718));
#77973=CARTESIAN_POINT('Ctrl Pts',(2.60899926650765,224.503580667874,3.85961703476777));
#77974=CARTESIAN_POINT('Ctrl Pts',(2.61698826864545,225.452417647336,3.91253632317837));
#77975=CARTESIAN_POINT('Ctrl Pts',(2.22458075496457,226.187516596923,3.96545561158897));
#77976=CARTESIAN_POINT('Ctrl Pts',(1.83217324128368,226.922615546509,4.01837489999956));
#77977=CARTESIAN_POINT('Ctrl Pts',(1.0393692117841,227.443976466221,4.07129418841016));
#77978=CARTESIAN_POINT('Ctrl Pts',(0.208955774755814,227.513024609426,4.12421347682076));
#77979=CARTESIAN_POINT('Ctrl Pts',(-0.621457662272467,227.58207275263,4.17713276523136));
#77980=CARTESIAN_POINT('Ctrl Pts',(-1.48948050682944,227.198808119328,4.23005205364195));
#77981=CARTESIAN_POINT('Ctrl Pts',(-1.99790552230265,226.538612598193,4.28297134205255));
#77982=CARTESIAN_POINT('Ctrl Pts',(-2.33239371528771,226.104275970056,4.3177864605377));
#77983=CARTESIAN_POINT('Ctrl Pts',(-2.51124061715918,225.550077992808,4.35260157902286));
#77984=CARTESIAN_POINT('Ctrl Pts',(-2.5150539014468,224.998127144802,4.38741669750802));
#77985=CARTESIAN_POINT('Origin',(0.,225.,10.));
#77986=CARTESIAN_POINT('',(-2.52148472081105,224.999338741875,5.38741669750802));
#77987=CARTESIAN_POINT('',(-2.51831101426404,225.002238014691,5.11258330249197));
#77988=CARTESIAN_POINT('',(-2.5175,225.,10.));
#77989=CARTESIAN_POINT('Ctrl Pts',(-2.51831101426404,225.002238014691,5.11258330249197));
#77990=CARTESIAN_POINT('Ctrl Pts',(-2.51987982331657,225.172535980322,5.1018060974671));
#77991=CARTESIAN_POINT('Ctrl Pts',(-2.50407981832776,225.342544535845,5.09102889244222));
#77992=CARTESIAN_POINT('Ctrl Pts',(-2.46984258279024,225.50875526306,5.08025168741734));
#77993=CARTESIAN_POINT('Ctrl Pts',(-2.3017275531875,226.324899466508,5.02733239900675));
#77994=CARTESIAN_POINT('Ctrl Pts',(-1.68907196797494,227.049474130712,4.97441311059615));
#77995=CARTESIAN_POINT('Ctrl Pts',(-0.912227010900041,227.350913903579,
4.92149382218555));
#77996=CARTESIAN_POINT('Ctrl Pts',(-0.135382053825148,227.652353676446,
4.86857453377495));
#77997=CARTESIAN_POINT('Ctrl Pts',(0.805652275112092,227.530658557975,4.81565524536436));
#77998=CARTESIAN_POINT('Ctrl Pts',(1.48025868549315,227.041516231988,4.76273595695376));
#77999=CARTESIAN_POINT('Ctrl Pts',(2.15486509587421,226.552373906002,4.70981666854316));
#78000=CARTESIAN_POINT('Ctrl Pts',(2.56304358769908,225.695784372502,4.65689738013257));
#78001=CARTESIAN_POINT('Ctrl Pts',(2.51801169113329,224.863722985166,4.60397809172197));
#78002=CARTESIAN_POINT('Ctrl Pts',(2.4729797945675,224.031661597831,4.55105880331137));
#78003=CARTESIAN_POINT('Ctrl Pts',(1.97473750961105,223.224128356661,4.49813951490077));
#78004=CARTESIAN_POINT('Ctrl Pts',(1.25128049606563,222.810650456954,4.44522022649017));
#78005=CARTESIAN_POINT('Ctrl Pts',(0.527823482520219,222.397172557246,4.39230093807958));
#78006=CARTESIAN_POINT('Ctrl Pts',(-0.420848259614152,222.377749999001,
4.33938164966898));
#78007=CARTESIAN_POINT('Ctrl Pts',(-1.16062255979383,222.761270544458,4.28646236125838));
#78008=CARTESIAN_POINT('Ctrl Pts',(-1.90039685997351,223.144791089915,4.23354307284779));
#78009=CARTESIAN_POINT('Ctrl Pts',(-2.43127371819849,223.931254739075,4.18062378443719));
#78010=CARTESIAN_POINT('Ctrl Pts',(-2.51032389457454,224.760775741608,4.12770449602659));
#78011=CARTESIAN_POINT('Ctrl Pts',(-2.51785317833117,224.839785040467,4.12266409818172));
#78012=CARTESIAN_POINT('Ctrl Pts',(-2.52128350363041,224.919184954378,4.11762370033684));
#78013=CARTESIAN_POINT('Ctrl Pts',(-2.52076226691227,224.998630464431,4.11258330249197));
#78014=CARTESIAN_POINT('Ctrl Pts',(-2.5150539014468,224.998127144802,4.38741669750802));
#78015=CARTESIAN_POINT('Ctrl Pts',(-2.51703684304577,224.711107815914,4.40552086743346));
#78016=CARTESIAN_POINT('Ctrl Pts',(-2.47168908238452,224.424696131468,4.4236250373589));
#78017=CARTESIAN_POINT('Ctrl Pts',(-2.37628376391044,224.156062397605,4.44172920728435));
#78018=CARTESIAN_POINT('Ctrl Pts',(-2.0974098036556,223.370834127117,4.49464849569494));
#78019=CARTESIAN_POINT('Ctrl Pts',(-1.39083469675649,222.73750399511,4.54756778410554));
#78020=CARTESIAN_POINT('Ctrl Pts',(-0.579887198234946,222.545883857538,
4.60048707251614));
#78021=CARTESIAN_POINT('Ctrl Pts',(0.231060300286584,222.354263719967,4.65340636092673));
#78022=CARTESIAN_POINT('Ctrl Pts',(1.14638019043053,222.604353576832,4.70632564933733));
#78023=CARTESIAN_POINT('Ctrl Pts',(1.74722210846285,223.181712314548,4.75924493774793));
#78024=CARTESIAN_POINT('Ctrl Pts',(2.34806402649518,223.759071052265,4.81216422615853));
#78025=CARTESIAN_POINT('Ctrl Pts',(2.63442797241588,224.663698670832,4.86508351456912));
#78026=CARTESIAN_POINT('Ctrl Pts',(2.47527381020271,225.481637589781,4.91800280297972));
#78027=CARTESIAN_POINT('Ctrl Pts',(2.31611964798954,226.29957650873,4.97092209139032));
#78028=CARTESIAN_POINT('Ctrl Pts',(1.71144737764256,227.030826728061,5.02384137980092));
#78029=CARTESIAN_POINT('Ctrl Pts',(0.937955018183124,227.340768161786,5.07676066821151));
#78030=CARTESIAN_POINT('Ctrl Pts',(0.164462658723686,227.650709595511,5.12967995662211));
#78031=CARTESIAN_POINT('Ctrl Pts',(-0.777849789848224,227.539342243629,
5.18259924503271));
#78032=CARTESIAN_POINT('Ctrl Pts',(-1.45778016959366,227.057627804173,5.23551853344331));
#78033=CARTESIAN_POINT('Ctrl Pts',(-2.10833172635816,226.596727559325,5.28615125479821));
#78034=CARTESIAN_POINT('Ctrl Pts',(-2.51868566269795,225.796793135942,5.33678397615311));
#78035=CARTESIAN_POINT('Ctrl Pts',(-2.52148472081105,224.999338741875,5.38741669750802));
#78036=CARTESIAN_POINT('Origin',(0.,225.,10.));
#78037=CARTESIAN_POINT('',(-2.51699557978349,225.002292230688,6.38741669750802));
#78038=CARTESIAN_POINT('',(-2.51344096553148,224.999964780717,6.11258330249198));
#78039=CARTESIAN_POINT('',(-2.5175,225.,10.));
#78040=CARTESIAN_POINT('Ctrl Pts',(-2.51344096553148,224.999964780717,6.11258330249198));
#78041=CARTESIAN_POINT('Ctrl Pts',(-2.5133882653449,225.422270773897,6.08598849459735));
#78042=CARTESIAN_POINT('Ctrl Pts',(-2.41266885591251,225.844600385848,6.05939368670273));
#78043=CARTESIAN_POINT('Ctrl Pts',(-2.21142314859194,226.211842382213,6.0327988788081));
#78044=CARTESIAN_POINT('Ctrl Pts',(-1.8109773296453,226.942593482169,5.9798795903975));
#78045=CARTESIAN_POINT('Ctrl Pts',(-1.01250319828182,227.455228217279,5.9269603019869));
#78046=CARTESIAN_POINT('Ctrl Pts',(-0.181382501313819,227.515164942836,
5.87404101357631));
#78047=CARTESIAN_POINT('Ctrl Pts',(0.649738195654195,227.575101668393,5.82112172516571));
#78048=CARTESIAN_POINT('Ctrl Pts',(1.51350545822674,227.182340384398,5.76820243675511));
#78049=CARTESIAN_POINT('Ctrl Pts',(2.01465940403403,226.516608646683,5.71528314834452));
#78050=CARTESIAN_POINT('Ctrl Pts',(2.51581334984132,225.850876908968,5.66236385993392));
#78051=CARTESIAN_POINT('Ctrl Pts',(2.65435397888336,224.912174717534,5.60944457152332));
#78052=CARTESIAN_POINT('Ctrl Pts',(2.36688510203449,224.130052176724,5.55652528311272));
#78053=CARTESIAN_POINT('Ctrl Pts',(2.07941622518562,223.347929635915,5.50360599470212));
#78054=CARTESIAN_POINT('Ctrl Pts',(1.36593784244583,222.722386745729,5.45068670629153));
#78055=CARTESIAN_POINT('Ctrl Pts',(0.552937647728462,222.539671920418,5.39776741788093));
#78056=CARTESIAN_POINT('Ctrl Pts',(-0.260062546988908,222.356957095107,
5.34484812947033));
#78057=CARTESIAN_POINT('Ctrl Pts',(-1.17258455368387,222.617070334669,5.29192884105973));
#78058=CARTESIAN_POINT('Ctrl Pts',(-1.76705832003488,223.200983825795,5.23900955264914));
#78059=CARTESIAN_POINT('Ctrl Pts',(-2.24046534769195,223.66598121658,5.19686746926341));
#78060=CARTESIAN_POINT('Ctrl Pts',(-2.51217650334442,224.336322218207,5.15472538587769));
#78061=CARTESIAN_POINT('Ctrl Pts',(-2.51831101426404,225.002238014691,5.11258330249197));
#78062=CARTESIAN_POINT('Ctrl Pts',(-2.52148472081105,224.999338741875,5.38741669750802));
#78063=CARTESIAN_POINT('Ctrl Pts',(-2.52161112590833,224.963325806029,5.38970326456371));
#78064=CARTESIAN_POINT('Ctrl Pts',(-2.52090635798137,224.927317927988,5.39198983161941));
#78065=CARTESIAN_POINT('Ctrl Pts',(-2.51935500348403,224.891346561095,5.3942763986751));
#78066=CARTESIAN_POINT('Ctrl Pts',(-2.48345114670998,224.058841284505,5.4471956870857));
#78067=CARTESIAN_POINT('Ctrl Pts',(-1.99409512224288,223.245892258356,5.50011497549629));
#78068=CARTESIAN_POINT('Ctrl Pts',(-1.2752162372571,222.82450494103,5.55303426390689));
#78069=CARTESIAN_POINT('Ctrl Pts',(-0.556337352271339,222.403117623704,
5.60595355231749));
#78070=CARTESIAN_POINT('Ctrl Pts',(0.392064393233094,222.373292015201,5.65887284072809));
#78071=CARTESIAN_POINT('Ctrl Pts',(1.13600037916085,222.748676313385,5.71179212913868));
#78072=CARTESIAN_POINT('Ctrl Pts',(1.87993636508862,223.124060611569,5.76471141754928));
#78073=CARTESIAN_POINT('Ctrl Pts',(2.41940659143971,223.904654816441,5.81763070595988));
#78074=CARTESIAN_POINT('Ctrl Pts',(2.50754949324294,224.733259035199,5.87054999437047));
#78075=CARTESIAN_POINT('Ctrl Pts',(2.59569239504618,225.561863253957,5.92346928278107));
#78076=CARTESIAN_POINT('Ctrl Pts',(2.23250797230156,226.438477486601,5.97638857119167));
#78077=CARTESIAN_POINT('Ctrl Pts',(1.58418940971608,226.961963077509,6.02930785960227));
#78078=CARTESIAN_POINT('Ctrl Pts',(0.935870847130601,227.485448668418,6.08222714801287));
#78079=CARTESIAN_POINT('Ctrl Pts',(0.00241814470426038,227.65580561759,
6.13514643642346));
#78080=CARTESIAN_POINT('Ctrl Pts',(-0.789020759286212,227.395078588435,
6.18806572483406));
#78081=CARTESIAN_POINT('Ctrl Pts',(-1.58045966327668,227.13435155928,6.24098501324466));
#78082=CARTESIAN_POINT('Ctrl Pts',(-2.22988476883129,226.442540551798,6.29390430165526));
#78083=CARTESIAN_POINT('Ctrl Pts',(-2.44011916041725,225.63621826941,6.34682359006585));
#78084=CARTESIAN_POINT('Ctrl Pts',(-2.4938744010362,225.430048156236,6.36035462587991));
#78085=CARTESIAN_POINT('Ctrl Pts',(-2.51891606819546,225.216391482443,6.37388566169396));
#78086=CARTESIAN_POINT('Ctrl Pts',(-2.51699557978349,225.002292230688,6.38741669750802));
#78087=CARTESIAN_POINT('Origin',(0.,225.,10.));
#78088=CARTESIAN_POINT('',(-2.51364339850779,224.999260136873,7.38741669750802));
#78089=CARTESIAN_POINT('',(-2.51844027096952,224.997780461794,7.11258330249198));
#78090=CARTESIAN_POINT('',(-2.5175,225.,10.));
#78091=CARTESIAN_POINT('Ctrl Pts',(-2.51844027096952,224.997780461794,7.11258330249198));
#78092=CARTESIAN_POINT('Ctrl Pts',(-2.51228349286758,225.667879389382,7.0701708917276));
#78093=CARTESIAN_POINT('Ctrl Pts',(-2.23669063730925,226.342450530656,7.02775848096323));
#78094=CARTESIAN_POINT('Ctrl Pts',(-1.75786844049796,226.807996915748,6.98534607019885));
#78095=CARTESIAN_POINT('Ctrl Pts',(-1.1604270436572,227.388873668029,6.93242678178825));
#78096=CARTESIAN_POINT('Ctrl Pts',(-0.246591469036519,227.644333748386,
6.87950749337766));
#78097=CARTESIAN_POINT('Ctrl Pts',(0.565467142385517,227.45747862907,6.82658820496706));
#78098=CARTESIAN_POINT('Ctrl Pts',(1.37752575380754,227.270623509755,6.77366891655647));
#78099=CARTESIAN_POINT('Ctrl Pts',(2.08780740203091,226.641453190767,6.72074962814587));
#78100=CARTESIAN_POINT('Ctrl Pts',(2.37128721879421,225.857875997705,6.66783033973527));
#78101=CARTESIAN_POINT('Ctrl Pts',(2.65476703555751,225.074298804643,6.61491105132467));
#78102=CARTESIAN_POINT('Ctrl Pts',(2.51144502086071,224.136314737507,6.56199176291408));
#78103=CARTESIAN_POINT('Ctrl Pts',(2.00690532581108,223.473145286975,6.50907247450348));
#78104=CARTESIAN_POINT('Ctrl Pts',(1.50236563076145,222.809975836444,6.45615318609288));
#78105=CARTESIAN_POINT('Ctrl Pts',(0.63660825535895,222.421621002517,6.40323389768228));
#78106=CARTESIAN_POINT('Ctrl Pts',(-0.194196242434726,222.485791949564,
6.35031460927168));
#78107=CARTESIAN_POINT('Ctrl Pts',(-1.02500074022841,222.549962896611,6.29739532086108));
#78108=CARTESIAN_POINT('Ctrl Pts',(-1.8208523604133,223.066659624631,6.24447603245049));
#78109=CARTESIAN_POINT('Ctrl Pts',(-2.21756941724085,223.799441721043,6.19155674403989));
#78110=CARTESIAN_POINT('Ctrl Pts',(-2.4149146716173,224.163961135396,6.16523226352392));
#78111=CARTESIAN_POINT('Ctrl Pts',(-2.51349313003819,224.581951387528,6.13890778300795));
#78112=CARTESIAN_POINT('Ctrl Pts',(-2.51344096553148,224.999964780717,6.11258330249198));
#78113=CARTESIAN_POINT('Ctrl Pts',(-2.51699557978349,225.002292230688,6.38741669750802));
#78114=CARTESIAN_POINT('Ctrl Pts',(-2.51140512213347,224.379058686358,6.42680495010456));
#78115=CARTESIAN_POINT('Ctrl Pts',(-2.27734636356429,223.752074884207,6.4661932027011));
#78116=CARTESIAN_POINT('Ctrl Pts',(-1.85802060188977,223.295091015239,6.50558145529765));
#78117=CARTESIAN_POINT('Ctrl Pts',(-1.29464397415902,222.681119600751,6.55850074370824));
#78118=CARTESIAN_POINT('Ctrl Pts',(-0.396847041080206,222.37401032907,6.61142003211884));
#78119=CARTESIAN_POINT('Ctrl Pts',(0.424538338422313,222.514296396878,6.66433932052944));
#78120=CARTESIAN_POINT('Ctrl Pts',(1.24592371792485,222.654582464686,6.71725860894004));
#78121=CARTESIAN_POINT('Ctrl Pts',(1.99089754385111,223.242263871983,6.77017789735063));
#78122=CARTESIAN_POINT('Ctrl Pts',(2.31855980810489,224.008417618346,6.82309718576123));
#78123=CARTESIAN_POINT('Ctrl Pts',(2.64622207235867,224.774571364709,6.87601647417183));
#78124=CARTESIAN_POINT('Ctrl Pts',(2.55657277494001,225.719197450137,6.92893576258243));
#78125=CARTESIAN_POINT('Ctrl Pts',(2.090635432585,226.410034996511,6.98185505099302));
#78126=CARTESIAN_POINT('Ctrl Pts',(1.62469809022998,227.100872542886,7.03477433940362));
#78127=CARTESIAN_POINT('Ctrl Pts',(0.782472702938629,227.537921550207,7.08769362781422));
#78128=CARTESIAN_POINT('Ctrl Pts',(-0.0506384086244314,227.521188401318,
7.14061291622481));
#78129=CARTESIAN_POINT('Ctrl Pts',(-0.88374952018748,227.504455252428,7.19353220463541));
#78130=CARTESIAN_POINT('Ctrl Pts',(-1.70774635602222,227.033939947329,7.246451493046));
#78131=CARTESIAN_POINT('Ctrl Pts',(-2.14556798025209,226.324950280381,7.2993707814566));
#78132=CARTESIAN_POINT('Ctrl Pts',(-2.38838055471039,225.931749952283,7.32871942014041));
#78133=CARTESIAN_POINT('Ctrl Pts',(-2.51241613654943,225.465201396059,7.35806805882421));
#78134=CARTESIAN_POINT('Ctrl Pts',(-2.51364339850779,224.999260136873,7.38741669750802));
#78135=CARTESIAN_POINT('Origin',(0.,225.,10.));
#78136=CARTESIAN_POINT('',(-2.51970634748832,224.998100077872,8.38741669750802));
#78137=CARTESIAN_POINT('',(-2.5206697586887,225.00143085894,8.11258330249197));
#78138=CARTESIAN_POINT('',(-2.5175,225.,10.));
#78139=CARTESIAN_POINT('Ctrl Pts',(-2.5206697586887,225.00143085894,8.11258330249197));
#78140=CARTESIAN_POINT('Ctrl Pts',(-2.52123853593806,225.085145295118,8.10727257726845));
#78141=CARTESIAN_POINT('Ctrl Pts',(-2.51742950928565,225.168807347417,8.10196185204492));
#78142=CARTESIAN_POINT('Ctrl Pts',(-2.50907233067035,225.252012580876,8.0966511268214));
#78143=CARTESIAN_POINT('Ctrl Pts',(-2.42579633222796,226.081120011841,8.0437318384108));
#78144=CARTESIAN_POINT('Ctrl Pts',(-1.89091891768193,226.864868352514,7.99081255000021));
#78145=CARTESIAN_POINT('Ctrl Pts',(-1.14919998141176,227.244614377611,7.93789326158961));
#78146=CARTESIAN_POINT('Ctrl Pts',(-0.407481045141574,227.624360402708,
7.88497397317902));
#78147=CARTESIAN_POINT('Ctrl Pts',(0.541079412852777,227.600104112231,7.83205468476842));
#78148=CARTESIAN_POINT('Ctrl Pts',(1.26242014564368,227.182945184224,7.77913539635782));
#78149=CARTESIAN_POINT('Ctrl Pts',(1.9837608784346,226.765786256217,7.72621610794722));
#78150=CARTESIAN_POINT('Ctrl Pts',(2.47788188602208,225.955724690681,7.67329681953662));
#78151=CARTESIAN_POINT('Ctrl Pts',(2.51867340504949,225.123444644078,7.62037753112602));
#78152=CARTESIAN_POINT('Ctrl Pts',(2.5594649240769,224.291164597474,7.56745824271542));
#78153=CARTESIAN_POINT('Ctrl Pts',(2.14692695454429,223.436666069803,7.51453895430482));
#78154=CARTESIAN_POINT('Ctrl Pts',(1.46983686319842,222.950967570526,7.46161966589423));
#78155=CARTESIAN_POINT('Ctrl Pts',(0.792746771852553,222.465269071248,7.40870037748363));
#78156=CARTESIAN_POINT('Ctrl Pts',(-0.148895441306572,222.348370600364,
7.35578108907304));
#78157=CARTESIAN_POINT('Ctrl Pts',(-0.924194318051915,222.653764895852,
7.30286180066244));
#78158=CARTESIAN_POINT('Ctrl Pts',(-1.69949319479726,222.95915919134,7.24994251225184));
#78159=CARTESIAN_POINT('Ctrl Pts',(-2.30844873512883,223.686846253199,7.19702322384125));
#78160=CARTESIAN_POINT('Ctrl Pts',(-2.4724028957642,224.503836496231,7.14410393543065));
#78161=CARTESIAN_POINT('Ctrl Pts',(-2.50495522889496,224.66604609465,7.13359705778442));
#78162=CARTESIAN_POINT('Ctrl Pts',(-2.51996549703062,224.831776046668,7.1230901801382));
#78163=CARTESIAN_POINT('Ctrl Pts',(-2.51844027096952,224.997780461794,7.11258330249198));
#78164=CARTESIAN_POINT('Ctrl Pts',(-2.51364339850779,224.999260136873,7.38741669750802));
#78165=CARTESIAN_POINT('Ctrl Pts',(-2.51462904428357,224.625050677558,7.41098734723481));
#78166=CARTESIAN_POINT('Ctrl Pts',(-2.4364019612172,224.251232931569,7.43455799696161));
#78167=CARTESIAN_POINT('Ctrl Pts',(-2.27687382072545,223.916117714943,7.4581286466884));
#78168=CARTESIAN_POINT('Ctrl Pts',(-1.91871162434389,223.163738845247,7.511047935099));
#78169=CARTESIAN_POINT('Ctrl Pts',(-1.15074081895573,222.606445134651,7.5639672235096));
#78170=CARTESIAN_POINT('Ctrl Pts',(-0.324384830006751,222.499254174166,
7.61688651192019));
#78171=CARTESIAN_POINT('Ctrl Pts',(0.501971158942218,222.392063213681,7.66980580033079));
#78172=CARTESIAN_POINT('Ctrl Pts',(1.38671233145202,222.734975003306,7.72272508874139));
#78173=CARTESIAN_POINT('Ctrl Pts',(1.92498114437798,223.371073114853,7.77564437715199));
#78174=CARTESIAN_POINT('Ctrl Pts',(2.46324995730394,224.007171226399,7.82856366556258));
#78175=CARTESIAN_POINT('Ctrl Pts',(2.65504641064604,224.936455659866,7.88148295397317));
#78176=CARTESIAN_POINT('Ctrl Pts',(2.41260445112607,225.733685876771,7.93440224238377));
#78177=CARTESIAN_POINT('Ctrl Pts',(2.17016249160608,226.530916093675,7.98732153079437));
#78178=CARTESIAN_POINT('Ctrl Pts',(1.49348211922398,227.196092094017,8.04024081920497));
#78179=CARTESIAN_POINT('Ctrl Pts',(0.692212259076926,227.424829353119,8.09316010761557));
#78180=CARTESIAN_POINT('Ctrl Pts',(-0.109057601070118,227.653566612221,
8.14607939602617));
#78181=CARTESIAN_POINT('Ctrl Pts',(-1.03491694898213,227.445865130083,8.19899868443676));
#78182=CARTESIAN_POINT('Ctrl Pts',(-1.66169256525882,226.896769100847,8.25191797284736));
#78183=CARTESIAN_POINT('Ctrl Pts',(-2.19664115838768,226.428119490518,8.29708421440091));
#78184=CARTESIAN_POINT('Ctrl Pts',(-2.51372212363046,225.710780926955,8.34225045595447));
#78185=CARTESIAN_POINT('Ctrl Pts',(-2.51970634748832,224.998100077872,8.38741669750802));
#78186=CARTESIAN_POINT('Origin',(0.,225.,10.));
#78187=CARTESIAN_POINT('',(-2.51957016294845,225.001947759268,9.38741669750802));
#78188=CARTESIAN_POINT('',(-2.51411981970798,225.001308619991,9.11258330249198));
#78189=CARTESIAN_POINT('',(-2.5175,225.,10.));
#78190=CARTESIAN_POINT('Ctrl Pts',(-2.51411981970798,225.001308619991,9.11258330249198));
#78191=CARTESIAN_POINT('Ctrl Pts',(-2.51569980701715,225.336584612862,9.0914549743987));
#78192=CARTESIAN_POINT('Ctrl Pts',(-2.45336466365061,225.671297040634,9.07032664630543));
#78193=CARTESIAN_POINT('Ctrl Pts',(-2.324342022709,225.977951155695,9.04919831821216));
#78194=CARTESIAN_POINT('Ctrl Pts',(-2.00118411275304,226.746015599105,8.99627902980156));
#78195=CARTESIAN_POINT('Ctrl Pts',(-1.25967391532669,227.338061152429,8.94335974139096));
#78196=CARTESIAN_POINT('Ctrl Pts',(-0.43912648219266,227.483167782107,8.89044045298036));
#78197=CARTESIAN_POINT('Ctrl Pts',(0.381420950941362,227.628274411784,8.83752116456977));
#78198=CARTESIAN_POINT('Ctrl Pts',(1.28100561978306,227.326442117814,8.78460187615917));
#78199=CARTESIAN_POINT('Ctrl Pts',(1.84797759755815,226.715789351983,8.73168258774857));
#78200=CARTESIAN_POINT('Ctrl Pts',(2.41494957533325,226.105136586152,8.67876329933797));
#78201=CARTESIAN_POINT('Ctrl Pts',(2.64930886204171,225.18566334846,8.62584401092738));
#78202=CARTESIAN_POINT('Ctrl Pts',(2.44381265269372,224.378120574396,8.57292472251678));
#78203=CARTESIAN_POINT('Ctrl Pts',(2.23831644334573,223.570577800332,8.52000543410618));
#78204=CARTESIAN_POINT('Ctrl Pts',(1.59296473794131,222.874965489897,8.46708614569558));
#78205=CARTESIAN_POINT('Ctrl Pts',(0.803070464184594,222.609595822667,8.41416685728498));
#78206=CARTESIAN_POINT('Ctrl Pts',(0.0131761904278596,222.344226155438,
8.36124756887439));
#78207=CARTESIAN_POINT('Ctrl Pts',(-0.921260651681179,222.509099131415,
8.30832828046379));
#78208=CARTESIAN_POINT('Ctrl Pts',(-1.57264178156633,223.028768880033,8.25540899205319));
#78209=CARTESIAN_POINT('Ctrl Pts',(-2.1586534346405,223.496287072483,8.20780042886612));
#78210=CARTESIAN_POINT('Ctrl Pts',(-2.51557089431972,224.250963859292,8.16019186567905));
#78211=CARTESIAN_POINT('Ctrl Pts',(-2.5206697586887,225.00143085894,8.11258330249197));
#78212=CARTESIAN_POINT('Ctrl Pts',(-2.51970634748832,224.998100077872,8.38741669750802));
#78213=CARTESIAN_POINT('Ctrl Pts',(-2.52073357415978,224.875764283992,8.39516974436507));
#78214=CARTESIAN_POINT('Ctrl Pts',(-2.51259411443575,224.753565732976,8.40292279122211));
#78215=CARTESIAN_POINT('Ctrl Pts',(-2.49481641921416,224.632785842068,8.41067583807916));
#78216=CARTESIAN_POINT('Ctrl Pts',(-2.37347277225141,223.808389188859,8.46359512648976));
#78217=CARTESIAN_POINT('Ctrl Pts',(-1.80309359368457,223.050086458773,8.51651441490035));
#78218=CARTESIAN_POINT('Ctrl Pts',(-1.044684384411,222.704876966188,8.56943370331095));
#78219=CARTESIAN_POINT('Ctrl Pts',(-0.286275175137409,222.359667473603,
8.62235299172154));
#78220=CARTESIAN_POINT('Ctrl Pts',(0.660164064842918,222.42755121852,8.67527228013214));
#78221=CARTESIAN_POINT('Ctrl Pts',(1.3615427579239,222.877464600599,8.72819156854274));
#78222=CARTESIAN_POINT('Ctrl Pts',(2.06292145100487,223.327377982678,8.78111085695334));
#78223=CARTESIAN_POINT('Ctrl Pts',(2.51923959718651,224.159321001919,8.83403014536394));
#78224=CARTESIAN_POINT('Ctrl Pts',(2.52168602174821,224.992596549075,8.88694943377453));
#78225=CARTESIAN_POINT('Ctrl Pts',(2.52413244630992,225.825872096231,8.93986872218513));
#78226=CARTESIAN_POINT('Ctrl Pts',(2.0727071492517,226.660480171302,8.99278801059573));
#78227=CARTESIAN_POINT('Ctrl Pts',(1.37398233763145,227.114504135546,9.04570729900633));
#78228=CARTESIAN_POINT('Ctrl Pts',(0.675257526011217,227.56852809979,9.09862658741692));
#78229=CARTESIAN_POINT('Ctrl Pts',(-0.270766800171062,227.641967953207,
9.15154587582752));
#78230=CARTESIAN_POINT('Ctrl Pts',(-1.03118992785508,227.301217620317,9.20446516423812));
#78231=CARTESIAN_POINT('Ctrl Pts',(-1.79161305553911,226.960467287426,9.25738445264872));
#78232=CARTESIAN_POINT('Ctrl Pts',(-2.3664349847249,226.205526768229,9.31030374105931));
#78233=CARTESIAN_POINT('Ctrl Pts',(-2.4926172119192,225.381856829466,9.36322302946991));
#78234=CARTESIAN_POINT('Ctrl Pts',(-2.51184656419469,225.256334877894,9.37128758548261));
#78235=CARTESIAN_POINT('Ctrl Pts',(-2.52065680612908,225.129216769309,9.37935214149532));
#78236=CARTESIAN_POINT('Ctrl Pts',(-2.51957016294845,225.001947759268,9.38741669750802));
#78237=CARTESIAN_POINT('Origin',(0.,225.,10.));
#78238=CARTESIAN_POINT('',(-2.51360226051679,225.000662435525,10.387416697508));
#78239=CARTESIAN_POINT('',(-2.5158975516969,224.997857973357,10.112583302492));
#78240=CARTESIAN_POINT('',(-2.5175,225.,10.));
#78241=CARTESIAN_POINT('Ctrl Pts',(-2.5158975516969,224.997857973357,10.112583302492));
#78242=CARTESIAN_POINT('Ctrl Pts',(-2.51116121626031,225.583094699563,10.075637371529));
#78243=CARTESIAN_POINT('Ctrl Pts',(-2.30769410526437,226.171300871144,10.0386914405659));
#78244=CARTESIAN_POINT('Ctrl Pts',(-1.93451251538482,226.617595632188,10.0017455096029));
#78245=CARTESIAN_POINT('Ctrl Pts',(-1.39998804490588,227.256843326324,9.94882622119231));
#78246=CARTESIAN_POINT('Ctrl Pts',(-0.517275688115731,227.604944181348,
9.89590693278172));
#78247=CARTESIAN_POINT('Ctrl Pts',(0.30969539787435,227.502607252845,9.84298764437112));
#78248=CARTESIAN_POINT('Ctrl Pts',(1.13666648386443,227.400270324341,9.79006835596052));
#78249=CARTESIAN_POINT('Ctrl Pts',(1.90789629905445,226.847495612311,9.73714906754992));
#78250=CARTESIAN_POINT('Ctrl Pts',(2.27047009517739,226.09723281411,9.68422977913933));
#78251=CARTESIAN_POINT('Ctrl Pts',(2.63304389130033,225.346970015909,9.63131049072872));
#78252=CARTESIAN_POINT('Ctrl Pts',(2.5869616683562,224.399219131538,9.57839120231813));
#78253=CARTESIAN_POINT('Ctrl Pts',(2.15331065065815,223.68767094705,9.52547191390753));
#78254=CARTESIAN_POINT('Ctrl Pts',(1.7196596329601,222.976122762562,9.47255262549694));
#78255=CARTESIAN_POINT('Ctrl Pts',(0.898439820508138,222.500777277956,9.41963333708634));
#78256=CARTESIAN_POINT('Ctrl Pts',(0.0654413833334434,222.479152577643,
9.36671404867574));
#78257=CARTESIAN_POINT('Ctrl Pts',(-0.767557053841252,222.45752787733,9.31379476026514));
#78258=CARTESIAN_POINT('Ctrl Pts',(-1.61233411573868,222.889623961309,9.26087547185455));
#78259=CARTESIAN_POINT('Ctrl Pts',(-2.08231983544461,223.577713670048,9.20795618344395));
#78260=CARTESIAN_POINT('Ctrl Pts',(-2.36466107270674,223.991079633239,9.17616522312662));
#78261=CARTESIAN_POINT('Ctrl Pts',(-2.51174247524297,224.496832083198,9.1443742628093));
#78262=CARTESIAN_POINT('Ctrl Pts',(-2.51411981970798,225.001308619991,9.11258330249198));
#78263=CARTESIAN_POINT('Ctrl Pts',(-2.51957016294845,225.001947759268,9.38741669750802));
#78264=CARTESIAN_POINT('Ctrl Pts',(-2.51352629779302,224.294082703961,9.43227142990591));
#78265=CARTESIAN_POINT('Ctrl Pts',(-2.20131841827154,223.581549453024,9.4771261623038));
#78266=CARTESIAN_POINT('Ctrl Pts',(-1.6728013216547,223.113020683305,9.5219808947017));
#78267=CARTESIAN_POINT('Ctrl Pts',(-1.04926067899306,222.560253834235,9.57490018311229));
#78268=CARTESIAN_POINT('Ctrl Pts',(-0.124636868466955,222.347119494424,
9.62781947152289));
#78269=CARTESIAN_POINT('Ctrl Pts',(0.677962272406855,222.571147933579,9.68073875993349));
#78270=CARTESIAN_POINT('Ctrl Pts',(1.48056141328067,222.795176372734,9.73365804834409));
#78271=CARTESIAN_POINT('Ctrl Pts',(2.16113588450219,223.456367590855,9.78657733675469));
#78272=CARTESIAN_POINT('Ctrl Pts',(2.40825482142189,224.252160499529,9.83949662516529));
#78273=CARTESIAN_POINT('Ctrl Pts',(2.65537375834158,225.047953408204,9.89241591357588));
#78274=CARTESIAN_POINT('Ctrl Pts',(2.46903716095948,225.978348007433,9.94533520198648));
#78275=CARTESIAN_POINT('Ctrl Pts',(1.93451265257388,226.617595746903,9.99825449039708));
#78276=CARTESIAN_POINT('Ctrl Pts',(1.39998814418828,227.256843486372,10.0511737788077));
#78277=CARTESIAN_POINT('Ctrl Pts',(0.517275724799156,227.604944366082,10.1040930672183));
#78278=CARTESIAN_POINT('Ctrl Pts',(-0.309695419836912,227.502607430321,
10.1570123556289));
#78279=CARTESIAN_POINT('Ctrl Pts',(-1.13666656447296,227.40027049456,10.2099316440395));
#78280=CARTESIAN_POINT('Ctrl Pts',(-1.90789643435596,226.847495743329,10.2628509324501));
#78281=CARTESIAN_POINT('Ctrl Pts',(-2.27047025619141,226.097232891922,10.3157702208607));
#78282=CARTESIAN_POINT('Ctrl Pts',(-2.43409765708363,225.758643746847,10.3396523797431));
#78283=CARTESIAN_POINT('Ctrl Pts',(-2.51449559242104,225.379832930983,10.3635345386256));
#78284=CARTESIAN_POINT('Ctrl Pts',(-2.51360226051679,225.000662435525,10.387416697508));
#78285=CARTESIAN_POINT('Origin',(0.,225.,10.));
#78286=CARTESIAN_POINT('',(-2.51714221557728,224.997701746028,11.387416697508));
#78287=CARTESIAN_POINT('',(-2.52169605742446,224.999954178766,11.112583302492));
#78288=CARTESIAN_POINT('',(-2.5175,225.,10.));
#78289=CARTESIAN_POINT('Ctrl Pts',(-2.52169565421209,224.999954183169,11.112583302492));
#78290=CARTESIAN_POINT('Ctrl Pts',(-2.52147281221073,225.830781657145,11.0598197686592));
#78291=CARTESIAN_POINT('Ctrl Pts',(-2.07065048216162,226.661816358474,11.0070562348264));
#78292=CARTESIAN_POINT('Ctrl Pts',(-1.37398224019328,227.114503985593,10.9542927009937));
#78293=CARTESIAN_POINT('Ctrl Pts',(-0.675257478124223,227.568527917639,
10.9013734125831));
#78294=CARTESIAN_POINT('Ctrl Pts',(0.270766780969211,227.641967765848,10.8484541241725));
#78295=CARTESIAN_POINT('Ctrl Pts',(1.03118985472662,227.301217457122,10.7955348357619));
#78296=CARTESIAN_POINT('Ctrl Pts',(1.79161292848402,226.960467148397,10.7426155473513));
#78297=CARTESIAN_POINT('Ctrl Pts',(2.36643481690539,226.205526682737,10.6896962589407));
#78298=CARTESIAN_POINT('Ctrl Pts',(2.49261703515127,225.381856802386,10.6367769705301));
#78299=CARTESIAN_POINT('Ctrl Pts',(2.61879925339715,224.558186922035,10.5838576821195));
#78300=CARTESIAN_POINT('Ctrl Pts',(2.29634180146753,223.665787626992,10.5309383937089));
#78301=CARTESIAN_POINT('Ctrl Pts',(1.67280120302526,223.113020817123,10.4780191052983));
#78302=CARTESIAN_POINT('Ctrl Pts',(1.04926060458298,222.560254007253,10.4250998168877));
#78303=CARTESIAN_POINT('Ctrl Pts',(0.124636859628036,222.347119682557,10.3721805284771));
#78304=CARTESIAN_POINT('Ctrl Pts',(-0.677962224328165,222.571148105825,
10.3192612400665));
#78305=CARTESIAN_POINT('Ctrl Pts',(-1.48056130828437,222.795176529092,10.2663419516559));
#78306=CARTESIAN_POINT('Ctrl Pts',(-2.16113573124182,223.456367700324,10.2134226632453));
#78307=CARTESIAN_POINT('Ctrl Pts',(-2.40825465063667,224.252160552564,10.1605033748347));
#78308=CARTESIAN_POINT('Ctrl Pts',(-2.48284595656893,224.49236566614,10.1445300173871));
#78309=CARTESIAN_POINT('Ctrl Pts',(-2.51794527865757,224.744834293198,10.1285566599396));
#78310=CARTESIAN_POINT('Ctrl Pts',(-2.5158975516969,224.997857973357,10.112583302492));
#78311=CARTESIAN_POINT('Ctrl Pts',(-2.51360226051679,225.000662435525,10.387416697508));
#78312=CARTESIAN_POINT('Ctrl Pts',(-2.51251610267223,224.539647883028,10.4164538270362));
#78313=CARTESIAN_POINT('Ctrl Pts',(-2.39125772294784,224.078101619103,10.4454909565643));
#78314=CARTESIAN_POINT('Ctrl Pts',(-2.15331080336361,223.687670853984,10.4745280860925));
#78315=CARTESIAN_POINT('Ctrl Pts',(-1.71965975491251,222.976122619035,10.5274473745031));
#78316=CARTESIAN_POINT('Ctrl Pts',(-0.898439884222463,222.50077710072,10.5803666629137));
#78317=CARTESIAN_POINT('Ctrl Pts',(-0.0654413879743779,222.479152398873,
10.6332859513243));
#78318=CARTESIAN_POINT('Ctrl Pts',(0.767557108273737,222.457527697027,10.6862052397348));
#78319=CARTESIAN_POINT('Ctrl Pts',(1.61233423007989,222.889623811649,10.7391245281454));
#78320=CARTESIAN_POINT('Ctrl Pts',(2.08231998311562,223.577713569184,10.792043816556));
#78321=CARTESIAN_POINT('Ctrl Pts',(2.55230573615135,224.265803326719,10.8449631049666));
#78322=CARTESIAN_POINT('Ctrl Pts',(2.64750012041665,225.209886727168,10.8978823933772));
#78323=CARTESIAN_POINT('Ctrl Pts',(2.32434218754344,225.977951225047,10.9508016817878));
#78324=CARTESIAN_POINT('Ctrl Pts',(2.00118425467023,226.746015722927,11.0037209701984));
#78325=CARTESIAN_POINT('Ctrl Pts',(1.2596740046585,227.338061318237,11.056640258609));
#78326=CARTESIAN_POINT('Ctrl Pts',(0.439126513334034,227.483167958204,11.1095595470196));
#78327=CARTESIAN_POINT('Ctrl Pts',(-0.381420977990437,227.628274598172,
11.1624788354302));
#78328=CARTESIAN_POINT('Ctrl Pts',(-1.28100571062764,227.326442282797,11.2153981238408));
#78329=CARTESIAN_POINT('Ctrl Pts',(-1.84797772861045,226.715789473661,11.2683174122514));
#78330=CARTESIAN_POINT('Ctrl Pts',(-2.27331704646822,226.257681064343,11.3080171740036));
#78331=CARTESIAN_POINT('Ctrl Pts',(-2.51146463506934,225.625770994084,11.3477169357558));
#78332=CARTESIAN_POINT('Ctrl Pts',(-2.51714221557728,224.997701746028,11.387416697508));
#78333=CARTESIAN_POINT('Origin',(0.,225.,10.));
#78334=CARTESIAN_POINT('',(-2.52142589487062,225.000747710561,12.387416697508));
#78335=CARTESIAN_POINT('',(-2.51603107573661,225.002171022738,12.112583302492));
#78336=CARTESIAN_POINT('',(-2.5175,225.,10.));
#78337=CARTESIAN_POINT('Ctrl Pts',(-2.51603107573661,225.002171022738,12.112583302492));
#78338=CARTESIAN_POINT('Ctrl Pts',(-2.51807394519329,225.250226974727,12.0969214542001));
#78339=CARTESIAN_POINT('Ctrl Pts',(-2.48435673616632,225.497739760452,12.0812596059081));
#78340=CARTESIAN_POINT('Ctrl Pts',(-2.41260428003234,225.73368582474,12.0655977576162));
#78341=CARTESIAN_POINT('Ctrl Pts',(-2.17016233770549,226.530915985108,12.0126784692056));
#78342=CARTESIAN_POINT('Ctrl Pts',(-1.49348201331126,227.196091938278,11.959759180795));
#78343=CARTESIAN_POINT('Ctrl Pts',(-0.692212209987538,227.424829181159,
11.9068398923844));
#78344=CARTESIAN_POINT('Ctrl Pts',(0.109057593336183,227.65356642404,11.8539206039738));
#78345=CARTESIAN_POINT('Ctrl Pts',(1.03491687558939,227.445864956631,11.8010013155632));
#78346=CARTESIAN_POINT('Ctrl Pts',(1.66169244741728,226.896768966335,11.7480820271526));
#78347=CARTESIAN_POINT('Ctrl Pts',(2.28846801924516,226.347672976039,11.695162738742));
#78348=CARTESIAN_POINT('Ctrl Pts',(2.61615988064774,225.457182462856,11.6422434503314));
#78349=CARTESIAN_POINT('Ctrl Pts',(2.49481624229027,224.63278586811,11.5893241619208));
#78350=CARTESIAN_POINT('Ctrl Pts',(2.37347260393281,223.808389273364,11.5364048735102));
#78351=CARTESIAN_POINT('Ctrl Pts',(1.8030934658153,223.050086597054,11.4834855850996));
#78352=CARTESIAN_POINT('Ctrl Pts',(1.04468431032549,222.70487712895,11.430566296689));
#78353=CARTESIAN_POINT('Ctrl Pts',(0.286275154835696,222.359667660847,11.3776470082784));
#78354=CARTESIAN_POINT('Ctrl Pts',(-0.660164018026388,222.427551400949,
11.3247277198678));
#78355=CARTESIAN_POINT('Ctrl Pts',(-1.36154266136797,222.877464751122,11.2718084314572));
#78356=CARTESIAN_POINT('Ctrl Pts',(-2.06292130470955,223.327378101294,11.2188891430466));
#78357=CARTESIAN_POINT('Ctrl Pts',(-2.51923941853063,224.159321061537,11.1659698546361));
#78358=CARTESIAN_POINT('Ctrl Pts',(-2.52168584291883,224.9925965496,11.1130505662255));
#78359=CARTESIAN_POINT('Ctrl Pts',(-2.52169304335196,224.995049085825,11.1128948116476));
#78360=CARTESIAN_POINT('Ctrl Pts',(-2.52169631202743,224.997501633594,11.1127390570698));
#78361=CARTESIAN_POINT('Ctrl Pts',(-2.52169565421209,224.999954183169,11.112583302492));
#78362=CARTESIAN_POINT('Ctrl Pts',(-2.51714221557728,224.997701746028,11.387416697508));
#78363=CARTESIAN_POINT('Ctrl Pts',(-2.51903277923729,224.788562501822,11.4006362241664));
#78364=CARTESIAN_POINT('Ctrl Pts',(-2.49514690270336,224.57984913072,11.4138557508248));
#78365=CARTESIAN_POINT('Ctrl Pts',(-2.44381282600061,224.378120530295,11.4270752774832));
#78366=CARTESIAN_POINT('Ctrl Pts',(-2.23831660207953,223.570577698963,11.4799945658938));
#78367=CARTESIAN_POINT('Ctrl Pts',(-1.59296485090897,222.874965339197,11.5329138543044));
#78368=CARTESIAN_POINT('Ctrl Pts',(-0.803070521135639,222.609595653148,
11.585833142715));
#78369=CARTESIAN_POINT('Ctrl Pts',(-0.0131761913623006,222.3442259671,11.6387524311256));
#78370=CARTESIAN_POINT('Ctrl Pts',(0.921260717013809,222.509098954769,11.6916717195362));
#78371=CARTESIAN_POINT('Ctrl Pts',(1.5726418930927,223.02876874024,11.7445910079468));
#78372=CARTESIAN_POINT('Ctrl Pts',(2.22402306917158,223.548438525711,11.7975102963574));
#78373=CARTESIAN_POINT('Ctrl Pts',(2.59234851295325,224.422905108984,11.850429584768));
#78374=CARTESIAN_POINT('Ctrl Pts',(2.50907250860523,225.252012598747,11.9033488731786));
#78375=CARTESIAN_POINT('Ctrl Pts',(2.42579650425721,226.081120088511,11.9562681615892));
#78376=CARTESIAN_POINT('Ctrl Pts',(1.8909190517795,226.864868484764,12.0091874499998));
#78377=CARTESIAN_POINT('Ctrl Pts',(1.14920006290913,227.244614536791,12.0621067384104));
#78378=CARTESIAN_POINT('Ctrl Pts',(0.407481074038757,227.624360588819,12.115026026821));
#78379=CARTESIAN_POINT('Ctrl Pts',(-0.541079451224263,227.600104296622,
12.1679453152316));
#78380=CARTESIAN_POINT('Ctrl Pts',(-1.26242023517021,227.182945339031,12.2208646036422));
#78381=CARTESIAN_POINT('Ctrl Pts',(-1.98376101911615,226.765786381441,12.2737838920528));
#78382=CARTESIAN_POINT('Ctrl Pts',(-2.47788206174501,225.955724758458,12.3267031804634));
#78383=CARTESIAN_POINT('Ctrl Pts',(-2.51867358366524,225.123444652832,12.379622468874));
#78384=CARTESIAN_POINT('Ctrl Pts',(-2.52067624632207,225.082583802119,12.3822205450853));
#78385=CARTESIAN_POINT('Ctrl Pts',(-2.52158623705894,225.041669397619,12.3848186212967));
#78386=CARTESIAN_POINT('Ctrl Pts',(-2.52142589487062,225.000747710561,12.387416697508));
#78387=CARTESIAN_POINT('Origin',(0.,225.,10.));
#78388=CARTESIAN_POINT('',(-2.5149421643676,225.001823827574,13.387416697508));
#78389=CARTESIAN_POINT('',(-2.51404431806768,224.998759332749,13.112583302492));
#78390=CARTESIAN_POINT('',(-2.5175,225.,10.));
#78391=CARTESIAN_POINT('Ctrl Pts',(-2.51404431806768,224.998759332749,13.112583302492));
#78392=CARTESIAN_POINT('Ctrl Pts',(-2.51181646834445,225.498330218278,13.0811038513303));
#78393=CARTESIAN_POINT('Ctrl Pts',(-2.36780172426376,225.999084826841,13.0496244001686));
#78394=CARTESIAN_POINT('Ctrl Pts',(-2.09063528432425,226.410034896516,13.018144949007));
#78395=CARTESIAN_POINT('Ctrl Pts',(-1.62469797501192,227.100872393899,12.9652256605964));
#78396=CARTESIAN_POINT('Ctrl Pts',(-0.782472647448307,227.537921370226,
12.9123063721858));
#78397=CARTESIAN_POINT('Ctrl Pts',(0.0506384050333455,227.521188222523,
12.8593870837752));
#78398=CARTESIAN_POINT('Ctrl Pts',(0.883749457514986,227.504455074821,12.8064677953646));
#78399=CARTESIAN_POINT('Ctrl Pts',(1.70774623491467,227.033939803089,12.753548506954));
#78400=CARTESIAN_POINT('Ctrl Pts',(2.14556782809573,226.324950186421,12.7006292185434));
#78401=CARTESIAN_POINT('Ctrl Pts',(2.58338942127679,225.615960569752,12.6477099301328));
#78402=CARTESIAN_POINT('Ctrl Pts',(2.63503583023922,224.668496608148,12.5947906417222));
#78403=CARTESIAN_POINT('Ctrl Pts',(2.2768736592573,223.916117791808,12.5418713533116));
#78404=CARTESIAN_POINT('Ctrl Pts',(1.91871148827538,223.163738975468,12.488952064901));
#78405=CARTESIAN_POINT('Ctrl Pts',(1.15074073734909,222.606445304394,12.4360327764904));
#78406=CARTESIAN_POINT('Ctrl Pts',(0.324384807002465,222.49925435151,12.3831134880798));
#78407=CARTESIAN_POINT('Ctrl Pts',(-0.501971123344163,222.392063398627,
12.3301941996692));
#78408=CARTESIAN_POINT('Ctrl Pts',(-1.38671223311115,222.734975163934,12.2772749112586));
#78409=CARTESIAN_POINT('Ctrl Pts',(-1.9249810078649,223.371073230371,12.224355622848));
#78410=CARTESIAN_POINT('Ctrl Pts',(-2.30394522385243,223.818913447646,12.1870981827293));
#78411=CARTESIAN_POINT('Ctrl Pts',(-2.51117136281936,224.412079125215,12.1498407426107));
#78412=CARTESIAN_POINT('Ctrl Pts',(-2.51603107573661,225.002171022738,12.112583302492));
#78413=CARTESIAN_POINT('Ctrl Pts',(-2.52142589487062,225.000747710561,12.387416697508));
#78414=CARTESIAN_POINT('Ctrl Pts',(-2.51832028417003,224.208150138174,12.4377379097073));
#78415=CARTESIAN_POINT('Ctrl Pts',(-2.11368531846519,223.412820555035,12.4880591219065));
#78416=CARTESIAN_POINT('Ctrl Pts',(-1.4698369674343,222.950967425215,12.5383803341058));
#78417=CARTESIAN_POINT('Ctrl Pts',(-0.792746828071511,222.465268891494,
12.5912996225164));
#78418=CARTESIAN_POINT('Ctrl Pts',(0.148895451865672,222.34837041232,12.644218910927));
#78419=CARTESIAN_POINT('Ctrl Pts',(0.924194383592584,222.653764729465,12.6971381993376));
#78420=CARTESIAN_POINT('Ctrl Pts',(1.6994933153195,222.959159046611,12.7500574877481));
#78421=CARTESIAN_POINT('Ctrl Pts',(2.30844889883614,223.686846160075,12.8029767761587));
#78422=CARTESIAN_POINT('Ctrl Pts',(2.47240307109859,224.503836461045,12.8558960645693));
#78423=CARTESIAN_POINT('Ctrl Pts',(2.63635724336105,225.320826762015,12.9088153529799));
#78424=CARTESIAN_POINT('Ctrl Pts',(2.35531000436931,226.227120250491,12.9617346413905));
#78425=CARTESIAN_POINT('Ctrl Pts',(1.75786856516005,226.807997043965,13.0146539298011));
#78426=CARTESIAN_POINT('Ctrl Pts',(1.16042712595079,227.38887383744,13.0675732182117));
#78427=CARTESIAN_POINT('Ctrl Pts',(0.246591486524002,227.644333935913,13.1204925066223));
#78428=CARTESIAN_POINT('Ctrl Pts',(-0.565467182486472,227.457478803346,
13.1734117950329));
#78429=CARTESIAN_POINT('Ctrl Pts',(-1.37752585149693,227.27062367078,13.2263310834435));
#78430=CARTESIAN_POINT('Ctrl Pts',(-2.08780755009108,226.641453307173,13.2792503718541));
#78431=CARTESIAN_POINT('Ctrl Pts',(-2.37128738695782,225.857876058543,13.3321696602647));
#78432=CARTESIAN_POINT('Ctrl Pts',(-2.46993712051424,225.585194630288,13.3505853393458));
#78433=CARTESIAN_POINT('Ctrl Pts',(-2.51690075091277,225.293814384377,13.3690010184269));
#78434=CARTESIAN_POINT('Ctrl Pts',(-2.5149421643676,225.001823827574,13.387416697508));
#78435=CARTESIAN_POINT('Origin',(0.,225.,10.));
#78436=CARTESIAN_POINT('',(-2.51484787790986,224.998220566968,14.387416697508));
#78437=CARTESIAN_POINT('',(-2.52055916665943,224.998500632631,14.112583302492));
#78438=CARTESIAN_POINT('',(-2.5175,225.,10.));
#78439=CARTESIAN_POINT('Ctrl Pts',(-2.52055916665943,224.998500632631,14.112583302492));
#78440=CARTESIAN_POINT('Ctrl Pts',(-2.51530317312179,225.744143280451,14.0652862484606));
#78441=CARTESIAN_POINT('Ctrl Pts',(-2.16362936224286,226.494093371989,14.0179891944291));
#78442=CARTESIAN_POINT('Ctrl Pts',(-1.58418929737073,226.961962938373,13.9706921403977));
#78443=CARTESIAN_POINT('Ctrl Pts',(-0.935870780761794,227.485448492158,
13.9177728519871));
#78444=CARTESIAN_POINT('Ctrl Pts',(-0.00241814453275091,227.655805429249,
13.8648535635765));
#78445=CARTESIAN_POINT('Ctrl Pts',(0.789020703331562,227.395078418584,13.8119342751659));
#78446=CARTESIAN_POINT('Ctrl Pts',(1.58045955119587,227.134351407919,13.7590149867553));
#78447=CARTESIAN_POINT('Ctrl Pts',(2.22988461069546,226.442540449498,13.7060956983447));
#78448=CARTESIAN_POINT('Ctrl Pts',(2.44011898737231,225.636218224291,13.6531764099341));
#78449=CARTESIAN_POINT('Ctrl Pts',(2.65035336404916,224.829895999084,13.6002571215235));
#78450=CARTESIAN_POINT('Ctrl Pts',(2.42139705790327,223.909062507092,13.5473378331129));
#78451=CARTESIAN_POINT('Ctrl Pts',(1.85802047012526,223.295091136145,13.4944185447023));
#78452=CARTESIAN_POINT('Ctrl Pts',(1.29464388234725,222.681119765198,13.4414992562917));
#78453=CARTESIAN_POINT('Ctrl Pts',(0.396847012937123,222.374010515296,13.3885799678811));
#78454=CARTESIAN_POINT('Ctrl Pts',(-0.424538308315552,222.514296573155,
13.3356606794705));
#78455=CARTESIAN_POINT('Ctrl Pts',(-1.24592362956823,222.654582631015,13.28274139106));
#78456=CARTESIAN_POINT('Ctrl Pts',(-1.99089740266345,223.242263996636,13.2298221026494));
#78457=CARTESIAN_POINT('Ctrl Pts',(-2.31855964368053,224.008417688666,13.1769028142388));
#78458=CARTESIAN_POINT('Ctrl Pts',(-2.45130944684338,224.318818885623,13.1554629769898));
#78459=CARTESIAN_POINT('Ctrl Pts',(-2.51556164869825,224.658514567202,13.1340231397409));
#78460=CARTESIAN_POINT('Ctrl Pts',(-2.51404431806768,224.998759332749,13.112583302492));
#78461=CARTESIAN_POINT('Ctrl Pts',(-2.5149421643676,225.001823827574,13.387416697508));
#78462=CARTESIAN_POINT('Ctrl Pts',(-2.51127255736073,224.454750431288,13.4219203068375));
#78463=CARTESIAN_POINT('Ctrl Pts',(-2.33586759681367,223.905534614577,13.456423916167));
#78464=CARTESIAN_POINT('Ctrl Pts',(-2.00690546813401,223.473145178696,13.4909275254965));
#78465=CARTESIAN_POINT('Ctrl Pts',(-1.50236573730415,222.809975681135,13.5438468139071));
#78466=CARTESIAN_POINT('Ctrl Pts',(-0.636608300505109,222.421620819667,
13.5967661023177));
#78467=CARTESIAN_POINT('Ctrl Pts',(0.19419625620641,222.485791771264,13.6496853907283));
#78468=CARTESIAN_POINT('Ctrl Pts',(1.02500081291792,222.549962722862,13.7026046791389));
#78469=CARTESIAN_POINT('Ctrl Pts',(1.82085248954192,223.066659487525,13.7555239675495));
#78470=CARTESIAN_POINT('Ctrl Pts',(2.21756957450331,223.799441635903,13.8084432559601));
#78471=CARTESIAN_POINT('Ctrl Pts',(2.61428665946469,224.532223784281,13.8613625443707));
#78472=CARTESIAN_POINT('Ctrl Pts',(2.61186915276347,225.481091316374,13.9142818327813));
#78473=CARTESIAN_POINT('Ctrl Pts',(2.21142330541858,226.211842468152,13.9672011211919));
#78474=CARTESIAN_POINT('Ctrl Pts',(1.81097745807369,226.942593619931,14.0201204096025));
#78475=CARTESIAN_POINT('Ctrl Pts',(1.01250327008514,227.455228391396,14.0730396980131));
#78476=CARTESIAN_POINT('Ctrl Pts',(0.181382514176868,227.515165121203,14.1259589864237));
#78477=CARTESIAN_POINT('Ctrl Pts',(-0.64973824173139,227.575101851011,14.1788782748343));
#78478=CARTESIAN_POINT('Ctrl Pts',(-1.51350556555936,227.182340539162,14.2317975632449));
#78479=CARTESIAN_POINT('Ctrl Pts',(-2.01465954690679,226.516608754235,14.2847168516555));
#78480=CARTESIAN_POINT('Ctrl Pts',(-2.33885410922109,226.085949450577,14.3189501336063));
#78481=CARTESIAN_POINT('Ctrl Pts',(-2.51130420518947,225.541058942732,14.3531834155572));
#78482=CARTESIAN_POINT('Ctrl Pts',(-2.51484787790986,224.998220566968,14.387416697508));
#78483=CARTESIAN_POINT('Origin',(0.,225.,10.));
#78484=CARTESIAN_POINT('',(-2.52136965310386,224.999178339809,15.387416697508));
#78485=CARTESIAN_POINT('',(-2.51858860887527,225.002195336597,15.112583302492));
#78486=CARTESIAN_POINT('',(-2.5175,225.,10.));
#78487=CARTESIAN_POINT('Ctrl Pts',(-2.51858860887527,225.002195336597,15.112583302492));
#78488=CARTESIAN_POINT('Ctrl Pts',(-2.52006205682024,225.163253597151,15.1023879340014));
#78489=CARTESIAN_POINT('Ctrl Pts',(-2.50593608807698,225.324054407012,15.0921925655108));
#78490=CARTESIAN_POINT('Ctrl Pts',(-2.47527363466472,225.481637555625,15.0819971970203));
#78491=CARTESIAN_POINT('Ctrl Pts',(-2.31611948373823,226.299576416568,15.0290779086097));
#78492=CARTESIAN_POINT('Ctrl Pts',(-1.71144725627252,227.030826584042,14.9761586201991));
#78493=CARTESIAN_POINT('Ctrl Pts',(-0.937954951666531,227.340767995787,
14.9232393317885));
#78494=CARTESIAN_POINT('Ctrl Pts',(-0.164462647060536,227.650709407532,
14.8703200433779));
#78495=CARTESIAN_POINT('Ctrl Pts',(0.777849734685748,227.539342063548,14.8174007549673));
#78496=CARTESIAN_POINT('Ctrl Pts',(1.45778006621284,227.057627658253,14.7644814665567));
#78497=CARTESIAN_POINT('Ctrl Pts',(2.13771039773993,226.575913252958,14.7115621781461));
#78498=CARTESIAN_POINT('Ctrl Pts',(2.55525867904782,225.723851786352,14.6586428897355));
#78499=CARTESIAN_POINT('Ctrl Pts',(2.51935482481995,224.8913465688,14.6057236013249));
#78500=CARTESIAN_POINT('Ctrl Pts',(2.48345097059207,224.058841351249,14.5528043129143));
#78501=CARTESIAN_POINT('Ctrl Pts',(1.99409498082843,223.245892382752,14.4998850245037));
#78502=CARTESIAN_POINT('Ctrl Pts',(1.27521614682309,222.824505095309,14.4469657360931));
#78503=CARTESIAN_POINT('Ctrl Pts',(0.55633731281776,222.403117807866,14.3940464476825));
#78504=CARTESIAN_POINT('Ctrl Pts',(-0.392064365429268,222.373292201478,
14.3411271592719));
#78505=CARTESIAN_POINT('Ctrl Pts',(-1.13600029859962,222.748676473042,14.2882078708613));
#78506=CARTESIAN_POINT('Ctrl Pts',(-1.87993623176996,223.124060744605,14.2352885824507));
#78507=CARTESIAN_POINT('Ctrl Pts',(-2.41940641986364,223.904654894119,14.1823692940401));
#78508=CARTESIAN_POINT('Ctrl Pts',(-2.50754931541607,224.733259054115,14.1294500056295));
#78509=CARTESIAN_POINT('Ctrl Pts',(-2.51691376517606,224.821291356419,14.1238277712503));
#78510=CARTESIAN_POINT('Ctrl Pts',(-2.5211839503414,224.909865561906,14.1182055368712));
#78511=CARTESIAN_POINT('Ctrl Pts',(-2.52055916665943,224.998500632631,14.112583302492));
#78512=CARTESIAN_POINT('Ctrl Pts',(-2.51484787790986,224.998220566968,14.387416697508));
#78513=CARTESIAN_POINT('Ctrl Pts',(-2.51678216780468,224.701915894494,14.4061027039678));
#78514=CARTESIAN_POINT('Ctrl Pts',(-2.46839165502543,224.406222644251,14.4247887104275));
#78515=CARTESIAN_POINT('Ctrl Pts',(-2.36688526988595,224.130052115031,14.4434747168873));
#78516=CARTESIAN_POINT('Ctrl Pts',(-2.07941637265078,223.347929518756,14.4963940052979));
#78517=CARTESIAN_POINT('Ctrl Pts',(-1.36593793931355,222.722386584209,14.5493132937085));
#78518=CARTESIAN_POINT('Ctrl Pts',(-0.552937686940973,222.53967174594,14.6022325821191));
#78519=CARTESIAN_POINT('Ctrl Pts',(0.260062565431603,222.356956907671,14.6551518705297));
#78520=CARTESIAN_POINT('Ctrl Pts',(1.17258463683953,222.61707016568,14.7080711589403));
#78521=CARTESIAN_POINT('Ctrl Pts',(1.76705844534861,223.200983698215,14.7609904473509));
#78522=CARTESIAN_POINT('Ctrl Pts',(2.3615322538577,223.784897230751,14.8139097357615));
#78523=CARTESIAN_POINT('Ctrl Pts',(2.63795779946796,224.692611037813,14.866829024172));
#78524=CARTESIAN_POINT('Ctrl Pts',(2.46984275794309,225.508755299139,14.9197483125826));
#78525=CARTESIAN_POINT('Ctrl Pts',(2.30172771641822,226.324899560465,14.9726676009932));
#78526=CARTESIAN_POINT('Ctrl Pts',(1.68907208775825,227.049474276054,15.0255868894038));
#78527=CARTESIAN_POINT('Ctrl Pts',(0.912227075592163,227.350914070298,15.0785061778144));
#78528=CARTESIAN_POINT('Ctrl Pts',(0.135382063426061,227.652353864542,15.131425466225));
#78529=CARTESIAN_POINT('Ctrl Pts',(-0.805652332246163,227.53065873744,15.1843447546356));
#78530=CARTESIAN_POINT('Ctrl Pts',(-1.48025879046803,227.041516376766,15.2372640430462));
#78531=CARTESIAN_POINT('Ctrl Pts',(-2.1182993075233,226.578887178787,15.2873149278668));
#78532=CARTESIAN_POINT('Ctrl Pts',(-2.51801170286182,225.787564939661,15.3373658126874));
#78533=CARTESIAN_POINT('Ctrl Pts',(-2.52136965310386,224.999178339809,15.387416697508));
#78534=CARTESIAN_POINT('Origin',(0.,225.,10.));
#78535=CARTESIAN_POINT('',(-2.51727025050597,225.002300995809,16.387416697508));
#78536=CARTESIAN_POINT('',(-2.51344539583794,225.000116344878,16.112583302492));
#78537=CARTESIAN_POINT('',(-2.5175,225.,10.));
#78538=CARTESIAN_POINT('Ctrl Pts',(-2.51344539583794,225.000116344878,16.112583302492));
#78539=CARTESIAN_POINT('Ctrl Pts',(-2.5136156958088,225.413181385681,16.0865703311317));
#78540=CARTESIAN_POINT('Ctrl Pts',(-2.41747216845691,225.826171771672,16.0605573597713));
#78541=CARTESIAN_POINT('Ctrl Pts',(-2.22458059720485,226.187516512708,16.034544388411));
#78542=CARTESIAN_POINT('Ctrl Pts',(-1.83217311135215,226.922615410164,15.9816251000004));
#78543=CARTESIAN_POINT('Ctrl Pts',(-1.03936913807555,227.443976292902,15.9287058115898));
#78544=CARTESIAN_POINT('Ctrl Pts',(-0.208955759937372,227.51302443121,15.8757865231792));
#78545=CARTESIAN_POINT('Ctrl Pts',(0.621457618200808,227.582072569518,15.8228672347686));
#78546=CARTESIAN_POINT('Ctrl Pts',(1.48948040120057,227.198807963396,15.769947946358));
#78547=CARTESIAN_POINT('Ctrl Pts',(1.99790538061801,226.53861248908,15.7170286579474));
#78548=CARTESIAN_POINT('Ctrl Pts',(2.50633036003544,225.878417014764,15.6641093695368));
#78549=CARTESIAN_POINT('Ctrl Pts',(2.65515753587054,224.941290672255,15.6111900811262));
#78550=CARTESIAN_POINT('Ctrl Pts',(2.37628359539248,224.156062457454,15.5582707927156));
#78551=CARTESIAN_POINT('Ctrl Pts',(2.09740965491442,223.370834242652,15.505351504305));
#78552=CARTESIAN_POINT('Ctrl Pts',(1.3908345981232,222.737504155558,15.4524322158944));
#78553=CARTESIAN_POINT('Ctrl Pts',(0.579887157111302,222.545884031576,15.3995129274838));
#78554=CARTESIAN_POINT('Ctrl Pts',(-0.231060283900595,222.354263907594,
15.3465936390732));
#78555=CARTESIAN_POINT('Ctrl Pts',(-1.14638010913316,222.604353746723,15.2936743506627));
#78556=CARTESIAN_POINT('Ctrl Pts',(-1.74722198455582,223.181712443495,15.2407550622521));
#78557=CARTESIAN_POINT('Ctrl Pts',(-2.23230636382754,223.647837885973,15.198031142332));
#78558=CARTESIAN_POINT('Ctrl Pts',(-2.51241409227338,224.327277089876,15.155307222412));
#78559=CARTESIAN_POINT('Ctrl Pts',(-2.51858860887527,225.002195336597,15.112583302492));
#78560=CARTESIAN_POINT('Ctrl Pts',(-2.52136965310386,224.999178339809,15.387416697508));
#78561=CARTESIAN_POINT('Ctrl Pts',(-2.52156209638561,224.953996102544,15.390285101098));
#78562=CARTESIAN_POINT('Ctrl Pts',(-2.52045275027353,224.908823507113,15.393153504688));
#78563=CARTESIAN_POINT('Ctrl Pts',(-2.51801186970213,224.863722975502,15.396021908278));
#78564=CARTESIAN_POINT('Ctrl Pts',(-2.47297996994284,224.03166152916,15.4489411966886));
#78565=CARTESIAN_POINT('Ctrl Pts',(-1.97473764965276,223.224128230723,15.5018604850992));
#78566=CARTESIAN_POINT('Ctrl Pts',(-1.25128058480224,222.810650301693,15.5547797735098));
#78567=CARTESIAN_POINT('Ctrl Pts',(-0.527823519951722,222.397172372662,
15.6076990619204));
#78568=CARTESIAN_POINT('Ctrl Pts',(0.420848289459224,222.37774981304,15.660618350331));
#78569=CARTESIAN_POINT('Ctrl Pts',(1.16062264210119,222.761270385695,15.7135376387416));
#78570=CARTESIAN_POINT('Ctrl Pts',(1.90039699474315,223.14479095835,15.7664569271522));
#78571=CARTESIAN_POINT('Ctrl Pts',(2.43127389061612,223.931254663283,15.8193762155628));
#78572=CARTESIAN_POINT('Ctrl Pts',(2.51032407259816,224.760775724643,15.8722955039734));
#78573=CARTESIAN_POINT('Ctrl Pts',(2.5893742545802,225.590296786003,15.925214792384));
#78574=CARTESIAN_POINT('Ctrl Pts',(2.21659772267131,226.462875203789,15.9781340807946));
#78575=CARTESIAN_POINT('Ctrl Pts',(1.56257701056091,226.979219111052,16.0310533692052));
#78576=CARTESIAN_POINT('Ctrl Pts',(0.908556298450499,227.495563018316,16.0839726576158));
#78577=CARTESIAN_POINT('Ctrl Pts',(-0.026708593861423,227.655672415057,
16.1368919460264));
#78578=CARTESIAN_POINT('Ctrl Pts',(-0.815240470077567,227.386281244732,
16.189811234437));
#78579=CARTESIAN_POINT('Ctrl Pts',(-1.60377234629372,227.116890074407,16.2427305228476));
#78580=CARTESIAN_POINT('Ctrl Pts',(-2.24557120641408,226.417998337017,16.2956498112582));
#78581=CARTESIAN_POINT('Ctrl Pts',(-2.44694990459468,225.609418877326,16.3485690996688));
#78582=CARTESIAN_POINT('Ctrl Pts',(-2.49622669896886,225.411561784543,16.3615182989485));
#78583=CARTESIAN_POINT('Ctrl Pts',(-2.5191325886196,225.207136953215,16.3744674982283));
#78584=CARTESIAN_POINT('Ctrl Pts',(-2.51727025050597,225.002300995809,16.387416697508));
#78585=CARTESIAN_POINT('Origin',(0.,225.,10.));
#78586=CARTESIAN_POINT('',(-2.51357028108852,224.999405388847,17.387416697508));
#78587=CARTESIAN_POINT('',(-2.51816163287682,224.997743614195,17.112583302492));
#78588=CARTESIAN_POINT('',(-2.5175,225.,10.));
#78589=CARTESIAN_POINT('Ctrl Pts',(-2.51816163287682,224.997743614195,17.112583302492));
#78590=CARTESIAN_POINT('Ctrl Pts',(-2.51206042535773,225.658837824156,17.0707527282619));
#78591=CARTESIAN_POINT('Ctrl Pts',(-2.24478065864621,226.324297969017,17.0289221540318));
#78592=CARTESIAN_POINT('Ctrl Pts',(-1.77759127638479,226.788609390717,16.9870915798018));
#78593=CARTESIAN_POINT('Ctrl Pts',(-1.18655636669689,227.376003431787,16.9341722913912));
#78594=CARTESIAN_POINT('Ctrl Pts',(-0.275577418352753,227.641470312515,
16.8812530029806));
#78595=CARTESIAN_POINT('Ctrl Pts',(0.538481621265696,227.463532391886,16.82833371457));
#78596=CARTESIAN_POINT('Ctrl Pts',(1.35254066088415,227.285594471258,16.7754144261594));
#78597=CARTESIAN_POINT('Ctrl Pts',(2.06967979177691,226.664251749274,16.7224951377488));
#78598=CARTESIAN_POINT('Ctrl Pts',(2.36173616102469,225.883830644091,16.6695758493382));
#78599=CARTESIAN_POINT('Ctrl Pts',(2.65379253027246,225.103409538909,16.6166565609276));
#78600=CARTESIAN_POINT('Ctrl Pts',(2.52076613787524,224.163910050527,16.563737272517));
#78601=CARTESIAN_POINT('Ctrl Pts',(2.02352985873453,223.495247125967,16.5108179841064));
#78602=CARTESIAN_POINT('Ctrl Pts',(1.52629357959382,222.826584201406,16.4578986956958));
#78603=CARTESIAN_POINT('Ctrl Pts',(0.66484741370963,222.428757840667,16.4049794072852));
#78604=CARTESIAN_POINT('Ctrl Pts',(-0.16661089052257,222.483813378794,16.3520601188746));
#78605=CARTESIAN_POINT('Ctrl Pts',(-0.998069194754779,222.53886891692,16.299140830464));
#78606=CARTESIAN_POINT('Ctrl Pts',(-1.79953963733499,223.046806353913,16.2462215420534));
#78607=CARTESIAN_POINT('Ctrl Pts',(-2.20426935941068,223.775193528496,16.1933022536428));
#78608=CARTESIAN_POINT('Ctrl Pts',(-2.41005039972525,224.14553517222,16.1663959365925));
#78609=CARTESIAN_POINT('Ctrl Pts',(-2.51326924737162,224.572865693797,16.1394896195423));
#78610=CARTESIAN_POINT('Ctrl Pts',(-2.51344539583794,225.000116344878,16.112583302492));
#78611=CARTESIAN_POINT('Ctrl Pts',(-2.51727025050597,225.002300995809,16.387416697508));
#78612=CARTESIAN_POINT('Ctrl Pts',(-2.51152180083078,224.370037077569,16.4273867866389));
#78613=CARTESIAN_POINT('Ctrl Pts',(-2.26979110135257,223.733856106507,16.4673568757697));
#78614=CARTESIAN_POINT('Ctrl Pts',(-1.83921088257949,223.274816376839,16.5073269649006));
#78615=CARTESIAN_POINT('Ctrl Pts',(-1.26913462614288,222.667060518033,16.5602462533112));
#78616=CARTESIAN_POINT('Ctrl Pts',(-0.368023577028847,222.369815982413,
16.6131655417218));
#78617=CARTESIAN_POINT('Ctrl Pts',(0.451773866702606,222.519101861478,16.6660848301324));
#78618=CARTESIAN_POINT('Ctrl Pts',(1.27157131043406,222.668387740542,16.719004118543));
#78619=CARTESIAN_POINT('Ctrl Pts',(2.01005514878293,223.264204034292,16.7719234069536));
#78620=CARTESIAN_POINT('Ctrl Pts',(2.32929519123782,224.0339052228,16.8248426953642));
#78621=CARTESIAN_POINT('Ctrl Pts',(2.64853523369271,224.803606411309,16.8777619837748));
#78622=CARTESIAN_POINT('Ctrl Pts',(2.54853148025362,225.747192494575,16.9306812721853));
#78623=CARTESIAN_POINT('Ctrl Pts',(2.07504564775282,226.432878490558,16.9836005605959));
#78624=CARTESIAN_POINT('Ctrl Pts',(1.60155981525203,227.11856448654,17.0365198490065));
#78625=CARTESIAN_POINT('Ctrl Pts',(0.754591903689518,227.546350395238,17.0894391374172));
#78626=CARTESIAN_POINT('Ctrl Pts',(-0.078285589744484,227.520481411304,
17.1423584258277));
#78627=CARTESIAN_POINT('Ctrl Pts',(-0.911163083178489,227.494612427371,
17.1952777142383));
#78628=CARTESIAN_POINT('Ctrl Pts',(-1.72995015848399,227.015088550806,17.2481970026489));
#78629=CARTESIAN_POINT('Ctrl Pts',(-2.15996986104755,226.301339861412,17.3011162910595));
#78630=CARTESIAN_POINT('Ctrl Pts',(-2.3937275716209,225.913347733231,17.329883093209));
#78631=CARTESIAN_POINT('Ctrl Pts',(-2.5126051329784,225.456142540028,17.3586498953585));
#78632=CARTESIAN_POINT('Ctrl Pts',(-2.51357028108852,224.999405388847,17.387416697508));
#78633=CARTESIAN_POINT('Origin',(0.,225.,10.));
#78634=CARTESIAN_POINT('',(-2.51944987787367,224.998011234297,18.387416697508));
#78635=CARTESIAN_POINT('',(-2.52086470301557,225.001296835693,18.112583302492));
#78636=CARTESIAN_POINT('',(-2.5175,225.,10.));
#78637=CARTESIAN_POINT('Ctrl Pts',(-2.52086470301557,225.001296835693,18.112583302492));
#78638=CARTESIAN_POINT('Ctrl Pts',(-2.52133257653149,225.075824437259,18.1078544138028));
#78639=CARTESIAN_POINT('Ctrl Pts',(-2.51831392254458,225.15031360591,18.1031255251135));
#78640=CARTESIAN_POINT('Ctrl Pts',(-2.51168534756933,225.224480139039,18.0983966364243));
#78641=CARTESIAN_POINT('Ctrl Pts',(-2.43750735482731,226.054451071963,18.0454773480137));
#78642=CARTESIAN_POINT('Ctrl Pts',(-1.91125747041057,226.844018225654,17.9925580596031));
#78643=CARTESIAN_POINT('Ctrl Pts',(-1.17374784032625,227.231875915892,17.9396387711925));
#78644=CARTESIAN_POINT('Ctrl Pts',(-0.436238210241938,227.619733606129,
17.8867194827819));
#78645=CARTESIAN_POINT('Ctrl Pts',(0.512531165509953,227.605881832913,17.8338001943713));
#78646=CARTESIAN_POINT('Ctrl Pts',(1.23840354227387,227.196659054247,17.7808809059607));
#78647=CARTESIAN_POINT('Ctrl Pts',(1.96427591903778,226.787436275581,17.7279616175501));
#78648=CARTESIAN_POINT('Ctrl Pts',(2.46725129681372,225.982842491466,17.6750423291396));
#78649=CARTESIAN_POINT('Ctrl Pts',(2.51716810188636,225.151059857407,17.622123040729));
#78650=CARTESIAN_POINT('Ctrl Pts',(2.56708490695901,224.319277223348,17.5692037523184));
#78651=CARTESIAN_POINT('Ctrl Pts',(2.16394313932837,223.460305739345,17.5162844639078));
#78652=CARTESIAN_POINT('Ctrl Pts',(1.49222048891769,222.967210712155,17.4633651754972));
#78653=CARTESIAN_POINT('Ctrl Pts',(0.820497838507012,222.474115684964,17.4104458870866));
#78654=CARTESIAN_POINT('Ctrl Pts',(-0.119805694683712,222.346897114587,
17.357526598676));
#78655=CARTESIAN_POINT('Ctrl Pts',(-0.898407244656005,222.643770229834,
17.3046073102654));
#78656=CARTESIAN_POINT('Ctrl Pts',(-1.67700879462829,222.940643345081,17.2516880218548));
#78657=CARTESIAN_POINT('Ctrl Pts',(-2.29390836138215,223.661608145953,17.1987687334442));
#78658=CARTESIAN_POINT('Ctrl Pts',(-2.46681270924325,224.476751147095,17.1458494450336));
#78659=CARTESIAN_POINT('Ctrl Pts',(-2.5030431074891,224.647556311476,17.134760730853));
#78660=CARTESIAN_POINT('Ctrl Pts',(-2.51977897969982,224.822496564027,17.1236720166725));
#78661=CARTESIAN_POINT('Ctrl Pts',(-2.51816163287682,224.997743614195,17.112583302492));
#78662=CARTESIAN_POINT('Ctrl Pts',(-2.51357028108852,224.999405388847,17.387416697508));
#78663=CARTESIAN_POINT('Ctrl Pts',(-2.51438061538806,224.61593079506,17.4115691837691));
#78664=CARTESIAN_POINT('Ctrl Pts',(-2.43207200078867,224.232786133973,17.4357216700302));
#78665=CARTESIAN_POINT('Ctrl Pts',(-2.26484979545939,223.891212085232,17.4598741562913));
#78666=CARTESIAN_POINT('Ctrl Pts',(-1.89845769748606,223.142806500668,17.5127934447019));
#78667=CARTESIAN_POINT('Ctrl Pts',(-1.12442117171776,222.593968833764,17.5657127331125));
#78668=CARTESIAN_POINT('Ctrl Pts',(-0.296939296283662,222.495847038768,
17.6186320215231));
#78669=CARTESIAN_POINT('Ctrl Pts',(0.530542579150434,222.397725243773,17.6715513099337));
#78670=CARTESIAN_POINT('Ctrl Pts',(1.41146980425034,222.750319320686,17.7244705983443));
#78671=CARTESIAN_POINT('Ctrl Pts',(1.94273005579705,223.392282534215,17.7773898867549));
#78672=CARTESIAN_POINT('Ctrl Pts',(2.47399030734377,224.034245747745,17.8303091751655));
#78673=CARTESIAN_POINT('Ctrl Pts',(2.65558358533729,224.965578097891,17.8832284635761));
#78674=CARTESIAN_POINT('Ctrl Pts',(2.40441289532158,225.760101295249,17.9361477519867));
#78675=CARTESIAN_POINT('Ctrl Pts',(2.15324220530586,226.554624492607,17.9890670403973));
#78676=CARTESIAN_POINT('Ctrl Pts',(1.46930754728092,227.212338537177,18.0419863288079));
#78677=CARTESIAN_POINT('Ctrl Pts',(0.665577232673735,227.432274763069,18.0949056172185));
#78678=CARTESIAN_POINT('Ctrl Pts',(-0.138153081933449,227.65221098896,18.1478249056291));
#78679=CARTESIAN_POINT('Ctrl Pts',(-1.06167905312287,227.434369396173,18.2007441940397));
#78680=CARTESIAN_POINT('Ctrl Pts',(-1.68239485993616,226.878431717949,18.2536634824503));
#78681=CARTESIAN_POINT('Ctrl Pts',(-2.20534680740171,226.410055226959,18.2982478874695));
#78682=CARTESIAN_POINT('Ctrl Pts',(-2.51336312809547,225.701697049152,18.3428322924888));
#78683=CARTESIAN_POINT('Ctrl Pts',(-2.51944987787367,224.998011234297,18.387416697508));
#78684=CARTESIAN_POINT('Origin',(0.,225.,10.));
#78685=CARTESIAN_POINT('',(-2.51981693572124,225.001815876221,19.387416697508));
#78686=CARTESIAN_POINT('',(-2.51426753931457,225.001426524072,19.112583302492));
#78687=CARTESIAN_POINT('',(-2.5175,225.,10.));
#78688=CARTESIAN_POINT('',(1.91346599666508,226.635987203375,20.));
#78689=CARTESIAN_POINT('Ctrl Pts',(-2.51981693572124,225.001815876221,19.387416697508));
#78690=CARTESIAN_POINT('Ctrl Pts',(-2.51391411286498,224.285104614356,19.4328532664402));
#78691=CARTESIAN_POINT('Ctrl Pts',(-2.19260500873154,223.563882178275,19.4782898353724));
#78692=CARTESIAN_POINT('Ctrl Pts',(-1.6520348486382,223.0949913699,19.5237264043046));
#78693=CARTESIAN_POINT('Ctrl Pts',(-1.02244091405153,222.54888129811,19.5766456927152));
#78694=CARTESIAN_POINT('Ctrl Pts',(-0.0954213187754091,222.3450568217,19.6295649811258));
#78695=CARTESIAN_POINT('Ctrl Pts',(0.704615011959953,222.5783234432,19.6824842695364));
#78696=CARTESIAN_POINT('Ctrl Pts',(1.50465134269532,222.811590064701,19.735403557947));
#78697=CARTESIAN_POINT('Ctrl Pts',(2.17770440888991,223.481947784111,19.7883228463576));
#78698=CARTESIAN_POINT('Ctrl Pts',(2.41590020207929,224.27898939678,19.8412421347682));
#78699=CARTESIAN_POINT('Ctrl Pts',(2.65409599526866,225.07603100945,19.8941614231788));
#78700=CARTESIAN_POINT('Ctrl Pts',(2.45743451545281,225.999756515378,19.9470807115894));
#78701=CARTESIAN_POINT('Ctrl Pts',(1.91346599666508,226.635987203375,20.));
#78702=CARTESIAN_POINT('',(-1.91712497064688,226.638739441994,20.));
#78703=CARTESIAN_POINT('Origin',(0.,225.,20.));
#78704=CARTESIAN_POINT('Ctrl Pts',(-1.91712853756764,226.638742124992,20.));
#78705=CARTESIAN_POINT('Ctrl Pts',(-1.38658184659742,227.25748310036,19.948244384658));
#78706=CARTESIAN_POINT('Ctrl Pts',(-0.527608215846001,227.597070123218,
19.896488769316));
#78707=CARTESIAN_POINT('Ctrl Pts',(0.282369170464696,227.505702112488,19.844733153974));
#78708=CARTESIAN_POINT('Ctrl Pts',(1.11055808540672,227.412279783734,19.7918138655634));
#78709=CARTESIAN_POINT('Ctrl Pts',(1.88752272406553,226.868305377813,19.7388945771528));
#78710=CARTESIAN_POINT('Ctrl Pts',(2.25823158349443,226.122142530554,19.6859752887422));
#78711=CARTESIAN_POINT('Ctrl Pts',(2.62894044292332,225.375979683295,19.6330560003316));
#78712=CARTESIAN_POINT('Ctrl Pts',(2.5933935231223,224.427628394699,19.580136711921));
#78713=CARTESIAN_POINT('Ctrl Pts',(2.16760736434175,223.711328508078,19.5272174235105));
#78714=CARTESIAN_POINT('Ctrl Pts',(1.7418212055612,222.995028621457,19.4742981350999));
#78715=CARTESIAN_POINT('Ctrl Pts',(0.925795807801111,222.510780136812,19.4213788466893));
#78716=CARTESIAN_POINT('Ctrl Pts',(0.0930673314969442,222.480040121849,
19.3684595582787));
#78717=CARTESIAN_POINT('Ctrl Pts',(-0.73966114480722,222.449300106886,19.3155402698681));
#78718=CARTESIAN_POINT('Ctrl Pts',(-1.58909269965547,222.872068561606,19.2626209814575));
#78719=CARTESIAN_POINT('Ctrl Pts',(-2.0665880130911,223.554953135211,19.2097016930469));
#78720=CARTESIAN_POINT('Ctrl Pts',(-2.35869055724325,223.972700316596,19.1773288961952));
#78721=CARTESIAN_POINT('Ctrl Pts',(-2.51160537190243,224.487789375327,19.1449560993436));
#78722=CARTESIAN_POINT('Ctrl Pts',(-2.51426753931457,225.001426524072,19.112583302492));
#78723=CARTESIAN_POINT('Origin',(0.,225.,22.2084234471774));
#78724=CARTESIAN_POINT('',(-3.07861193515008,225.000167983521,0.791576552822533));
#78725=CARTESIAN_POINT('',(-3.06858470798512,225.000715214498,0.708423447177441));
#78726=CARTESIAN_POINT('',(-3.0735,225.,22.2084234471774));
#78727=CARTESIAN_POINT('',(0.793799282532883,222.030777046254,0.));
#78728=CARTESIAN_POINT('Ctrl Pts',(-3.06858470798512,225.000715214498,0.708423447177441));
#78729=CARTESIAN_POINT('Ctrl Pts',(-3.06942183630073,225.474969719701,0.683959451760685));
#78730=CARTESIAN_POINT('Ctrl Pts',(-2.74289880307249,226.973915933301,0.60657616793333));
#78731=CARTESIAN_POINT('Ctrl Pts',(-0.407268936110244,228.609155678633,
0.476273595695376));
#78732=CARTESIAN_POINT('Ctrl Pts',(2.8136368462077,227.3011440524,0.317515730463589));
#78733=CARTESIAN_POINT('Ctrl Pts',(3.45438708523699,223.881452722834,0.158757865231792));
#78734=CARTESIAN_POINT('Ctrl Pts',(1.7810709486973,222.29471665351,0.0529192884105984));
#78735=CARTESIAN_POINT('Ctrl Pts',(0.793799282532894,222.030777046254,0.));
#78736=CARTESIAN_POINT('',(-0.79379928253288,222.030777046254,0.));
#78737=CARTESIAN_POINT('Origin',(0.,225.,0.));
#78738=CARTESIAN_POINT('Ctrl Pts',(-3.07861193515008,225.000167983521,0.791576552822533));
#78739=CARTESIAN_POINT('Ctrl Pts',(-3.07861787757322,225.008358867736,0.79115047086606));
#78740=CARTESIAN_POINT('Ctrl Pts',(-3.0748809971153,226.033849902817,0.737805100498988));
#78741=CARTESIAN_POINT('Ctrl Pts',(-1.94583850483642,228.067541710309,0.631540441721317));
#78742=CARTESIAN_POINT('Ctrl Pts',(1.52182603612892,228.298871095165,0.472782576489527));
#78743=CARTESIAN_POINT('Ctrl Pts',(3.59659353011021,225.51018574291,0.314024711257735));
#78744=CARTESIAN_POINT('Ctrl Pts',(2.38892360237163,222.280232421953,0.156430519094557));
#78745=CARTESIAN_POINT('Ctrl Pts',(0.166093927952955,221.76984766752,0.0517556153419845));
#78746=CARTESIAN_POINT('Ctrl Pts',(-0.795579049799779,222.025472494795,
5.56033084159191E-15));
#78747=CARTESIAN_POINT('Origin',(0.,225.,22.2084234471774));
#78748=CARTESIAN_POINT('',(-3.07140444904293,225.0025819181,1.79157655282252));
#78749=CARTESIAN_POINT('',(-3.07340046570963,224.997190573684,1.70842344717744));
#78750=CARTESIAN_POINT('',(-3.0735,225.,22.2084234471774));
#78751=CARTESIAN_POINT('Ctrl Pts',(-3.07340046570963,224.997190573684,1.70842344717744));
#78752=CARTESIAN_POINT('Ctrl Pts',(-3.06628884246803,225.774992353981,1.66814184889093));
#78753=CARTESIAN_POINT('Ctrl Pts',(-2.37168484978274,227.585923512749,1.57494096219383));
#78754=CARTESIAN_POINT('Ctrl Pts',(0.671786446474784,228.570069051027,1.42882078708613));
#78755=CARTESIAN_POINT('Ctrl Pts',(3.36369902404275,226.372043545379,1.27006292185434));
#78756=CARTESIAN_POINT('Ctrl Pts',(2.97708237215331,222.918244820821,1.11130505662255));
#78757=CARTESIAN_POINT('Ctrl Pts',(-0.134013682612229,221.369828849617,
0.952547191390754));
#78758=CARTESIAN_POINT('Ctrl Pts',(-2.66220321452624,222.870115699926,0.81825332157572));
#78759=CARTESIAN_POINT('Ctrl Pts',(-3.0676110022969,224.449086150263,0.736878740171281));
#78760=CARTESIAN_POINT('Ctrl Pts',(-3.06858470798512,225.000715214498,0.708423447177441));
#78761=CARTESIAN_POINT('Ctrl Pts',(-3.07140444904293,225.0025819181,1.79157655282252));
#78762=CARTESIAN_POINT('Ctrl Pts',(-3.07390606281625,225.316750705799,1.7753328679963));
#78763=CARTESIAN_POINT('Ctrl Pts',(-2.88509438037845,226.651495277729,1.70616989475949));
#78764=CARTESIAN_POINT('Ctrl Pts',(-0.958825582149559,228.5039149863,1.58408763311207));
#78765=CARTESIAN_POINT('Ctrl Pts',(2.42364536547895,227.706056696193,1.42532976788028));
#78766=CARTESIAN_POINT('Ctrl Pts',(3.58799443175235,224.431602766551,1.26657190264849));
#78767=CARTESIAN_POINT('Ctrl Pts',(1.46861466513916,221.677371668161,1.1078140374167));
#78768=CARTESIAN_POINT('Ctrl Pts',(-1.98555294623619,221.963188531272,0.949482254141378));
#78769=CARTESIAN_POINT('Ctrl Pts',(-3.07787982988179,223.991052789571,0.844069759276657));
#78770=CARTESIAN_POINT('Ctrl Pts',(-3.07861193515008,225.000167983521,0.791576552822533));
#78771=CARTESIAN_POINT('Origin',(0.,225.,22.2084234471774));
#78772=CARTESIAN_POINT('',(-3.06945735251731,224.998331954781,2.79157655282253));
#78773=CARTESIAN_POINT('',(-3.07813813283449,225.001105495988,2.70842344717744));
#78774=CARTESIAN_POINT('',(-3.0735,225.,22.2084234471774));
#78775=CARTESIAN_POINT('Ctrl Pts',(-3.07813813283449,225.001105495988,2.70842344717744));
#78776=CARTESIAN_POINT('Ctrl Pts',(-3.07842171245361,225.062261455412,2.70524353443178));
#78777=CARTESIAN_POINT('Ctrl Pts',(-3.04905263632461,226.140881525194,2.64914433327553));
#78778=CARTESIAN_POINT('Ctrl Pts',(-1.78403476954297,228.164490547375,2.54012584370868));
#78779=CARTESIAN_POINT('Ctrl Pts',(1.69089220174611,228.21522353059,2.38136797847689));
#78780=CARTESIAN_POINT('Ctrl Pts',(3.61831520156474,225.323384619251,2.22261011324509));
#78781=CARTESIAN_POINT('Ctrl Pts',(2.23425524535826,222.135582991462,2.0638522480133));
#78782=CARTESIAN_POINT('Ctrl Pts',(-1.19459293999268,221.56929798347,1.90509438278151));
#78783=CARTESIAN_POINT('Ctrl Pts',(-2.9375525643654,223.489815960057,1.78661811583622));
#78784=CARTESIAN_POINT('Ctrl Pts',(-3.07563162074394,224.753168034969,1.72106113730153));
#78785=CARTESIAN_POINT('Ctrl Pts',(-3.07340046570963,224.997190573684,1.70842344717744));
#78786=CARTESIAN_POINT('Ctrl Pts',(-3.06945735251731,224.998331954781,2.79157655282253));
#78787=CARTESIAN_POINT('Ctrl Pts',(-3.06639628624136,225.619418678826,2.75951526512656));
#78788=CARTESIAN_POINT('Ctrl Pts',(-2.58173678204169,227.270042729222,2.67453468901999));
#78789=CARTESIAN_POINT('Ctrl Pts',(0.112777612738978,228.630986010631,2.53663482450283));
#78790=CARTESIAN_POINT('Ctrl Pts',(3.11163588183028,226.874700175507,2.37787695927104));
#78791=CARTESIAN_POINT('Ctrl Pts',(3.26272508945618,223.402688633055,2.21911909403925));
#78792=CARTESIAN_POINT('Ctrl Pts',(0.42776847383237,221.392536757232,2.06036122880745));
#78793=CARTESIAN_POINT('Ctrl Pts',(-2.46856006320185,222.551801968966,1.91784704840188));
#78794=CARTESIAN_POINT('Ctrl Pts',(-3.06575621121678,224.293239792867,1.8282521564069));
#78795=CARTESIAN_POINT('Ctrl Pts',(-3.07140444904293,225.0025819181,1.79157655282252));
#78796=CARTESIAN_POINT('Origin',(0.,225.,22.2084234471774));
#78797=CARTESIAN_POINT('',(-3.07748275168016,224.998327996994,3.79157655282253));
#78798=CARTESIAN_POINT('',(-3.07013338639129,225.002107447932,3.70842344717744));
#78799=CARTESIAN_POINT('',(-3.0735,225.,22.2084234471774));
#78800=CARTESIAN_POINT('Ctrl Pts',(-3.07013338639129,225.002107447932,3.70842344717744));
#78801=CARTESIAN_POINT('Ctrl Pts',(-3.07245621738108,225.369921503297,3.68942593156204));
#78802=CARTESIAN_POINT('Ctrl Pts',(-2.84108114631271,226.759489676162,3.61750912753603));
#78803=CARTESIAN_POINT('Ctrl Pts',(-0.77573256839211,228.548946215303,3.49267303509943));
#78804=CARTESIAN_POINT('Ctrl Pts',(2.56078460694016,227.576657219349,3.33391516986764));
#78805=CARTESIAN_POINT('Ctrl Pts',(3.55367181789592,224.246211645467,3.17515730463585));
#78806=CARTESIAN_POINT('Ctrl Pts',(1.2942387062452,221.605633127976,3.01639943940405));
#78807=CARTESIAN_POINT('Ctrl Pts',(-2.08070002352559,222.062246195024,2.86082148691792));
#78808=CARTESIAN_POINT('Ctrl Pts',(-3.07370245351417,224.04451973933,2.75816282284238));
#78809=CARTESIAN_POINT('Ctrl Pts',(-3.07813813283449,225.001105495988,2.70842344717744));
#78810=CARTESIAN_POINT('Ctrl Pts',(-3.07748275168016,224.998327996994,3.79157655282253));
#78811=CARTESIAN_POINT('Ctrl Pts',(-3.07143800644999,225.919651939133,3.74369766225681));
#78812=CARTESIAN_POINT('Ctrl Pts',(-2.14228137459996,227.869865672693,3.6428994832805));
#78813=CARTESIAN_POINT('Ctrl Pts',(1.17442911621855,228.437658305789,3.48918201589358));
#78814=CARTESIAN_POINT('Ctrl Pts',(3.52505710830432,225.877924122033,3.33042415066179));
#78815=CARTESIAN_POINT('Ctrl Pts',(2.64955297313634,222.514713813743,3.17166628543));
#78816=CARTESIAN_POINT('Ctrl Pts',(-0.650821938137665,221.426037330607,
3.01290842019821));
#78817=CARTESIAN_POINT('Ctrl Pts',(-2.80933951944355,223.167551333338,2.88621184266238));
#78818=CARTESIAN_POINT('Ctrl Pts',(-3.07144877978551,224.594273719291,2.81243455353716));
#78819=CARTESIAN_POINT('Ctrl Pts',(-3.06945735251731,224.998331954781,2.79157655282253));
#78820=CARTESIAN_POINT('Origin',(0.,225.,22.2084234471774));
#78821=CARTESIAN_POINT('',(-3.07449013002601,225.002732289237,4.79157655282253));
#78822=CARTESIAN_POINT('',(-3.07051367074349,224.9977135172,4.70842344717744));
#78823=CARTESIAN_POINT('',(-3.0735,225.,22.2084234471774));
#78824=CARTESIAN_POINT('Ctrl Pts',(-3.07051367074349,224.9977135172,4.70842344717744));
#78825=CARTESIAN_POINT('Ctrl Pts',(-3.06585820728449,225.671564929849,4.67360832869228));
#78826=CARTESIAN_POINT('Ctrl Pts',(-2.51562445587184,227.376589891734,4.58587392179654));
#78827=CARTESIAN_POINT('Ctrl Pts',(0.301020094439488,228.620244073749,4.44522022649019));
#78828=CARTESIAN_POINT('Ctrl Pts',(3.20471405829287,226.710727346758,4.28646236125839));
#78829=CARTESIAN_POINT('Ctrl Pts',(3.17545384212145,223.235553019399,4.12770449602661));
#78830=CARTESIAN_POINT('Ctrl Pts',(0.24001839430402,221.375200499072,3.96894663079481));
#78831=CARTESIAN_POINT('Ctrl Pts',(-2.53753165970314,222.657907037816,3.82918628117842));
#78832=CARTESIAN_POINT('Ctrl Pts',(-3.06598576274026,224.345342370355,3.74234521997263));
#78833=CARTESIAN_POINT('Ctrl Pts',(-3.07013338639129,225.002107447932,3.70842344717744));
#78834=CARTESIAN_POINT('Ctrl Pts',(-3.07449013002601,225.002732289237,4.79157655282253));
#78835=CARTESIAN_POINT('Ctrl Pts',(-3.07640541686727,225.210641245489,4.78079934779766));
#78836=CARTESIAN_POINT('Ctrl Pts',(-2.96239872551369,226.437356865561,4.71710285436219));
#78837=CARTESIAN_POINT('Ctrl Pts',(-1.31414727007755,228.386708628075,4.60048707251613));
#78838=CARTESIAN_POINT('Ctrl Pts',(2.13244936546002,227.9409927036,4.44172920728434));
#78839=CARTESIAN_POINT('Ctrl Pts',(3.62742842558762,224.80368037246,4.28297134205255));
#78840=CARTESIAN_POINT('Ctrl Pts',(1.80258513325755,221.846039756688,4.12421347682075));
#78841=CARTESIAN_POINT('Ctrl Pts',(-1.67198400213467,221.774903431643,3.96545561158896));
#78842=CARTESIAN_POINT('Ctrl Pts',(-3.0299620136904,223.786670051152,3.85457663692289));
#78843=CARTESIAN_POINT('Ctrl Pts',(-3.07811910562385,224.901336626527,3.79661695066741));
#78844=CARTESIAN_POINT('Ctrl Pts',(-3.07748275168016,224.998327996994,3.79157655282253));
#78845=CARTESIAN_POINT('Origin',(0.,225.,22.2084234471774));
#78846=CARTESIAN_POINT('',(-3.06854451144427,224.999957002397,5.79157655282253));
#78847=CARTESIAN_POINT('',(-3.0783647624281,224.999192700359,5.70842344717744));
#78848=CARTESIAN_POINT('',(-3.0735,225.,22.2084234471774));
#78849=CARTESIAN_POINT('Ctrl Pts',(-3.0783647624281,224.999192700359,5.70842344717744));
#78850=CARTESIAN_POINT('Ctrl Pts',(-3.07494752107333,225.972768104595,5.65779072582254));
#78851=CARTESIAN_POINT('Ctrl Pts',(-2.05035872108597,227.970077691126,5.55423871605705));
#78852=CARTESIAN_POINT('Ctrl Pts',(1.35121084102199,228.372092749875,5.39776741788093));
#78853=CARTESIAN_POINT('Ctrl Pts',(3.56586056047961,225.693843436134,5.23900955264916));
#78854=CARTESIAN_POINT('Ctrl Pts',(2.51703483521181,222.380588636929,5.08025168741735));
#78855=CARTESIAN_POINT('Ctrl Pts',(-0.835381072264795,221.464619014198,
4.92149382218557));
#78856=CARTESIAN_POINT('Ctrl Pts',(-2.85574307416149,223.275546289828,4.79755107543892));
#78857=CARTESIAN_POINT('Ctrl Pts',(-3.07293455296969,224.647304815178,4.72652761710288));
#78858=CARTESIAN_POINT('Ctrl Pts',(-3.07051367074349,224.9977135172,4.70842344717744));
#78859=CARTESIAN_POINT('Ctrl Pts',(-3.06854451144427,224.999957002397,5.79157655282253));
#78860=CARTESIAN_POINT('Ctrl Pts',(-3.06848017220945,225.51553097262,5.76498174492791));
#78861=CARTESIAN_POINT('Ctrl Pts',(-2.70083896904008,227.057098457445,5.6854676486227));
#78862=CARTESIAN_POINT('Ctrl Pts',(-0.261298247139434,228.623327421715,
5.55303426390689));
#78863=CARTESIAN_POINT('Ctrl Pts',(2.9023029622151,227.184814842139,5.39427639867509));
#78864=CARTESIAN_POINT('Ctrl Pts',(3.40971661468071,223.746759804953,5.2355185334433));
#78865=CARTESIAN_POINT('Ctrl Pts',(0.796557755474301,221.455670144991,5.07676066821152));
#78866=CARTESIAN_POINT('Ctrl Pts',(-2.31872915212835,222.343678723149,4.92878000800458));
#78867=CARTESIAN_POINT('Ctrl Pts',(-3.06700078769786,224.189746310888,4.83371863620826));
#78868=CARTESIAN_POINT('Ctrl Pts',(-3.07449013002601,225.002732289237,4.79157655282253));
#78869=CARTESIAN_POINT('Origin',(0.,225.,22.2084234471774));
#78870=CARTESIAN_POINT('',(-3.07464793359474,224.997290267855,6.79157655282253));
#78871=CARTESIAN_POINT('',(-3.07288417654997,225.002798479054,6.70842344717745));
#78872=CARTESIAN_POINT('',(-3.0735,225.,22.2084234471774));
#78873=CARTESIAN_POINT('Ctrl Pts',(-3.07288417654997,225.002798479054,6.70842344717745));
#78874=CARTESIAN_POINT('Ctrl Pts',(-3.07522881255163,225.264182411633,6.69489241136339));
#78875=CARTESIAN_POINT('Ctrl Pts',(-2.92508997887231,226.545173952939,6.62844208713874));
#78876=CARTESIAN_POINT('Ctrl Pts',(-1.13665728427362,228.450331936026,6.50907247450349));
#78877=CARTESIAN_POINT('Ctrl Pts',(2.28217117361002,227.826389036385,6.3503146092717));
#78878=CARTESIAN_POINT('Ctrl Pts',(3.61235666314995,224.615735001789,6.1915567440399));
#78879=CARTESIAN_POINT('Ctrl Pts',(1.63651347662755,221.756760278445,6.03279887880811));
#78880=CARTESIAN_POINT('Ctrl Pts',(-1.83706677935009,221.865998420731,5.87404101357633));
#78881=CARTESIAN_POINT('Ctrl Pts',(-3.05774551774456,223.893866766071,5.76591586969943));
#78882=CARTESIAN_POINT('Ctrl Pts',(-3.0785190845995,224.955226162792,5.71071001423313));
#78883=CARTESIAN_POINT('Ctrl Pts',(-3.0783647624281,224.999192700359,5.70842344717744));
#78884=CARTESIAN_POINT('Ctrl Pts',(-3.07464793359474,224.997290267855,6.79157655282253));
#78885=CARTESIAN_POINT('Ctrl Pts',(-3.06713140628724,225.815383238637,6.74916414205817));
#78886=CARTESIAN_POINT('Ctrl Pts',(-2.31086280809112,227.66650877076,6.65383244288321));
#78887=CARTESIAN_POINT('Ctrl Pts',(0.814607649856128,228.540224958348,6.50558145529764));
#78888=CARTESIAN_POINT('Ctrl Pts',(3.41605827048919,226.235849615258,6.34682359006585));
#78889=CARTESIAN_POINT('Ctrl Pts',(2.89113249630378,222.800424752883,6.18806572483406));
#78890=CARTESIAN_POINT('Ctrl Pts',(-0.279757624807835,221.378051070173,
6.02930785960226));
#78891=CARTESIAN_POINT('Ctrl Pts',(-2.70632259531143,222.95346808107,5.89714480226509));
#78892=CARTESIAN_POINT('Ctrl Pts',(-3.06860819669216,224.489623670136,5.81790103333851));
#78893=CARTESIAN_POINT('Ctrl Pts',(-3.06854451144427,224.999957002397,5.79157655282253));
#78894=CARTESIAN_POINT('Origin',(0.,225.,22.2084234471774));
#78895=CARTESIAN_POINT('',(-3.07736981264336,225.001746869892,7.79157655282253));
#78896=CARTESIAN_POINT('',(-3.06879165255757,224.999096735126,7.70842344717744));
#78897=CARTESIAN_POINT('',(-3.0735,225.,22.2084234471774));
#78898=CARTESIAN_POINT('Ctrl Pts',(-3.06879165255757,224.999096735126,7.70842344717744));
#78899=CARTESIAN_POINT('Ctrl Pts',(-3.06729334485985,225.567942995347,7.67907480849364));
#78900=CARTESIAN_POINT('Ctrl Pts',(-2.64281785384595,227.164568935651,7.59680688139924));
#78901=CARTESIAN_POINT('Ctrl Pts',(-0.0729493050082294,228.632004770035,
7.46161966589425));
#78902=CARTESIAN_POINT('Ctrl Pts',(3.01175344912091,227.031285655038,7.30286180066245));
#78903=CARTESIAN_POINT('Ctrl Pts',(3.3400995650489,223.571533988429,7.14410393543066));
#78904=CARTESIAN_POINT('Ctrl Pts',(0.611586690390379,221.419114359437,6.98534607019887));
#78905=CARTESIAN_POINT('Ctrl Pts',(-2.39639172809182,222.448053117521,6.84011924078113));
#78906=CARTESIAN_POINT('Ctrl Pts',(-3.06605904384397,224.241921299909,6.74781169977399));
#78907=CARTESIAN_POINT('Ctrl Pts',(-3.07288417654997,225.002798479054,6.70842344717745));
#78908=CARTESIAN_POINT('Ctrl Pts',(-3.07736981264336,225.001746869892,7.79157655282253));
#78909=CARTESIAN_POINT('Ctrl Pts',(-3.07806420663577,225.103949975987,7.78626582759902));
#78910=CARTESIAN_POINT('Ctrl Pts',(-3.02707587405751,226.223865622706,7.7280358139649));
#78911=CARTESIAN_POINT('Ctrl Pts',(-1.65552872289502,228.233574342207,7.61688651192019));
#78912=CARTESIAN_POINT('Ctrl Pts',(1.81863282742744,228.144734172854,7.4581286466884));
#78913=CARTESIAN_POINT('Ctrl Pts',(3.62838168560431,225.177833412168,7.2993707814566));
#78914=CARTESIAN_POINT('Ctrl Pts',(2.11743576779875,222.048179519659,7.14061291622482));
#78915=CARTESIAN_POINT('Ctrl Pts',(-1.33138728143009,221.620031614681,6.98185505099302));
#78916=CARTESIAN_POINT('Ctrl Pts',(-2.96588661920454,223.573218574879,6.86550959652559));
#78917=CARTESIAN_POINT('Ctrl Pts',(-3.07651001196569,224.794623110004,6.80208343046876));
#78918=CARTESIAN_POINT('Ctrl Pts',(-3.07464793359474,224.997290267855,6.79157655282253));
#78919=CARTESIAN_POINT('Origin',(0.,225.,22.2084234471774));
#78920=CARTESIAN_POINT('',(-3.06937329329591,225.001597633979,8.79157655282253));
#78921=CARTESIAN_POINT('',(-3.07619362820471,224.997680472429,8.70842344717745));
#78922=CARTESIAN_POINT('',(-3.0735,225.,22.2084234471774));
#78923=CARTESIAN_POINT('Ctrl Pts',(-3.07619362820471,224.997680472429,8.70842344717745));
#78924=CARTESIAN_POINT('Ctrl Pts',(-3.06888776444019,225.867759753325,8.66325720562389));
#78925=CARTESIAN_POINT('Ctrl Pts',(-2.22821902191904,227.769621341675,8.56517167565974));
#78926=CARTESIAN_POINT('Ctrl Pts',(0.997195697683612,228.493190660582,8.41416685728499));
#78927=CARTESIAN_POINT('Ctrl Pts',(3.47557956006656,226.05694227482,8.25540899205321));
#78928=CARTESIAN_POINT('Ctrl Pts',(2.77311314575043,222.653380360706,8.09665112682141));
#78929=CARTESIAN_POINT('Ctrl Pts',(-0.467306310506461,221.397444648195,
7.93789326158963));
#78930=CARTESIAN_POINT('Ctrl Pts',(-2.76007210838313,223.061237008611,7.80848403504163));
#78931=CARTESIAN_POINT('Ctrl Pts',(-3.06999498216705,224.542241611707,7.73199409690424));
#78932=CARTESIAN_POINT('Ctrl Pts',(-3.06879165255757,224.999096735126,7.70842344717744));
#78933=CARTESIAN_POINT('Ctrl Pts',(-3.06937329329591,225.001597633979,8.79157655282253));
#78934=CARTESIAN_POINT('Ctrl Pts',(-3.0713022271567,225.410920678304,8.77044822472927));
#78935=CARTESIAN_POINT('Ctrl Pts',(-2.80459016801079,226.843047661762,8.6964006082254));
#78936=CARTESIAN_POINT('Ctrl Pts',(-0.632602258973873,228.57723255616,8.56943370331094));
#78937=CARTESIAN_POINT('Ctrl Pts',(2.66218242386824,227.471753046111,8.41067583807915));
#78938=CARTESIAN_POINT('Ctrl Pts',(3.52053785707391,224.10412524546,8.25191797284736));
#78939=CARTESIAN_POINT('Ctrl Pts',(1.15689718192732,221.556401984935,8.09316010761557));
#78940=CARTESIAN_POINT('Ctrl Pts',(-2.1510494467117,222.140059414158,7.93971296760729));
#78941=CARTESIAN_POINT('Ctrl Pts',(-3.07114484357178,224.085536215108,7.83918511600961));
#78942=CARTESIAN_POINT('Ctrl Pts',(-3.07736981264336,225.001746869892,7.79157655282253));
#78943=CARTESIAN_POINT('Origin',(0.,225.,22.2084234471774));
#78944=CARTESIAN_POINT('',(-3.07154364454433,224.997384898158,9.79157655282253));
#78945=CARTESIAN_POINT('',(-3.07602736676149,225.002377929736,9.70842344717745));
#78946=CARTESIAN_POINT('',(-3.0735,225.,22.2084234471774));
#78947=CARTESIAN_POINT('Ctrl Pts',(-3.07602736676149,225.002377929736,9.70842344717745));
#78948=CARTESIAN_POINT('Ctrl Pts',(-3.07735399945888,225.157754812501,9.70035889116475));
#78949=CARTESIAN_POINT('Ctrl Pts',(-2.99601741917923,226.331315348169,9.63937504674145));
#78950=CARTESIAN_POINT('Ctrl Pts',(-1.48552434035628,228.315116541671,9.52547191390755));
#78951=CARTESIAN_POINT('Ctrl Pts',(1.97934846979805,228.046138520449,9.36671404867575));
#78952=CARTESIAN_POINT('Ctrl Pts',(3.63272163822919,224.989334645098,9.20795618344396));
#78953=CARTESIAN_POINT('Ctrl Pts',(1.96142810620627,221.942291702134,9.04919831821217));
#78954=CARTESIAN_POINT('Ctrl Pts',(-1.50496435148532,221.693663273135,8.89044045298037));
#78955=CARTESIAN_POINT('Ctrl Pts',(-2.99968389613058,223.680849962287,8.77684882930214));
#78956=CARTESIAN_POINT('Ctrl Pts',(-3.0774477220179,224.848326326454,8.71617649403449));
#78957=CARTESIAN_POINT('Ctrl Pts',(-3.07619362820471,224.997680472429,8.70842344717745));
#78958=CARTESIAN_POINT('Ctrl Pts',(-3.07154364454433,224.997384898158,9.79157655282253));
#78959=CARTESIAN_POINT('Ctrl Pts',(-3.06576127037765,225.711873509079,9.75463062185952));
#78960=CARTESIAN_POINT('Ctrl Pts',(-2.46155812568994,227.45857358682,9.6647654024859));
#78961=CARTESIAN_POINT('Ctrl Pts',(0.446144826681538,228.60523690935,9.5219808947017));
#78962=CARTESIAN_POINT('Ctrl Pts',(3.27082189161085,226.580665218277,9.36322302946991));
#78963=CARTESIAN_POINT('Ctrl Pts',(3.10204288995985,223.109468781596,9.20446516423812));
#78964=CARTESIAN_POINT('Ctrl Pts',(0.094274357402458,221.368486441654,9.04570729900631));
#78965=CARTESIAN_POINT('Ctrl Pts',(-2.58800189649888,222.74044730297,8.90807776186779));
#78966=CARTESIAN_POINT('Ctrl Pts',(-3.06647090274457,224.385705425108,8.82336751313986));
#78967=CARTESIAN_POINT('Ctrl Pts',(-3.06937329329591,225.001597633979,8.79157655282253));
#78968=CARTESIAN_POINT('Origin',(0.,225.,22.2084234471774));
#78969=CARTESIAN_POINT('',(-3.07862277358246,224.999944058962,10.7915765528225));
#78970=CARTESIAN_POINT('',(-3.06874142907581,225.000808737075,10.7084234471774));
#78971=CARTESIAN_POINT('',(-3.0735,225.,22.2084234471774));
#78972=CARTESIAN_POINT('Ctrl Pts',(-3.06874142907581,225.000808737075,10.7084234471774));
#78973=CARTESIAN_POINT('Ctrl Pts',(-3.06983205692395,225.46372056142,10.684541288295));
#78974=CARTESIAN_POINT('Ctrl Pts',(-2.75418302977163,226.950963548454,10.6077398410019));
#78975=CARTESIAN_POINT('Ctrl Pts',(-0.446144858320614,228.605237165021,
10.4780191052983));
#78976=CARTESIAN_POINT('Ctrl Pts',(2.78684416371602,227.330296088014,10.3192612400665));
#78977=CARTESIAN_POINT('Ctrl Pts',(3.46931351670972,223.922668122894,10.1605033748347));
#78978=CARTESIAN_POINT('Ctrl Pts',(0.976667275638124,221.501014249336,10.0017455096029));
#78979=CARTESIAN_POINT('Ctrl Pts',(-2.23779834748522,222.241978304803,9.85105220038384));
#78980=CARTESIAN_POINT('Ctrl Pts',(-3.06864868967899,224.138178030039,9.75327817957534));
#78981=CARTESIAN_POINT('Ctrl Pts',(-3.07602736676149,225.002377929736,9.70842344717745));
#78982=CARTESIAN_POINT('Ctrl Pts',(-3.07862228131909,224.999944064338,10.7915765528225));
#78983=CARTESIAN_POINT('Ctrl Pts',(-3.07835022376532,226.014263127402,10.7388130189898));
#78984=CARTESIAN_POINT('Ctrl Pts',(-1.97594900327483,228.046402194062,10.6331301967464));
#78985=CARTESIAN_POINT('Ctrl Pts',(1.48552423500794,228.315116306574,10.4745280860925));
#78986=CARTESIAN_POINT('Ctrl Pts',(3.59084507798282,225.550099995309,10.3157702208607));
#78987=CARTESIAN_POINT('Ctrl Pts',(2.40982464679436,222.281632189969,10.1570123556289));
#78988=CARTESIAN_POINT('Ctrl Pts',(-0.976667206376252,221.501014497472,
9.99825449039707));
#78989=CARTESIAN_POINT('Ctrl Pts',(-2.88922780988848,223.35910399192,9.8764425561283));
#78990=CARTESIAN_POINT('Ctrl Pts',(-3.07404362023996,224.688479920614,9.80754991027012));
#78991=CARTESIAN_POINT('Ctrl Pts',(-3.07154364454433,224.997384898158,9.79157655282253));
#78992=CARTESIAN_POINT('Origin',(0.,225.,22.2084234471774));
#78993=CARTESIAN_POINT('',(-3.07170665790524,225.002650501842,11.7915765528225));
#78994=CARTESIAN_POINT('',(-3.07306319744856,224.997194167395,11.7084234471774));
#78995=CARTESIAN_POINT('',(-3.0735,225.,22.2084234471774));
#78996=CARTESIAN_POINT('Ctrl Pts',(-3.07306319744856,224.997194167395,11.7084234471774));
#78997=CARTESIAN_POINT('Ctrl Pts',(-3.0661317004511,225.763975034882,11.6687236854252));
#78998=CARTESIAN_POINT('Ctrl Pts',(-2.38783086968629,227.563804830108,11.5761046352624));
#78999=CARTESIAN_POINT('Ctrl Pts',(0.632602303835877,228.577232809845,11.430566296689));
#79000=CARTESIAN_POINT('Ctrl Pts',(3.34842961673882,226.408829071393,11.2718084314573));
#79001=CARTESIAN_POINT('Ctrl Pts',(2.99977427607618,222.951065022201,11.1130505662255));
#79002=CARTESIAN_POINT('Ctrl Pts',(-0.0942743640881148,221.36848618412,
10.9542927009937));
#79003=CARTESIAN_POINT('Ctrl Pts',(-2.64958041800097,222.847570317374,10.8194169946443));
#79004=CARTESIAN_POINT('Ctrl Pts',(-3.06741538890292,224.437977266529,10.7374605767056));
#79005=CARTESIAN_POINT('Ctrl Pts',(-3.06874142907581,225.000808737075,10.7084234471774));
#79006=CARTESIAN_POINT('Ctrl Pts',(-3.07170665790524,225.002650501842,11.7915765528225));
#79007=CARTESIAN_POINT('Ctrl Pts',(-3.07420070329748,225.305490608471,11.7759147045306));
#79008=CARTESIAN_POINT('Ctrl Pts',(-2.89394997723761,226.628683144966,11.7073335678281));
#79009=CARTESIAN_POINT('Ctrl Pts',(-0.997195626965866,228.493190412856,
11.585833142715));
#79010=CARTESIAN_POINT('Ctrl Pts',(2.39382145824392,227.732470897368,11.4270752774832));
#79011=CARTESIAN_POINT('Ctrl Pts',(3.59401323900362,224.47099412406,11.2683174122514));
#79012=CARTESIAN_POINT('Ctrl Pts',(1.50496424475834,221.69366350761,11.1095595470196));
#79013=CARTESIAN_POINT('Ctrl Pts',(-1.9614279671085,221.942291918976,10.9508016817878));
#79014=CARTESIAN_POINT('Ctrl Pts',(-3.07726325298195,223.97664313747,10.8448073503888));
#79015=CARTESIAN_POINT('Ctrl Pts',(-3.07862308441559,224.996949859326,10.7917323074004));
#79016=CARTESIAN_POINT('Ctrl Pts',(-3.07862228131909,224.999944064338,10.7915765528225));
#79017=CARTESIAN_POINT('Origin',(0.,225.,22.2084234471774));
#79018=CARTESIAN_POINT('',(-3.06928111681468,224.998485326397,12.7915765528225));
#79019=CARTESIAN_POINT('',(-3.07829294454214,225.000912845446,12.7084234471774));
#79020=CARTESIAN_POINT('',(-3.0735,225.,22.2084234471774));
#79021=CARTESIAN_POINT('Ctrl Pts',(-3.07829294454214,225.000912845446,12.7084234471774));
#79022=CARTESIAN_POINT('Ctrl Pts',(-3.07848869894762,225.050872251671,12.7058253709661));
#79023=CARTESIAN_POINT('Ctrl Pts',(-3.05474886562024,226.118247010729,12.6503080063441));
#79024=CARTESIAN_POINT('Ctrl Pts',(-1.81863295639868,228.144734395868,12.5418713533116));
#79025=CARTESIAN_POINT('Ctrl Pts',(1.65552884029951,228.233574571522,12.3831134880798));
#79026=CARTESIAN_POINT('Ctrl Pts',(3.6145507074577,225.363047426476,12.224355622848));
#79027=CARTESIAN_POINT('Ctrl Pts',(2.26553590928934,222.160259290996,12.0655977576162));
#79028=CARTESIAN_POINT('Ctrl Pts',(-1.15689726397057,221.556401740727,11.9068398923844));
#79029=CARTESIAN_POINT('Ctrl Pts',(-2.9294746139871,223.467029101815,11.7877817889048));
#79030=CARTESIAN_POINT('Ctrl Pts',(-3.07537129969644,224.74186567998,11.7216429738358));
#79031=CARTESIAN_POINT('Ctrl Pts',(-3.07306319744856,224.997194167395,11.7084234471774));
#79032=CARTESIAN_POINT('Ctrl Pts',(-3.06928111681467,224.998485326397,12.7915765528225));
#79033=CARTESIAN_POINT('Ctrl Pts',(-3.06656123751991,225.608388451192,12.7600971016609));
#79034=CARTESIAN_POINT('Ctrl Pts',(-2.59517217214773,227.247458453491,12.6756983620886));
#79035=CARTESIAN_POINT('Ctrl Pts',(0.0729492998349137,228.632004512465,
12.5383803341058));
#79036=CARTESIAN_POINT('Ctrl Pts',(3.09088863886716,226.908713126961,12.3796224688739));
#79037=CARTESIAN_POINT('Ctrl Pts',(3.28004681715442,223.438567562721,12.2208646036422));
#79038=CARTESIAN_POINT('Ctrl Pts',(0.46730627736665,221.397444903677,12.0621067384104));
#79039=CARTESIAN_POINT('Ctrl Pts',(-2.45343773644609,222.529479433023,11.9190107214705));
#79040=CARTESIAN_POINT('Ctrl Pts',(-3.0657736578453,224.282234435491,11.8288339929412));
#79041=CARTESIAN_POINT('Ctrl Pts',(-3.07170665790524,225.002650501842,11.7915765528225));
#79042=CARTESIAN_POINT('Origin',(0.,225.,22.2084234471774));
#79043=CARTESIAN_POINT('',(-3.07723479591964,224.998169491318,13.7915765528225));
#79044=CARTESIAN_POINT('',(-3.07037725608096,225.002226627229,13.7084234471775));
#79045=CARTESIAN_POINT('',(-3.0735,225.,22.2084234471774));
#79046=CARTESIAN_POINT('Ctrl Pts',(-3.07037725608096,225.002226627229,13.7084234471775));
#79047=CARTESIAN_POINT('Ctrl Pts',(-3.07276840434177,225.358704472843,13.6900077680964));
#79048=CARTESIAN_POINT('Ctrl Pts',(-2.85067271507903,226.736670699133,13.6186728006047));
#79049=CARTESIAN_POINT('Ctrl Pts',(-0.814607707625303,228.540225209408,
13.4944185447024));
#79050=CARTESIAN_POINT('Ctrl Pts',(2.53237203947883,227.604586743482,13.3356606794706));
#79051=CARTESIAN_POINT('Ctrl Pts',(3.56172499563507,224.285230592343,13.1769028142388));
#79052=CARTESIAN_POINT('Ctrl Pts',(1.33138737584751,221.620031374985,13.018144949007));
#79053=CARTESIAN_POINT('Ctrl Pts',(-2.06099584336155,222.041172659259,12.8619851599865));
#79054=CARTESIAN_POINT('Ctrl Pts',(-3.07450144722803,224.033266911491,12.7587446593767));
#79055=CARTESIAN_POINT('Ctrl Pts',(-3.07829294454214,225.000912845446,12.7084234471774));
#79056=CARTESIAN_POINT('Ctrl Pts',(-3.07723479591964,224.998169491318,13.7915765528225));
#79057=CARTESIAN_POINT('Ctrl Pts',(-3.07081799507026,225.908490316769,13.7442794987911));
#79058=CARTESIAN_POINT('Ctrl Pts',(-2.1610969881185,227.848485082751,13.6440631563491));
#79059=CARTESIAN_POINT('Ctrl Pts',(1.13665720366575,228.45033169134,13.4909275254965));
#79060=CARTESIAN_POINT('Ctrl Pts',(3.51521679100075,225.9165311185,13.3321696602647));
#79061=CARTESIAN_POINT('Ctrl Pts',(2.6766501094444,222.54392130205,13.1734117950329));
#79062=CARTESIAN_POINT('Ctrl Pts',(-0.611586647018769,221.419114613381,
13.0146539298011));
#79063=CARTESIAN_POINT('Ctrl Pts',(-2.79907365008124,223.144739589274,12.887375515731));
#79064=CARTESIAN_POINT('Ctrl Pts',(-3.07113355601754,224.583096135967,12.8130163900715));
#79065=CARTESIAN_POINT('Ctrl Pts',(-3.06928111681467,224.998485326397,12.7915765528225));
#79066=CARTESIAN_POINT('Origin',(0.,225.,22.2084234471774));
#79067=CARTESIAN_POINT('',(-3.07482903252357,225.002680185515,14.7915765528225));
#79068=CARTESIAN_POINT('',(-3.07026214607982,224.997827572026,14.7084234471775));
#79069=CARTESIAN_POINT('',(-3.0735,225.,22.2084234471774));
#79070=CARTESIAN_POINT('Ctrl Pts',(-3.07026214607981,224.997827572026,14.7084234471775));
#79071=CARTESIAN_POINT('Ctrl Pts',(-3.06593583898703,225.660553986291,14.6741901652266));
#79072=CARTESIAN_POINT('Ctrl Pts',(-2.52994317982435,227.354129803758,14.5870375948652));
#79073=CARTESIAN_POINT('Ctrl Pts',(0.261298265669851,228.62332767867,14.4469657360931));
#79074=CARTESIAN_POINT('Ctrl Pts',(3.18575953691054,226.745771011226,14.2882078708613));
#79075=CARTESIAN_POINT('Ctrl Pts',(3.19461380524764,223.270484782959,14.1294500056295));
#79076=CARTESIAN_POINT('Ctrl Pts',(0.279757644647243,221.378050813317,13.9706921403977));
#79077=CARTESIAN_POINT('Ctrl Pts',(-2.52331408064506,222.6354313281,13.830349954247));
#79078=CARTESIAN_POINT('Ctrl Pts',(-3.065897201608,224.334329871127,13.7429270565069));
#79079=CARTESIAN_POINT('Ctrl Pts',(-3.07037725608096,225.002226627229,13.7084234471775));
#79080=CARTESIAN_POINT('Ctrl Pts',(-3.07482903252357,225.002680185515,14.7915765528225));
#79081=CARTESIAN_POINT('Ctrl Pts',(-3.07662789737314,225.199308810663,14.781381184332));
#79082=CARTESIAN_POINT('Ctrl Pts',(-2.96986772218245,226.414596975574,14.7182665274308));
#79083=CARTESIAN_POINT('Ctrl Pts',(-1.35121074519871,228.372092510738,14.6022325821191));
#79084=CARTESIAN_POINT('Ctrl Pts',(2.10006683807499,227.964202701323,14.4434747168873));
#79085=CARTESIAN_POINT('Ctrl Pts',(3.62936333372522,224.843474696222,14.2847168516555));
#79086=CARTESIAN_POINT('Ctrl Pts',(1.83706664907154,221.865998642983,14.1259589864237));
#79087=CARTESIAN_POINT('Ctrl Pts',(-1.6365133605716,221.756760508445,13.9672011211919));
#79088=CARTESIAN_POINT('Ctrl Pts',(-3.02371435647241,223.763990945825,13.8557403099915));
#79089=CARTESIAN_POINT('Ctrl Pts',(-3.07799756559058,224.889959008746,13.7971987872017));
#79090=CARTESIAN_POINT('Ctrl Pts',(-3.07723479591964,224.998169491318,13.7915765528225));
#79091=CARTESIAN_POINT('Origin',(0.,225.,22.2084234471774));
#79092=CARTESIAN_POINT('',(-3.06854992020173,225.000142040112,15.7915765528225));
#79093=CARTESIAN_POINT('',(-3.078224281555,224.998996872852,15.7084234471775));
#79094=CARTESIAN_POINT('',(-3.0735,225.,22.2084234471774));
#79095=CARTESIAN_POINT('Ctrl Pts',(-3.078224281555,224.998996872852,15.7084234471775));
#79096=CARTESIAN_POINT('Ctrl Pts',(-3.07412471449684,225.96150182405,15.6583725623569));
#79097=CARTESIAN_POINT('Ctrl Pts',(-2.07017713194897,227.949046013955,15.5554023891256));
#79098=CARTESIAN_POINT('Ctrl Pts',(1.31414736327247,228.386708868249,15.3995129274839));
#79099=CARTESIAN_POINT('Ctrl Pts',(3.55803662804284,225.732909001281,15.2407550622521));
#79100=CARTESIAN_POINT('Ctrl Pts',(2.54561091074421,222.408350845166,15.0819971970203));
#79101=CARTESIAN_POINT('Ctrl Pts',(-0.796557811963526,221.455669893639,
14.9232393317885));
#79102=CARTESIAN_POINT('Ctrl Pts',(-2.84623604737516,223.252727349544,14.7987147485075));
#79103=CARTESIAN_POINT('Ctrl Pts',(-3.07262363167733,224.636082820945,14.7271094536372));
#79104=CARTESIAN_POINT('Ctrl Pts',(-3.07026214607981,224.997827572026,14.7084234471775));
#79105=CARTESIAN_POINT('Ctrl Pts',(-3.06854992020173,225.000142040112,15.7915765528225));
#79106=CARTESIAN_POINT('Ctrl Pts',(-3.06875783160601,225.504434156461,15.7655635814622));
#79107=CARTESIAN_POINT('Ctrl Pts',(-2.71259519013905,227.034352506937,15.6866313216913));
#79108=CARTESIAN_POINT('Ctrl Pts',(-0.301020073092202,228.620243817014,
15.5547797735098));
#79109=CARTESIAN_POINT('Ctrl Pts',(2.87816724394823,227.216513409565,15.396021908278));
#79110=CARTESIAN_POINT('Ctrl Pts',(3.4232560124835,223.784230016872,15.2372640430462));
#79111=CARTESIAN_POINT('Ctrl Pts',(0.835381013022407,221.464619264915,15.0785061778144));
#79112=CARTESIAN_POINT('Ctrl Pts',(-2.30174382348909,222.321765613181,14.9299436810732));
#79113=CARTESIAN_POINT('Ctrl Pts',(-3.06729084909732,224.178703529587,14.8343004727426));
#79114=CARTESIAN_POINT('Ctrl Pts',(-3.07482903252357,225.002680185515,14.7915765528225));
#79115=CARTESIAN_POINT('Origin',(0.,225.,22.2084234471774));
#79116=CARTESIAN_POINT('',(-3.07430775715862,224.997245282316,16.7915765528225));
#79117=CARTESIAN_POINT('',(-3.07321950940619,225.002809179988,16.7084234471775));
#79118=CARTESIAN_POINT('',(-3.0735,225.,22.2084234471774));
#79119=CARTESIAN_POINT('Ctrl Pts',(-3.07321950940619,225.002809179988,16.7084234471775));
#79120=CARTESIAN_POINT('Ctrl Pts',(-3.07549315238226,225.252883982405,16.6954742478977));
#79121=CARTESIAN_POINT('Ctrl Pts',(-2.93324531242376,226.5223824011,16.6296057602074));
#79122=CARTESIAN_POINT('Ctrl Pts',(-1.174429199505,228.437658549578,16.5108179841064));
#79123=CARTESIAN_POINT('Ctrl Pts',(2.25103651630915,227.851247946737,16.3520601188746));
#79124=CARTESIAN_POINT('Ctrl Pts',(3.61635370100267,224.655375334543,16.1933022536428));
#79125=CARTESIAN_POINT('Ctrl Pts',(1.67198412070606,221.77490320293,16.034544388411));
#79126=CARTESIAN_POINT('Ctrl Pts',(-1.80258526109082,221.84603953302,15.8757865231792));
#79127=CARTESIAN_POINT('Ctrl Pts',(-3.0521184279115,223.871238113346,15.7670795427681));
#79128=CARTESIAN_POINT('Ctrl Pts',(-3.0784592267095,224.94383595677,15.7112918507675));
#79129=CARTESIAN_POINT('Ctrl Pts',(-3.078224281555,224.998996872852,15.7084234471775));
#79130=CARTESIAN_POINT('Ctrl Pts',(-3.07430775715862,224.997245282316,16.7915765528225));
#79131=CARTESIAN_POINT('Ctrl Pts',(-3.06685907342071,225.804344807366,16.7497459785925));
#79132=CARTESIAN_POINT('Ctrl Pts',(-2.3277397025553,227.644568216933,16.6549961159518));
#79133=CARTESIAN_POINT('Ctrl Pts',(0.77573251337774,228.548945963627,16.5073269649006));
#79134=CARTESIAN_POINT('Ctrl Pts',(3.40229908990077,226.273239680388,16.3485690996688));
#79135=CARTESIAN_POINT('Ctrl Pts',(2.91508167139093,222.832264493646,16.189811234437));
#79136=CARTESIAN_POINT('Ctrl Pts',(-0.24001837728243,221.37520075613,16.0310533692052));
#79137=CARTESIAN_POINT('Ctrl Pts',(-2.69447339772875,222.930728603527,15.8983084753337));
#79138=CARTESIAN_POINT('Ctrl Pts',(-3.06833486863825,224.478531364404,15.8184828698728));
#79139=CARTESIAN_POINT('Ctrl Pts',(-3.06854992020173,225.000142040112,15.7915765528225));
#79140=CARTESIAN_POINT('Origin',(0.,225.,22.2084234471774));
#79141=CARTESIAN_POINT('',(-3.07760781120887,225.001583247072,17.7915765528225));
#79142=CARTESIAN_POINT('',(-3.06870238686219,224.999274066583,17.7084234471775));
#79143=CARTESIAN_POINT('',(-3.0735,225.,22.2084234471774));
#79144=CARTESIAN_POINT('Ctrl Pts',(-3.06870238686219,224.999274066583,17.7084234471775));
#79145=CARTESIAN_POINT('Ctrl Pts',(-3.06752408191027,225.556883454529,17.679656645028));
#79146=CARTESIAN_POINT('Ctrl Pts',(-2.65540744149069,227.141891306754,17.5979705544679));
#79147=CARTESIAN_POINT('Ctrl Pts',(-0.112777620733934,228.630986268181,
17.4633651754972));
#79148=CARTESIAN_POINT('Ctrl Pts',(2.98929492288558,227.064193826811,17.3046073102654));
#79149=CARTESIAN_POINT('Ctrl Pts',(3.35556487664332,223.608251232666,17.1458494450336));
#79150=CARTESIAN_POINT('Ctrl Pts',(0.650821984291496,221.426037077147,16.9870915798018));
#79151=CARTESIAN_POINT('Ctrl Pts',(-2.38035569234535,222.425914952088,16.8412829138497));
#79152=CARTESIAN_POINT('Ctrl Pts',(-3.06620149150084,224.230907232535,16.7483935363083));
#79153=CARTESIAN_POINT('Ctrl Pts',(-3.07321950940619,225.002809179988,16.7084234471775));
#79154=CARTESIAN_POINT('Ctrl Pts',(-3.07760781120886,225.001583247072,17.7915765528225));
#79155=CARTESIAN_POINT('Ctrl Pts',(-3.07817901647247,225.092570569182,17.7868476641333));
#79156=CARTESIAN_POINT('Ctrl Pts',(-3.03325241567471,226.201192212555,17.7291994870335));
#79157=CARTESIAN_POINT('Ctrl Pts',(-1.69089208164927,228.215223302252,17.6186320215231));
#79158=CARTESIAN_POINT('Ctrl Pts',(1.7840346429268,228.164490323129,17.4598741562913));
#79159=CARTESIAN_POINT('Ctrl Pts',(3.6262131814702,225.217615651258,17.3011162910595));
#79160=CARTESIAN_POINT('Ctrl Pts',(2.14968143631101,222.071579278568,17.1423584258277));
#79161=CARTESIAN_POINT('Ctrl Pts',(-1.29423861444767,221.60563336867,16.9836005605959));
#79162=CARTESIAN_POINT('Ctrl Pts',(-2.95834120127935,223.550454624517,16.8666732695942));
#79163=CARTESIAN_POINT('Ctrl Pts',(-3.07628230153224,224.783294216301,16.8026652670031));
#79164=CARTESIAN_POINT('Ctrl Pts',(-3.07430775715862,224.997245282316,16.7915765528225));
#79165=CARTESIAN_POINT('Origin',(0.,225.,22.2084234471774));
#79166=CARTESIAN_POINT('',(-3.06955363737172,225.001741577652,18.7915765528225));
#79167=CARTESIAN_POINT('',(-3.07588051624417,224.997572007392,18.7084234471775));
#79168=CARTESIAN_POINT('',(-3.0735,225.,22.2084234471774));
#79169=CARTESIAN_POINT('Ctrl Pts',(-3.07588051624417,224.997572007392,18.7084234471775));
#79170=CARTESIAN_POINT('Ctrl Pts',(-3.06844948329747,225.856669664575,18.6638390421582));
#79171=CARTESIAN_POINT('Ctrl Pts',(-2.24606376672136,227.747944926667,18.5663353487284));
#79172=CARTESIAN_POINT('Ctrl Pts',(0.958825650497796,228.503915237338,18.4159123668879));
#79173=CARTESIAN_POINT('Ctrl Pts',(3.46377878428887,226.094996727722,18.2571545016561));
#79174=CARTESIAN_POINT('Ctrl Pts',(2.79868213295254,222.683934191666,18.0983966364244));
#79175=CARTESIAN_POINT('Ctrl Pts',(-0.427768504200867,221.39253650103,17.9396387711925));
#79176=CARTESIAN_POINT('Ctrl Pts',(-2.74903334262051,223.038450531923,17.8096477081103));
#79177=CARTESIAN_POINT('Ctrl Pts',(-3.06969168675082,224.531107566481,17.7325759334386));
#79178=CARTESIAN_POINT('Ctrl Pts',(-3.06870238686219,224.999274066583,17.7084234471775));
#79179=CARTESIAN_POINT('Ctrl Pts',(-3.06955363737172,225.001741577652,18.7915765528225));
#79180=CARTESIAN_POINT('Ctrl Pts',(-3.07161643466669,225.39973657835,18.7710300612636));
#79181=CARTESIAN_POINT('Ctrl Pts',(-2.81478278977398,226.820249470738,18.697564281294));
#79182=CARTESIAN_POINT('Ctrl Pts',(-0.671786392406203,228.570068782136,
18.5711792129139));
#79183=CARTESIAN_POINT('Ctrl Pts',(2.6349094131999,227.500806238298,18.4124213476821));
#79184=CARTESIAN_POINT('Ctrl Pts',(3.53015369719777,224.142786739032,18.2536634824503));
#79185=CARTESIAN_POINT('Ctrl Pts',(1.19459285411968,221.569298229067,18.0949056172185));
#79186=CARTESIAN_POINT('Ctrl Pts',(-2.13212068041073,222.118715376741,17.9408766406759));
#79187=CARTESIAN_POINT('Ctrl Pts',(-3.07178686430458,224.074364251189,17.8397669525439));
#79188=CARTESIAN_POINT('Ctrl Pts',(-3.07760781120886,225.001583247072,17.7915765528225));
#79189=CARTESIAN_POINT('Origin',(0.,225.,22.2084234471774));
#79190=CARTESIAN_POINT('',(-3.07038312444426,224.996706709974,19.7915765528225));
#79191=CARTESIAN_POINT('',(-3.07632864029364,225.002216919788,19.7084234471775));
#79192=CARTESIAN_POINT('',(-3.0735,225.,22.2084234471774));
#79193=CARTESIAN_POINT('',(-0.793799282532889,222.030777046254,20.));
#79194=CARTESIAN_POINT('Ctrl Pts',(-0.793799282532863,222.030777046254,
20.));
#79195=CARTESIAN_POINT('Ctrl Pts',(-1.78107094869726,222.29471665351,19.9470807115894));
#79196=CARTESIAN_POINT('Ctrl Pts',(-2.87946818977925,223.336279021215,19.8776062291969));
#79197=CARTESIAN_POINT('Ctrl Pts',(-3.07279576536299,224.676472836184,19.8081317468044));
#79198=CARTESIAN_POINT('Ctrl Pts',(-3.07038312444426,224.996706709974,19.7915765528225));
#79199=CARTESIAN_POINT('',(0.795577463231005,222.025477587473,20.));
#79200=CARTESIAN_POINT('Origin',(0.,225.,20.));
#79201=CARTESIAN_POINT('Ctrl Pts',(0.795579197825938,222.025472417912,20.));
#79202=CARTESIAN_POINT('Ctrl Pts',(-0.166093587115772,221.769847778298,
19.948244384658));
#79203=CARTESIAN_POINT('Ctrl Pts',(-2.23002435410521,222.243746776087,19.8510522003838));
#79204=CARTESIAN_POINT('Ctrl Pts',(-3.06912215526932,224.127217093236,19.7538600161097));
#79205=CARTESIAN_POINT('Ctrl Pts',(-3.07632864029364,225.002216919788,19.7084234471775));
#79206=CARTESIAN_POINT('Origin',(160.,225.,22.2084234471774));
#79207=CARTESIAN_POINT('',(156.921337686793,225.000165205707,0.791576552822524));
#79208=CARTESIAN_POINT('',(156.931363809071,225.000702042684,0.708423447177432));
#79209=CARTESIAN_POINT('',(156.9265,225.,22.2084234471774));
#79210=CARTESIAN_POINT('',(160.793799282533,222.030777046254,0.));
#79211=CARTESIAN_POINT('Ctrl Pts',(156.931363809071,225.000702042684,0.708423447177431));
#79212=CARTESIAN_POINT('Ctrl Pts',(156.93052536392,225.474958108265,0.683959451760675));
#79213=CARTESIAN_POINT('Ctrl Pts',(157.257049637554,226.973918093966,0.606576167933322));
#79214=CARTESIAN_POINT('Ctrl Pts',(159.592724492903,228.609330790972,0.47627359569537));
#79215=CARTESIAN_POINT('Ctrl Pts',(162.813708975205,227.300991022112,0.317515730463582));
#79216=CARTESIAN_POINT('Ctrl Pts',(163.454303623542,223.882029725929,0.158757865231786));
#79217=CARTESIAN_POINT('Ctrl Pts',(161.781070948697,222.29471665351,0.0529192884105924));
#79218=CARTESIAN_POINT('Ctrl Pts',(160.793799282533,222.030777046254,-4.44089209850063E-15));
#79219=CARTESIAN_POINT('',(159.206200717467,222.030777046254,0.));
#79220=CARTESIAN_POINT('Origin',(160.,225.,0.));
#79221=CARTESIAN_POINT('Ctrl Pts',(156.921337686793,225.000165205707,0.791576552822524));
#79222=CARTESIAN_POINT('Ctrl Pts',(156.921331738014,225.008356241664,0.791150470866056));
#79223=CARTESIAN_POINT('Ctrl Pts',(156.925067879715,226.033866332656,0.73780510049899));
#79224=CARTESIAN_POINT('Ctrl Pts',(158.05412312597,228.067610591205,0.631540441721325));
#79225=CARTESIAN_POINT('Ctrl Pts',(161.521864702141,228.298893654481,0.472782576489533));
#79226=CARTESIAN_POINT('Ctrl Pts',(163.59662383415,225.510249900124,0.314024711257741));
#79227=CARTESIAN_POINT('Ctrl Pts',(162.389027673369,222.280093327593,0.156430519094562));
#79228=CARTESIAN_POINT('Ctrl Pts',(160.166034912224,221.769854531922,0.0517556153419853));
#79229=CARTESIAN_POINT('Ctrl Pts',(159.204403756969,222.025437709964,5.35135087284533E-15));
#79230=CARTESIAN_POINT('Origin',(160.,225.,22.2084234471774));
#79231=CARTESIAN_POINT('',(156.928544657468,225.00258189294,1.79157655282252));
#79232=CARTESIAN_POINT('',(156.926548550309,224.997190523908,1.70842344717743));
#79233=CARTESIAN_POINT('',(156.9265,225.,22.2084234471774));
#79234=CARTESIAN_POINT('Ctrl Pts',(156.926548550309,224.997190523908,1.70842344717743));
#79235=CARTESIAN_POINT('Ctrl Pts',(156.933660165655,225.775004947959,1.66814184889092));
#79236=CARTESIAN_POINT('Ctrl Pts',(157.628275269786,227.585965325339,1.57494096219383));
#79237=CARTESIAN_POINT('Ctrl Pts',(160.671798784727,228.570131009447,1.42882078708613));
#79238=CARTESIAN_POINT('Ctrl Pts',(163.363752796435,226.372061137603,1.27006292185433));
#79239=CARTESIAN_POINT('Ctrl Pts',(162.977135122943,222.918220049959,1.11130505662254));
#79240=CARTESIAN_POINT('Ctrl Pts',(159.865978920635,221.369750301164,0.952547191390749));
#79241=CARTESIAN_POINT('Ctrl Pts',(157.337757826407,222.870106331044,0.818253321575712));
#79242=CARTESIAN_POINT('Ctrl Pts',(156.932339046436,224.449071163496,0.736878740171274));
#79243=CARTESIAN_POINT('Ctrl Pts',(156.931363809071,225.000702042684,0.708423447177431));
#79244=CARTESIAN_POINT('Ctrl Pts',(156.928544657468,225.00258189294,1.79157655282252));
#79245=CARTESIAN_POINT('Ctrl Pts',(156.926043002634,225.316755878999,1.7753328679963));
#79246=CARTESIAN_POINT('Ctrl Pts',(157.114857812095,226.651522572006,1.70616989475949));
#79247=CARTESIAN_POINT('Ctrl Pts',(159.041158479961,228.50397348879,1.58408763311208));
#79248=CARTESIAN_POINT('Ctrl Pts',(162.423685640744,227.706100715127,1.42532976788028));
#79249=CARTESIAN_POINT('Ctrl Pts',(163.588053642863,224.431594906927,1.2665719026485));
#79250=CARTESIAN_POINT('Ctrl Pts',(161.468639564753,221.677313682196,1.1078140374167));
#79251=CARTESIAN_POINT('Ctrl Pts',(158.014412901123,221.963143608921,0.949482254141379));
#79252=CARTESIAN_POINT('Ctrl Pts',(156.922070575081,223.99103131721,0.844069759276654));
#79253=CARTESIAN_POINT('Ctrl Pts',(156.921337686793,225.000165205707,0.791576552822524));
#79254=CARTESIAN_POINT('Origin',(160.,225.,22.2084234471774));
#79255=CARTESIAN_POINT('',(156.930491779875,224.998331926605,2.79157655282252));
#79256=CARTESIAN_POINT('',(156.921810795731,225.001105518347,2.70842344717743));
#79257=CARTESIAN_POINT('',(156.9265,225.,22.2084234471774));
#79258=CARTESIAN_POINT('Ctrl Pts',(156.921810795731,225.001105518347,2.70842344717743));
#79259=CARTESIAN_POINT('Ctrl Pts',(156.92152721133,225.062262492373,2.70524353443178));
#79260=CARTESIAN_POINT('Ctrl Pts',(156.950896773024,226.140900456302,2.64914433327553));
#79261=CARTESIAN_POINT('Ctrl Pts',(158.215935612034,228.164543027245,2.54012584370868));
#79262=CARTESIAN_POINT('Ctrl Pts',(161.69092028973,228.215276931872,2.38136797847688));
#79263=CARTESIAN_POINT('Ctrl Pts',(163.618375178607,225.323389882532,2.22261011324509));
#79264=CARTESIAN_POINT('Ctrl Pts',(162.23429242903,222.135535662507,2.0638522480133));
#79265=CARTESIAN_POINT('Ctrl Pts',(158.805387032225,221.569240674643,1.90509438278151));
#79266=CARTESIAN_POINT('Ctrl Pts',(157.062398923068,223.489791358345,1.78661811583621));
#79267=CARTESIAN_POINT('Ctrl Pts',(156.924317397752,224.753164018422,1.72106113730152));
#79268=CARTESIAN_POINT('Ctrl Pts',(156.926548550309,224.997190523908,1.70842344717743));
#79269=CARTESIAN_POINT('Ctrl Pts',(156.930491779875,224.998331926605,2.79157655282252));
#79270=CARTESIAN_POINT('Ctrl Pts',(156.933552896885,225.619428942765,2.75951526512655));
#79271=CARTESIAN_POINT('Ctrl Pts',(157.418220432956,227.270080346152,2.67453468901999));
#79272=CARTESIAN_POINT('Ctrl Pts',(160.112779481517,228.63104619244,2.53663482450283));
#79273=CARTESIAN_POINT('Ctrl Pts',(163.111687448995,226.874731226991,2.37787695927104));
#79274=CARTESIAN_POINT('Ctrl Pts',(163.262779158505,223.402662193936,2.21911909403925));
#79275=CARTESIAN_POINT('Ctrl Pts',(160.427775566504,221.392476912117,2.06036122880746));
#79276=CARTESIAN_POINT('Ctrl Pts',(157.531399019878,222.551761497166,1.91784704840188));
#79277=CARTESIAN_POINT('Ctrl Pts',(156.934192988001,224.293228030656,1.8282521564069));
#79278=CARTESIAN_POINT('Ctrl Pts',(156.928544657468,225.00258189294,1.79157655282252));
#79279=CARTESIAN_POINT('Origin',(160.,225.,22.2084234471774));
#79280=CARTESIAN_POINT('',(156.922466247698,224.998327969291,3.79157655282252));
#79281=CARTESIAN_POINT('',(156.929815672431,225.002107482967,3.70842344717743));
#79282=CARTESIAN_POINT('',(156.9265,225.,22.2084234471774));
#79283=CARTESIAN_POINT('Ctrl Pts',(156.929815672431,225.002107482967,3.70842344717743));
#79284=CARTESIAN_POINT('Ctrl Pts',(156.927492802909,225.369927641302,3.68942593156203));
#79285=CARTESIAN_POINT('Ctrl Pts',(157.158871713077,226.759518870601,3.61750912753603));
#79286=CARTESIAN_POINT('Ctrl Pts',(159.224254559927,228.549005100767,3.49267303509943));
#79287=CARTESIAN_POINT('Ctrl Pts',(162.560827097429,227.576699973488,3.33391516986764));
#79288=CARTESIAN_POINT('Ctrl Pts',(163.553730780998,224.246199136404,3.17515730463585));
#79289=CARTESIAN_POINT('Ctrl Pts',(161.29426018331,221.605576810485,3.01639943940405));
#79290=CARTESIAN_POINT('Ctrl Pts',(157.919265447971,222.062197443487,2.86082148691792));
#79291=CARTESIAN_POINT('Ctrl Pts',(156.92624654986,224.044503891545,2.75816282284237));
#79292=CARTESIAN_POINT('Ctrl Pts',(156.921810795731,225.001105518347,2.70842344717743));
#79293=CARTESIAN_POINT('Ctrl Pts',(156.922466247698,224.998327969291,3.79157655282252));
#79294=CARTESIAN_POINT('Ctrl Pts',(156.928511093102,225.919667179771,3.74369766225681));
#79295=CARTESIAN_POINT('Ctrl Pts',(157.857683123109,227.869913232578,3.6428994832805));
#79296=CARTESIAN_POINT('Ctrl Pts',(161.174448579081,228.437715275457,3.48918201589359));
#79297=CARTESIAN_POINT('Ctrl Pts',(163.525115526208,225.877938670865,3.3304241506618));
#79298=CARTESIAN_POINT('Ctrl Pts',(162.649596882032,222.514672627688,3.17166628543));
#79299=CARTESIAN_POINT('Ctrl Pts',(159.349167276316,221.4259781011,3.01290842019821));
#79300=CARTESIAN_POINT('Ctrl Pts',(157.190613923645,223.167520967189,2.88621184266239));
#79301=CARTESIAN_POINT('Ctrl Pts',(156.928500319601,224.594266995409,2.81243455353715));
#79302=CARTESIAN_POINT('Ctrl Pts',(156.930491779875,224.998331926605,2.79157655282252));
#79303=CARTESIAN_POINT('Origin',(160.,225.,22.2084234471774));
#79304=CARTESIAN_POINT('',(156.925458918946,225.002732334518,4.79157655282252));
#79305=CARTESIAN_POINT('',(156.929435381723,224.997713479262,4.70842344717743));
#79306=CARTESIAN_POINT('',(156.9265,225.,22.2084234471774));
#79307=CARTESIAN_POINT('Ctrl Pts',(156.929435381723,224.997713479262,4.70842344717743));
#79308=CARTESIAN_POINT('Ctrl Pts',(156.934090922428,225.671576072799,4.67360832869228));
#79309=CARTESIAN_POINT('Ctrl Pts',(157.484333803602,227.376629325332,4.58587392179653));
#79310=CARTESIAN_POINT('Ctrl Pts',(160.301025089113,228.620304142684,4.44522022649019));
#79311=CARTESIAN_POINT('Ctrl Pts',(163.20476723256,226.710755732037,4.28646236125839));
#79312=CARTESIAN_POINT('Ctrl Pts',(163.175506530854,223.235523742761,4.1277044960266));
#79313=CARTESIAN_POINT('Ctrl Pts',(160.240022376856,221.375140354604,3.96894663079481));
#79314=CARTESIAN_POINT('Ctrl Pts',(157.462426236202,222.657868176513,3.82918628117842));
#79315=CARTESIAN_POINT('Ctrl Pts',(156.933963364886,224.345331507984,3.74234521997263));
#79316=CARTESIAN_POINT('Ctrl Pts',(156.929815672431,225.002107482967,3.70842344717743));
#79317=CARTESIAN_POINT('Ctrl Pts',(156.925458918946,225.002732334518,4.79157655282252));
#79318=CARTESIAN_POINT('Ctrl Pts',(156.923543600364,225.210644736276,4.78079934779765));
#79319=CARTESIAN_POINT('Ctrl Pts',(157.037552181058,226.437380685709,4.71710285436219));
#79320=CARTESIAN_POINT('Ctrl Pts',(158.685830951627,228.386764753245,4.60048707251613));
#79321=CARTESIAN_POINT('Ctrl Pts',(162.132484704811,227.941041442286,4.44172920728434));
#79322=CARTESIAN_POINT('Ctrl Pts',(163.627488540013,224.80367711901,4.28297134205255));
#79323=CARTESIAN_POINT('Ctrl Pts',(161.802615006038,221.845987488677,4.12421347682076));
#79324=CARTESIAN_POINT('Ctrl Pts',(158.327988289432,221.774849984717,3.96545561158897));
#79325=CARTESIAN_POINT('Ctrl Pts',(156.969987773211,223.786649943641,3.85457663692288));
#79326=CARTESIAN_POINT('Ctrl Pts',(156.921829883209,224.901334991466,3.7966169506674));
#79327=CARTESIAN_POINT('Ctrl Pts',(156.922466247698,224.998327969291,3.79157655282252));
#79328=CARTESIAN_POINT('Origin',(160.,225.,22.2084234471774));
#79329=CARTESIAN_POINT('',(156.93140463606,224.999957001684,5.79157655282252));
#79330=CARTESIAN_POINT('',(156.921584159768,224.999192686964,5.70842344717744));
#79331=CARTESIAN_POINT('',(156.9265,225.,22.2084234471774));
#79332=CARTESIAN_POINT('Ctrl Pts',(156.921584159768,224.999192686964,5.70842344717744));
#79333=CARTESIAN_POINT('Ctrl Pts',(156.925001457824,225.972784245262,5.65779072582253));
#79334=CARTESIAN_POINT('Ctrl Pts',(157.949607258313,227.970126972175,5.55423871605704));
#79335=CARTESIAN_POINT('Ctrl Pts',(161.351233261004,228.372148701364,5.39776741788094));
#79336=CARTESIAN_POINT('Ctrl Pts',(163.565919727063,225.69385494874,5.23900955264914));
#79337=CARTESIAN_POINT('Ctrl Pts',(162.517076599142,222.380545174315,5.08025168741736));
#79338=CARTESIAN_POINT('Ctrl Pts',(159.164605066666,221.464560353348,4.92149382218556));
#79339=CARTESIAN_POINT('Ctrl Pts',(157.144209541887,223.275517676808,4.79755107543892));
#79340=CARTESIAN_POINT('Ctrl Pts',(156.927014459328,224.647298963079,4.72652761710288));
#79341=CARTESIAN_POINT('Ctrl Pts',(156.929435381723,224.997713479262,4.70842344717743));
#79342=CARTESIAN_POINT('Ctrl Pts',(156.93140463606,224.999957001684,5.79157655282252));
#79343=CARTESIAN_POINT('Ctrl Pts',(156.931468976361,225.515539516096,5.76498174492791));
#79344=CARTESIAN_POINT('Ctrl Pts',(157.299116272149,227.057132548067,5.6854676486227));
#79345=CARTESIAN_POINT('Ctrl Pts',(159.738697422576,228.623387468178,5.55303426390689));
#79346=CARTESIAN_POINT('Ctrl Pts',(162.902351059725,227.184851049301,5.3942763986751));
#79347=CARTESIAN_POINT('Ctrl Pts',(163.409773121145,223.746739036021,5.2355185334433));
#79348=CARTESIAN_POINT('Ctrl Pts',(160.796570956179,221.455611407691,5.07676066821152));
#79349=CARTESIAN_POINT('Ctrl Pts',(157.681232421457,222.343634702093,4.92878000800458));
#79350=CARTESIAN_POINT('Ctrl Pts',(156.932948385389,224.189732883212,4.83371863620825));
#79351=CARTESIAN_POINT('Ctrl Pts',(156.925458918946,225.002732334518,4.79157655282252));
#79352=CARTESIAN_POINT('Origin',(160.,225.,22.2084234471774));
#79353=CARTESIAN_POINT('',(156.925301112762,224.997290222949,6.79157655282252));
#79354=CARTESIAN_POINT('',(156.927064836583,225.002798525488,6.70842344717744));
#79355=CARTESIAN_POINT('',(156.9265,225.,22.2084234471774));
#79356=CARTESIAN_POINT('Ctrl Pts',(156.927064836583,225.002798525488,6.70842344717744));
#79357=CARTESIAN_POINT('Ctrl Pts',(156.924720161678,225.264186795083,6.69489241136339));
#79358=CARTESIAN_POINT('Ctrl Pts',(157.074861486538,226.545199591255,6.62844208713874));
#79359=CARTESIAN_POINT('Ctrl Pts',(158.863323855727,228.450389185699,6.50907247450349));
#79360=CARTESIAN_POINT('Ctrl Pts',(162.282209040562,227.826435933279,6.35031460927169));
#79361=CARTESIAN_POINT('Ctrl Pts',(163.612416601221,224.615728625868,6.1915567440399));
#79362=CARTESIAN_POINT('Ctrl Pts',(161.636540630497,221.756706464952,6.03279887880811));
#79363=CARTESIAN_POINT('Ctrl Pts',(158.162902739098,221.865946419773,5.87404101357632));
#79364=CARTESIAN_POINT('Ctrl Pts',(156.942203746577,223.893848412542,5.76591586969943));
#79365=CARTESIAN_POINT('Ctrl Pts',(156.921429835036,224.955225419882,5.71071001423313));
#79366=CARTESIAN_POINT('Ctrl Pts',(156.921584159768,224.999192686964,5.70842344717744));
#79367=CARTESIAN_POINT('Ctrl Pts',(156.925301112762,224.997290222949,6.79157655282253));
#79368=CARTESIAN_POINT('Ctrl Pts',(156.932817764635,225.815396751321,6.74916414205816));
#79369=CARTESIAN_POINT('Ctrl Pts',(157.689098895856,227.666552960644,6.6538324428832));
#79370=CARTESIAN_POINT('Ctrl Pts',(160.814621149687,228.540283627621,6.50558145529764));
#79371=CARTESIAN_POINT('Ctrl Pts',(163.416114882048,226.235870095991,6.34682359006586));
#79372=CARTESIAN_POINT('Ctrl Pts',(162.891180408695,222.800388301109,6.18806572483405));
#79373=CARTESIAN_POINT('Ctrl Pts',(159.720237738997,221.377991046555,6.02930785960227));
#79374=CARTESIAN_POINT('Ctrl Pts',(157.293632555002,222.953434165558,5.89714480226508));
#79375=CARTESIAN_POINT('Ctrl Pts',(156.931340949756,224.489615212083,5.8179010333385));
#79376=CARTESIAN_POINT('Ctrl Pts',(156.93140463606,224.999957001684,5.79157655282252));
#79377=CARTESIAN_POINT('Origin',(160.,225.,22.2084234471774));
#79378=CARTESIAN_POINT('',(156.922579188606,225.001746898842,7.79157655282252));
#79379=CARTESIAN_POINT('',(156.931157428481,224.999096720139,7.70842344717743));
#79380=CARTESIAN_POINT('',(156.9265,225.,22.2084234471774));
#79381=CARTESIAN_POINT('Ctrl Pts',(156.931157428481,224.999096720139,7.70842344717743));
#79382=CARTESIAN_POINT('Ctrl Pts',(156.932655761039,225.567952418948,7.67907480849363));
#79383=CARTESIAN_POINT('Ctrl Pts',(157.357138295168,227.164604851287,7.59680688139924));
#79384=CARTESIAN_POINT('Ctrl Pts',(159.927049484579,228.632065034116,7.46161966589424));
#79385=CARTESIAN_POINT('Ctrl Pts',(163.011803421676,227.031319359169,7.30286180066245));
#79386=CARTESIAN_POINT('Ctrl Pts',(163.34015498569,223.57151028659,7.14410393543066));
#79387=CARTESIAN_POINT('Ctrl Pts',(160.61159683815,221.41905494355,6.98534607019886));
#79388=CARTESIAN_POINT('Ctrl Pts',(157.60356850975,222.448010774312,6.84011924078113));
#79389=CARTESIAN_POINT('Ctrl Pts',(156.933890082535,224.241908721479,6.74781169977398));
#79390=CARTESIAN_POINT('Ctrl Pts',(156.927064836583,225.002798525488,6.70842344717744));
#79391=CARTESIAN_POINT('Ctrl Pts',(156.922579188606,225.001746898842,7.79157655282252));
#79392=CARTESIAN_POINT('Ctrl Pts',(156.921884783106,225.103951698665,7.78626582759901));
#79393=CARTESIAN_POINT('Ctrl Pts',(156.972873960673,226.223885904837,7.7280358139649));
#79394=CARTESIAN_POINT('Ctrl Pts',(158.344443841372,228.233627929609,7.61688651192019));
#79395=CARTESIAN_POINT('Ctrl Pts',(161.818662966152,228.144786287979,7.4581286466884));
#79396=CARTESIAN_POINT('Ctrl Pts',(163.628441815827,225.177836359257,7.29937078145661));
#79397=CARTESIAN_POINT('Ctrl Pts',(162.117470858342,222.048130601536,7.14061291622482));
#79398=CARTESIAN_POINT('Ctrl Pts',(158.66859065457,221.61997560121,6.98185505099302));
#79399=CARTESIAN_POINT('Ctrl Pts',(157.034064229565,223.573194929989,6.86550959652559));
#79400=CARTESIAN_POINT('Ctrl Pts',(156.923439003533,224.794619706459,6.80208343046876));
#79401=CARTESIAN_POINT('Ctrl Pts',(156.925301112762,224.997290222949,6.79157655282253));
#79402=CARTESIAN_POINT('Origin',(160.,225.,22.2084234471774));
#79403=CARTESIAN_POINT('',(156.930575840473,225.001597660456,8.79157655282252));
#79404=CARTESIAN_POINT('',(156.923755330016,224.997680433942,8.70842344717743));
#79405=CARTESIAN_POINT('',(156.9265,225.,22.2084234471774));
#79406=CARTESIAN_POINT('Ctrl Pts',(156.923755330016,224.997680433942,8.70842344717744));
#79407=CARTESIAN_POINT('Ctrl Pts',(156.931061315003,225.867774151639,8.66325720562389));
#79408=CARTESIAN_POINT('Ctrl Pts',(157.77174400633,227.76966729665,8.56517167565974));
#79409=CARTESIAN_POINT('Ctrl Pts',(160.997212243665,228.493248621389,8.414166857285));
#79410=CARTESIAN_POINT('Ctrl Pts',(163.475637228661,226.056959812147,8.2554089920532));
#79411=CARTESIAN_POINT('Ctrl Pts',(162.773159158663,222.653341424392,8.09665112682142));
#79412=CARTESIAN_POINT('Ctrl Pts',(159.532685935708,221.397384872754,7.93789326158962));
#79413=CARTESIAN_POINT('Ctrl Pts',(157.239882095088,223.061204839663,7.80848403504163));
#79414=CARTESIAN_POINT('Ctrl Pts',(156.929954078905,224.542234016346,7.73199409690423));
#79415=CARTESIAN_POINT('Ctrl Pts',(156.931157428481,224.999096720139,7.70842344717743));
#79416=CARTESIAN_POINT('Ctrl Pts',(156.930575840473,225.001597660456,8.79157655282252));
#79417=CARTESIAN_POINT('Ctrl Pts',(156.928646874646,225.410927488159,8.77044822472926));
#79418=CARTESIAN_POINT('Ctrl Pts',(157.195363353794,226.843078205094,8.6964006082254));
#79419=CARTESIAN_POINT('Ctrl Pts',(159.367387257422,228.57729183873,8.56943370331094));
#79420=CARTESIAN_POINT('Ctrl Pts',(162.662226542055,227.471794008467,8.41067583807916));
#79421=CARTESIAN_POINT('Ctrl Pts',(163.520596200089,224.104110398856,8.25191797284736));
#79422=CARTESIAN_POINT('Ctrl Pts',(161.156916354245,221.556344916982,8.09316010761557));
#79423=CARTESIAN_POINT('Ctrl Pts',(157.848914905693,222.140012018685,7.93971296760729));
#79424=CARTESIAN_POINT('Ctrl Pts',(156.928804260839,224.085521060443,7.83918511600961));
#79425=CARTESIAN_POINT('Ctrl Pts',(156.922579188606,225.001746898842,7.79157655282252));
#79426=CARTESIAN_POINT('Origin',(160.,225.,22.2084234471774));
#79427=CARTESIAN_POINT('',(156.928405453258,224.99738485482,9.79157655282252));
#79428=CARTESIAN_POINT('',(156.923921594218,225.002377969191,9.70842344717744));
#79429=CARTESIAN_POINT('',(156.9265,225.,22.2084234471774));
#79430=CARTESIAN_POINT('Ctrl Pts',(156.923921594218,225.002377969191,9.70842344717744));
#79431=CARTESIAN_POINT('Ctrl Pts',(156.922594939509,225.15775743005,9.70035889116474));
#79432=CARTESIAN_POINT('Ctrl Pts',(157.003932869366,226.331337438034,9.63937504674144));
#79433=CARTESIAN_POINT('Ctrl Pts',(158.514451011063,228.315171547782,9.52547191390754));
#79434=CARTESIAN_POINT('Ctrl Pts',(161.979381312161,228.046189063538,9.36671404867575));
#79435=CARTESIAN_POINT('Ctrl Pts',(163.632781914206,224.989334468133,9.20795618344396));
#79436=CARTESIAN_POINT('Ctrl Pts',(161.961460651225,221.942240967073,9.04919831821217));
#79437=CARTESIAN_POINT('Ctrl Pts',(158.495010677376,221.693608412704,8.89044045298037));
#79438=CARTESIAN_POINT('Ctrl Pts',(157.000266331579,223.680828074275,8.77684882930213));
#79439=CARTESIAN_POINT('Ctrl Pts',(156.922501215394,224.848323809807,8.71617649403449));
#79440=CARTESIAN_POINT('Ctrl Pts',(156.923755330016,224.997680433942,8.70842344717744));
#79441=CARTESIAN_POINT('Ctrl Pts',(156.928405453258,224.99738485482,9.79157655282252));
#79442=CARTESIAN_POINT('Ctrl Pts',(156.934187923251,225.71188530638,9.75463062185951));
#79443=CARTESIAN_POINT('Ctrl Pts',(157.538401080906,227.458614330763,9.6647654024859));
#79444=CARTESIAN_POINT('Ctrl Pts',(160.446152220277,228.605296656013,9.52198089470171));
#79445=CARTESIAN_POINT('Ctrl Pts',(163.270876096285,226.580691413359,9.3632230294699));
#79446=CARTESIAN_POINT('Ctrl Pts',(163.102094297597,223.109437451357,9.20446516423812));
#79447=CARTESIAN_POINT('Ctrl Pts',(160.094275919735,221.36842625953,9.04570729900632));
#79448=CARTESIAN_POINT('Ctrl Pts',(157.411955214648,222.740409857239,8.9080777618678));
#79449=CARTESIAN_POINT('Ctrl Pts',(156.933478279124,224.385695244903,8.82336751313986));
#79450=CARTESIAN_POINT('Ctrl Pts',(156.930575840473,225.001597660456,8.79157655282252));
#79451=CARTESIAN_POINT('Origin',(160.,225.,22.2084234471774));
#79452=CARTESIAN_POINT('',(156.921326205399,224.999944058072,10.7915765528225));
#79453=CARTESIAN_POINT('',(156.931207652796,225.000808750494,10.7084234471774));
#79454=CARTESIAN_POINT('',(156.9265,225.,22.2084234471774));
#79455=CARTESIAN_POINT('Ctrl Pts',(156.931207652796,225.000808750494,10.7084234471774));
#79456=CARTESIAN_POINT('Ctrl Pts',(156.930117006851,225.463728255709,10.684541288295));
#79457=CARTESIAN_POINT('Ctrl Pts',(157.245771271414,226.950995919839,10.6077398410019));
#79458=CARTESIAN_POINT('Ctrl Pts',(159.553847739015,228.605296984961,10.4780191052983));
#79459=CARTESIAN_POINT('Ctrl Pts',(162.786890404461,227.33033475348,10.3192612400665));
#79460=CARTESIAN_POINT('Ctrl Pts',(163.469371081335,223.922650247252,10.1605033748347));
#79461=CARTESIAN_POINT('Ctrl Pts',(160.976683481002,221.500956192374,10.0017455096029));
#79462=CARTESIAN_POINT('Ctrl Pts',(157.762164521819,222.241932542296,9.85105220038383));
#79463=CARTESIAN_POINT('Ctrl Pts',(156.931300393731,224.138163730248,9.75327817957534));
#79464=CARTESIAN_POINT('Ctrl Pts',(156.923921594218,225.002377969191,9.70842344717744));
#79465=CARTESIAN_POINT('Ctrl Pts',(156.921326699174,224.999944063411,10.7915765528225));
#79466=CARTESIAN_POINT('Ctrl Pts',(156.921598761237,226.014279935961,10.7388130189898));
#79467=CARTESIAN_POINT('Ctrl Pts',(158.024018250927,228.046452679611,10.6331301967464));
#79468=CARTESIAN_POINT('Ctrl Pts',(161.485548853394,228.315171245305,10.4745280860925));
#79469=CARTESIAN_POINT('Ctrl Pts',(163.590904586142,225.55010911167,10.3157702208607));
#79470=CARTESIAN_POINT('Ctrl Pts',(162.409864582861,222.281587140667,10.1570123556289));
#79471=CARTESIAN_POINT('Ctrl Pts',(159.023316608111,221.500956511627,9.99825449039707));
#79472=CARTESIAN_POINT('Ctrl Pts',(157.110724309286,223.359076798683,9.87644255612829));
#79473=CARTESIAN_POINT('Ctrl Pts',(156.925905436132,224.688474758045,9.80754991027011));
#79474=CARTESIAN_POINT('Ctrl Pts',(156.928405453258,224.99738485482,9.79157655282252));
#79475=CARTESIAN_POINT('Origin',(160.,225.,22.2084234471774));
#79476=CARTESIAN_POINT('',(156.928242437195,225.002650545767,11.7915765528225));
#79477=CARTESIAN_POINT('',(156.926885812714,224.997194120839,11.7084234471774));
#79478=CARTESIAN_POINT('',(156.9265,225.,22.2084234471774));
#79479=CARTESIAN_POINT('Ctrl Pts',(156.926885812714,224.997194120839,11.7084234471774));
#79480=CARTESIAN_POINT('Ctrl Pts',(156.933817424723,225.763987711147,11.6687236854252));
#79481=CARTESIAN_POINT('Ctrl Pts',(157.612129510202,227.56384737007,11.5761046352624));
#79482=CARTESIAN_POINT('Ctrl Pts',(160.632612800297,228.577292165123,11.4305662966891));
#79483=CARTESIAN_POINT('Ctrl Pts',(163.348485175597,226.408852447405,11.2718084314573));
#79484=CARTESIAN_POINT('Ctrl Pts',(162.999824049866,222.951031025224,11.1130505662255));
#79485=CARTESIAN_POINT('Ctrl Pts',(159.905724071664,221.368425928184,10.9542927009937));
#79486=CARTESIAN_POINT('Ctrl Pts',(157.350375618805,222.847534603159,10.8194169946443));
#79487=CARTESIAN_POINT('Ctrl Pts',(156.932533714971,224.43796794116,10.7374605767056));
#79488=CARTESIAN_POINT('Ctrl Pts',(156.931207652796,225.000808750494,10.7084234471774));
#79489=CARTESIAN_POINT('Ctrl Pts',(156.928242437195,225.002650545767,11.7915765528225));
#79490=CARTESIAN_POINT('Ctrl Pts',(156.925748350471,225.305495671118,11.7759147045306));
#79491=CARTESIAN_POINT('Ctrl Pts',(157.10600206368,226.628710135808,11.7073335678281));
#79492=CARTESIAN_POINT('Ctrl Pts',(159.002787847321,228.493248302664,11.585833142715));
#79493=CARTESIAN_POINT('Ctrl Pts',(162.393861129102,227.732516180389,11.4270752774832));
#79494=CARTESIAN_POINT('Ctrl Pts',(163.594072799666,224.470985357276,11.2683174122514));
#79495=CARTESIAN_POINT('Ctrl Pts',(161.504989185309,221.693608714381,11.1095595470196));
#79496=CARTESIAN_POINT('Ctrl Pts',(158.038539527739,221.942241246064,10.9508016817878));
#79497=CARTESIAN_POINT('Ctrl Pts',(156.922685750034,223.976626178208,10.8448073503888));
#79498=CARTESIAN_POINT('Ctrl Pts',(156.921325896064,224.996949808778,10.7917323074004));
#79499=CARTESIAN_POINT('Ctrl Pts',(156.921326699174,224.999944063411,10.7915765528225));
#79500=CARTESIAN_POINT('Origin',(160.,225.,22.2084234471774));
#79501=CARTESIAN_POINT('',(156.930668018482,224.998485301295,12.7915765528225));
#79502=CARTESIAN_POINT('',(156.921655978846,225.000912860592,12.7084234471774));
#79503=CARTESIAN_POINT('',(156.9265,225.,22.2084234471774));
#79504=CARTESIAN_POINT('Ctrl Pts',(156.921655978846,225.000912860592,12.7084234471774));
#79505=CARTESIAN_POINT('Ctrl Pts',(156.921460221192,225.05087309577,12.7058253709661));
#79506=CARTESIAN_POINT('Ctrl Pts',(156.945200448423,226.118265565256,12.6503080063441));
#79507=CARTESIAN_POINT('Ctrl Pts',(158.181336867912,228.14478657491,12.5418713533116));
#79508=CARTESIAN_POINT('Ctrl Pts',(161.655556309681,228.233628224646,12.3831134880798));
#79509=CARTESIAN_POINT('Ctrl Pts',(163.614610681933,225.363053450345,12.224355622848));
#79510=CARTESIAN_POINT('Ctrl Pts',(162.265573500221,222.160212172565,12.0655977576162));
#79511=CARTESIAN_POINT('Ctrl Pts',(158.843083540198,221.556344602782,11.9068398923844));
#79512=CARTESIAN_POINT('Ctrl Pts',(157.070476778671,223.467003665978,11.7877817889048));
#79513=CARTESIAN_POINT('Ctrl Pts',(156.924577672169,224.741861396884,11.7216429738358));
#79514=CARTESIAN_POINT('Ctrl Pts',(156.926885812714,224.997194120839,11.7084234471774));
#79515=CARTESIAN_POINT('Ctrl Pts',(156.930668018482,224.998485301295,12.7915765528225));
#79516=CARTESIAN_POINT('Ctrl Pts',(156.933387942851,225.60839853352,12.7600971016609));
#79517=CARTESIAN_POINT('Ctrl Pts',(157.404784820172,227.247495698794,12.6756983620886));
#79518=CARTESIAN_POINT('Ctrl Pts',(160.072950508764,228.632064702726,12.5383803341058));
#79519=CARTESIAN_POINT('Ctrl Pts',(163.090939861654,226.908744758514,12.379622468874));
#79520=CARTESIAN_POINT('Ctrl Pts',(163.280101174706,223.438541686369,12.2208646036422));
#79521=CARTESIAN_POINT('Ctrl Pts',(160.467314021654,221.397385201457,12.0621067384104));
#79522=CARTESIAN_POINT('Ctrl Pts',(157.546521604723,222.529438491092,11.9190107214705));
#79523=CARTESIAN_POINT('Ctrl Pts',(156.934175535578,224.282222540545,11.8288339929412));
#79524=CARTESIAN_POINT('Ctrl Pts',(156.928242437195,225.002650545767,11.7915765528225));
#79525=CARTESIAN_POINT('Origin',(160.,225.,22.2084234471774));
#79526=CARTESIAN_POINT('',(156.922714207567,224.998169460982,13.7915765528225));
#79527=CARTESIAN_POINT('',(156.929571798648,225.002226664175,13.7084234471774));
#79528=CARTESIAN_POINT('',(156.9265,225.,22.2084234471774));
#79529=CARTESIAN_POINT('Ctrl Pts',(156.929571798648,225.002226664174,13.7084234471774));
#79530=CARTESIAN_POINT('Ctrl Pts',(156.927180610712,225.358710424651,13.6900077680964));
#79531=CARTESIAN_POINT('Ctrl Pts',(157.1492799851,226.736699514861,13.6186728006047));
#79532=CARTESIAN_POINT('Ctrl Pts',(159.185378775986,228.540283950637,13.4944185447024));
#79533=CARTESIAN_POINT('Ctrl Pts',(162.532414057892,227.604629960118,13.3356606794706));
#79534=CARTESIAN_POINT('Ctrl Pts',(163.561784093599,224.285218732523,13.1769028142388));
#79535=CARTESIAN_POINT('Ctrl Pts',(161.331409466909,221.619975292816,13.018144949007));
#79536=CARTESIAN_POINT('Ctrl Pts',(157.938969959541,222.041123564882,12.8619851599865));
#79537=CARTESIAN_POINT('Ctrl Pts',(156.92544753907,224.03325087096,12.7587446593767));
#79538=CARTESIAN_POINT('Ctrl Pts',(156.921655978846,225.000912860592,12.7084234471774));
#79539=CARTESIAN_POINT('Ctrl Pts',(156.922714207567,224.998169460982,13.7915765528225));
#79540=CARTESIAN_POINT('Ctrl Pts',(156.929131114757,225.908505372441,13.7442794987911));
#79541=CARTESIAN_POINT('Ctrl Pts',(157.838867197776,227.848532288381,13.6440631563491));
#79542=CARTESIAN_POINT('Ctrl Pts',(161.136676040562,228.450388870885,13.4909275254965));
#79543=CARTESIAN_POINT('Ctrl Pts',(163.515275045834,225.916546307426,13.3321696602647));
#79544=CARTESIAN_POINT('Ctrl Pts',(162.676694467393,222.543880599453,13.1734117950329));
#79545=CARTESIAN_POINT('Ctrl Pts',(159.388403217653,221.419055270276,13.0146539298011));
#79546=CARTESIAN_POINT('Ctrl Pts',(157.200879963145,223.14470884355,12.887375515731));
#79547=CARTESIAN_POINT('Ctrl Pts',(156.92881554858,224.583089226957,12.8130163900715));
#79548=CARTESIAN_POINT('Ctrl Pts',(156.930668018482,224.998485301295,12.7915765528225));
#79549=CARTESIAN_POINT('Origin',(160.,225.,22.2084234471774));
#79550=CARTESIAN_POINT('',(156.925120010832,225.002680229931,14.7915765528225));
#79551=CARTESIAN_POINT('',(156.929686910559,224.99782753598,14.7084234471775));
#79552=CARTESIAN_POINT('',(156.9265,225.,22.2084234471774));
#79553=CARTESIAN_POINT('Ctrl Pts',(156.929686910559,224.99782753598,14.7084234471775));
#79554=CARTESIAN_POINT('Ctrl Pts',(156.934013289436,225.660564946541,14.6741901652266));
#79555=CARTESIAN_POINT('Ctrl Pts',(157.470014842063,227.354168864685,14.5870375948652));
#79556=CARTESIAN_POINT('Ctrl Pts',(160.261302601264,228.623387798777,14.4469657360931));
#79557=CARTESIAN_POINT('Ctrl Pts',(163.185812396663,226.745799977952,14.2882078708613));
#79558=CARTESIAN_POINT('Ctrl Pts',(163.194666811915,223.270456085958,14.1294500056295));
#79559=CARTESIAN_POINT('Ctrl Pts',(160.27976228653,221.377990716082,13.9706921403978));
#79560=CARTESIAN_POINT('Ctrl Pts',(157.476644051236,222.635392093966,13.830349954247));
#79561=CARTESIAN_POINT('Ctrl Pts',(156.934051927457,224.334318825988,13.7429270565069));
#79562=CARTESIAN_POINT('Ctrl Pts',(156.929571798648,225.002226664174,13.7084234471774));
#79563=CARTESIAN_POINT('Ctrl Pts',(156.925120010832,225.002680229931,14.7915765528225));
#79564=CARTESIAN_POINT('Ctrl Pts',(156.923321116172,225.199312113646,14.781381184332));
#79565=CARTESIAN_POINT('Ctrl Pts',(157.030083060612,226.414620418541,14.7182665274308));
#79566=CARTESIAN_POINT('Ctrl Pts',(158.648766862283,228.372148393688,14.6022325821191));
#79567=CARTESIAN_POINT('Ctrl Pts',(162.100101640777,227.964251824647,14.4434747168873));
#79568=CARTESIAN_POINT('Ctrl Pts',(163.629423480216,224.843472102255,14.2847168516555));
#79569=CARTESIAN_POINT('Ctrl Pts',(161.837097093285,221.865946705725,14.1259589864237));
#79570=CARTESIAN_POINT('Ctrl Pts',(158.363459518822,221.756706760871,13.9672011211919));
#79571=CARTESIAN_POINT('Ctrl Pts',(156.976235533965,223.763970462451,13.8557403099915));
#79572=CARTESIAN_POINT('Ctrl Pts',(156.921951425256,224.889957185126,13.7971987872017));
#79573=CARTESIAN_POINT('Ctrl Pts',(156.922714207567,224.998169460982,13.7915765528225));
#79574=CARTESIAN_POINT('Origin',(160.,225.,22.2084234471774));
#79575=CARTESIAN_POINT('',(156.931399227217,225.00014204246,15.7915765528225));
#79576=CARTESIAN_POINT('',(156.921724642972,224.998996856206,15.7084234471774));
#79577=CARTESIAN_POINT('',(156.9265,225.,22.2084234471774));
#79578=CARTESIAN_POINT('Ctrl Pts',(156.921724642972,224.998996856206,15.7084234471774));
#79579=CARTESIAN_POINT('Ctrl Pts',(156.925824278053,225.961517777779,15.6583725623568));
#79580=CARTESIAN_POINT('Ctrl Pts',(157.929788518612,227.949094946038,15.5554023891257));
#79581=CARTESIAN_POINT('Ctrl Pts',(161.314169168278,228.386765062254,15.3995129274839));
#79582=CARTESIAN_POINT('Ctrl Pts',(163.558095664808,225.732921162083,15.2407550622521));
#79583=CARTESIAN_POINT('Ctrl Pts',(162.545653148823,222.408307843197,15.0819971970203));
#79584=CARTESIAN_POINT('Ctrl Pts',(159.203428971142,221.4556110843,14.9232393317885));
#79585=CARTESIAN_POINT('Ctrl Pts',(157.15371672642,223.252698357902,14.7987147485075));
#79586=CARTESIAN_POINT('Ctrl Pts',(156.927325385779,224.636076782644,14.7271094536372));
#79587=CARTESIAN_POINT('Ctrl Pts',(156.929686910559,224.99782753598,14.7084234471775));
#79588=CARTESIAN_POINT('Ctrl Pts',(156.931399227217,225.00014204246,15.7915765528225));
#79589=CARTESIAN_POINT('Ctrl Pts',(156.931191312365,225.504442516036,15.7655635814622));
#79590=CARTESIAN_POINT('Ctrl Pts',(157.287359856215,227.03438622062,15.6866313216913));
#79591=CARTESIAN_POINT('Ctrl Pts',(159.698974938352,228.620303812367,15.5547797735098));
#79592=CARTESIAN_POINT('Ctrl Pts',(162.878214941473,227.216550142046,15.396021908278));
#79593=CARTESIAN_POINT('Ctrl Pts',(163.423312743327,223.784209868902,15.2372640430462));
#79594=CARTESIAN_POINT('Ctrl Pts',(160.835394857113,221.464560675923,15.0785061778144));
#79595=CARTESIAN_POINT('Ctrl Pts',(157.69821803158,222.321721228977,14.9299436810732));
#79596=CARTESIAN_POINT('Ctrl Pts',(156.932658319183,224.178689918907,14.8343004727426));
#79597=CARTESIAN_POINT('Ctrl Pts',(156.925120010832,225.002680229931,14.7915765528225));
#79598=CARTESIAN_POINT('Origin',(160.,225.,22.2084234471774));
#79599=CARTESIAN_POINT('',(156.925641295233,224.997245236081,16.7915765528225));
#79600=CARTESIAN_POINT('',(156.926729498164,225.002809226607,16.7084234471774));
#79601=CARTESIAN_POINT('',(156.9265,225.,22.2084234471774));
#79602=CARTESIAN_POINT('Ctrl Pts',(156.926729498164,225.002809226607,16.7084234471774));
#79603=CARTESIAN_POINT('Ctrl Pts',(156.924455817463,225.252888178359,16.6954742478977));
#79604=CARTESIAN_POINT('Ctrl Pts',(157.066706017672,226.522407661068,16.6296057602073));
#79605=CARTESIAN_POINT('Ctrl Pts',(158.825551313761,228.437715589115,16.5108179841064));
#79606=CARTESIAN_POINT('Ctrl Pts',(162.251073866661,227.851295256028,16.3520601188746));
#79607=CARTESIAN_POINT('Ctrl Pts',(163.616413705393,224.655369616393,16.1933022536428));
#79608=CARTESIAN_POINT('Ctrl Pts',(161.672011863123,221.774849690454,16.034544388411));
#79609=CARTESIAN_POINT('Ctrl Pts',(158.197384829492,221.845987200903,15.8757865231793));
#79610=CARTESIAN_POINT('Ctrl Pts',(156.947830929778,223.87121938435,15.767079542768));
#79611=CARTESIAN_POINT('Ctrl Pts',(156.92148969392,224.943835024866,15.7112918507674));
#79612=CARTESIAN_POINT('Ctrl Pts',(156.921724642972,224.998996856206,15.7084234471774));
#79613=CARTESIAN_POINT('Ctrl Pts',(156.925641295233,224.997245236081,16.7915765528225));
#79614=CARTESIAN_POINT('Ctrl Pts',(156.933090102387,225.804358136565,16.7497459785925));
#79615=CARTESIAN_POINT('Ctrl Pts',(157.672221721132,227.644612044043,16.6549961159518));
#79616=CARTESIAN_POINT('Ctrl Pts',(160.775745369292,228.549004776956,16.5073269649006));
#79617=CARTESIAN_POINT('Ctrl Pts',(163.402355473271,226.273260780993,16.3485690996688));
#79618=CARTESIAN_POINT('Ctrl Pts',(162.915129980759,222.832228569406,16.189811234437));
#79619=CARTESIAN_POINT('Ctrl Pts',(159.759977645044,221.375140685337,16.0310533692052));
#79620=CARTESIAN_POINT('Ctrl Pts',(157.305481948964,222.930694311157,15.8983084753337));
#79621=CARTESIAN_POINT('Ctrl Pts',(156.931614282347,224.478522722518,15.8184828698728));
#79622=CARTESIAN_POINT('Ctrl Pts',(156.931399227217,225.00014204246,15.7915765528225));
#79623=CARTESIAN_POINT('Origin',(160.,225.,22.2084234471774));
#79624=CARTESIAN_POINT('',(156.922341197581,225.001583255068,17.7915765528225));
#79625=CARTESIAN_POINT('',(156.931246696043,224.999274061703,17.7084234471774));
#79626=CARTESIAN_POINT('',(156.9265,225.,22.2084234471774));
#79627=CARTESIAN_POINT('Ctrl Pts',(156.931246696043,224.999274061703,17.7084234471774));
#79628=CARTESIAN_POINT('Ctrl Pts',(156.932425020426,225.556892698229,17.679656645028));
#79629=CARTESIAN_POINT('Ctrl Pts',(157.344548498198,227.141926833519,17.5979705544679));
#79630=CARTESIAN_POINT('Ctrl Pts',(159.887220508192,228.631046523769,17.4633651754972));
#79631=CARTESIAN_POINT('Ctrl Pts',(162.98934452274,227.064228072664,17.3046073102654));
#79632=CARTESIAN_POINT('Ctrl Pts',(163.355620553903,223.60822814226,17.1458494450336));
#79633=CARTESIAN_POINT('Ctrl Pts',(160.650832783067,221.425977775001,16.9870915798018));
#79634=CARTESIAN_POINT('Ctrl Pts',(157.61960481157,222.425872241985,16.8412829138498));
#79635=CARTESIAN_POINT('Ctrl Pts',(156.933747632514,224.230894471467,16.7483935363083));
#79636=CARTESIAN_POINT('Ctrl Pts',(156.926729498164,225.002809226607,16.7084234471774));
#79637=CARTESIAN_POINT('Ctrl Pts',(156.922341197581,225.001583255068,17.7915765528225));
#79638=CARTESIAN_POINT('Ctrl Pts',(156.921769984656,225.092572081796,17.7868476641333));
#79639=CARTESIAN_POINT('Ctrl Pts',(156.966697348799,226.201212063418,17.7291994870335));
#79640=CARTESIAN_POINT('Ctrl Pts',(158.309079864678,228.215276638311,17.6186320215231));
#79641=CARTESIAN_POINT('Ctrl Pts',(161.78406422512,228.164542738612,17.4598741562913));
#79642=CARTESIAN_POINT('Ctrl Pts',(163.62627326692,225.217619271453,17.3011162910595));
#79643=CARTESIAN_POINT('Ctrl Pts',(162.14971706585,222.071530741175,17.1423584258277));
#79644=CARTESIAN_POINT('Ctrl Pts',(158.705739934788,221.605577120181,16.9836005605959));
#79645=CARTESIAN_POINT('Ctrl Pts',(157.041609772818,223.55043060198,16.8666732695942));
#79646=CARTESIAN_POINT('Ctrl Pts',(156.923666718143,224.783290624422,16.8026652670031));
#79647=CARTESIAN_POINT('Ctrl Pts',(156.925641295233,224.997245236081,16.7915765528225));
#79648=CARTESIAN_POINT('Origin',(160.,225.,22.2084234471774));
#79649=CARTESIAN_POINT('',(156.930395245889,225.001742688239,18.7915765528225));
#79650=CARTESIAN_POINT('',(156.924068523622,224.997572468126,18.7084234471774));
#79651=CARTESIAN_POINT('',(156.9265,225.,22.2084234471774));
#79652=CARTESIAN_POINT('Ctrl Pts',(156.924068523622,224.997572468126,18.7084234471774));
#79653=CARTESIAN_POINT('Ctrl Pts',(156.931499697293,225.856684407074,18.6638390421582));
#79654=CARTESIAN_POINT('Ctrl Pts',(157.753898863975,227.747989763203,18.5663353487284));
#79655=CARTESIAN_POINT('Ctrl Pts',(160.958841607661,228.503973810221,18.4159123668879));
#79656=CARTESIAN_POINT('Ctrl Pts',(163.46383623651,226.095014669232,18.2571545016561));
#79657=CARTESIAN_POINT('Ctrl Pts',(162.798728578809,222.6838958807,18.0983966364243));
#79658=CARTESIAN_POINT('Ctrl Pts',(159.57222439446,221.39247658273,17.9396387711925));
#79659=CARTESIAN_POINT('Ctrl Pts',(157.250921044534,223.038417999758,17.8096477081103));
#79660=CARTESIAN_POINT('Ctrl Pts',(156.93025737984,224.531099796532,17.7325759334386));
#79661=CARTESIAN_POINT('Ctrl Pts',(156.931246696043,224.999274061703,17.7084234471774));
#79662=CARTESIAN_POINT('Ctrl Pts',(156.930395245889,225.001742688239,18.7915765528225));
#79663=CARTESIAN_POINT('Ctrl Pts',(156.928332768056,225.399743321893,18.7710300612636));
#79664=CARTESIAN_POINT('Ctrl Pts',(157.185171945213,226.820276067233,18.697564281294));
#79665=CARTESIAN_POINT('Ctrl Pts',(159.328201281756,228.570130672657,18.5711792129139));
#79666=CARTESIAN_POINT('Ctrl Pts',(162.634953757174,227.500846255061,18.4124213476821));
#79667=CARTESIAN_POINT('Ctrl Pts',(163.530211822273,224.142773276525,18.2536634824503));
#79668=CARTESIAN_POINT('Ctrl Pts',(161.194612857913,221.569240989169,18.0949056172185));
#79669=CARTESIAN_POINT('Ctrl Pts',(157.867843883242,222.118667809481,17.9408766406759));
#79670=CARTESIAN_POINT('Ctrl Pts',(156.928162222561,224.074348926167,17.8397669525439));
#79671=CARTESIAN_POINT('Ctrl Pts',(156.922341197581,225.001583255068,17.7915765528225));
#79672=CARTESIAN_POINT('Origin',(160.,225.,22.2084234471774));
#79673=CARTESIAN_POINT('',(156.929637674279,224.99697422706,19.7915765528225));
#79674=CARTESIAN_POINT('',(156.923621908153,225.002226325067,19.7084234471775));
#79675=CARTESIAN_POINT('',(156.9265,225.,22.2084234471774));
#79676=CARTESIAN_POINT('',(159.206200717467,222.030777046254,20.));
#79677=CARTESIAN_POINT('Ctrl Pts',(159.206200717467,222.030777046254,20.));
#79678=CARTESIAN_POINT('Ctrl Pts',(158.218929051303,222.29471665351,19.9470807115894));
#79679=CARTESIAN_POINT('Ctrl Pts',(157.120586599505,223.3366576531,19.8776062291969));
#79680=CARTESIAN_POINT('Ctrl Pts',(156.927233150508,224.676771814036,19.8081317468044));
#79681=CARTESIAN_POINT('Ctrl Pts',(156.929637674279,224.99697422706,19.7915765528225));
#79682=CARTESIAN_POINT('',(160.795594451476,222.025442790985,20.));
#79683=CARTESIAN_POINT('Origin',(160.,225.,20.));
#79684=CARTESIAN_POINT('Ctrl Pts',(160.795596253159,222.025437437374,20.));
#79685=CARTESIAN_POINT('Ctrl Pts',(159.833965310981,221.769854476539,19.948244384658));
#79686=CARTESIAN_POINT('Ctrl Pts',(157.769883232907,222.243618109764,19.8510522003838));
#79687=CARTESIAN_POINT('Ctrl Pts',(156.930816787522,224.127195112091,19.7538600161097));
#79688=CARTESIAN_POINT('Ctrl Pts',(156.923621908153,225.002226325067,19.7084234471775));
#79689=CARTESIAN_POINT('Origin',(-160.,225.,22.2084234471774));
#79690=CARTESIAN_POINT('',(-163.078662397867,225.00016520217,0.791576552822534));
#79691=CARTESIAN_POINT('',(-163.068635962885,225.000702088854,0.708423447177441));
#79692=CARTESIAN_POINT('',(-163.0735,225.,22.2084234471774));
#79693=CARTESIAN_POINT('',(-159.206200717467,222.030777046254,0.));
#79694=CARTESIAN_POINT('Ctrl Pts',(-163.068635962885,225.000702088854,0.708423447177441));
#79695=CARTESIAN_POINT('Ctrl Pts',(-163.069474402958,225.474958141244,0.683959451760685));
#79696=CARTESIAN_POINT('Ctrl Pts',(-162.742950137614,226.973918053232,0.60657616793333));
#79697=CARTESIAN_POINT('Ctrl Pts',(-160.407275482247,228.609330107362,0.476273595695376));
#79698=CARTESIAN_POINT('Ctrl Pts',(-157.186291303474,227.300991486183,0.317515730463588));
#79699=CARTESIAN_POINT('Ctrl Pts',(-156.545696053065,223.882027393836,0.158757865231792));
#79700=CARTESIAN_POINT('Ctrl Pts',(-158.218929051303,222.29471665351,0.0529192884105984));
#79701=CARTESIAN_POINT('Ctrl Pts',(-159.206200717467,222.030777046254,0.));
#79702=CARTESIAN_POINT('',(-160.793799282533,222.030777046254,0.));
#79703=CARTESIAN_POINT('Origin',(-160.,225.,0.));
#79704=CARTESIAN_POINT('Ctrl Pts',(-163.078662397867,225.00016520217,0.791576552822534));
#79705=CARTESIAN_POINT('Ctrl Pts',(-163.078668346653,225.008356238375,0.791150470866062));
#79706=CARTESIAN_POINT('Ctrl Pts',(-163.074932205839,226.033866360525,0.737805100498993));
#79707=CARTESIAN_POINT('Ctrl Pts',(-161.945876935419,228.067610699799,0.631540441721325));
#79708=CARTESIAN_POINT('Ctrl Pts',(-158.478135238796,228.298893703494,0.472782576489533));
#79709=CARTESIAN_POINT('Ctrl Pts',(-156.403376103572,225.51024998876,0.314024711257742));
#79710=CARTESIAN_POINT('Ctrl Pts',(-157.610972173068,222.280093121964,0.156430519094562));
#79711=CARTESIAN_POINT('Ctrl Pts',(-159.833965155725,221.769854515183,0.0517556153419857));
#79712=CARTESIAN_POINT('Ctrl Pts',(-160.795596246196,222.025437627191,5.28345271179342E-15));
#79713=CARTESIAN_POINT('Origin',(-160.,225.,22.2084234471774));
#79714=CARTESIAN_POINT('',(-163.071455427707,225.00258189293,1.79157655282252));
#79715=CARTESIAN_POINT('',(-163.073451224303,224.99719052414,1.70842344717743));
#79716=CARTESIAN_POINT('',(-163.0735,225.,22.2084234471774));
#79717=CARTESIAN_POINT('Ctrl Pts',(-163.073451224303,224.99719052414,1.70842344717743));
#79718=CARTESIAN_POINT('Ctrl Pts',(-163.066339609044,225.775004891986,1.66814184889093));
#79719=CARTESIAN_POINT('Ctrl Pts',(-162.371724554443,227.585965139188,1.57494096219383));
#79720=CARTESIAN_POINT('Ctrl Pts',(-159.328201268715,228.570130738719,1.42882078708613));
#79721=CARTESIAN_POINT('Ctrl Pts',(-156.636247443033,226.37206105408,1.27006292185434));
#79722=CARTESIAN_POINT('Ctrl Pts',(-157.022865107512,222.918220169874,1.11130505662255));
#79723=CARTESIAN_POINT('Ctrl Pts',(-160.134021050498,221.369750629735,0.952547191390755));
#79724=CARTESIAN_POINT('Ctrl Pts',(-162.66224199813,222.870106397301,0.81825332157572));
#79725=CARTESIAN_POINT('Ctrl Pts',(-163.067660731426,224.449071225008,0.736878740171281));
#79726=CARTESIAN_POINT('Ctrl Pts',(-163.068635962885,225.000702088854,0.708423447177441));
#79727=CARTESIAN_POINT('Ctrl Pts',(-163.071455427707,225.00258189293,1.79157655282252));
#79728=CARTESIAN_POINT('Ctrl Pts',(-163.07395708261,225.316755887693,1.77533286799631));
#79729=CARTESIAN_POINT('Ctrl Pts',(-162.885142267915,226.65152261772,1.70616989475949));
#79730=CARTESIAN_POINT('Ctrl Pts',(-160.958841546672,228.50397358649,1.58408763311208));
#79731=CARTESIAN_POINT('Ctrl Pts',(-157.576314291936,227.706100789163,1.42532976788028));
#79732=CARTESIAN_POINT('Ctrl Pts',(-156.411946257884,224.431594893095,1.2665719026485));
#79733=CARTESIAN_POINT('Ctrl Pts',(-158.531360393914,221.677313586384,1.1078140374167));
#79734=CARTESIAN_POINT('Ctrl Pts',(-161.985587155348,221.963143531564,0.949482254141382));
#79735=CARTESIAN_POINT('Ctrl Pts',(-163.077929508605,223.991031283085,0.84406975927666));
#79736=CARTESIAN_POINT('Ctrl Pts',(-163.078662397867,225.00016520217,0.791576552822534));
#79737=CARTESIAN_POINT('Origin',(-160.,225.,22.2084234471774));
#79738=CARTESIAN_POINT('',(-163.069508305251,224.998331926558,2.79157655282253));
#79739=CARTESIAN_POINT('',(-163.07818897851,225.001105518255,2.70842344717743));
#79740=CARTESIAN_POINT('',(-163.0735,225.,22.2084234471774));
#79741=CARTESIAN_POINT('Ctrl Pts',(-163.07818897851,225.001105518255,2.70842344717743));
#79742=CARTESIAN_POINT('Ctrl Pts',(-163.078472562891,225.062262487795,2.70524353443178));
#79743=CARTESIAN_POINT('Ctrl Pts',(-163.049103003345,226.140900372622,2.64914433327553));
#79744=CARTESIAN_POINT('Ctrl Pts',(-161.784064257062,228.164542795226,2.54012584370868));
#79745=CARTESIAN_POINT('Ctrl Pts',(-158.309079834391,228.215276695892,2.38136797847689));
#79746=CARTESIAN_POINT('Ctrl Pts',(-156.381625086582,225.323389859127,2.22261011324509));
#79747=CARTESIAN_POINT('Ctrl Pts',(-157.765707735213,222.135535871982,2.0638522480133));
#79748=CARTESIAN_POINT('Ctrl Pts',(-161.194612879462,221.569240927476,1.90509438278151));
#79749=CARTESIAN_POINT('Ctrl Pts',(-162.937600862259,223.489791467657,1.78661811583622));
#79750=CARTESIAN_POINT('Ctrl Pts',(-163.075682376832,224.753164036289,1.72106113730153));
#79751=CARTESIAN_POINT('Ctrl Pts',(-163.073451224303,224.99719052414,1.70842344717743));
#79752=CARTESIAN_POINT('Ctrl Pts',(-163.069508305251,224.998331926558,2.79157655282253));
#79753=CARTESIAN_POINT('Ctrl Pts',(-163.066447188156,225.619428959942,2.75951526512656));
#79754=CARTESIAN_POINT('Ctrl Pts',(-162.581779638644,227.270080409104,2.67453468902));
#79755=CARTESIAN_POINT('Ctrl Pts',(-159.887220515355,228.631046293149,2.53663482450283));
#79756=CARTESIAN_POINT('Ctrl Pts',(-156.88831246471,226.874731278963,2.37787695927104));
#79757=CARTESIAN_POINT('Ctrl Pts',(-156.73722075101,223.402662149674,2.21911909403925));
#79758=CARTESIAN_POINT('Ctrl Pts',(-159.572224421631,221.392476811998,2.06036122880746));
#79759=CARTESIAN_POINT('Ctrl Pts',(-162.468601048588,222.551761429388,1.91784704840188));
#79760=CARTESIAN_POINT('Ctrl Pts',(-163.065807097017,224.293228010995,1.8282521564069));
#79761=CARTESIAN_POINT('Ctrl Pts',(-163.071455427707,225.00258189293,1.79157655282252));
#79762=CARTESIAN_POINT('Origin',(-160.,225.,22.2084234471774));
#79763=CARTESIAN_POINT('',(-163.07753383765,224.998327969244,3.79157655282253));
#79764=CARTESIAN_POINT('',(-163.07018410239,225.002107482812,3.70842344717744));
#79765=CARTESIAN_POINT('',(-163.0735,225.,22.2084234471774));
#79766=CARTESIAN_POINT('Ctrl Pts',(-163.07018410239,225.002107482812,3.70842344717744));
#79767=CARTESIAN_POINT('Ctrl Pts',(-163.072506971742,225.36992761417,3.68942593156203));
#79768=CARTESIAN_POINT('Ctrl Pts',(-162.841128078544,226.759518741551,3.61750912753603));
#79769=CARTESIAN_POINT('Ctrl Pts',(-160.775745383176,228.54900484047,3.49267303509943));
#79770=CARTESIAN_POINT('Ctrl Pts',(-157.439173090395,227.576699784501,3.33391516986764));
#79771=CARTESIAN_POINT('Ctrl Pts',(-156.446269479642,224.246199191696,3.17515730463585));
#79772=CARTESIAN_POINT('Ctrl Pts',(-158.705739911624,221.605577059435,3.01639943940406));
#79773=CARTESIAN_POINT('Ctrl Pts',(-162.080734399406,222.062197658976,2.86082148691792));
#79774=CARTESIAN_POINT('Ctrl Pts',(-163.073753224711,224.044503961607,2.75816282284238));
#79775=CARTESIAN_POINT('Ctrl Pts',(-163.07818897851,225.001105518255,2.70842344717743));
#79776=CARTESIAN_POINT('Ctrl Pts',(-163.077533837651,224.998327969245,3.79157655282253));
#79777=CARTESIAN_POINT('Ctrl Pts',(-163.071488992078,225.919667205275,3.74369766225681));
#79778=CARTESIAN_POINT('Ctrl Pts',(-162.142316936304,227.869913312169,3.6428994832805));
#79779=CARTESIAN_POINT('Ctrl Pts',(-158.825551388348,228.437715370794,3.48918201589359));
#79780=CARTESIAN_POINT('Ctrl Pts',(-156.474884376031,225.877938695212,3.3304241506618));
#79781=CARTESIAN_POINT('Ctrl Pts',(-157.350403044487,222.514672558763,3.17166628543001));
#79782=CARTESIAN_POINT('Ctrl Pts',(-160.650832741734,221.425978001981,3.01290842019821));
#79783=CARTESIAN_POINT('Ctrl Pts',(-162.809386154267,223.167520916372,2.88621184266239));
#79784=CARTESIAN_POINT('Ctrl Pts',(-163.071499765581,224.594266984157,2.81243455353716));
#79785=CARTESIAN_POINT('Ctrl Pts',(-163.069508305251,224.998331926558,2.79157655282253));
#79786=CARTESIAN_POINT('Origin',(-160.,225.,22.2084234471774));
#79787=CARTESIAN_POINT('',(-163.074541166319,225.002732334593,4.79157655282253));
#79788=CARTESIAN_POINT('',(-163.07056439307,224.997713479429,4.70842344717743));
#79789=CARTESIAN_POINT('',(-163.0735,225.,22.2084234471774));
#79790=CARTESIAN_POINT('Ctrl Pts',(-163.07056439307,224.997713479429,4.70842344717743));
#79791=CARTESIAN_POINT('Ctrl Pts',(-163.065908852707,225.671576023543,4.67360832869228));
#79792=CARTESIAN_POINT('Ctrl Pts',(-162.51566601189,227.376629151021,4.58587392179654));
#79793=CARTESIAN_POINT('Ctrl Pts',(-159.698974932965,228.620303877157,4.44522022649019));
#79794=CARTESIAN_POINT('Ctrl Pts',(-156.79523300249,226.710755606563,4.28646236125839));
#79795=CARTESIAN_POINT('Ctrl Pts',(-156.82449370205,223.235523872175,4.1277044960266));
#79796=CARTESIAN_POINT('Ctrl Pts',(-159.759977640748,221.375140620465,3.96894663079481));
#79797=CARTESIAN_POINT('Ctrl Pts',(-162.537573577682,222.657868348294,3.82918628117842));
#79798=CARTESIAN_POINT('Ctrl Pts',(-163.066036410239,224.345331556,3.74234521997263));
#79799=CARTESIAN_POINT('Ctrl Pts',(-163.07018410239,225.002107482812,3.70842344717744));
#79800=CARTESIAN_POINT('Ctrl Pts',(-163.074541166319,225.002732334593,4.79157655282253));
#79801=CARTESIAN_POINT('Ctrl Pts',(-163.076456484954,225.210644742118,4.78079934779766));
#79802=CARTESIAN_POINT('Ctrl Pts',(-162.962447901099,226.437380725571,4.71710285436219));
#79803=CARTESIAN_POINT('Ctrl Pts',(-161.314169084819,228.386764847169,4.60048707251614));
#79804=CARTESIAN_POINT('Ctrl Pts',(-157.867515236049,227.941041523849,4.44172920728434));
#79805=CARTESIAN_POINT('Ctrl Pts',(-156.372511359387,224.803677113565,4.28297134205255));
#79806=CARTESIAN_POINT('Ctrl Pts',(-158.197384943971,221.845987401207,4.12421347682076));
#79807=CARTESIAN_POINT('Ctrl Pts',(-161.672011756938,221.774849895275,3.96545561158897));
#79808=CARTESIAN_POINT('Ctrl Pts',(-163.03001231082,223.786649909991,3.85457663692289));
#79809=CARTESIAN_POINT('Ctrl Pts',(-163.078170202158,224.90133498873,3.79661695066741));
#79810=CARTESIAN_POINT('Ctrl Pts',(-163.077533837651,224.998327969245,3.79157655282253));
#79811=CARTESIAN_POINT('Origin',(-160.,225.,22.2084234471774));
#79812=CARTESIAN_POINT('',(-163.068595449041,224.999957001683,5.79157655282253));
#79813=CARTESIAN_POINT('',(-163.078415614449,224.999192687023,5.70842344717743));
#79814=CARTESIAN_POINT('',(-163.0735,225.,22.2084234471774));
#79815=CARTESIAN_POINT('Ctrl Pts',(-163.078415614449,224.999192687023,5.70842344717743));
#79816=CARTESIAN_POINT('Ctrl Pts',(-163.074998316644,225.972784173914,5.65779072582253));
#79817=CARTESIAN_POINT('Ctrl Pts',(-162.050392591303,227.970126754334,5.55423871605704));
#79818=CARTESIAN_POINT('Ctrl Pts',(-158.648766838101,228.372148454037,5.39776741788094));
#79819=CARTESIAN_POINT('Ctrl Pts',(-156.434080534475,225.69385489785,5.23900955264915));
#79820=CARTESIAN_POINT('Ctrl Pts',(-157.48292358547,222.380545366436,5.08025168741736));
#79821=CARTESIAN_POINT('Ctrl Pts',(-160.835394872063,221.464560612651,4.92149382218557));
#79822=CARTESIAN_POINT('Ctrl Pts',(-162.855790248658,223.275517803288,4.79755107543892));
#79823=CARTESIAN_POINT('Ctrl Pts',(-163.072985315288,224.647298988948,4.72652761710288));
#79824=CARTESIAN_POINT('Ctrl Pts',(-163.07056439307,224.997713479429,4.70842344717743));
#79825=CARTESIAN_POINT('Ctrl Pts',(-163.068595449041,224.999957001683,5.79157655282253));
#79826=CARTESIAN_POINT('Ctrl Pts',(-163.068531108738,225.515539530394,5.76498174492791));
#79827=CARTESIAN_POINT('Ctrl Pts',(-162.700883802754,227.057132605117,5.6854676486227));
#79828=CARTESIAN_POINT('Ctrl Pts',(-160.26130258467,228.623387568664,5.5530342639069));
#79829=CARTESIAN_POINT('Ctrl Pts',(-157.097648859785,227.184851109893,5.39427639867509));
#79830=CARTESIAN_POINT('Ctrl Pts',(-156.590226784293,223.746739001265,5.23551853344331));
#79831=CARTESIAN_POINT('Ctrl Pts',(-159.203429021729,221.455611309395,5.07676066821151));
#79832=CARTESIAN_POINT('Ctrl Pts',(-162.318767642849,222.343634628425,4.92878000800459));
#79833=CARTESIAN_POINT('Ctrl Pts',(-163.067051699669,224.189732860741,4.83371863620826));
#79834=CARTESIAN_POINT('Ctrl Pts',(-163.074541166319,225.002732334593,4.79157655282253));
#79835=CARTESIAN_POINT('Origin',(-160.,225.,22.2084234471774));
#79836=CARTESIAN_POINT('',(-163.074698972508,224.997290222874,6.79157655282254));
#79837=CARTESIAN_POINT('',(-163.072934938036,225.002798525283,6.70842344717744));
#79838=CARTESIAN_POINT('',(-163.0735,225.,22.2084234471774));
#79839=CARTESIAN_POINT('Ctrl Pts',(-163.072934938036,225.002798525283,6.70842344717744));
#79840=CARTESIAN_POINT('Ctrl Pts',(-163.075279612769,225.264186775707,6.69489241136339));
#79841=CARTESIAN_POINT('Ctrl Pts',(-162.925138298921,226.545199477924,6.62844208713874));
#79842=CARTESIAN_POINT('Ctrl Pts',(-161.136676060905,228.450388932634,6.50907247450349));
#79843=CARTESIAN_POINT('Ctrl Pts',(-157.717791126824,227.826435725977,6.3503146092717));
#79844=CARTESIAN_POINT('Ctrl Pts',(-156.387583663728,224.615728654052,6.1915567440399));
#79845=CARTESIAN_POINT('Ctrl Pts',(-158.363459489534,221.756706702828,6.03279887880811));
#79846=CARTESIAN_POINT('Ctrl Pts',(-161.837097126162,221.865946649636,5.87404101357632));
#79847=CARTESIAN_POINT('Ctrl Pts',(-163.057796029152,223.893848493671,5.76591586969943));
#79848=CARTESIAN_POINT('Ctrl Pts',(-163.078569939169,224.955225423166,5.71071001423313));
#79849=CARTESIAN_POINT('Ctrl Pts',(-163.078415614449,224.999192687023,5.70842344717743));
#79850=CARTESIAN_POINT('Ctrl Pts',(-163.074698972508,224.997290222874,6.79157655282254));
#79851=CARTESIAN_POINT('Ctrl Pts',(-163.067182320426,225.815396773934,6.74916414205817));
#79852=CARTESIAN_POINT('Ctrl Pts',(-162.310901168231,227.666553034595,6.65383244288321));
#79853=CARTESIAN_POINT('Ctrl Pts',(-159.185378827721,228.540283725802,6.50558145529764));
#79854=CARTESIAN_POINT('Ctrl Pts',(-156.583885023213,226.235870130265,6.34682359006585));
#79855=CARTESIAN_POINT('Ctrl Pts',(-157.108819511125,222.800388240108,6.18806572483406));
#79856=CARTESIAN_POINT('Ctrl Pts',(-160.279762268762,221.377990946107,6.02930785960227));
#79857=CARTESIAN_POINT('Ctrl Pts',(-162.706367520053,222.953434108801,5.89714480226509));
#79858=CARTESIAN_POINT('Ctrl Pts',(-163.068659135346,224.489615197929,5.81790103333851));
#79859=CARTESIAN_POINT('Ctrl Pts',(-163.068595449041,224.999957001683,5.79157655282253));
#79860=CARTESIAN_POINT('Origin',(-160.,225.,22.2084234471774));
#79861=CARTESIAN_POINT('',(-163.077420896739,225.00174689889,7.79157655282253));
#79862=CARTESIAN_POINT('',(-163.068842346438,224.999096720205,7.70842344717744));
#79863=CARTESIAN_POINT('',(-163.0735,225.,22.2084234471774));
#79864=CARTESIAN_POINT('Ctrl Pts',(-163.068842346438,224.999096720205,7.70842344717744));
#79865=CARTESIAN_POINT('Ctrl Pts',(-163.06734401399,225.567952377292,7.67907480849364));
#79866=CARTESIAN_POINT('Ctrl Pts',(-162.642861510995,227.164604692527,7.59680688139924));
#79867=CARTESIAN_POINT('Ctrl Pts',(-160.07295051007,228.632064767727,7.46161966589424));
#79868=CARTESIAN_POINT('Ctrl Pts',(-156.988196799222,227.031319210184,7.30286180066245));
#79869=CARTESIAN_POINT('Ctrl Pts',(-156.65984525929,223.571510391361,7.14410393543066));
#79870=CARTESIAN_POINT('Ctrl Pts',(-159.388403206707,221.41905520619,6.98534607019887));
#79871=CARTESIAN_POINT('Ctrl Pts',(-162.396431314486,222.448010961485,6.84011924078112));
#79872=CARTESIAN_POINT('Ctrl Pts',(-163.066109692584,224.241908777081,6.74781169977398));
#79873=CARTESIAN_POINT('Ctrl Pts',(-163.072934938036,225.002798525283,6.70842344717744));
#79874=CARTESIAN_POINT('Ctrl Pts',(-163.077420896739,225.00174689889,7.79157655282253));
#79875=CARTESIAN_POINT('Ctrl Pts',(-163.078115302259,225.103951701548,7.78626582759902));
#79876=CARTESIAN_POINT('Ctrl Pts',(-163.027126123278,226.223885938778,7.7280358139649));
#79877=CARTESIAN_POINT('Ctrl Pts',(-161.655556204541,228.233628019286,7.61688651192019));
#79878=CARTESIAN_POINT('Ctrl Pts',(-158.181336983412,228.144786375193,7.45812864668841));
#79879=CARTESIAN_POINT('Ctrl Pts',(-156.371558083546,225.177836364189,7.2993707814566));
#79880=CARTESIAN_POINT('Ctrl Pts',(-157.882529082935,222.048130519673,7.14061291622482));
#79881=CARTESIAN_POINT('Ctrl Pts',(-161.331409382354,221.619975507472,6.98185505099302));
#79882=CARTESIAN_POINT('Ctrl Pts',(-162.965935852688,223.57319489042,6.8655095965256));
#79883=CARTESIAN_POINT('Ctrl Pts',(-163.076561081789,224.794619700763,6.80208343046877));
#79884=CARTESIAN_POINT('Ctrl Pts',(-163.074698972508,224.997290222874,6.79157655282254));
#79885=CARTESIAN_POINT('Origin',(-160.,225.,22.2084234471774));
#79886=CARTESIAN_POINT('',(-163.06942424465,225.0015976605,8.79157655282253));
#79887=CARTESIAN_POINT('',(-163.07624444436,224.997680434113,8.70842344717744));
#79888=CARTESIAN_POINT('',(-163.0735,225.,22.2084234471774));
#79889=CARTESIAN_POINT('Ctrl Pts',(-163.07624444436,224.997680434113,8.70842344717744));
#79890=CARTESIAN_POINT('Ctrl Pts',(-163.068938459909,225.867774087993,8.66325720562389));
#79891=CARTESIAN_POINT('Ctrl Pts',(-162.228255830241,227.769667093511,8.56517167565974));
#79892=CARTESIAN_POINT('Ctrl Pts',(-159.002787829475,228.493248365181,8.414166857285));
#79893=CARTESIAN_POINT('Ctrl Pts',(-156.524363026255,226.056959734625,8.2554089920532));
#79894=CARTESIAN_POINT('Ctrl Pts',(-157.226841044731,222.653341596505,8.09665112682142));
#79895=CARTESIAN_POINT('Ctrl Pts',(-160.467314030017,221.397385136983,7.93789326158962));
#79896=CARTESIAN_POINT('Ctrl Pts',(-162.760117702474,223.061204981861,7.80848403504163));
#79897=CARTESIAN_POINT('Ctrl Pts',(-163.070045695926,224.54223404992,7.73199409690424));
#79898=CARTESIAN_POINT('Ctrl Pts',(-163.068842346438,224.999096720205,7.70842344717744));
#79899=CARTESIAN_POINT('Ctrl Pts',(-163.06942424465,225.0015976605,8.79157655282253));
#79900=CARTESIAN_POINT('Ctrl Pts',(-163.071353210531,225.410927499555,8.77044822472927));
#79901=CARTESIAN_POINT('Ctrl Pts',(-162.804636723986,226.843078256208,8.69640060822541));
#79902=CARTESIAN_POINT('Ctrl Pts',(-160.632612760122,228.577291937938,8.56943370331094));
#79903=CARTESIAN_POINT('Ctrl Pts',(-157.337773384114,227.471794077016,8.41067583807916));
#79904=CARTESIAN_POINT('Ctrl Pts',(-156.479403702276,224.10411037401,8.25191797284736));
#79905=CARTESIAN_POINT('Ctrl Pts',(-158.843083613671,221.55634482148,8.09316010761557));
#79906=CARTESIAN_POINT('Ctrl Pts',(-162.151085153962,222.14001193937,7.93971296760729));
#79907=CARTESIAN_POINT('Ctrl Pts',(-163.071195824334,224.085521035082,7.83918511600961));
#79908=CARTESIAN_POINT('Ctrl Pts',(-163.077420896739,225.00174689889,7.79157655282253));
#79909=CARTESIAN_POINT('Origin',(-160.,225.,22.2084234471774));
#79910=CARTESIAN_POINT('',(-163.071594631926,224.997384854747,9.79157655282253));
#79911=CARTESIAN_POINT('',(-163.07607818017,225.002377969017,9.70842344717744));
#79912=CARTESIAN_POINT('',(-163.0735,225.,22.2084234471774));
#79913=CARTESIAN_POINT('Ctrl Pts',(-163.07607818017,225.002377969017,9.70842344717744));
#79914=CARTESIAN_POINT('Ctrl Pts',(-163.077404834783,225.157757418479,9.70035889116474));
#79915=CARTESIAN_POINT('Ctrl Pts',(-162.99606691089,226.331337340389,9.63937504674144));
#79916=CARTESIAN_POINT('Ctrl Pts',(-161.485548879981,228.315171304634,9.52547191390754));
#79917=CARTESIAN_POINT('Ctrl Pts',(-158.020618833015,228.046188840119,9.36671404867576));
#79918=CARTESIAN_POINT('Ctrl Pts',(-156.367218352237,224.989334468915,9.20795618344395));
#79919=CARTESIAN_POINT('Ctrl Pts',(-158.038539492636,221.942241191341,9.04919831821217));
#79920=CARTESIAN_POINT('Ctrl Pts',(-161.504989212242,221.693608655208,8.89044045298038));
#79921=CARTESIAN_POINT('Ctrl Pts',(-162.999733448409,223.680828171028,8.77684882930214));
#79922=CARTESIAN_POINT('Ctrl Pts',(-163.07749855889,224.848323820932,8.71617649403449));
#79923=CARTESIAN_POINT('Ctrl Pts',(-163.07624444436,224.997680434113,8.70842344717744));
#79924=CARTESIAN_POINT('Ctrl Pts',(-163.071594631926,224.997384854747,9.79157655282253));
#79925=CARTESIAN_POINT('Ctrl Pts',(-163.065812161773,225.711885326123,9.75463062185952));
#79926=CARTESIAN_POINT('Ctrl Pts',(-162.461598987361,227.458614398947,9.66476540248591));
#79927=CARTESIAN_POINT('Ctrl Pts',(-159.55384776735,228.605296755998,9.52198089470171));
#79928=CARTESIAN_POINT('Ctrl Pts',(-156.729123813004,226.580691457195,9.36322302946991));
#79929=CARTESIAN_POINT('Ctrl Pts',(-156.897905616373,223.109437398927,9.20446516423812));
#79930=CARTESIAN_POINT('Ctrl Pts',(-159.90572407765,221.368426158816,9.04570729900633));
#79931=CARTESIAN_POINT('Ctrl Pts',(-162.588044857126,222.740409794574,8.90807776186779));
#79932=CARTESIAN_POINT('Ctrl Pts',(-163.066521805919,224.385695227867,8.82336751313987));
#79933=CARTESIAN_POINT('Ctrl Pts',(-163.06942424465,225.0015976605,8.79157655282253));
#79934=CARTESIAN_POINT('Origin',(-160.,225.,22.2084234471774));
#79935=CARTESIAN_POINT('',(-163.078673879984,224.99994405807,10.7915765528225));
#79936=CARTESIAN_POINT('',(-163.068792122127,225.000808750435,10.7084234471774));
#79937=CARTESIAN_POINT('',(-163.0735,225.,22.2084234471774));
#79938=CARTESIAN_POINT('Ctrl Pts',(-163.068792122127,225.000808750435,10.7084234471774));
#79939=CARTESIAN_POINT('Ctrl Pts',(-163.069882767991,225.463728221697,10.684541288295));
#79940=CARTESIAN_POINT('Ctrl Pts',(-162.75422852658,226.950995776746,10.6077398410019));
#79941=CARTESIAN_POINT('Ctrl Pts',(-160.446152228262,228.605296720535,10.4780191052983));
#79942=CARTESIAN_POINT('Ctrl Pts',(-157.213109799941,227.330334582564,10.3192612400665));
#79943=CARTESIAN_POINT('Ctrl Pts',(-156.530629173122,223.922650326269,10.1605033748347));
#79944=CARTESIAN_POINT('Ctrl Pts',(-159.023316590632,221.500956449007,10.0017455096029));
#79945=CARTESIAN_POINT('Ctrl Pts',(-162.237835314049,222.241932744583,9.85105220038383));
#79946=CARTESIAN_POINT('Ctrl Pts',(-163.068699381198,224.138163793459,9.75327817957534));
#79947=CARTESIAN_POINT('Ctrl Pts',(-163.07607818017,225.002377969017,9.70842344717744));
#79948=CARTESIAN_POINT('Ctrl Pts',(-163.078673386206,224.999944063409,10.7915765528225));
#79949=CARTESIAN_POINT('Ctrl Pts',(-163.078401324136,226.01427996409,10.7388130189898));
#79950=CARTESIAN_POINT('Ctrl Pts',(-161.975981803872,228.046452764098,10.6331301967464));
#79951=CARTESIAN_POINT('Ctrl Pts',(-158.514451105407,228.315171337243,10.4745280860925));
#79952=CARTESIAN_POINT('Ctrl Pts',(-156.409095314272,225.550109126926,10.3157702208607));
#79953=CARTESIAN_POINT('Ctrl Pts',(-157.590135350307,222.281587065278,10.1570123556289));
#79954=CARTESIAN_POINT('Ctrl Pts',(-160.976683418975,221.500956414589,9.99825449039708));
#79955=CARTESIAN_POINT('Ctrl Pts',(-162.889275770842,223.359076753176,9.8764425561283));
#79956=CARTESIAN_POINT('Ctrl Pts',(-163.074094649121,224.688474749405,9.80754991027012));
#79957=CARTESIAN_POINT('Ctrl Pts',(-163.071594631926,224.997384854747,9.79157655282253));
#79958=CARTESIAN_POINT('Origin',(-160.,225.,22.2084234471774));
#79959=CARTESIAN_POINT('',(-163.071757647993,225.00265054584,11.7915765528225));
#79960=CARTESIAN_POINT('',(-163.073113961892,224.997194121045,11.7084234471774));
#79961=CARTESIAN_POINT('',(-163.0735,225.,22.2084234471774));
#79962=CARTESIAN_POINT('Ctrl Pts',(-163.073113961892,224.997194121045,11.7084234471774));
#79963=CARTESIAN_POINT('Ctrl Pts',(-163.066182350392,225.763987655113,11.6687236854252));
#79964=CARTESIAN_POINT('Ctrl Pts',(-162.387870314662,227.563847182028,11.5761046352624));
#79965=CARTESIAN_POINT('Ctrl Pts',(-159.367387246101,228.577291902751,11.4305662966891));
#79966=CARTESIAN_POINT('Ctrl Pts',(-156.651515069994,226.408852344075,11.2718084314573));
#79967=CARTESIAN_POINT('Ctrl Pts',(-157.000176170152,222.951031175503,11.1130505662255));
#79968=CARTESIAN_POINT('Ctrl Pts',(-160.094275921422,221.368426194538,10.9542927009937));
#79969=CARTESIAN_POINT('Ctrl Pts',(-162.649624186861,222.847534761029,10.8194169946443));
#79970=CARTESIAN_POINT('Ctrl Pts',(-163.067466060049,224.437967982382,10.7374605767056));
#79971=CARTESIAN_POINT('Ctrl Pts',(-163.068792122127,225.000808750435,10.7084234471774));
#79972=CARTESIAN_POINT('Ctrl Pts',(-163.071757647993,225.00265054584,11.7915765528225));
#79973=CARTESIAN_POINT('Ctrl Pts',(-163.074251734786,225.30549567959,11.7759147045306));
#79974=CARTESIAN_POINT('Ctrl Pts',(-162.893998016579,226.628710180977,11.7073335678281));
#79975=CARTESIAN_POINT('Ctrl Pts',(-160.997212180335,228.493248399541,11.585833142715));
#79976=CARTESIAN_POINT('Ctrl Pts',(-157.606138804509,227.732516256169,11.4270752774832));
#79977=CARTESIAN_POINT('Ctrl Pts',(-156.40592710066,224.470985342605,11.2683174122514));
#79978=CARTESIAN_POINT('Ctrl Pts',(-158.495010772954,221.693608622685,11.1095595470196));
#79979=CARTESIAN_POINT('Ctrl Pts',(-161.961460526658,221.942241161264,10.9508016817878));
#79980=CARTESIAN_POINT('Ctrl Pts',(-163.077314335309,223.976626149827,10.8448073503888));
#79981=CARTESIAN_POINT('Ctrl Pts',(-163.078674189316,224.996949808694,10.7917323074004));
#79982=CARTESIAN_POINT('Ctrl Pts',(-163.078673386206,224.999944063409,10.7915765528225));
#79983=CARTESIAN_POINT('Origin',(-160.,225.,22.2084234471774));
#79984=CARTESIAN_POINT('',(-163.069332066639,224.998485301253,12.7915765528225));
#79985=CARTESIAN_POINT('',(-163.078343795376,225.000912860525,12.7084234471774));
#79986=CARTESIAN_POINT('',(-163.0735,225.,22.2084234471774));
#79987=CARTESIAN_POINT('Ctrl Pts',(-163.078343795376,225.000912860525,12.7084234471774));
#79988=CARTESIAN_POINT('Ctrl Pts',(-163.078539553016,225.050873092039,12.7058253709661));
#79989=CARTESIAN_POINT('Ctrl Pts',(-163.054799327526,226.118265483238,12.6503080063441));
#79990=CARTESIAN_POINT('Ctrl Pts',(-161.8186629987,228.14478634426,12.5418713533116));
#79991=CARTESIAN_POINT('Ctrl Pts',(-158.344443811744,228.233627987479,12.3831134880798));
#79992=CARTESIAN_POINT('Ctrl Pts',(-156.385389583177,225.363053423717,12.224355622848));
#79993=CARTESIAN_POINT('Ctrl Pts',(-157.734426665945,222.160212380846,12.0655977576162));
#79994=CARTESIAN_POINT('Ctrl Pts',(-161.156916374949,221.556344855353,11.9068398923844));
#79995=CARTESIAN_POINT('Ctrl Pts',(-162.929523006467,223.467003778414,11.7877817889048));
#79996=CARTESIAN_POINT('Ctrl Pts',(-163.075422102268,224.741861415817,11.7216429738358));
#79997=CARTESIAN_POINT('Ctrl Pts',(-163.073113961892,224.997194121045,11.7084234471774));
#79998=CARTESIAN_POINT('Ctrl Pts',(-163.069332066639,224.998485301253,12.7915765528225));
#79999=CARTESIAN_POINT('Ctrl Pts',(-163.066612142194,225.608398550393,12.7600971016609));
#80000=CARTESIAN_POINT('Ctrl Pts',(-162.595215251801,227.247495761124,12.6756983620886));
#80001=CARTESIAN_POINT('Ctrl Pts',(-159.927049489213,228.632064803453,12.5383803341058));
#80002=CARTESIAN_POINT('Ctrl Pts',(-156.909060052626,226.908744811449,12.379622468874));
#80003=CARTESIAN_POINT('Ctrl Pts',(-156.719898734327,223.438541643066,12.2208646036422));
#80004=CARTESIAN_POINT('Ctrl Pts',(-159.532685965386,221.397385101546,12.0621067384104));
#80005=CARTESIAN_POINT('Ctrl Pts',(-162.453478463319,222.529438422577,11.9190107214705));
#80006=CARTESIAN_POINT('Ctrl Pts',(-163.065824549446,224.282222520639,11.8288339929412));
#80007=CARTESIAN_POINT('Ctrl Pts',(-163.071757647993,225.00265054584,11.7915765528225));
#80008=CARTESIAN_POINT('Origin',(-160.,225.,22.2084234471774));
#80009=CARTESIAN_POINT('',(-163.077285877774,224.998169460932,13.7915765528225));
#80010=CARTESIAN_POINT('',(-163.070427976155,225.002226664011,13.7084234471774));
#80011=CARTESIAN_POINT('',(-163.0735,225.,22.2084234471774));
#80012=CARTESIAN_POINT('Ctrl Pts',(-163.070427976155,225.002226664011,13.7084234471774));
#80013=CARTESIAN_POINT('Ctrl Pts',(-163.072819163915,225.358710398342,13.6900077680963));
#80014=CARTESIAN_POINT('Ctrl Pts',(-162.850719805817,226.736699387485,13.6186728006046));
#80015=CARTESIAN_POINT('Ctrl Pts',(-160.814621164266,228.540283690979,13.4944185447024));
#80016=CARTESIAN_POINT('Ctrl Pts',(-157.467586127845,227.604629769084,13.3356606794706));
#80017=CARTESIAN_POINT('Ctrl Pts',(-156.438216167636,224.285218784948,13.1769028142388));
#80018=CARTESIAN_POINT('Ctrl Pts',(-158.668590630742,221.61997554072,13.018144949007));
#80019=CARTESIAN_POINT('Ctrl Pts',(-162.061029889295,222.041123781898,12.8619851599865));
#80020=CARTESIAN_POINT('Ctrl Pts',(-163.07455223543,224.033250941865,12.7587446593767));
#80021=CARTESIAN_POINT('Ctrl Pts',(-163.078343795376,225.000912860525,12.7084234471774));
#80022=CARTESIAN_POINT('Ctrl Pts',(-163.077285877774,224.998169460932,13.7915765528225));
#80023=CARTESIAN_POINT('Ctrl Pts',(-163.070868970407,225.908505397637,13.7442794987911));
#80024=CARTESIAN_POINT('Ctrl Pts',(-162.161132862158,227.848532367378,13.6440631563491));
#80025=CARTESIAN_POINT('Ctrl Pts',(-158.863323927915,228.450388966574,13.4909275254965));
#80026=CARTESIAN_POINT('Ctrl Pts',(-156.484724856678,225.916546332844,13.3321696602647));
#80027=CARTESIAN_POINT('Ctrl Pts',(-157.323305458375,222.543880531338,13.1734117950329));
#80028=CARTESIAN_POINT('Ctrl Pts',(-160.611596799308,221.419055170966,13.0146539298011));
#80029=CARTESIAN_POINT('Ctrl Pts',(-162.799120114483,223.144708792098,12.887375515731));
#80030=CARTESIAN_POINT('Ctrl Pts',(-163.071184536592,224.583089215395,12.8130163900715));
#80031=CARTESIAN_POINT('Ctrl Pts',(-163.069332066639,224.998485301253,12.7915765528225));
#80032=CARTESIAN_POINT('Origin',(-160.,225.,22.2084234471774));
#80033=CARTESIAN_POINT('',(-163.074880074443,225.002680230006,14.7915765528225));
#80034=CARTESIAN_POINT('',(-163.070312864252,224.997827536139,14.7084234471775));
#80035=CARTESIAN_POINT('',(-163.0735,225.,22.2084234471774));
#80036=CARTESIAN_POINT('Ctrl Pts',(-163.070312864252,224.997827536139,14.7084234471775));
#80037=CARTESIAN_POINT('Ctrl Pts',(-163.065986485692,225.660564898092,14.6741901652266));
#80038=CARTESIAN_POINT('Ctrl Pts',(-162.529984972378,227.354168692021,14.5870375948652));
#80039=CARTESIAN_POINT('Ctrl Pts',(-159.738697417901,228.623387533023,14.4469657360931));
#80040=CARTESIAN_POINT('Ctrl Pts',(-156.814187836997,226.745799849908,14.2882078708613));
#80041=CARTESIAN_POINT('Ctrl Pts',(-156.805333422394,223.270456212809,14.1294500056295));
#80042=CARTESIAN_POINT('Ctrl Pts',(-159.720237733989,221.377990981734,13.9706921403977));
#80043=CARTESIAN_POINT('Ctrl Pts',(-162.523355763691,222.635392267396,13.830349954247));
#80044=CARTESIAN_POINT('Ctrl Pts',(-163.065947847675,224.334318874811,13.7429270565069));
#80045=CARTESIAN_POINT('Ctrl Pts',(-163.070427976155,225.002226664011,13.7084234471774));
#80046=CARTESIAN_POINT('Ctrl Pts',(-163.074880074443,225.002680230006,14.7915765528225));
#80047=CARTESIAN_POINT('Ctrl Pts',(-163.076678969153,225.199312119173,14.781381184332));
#80048=CARTESIAN_POINT('Ctrl Pts',(-162.969917021752,226.414620457773,14.7182665274308));
#80049=CARTESIAN_POINT('Ctrl Pts',(-161.35123317519,228.372148487207,14.602232582119));
#80050=CARTESIAN_POINT('Ctrl Pts',(-157.899898300982,227.964251906854,14.4434747168873));
#80051=CARTESIAN_POINT('Ctrl Pts',(-156.37057641913,224.843472097915,14.2847168516555));
#80052=CARTESIAN_POINT('Ctrl Pts',(-158.162902855767,221.865946618808,14.1259589864237));
#80053=CARTESIAN_POINT('Ctrl Pts',(-161.636540526564,221.756706670925,13.9672011211919));
#80054=CARTESIAN_POINT('Ctrl Pts',(-163.023764549892,223.763970428172,13.8557403099915));
#80055=CARTESIAN_POINT('Ctrl Pts',(-163.078048660107,224.889957182075,13.7971987872017));
#80056=CARTESIAN_POINT('Ctrl Pts',(-163.077285877774,224.998169460932,13.7915765528225));
#80057=CARTESIAN_POINT('Origin',(-160.,225.,22.2084234471774));
#80058=CARTESIAN_POINT('',(-163.068600857884,225.000142042464,15.7915765528225));
#80059=CARTESIAN_POINT('',(-163.078275131255,224.99899685628,15.7084234471774));
#80060=CARTESIAN_POINT('',(-163.0735,225.,22.2084234471774));
#80061=CARTESIAN_POINT('Ctrl Pts',(-163.078275131255,224.99899685628,15.7084234471774));
#80062=CARTESIAN_POINT('Ctrl Pts',(-163.074175496475,225.961517707257,15.6583725623568));
#80063=CARTESIAN_POINT('Ctrl Pts',(-162.07021132955,227.949094729739,15.5554023891257));
#80064=CARTESIAN_POINT('Ctrl Pts',(-158.685830928108,228.386764813856,15.3995129274839));
#80065=CARTESIAN_POINT('Ctrl Pts',(-156.441904596157,225.732921108328,15.2407550622521));
#80066=CARTESIAN_POINT('Ctrl Pts',(-157.454347037885,222.408308033282,15.0819971970203));
#80067=CARTESIAN_POINT('Ctrl Pts',(-160.796570970435,221.455611344259,14.9232393317885));
#80068=CARTESIAN_POINT('Ctrl Pts',(-162.846283064823,223.252698486056,14.7987147485075));
#80069=CARTESIAN_POINT('Ctrl Pts',(-163.072674388859,224.636076809336,14.7271094536372));
#80070=CARTESIAN_POINT('Ctrl Pts',(-163.070312864252,224.997827536139,14.7084234471775));
#80071=CARTESIAN_POINT('Ctrl Pts',(-163.068600857884,225.000142042464,15.7915765528225));
#80072=CARTESIAN_POINT('Ctrl Pts',(-163.068808772742,225.504442530025,15.7655635814622));
#80073=CARTESIAN_POINT('Ctrl Pts',(-162.712640219014,227.034386277039,15.6866313216913));
#80074=CARTESIAN_POINT('Ctrl Pts',(-160.301025069996,228.620303912768,15.5547797735098));
#80075=CARTESIAN_POINT('Ctrl Pts',(-157.121784978706,227.216550203517,15.396021908278));
#80076=CARTESIAN_POINT('Ctrl Pts',(-156.576687161735,223.784209835184,15.2372640430462));
#80077=CARTESIAN_POINT('Ctrl Pts',(-159.164605119719,221.464560577875,15.0785061778144));
#80078=CARTESIAN_POINT('Ctrl Pts',(-162.301782032254,222.321721154701,14.9299436810732));
#80079=CARTESIAN_POINT('Ctrl Pts',(-163.067341765883,224.17868989613,14.8343004727426));
#80080=CARTESIAN_POINT('Ctrl Pts',(-163.074880074443,225.002680230006,14.7915765528225));
#80081=CARTESIAN_POINT('Origin',(-160.,225.,22.2084234471774));
#80082=CARTESIAN_POINT('',(-163.074358790027,224.997245236004,16.7915765528225));
#80083=CARTESIAN_POINT('',(-163.073270276431,225.002809226401,16.7084234471774));
#80084=CARTESIAN_POINT('',(-163.0735,225.,22.2084234471774));
#80085=CARTESIAN_POINT('Ctrl Pts',(-163.073270276431,225.002809226401,16.7084234471774));
#80086=CARTESIAN_POINT('Ctrl Pts',(-163.075543956965,225.252888159811,16.6954742478977));
#80087=CARTESIAN_POINT('Ctrl Pts',(-162.933293767189,226.522407549409,16.6296057602074));
#80088=CARTESIAN_POINT('Ctrl Pts',(-161.1744486001,228.437715336979,16.5108179841064));
#80089=CARTESIAN_POINT('Ctrl Pts',(-157.748926298441,227.851295046903,16.3520601188746));
#80090=CARTESIAN_POINT('Ctrl Pts',(-156.383586559849,224.655369641669,16.1933022536428));
#80091=CARTESIAN_POINT('Ctrl Pts',(-158.327988259509,221.774849926999,16.034544388411));
#80092=CARTESIAN_POINT('Ctrl Pts',(-161.802615038297,221.845987432231,15.8757865231792));
#80093=CARTESIAN_POINT('Ctrl Pts',(-163.052168846365,223.87121946714,15.767079542768));
#80094=CARTESIAN_POINT('Ctrl Pts',(-163.078510080291,224.943835028985,15.7112918507674));
#80095=CARTESIAN_POINT('Ctrl Pts',(-163.078275131255,224.99899685628,15.7084234471774));
#80096=CARTESIAN_POINT('Ctrl Pts',(-163.074358790027,224.997245236004,16.7915765528225));
#80097=CARTESIAN_POINT('Ctrl Pts',(-163.066909982667,225.804358158871,16.7497459785925));
#80098=CARTESIAN_POINT('Ctrl Pts',(-162.327778343425,227.644612117386,16.6549961159518));
#80099=CARTESIAN_POINT('Ctrl Pts',(-159.224254609194,228.54900487538,16.5073269649006));
#80100=CARTESIAN_POINT('Ctrl Pts',(-156.597644432372,226.273260816304,16.3485690996688));
#80101=CARTESIAN_POINT('Ctrl Pts',(-157.084869938397,222.832228509288,16.189811234437));
#80102=CARTESIAN_POINT('Ctrl Pts',(-160.240022361613,221.37514058481,16.0310533692052));
#80103=CARTESIAN_POINT('Ctrl Pts',(-162.694518125763,222.93069425377,15.8983084753337));
#80104=CARTESIAN_POINT('Ctrl Pts',(-163.068385802748,224.478522708056,15.8184828698728));
#80105=CARTESIAN_POINT('Ctrl Pts',(-163.068600857884,225.000142042464,15.7915765528225));
#80106=CARTESIAN_POINT('Origin',(-160.,225.,22.2084234471774));
#80107=CARTESIAN_POINT('',(-163.077658887757,225.001583255091,17.7915765528225));
#80108=CARTESIAN_POINT('',(-163.068753078883,224.999274061734,17.7084234471774));
#80109=CARTESIAN_POINT('',(-163.0735,225.,22.2084234471774));
#80110=CARTESIAN_POINT('Ctrl Pts',(-163.068753078883,224.999274061734,17.7084234471775));
#80111=CARTESIAN_POINT('Ctrl Pts',(-163.067574754586,225.556892657374,17.679656645028));
#80112=CARTESIAN_POINT('Ctrl Pts',(-162.655451307041,227.14192667646,17.5979705544679));
#80113=CARTESIAN_POINT('Ctrl Pts',(-160.112779483536,228.631046257429,17.4633651754972));
#80114=CARTESIAN_POINT('Ctrl Pts',(-157.01065569651,227.064227921279,17.3046073102654));
#80115=CARTESIAN_POINT('Ctrl Pts',(-156.644379692211,223.608228244332,17.1458494450336));
#80116=CARTESIAN_POINT('Ctrl Pts',(-159.349167264668,221.425978037138,16.9870915798018));
#80117=CARTESIAN_POINT('Ctrl Pts',(-162.380395013843,222.425872430781,16.8412829138497));
#80118=CARTESIAN_POINT('Ctrl Pts',(-163.066252142595,224.230894527875,16.7483935363083));
#80119=CARTESIAN_POINT('Ctrl Pts',(-163.073270276431,225.002809226401,16.7084234471774));
#80120=CARTESIAN_POINT('Ctrl Pts',(-163.077658887757,225.001583255091,17.7915765528225));
#80121=CARTESIAN_POINT('Ctrl Pts',(-163.078230100695,225.092572084339,17.7868476641333));
#80122=CARTESIAN_POINT('Ctrl Pts',(-163.033302735283,226.201212096667,17.7291994870335));
#80123=CARTESIAN_POINT('Ctrl Pts',(-161.690920182255,228.21527672754,17.6186320215231));
#80124=CARTESIAN_POINT('Ctrl Pts',(-158.215935725382,228.164542826343,17.4598741562913));
#80125=CARTESIAN_POINT('Ctrl Pts',(-156.373726632524,225.217619277503,17.3011162910595));
#80126=CARTESIAN_POINT('Ctrl Pts',(-157.850282874527,222.071530659953,17.1423584258277));
#80127=CARTESIAN_POINT('Ctrl Pts',(-161.294260101108,221.605577026048,16.9836005605959));
#80128=CARTESIAN_POINT('Ctrl Pts',(-162.958390309227,223.55043056178,16.8666732695942));
#80129=CARTESIAN_POINT('Ctrl Pts',(-163.076333367171,224.783290618411,16.8026652670031));
#80130=CARTESIAN_POINT('Ctrl Pts',(-163.074358790027,224.997245236004,16.7915765528225));
#80131=CARTESIAN_POINT('Origin',(-160.,225.,22.2084234471774));
#80132=CARTESIAN_POINT('',(-163.069604839599,225.001742689702,18.7915765528225));
#80133=CARTESIAN_POINT('',(-163.07593125098,224.997572466666,18.7084234471774));
#80134=CARTESIAN_POINT('',(-163.0735,225.,22.2084234471774));
#80135=CARTESIAN_POINT('Ctrl Pts',(-163.07593125098,224.997572466666,18.7084234471774));
#80136=CARTESIAN_POINT('Ctrl Pts',(-163.068500077913,225.856684342497,18.6638390421582));
#80137=CARTESIAN_POINT('Ctrl Pts',(-162.24610097103,227.747989564111,18.5663353487284));
#80138=CARTESIAN_POINT('Ctrl Pts',(-159.041158462775,228.503973551838,18.4159123668879));
#80139=CARTESIAN_POINT('Ctrl Pts',(-156.536164017499,226.095014589637,18.2571545016561));
#80140=CARTESIAN_POINT('Ctrl Pts',(-157.201271626476,222.683896050202,18.0983966364243));
#80141=CARTESIAN_POINT('Ctrl Pts',(-160.427775574161,221.392476847509,17.9396387711926));
#80142=CARTESIAN_POINT('Ctrl Pts',(-162.749078753838,223.038418143583,17.8096477081103));
#80143=CARTESIAN_POINT('Ctrl Pts',(-163.069742395014,224.531099830892,17.7325759334386));
#80144=CARTESIAN_POINT('Ctrl Pts',(-163.068753078883,224.999274061734,17.7084234471775));
#80145=CARTESIAN_POINT('Ctrl Pts',(-163.069604839599,225.001742689702,18.7915765528225));
#80146=CARTESIAN_POINT('Ctrl Pts',(-163.071667317009,225.399743333181,18.7710300612636));
#80147=CARTESIAN_POINT('Ctrl Pts',(-162.814828130989,226.820276113243,18.697564281294));
#80148=CARTESIAN_POINT('Ctrl Pts',(-160.671798738453,228.570130775029,18.5711792129139));
#80149=CARTESIAN_POINT('Ctrl Pts',(-157.365046168866,227.50084632268,18.4124213476821));
#80150=CARTESIAN_POINT('Ctrl Pts',(-156.469788080311,224.142773253644,18.2536634824503));
#80151=CARTESIAN_POINT('Ctrl Pts',(-158.805387108694,221.569240893567,18.0949056172185));
#80152=CARTESIAN_POINT('Ctrl Pts',(-162.132156176017,222.118667729787,17.9408766406759));
#80153=CARTESIAN_POINT('Ctrl Pts',(-163.071837862639,224.074348900514,17.8397669525439));
#80154=CARTESIAN_POINT('Ctrl Pts',(-163.077658887757,225.001583255091,17.7915765528225));
#80155=CARTESIAN_POINT('Origin',(-160.,225.,22.2084234471774));
#80156=CARTESIAN_POINT('',(-163.070362295124,224.996974657089,19.7915765528225));
#80157=CARTESIAN_POINT('',(-163.076377868511,225.002226294578,19.7084234471774));
#80158=CARTESIAN_POINT('',(-163.0735,225.,22.2084234471774));
#80159=CARTESIAN_POINT('',(-160.793799282533,222.030777046254,20.));
#80160=CARTESIAN_POINT('Ctrl Pts',(-160.793799282533,222.030777046254,20.));
#80161=CARTESIAN_POINT('Ctrl Pts',(-161.781070948697,222.29471665351,19.9470807115894));
#80162=CARTESIAN_POINT('Ctrl Pts',(-162.879413320178,223.336658232169,19.8776062291969));
#80163=CARTESIAN_POINT('Ctrl Pts',(-163.072766807016,224.67677228815,19.8081317468044));
#80164=CARTESIAN_POINT('Ctrl Pts',(-163.070362295124,224.996974657089,19.7915765528225));
#80165=CARTESIAN_POINT('',(-159.204405557221,222.025443011815,20.));
#80166=CARTESIAN_POINT('Origin',(-160.,225.,20.));
#80167=CARTESIAN_POINT('Ctrl Pts',(-159.204403754918,222.025437656558,20.));
#80168=CARTESIAN_POINT('Ctrl Pts',(-160.166034868365,221.76985452113,19.948244384658));
#80169=CARTESIAN_POINT('Ctrl Pts',(-162.230116403007,222.243618617642,19.8510522003838));
#80170=CARTESIAN_POINT('Ctrl Pts',(-163.069182947608,224.12719520771,19.7538600161096));
#80171=CARTESIAN_POINT('Ctrl Pts',(-163.076377868511,225.002226294578,19.7084234471774));
#80172=CARTESIAN_POINT('Origin',(-160.,-225.,22.2084234471774));
#80173=CARTESIAN_POINT('',(-163.078662475314,-224.999834801063,0.791576552822534));
#80174=CARTESIAN_POINT('',(-163.068636046267,-224.999297928038,0.708423447177441));
#80175=CARTESIAN_POINT('',(-163.0735,-225.,22.2084234471774));
#80176=CARTESIAN_POINT('',(-159.206200717467,-227.969222953746,0.));
#80177=CARTESIAN_POINT('Ctrl Pts',(-163.068636046267,-224.999297928038,
0.708423447177441));
#80178=CARTESIAN_POINT('Ctrl Pts',(-163.069474488198,-224.52504187083,0.683959451760682));
#80179=CARTESIAN_POINT('Ctrl Pts',(-162.742950219825,-223.0260819319,0.606576167933325));
#80180=CARTESIAN_POINT('Ctrl Pts',(-160.407275491335,-221.390669642609,
0.47627359569537));
#80181=CARTESIAN_POINT('Ctrl Pts',(-157.18629120154,-222.69900868369,0.317515730463582));
#80182=CARTESIAN_POINT('Ctrl Pts',(-156.545696171353,-226.117971753255,
0.158757865231786));
#80183=CARTESIAN_POINT('Ctrl Pts',(-158.218929051303,-227.70528334649,0.0529192884105924));
#80184=CARTESIAN_POINT('Ctrl Pts',(-159.206200717467,-227.969222953746,
-4.44089209850063E-15));
#80185=CARTESIAN_POINT('',(-160.793799282533,-227.969222953746,0.));
#80186=CARTESIAN_POINT('Origin',(-160.,-225.,0.));
#80187=CARTESIAN_POINT('Ctrl Pts',(-163.078662475314,-224.999834801063,
0.791576552822534));
#80188=CARTESIAN_POINT('Ctrl Pts',(-163.078668424108,-224.991643764631,
0.791150470866062));
#80189=CARTESIAN_POINT('Ctrl Pts',(-163.074932284103,-223.966133613979,
0.737805100498994));
#80190=CARTESIAN_POINT('Ctrl Pts',(-161.945876991572,-221.932389200875,
0.631540441721325));
#80191=CARTESIAN_POINT('Ctrl Pts',(-158.478135184779,-221.701106251642,
0.472782576489533));
#80192=CARTESIAN_POINT('Ctrl Pts',(-156.403376046572,-224.489749930199,
0.314024711257741));
#80193=CARTESIAN_POINT('Ctrl Pts',(-157.610972032634,-227.719907066083,
0.156430519094562));
#80194=CARTESIAN_POINT('Ctrl Pts',(-159.833965217804,-228.230145500202,
0.0517556153419857));
#80195=CARTESIAN_POINT('Ctrl Pts',(-160.795596249024,-227.974562448592,
5.26163314307215E-15));
#80196=CARTESIAN_POINT('Origin',(-160.,-225.,22.2084234471774));
#80197=CARTESIAN_POINT('',(-163.071455505625,-224.997418107078,1.79157655282252));
#80198=CARTESIAN_POINT('',(-163.073451306714,-225.002809475945,1.70842344717744));
#80199=CARTESIAN_POINT('',(-163.0735,-225.,22.2084234471774));
#80200=CARTESIAN_POINT('Ctrl Pts',(-163.073451306714,-225.002809475945,
1.70842344717744));
#80201=CARTESIAN_POINT('Ctrl Pts',(-163.066339691424,-224.224995087548,
1.66814184889093));
#80202=CARTESIAN_POINT('Ctrl Pts',(-162.371724618713,-222.414034792748,
1.57494096219383));
#80203=CARTESIAN_POINT('Ctrl Pts',(-159.328201249173,-221.429869162289,
1.42882078708612));
#80204=CARTESIAN_POINT('Ctrl Pts',(-156.636247355474,-223.627938915385,
1.27006292185434));
#80205=CARTESIAN_POINT('Ctrl Pts',(-157.022865023245,-227.081779873964,
1.11130505662254));
#80206=CARTESIAN_POINT('Ctrl Pts',(-160.134021061057,-228.63024949042,0.952547191390747));
#80207=CARTESIAN_POINT('Ctrl Pts',(-162.662242062284,-227.129893626905,
0.818253321575716));
#80208=CARTESIAN_POINT('Ctrl Pts',(-163.067660812648,-225.550928797488,
0.73687874017128));
#80209=CARTESIAN_POINT('Ctrl Pts',(-163.068636046267,-224.999297928038,
0.708423447177441));
#80210=CARTESIAN_POINT('Ctrl Pts',(-163.071455505625,-224.997418107078,
1.79157655282252));
#80211=CARTESIAN_POINT('Ctrl Pts',(-163.073957160591,-224.683244104354,
1.77533286799631));
#80212=CARTESIAN_POINT('Ctrl Pts',(-162.885142341109,-223.348477340461,
1.70616989475949));
#80213=CARTESIAN_POINT('Ctrl Pts',(-160.958841571036,-221.496026324134,
1.58408763311208));
#80214=CARTESIAN_POINT('Ctrl Pts',(-157.576314230351,-222.293899143107,
1.42532976788029));
#80215=CARTESIAN_POINT('Ctrl Pts',(-156.411946167088,-225.568405119559,
1.2665719026485));
#80216=CARTESIAN_POINT('Ctrl Pts',(-158.531360356103,-228.322686501262,
1.1078140374167));
#80217=CARTESIAN_POINT('Ctrl Pts',(-161.985587207006,-228.036856539208,
0.949482254141382));
#80218=CARTESIAN_POINT('Ctrl Pts',(-163.077929585162,-226.008968748127,
0.844069759276661));
#80219=CARTESIAN_POINT('Ctrl Pts',(-163.078662475314,-224.999834801063,
0.791576552822534));
#80220=CARTESIAN_POINT('Origin',(-160.,-225.,22.2084234471774));
#80221=CARTESIAN_POINT('',(-163.069508383124,-225.001668073485,2.79157655282253));
#80222=CARTESIAN_POINT('',(-163.078189061057,-224.998894481712,2.70842344717744));
#80223=CARTESIAN_POINT('',(-163.0735,-225.,22.2084234471774));
#80224=CARTESIAN_POINT('Ctrl Pts',(-163.078189061057,-224.998894481711,
2.70842344717744));
#80225=CARTESIAN_POINT('Ctrl Pts',(-163.078472645446,-224.937737510531,
2.70524353443178));
#80226=CARTESIAN_POINT('Ctrl Pts',(-163.049103085114,-223.859099596781,
2.64914433327553));
#80227=CARTESIAN_POINT('Ctrl Pts',(-161.784064304926,-221.835457119938,
2.54012584370867));
#80228=CARTESIAN_POINT('Ctrl Pts',(-158.309079789007,-221.784723217824,
2.38136797847688));
#80229=CARTESIAN_POINT('Ctrl Pts',(-156.381624989618,-224.676610132315,
2.22261011324509));
#80230=CARTESIAN_POINT('Ctrl Pts',(-157.765707675159,-227.864464204611,
2.0638522480133));
#80231=CARTESIAN_POINT('Ctrl Pts',(-161.194612911753,-228.430759164971,
1.90509438278151));
#80232=CARTESIAN_POINT('Ctrl Pts',(-162.937600940753,-226.510208572312,
1.78661811583622));
#80233=CARTESIAN_POINT('Ctrl Pts',(-163.075682459254,-225.246835970244,
1.72106113730153));
#80234=CARTESIAN_POINT('Ctrl Pts',(-163.073451306714,-225.002809475945,
1.70842344717744));
#80235=CARTESIAN_POINT('Ctrl Pts',(-163.069508383124,-225.001668073485,
2.79157655282253));
#80236=CARTESIAN_POINT('Ctrl Pts',(-163.066447265951,-224.380571024344,
2.75951526512656));
#80237=CARTESIAN_POINT('Ctrl Pts',(-162.581779704143,-222.729919533307,
2.67453468902));
#80238=CARTESIAN_POINT('Ctrl Pts',(-159.887220512494,-221.368953614723,
2.53663482450283));
#80239=CARTESIAN_POINT('Ctrl Pts',(-156.888312385766,-223.125268673492,
2.37787695927104));
#80240=CARTESIAN_POINT('Ctrl Pts',(-156.737220668234,-226.597337890817,
2.21911909403925));
#80241=CARTESIAN_POINT('Ctrl Pts',(-159.572224410776,-228.60752327959,2.06036122880746));
#80242=CARTESIAN_POINT('Ctrl Pts',(-162.468601111221,-227.448238632615,
1.91784704840188));
#80243=CARTESIAN_POINT('Ctrl Pts',(-163.065807174792,-225.706772006991,
1.8282521564069));
#80244=CARTESIAN_POINT('Ctrl Pts',(-163.071455505625,-224.997418107078,
1.79157655282252));
#80245=CARTESIAN_POINT('Origin',(-160.,-225.,22.2084234471774));
#80246=CARTESIAN_POINT('',(-163.077533915727,-225.001672030798,3.79157655282253));
#80247=CARTESIAN_POINT('',(-163.070184184725,-224.997892517132,3.70842344717744));
#80248=CARTESIAN_POINT('',(-163.0735,-225.,22.2084234471774));
#80249=CARTESIAN_POINT('Ctrl Pts',(-163.070184184725,-224.997892517132,
3.70842344717744));
#80250=CARTESIAN_POINT('Ctrl Pts',(-163.072507054139,-224.630072375909,
3.68942593156203));
#80251=CARTESIAN_POINT('Ctrl Pts',(-162.841128154736,-223.240481211263,
3.61750912753603));
#80252=CARTESIAN_POINT('Ctrl Pts',(-160.77574540398,-221.450995064354,3.49267303509943));
#80253=CARTESIAN_POINT('Ctrl Pts',(-157.439173021718,-222.423300146398,
3.33391516986764));
#80254=CARTESIAN_POINT('Ctrl Pts',(-156.446269384341,-225.753800828521,
3.17515730463584));
#80255=CARTESIAN_POINT('Ctrl Pts',(-158.705739876912,-228.394423031591,
3.01639943940405));
#80256=CARTESIAN_POINT('Ctrl Pts',(-162.080734455212,-227.937802419816,
2.86082148691792));
#80257=CARTESIAN_POINT('Ctrl Pts',(-163.073753307137,-225.95549606401,2.75816282284238));
#80258=CARTESIAN_POINT('Ctrl Pts',(-163.078189061057,-224.998894481711,
2.70842344717744));
#80259=CARTESIAN_POINT('Ctrl Pts',(-163.077533915727,-225.001672030798,
3.79157655282253));
#80260=CARTESIAN_POINT('Ctrl Pts',(-163.071489070002,-224.080332771393,
3.74369766225681));
#80261=CARTESIAN_POINT('Ctrl Pts',(-162.142316990654,-222.130086615022,
3.6428994832805));
#80262=CARTESIAN_POINT('Ctrl Pts',(-158.825551358552,-221.562284541991,
3.48918201589359));
#80263=CARTESIAN_POINT('Ctrl Pts',(-156.474884286599,-224.122061282515,
3.3304241506618));
#80264=CARTESIAN_POINT('Ctrl Pts',(-157.350402977267,-227.485327504289,
3.17166628543));
#80265=CARTESIAN_POINT('Ctrl Pts',(-160.650832758246,-228.574022088692,
3.01290842019821));
#80266=CARTESIAN_POINT('Ctrl Pts',(-162.80938622554,-226.832479130116,2.88621184266238));
#80267=CARTESIAN_POINT('Ctrl Pts',(-163.071499843504,-225.405733026137,
2.81243455353716));
#80268=CARTESIAN_POINT('Ctrl Pts',(-163.069508383124,-225.001668073485,
2.79157655282253));
#80269=CARTESIAN_POINT('Origin',(-160.,-225.,22.2084234471774));
#80270=CARTESIAN_POINT('',(-163.07454124432,-224.997267665337,4.79157655282253));
#80271=CARTESIAN_POINT('',(-163.070564475416,-225.002286520632,4.70842344717744));
#80272=CARTESIAN_POINT('',(-163.0735,-225.,22.2084234471774));
#80273=CARTESIAN_POINT('Ctrl Pts',(-163.070564475416,-225.002286520632,
4.70842344717744));
#80274=CARTESIAN_POINT('Ctrl Pts',(-163.065908934927,-224.328423958447,
4.67360832869229));
#80275=CARTESIAN_POINT('Ctrl Pts',(-162.515666079354,-222.623370785243,
4.58587392179653));
#80276=CARTESIAN_POINT('Ctrl Pts',(-159.698974924892,-221.379696025755,
4.44522022649019));
#80277=CARTESIAN_POINT('Ctrl Pts',(-156.795232916545,-223.289244347558,
4.28646236125839));
#80278=CARTESIAN_POINT('Ctrl Pts',(-156.82449361689,-226.764476175145,4.1277044960266));
#80279=CARTESIAN_POINT('Ctrl Pts',(-159.759977634311,-228.624859476745,
3.96894663079481));
#80280=CARTESIAN_POINT('Ctrl Pts',(-162.537573645734,-227.342131714516,
3.82918628117842));
#80281=CARTESIAN_POINT('Ctrl Pts',(-163.066036492463,-225.654668461557,
3.74234521997263));
#80282=CARTESIAN_POINT('Ctrl Pts',(-163.070184184725,-224.997892517132,
3.70842344717744));
#80283=CARTESIAN_POINT('Ctrl Pts',(-163.07454124432,-224.997267665337,4.79157655282253));
#80284=CARTESIAN_POINT('Ctrl Pts',(-163.076456563004,-224.789355252538,
4.78079934779766));
#80285=CARTESIAN_POINT('Ctrl Pts',(-162.962447976256,-223.562619237962,
4.71710285436219));
#80286=CARTESIAN_POINT('Ctrl Pts',(-161.314169118159,-221.613235066909,
4.60048707251614));
#80287=CARTESIAN_POINT('Ctrl Pts',(-157.867515181948,-222.058958401537,
4.44172920728434));
#80288=CARTESIAN_POINT('Ctrl Pts',(-156.372511267358,-225.196322891415,
4.28297134205255));
#80289=CARTESIAN_POINT('Ctrl Pts',(-158.197384898239,-228.15401267881,4.12421347682076));
#80290=CARTESIAN_POINT('Ctrl Pts',(-161.672011799357,-228.225150186546,
3.96545561158896));
#80291=CARTESIAN_POINT('Ctrl Pts',(-163.030012387691,-226.213350120791,
3.85457663692289));
#80292=CARTESIAN_POINT('Ctrl Pts',(-163.07817028025,-225.098665013773,3.79661695066741));
#80293=CARTESIAN_POINT('Ctrl Pts',(-163.077533915727,-225.001672030798,
3.79157655282253));
#80294=CARTESIAN_POINT('Origin',(-160.,-225.,22.2084234471774));
#80295=CARTESIAN_POINT('',(-163.068595526891,-225.000042998318,5.79157655282253));
#80296=CARTESIAN_POINT('',(-163.078415697005,-225.000807312998,5.70842344717744));
#80297=CARTESIAN_POINT('',(-163.0735,-225.,22.2084234471774));
#80298=CARTESIAN_POINT('Ctrl Pts',(-163.078415697005,-225.000807312998,
5.70842344717744));
#80299=CARTESIAN_POINT('Ctrl Pts',(-163.074998399108,-224.027215799998,
5.65779072582254));
#80300=CARTESIAN_POINT('Ctrl Pts',(-162.05039264629,-222.029873166014,5.55423871605704));
#80301=CARTESIAN_POINT('Ctrl Pts',(-158.648766801864,-221.627851455529,
5.39776741788094));
#80302=CARTESIAN_POINT('Ctrl Pts',(-156.434080438846,-224.306145083543,
5.23900955264915));
#80303=CARTESIAN_POINT('Ctrl Pts',(-157.482923517968,-227.619454703812,
5.08025168741736));
#80304=CARTESIAN_POINT('Ctrl Pts',(-160.835394894467,-228.535439482161,
4.92149382218556));
#80305=CARTESIAN_POINT('Ctrl Pts',(-162.855790325244,-226.724482242959,
4.79755107543892));
#80306=CARTESIAN_POINT('Ctrl Pts',(-163.072985397698,-225.352701020511,
4.72652761710288));
#80307=CARTESIAN_POINT('Ctrl Pts',(-163.070564475416,-225.002286520632,
4.70842344717744));
#80308=CARTESIAN_POINT('Ctrl Pts',(-163.068595526891,-225.000042998318,
5.79157655282253));
#80309=CARTESIAN_POINT('Ctrl Pts',(-163.068531186586,-224.484460456527,
5.76498174492791));
#80310=CARTESIAN_POINT('Ctrl Pts',(-162.700883871275,-222.942867342694,
5.6854676486227));
#80311=CARTESIAN_POINT('Ctrl Pts',(-160.261302591299,-221.376612339411,
5.55303426390689));
#80312=CARTESIAN_POINT('Ctrl Pts',(-157.097648786153,-222.815148834678,
5.3942763986751));
#80313=CARTESIAN_POINT('Ctrl Pts',(-156.590226697787,-226.253261030531,
5.2355185334433));
#80314=CARTESIAN_POINT('Ctrl Pts',(-159.203429001521,-228.544388780525,
5.07676066821151));
#80315=CARTESIAN_POINT('Ctrl Pts',(-162.318767701676,-227.656365438967,
4.92878000800459));
#80316=CARTESIAN_POINT('Ctrl Pts',(-163.067051777479,-225.810267159815,
4.83371863620826));
#80317=CARTESIAN_POINT('Ctrl Pts',(-163.07454124432,-224.997267665337,4.79157655282253));
#80318=CARTESIAN_POINT('Origin',(-160.,-225.,22.2084234471774));
#80319=CARTESIAN_POINT('',(-163.074699050512,-225.002709777195,6.79157655282254));
#80320=CARTESIAN_POINT('',(-163.072935020445,-224.997201474642,6.70842344717745));
#80321=CARTESIAN_POINT('',(-163.0735,-225.,22.2084234471774));
#80322=CARTESIAN_POINT('Ctrl Pts',(-163.072935020445,-224.997201474642,
6.70842344717745));
#80323=CARTESIAN_POINT('Ctrl Pts',(-163.075279695241,-224.735813217208,
6.69489241136339));
#80324=CARTESIAN_POINT('Ctrl Pts',(-162.925138377367,-223.454800480637,
6.62844208713874));
#80325=CARTESIAN_POINT('Ctrl Pts',(-161.136676091388,-221.549610974834,
6.50907247450348));
#80326=CARTESIAN_POINT('Ctrl Pts',(-157.71779106562,-222.173564198225,6.3503146092717));
#80327=CARTESIAN_POINT('Ctrl Pts',(-156.387583566852,-225.384271356254,
6.1915567440399));
#80328=CARTESIAN_POINT('Ctrl Pts',(-158.363459445645,-228.24329338415,6.03279887880811));
#80329=CARTESIAN_POINT('Ctrl Pts',(-161.837097175429,-228.134053434412,
5.87404101357632));
#80330=CARTESIAN_POINT('Ctrl Pts',(-163.057796111155,-226.106151535993,
5.76591586969943));
#80331=CARTESIAN_POINT('Ctrl Pts',(-163.07857002173,-225.044774578035,5.71071001423314));
#80332=CARTESIAN_POINT('Ctrl Pts',(-163.078415697005,-225.000807312998,
5.70842344717744));
#80333=CARTESIAN_POINT('Ctrl Pts',(-163.074699050512,-225.002709777195,
6.79157655282254));
#80334=CARTESIAN_POINT('Ctrl Pts',(-163.067182398241,-224.18460320538,6.74916414205817));
#80335=CARTESIAN_POINT('Ctrl Pts',(-162.310901226859,-222.333446897755,
6.65383244288321));
#80336=CARTESIAN_POINT('Ctrl Pts',(-159.185378807054,-221.459716184381,
6.50558145529764));
#80337=CARTESIAN_POINT('Ctrl Pts',(-156.583884936547,-223.764129838381,
6.34682359006585));
#80338=CARTESIAN_POINT('Ctrl Pts',(-157.108819437776,-227.199611815696,
6.18806572483406));
#80339=CARTESIAN_POINT('Ctrl Pts',(-160.27976227586,-228.622009145783,6.02930785960227));
#80340=CARTESIAN_POINT('Ctrl Pts',(-162.706367588713,-227.04656594312,5.89714480226509));
#80341=CARTESIAN_POINT('Ctrl Pts',(-163.068659213197,-225.510384815019,
5.81790103333851));
#80342=CARTESIAN_POINT('Ctrl Pts',(-163.068595526891,-225.000042998318,
5.79157655282253));
#80343=CARTESIAN_POINT('Origin',(-160.,-225.,22.2084234471774));
#80344=CARTESIAN_POINT('',(-163.077420974813,-224.998253101066,7.79157655282253));
#80345=CARTESIAN_POINT('',(-163.068842428738,-225.000903279819,7.70842344717744));
#80346=CARTESIAN_POINT('',(-163.0735,-225.,22.2084234471774));
#80347=CARTESIAN_POINT('Ctrl Pts',(-163.068842428738,-225.000903279819,
7.70842344717744));
#80348=CARTESIAN_POINT('Ctrl Pts',(-163.067344096249,-224.432047607476,
7.67907480849364));
#80349=CARTESIAN_POINT('Ctrl Pts',(-162.64286158187,-222.835395249423,7.59680688139924));
#80350=CARTESIAN_POINT('Ctrl Pts',(-160.072950512026,-221.36793513487,7.46161966589424));
#80351=CARTESIAN_POINT('Ctrl Pts',(-156.988196718452,-222.968680735341,
7.30286180066245));
#80352=CARTESIAN_POINT('Ctrl Pts',(-156.659845169714,-226.428489646948,
7.14410393543065));
#80353=CARTESIAN_POINT('Ctrl Pts',(-159.388403190305,-228.580944889843,
6.98534607019887));
#80354=CARTESIAN_POINT('Ctrl Pts',(-162.396431378753,-227.551989106954,
6.84011924078113));
#80355=CARTESIAN_POINT('Ctrl Pts',(-163.06610977481,-225.75809124325,6.74781169977399));
#80356=CARTESIAN_POINT('Ctrl Pts',(-163.072935020445,-224.997201474642,
6.70842344717745));
#80357=CARTESIAN_POINT('Ctrl Pts',(-163.077420974813,-224.998253101066,
7.79157655282253));
#80358=CARTESIAN_POINT('Ctrl Pts',(-163.07811538035,-224.896048295815,7.78626582759902));
#80359=CARTESIAN_POINT('Ctrl Pts',(-163.027126200076,-223.776114030172,
7.7280358139649));
#80360=CARTESIAN_POINT('Ctrl Pts',(-161.655556246542,-221.766371898677,
7.61688651192019));
#80361=CARTESIAN_POINT('Ctrl Pts',(-158.181336937272,-221.855213545024,
7.4581286466884));
#80362=CARTESIAN_POINT('Ctrl Pts',(-156.371557991493,-224.822163631299,
7.29937078145661));
#80363=CARTESIAN_POINT('Ctrl Pts',(-157.882529029215,-227.951869555216,
7.14061291622481));
#80364=CARTESIAN_POINT('Ctrl Pts',(-161.331409416131,-228.380024578279,
6.98185505099302));
#80365=CARTESIAN_POINT('Ctrl Pts',(-162.965935927934,-226.426805145778,
6.8655095965256));
#80366=CARTESIAN_POINT('Ctrl Pts',(-163.076561159841,-225.205380304447,
6.80208343046877));
#80367=CARTESIAN_POINT('Ctrl Pts',(-163.074699050512,-225.002709777195,
6.79157655282254));
#80368=CARTESIAN_POINT('Origin',(-160.,-225.,22.2084234471774));
#80369=CARTESIAN_POINT('',(-163.069424322521,-224.99840233946,8.79157655282254));
#80370=CARTESIAN_POINT('',(-163.076244526858,-225.00231956595,8.70842344717745));
#80371=CARTESIAN_POINT('',(-163.0735,-225.,22.2084234471774));
#80372=CARTESIAN_POINT('Ctrl Pts',(-163.076244526858,-225.00231956595,8.70842344717745));
#80373=CARTESIAN_POINT('Ctrl Pts',(-163.068938542211,-224.132225888735,
8.66325720562389));
#80374=CARTESIAN_POINT('Ctrl Pts',(-162.228255889997,-222.230332832212,
8.56517167565975));
#80375=CARTESIAN_POINT('Ctrl Pts',(-159.002787802732,-221.506751541139,
8.41416685728499));
#80376=CARTESIAN_POINT('Ctrl Pts',(-156.524362933047,-223.943040237029,
8.25540899205321));
#80377=CARTESIAN_POINT('Ctrl Pts',(-157.226840970362,-227.346658466427,
8.09665112682141));
#80378=CARTESIAN_POINT('Ctrl Pts',(-160.46731404255,-228.602614959631,7.93789326158962));
#80379=CARTESIAN_POINT('Ctrl Pts',(-162.760117776494,-226.938795070132,
7.80848403504163));
#80380=CARTESIAN_POINT('Ctrl Pts',(-163.070045778257,-225.457765962356,
7.73199409690424));
#80381=CARTESIAN_POINT('Ctrl Pts',(-163.068842428738,-225.000903279819,
7.70842344717744));
#80382=CARTESIAN_POINT('Ctrl Pts',(-163.069424322521,-224.99840233946,8.79157655282254));
#80383=CARTESIAN_POINT('Ctrl Pts',(-163.071353288451,-224.58907249002,8.77044822472927));
#80384=CARTESIAN_POINT('Ctrl Pts',(-162.804636795139,-223.156921697034,
8.6964006082254));
#80385=CARTESIAN_POINT('Ctrl Pts',(-160.632612776171,-221.422707971306,
8.56943370331094));
#80386=CARTESIAN_POINT('Ctrl Pts',(-157.337773316573,-222.528205860274,
8.41067583807916));
#80387=CARTESIAN_POINT('Ctrl Pts',(-156.479403612958,-225.895889648718,
8.25191797284736));
#80388=CARTESIAN_POINT('Ctrl Pts',(-158.84308358432,-228.443655265885,8.09316010761556));
#80389=CARTESIAN_POINT('Ctrl Pts',(-162.151085208535,-227.859988133188,
7.93971296760729));
#80390=CARTESIAN_POINT('Ctrl Pts',(-163.07119590225,-225.914478988118,7.83918511600961));
#80391=CARTESIAN_POINT('Ctrl Pts',(-163.077420974813,-224.998253101066,
7.79157655282253));
#80392=CARTESIAN_POINT('Origin',(-160.,-225.,22.2084234471774));
#80393=CARTESIAN_POINT('',(-163.071594709852,-225.002615145319,9.79157655282253));
#80394=CARTESIAN_POINT('',(-163.076078262664,-224.997622030919,9.70842344717745));
#80395=CARTESIAN_POINT('',(-163.0735,-225.,22.2084234471774));
#80396=CARTESIAN_POINT('Ctrl Pts',(-163.076078262664,-224.997622030919,
9.70842344717745));
#80397=CARTESIAN_POINT('Ctrl Pts',(-163.077404917311,-224.84224257729,9.70035889116474));
#80398=CARTESIAN_POINT('Ctrl Pts',(-162.996066991238,-223.668662623908,
9.63937504674145));
#80399=CARTESIAN_POINT('Ctrl Pts',(-161.48554891982,-221.684828606461,9.52547191390754));
#80400=CARTESIAN_POINT('Ctrl Pts',(-158.020618779932,-221.953811078189,
9.36671404867575));
#80401=CARTESIAN_POINT('Ctrl Pts',(-156.367218254814,-225.010665531371,
9.20795618344397));
#80402=CARTESIAN_POINT('Ctrl Pts',(-158.038539440034,-228.057758890661,
9.04919831821217));
#80403=CARTESIAN_POINT('Ctrl Pts',(-161.504989252603,-228.306391433462,
8.89044045298037));
#80404=CARTESIAN_POINT('Ctrl Pts',(-162.999733528855,-226.319171864349,
8.77684882930213));
#80405=CARTESIAN_POINT('Ctrl Pts',(-163.077498641421,-225.151676183136,
8.71617649403449));
#80406=CARTESIAN_POINT('Ctrl Pts',(-163.076244526858,-225.00231956595,8.70842344717745));
#80407=CARTESIAN_POINT('Ctrl Pts',(-163.071594709852,-225.002615145319,
9.79157655282253));
#80408=CARTESIAN_POINT('Ctrl Pts',(-163.065812239552,-224.288114655817,
9.75463062185952));
#80409=CARTESIAN_POINT('Ctrl Pts',(-162.461599049811,-222.541385538678,
9.66476540248591));
#80410=CARTESIAN_POINT('Ctrl Pts',(-159.553847756031,-221.394703152536,
9.5219808947017));
#80411=CARTESIAN_POINT('Ctrl Pts',(-156.729123730022,-223.419308502703,
9.3632230294699));
#80412=CARTESIAN_POINT('Ctrl Pts',(-156.897905537673,-226.890562649037,
9.20446516423812));
#80413=CARTESIAN_POINT('Ctrl Pts',(-159.905724075259,-228.631573933316,
9.04570729900632));
#80414=CARTESIAN_POINT('Ctrl Pts',(-162.588044922784,-227.259590262751,
8.9080777618678));
#80415=CARTESIAN_POINT('Ctrl Pts',(-163.066521883717,-225.614304787718,
8.82336751313987));
#80416=CARTESIAN_POINT('Ctrl Pts',(-163.069424322521,-224.99840233946,8.79157655282254));
#80417=CARTESIAN_POINT('Origin',(-160.,-225.,22.2084234471774));
#80418=CARTESIAN_POINT('',(-163.078673958092,-225.000055941931,10.7915765528225));
#80419=CARTESIAN_POINT('',(-163.068792204425,-224.999191249543,10.7084234471774));
#80420=CARTESIAN_POINT('',(-163.0735,-225.,22.2084234471774));
#80421=CARTESIAN_POINT('Ctrl Pts',(-163.068792204425,-224.999191249543,
10.7084234471774));
#80422=CARTESIAN_POINT('Ctrl Pts',(-163.069882850319,-224.536271765866,
10.684541288295));
#80423=CARTESIAN_POINT('Ctrl Pts',(-162.754228600442,-223.049004170933,
10.6077398410019));
#80424=CARTESIAN_POINT('Ctrl Pts',(-160.446152240227,-221.39470318278,10.4780191052983));
#80425=CARTESIAN_POINT('Ctrl Pts',(-157.213109725203,-222.669665354942,
10.3192612400665));
#80426=CARTESIAN_POINT('Ctrl Pts',(-156.530629080082,-226.077349702623,
10.1605033748347));
#80427=CARTESIAN_POINT('Ctrl Pts',(-159.02331656444,-228.499043644829,10.0017455096029));
#80428=CARTESIAN_POINT('Ctrl Pts',(-162.237835374063,-227.758067329382,
9.85105220038383));
#80429=CARTESIAN_POINT('Ctrl Pts',(-163.068699463494,-225.861836229654,
9.75327817957534));
#80430=CARTESIAN_POINT('Ctrl Pts',(-163.076078262664,-224.997622030919,
9.70842344717745));
#80431=CARTESIAN_POINT('Ctrl Pts',(-163.078673464311,-225.000055936592,
10.7915765528225));
#80432=CARTESIAN_POINT('Ctrl Pts',(-163.078401402235,-223.985720010178,
10.7388130189898));
#80433=CARTESIAN_POINT('Ctrl Pts',(-161.975981854003,-221.953547158614,
10.6331301967464));
#80434=CARTESIAN_POINT('Ctrl Pts',(-158.514451067719,-221.684828578651,
10.4745280860924));
#80435=CARTESIAN_POINT('Ctrl Pts',(-156.409095223172,-224.449890859119,
10.3157702208607));
#80436=CARTESIAN_POINT('Ctrl Pts',(-157.590135289169,-227.718413003688,
10.1570123556289));
#80437=CARTESIAN_POINT('Ctrl Pts',(-160.976683443753,-228.499043674182,
9.99825449039708));
#80438=CARTESIAN_POINT('Ctrl Pts',(-162.889275844143,-226.640923288454,
9.87644255612829));
#80439=CARTESIAN_POINT('Ctrl Pts',(-163.074094727111,-225.311525258498,
9.80754991027011));
#80440=CARTESIAN_POINT('Ctrl Pts',(-163.071594709852,-225.002615145319,
9.79157655282253));
#80441=CARTESIAN_POINT('Origin',(-160.,-225.,22.2084234471774));
#80442=CARTESIAN_POINT('',(-163.071757725923,-224.997349454093,11.7915765528225));
#80443=CARTESIAN_POINT('',(-163.073114044306,-225.00280587903,11.7084234471775));
#80444=CARTESIAN_POINT('',(-163.0735,-225.,22.2084234471774));
#80445=CARTESIAN_POINT('Ctrl Pts',(-163.073114044306,-225.00280587903,11.7084234471775));
#80446=CARTESIAN_POINT('Ctrl Pts',(-163.06618243262,-224.236012324399,11.6687236854253));
#80447=CARTESIAN_POINT('Ctrl Pts',(-162.3878703787,-222.436152749216,11.5761046352624));
#80448=CARTESIAN_POINT('Ctrl Pts',(-159.367387229136,-221.422708001315,
11.4305662966891));
#80449=CARTESIAN_POINT('Ctrl Pts',(-156.651514980196,-223.591147618143,
11.2718084314573));
#80450=CARTESIAN_POINT('Ctrl Pts',(-157.000176089704,-227.048968879445,
11.1130505662255));
#80451=CARTESIAN_POINT('Ctrl Pts',(-160.09427592395,-228.631573902853,10.9542927009937));
#80452=CARTESIAN_POINT('Ctrl Pts',(-162.649624257918,-227.152465296695,
10.8194169946443));
#80453=CARTESIAN_POINT('Ctrl Pts',(-163.067466142311,-225.56203203269,10.7374605767056));
#80454=CARTESIAN_POINT('Ctrl Pts',(-163.068792204425,-224.999191249543,
10.7084234471774));
#80455=CARTESIAN_POINT('Ctrl Pts',(-163.071757725923,-224.997349454093,
11.7915765528225));
#80456=CARTESIAN_POINT('Ctrl Pts',(-163.07425181278,-224.694504312659,11.7759147045306));
#80457=CARTESIAN_POINT('Ctrl Pts',(-162.893998089999,-223.371289777703,
11.7073335678281));
#80458=CARTESIAN_POINT('Ctrl Pts',(-160.997212205634,-221.506751511835,
11.585833142715));
#80459=CARTESIAN_POINT('Ctrl Pts',(-157.606138743777,-222.267483674507,
11.4270752774832));
#80460=CARTESIAN_POINT('Ctrl Pts',(-156.405927009479,-225.529014670817,
11.2683174122514));
#80461=CARTESIAN_POINT('Ctrl Pts',(-158.495010734773,-228.306391461198,
11.1095595470196));
#80462=CARTESIAN_POINT('Ctrl Pts',(-161.96146057642,-228.057758916311,10.9508016817878));
#80463=CARTESIAN_POINT('Ctrl Pts',(-163.07731441338,-226.023373876136,10.8448073503888));
#80464=CARTESIAN_POINT('Ctrl Pts',(-163.078674267421,-225.003050191384,
10.7917323074004));
#80465=CARTESIAN_POINT('Ctrl Pts',(-163.078673464311,-225.000055936592,
10.7915765528225));
#80466=CARTESIAN_POINT('Origin',(-160.,-225.,22.2084234471774));
#80467=CARTESIAN_POINT('',(-163.069332144507,-225.001514698785,12.7915765528225));
#80468=CARTESIAN_POINT('',(-163.07834387793,-224.99908713945,12.7084234471775));
#80469=CARTESIAN_POINT('',(-163.0735,-225.,22.2084234471774));
#80470=CARTESIAN_POINT('Ctrl Pts',(-163.07834387793,-224.99908713945,12.7084234471775));
#80471=CARTESIAN_POINT('Ctrl Pts',(-163.078539635575,-224.949126906597,
12.7058253709661));
#80472=CARTESIAN_POINT('Ctrl Pts',(-163.054799409449,-223.881734486773,
12.6503080063442));
#80473=CARTESIAN_POINT('Ctrl Pts',(-161.818663047472,-221.855213571405,
12.5418713533116));
#80474=CARTESIAN_POINT('Ctrl Pts',(-158.344443767345,-221.766371925803,
12.3831134880798));
#80475=CARTESIAN_POINT('Ctrl Pts',(-156.385389486241,-224.636946566547,
12.224355622848));
#80476=CARTESIAN_POINT('Ctrl Pts',(-157.734426605188,-227.839787695311,
12.0655977576162));
#80477=CARTESIAN_POINT('Ctrl Pts',(-161.156916405975,-228.443655236998,
11.9068398923844));
#80478=CARTESIAN_POINT('Ctrl Pts',(-162.92952308503,-226.532996262698,11.7877817889048));
#80479=CARTESIAN_POINT('Ctrl Pts',(-163.075422184743,-225.258138591106,
11.7216429738358));
#80480=CARTESIAN_POINT('Ctrl Pts',(-163.073114044306,-225.00280587903,11.7084234471775));
#80481=CARTESIAN_POINT('Ctrl Pts',(-163.069332144507,-225.001514698785,
12.7915765528225));
#80482=CARTESIAN_POINT('Ctrl Pts',(-163.066612219994,-224.391601434172,
12.7600971016609));
#80483=CARTESIAN_POINT('Ctrl Pts',(-162.595215317641,-222.752504181858,
12.6756983620886));
#80484=CARTESIAN_POINT('Ctrl Pts',(-159.927049487362,-221.367935104402,
12.5383803341058));
#80485=CARTESIAN_POINT('Ctrl Pts',(-156.909059974209,-223.091255140127,
12.379622468874));
#80486=CARTESIAN_POINT('Ctrl Pts',(-156.719898651112,-226.561458396548,
12.2208646036422));
#80487=CARTESIAN_POINT('Ctrl Pts',(-159.53268595353,-228.602614989851,12.0621067384104));
#80488=CARTESIAN_POINT('Ctrl Pts',(-162.453478525563,-227.470561640101,
11.9190107214705));
#80489=CARTESIAN_POINT('Ctrl Pts',(-163.065824627226,-225.717777497571,
11.8288339929412));
#80490=CARTESIAN_POINT('Ctrl Pts',(-163.071757725923,-224.997349454093,
11.7915765528225));
#80491=CARTESIAN_POINT('Origin',(-160.,-225.,22.2084234471774));
#80492=CARTESIAN_POINT('',(-163.077285955845,-225.001830539115,13.7915765528225));
#80493=CARTESIAN_POINT('',(-163.070428058496,-224.997773335929,13.7084234471775));
#80494=CARTESIAN_POINT('',(-163.0735,-225.,22.2084234471774));
#80495=CARTESIAN_POINT('Ctrl Pts',(-163.070428058496,-224.997773335929,
13.7084234471775));
#80496=CARTESIAN_POINT('Ctrl Pts',(-163.072819246321,-224.641289592038,
13.6900077680964));
#80497=CARTESIAN_POINT('Ctrl Pts',(-162.850719882267,-223.26330056594,13.6186728006047));
#80498=CARTESIAN_POINT('Ctrl Pts',(-160.814621186112,-221.459716214079,
13.4944185447024));
#80499=CARTESIAN_POINT('Ctrl Pts',(-157.467586059932,-222.395370161066,
13.3356606794706));
#80500=CARTESIAN_POINT('Ctrl Pts',(-156.438216072117,-225.714781234221,
13.1769028142388));
#80501=CARTESIAN_POINT('Ctrl Pts',(-158.668590595037,-228.380024549925,
13.018144949007));
#80502=CARTESIAN_POINT('Ctrl Pts',(-162.061029944568,-227.958876297453,
12.8619851599865));
#80503=CARTESIAN_POINT('Ctrl Pts',(-163.074552317882,-225.966749084061,
12.7587446593767));
#80504=CARTESIAN_POINT('Ctrl Pts',(-163.07834387793,-224.99908713945,12.7084234471775));
#80505=CARTESIAN_POINT('Ctrl Pts',(-163.077285955845,-225.001830539115,
13.7915765528225));
#80506=CARTESIAN_POINT('Ctrl Pts',(-163.070869048314,-224.091494579315,
13.7442794987911));
#80507=CARTESIAN_POINT('Ctrl Pts',(-162.161132916986,-222.151467560355,
13.6440631563491));
#80508=CARTESIAN_POINT('Ctrl Pts',(-158.863323899077,-221.54961094589,13.4909275254965));
#80509=CARTESIAN_POINT('Ctrl Pts',(-156.484724767496,-224.083453643903,
13.3321696602647));
#80510=CARTESIAN_POINT('Ctrl Pts',(-157.323305390468,-227.456119530974,
13.1734117950329));
#80511=CARTESIAN_POINT('Ctrl Pts',(-160.611596814825,-228.580944919882,
13.0146539298011));
#80512=CARTESIAN_POINT('Ctrl Pts',(-162.799120185496,-226.855291254971,
12.887375515731));
#80513=CARTESIAN_POINT('Ctrl Pts',(-163.071184614508,-225.416910795182,
12.8130163900715));
#80514=CARTESIAN_POINT('Ctrl Pts',(-163.069332144507,-225.001514698785,
12.7915765528225));
#80515=CARTESIAN_POINT('Origin',(-160.,-225.,22.2084234471774));
#80516=CARTESIAN_POINT('',(-163.074880152452,-224.997319769926,14.7915765528225));
#80517=CARTESIAN_POINT('',(-163.070312946591,-225.002172463919,14.7084234471775));
#80518=CARTESIAN_POINT('',(-163.0735,-225.,22.2084234471774));
#80519=CARTESIAN_POINT('Ctrl Pts',(-163.070312946591,-225.002172463919,
14.7084234471775));
#80520=CARTESIAN_POINT('Ctrl Pts',(-163.065986567915,-224.339435084193,
14.6741901652266));
#80521=CARTESIAN_POINT('Ctrl Pts',(-162.529985040226,-222.645831244846,
14.5870375948652));
#80522=CARTESIAN_POINT('Ctrl Pts',(-159.738697410893,-221.376612369806,
14.4469657360931));
#80523=CARTESIAN_POINT('Ctrl Pts',(-156.814187751561,-223.254200103273,
14.2882078708613));
#80524=CARTESIAN_POINT('Ctrl Pts',(-156.805333336721,-226.729543833573,
14.1294500056295));
#80525=CARTESIAN_POINT('Ctrl Pts',(-159.720237726487,-228.622009115399,
13.9706921403977));
#80526=CARTESIAN_POINT('Ctrl Pts',(-162.523355831361,-227.364607796017,
13.830349954247));
#80527=CARTESIAN_POINT('Ctrl Pts',(-163.065947929897,-225.665681143041,
13.7429270565069));
#80528=CARTESIAN_POINT('Ctrl Pts',(-163.070428058496,-224.997773335929,
13.7084234471775));
#80529=CARTESIAN_POINT('Ctrl Pts',(-163.074880152452,-224.997319769926,
14.7915765528225));
#80530=CARTESIAN_POINT('Ctrl Pts',(-163.076679047208,-224.80068787577,14.781381184332));
#80531=CARTESIAN_POINT('Ctrl Pts',(-162.969917097099,-223.585379506338,
14.7182665274308));
#80532=CARTESIAN_POINT('Ctrl Pts',(-161.351233209471,-221.627851427242,
14.6022325821191));
#80533=CARTESIAN_POINT('Ctrl Pts',(-157.899898247702,-222.035748017944,
14.4434747168873));
#80534=CARTESIAN_POINT('Ctrl Pts',(-156.370576327052,-225.156527906056,
14.2847168516555));
#80535=CARTESIAN_POINT('Ctrl Pts',(-158.16290280916,-228.134053460702,14.1259589864237));
#80536=CARTESIAN_POINT('Ctrl Pts',(-161.636540568083,-228.243293411356,
13.9672011211919));
#80537=CARTESIAN_POINT('Ctrl Pts',(-163.023764626605,-226.236029603186,
13.8557403099915));
#80538=CARTESIAN_POINT('Ctrl Pts',(-163.078048738197,-225.110042820717,
13.7971987872017));
#80539=CARTESIAN_POINT('Ctrl Pts',(-163.077285955845,-225.001830539115,
13.7915765528225));
#80540=CARTESIAN_POINT('Origin',(-160.,-225.,22.2084234471774));
#80541=CARTESIAN_POINT('',(-163.068600935734,-224.999857957532,15.7915765528225));
#80542=CARTESIAN_POINT('',(-163.078275213807,-225.001003143747,15.7084234471775));
#80543=CARTESIAN_POINT('',(-163.0735,-225.,22.2084234471774));
#80544=CARTESIAN_POINT('Ctrl Pts',(-163.078275213807,-225.001003143747,
15.7084234471775));
#80545=CARTESIAN_POINT('Ctrl Pts',(-163.074175578918,-224.038482266957,
15.6583725623569));
#80546=CARTESIAN_POINT('Ctrl Pts',(-162.070211385068,-222.050905191173,
15.5554023891257));
#80547=CARTESIAN_POINT('Ctrl Pts',(-158.685830892865,-221.613235095319,
15.3995129274839));
#80548=CARTESIAN_POINT('Ctrl Pts',(-156.441904500737,-224.267078872017,
15.2407550622521));
#80549=CARTESIAN_POINT('Ctrl Pts',(-157.454346969616,-227.591692036222,
15.0819971970203));
#80550=CARTESIAN_POINT('Ctrl Pts',(-160.796570991797,-228.544388750793,
14.9232393317885));
#80551=CARTESIAN_POINT('Ctrl Pts',(-162.846283141153,-226.747301560803,
14.7987147485075));
#80552=CARTESIAN_POINT('Ctrl Pts',(-163.072674471261,-225.363923200424,
14.7271094536372));
#80553=CARTESIAN_POINT('Ctrl Pts',(-163.070312946591,-225.002172463919,
14.7084234471775));
#80554=CARTESIAN_POINT('Ctrl Pts',(-163.068600935734,-224.999857957532,
15.7915765528225));
#80555=CARTESIAN_POINT('Ctrl Pts',(-163.068808850597,-224.495557457177,
15.7655635814622));
#80556=CARTESIAN_POINT('Ctrl Pts',(-162.712640287833,-222.965613671348,
15.6866313216913));
#80557=CARTESIAN_POINT('Ctrl Pts',(-160.301025077633,-221.379695995386,
15.5547797735098));
#80558=CARTESIAN_POINT('Ctrl Pts',(-157.121784905686,-222.78344974025,15.396021908278));
#80559=CARTESIAN_POINT('Ctrl Pts',(-156.576687074886,-226.21579019566,15.2372640430462));
#80560=CARTESIAN_POINT('Ctrl Pts',(-159.164605098526,-228.535439511819,
15.0785061778144));
#80561=CARTESIAN_POINT('Ctrl Pts',(-162.30178209065,-227.678278913247,14.9299436810732));
#80562=CARTESIAN_POINT('Ctrl Pts',(-163.067341843701,-225.821310124706,
14.8343004727426));
#80563=CARTESIAN_POINT('Ctrl Pts',(-163.074880152452,-224.997319769926,
14.7915765528225));
#80564=CARTESIAN_POINT('Origin',(-160.,-225.,22.2084234471774));
#80565=CARTESIAN_POINT('',(-163.074358868023,-225.002754764066,16.7915765528225));
#80566=CARTESIAN_POINT('',(-163.073270358849,-224.997190773524,16.7084234471775));
#80567=CARTESIAN_POINT('',(-163.0735,-225.,22.2084234471774));
#80568=CARTESIAN_POINT('Ctrl Pts',(-163.073270358849,-224.997190773524,
16.7084234471774));
#80569=CARTESIAN_POINT('Ctrl Pts',(-163.075544039444,-224.747111833407,
16.6954742478977));
#80570=CARTESIAN_POINT('Ctrl Pts',(-162.933293845853,-223.477592409764,
16.6296057602074));
#80571=CARTESIAN_POINT('Ctrl Pts',(-161.174448631596,-221.562284570829,
16.5108179841064));
#80572=CARTESIAN_POINT('Ctrl Pts',(-157.748926238073,-222.148704876632,
16.3520601188746));
#80573=CARTESIAN_POINT('Ctrl Pts',(-156.383586462865,-225.344630367573,
16.1933022536428));
#80574=CARTESIAN_POINT('Ctrl Pts',(-158.327988214669,-228.225150159492,
16.034544388411));
#80575=CARTESIAN_POINT('Ctrl Pts',(-161.80261508664,-228.154012652352,15.8757865231792));
#80576=CARTESIAN_POINT('Ctrl Pts',(-163.052168928217,-226.128780563132,
15.767079542768));
#80577=CARTESIAN_POINT('Ctrl Pts',(-163.078510162849,-225.056164972521,
15.7112918507675));
#80578=CARTESIAN_POINT('Ctrl Pts',(-163.078275213807,-225.001003143747,
15.7084234471775));
#80579=CARTESIAN_POINT('Ctrl Pts',(-163.074358868023,-225.002754764066,
16.7915765528225));
#80580=CARTESIAN_POINT('Ctrl Pts',(-163.066910060473,-224.195641820723,
16.7497459785925));
#80581=CARTESIAN_POINT('Ctrl Pts',(-162.327778402481,-222.35538781552,16.6549961159518));
#80582=CARTESIAN_POINT('Ctrl Pts',(-159.224254589513,-221.450995034583,
16.5073269649006));
#80583=CARTESIAN_POINT('Ctrl Pts',(-156.597644346055,-223.726739151393,
16.3485690996688));
#80584=CARTESIAN_POINT('Ctrl Pts',(-157.08486986444,-227.167771545708,16.189811234437));
#80585=CARTESIAN_POINT('Ctrl Pts',(-160.240022367702,-228.624859507152,
16.0310533692052));
#80586=CARTESIAN_POINT('Ctrl Pts',(-162.694518194122,-227.069305798728,
15.8983084753337));
#80587=CARTESIAN_POINT('Ctrl Pts',(-163.068385880592,-225.521477305173,
15.8184828698728));
#80588=CARTESIAN_POINT('Ctrl Pts',(-163.068600935734,-224.999857957532,
15.7915765528225));
#80589=CARTESIAN_POINT('Origin',(-160.,-225.,22.2084234471774));
#80590=CARTESIAN_POINT('',(-163.077658965824,-224.998416744887,17.7915765528225));
#80591=CARTESIAN_POINT('',(-163.06875316118,-225.000725938278,17.7084234471775));
#80592=CARTESIAN_POINT('',(-163.0735,-225.,22.2084234471774));
#80593=CARTESIAN_POINT('Ctrl Pts',(-163.06875316118,-225.000725938278,17.7084234471775));
#80594=CARTESIAN_POINT('Ctrl Pts',(-163.067574836851,-224.443107327688,
17.679656645028));
#80595=CARTESIAN_POINT('Ctrl Pts',(-162.655451378254,-222.858073266113,
17.5979705544679));
#80596=CARTESIAN_POINT('Ctrl Pts',(-160.11277948656,-221.368953645186,17.4633651754972));
#80597=CARTESIAN_POINT('Ctrl Pts',(-157.010655616342,-222.935772023368,
17.3046073102654));
#80598=CARTESIAN_POINT('Ctrl Pts',(-156.644379602221,-226.39177179299,17.1458494450336));
#80599=CARTESIAN_POINT('Ctrl Pts',(-159.349167247214,-228.574022058711,
16.9870915798018));
#80600=CARTESIAN_POINT('Ctrl Pts',(-162.38039507768,-227.574127638251,16.8412829138497));
#80601=CARTESIAN_POINT('Ctrl Pts',(-163.066252224825,-225.76910549275,16.7483935363083));
#80602=CARTESIAN_POINT('Ctrl Pts',(-163.073270358849,-224.997190773524,
16.7084234471774));
#80603=CARTESIAN_POINT('Ctrl Pts',(-163.077658965824,-224.998416744887,
17.7915765528225));
#80604=CARTESIAN_POINT('Ctrl Pts',(-163.078230178775,-224.907427913335,
17.7868476641333));
#80605=CARTESIAN_POINT('Ctrl Pts',(-163.033302812201,-223.798787872917,
17.7291994870335));
#80606=CARTESIAN_POINT('Ctrl Pts',(-161.690920225189,-221.784723190834,
17.6186320215231));
#80607=CARTESIAN_POINT('Ctrl Pts',(-158.215935680102,-221.835457093401,
17.4598741562913));
#80608=CARTESIAN_POINT('Ctrl Pts',(-156.373726540536,-224.782380716962,
17.3011162910595));
#80609=CARTESIAN_POINT('Ctrl Pts',(-157.850282819984,-227.928469414349,
17.1423584258277));
#80610=CARTESIAN_POINT('Ctrl Pts',(-161.294260133946,-228.394423060065,
16.9836005605959));
#80611=CARTESIAN_POINT('Ctrl Pts',(-162.95839038428,-226.449569474996,16.8666732695942));
#80612=CARTESIAN_POINT('Ctrl Pts',(-163.076333445217,-225.216709387087,
16.8026652670031));
#80613=CARTESIAN_POINT('Ctrl Pts',(-163.074358868023,-225.002754764066,
16.7915765528225));
#80614=CARTESIAN_POINT('Origin',(-160.,-225.,22.2084234471774));
#80615=CARTESIAN_POINT('',(-163.069604917803,-224.99825730896,18.7915765528225));
#80616=CARTESIAN_POINT('',(-163.075931333395,-225.0024275328,18.7084234471774));
#80617=CARTESIAN_POINT('',(-163.0735,-225.,22.2084234471774));
#80618=CARTESIAN_POINT('Ctrl Pts',(-163.075931333395,-225.0024275328,18.7084234471774));
#80619=CARTESIAN_POINT('Ctrl Pts',(-163.068500160107,-224.143315633891,
18.6638390421582));
#80620=CARTESIAN_POINT('Ctrl Pts',(-162.246101031359,-222.252010363093,
18.5663353487284));
#80621=CARTESIAN_POINT('Ctrl Pts',(-159.04115843702,-221.496026353686,18.4159123668879));
#80622=CARTESIAN_POINT('Ctrl Pts',(-156.536163924622,-223.90498538126,18.2571545016561));
#80623=CARTESIAN_POINT('Ctrl Pts',(-157.201271551415,-227.316104011775,
18.0983966364243));
#80624=CARTESIAN_POINT('Ctrl Pts',(-160.427775585634,-228.607523249306,
17.9396387711926));
#80625=CARTESIAN_POINT('Ctrl Pts',(-162.749078827562,-226.961581909006,
17.8096477081103));
#80626=CARTESIAN_POINT('Ctrl Pts',(-163.069742477337,-225.468900181672,
17.7325759334386));
#80627=CARTESIAN_POINT('Ctrl Pts',(-163.06875316118,-225.000725938278,17.7084234471775));
#80628=CARTESIAN_POINT('Ctrl Pts',(-163.069604917803,-224.99825730896,18.7915765528225));
#80629=CARTESIAN_POINT('Ctrl Pts',(-163.071667394827,-224.600256656493,
18.7710300612636));
#80630=CARTESIAN_POINT('Ctrl Pts',(-162.8148282007,-223.179723844664,18.697564281294));
#80631=CARTESIAN_POINT('Ctrl Pts',(-160.671798756939,-221.429869131324,
18.5711792129139));
#80632=CARTESIAN_POINT('Ctrl Pts',(-157.365046101209,-222.499153615461,
18.4124213476821));
#80633=CARTESIAN_POINT('Ctrl Pts',(-156.469787991194,-225.857226767288,
18.2536634824503));
#80634=CARTESIAN_POINT('Ctrl Pts',(-158.805387078146,-228.430759193889,
18.0949056172185));
#80635=CARTESIAN_POINT('Ctrl Pts',(-162.132156230227,-227.881332343118,
17.9408766406759));
#80636=CARTESIAN_POINT('Ctrl Pts',(-163.071837940579,-225.925651122953,
17.8397669525439));
#80637=CARTESIAN_POINT('Ctrl Pts',(-163.077658965824,-224.998416744887,
17.7915765528225));
#80638=CARTESIAN_POINT('Origin',(-160.,-225.,22.2084234471774));
#80639=CARTESIAN_POINT('',(-163.070362267144,-225.003024949566,19.7915765528225));
#80640=CARTESIAN_POINT('',(-163.076377950168,-224.997773694264,19.7084234471775));
#80641=CARTESIAN_POINT('',(-163.0735,-225.,22.2084234471774));
#80642=CARTESIAN_POINT('',(-160.793799282533,-227.969222953746,20.));
#80643=CARTESIAN_POINT('Ctrl Pts',(-160.793799282533,-227.969222953746,
20.));
#80644=CARTESIAN_POINT('Ctrl Pts',(-161.781070948697,-227.70528334649,19.9470807115894));
#80645=CARTESIAN_POINT('Ctrl Pts',(-162.879413246734,-226.663341238238,
19.8776062291969));
#80646=CARTESIAN_POINT('Ctrl Pts',(-163.072766768174,-225.323227278198,
19.8081317468044));
#80647=CARTESIAN_POINT('Ctrl Pts',(-163.070362267144,-225.003024949566,
19.7915765528225));
#80648=CARTESIAN_POINT('',(-159.204405553981,-227.97455706887,20.));
#80649=CARTESIAN_POINT('Origin',(-160.,-225.,20.));
#80650=CARTESIAN_POINT('Ctrl Pts',(-159.204403751904,-227.974562423527,
20.));
#80651=CARTESIAN_POINT('Ctrl Pts',(-160.166034802714,-228.230145495107,
19.948244384658));
#80652=CARTESIAN_POINT('Ctrl Pts',(-162.230116536165,-227.756381568108,
19.8510522003838));
#80653=CARTESIAN_POINT('Ctrl Pts',(-163.069183044459,-225.872804827253,
19.7538600161097));
#80654=CARTESIAN_POINT('Ctrl Pts',(-163.076377950168,-224.997773694264,
19.7084234471775));
#80655=CARTESIAN_POINT('Origin',(160.,-225.,22.2084234471774));
#80656=CARTESIAN_POINT('',(156.921337778595,-224.999834790454,0.791576552822529));
#80657=CARTESIAN_POINT('',(156.931363877713,-224.999297943428,0.708423447177436));
#80658=CARTESIAN_POINT('',(156.9265,-225.,22.2084234471774));
#80659=CARTESIAN_POINT('',(160.793799282533,-227.969222953746,0.));
#80660=CARTESIAN_POINT('Ctrl Pts',(156.931363877713,-224.999297943428,0.708423447177436));
#80661=CARTESIAN_POINT('Ctrl Pts',(156.93052543409,-224.525041881822,0.683959451760682));
#80662=CARTESIAN_POINT('Ctrl Pts',(157.257049705227,-223.026081918318,0.606576167933329));
#80663=CARTESIAN_POINT('Ctrl Pts',(159.592724500381,-221.390669414731,0.476273595695376));
#80664=CARTESIAN_POINT('Ctrl Pts',(162.813708891355,-222.699008838373,0.317515730463588));
#80665=CARTESIAN_POINT('Ctrl Pts',(163.454303720846,-226.117970975858,0.158757865231792));
#80666=CARTESIAN_POINT('Ctrl Pts',(161.781070948697,-227.70528334649,0.0529192884105984));
#80667=CARTESIAN_POINT('Ctrl Pts',(160.793799282533,-227.969222953746,0.));
#80668=CARTESIAN_POINT('',(159.206200717467,-227.969222953746,0.));
#80669=CARTESIAN_POINT('Origin',(160.,-225.,0.));
#80670=CARTESIAN_POINT('Ctrl Pts',(156.921337778595,-224.999834790454,0.791576552822529));
#80671=CARTESIAN_POINT('Ctrl Pts',(156.921331829825,-224.991643754766,0.791150470866057));
#80672=CARTESIAN_POINT('Ctrl Pts',(156.925067972487,-223.966133697564,0.737805100498987));
#80673=CARTESIAN_POINT('Ctrl Pts',(158.054123192547,-221.932389526572,0.631540441721319));
#80674=CARTESIAN_POINT('Ctrl Pts',(161.52186463808,-221.701106398635,0.472782576489526));
#80675=CARTESIAN_POINT('Ctrl Pts',(163.596623766652,-224.489750196051,0.314024711257736));
#80676=CARTESIAN_POINT('Ctrl Pts',(162.389027506789,-227.719906449348,0.156430519094557));
#80677=CARTESIAN_POINT('Ctrl Pts',(160.16603498601,-228.230145450022,0.0517556153419843));
#80678=CARTESIAN_POINT('Ctrl Pts',(159.204403760484,-227.974562200359,5.38238616003273E-15));
#80679=CARTESIAN_POINT('Origin',(160.,-225.,22.2084234471774));
#80680=CARTESIAN_POINT('',(156.92854474983,-224.997418107049,1.79157655282252));
#80681=CARTESIAN_POINT('',(156.926548618152,-225.002809476022,1.70842344717743));
#80682=CARTESIAN_POINT('',(156.9265,-225.,22.2084234471774));
#80683=CARTESIAN_POINT('Ctrl Pts',(156.926548618152,-225.002809476022,1.70842344717743));
#80684=CARTESIAN_POINT('Ctrl Pts',(156.933660233471,-224.224995068889,1.66814184889093));
#80685=CARTESIAN_POINT('Ctrl Pts',(157.628275322693,-222.414034730693,1.57494096219383));
#80686=CARTESIAN_POINT('Ctrl Pts',(160.671798768642,-221.429869072041,1.42882078708613));
#80687=CARTESIAN_POINT('Ctrl Pts',(163.363752724354,-223.627938887541,1.27006292185434));
#80688=CARTESIAN_POINT('Ctrl Pts',(162.977135053578,-227.081779913939,1.11130505662255));
#80689=CARTESIAN_POINT('Ctrl Pts',(159.865978929321,-228.630249599949,0.952547191390754));
#80690=CARTESIAN_POINT('Ctrl Pts',(157.337757879225,-227.129893648995,0.818253321575718));
#80691=CARTESIAN_POINT('Ctrl Pts',(156.932339113301,-225.550928817993,0.736878740171278));
#80692=CARTESIAN_POINT('Ctrl Pts',(156.931363877713,-224.999297943428,0.708423447177436));
#80693=CARTESIAN_POINT('Ctrl Pts',(156.92854474983,-224.997418107049,1.79157655282252));
#80694=CARTESIAN_POINT('Ctrl Pts',(156.926043095071,-224.683244130428,1.7753328679963));
#80695=CARTESIAN_POINT('Ctrl Pts',(157.114857898856,-223.348477477565,1.70616989475949));
#80696=CARTESIAN_POINT('Ctrl Pts',(159.041158508843,-221.496026617155,1.58408763311207));
#80697=CARTESIAN_POINT('Ctrl Pts',(162.423685567743,-222.293899365156,1.42532976788028));
#80698=CARTESIAN_POINT('Ctrl Pts',(163.588053535237,-225.568405078077,1.26657190264849));
#80699=CARTESIAN_POINT('Ctrl Pts',(161.468639519931,-228.322686213904,1.1078140374167));
#80700=CARTESIAN_POINT('Ctrl Pts',(158.01441296236,-228.036856307199,0.949482254141376));
#80701=CARTESIAN_POINT('Ctrl Pts',(156.922070665826,-226.008968645781,0.844069759276654));
#80702=CARTESIAN_POINT('Ctrl Pts',(156.921337778595,-224.999834790454,0.791576552822529));
#80703=CARTESIAN_POINT('Origin',(160.,-225.,22.2084234471774));
#80704=CARTESIAN_POINT('',(156.930491872184,-225.001668073344,2.79157655282252));
#80705=CARTESIAN_POINT('',(156.921810863685,-224.99889448168,2.70842344717744));
#80706=CARTESIAN_POINT('',(156.9265,-225.,22.2084234471774));
#80707=CARTESIAN_POINT('Ctrl Pts',(156.921810863685,-224.998894481681,2.70842344717744));
#80708=CARTESIAN_POINT('Ctrl Pts',(156.92152727929,-224.937737509005,2.70524353443178));
#80709=CARTESIAN_POINT('Ctrl Pts',(156.950896840338,-223.859099568886,2.64914433327553));
#80710=CARTESIAN_POINT('Ctrl Pts',(158.215935651436,-221.835457042593,2.54012584370868));
#80711=CARTESIAN_POINT('Ctrl Pts',(161.69092025237,-221.784723139159,2.38136797847689));
#80712=CARTESIAN_POINT('Ctrl Pts',(163.618375098784,-224.676610124513,2.22261011324509));
#80713=CARTESIAN_POINT('Ctrl Pts',(162.234292379592,-227.864464274441,2.0638522480133));
#80714=CARTESIAN_POINT('Ctrl Pts',(158.805387058807,-228.430759249254,1.90509438278151));
#80715=CARTESIAN_POINT('Ctrl Pts',(157.062398987685,-226.510208608751,1.78661811583622));
#80716=CARTESIAN_POINT('Ctrl Pts',(156.924317465603,-225.2468359762,1.72106113730153));
#80717=CARTESIAN_POINT('Ctrl Pts',(156.926548618152,-225.002809476022,1.70842344717743));
#80718=CARTESIAN_POINT('Ctrl Pts',(156.930491872184,-225.001668073344,2.79157655282252));
#80719=CARTESIAN_POINT('Ctrl Pts',(156.933552989102,-224.380571075862,2.75951526512656));
#80720=CARTESIAN_POINT('Ctrl Pts',(157.418220510598,-222.729919722113,2.67453468901999));
#80721=CARTESIAN_POINT('Ctrl Pts',(160.112779478126,-221.368953916766,2.53663482450283));
#80722=CARTESIAN_POINT('Ctrl Pts',(163.111687355417,-223.125268829368,2.37787695927104));
#80723=CARTESIAN_POINT('Ctrl Pts',(163.262779060384,-226.597337758068,2.21911909403925));
#80724=CARTESIAN_POINT('Ctrl Pts',(160.427775553637,-228.607522979317,2.06036122880745));
#80725=CARTESIAN_POINT('Ctrl Pts',(157.531399094122,-227.448238429336,1.91784704840188));
#80726=CARTESIAN_POINT('Ctrl Pts',(156.934193080194,-225.706771948024,1.8282521564069));
#80727=CARTESIAN_POINT('Ctrl Pts',(156.92854474983,-224.997418107049,1.79157655282252));
#80728=CARTESIAN_POINT('Origin',(160.,-225.,22.2084234471774));
#80729=CARTESIAN_POINT('',(156.922466340248,-225.001672030659,3.79157655282253));
#80730=CARTESIAN_POINT('',(156.929815740211,-224.99789251708,3.70842344717744));
#80731=CARTESIAN_POINT('',(156.9265,-225.,22.2084234471774));
#80732=CARTESIAN_POINT('Ctrl Pts',(156.929815740211,-224.99789251708,3.70842344717744));
#80733=CARTESIAN_POINT('Ctrl Pts',(156.92749287074,-224.630072366865,3.68942593156203));
#80734=CARTESIAN_POINT('Ctrl Pts',(157.1588717758,-223.240481168243,3.61750912753603));
#80735=CARTESIAN_POINT('Ctrl Pts',(159.224254577053,-221.450994977583,3.49267303509943));
#80736=CARTESIAN_POINT('Ctrl Pts',(162.560827040894,-222.423300083398,3.33391516986764));
#80737=CARTESIAN_POINT('Ctrl Pts',(163.553730702545,-225.753800846953,3.17515730463585));
#80738=CARTESIAN_POINT('Ctrl Pts',(161.294260154735,-228.39442311458,3.01639943940406));
#80739=CARTESIAN_POINT('Ctrl Pts',(157.91926549391,-227.937802491651,2.86082148691792));
#80740=CARTESIAN_POINT('Ctrl Pts',(156.926246617715,-225.955496087366,2.75816282284238));
#80741=CARTESIAN_POINT('Ctrl Pts',(156.921810863685,-224.998894481681,2.70842344717744));
#80742=CARTESIAN_POINT('Ctrl Pts',(156.922466340248,-225.001672030659,3.79157655282253));
#80743=CARTESIAN_POINT('Ctrl Pts',(156.928511185471,-224.080332847886,3.74369766225681));
#80744=CARTESIAN_POINT('Ctrl Pts',(157.857683187534,-222.130086853728,3.6428994832805));
#80745=CARTESIAN_POINT('Ctrl Pts',(161.174448543763,-221.562284827925,3.48918201589358));
#80746=CARTESIAN_POINT('Ctrl Pts',(163.525115420198,-224.122061355537,3.33042415066179));
#80747=CARTESIAN_POINT('Ctrl Pts',(162.649596802351,-227.485327297572,3.17166628543));
#80748=CARTESIAN_POINT('Ctrl Pts',(159.349167295888,-228.574021791418,3.01290842019821));
#80749=CARTESIAN_POINT('Ctrl Pts',(157.190614008131,-226.832478977704,2.88621184266238));
#80750=CARTESIAN_POINT('Ctrl Pts',(156.928500411969,-225.405732992389,2.81243455353715));
#80751=CARTESIAN_POINT('Ctrl Pts',(156.930491872184,-225.001668073344,2.79157655282252));
#80752=CARTESIAN_POINT('Origin',(160.,-225.,22.2084234471774));
#80753=CARTESIAN_POINT('',(156.925459011406,-224.997267665565,4.79157655282252));
#80754=CARTESIAN_POINT('',(156.92943544951,-225.002286520688,4.70842344717744));
#80755=CARTESIAN_POINT('',(156.9265,-225.,22.2084234471774));
#80756=CARTESIAN_POINT('Ctrl Pts',(156.92943544951,-225.002286520688,4.70842344717743));
#80757=CARTESIAN_POINT('Ctrl Pts',(156.934090990113,-224.328423942027,4.67360832869228));
#80758=CARTESIAN_POINT('Ctrl Pts',(157.484333859139,-222.623370727135,4.58587392179654));
#80759=CARTESIAN_POINT('Ctrl Pts',(160.301025082467,-221.37969593724,4.44522022649019));
#80760=CARTESIAN_POINT('Ctrl Pts',(163.20476716181,-223.289244305731,4.2864623612584));
#80761=CARTESIAN_POINT('Ctrl Pts',(163.17550646075,-226.764476218285,4.1277044960266));
#80762=CARTESIAN_POINT('Ctrl Pts',(160.240022371557,-228.624859565371,3.96894663079482));
#80763=CARTESIAN_POINT('Ctrl Pts',(157.462426292223,-227.34213177178,3.82918628117842));
#80764=CARTESIAN_POINT('Ctrl Pts',(156.933963432573,-225.654668477563,3.74234521997263));
#80765=CARTESIAN_POINT('Ctrl Pts',(156.929815740211,-224.99789251708,3.70842344717744));
#80766=CARTESIAN_POINT('Ctrl Pts',(156.925459011406,-224.997267665564,4.79157655282252));
#80767=CARTESIAN_POINT('Ctrl Pts',(156.923543692882,-224.789355270059,4.78079934779766));
#80768=CARTESIAN_POINT('Ctrl Pts',(157.037552270148,-223.562619357517,4.71710285436219));
#80769=CARTESIAN_POINT('Ctrl Pts',(158.685830991148,-221.613235348605,4.60048707251613));
#80770=CARTESIAN_POINT('Ctrl Pts',(162.132484640682,-222.05895864616,4.44172920728435));
#80771=CARTESIAN_POINT('Ctrl Pts',(163.627488430923,-225.196322875086,4.28297134205254));
#80772=CARTESIAN_POINT('Ctrl Pts',(161.802614951828,-228.154012416474,4.12421347682076));
#80773=CARTESIAN_POINT('Ctrl Pts',(158.327988339714,-228.225149918293,3.96545561158896));
#80774=CARTESIAN_POINT('Ctrl Pts',(156.969987864332,-226.21335001987,3.85457663692289));
#80775=CARTESIAN_POINT('Ctrl Pts',(156.921829975778,-225.098665005566,3.79661695066741));
#80776=CARTESIAN_POINT('Ctrl Pts',(156.922466340248,-225.001672030659,3.79157655282253));
#80777=CARTESIAN_POINT('Origin',(160.,-225.,22.2084234471774));
#80778=CARTESIAN_POINT('',(156.931404728341,-225.000042998315,5.79157655282252));
#80779=CARTESIAN_POINT('',(156.921584227729,-225.000807313018,5.70842344717744));
#80780=CARTESIAN_POINT('',(156.9265,-225.,22.2084234471774));
#80781=CARTESIAN_POINT('Ctrl Pts',(156.921584227729,-225.000807313018,5.70842344717744));
#80782=CARTESIAN_POINT('Ctrl Pts',(156.925001525709,-224.027215776214,5.65779072582254));
#80783=CARTESIAN_POINT('Ctrl Pts',(157.949607303578,-222.029873093395,5.55423871605704));
#80784=CARTESIAN_POINT('Ctrl Pts',(161.351233231173,-221.627851373082,5.39776741788094));
#80785=CARTESIAN_POINT('Ctrl Pts',(163.56591964834,-224.306145066578,5.23900955264915));
#80786=CARTESIAN_POINT('Ctrl Pts',(162.517076543573,-227.619454767856,5.08025168741736));
#80787=CARTESIAN_POINT('Ctrl Pts',(159.164605085109,-228.535439568601,4.92149382218557));
#80788=CARTESIAN_POINT('Ctrl Pts',(157.144209604933,-226.724482285122,4.79755107543892));
#80789=CARTESIAN_POINT('Ctrl Pts',(156.927014527169,-225.352701029134,4.72652761710288));
#80790=CARTESIAN_POINT('Ctrl Pts',(156.92943544951,-225.002286520688,4.70842344717743));
#80791=CARTESIAN_POINT('Ctrl Pts',(156.931404728341,-225.000042998315,5.79157655282252));
#80792=CARTESIAN_POINT('Ctrl Pts',(156.93146906864,-224.484460499407,5.76498174492791));
#80793=CARTESIAN_POINT('Ctrl Pts',(157.299116353373,-222.942867513797,5.6854676486227));
#80794=CARTESIAN_POINT('Ctrl Pts',(159.738697430435,-221.376612640788,5.55303426390689));
#80795=CARTESIAN_POINT('Ctrl Pts',(162.902350972443,-222.815149016404,5.39427639867509));
#80796=CARTESIAN_POINT('Ctrl Pts',(163.409773018603,-226.25326092629,5.23551853344331));
#80797=CARTESIAN_POINT('Ctrl Pts',(160.796570932224,-228.544388485719,5.07676066821151));
#80798=CARTESIAN_POINT('Ctrl Pts',(157.681232491188,-227.656365218022,4.92878000800459));
#80799=CARTESIAN_POINT('Ctrl Pts',(156.932948477624,-225.810267092421,4.83371863620826));
#80800=CARTESIAN_POINT('Ctrl Pts',(156.925459011406,-224.997267665564,4.79157655282252));
#80801=CARTESIAN_POINT('Origin',(160.,-225.,22.2084234471774));
#80802=CARTESIAN_POINT('',(156.925301205227,-225.00270977697,6.79157655282253));
#80803=CARTESIAN_POINT('',(156.927064904423,-224.997201474574,6.70842344717744));
#80804=CARTESIAN_POINT('',(156.9265,-225.,22.2084234471774));
#80805=CARTESIAN_POINT('Ctrl Pts',(156.927064904423,-224.997201474574,6.70842344717744));
#80806=CARTESIAN_POINT('Ctrl Pts',(156.92472022957,-224.735813210749,6.69489241136339));
#80807=CARTESIAN_POINT('Ctrl Pts',(157.074861551115,-223.454800442857,6.62844208713874));
#80808=CARTESIAN_POINT('Ctrl Pts',(158.863323880821,-221.549610890473,6.50907247450349));
#80809=CARTESIAN_POINT('Ctrl Pts',(162.282208990179,-222.17356412912,6.3503146092717));
#80810=CARTESIAN_POINT('Ctrl Pts',(163.61241652147,-225.384271365649,6.19155674403991));
#80811=CARTESIAN_POINT('Ctrl Pts',(161.636540594368,-228.243293463447,6.03279887880811));
#80812=CARTESIAN_POINT('Ctrl Pts',(158.162902779655,-228.134053511038,5.87404101357632));
#80813=CARTESIAN_POINT('Ctrl Pts',(156.942203814083,-226.106151563038,5.76591586969943));
#80814=CARTESIAN_POINT('Ctrl Pts',(156.921429903001,-225.04477457913,5.71071001423314));
#80815=CARTESIAN_POINT('Ctrl Pts',(156.921584227729,-225.000807313018,5.70842344717744));
#80816=CARTESIAN_POINT('Ctrl Pts',(156.925301205227,-225.00270977697,6.79157655282253));
#80817=CARTESIAN_POINT('Ctrl Pts',(156.932817856874,-224.184603273201,6.74916414205816));
#80818=CARTESIAN_POINT('Ctrl Pts',(157.689098965352,-222.333447119547,6.6538324428832));
#80819=CARTESIAN_POINT('Ctrl Pts',(160.814621125189,-221.459716478846,6.50558145529765));
#80820=CARTESIAN_POINT('Ctrl Pts',(163.416114779316,-223.764129941176,6.34682359006585));
#80821=CARTESIAN_POINT('Ctrl Pts',(162.891180321749,-227.199611632742,6.18806572483406));
#80822=CARTESIAN_POINT('Ctrl Pts',(159.72023774741,-228.622008844521,6.02930785960227));
#80823=CARTESIAN_POINT('Ctrl Pts',(157.29363263639,-227.046565772896,5.89714480226509));
#80824=CARTESIAN_POINT('Ctrl Pts',(156.93134104204,-225.510384772568,5.81790103333851));
#80825=CARTESIAN_POINT('Ctrl Pts',(156.931404728341,-225.000042998315,5.79157655282252));
#80826=CARTESIAN_POINT('Origin',(160.,-225.,22.2084234471774));
#80827=CARTESIAN_POINT('',(156.922579281153,-224.998253101211,7.79157655282253));
#80828=CARTESIAN_POINT('',(156.93115749623,-225.000903279841,7.70842344717744));
#80829=CARTESIAN_POINT('',(156.9265,-225.,22.2084234471774));
#80830=CARTESIAN_POINT('Ctrl Pts',(156.93115749623,-225.000903279841,7.70842344717744));
#80831=CARTESIAN_POINT('Ctrl Pts',(156.932655828756,-224.43204759359,7.67907480849364));
#80832=CARTESIAN_POINT('Ctrl Pts',(157.357138353513,-222.8353951965,7.59680688139925));
#80833=CARTESIAN_POINT('Ctrl Pts',(159.92704948619,-221.367935046067,7.46161966589424));
#80834=CARTESIAN_POINT('Ctrl Pts',(163.011803355185,-222.968680685676,7.30286180066245));
#80835=CARTESIAN_POINT('Ctrl Pts',(163.340154911951,-226.428489681874,7.14410393543066));
#80836=CARTESIAN_POINT('Ctrl Pts',(160.611596824648,-228.580944977395,6.98534607019887));
#80837=CARTESIAN_POINT('Ctrl Pts',(157.603568562655,-227.551989169349,6.84011924078113));
#80838=CARTESIAN_POINT('Ctrl Pts',(156.933890150225,-225.758091261785,6.74781169977399));
#80839=CARTESIAN_POINT('Ctrl Pts',(156.927064904423,-224.997201474574,6.70842344717744));
#80840=CARTESIAN_POINT('Ctrl Pts',(156.922579281153,-224.998253101211,7.79157655282253));
#80841=CARTESIAN_POINT('Ctrl Pts',(156.921884875674,-224.896048304461,7.78626582759901));
#80842=CARTESIAN_POINT('Ctrl Pts',(156.972874051707,-223.776114131969,7.7280358139649));
#80843=CARTESIAN_POINT('Ctrl Pts',(158.344443891159,-221.766372167636,7.6168865119202));
#80844=CARTESIAN_POINT('Ctrl Pts',(161.81866291146,-221.855213806593,7.45812864668839));
#80845=CARTESIAN_POINT('Ctrl Pts',(163.628441706709,-224.822163646091,7.29937078145661));
#80846=CARTESIAN_POINT('Ctrl Pts',(162.117470794664,-227.951869309693,7.14061291622481));
#80847=CARTESIAN_POINT('Ctrl Pts',(158.668590694609,-228.380024297143,6.98185505099302));
#80848=CARTESIAN_POINT('Ctrl Pts',(157.03406431876,-226.426805027102,6.86550959652559));
#80849=CARTESIAN_POINT('Ctrl Pts',(156.923439096054,-225.205380287364,6.80208343046876));
#80850=CARTESIAN_POINT('Ctrl Pts',(156.925301205227,-225.00270977697,6.79157655282253));
#80851=CARTESIAN_POINT('Origin',(160.,-225.,22.2084234471774));
#80852=CARTESIAN_POINT('',(156.93057593278,-224.998402339592,8.79157655282253));
#80853=CARTESIAN_POINT('',(156.923755397929,-225.002319566006,8.70842344717744));
#80854=CARTESIAN_POINT('',(156.9265,-225.,22.2084234471774));
#80855=CARTESIAN_POINT('Ctrl Pts',(156.923755397929,-225.002319566006,8.70842344717744));
#80856=CARTESIAN_POINT('Ctrl Pts',(156.931061382755,-224.132225867519,8.66325720562389));
#80857=CARTESIAN_POINT('Ctrl Pts',(157.771744055523,-222.230332764495,8.56517167565975));
#80858=CARTESIAN_POINT('Ctrl Pts',(160.99721222165,-221.50675145573,8.41416685728499));
#80859=CARTESIAN_POINT('Ctrl Pts',(163.475637151931,-223.943040211187,8.25540899205321));
#80860=CARTESIAN_POINT('Ctrl Pts',(162.773159097441,-227.346658523802,8.09665112682141));
#80861=CARTESIAN_POINT('Ctrl Pts',(159.532685946025,-228.602615047713,7.93789326158963));
#80862=CARTESIAN_POINT('Ctrl Pts',(157.239882156022,-226.938795117535,7.80848403504162));
#80863=CARTESIAN_POINT('Ctrl Pts',(156.929954146681,-225.457765973548,7.73199409690423));
#80864=CARTESIAN_POINT('Ctrl Pts',(156.93115749623,-225.000903279841,7.70842344717744));
#80865=CARTESIAN_POINT('Ctrl Pts',(156.93057593278,-224.998402339592,8.79157655282253));
#80866=CARTESIAN_POINT('Ctrl Pts',(156.92864696701,-224.589072524199,8.77044822472927));
#80867=CARTESIAN_POINT('Ctrl Pts',(157.195363438138,-223.156921850333,8.69640060822541));
#80868=CARTESIAN_POINT('Ctrl Pts',(159.367387276447,-221.422708268849,8.56943370331094));
#80869=CARTESIAN_POINT('Ctrl Pts',(162.662226461995,-222.528206065867,8.41067583807915));
#80870=CARTESIAN_POINT('Ctrl Pts',(163.520596094214,-225.895889574202,8.25191797284736));
#80871=CARTESIAN_POINT('Ctrl Pts',(161.156916319453,-228.443654979458,8.09316010761556));
#80872=CARTESIAN_POINT('Ctrl Pts',(157.848914970382,-227.859987895307,7.93971296760729));
#80873=CARTESIAN_POINT('Ctrl Pts',(156.928804353199,-225.914478912056,7.83918511600961));
#80874=CARTESIAN_POINT('Ctrl Pts',(156.922579281153,-224.998253101211,7.79157655282253));
#80875=CARTESIAN_POINT('Origin',(160.,-225.,22.2084234471774));
#80876=CARTESIAN_POINT('',(156.928405545629,-225.002615145101,9.79157655282253));
#80877=CARTESIAN_POINT('',(156.923921662128,-224.997622030861,9.70842344717744));
#80878=CARTESIAN_POINT('',(156.9265,-225.,22.2084234471774));
#80879=CARTESIAN_POINT('Ctrl Pts',(156.923921662128,-224.997622030861,9.70842344717744));
#80880=CARTESIAN_POINT('Ctrl Pts',(156.922595007447,-224.842242573433,9.70035889116474));
#80881=CARTESIAN_POINT('Ctrl Pts',(157.003932935509,-223.668662591357,9.63937504674144));
#80882=CARTESIAN_POINT('Ctrl Pts',(158.514451043859,-221.684828525406,9.52547191390756));
#80883=CARTESIAN_POINT('Ctrl Pts',(161.979381268463,-221.953811003712,9.36671404867575));
#80884=CARTESIAN_POINT('Ctrl Pts',(163.632781834006,-225.010665531631,9.20795618344396));
#80885=CARTESIAN_POINT('Ctrl Pts',(161.961460607923,-228.057758965422,9.04919831821217));
#80886=CARTESIAN_POINT('Ctrl Pts',(158.495010710601,-228.306391514302,8.89044045298037));
#80887=CARTESIAN_POINT('Ctrl Pts',(157.000266397803,-226.319171896602,8.77684882930213));
#80888=CARTESIAN_POINT('Ctrl Pts',(156.922501283335,-225.151676186844,8.71617649403449));
#80889=CARTESIAN_POINT('Ctrl Pts',(156.923755397929,-225.002319566006,8.70842344717744));
#80890=CARTESIAN_POINT('Ctrl Pts',(156.928405545629,-225.002615145101,9.79157655282253));
#80891=CARTESIAN_POINT('Ctrl Pts',(156.934188015448,-224.288114715028,9.75463062185952));
#80892=CARTESIAN_POINT('Ctrl Pts',(157.538401154934,-222.541385743175,9.66476540248591));
#80893=CARTESIAN_POINT('Ctrl Pts',(160.44615220686,-221.394703452409,9.52198089470169));
#80894=CARTESIAN_POINT('Ctrl Pts',(163.270875997921,-223.419308634178,9.36322302946991));
#80895=CARTESIAN_POINT('Ctrl Pts',(163.102094204308,-226.890562491788,9.20446516423811));
#80896=CARTESIAN_POINT('Ctrl Pts',(160.0942759169,-228.631573631259,9.04570729900633));
#80897=CARTESIAN_POINT('Ctrl Pts',(157.411955292478,-227.259590074809,8.90807776186779));
#80898=CARTESIAN_POINT('Ctrl Pts',(156.933478371343,-225.614304736623,8.82336751313986));
#80899=CARTESIAN_POINT('Ctrl Pts',(156.93057593278,-224.998402339592,8.79157655282253));
#80900=CARTESIAN_POINT('Origin',(160.,-225.,22.2084234471774));
#80901=CARTESIAN_POINT('',(156.921326297986,-225.000055941926,10.7915765528225));
#80902=CARTESIAN_POINT('',(156.931207720544,-224.999191249524,10.7084234471774));
#80903=CARTESIAN_POINT('',(156.9265,-225.,22.2084234471774));
#80904=CARTESIAN_POINT('Ctrl Pts',(156.931207720544,-224.999191249524,10.7084234471774));
#80905=CARTESIAN_POINT('Ctrl Pts',(156.930117074624,-224.536271754528,10.684541288295));
#80906=CARTESIAN_POINT('Ctrl Pts',(157.245771332218,-223.049004123232,10.6077398410019));
#80907=CARTESIAN_POINT('Ctrl Pts',(159.553847748865,-221.394703094632,10.4780191052983));
#80908=CARTESIAN_POINT('Ctrl Pts',(162.786890342936,-222.669665297966,10.3192612400665));
#80909=CARTESIAN_POINT('Ctrl Pts',(163.469371004743,-226.077349728964,10.1605033748347));
#80910=CARTESIAN_POINT('Ctrl Pts',(160.97668345944,-228.499043730379,10.0017455096029));
#80911=CARTESIAN_POINT('Ctrl Pts',(157.762164571223,-227.758067396816,9.85105220038384));
#80912=CARTESIAN_POINT('Ctrl Pts',(156.931300461478,-225.861836250725,9.75327817957534));
#80913=CARTESIAN_POINT('Ctrl Pts',(156.923921662128,-224.997622030861,9.70842344717744));
#80914=CARTESIAN_POINT('Ctrl Pts',(156.921326791759,-225.000055936587,10.7915765528225));
#80915=CARTESIAN_POINT('Ctrl Pts',(156.921598853813,-223.985720094541,10.7388130189898));
#80916=CARTESIAN_POINT('Ctrl Pts',(158.024018310351,-221.953547412004,10.6331301967464));
#80917=CARTESIAN_POINT('Ctrl Pts',(161.48554880872,-221.684828854392,10.4745280860924));
#80918=CARTESIAN_POINT('Ctrl Pts',(163.590904478153,-224.449890904874,10.3157702208607));
#80919=CARTESIAN_POINT('Ctrl Pts',(162.40986451039,-227.718412777583,10.1570123556289));
#80920=CARTESIAN_POINT('Ctrl Pts',(159.023316637483,-228.499043383147,9.99825449039708));
#80921=CARTESIAN_POINT('Ctrl Pts',(157.110724396174,-226.64092315197,9.87644255612829));
#80922=CARTESIAN_POINT('Ctrl Pts',(156.925905528579,-225.311525232587,9.80754991027011));
#80923=CARTESIAN_POINT('Ctrl Pts',(156.928405545629,-225.002615145101,9.79157655282253));
#80924=CARTESIAN_POINT('Origin',(160.,-225.,22.2084234471774));
#80925=CARTESIAN_POINT('',(156.928242529572,-224.997349454313,11.7915765528225));
#80926=CARTESIAN_POINT('',(156.926885880558,-225.002805879099,11.7084234471774));
#80927=CARTESIAN_POINT('',(156.9265,-225.,22.2084234471774));
#80928=CARTESIAN_POINT('Ctrl Pts',(156.926885880558,-225.002805879099,11.7084234471774));
#80929=CARTESIAN_POINT('Ctrl Pts',(156.933817492414,-224.236012305719,11.6687236854252));
#80930=CARTESIAN_POINT('Ctrl Pts',(157.612129562918,-222.436152686531,11.5761046352624));
#80931=CARTESIAN_POINT('Ctrl Pts',(160.632612786331,-221.422707913851,11.4305662966891));
#80932=CARTESIAN_POINT('Ctrl Pts',(163.348485101673,-223.591147583697,11.2718084314573));
#80933=CARTESIAN_POINT('Ctrl Pts',(162.99982398364,-227.048968929542,11.1130505662255));
#80934=CARTESIAN_POINT('Ctrl Pts',(159.905724073745,-228.631573991643,10.9542927009937));
#80935=CARTESIAN_POINT('Ctrl Pts',(157.350375677299,-227.152465349322,10.8194169946443));
#80936=CARTESIAN_POINT('Ctrl Pts',(156.93253378269,-225.562032046432,10.7374605767056));
#80937=CARTESIAN_POINT('Ctrl Pts',(156.931207720544,-224.999191249524,10.7084234471774));
#80938=CARTESIAN_POINT('Ctrl Pts',(156.928242529572,-224.997349454313,11.7915765528225));
#80939=CARTESIAN_POINT('Ctrl Pts',(156.925748442923,-224.694504338069,11.7759147045306));
#80940=CARTESIAN_POINT('Ctrl Pts',(157.106002150711,-223.371289913171,11.7073335678281));
#80941=CARTESIAN_POINT('Ctrl Pts',(159.00278787731,-221.506751802388,11.585833142715));
#80942=CARTESIAN_POINT('Ctrl Pts',(162.393861057113,-222.267483901785,11.4270752774832));
#80943=CARTESIAN_POINT('Ctrl Pts',(163.594072691582,-225.529014626816,11.2683174122514));
#80944=CARTESIAN_POINT('Ctrl Pts',(161.504989140049,-228.306391186187,11.1095595470196));
#80945=CARTESIAN_POINT('Ctrl Pts',(158.038539586726,-228.057758661981,10.9508016817878));
#80946=CARTESIAN_POINT('Ctrl Pts',(156.922685842577,-226.023373791017,10.8448073503888));
#80947=CARTESIAN_POINT('Ctrl Pts',(156.921325988649,-225.00305019113,10.7917323074004));
#80948=CARTESIAN_POINT('Ctrl Pts',(156.921326791759,-225.000055936587,10.7915765528225));
#80949=CARTESIAN_POINT('Origin',(160.,-225.,22.2084234471774));
#80950=CARTESIAN_POINT('',(156.930668110786,-225.001514698659,12.7915765528225));
#80951=CARTESIAN_POINT('',(156.921656046805,-224.999087139428,12.7084234471775));
#80952=CARTESIAN_POINT('',(156.9265,-225.,22.2084234471774));
#80953=CARTESIAN_POINT('Ctrl Pts',(156.921656046805,-224.999087139428,12.7084234471775));
#80954=CARTESIAN_POINT('Ctrl Pts',(156.921460289156,-224.949126905353,12.7058253709661));
#80955=CARTESIAN_POINT('Ctrl Pts',(156.945200515863,-223.881734459432,12.6503080063441));
#80956=CARTESIAN_POINT('Ctrl Pts',(158.181336908062,-221.855213494516,12.5418713533116));
#80957=CARTESIAN_POINT('Ctrl Pts',(161.655556273132,-221.766371846742,12.3831134880798));
#80958=CARTESIAN_POINT('Ctrl Pts',(163.614610602134,-224.63694655767,12.224355622848));
#80959=CARTESIAN_POINT('Ctrl Pts',(162.265573450205,-227.839787764742,12.0655977576162));
#80960=CARTESIAN_POINT('Ctrl Pts',(158.843083565739,-228.443655321194,11.9068398923844));
#80961=CARTESIAN_POINT('Ctrl Pts',(157.070476843345,-226.532996300179,11.7877817889048));
#80962=CARTESIAN_POINT('Ctrl Pts',(156.924577740064,-225.258138597417,11.7216429738358));
#80963=CARTESIAN_POINT('Ctrl Pts',(156.926885880558,-225.002805879099,11.7084234471774));
#80964=CARTESIAN_POINT('Ctrl Pts',(156.930668110786,-225.001514698659,12.7915765528225));
#80965=CARTESIAN_POINT('Ctrl Pts',(156.933388035073,-224.391601484776,12.7600971016609));
#80966=CARTESIAN_POINT('Ctrl Pts',(157.404784898217,-222.752504368794,12.6756983620886));
#80967=CARTESIAN_POINT('Ctrl Pts',(160.072950506571,-221.367935406501,12.5383803341058));
#80968=CARTESIAN_POINT('Ctrl Pts',(163.090939768701,-223.091255298888,12.379622468874));
#80969=CARTESIAN_POINT('Ctrl Pts',(163.280101076064,-226.561458266673,12.2208646036422));
#80970=CARTESIAN_POINT('Ctrl Pts',(160.467314007601,-228.602614690202,12.0621067384104));
#80971=CARTESIAN_POINT('Ctrl Pts',(157.546521678506,-227.470561434611,11.9190107214705));
#80972=CARTESIAN_POINT('Ctrl Pts',(156.934175627776,-225.717777437869,11.8288339929412));
#80973=CARTESIAN_POINT('Ctrl Pts',(156.928242529572,-224.997349454313,11.7915765528225));
#80974=CARTESIAN_POINT('Origin',(160.,-225.,22.2084234471774));
#80975=CARTESIAN_POINT('',(156.92271430011,-225.001830538963,13.7915765528225));
#80976=CARTESIAN_POINT('',(156.929571866433,-224.997773335875,13.7084234471774));
#80977=CARTESIAN_POINT('',(156.9265,-225.,22.2084234471774));
#80978=CARTESIAN_POINT('Ctrl Pts',(156.929571866433,-224.997773335875,13.7084234471774));
#80979=CARTESIAN_POINT('Ctrl Pts',(156.92718067855,-224.641289583268,13.6900077680964));
#80980=CARTESIAN_POINT('Ctrl Pts',(157.149280048035,-223.263300523479,13.6186728006047));
#80981=CARTESIAN_POINT('Ctrl Pts',(159.185378793971,-221.459716127521,13.4944185447024));
#80982=CARTESIAN_POINT('Ctrl Pts',(162.532414001985,-222.395370097384,13.3356606794706));
#80983=CARTESIAN_POINT('Ctrl Pts',(163.561784014967,-225.714781251697,13.1769028142388));
#80984=CARTESIAN_POINT('Ctrl Pts',(161.331409437515,-228.380024632565,13.018144949007));
#80985=CARTESIAN_POINT('Ctrl Pts',(157.938970005041,-227.958876369796,12.8619851599865));
#80986=CARTESIAN_POINT('Ctrl Pts',(156.925447606946,-225.966749107697,12.7587446593767));
#80987=CARTESIAN_POINT('Ctrl Pts',(156.921656046805,-224.999087139428,12.7084234471775));
#80988=CARTESIAN_POINT('Ctrl Pts',(156.92271430011,-225.001830538963,13.7915765528225));
#80989=CARTESIAN_POINT('Ctrl Pts',(156.929131207107,-224.09149465488,13.7442794987911));
#80990=CARTESIAN_POINT('Ctrl Pts',(157.838867262768,-222.151467797283,13.6440631563491));
#80991=CARTESIAN_POINT('Ctrl Pts',(161.136676006379,-221.549611232878,13.4909275254965));
#80992=CARTESIAN_POINT('Ctrl Pts',(163.515274940119,-224.083453720138,13.3321696602647));
#80993=CARTESIAN_POINT('Ctrl Pts',(162.676694386897,-227.456119326685,13.1734117950329));
#80994=CARTESIAN_POINT('Ctrl Pts',(159.388403236045,-228.580944622035,13.0146539298011));
#80995=CARTESIAN_POINT('Ctrl Pts',(157.200880047322,-226.855291100656,12.887375515731));
#80996=CARTESIAN_POINT('Ctrl Pts',(156.92881564094,-225.416910760505,12.8130163900715));
#80997=CARTESIAN_POINT('Ctrl Pts',(156.930668110786,-225.001514698659,12.7915765528225));
#80998=CARTESIAN_POINT('Origin',(160.,-225.,22.2084234471774));
#80999=CARTESIAN_POINT('',(156.925120103303,-224.997319770149,14.7915765528225));
#81000=CARTESIAN_POINT('',(156.929686978342,-225.002172463972,14.7084234471774));
#81001=CARTESIAN_POINT('',(156.9265,-225.,22.2084234471774));
#81002=CARTESIAN_POINT('Ctrl Pts',(156.929686978341,-225.002172463972,14.7084234471774));
#81003=CARTESIAN_POINT('Ctrl Pts',(156.934013357123,-224.339435068042,14.6741901652266));
#81004=CARTESIAN_POINT('Ctrl Pts',(157.470014897917,-222.645831187287,14.5870375948652));
#81005=CARTESIAN_POINT('Ctrl Pts',(160.261302595496,-221.376612281216,14.4469657360931));
#81006=CARTESIAN_POINT('Ctrl Pts',(163.185812326331,-223.254200060589,14.2882078708613));
#81007=CARTESIAN_POINT('Ctrl Pts',(163.194666741387,-226.72954387586,14.1294500056295));
#81008=CARTESIAN_POINT('Ctrl Pts',(160.279762280353,-228.622009203956,13.9706921403977));
#81009=CARTESIAN_POINT('Ctrl Pts',(157.476644106943,-227.364607853831,13.830349954247));
#81010=CARTESIAN_POINT('Ctrl Pts',(156.934051995142,-225.665681159316,13.7429270565069));
#81011=CARTESIAN_POINT('Ctrl Pts',(156.929571866433,-224.997773335875,13.7084234471774));
#81012=CARTESIAN_POINT('Ctrl Pts',(156.925120103303,-224.997319770149,14.7915765528225));
#81013=CARTESIAN_POINT('Ctrl Pts',(156.923321208696,-224.800687892348,14.781381184332));
#81014=CARTESIAN_POINT('Ctrl Pts',(157.030083149926,-223.585379624,14.7182665274308));
#81015=CARTESIAN_POINT('Ctrl Pts',(158.648766902918,-221.627851707722,14.6022325821191));
#81016=CARTESIAN_POINT('Ctrl Pts',(162.100101577621,-222.035748264497,14.4434747168873));
#81017=CARTESIAN_POINT('Ctrl Pts',(163.629423371069,-225.156527893037,14.2847168516555));
#81018=CARTESIAN_POINT('Ctrl Pts',(161.837097038039,-228.134053200026,14.1259589864237));
#81019=CARTESIAN_POINT('Ctrl Pts',(158.363459568037,-228.243293141594,13.9672011211919));
#81020=CARTESIAN_POINT('Ctrl Pts',(156.976235624899,-226.236029500378,13.8557403099915));
#81021=CARTESIAN_POINT('Ctrl Pts',(156.921951517821,-225.110042811564,13.7971987872017));
#81022=CARTESIAN_POINT('Ctrl Pts',(156.92271430011,-225.001830538963,13.7915765528225));
#81023=CARTESIAN_POINT('Origin',(160.,-225.,22.2084234471774));
#81024=CARTESIAN_POINT('',(156.931399319499,-224.999857957544,15.7915765528225));
#81025=CARTESIAN_POINT('',(156.92172471093,-225.001003143772,15.7084234471775));
#81026=CARTESIAN_POINT('',(156.9265,-225.,22.2084234471774));
#81027=CARTESIAN_POINT('Ctrl Pts',(156.92172471093,-225.001003143772,15.7084234471775));
#81028=CARTESIAN_POINT('Ctrl Pts',(156.92582434592,-224.038482243449,15.6583725623569));
#81029=CARTESIAN_POINT('Ctrl Pts',(157.929788564316,-222.050905119068,15.5554023891257));
#81030=CARTESIAN_POINT('Ctrl Pts',(161.314169139266,-221.613235012514,15.3995129274839));
#81031=CARTESIAN_POINT('Ctrl Pts',(163.558095586257,-224.267078854098,15.2407550622521));
#81032=CARTESIAN_POINT('Ctrl Pts',(162.545653092624,-227.591692099587,15.0819971970203));
#81033=CARTESIAN_POINT('Ctrl Pts',(159.203428988727,-228.544388837452,14.9232393317885));
#81034=CARTESIAN_POINT('Ctrl Pts',(157.153716789256,-226.747301603524,14.7987147485075));
#81035=CARTESIAN_POINT('Ctrl Pts',(156.927325453613,-225.363923209321,14.7271094536372));
#81036=CARTESIAN_POINT('Ctrl Pts',(156.929686978341,-225.002172463972,14.7084234471774));
#81037=CARTESIAN_POINT('Ctrl Pts',(156.931399319499,-224.999857957544,15.7915765528225));
#81038=CARTESIAN_POINT('Ctrl Pts',(156.931191404653,-224.495557499134,15.7655635814622));
#81039=CARTESIAN_POINT('Ctrl Pts',(157.287359937792,-222.96561384056,15.6866313216913));
#81040=CARTESIAN_POINT('Ctrl Pts',(159.698974947405,-221.379696296506,15.5547797735098));
#81041=CARTESIAN_POINT('Ctrl Pts',(162.878214854917,-222.783449924613,15.396021908278));
#81042=CARTESIAN_POINT('Ctrl Pts',(163.423312640378,-226.215790094536,15.2372640430462));
#81043=CARTESIAN_POINT('Ctrl Pts',(160.83539483199,-228.535439217757,15.0785061778144));
#81044=CARTESIAN_POINT('Ctrl Pts',(157.698218100801,-227.67827869048,14.9299436810732));
#81045=CARTESIAN_POINT('Ctrl Pts',(156.932658411426,-225.821310056393,14.8343004727426));
#81046=CARTESIAN_POINT('Ctrl Pts',(156.925120103303,-224.997319770149,14.7915765528225));
#81047=CARTESIAN_POINT('Origin',(160.,-225.,22.2084234471774));
#81048=CARTESIAN_POINT('',(156.925641387687,-225.002754763835,16.7915765528225));
#81049=CARTESIAN_POINT('',(156.926729566011,-224.997190773455,16.7084234471774));
#81050=CARTESIAN_POINT('',(156.9265,-225.,22.2084234471774));
#81051=CARTESIAN_POINT('Ctrl Pts',(156.926729566011,-224.997190773455,16.7084234471775));
#81052=CARTESIAN_POINT('Ctrl Pts',(156.92445588536,-224.747111827224,16.6954742478977));
#81053=CARTESIAN_POINT('Ctrl Pts',(157.066706082429,-223.477592372542,16.6296057602074));
#81054=CARTESIAN_POINT('Ctrl Pts',(158.825551339689,-221.562284486778,16.5108179841064));
#81055=CARTESIAN_POINT('Ctrl Pts',(162.251073816965,-222.14870480692,16.3520601188746));
#81056=CARTESIAN_POINT('Ctrl Pts',(163.616413625555,-225.344630375999,16.1933022536428));
#81057=CARTESIAN_POINT('Ctrl Pts',(161.672011826211,-228.225150238345,16.034544388411));
#81058=CARTESIAN_POINT('Ctrl Pts',(158.197384869287,-228.154012729466,15.8757865231792));
#81059=CARTESIAN_POINT('Ctrl Pts',(156.947830997159,-226.12878059073,15.767079542768));
#81060=CARTESIAN_POINT('Ctrl Pts',(156.921489761883,-225.056164973894,15.7112918507675));
#81061=CARTESIAN_POINT('Ctrl Pts',(156.92172471093,-225.001003143772,15.7084234471775));
#81062=CARTESIAN_POINT('Ctrl Pts',(156.925641387687,-225.002754763835,16.7915765528225));
#81063=CARTESIAN_POINT('Ctrl Pts',(156.933090194617,-224.195641887624,16.7497459785925));
#81064=CARTESIAN_POINT('Ctrl Pts',(157.672221791135,-222.355388035489,16.6549961159518));
#81065=CARTESIAN_POINT('Ctrl Pts',(160.775745345963,-221.450995329772,16.5073269649006));
#81066=CARTESIAN_POINT('Ctrl Pts',(163.402355370953,-223.726739257298,16.3485690996688));
#81067=CARTESIAN_POINT('Ctrl Pts',(162.915129893092,-227.167771365402,16.189811234437));
#81068=CARTESIAN_POINT('Ctrl Pts',(159.759977652262,-228.624859205653,16.0310533692052));
#81069=CARTESIAN_POINT('Ctrl Pts',(157.305482029995,-227.069305626613,15.8983084753337));
#81070=CARTESIAN_POINT('Ctrl Pts',(156.931614374622,-225.521477261799,15.8184828698728));
#81071=CARTESIAN_POINT('Ctrl Pts',(156.931399319499,-224.999857957544,15.7915765528225));
#81072=CARTESIAN_POINT('Origin',(160.,-225.,22.2084234471774));
#81073=CARTESIAN_POINT('',(156.92234129012,-224.998416744957,17.7915765528225));
#81074=CARTESIAN_POINT('',(156.93124676379,-225.000725938288,17.7084234471774));
#81075=CARTESIAN_POINT('',(156.9265,-225.,22.2084234471774));
#81076=CARTESIAN_POINT('Ctrl Pts',(156.93124676379,-225.000725938288,17.7084234471775));
#81077=CARTESIAN_POINT('Ctrl Pts',(156.932425088148,-224.443107314068,17.679656645028));
#81078=CARTESIAN_POINT('Ctrl Pts',(157.344548556821,-222.858073213756,17.5979705544679));
#81079=CARTESIAN_POINT('Ctrl Pts',(159.887220510682,-221.3689535564,17.4633651754972));
#81080=CARTESIAN_POINT('Ctrl Pts',(162.989344456746,-222.935771972903,17.3046073102654));
#81081=CARTESIAN_POINT('Ctrl Pts',(163.355620479822,-226.391771827016,17.1458494450336));
#81082=CARTESIAN_POINT('Ctrl Pts',(160.650832768699,-228.574022146095,16.9870915798018));
#81083=CARTESIAN_POINT('Ctrl Pts',(157.619604864121,-227.574127701187,16.8412829138497));
#81084=CARTESIAN_POINT('Ctrl Pts',(156.933747700207,-225.769105511554,16.7483935363083));
#81085=CARTESIAN_POINT('Ctrl Pts',(156.926729566011,-224.997190773455,16.7084234471775));
#81086=CARTESIAN_POINT('Ctrl Pts',(156.92234129012,-224.998416744957,17.7915765528225));
#81087=CARTESIAN_POINT('Ctrl Pts',(156.92177007721,-224.907427920962,17.7868476641333));
#81088=CARTESIAN_POINT('Ctrl Pts',(156.966697439976,-223.798787972635,17.7291994870335));
#81089=CARTESIAN_POINT('Ctrl Pts',(158.309079915571,-221.784723458447,17.6186320215231));
#81090=CARTESIAN_POINT('Ctrl Pts',(161.784064171446,-221.835457356522,17.4598741562913));
#81091=CARTESIAN_POINT('Ctrl Pts',(163.626273157879,-224.782380735109,17.3011162910595));
#81092=CARTESIAN_POINT('Ctrl Pts',(162.149717001196,-227.928469170749,17.1423584258277));
#81093=CARTESIAN_POINT('Ctrl Pts',(158.705739973713,-228.394422777744,16.983600560596));
#81094=CARTESIAN_POINT('Ctrl Pts',(157.041609861784,-226.449569354426,16.8666732695942));
#81095=CARTESIAN_POINT('Ctrl Pts',(156.923666810657,-225.21670936906,16.8026652670031));
#81096=CARTESIAN_POINT('Ctrl Pts',(156.925641387687,-225.002754763835,16.7915765528225));
#81097=CARTESIAN_POINT('Origin',(160.,-225.,22.2084234471774));
#81098=CARTESIAN_POINT('',(156.93039533859,-224.998257313349,18.7915765528225));
#81099=CARTESIAN_POINT('',(156.924068591467,-225.002427532313,18.7084234471774));
#81100=CARTESIAN_POINT('',(156.9265,-225.,22.2084234471774));
#81101=CARTESIAN_POINT('Ctrl Pts',(156.924068591467,-225.002427532313,18.7084234471774));
#81102=CARTESIAN_POINT('Ctrl Pts',(156.931499764956,-224.143315612363,18.6638390421582));
#81103=CARTESIAN_POINT('Ctrl Pts',(157.753898913639,-222.252010296725,18.5663353487284));
#81104=CARTESIAN_POINT('Ctrl Pts',(160.95884158646,-221.496026267553,18.4159123668879));
#81105=CARTESIAN_POINT('Ctrl Pts',(163.463836160053,-223.904985354727,18.2571545016561));
#81106=CARTESIAN_POINT('Ctrl Pts',(162.798728517017,-227.31610406828,18.0983966364243));
#81107=CARTESIAN_POINT('Ctrl Pts',(159.572224403905,-228.607523337571,17.9396387711925));
#81108=CARTESIAN_POINT('Ctrl Pts',(157.250921105224,-226.961581956951,17.8096477081102));
#81109=CARTESIAN_POINT('Ctrl Pts',(156.930257447609,-225.468900193126,17.7325759334386));
#81110=CARTESIAN_POINT('Ctrl Pts',(156.93124676379,-225.000725938288,17.7084234471775));
#81111=CARTESIAN_POINT('Ctrl Pts',(156.93039533859,-224.998257313349,18.7915765528225));
#81112=CARTESIAN_POINT('Ctrl Pts',(156.9283328603,-224.600256690347,18.7710300612636));
#81113=CARTESIAN_POINT('Ctrl Pts',(157.185172027845,-223.179723982655,18.697564281294));
#81114=CARTESIAN_POINT('Ctrl Pts',(159.328201303672,-221.429869438357,18.5711792129139));
#81115=CARTESIAN_POINT('Ctrl Pts',(162.634953676974,-222.499153818262,18.4124213476821));
#81116=CARTESIAN_POINT('Ctrl Pts',(163.530211716637,-225.857226698665,18.2536634824503));
#81117=CARTESIAN_POINT('Ctrl Pts',(161.194612821702,-228.430758907163,18.0949056172185));
#81118=CARTESIAN_POINT('Ctrl Pts',(157.867843947502,-227.8813321041,17.9408766406759));
#81119=CARTESIAN_POINT('Ctrl Pts',(156.92816231495,-225.925651046016,17.8397669525439));
#81120=CARTESIAN_POINT('Ctrl Pts',(156.92234129012,-224.998416744957,17.7915765528225));
#81121=CARTESIAN_POINT('Origin',(160.,-225.,22.2084234471774));
#81122=CARTESIAN_POINT('',(156.929637641087,-225.003026239314,19.7915765528225));
#81123=CARTESIAN_POINT('',(156.923621975382,-224.997773684101,19.7084234471775));
#81124=CARTESIAN_POINT('',(156.9265,-225.,22.2084234471774));
#81125=CARTESIAN_POINT('',(159.206200717467,-227.969222953746,20.));
#81126=CARTESIAN_POINT('Ctrl Pts',(159.206200717467,-227.969222953746,20.));
#81127=CARTESIAN_POINT('Ctrl Pts',(158.218929051303,-227.70528334649,19.9470807115894));
#81128=CARTESIAN_POINT('Ctrl Pts',(157.120586512374,-226.663342975009,19.8776062291969));
#81129=CARTESIAN_POINT('Ctrl Pts',(156.927233104428,-225.32322870017,19.8081317468044));
#81130=CARTESIAN_POINT('Ctrl Pts',(156.929637641087,-225.003026239314,19.7915765528225));
#81131=CARTESIAN_POINT('',(160.795594448913,-227.974557142491,20.));
#81132=CARTESIAN_POINT('Origin',(160.,-225.,20.));
#81133=CARTESIAN_POINT('Ctrl Pts',(160.795596250783,-227.974562496599,20.));
#81134=CARTESIAN_POINT('Ctrl Pts',(159.833965257065,-228.230145509978,19.948244384658));
#81135=CARTESIAN_POINT('Ctrl Pts',(157.769883342468,-227.756381737407,19.8510522003838));
#81136=CARTESIAN_POINT('Ctrl Pts',(156.930816867245,-225.872804859128,19.7538600161097));
#81137=CARTESIAN_POINT('Ctrl Pts',(156.923621975382,-224.997773684101,19.7084234471775));
#81138=CARTESIAN_POINT('Origin',(0.,-225.,22.2084234471774));
#81139=CARTESIAN_POINT('',(-3.07861202077411,-224.999832022693,0.791576552822534));
#81140=CARTESIAN_POINT('',(-3.0685846317264,-224.999284761019,0.708423447177441));
#81141=CARTESIAN_POINT('',(-3.0735,-225.,22.2084234471774));
#81142=CARTESIAN_POINT('',(0.793799282532883,-227.969222953746,0.));
#81143=CARTESIAN_POINT('Ctrl Pts',(-3.0685846317264,-224.999284761019,0.708423447177441));
#81144=CARTESIAN_POINT('Ctrl Pts',(-3.06942175779765,-224.525030255484,
0.683959451760685));
#81145=CARTESIAN_POINT('Ctrl Pts',(-2.74289872526648,-223.026084056979,
0.606576167933331));
#81146=CARTESIAN_POINT('Ctrl Pts',(-0.407268923958301,-221.390844620734,
0.476273595695375));
#81147=CARTESIAN_POINT('Ctrl Pts',(2.81363672347351,-222.698855636535,0.317515730463589));
#81148=CARTESIAN_POINT('Ctrl Pts',(3.45438722685837,-226.118548219769,0.158757865231791));
#81149=CARTESIAN_POINT('Ctrl Pts',(1.7810709486973,-227.70528334649,0.0529192884105984));
#81150=CARTESIAN_POINT('Ctrl Pts',(0.793799282532894,-227.969222953746,
0.));
#81151=CARTESIAN_POINT('',(-0.79379928253288,-227.969222953746,0.));
#81152=CARTESIAN_POINT('Origin',(0.,-225.,0.));
#81153=CARTESIAN_POINT('Ctrl Pts',(-3.07861202077411,-224.999832022693,
0.791576552822534));
#81154=CARTESIAN_POINT('Ctrl Pts',(-3.07861796321176,-224.991641138211,
0.791150470866062));
#81155=CARTESIAN_POINT('Ctrl Pts',(-3.0748810844841,-223.966150069617,0.737805100498994));
#81156=CARTESIAN_POINT('Ctrl Pts',(-1.94583857424385,-221.93245816329,0.631540441721324));
#81157=CARTESIAN_POINT('Ctrl Pts',(1.52182610974532,-221.701128880727,0.472782576489534));
#81158=CARTESIAN_POINT('Ctrl Pts',(3.59659356700835,-224.489814123823,0.314024711257741));
#81159=CARTESIAN_POINT('Ctrl Pts',(2.38892380770087,-227.719767850893,0.156430519094562));
#81160=CARTESIAN_POINT('Ctrl Pts',(0.166093791691783,-228.230152288131,
0.0517556153419859));
#81161=CARTESIAN_POINT('Ctrl Pts',(-0.795579109021638,-227.974527535833,
5.47833805229769E-15));
#81162=CARTESIAN_POINT('Origin',(0.,-225.,22.2084234471774));
#81163=CARTESIAN_POINT('',(-3.07140453603582,-224.997418081988,1.79157655282252));
#81164=CARTESIAN_POINT('',(-3.0734003899706,-225.00280942625,1.70842344717744));
#81165=CARTESIAN_POINT('',(-3.0735,-225.,22.2084234471774));
#81166=CARTESIAN_POINT('Ctrl Pts',(-3.0734003899706,-225.00280942625,1.70842344717744));
#81167=CARTESIAN_POINT('Ctrl Pts',(-3.0662887666649,-224.225007664595,1.66814184889093));
#81168=CARTESIAN_POINT('Ctrl Pts',(-2.37168479031072,-222.414076548772,
1.57494096219383));
#81169=CARTESIAN_POINT('Ctrl Pts',(0.671786427681058,-221.42993104244,1.42882078708613));
#81170=CARTESIAN_POINT('Ctrl Pts',(3.36369894488889,-223.627956478202,1.27006292185434));
#81171=CARTESIAN_POINT('Ctrl Pts',(2.97708229266655,-227.081755146954,1.11130505662255));
#81172=CARTESIAN_POINT('Ctrl Pts',(-0.134013670091176,-228.630171025583,
0.952547191390754));
#81173=CARTESIAN_POINT('Ctrl Pts',(-2.66220315787947,-227.129884296831,
0.818253321575719));
#81174=CARTESIAN_POINT('Ctrl Pts',(-3.0676109286487,-225.55091382564,0.736878740171282));
#81175=CARTESIAN_POINT('Ctrl Pts',(-3.0685846317264,-224.999284761019,0.708423447177441));
#81176=CARTESIAN_POINT('Ctrl Pts',(-3.07140453603582,-224.997418081988,
1.79157655282252));
#81177=CARTESIAN_POINT('Ctrl Pts',(-3.07390614987845,-224.683249285408,
1.77533286799631));
#81178=CARTESIAN_POINT('Ctrl Pts',(-2.88509446209608,-223.348504675664,
1.70616989475949));
#81179=CARTESIAN_POINT('Ctrl Pts',(-0.958825609453758,-221.496084913414,
1.58408763311208));
#81180=CARTESIAN_POINT('Ctrl Pts',(2.42364543444732,-222.293943229063,1.42532976788028));
#81181=CARTESIAN_POINT('Ctrl Pts',(3.58799453273333,-225.568397245971,1.2665719026485));
#81182=CARTESIAN_POINT('Ctrl Pts',(1.46861470818642,-228.322628432602,1.1078140374167));
#81183=CARTESIAN_POINT('Ctrl Pts',(-1.98555300558023,-228.036811542638,
0.949482254141381));
#81184=CARTESIAN_POINT('Ctrl Pts',(-3.07787991371872,-226.008947249495,
0.844069759276661));
#81185=CARTESIAN_POINT('Ctrl Pts',(-3.07861202077411,-224.999832022693,
0.791576552822534));
#81186=CARTESIAN_POINT('Origin',(0.,-225.,22.2084234471774));
#81187=CARTESIAN_POINT('',(-3.0694574394746,-225.001668045267,2.79157655282253));
#81188=CARTESIAN_POINT('',(-3.07813805695758,-224.998894504048,2.70842344717744));
#81189=CARTESIAN_POINT('',(-3.0735,-225.,22.2084234471774));
#81190=CARTESIAN_POINT('Ctrl Pts',(-3.07813805695758,-224.998894504048,
2.70842344717744));
#81191=CARTESIAN_POINT('Ctrl Pts',(-3.07842163656956,-224.937738546132,
2.70524353443178));
#81192=CARTESIAN_POINT('Ctrl Pts',(-3.04905256116106,-223.859118502933,
2.64914433327553));
#81193=CARTESIAN_POINT('Ctrl Pts',(-1.78403472552871,-221.835509530578,
2.54012584370868));
#81194=CARTESIAN_POINT('Ctrl Pts',(1.69089215999812,-221.784776548785,2.38136797847689));
#81195=CARTESIAN_POINT('Ctrl Pts',(3.61831511248521,-224.676615388503,2.2226101132451));
#81196=CARTESIAN_POINT('Ctrl Pts',(2.23425519005939,-227.864416938342,2.0638522480133));
#81197=CARTESIAN_POINT('Ctrl Pts',(-1.19459291014185,-228.430701931157,
1.90509438278151));
#81198=CARTESIAN_POINT('Ctrl Pts',(-2.93755249238743,-226.510184003648,
1.78661811583622));
#81199=CARTESIAN_POINT('Ctrl Pts',(-3.07563154502501,-225.246831959117,
1.72106113730153));
#81200=CARTESIAN_POINT('Ctrl Pts',(-3.0734003899706,-225.00280942625,1.70842344717744));
#81201=CARTESIAN_POINT('Ctrl Pts',(-3.0694574394746,-225.001668045267,2.79157655282253));
#81202=CARTESIAN_POINT('Ctrl Pts',(-3.06639637311186,-224.380581303629,
2.75951526512656));
#81203=CARTESIAN_POINT('Ctrl Pts',(-2.58173685518177,-222.729957206475,
2.67453468902));
#81204=CARTESIAN_POINT('Ctrl Pts',(0.112777615932726,-221.369013886482,
2.53663482450283));
#81205=CARTESIAN_POINT('Ctrl Pts',(3.11163596998505,-223.125299771423,2.37787695927105));
#81206=CARTESIAN_POINT('Ctrl Pts',(3.26272518188304,-226.597311412118,2.21911909403925));
#81207=CARTESIAN_POINT('Ctrl Pts',(0.427768485964111,-228.607463345116,
2.06036122880746));
#81208=CARTESIAN_POINT('Ctrl Pts',(-2.46856013316054,-227.448198100151,
1.91784704840188));
#81209=CARTESIAN_POINT('Ctrl Pts',(-3.06575629805317,-225.706760227272,
1.8282521564069));
#81210=CARTESIAN_POINT('Ctrl Pts',(-3.07140453603582,-224.997418081988,
1.79157655282252));
#81211=CARTESIAN_POINT('Origin',(0.,-225.,22.2084234471774));
#81212=CARTESIAN_POINT('',(-3.07748283886488,-225.001672003054,3.79157655282253));
#81213=CARTESIAN_POINT('',(-3.07013331070642,-224.99789255212,3.70842344717744));
#81214=CARTESIAN_POINT('',(-3.0735,-225.,22.2084234471774));
#81215=CARTESIAN_POINT('Ctrl Pts',(-3.07013331070642,-224.99789255212,3.70842344717744));
#81216=CARTESIAN_POINT('Ctrl Pts',(-3.07245614163896,-224.630078505823,
3.68942593156204));
#81217=CARTESIAN_POINT('Ctrl Pts',(-2.84108107627447,-223.240510367213,
3.61750912753603));
#81218=CARTESIAN_POINT('Ctrl Pts',(-0.775732549268024,-221.451053872185,
3.49267303509943));
#81219=CARTESIAN_POINT('Ctrl Pts',(2.56078454381028,-222.423342844173,3.33391516986764));
#81220=CARTESIAN_POINT('Ctrl Pts',(3.55367173029338,-225.753788335947,3.17515730463585));
#81221=CARTESIAN_POINT('Ctrl Pts',(1.29423867433457,-228.394366788354,3.01639943940406));
#81222=CARTESIAN_POINT('Ctrl Pts',(-2.08069997222285,-227.93775373254,2.86082148691792));
#81223=CARTESIAN_POINT('Ctrl Pts',(-3.07370237774903,-225.955480237129,
2.75816282284238));
#81224=CARTESIAN_POINT('Ctrl Pts',(-3.07813805695758,-224.998894504048,
2.70842344717744));
#81225=CARTESIAN_POINT('Ctrl Pts',(-3.07748283886488,-225.001672003054,
3.79157655282253));
#81226=CARTESIAN_POINT('Ctrl Pts',(-3.07143809346347,-224.080348034814,
3.74369766225681));
#81227=CARTESIAN_POINT('Ctrl Pts',(-2.1422814352906,-222.130134246004,3.6428994832805));
#81228=CARTESIAN_POINT('Ctrl Pts',(1.17442914948988,-221.562341596822,3.48918201589359));
#81229=CARTESIAN_POINT('Ctrl Pts',(3.52505720816877,-224.122075853096,3.3304241506618));
#81230=CARTESIAN_POINT('Ctrl Pts',(2.64955304819789,-227.485286256663,3.17166628543001));
#81231=CARTESIAN_POINT('Ctrl Pts',(-0.650821956575191,-228.573962770645,
3.01290842019821));
#81232=CARTESIAN_POINT('Ctrl Pts',(-2.80933959903191,-226.832448718571,
2.88621184266239));
#81233=CARTESIAN_POINT('Ctrl Pts',(-3.07144886679926,-225.405726292203,
2.81243455353716));
#81234=CARTESIAN_POINT('Ctrl Pts',(-3.0694574394746,-225.001668045267,2.79157655282253));
#81235=CARTESIAN_POINT('Origin',(0.,-225.,22.2084234471774));
#81236=CARTESIAN_POINT('',(-3.07449021712595,-224.997267710685,4.79157655282253));
#81237=CARTESIAN_POINT('',(-3.07051359504914,-225.002286482744,4.70842344717744));
#81238=CARTESIAN_POINT('',(-3.0735,-225.,22.2084234471774));
#81239=CARTESIAN_POINT('Ctrl Pts',(-3.07051359504914,-225.002286482744,
4.70842344717744));
#81240=CARTESIAN_POINT('Ctrl Pts',(-3.0658581317049,-224.328435086706,4.67360832869229));
#81241=CARTESIAN_POINT('Ctrl Pts',(-2.51562439385663,-222.623410166854,
4.58587392179654));
#81242=CARTESIAN_POINT('Ctrl Pts',(0.301020087018748,-221.379756015497,
4.44522022649019));
#81243=CARTESIAN_POINT('Ctrl Pts',(3.20471397929018,-223.289272695415,4.2864623612584));
#81244=CARTESIAN_POINT('Ctrl Pts',(3.17545376384016,-226.764446937104,4.1277044960266));
#81245=CARTESIAN_POINT('Ctrl Pts',(0.240018388386984,-228.624799411569,
3.96894663079481));
#81246=CARTESIAN_POINT('Ctrl Pts',(-2.53753159714771,-227.342092904446,
3.82918628117842));
#81247=CARTESIAN_POINT('Ctrl Pts',(-3.0659856871576,-225.654657613507,3.74234521997263));
#81248=CARTESIAN_POINT('Ctrl Pts',(-3.07013331070642,-224.99789255212,3.70842344717744));
#81249=CARTESIAN_POINT('Ctrl Pts',(-3.07449021712595,-224.997267710685,
4.79157655282253));
#81250=CARTESIAN_POINT('Ctrl Pts',(-3.07640550402147,-224.789358748543,
4.78079934779766));
#81251=CARTESIAN_POINT('Ctrl Pts',(-2.96239880943811,-223.562643093719,
4.7171028543622));
#81252=CARTESIAN_POINT('Ctrl Pts',(-1.31414730730727,-221.61329127598,4.60048707251613));
#81253=CARTESIAN_POINT('Ctrl Pts',(2.13244942587199,-222.059007213082,4.44172920728434));
#81254=CARTESIAN_POINT('Ctrl Pts',(3.62742852835224,-225.196319633101,4.28297134205255));
#81255=CARTESIAN_POINT('Ctrl Pts',(1.80258518432463,-228.153960332663,4.12421347682076));
#81256=CARTESIAN_POINT('Ctrl Pts',(-1.67198404950171,-228.225096659724,
3.96545561158897));
#81257=CARTESIAN_POINT('Ctrl Pts',(-3.02996209952885,-226.213329983221,
3.85457663692289));
#81258=CARTESIAN_POINT('Ctrl Pts',(-3.0781191928266,-225.098663376268,3.79661695066741));
#81259=CARTESIAN_POINT('Ctrl Pts',(-3.07748283886488,-225.001672003054,
3.79157655282253));
#81260=CARTESIAN_POINT('Origin',(0.,-225.,22.2084234471774));
#81261=CARTESIAN_POINT('',(-3.06854459837578,-225.000042997605,5.79157655282253));
#81262=CARTESIAN_POINT('',(-3.0783646865402,-225.000807299621,5.70842344717745));
#81263=CARTESIAN_POINT('',(-3.0735,-225.,22.2084234471774));
#81264=CARTESIAN_POINT('Ctrl Pts',(-3.0783646865402,-225.000807299621,5.70842344717745));
#81265=CARTESIAN_POINT('Ctrl Pts',(-3.07494744526968,-224.027231919385,
5.65779072582254));
#81266=CARTESIAN_POINT('Ctrl Pts',(-2.0503586705405,-222.029922382093,5.55423871605704));
#81267=CARTESIAN_POINT('Ctrl Pts',(1.35121080771192,-221.627907333254,5.39776741788095));
#81268=CARTESIAN_POINT('Ctrl Pts',(3.56586047257395,-224.306156580971,5.23900955264915));
#81269=CARTESIAN_POINT('Ctrl Pts',(2.51703477316183,-227.619411298497,5.08025168741736));
#81270=CARTESIAN_POINT('Ctrl Pts',(-0.835381051670971,-228.535380898648,
4.92149382218557));
#81271=CARTESIAN_POINT('Ctrl Pts',(-2.85574300376166,-226.724453667661,
4.79755107543892));
#81272=CARTESIAN_POINT('Ctrl Pts',(-3.07293447721565,-225.352695176127,
4.72652761710288));
#81273=CARTESIAN_POINT('Ctrl Pts',(-3.07051359504914,-225.002286482744,
4.70842344717744));
#81274=CARTESIAN_POINT('Ctrl Pts',(-3.06854459837578,-225.000042997605,
5.79157655282253));
#81275=CARTESIAN_POINT('Ctrl Pts',(-3.06848025913913,-224.484469012775,
5.76498174492791));
#81276=CARTESIAN_POINT('Ctrl Pts',(-2.70083904555456,-222.942901484278,
5.6854676486227));
#81277=CARTESIAN_POINT('Ctrl Pts',(-0.261298254542071,-221.376672475636,
5.5530342639069));
#81278=CARTESIAN_POINT('Ctrl Pts',(2.90230304443695,-222.815185095966,5.3942763986751));
#81279=CARTESIAN_POINT('Ctrl Pts',(3.40971671127761,-226.253240230551,5.23551853344331));
#81280=CARTESIAN_POINT('Ctrl Pts',(0.796557778040768,-228.54432995542,5.07676066821151));
#81281=CARTESIAN_POINT('Ctrl Pts',(-2.31872921781764,-227.656321352104,
4.92878000800459));
#81282=CARTESIAN_POINT('Ctrl Pts',(-3.06700087458563,-225.810253712066,
4.83371863620826));
#81283=CARTESIAN_POINT('Ctrl Pts',(-3.07449021712595,-224.997267710685,
4.79157655282253));
#81284=CARTESIAN_POINT('Origin',(0.,-225.,22.2084234471774));
#81285=CARTESIAN_POINT('',(-3.07464802069915,-225.002709732222,6.79157655282253));
#81286=CARTESIAN_POINT('',(-3.07288410079718,-224.997201521015,6.70842344717745));
#81287=CARTESIAN_POINT('',(-3.0735,-225.,22.2084234471774));
#81288=CARTESIAN_POINT('Ctrl Pts',(-3.07288410079718,-224.997201521015,
6.70842344717745));
#81289=CARTESIAN_POINT('Ctrl Pts',(-3.07522873674104,-224.735817594879,
6.69489241136339));
#81290=CARTESIAN_POINT('Ctrl Pts',(-2.92508990676295,-223.454826085153,
6.62844208713874));
#81291=CARTESIAN_POINT('Ctrl Pts',(-1.13665725625273,-221.549668149031,
6.50907247450349));
#81292=CARTESIAN_POINT('Ctrl Pts',(2.2821711173499,-222.173611033291,6.35031460927169));
#81293=CARTESIAN_POINT('Ctrl Pts',(3.61235657409808,-225.384264988738,6.19155674403991));
#81294=CARTESIAN_POINT('Ctrl Pts',(1.63651343628419,-228.243239641602,6.03279887880811));
#81295=CARTESIAN_POINT('Ctrl Pts',(-1.83706673406269,-228.13400150201,5.87404101357632));
#81296=CARTESIAN_POINT('Ctrl Pts',(-3.05774544236497,-226.106133206661,
5.76591586969943));
#81297=CARTESIAN_POINT('Ctrl Pts',(-3.0785190087078,-225.044773836104,5.71071001423314));
#81298=CARTESIAN_POINT('Ctrl Pts',(-3.0783646865402,-225.000807299621,5.70842344717745));
#81299=CARTESIAN_POINT('Ctrl Pts',(-3.07464802069915,-225.002709732222,
6.79157655282254));
#81300=CARTESIAN_POINT('Ctrl Pts',(-3.06713149317871,-224.184616738264,
6.74916414205817));
#81301=CARTESIAN_POINT('Ctrl Pts',(-2.31086287355762,-222.333491153698,
6.65383244288321));
#81302=CARTESIAN_POINT('Ctrl Pts',(0.814607672933798,-221.459774941358,
6.50558145529765));
#81303=CARTESIAN_POINT('Ctrl Pts',(3.41605836726569,-223.76415034973,6.34682359006585));
#81304=CARTESIAN_POINT('Ctrl Pts',(2.89113257820927,-227.19957530943,6.18806572483406));
#81305=CARTESIAN_POINT('Ctrl Pts',(-0.279757632733263,-228.621949032436,
6.02930785960227));
#81306=CARTESIAN_POINT('Ctrl Pts',(-2.70632267198121,-227.046531976909,
5.89714480226509));
#81307=CARTESIAN_POINT('Ctrl Pts',(-3.06860828362547,-225.510376344323,
5.81790103333851));
#81308=CARTESIAN_POINT('Ctrl Pts',(-3.06854459837578,-225.000042997605,
5.79157655282253));
#81309=CARTESIAN_POINT('Origin',(0.,-225.,22.2084234471774));
#81310=CARTESIAN_POINT('',(-3.07736989982489,-224.998253130058,7.79157655282253));
#81311=CARTESIAN_POINT('',(-3.06879157690567,-225.000903264851,7.70842344717744));
#81312=CARTESIAN_POINT('',(-3.0735,-225.,22.2084234471774));
#81313=CARTESIAN_POINT('Ctrl Pts',(-3.06879157690567,-225.000903264851,
7.70842344717744));
#81314=CARTESIAN_POINT('Ctrl Pts',(-3.06729326924488,-224.432057018653,
7.67907480849364));
#81315=CARTESIAN_POINT('Ctrl Pts',(-2.64281778869516,-222.835431117709,
7.59680688139924));
#81316=CARTESIAN_POINT('Ctrl Pts',(-0.0729493032098818,-221.367995319502,
7.46161966589424));
#81317=CARTESIAN_POINT('Ctrl Pts',(3.01175337487511,-222.968714395038,7.30286180066245));
#81318=CARTESIAN_POINT('Ctrl Pts',(3.34009948270872,-226.428465976356,7.14410393543066));
#81319=CARTESIAN_POINT('Ctrl Pts',(0.611586675313532,-228.580885552287,
6.98534607019887));
#81320=CARTESIAN_POINT('Ctrl Pts',(-2.39639166901593,-227.551946819569,
6.84011924078113));
#81321=CARTESIAN_POINT('Ctrl Pts',(-3.06605896825943,-225.758078681403,
6.74781169977399));
#81322=CARTESIAN_POINT('Ctrl Pts',(-3.07288410079718,-224.997201521015,
6.70842344717745));
#81323=CARTESIAN_POINT('Ctrl Pts',(-3.07736989982489,-224.998253130058,
7.79157655282253));
#81324=CARTESIAN_POINT('Ctrl Pts',(-3.07806429383697,-224.896050021069,
7.78626582759902));
#81325=CARTESIAN_POINT('Ctrl Pts',(-3.02707595981422,-223.776134342622,
7.7280358139649));
#81326=CARTESIAN_POINT('Ctrl Pts',(-1.655528769796,-221.766425566186,7.6168865119202));
#81327=CARTESIAN_POINT('Ctrl Pts',(1.81863287894903,-221.855265738056,7.4581286466884));
#81328=CARTESIAN_POINT('Ctrl Pts',(3.62838178839593,-224.822166582794,7.29937078145661));
#81329=CARTESIAN_POINT('Ctrl Pts',(2.11743582778552,-227.951820563965,7.14061291622481));
#81330=CARTESIAN_POINT('Ctrl Pts',(-1.33138731914806,-228.379968481073,
6.98185505099303));
#81331=CARTESIAN_POINT('Ctrl Pts',(-2.96588670322775,-226.426781465541,
6.8655095965256));
#81332=CARTESIAN_POINT('Ctrl Pts',(-3.07651009912286,-225.205376895815,
6.80208343046877));
#81333=CARTESIAN_POINT('Ctrl Pts',(-3.07464802069915,-225.002709732222,
6.79157655282254));
#81334=CARTESIAN_POINT('Origin',(0.,-225.,22.2084234471774));
#81335=CARTESIAN_POINT('',(-3.06937338025089,-224.998402365976,8.79157655282253));
#81336=CARTESIAN_POINT('',(-3.07619355237033,-225.002319527513,8.70842344717744));
#81337=CARTESIAN_POINT('',(-3.0735,-225.,22.2084234471774));
#81338=CARTESIAN_POINT('Ctrl Pts',(-3.07619355237033,-225.002319527513,
8.70842344717744));
#81339=CARTESIAN_POINT('Ctrl Pts',(-3.06888768878592,-224.132240268067,
8.66325720562389));
#81340=CARTESIAN_POINT('Ctrl Pts',(-2.22821896698895,-222.230378726602,
8.56517167565974));
#81341=CARTESIAN_POINT('Ctrl Pts',(0.997195673100731,-221.506809425532,
8.414166857285));
#81342=CARTESIAN_POINT('Ctrl Pts',(3.47557947438652,-223.943057751236,8.2554089920532));
#81343=CARTESIAN_POINT('Ctrl Pts',(2.7731130773876,-227.346619581445,8.09665112682141));
#81344=CARTESIAN_POINT('Ctrl Pts',(-0.467306298986418,-228.602555262994,
7.93789326158962));
#81345=CARTESIAN_POINT('Ctrl Pts',(-2.76007204034179,-226.938762943595,
7.80848403504163));
#81346=CARTESIAN_POINT('Ctrl Pts',(-3.06999490648549,-225.457758377008,
7.73199409690424));
#81347=CARTESIAN_POINT('Ctrl Pts',(-3.06879157690567,-225.000903264851,
7.70842344717744));
#81348=CARTESIAN_POINT('Ctrl Pts',(-3.06937338025089,-224.998402365975,
8.79157655282253));
#81349=CARTESIAN_POINT('Ctrl Pts',(-3.07130231416634,-224.589079310054,
8.77044822472927));
#81350=CARTESIAN_POINT('Ctrl Pts',(-2.8045902474645,-223.156952286025,8.6964006082254));
#81351=CARTESIAN_POINT('Ctrl Pts',(-0.632602276895449,-221.422767342497,
8.56943370331095));
#81352=CARTESIAN_POINT('Ctrl Pts',(2.6621824992875,-222.528246883865,8.41067583807915));
#81353=CARTESIAN_POINT('Ctrl Pts',(3.52053795681035,-225.89587477992,8.25191797284737));
#81354=CARTESIAN_POINT('Ctrl Pts',(1.15689721470216,-228.443598112622,8.09316010761557));
#81355=CARTESIAN_POINT('Ctrl Pts',(-2.15104950765063,-227.859940666864,
7.93971296760729));
#81356=CARTESIAN_POINT('Ctrl Pts',(-3.07114493057695,-225.914463810798,
7.83918511600961));
#81357=CARTESIAN_POINT('Ctrl Pts',(-3.07736989982489,-224.998253130058,
7.79157655282253));
#81358=CARTESIAN_POINT('Origin',(0.,-225.,22.2084234471774));
#81359=CARTESIAN_POINT('',(-3.0715437315608,-225.002615101916,9.79157655282254));
#81360=CARTESIAN_POINT('',(-3.07602729093121,-224.997622070323,9.70842344717745));
#81361=CARTESIAN_POINT('',(-3.0735,-225.,22.2084234471774));
#81362=CARTESIAN_POINT('Ctrl Pts',(-3.07602729093122,-224.997622070323,
9.70842344717744));
#81363=CARTESIAN_POINT('Ctrl Pts',(-3.0773539235959,-224.842245191388,9.70035889116474));
#81364=CARTESIAN_POINT('Ctrl Pts',(-2.99601734532136,-223.668684684651,
9.63937504674144));
#81365=CARTESIAN_POINT('Ctrl Pts',(-1.48552430373511,-221.684883540053,
9.52547191390755));
#81366=CARTESIAN_POINT('Ctrl Pts',(1.97934842100312,-221.953861554645,9.36671404867575));
#81367=CARTESIAN_POINT('Ctrl Pts',(3.63272154867527,-225.010665354639,9.20795618344396));
#81368=CARTESIAN_POINT('Ctrl Pts',(1.96142805785311,-228.057708222487,9.04919831821216));
#81369=CARTESIAN_POINT('Ctrl Pts',(-1.50496431438492,-228.306336645357,
8.89044045298038));
#81370=CARTESIAN_POINT('Ctrl Pts',(-2.99968382218232,-226.319150005193,
8.77684882930213));
#81371=CARTESIAN_POINT('Ctrl Pts',(-3.07744764615261,-225.151673669807,
8.71617649403449));
#81372=CARTESIAN_POINT('Ctrl Pts',(-3.07619355237033,-225.002319527513,
8.70842344717744));
#81373=CARTESIAN_POINT('Ctrl Pts',(-3.0715437315608,-225.002615101916,9.79157655282254));
#81374=CARTESIAN_POINT('Ctrl Pts',(-3.0657613572303,-224.288126470754,9.75463062185952));
#81375=CARTESIAN_POINT('Ctrl Pts',(-2.4615581954256,-222.541426343529,9.66476540248591));
#81376=CARTESIAN_POINT('Ctrl Pts',(0.446144839320715,-221.394762988514,
9.5219808947017));
#81377=CARTESIAN_POINT('Ctrl Pts',(3.27082198427282,-223.419334736943,9.36322302946992));
#81378=CARTESIAN_POINT('Ctrl Pts',(3.1020429778404,-226.890531271963,9.20446516423812));
#81379=CARTESIAN_POINT('Ctrl Pts',(0.0942743600733127,-228.631513661226,
9.04570729900632));
#81380=CARTESIAN_POINT('Ctrl Pts',(-2.58800196981665,-227.259552761042,
8.9080777618678));
#81381=CARTESIAN_POINT('Ctrl Pts',(-3.06647098961733,-225.614294592295,
8.82336751313987));
#81382=CARTESIAN_POINT('Ctrl Pts',(-3.06937338025089,-224.998402365975,
8.79157655282253));
#81383=CARTESIAN_POINT('Origin',(0.,-225.,22.2084234471774));
#81384=CARTESIAN_POINT('',(-3.0786228608021,-225.000055941039,10.7915765528225));
#81385=CARTESIAN_POINT('',(-3.06874135342515,-224.999191262945,10.7084234471775));
#81386=CARTESIAN_POINT('',(-3.0735,-225.,22.2084234471774));
#81387=CARTESIAN_POINT('Ctrl Pts',(-3.06874135342515,-224.999191262945,
10.7084234471774));
#81388=CARTESIAN_POINT('Ctrl Pts',(-3.06983198124641,-224.536279450012,
10.684541288295));
#81389=CARTESIAN_POINT('Ctrl Pts',(-2.75418296187546,-223.049036499641,
10.607739841002));
#81390=CARTESIAN_POINT('Ctrl Pts',(-0.446144847322243,-221.394762923856,
10.4780191052983));
#81391=CARTESIAN_POINT('Ctrl Pts',(2.78684409501469,-222.669703969432,10.3192612400665));
#81392=CARTESIAN_POINT('Ctrl Pts',(3.46931343118415,-226.077331850548,10.1605033748347));
#81393=CARTESIAN_POINT('Ctrl Pts',(0.976667251561304,-228.498985664407,
10.0017455096029));
#81394=CARTESIAN_POINT('Ctrl Pts',(-2.23779829231897,-227.758021627206,
9.85105220038384));
#81395=CARTESIAN_POINT('Ctrl Pts',(-3.06864861403061,-225.861821948715,
9.75327817957534));
#81396=CARTESIAN_POINT('Ctrl Pts',(-3.07602729093122,-224.997622070323,
9.70842344717744));
#81397=CARTESIAN_POINT('Ctrl Pts',(-3.07862236853609,-225.000055935664,
10.7915765528225));
#81398=CARTESIAN_POINT('Ctrl Pts',(-3.07835031097462,-223.985736843864,
10.7388130189898));
#81399=CARTESIAN_POINT('Ctrl Pts',(-1.97594905925326,-221.953597719633,
10.6331301967464));
#81400=CARTESIAN_POINT('Ctrl Pts',(1.48552427709262,-221.684883599509,10.4745280860925));
#81401=CARTESIAN_POINT('Ctrl Pts',(3.59084517971103,-224.449899989107,10.3157702208607));
#81402=CARTESIAN_POINT('Ctrl Pts',(2.40982471506444,-227.718367887042,10.1570123556289));
#81403=CARTESIAN_POINT('Ctrl Pts',(-0.97666723404505,-228.498985601654,
9.99825449039707));
#81404=CARTESIAN_POINT('Ctrl Pts',(-2.88922789173994,-226.640896054566,
9.8764425561283));
#81405=CARTESIAN_POINT('Ctrl Pts',(-3.07404370732726,-225.311520088211,
9.80754991027012));
#81406=CARTESIAN_POINT('Ctrl Pts',(-3.0715437315608,-225.002615101916,9.79157655282254));
#81407=CARTESIAN_POINT('Origin',(0.,-225.,22.2084234471774));
#81408=CARTESIAN_POINT('',(-3.07170674492633,-224.997349498083,11.7915765528225));
#81409=CARTESIAN_POINT('',(-3.07306312169136,-225.002805832536,11.7084234471775));
#81410=CARTESIAN_POINT('',(-3.0735,-225.,22.2084234471774));
#81411=CARTESIAN_POINT('Ctrl Pts',(-3.07306312169136,-225.002805832536,
11.7084234471775));
#81412=CARTESIAN_POINT('Ctrl Pts',(-3.06613162486477,-224.236024983951,
11.6687236854253));
#81413=CARTESIAN_POINT('Ctrl Pts',(-2.38783081082145,-222.436195233095,
11.5761046352625));
#81414=CARTESIAN_POINT('Ctrl Pts',(0.632602288240958,-221.42276727834,11.430566296689));
#81415=CARTESIAN_POINT('Ctrl Pts',(3.34842953419328,-223.591170963338,11.2718084314573));
#81416=CARTESIAN_POINT('Ctrl Pts',(2.99977420212569,-227.048934927288,11.1130505662255));
#81417=CARTESIAN_POINT('Ctrl Pts',(-0.0942743617640601,-228.631513726356,
10.9542927009937));
#81418=CARTESIAN_POINT('Ctrl Pts',(-2.64958035268347,-227.152429629564,
10.8194169946443));
#81419=CARTESIAN_POINT('Ctrl Pts',(-3.06741531328495,-225.562022719616,
10.7374605767056));
#81420=CARTESIAN_POINT('Ctrl Pts',(-3.06874135342515,-224.999191262945,
10.7084234471774));
#81421=CARTESIAN_POINT('Ctrl Pts',(-3.07170674492633,-224.997349498083,
11.7915765528225));
#81422=CARTESIAN_POINT('Ctrl Pts',(-3.07420079038922,-224.694509382875,
11.7759147045306));
#81423=CARTESIAN_POINT('Ctrl Pts',(-2.89395005922289,-223.371316808894,
11.7073335678281));
#81424=CARTESIAN_POINT('Ctrl Pts',(-0.997195655216347,-221.506809488182,
11.585833142715));
#81425=CARTESIAN_POINT('Ctrl Pts',(2.39382152606057,-222.267529025221,11.4270752774832));
#81426=CARTESIAN_POINT('Ctrl Pts',(3.5940133408216,-225.529005890927,11.2683174122514));
#81427=CARTESIAN_POINT('Ctrl Pts',(1.50496428739385,-228.306336586058,11.1095595470196));
#81428=CARTESIAN_POINT('Ctrl Pts',(-1.96142802267546,-228.057708167648,
10.9508016817878));
#81429=CARTESIAN_POINT('Ctrl Pts',(-3.07726334016045,-226.023356891522,
10.8448073503888));
#81430=CARTESIAN_POINT('Ctrl Pts',(-3.07862317163262,-225.003050140761,
10.7917323074004));
#81431=CARTESIAN_POINT('Ctrl Pts',(-3.07862236853609,-225.000055935664,
10.7915765528225));
#81432=CARTESIAN_POINT('Origin',(0.,-225.,22.2084234471774));
#81433=CARTESIAN_POINT('',(-3.06928120376705,-225.001514673646,12.7915765528225));
#81434=CARTESIAN_POINT('',(-3.07829286865601,-224.999087154577,12.7084234471774));
#81435=CARTESIAN_POINT('',(-3.0735,-225.,22.2084234471774));
#81436=CARTESIAN_POINT('Ctrl Pts',(-3.07829286865601,-224.999087154577,
12.7084234471774));
#81437=CARTESIAN_POINT('Ctrl Pts',(-3.07848862305667,-224.949127749583,
12.7058253709661));
#81438=CARTESIAN_POINT('Ctrl Pts',(-3.05474879031452,-223.881753016838,
12.6503080063441));
#81439=CARTESIAN_POINT('Ctrl Pts',(-1.81863291156572,-221.855265681656,
12.5418713533116));
#81440=CARTESIAN_POINT('Ctrl Pts',(1.65552879948739,-221.766425508193,12.3831134880798));
#81441=CARTESIAN_POINT('Ctrl Pts',(3.61455061835174,-224.636952582474,12.224355622848));
#81442=CARTESIAN_POINT('Ctrl Pts',(2.26553585343932,-227.839740638999,12.0655977576162));
#81443=CARTESIAN_POINT('Ctrl Pts',(-1.15689723545072,-228.443598174382,
11.9068398923844));
#81444=CARTESIAN_POINT('Ctrl Pts',(-2.92947454176964,-226.532970860394,
11.7877817889048));
#81445=CARTESIAN_POINT('Ctrl Pts',(-3.07537122388234,-225.258134313656,
11.7216429738359));
#81446=CARTESIAN_POINT('Ctrl Pts',(-3.07306312169136,-225.002805832536,
11.7084234471775));
#81447=CARTESIAN_POINT('Ctrl Pts',(-3.06928120376705,-225.001514673646,
12.7915765528225));
#81448=CARTESIAN_POINT('Ctrl Pts',(-3.06656132439523,-224.391611531572,
12.7600971016609));
#81449=CARTESIAN_POINT('Ctrl Pts',(-2.59517224566867,-222.752541482839,
12.6756983620886));
#81450=CARTESIAN_POINT('Ctrl Pts',(0.0729493019015324,-221.367995384641,
12.5383803341057));
#81451=CARTESIAN_POINT('Ctrl Pts',(3.09088872643165,-223.091286818965,12.379622468874));
#81452=CARTESIAN_POINT('Ctrl Pts',(3.28004691007777,-226.561432481514,12.2208646036422));
#81453=CARTESIAN_POINT('Ctrl Pts',(0.467306290605433,-228.602555198383,
12.0621067384104));
#81454=CARTESIAN_POINT('Ctrl Pts',(-2.45343780595167,-227.470520636967,
11.9190107214705));
#81455=CARTESIAN_POINT('Ctrl Pts',(-3.06577374469831,-225.717765584843,
11.8288339929412));
#81456=CARTESIAN_POINT('Ctrl Pts',(-3.07170674492633,-224.997349498083,
11.7915765528225));
#81457=CARTESIAN_POINT('Origin',(0.,-225.,22.2084234471774));
#81458=CARTESIAN_POINT('',(-3.07723488309734,-225.001830508734,13.7915765528225));
#81459=CARTESIAN_POINT('',(-3.07037718038997,-224.997773372826,13.7084234471775));
#81460=CARTESIAN_POINT('',(-3.0735,-225.,22.2084234471774));
#81461=CARTESIAN_POINT('Ctrl Pts',(-3.07037718038997,-224.997773372826,
13.7084234471775));
#81462=CARTESIAN_POINT('Ctrl Pts',(-3.07276832859184,-224.641295536,13.6900077680964));
#81463=CARTESIAN_POINT('Ctrl Pts',(-2.8506726448042,-223.26332934368,13.6186728006047));
#81464=CARTESIAN_POINT('Ctrl Pts',(-0.814607687543583,-221.459774877865,
13.4944185447024));
#81465=CARTESIAN_POINT('Ctrl Pts',(2.53237197705076,-222.395413320727,13.3356606794706));
#81466=CARTESIAN_POINT('Ctrl Pts',(3.56172490783136,-225.714769390036,13.1769028142388));
#81467=CARTESIAN_POINT('Ctrl Pts',(1.33138734302612,-228.379968541692,13.018144949007));
#81468=CARTESIAN_POINT('Ctrl Pts',(-2.06099579255385,-227.958827267799,
12.8619851599865));
#81469=CARTESIAN_POINT('Ctrl Pts',(-3.07450137143537,-225.966733064678,
12.7587446593767));
#81470=CARTESIAN_POINT('Ctrl Pts',(-3.07829286865601,-224.999087154577,
12.7084234471774));
#81471=CARTESIAN_POINT('Ctrl Pts',(-3.07723488309734,-225.001830508734,
13.7915765528225));
#81472=CARTESIAN_POINT('Ctrl Pts',(-3.07081808206618,-224.091509657493,
13.7442794987911));
#81473=CARTESIAN_POINT('Ctrl Pts',(-2.16109704934214,-222.151514836552,
13.6440631563491));
#81474=CARTESIAN_POINT('Ctrl Pts',(1.13665723586709,-221.549668210912,13.4909275254965));
#81475=CARTESIAN_POINT('Ctrl Pts',(3.51521689058642,-224.083468855535,13.3321696602647));
#81476=CARTESIAN_POINT('Ctrl Pts',(2.67665018527361,-227.45607876753,13.1734117950329));
#81477=CARTESIAN_POINT('Ctrl Pts',(-0.611586664344894,-228.580885488065,
13.0146539298011));
#81478=CARTESIAN_POINT('Ctrl Pts',(-2.79907372937866,-226.855260463285,
12.887375515731));
#81479=CARTESIAN_POINT('Ctrl Pts',(-3.07113364302239,-225.416903875844,
12.8130163900715));
#81480=CARTESIAN_POINT('Ctrl Pts',(-3.06928120376705,-225.001514673646,
12.7915765528225));
#81481=CARTESIAN_POINT('Origin',(0.,-225.,22.2084234471774));
#81482=CARTESIAN_POINT('',(-3.07482911963311,-224.997319814409,14.7915765528225));
#81483=CARTESIAN_POINT('',(-3.07026207039166,-225.002172427921,14.7084234471775));
#81484=CARTESIAN_POINT('',(-3.0735,-225.,22.2084234471774));
#81485=CARTESIAN_POINT('Ctrl Pts',(-3.07026207039166,-225.002172427921,
14.7084234471775));
#81486=CARTESIAN_POINT('Ctrl Pts',(-3.06593576340553,-224.339446029993,
14.6741901652266));
#81487=CARTESIAN_POINT('Ctrl Pts',(-2.52994311745615,-222.645870254276,
14.5870375948652));
#81488=CARTESIAN_POINT('Ctrl Pts',(0.261298259228322,-221.376672410653,
14.4469657360931));
#81489=CARTESIAN_POINT('Ctrl Pts',(3.18575945837514,-223.254229031811,14.2882078708613));
#81490=CARTESIAN_POINT('Ctrl Pts',(3.19461372649398,-226.729515174404,14.1294500056295));
#81491=CARTESIAN_POINT('Ctrl Pts',(0.279757637750653,-228.621949097395,
13.9706921403977));
#81492=CARTESIAN_POINT('Ctrl Pts',(-2.52331401844028,-227.364568613608,
13.830349954247));
#81493=CARTESIAN_POINT('Ctrl Pts',(-3.06589712602745,-225.665670112463,
13.7429270565069));
#81494=CARTESIAN_POINT('Ctrl Pts',(-3.07037718038997,-224.997773372826,
13.7084234471775));
#81495=CARTESIAN_POINT('Ctrl Pts',(-3.07482911963311,-224.997319814409,
14.7915765528225));
#81496=CARTESIAN_POINT('Ctrl Pts',(-3.07662798453365,-224.800691183691,
14.781381184332));
#81497=CARTESIAN_POINT('Ctrl Pts',(-2.96986780631845,-223.58540298435,14.7182665274308));
#81498=CARTESIAN_POINT('Ctrl Pts',(-1.35121078347837,-221.627907393731,
14.6022325821191));
#81499=CARTESIAN_POINT('Ctrl Pts',(2.10006689756961,-222.035797214701,14.4434747168873));
#81500=CARTESIAN_POINT('Ctrl Pts',(3.62936343654465,-225.156525308212,14.2847168516555));
#81501=CARTESIAN_POINT('Ctrl Pts',(1.83706670111546,-228.134001445802,14.1259589864237));
#81502=CARTESIAN_POINT('Ctrl Pts',(-1.6365134069338,-228.243239583436,13.9672011211919));
#81503=CARTESIAN_POINT('Ctrl Pts',(-3.02371444213389,-226.236009089191,
13.8557403099915));
#81504=CARTESIAN_POINT('Ctrl Pts',(-3.07799765278989,-225.110040994371,
13.7971987872017));
#81505=CARTESIAN_POINT('Ctrl Pts',(-3.07723488309734,-225.001830508734,
13.7915765528225));
#81506=CARTESIAN_POINT('Origin',(0.,-225.,22.2084234471774));
#81507=CARTESIAN_POINT('',(-3.06855000713338,-224.999857959883,15.7915765528225));
#81508=CARTESIAN_POINT('',(-3.07822420567057,-225.001003127123,15.7084234471775));
#81509=CARTESIAN_POINT('',(-3.0735,-225.,22.2084234471774));
#81510=CARTESIAN_POINT('Ctrl Pts',(-3.07822420567056,-225.001003127123,
15.7084234471775));
#81511=CARTESIAN_POINT('Ctrl Pts',(-3.07412463871347,-224.038498199653,
15.6583725623569));
#81512=CARTESIAN_POINT('Ctrl Pts',(-2.07017708091493,-222.050954058745,
15.5554023891257));
#81513=CARTESIAN_POINT('Ctrl Pts',(1.31414733087609,-221.613291215241,15.3995129274839));
#81514=CARTESIAN_POINT('Ctrl Pts',(3.55803654033007,-224.267091016787,15.2407550622521));
#81515=CARTESIAN_POINT('Ctrl Pts',(2.54561084798977,-227.591649090945,15.0819971970203));
#81516=CARTESIAN_POINT('Ctrl Pts',(-0.796557792326769,-228.544330018986,
14.9232393317885));
#81517=CARTESIAN_POINT('Ctrl Pts',(-2.8462359772097,-226.747272607382,14.7987147485075));
#81518=CARTESIAN_POINT('Ctrl Pts',(-3.07262355593096,-225.363917170084,
14.7271094536372));
#81519=CARTESIAN_POINT('Ctrl Pts',(-3.07026207039166,-225.002172427921,
14.7084234471775));
#81520=CARTESIAN_POINT('Ctrl Pts',(-3.06855000713338,-224.999857959883,
15.7915765528225));
#81521=CARTESIAN_POINT('Ctrl Pts',(-3.06875791854356,-224.495565829248,
15.7655635814622));
#81522=CARTESIAN_POINT('Ctrl Pts',(-2.71259526698658,-222.96564743543,15.6866313216913));
#81523=CARTESIAN_POINT('Ctrl Pts',(-0.301020081620057,-221.379756080425,
15.5547797735098));
#81524=CARTESIAN_POINT('Ctrl Pts',(2.87816732548634,-222.783486527642,15.396021908278));
#81525=CARTESIAN_POINT('Ctrl Pts',(3.42325610946395,-226.21577001757,15.2372640430462));
#81526=CARTESIAN_POINT('Ctrl Pts',(0.835381036688694,-228.535380835242,
15.0785061778144));
#81527=CARTESIAN_POINT('Ctrl Pts',(-2.30174388869721,-227.678234462693,
14.9299436810732));
#81528=CARTESIAN_POINT('Ctrl Pts',(-3.0672909359933,-225.82129649368,14.8343004727426));
#81529=CARTESIAN_POINT('Ctrl Pts',(-3.07482911963311,-224.997319814409,
14.7915765528225));
#81530=CARTESIAN_POINT('Origin',(0.,-225.,22.2084234471774));
#81531=CARTESIAN_POINT('',(-3.07430784425243,-225.002754717764,16.7915765528225));
#81532=CARTESIAN_POINT('',(-3.07321943364514,-224.997190820081,16.7084234471775));
#81533=CARTESIAN_POINT('',(-3.0735,-225.,22.2084234471774));
#81534=CARTESIAN_POINT('Ctrl Pts',(-3.07321943364514,-224.997190820081,
16.7084234471775));
#81535=CARTESIAN_POINT('Ctrl Pts',(-3.07549307656515,-224.747116023829,
16.6954742478977));
#81536=CARTESIAN_POINT('Ctrl Pts',(-2.93324524011334,-223.477617636429,
16.6296057602074));
#81537=CARTESIAN_POINT('Ctrl Pts',(-1.17442917055295,-221.562341535168,
16.5108179841064));
#81538=CARTESIAN_POINT('Ctrl Pts',(2.25103646081656,-222.148752123552,16.3520601188746));
#81539=CARTESIAN_POINT('Ctrl Pts',(3.61635361185226,-225.344624656961,16.1933022536428));
#81540=CARTESIAN_POINT('Ctrl Pts',(1.67198407948828,-228.225096717565,16.034544388411));
#81541=CARTESIAN_POINT('Ctrl Pts',(-1.80258521665346,-228.153960389228,
15.8757865231792));
#81542=CARTESIAN_POINT('Ctrl Pts',(-3.05211835267063,-226.128761858828,
15.767079542768));
#81543=CARTESIAN_POINT('Ctrl Pts',(-3.07845915081927,-225.056164041845,
15.7112918507675));
#81544=CARTESIAN_POINT('Ctrl Pts',(-3.07822420567056,-225.001003127123,
15.7084234471775));
#81545=CARTESIAN_POINT('Ctrl Pts',(-3.07430784425243,-225.002754717764,
16.7915765528225));
#81546=CARTESIAN_POINT('Ctrl Pts',(-3.06685916030357,-224.195655169849,
16.7497459785925));
#81547=CARTESIAN_POINT('Ctrl Pts',(-2.32773976850131,-222.355431708145,
16.6549961159518));
#81548=CARTESIAN_POINT('Ctrl Pts',(0.775732535354965,-221.451053935833,
16.5073269649006));
#81549=CARTESIAN_POINT('Ctrl Pts',(3.40229918628707,-223.726760283541,16.3485690996688));
#81550=CARTESIAN_POINT('Ctrl Pts',(2.91508175397509,-227.167735567766,16.189811234437));
#81551=CARTESIAN_POINT('Ctrl Pts',(-0.240018384082209,-228.62479934656,
16.0310533692052));
#81552=CARTESIAN_POINT('Ctrl Pts',(-2.69447347406282,-227.069271455095,
15.8983084753337));
#81553=CARTESIAN_POINT('Ctrl Pts',(-3.06833495556379,-225.521468650369,
15.8184828698728));
#81554=CARTESIAN_POINT('Ctrl Pts',(-3.06855000713338,-224.999857959883,
15.7915765528225));
#81555=CARTESIAN_POINT('Origin',(0.,-225.,22.2084234471774));
#81556=CARTESIAN_POINT('',(-3.07760789837034,-224.998416752929,17.7915765528225));
#81557=CARTESIAN_POINT('',(-3.06870231121375,-225.000725933415,17.7084234471775));
#81558=CARTESIAN_POINT('',(-3.0735,-225.,22.2084234471774));
#81559=CARTESIAN_POINT('Ctrl Pts',(-3.06870231121375,-225.000725933415,
17.7084234471775));
#81560=CARTESIAN_POINT('Ctrl Pts',(-3.06752400629039,-224.443116559207,
17.679656645028));
#81561=CARTESIAN_POINT('Ctrl Pts',(-2.65540737602782,-222.858108746021,
17.5979705544679));
#81562=CARTESIAN_POINT('Ctrl Pts',(-0.112777617954695,-221.369013821348,
17.4633651754972));
#81563=CARTESIAN_POINT('Ctrl Pts',(2.98929484919384,-222.935806224066,17.3046073102654));
#81564=CARTESIAN_POINT('Ctrl Pts',(3.35556479392172,-226.39174873303,17.1458494450336));
#81565=CARTESIAN_POINT('Ctrl Pts',(0.650821968247489,-228.573962834745,
16.9870915798018));
#81566=CARTESIAN_POINT('Ctrl Pts',(-2.3803556336648,-227.574084984456,16.8412829138497));
#81567=CARTESIAN_POINT('Ctrl Pts',(-3.0662014159128,-225.769092748505,16.7483935363083));
#81568=CARTESIAN_POINT('Ctrl Pts',(-3.07321943364514,-224.997190820081,
16.7084234471775));
#81569=CARTESIAN_POINT('Ctrl Pts',(-3.07760789837034,-224.998416752929,
17.7915765528225));
#81570=CARTESIAN_POINT('Ctrl Pts',(-3.07817910364606,-224.907429428249,
17.7868476641333));
#81571=CARTESIAN_POINT('Ctrl Pts',(-3.03325250153319,-223.79880775355,17.7291994870335));
#81572=CARTESIAN_POINT('Ctrl Pts',(-1.69089212962583,-221.784776606531,
17.6186320215231));
#81573=CARTESIAN_POINT('Ctrl Pts',(1.78403469350766,-221.835509587289,17.4598741562913));
#81574=CARTESIAN_POINT('Ctrl Pts',(3.6262132841795,-224.782384342542,17.3011162910595));
#81575=CARTESIAN_POINT('Ctrl Pts',(2.14968149722227,-227.928420804412,17.1423584258278));
#81576=CARTESIAN_POINT('Ctrl Pts',(-1.29423865111908,-228.394366727483,
16.9836005605959));
#81577=CARTESIAN_POINT('Ctrl Pts',(-2.9583412850881,-226.44954541655,16.8666732695942));
#81578=CARTESIAN_POINT('Ctrl Pts',(-3.07628238868196,-225.216705789839,
16.8026652670031));
#81579=CARTESIAN_POINT('Ctrl Pts',(-3.07430784425243,-225.002754717764,
16.7915765528225));
#81580=CARTESIAN_POINT('Origin',(0.,-225.,22.2084234471774));
#81581=CARTESIAN_POINT('',(-3.06955372481635,-224.998258419941,18.7915765528225));
#81582=CARTESIAN_POINT('',(-3.07588044059715,-225.00242799355,18.7084234471775));
#81583=CARTESIAN_POINT('',(-3.0735,-225.,22.2084234471774));
#81584=CARTESIAN_POINT('Ctrl Pts',(-3.07588044059715,-225.00242799355,18.7084234471775));
#81585=CARTESIAN_POINT('Ctrl Pts',(-3.06844940786727,-224.143330357591,
18.6638390421582));
#81586=CARTESIAN_POINT('Ctrl Pts',(-2.24606371110549,-222.252055139543,
18.5663353487284));
#81587=CARTESIAN_POINT('Ctrl Pts',(0.958825626738842,-221.496084849927,
18.4159123668879));
#81588=CARTESIAN_POINT('Ctrl Pts',(3.4637786989553,-223.905003298803,18.2571545016562));
#81589=CARTESIAN_POINT('Ctrl Pts',(2.79868206393424,-227.316065751486,18.0983966364243));
#81590=CARTESIAN_POINT('Ctrl Pts',(-0.427768493644222,-228.607463409909,
17.9396387711926));
#81591=CARTESIAN_POINT('Ctrl Pts',(-2.74903327485336,-226.961549419753,
17.8096477081102));
#81592=CARTESIAN_POINT('Ctrl Pts',(-3.06969161107839,-225.468892421981,
17.7325759334385));
#81593=CARTESIAN_POINT('Ctrl Pts',(-3.06870231121375,-225.000725933415,
17.7084234471775));
#81594=CARTESIAN_POINT('Ctrl Pts',(-3.06955372481635,-224.998258419941,
18.7915765528225));
#81595=CARTESIAN_POINT('Ctrl Pts',(-3.07161652142556,-224.600263410142,
18.7710300612636));
#81596=CARTESIAN_POINT('Ctrl Pts',(-2.81478286658869,-223.1797504858,18.697564281294));
#81597=CARTESIAN_POINT('Ctrl Pts',(-0.671786414007324,-221.429931110442,
18.5711792129139));
#81598=CARTESIAN_POINT('Ctrl Pts',(2.63490948932574,-222.499193694183,18.4124213476821));
#81599=CARTESIAN_POINT('Ctrl Pts',(3.53015379637291,-225.857213283498,18.2536634824503));
#81600=CARTESIAN_POINT('Ctrl Pts',(1.19459288842475,-228.430701869046,18.0949056172185));
#81601=CARTESIAN_POINT('Ctrl Pts',(-2.13212074104536,-227.881284704446,
17.9408766406759));
#81602=CARTESIAN_POINT('Ctrl Pts',(-3.07178695134263,-225.925635775,17.8397669525439));
#81603=CARTESIAN_POINT('Ctrl Pts',(-3.07760789837034,-224.998416752929,
17.7915765528225));
#81604=CARTESIAN_POINT('Origin',(0.,-225.,22.2084234471774));
#81605=CARTESIAN_POINT('',(-3.07038308399263,-225.003292812227,19.7915765528225));
#81606=CARTESIAN_POINT('',(-3.0763285686357,-224.997783098605,19.7084234471775));
#81607=CARTESIAN_POINT('',(-3.0735,-225.,22.2084234471774));
#81608=CARTESIAN_POINT('',(-0.793799282532889,-227.969222953746,20.));
#81609=CARTESIAN_POINT('Ctrl Pts',(-0.793799282532874,-227.969222953746,
20.));
#81610=CARTESIAN_POINT('Ctrl Pts',(-1.78107094869727,-227.70528334649,19.9470807115894));
#81611=CARTESIAN_POINT('Ctrl Pts',(-2.87946808286553,-226.663720267333,
19.8776062291969));
#81612=CARTESIAN_POINT('Ctrl Pts',(-3.07279570905048,-225.323526622123,
19.8081317468044));
#81613=CARTESIAN_POINT('Ctrl Pts',(-3.07038308399263,-225.003292812227,
19.7915765528225));
#81614=CARTESIAN_POINT('',(0.795577412305969,-227.974522386933,20.));
#81615=CARTESIAN_POINT('Origin',(0.,-225.,20.));
#81616=CARTESIAN_POINT('Ctrl Pts',(0.795579146452471,-227.974527555281,
20.));
#81617=CARTESIAN_POINT('Ctrl Pts',(-0.166093705500148,-228.23015226012,
19.948244384658));
#81618=CARTESIAN_POINT('Ctrl Pts',(-2.23002419682037,-227.756253006398,
19.8510522003838));
#81619=CARTESIAN_POINT('Ctrl Pts',(-3.06912206206202,-225.872782873122,
19.7538600161097));
#81620=CARTESIAN_POINT('Ctrl Pts',(-3.0763285686357,-224.997783098605,19.7084234471775));
#81621=CARTESIAN_POINT('Origin',(0.,-225.,22.2084234471774));
#81622=CARTESIAN_POINT('Ctrl Pts',(-3.0763285686357,-224.997783098605,19.7084234471775));
#81623=CARTESIAN_POINT('Ctrl Pts',(-3.07751537187321,-224.85368379687,19.7009407276991));
#81624=CARTESIAN_POINT('Ctrl Pts',(-3.00279426336461,-223.69169114993,19.6405387198101));
#81625=CARTESIAN_POINT('Ctrl Pts',(-1.52182615633225,-221.701128865433,
19.5272174235105));
#81626=CARTESIAN_POINT('Ctrl Pts',(1.94583861817437,-221.932458083289,19.3684595582787));
#81627=CARTESIAN_POINT('Ctrl Pts',(3.63261183657197,-224.970764508319,19.2097016930469));
#81628=CARTESIAN_POINT('Ctrl Pts',(1.99484845140044,-228.036042436051,19.0509438278151));
#81629=CARTESIAN_POINT('Ctrl Pts',(-1.46861473543692,-228.322628496388,
18.8921859625833));
#81630=CARTESIAN_POINT('Ctrl Pts',(-2.9928033600919,-226.341875538283,18.7780125023707));
#81631=CARTESIAN_POINT('Ctrl Pts',(-3.07726964364369,-225.163032999144,
18.7167583305688));
#81632=CARTESIAN_POINT('Ctrl Pts',(-3.07588044059715,-225.00242799355,18.7084234471775));
#81633=CARTESIAN_POINT('Ctrl Pts',(-3.07038308399263,-225.003292812227,
19.7915765528225));
#81634=CARTESIAN_POINT('Ctrl Pts',(-3.06508366403289,-224.299887432922,
19.7552124583938));
#81635=CARTESIAN_POINT('Ctrl Pts',(-2.47776214952136,-222.562456695511,
19.6659290755545));
#81636=CARTESIAN_POINT('Ctrl Pts',(0.40726891511089,-221.390844838622,19.5237264043046));
#81637=CARTESIAN_POINT('Ctrl Pts',(3.25295021883841,-223.383185295634,19.3649685390728));
#81638=CARTESIAN_POINT('Ctrl Pts',(3.12275738725604,-226.856580639298,19.206210673841));
#81639=CARTESIAN_POINT('Ctrl Pts',(0.1340136609786,-228.63017093477,19.0474528086092));
#81640=CARTESIAN_POINT('Ctrl Pts',(-2.57444325081393,-227.28215157222,18.9092414349364));
#81641=CARTESIAN_POINT('Ctrl Pts',(-3.06630360810496,-225.625334413095,
18.8239493496742));
#81642=CARTESIAN_POINT('Ctrl Pts',(-3.06955372481635,-224.998258419941,
18.7915765528225));
#81643=CARTESIAN_POINT('Ctrl Pts',(1.91346599666507,-223.364012796625,20.));
#81644=CARTESIAN_POINT('Ctrl Pts',(2.45743451545281,-224.000243484622,19.9470807115894));
#81645=CARTESIAN_POINT('Ctrl Pts',(2.85075800802285,-225.847693925911,19.8412421347682));
#81646=CARTESIAN_POINT('Ctrl Pts',(0.831598049327248,-227.85876780774,19.6824842695364));
#81647=CARTESIAN_POINT('Ctrl Pts',(-1.94946036222679,-227.24729402904,19.5237264043046));
#81648=CARTESIAN_POINT('Ctrl Pts',(-2.94596530464746,-224.582107318842,
19.3649685390728));
#81649=CARTESIAN_POINT('Ctrl Pts',(-1.24652589834599,-222.297898785986,
19.206210673841));
#81650=CARTESIAN_POINT('Ctrl Pts',(1.59383397470441,-222.487380258559,19.0474528086093));
#81651=CARTESIAN_POINT('Ctrl Pts',(2.97546780496825,-224.976053245386,18.8886949433774));
#81652=CARTESIAN_POINT('Ctrl Pts',(1.63397786770802,-227.48681855629,18.7299370781457));
#81653=CARTESIAN_POINT('Ctrl Pts',(-1.20294049014559,-227.721560839322,
18.5711792129139));
#81654=CARTESIAN_POINT('Ctrl Pts',(-2.93892187964717,-225.46557347867,18.4124213476821));
#81655=CARTESIAN_POINT('Ctrl Pts',(-1.9852049751549,-222.783472249891,18.2536634824503));
#81656=CARTESIAN_POINT('Ctrl Pts',(0.785372869795044,-222.129947489732,
18.0949056172185));
#81657=CARTESIAN_POINT('Ctrl Pts',(2.83717679343419,-224.10308957369,17.9361477519867));
#81658=CARTESIAN_POINT('Ctrl Pts',(2.29239697281744,-226.897086555837,17.7773898867549));
#81659=CARTESIAN_POINT('Ctrl Pts',(-0.350384637302541,-227.954868760191,
17.6186320215231));
#81660=CARTESIAN_POINT('Ctrl Pts',(-2.67249415737608,-226.308355800229,
17.4598741562913));
#81661=CARTESIAN_POINT('Ctrl Pts',(-2.54873717095616,-223.464435363585,
17.3011162910595));
#81662=CARTESIAN_POINT('Ctrl Pts',(-0.0923760055965229,-222.025863769398,
17.1423584258277));
#81663=CARTESIAN_POINT('Ctrl Pts',(2.44852766645372,-223.309221463831,16.9836005605959));
#81664=CARTESIAN_POINT('Ctrl Pts',(2.74853891937463,-226.13997964386,16.8248426953642));
#81665=CARTESIAN_POINT('Ctrl Pts',(0.533087458943556,-227.927428481038,
16.6660848301323));
#81666=CARTESIAN_POINT('Ctrl Pts',(-2.170245621756,-227.035694896164,16.5073269649006));
#81667=CARTESIAN_POINT('Ctrl Pts',(-2.88736999535495,-224.280893418101,
16.3485690996688));
#81668=CARTESIAN_POINT('Ctrl Pts',(-0.961973462458767,-222.184218257617,
16.189811234437));
#81669=CARTESIAN_POINT('Ctrl Pts',(1.84382114530851,-222.664546435999,16.0310533692052));
#81670=CARTESIAN_POINT('Ctrl Pts',(2.96215071346611,-225.282281624825,15.8722955039734));
#81671=CARTESIAN_POINT('Ctrl Pts',(1.36952006510874,-227.641672681461,15.7135376387416));
#81672=CARTESIAN_POINT('Ctrl Pts',(-1.47649529296408,-227.583405004029,
15.5547797735098));
#81673=CARTESIAN_POINT('Ctrl Pts',(-2.9712222169863,-225.160805168439,15.396021908278));
#81674=CARTESIAN_POINT('Ctrl Pts',(-1.74668668485902,-222.591036449047,
15.2372640430462));
#81675=CARTESIAN_POINT('Ctrl Pts',(1.07641643256242,-222.225951076743,15.0785061778144));
#81676=CARTESIAN_POINT('Ctrl Pts',(2.91438327323278,-224.399675169924,14.9197483125827));
#81677=CARTESIAN_POINT('Ctrl Pts',(2.08510665684536,-227.12281652398,14.7609904473508));
#81678=CARTESIAN_POINT('Ctrl Pts',(-0.652459489891874,-227.903156278769,
14.6022325821191));
#81679=CARTESIAN_POINT('Ctrl Pts',(-2.79289473713753,-226.026527521392,
14.4434747168873));
#81680=CARTESIAN_POINT('Ctrl Pts',(-2.37727283078277,-223.210420816804,
14.2847168516555));
#81681=CARTESIAN_POINT('Ctrl Pts',(0.214029076820345,-222.032136910304,
14.1259589864237));
#81682=CARTESIAN_POINT('Ctrl Pts',(2.60945158173399,-223.570041186785,13.9672011211919));
#81683=CARTESIAN_POINT('Ctrl Pts',(2.61670410165888,-226.416643712889,13.8084432559601));
#81684=CARTESIAN_POINT('Ctrl Pts',(0.229149130644944,-227.966733968665,
13.6496853907283));
#81685=CARTESIAN_POINT('Ctrl Pts',(-2.36812311572418,-226.801669412983,
13.4909275254965));
#81686=CARTESIAN_POINT('Ctrl Pts',(-2.7980891797067,-223.987717081388,13.3321696602647));
#81687=CARTESIAN_POINT('Ctrl Pts',(-0.66724413645386,-222.1002060371,13.1734117950329));
#81688=CARTESIAN_POINT('Ctrl Pts',(2.07426271424282,-222.866586313626,13.0146539298011));
#81689=CARTESIAN_POINT('Ctrl Pts',(2.91740441043288,-225.585466712028,12.8558960645693));
#81690=CARTESIAN_POINT('Ctrl Pts',(1.0905377049189,-227.768527998604,12.6971381993376));
#81691=CARTESIAN_POINT('Ctrl Pts',(-1.7343890652525,-227.417832569728,12.5383803341058));
#81692=CARTESIAN_POINT('Ctrl Pts',(-2.972003031108,-224.854336868116,12.379622468874));
#81693=CARTESIAN_POINT('Ctrl Pts',(-1.48963993976465,-222.424152059076,
12.2208646036422));
#81694=CARTESIAN_POINT('Ctrl Pts',(1.35604156587263,-222.351383184277,12.0621067384104));
#81695=CARTESIAN_POINT('Ctrl Pts',(2.96067388374833,-224.702628315074,11.9033488731786));
#81696=CARTESIAN_POINT('Ctrl Pts',(1.85569757964323,-227.326028000221,11.7445910079468));
#81697=CARTESIAN_POINT('Ctrl Pts',(-0.947613076377819,-227.820646951035,
11.585833142715));
#81698=CARTESIAN_POINT('Ctrl Pts',(-2.88366828216186,-225.733809923181,
11.4270752774832));
#81699=CARTESIAN_POINT('Ctrl Pts',(-2.18059038950889,-222.975390082488,
11.2683174122514));
#81700=CARTESIAN_POINT('Ctrl Pts',(0.518163741872992,-222.069893158686,
11.1095595470196));
#81701=CARTESIAN_POINT('Ctrl Pts',(2.74269443706901,-223.846029900831,10.9508016817878));
#81702=CARTESIAN_POINT('Ctrl Pts',(2.4571112913133,-226.678280032356,10.792043816556));
#81703=CARTESIAN_POINT('Ctrl Pts',(-0.0772200116287812,-227.974568344266,
10.6332859513242));
#81704=CARTESIAN_POINT('Ctrl Pts',(-2.54087956296479,-226.548531824475,
10.4745280860925));
#81705=CARTESIAN_POINT('Ctrl Pts',(-2.67912623819311,-223.70527903982,10.3157702208607));
#81706=CARTESIAN_POINT('Ctrl Pts',(-0.365436685581164,-222.046954827007,
10.1570123556289));
#81707=CARTESIAN_POINT('Ctrl Pts',(2.28270050730421,-223.091257440392,9.99825449039708));
#81708=CARTESIAN_POINT('Ctrl Pts',(2.84171028566979,-225.882441169271,9.83949662516528));
#81709=CARTESIAN_POINT('Ctrl Pts',(0.799986922337905,-227.866014774734,
9.6807387599335));
#81710=CARTESIAN_POINT('Ctrl Pts',(-1.97388444085889,-227.226611771064,
9.5219808947017));
#81711=CARTESIAN_POINT('Ctrl Pts',(-2.94125684140276,-224.549413762076,
9.36322302946991));
#81712=CARTESIAN_POINT('Ctrl Pts',(-1.21679109635696,-222.284592260317,
9.20446516423812));
#81713=CARTESIAN_POINT('Ctrl Pts',(1.6212818122256,-222.504911815135,9.04570729900632));
#81714=CARTESIAN_POINT('Ctrl Pts',(2.97555767001464,-225.008735978625,8.88694943377453));
#81715=CARTESIAN_POINT('Ctrl Pts',(1.60660326521724,-227.504564974821,8.72819156854273));
#81716=CARTESIAN_POINT('Ctrl Pts',(-1.23271438472883,-227.70821620455,8.56943370331095));
#81717=CARTESIAN_POINT('Ctrl Pts',(-2.94385187824639,-225.433308070373,
8.41067583807916));
#81718=CARTESIAN_POINT('Ctrl Pts',(-1.96077624855704,-222.76183640723,8.25191797284736));
#81719=CARTESIAN_POINT('Ctrl Pts',(0.816801726706074,-222.138731976176,
8.09316010761557));
#81720=CARTESIAN_POINT('Ctrl Pts',(2.84684279380774,-224.134259928009,7.93440224238378));
#81721=CARTESIAN_POINT('Ctrl Pts',(2.27145344796592,-226.922113159684,7.77564437715198));
#81722=CARTESIAN_POINT('Ctrl Pts',(-0.382770004131556,-227.950848503201,
7.61688651192019));
#81723=CARTESIAN_POINT('Ctrl Pts',(-2.6866823634999,-226.278967412628,7.4581286466884));
#81724=CARTESIAN_POINT('Ctrl Pts',(-2.53174312944437,-223.436575396312,
7.29937078145661));
#81725=CARTESIAN_POINT('Ctrl Pts',(-0.0597526828797273,-222.025029515811,
7.14061291622481));
#81726=CARTESIAN_POINT('Ctrl Pts',(2.46692341670672,-223.336176505452,6.98185505099303));
#81727=CARTESIAN_POINT('Ctrl Pts',(2.73587130233258,-226.170054691875,6.82309718576122));
#81728=CARTESIAN_POINT('Ctrl Pts',(0.500949879649189,-227.933098870305,
6.66433932052944));
#81729=CARTESIAN_POINT('Ctrl Pts',(-2.19244085318975,-227.011771077973,
6.50558145529764));
#81730=CARTESIAN_POINT('Ctrl Pts',(-2.8793098034051,-224.249270474191,6.34682359006586));
#81731=CARTESIAN_POINT('Ctrl Pts',(-0.9310345347702,-222.173837502908,6.18806572483406));
#81732=CARTESIAN_POINT('Ctrl Pts',(1.86932350347434,-222.684908337827,6.02930785960227));
#81733=CARTESIAN_POINT('Ctrl Pts',(2.95887674484852,-225.314750970928,5.87054999437047));
#81734=CARTESIAN_POINT('Ctrl Pts',(1.34046610569235,-227.656533527813,5.71179212913868));
#81735=CARTESIAN_POINT('Ctrl Pts',(-1.50473906068093,-227.56705670451,5.55303426390689));
#81736=CARTESIAN_POINT('Ctrl Pts',(-2.97280709789139,-225.128209686185,
5.3942763986751));
#81737=CARTESIAN_POINT('Ctrl Pts',(-1.72016219601459,-222.572025168107,
5.2355185334433));
#81738=CARTESIAN_POINT('Ctrl Pts',(1.10677508001132,-222.237923120698,5.07676066821152));
#81739=CARTESIAN_POINT('Ctrl Pts',(2.92079184633315,-224.431673724612,4.91800280297971));
#81740=CARTESIAN_POINT('Ctrl Pts',(2.06170002974943,-227.14555651341,4.75924493774793));
#81741=CARTESIAN_POINT('Ctrl Pts',(-0.684259572989003,-227.89582606551,
4.60048707251613));
#81742=CARTESIAN_POINT('Ctrl Pts',(-2.80398484143082,-225.995835716326,
4.44172920728434));
#81743=CARTESIAN_POINT('Ctrl Pts',(-2.35750329326922,-223.184456558731,
4.28297134205255));
#81744=CARTESIAN_POINT('Ctrl Pts',(0.246565176206193,-222.034662687169,
4.12421347682075));
#81745=CARTESIAN_POINT('Ctrl Pts',(2.62497720607225,-223.598745407746,3.96545561158896));
#81746=CARTESIAN_POINT('Ctrl Pts',(2.60101020024974,-226.445256275959,3.80669774635717));
#81747=CARTESIAN_POINT('Ctrl Pts',(0.196598761270279,-227.969068657434,
3.64793988112538));
#81748=CARTESIAN_POINT('Ctrl Pts',(-2.38773985594611,-226.775589520002,
3.48918201589359));
#81749=CARTESIAN_POINT('Ctrl Pts',(-2.78681905160012,-223.957090924459,
3.33042415066179));
#81750=CARTESIAN_POINT('Ctrl Pts',(-0.635401559389043,-222.093062672271,
3.17166628543));
#81751=CARTESIAN_POINT('Ctrl Pts',(2.09753541208473,-222.889463351295,3.01290842019821));
#81752=CARTESIAN_POINT('Ctrl Pts',(2.91080806279928,-225.617427081746,2.85415055496642));
#81753=CARTESIAN_POINT('Ctrl Pts',(1.06010927692769,-227.780321584409,2.69539268973463));
#81754=CARTESIAN_POINT('Ctrl Pts',(-1.76080145317522,-227.398665855655,
2.53663482450284));
#81755=CARTESIAN_POINT('Ctrl Pts',(-2.97022681197801,-224.821751284356,
2.37787695927104));
#81756=CARTESIAN_POINT('Ctrl Pts',(-1.46130060892094,-222.407969820474,
2.21911909403925));
#81757=CARTESIAN_POINT('Ctrl Pts',(1.38500765016929,-222.366414498639,2.06036122880746));
#81758=CARTESIAN_POINT('Ctrl Pts',(2.96375737617749,-224.735116069809,1.90160336357566));
#81759=CARTESIAN_POINT('Ctrl Pts',(1.83007562745225,-227.346240326103,1.74284549834387));
#81760=CARTESIAN_POINT('Ctrl Pts',(-0.978489556298073,-227.810083654364,
1.58408763311208));
#81761=CARTESIAN_POINT('Ctrl Pts',(-2.89154460401165,-225.702142338414,
1.42532976788028));
#81762=CARTESIAN_POINT('Ctrl Pts',(-2.15825110157835,-222.951592652511,
1.2665719026485));
#81763=CARTESIAN_POINT('Ctrl Pts',(0.550259421404619,-222.075760988886,
1.1078140374167));
#81764=CARTESIAN_POINT('Ctrl Pts',(2.75520159224266,-223.876160869976,0.94905617218491));
#81765=CARTESIAN_POINT('Ctrl Pts',(2.43852437670019,-226.705163033173,0.790298306953122));
#81766=CARTESIAN_POINT('Ctrl Pts',(-0.109770429300331,-227.973468539745,
0.631540441721324));
#81767=CARTESIAN_POINT('Ctrl Pts',(-2.55784670274268,-226.520722864724,
0.472782576489534));
#81768=CARTESIAN_POINT('Ctrl Pts',(-2.66448750437358,-223.675669147007,
0.314024711257742));
#81769=CARTESIAN_POINT('Ctrl Pts',(-0.333593465451435,-222.043745349829,
0.155266846025945));
#81770=CARTESIAN_POINT('Ctrl Pts',(2.30464631571321,-223.1151355344,-0.0034910192058416));
#81771=CARTESIAN_POINT('Ctrl Pts',(2.82948425040376,-225.916201445671,-0.162248884437639));
#81772=CARTESIAN_POINT('Ctrl Pts',(1.45887298303089,-227.215894200354,-0.268087461258832));
#81773=CARTESIAN_POINT('Ctrl Pts',(0.65019999797512,-227.432086802035,-0.32100674966943));
#81774=CARTESIAN_POINT('Ctrl Pts',(2.0543315503421,-223.243574678773,20.1070022498898));
#81775=CARTESIAN_POINT('Ctrl Pts',(2.63834594750733,-223.926643402192,20.0540829614792));
#81776=CARTESIAN_POINT('Ctrl Pts',(3.06062513181772,-225.910099463522,19.948244384658));
#81777=CARTESIAN_POINT('Ctrl Pts',(0.892818640578617,-228.069224597028,
19.7894865194262));
#81778=CARTESIAN_POINT('Ctrl Pts',(-2.09297574936987,-227.412735337235,
19.6307286541944));
#81779=CARTESIAN_POINT('Ctrl Pts',(-3.16284139989857,-224.551342892398,
19.4719707889626));
#81780=CARTESIAN_POINT('Ctrl Pts',(-1.33829265100808,-222.098975479135,
19.3132129237308));
#81781=CARTESIAN_POINT('Ctrl Pts',(1.71116885586107,-222.302406200136,19.1544550584991));
#81782=CARTESIAN_POINT('Ctrl Pts',(3.19451581550283,-224.97429033303,18.9956971932673));
#81783=CARTESIAN_POINT('Ctrl Pts',(1.75426806227216,-227.669893182877,18.8369393280355));
#81784=CARTESIAN_POINT('Ctrl Pts',(-1.29149857190937,-227.921916725011,
18.6781814628037));
#81785=CARTESIAN_POINT('Ctrl Pts',(-3.15527945198531,-225.499848070413,
18.5194235975719));
#81786=CARTESIAN_POINT('Ctrl Pts',(-2.13135180947283,-222.620295893842,
18.3606657323401));
#81787=CARTESIAN_POINT('Ctrl Pts',(0.843190455442978,-221.91865994313,18.2019078671083));
#81788=CARTESIAN_POINT('Ctrl Pts',(3.04604409527456,-224.037060815394,18.0431500018765));
#81789=CARTESIAN_POINT('Ctrl Pts',(2.46115866985638,-227.03674628772,17.8843921366447));
#81790=CARTESIAN_POINT('Ctrl Pts',(-0.376179256083103,-228.172400310097,
17.7256342714129));
#81791=CARTESIAN_POINT('Ctrl Pts',(-2.86923785171585,-226.404674347058,
17.5668764061811));
#81792=CARTESIAN_POINT('Ctrl Pts',(-2.73637012256843,-223.351390154999,
17.4081185409494));
#81793=CARTESIAN_POINT('Ctrl Pts',(-0.0991765430492469,-221.806913786715,
17.2493606757175));
#81794=CARTESIAN_POINT('Ctrl Pts',(2.62878339403376,-223.184749717243,17.0906028104857));
#81795=CARTESIAN_POINT('Ctrl Pts',(2.95088087755699,-226.223902673583,16.931844945254));
#81796=CARTESIAN_POINT('Ctrl Pts',(0.5723322953782,-228.142939932274,16.7730870800222));
#81797=CARTESIAN_POINT('Ctrl Pts',(-2.33001477974293,-227.185558697854,
16.6143292147904));
#81798=CARTESIAN_POINT('Ctrl Pts',(-3.09993242069985,-224.227954224518,
16.4555713495586));
#81799=CARTESIAN_POINT('Ctrl Pts',(-1.0327920318235,-221.9769260168,16.2968134843268));
#81800=CARTESIAN_POINT('Ctrl Pts',(1.97955958381119,-222.492614998516,16.138055619095));
#81801=CARTESIAN_POINT('Ctrl Pts',(3.18021834626149,-225.303062635537,15.9792977538632));
#81802=CARTESIAN_POINT('Ctrl Pts',(1.47034140323525,-227.836147360162,15.8205398886314));
#81803=CARTESIAN_POINT('Ctrl Pts',(-1.58519193419387,-227.773590132429,
15.6617820233996));
#81804=CARTESIAN_POINT('Ctrl Pts',(-3.1899576757939,-225.1726433245,15.5030241581678));
#81805=CARTESIAN_POINT('Ctrl Pts',(-1.87527427794497,-222.41369335281,15.344266292936));
#81806=CARTESIAN_POINT('Ctrl Pts',(1.15566006533364,-222.021731122909,15.1855084277043));
#81807=CARTESIAN_POINT('Ctrl Pts',(3.12893436226521,-224.355480452212,15.0267505624724));
#81808=CARTESIAN_POINT('Ctrl Pts',(2.23860805389349,-227.279094046301,14.8679926972407));
#81809=CARTESIAN_POINT('Ctrl Pts',(-0.700492257370171,-228.116880858842,
14.7092348320089));
#81810=CARTESIAN_POINT('Ctrl Pts',(-2.99850208223497,-226.102098431937,
14.5504769667771));
#81811=CARTESIAN_POINT('Ctrl Pts',(-2.55228291935149,-223.078675563464,
14.3917191015453));
#81812=CARTESIAN_POINT('Ctrl Pts',(0.229785470956337,-221.813648743753,
14.2329612363135));
#81813=CARTESIAN_POINT('Ctrl Pts',(2.80155420728104,-223.46477046846,14.0742033710817));
#81814=CARTESIAN_POINT('Ctrl Pts',(2.80934064327058,-226.520934200061,13.9154455058499));
#81815=CARTESIAN_POINT('Ctrl Pts',(0.246018633013514,-228.185139011575,
13.7566876406181));
#81816=CARTESIAN_POINT('Ctrl Pts',(-2.54245962050307,-226.934304724948,
13.5979297753863));
#81817=CARTESIAN_POINT('Ctrl Pts',(-3.00407892931503,-223.913194830113,
13.4391719101545));
#81818=CARTESIAN_POINT('Ctrl Pts',(-0.716365320150435,-221.886728984022,
13.2804140449227));
#81819=CARTESIAN_POINT('Ctrl Pts',(2.22696580184547,-222.709528649326,13.1216561796909));
#81820=CARTESIAN_POINT('Ctrl Pts',(3.1321779095657,-225.628567604697,12.9628983144592));
#81821=CARTESIAN_POINT('Ctrl Pts',(1.17082091762131,-227.972341512967,12.8041404492274));
#81822=CARTESIAN_POINT('Ctrl Pts',(-1.8620713320887,-227.595828585454,12.6453825839956));
#81823=CARTESIAN_POINT('Ctrl Pts',(-3.19079597189529,-224.843613438612,
12.4866247187638));
#81824=CARTESIAN_POINT('Ctrl Pts',(-1.59930426369834,-222.234523266603,
12.327866853532));
#81825=CARTESIAN_POINT('Ctrl Pts',(1.45587064374422,-222.156397292249,12.1691089883002));
#81826=CARTESIAN_POINT('Ctrl Pts',(3.1786327952828,-224.680736404207,12.0103511230684));
#81827=CARTESIAN_POINT('Ctrl Pts',(1.99231033757526,-227.49726554648,11.8515932578366));
#81828=CARTESIAN_POINT('Ctrl Pts',(-1.01737446273545,-228.028297358817,
11.6928353926048));
#81829=CARTESIAN_POINT('Ctrl Pts',(-3.09595819475795,-225.78783154745,11.534077527373));
#81830=CARTESIAN_POINT('Ctrl Pts',(-2.3411211086836,-222.826342334837,11.3753196621412));
#81831=CARTESIAN_POINT('Ctrl Pts',(0.556309923995647,-221.854184531904,
11.2165617969094));
#81832=CARTESIAN_POINT('Ctrl Pts',(2.94460613611043,-223.761076921667,11.0578039316776));
#81833=CARTESIAN_POINT('Ctrl Pts',(2.63799892825076,-226.801831664,10.8990460664458));
#81834=CARTESIAN_POINT('Ctrl Pts',(-0.0829047950072066,-228.193550138296,
10.7402882012141));
#81835=CARTESIAN_POINT('Ctrl Pts',(-2.72793405313473,-226.662531651607,
10.5815303359823));
#81836=CARTESIAN_POINT('Ctrl Pts',(-2.87635817310677,-223.609964262744,
10.4227724707505));
#81837=CARTESIAN_POINT('Ctrl Pts',(-0.392339406161525,-221.829557525957,
10.2640146055187));
#81838=CARTESIAN_POINT('Ctrl Pts',(2.45074836987437,-222.950739616739,10.1052567402869));
#81839=CARTESIAN_POINT('Ctrl Pts',(3.05091133417458,-225.947404729696,9.9464988750551));
#81840=CARTESIAN_POINT('Ctrl Pts',(0.858880365412371,-228.077005071292,
9.7877410098233));
#81841=CARTESIAN_POINT('Ctrl Pts',(-2.11919788000057,-227.390530492641,
9.62898314459151));
#81842=CARTESIAN_POINT('Ctrl Pts',(-3.15778630897244,-224.516242501131,
9.47022527935972));
#81843=CARTESIAN_POINT('Ctrl Pts',(-1.30636883214967,-222.084689353562,
9.31146741412793));
#81844=CARTESIAN_POINT('Ctrl Pts',(1.74063734848477,-222.321228394972,9.15270954889614));
#81845=CARTESIAN_POINT('Ctrl Pts',(3.19461229623485,-225.009379103963,8.99395168366434));
#81846=CARTESIAN_POINT('Ctrl Pts',(1.72487819609586,-227.688946057376,8.83519381843254));
#81847=CARTESIAN_POINT('Ctrl Pts',(-1.32346436128086,-227.907589684819,
8.67643595320076));
#81848=CARTESIAN_POINT('Ctrl Pts',(-3.16057238725731,-225.465207347053,
8.51767808796896));
#81849=CARTESIAN_POINT('Ctrl Pts',(-2.10512468870239,-222.597067263559,
8.35892022273717));
#81850=CARTESIAN_POINT('Ctrl Pts',(0.87693304217096,-221.928091125962,8.20016235750538));
#81851=CARTESIAN_POINT('Ctrl Pts',(3.05642168733399,-224.070525869085,8.04140449227358));
#81852=CARTESIAN_POINT('Ctrl Pts',(2.43867332443981,-227.063615300271,7.88264662704179));
#81853=CARTESIAN_POINT('Ctrl Pts',(-0.410948769083177,-228.168084089798,
7.72388876181));
#81854=CARTESIAN_POINT('Ctrl Pts',(-2.88447056530141,-226.373122444925,
7.56513089657821));
#81855=CARTESIAN_POINT('Ctrl Pts',(-2.71812501358486,-223.321479192452,
7.40637303134642));
#81856=CARTESIAN_POINT('Ctrl Pts',(-0.0641515563231119,-221.806018117041,
7.24761516611463));
#81857=CARTESIAN_POINT('Ctrl Pts',(2.64853340276285,-223.213689135314,7.08885730088283));
#81858=CARTESIAN_POINT('Ctrl Pts',(2.93728069579129,-226.256191786702,6.93009943565104));
#81859=CARTESIAN_POINT('Ctrl Pts',(0.537828811537304,-228.149027764299,
6.77134157041925));
#81860=CARTESIAN_POINT('Ctrl Pts',(-2.35384397988601,-227.159873655842,
6.61258370518746));
#81861=CARTESIAN_POINT('Ctrl Pts',(-3.09127885348033,-224.194003262493,
6.45382583995566));
#81862=CARTESIAN_POINT('Ctrl Pts',(-0.999575441931042,-221.965781051616,
6.29506797472387));
#81863=CARTESIAN_POINT('Ctrl Pts',(2.0069393747662,-222.514475902981,6.13631010949208));
#81864=CARTESIAN_POINT('Ctrl Pts',(3.17670335459837,-225.337922310198,5.97755224426028));
#81865=CARTESIAN_POINT('Ctrl Pts',(1.43914854922296,-227.85210223241,5.81879437902849));
#81866=CARTESIAN_POINT('Ctrl Pts',(-1.61551495180818,-227.756038303676,
5.6600365137967));
#81867=CARTESIAN_POINT('Ctrl Pts',(-3.191659232473,-225.137648227797,5.50127864856491));
#81868=CARTESIAN_POINT('Ctrl Pts',(-1.84679710908763,-222.393282499251,
5.34252078333311));
#81869=CARTESIAN_POINT('Ctrl Pts',(1.18825365591152,-222.034584524883,5.18376291810132));
#81870=CARTESIAN_POINT('Ctrl Pts',(3.13581472174675,-224.389834676731,5.02500505286953));
#81871=CARTESIAN_POINT('Ctrl Pts',(2.21347827755356,-227.303508108439,4.86624718763774));
#81872=CARTESIAN_POINT('Ctrl Pts',(-0.734633399216325,-228.109011009889,
4.70748932240595));
#81873=CARTESIAN_POINT('Ctrl Pts',(-3.0104086179069,-226.069147157342,4.54873145717415));
#81874=CARTESIAN_POINT('Ctrl Pts',(-2.53105798788129,-223.05079986845,4.38997359194236));
#81875=CARTESIAN_POINT('Ctrl Pts',(0.264716813143711,-221.816360463278,
4.23121572671057));
#81876=CARTESIAN_POINT('Ctrl Pts',(2.81822279714489,-223.495587836969,4.07245786147878));
#81877=CARTESIAN_POINT('Ctrl Pts',(2.79249138811321,-226.551653163007,3.91369999624698));
#81878=CARTESIAN_POINT('Ctrl Pts',(0.21107197030918,-228.18764557548,3.75494213101519));
#81879=CARTESIAN_POINT('Ctrl Pts',(-2.56352050604952,-226.906304882216,
3.5961842657834));
#81880=CARTESIAN_POINT('Ctrl Pts',(-2.99197911683543,-223.880314036541,
3.43742640055161));
#81881=CARTESIAN_POINT('Ctrl Pts',(-0.682178556015369,-221.879059738909,
3.27866853531981));
#81882=CARTESIAN_POINT('Ctrl Pts',(2.25195178932658,-222.734089848921,3.11991067008802));
#81883=CARTESIAN_POINT('Ctrl Pts',(3.12509595196398,-225.662880833146,2.96115280485623));
#81884=CARTESIAN_POINT('Ctrl Pts',(1.13815240939665,-227.985003319058,2.80239493962443));
#81885=CARTESIAN_POINT('Ctrl Pts',(-1.89042814737785,-227.575250856085,
2.64363707439265));
#81886=CARTESIAN_POINT('Ctrl Pts',(-3.18888899105247,-224.80862896911,2.48487920916085));
#81887=CARTESIAN_POINT('Ctrl Pts',(-1.5688786477902,-222.217149723842,2.32612134392906));
#81888=CARTESIAN_POINT('Ctrl Pts',(1.48696915344557,-222.172535182021,2.16736347869727));
#81889=CARTESIAN_POINT('Ctrl Pts',(3.18194328828006,-224.715615842707,2.00860561346548));
#81890=CARTESIAN_POINT('Ctrl Pts',(1.96480214832129,-227.518965863516,1.84984774823368));
#81891=CARTESIAN_POINT('Ctrl Pts',(-1.05052400757933,-228.016956413295,
1.69108988300189));
#81892=CARTESIAN_POINT('Ctrl Pts',(-3.10441435572704,-225.753832658197,
1.53233201777009));
#81893=CARTESIAN_POINT('Ctrl Pts',(-2.3171372468915,-222.800792985486,1.37357415253831));
#81894=CARTESIAN_POINT('Ctrl Pts',(0.590768423496762,-221.860484340071,
1.21481628730651));
#81895=CARTESIAN_POINT('Ctrl Pts',(2.95803404312474,-223.793426072718,1.05605842207472));
#81896=CARTESIAN_POINT('Ctrl Pts',(2.61804368202231,-226.830693737766,0.897300556842932));
#81897=CARTESIAN_POINT('Ctrl Pts',(-0.117851509563945,-228.192369368358,
0.738542691611135));
#81898=CARTESIAN_POINT('Ctrl Pts',(-2.74615027993235,-226.632675451654,
0.579784826379343));
#81899=CARTESIAN_POINT('Ctrl Pts',(-2.86064176487431,-223.578174548627,
0.421026961147553));
#81900=CARTESIAN_POINT('Ctrl Pts',(-0.35815195162039,-221.826111773464,
0.262269095915755));
#81901=CARTESIAN_POINT('Ctrl Pts',(2.47430978496665,-222.976375568444,0.103511230683969));
#81902=CARTESIAN_POINT('Ctrl Pts',(3.0377852425553,-225.98365037037,-0.0552466345478286));
#81903=CARTESIAN_POINT('Ctrl Pts',(1.56627230491969,-227.379023915733,-0.161085211369022));
#81904=CARTESIAN_POINT('Ctrl Pts',(0.698066426161045,-227.611132185939,
-0.21400449977962));
#81905=CARTESIAN_POINT('Ctrl Pts',(2.19519710401913,-223.123136560921,20.2140044997796));
#81906=CARTESIAN_POINT('Ctrl Pts',(2.81925737956185,-223.853043319762,20.161085211369));
#81907=CARTESIAN_POINT('Ctrl Pts',(3.27049225561258,-225.972505001132,20.0552466345478));
#81908=CARTESIAN_POINT('Ctrl Pts',(0.95403923182999,-228.279681386317,19.896488769316));
#81909=CARTESIAN_POINT('Ctrl Pts',(-2.23649113651294,-227.57817664543,19.7377309040842));
#81910=CARTESIAN_POINT('Ctrl Pts',(-3.37971749514968,-224.520578465953,
19.5789730388524));
#81911=CARTESIAN_POINT('Ctrl Pts',(-1.43005940367016,-221.900052172284,
19.4202151736207));
#81912=CARTESIAN_POINT('Ctrl Pts',(1.82850373701772,-222.117432141712,19.2614573083889));
#81913=CARTESIAN_POINT('Ctrl Pts',(3.4135638260374,-224.972527420675,19.1026994431571));
#81914=CARTESIAN_POINT('Ctrl Pts',(1.8745582568363,-227.852967809464,18.9439415779253));
#81915=CARTESIAN_POINT('Ctrl Pts',(-1.38005665367314,-228.122272610699,
18.7851837126935));
#81916=CARTESIAN_POINT('Ctrl Pts',(-3.37163702432346,-225.534122662157,
18.6264258474617));
#81917=CARTESIAN_POINT('Ctrl Pts',(-2.27749864379076,-222.457119537793,
18.4676679822299));
#81918=CARTESIAN_POINT('Ctrl Pts',(0.901008041090908,-221.707372396528,
18.3089101169981));
#81919=CARTESIAN_POINT('Ctrl Pts',(3.25491139711493,-223.971032057098,18.1501522517663));
#81920=CARTESIAN_POINT('Ctrl Pts',(2.62992036689531,-227.176406019603,17.9913943865345));
#81921=CARTESIAN_POINT('Ctrl Pts',(-0.401973874863661,-228.389931860003,
17.8326365213027));
#81922=CARTESIAN_POINT('Ctrl Pts',(-3.06598154605562,-226.500992893887,
17.6738786560709));
#81923=CARTESIAN_POINT('Ctrl Pts',(-2.92400307418069,-223.238344946413,
17.5151207908392));
#81924=CARTESIAN_POINT('Ctrl Pts',(-0.105977080501971,-221.587963804031,
17.3563629256074));
#81925=CARTESIAN_POINT('Ctrl Pts',(2.8090391216138,-223.060277970654,17.1976050603756));
#81926=CARTESIAN_POINT('Ctrl Pts',(3.15322283573935,-226.307825703306,17.0388471951438));
#81927=CARTESIAN_POINT('Ctrl Pts',(0.611577131812846,-228.358451383509,
16.880089329912));
#81928=CARTESIAN_POINT('Ctrl Pts',(-2.48978393772987,-227.335422499545,
16.7213314646802));
#81929=CARTESIAN_POINT('Ctrl Pts',(-3.31249484604475,-224.175015030935,
16.5625735994484));
#81930=CARTESIAN_POINT('Ctrl Pts',(-1.10361060118822,-221.769633775984,
16.4038157342166));
#81931=CARTESIAN_POINT('Ctrl Pts',(2.11529802231388,-222.320683561034,16.2450578689848));
#81932=CARTESIAN_POINT('Ctrl Pts',(3.39828597905688,-225.323843646249,16.086300003753));
#81933=CARTESIAN_POINT('Ctrl Pts',(1.57116274136176,-228.030622038864,15.9275421385212));
#81934=CARTESIAN_POINT('Ctrl Pts',(-1.69388857542366,-227.963775260828,
15.7687842732894));
#81935=CARTESIAN_POINT('Ctrl Pts',(-3.4086931346015,-225.184481480561,15.6100264080576));
#81936=CARTESIAN_POINT('Ctrl Pts',(-2.00386187103092,-222.236350256573,
15.4512685428259));
#81937=CARTESIAN_POINT('Ctrl Pts',(1.23490369810486,-221.817511169074,15.2925106775941));
#81938=CARTESIAN_POINT('Ctrl Pts',(3.34348545129764,-224.311285734499,15.1337528123623));
#81939=CARTESIAN_POINT('Ctrl Pts',(2.39210945094163,-227.435371568623,14.9749949471305));
#81940=CARTESIAN_POINT('Ctrl Pts',(-0.748525024848471,-228.330605438914,
14.8162370818987));
#81941=CARTESIAN_POINT('Ctrl Pts',(-3.20410942733242,-226.177669342483,
14.6574792166669));
#81942=CARTESIAN_POINT('Ctrl Pts',(-2.7272930079202,-222.946930310123,14.4987213514351));
#81943=CARTESIAN_POINT('Ctrl Pts',(0.245541865092328,-221.595160577203,
14.3399634862033));
#81944=CARTESIAN_POINT('Ctrl Pts',(2.99365683282809,-223.359499750136,14.1812056209715));
#81945=CARTESIAN_POINT('Ctrl Pts',(3.00197718488228,-226.625224687232,14.0224477557397));
#81946=CARTESIAN_POINT('Ctrl Pts',(0.262888135382085,-228.403544054485,
13.8636898905079));
#81947=CARTESIAN_POINT('Ctrl Pts',(-2.71679612528197,-227.066940036914,
13.7049320252761));
#81948=CARTESIAN_POINT('Ctrl Pts',(-3.21006867892337,-223.83867257884,13.5461741600443));
#81949=CARTESIAN_POINT('Ctrl Pts',(-0.765486503847009,-221.673251930943,
13.3874162948126));
#81950=CARTESIAN_POINT('Ctrl Pts',(2.37966888944811,-222.552470985027,13.2286584295807));
#81951=CARTESIAN_POINT('Ctrl Pts',(3.34695140869854,-225.671668497367,13.069900564349));
#81952=CARTESIAN_POINT('Ctrl Pts',(1.25110413032372,-228.17615502733,12.9111426991172));
#81953=CARTESIAN_POINT('Ctrl Pts',(-1.9897535989249,-227.773824601179,12.7523848338854));
#81954=CARTESIAN_POINT('Ctrl Pts',(-3.40958891268259,-224.832890009108,
12.5936269686536));
#81955=CARTESIAN_POINT('Ctrl Pts',(-1.70896858763203,-222.044894474129,
12.4348691034218));
#81956=CARTESIAN_POINT('Ctrl Pts',(1.5556997216158,-221.961411400221,12.27611123819));
#81957=CARTESIAN_POINT('Ctrl Pts',(3.39659170681727,-224.658844493341,12.1173533729582));
#81958=CARTESIAN_POINT('Ctrl Pts',(2.12892309550729,-227.668503092739,11.9585955077264));
#81959=CARTESIAN_POINT('Ctrl Pts',(-1.08713584909309,-228.2359477666,11.7998376424946));
#81960=CARTESIAN_POINT('Ctrl Pts',(-3.30824810735405,-225.841853171718,
11.6410797772628));
#81961=CARTESIAN_POINT('Ctrl Pts',(-2.5016518278583,-222.677294587186,11.482321912031));
#81962=CARTESIAN_POINT('Ctrl Pts',(0.594456106118301,-221.638475905122,
11.3235640467992));
#81963=CARTESIAN_POINT('Ctrl Pts',(3.14651783515185,-223.676123942502,11.1648061815675));
#81964=CARTESIAN_POINT('Ctrl Pts',(2.81888656518823,-226.925383295644,11.0060483163357));
#81965=CARTESIAN_POINT('Ctrl Pts',(-0.088589578385632,-228.412531932326,
10.8472904511039));
#81966=CARTESIAN_POINT('Ctrl Pts',(-2.91498854330466,-226.776531478738,
10.6885325858721));
#81967=CARTESIAN_POINT('Ctrl Pts',(-3.07359010802042,-223.514649485669,
10.5297747206403));
#81968=CARTESIAN_POINT('Ctrl Pts',(-0.419242126741886,-221.612160224906,
10.3710168554085));
#81969=CARTESIAN_POINT('Ctrl Pts',(2.61879623244453,-222.810221793085,10.2122589901767));
#81970=CARTESIAN_POINT('Ctrl Pts',(3.26011238267936,-226.012368290122,10.0535011249449));
#81971=CARTESIAN_POINT('Ctrl Pts',(0.917773808486839,-228.287995367849,
9.89474325971311));
#81972=CARTESIAN_POINT('Ctrl Pts',(-2.26451131914225,-227.554449214218,
9.73598539448132));
#81973=CARTESIAN_POINT('Ctrl Pts',(-3.37431577654211,-224.483071240186,
9.57722752924952));
#81974=CARTESIAN_POINT('Ctrl Pts',(-1.39594656794239,-221.884786446808,
9.41846966401774));
#81975=CARTESIAN_POINT('Ctrl Pts',(1.85999288474394,-222.137544974808,9.25971179878594));
#81976=CARTESIAN_POINT('Ctrl Pts',(3.41366692245506,-225.010022229301,9.10095393355416));
#81977=CARTESIAN_POINT('Ctrl Pts',(1.84315312697449,-227.873327139932,8.94219606832235));
#81978=CARTESIAN_POINT('Ctrl Pts',(-1.41421433783289,-228.106963165088,
8.78343820309057));
#81979=CARTESIAN_POINT('Ctrl Pts',(-3.37729289626824,-225.497106623734,
8.62468033785877));
#81980=CARTESIAN_POINT('Ctrl Pts',(-2.24947312884774,-222.432298119887,
8.46592247262698));
#81981=CARTESIAN_POINT('Ctrl Pts',(0.937064357635844,-221.717450275747,
8.30716460739519));
#81982=CARTESIAN_POINT('Ctrl Pts',(3.26600058086026,-224.00679181016,8.1484067421634));
#81983=CARTESIAN_POINT('Ctrl Pts',(2.6058932009137,-227.205117440858,7.9896488769316));
#81984=CARTESIAN_POINT('Ctrl Pts',(-0.439127534034797,-228.385319676397,
7.83089101169981));
#81985=CARTESIAN_POINT('Ctrl Pts',(-3.08225876710292,-226.467277477221,
7.67213314646802));
#81986=CARTESIAN_POINT('Ctrl Pts',(-2.90450689772536,-223.206382988593,
7.51337528123622));
#81987=CARTESIAN_POINT('Ctrl Pts',(-0.0685504297664977,-221.587006718271,
7.35461741600443));
#81988=CARTESIAN_POINT('Ctrl Pts',(2.83014338881898,-223.091201765176,7.19585955077264));
#81989=CARTESIAN_POINT('Ctrl Pts',(3.13869008925,-226.342328881529,7.03710168554085));
#81990=CARTESIAN_POINT('Ctrl Pts',(0.574707743425419,-228.364956658293,
6.87834382030906));
#81991=CARTESIAN_POINT('Ctrl Pts',(-2.51524710658227,-227.307976233711,
6.71958595507726));
#81992=CARTESIAN_POINT('Ctrl Pts',(-3.30324790355557,-224.138736050795,
6.56082808984547));
#81993=CARTESIAN_POINT('Ctrl Pts',(-1.06811634909188,-221.757724600324,
6.40207022461368));
#81994=CARTESIAN_POINT('Ctrl Pts',(2.14455524605805,-222.344043468136,6.24331235938189));
#81995=CARTESIAN_POINT('Ctrl Pts',(3.39452996434822,-225.361093649468,6.08455449415009));
#81996=CARTESIAN_POINT('Ctrl Pts',(1.53783099275358,-228.047670937006,5.9257966289183));
#81997=CARTESIAN_POINT('Ctrl Pts',(-1.72629084293543,-227.945019902843,
5.76703876368651));
#81998=CARTESIAN_POINT('Ctrl Pts',(-3.41051136705461,-225.147086769408,
5.60828089845472));
#81999=CARTESIAN_POINT('Ctrl Pts',(-1.97343202216067,-222.214539830395,
5.44952303322292));
#82000=CARTESIAN_POINT('Ctrl Pts',(1.26973223181172,-221.831245929069,5.29076516799113));
#82001=CARTESIAN_POINT('Ctrl Pts',(3.35083759716036,-224.347995628851,5.13200730275934));
#82002=CARTESIAN_POINT('Ctrl Pts',(2.36525652535769,-227.461459703468,4.97324943752755));
#82003=CARTESIAN_POINT('Ctrl Pts',(-0.785007225443646,-228.322195954269,
4.81449157229575));
#82004=CARTESIAN_POINT('Ctrl Pts',(-3.21683239438297,-226.142458598359,
4.65573370706396));
#82005=CARTESIAN_POINT('Ctrl Pts',(-2.70461268249337,-222.91714317817,4.49697584183217));
#82006=CARTESIAN_POINT('Ctrl Pts',(0.282868450081229,-221.598058239388,
4.33821797660038));
#82007=CARTESIAN_POINT('Ctrl Pts',(3.01146838821754,-223.392430266192,4.17946011136859));
#82008=CARTESIAN_POINT('Ctrl Pts',(2.98397257597669,-226.658050050056,4.02070224613679));
#82009=CARTESIAN_POINT('Ctrl Pts',(0.225545179348082,-228.406222493524,
3.861944380905));
#82010=CARTESIAN_POINT('Ctrl Pts',(-2.73930115615294,-227.03702024443,3.70318651567321));
#82011=CARTESIAN_POINT('Ctrl Pts',(-3.19713918207074,-223.803537148623,
3.54442865044141));
#82012=CARTESIAN_POINT('Ctrl Pts',(-0.728955552641697,-221.665056805547,
3.38567078520962));
#82013=CARTESIAN_POINT('Ctrl Pts',(2.40636816656843,-222.578716346547,3.22691291997783));
#82014=CARTESIAN_POINT('Ctrl Pts',(3.33938384112868,-225.708334584547,3.06815505474604));
#82015=CARTESIAN_POINT('Ctrl Pts',(1.21619554186561,-228.189685053706,2.90939718951424));
#82016=CARTESIAN_POINT('Ctrl Pts',(-2.02005484158048,-227.751835856514,
2.75063932428246));
#82017=CARTESIAN_POINT('Ctrl Pts',(-3.40755117012691,-224.795506653864,
2.59188145905066));
#82018=CARTESIAN_POINT('Ctrl Pts',(-1.67645668665946,-222.02632962721,2.43312359381887));
#82019=CARTESIAN_POINT('Ctrl Pts',(1.58893065672184,-221.978655865403,2.27436572858708));
#82020=CARTESIAN_POINT('Ctrl Pts',(3.40012920038263,-224.696115615605,2.11560786335529));
#82021=CARTESIAN_POINT('Ctrl Pts',(2.09952866919034,-227.691691400929,1.95684999812349));
#82022=CARTESIAN_POINT('Ctrl Pts',(-1.12255845886059,-228.223829172226,
1.7980921328917));
#82023=CARTESIAN_POINT('Ctrl Pts',(-3.31728410744242,-225.80552297798,1.6393342676599));
#82024=CARTESIAN_POINT('Ctrl Pts',(-2.47602339220465,-222.649993318462,
1.48057640242812));
#82025=CARTESIAN_POINT('Ctrl Pts',(0.631277425588911,-221.645207691255,
1.32181853719632));
#82026=CARTESIAN_POINT('Ctrl Pts',(3.16086649400682,-223.71069127546,1.16306067196453));
#82027=CARTESIAN_POINT('Ctrl Pts',(2.79756298734443,-226.95622444236,1.00430280673274));
#82028=CARTESIAN_POINT('Ctrl Pts',(-0.12593258982756,-228.41127019697,0.845544941500945));
#82029=CARTESIAN_POINT('Ctrl Pts',(-2.93445385712201,-226.744628038583,
0.686787076269153));
#82030=CARTESIAN_POINT('Ctrl Pts',(-3.05679602537503,-223.480679950247,
0.528029211037362));
#82031=CARTESIAN_POINT('Ctrl Pts',(-0.382710437789346,-221.608478197099,
0.369271345805565));
#82032=CARTESIAN_POINT('Ctrl Pts',(2.64397325422008,-222.83761560249,0.210513480573779));
#82033=CARTESIAN_POINT('Ctrl Pts',(3.24608623470683,-226.05109929507,0.0517556153419814));
#82034=CARTESIAN_POINT('Ctrl Pts',(1.6736716268085,-227.542153631111,-0.0540829614792118));
#82035=CARTESIAN_POINT('Ctrl Pts',(0.745932854346969,-227.790177569842,
-0.10700224988981));
#82036=CARTESIAN_POINT('Ctrl Pts',(2.33606265769616,-223.002698443069,20.3210067496694));
#82037=CARTESIAN_POINT('Ctrl Pts',(3.00016881161637,-223.779443237332,20.2680874612588));
#82038=CARTESIAN_POINT('Ctrl Pts',(3.48035937940744,-226.034910538743,20.1622488844376));
#82039=CARTESIAN_POINT('Ctrl Pts',(1.01525982308136,-228.490138175606,20.0034910192058));
#82040=CARTESIAN_POINT('Ctrl Pts',(-2.38000652365602,-227.743617953626,
19.8447331539741));
#82041=CARTESIAN_POINT('Ctrl Pts',(-3.59659359040079,-224.489814039508,
19.6859752887423));
#82042=CARTESIAN_POINT('Ctrl Pts',(-1.52182615633225,-221.701128865433,
19.5272174235105));
#82043=CARTESIAN_POINT('Ctrl Pts',(1.94583861817437,-221.932458083289,19.3684595582787));
#82044=CARTESIAN_POINT('Ctrl Pts',(3.63261183657197,-224.970764508319,19.2097016930469));
#82045=CARTESIAN_POINT('Ctrl Pts',(1.99484845140044,-228.036042436051,19.0509438278151));
#82046=CARTESIAN_POINT('Ctrl Pts',(-1.46861473543692,-228.322628496388,
18.8921859625833));
#82047=CARTESIAN_POINT('Ctrl Pts',(-3.5879945966616,-225.5683972539,18.7334280973515));
#82048=CARTESIAN_POINT('Ctrl Pts',(-2.42364547810869,-222.293943181744,
18.5746702321197));
#82049=CARTESIAN_POINT('Ctrl Pts',(0.958825626738842,-221.496084849927,
18.4159123668879));
#82050=CARTESIAN_POINT('Ctrl Pts',(3.4637786989553,-223.905003298803,18.2571545016562));
#82051=CARTESIAN_POINT('Ctrl Pts',(2.79868206393424,-227.316065751486,18.0983966364243));
#82052=CARTESIAN_POINT('Ctrl Pts',(-0.427768493644222,-228.607463409909,
17.9396387711926));
#82053=CARTESIAN_POINT('Ctrl Pts',(-3.26272524039538,-226.597311440717,
17.7808809059607));
#82054=CARTESIAN_POINT('Ctrl Pts',(-3.11163602579296,-223.125299737827,
17.622123040729));
#82055=CARTESIAN_POINT('Ctrl Pts',(-0.112777617954695,-221.369013821348,
17.4633651754972));
#82056=CARTESIAN_POINT('Ctrl Pts',(2.98929484919384,-222.935806224066,17.3046073102654));
#82057=CARTESIAN_POINT('Ctrl Pts',(3.35556479392172,-226.39174873303,17.1458494450336));
#82058=CARTESIAN_POINT('Ctrl Pts',(0.650821968247489,-228.573962834745,
16.9870915798018));
#82059=CARTESIAN_POINT('Ctrl Pts',(-2.6495530957168,-227.485286301235,16.82833371457));
#82060=CARTESIAN_POINT('Ctrl Pts',(-3.52505727138965,-224.122075837352,
16.6695758493382));
#82061=CARTESIAN_POINT('Ctrl Pts',(-1.17442917055295,-221.562341535168,
16.5108179841064));
#82062=CARTESIAN_POINT('Ctrl Pts',(2.25103646081656,-222.148752123552,16.3520601188746));
#82063=CARTESIAN_POINT('Ctrl Pts',(3.61635361185226,-225.344624656961,16.1933022536428));
#82064=CARTESIAN_POINT('Ctrl Pts',(1.67198407948828,-228.225096717565,16.034544388411));
#82065=CARTESIAN_POINT('Ctrl Pts',(-1.80258521665346,-228.153960389228,
15.8757865231792));
#82066=CARTESIAN_POINT('Ctrl Pts',(-3.6274285934091,-225.196319636622,15.7170286579474));
#82067=CARTESIAN_POINT('Ctrl Pts',(-2.13244946411687,-222.059007160336,
15.5582707927157));
#82068=CARTESIAN_POINT('Ctrl Pts',(1.31414733087609,-221.613291215241,15.3995129274839));
#82069=CARTESIAN_POINT('Ctrl Pts',(3.55803654033007,-224.267091016787,15.2407550622521));
#82070=CARTESIAN_POINT('Ctrl Pts',(2.54561084798977,-227.591649090945,15.0819971970203));
#82071=CARTESIAN_POINT('Ctrl Pts',(-0.796557792326769,-228.544330018986,
14.9232393317885));
#82072=CARTESIAN_POINT('Ctrl Pts',(-3.40971677242986,-226.253240253028,
14.7644814665567));
#82073=CARTESIAN_POINT('Ctrl Pts',(-2.90230309648892,-222.815185056782,
14.6057236013249));
#82074=CARTESIAN_POINT('Ctrl Pts',(0.261298259228322,-221.376672410653,
14.4469657360931));
#82075=CARTESIAN_POINT('Ctrl Pts',(3.18575945837514,-223.254229031811,14.2882078708613));
#82076=CARTESIAN_POINT('Ctrl Pts',(3.19461372649398,-226.729515174404,14.1294500056295));
#82077=CARTESIAN_POINT('Ctrl Pts',(0.279757637750653,-228.621949097395,
13.9706921403977));
#82078=CARTESIAN_POINT('Ctrl Pts',(-2.89113263006087,-227.199575348879,
13.8119342751659));
#82079=CARTESIAN_POINT('Ctrl Pts',(-3.4160584285317,-223.764150327565,13.6531764099342));
#82080=CARTESIAN_POINT('Ctrl Pts',(-0.814607687543583,-221.459774877865,
13.4944185447024));
#82081=CARTESIAN_POINT('Ctrl Pts',(2.53237197705076,-222.395413320727,13.3356606794706));
#82082=CARTESIAN_POINT('Ctrl Pts',(3.56172490783136,-225.714769390036,13.1769028142388));
#82083=CARTESIAN_POINT('Ctrl Pts',(1.33138734302612,-228.379968541692,13.018144949007));
#82084=CARTESIAN_POINT('Ctrl Pts',(-2.11743586576109,-227.951820616905,
12.8593870837752));
#82085=CARTESIAN_POINT('Ctrl Pts',(-3.62838185346989,-224.822166579605,
12.7006292185434));
#82086=CARTESIAN_POINT('Ctrl Pts',(-1.81863291156572,-221.855265681656,
12.5418713533116));
#82087=CARTESIAN_POINT('Ctrl Pts',(1.65552879948739,-221.766425508193,12.3831134880798));
#82088=CARTESIAN_POINT('Ctrl Pts',(3.61455061835174,-224.636952582474,12.224355622848));
#82089=CARTESIAN_POINT('Ctrl Pts',(2.26553585343932,-227.839740638999,12.0655977576162));
#82090=CARTESIAN_POINT('Ctrl Pts',(-1.15689723545072,-228.443598174382,
11.9068398923844));
#82091=CARTESIAN_POINT('Ctrl Pts',(-3.52053801995014,-225.895874795987,
11.7480820271526));
#82092=CARTESIAN_POINT('Ctrl Pts',(-2.66218254703301,-222.528246839534,
11.5893241619209));
#82093=CARTESIAN_POINT('Ctrl Pts',(0.632602288240958,-221.42276727834,11.430566296689));
#82094=CARTESIAN_POINT('Ctrl Pts',(3.34842953419328,-223.591170963338,11.2718084314573));
#82095=CARTESIAN_POINT('Ctrl Pts',(2.99977420212569,-227.048934927288,11.1130505662255));
#82096=CARTESIAN_POINT('Ctrl Pts',(-0.0942743617640601,-228.631513726356,
10.9542927009937));
#82097=CARTESIAN_POINT('Ctrl Pts',(-3.10204303347459,-226.890531305869,
10.7955348357619));
#82098=CARTESIAN_POINT('Ctrl Pts',(-3.27082204293408,-223.419334708594,
10.6367769705301));
#82099=CARTESIAN_POINT('Ctrl Pts',(-0.446144847322243,-221.394762923856,
10.4780191052983));
#82100=CARTESIAN_POINT('Ctrl Pts',(2.78684409501469,-222.669703969432,10.3192612400665));
#82101=CARTESIAN_POINT('Ctrl Pts',(3.46931343118415,-226.077331850548,10.1605033748347));
#82102=CARTESIAN_POINT('Ctrl Pts',(0.976667251561304,-228.498985664407,
10.0017455096029));
#82103=CARTESIAN_POINT('Ctrl Pts',(-2.40982475828392,-227.718367935795,
9.84298764437113));
#82104=CARTESIAN_POINT('Ctrl Pts',(-3.59084524411178,-224.449899979241,
9.68422977913933));
#82105=CARTESIAN_POINT('Ctrl Pts',(-1.48552430373511,-221.684883540053,
9.52547191390755));
#82106=CARTESIAN_POINT('Ctrl Pts',(1.97934842100312,-221.953861554645,9.36671404867575));
#82107=CARTESIAN_POINT('Ctrl Pts',(3.63272154867527,-225.010665354639,9.20795618344396));
#82108=CARTESIAN_POINT('Ctrl Pts',(1.96142805785311,-228.057708222487,9.04919831821216));
#82109=CARTESIAN_POINT('Ctrl Pts',(-1.50496431438492,-228.306336645357,
8.89044045298038));
#82110=CARTESIAN_POINT('Ctrl Pts',(-3.59401340527916,-225.529005900414,
8.73168258774858));
#82111=CARTESIAN_POINT('Ctrl Pts',(-2.39382156899309,-222.267528976215,
8.57292472251679));
#82112=CARTESIAN_POINT('Ctrl Pts',(0.997195673100731,-221.506809425532,
8.414166857285));
#82113=CARTESIAN_POINT('Ctrl Pts',(3.47557947438652,-223.943057751236,8.2554089920532));
#82114=CARTESIAN_POINT('Ctrl Pts',(2.7731130773876,-227.346619581445,8.09665112682141));
#82115=CARTESIAN_POINT('Ctrl Pts',(-0.467306298986418,-228.602555262994,
7.93789326158962));
#82116=CARTESIAN_POINT('Ctrl Pts',(-3.28004696890443,-226.561432509518,
7.77913539635783));
#82117=CARTESIAN_POINT('Ctrl Pts',(-3.09088878186585,-223.091286784733,
7.62037753112604));
#82118=CARTESIAN_POINT('Ctrl Pts',(-0.0729493032098818,-221.367995319502,
7.46161966589424));
#82119=CARTESIAN_POINT('Ctrl Pts',(3.01175337487511,-222.968714395038,7.30286180066245));
#82120=CARTESIAN_POINT('Ctrl Pts',(3.34009948270872,-226.428465976356,7.14410393543066));
#82121=CARTESIAN_POINT('Ctrl Pts',(0.611586675313532,-228.580885552287,
6.98534607019887));
#82122=CARTESIAN_POINT('Ctrl Pts',(-2.67665023327852,-227.456078811579,
6.82658820496708));
#82123=CARTESIAN_POINT('Ctrl Pts',(-3.51521695363081,-224.083468839097,
6.66783033973528));
#82124=CARTESIAN_POINT('Ctrl Pts',(-1.13665725625273,-221.549668149031,
6.50907247450349));
#82125=CARTESIAN_POINT('Ctrl Pts',(2.2821711173499,-222.173611033291,6.35031460927169));
#82126=CARTESIAN_POINT('Ctrl Pts',(3.61235657409808,-225.384264988738,6.19155674403991));
#82127=CARTESIAN_POINT('Ctrl Pts',(1.63651343628419,-228.243239641602,6.03279887880811));
#82128=CARTESIAN_POINT('Ctrl Pts',(-1.83706673406269,-228.13400150201,5.87404101357632));
#82129=CARTESIAN_POINT('Ctrl Pts',(-3.62936350163622,-225.156525311019,
5.71528314834453));
#82130=CARTESIAN_POINT('Ctrl Pts',(-2.10006693523372,-222.03579716154,5.55652528311273));
#82131=CARTESIAN_POINT('Ctrl Pts',(1.35121080771192,-221.627907333254,5.39776741788095));
#82132=CARTESIAN_POINT('Ctrl Pts',(3.56586047257395,-224.306156580971,5.23900955264915));
#82133=CARTESIAN_POINT('Ctrl Pts',(2.51703477316183,-227.619411298497,5.08025168741736));
#82134=CARTESIAN_POINT('Ctrl Pts',(-0.835381051670971,-228.535380898648,
4.92149382218557));
#82135=CARTESIAN_POINT('Ctrl Pts',(-3.42325617085904,-226.215770039375,
4.76273595695377));
#82136=CARTESIAN_POINT('Ctrl Pts',(-2.87816737710544,-222.783486487889,
4.60397809172198));
#82137=CARTESIAN_POINT('Ctrl Pts',(0.301020087018748,-221.379756015497,
4.44522022649019));
#82138=CARTESIAN_POINT('Ctrl Pts',(3.20471397929018,-223.289272695415,4.2864623612584));
#82139=CARTESIAN_POINT('Ctrl Pts',(3.17545376384016,-226.764446937104,4.1277044960266));
#82140=CARTESIAN_POINT('Ctrl Pts',(0.240018388386984,-228.624799411569,
3.96894663079481));
#82141=CARTESIAN_POINT('Ctrl Pts',(-2.91508180625635,-227.167735606644,
3.81018876556302));
#82142=CARTESIAN_POINT('Ctrl Pts',(-3.40229924730605,-223.726760260705,
3.65143090033123));
#82143=CARTESIAN_POINT('Ctrl Pts',(-0.775732549268024,-221.451053872185,
3.49267303509943));
#82144=CARTESIAN_POINT('Ctrl Pts',(2.56078454381028,-222.423342844173,3.33391516986764));
#82145=CARTESIAN_POINT('Ctrl Pts',(3.55367173029338,-225.753788335947,3.17515730463585));
#82146=CARTESIAN_POINT('Ctrl Pts',(1.29423867433457,-228.394366788354,3.01639943940406));
#82147=CARTESIAN_POINT('Ctrl Pts',(-2.14968153578312,-227.928420856944,
2.85764157417227));
#82148=CARTESIAN_POINT('Ctrl Pts',(-3.62621334920136,-224.782384338617,
2.69888370894047));
#82149=CARTESIAN_POINT('Ctrl Pts',(-1.78403472552871,-221.835509530578,
2.54012584370868));
#82150=CARTESIAN_POINT('Ctrl Pts',(1.69089215999812,-221.784776548785,2.38136797847689));
#82151=CARTESIAN_POINT('Ctrl Pts',(3.61831511248521,-224.676615388503,2.2226101132451));
#82152=CARTESIAN_POINT('Ctrl Pts',(2.23425519005939,-227.864416938342,2.0638522480133));
#82153=CARTESIAN_POINT('Ctrl Pts',(-1.19459291014185,-228.430701931157,
1.90509438278151));
#82154=CARTESIAN_POINT('Ctrl Pts',(-3.53015385915781,-225.857213297762,
1.74633651754971));
#82155=CARTESIAN_POINT('Ctrl Pts',(-2.63490953751781,-222.499193651437,
1.58757865231793));
#82156=CARTESIAN_POINT('Ctrl Pts',(0.671786427681058,-221.42993104244,1.42882078708613));
#82157=CARTESIAN_POINT('Ctrl Pts',(3.36369894488889,-223.627956478202,1.27006292185434));
#82158=CARTESIAN_POINT('Ctrl Pts',(2.97708229266655,-227.081755146954,1.11130505662255));
#82159=CARTESIAN_POINT('Ctrl Pts',(-0.134013670091176,-228.630171025583,
0.952547191390754));
#82160=CARTESIAN_POINT('Ctrl Pts',(-3.12275743431167,-226.856580625513,
0.793789326158964));
#82161=CARTESIAN_POINT('Ctrl Pts',(-3.25295028587576,-223.383185351868,
0.635031460927172));
#82162=CARTESIAN_POINT('Ctrl Pts',(-0.407268923958301,-221.390844620734,
0.476273595695375));
#82163=CARTESIAN_POINT('Ctrl Pts',(2.81363672347351,-222.698855636535,0.317515730463589));
#82164=CARTESIAN_POINT('Ctrl Pts',(3.45438722685837,-226.118548219769,0.158757865231791));
#82165=CARTESIAN_POINT('Ctrl Pts',(1.7810709486973,-227.70528334649,0.0529192884105984));
#82166=CARTESIAN_POINT('Ctrl Pts',(0.793799282532894,-227.969222953746,
0.));
#82167=CARTESIAN_POINT('Ctrl Pts',(0.793799282532894,-227.969222953746,
0.));
#82168=CARTESIAN_POINT('Ctrl Pts',(0.886846209318506,-227.93518597229,-1.38596896950808E-16));
#82169=CARTESIAN_POINT('Ctrl Pts',(0.977826029880219,-227.896378586582,
-3.02210246537631E-15));
#82170=CARTESIAN_POINT('Ctrl Pts',(1.06653104448955,-227.853129778678,-2.55351295663786E-15));
#82171=CARTESIAN_POINT('Ctrl Pts',(1.15720914088208,-227.808918979669,-2.07450052617888E-15));
#82172=CARTESIAN_POINT('Ctrl Pts',(1.24551077493275,-227.760066361007,6.89322567199222E-15));
#82173=CARTESIAN_POINT('Ctrl Pts',(1.33118514398854,-227.706877789535,9.71445146547012E-15));
#82174=CARTESIAN_POINT('Ctrl Pts',(1.41411883983993,-227.65539068951,1.24454278877419E-14));
#82175=CARTESIAN_POINT('Ctrl Pts',(1.49459099567019,-227.59983974531,7.56147219830355E-15));
#82176=CARTESIAN_POINT('Ctrl Pts',(1.57234042917301,-227.540471725161,8.60422844084496E-15));
#82177=CARTESIAN_POINT('Ctrl Pts',(1.64037118348797,-227.488524707531,9.5166401530687E-15));
#82178=CARTESIAN_POINT('Ctrl Pts',(1.70631705692185,-227.433654524465,-2.93526588135532E-15));
#82179=CARTESIAN_POINT('Ctrl Pts',(1.76997783386621,-227.376013525802,-4.27435864480685E-15));
#82180=CARTESIAN_POINT('Ctrl Pts',(1.78334877283042,-227.363906946022,-4.55561389280964E-15));
#82181=CARTESIAN_POINT('Ctrl Pts',(1.79662071187958,-227.351676197238,9.63133291544271E-15));
#82182=CARTESIAN_POINT('Ctrl Pts',(1.80977452688484,-227.339339080185,9.2148511043888E-15));
#82183=CARTESIAN_POINT('Ctrl Pts',(1.88220124459658,-227.271409213922,6.92164487112471E-15));
#82184=CARTESIAN_POINT('Ctrl Pts',(1.95116222786656,-227.200157774703,-1.31419746077129E-15));
#82185=CARTESIAN_POINT('Ctrl Pts',(2.01641817244364,-227.125876259157,-1.55431223447522E-15));
#82186=CARTESIAN_POINT('Ctrl Pts',(2.08131428700746,-227.052004341832,-1.79310298317626E-15));
#82187=CARTESIAN_POINT('Ctrl Pts',(2.14254659564994,-226.97513487391,-3.97077426484381E-15));
#82188=CARTESIAN_POINT('Ctrl Pts',(2.19983611488132,-226.895527810078,-6.80011602582908E-15));
#82189=CARTESIAN_POINT('Ctrl Pts',(2.25566846428196,-226.817945567073,-9.55749294035897E-15));
#82190=CARTESIAN_POINT('Ctrl Pts',(2.30775631089947,-226.737762479143,2.11375777811272E-16));
#82191=CARTESIAN_POINT('Ctrl Pts',(2.35579462634617,-226.655205071499,7.49400541621981E-16));
#82192=CARTESIAN_POINT('Ctrl Pts',(2.37650837701366,-226.619606954834,9.813926651359E-16));
#82193=CARTESIAN_POINT('Ctrl Pts',(2.39646858799471,-226.583567271918,-1.66443892832159E-16));
#82194=CARTESIAN_POINT('Ctrl Pts',(2.41564783026698,-226.54710385228,-5.55111512312578E-17));
#82195=CARTESIAN_POINT('Ctrl Pts',(2.42885133814525,-226.522001450339,2.08579412955737E-17));
#82196=CARTESIAN_POINT('Ctrl Pts',(2.44168468213581,-226.496698223146,-2.0325727317242E-15));
#82197=CARTESIAN_POINT('Ctrl Pts',(2.45413838324072,-226.471199984441,-2.41473507855972E-15));
#82198=CARTESIAN_POINT('Ctrl Pts',(2.4603528762171,-226.458476166518,-2.60543703938581E-15));
#82199=CARTESIAN_POINT('Ctrl Pts',(2.46647229162971,-226.445704742015,-5.19532788277858E-16));
#82200=CARTESIAN_POINT('Ctrl Pts',(2.47249024612966,-226.432897989824,-5.55111512312578E-16));
#82201=CARTESIAN_POINT('Ctrl Pts',(2.51269156419726,-226.347345944149,-7.92785559427772E-16));
#82202=CARTESIAN_POINT('Ctrl Pts',(2.54843636148031,-226.260082355034,-2.00368207205225E-16));
#82203=CARTESIAN_POINT('Ctrl Pts',(2.57947355676129,-226.171344793313,-4.71844785465692E-16));
#82204=CARTESIAN_POINT('Ctrl Pts',(2.60982489863058,-226.084568135563,-7.37322331413281E-16));
#82205=CARTESIAN_POINT('Ctrl Pts',(2.63567461225329,-225.99638125368,1.04889574150456E-16));
#82206=CARTESIAN_POINT('Ctrl Pts',(2.65673876288241,-225.906997538612,2.22044604925031E-15));
#82207=CARTESIAN_POINT('Ctrl Pts',(2.66036639126544,-225.891604043404,2.58478320435806E-15));
#82208=CARTESIAN_POINT('Ctrl Pts',(2.66385195947195,-225.876175043544,3.7568071414668E-15));
#82209=CARTESIAN_POINT('Ctrl Pts',(2.66719385858464,-225.860711623932,3.91353616180368E-15));
#82210=CARTESIAN_POINT('Ctrl Pts',(2.68732100412239,-225.767580596769,4.9129740133754E-15));
#82211=CARTESIAN_POINT('Ctrl Pts',(2.70224099955236,-225.673200037675,1.70107545693557E-15));
#82212=CARTESIAN_POINT('Ctrl Pts',(2.71203222946397,-225.577978516612,3.88578058618805E-16));
#82213=CARTESIAN_POINT('Ctrl Pts',(2.71529428522032,-225.546254421303,-4.86948613332932E-17));
#82214=CARTESIAN_POINT('Ctrl Pts',(2.71798665538282,-225.514437102176,2.56884507968682E-15));
#82215=CARTESIAN_POINT('Ctrl Pts',(2.72011103974616,-225.482542126578,2.33146835171283E-15));
#82216=CARTESIAN_POINT('Ctrl Pts',(2.72133536904072,-225.464160352711,2.19466293790962E-15));
#82217=CARTESIAN_POINT('Ctrl Pts',(2.72237103286684,-225.445752790738,1.60478203702852E-15));
#82218=CARTESIAN_POINT('Ctrl Pts',(2.72321827117276,-225.427322468988,1.4432899320127E-15));
#82219=CARTESIAN_POINT('Ctrl Pts',(2.72379256091328,-225.414829709134,1.33382455676117E-15));
#82220=CARTESIAN_POINT('Ctrl Pts',(2.72428015707703,-225.402328109628,7.25841149902439E-15));
#82221=CARTESIAN_POINT('Ctrl Pts',(2.72468101504371,-225.389828006928,7.16093850883226E-15));
#82222=CARTESIAN_POINT('Ctrl Pts',(2.7276693801058,-225.296640710458,6.43428492425922E-15));
#82223=CARTESIAN_POINT('Ctrl Pts',(2.72584874303933,-225.203390463169,-1.34546639841518E-16));
#82224=CARTESIAN_POINT('Ctrl Pts',(2.71935799045516,-225.110452110792,1.0547118733939E-15));
#82225=CARTESIAN_POINT('Ctrl Pts',(2.71285438848203,-225.017329773426,2.24632469685943E-15));
#82226=CARTESIAN_POINT('Ctrl Pts',(2.70166177912954,-224.924519586133,3.29155883824727E-15));
#82227=CARTESIAN_POINT('Ctrl Pts',(2.68586883845382,-224.832410644551,2.70616862252382E-15));
#82228=CARTESIAN_POINT('Ctrl Pts',(2.67029895478562,-224.741602635157,2.12904636603819E-15));
#82229=CARTESIAN_POINT('Ctrl Pts',(2.65025730337592,-224.651475356299,2.00810859991659E-15));
#82230=CARTESIAN_POINT('Ctrl Pts',(2.62578581077489,-224.562426807779,2.44249065417534E-15));
#82231=CARTESIAN_POINT('Ctrl Pts',(2.61627028276454,-224.527801050718,2.61139635485662E-15));
#82232=CARTESIAN_POINT('Ctrl Pts',(2.60608454518282,-224.493338733998,1.87075692833301E-15));
#82233=CARTESIAN_POINT('Ctrl Pts',(2.59522949564799,-224.459064719813,1.52655665885959E-15));
#82234=CARTESIAN_POINT('Ctrl Pts',(2.58886717656257,-224.438976168961,1.32481534605862E-15));
#82235=CARTESIAN_POINT('Ctrl Pts',(2.58227491151728,-224.418952323084,4.28946205561218E-15));
#82236=CARTESIAN_POINT('Ctrl Pts',(2.57545275110093,-224.398998344058,4.57966997657877E-15));
#82237=CARTESIAN_POINT('Ctrl Pts',(2.5704218465062,-224.384283567705,4.79367965590514E-15));
#82238=CARTESIAN_POINT('Ctrl Pts',(2.56526611083976,-224.369607571018,5.69313263505859E-15));
#82239=CARTESIAN_POINT('Ctrl Pts',(2.55999017666067,-224.354984576636,5.64825963778048E-15));
#82240=CARTESIAN_POINT('Ctrl Pts',(2.52758631659065,-224.265172716277,5.3726575784364E-15));
#82241=CARTESIAN_POINT('Ctrl Pts',(2.49061098433064,-224.177234165273,8.16050019748306E-15));
#82242=CARTESIAN_POINT('Ctrl Pts',(2.44913633387512,-224.091610553351,5.87724313660942E-15));
#82243=CARTESIAN_POINT('Ctrl Pts',(2.41803034603348,-224.02739284441,4.16480034095419E-15));
#82244=CARTESIAN_POINT('Ctrl Pts',(2.38439235385754,-223.964477823302,3.84165326499715E-15));
#82245=CARTESIAN_POINT('Ctrl Pts',(2.34823558025232,-223.903068833463,2.69922972861991E-15));
#82246=CARTESIAN_POINT('Ctrl Pts',(2.33711744989038,-223.884185700751,2.347936940589E-15));
#82247=CARTESIAN_POINT('Ctrl Pts',(2.32576105888447,-223.865445092701,7.90760064772973E-15));
#82248=CARTESIAN_POINT('Ctrl Pts',(2.3141665399975,-223.84685326456,8.88178419700125E-15));
#82249=CARTESIAN_POINT('Ctrl Pts',(2.30317844043336,-223.829233830698,9.80501576335647E-15));
#82250=CARTESIAN_POINT('Ctrl Pts',(2.29197545802167,-223.811746728186,9.82976587205289E-15));
#82251=CARTESIAN_POINT('Ctrl Pts',(2.28056965781359,-223.794414998359,9.61036805691151E-15));
#82252=CARTESIAN_POINT('Ctrl Pts',(2.23334862735917,-223.722660090588,8.70204152817875E-15));
#82253=CARTESIAN_POINT('Ctrl Pts',(2.18261057933454,-223.653494343049,7.7981406418901E-15));
#82254=CARTESIAN_POINT('Ctrl Pts',(2.12839132810104,-223.587269158508,5.40886779809568E-15));
#82255=CARTESIAN_POINT('Ctrl Pts',(2.07470602204923,-223.521696152249,3.04312424866893E-15));
#82256=CARTESIAN_POINT('Ctrl Pts',(2.01760738089684,-223.459005490671,5.95831660746538E-15));
#82257=CARTESIAN_POINT('Ctrl Pts',(1.95710205007443,-223.399580086106,4.69329436425525E-15));
#82258=CARTESIAN_POINT('Ctrl Pts',(1.94393780877166,-223.386650806081,4.39418859168102E-15));
#82259=CARTESIAN_POINT('Ctrl Pts',(1.93061220615115,-223.373876274008,9.21580020631812E-16));
#82260=CARTESIAN_POINT('Ctrl Pts',(1.91712862604369,-223.36125788605,9.43689570931383E-16));
#82261=CARTESIAN_POINT('Ctrl Pts',(1.91346599666507,-223.364012796625,20.));
#82262=CARTESIAN_POINT('Ctrl Pts',(1.97507204620631,-223.421907355683,20.));
#82263=CARTESIAN_POINT('Ctrl Pts',(2.0333066520343,-223.482952882657,20.));
#82264=CARTESIAN_POINT('Ctrl Pts',(2.08817311815043,-223.546764476174,20.));
#82265=CARTESIAN_POINT('Ctrl Pts',(2.14449280559963,-223.612266216252,20.));
#82266=CARTESIAN_POINT('Ctrl Pts',(2.19726400543086,-223.680682922028,20.));
#82267=CARTESIAN_POINT('Ctrl Pts',(2.2464647374009,-223.751646843991,20.));
#82268=CARTESIAN_POINT('Ctrl Pts',(2.29735442070123,-223.825046799029,20.));
#82269=CARTESIAN_POINT('Ctrl Pts',(2.3444248776897,-223.901172374798,20.));
#82270=CARTESIAN_POINT('Ctrl Pts',(2.38761687181107,-223.979660611969,20.));
#82271=CARTESIAN_POINT('Ctrl Pts',(2.40651336923917,-224.013999215731,20.));
#82272=CARTESIAN_POINT('Ctrl Pts',(2.42466701090125,-224.048790553719,20.));
#82273=CARTESIAN_POINT('Ctrl Pts',(2.44207039268086,-224.084006319604,20.));
#82274=CARTESIAN_POINT('Ctrl Pts',(2.45159423353378,-224.103277824076,20.));
#82275=CARTESIAN_POINT('Ctrl Pts',(2.46089336489712,-224.122676452755,20.));
#82276=CARTESIAN_POINT('Ctrl Pts',(2.46996636855114,-224.142197696102,20.));
#82277=CARTESIAN_POINT('Ctrl Pts',(2.47861912489588,-224.160814746053,20.));
#82278=CARTESIAN_POINT('Ctrl Pts',(2.48706870907561,-224.179549321891,20.));
#82279=CARTESIAN_POINT('Ctrl Pts',(2.49529978068773,-224.19836470108,20.));
#82280=CARTESIAN_POINT('Ctrl Pts',(2.5318521426381,-224.281919623545,20.));
#82281=CARTESIAN_POINT('Ctrl Pts',(2.56414460268445,-224.367158064701,20.));
#82282=CARTESIAN_POINT('Ctrl Pts',(2.59215310190908,-224.453681020382,20.));
#82283=CARTESIAN_POINT('Ctrl Pts',(2.6206247923598,-224.541634851514,20.));
#82284=CARTESIAN_POINT('Ctrl Pts',(2.64467014986719,-224.630916789565,20.));
#82285=CARTESIAN_POINT('Ctrl Pts',(2.66422479244635,-224.721144837958,20.));
#82286=CARTESIAN_POINT('Ctrl Pts',(2.68343404373964,-224.809779199249,20.));
#82287=CARTESIAN_POINT('Ctrl Pts',(2.69831007225569,-224.899327453851,20.));
#82288=CARTESIAN_POINT('Ctrl Pts',(2.70874920819526,-224.989450307808,20.));
#82289=CARTESIAN_POINT('Ctrl Pts',(2.71288525755108,-225.025157532449,20.));
#82290=CARTESIAN_POINT('Ctrl Pts',(2.71632430966266,-225.060955138582,20.));
#82291=CARTESIAN_POINT('Ctrl Pts',(2.71905787810446,-225.096822560585,20.));
#82292=CARTESIAN_POINT('Ctrl Pts',(2.72067784521375,-225.118078309317,20.));
#82293=CARTESIAN_POINT('Ctrl Pts',(2.72205002487447,-225.139358581396,20.));
#82294=CARTESIAN_POINT('Ctrl Pts',(2.72317244633848,-225.160659119609,20.));
#82295=CARTESIAN_POINT('Ctrl Pts',(2.72391546865431,-225.174759683202,20.));
#82296=CARTESIAN_POINT('Ctrl Pts',(2.72454895911028,-225.188869036708,20.));
#82297=CARTESIAN_POINT('Ctrl Pts',(2.72507200358104,-225.202971554569,20.));
#82298=CARTESIAN_POINT('Ctrl Pts',(2.72860218826004,-225.298153695426,20.));
#82299=CARTESIAN_POINT('Ctrl Pts',(2.72711435296688,-225.393186006008,20.));
#82300=CARTESIAN_POINT('Ctrl Pts',(2.72055005265772,-225.487669542712,20.));
#82301=CARTESIAN_POINT('Ctrl Pts',(2.71400792544162,-225.581833930055,20.));
#82302=CARTESIAN_POINT('Ctrl Pts',(2.70242392945975,-225.675454198458,20.));
#82303=CARTESIAN_POINT('Ctrl Pts',(2.68569220565089,-225.768153332782,20.));
#82304=CARTESIAN_POINT('Ctrl Pts',(2.68378820044636,-225.778702134341,20.));
#82305=CARTESIAN_POINT('Ctrl Pts',(2.6818174797233,-225.789239017697,20.));
#82306=CARTESIAN_POINT('Ctrl Pts',(2.6797798446426,-225.799763433399,20.));
#82307=CARTESIAN_POINT('Ctrl Pts',(2.66224922851865,-225.890309328171,20.));
#82308=CARTESIAN_POINT('Ctrl Pts',(2.63977008234293,-225.979932689554,20.));
#82309=CARTESIAN_POINT('Ctrl Pts',(2.61261752651431,-226.068395697362,20.));
#82310=CARTESIAN_POINT('Ctrl Pts',(2.6019190685787,-226.103251265798,20.));
#82311=CARTESIAN_POINT('Ctrl Pts',(2.59049450555523,-226.137926643292,20.));
#82312=CARTESIAN_POINT('Ctrl Pts',(2.57835850114292,-226.172406945337,20.));
#82313=CARTESIAN_POINT('Ctrl Pts',(2.57307177652304,-226.187427363552,20.));
#82314=CARTESIAN_POINT('Ctrl Pts',(2.56765002841871,-226.202410759174,20.));
#82315=CARTESIAN_POINT('Ctrl Pts',(2.56209440081032,-226.217355882885,20.));
#82316=CARTESIAN_POINT('Ctrl Pts',(2.5576754550037,-226.229243233227,20.));
#82317=CARTESIAN_POINT('Ctrl Pts',(2.5531721611383,-226.241105288201,20.));
#82318=CARTESIAN_POINT('Ctrl Pts',(2.54858887947735,-226.252932113005,20.));
#82319=CARTESIAN_POINT('Ctrl Pts',(2.5148395638014,-226.340019766195,20.));
#82320=CARTESIAN_POINT('Ctrl Pts',(2.47670681197659,-226.425334524189,20.));
#82321=CARTESIAN_POINT('Ctrl Pts',(2.43452410494245,-226.508645454499,20.));
#82322=CARTESIAN_POINT('Ctrl Pts',(2.39075655225714,-226.595086458123,20.));
#82323=CARTESIAN_POINT('Ctrl Pts',(2.34262888455579,-226.679370953022,20.));
#82324=CARTESIAN_POINT('Ctrl Pts',(2.2904575051027,-226.761237987111,20.));
#82325=CARTESIAN_POINT('Ctrl Pts',(2.23768209969329,-226.844052855319,20.));
#82326=CARTESIAN_POINT('Ctrl Pts',(2.18076839577045,-226.924394776583,20.));
#82327=CARTESIAN_POINT('Ctrl Pts',(2.11999199178509,-227.001978860565,20.));
#82328=CARTESIAN_POINT('Ctrl Pts',(2.07727651489662,-227.056507278322,20.));
#82329=CARTESIAN_POINT('Ctrl Pts',(2.03265187999783,-227.109673119658,20.));
#82330=CARTESIAN_POINT('Ctrl Pts',(1.98620043359043,-227.161369816309,20.));
#82331=CARTESIAN_POINT('Ctrl Pts',(1.9748368627249,-227.174016550078,20.));
#82332=CARTESIAN_POINT('Ctrl Pts',(1.96336316985503,-227.186576018518,20.));
#82333=CARTESIAN_POINT('Ctrl Pts',(1.95179223578434,-227.199034258492,20.));
#82334=CARTESIAN_POINT('Ctrl Pts',(1.88311834246096,-227.272974342998,20.));
#82335=CARTESIAN_POINT('Ctrl Pts',(1.81093148723848,-227.343453721762,20.));
#82336=CARTESIAN_POINT('Ctrl Pts',(1.73554509733181,-227.410185133041,20.));
#82337=CARTESIAN_POINT('Ctrl Pts',(1.67071538458667,-227.467571860668,20.));
#82338=CARTESIAN_POINT('Ctrl Pts',(1.60351843822465,-227.522186884759,20.));
#82339=CARTESIAN_POINT('Ctrl Pts',(1.53412735933154,-227.573832219717,20.));
#82340=CARTESIAN_POINT('Ctrl Pts',(1.50861560997377,-227.592819715833,20.));
#82341=CARTESIAN_POINT('Ctrl Pts',(1.48280707006451,-227.611405636062,20.));
#82342=CARTESIAN_POINT('Ctrl Pts',(1.45670963374051,-227.629579490491,20.));
#82343=CARTESIAN_POINT('Ctrl Pts',(1.43999804908724,-227.641217181758,20.));
#82344=CARTESIAN_POINT('Ctrl Pts',(1.42316693937207,-227.652686484956,20.));
#82345=CARTESIAN_POINT('Ctrl Pts',(1.40623320439776,-227.663974970311,20.));
#82346=CARTESIAN_POINT('Ctrl Pts',(1.32003064973545,-227.721439922805,20.));
#82347=CARTESIAN_POINT('Ctrl Pts',(1.23108709427863,-227.774282172299,20.));
#82348=CARTESIAN_POINT('Ctrl Pts',(1.13970922754748,-227.822182038463,20.));
#82349=CARTESIAN_POINT('Ctrl Pts',(1.04833136081634,-227.870081904628,20.));
#82350=CARTESIAN_POINT('Ctrl Pts',(0.95451854354455,-227.913040290229,20.));
#82351=CARTESIAN_POINT('Ctrl Pts',(0.858539654927881,-227.950697062107,
20.));
#82352=CARTESIAN_POINT('Ctrl Pts',(0.837654143889281,-227.958891373753,
20.));
#82353=CARTESIAN_POINT('Ctrl Pts',(0.816665943600311,-227.966834461527,
20.));
#82354=CARTESIAN_POINT('Ctrl Pts',(0.79557914645247,-227.974527555281,20.));
#82355=CARTESIAN_POINT('Ctrl Pts',(-2.51944981591128,-225.001988766476,
18.387416697508));
#82356=CARTESIAN_POINT('Ctrl Pts',(-2.52058771038653,-225.133540125377,
18.3957515808994));
#82357=CARTESIAN_POINT('Ctrl Pts',(-2.51117350858125,-225.264928190453,
18.4040864642907));
#82358=CARTESIAN_POINT('Ctrl Pts',(-2.4906388306482,-225.394554500649,18.4124213476821));
#82359=CARTESIAN_POINT('Ctrl Pts',(-2.36026141647998,-226.217569265554,
18.4653406360927));
#82360=CARTESIAN_POINT('Ctrl Pts',(-1.78160095331279,-226.969565052438,
18.5182599245033));
#82361=CARTESIAN_POINT('Ctrl Pts',(-1.01945099542026,-227.306439232042,
18.5711792129139));
#82362=CARTESIAN_POINT('Ctrl Pts',(-0.257301037527725,-227.643313411645,
18.6240985013245));
#82363=CARTESIAN_POINT('Ctrl Pts',(0.688338415090144,-227.565065983968,
18.6770177897351));
#82364=CARTESIAN_POINT('Ctrl Pts',(1.38473979760912,-227.107481384978,18.7299370781457));
#82365=CARTESIAN_POINT('Ctrl Pts',(2.0811411801281,-226.649896785989,18.7828563665563));
#82366=CARTESIAN_POINT('Ctrl Pts',(2.52830449254818,-225.812975015687,18.8357756549669));
#82367=CARTESIAN_POINT('Ctrl Pts',(2.52161384371424,-224.979735299399,18.8886949433774));
#82368=CARTESIAN_POINT('Ctrl Pts',(2.51492319488031,-224.14649558311,18.941614231788));
#82369=CARTESIAN_POINT('Ctrl Pts',(2.05437858479236,-223.316937920834,18.9945335201986));
#82370=CARTESIAN_POINT('Ctrl Pts',(1.35071296757332,-222.870578844268,19.0474528086093));
#82371=CARTESIAN_POINT('Ctrl Pts',(0.64704735035428,-222.424219767701,19.1003720970199));
#82372=CARTESIAN_POINT('Ctrl Pts',(-0.299739273995854,-222.361059276843,
19.1532913854304));
#82373=CARTESIAN_POINT('Ctrl Pts',(-1.05637248722117,-222.710180453557,
19.206210673841));
#82374=CARTESIAN_POINT('Ctrl Pts',(-1.81300570044648,-223.059301630271,
19.2591299622516));
#82375=CARTESIAN_POINT('Ctrl Pts',(-2.37948550254698,-223.820704474557,
19.3120492506622));
#82376=CARTESIAN_POINT('Ctrl Pts',(-2.49664124652711,-224.645603681732,
19.3649685390728));
#82377=CARTESIAN_POINT('Ctrl Pts',(-2.51320691839867,-224.762243371166,
19.3724512585512));
#82378=CARTESIAN_POINT('Ctrl Pts',(-2.52078898607152,-224.880152581298,
19.3799339780296));
#82379=CARTESIAN_POINT('Ctrl Pts',(-2.51981687702631,-224.998184138844,
19.387416697508));
#82380=CARTESIAN_POINT('Ctrl Pts',(-0.793799282532874,-227.969222953746,
20.));
#82381=CARTESIAN_POINT('Ctrl Pts',(-1.78107094869727,-227.70528334649,19.9470807115894));
#82382=CARTESIAN_POINT('Ctrl Pts',(-3.45438732992763,-226.118548905711,
19.8412421347682));
#82383=CARTESIAN_POINT('Ctrl Pts',(-2.8136366341492,-222.698855410048,19.6824842695364));
#82384=CARTESIAN_POINT('Ctrl Pts',(0.40726891511089,-221.390844838622,19.5237264043046));
#82385=CARTESIAN_POINT('Ctrl Pts',(3.25295021883841,-223.383185295634,19.3649685390728));
#82386=CARTESIAN_POINT('Ctrl Pts',(3.12275738725604,-226.856580639298,19.206210673841));
#82387=CARTESIAN_POINT('Ctrl Pts',(0.1340136609786,-228.63017093477,19.0474528086092));
#82388=CARTESIAN_POINT('Ctrl Pts',(-2.97708223483621,-227.08175512352,18.8886949433775));
#82389=CARTESIAN_POINT('Ctrl Pts',(-3.36369888730502,-223.627956495351,
18.7299370781457));
#82390=CARTESIAN_POINT('Ctrl Pts',(-0.671786414007324,-221.429931110442,
18.5711792129139));
#82391=CARTESIAN_POINT('Ctrl Pts',(2.63490948932574,-222.499193694183,18.4124213476821));
#82392=CARTESIAN_POINT('Ctrl Pts',(3.53015379637291,-225.857213283498,18.2536634824503));
#82393=CARTESIAN_POINT('Ctrl Pts',(1.19459288842475,-228.430701869046,18.0949056172185));
#82394=CARTESIAN_POINT('Ctrl Pts',(-2.23425514982848,-227.864416887275,
17.9361477519867));
#82395=CARTESIAN_POINT('Ctrl Pts',(-3.61831504767861,-224.676615394144,
17.7773898867549));
#82396=CARTESIAN_POINT('Ctrl Pts',(-1.69089212962583,-221.784776606531,
17.6186320215231));
#82397=CARTESIAN_POINT('Ctrl Pts',(1.78403469350766,-221.835509587289,17.4598741562913));
#82398=CARTESIAN_POINT('Ctrl Pts',(3.6262132841795,-224.782384342542,17.3011162910595));
#82399=CARTESIAN_POINT('Ctrl Pts',(2.14968149722227,-227.928420804412,17.1423584258278));
#82400=CARTESIAN_POINT('Ctrl Pts',(-1.29423865111908,-228.394366727483,
16.9836005605959));
#82401=CARTESIAN_POINT('Ctrl Pts',(-3.55367166656124,-225.753788322425,
16.8248426953642));
#82402=CARTESIAN_POINT('Ctrl Pts',(-2.56078449788238,-222.423342890386,
16.6660848301324));
#82403=CARTESIAN_POINT('Ctrl Pts',(0.775732535354965,-221.451053935833,
16.5073269649006));
#82404=CARTESIAN_POINT('Ctrl Pts',(3.40229918628707,-223.726760283541,16.3485690996688));
#82405=CARTESIAN_POINT('Ctrl Pts',(2.91508175397509,-227.167735567766,16.189811234437));
#82406=CARTESIAN_POINT('Ctrl Pts',(-0.240018384082209,-228.62479934656,
16.0310533692052));
#82407=CARTESIAN_POINT('Ctrl Pts',(-3.17545370688936,-226.764446905459,
15.8722955039734));
#82408=CARTESIAN_POINT('Ctrl Pts',(-3.20471392181458,-223.289272726097,
15.7135376387416));
#82409=CARTESIAN_POINT('Ctrl Pts',(-0.301020081620057,-221.379756080425,
15.5547797735098));
#82410=CARTESIAN_POINT('Ctrl Pts',(2.87816732548634,-222.783486527642,15.396021908278));
#82411=CARTESIAN_POINT('Ctrl Pts',(3.42325610946395,-226.21577001757,15.2372640430462));
#82412=CARTESIAN_POINT('Ctrl Pts',(0.835381036688694,-228.535380835242,
15.0785061778144));
#82413=CARTESIAN_POINT('Ctrl Pts',(-2.51703472801954,-227.619411251518,
14.9197483125827));
#82414=CARTESIAN_POINT('Ctrl Pts',(-3.5658604086213,-224.306156593415,14.7609904473508));
#82415=CARTESIAN_POINT('Ctrl Pts',(-1.35121078347837,-221.627907393731,
14.6022325821191));
#82416=CARTESIAN_POINT('Ctrl Pts',(2.10006689756961,-222.035797214701,14.4434747168873));
#82417=CARTESIAN_POINT('Ctrl Pts',(3.62936343654465,-225.156525308212,14.2847168516555));
#82418=CARTESIAN_POINT('Ctrl Pts',(1.83706670111546,-228.134001445802,14.1259589864237));
#82419=CARTESIAN_POINT('Ctrl Pts',(-1.6365134069338,-228.243239583436,13.9672011211919));
#82420=CARTESIAN_POINT('Ctrl Pts',(-3.61235650931153,-225.384264981846,
13.8084432559601));
#82421=CARTESIAN_POINT('Ctrl Pts',(-2.28217107641984,-222.173611083982,
13.6496853907283));
#82422=CARTESIAN_POINT('Ctrl Pts',(1.13665723586709,-221.549668210912,13.4909275254965));
#82423=CARTESIAN_POINT('Ctrl Pts',(3.51521689058642,-224.083468855535,13.3321696602647));
#82424=CARTESIAN_POINT('Ctrl Pts',(2.67665018527361,-227.45607876753,13.1734117950329));
#82425=CARTESIAN_POINT('Ctrl Pts',(-0.611586664344894,-228.580885488065,
13.0146539298011));
#82426=CARTESIAN_POINT('Ctrl Pts',(-3.34009942280501,-226.428465950738,
12.8558960645693));
#82427=CARTESIAN_POINT('Ctrl Pts',(-3.01175332086021,-222.968714431468,
12.6971381993376));
#82428=CARTESIAN_POINT('Ctrl Pts',(0.0729493019015324,-221.367995384641,
12.5383803341057));
#82429=CARTESIAN_POINT('Ctrl Pts',(3.09088872643165,-223.091286818965,12.379622468874));
#82430=CARTESIAN_POINT('Ctrl Pts',(3.28004691007777,-226.561432481514,12.2208646036422));
#82431=CARTESIAN_POINT('Ctrl Pts',(0.467306290605433,-228.602555198383,
12.0621067384104));
#82432=CARTESIAN_POINT('Ctrl Pts',(-2.77311302765262,-227.346619539359,
11.9033488731786));
#82433=CARTESIAN_POINT('Ctrl Pts',(-3.47557941205303,-223.943057770192,
11.7445910079468));
#82434=CARTESIAN_POINT('Ctrl Pts',(-0.997195655216347,-221.506809488182,
11.585833142715));
#82435=CARTESIAN_POINT('Ctrl Pts',(2.39382152606057,-222.267529025221,11.4270752774832));
#82436=CARTESIAN_POINT('Ctrl Pts',(3.5940133408216,-225.529005890927,11.2683174122514));
#82437=CARTESIAN_POINT('Ctrl Pts',(1.50496428739385,-228.306336586058,11.1095595470196));
#82438=CARTESIAN_POINT('Ctrl Pts',(-1.96142802267546,-228.057708167648,
10.9508016817878));
#82439=CARTESIAN_POINT('Ctrl Pts',(-3.63272148352348,-225.010665354448,
10.792043816556));
#82440=CARTESIAN_POINT('Ctrl Pts',(-1.97934838550411,-221.953861609276,
10.6332859513242));
#82441=CARTESIAN_POINT('Ctrl Pts',(1.48552427709262,-221.684883599509,10.4745280860925));
#82442=CARTESIAN_POINT('Ctrl Pts',(3.59084517971103,-224.449899989107,10.3157702208607));
#82443=CARTESIAN_POINT('Ctrl Pts',(2.40982471506444,-227.718367887042,10.1570123556289));
#82444=CARTESIAN_POINT('Ctrl Pts',(-0.97666723404505,-228.498985601654,
9.99825449039707));
#82445=CARTESIAN_POINT('Ctrl Pts',(-3.46931336896303,-226.077331831226,
9.83949662516529));
#82446=CARTESIAN_POINT('Ctrl Pts',(-2.78684404503348,-222.669704011225,
9.6807387599335));
#82447=CARTESIAN_POINT('Ctrl Pts',(0.446144839320715,-221.394762988514,
9.5219808947017));
#82448=CARTESIAN_POINT('Ctrl Pts',(3.27082198427282,-223.419334736943,9.36322302946992));
#82449=CARTESIAN_POINT('Ctrl Pts',(3.1020429778404,-226.890531271963,9.20446516423812));
#82450=CARTESIAN_POINT('Ctrl Pts',(0.0942743600733127,-228.631513661226,
9.04570729900632));
#82451=CARTESIAN_POINT('Ctrl Pts',(-2.99977414832561,-227.048934890541,
8.88694943377454));
#82452=CARTESIAN_POINT('Ctrl Pts',(-3.34842947414019,-223.591170988605,
8.72819156854274));
#82453=CARTESIAN_POINT('Ctrl Pts',(-0.632602276895449,-221.422767342497,
8.56943370331095));
#82454=CARTESIAN_POINT('Ctrl Pts',(2.6621824992875,-222.528246883865,8.41067583807915));
#82455=CARTESIAN_POINT('Ctrl Pts',(3.52053795681035,-225.89587477992,8.25191797284737));
#82456=CARTESIAN_POINT('Ctrl Pts',(1.15689721470216,-228.443598112622,8.09316010761557));
#82457=CARTESIAN_POINT('Ctrl Pts',(-2.26553581280758,-227.839740588069,
7.93440224238378));
#82458=CARTESIAN_POINT('Ctrl Pts',(-3.61455055352584,-224.636952588985,
7.77564437715198));
#82459=CARTESIAN_POINT('Ctrl Pts',(-1.655528769796,-221.766425566186,7.6168865119202));
#82460=CARTESIAN_POINT('Ctrl Pts',(1.81863287894903,-221.855265738056,7.4581286466884));
#82461=CARTESIAN_POINT('Ctrl Pts',(3.62838178839593,-224.822166582794,7.29937078145661));
#82462=CARTESIAN_POINT('Ctrl Pts',(2.11743582778552,-227.951820563965,7.14061291622481));
#82463=CARTESIAN_POINT('Ctrl Pts',(-1.33138731914806,-228.379968481073,
6.98185505099303));
#82464=CARTESIAN_POINT('Ctrl Pts',(-3.56172484395287,-225.714769377217,
6.82309718576123));
#82465=CARTESIAN_POINT('Ctrl Pts',(-2.53237193163343,-222.395413367439,
6.66433932052944));
#82466=CARTESIAN_POINT('Ctrl Pts',(0.814607672933798,-221.459774941358,
6.50558145529765));
#82467=CARTESIAN_POINT('Ctrl Pts',(3.41605836726569,-223.76415034973,6.34682359006585));
#82468=CARTESIAN_POINT('Ctrl Pts',(2.89113257820927,-227.19957530943,6.18806572483406));
#82469=CARTESIAN_POINT('Ctrl Pts',(-0.279757632733263,-228.621949032436,
6.02930785960227));
#82470=CARTESIAN_POINT('Ctrl Pts',(-3.19461366919951,-226.729515143386,
5.87054999437048));
#82471=CARTESIAN_POINT('Ctrl Pts',(-3.18575940123949,-223.254229063121,
5.71179212913868));
#82472=CARTESIAN_POINT('Ctrl Pts',(-0.261298254542071,-221.376672475636,
5.5530342639069));
#82473=CARTESIAN_POINT('Ctrl Pts',(2.90230304443695,-222.815185095966,5.3942763986751));
#82474=CARTESIAN_POINT('Ctrl Pts',(3.40971671127761,-226.253240230551,5.23551853344331));
#82475=CARTESIAN_POINT('Ctrl Pts',(0.796557778040768,-228.54432995542,5.07676066821151));
#82476=CARTESIAN_POINT('Ctrl Pts',(-2.54561080233497,-227.591649044464,
4.91800280297972));
#82477=CARTESIAN_POINT('Ctrl Pts',(-3.55803647651774,-224.267091029931,
4.75924493774793));
#82478=CARTESIAN_POINT('Ctrl Pts',(-1.31414730730727,-221.61329127598,4.60048707251613));
#82479=CARTESIAN_POINT('Ctrl Pts',(2.13244942587199,-222.059007213082,4.44172920728434));
#82480=CARTESIAN_POINT('Ctrl Pts',(3.62742852835224,-225.196319633101,4.28297134205255));
#82481=CARTESIAN_POINT('Ctrl Pts',(1.80258518432463,-228.153960332663,4.12421347682076));
#82482=CARTESIAN_POINT('Ctrl Pts',(-1.67198404950171,-228.225096659724,
3.96545561158897));
#82483=CARTESIAN_POINT('Ctrl Pts',(-3.61635354699401,-225.34462465078,3.80669774635717));
#82484=CARTESIAN_POINT('Ctrl Pts',(-2.25103642044492,-222.148752174688,
3.64793988112538));
#82485=CARTESIAN_POINT('Ctrl Pts',(1.17442914948988,-221.562341596822,3.48918201589359));
#82486=CARTESIAN_POINT('Ctrl Pts',(3.52505720816877,-224.122075853096,3.3304241506618));
#82487=CARTESIAN_POINT('Ctrl Pts',(2.64955304819789,-227.485286256663,3.17166628543001));
#82488=CARTESIAN_POINT('Ctrl Pts',(-0.650821956575191,-228.573962770645,
3.01290842019821));
#82489=CARTESIAN_POINT('Ctrl Pts',(-3.35556473374051,-226.391748708072,
2.85415055496642));
#82490=CARTESIAN_POINT('Ctrl Pts',(-2.98929479558205,-222.93580626108,2.69539268973463));
#82491=CARTESIAN_POINT('Ctrl Pts',(0.112777615932726,-221.369013886482,
2.53663482450283));
#82492=CARTESIAN_POINT('Ctrl Pts',(3.11163596998505,-223.125299771423,2.37787695927105));
#82493=CARTESIAN_POINT('Ctrl Pts',(3.26272518188304,-226.597311412118,2.21911909403925));
#82494=CARTESIAN_POINT('Ctrl Pts',(0.427768485964111,-228.607463345116,
2.06036122880746));
#82495=CARTESIAN_POINT('Ctrl Pts',(-2.79868201372234,-227.316065710128,
1.90160336357566));
#82496=CARTESIAN_POINT('Ctrl Pts',(-3.46377863687395,-223.905003318099,
1.74284549834387));
#82497=CARTESIAN_POINT('Ctrl Pts',(-0.958825609453758,-221.496084913414,
1.58408763311208));
#82498=CARTESIAN_POINT('Ctrl Pts',(2.42364543444732,-222.293943229063,1.42532976788028));
#82499=CARTESIAN_POINT('Ctrl Pts',(3.58799453273333,-225.568397245971,1.2665719026485));
#82500=CARTESIAN_POINT('Ctrl Pts',(1.46861470818642,-228.322628432602,1.1078140374167));
#82501=CARTESIAN_POINT('Ctrl Pts',(-1.9948484136595,-228.0360423893,0.949056172184909));
#82502=CARTESIAN_POINT('Ctrl Pts',(-3.63261177564012,-224.970764494873,
0.790298306953122));
#82503=CARTESIAN_POINT('Ctrl Pts',(-1.94583857424385,-221.93245816329,0.631540441721324));
#82504=CARTESIAN_POINT('Ctrl Pts',(1.52182610974532,-221.701128880727,0.472782576489534));
#82505=CARTESIAN_POINT('Ctrl Pts',(3.59659356700835,-224.489814123823,0.314024711257741));
#82506=CARTESIAN_POINT('Ctrl Pts',(2.38000639294467,-227.743617779076,0.155266846025945));
#82507=CARTESIAN_POINT('Ctrl Pts',(-1.0152596211774,-228.490138311657,-0.00349101920584169));
#82508=CARTESIAN_POINT('Ctrl Pts',(-3.48035985289286,-226.03491003184,-0.162248884437638));
#82509=CARTESIAN_POINT('Ctrl Pts',(-3.00016881161638,-223.779443237332,
-0.268087461258832));
#82510=CARTESIAN_POINT('Ctrl Pts',(-2.33606265769617,-223.002698443069,
-0.32100674966943));
#82511=CARTESIAN_POINT('Ctrl Pts',(-0.745932854346956,-227.790177569842,
20.1070022498898));
#82512=CARTESIAN_POINT('Ctrl Pts',(-1.67367162680847,-227.542153631111,
20.0540829614792));
#82513=CARTESIAN_POINT('Ctrl Pts',(-3.24608633156098,-226.051099939649,
19.948244384658));
#82514=CARTESIAN_POINT('Ctrl Pts',(-2.64397317028206,-222.83761538966,19.7894865194262));
#82515=CARTESIAN_POINT('Ctrl Pts',(0.382710429475444,-221.608478401848,
19.6307286541944));
#82516=CARTESIAN_POINT('Ctrl Pts',(3.05679596238007,-223.480679897405,19.4719707889627));
#82517=CARTESIAN_POINT('Ctrl Pts',(2.93445381290385,-226.744628051537,19.3132129237308));
#82518=CARTESIAN_POINT('Ctrl Pts',(0.125932581264471,-228.411270111633,
19.1544550584991));
#82519=CARTESIAN_POINT('Ctrl Pts',(-2.79756293300129,-226.95622442034,18.9956971932673));
#82520=CARTESIAN_POINT('Ctrl Pts',(-3.16086643989526,-223.710691291575,
18.8369393280355));
#82521=CARTESIAN_POINT('Ctrl Pts',(-0.631277412739705,-221.645207755157,
18.6781814628037));
#82522=CARTESIAN_POINT('Ctrl Pts',(2.4760233469186,-222.64999335863,18.5194235975719));
#82523=CARTESIAN_POINT('Ctrl Pts',(3.31728404844348,-225.805522964576,18.3606657323401));
#82524=CARTESIAN_POINT('Ctrl Pts',(1.12255843845303,-228.22382911386,18.2019078671083));
#82525=CARTESIAN_POINT('Ctrl Pts',(-2.09952863138538,-227.691691352941,
18.0431500018765));
#82526=CARTESIAN_POINT('Ctrl Pts',(-3.4001291394839,-224.696115620906,17.8843921366447));
#82527=CARTESIAN_POINT('Ctrl Pts',(-1.588930628181,-221.978655919667,17.7256342714129));
#82528=CARTESIAN_POINT('Ctrl Pts',(1.67645665656929,-222.026329680502,17.5668764061811));
#82529=CARTESIAN_POINT('Ctrl Pts',(3.4075511090259,-224.795506657551,17.4081185409493));
#82530=CARTESIAN_POINT('Ctrl Pts',(2.02005480534486,-227.751835807151,17.2493606757176));
#82531=CARTESIAN_POINT('Ctrl Pts',(-1.21619552005003,-228.189684996505,
17.0906028104857));
#82532=CARTESIAN_POINT('Ctrl Pts',(-3.33938378123961,-225.70833457184,16.931844945254));
#82533=CARTESIAN_POINT('Ctrl Pts',(-2.40636812341,-222.578716389973,16.7730870800222));
#82534=CARTESIAN_POINT('Ctrl Pts',(0.728955539567609,-221.665056865358,
16.6143292147904));
#82535=CARTESIAN_POINT('Ctrl Pts',(3.19713912473123,-223.803537170082,16.4555713495586));
#82536=CARTESIAN_POINT('Ctrl Pts',(2.73930110702426,-227.037020207896,16.2968134843268));
#82537=CARTESIAN_POINT('Ctrl Pts',(-0.225545175302894,-228.406222432435,
16.138055619095));
#82538=CARTESIAN_POINT('Ctrl Pts',(-2.98397252246004,-226.658050020319,
15.9792977538632));
#82539=CARTESIAN_POINT('Ctrl Pts',(-3.01146833420773,-223.392430295024,
15.8205398886314));
#82540=CARTESIAN_POINT('Ctrl Pts',(-0.282868445008073,-221.5980583004,15.6617820233996));
#82541=CARTESIAN_POINT('Ctrl Pts',(2.70461263398692,-222.917143215525,15.5030241581679));
#82542=CARTESIAN_POINT('Ctrl Pts',(3.21683233669003,-226.142458577869,15.344266292936));
#82543=CARTESIAN_POINT('Ctrl Pts',(0.785007211364801,-228.322195894686,
15.1855084277043));
#82544=CARTESIAN_POINT('Ctrl Pts',(-2.36525648293751,-227.461459659322,
15.0267505624725));
#82545=CARTESIAN_POINT('Ctrl Pts',(-3.35083753706407,-224.347995640544,
14.8679926972407));
#82546=CARTESIAN_POINT('Ctrl Pts',(-1.26973220903945,-221.831245985899,
14.7092348320089));
#82547=CARTESIAN_POINT('Ctrl Pts',(1.97343198676774,-222.214539880352,14.5504769667771));
#82548=CARTESIAN_POINT('Ctrl Pts',(3.41051130588809,-225.14708676677,14.3917191015453));
#82549=CARTESIAN_POINT('Ctrl Pts',(1.72629081197493,-227.945019850025,14.2329612363135));
#82550=CARTESIAN_POINT('Ctrl Pts',(-1.53783096517303,-228.047670882347,
14.0742033710817));
#82551=CARTESIAN_POINT('Ctrl Pts',(-3.39452990346833,-225.361093642992,
13.9154455058499));
#82552=CARTESIAN_POINT('Ctrl Pts',(-2.14455520759608,-222.34404351577,13.7566876406181));
#82553=CARTESIAN_POINT('Ctrl Pts',(1.06811632993552,-221.757724658473,13.5979297753863));
#82554=CARTESIAN_POINT('Ctrl Pts',(3.30324784431278,-224.138736066242,13.4391719101545));
#82555=CARTESIAN_POINT('Ctrl Pts',(2.51524706147206,-227.307976192318,13.2804140449227));
#82556=CARTESIAN_POINT('Ctrl Pts',(-0.574707733118198,-228.364956597944,
13.121656179691));
#82557=CARTESIAN_POINT('Ctrl Pts',(-3.13869003295852,-226.342328857455,
12.9628983144591));
#82558=CARTESIAN_POINT('Ctrl Pts',(-2.83014333806119,-223.091201799409,
12.8041404492274));
#82559=CARTESIAN_POINT('Ctrl Pts',(0.0685504285370491,-221.587006779483,
12.6453825839956));
#82560=CARTESIAN_POINT('Ctrl Pts',(2.90450684563386,-223.206383020761,12.4866247187638));
#82561=CARTESIAN_POINT('Ctrl Pts',(3.08225871182353,-226.467277450906,12.327866853532));
#82562=CARTESIAN_POINT('Ctrl Pts',(0.439127526159182,-228.385319615682,
12.1691089883002));
#82563=CARTESIAN_POINT('Ctrl Pts',(-2.60589315417777,-227.20511740131,12.0103511230684));
#82564=CARTESIAN_POINT('Ctrl Pts',(-3.2660005222855,-224.006791827973,11.8515932578366));
#82565=CARTESIAN_POINT('Ctrl Pts',(-0.937064340829889,-221.717450334619,
11.6928353926048));
#82566=CARTESIAN_POINT('Ctrl Pts',(2.24947308850407,-222.432298165938,11.534077527373));
#82567=CARTESIAN_POINT('Ctrl Pts',(3.3772928356975,-225.497106614819,11.3753196621412));
#82568=CARTESIAN_POINT('Ctrl Pts',(1.41421431246939,-228.106963109365,11.2165617969094));
#82569=CARTESIAN_POINT('Ctrl Pts',(-1.84315309391807,-227.8733270884,11.0578039316776));
#82570=CARTESIAN_POINT('Ctrl Pts',(-3.41366686123195,-225.010022229121,
10.8990460664459));
#82571=CARTESIAN_POINT('Ctrl Pts',(-1.85999285138554,-222.137545026145,
10.7402882012141));
#82572=CARTESIAN_POINT('Ctrl Pts',(1.39594654290646,-221.884786502678,10.5815303359823));
#82573=CARTESIAN_POINT('Ctrl Pts',(3.37431571602475,-224.483071249457,10.4227724707505));
#82574=CARTESIAN_POINT('Ctrl Pts',(2.26451127852891,-227.554449168405,10.2640146055187));
#82575=CARTESIAN_POINT('Ctrl Pts',(-0.917773792026828,-228.28799530888,
10.1052567402869));
#82576=CARTESIAN_POINT('Ctrl Pts',(-3.2601123242102,-226.012368271965,9.9464988750551));
#82577=CARTESIAN_POINT('Ctrl Pts',(-2.61879618547721,-222.810221832358,
9.7877410098233));
#82578=CARTESIAN_POINT('Ctrl Pts',(0.419242119222859,-221.612160285666,
9.62898314459151));
#82579=CARTESIAN_POINT('Ctrl Pts',(3.07359005289646,-223.514649512308,9.47022527935973));
#82580=CARTESIAN_POINT('Ctrl Pts',(2.91498849102523,-226.776531446877,9.31146741412793));
#82581=CARTESIAN_POINT('Ctrl Pts',(0.0885895767968314,-228.412531871123,
9.15270954889614));
#82582=CARTESIAN_POINT('Ctrl Pts',(-2.81888651463232,-226.925383261113,
8.99395168366434));
#82583=CARTESIAN_POINT('Ctrl Pts',(-3.14651777871999,-223.676123966246,
8.83519381843255));
#82584=CARTESIAN_POINT('Ctrl Pts',(-0.594456095456926,-221.63847596541,
8.67643595320076));
#82585=CARTESIAN_POINT('Ctrl Pts',(2.50165178299187,-222.677294628843,8.51767808796896));
#82586=CARTESIAN_POINT('Ctrl Pts',(3.30824804802161,-225.84185315662,8.35892022273718));
#82587=CARTESIAN_POINT('Ctrl Pts',(1.08713582959566,-228.235947708564,8.20016235750538));
#82588=CARTESIAN_POINT('Ctrl Pts',(-2.12892305732567,-227.66850304488,8.04140449227359));
#82589=CARTESIAN_POINT('Ctrl Pts',(-3.3965916459004,-224.658844499459,7.8826466270418));
#82590=CARTESIAN_POINT('Ctrl Pts',(-1.55569969371482,-221.961411454717,
7.72388876181));
#82591=CARTESIAN_POINT('Ctrl Pts',(1.70896855698215,-222.044894527128,7.56513089657821));
#82592=CARTESIAN_POINT('Ctrl Pts',(3.40958885153262,-224.832890012105,7.40637303134642));
#82593=CARTESIAN_POINT('Ctrl Pts',(1.98975356323926,-227.773824551432,7.24761516611463));
#82594=CARTESIAN_POINT('Ctrl Pts',(-1.25110410788551,-228.176154970366,
7.08885730088283));
#82595=CARTESIAN_POINT('Ctrl Pts',(-3.34695134867194,-225.671668485321,
6.93009943565104));
#82596=CARTESIAN_POINT('Ctrl Pts',(-2.37966884676946,-222.552471028922,
6.77134157041925));
#82597=CARTESIAN_POINT('Ctrl Pts',(0.765486490118206,-221.673251990608,
6.61258370518745));
#82598=CARTESIAN_POINT('Ctrl Pts',(3.21006862135173,-223.838672599668,6.45382583995566));
#82599=CARTESIAN_POINT('Ctrl Pts',(2.71679607655705,-227.066939999844,6.29506797472387));
#82600=CARTESIAN_POINT('Ctrl Pts',(-0.262888130667251,-228.403543993443,
6.13631010949208));
#82601=CARTESIAN_POINT('Ctrl Pts',(-3.00197713104269,-226.625224658085,
5.97755224426029));
#82602=CARTESIAN_POINT('Ctrl Pts',(-2.99365677913774,-223.359499779557,
5.81879437902849));
#82603=CARTESIAN_POINT('Ctrl Pts',(-0.245541860688655,-221.595160638268,
5.66003651379671));
#82604=CARTESIAN_POINT('Ctrl Pts',(2.72729295900699,-222.946930346944,5.50127864856491));
#82605=CARTESIAN_POINT('Ctrl Pts',(3.20410936986766,-226.177669321362,5.34252078333311));
#82606=CARTESIAN_POINT('Ctrl Pts',(0.748525011423917,-228.33060537918,5.18376291810133));
#82607=CARTESIAN_POINT('Ctrl Pts',(-2.39210940803985,-227.435371524945,
5.02500505286953));
#82608=CARTESIAN_POINT('Ctrl Pts',(-3.34348539133322,-224.311285746851,
4.86624718763774));
#82609=CARTESIAN_POINT('Ctrl Pts',(-1.23490367595725,-221.817511226152,
4.70748932240594));
#82610=CARTESIAN_POINT('Ctrl Pts',(2.00386183509223,-222.236350306138,4.54873145717416));
#82611=CARTESIAN_POINT('Ctrl Pts',(3.4086930734676,-225.184481477252,4.38997359194236));
#82612=CARTESIAN_POINT('Ctrl Pts',(1.69388854504428,-227.963775207674,4.23121572671057));
#82613=CARTESIAN_POINT('Ctrl Pts',(-1.57116271318341,-228.03062198451,4.07245786147877));
#82614=CARTESIAN_POINT('Ctrl Pts',(-3.3982859181096,-225.323843640441,3.91369999624699));
#82615=CARTESIAN_POINT('Ctrl Pts',(-2.11529798437666,-222.320683609087,
3.75494213101519));
#82616=CARTESIAN_POINT('Ctrl Pts',(1.10361058139527,-221.76963383392,3.5961842657834));
#82617=CARTESIAN_POINT('Ctrl Pts',(3.31249478663612,-224.17501504573,3.4374264005516));
#82618=CARTESIAN_POINT('Ctrl Pts',(2.48978389307636,-227.33542245766,3.27866853531981));
#82619=CARTESIAN_POINT('Ctrl Pts',(-0.611577120844398,-228.358451323275,
3.11991067008802));
#82620=CARTESIAN_POINT('Ctrl Pts',(-3.1532227791871,-226.307825679854,2.96115280485623));
#82621=CARTESIAN_POINT('Ctrl Pts',(-2.80903907123482,-223.060278005436,
2.80239493962444));
#82622=CARTESIAN_POINT('Ctrl Pts',(0.105977078601933,-221.587963865238,
2.64363707439264));
#82623=CARTESIAN_POINT('Ctrl Pts',(2.92400302173803,-223.238344977983,2.48487920916086));
#82624=CARTESIAN_POINT('Ctrl Pts',(3.06598149107159,-226.500992867014,2.32612134392906));
#82625=CARTESIAN_POINT('Ctrl Pts',(0.401973867646657,-228.389931799117,
2.16736347869727));
#82626=CARTESIAN_POINT('Ctrl Pts',(-2.62992031971121,-227.176405980739,
2.00860561346547));
#82627=CARTESIAN_POINT('Ctrl Pts',(-3.25491133877711,-223.971032075231,
1.84984774823368));
#82628=CARTESIAN_POINT('Ctrl Pts',(-0.901008024848114,-221.707372456188,
1.69108988300189));
#82629=CARTESIAN_POINT('Ctrl Pts',(2.2774986027622,-222.457119582258,1.53233201777009));
#82630=CARTESIAN_POINT('Ctrl Pts',(3.37163696425009,-225.534122654706,1.37357415253831));
#82631=CARTESIAN_POINT('Ctrl Pts',(1.38005662806585,-228.12227255076,1.21481628730651));
#82632=CARTESIAN_POINT('Ctrl Pts',(-1.87455822137116,-227.852967765532,
1.05605842207472));
#82633=CARTESIAN_POINT('Ctrl Pts',(-3.41356376877976,-224.97252740804,0.897300556842932));
#82634=CARTESIAN_POINT('Ctrl Pts',(-1.82850369573622,-222.117432216889,
0.738542691611134));
#82635=CARTESIAN_POINT('Ctrl Pts',(1.43005935989245,-221.900052186656,0.579784826379344));
#82636=CARTESIAN_POINT('Ctrl Pts',(3.37971747316782,-224.520578545184,0.421026961147552));
#82637=CARTESIAN_POINT('Ctrl Pts',(2.23649101368354,-227.578176481406,0.262269095915755));
#82638=CARTESIAN_POINT('Ctrl Pts',(-0.954039042100929,-228.279681514165,
0.103511230683968));
#82639=CARTESIAN_POINT('Ctrl Pts',(-3.27049270054663,-225.972504524796,
-0.0552466345478283));
#82640=CARTESIAN_POINT('Ctrl Pts',(-2.81925737956186,-223.853043319762,
-0.161085211369022));
#82641=CARTESIAN_POINT('Ctrl Pts',(-2.19519710401913,-223.123136560921,
-0.21400449977962));
#82642=CARTESIAN_POINT('Ctrl Pts',(-0.698066426161038,-227.611132185939,
20.2140044997796));
#82643=CARTESIAN_POINT('Ctrl Pts',(-1.56627230491967,-227.379023915733,
20.161085211369));
#82644=CARTESIAN_POINT('Ctrl Pts',(-3.03778533319432,-225.983650973587,
20.0552466345478));
#82645=CARTESIAN_POINT('Ctrl Pts',(-2.47430970641492,-222.976375369272,
19.896488769316));
#82646=CARTESIAN_POINT('Ctrl Pts',(0.358151943839997,-221.826111965074,
19.7377309040843));
#82647=CARTESIAN_POINT('Ctrl Pts',(2.86064170592173,-223.578174499175,19.5789730388525));
#82648=CARTESIAN_POINT('Ctrl Pts',(2.74615023855165,-226.632675463776,19.4202151736207));
#82649=CARTESIAN_POINT('Ctrl Pts',(0.117851501550342,-228.192369288497,
19.2614573083889));
#82650=CARTESIAN_POINT('Ctrl Pts',(-2.61804363116637,-226.830693717159,
19.1026994431571));
#82651=CARTESIAN_POINT('Ctrl Pts',(-2.95803399248552,-223.793426087799,
18.9439415779253));
#82652=CARTESIAN_POINT('Ctrl Pts',(-0.590768411472084,-221.860484399872,
18.7851837126935));
#82653=CARTESIAN_POINT('Ctrl Pts',(2.31713720451145,-222.800793023077,18.6264258474617));
#82654=CARTESIAN_POINT('Ctrl Pts',(3.10441430051404,-225.753832645653,18.4676679822299));
#82655=CARTESIAN_POINT('Ctrl Pts',(1.05052398848132,-228.016956358674,18.3089101169981));
#82656=CARTESIAN_POINT('Ctrl Pts',(-1.96480211294228,-227.518965818607,
18.1501522517663));
#82657=CARTESIAN_POINT('Ctrl Pts',(-3.1819432312892,-224.715615847668,17.9913943865345));
#82658=CARTESIAN_POINT('Ctrl Pts',(-1.48696912673618,-222.172535232803,
17.8326365213027));
#82659=CARTESIAN_POINT('Ctrl Pts',(1.56887861963092,-222.217149773714,17.673878656071));
#82660=CARTESIAN_POINT('Ctrl Pts',(3.1888889338723,-224.808628972561,17.5151207908391));
#82661=CARTESIAN_POINT('Ctrl Pts',(1.89042811346746,-227.575250809889,17.3563629256074));
#82662=CARTESIAN_POINT('Ctrl Pts',(-1.13815238898098,-227.985003265527,
17.1976050603756));
#82663=CARTESIAN_POINT('Ctrl Pts',(-3.12509589591799,-225.662880821255,
17.0388471951438));
#82664=CARTESIAN_POINT('Ctrl Pts',(-2.25195174893761,-222.73408988956,16.880089329912));
#82665=CARTESIAN_POINT('Ctrl Pts',(0.682178543780247,-221.879059794881,
16.7213314646802));
#82666=CARTESIAN_POINT('Ctrl Pts',(2.9919790631754,-223.880314056623,16.5625735994484));
#82667=CARTESIAN_POINT('Ctrl Pts',(2.56352046007342,-226.906304848026,16.4038157342166));
#82668=CARTESIAN_POINT('Ctrl Pts',(-0.211071966523578,-228.18764551831,
16.2450578689848));
#82669=CARTESIAN_POINT('Ctrl Pts',(-2.79249133803074,-226.551653135178,
16.086300003753));
#82670=CARTESIAN_POINT('Ctrl Pts',(-2.81822274660089,-223.49558786395,15.9275421385212));
#82671=CARTESIAN_POINT('Ctrl Pts',(-0.264716808396092,-221.816360520376,
15.7687842732894));
#82672=CARTESIAN_POINT('Ctrl Pts',(2.5310579424875,-223.050799903409,15.6100264080577));
#82673=CARTESIAN_POINT('Ctrl Pts',(3.01040856391611,-226.069147138167,15.4512685428258));
#82674=CARTESIAN_POINT('Ctrl Pts',(0.73463338604091,-228.10901095413,15.2925106775941));
#82675=CARTESIAN_POINT('Ctrl Pts',(-2.21347823785548,-227.303508067126,
15.1337528123623));
#82676=CARTESIAN_POINT('Ctrl Pts',(-3.13581466550684,-224.389834687674,
14.9749949471305));
#82677=CARTESIAN_POINT('Ctrl Pts',(-1.18825363460054,-222.034584578067,
14.8162370818987));
#82678=CARTESIAN_POINT('Ctrl Pts',(1.84679707596586,-222.393282546002,14.6574792166669));
#82679=CARTESIAN_POINT('Ctrl Pts',(3.19165917523153,-225.137648225328,14.4987213514351));
#82680=CARTESIAN_POINT('Ctrl Pts',(1.61551492283441,-227.756038254248,14.3399634862033));
#82681=CARTESIAN_POINT('Ctrl Pts',(-1.43914852341226,-227.852102181258,
14.1812056209715));
#82682=CARTESIAN_POINT('Ctrl Pts',(-3.17670329762513,-225.337922304137,
14.0224477557397));
#82683=CARTESIAN_POINT('Ctrl Pts',(-2.00693933877233,-222.514475947559,
13.8636898905079));
#82684=CARTESIAN_POINT('Ctrl Pts',(0.999575424003943,-221.965781106033,
13.7049320252761));
#82685=CARTESIAN_POINT('Ctrl Pts',(3.09127879803915,-224.194003276949,13.5461741600443));
#82686=CARTESIAN_POINT('Ctrl Pts',(2.35384393767052,-227.159873617105,13.3874162948125));
#82687=CARTESIAN_POINT('Ctrl Pts',(-0.537828801891506,-228.149027707822,
13.2286584295808));
#82688=CARTESIAN_POINT('Ctrl Pts',(-2.93728064311203,-226.256191764173,
13.069900564349));
#82689=CARTESIAN_POINT('Ctrl Pts',(-2.64853335526218,-223.213689167351,
12.9111426991172));
#82690=CARTESIAN_POINT('Ctrl Pts',(0.0641515551725655,-221.806018174325,
12.7523848338854));
#82691=CARTESIAN_POINT('Ctrl Pts',(2.71812496483608,-223.321479222556,12.5936269686536));
#82692=CARTESIAN_POINT('Ctrl Pts',(2.88447051356929,-226.373122420298,12.4348691034218));
#82693=CARTESIAN_POINT('Ctrl Pts',(0.410948761712932,-228.16808403298,12.27611123819));
#82694=CARTESIAN_POINT('Ctrl Pts',(-2.43867328070292,-227.063615263261,
12.1173533729582));
#82695=CARTESIAN_POINT('Ctrl Pts',(-3.05642163251797,-224.070525885755,
11.9585955077264));
#82696=CARTESIAN_POINT('Ctrl Pts',(-0.876933026443435,-221.928091181056,
11.7998376424946));
#82697=CARTESIAN_POINT('Ctrl Pts',(2.10512465094758,-222.597067306654,11.6410797772628));
#82698=CARTESIAN_POINT('Ctrl Pts',(3.16057233057339,-225.46520733871,11.482321912031));
#82699=CARTESIAN_POINT('Ctrl Pts',(1.32346433754493,-227.907589632672,11.3235640467992));
#82700=CARTESIAN_POINT('Ctrl Pts',(-1.72487816516068,-227.688946009151,
11.1648061815675));
#82701=CARTESIAN_POINT('Ctrl Pts',(-3.19461223894042,-225.009379103795,
11.0060483163357));
#82702=CARTESIAN_POINT('Ctrl Pts',(-1.74063731726696,-222.321228443015,
10.8472904511039));
#82703=CARTESIAN_POINT('Ctrl Pts',(1.30636880872031,-222.084689405847,10.6885325858721));
#82704=CARTESIAN_POINT('Ctrl Pts',(3.15778625233847,-224.516242509807,10.5297747206403));
#82705=CARTESIAN_POINT('Ctrl Pts',(2.11919784199338,-227.390530449768,10.3710168554085));
#82706=CARTESIAN_POINT('Ctrl Pts',(-0.858880350008606,-228.077005016107,
10.2122589901767));
#82707=CARTESIAN_POINT('Ctrl Pts',(-3.05091127945738,-225.947404712705,
10.0535011249449));
#82708=CARTESIAN_POINT('Ctrl Pts',(-2.45074832592093,-222.950739653492,
9.89474325971312));
#82709=CARTESIAN_POINT('Ctrl Pts',(0.392339399125002,-221.829557582818,
9.73598539448132));
#82710=CARTESIAN_POINT('Ctrl Pts',(2.87635812152011,-223.609964287674,9.57722752924953));
#82711=CARTESIAN_POINT('Ctrl Pts',(2.72793400421006,-226.66253162179,9.41846966401774));
#82712=CARTESIAN_POINT('Ctrl Pts',(0.0829047935203504,-228.193550081021,
9.25971179878595));
#82713=CARTESIAN_POINT('Ctrl Pts',(-2.63799888093902,-226.801831631685,
9.10095393355415));
#82714=CARTESIAN_POINT('Ctrl Pts',(-2.94460608329979,-223.761076943886,
8.94219606832236));
#82715=CARTESIAN_POINT('Ctrl Pts',(-0.556309914018403,-221.854184588324,
8.78343820309057));
#82716=CARTESIAN_POINT('Ctrl Pts',(2.34112106669625,-222.826342373821,8.62468033785877));
#82717=CARTESIAN_POINT('Ctrl Pts',(3.09595813923287,-225.78783153332,8.46592247262699));
#82718=CARTESIAN_POINT('Ctrl Pts',(1.01737444448917,-228.028297304506,8.30716460739519));
#82719=CARTESIAN_POINT('Ctrl Pts',(-1.99231030184375,-227.497265501692,
8.14840674216339));
#82720=CARTESIAN_POINT('Ctrl Pts',(-3.17863273827496,-224.680736409933,
7.98964887693161));
#82721=CARTESIAN_POINT('Ctrl Pts',(-1.45587061763363,-222.156397343248,
7.83089101169982));
#82722=CARTESIAN_POINT('Ctrl Pts',(1.59930423501526,-222.234523316201,7.67213314646802));
#82723=CARTESIAN_POINT('Ctrl Pts',(3.19079591466932,-224.843613441417,7.51337528123624));
#82724=CARTESIAN_POINT('Ctrl Pts',(1.862071298693,-227.595828538898,7.35461741600443));
#82725=CARTESIAN_POINT('Ctrl Pts',(-1.17082089662297,-227.972341459659,
7.19585955077264));
#82726=CARTESIAN_POINT('Ctrl Pts',(-3.13217785339102,-225.628567593424,
7.03710168554085));
#82727=CARTESIAN_POINT('Ctrl Pts',(-2.2269657619055,-222.709528690405,6.87834382030906));
#82728=CARTESIAN_POINT('Ctrl Pts',(0.716365307302614,-221.886729039857,
6.71958595507727));
#82729=CARTESIAN_POINT('Ctrl Pts',(3.00407887543776,-223.913194849605,6.56082808984548));
#82730=CARTESIAN_POINT('Ctrl Pts',(2.54245957490482,-226.934304690257,6.40207022461368));
#82731=CARTESIAN_POINT('Ctrl Pts',(-0.246018628601239,-228.18513895445,
6.24331235938189));
#82732=CARTESIAN_POINT('Ctrl Pts',(-2.80934059288588,-226.520934172783,
6.08455449415009));
#82733=CARTESIAN_POINT('Ctrl Pts',(-2.80155415703599,-223.464770495994,
5.9257966289183));
#82734=CARTESIAN_POINT('Ctrl Pts',(-0.22978546683524,-221.8136488009,5.76703876368652));
#82735=CARTESIAN_POINT('Ctrl Pts',(2.55228287357704,-223.078675597922,5.60828089845472));
#82736=CARTESIAN_POINT('Ctrl Pts',(2.99850202845772,-226.102098412171,5.44952303322292));
#82737=CARTESIAN_POINT('Ctrl Pts',(0.700492244807063,-228.116880802941,
5.29076516799113));
#82738=CARTESIAN_POINT('Ctrl Pts',(-2.23860801374472,-227.279094005426,
5.13200730275934));
#82739=CARTESIAN_POINT('Ctrl Pts',(-3.1289343061487,-224.355480463771,4.97324943752755));
#82740=CARTESIAN_POINT('Ctrl Pts',(-1.15566004460723,-222.021731176323,
4.81449157229576));
#82741=CARTESIAN_POINT('Ctrl Pts',(1.87527424431247,-222.413693399195,4.65573370706397));
#82742=CARTESIAN_POINT('Ctrl Pts',(3.18995761858296,-225.172643321403,4.49697584183217));
#82743=CARTESIAN_POINT('Ctrl Pts',(1.58519190576392,-227.773590082685,4.33821797660038));
#82744=CARTESIAN_POINT('Ctrl Pts',(-1.4703413768651,-227.836147309296,4.17946011136858));
#82745=CARTESIAN_POINT('Ctrl Pts',(-3.1802182892252,-225.303062630102,4.0207022461368));
#82746=CARTESIAN_POINT('Ctrl Pts',(-1.9795595483084,-222.492615043485,3.861944380905));
#82747=CARTESIAN_POINT('Ctrl Pts',(1.03279201330066,-221.976926071019,3.70318651567321));
#82748=CARTESIAN_POINT('Ctrl Pts',(3.09993236510347,-224.227954238364,3.54442865044142));
#82749=CARTESIAN_POINT('Ctrl Pts',(2.33001473795483,-227.185558658658,3.38567078520963));
#82750=CARTESIAN_POINT('Ctrl Pts',(-0.572332285113605,-228.142939875904,
3.22691291997783));
#82751=CARTESIAN_POINT('Ctrl Pts',(-2.95088082463369,-226.223902651636,
3.06815505474604));
#82752=CARTESIAN_POINT('Ctrl Pts',(-2.62878334688759,-223.184749749793,
2.90939718951425));
#82753=CARTESIAN_POINT('Ctrl Pts',(0.0991765412711432,-221.806913843993,
2.75063932428246));
#82754=CARTESIAN_POINT('Ctrl Pts',(2.73637007349101,-223.351390184544,2.59188145905066));
#82755=CARTESIAN_POINT('Ctrl Pts',(2.86923780026014,-226.404674321909,2.43312359381887));
#82756=CARTESIAN_POINT('Ctrl Pts',(0.376179249329203,-228.172400253118,
2.27436572858708));
#82757=CARTESIAN_POINT('Ctrl Pts',(-2.46115862570008,-227.03674625135,2.11560786335528));
#82758=CARTESIAN_POINT('Ctrl Pts',(-3.04604404068027,-224.037060832363,
1.95684999812349));
#82759=CARTESIAN_POINT('Ctrl Pts',(-0.843190440242474,-221.918659998961,
1.7980921328917));
#82760=CARTESIAN_POINT('Ctrl Pts',(2.13135177107707,-222.620295935454,1.6393342676599));
#82761=CARTESIAN_POINT('Ctrl Pts',(3.15527939576685,-225.499848063441,1.48057640242812));
#82762=CARTESIAN_POINT('Ctrl Pts',(1.29149854794529,-227.921916668918,1.32181853719632));
#82763=CARTESIAN_POINT('Ctrl Pts',(-1.75426802908282,-227.669893141764,
1.16306067196453));
#82764=CARTESIAN_POINT('Ctrl Pts',(-3.19451576191941,-224.974290321206,
1.00430280673274));
#82765=CARTESIAN_POINT('Ctrl Pts',(-1.71116881722859,-222.302406270488,
0.845544941500944));
#82766=CARTESIAN_POINT('Ctrl Pts',(1.33829261003958,-222.098975492584,0.686787076269154));
#82767=CARTESIAN_POINT('Ctrl Pts',(3.16284137932728,-224.551342966544,0.528029211037361));
#82768=CARTESIAN_POINT('Ctrl Pts',(2.09297563442241,-227.412735183736,0.369271345805565));
#82769=CARTESIAN_POINT('Ctrl Pts',(-0.892818463024459,-228.069224716672,
0.210513480573778));
#82770=CARTESIAN_POINT('Ctrl Pts',(-3.0606255482004,-225.910099017751,0.0517556153419817));
#82771=CARTESIAN_POINT('Ctrl Pts',(-2.63834594750734,-223.926643402192,
-0.0540829614792118));
#82772=CARTESIAN_POINT('Ctrl Pts',(-2.0543315503421,-223.243574678773,-0.10700224988981));
#82773=CARTESIAN_POINT('Ctrl Pts',(-0.65019999797512,-227.432086802035,
20.3210067496694));
#82774=CARTESIAN_POINT('Ctrl Pts',(-1.45887298303087,-227.215894200354,
20.2680874612588));
#82775=CARTESIAN_POINT('Ctrl Pts',(-2.82948433482767,-225.916202007525,
20.1622488844376));
#82776=CARTESIAN_POINT('Ctrl Pts',(-2.30464624254778,-223.115135348884,
20.0034910192059));
#82777=CARTESIAN_POINT('Ctrl Pts',(0.333593458204553,-222.0437455283,19.844733153974));
#82778=CARTESIAN_POINT('Ctrl Pts',(2.66448744946339,-223.675669100946,19.6859752887423));
#82779=CARTESIAN_POINT('Ctrl Pts',(2.55784666419947,-226.520722876015,19.5272174235105));
#82780=CARTESIAN_POINT('Ctrl Pts',(0.109770421836213,-227.97346846536,19.3684595582787));
#82781=CARTESIAN_POINT('Ctrl Pts',(-2.43852432933144,-226.705163013978,
19.2097016930469));
#82782=CARTESIAN_POINT('Ctrl Pts',(-2.75520154507576,-223.876160884024,
19.0509438278151));
#82783=CARTESIAN_POINT('Ctrl Pts',(-0.550259410204463,-222.075761044586,
18.8921859625833));
#82784=CARTESIAN_POINT('Ctrl Pts',(2.1582510621043,-222.951592687525,18.7334280973515));
#82785=CARTESIAN_POINT('Ctrl Pts',(2.89154455258461,-225.702142326731,18.5746702321197));
#82786=CARTESIAN_POINT('Ctrl Pts',(0.978489538509605,-227.810083603489,
18.4159123668879));
#82787=CARTESIAN_POINT('Ctrl Pts',(-1.83007559449918,-227.346240284273,
18.2571545016561));
#82788=CARTESIAN_POINT('Ctrl Pts',(-2.96375732309449,-224.735116074429,
18.0983966364243));
#82789=CARTESIAN_POINT('Ctrl Pts',(-1.38500762529136,-222.366414545939,
17.9396387711926));
#82790=CARTESIAN_POINT('Ctrl Pts',(1.46130058269256,-222.407969866927,17.7808809059608));
#82791=CARTESIAN_POINT('Ctrl Pts',(2.97022675871869,-224.821751287571,17.6221230407289));
#82792=CARTESIAN_POINT('Ctrl Pts',(1.76080142159005,-227.398665812627,17.4633651754972));
#82793=CARTESIAN_POINT('Ctrl Pts',(-1.06010925791193,-227.780321534549,
17.3046073102654));
#82794=CARTESIAN_POINT('Ctrl Pts',(-2.91080801059636,-225.61742707067,17.1458494450336));
#82795=CARTESIAN_POINT('Ctrl Pts',(-2.09753537446523,-222.889463389148,
16.9870915798018));
#82796=CARTESIAN_POINT('Ctrl Pts',(0.635401547992891,-222.093062724406,
16.82833371457));
#82797=CARTESIAN_POINT('Ctrl Pts',(2.78681900161956,-223.957090943164,16.6695758493382));
#82798=CARTESIAN_POINT('Ctrl Pts',(2.38773981312259,-226.775589488157,16.5108179841064));
#82799=CARTESIAN_POINT('Ctrl Pts',(-0.196598757744262,-227.969068604185,
16.3520601188746));
#82800=CARTESIAN_POINT('Ctrl Pts',(-2.60101015360142,-226.445256250038,
16.1933022536428));
#82801=CARTESIAN_POINT('Ctrl Pts',(-2.62497715899404,-223.598745432877,
16.034544388411));
#82802=CARTESIAN_POINT('Ctrl Pts',(-0.246565171784112,-222.034662740351,
15.8757865231792));
#82803=CARTESIAN_POINT('Ctrl Pts',(2.35750325098809,-223.184456591293,15.7170286579475));
#82804=CARTESIAN_POINT('Ctrl Pts',(2.80398479114218,-225.995835698465,15.5582707927156));
#82805=CARTESIAN_POINT('Ctrl Pts',(0.684259560717021,-227.895826013575,
15.3995129274839));
#82806=CARTESIAN_POINT('Ctrl Pts',(-2.06169999277346,-227.14555647493,15.2407550622521));
#82807=CARTESIAN_POINT('Ctrl Pts',(-2.9207917939496,-224.431673734804,15.0819971970203));
#82808=CARTESIAN_POINT('Ctrl Pts',(-1.10677506016163,-222.237923170235,
14.9232393317885));
#82809=CARTESIAN_POINT('Ctrl Pts',(1.72016216516399,-222.572025211652,14.7644814665567));
#82810=CARTESIAN_POINT('Ctrl Pts',(2.97280704457497,-225.128209683886,14.6057236013249));
#82811=CARTESIAN_POINT('Ctrl Pts',(1.50473903369388,-227.56705665847,14.4469657360931));
#82812=CARTESIAN_POINT('Ctrl Pts',(-1.34046608165149,-227.656533480169,
14.2882078708613));
#82813=CARTESIAN_POINT('Ctrl Pts',(-2.95887669178193,-225.314750965283,
14.1294500056295));
#82814=CARTESIAN_POINT('Ctrl Pts',(-1.86932346994857,-222.684908379347,
13.9706921403977));
#82815=CARTESIAN_POINT('Ctrl Pts',(0.931034518072369,-222.173837553594,
13.8119342751659));
#82816=CARTESIAN_POINT('Ctrl Pts',(2.87930975176552,-224.249270487656,13.6531764099341));
#82817=CARTESIAN_POINT('Ctrl Pts',(2.19244081386897,-227.011771041893,13.4944185447024));
#82818=CARTESIAN_POINT('Ctrl Pts',(-0.50094987066481,-227.933098817701,
13.3356606794706));
#82819=CARTESIAN_POINT('Ctrl Pts',(-2.73587125326554,-226.17005467089,13.1769028142388));
#82820=CARTESIAN_POINT('Ctrl Pts',(-2.46692337246317,-223.336176535292,
13.018144949007));
#82821=CARTESIAN_POINT('Ctrl Pts',(0.059752681808081,-222.025029569166,
12.8593870837752));
#82822=CARTESIAN_POINT('Ctrl Pts',(2.53174308403829,-223.436575424352,12.7006292185434));
#82823=CARTESIAN_POINT('Ctrl Pts',(2.68668231531504,-226.27896738969,12.5418713533116));
#82824=CARTESIAN_POINT('Ctrl Pts',(0.382769997266682,-227.950848450278,
12.3831134880798));
#82825=CARTESIAN_POINT('Ctrl Pts',(-2.27145340722807,-226.922113125211,
12.224355622848));
#82826=CARTESIAN_POINT('Ctrl Pts',(-2.84684274275044,-224.134259943536,
12.0655977576162));
#82827=CARTESIAN_POINT('Ctrl Pts',(-0.816801712056979,-222.138732027492,
11.9068398923844));
#82828=CARTESIAN_POINT('Ctrl Pts',(1.96077621339108,-222.761836447371,11.7480820271526));
#82829=CARTESIAN_POINT('Ctrl Pts',(2.94385182544929,-225.433308062602,11.5893241619208));
#82830=CARTESIAN_POINT('Ctrl Pts',(1.23271436262047,-227.708216155979,11.4305662966891));
#82831=CARTESIAN_POINT('Ctrl Pts',(-1.60660323640329,-227.504564929902,
11.2718084314573));
#82832=CARTESIAN_POINT('Ctrl Pts',(-2.97555761664889,-225.008735978468,
11.1130505662255));
#82833=CARTESIAN_POINT('Ctrl Pts',(-1.62128178314839,-222.504911859884,
10.9542927009937));
#82834=CARTESIAN_POINT('Ctrl Pts',(1.21679107453415,-222.284592309017,10.7955348357619));
#82835=CARTESIAN_POINT('Ctrl Pts',(2.94125678865219,-224.549413770157,10.6367769705301));
#82836=CARTESIAN_POINT('Ctrl Pts',(1.97388440545785,-227.22661173113,10.4780191052983));
#82837=CARTESIAN_POINT('Ctrl Pts',(-0.799986907990383,-227.866014723333,
10.3192612400665));
#82838=CARTESIAN_POINT('Ctrl Pts',(-2.84171023470455,-225.882441153445,
10.1605033748347));
#82839=CARTESIAN_POINT('Ctrl Pts',(-2.28270046636465,-223.091257474625,
10.0017455096029));
#82840=CARTESIAN_POINT('Ctrl Pts',(0.365436679027144,-222.046954879969,
9.84298764437113));
#82841=CARTESIAN_POINT('Ctrl Pts',(2.67912619014375,-223.70527906304,9.68422977913934));
#82842=CARTESIAN_POINT('Ctrl Pts',(2.54087951739489,-226.548531796703,9.52547191390754));
#82843=CARTESIAN_POINT('Ctrl Pts',(0.0772200102438696,-227.974568290918,
9.36671404867575));
#82844=CARTESIAN_POINT('Ctrl Pts',(-2.45711124724573,-226.678280002257,
9.20795618344397));
#82845=CARTESIAN_POINT('Ctrl Pts',(-2.74269438787959,-223.846029921527,
9.04919831821217));
#82846=CARTESIAN_POINT('Ctrl Pts',(-0.518163732579882,-222.069893211237,
8.89044045298037));
#82847=CARTESIAN_POINT('Ctrl Pts',(2.18059035040062,-222.975390118799,8.73168258774859));
#82848=CARTESIAN_POINT('Ctrl Pts',(2.88366823044413,-225.733809910021,8.57292472251679));
#82849=CARTESIAN_POINT('Ctrl Pts',(0.947613059382676,-227.820646900448,
8.41416685728501));
#82850=CARTESIAN_POINT('Ctrl Pts',(-1.85569754636184,-227.326027958504,
8.2554089920532));
#82851=CARTESIAN_POINT('Ctrl Pts',(-2.96067383064952,-224.702628320407,
8.09665112682142));
#82852=CARTESIAN_POINT('Ctrl Pts',(-1.35604154155244,-222.351383231779,
7.93789326158962));
#82853=CARTESIAN_POINT('Ctrl Pts',(1.48963991304838,-222.424152105273,7.77913539635783));
#82854=CARTESIAN_POINT('Ctrl Pts',(2.97200297780601,-224.854336870728,7.62037753112604));
#82855=CARTESIAN_POINT('Ctrl Pts',(1.73438903414674,-227.417832526365,7.46161966589424));
#82856=CARTESIAN_POINT('Ctrl Pts',(-1.09053768536042,-227.768527948952,
7.30286180066246));
#82857=CARTESIAN_POINT('Ctrl Pts',(-2.91740435811009,-225.585466701527,
7.14410393543065));
#82858=CARTESIAN_POINT('Ctrl Pts',(-2.07426267704153,-222.866586351888,
6.98534607019887));
#82859=CARTESIAN_POINT('Ctrl Pts',(0.667244124487021,-222.100206089107,
6.82658820496707));
#82860=CARTESIAN_POINT('Ctrl Pts',(2.7980891295238,-223.987717099543,6.66783033973529));
#82861=CARTESIAN_POINT('Ctrl Pts',(2.36812307325259,-226.801669380671,6.50907247450349));
#82862=CARTESIAN_POINT('Ctrl Pts',(-0.229149126535227,-227.966733915457,
6.3503146092717));
#82863=CARTESIAN_POINT('Ctrl Pts',(-2.61670405472906,-226.416643687482,
6.19155674403991));
#82864=CARTESIAN_POINT('Ctrl Pts',(-2.60945153493425,-223.570041212431,
6.03279887880811));
#82865=CARTESIAN_POINT('Ctrl Pts',(-0.214029072981824,-222.032136963532,
5.87404101357633));
#82866=CARTESIAN_POINT('Ctrl Pts',(2.37727278814708,-223.2104208489,5.71528314834453));
#82867=CARTESIAN_POINT('Ctrl Pts',(2.79289468704778,-226.026527502981,5.55652528311273));
#82868=CARTESIAN_POINT('Ctrl Pts',(0.652459478190211,-227.903156226702,
5.39776741788094));
#82869=CARTESIAN_POINT('Ctrl Pts',(-2.08510661944959,-227.122816485908,
5.23900955264915));
#82870=CARTESIAN_POINT('Ctrl Pts',(-2.91438322096418,-224.39967518069,5.08025168741736));
#82871=CARTESIAN_POINT('Ctrl Pts',(-1.07641641325721,-222.225951126495,
4.92149382218557));
#82872=CARTESIAN_POINT('Ctrl Pts',(1.7466866535327,-222.591036492251,4.76273595695378));
#82873=CARTESIAN_POINT('Ctrl Pts',(2.97122216369831,-225.160805165555,4.60397809172198));
#82874=CARTESIAN_POINT('Ctrl Pts',(1.47649526648357,-227.583404957696,4.44522022649019));
#82875=CARTESIAN_POINT('Ctrl Pts',(-1.3695200405468,-227.641672634083,4.28646236125839));
#82876=CARTESIAN_POINT('Ctrl Pts',(-2.96215066034079,-225.282281619762,
4.12770449602661));
#82877=CARTESIAN_POINT('Ctrl Pts',(-1.84382111224014,-222.664546477884,
3.96894663079481));
#82878=CARTESIAN_POINT('Ctrl Pts',(0.961973445206051,-222.184218308117,
3.81018876556302));
#82879=CARTESIAN_POINT('Ctrl Pts',(2.88736994357081,-224.280893430997,3.65143090033123));
#82880=CARTESIAN_POINT('Ctrl Pts',(2.1702455828333,-227.035694859655,3.49267303509943));
#82881=CARTESIAN_POINT('Ctrl Pts',(-0.53308744938281,-227.927428428534,
3.33391516986764));
#82882=CARTESIAN_POINT('Ctrl Pts',(-2.74853887008028,-226.139979623417,
3.17515730463585));
#82883=CARTESIAN_POINT('Ctrl Pts',(-2.44852762254036,-223.309221494149,
3.01639943940406));
#82884=CARTESIAN_POINT('Ctrl Pts',(0.0923760039403491,-222.025863822749,
2.85764157417226));
#82885=CARTESIAN_POINT('Ctrl Pts',(2.54873712524399,-223.464435391104,2.69888370894047));
#82886=CARTESIAN_POINT('Ctrl Pts',(2.67249410944869,-226.308355776804,2.54012584370868));
#82887=CARTESIAN_POINT('Ctrl Pts',(0.350384631011751,-227.954868707119,
2.38136797847689));
#82888=CARTESIAN_POINT('Ctrl Pts',(-2.29239693168896,-226.897086521961,
2.22261011324509));
#82889=CARTESIAN_POINT('Ctrl Pts',(-2.83717674258343,-224.103089589495,
2.0638522480133));
#82890=CARTESIAN_POINT('Ctrl Pts',(-0.785372855636834,-222.129947541734,
1.90509438278151));
#82891=CARTESIAN_POINT('Ctrl Pts',(1.98520493939195,-222.78347228865,1.74633651754971));
#82892=CARTESIAN_POINT('Ctrl Pts',(2.9389218272836,-225.465573472176,1.58757865231793));
#82893=CARTESIAN_POINT('Ctrl Pts',(1.20294046782472,-227.721560787075,1.42882078708613));
#82894=CARTESIAN_POINT('Ctrl Pts',(-1.63397783679448,-227.486818517997,
1.27006292185434));
#82895=CARTESIAN_POINT('Ctrl Pts',(-2.97546775505905,-224.976053234372,
1.11130505662255));
#82896=CARTESIAN_POINT('Ctrl Pts',(-1.59383393872096,-222.487380324087,
0.952547191390754));
#82897=CARTESIAN_POINT('Ctrl Pts',(1.24652586018671,-222.297898798513,0.793789326158964));
#82898=CARTESIAN_POINT('Ctrl Pts',(2.94596528548675,-224.582107387905,0.635031460927171));
#82899=CARTESIAN_POINT('Ctrl Pts',(1.94946025516128,-227.247293886066,0.476273595695376));
#82900=CARTESIAN_POINT('Ctrl Pts',(-0.831597883947986,-227.858767919179,
0.317515730463588));
#82901=CARTESIAN_POINT('Ctrl Pts',(-2.85075839585417,-225.847693510707,
0.158757865231792));
#82902=CARTESIAN_POINT('Ctrl Pts',(-2.45743451545282,-224.000243484622,
0.0529192884105984));
#82903=CARTESIAN_POINT('Ctrl Pts',(-1.91346599666507,-223.364012796625,
0.));
#82904=CARTESIAN_POINT('Ctrl Pts',(-1.91346599666507,-223.364012796625,
0.));
#82905=CARTESIAN_POINT('Ctrl Pts',(-1.97507205842691,-223.421907367167,
4.15794293990103E-16));
#82906=CARTESIAN_POINT('Ctrl Pts',(-2.03330667709052,-223.482952904785,
4.29084976747441E-15));
#82907=CARTESIAN_POINT('Ctrl Pts',(-2.08817315626043,-223.546764508293,
4.10782519111308E-15));
#82908=CARTESIAN_POINT('Ctrl Pts',(-2.1444928557844,-223.612266257087,3.91995293646646E-15));
#82909=CARTESIAN_POINT('Ctrl Pts',(-2.19726406808799,-223.680682970755,
1.5045519229708E-16));
#82910=CARTESIAN_POINT('Ctrl Pts',(-2.24646481250915,-223.751646900022,
-2.05391259555654E-15));
#82911=CARTESIAN_POINT('Ctrl Pts',(-2.2973544975264,-223.825046846515,-4.33395091013519E-15));
#82912=CARTESIAN_POINT('Ctrl Pts',(-2.34442495788414,-223.901172411917,
4.72218969058781E-15));
#82913=CARTESIAN_POINT('Ctrl Pts',(-2.38761695660309,-223.979660637394,
5.32907051820075E-15));
#82914=CARTESIAN_POINT('Ctrl Pts',(-2.40651345604263,-224.01399923604,5.59458088028141E-15));
#82915=CARTESIAN_POINT('Ctrl Pts',(-2.42466709995156,-224.048790568658,
4.43801222596687E-15));
#82916=CARTESIAN_POINT('Ctrl Pts',(-2.44207048417908,-224.084006328958,
3.99680288865056E-15));
#82917=CARTESIAN_POINT('Ctrl Pts',(-2.45159432012311,-224.10327781773,3.75535528911235E-15));
#82918=CARTESIAN_POINT('Ctrl Pts',(-2.46089344693261,-224.122676430478,
-1.57841351860035E-15));
#82919=CARTESIAN_POINT('Ctrl Pts',(-2.46996644638514,-224.142197657679,
-2.05391259555654E-15));
#82920=CARTESIAN_POINT('Ctrl Pts',(-2.47861919862404,-224.160814692018,
-2.50738729532423E-15));
#82921=CARTESIAN_POINT('Ctrl Pts',(-2.4870687790189,-224.179549252033,-4.26985750199731E-15));
#82922=CARTESIAN_POINT('Ctrl Pts',(-2.49529984718043,-224.198364615252,
-3.88578058618805E-15));
#82923=CARTESIAN_POINT('Ctrl Pts',(-2.53185222452328,-224.28191953701,-2.18017882468746E-15));
#82924=CARTESIAN_POINT('Ctrl Pts',(-2.56414469936887,-224.367157977321,
1.02042468065935E-14));
#82925=CARTESIAN_POINT('Ctrl Pts',(-2.59215321235953,-224.453680932318,
9.04831765069503E-15));
#82926=CARTESIAN_POINT('Ctrl Pts',(-2.62062491493274,-224.541634756973,
7.87327236594828E-15));
#82927=CARTESIAN_POINT('Ctrl Pts',(-2.64467028407739,-224.630916688536,
3.55782650275821E-15));
#82928=CARTESIAN_POINT('Ctrl Pts',(-2.66422493735634,-224.721144730816,
3.52495810318487E-15));
#82929=CARTESIAN_POINT('Ctrl Pts',(-2.68343419721698,-224.809779077134,
3.49267025744293E-15));
#82930=CARTESIAN_POINT('Ctrl Pts',(-2.69831023427265,-224.89932731694,4.43043718819613E-15));
#82931=CARTESIAN_POINT('Ctrl Pts',(-2.7087493783213,-224.989450156742,4.91273688396632E-15));
#82932=CARTESIAN_POINT('Ctrl Pts',(-2.71288543016613,-225.025157369526,
5.1038269328395E-15));
#82933=CARTESIAN_POINT('Ctrl Pts',(-2.71632448494311,-225.06095496387,4.19046218398344E-15));
#82934=CARTESIAN_POINT('Ctrl Pts',(-2.71905805620622,-225.096822374193,
3.83026943495679E-15));
#82935=CARTESIAN_POINT('Ctrl Pts',(-2.72067802537057,-225.11807812103,3.61681198662921E-15));
#82936=CARTESIAN_POINT('Ctrl Pts',(-2.72205020702394,-225.139358391265,
8.83539236091481E-15));
#82937=CARTESIAN_POINT('Ctrl Pts',(-2.72317263041263,-225.160658927688,
9.27036225562006E-15));
#82938=CARTESIAN_POINT('Ctrl Pts',(-2.72391565392553,-225.174759488635,
9.55830427681055E-15));
#82939=CARTESIAN_POINT('Ctrl Pts',(-2.72454914557126,-225.188868839512,
5.13496310570189E-15));
#82940=CARTESIAN_POINT('Ctrl Pts',(-2.72507219122218,-225.202971354773,
4.94049245958195E-15));
#82941=CARTESIAN_POINT('Ctrl Pts',(-2.72860238425918,-225.298153488667,
3.62795134651196E-15));
#82942=CARTESIAN_POINT('Ctrl Pts',(-2.72711455578113,-225.393185793488,
7.04171290797418E-15));
#82943=CARTESIAN_POINT('Ctrl Pts',(-2.72055026029093,-225.487669326062,
5.82867087928207E-15));
#82944=CARTESIAN_POINT('Ctrl Pts',(-2.71400813842156,-225.581833701457,
4.61972640135258E-15));
#82945=CARTESIAN_POINT('Ctrl Pts',(-2.70242414664252,-225.675453959622,
3.25016722958927E-15));
#82946=CARTESIAN_POINT('Ctrl Pts',(-2.68569242546438,-225.768153085937,
3.30291349825984E-15));
#82947=CARTESIAN_POINT('Ctrl Pts',(-2.68378842047261,-225.778701887065,
3.30891581910756E-15));
#82948=CARTESIAN_POINT('Ctrl Pts',(-2.68181769993591,-225.789238770017,
7.06369997675108E-17));
#82949=CARTESIAN_POINT('Ctrl Pts',(-2.67978006501446,-225.799763185344,
5.55111512312578E-17));
#82950=CARTESIAN_POINT('Ctrl Pts',(-2.662249451615,-225.890309069892,-7.2557142862657E-17));
#82951=CARTESIAN_POINT('Ctrl Pts',(-2.63977030692457,-225.979932423301,
9.99427761194622E-15));
#82952=CARTESIAN_POINT('Ctrl Pts',(-2.61261775161457,-226.06839542511,1.12687636999453E-14));
#82953=CARTESIAN_POINT('Ctrl Pts',(-2.60191929570249,-226.103250985255,
1.17709276056017E-14));
#82954=CARTESIAN_POINT('Ctrl Pts',(-2.59049473479936,-226.137926354826,
5.52161406979016E-15));
#82955=CARTESIAN_POINT('Ctrl Pts',(-2.57835873261334,-226.172406649309,
5.07927033766009E-15));
#82956=CARTESIAN_POINT('Ctrl Pts',(-2.57307203674103,-226.187426985308,
4.8865761747103E-15));
#82957=CARTESIAN_POINT('Ctrl Pts',(-2.56765031882317,-226.202410299172,
1.43913399914977E-14));
#82958=CARTESIAN_POINT('Ctrl Pts',(-2.56209472282316,-226.217355341601,
1.50435219836709E-14));
#82959=CARTESIAN_POINT('Ctrl Pts',(-2.5576757777398,-226.229242692979,1.55622703605811E-14));
#82960=CARTESIAN_POINT('Ctrl Pts',(-2.55317248450269,-226.241104749176,
7.04610913755306E-15));
#82961=CARTESIAN_POINT('Ctrl Pts',(-2.54858920344051,-226.252931575211,
7.04991620636974E-15));
#82962=CARTESIAN_POINT('Ctrl Pts',(-2.51483989794928,-226.340019222562,
7.07794981957767E-15));
#82963=CARTESIAN_POINT('Ctrl Pts',(-2.47670715576013,-226.425333977051,
1.5520638419296E-15));
#82964=CARTESIAN_POINT('Ctrl Pts',(-2.43452445807767,-226.508644905945,
3.17801340798951E-15));
#82965=CARTESIAN_POINT('Ctrl Pts',(-2.3907569116245,-226.595085914954,4.8650516268052E-15));
#82966=CARTESIAN_POINT('Ctrl Pts',(-2.34262924915847,-226.679370417143,
1.31883169502519E-14));
#82967=CARTESIAN_POINT('Ctrl Pts',(-2.29045787431518,-226.761237460125,
1.41137102005473E-14));
#82968=CARTESIAN_POINT('Ctrl Pts',(-2.23768247068651,-226.844052341854,
1.50498174518185E-14));
#82969=CARTESIAN_POINT('Ctrl Pts',(-2.18076876745232,-226.924394278009,
6.05769873306914E-15));
#82970=CARTESIAN_POINT('Ctrl Pts',(-2.11999236348112,-227.001978377933,
6.13398221105399E-15));
#82971=CARTESIAN_POINT('Ctrl Pts',(-2.0772769846332,-227.056506681752,6.18759640092123E-15));
#82972=CARTESIAN_POINT('Ctrl Pts',(-2.03265245620046,-227.109672415922,
5.62971077108756E-15));
#82973=CARTESIAN_POINT('Ctrl Pts',(-1.9862011242703,-227.161369012814,5.27355936696949E-15));
#82974=CARTESIAN_POINT('Ctrl Pts',(-1.97483735729176,-227.174015971604,
5.18643115347578E-15));
#82975=CARTESIAN_POINT('Ctrl Pts',(-1.96336346430018,-227.186575662225,
1.11966090312159E-14));
#82976=CARTESIAN_POINT('Ctrl Pts',(-1.9517923266943,-227.199034120884,1.14630527292547E-14));
#82977=CARTESIAN_POINT('Ctrl Pts',(-1.88311842249801,-227.272974214377,
1.3044377713544E-14));
#82978=CARTESIAN_POINT('Ctrl Pts',(-1.81093155645743,-227.343453602481,
1.5011818698465E-14));
#82979=CARTESIAN_POINT('Ctrl Pts',(-1.73554515615118,-227.410185023087,
1.47104550762833E-14));
#82980=CARTESIAN_POINT('Ctrl Pts',(-1.67071543344256,-227.467571759637,
1.44512926811943E-14));
#82981=CARTESIAN_POINT('Ctrl Pts',(-1.60351847735171,-227.522186792558,
1.4270685325907E-14));
#82982=CARTESIAN_POINT('Ctrl Pts',(-1.53412738920272,-227.573832136014,
1.57721058435811E-14));
#82983=CARTESIAN_POINT('Ctrl Pts',(-1.50861563521692,-227.592819636165,
1.63241057026105E-14));
#82984=CARTESIAN_POINT('Ctrl Pts',(-1.48280709071513,-227.611405560347,
1.28582553745796E-14));
#82985=CARTESIAN_POINT('Ctrl Pts',(-1.456709649847,-227.629579418633,1.27953203588049E-14));
#82986=CARTESIAN_POINT('Ctrl Pts',(-1.43999806640841,-227.641217109496,
1.27550197112187E-14));
#82987=CARTESIAN_POINT('Ctrl Pts',(-1.42316695798824,-227.652686412334,
1.13266969957101E-14));
#82988=CARTESIAN_POINT('Ctrl Pts',(-1.40623322438547,-227.663974897373,
1.14491749414469E-14));
#82989=CARTESIAN_POINT('Ctrl Pts',(-1.32003065852118,-227.72143986038,1.20726590136525E-14));
#82990=CARTESIAN_POINT('Ctrl Pts',(-1.23108709270465,-227.774282119576,
6.07164638895382E-15));
#82991=CARTESIAN_POINT('Ctrl Pts',(-1.13970921686585,-227.822181994227,
5.06192310290032E-15));
#82992=CARTESIAN_POINT('Ctrl Pts',(-1.04833134102704,-227.870081868879,
4.05219981684683E-15));
#82993=CARTESIAN_POINT('Ctrl Pts',(-0.95451851589892,-227.913040261751,
1.85386244543852E-15));
#82994=CARTESIAN_POINT('Ctrl Pts',(-0.858539621091319,-227.950697039278,
2.63894808782972E-15));
#82995=CARTESIAN_POINT('Ctrl Pts',(-0.837654108775876,-227.958891352125,
2.84162983745592E-15));
#82996=CARTESIAN_POINT('Ctrl Pts',(-0.816665907289689,-227.966834441025,
1.13024051429371E-15));
#82997=CARTESIAN_POINT('Ctrl Pts',(-0.795579109021723,-227.974527535833,
9.43689570931383E-16));
#82998=CARTESIAN_POINT('Ctrl Pts',(-2.51426761094033,-224.998573473955,
19.112583302492));
#82999=CARTESIAN_POINT('Ctrl Pts',(-2.51595724505903,-224.672576259975,
19.092036810933));
#83000=CARTESIAN_POINT('Ctrl Pts',(-2.45712156548907,-224.347163909734,
19.0714903193741));
#83001=CARTESIAN_POINT('Ctrl Pts',(-2.33493165330648,-224.04759459911,19.0509438278151));
#83002=CARTESIAN_POINT('Ctrl Pts',(-2.02022083345199,-223.276027604211,
18.9980245394045));
#83003=CARTESIAN_POINT('Ctrl Pts',(-1.28524012182822,-222.675894324399,
18.9451052509939));
#83004=CARTESIAN_POINT('Ctrl Pts',(-0.466331353964879,-222.521799624982,
18.8921859625833));
#83005=CARTESIAN_POINT('Ctrl Pts',(0.352577413898463,-222.367704925566,
18.8392666741727));
#83006=CARTESIAN_POINT('Ctrl Pts',(1.25541423800138,-222.659648806545,18.7863473857621));
#83007=CARTESIAN_POINT('Ctrl Pts',(1.82904823179956,-223.264045686903,18.7334280973515));
#83008=CARTESIAN_POINT('Ctrl Pts',(2.40268222559773,-223.86844256726,18.6805088089409));
#83009=CARTESIAN_POINT('Ctrl Pts',(2.64711338909116,-224.785292446995,18.6275895205303));
#83010=CARTESIAN_POINT('Ctrl Pts',(2.45048646849204,-225.595040932989,18.5746702321197));
#83011=CARTESIAN_POINT('Ctrl Pts',(2.25385954789293,-226.404789418983,18.5217509437091));
#83012=CARTESIAN_POINT('Ctrl Pts',(1.61617454320126,-227.107436511236,18.4688316552985));
#83013=CARTESIAN_POINT('Ctrl Pts',(0.829237852020633,-227.381452837493,
18.4159123668879));
#83014=CARTESIAN_POINT('Ctrl Pts',(0.0423011608400069,-227.65546916375,
18.3629930784773));
#83015=CARTESIAN_POINT('Ctrl Pts',(-0.89388721682958,-227.500854724012,
18.3100737900667));
#83016=CARTESIAN_POINT('Ctrl Pts',(-1.55092836043026,-226.988360135835,
18.2571545016561));
#83017=CARTESIAN_POINT('Ctrl Pts',(-2.14925604575053,-226.521662268176,
18.2089641019348));
#83018=CARTESIAN_POINT('Ctrl Pts',(-2.51609684399047,-225.758187103811,
18.1607737022134));
#83019=CARTESIAN_POINT('Ctrl Pts',(-2.52086477440939,-224.998703164308,
18.112583302492));
#83020=CARTESIAN_POINT('Ctrl Pts',(-0.793799282532874,-227.969222953746,
20.));
#83021=CARTESIAN_POINT('Ctrl Pts',(-0.886846222511741,-227.935185967463,
20.));
#83022=CARTESIAN_POINT('Ctrl Pts',(-0.977826056161207,-227.896378578773,
20.));
#83023=CARTESIAN_POINT('Ctrl Pts',(-1.0665310835594,-227.853129769234,20.));
#83024=CARTESIAN_POINT('Ctrl Pts',(-1.15720918642954,-227.808918971769,
20.));
#83025=CARTESIAN_POINT('Ctrl Pts',(-1.24551082699134,-227.760066356736,
20.));
#83026=CARTESIAN_POINT('Ctrl Pts',(-1.33118520242785,-227.706877790385,
20.));
#83027=CARTESIAN_POINT('Ctrl Pts',(-1.414118896504,-227.655390700253,20.));
#83028=CARTESIAN_POINT('Ctrl Pts',(-1.49459105090855,-227.599839768124,
20.));
#83029=CARTESIAN_POINT('Ctrl Pts',(-1.57234048325287,-227.540471761617,
20.));
#83030=CARTESIAN_POINT('Ctrl Pts',(-1.64037123655415,-227.488524755923,
20.));
#83031=CARTESIAN_POINT('Ctrl Pts',(-1.7063171091793,-227.433654585998,20.));
#83032=CARTESIAN_POINT('Ctrl Pts',(-1.76997788546532,-227.376013601272,
20.));
#83033=CARTESIAN_POINT('Ctrl Pts',(-1.78334881537323,-227.363907032494,
20.));
#83034=CARTESIAN_POINT('Ctrl Pts',(-1.79662074549451,-227.351676294922,
20.));
#83035=CARTESIAN_POINT('Ctrl Pts',(-1.80977455173367,-227.339339189254,
20.));
#83036=CARTESIAN_POINT('Ctrl Pts',(-1.88220127158014,-227.271409338402,
20.));
#83037=CARTESIAN_POINT('Ctrl Pts',(-1.95116225702347,-227.200157915227,
20.));
#83038=CARTESIAN_POINT('Ctrl Pts',(-2.01641820370584,-227.125876415728,
20.));
#83039=CARTESIAN_POINT('Ctrl Pts',(-2.08131431772935,-227.052004517359,
20.));
#83040=CARTESIAN_POINT('Ctrl Pts',(-2.14254662606162,-226.97513506864,20.));
#83041=CARTESIAN_POINT('Ctrl Pts',(-2.19983614514141,-226.895528023604,
20.));
#83042=CARTESIAN_POINT('Ctrl Pts',(-2.25566849653972,-226.817945795936,
20.));
#83043=CARTESIAN_POINT('Ctrl Pts',(-2.30775634501805,-226.737762722758,
20.));
#83044=CARTESIAN_POINT('Ctrl Pts',(-2.35579466209043,-226.655205328684,
20.));
#83045=CARTESIAN_POINT('Ctrl Pts',(-2.37650841258532,-226.619607219371,
20.));
#83046=CARTESIAN_POINT('Ctrl Pts',(-2.39646862341355,-226.583567543625,
20.));
#83047=CARTESIAN_POINT('Ctrl Pts',(-2.41564786554802,-226.547104130923,
20.));
#83048=CARTESIAN_POINT('Ctrl Pts',(-2.42885136523054,-226.522001749157,
20.));
#83049=CARTESIAN_POINT('Ctrl Pts',(-2.44168470148669,-226.496698542274,
20.));
#83050=CARTESIAN_POINT('Ctrl Pts',(-2.45413839533455,-226.471200323988,
20.));
#83051=CARTESIAN_POINT('Ctrl Pts',(-2.46035289057376,-226.458476504206,
20.));
#83052=CARTESIAN_POINT('Ctrl Pts',(-2.46647230820266,-226.445705077751,
20.));
#83053=CARTESIAN_POINT('Ctrl Pts',(-2.4724902648514,-226.43289832355,20.));
#83054=CARTESIAN_POINT('Ctrl Pts',(-2.51269158383526,-226.347346293045,
20.));
#83055=CARTESIAN_POINT('Ctrl Pts',(-2.54843638213312,-226.26008271746,20.));
#83056=CARTESIAN_POINT('Ctrl Pts',(-2.57947357847436,-226.171345167024,
20.));
#83057=CARTESIAN_POINT('Ctrl Pts',(-2.6098249216307,-226.084568519594,20.));
#83058=CARTESIAN_POINT('Ctrl Pts',(-2.63567463650983,-225.99638164586,20.));
#83059=CARTESIAN_POINT('Ctrl Pts',(-2.65673878831304,-225.906997936184,
20.));
#83060=CARTESIAN_POINT('Ctrl Pts',(-2.66036642238348,-225.891604418629,
20.));
#83061=CARTESIAN_POINT('Ctrl Pts',(-2.66385199584536,-225.876175396232,
20.));
#83062=CARTESIAN_POINT('Ctrl Pts',(-2.6671938997738,-225.860711953896,20.));
#83063=CARTESIAN_POINT('Ctrl Pts',(-2.68732104473893,-225.767580926726,
20.));
#83064=CARTESIAN_POINT('Ctrl Pts',(-2.70224103896547,-225.673200364495,
20.));
#83065=CARTESIAN_POINT('Ctrl Pts',(-2.71203226714566,-225.577978837703,
20.));
#83066=CARTESIAN_POINT('Ctrl Pts',(-2.71529432210383,-225.546254742638,
20.));
#83067=CARTESIAN_POINT('Ctrl Pts',(-2.71798669148681,-225.514437423479,
20.));
#83068=CARTESIAN_POINT('Ctrl Pts',(-2.72011107509275,-225.482542447591,
20.));
#83069=CARTESIAN_POINT('Ctrl Pts',(-2.72133540379954,-225.464160675827,
20.));
#83070=CARTESIAN_POINT('Ctrl Pts',(-2.72237106709187,-225.445753115879,
20.));
#83071=CARTESIAN_POINT('Ctrl Pts',(-2.72321830491854,-225.427322796075,
20.));
#83072=CARTESIAN_POINT('Ctrl Pts',(-2.72379259438604,-225.414830036413,
20.));
#83073=CARTESIAN_POINT('Ctrl Pts',(-2.72428019028657,-225.402328437053,
20.));
#83074=CARTESIAN_POINT('Ctrl Pts',(-2.72468104799973,-225.389828334462,
20.));
#83075=CARTESIAN_POINT('Ctrl Pts',(-2.72766941146398,-225.296641029703,
20.));
#83076=CARTESIAN_POINT('Ctrl Pts',(-2.72584877239909,-225.203390772035,
20.));
#83077=CARTESIAN_POINT('Ctrl Pts',(-2.71935801752115,-225.110452407722,
20.));
#83078=CARTESIAN_POINT('Ctrl Pts',(-2.71285441326256,-225.017330058581,
20.));
#83079=CARTESIAN_POINT('Ctrl Pts',(-2.70166180134637,-224.924519857946,
20.));
#83080=CARTESIAN_POINT('Ctrl Pts',(-2.68586885793089,-224.832410901971,
20.));
#83081=CARTESIAN_POINT('Ctrl Pts',(-2.67029897206218,-224.741602881307,
20.));
#83082=CARTESIAN_POINT('Ctrl Pts',(-2.65025731856795,-224.651475590115,
20.));
#83083=CARTESIAN_POINT('Ctrl Pts',(-2.62578582409315,-224.562427028653,
20.));
#83084=CARTESIAN_POINT('Ctrl Pts',(-2.6162702977942,-224.527801275439,20.));
#83085=CARTESIAN_POINT('Ctrl Pts',(-2.60608456229951,-224.49333896239,20.));
#83086=CARTESIAN_POINT('Ctrl Pts',(-2.5952295152326,-224.459064951709,20.));
#83087=CARTESIAN_POINT('Ctrl Pts',(-2.58886662729354,-224.438974602229,
20.));
#83088=CARTESIAN_POINT('Ctrl Pts',(-2.58227375230166,-224.418948969267,
20.));
#83089=CARTESIAN_POINT('Ctrl Pts',(-2.57545094085638,-224.398993216091,
20.));
#83090=CARTESIAN_POINT('Ctrl Pts',(-2.57042017973329,-224.384278955252,
20.));
#83091=CARTESIAN_POINT('Ctrl Pts',(-2.56526459701236,-224.369603474027,
20.));
#83092=CARTESIAN_POINT('Ctrl Pts',(-2.55998882406935,-224.354980991355,
20.));
#83093=CARTESIAN_POINT('Ctrl Pts',(-2.52758494590353,-224.265169478969,
20.));
#83094=CARTESIAN_POINT('Ctrl Pts',(-2.49060962869267,-224.177231268765,
20.));
#83095=CARTESIAN_POINT('Ctrl Pts',(-2.44913502518246,-224.091607986908,
20.));
#83096=CARTESIAN_POINT('Ctrl Pts',(-2.41802907254981,-224.027390525516,
20.));
#83097=CARTESIAN_POINT('Ctrl Pts',(-2.38439113354255,-223.964475745917,
20.));
#83098=CARTESIAN_POINT('Ctrl Pts',(-2.34823443080839,-223.903066989878,
20.));
#83099=CARTESIAN_POINT('Ctrl Pts',(-2.33711427891036,-223.884180458658,
20.));
#83100=CARTESIAN_POINT('Ctrl Pts',(-2.32575578046286,-223.865436503756,
20.));
#83101=CARTESIAN_POINT('Ctrl Pts',(-2.31415906828801,-223.846841383834,
20.));
#83102=CARTESIAN_POINT('Ctrl Pts',(-2.3031725094525,-223.829224633845,20.));
#83103=CARTESIAN_POINT('Ctrl Pts',(-2.29197113405253,-223.81174018047,20.));
#83104=CARTESIAN_POINT('Ctrl Pts',(-2.28056700193948,-223.794411054613,
20.));
#83105=CARTESIAN_POINT('Ctrl Pts',(-2.23334585426799,-223.722656255296,
20.));
#83106=CARTESIAN_POINT('Ctrl Pts',(-2.1826076926359,-223.653490621674,20.));
#83107=CARTESIAN_POINT('Ctrl Pts',(-2.12838833087224,-223.587265557295,
20.));
#83108=CARTESIAN_POINT('Ctrl Pts',(-2.07470388645401,-223.521693856114,
20.));
#83109=CARTESIAN_POINT('Ctrl Pts',(-2.01760623335831,-223.45900440161,20.));
#83110=CARTESIAN_POINT('Ctrl Pts',(-1.95710201649547,-223.399580085816,
20.));
#83111=CARTESIAN_POINT('Ctrl Pts',(-1.94393777493637,-223.386650804384,
20.));
#83112=CARTESIAN_POINT('Ctrl Pts',(-1.93061217207899,-223.373876270997,
20.));
#83113=CARTESIAN_POINT('Ctrl Pts',(-1.91712859175369,-223.361257881811,
20.));
#83114=CARTESIAN_POINT('Origin',(0.,0.,20.));
#83115=CARTESIAN_POINT('',(-325.,275.,20.));
#83116=CARTESIAN_POINT('',(-325.,-275.,20.));
#83117=CARTESIAN_POINT('',(-325.,275.,20.));
#83118=CARTESIAN_POINT('',(325.,-275.,20.));
#83119=CARTESIAN_POINT('',(-325.,-275.,20.));
#83120=CARTESIAN_POINT('',(325.,275.,20.));
#83121=CARTESIAN_POINT('',(325.,-275.,20.));
#83122=CARTESIAN_POINT('',(325.,275.,20.));
#83123=CARTESIAN_POINT('Ctrl Pts',(161.913465996665,226.635987203375,20.));
#83124=CARTESIAN_POINT('Ctrl Pts',(161.975061800004,226.578102273232,20.));
#83125=CARTESIAN_POINT('Ctrl Pts',(162.0332856474,226.517065654258,20.));
#83126=CARTESIAN_POINT('Ctrl Pts',(162.088141171723,226.453262405738,20.));
#83127=CARTESIAN_POINT('Ctrl Pts',(162.144450720438,226.387767960555,20.));
#83128=CARTESIAN_POINT('Ctrl Pts',(162.19721144993,226.319357843406,20.));
#83129=CARTESIAN_POINT('Ctrl Pts',(162.246401727216,226.248399999785,20.));
#83130=CARTESIAN_POINT('Ctrl Pts',(162.29728997268,226.174992807083,20.));
#83131=CARTESIAN_POINT('Ctrl Pts',(162.344357601167,226.098858443986,20.));
#83132=CARTESIAN_POINT('Ctrl Pts',(162.387545727347,226.020360285483,20.));
#83133=CARTESIAN_POINT('Ctrl Pts',(162.406440532551,225.986017341139,20.));
#83134=CARTESIAN_POINT('Ctrl Pts',(162.424592282786,225.951221445178,20.));
#83135=CARTESIAN_POINT('Ctrl Pts',(162.441993602386,225.916000937453,20.));
#83136=CARTESIAN_POINT('Ctrl Pts',(162.451521583465,225.896716174059,20.));
#83137=CARTESIAN_POINT('Ctrl Pts',(162.460824555144,225.877304090621,20.));
#83138=CARTESIAN_POINT('Ctrl Pts',(162.469901101426,225.857769209579,20.));
#83139=CARTESIAN_POINT('Ctrl Pts',(162.478557268221,225.839139084926,20.));
#83140=CARTESIAN_POINT('Ctrl Pts',(162.487009994063,225.820391256647,20.));
#83141=CARTESIAN_POINT('Ctrl Pts',(162.495243927467,225.801562500441,20.));
#83142=CARTESIAN_POINT('Ctrl Pts',(162.53178332527,225.718006880125,20.));
#83143=CARTESIAN_POINT('Ctrl Pts',(162.564063310772,225.63276760616,20.));
#83144=CARTESIAN_POINT('Ctrl Pts',(162.592060189714,225.546243928286,20.));
#83145=CARTESIAN_POINT('Ctrl Pts',(162.620521622014,225.458284559485,20.));
#83146=CARTESIAN_POINT('Ctrl Pts',(162.64455712023,225.368997053047,20.));
#83147=CARTESIAN_POINT('Ctrl Pts',(162.664102677438,225.278763725346,20.));
#83148=CARTESIAN_POINT('Ctrl Pts',(162.683304662781,225.190116519363,20.));
#83149=CARTESIAN_POINT('Ctrl Pts',(162.69817342338,225.100555540895,20.));
#83150=CARTESIAN_POINT('Ctrl Pts',(162.70860562281,225.010420473573,20.));
#83151=CARTESIAN_POINT('Ctrl Pts',(162.71273953757,224.974703107576,20.));
#83152=CARTESIAN_POINT('Ctrl Pts',(162.716176300128,224.938895413385,20.));
#83153=CARTESIAN_POINT('Ctrl Pts',(162.718907440897,224.90301799008,20.));
#83154=CARTESIAN_POINT('Ctrl Pts',(162.720525638553,224.881760659461,20.));
#83155=CARTESIAN_POINT('Ctrl Pts',(162.721896101523,224.860478845972,20.));
#83156=CARTESIAN_POINT('Ctrl Pts',(162.723016863678,224.839176811201,20.));
#83157=CARTESIAN_POINT('Ctrl Pts',(162.723758858197,224.825073914374,20.));
#83158=CARTESIAN_POINT('Ctrl Pts',(162.724391325361,224.810962241637,20.));
#83159=CARTESIAN_POINT('Ctrl Pts',(162.724913352953,224.796857427549,20.));
#83160=CARTESIAN_POINT('Ctrl Pts',(162.728436324273,224.701669249314,20.));
#83161=CARTESIAN_POINT('Ctrl Pts',(162.726942555487,224.606631878699,20.));
#83162=CARTESIAN_POINT('Ctrl Pts',(162.720373977506,224.51214461544,20.));
#83163=CARTESIAN_POINT('Ctrl Pts',(162.713827131361,224.417969958907,20.));
#83164=CARTESIAN_POINT('Ctrl Pts',(162.702239359173,224.324340821208,20.));
#83165=CARTESIAN_POINT('Ctrl Pts',(162.685505157103,224.231634650513,20.));
#83166=CARTESIAN_POINT('Ctrl Pts',(162.683600867107,224.221085032865,20.));
#83167=CARTESIAN_POINT('Ctrl Pts',(162.681629878204,224.210547357196,20.));
#83168=CARTESIAN_POINT('Ctrl Pts',(162.67959199208,224.200022173605,20.));
#83169=CARTESIAN_POINT('Ctrl Pts',(162.662058769681,224.109467366597,20.));
#83170=CARTESIAN_POINT('Ctrl Pts',(162.639578033128,224.019836946214,20.));
#83171=CARTESIAN_POINT('Ctrl Pts',(162.612424683658,223.931368511278,20.));
#83172=CARTESIAN_POINT('Ctrl Pts',(162.601724422561,223.896505948419,20.));
#83173=CARTESIAN_POINT('Ctrl Pts',(162.59029797784,223.86182388033,20.));
#83174=CARTESIAN_POINT('Ctrl Pts',(162.578160005908,223.827337185001,20.));
#83175=CARTESIAN_POINT('Ctrl Pts',(162.572849528586,223.812248930187,20.));
#83176=CARTESIAN_POINT('Ctrl Pts',(162.567402839519,223.797198076188,20.));
#83177=CARTESIAN_POINT('Ctrl Pts',(162.561821096873,223.782185888141,20.));
#83178=CARTESIAN_POINT('Ctrl Pts',(162.557400342449,223.770296196883,20.));
#83179=CARTESIAN_POINT('Ctrl Pts',(162.552895274848,223.7584319722,20.));
#83180=CARTESIAN_POINT('Ctrl Pts',(162.548310201456,223.746603001261,20.));
#83181=CARTESIAN_POINT('Ctrl Pts',(162.514551802678,223.659510149315,20.));
#83182=CARTESIAN_POINT('Ctrl Pts',(162.476410434573,223.574192137851,20.));
#83183=CARTESIAN_POINT('Ctrl Pts',(162.434219363372,223.490879700338,20.));
#83184=CARTESIAN_POINT('Ctrl Pts',(162.390445975646,223.404442747548,20.));
#83185=CARTESIAN_POINT('Ctrl Pts',(162.342313310282,223.320163902973,20.));
#83186=CARTESIAN_POINT('Ctrl Pts',(162.290137469479,223.238303878085,20.));
#83187=CARTESIAN_POINT('Ctrl Pts',(162.2373599398,223.155499847971,20.));
#83188=CARTESIAN_POINT('Ctrl Pts',(162.18044503493,223.075169931722,20.));
#83189=CARTESIAN_POINT('Ctrl Pts',(162.119668013951,222.997598761584,20.));
#83190=CARTESIAN_POINT('Ctrl Pts',(162.076868402372,222.942972590408,20.));
#83191=CARTESIAN_POINT('Ctrl Pts',(162.032152436797,222.889714789462,20.));
#83192=CARTESIAN_POINT('Ctrl Pts',(161.985602823726,222.83793247878,20.));
#83193=CARTESIAN_POINT('Ctrl Pts',(161.974397260002,222.825467284252,20.));
#83194=CARTESIAN_POINT('Ctrl Pts',(161.963084797841,222.813087095521,20.));
#83195=CARTESIAN_POINT('Ctrl Pts',(161.951677829852,222.800805336977,20.));
#83196=CARTESIAN_POINT('Ctrl Pts',(161.88301156409,222.726873114409,20.));
#83197=CARTESIAN_POINT('Ctrl Pts',(161.810832354244,222.656401977612,20.));
#83198=CARTESIAN_POINT('Ctrl Pts',(161.7354533295,222.589678899564,20.));
#83199=CARTESIAN_POINT('Ctrl Pts',(161.670633416166,222.532302405889,20.));
#83200=CARTESIAN_POINT('Ctrl Pts',(161.603446315265,222.477697387466,20.));
#83201=CARTESIAN_POINT('Ctrl Pts',(161.534064912603,222.42606161964,20.));
#83202=CARTESIAN_POINT('Ctrl Pts',(161.508545124964,222.407069010973,20.));
#83203=CARTESIAN_POINT('Ctrl Pts',(161.482728254045,222.388478284016,20.));
#83204=CARTESIAN_POINT('Ctrl Pts',(161.456622194046,222.37029993255,20.));
#83205=CARTESIAN_POINT('Ctrl Pts',(161.439929880381,222.358676625755,20.));
#83206=CARTESIAN_POINT('Ctrl Pts',(161.423118286825,222.347221341864,20.));
#83207=CARTESIAN_POINT('Ctrl Pts',(161.406204262001,222.335946470941,20.));
#83208=CARTESIAN_POINT('Ctrl Pts',(161.3200106339,222.278489890305,20.));
#83209=CARTESIAN_POINT('Ctrl Pts',(161.23107534457,222.225655428716,20.));
#83210=CARTESIAN_POINT('Ctrl Pts',(161.139704755267,222.177762443093,20.));
#83211=CARTESIAN_POINT('Ctrl Pts',(161.048334165963,222.12986945747,20.));
#83212=CARTESIAN_POINT('Ctrl Pts',(160.95452763806,222.086917045673,20.));
#83213=CARTESIAN_POINT('Ctrl Pts',(160.858553719049,222.049265014674,20.));
#83214=CARTESIAN_POINT('Ctrl Pts',(160.837669284144,222.041071732598,20.));
#83215=CARTESIAN_POINT('Ctrl Pts',(160.816682097409,222.033129616109,20.));
#83216=CARTESIAN_POINT('Ctrl Pts',(160.795596253159,222.025437437374,20.));
#83217=CARTESIAN_POINT('Ctrl Pts',(159.206200717467,222.030777046254,20.));
#83218=CARTESIAN_POINT('Ctrl Pts',(159.113164826053,222.064809990922,20.));
#83219=CARTESIAN_POINT('Ctrl Pts',(159.022195938487,222.10361488715,20.));
#83220=CARTESIAN_POINT('Ctrl Pts',(158.933501595931,222.146862343058,20.));
#83221=CARTESIAN_POINT('Ctrl Pts',(158.842828942866,222.191074425278,20.));
#83222=CARTESIAN_POINT('Ctrl Pts',(158.754532766168,222.239930075798,20.));
#83223=CARTESIAN_POINT('Ctrl Pts',(158.668863733849,222.293122937636,20.));
#83224=CARTESIAN_POINT('Ctrl Pts',(158.585928500332,222.344618353173,20.));
#83225=CARTESIAN_POINT('Ctrl Pts',(158.505455091515,222.400179449777,20.));
#83226=CARTESIAN_POINT('Ctrl Pts',(158.42770462389,222.459558956778,20.));
#83227=CARTESIAN_POINT('Ctrl Pts',(158.359672964719,222.511516025404,20.));
#83228=CARTESIAN_POINT('Ctrl Pts',(158.293726354064,222.566397281688,20.));
#83229=CARTESIAN_POINT('Ctrl Pts',(158.230064964185,222.62405003757,20.));
#83230=CARTESIAN_POINT('Ctrl Pts',(158.216686188916,222.636166066864,20.));
#83231=CARTESIAN_POINT('Ctrl Pts',(158.203406524907,222.648406446606,20.));
#83232=CARTESIAN_POINT('Ctrl Pts',(158.190245124516,222.660753343364,20.));
#83233=CARTESIAN_POINT('Ctrl Pts',(158.117820209736,222.728696185234,20.));
#83234=CARTESIAN_POINT('Ctrl Pts',(158.048861054711,222.799961146741,20.));
#83235=CARTESIAN_POINT('Ctrl Pts',(157.983606877175,222.874256209938,20.));
#83236=CARTESIAN_POINT('Ctrl Pts',(157.918710344149,222.948144077421,20.));
#83237=CARTESIAN_POINT('Ctrl Pts',(157.85747780208,223.025029722442,20.));
#83238=CARTESIAN_POINT('Ctrl Pts',(157.80018817671,223.1046526491,20.));
#83239=CARTESIAN_POINT('Ctrl Pts',(157.744357459177,223.182247939675,20.));
#83240=CARTESIAN_POINT('Ctrl Pts',(157.692271132893,223.262443615976,20.));
#83241=CARTESIAN_POINT('Ctrl Pts',(157.644234146577,223.345012659254,20.));
#83242=CARTESIAN_POINT('Ctrl Pts',(157.62352025824,223.380617014851,20.));
#83243=CARTESIAN_POINT('Ctrl Pts',(157.603559925696,223.416662789586,20.));
#83244=CARTESIAN_POINT('Ctrl Pts',(157.584380574184,223.453132111068,20.));
#83245=CARTESIAN_POINT('Ctrl Pts',(157.571170252012,223.478251390303,20.));
#83246=CARTESIAN_POINT('Ctrl Pts',(157.558330477497,223.503571609699,20.));
#83247=CARTESIAN_POINT('Ctrl Pts',(157.545870743057,223.52908693229,20.));
#83248=CARTESIAN_POINT('Ctrl Pts',(157.539658096197,223.541809329346,20.));
#83249=CARTESIAN_POINT('Ctrl Pts',(157.533540489381,223.554579256024,20.));
#83250=CARTESIAN_POINT('Ctrl Pts',(157.527524288537,223.56738446368,20.));
#83251=CARTESIAN_POINT('Ctrl Pts',(157.487323756338,223.652949453292,20.));
#83252=CARTESIAN_POINT('Ctrl Pts',(157.451579825719,223.740224649066,20.));
#83253=CARTESIAN_POINT('Ctrl Pts',(157.420543535262,223.828971978343,20.));
#83254=CARTESIAN_POINT('Ctrl Pts',(157.390193276996,223.915757619425,20.));
#83255=CARTESIAN_POINT('Ctrl Pts',(157.36434462463,224.003951708281,20.));
#83256=CARTESIAN_POINT('Ctrl Pts',(157.343281471526,224.09334036721,20.));
#83257=CARTESIAN_POINT('Ctrl Pts',(157.339658550573,224.108715465315,20.));
#83258=CARTESIAN_POINT('Ctrl Pts',(157.336177332896,224.124125912316,20.));
#83259=CARTESIAN_POINT('Ctrl Pts',(157.332839421148,224.139570624809,20.));
#83260=CARTESIAN_POINT('Ctrl Pts',(157.31271183051,224.232702161571,20.));
#83261=CARTESIAN_POINT('Ctrl Pts',(157.297790873772,224.327080661966,20.));
#83262=CARTESIAN_POINT('Ctrl Pts',(157.287998249313,224.422297987317,20.));
#83263=CARTESIAN_POINT('Ctrl Pts',(157.284735553856,224.454022387265,20.));
#83264=CARTESIAN_POINT('Ctrl Pts',(157.282042557023,224.485839783746,20.));
#83265=CARTESIAN_POINT('Ctrl Pts',(157.279917561785,224.517734622728,20.));
#83266=CARTESIAN_POINT('Ctrl Pts',(157.278692761054,224.536118109621,20.));
#83267=CARTESIAN_POINT('Ctrl Pts',(157.277656667823,224.554527318563,20.));
#83268=CARTESIAN_POINT('Ctrl Pts',(157.276809042623,224.572959222881,20.));
#83269=CARTESIAN_POINT('Ctrl Pts',(157.276234517208,224.585452477542,20.));
#83270=CARTESIAN_POINT('Ctrl Pts',(157.275746697198,224.597954534638,20.));
#83271=CARTESIAN_POINT('Ctrl Pts',(157.275345627116,224.61045506494,20.));
#83272=CARTESIAN_POINT('Ctrl Pts',(157.272355985663,224.703636045658,20.));
#83273=CARTESIAN_POINT('Ctrl Pts',(157.274175017621,224.7968782471,20.));
#83274=CARTESIAN_POINT('Ctrl Pts',(157.280663921379,224.889807250199,20.));
#83275=CARTESIAN_POINT('Ctrl Pts',(157.2871656766,224.982920301909,20.));
#83276=CARTESIAN_POINT('Ctrl Pts',(157.298356202607,225.07571989352,20.));
#83277=CARTESIAN_POINT('Ctrl Pts',(157.314146905939,225.167817345856,20.));
#83278=CARTESIAN_POINT('Ctrl Pts',(157.329714980876,225.258616343805,20.));
#83279=CARTESIAN_POINT('Ctrl Pts',(157.349754901625,225.348733707285,20.));
#83280=CARTESIAN_POINT('Ctrl Pts',(157.3742248181,225.437771805825,20.));
#83281=CARTESIAN_POINT('Ctrl Pts',(157.383741654276,225.472400489504,20.));
#83282=CARTESIAN_POINT('Ctrl Pts',(157.393928994079,225.506865586047,20.));
#83283=CARTESIAN_POINT('Ctrl Pts',(157.404785944163,225.541142240111,20.));
#83284=CARTESIAN_POINT('Ctrl Pts',(157.410770474058,225.560036096983,20.));
#83285=CARTESIAN_POINT('Ctrl Pts',(157.416958472911,225.578872681468,20.));
#83286=CARTESIAN_POINT('Ctrl Pts',(157.423349897143,225.597647704039,20.));
#83287=CARTESIAN_POINT('Ctrl Pts',(157.428585354712,225.613027035854,20.));
#83288=CARTESIAN_POINT('Ctrl Pts',(157.433957583455,225.628365578923,20.));
#83289=CARTESIAN_POINT('Ctrl Pts',(157.439461066734,225.643646297879,20.));
#83290=CARTESIAN_POINT('Ctrl Pts',(157.471856101309,225.73359286331,20.));
#83291=CARTESIAN_POINT('Ctrl Pts',(157.508836086653,225.821663133571,20.));
#83292=CARTESIAN_POINT('Ctrl Pts',(157.550328404654,225.907414260252,20.));
#83293=CARTESIAN_POINT('Ctrl Pts',(157.581447643154,225.971727605262,20.));
#83294=CARTESIAN_POINT('Ctrl Pts',(157.61510621399,226.034735896424,20.));
#83295=CARTESIAN_POINT('Ctrl Pts',(157.651290808751,226.096235211794,20.));
#83296=CARTESIAN_POINT('Ctrl Pts',(157.665718308263,226.120756181238,20.));
#83297=CARTESIAN_POINT('Ctrl Pts',(157.680547541966,226.145037068919,20.));
#83298=CARTESIAN_POINT('Ctrl Pts',(157.695778254971,226.169064140891,20.));
#83299=CARTESIAN_POINT('Ctrl Pts',(157.706207067959,226.18551601942,20.));
#83300=CARTESIAN_POINT('Ctrl Pts',(157.716819725857,226.201841855266,20.));
#83301=CARTESIAN_POINT('Ctrl Pts',(157.727611766764,226.218031728238,20.));
#83302=CARTESIAN_POINT('Ctrl Pts',(157.775201490332,226.289424302256,20.));
#83303=CARTESIAN_POINT('Ctrl Pts',(157.826300374104,226.35821312358,20.));
#83304=CARTESIAN_POINT('Ctrl Pts',(157.880874545296,226.424045717618,20.));
#83305=CARTESIAN_POINT('Ctrl Pts',(157.931843171733,226.485528958125,20.));
#83306=CARTESIAN_POINT('Ctrl Pts',(157.985843573699,226.544433813733,20.));
#83307=CARTESIAN_POINT('Ctrl Pts',(158.042870872967,226.60043887372,20.));
#83308=CARTESIAN_POINT('Ctrl Pts',(158.056034905552,226.613366935264,20.));
#83309=CARTESIAN_POINT('Ctrl Pts',(158.069360315117,226.6261403196,20.));
#83310=CARTESIAN_POINT('Ctrl Pts',(158.082843717471,226.638757628308,20.));
#83311=CARTESIAN_POINT('Ctrl Pts',(-158.086534003335,226.635987203375,20.));
#83312=CARTESIAN_POINT('Ctrl Pts',(-158.02493815882,226.578102234536,20.));
#83313=CARTESIAN_POINT('Ctrl Pts',(-157.966714268211,226.517065579823,20.));
#83314=CARTESIAN_POINT('Ctrl Pts',(-157.911858699942,226.45326229789,20.));
#83315=CARTESIAN_POINT('Ctrl Pts',(-157.855549110443,226.387767823441,20.));
#83316=CARTESIAN_POINT('Ctrl Pts',(-157.802788338847,226.319357679923,20.));
#83317=CARTESIAN_POINT('Ctrl Pts',(-157.753598019515,226.248399812053,20.));
#83318=CARTESIAN_POINT('Ctrl Pts',(-157.702709768307,226.174992648725,20.));
#83319=CARTESIAN_POINT('Ctrl Pts',(-157.655642128471,226.098858321311,20.));
#83320=CARTESIAN_POINT('Ctrl Pts',(-157.612453986729,226.020360203137,20.));
#83321=CARTESIAN_POINT('Ctrl Pts',(-157.593559174717,225.986017276436,20.));
#83322=CARTESIAN_POINT('Ctrl Pts',(-157.575407416866,225.95122139901,20.));
#83323=CARTESIAN_POINT('Ctrl Pts',(-157.558006088956,225.916000910576,20.));
#83324=CARTESIAN_POINT('Ctrl Pts',(-157.548478124627,225.896716200858,20.));
#83325=CARTESIAN_POINT('Ctrl Pts',(-157.539175168484,225.877304171892,20.));
#83326=CARTESIAN_POINT('Ctrl Pts',(-157.530098636533,225.857769346065,20.));
#83327=CARTESIAN_POINT('Ctrl Pts',(-157.521442483325,225.8391392739,20.));
#83328=CARTESIAN_POINT('Ctrl Pts',(-157.512989769992,225.820391498827,20.));
#83329=CARTESIAN_POINT('Ctrl Pts',(-157.504755847974,225.80156279633,20.));
#83330=CARTESIAN_POINT('Ctrl Pts',(-157.468216397868,225.718007179217,20.));
#83331=CARTESIAN_POINT('Ctrl Pts',(-157.435936362002,225.632767909081,20.));
#83332=CARTESIAN_POINT('Ctrl Pts',(-157.407939436079,225.546244234685,20.));
#83333=CARTESIAN_POINT('Ctrl Pts',(-157.379477962203,225.458284888532,20.));
#83334=CARTESIAN_POINT('Ctrl Pts',(-157.355442423985,225.368997404955,20.));
#83335=CARTESIAN_POINT('Ctrl Pts',(-157.335896829832,225.278764099056,20.));
#83336=CARTESIAN_POINT('Ctrl Pts',(-157.316694814992,225.190116945868,20.));
#83337=CARTESIAN_POINT('Ctrl Pts',(-157.301826024782,225.10055601982,20.));
#83338=CARTESIAN_POINT('Ctrl Pts',(-157.291393796945,225.010421002983,20.));
#83339=CARTESIAN_POINT('Ctrl Pts',(-157.287259873426,224.974703678566,20.));
#83340=CARTESIAN_POINT('Ctrl Pts',(-157.283823101457,224.93889602576,20.));
#83341=CARTESIAN_POINT('Ctrl Pts',(-157.281091950689,224.903018643511,20.));
#83342=CARTESIAN_POINT('Ctrl Pts',(-157.279473745741,224.881761319259,20.));
#83343=CARTESIAN_POINT('Ctrl Pts',(-157.278103275693,224.86047951198,20.));
#83344=CARTESIAN_POINT('Ctrl Pts',(-157.27698250669,224.839177483244,20.));
#83345=CARTESIAN_POINT('Ctrl Pts',(-157.276240507937,224.825074596109,20.));
#83346=CARTESIAN_POINT('Ctrl Pts',(-157.275608036552,224.810962933012,20.));
#83347=CARTESIAN_POINT('Ctrl Pts',(-157.275086004761,224.796858128474,20.));
#83348=CARTESIAN_POINT('Ctrl Pts',(-157.271563003652,224.701669975447,20.));
#83349=CARTESIAN_POINT('Ctrl Pts',(-157.273056747714,224.606632626241,20.));
#83350=CARTESIAN_POINT('Ctrl Pts',(-157.279625307528,224.512145379171,20.));
#83351=CARTESIAN_POINT('Ctrl Pts',(-157.286172133748,224.417970764943,20.));
#83352=CARTESIAN_POINT('Ctrl Pts',(-157.297759889722,224.324341664064,20.));
#83353=CARTESIAN_POINT('Ctrl Pts',(-157.3144940807,224.23163552298,20.));
#83354=CARTESIAN_POINT('Ctrl Pts',(-157.316398369121,224.22108591044,20.));
#83355=CARTESIAN_POINT('Ctrl Pts',(-157.318369356492,224.210548239782,20.));
#83356=CARTESIAN_POINT('Ctrl Pts',(-157.320407241131,224.200023061102,20.));
#83357=CARTESIAN_POINT('Ctrl Pts',(-157.337940451736,224.109468291248,20.));
#83358=CARTESIAN_POINT('Ctrl Pts',(-157.360421180481,224.019837900717,20.));
#83359=CARTESIAN_POINT('Ctrl Pts',(-157.387574525284,223.931369489181,20.));
#83360=CARTESIAN_POINT('Ctrl Pts',(-157.39827477871,223.896506954546,20.));
#83361=CARTESIAN_POINT('Ctrl Pts',(-157.409701215456,223.86182491348,20.));
#83362=CARTESIAN_POINT('Ctrl Pts',(-157.421839179082,223.827338244001,20.));
#83363=CARTESIAN_POINT('Ctrl Pts',(-157.427149562768,223.812250256212,20.));
#83364=CARTESIAN_POINT('Ctrl Pts',(-157.432596153518,223.797199667747,20.));
#83365=CARTESIAN_POINT('Ctrl Pts',(-157.438177793222,223.782187743678,20.));
#83366=CARTESIAN_POINT('Ctrl Pts',(-157.442598536132,223.770298073187,20.));
#83367=CARTESIAN_POINT('Ctrl Pts',(-157.447103592198,223.758433868541,20.));
#83368=CARTESIAN_POINT('Ctrl Pts',(-157.451688653832,223.746604917481,20.));
#83369=CARTESIAN_POINT('Ctrl Pts',(-157.485447014203,223.659512087652,20.));
#83370=CARTESIAN_POINT('Ctrl Pts',(-157.523588345799,223.574194090561,20.));
#83371=CARTESIAN_POINT('Ctrl Pts',(-157.565779381558,223.490881660441,20.));
#83372=CARTESIAN_POINT('Ctrl Pts',(-157.609552743621,223.404444693386,20.));
#83373=CARTESIAN_POINT('Ctrl Pts',(-157.657685386683,223.320165828126,20.));
#83374=CARTESIAN_POINT('Ctrl Pts',(-157.709861207378,223.238305777056,20.));
#83375=CARTESIAN_POINT('Ctrl Pts',(-157.762638726167,223.155501705632,20.));
#83376=CARTESIAN_POINT('Ctrl Pts',(-157.819553623873,223.075171743332,20.));
#83377=CARTESIAN_POINT('Ctrl Pts',(-157.880330640098,222.997600523389,20.));
#83378=CARTESIAN_POINT('Ctrl Pts',(-157.923129908507,222.942974750863,20.));
#83379=CARTESIAN_POINT('Ctrl Pts',(-157.967845501693,222.889717324985,20.));
#83380=CARTESIAN_POINT('Ctrl Pts',(-158.014394714637,222.837935363524,20.));
#83381=CARTESIAN_POINT('Ctrl Pts',(-158.025600881673,222.825469474782,20.));
#83382=CARTESIAN_POINT('Ctrl Pts',(-158.036913959438,222.813088600348,20.));
#83383=CARTESIAN_POINT('Ctrl Pts',(-158.048321553421,222.800806166716,20.));
#83384=CARTESIAN_POINT('Ctrl Pts',(-158.116987843626,222.72687391128,20.));
#83385=CARTESIAN_POINT('Ctrl Pts',(-158.189167078244,222.656402739744,20.));
#83386=CARTESIAN_POINT('Ctrl Pts',(-158.26454612692,222.589679626182,20.));
#83387=CARTESIAN_POINT('Ctrl Pts',(-158.329366085462,222.532303080167,20.));
#83388=CARTESIAN_POINT('Ctrl Pts',(-158.396553232748,222.477698010934,20.));
#83389=CARTESIAN_POINT('Ctrl Pts',(-158.465934682045,222.426062194725,20.));
#83390=CARTESIAN_POINT('Ctrl Pts',(-158.491454388474,222.407069641467,20.));
#83391=CARTESIAN_POINT('Ctrl Pts',(-158.517271175927,222.388478967149,20.));
#83392=CARTESIAN_POINT('Ctrl Pts',(-158.54337715025,222.370300665476,20.));
#83393=CARTESIAN_POINT('Ctrl Pts',(-158.560069624725,222.358677240396,20.));
#83394=CARTESIAN_POINT('Ctrl Pts',(-158.576881381361,222.347221841334,20.));
#83395=CARTESIAN_POINT('Ctrl Pts',(-158.593795571103,222.335946858683,20.));
#83396=CARTESIAN_POINT('Ctrl Pts',(-158.67998923295,222.278490246407,20.));
#83397=CARTESIAN_POINT('Ctrl Pts',(-158.768924553551,222.225655755127,20.));
#83398=CARTESIAN_POINT('Ctrl Pts',(-158.860295170393,222.177762742994,20.));
#83399=CARTESIAN_POINT('Ctrl Pts',(-158.951665787236,222.129869730861,20.));
#83400=CARTESIAN_POINT('Ctrl Pts',(-159.045472338951,222.086917295733,20.));
#83401=CARTESIAN_POINT('Ctrl Pts',(-159.141446276778,222.049265245825,20.));
#83402=CARTESIAN_POINT('Ctrl Pts',(-159.162330715998,222.041071959548,20.));
#83403=CARTESIAN_POINT('Ctrl Pts',(-159.183317906813,222.033129839072,20.));
#83404=CARTESIAN_POINT('Ctrl Pts',(-159.204403754918,222.025437656558,20.));
#83405=CARTESIAN_POINT('Ctrl Pts',(-160.793799282533,222.030777046254,20.));
#83406=CARTESIAN_POINT('Ctrl Pts',(-160.886835157066,222.064809984747,20.));
#83407=CARTESIAN_POINT('Ctrl Pts',(-160.97780402793,222.103614877177,20.));
#83408=CARTESIAN_POINT('Ctrl Pts',(-161.066498354202,222.146862331045,20.));
#83409=CARTESIAN_POINT('Ctrl Pts',(-161.157170998911,222.191074415223,20.));
#83410=CARTESIAN_POINT('Ctrl Pts',(-161.245467167254,222.239930070387,20.));
#83411=CARTESIAN_POINT('Ctrl Pts',(-161.331136191421,222.293122938813,20.));
#83412=CARTESIAN_POINT('Ctrl Pts',(-161.414071427374,222.344618367142,20.));
#83413=CARTESIAN_POINT('Ctrl Pts',(-161.494544838205,222.400179479374,20.));
#83414=CARTESIAN_POINT('Ctrl Pts',(-161.572295307516,222.459559004075,20.));
#83415=CARTESIAN_POINT('Ctrl Pts',(-161.640326968163,222.511516088189,20.));
#83416=CARTESIAN_POINT('Ctrl Pts',(-161.706273580043,222.566397361551,20.));
#83417=CARTESIAN_POINT('Ctrl Pts',(-161.76993497096,222.624050135585,20.));
#83418=CARTESIAN_POINT('Ctrl Pts',(-161.783313758306,222.636166179433,20.));
#83419=CARTESIAN_POINT('Ctrl Pts',(-161.79659343422,222.648406574009,20.));
#83420=CARTESIAN_POINT('Ctrl Pts',(-161.809754846302,222.660753485833,20.));
#83421=CARTESIAN_POINT('Ctrl Pts',(-161.88217975833,222.728696347667,20.));
#83422=CARTESIAN_POINT('Ctrl Pts',(-161.951138910575,222.799961330003,20.));
#83423=CARTESIAN_POINT('Ctrl Pts',(-162.016393085433,222.874256414107,20.));
#83424=CARTESIAN_POINT('Ctrl Pts',(-162.081289619105,222.94814430615,20.));
#83425=CARTESIAN_POINT('Ctrl Pts',(-162.142522161547,223.025029976113,20.));
#83426=CARTESIAN_POINT('Ctrl Pts',(-162.199811787101,223.104652927277,20.));
#83427=CARTESIAN_POINT('Ctrl Pts',(-162.255642502291,223.182248238225,20.));
#83428=CARTESIAN_POINT('Ctrl Pts',(-162.307728826392,223.262443934253,20.));
#83429=CARTESIAN_POINT('Ctrl Pts',(-162.355765810799,223.34501299586,20.));
#83430=CARTESIAN_POINT('Ctrl Pts',(-162.376479699321,223.380617361091,20.));
#83431=CARTESIAN_POINT('Ctrl Pts',(-162.396440032026,223.416663145243,20.));
#83432=CARTESIAN_POINT('Ctrl Pts',(-162.415619383683,223.453132475859,20.));
#83433=CARTESIAN_POINT('Ctrl Pts',(-162.428829714613,223.478251777848,20.));
#83434=CARTESIAN_POINT('Ctrl Pts',(-162.441669497393,223.503572020127,20.));
#83435=CARTESIAN_POINT('Ctrl Pts',(-162.454129239588,223.529087365697,20.));
#83436=CARTESIAN_POINT('Ctrl Pts',(-162.460341884048,223.54180976138,20.));
#83437=CARTESIAN_POINT('Ctrl Pts',(-162.466459488514,223.554579686581,20.));
#83438=CARTESIAN_POINT('Ctrl Pts',(-162.472475687079,223.567384892693,20.));
#83439=CARTESIAN_POINT('Ctrl Pts',(-162.512676218372,223.652949902466,20.));
#83440=CARTESIAN_POINT('Ctrl Pts',(-162.548420147964,223.740225116418,20.));
#83441=CARTESIAN_POINT('Ctrl Pts',(-162.579456437337,223.828972461131,20.));
#83442=CARTESIAN_POINT('Ctrl Pts',(-162.609806694244,223.91575811645,20.));
#83443=CARTESIAN_POINT('Ctrl Pts',(-162.635655345283,224.003952216894,20.));
#83444=CARTESIAN_POINT('Ctrl Pts',(-162.656718497157,224.093340884024,20.));
#83445=CARTESIAN_POINT('Ctrl Pts',(-162.660341411732,224.108715957369,20.));
#83446=CARTESIAN_POINT('Ctrl Pts',(-162.663822623516,224.124126379391,20.));
#83447=CARTESIAN_POINT('Ctrl Pts',(-162.667160529864,224.139571066685,20.));
#83448=CARTESIAN_POINT('Ctrl Pts',(-162.687288121125,224.232702605024,20.));
#83449=CARTESIAN_POINT('Ctrl Pts',(-162.702209079259,224.327081103144,20.));
#83450=CARTESIAN_POINT('Ctrl Pts',(-162.712001705764,224.422298423,20.));
#83451=CARTESIAN_POINT('Ctrl Pts',(-162.715264402153,224.454022823543,20.));
#83452=CARTESIAN_POINT('Ctrl Pts',(-162.717957399902,224.485840220276,20.));
#83453=CARTESIAN_POINT('Ctrl Pts',(-162.720082396037,224.517735059187,20.));
#83454=CARTESIAN_POINT('Ctrl Pts',(-162.721307197425,224.536118548139,20.));
#83455=CARTESIAN_POINT('Ctrl Pts',(-162.722343291264,224.554527759039,20.));
#83456=CARTESIAN_POINT('Ctrl Pts',(-162.723190917022,224.572959665217,20.));
#83457=CARTESIAN_POINT('Ctrl Pts',(-162.723765442786,224.585452920495,20.));
#83458=CARTESIAN_POINT('Ctrl Pts',(-162.724253263129,224.597954978153,20.));
#83459=CARTESIAN_POINT('Ctrl Pts',(-162.72465433353,224.610455508973,20.));
#83460=CARTESIAN_POINT('Ctrl Pts',(-162.727643976961,224.703636480985,20.));
#83461=CARTESIAN_POINT('Ctrl Pts',(-162.725824947473,224.796878671104,20.));
#83462=CARTESIAN_POINT('Ctrl Pts',(-162.719336046552,224.889807660892,20.));
#83463=CARTESIAN_POINT('Ctrl Pts',(-162.71283429417,224.982920699303,20.));
#83464=CARTESIAN_POINT('Ctrl Pts',(-162.701643771368,225.075720275617,20.));
#83465=CARTESIAN_POINT('Ctrl Pts',(-162.685853071485,225.167817711271,20.));
#83466=CARTESIAN_POINT('Ctrl Pts',(-162.670284999373,225.258616696131,20.));
#83467=CARTESIAN_POINT('Ctrl Pts',(-162.650245081355,225.348734045122,20.));
#83468=CARTESIAN_POINT('Ctrl Pts',(-162.625775167407,225.437772128322,20.));
#83469=CARTESIAN_POINT('Ctrl Pts',(-162.616258329812,225.472400814772,20.));
#83470=CARTESIAN_POINT('Ctrl Pts',(-162.606070988221,225.506865913873,20.));
#83471=CARTESIAN_POINT('Ctrl Pts',(-162.595214035973,225.541142570298,20.));
#83472=CARTESIAN_POINT('Ctrl Pts',(-162.589229904893,225.560035165602,20.));
#83473=CARTESIAN_POINT('Ctrl Pts',(-162.583042331939,225.578870496113,20.));
#83474=CARTESIAN_POINT('Ctrl Pts',(-162.576651360682,225.59764427317,20.));
#83475=CARTESIAN_POINT('Ctrl Pts',(-162.57141557596,225.613024635739,20.));
#83476=CARTESIAN_POINT('Ctrl Pts',(-162.566043001402,225.628364205394,20.));
#83477=CARTESIAN_POINT('Ctrl Pts',(-162.560539154716,225.643645943324,20.));
#83478=CARTESIAN_POINT('Ctrl Pts',(-162.528144126739,225.733592549036,20.));
#83479=CARTESIAN_POINT('Ctrl Pts',(-162.491164142524,225.821662858184,20.));
#83480=CARTESIAN_POINT('Ctrl Pts',(-162.449671820276,225.907414022356,20.));
#83481=CARTESIAN_POINT('Ctrl Pts',(-162.41855257859,225.971727395484,20.));
#83482=CARTESIAN_POINT('Ctrl Pts',(-162.384894001541,226.034735713979,20.));
#83483=CARTESIAN_POINT('Ctrl Pts',(-162.348709397534,226.096235055875,20.));
#83484=CARTESIAN_POINT('Ctrl Pts',(-162.334282224949,226.120755473986,20.));
#83485=CARTESIAN_POINT('Ctrl Pts',(-162.319453336099,226.145035821206,20.));
#83486=CARTESIAN_POINT('Ctrl Pts',(-162.304222985861,226.169062364537,20.));
#83487=CARTESIAN_POINT('Ctrl Pts',(-162.293793871983,226.185514747611,20.));
#83488=CARTESIAN_POINT('Ctrl Pts',(-162.283180901156,226.20184108192,20.));
#83489=CARTESIAN_POINT('Ctrl Pts',(-162.27238853677,226.218031444641,20.));
#83490=CARTESIAN_POINT('Ctrl Pts',(-162.224798823911,226.289424022337,20.));
#83491=CARTESIAN_POINT('Ctrl Pts',(-162.173699949597,226.358212848466,20.));
#83492=CARTESIAN_POINT('Ctrl Pts',(-162.11912578658,226.424045448902,20.));
#83493=CARTESIAN_POINT('Ctrl Pts',(-162.068157074919,226.485528807399,20.));
#83494=CARTESIAN_POINT('Ctrl Pts',(-162.014156575569,226.544433773001,20.));
#83495=CARTESIAN_POINT('Ctrl Pts',(-161.957129166719,226.600438933592,20.));
#83496=CARTESIAN_POINT('Ctrl Pts',(-161.943965134441,226.613366993215,20.));
#83497=CARTESIAN_POINT('Ctrl Pts',(-161.930639725161,226.626140375729,20.));
#83498=CARTESIAN_POINT('Ctrl Pts',(-161.917156323069,226.638757682714,20.));
#83499=CARTESIAN_POINT('Ctrl Pts',(-158.086534003335,-223.364012796625,
20.));
#83500=CARTESIAN_POINT('Ctrl Pts',(-158.024938173881,-223.42189775131,20.));
#83501=CARTESIAN_POINT('Ctrl Pts',(-157.966714299078,-223.482934392949,
20.));
#83502=CARTESIAN_POINT('Ctrl Pts',(-157.911858746884,-223.54673766266,20.));
#83503=CARTESIAN_POINT('Ctrl Pts',(-157.8555491723,-223.612232126406,20.));
#83504=CARTESIAN_POINT('Ctrl Pts',(-157.802788416102,-223.680642260279,
20.));
#83505=CARTESIAN_POINT('Ctrl Pts',(-157.753598112148,-223.751600119281,
20.));
#83506=CARTESIAN_POINT('Ctrl Pts',(-157.70270986304,-223.825007293352,20.));
#83507=CARTESIAN_POINT('Ctrl Pts',(-157.655642227354,-223.901141633816,
20.));
#83508=CARTESIAN_POINT('Ctrl Pts',(-157.612454091303,-223.979639766739,
20.));
#83509=CARTESIAN_POINT('Ctrl Pts',(-157.593559281781,-224.013982699893,
20.));
#83510=CARTESIAN_POINT('Ctrl Pts',(-157.575407526715,-224.048778584098,
20.));
#83511=CARTESIAN_POINT('Ctrl Pts',(-157.558006201844,-224.083999079587,
20.));
#83512=CARTESIAN_POINT('Ctrl Pts',(-157.548478231389,-224.103283808936,
20.));
#83513=CARTESIAN_POINT('Ctrl Pts',(-157.539175269563,-224.122695857825,
20.));
#83514=CARTESIAN_POINT('Ctrl Pts',(-157.530098732371,-224.142230703846,
20.));
#83515=CARTESIAN_POINT('Ctrl Pts',(-157.52144257418,-224.160860795237,20.));
#83516=CARTESIAN_POINT('Ctrl Pts',(-157.512989856259,-224.179608589799,
20.));
#83517=CARTESIAN_POINT('Ctrl Pts',(-157.504755930064,-224.198437311969,
20.));
#83518=CARTESIAN_POINT('Ctrl Pts',(-157.468216499089,-224.281992930256,
20.));
#83519=CARTESIAN_POINT('Ctrl Pts',(-157.435936481645,-224.367232201794,
20.));
#83520=CARTESIAN_POINT('Ctrl Pts',(-157.407939572907,-224.453755877463,
20.));
#83521=CARTESIAN_POINT('Ctrl Pts',(-157.37947811424,-224.5417152319,20.));
#83522=CARTESIAN_POINT('Ctrl Pts',(-157.355442590654,-224.631002723839,
20.));
#83523=CARTESIAN_POINT('Ctrl Pts',(-157.335897010016,-224.721236037712,
20.));
#83524=CARTESIAN_POINT('Ctrl Pts',(-157.316695005968,-224.809883210201,
20.));
#83525=CARTESIAN_POINT('Ctrl Pts',(-157.301826226592,-224.899444155411,
20.));
#83526=CARTESIAN_POINT('Ctrl Pts',(-157.291394009147,-224.989579190703,
20.));
#83527=CARTESIAN_POINT('Ctrl Pts',(-157.287260088834,-225.025296530308,
20.));
#83528=CARTESIAN_POINT('Ctrl Pts',(-157.283823320309,-225.06110419823,20.));
#83529=CARTESIAN_POINT('Ctrl Pts',(-157.281092173199,-225.096981595475,
20.));
#83530=CARTESIAN_POINT('Ctrl Pts',(-157.279473970919,-225.118238922047,
20.));
#83531=CARTESIAN_POINT('Ctrl Pts',(-157.27810350346,-225.139520731589,20.));
#83532=CARTESIAN_POINT('Ctrl Pts',(-157.276982736962,-225.160822762524,
20.));
#83533=CARTESIAN_POINT('Ctrl Pts',(-157.276240739759,-225.174925653178,
20.));
#83534=CARTESIAN_POINT('Ctrl Pts',(-157.275608269918,-225.189037319775,
20.));
#83535=CARTESIAN_POINT('Ctrl Pts',(-157.275086239663,-225.203142127781,
20.));
#83536=CARTESIAN_POINT('Ctrl Pts',(-157.271563249445,-225.298330290024,
20.));
#83537=CARTESIAN_POINT('Ctrl Pts',(-157.273057002546,-225.393367647058,
20.));
#83538=CARTESIAN_POINT('Ctrl Pts',(-157.279625569,-225.487854900047,20.));
#83539=CARTESIAN_POINT('Ctrl Pts',(-157.286172402503,-225.582029529748,
20.));
#83540=CARTESIAN_POINT('Ctrl Pts',(-157.297760164404,-225.675658644094,
20.));
#83541=CARTESIAN_POINT('Ctrl Pts',(-157.314494359435,-225.768364796008,
20.));
#83542=CARTESIAN_POINT('Ctrl Pts',(-157.316398648436,-225.778914410441,
20.));
#83543=CARTESIAN_POINT('Ctrl Pts',(-157.318369636371,-225.789452082957,
20.));
#83544=CARTESIAN_POINT('Ctrl Pts',(-157.320407521558,-225.799977263458,
20.));
#83545=CARTESIAN_POINT('Ctrl Pts',(-157.337940736475,-225.890532046898,
20.));
#83546=CARTESIAN_POINT('Ctrl Pts',(-157.360421468074,-225.980162448345,
20.));
#83547=CARTESIAN_POINT('Ctrl Pts',(-157.387574814582,-226.068630868437,
20.));
#83548=CARTESIAN_POINT('Ctrl Pts',(-157.398275070813,-226.103493413393,
20.));
#83549=CARTESIAN_POINT('Ctrl Pts',(-157.409701510474,-226.13817546434,20.));
#83550=CARTESIAN_POINT('Ctrl Pts',(-157.421839477138,-226.172662143273,
20.));
#83551=CARTESIAN_POINT('Ctrl Pts',(-157.427149894992,-226.187750228502,
20.));
#83552=CARTESIAN_POINT('Ctrl Pts',(-157.432596521619,-226.202800913864,
20.));
#83553=CARTESIAN_POINT('Ctrl Pts',(-157.438178198887,-226.217812934261,
20.));
#83554=CARTESIAN_POINT('Ctrl Pts',(-157.442598945982,-226.229702612288,
20.));
#83555=CARTESIAN_POINT('Ctrl Pts',(-157.44710400624,-226.241566824203,20.));
#83556=CARTESIAN_POINT('Ctrl Pts',(-157.451689072148,-226.253395782476,
20.));
#83557=CARTESIAN_POINT('Ctrl Pts',(-157.485447446532,-226.340488620394,
20.));
#83558=CARTESIAN_POINT('Ctrl Pts',(-157.523588791448,-226.425806622743,
20.));
#83559=CARTESIAN_POINT('Ctrl Pts',(-157.565779840137,-226.50911905557,20.));
#83560=CARTESIAN_POINT('Ctrl Pts',(-157.609553211554,-226.595556017415,
20.));
#83561=CARTESIAN_POINT('Ctrl Pts',(-157.657685862741,-226.679834875118,
20.));
#83562=CARTESIAN_POINT('Ctrl Pts',(-157.70986169076,-226.761694916622,20.));
#83563=CARTESIAN_POINT('Ctrl Pts',(-157.762639213503,-226.844498972949,
20.));
#83564=CARTESIAN_POINT('Ctrl Pts',(-157.8195541138,-226.92482891842,20.));
#83565=CARTESIAN_POINT('Ctrl Pts',(-157.880331131737,-227.002400120161,
20.));
#83566=CARTESIAN_POINT('Ctrl Pts',(-157.923130525395,-227.057026038192,
20.));
#83567=CARTESIAN_POINT('Ctrl Pts',(-157.967846254496,-227.110283600964,
20.));
#83568=CARTESIAN_POINT('Ctrl Pts',(-158.01439561348,-227.162065689885,20.));
#83569=CARTESIAN_POINT('Ctrl Pts',(-158.025601560259,-227.174531325184,
20.));
#83570=CARTESIAN_POINT('Ctrl Pts',(-158.036914413278,-227.186911949283,
20.));
#83571=CARTESIAN_POINT('Ctrl Pts',(-158.048321778722,-227.199194136455,
20.));
#83572=CARTESIAN_POINT('Ctrl Pts',(-158.116988059975,-227.273126379872,
20.));
#83573=CARTESIAN_POINT('Ctrl Pts',(-158.189167285521,-227.343597538705,
20.));
#83574=CARTESIAN_POINT('Ctrl Pts',(-158.264546325432,-227.410320639282,
20.));
#83575=CARTESIAN_POINT('Ctrl Pts',(-158.329366267453,-227.467697166178,
20.));
#83576=CARTESIAN_POINT('Ctrl Pts',(-158.396553397789,-227.522302216849,
20.));
#83577=CARTESIAN_POINT('Ctrl Pts',(-158.465934830046,-227.573938015384,
20.));
#83578=CARTESIAN_POINT('Ctrl Pts',(-158.491454566082,-227.592930588839,
20.));
#83579=CARTESIAN_POINT('Ctrl Pts',(-158.517271383963,-227.611521282344,
20.));
#83580=CARTESIAN_POINT('Ctrl Pts',(-158.543377389521,-227.629699602166,
20.));
#83581=CARTESIAN_POINT('Ctrl Pts',(-158.560069805416,-227.641322984153,
20.));
#83582=CARTESIAN_POINT('Ctrl Pts',(-158.576881502645,-227.652778341256,
20.));
#83583=CARTESIAN_POINT('Ctrl Pts',(-158.593795632311,-227.664053283202,
20.));
#83584=CARTESIAN_POINT('Ctrl Pts',(-158.679989281783,-227.721509883872,
20.));
#83585=CARTESIAN_POINT('Ctrl Pts',(-158.76892459091,-227.774344364263,20.));
#83586=CARTESIAN_POINT('Ctrl Pts',(-158.860295197642,-227.822237366675,
20.));
#83587=CARTESIAN_POINT('Ctrl Pts',(-158.951665804375,-227.870130369087,
20.));
#83588=CARTESIAN_POINT('Ctrl Pts',(-159.045472347341,-227.913082795661,
20.));
#83589=CARTESIAN_POINT('Ctrl Pts',(-159.141446278244,-227.950734838636,
20.));
#83590=CARTESIAN_POINT('Ctrl Pts',(-159.162330715886,-227.958928123377,
20.));
#83591=CARTESIAN_POINT('Ctrl Pts',(-159.183317905209,-227.966870242395,
20.));
#83592=CARTESIAN_POINT('Ctrl Pts',(-159.204403751904,-227.974562423528,
20.));
#83593=CARTESIAN_POINT('Ctrl Pts',(-160.793799282533,-227.969222953746,
20.));
#83594=CARTESIAN_POINT('Ctrl Pts',(-160.886835141626,-227.935190020901,
20.));
#83595=CARTESIAN_POINT('Ctrl Pts',(-160.977803997214,-227.896385131945,
20.));
#83596=CARTESIAN_POINT('Ctrl Pts',(-161.066498308592,-227.853137679943,
20.));
#83597=CARTESIAN_POINT('Ctrl Pts',(-161.157170945659,-227.808925593975,
20.));
#83598=CARTESIAN_POINT('Ctrl Pts',(-161.245467106361,-227.760069934564,
20.));
#83599=CARTESIAN_POINT('Ctrl Pts',(-161.331136123072,-227.706877060112,
20.));
#83600=CARTESIAN_POINT('Ctrl Pts',(-161.414071361254,-227.655381620085,
20.));
#83601=CARTESIAN_POINT('Ctrl Pts',(-161.494544773927,-227.599820493561,
20.));
#83602=CARTESIAN_POINT('Ctrl Pts',(-161.57229524478,-227.540440952671,20.));
#83603=CARTESIAN_POINT('Ctrl Pts',(-161.640326906778,-227.488483854392,
20.));
#83604=CARTESIAN_POINT('Ctrl Pts',(-161.706273519779,-227.433602565413,
20.));
#83605=CARTESIAN_POINT('Ctrl Pts',(-161.769934911645,-227.375949774776,
20.));
#83606=CARTESIAN_POINT('Ctrl Pts',(-161.783313710025,-227.363833717628,
20.));
#83607=CARTESIAN_POINT('Ctrl Pts',(-161.796593396817,-227.351593309494,
20.));
#83608=CARTESIAN_POINT('Ctrl Pts',(-161.80975481958,-227.339246383904,20.));
#83609=CARTESIAN_POINT('Ctrl Pts',(-161.882179729091,-227.271303503813,
20.));
#83610=CARTESIAN_POINT('Ctrl Pts',(-161.951138878795,-227.200038502427,
20.));
#83611=CARTESIAN_POINT('Ctrl Pts',(-162.016393051206,-227.125743399203,
20.));
#83612=CARTESIAN_POINT('Ctrl Pts',(-162.081289585469,-227.051855484701,
20.));
#83613=CARTESIAN_POINT('Ctrl Pts',(-162.142522128253,-226.974969791928,
20.));
#83614=CARTESIAN_POINT('Ctrl Pts',(-162.199811753977,-226.895346818353,
20.));
#83615=CARTESIAN_POINT('Ctrl Pts',(-162.255642467028,-226.817751488767,
20.));
#83616=CARTESIAN_POINT('Ctrl Pts',(-162.307728789136,-226.737555774695,
20.));
#83617=CARTESIAN_POINT('Ctrl Pts',(-162.355765771803,-226.65498669632,20.));
#83618=CARTESIAN_POINT('Ctrl Pts',(-162.376479660491,-226.619382322281,
20.));
#83619=CARTESIAN_POINT('Ctrl Pts',(-162.396439993344,-226.583336529519,
20.));
#83620=CARTESIAN_POINT('Ctrl Pts',(-162.415619345134,-226.546867190551,
20.));
#83621=CARTESIAN_POINT('Ctrl Pts',(-162.428829684002,-226.52174786789,20.));
#83622=CARTESIAN_POINT('Ctrl Pts',(-162.441669474272,-226.496427604822,
20.));
#83623=CARTESIAN_POINT('Ctrl Pts',(-162.454129223494,-226.470912238378,
20.));
#83624=CARTESIAN_POINT('Ctrl Pts',(-162.460341865666,-226.458189844148,
20.));
#83625=CARTESIAN_POINT('Ctrl Pts',(-162.466459467892,-226.445419920498,
20.));
#83626=CARTESIAN_POINT('Ctrl Pts',(-162.472475664286,-226.432614715998,
20.));
#83627=CARTESIAN_POINT('Ctrl Pts',(-162.512676194786,-226.3470496878,20.));
#83628=CARTESIAN_POINT('Ctrl Pts',(-162.548420123478,-226.259774457234,
20.));
#83629=CARTESIAN_POINT('Ctrl Pts',(-162.579456411898,-226.171027098414,
20.));
#83630=CARTESIAN_POINT('Ctrl Pts',(-162.6098066676,-226.084241430083,20.));
#83631=CARTESIAN_POINT('Ctrl Pts',(-162.635655317466,-225.996047319049,
20.));
#83632=CARTESIAN_POINT('Ctrl Pts',(-162.656718468256,-225.906658644424,
20.));
#83633=CARTESIAN_POINT('Ctrl Pts',(-162.660341377093,-225.891283593348,
20.));
#83634=CARTESIAN_POINT('Ctrl Pts',(-162.663822583577,-225.875873193796,
20.));
#83635=CARTESIAN_POINT('Ctrl Pts',(-162.667160485068,-225.860428529169,
20.));
#83636=CARTESIAN_POINT('Ctrl Pts',(-162.6872880769,-225.767296989379,20.));
#83637=CARTESIAN_POINT('Ctrl Pts',(-162.702209036311,-225.67291849333,20.));
#83638=CARTESIAN_POINT('Ctrl Pts',(-162.712001664687,-225.577701178491,
20.));
#83639=CARTESIAN_POINT('Ctrl Pts',(-162.715264361927,-225.545976777395,
20.));
#83640=CARTESIAN_POINT('Ctrl Pts',(-162.717957360515,-225.514159380424,
20.));
#83641=CARTESIAN_POINT('Ctrl Pts',(-162.72008235747,-225.48226454157,20.));
#83642=CARTESIAN_POINT('Ctrl Pts',(-162.721307159468,-225.463881050598,
20.));
#83643=CARTESIAN_POINT('Ctrl Pts',(-162.722343253869,-225.445471837771,
20.));
#83644=CARTESIAN_POINT('Ctrl Pts',(-162.72319088014,-225.427039929757,20.));
#83645=CARTESIAN_POINT('Ctrl Pts',(-162.723765406226,-225.414546673798,
20.));
#83646=CARTESIAN_POINT('Ctrl Pts',(-162.724253226876,-225.402044615508,
20.));
#83647=CARTESIAN_POINT('Ctrl Pts',(-162.724654297569,-225.389544084099,
20.));
#83648=CARTESIAN_POINT('Ctrl Pts',(-162.727643942782,-225.296363120045,
20.));
#83649=CARTESIAN_POINT('Ctrl Pts',(-162.725824915524,-225.203120940277,
20.));
#83650=CARTESIAN_POINT('Ctrl Pts',(-162.719336017171,-225.11019196266,20.));
#83651=CARTESIAN_POINT('Ctrl Pts',(-162.712834267359,-225.017078936413,
20.));
#83652=CARTESIAN_POINT('Ctrl Pts',(-162.701643747461,-224.924279374092,
20.));
#83653=CARTESIAN_POINT('Ctrl Pts',(-162.685853050706,-224.832181953698,
20.));
#83654=CARTESIAN_POINT('Ctrl Pts',(-162.670284981152,-224.74138298082,20.));
#83655=CARTESIAN_POINT('Ctrl Pts',(-162.650245065609,-224.65126564509,20.));
#83656=CARTESIAN_POINT('Ctrl Pts',(-162.625775153949,-224.562227575932,
20.));
#83657=CARTESIAN_POINT('Ctrl Pts',(-162.616258314973,-224.52759888668,20.));
#83658=CARTESIAN_POINT('Ctrl Pts',(-162.606070971652,-224.493133784971,
20.));
#83659=CARTESIAN_POINT('Ctrl Pts',(-162.595214017321,-224.458857126123,
20.));
#83660=CARTESIAN_POINT('Ctrl Pts',(-162.589230261228,-224.43996571699,20.));
#83661=CARTESIAN_POINT('Ctrl Pts',(-162.583043088727,-224.421131565508,
20.));
#83662=CARTESIAN_POINT('Ctrl Pts',(-162.576652543383,-224.402358959524,
20.));
#83663=CARTESIAN_POINT('Ctrl Pts',(-162.57141645097,-224.386977627499,20.));
#83664=CARTESIAN_POINT('Ctrl Pts',(-162.56604355117,-224.371637092308,20.));
#83665=CARTESIAN_POINT('Ctrl Pts',(-162.560539362696,-224.356354396001,
20.));
#83666=CARTESIAN_POINT('Ctrl Pts',(-162.528144340813,-224.266407751976,
20.));
#83667=CARTESIAN_POINT('Ctrl Pts',(-162.491164357556,-224.178337405817,
20.));
#83668=CARTESIAN_POINT('Ctrl Pts',(-162.449672031221,-224.092586205957,
20.));
#83669=CARTESIAN_POINT('Ctrl Pts',(-162.41855278647,-224.028272806063,20.));
#83670=CARTESIAN_POINT('Ctrl Pts',(-162.384894203516,-223.965264461546,
20.));
#83671=CARTESIAN_POINT('Ctrl Pts',(-162.348709590758,-223.903765094401,
20.));
#83672=CARTESIAN_POINT('Ctrl Pts',(-162.334282725247,-223.879245194058,
20.));
#83673=CARTESIAN_POINT('Ctrl Pts',(-162.319454160314,-223.854965354395,
20.));
#83674=CARTESIAN_POINT('Ctrl Pts',(-162.304224150818,-223.830939307521,
20.));
#83675=CARTESIAN_POINT('Ctrl Pts',(-162.293794754286,-223.814486450417,
20.));
#83676=CARTESIAN_POINT('Ctrl Pts',(-162.283181489495,-223.798159647794,
20.));
#83677=CARTESIAN_POINT('Ctrl Pts',(-162.272388821235,-223.781968824945,
20.));
#83678=CARTESIAN_POINT('Ctrl Pts',(-162.224799118483,-223.710576243596,
20.));
#83679=CARTESIAN_POINT('Ctrl Pts',(-162.173700253124,-223.64178741277,20.));
#83680=CARTESIAN_POINT('Ctrl Pts',(-162.119126097886,-223.575954806167,
20.));
#83681=CARTESIAN_POINT('Ctrl Pts',(-162.068157305994,-223.514471336365,
20.));
#83682=CARTESIAN_POINT('Ctrl Pts',(-162.014156714983,-223.455566267017,
20.));
#83683=CARTESIAN_POINT('Ctrl Pts',(-161.957129203007,-223.399561011565,
20.));
#83684=CARTESIAN_POINT('Ctrl Pts',(-161.943965171011,-223.3866329537,20.));
#83685=CARTESIAN_POINT('Ctrl Pts',(-161.930639761992,-223.373859572851,
20.));
#83686=CARTESIAN_POINT('Ctrl Pts',(-161.91715636014,-223.361242267443,20.));
#83687=CARTESIAN_POINT('Ctrl Pts',(161.913465996665,-223.364012796625,20.));
#83688=CARTESIAN_POINT('Ctrl Pts',(161.975061812394,-223.421897738412,20.));
#83689=CARTESIAN_POINT('Ctrl Pts',(162.033285672793,-223.482934368139,20.));
#83690=CARTESIAN_POINT('Ctrl Pts',(162.088141210339,-223.546737626713,20.));
#83691=CARTESIAN_POINT('Ctrl Pts',(162.144450771328,-223.612232080702,20.));
#83692=CARTESIAN_POINT('Ctrl Pts',(162.19721151349,-223.680642205787,20.));
#83693=CARTESIAN_POINT('Ctrl Pts',(162.246401803429,-223.751600056706,20.));
#83694=CARTESIAN_POINT('Ctrl Pts',(162.297290050622,-223.825007240568,20.));
#83695=CARTESIAN_POINT('Ctrl Pts',(162.344357682524,-223.901141592927,20.));
#83696=CARTESIAN_POINT('Ctrl Pts',(162.387545813387,-223.979639739294,20.));
#83697=CARTESIAN_POINT('Ctrl Pts',(162.40644062064,-224.013982678329,20.));
#83698=CARTESIAN_POINT('Ctrl Pts',(162.424592373166,-224.048778568712,20.));
#83699=CARTESIAN_POINT('Ctrl Pts',(162.441993695267,-224.083999070632,20.));
#83700=CARTESIAN_POINT('Ctrl Pts',(162.451521671306,-224.103283817873,20.));
#83701=CARTESIAN_POINT('Ctrl Pts',(162.46082463831,-224.122695884918,20.));
#83702=CARTESIAN_POINT('Ctrl Pts',(162.469901180279,-224.142230749344,20.));
#83703=CARTESIAN_POINT('Ctrl Pts',(162.478557342987,-224.160860858206,20.));
#83704=CARTESIAN_POINT('Ctrl Pts',(162.487010065066,-224.179608670477,20.));
#83705=CARTESIAN_POINT('Ctrl Pts',(162.495243995045,-224.198437410524,20.));
#83706=CARTESIAN_POINT('Ctrl Pts',(162.531783408589,-224.281993029878,20.));
#83707=CARTESIAN_POINT('Ctrl Pts',(162.564063409247,-224.367232302693,20.));
#83708=CARTESIAN_POINT('Ctrl Pts',(162.592060302327,-224.453755979522,20.));
#83709=CARTESIAN_POINT('Ctrl Pts',(162.620521747138,-224.541715341508,20.));
#83710=CARTESIAN_POINT('Ctrl Pts',(162.644557257391,-224.631002841067,20.));
#83711=CARTESIAN_POINT('Ctrl Pts',(162.664102825717,-224.721236162207,20.));
#83712=CARTESIAN_POINT('Ctrl Pts',(162.683304819936,-224.809883352301,20.));
#83713=CARTESIAN_POINT('Ctrl Pts',(162.698173589444,-224.899444314992,20.));
#83714=CARTESIAN_POINT('Ctrl Pts',(162.708605797423,-224.989579367119,20.));
#83715=CARTESIAN_POINT('Ctrl Pts',(162.712739714819,-225.0252967206,20.));
#83716=CARTESIAN_POINT('Ctrl Pts',(162.716176480208,-225.061104402333,20.));
#83717=CARTESIAN_POINT('Ctrl Pts',(162.718907623986,-225.09698181328,20.));
#83718=CARTESIAN_POINT('Ctrl Pts',(162.720525823836,-225.118239141982,20.));
#83719=CARTESIAN_POINT('Ctrl Pts',(162.721896288936,-225.139520953601,20.));
#83720=CARTESIAN_POINT('Ctrl Pts',(162.723017053152,-225.160822986555,20.));
#83721=CARTESIAN_POINT('Ctrl Pts',(162.72375904895,-225.174925880562,20.));
#83722=CARTESIAN_POINT('Ctrl Pts',(162.724391517388,-225.189037550495,20.));
#83723=CARTESIAN_POINT('Ctrl Pts',(162.724913546246,-225.203142361806,20.));
#83724=CARTESIAN_POINT('Ctrl Pts',(162.728436526521,-225.298330532454,20.));
#83725=CARTESIAN_POINT('Ctrl Pts',(162.726942765165,-225.393367896624,20.));
#83726=CARTESIAN_POINT('Ctrl Pts',(162.720374192642,-225.487855155009,20.));
#83727=CARTESIAN_POINT('Ctrl Pts',(162.713827352484,-225.582029798809,20.));
#83728=CARTESIAN_POINT('Ctrl Pts',(162.702239585165,-225.675658925426,20.));
#83729=CARTESIAN_POINT('Ctrl Pts',(162.685505386423,-225.768365087207,20.));
#83730=CARTESIAN_POINT('Ctrl Pts',(162.683601096917,-225.778914703222,20.));
#83731=CARTESIAN_POINT('Ctrl Pts',(162.681630108493,-225.789452377287,20.));
#83732=CARTESIAN_POINT('Ctrl Pts',(162.679592222834,-225.799977559304,20.));
#83733=CARTESIAN_POINT('Ctrl Pts',(162.662059003986,-225.890532355132,20.));
#83734=CARTESIAN_POINT('Ctrl Pts',(162.639578269783,-225.98016276653,20.));
#83735=CARTESIAN_POINT('Ctrl Pts',(162.612424921719,-226.068631194424,20.));
#83736=CARTESIAN_POINT('Ctrl Pts',(162.60172466293,-226.10349374879,20.));
#83737=CARTESIAN_POINT('Ctrl Pts',(162.590298220609,-226.138175808748,20.));
#83738=CARTESIAN_POINT('Ctrl Pts',(162.578160251176,-226.172662496298,20.));
#83739=CARTESIAN_POINT('Ctrl Pts',(162.572849802005,-226.187750670834,20.));
#83740=CARTESIAN_POINT('Ctrl Pts',(162.567403142496,-226.202801445002,20.));
#83741=CARTESIAN_POINT('Ctrl Pts',(162.5618214308,-226.217813553686,20.));
#83742=CARTESIAN_POINT('Ctrl Pts',(162.55740067986,-226.22970323864,20.));
#83743=CARTESIAN_POINT('Ctrl Pts',(162.55289561575,-226.241567457238,20.));
#83744=CARTESIAN_POINT('Ctrl Pts',(162.548310545917,-226.253396422141,20.));
#83745=CARTESIAN_POINT('Ctrl Pts',(162.514552158695,-226.34048926743,20.));
#83746=CARTESIAN_POINT('Ctrl Pts',(162.476410801576,-226.425807274567,20.));
#83747=CARTESIAN_POINT('Ctrl Pts',(162.434219741038,-226.509119709854,20.));
#83748=CARTESIAN_POINT('Ctrl Pts',(162.390446361034,-226.595556666934,20.));
#83749=CARTESIAN_POINT('Ctrl Pts',(162.342313702381,-226.67983551773,20.));
#83750=CARTESIAN_POINT('Ctrl Pts',(162.290137867628,-226.761695550495,20.));
#83751=CARTESIAN_POINT('Ctrl Pts',(162.237360341227,-226.844499593035,20.));
#83752=CARTESIAN_POINT('Ctrl Pts',(162.180445438513,-226.924829523137,20.));
#83753=CARTESIAN_POINT('Ctrl Pts',(162.119668418965,-227.002400708259,20.));
#83754=CARTESIAN_POINT('Ctrl Pts',(162.076868910637,-227.057026759491,20.));
#83755=CARTESIAN_POINT('Ctrl Pts',(162.032153057103,-227.110284447588,20.));
#83756=CARTESIAN_POINT('Ctrl Pts',(161.98560356442,-227.162066653199,20.));
#83757=CARTESIAN_POINT('Ctrl Pts',(161.974397819258,-227.174532056505,20.));
#83758=CARTESIAN_POINT('Ctrl Pts',(161.963085171963,-227.186912451454,20.));
#83759=CARTESIAN_POINT('Ctrl Pts',(161.951678015715,-227.199194413025,20.));
#83760=CARTESIAN_POINT('Ctrl Pts',(161.883011742611,-227.273126645486,20.));
#83761=CARTESIAN_POINT('Ctrl Pts',(161.810832525324,-227.343597792739,20.));
#83762=CARTESIAN_POINT('Ctrl Pts',(161.735453493392,-227.410320881478,20.));
#83763=CARTESIAN_POINT('Ctrl Pts',(161.670633566439,-227.46769739093,20.));
#83764=CARTESIAN_POINT('Ctrl Pts',(161.603446451563,-227.522302424667,20.));
#83765=CARTESIAN_POINT('Ctrl Pts',(161.534065034849,-227.573938207076,20.));
#83766=CARTESIAN_POINT('Ctrl Pts',(161.508545271754,-227.592930798994,20.));
#83767=CARTESIAN_POINT('Ctrl Pts',(161.48272842606,-227.611521510039,20.));
#83768=CARTESIAN_POINT('Ctrl Pts',(161.456622391953,-227.629699846453,20.));
#83769=CARTESIAN_POINT('Ctrl Pts',(161.439930029612,-227.641323189046,20.));
#83770=CARTESIAN_POINT('Ctrl Pts',(161.423118386691,-227.652778507793,20.));
#83771=CARTESIAN_POINT('Ctrl Pts',(161.406204311947,-227.66405341253,20.));
#83772=CARTESIAN_POINT('Ctrl Pts',(161.320010673739,-227.721510002638,20.));
#83773=CARTESIAN_POINT('Ctrl Pts',(161.231075375052,-227.774344473118,20.));
#83774=CARTESIAN_POINT('Ctrl Pts',(161.139704777517,-227.822237466682,20.));
#83775=CARTESIAN_POINT('Ctrl Pts',(161.048334179982,-227.870130460245,20.));
#83776=CARTESIAN_POINT('Ctrl Pts',(160.954527644971,-227.913082879032,20.));
#83777=CARTESIAN_POINT('Ctrl Pts',(160.858553720359,-227.950734915697,20.));
#83778=CARTESIAN_POINT('Ctrl Pts',(160.837669284155,-227.958928199038,20.));
#83779=CARTESIAN_POINT('Ctrl Pts',(160.816682096193,-227.966870316727,20.));
#83780=CARTESIAN_POINT('Ctrl Pts',(160.795596250783,-227.974562496599,20.));
#83781=CARTESIAN_POINT('Ctrl Pts',(159.206200717467,-227.969222953746,20.));
#83782=CARTESIAN_POINT('Ctrl Pts',(159.113164807739,-227.935190002378,20.));
#83783=CARTESIAN_POINT('Ctrl Pts',(159.022195902054,-227.89638510203,20.));
#83784=CARTESIAN_POINT('Ctrl Pts',(158.933501541831,-227.853137643908,20.));
#83785=CARTESIAN_POINT('Ctrl Pts',(158.842828879704,-227.808925563812,20.));
#83786=CARTESIAN_POINT('Ctrl Pts',(158.754532693946,-227.76006991833,20.));
#83787=CARTESIAN_POINT('Ctrl Pts',(158.668863652786,-227.706877063639,20.));
#83788=CARTESIAN_POINT('Ctrl Pts',(158.585928421912,-227.655381661977,20.));
#83789=CARTESIAN_POINT('Ctrl Pts',(158.505455015278,-227.599820582323,20.));
#83790=CARTESIAN_POINT('Ctrl Pts',(158.427704549483,-227.540441094521,20.));
#83791=CARTESIAN_POINT('Ctrl Pts',(158.359672891912,-227.488484042695,20.));
#83792=CARTESIAN_POINT('Ctrl Pts',(158.293726282585,-227.433602804933,20.));
#83793=CARTESIAN_POINT('Ctrl Pts',(158.230064893832,-227.375950068741,20.));
#83794=CARTESIAN_POINT('Ctrl Pts',(158.216686131675,-227.363834055246,20.));
#83795=CARTESIAN_POINT('Ctrl Pts',(158.203406480592,-227.351593691606,20.));
#83796=CARTESIAN_POINT('Ctrl Pts',(158.190245092894,-227.3392468112,20.));
#83797=CARTESIAN_POINT('Ctrl Pts',(158.117820175126,-227.271303990985,20.));
#83798=CARTESIAN_POINT('Ctrl Pts',(158.048861017085,-227.200039052072,20.));
#83799=CARTESIAN_POINT('Ctrl Pts',(157.983606836642,-227.125744011552,20.));
#83800=CARTESIAN_POINT('Ctrl Pts',(157.918710304314,-227.051856170708,20.));
#83801=CARTESIAN_POINT('Ctrl Pts',(157.857477762648,-226.974970552741,20.));
#83802=CARTESIAN_POINT('Ctrl Pts',(157.800188137478,-226.895347652663,20.));
#83803=CARTESIAN_POINT('Ctrl Pts',(157.744357417399,-226.817752384185,20.));
#83804=CARTESIAN_POINT('Ctrl Pts',(157.692271088743,-226.737556729277,20.));
#83805=CARTESIAN_POINT('Ctrl Pts',(157.644234100355,-226.654987705877,20.));
#83806=CARTESIAN_POINT('Ctrl Pts',(157.623520212217,-226.619383360731,20.));
#83807=CARTESIAN_POINT('Ctrl Pts',(157.603559879849,-226.583337596211,20.));
#83808=CARTESIAN_POINT('Ctrl Pts',(157.584380528496,-226.54686828464,20.));
#83809=CARTESIAN_POINT('Ctrl Pts',(157.571170215891,-226.521749030213,20.));
#83810=CARTESIAN_POINT('Ctrl Pts',(157.558330450404,-226.496428835769,20.));
#83811=CARTESIAN_POINT('Ctrl Pts',(157.545870724434,-226.470913538237,20.));
#83812=CARTESIAN_POINT('Ctrl Pts',(157.539658074865,-226.458191139478,20.));
#83813=CARTESIAN_POINT('Ctrl Pts',(157.533540465395,-226.44542121098,20.));
#83814=CARTESIAN_POINT('Ctrl Pts',(157.527524261978,-226.432616001431,20.));
#83815=CARTESIAN_POINT('Ctrl Pts',(157.487323728804,-226.347051033682,20.));
#83816=CARTESIAN_POINT('Ctrl Pts',(157.451579797078,-226.259775857621,20.));
#83817=CARTESIAN_POINT('Ctrl Pts',(157.420543505454,-226.171028545081,20.));
#83818=CARTESIAN_POINT('Ctrl Pts',(157.390193245719,-226.084242919436,20.));
#83819=CARTESIAN_POINT('Ctrl Pts',(157.364344591923,-225.996048843143,20.));
#83820=CARTESIAN_POINT('Ctrl Pts',(157.343281437493,-225.906660193104,20.));
#83821=CARTESIAN_POINT('Ctrl Pts',(157.339658509642,-225.891285068221,20.));
#83822=CARTESIAN_POINT('Ctrl Pts',(157.336177285591,-225.875874594203,20.));
#83823=CARTESIAN_POINT('Ctrl Pts',(157.332839368005,-225.860429854456,20.));
#83824=CARTESIAN_POINT('Ctrl Pts',(157.312711778046,-225.767298319419,20.));
#83825=CARTESIAN_POINT('Ctrl Pts',(157.297790822823,-225.672919816567,20.));
#83826=CARTESIAN_POINT('Ctrl Pts',(157.287998200584,-225.57770248527,20.));
#83827=CARTESIAN_POINT('Ctrl Pts',(157.284735506138,-225.545978085985,20.));
#83828=CARTESIAN_POINT('Ctrl Pts',(157.2820425103,-225.514160689795,20.));
#83829=CARTESIAN_POINT('Ctrl Pts',(157.279917516036,-225.482265850753,20.));
#83830=CARTESIAN_POINT('Ctrl Pts',(157.278692716036,-225.463882366374,20.));
#83831=CARTESIAN_POINT('Ctrl Pts',(157.277656623476,-225.445473159836,20.));
#83832=CARTESIAN_POINT('Ctrl Pts',(157.276808998887,-225.427041257816,20.));
#83833=CARTESIAN_POINT('Ctrl Pts',(157.276234473842,-225.414548003757,20.));
#83834=CARTESIAN_POINT('Ctrl Pts',(157.275746654189,-225.402045947204,20.));
#83835=CARTESIAN_POINT('Ctrl Pts',(157.275345584448,-225.389545417394,20.));
#83836=CARTESIAN_POINT('Ctrl Pts',(157.272355945115,-225.296364427232,20.));
#83837=CARTESIAN_POINT('Ctrl Pts',(157.274174979727,-225.203122213506,20.));
#83838=CARTESIAN_POINT('Ctrl Pts',(157.280663886537,-225.110193195966,20.));
#83839=CARTESIAN_POINT('Ctrl Pts',(157.287165644814,-225.017080129825,20.));
#83840=CARTESIAN_POINT('Ctrl Pts',(157.298356174273,-224.924280521615,20.));
#83841=CARTESIAN_POINT('Ctrl Pts',(157.314146881321,-224.832183051177,20.));
#83842=CARTESIAN_POINT('Ctrl Pts',(157.329714959299,-224.741384039015,20.));
#83843=CARTESIAN_POINT('Ctrl Pts',(157.349754882989,-224.651266659807,20.));
#83844=CARTESIAN_POINT('Ctrl Pts',(157.374224802182,-224.562228544611,20.));
#83845=CARTESIAN_POINT('Ctrl Pts',(157.383741636739,-224.527599864197,20.));
#83846=CARTESIAN_POINT('Ctrl Pts',(157.393928974511,-224.493134770686,20.));
#83847=CARTESIAN_POINT('Ctrl Pts',(157.404785922147,-224.458858119435,20.));
#83848=CARTESIAN_POINT('Ctrl Pts',(157.410770895666,-224.439962859281,20.));
#83849=CARTESIAN_POINT('Ctrl Pts',(157.416959368274,-224.421124879963,20.));
#83850=CARTESIAN_POINT('Ctrl Pts',(157.423351296383,-224.402348471971,20.));
#83851=CARTESIAN_POINT('Ctrl Pts',(157.428586390486,-224.386970285439,20.));
#83852=CARTESIAN_POINT('Ctrl Pts',(157.433958235031,-224.371632883023,20.));
#83853=CARTESIAN_POINT('Ctrl Pts',(157.439461314568,-224.356353296267,20.));
#83854=CARTESIAN_POINT('Ctrl Pts',(157.471856356384,-224.266406776585,20.));
#83855=CARTESIAN_POINT('Ctrl Pts',(157.508836342851,-224.17833655052,20.));
#83856=CARTESIAN_POINT('Ctrl Pts',(157.550328655963,-224.09258546646,20.));
#83857=CARTESIAN_POINT('Ctrl Pts',(157.581447890797,-224.028272153415,20.));
#83858=CARTESIAN_POINT('Ctrl Pts',(157.615106454581,-223.96526389333,20.));
#83859=CARTESIAN_POINT('Ctrl Pts',(157.651291038901,-223.903764608115,20.));
#83860=CARTESIAN_POINT('Ctrl Pts',(157.665718904402,-223.879243021583,20.));
#83861=CARTESIAN_POINT('Ctrl Pts',(157.680548524169,-223.854961528985,20.));
#83862=CARTESIAN_POINT('Ctrl Pts',(157.695779643291,-223.830933865326,20.));
#83863=CARTESIAN_POINT('Ctrl Pts',(157.706208119446,-223.814482551703,20.));
#83864=CARTESIAN_POINT('Ctrl Pts',(157.71682042703,-223.798157273954,20.));
#83865=CARTESIAN_POINT('Ctrl Pts',(157.727612105819,-223.781967949323,20.));
#83866=CARTESIAN_POINT('Ctrl Pts',(157.775201841441,-223.710575379717,20.));
#83867=CARTESIAN_POINT('Ctrl Pts',(157.8263007359,-223.641786564049,20.));
#83868=CARTESIAN_POINT('Ctrl Pts',(157.88087491638,-223.575953977412,20.));
#83869=CARTESIAN_POINT('Ctrl Pts',(157.931843447117,-223.514470869724,20.));
#83870=CARTESIAN_POINT('Ctrl Pts',(157.985843739753,-223.45556613791,20.));
#83871=CARTESIAN_POINT('Ctrl Pts',(158.04287091602,-223.399561191111,20.));
#83872=CARTESIAN_POINT('Ctrl Pts',(158.056034948939,-223.386633127483,20.));
#83873=CARTESIAN_POINT('Ctrl Pts',(158.069360358813,-223.373859741172,20.));
#83874=CARTESIAN_POINT('Ctrl Pts',(158.082843761452,-223.361242430594,20.));
#83875=CARTESIAN_POINT('Ctrl Pts',(1.91346599666507,226.635987203375,20.));
#83876=CARTESIAN_POINT('Ctrl Pts',(1.97507202942767,226.578092660085,20.));
#83877=CARTESIAN_POINT('Ctrl Pts',(2.03330661763037,226.517047147721,20.));
#83878=CARTESIAN_POINT('Ctrl Pts',(2.08817306581981,226.453235567918,20.));
#83879=CARTESIAN_POINT('Ctrl Pts',(2.14449273668366,226.387733839805,20.));
#83880=CARTESIAN_POINT('Ctrl Pts',(2.19726391938203,226.31931714486,20.));
#83881=CARTESIAN_POINT('Ctrl Pts',(2.24646463424728,226.248353232921,20.));
#83882=CARTESIAN_POINT('Ctrl Pts',(2.29735431518303,226.174953266143,20.));
#83883=CARTESIAN_POINT('Ctrl Pts',(2.34442476753679,226.098827676128,20.));
#83884=CARTESIAN_POINT('Ctrl Pts',(2.38761675533576,226.020339422889,20.));
#83885=CARTESIAN_POINT('Ctrl Pts',(2.40651324999781,225.986000812098,20.));
#83886=CARTESIAN_POINT('Ctrl Pts',(2.4246668885704,225.951209466731,20.));
#83887=CARTESIAN_POINT('Ctrl Pts',(2.44207026698428,225.915993693173,20.));
#83888=CARTESIAN_POINT('Ctrl Pts',(2.45159411457209,225.896722167146,20.));
#83889=CARTESIAN_POINT('Ctrl Pts',(2.46089325218288,225.877323516596,20.));
#83890=CARTESIAN_POINT('Ctrl Pts',(2.46996626160065,225.857802251082,20.));
#83891=CARTESIAN_POINT('Ctrl Pts',(2.47861902358291,225.839185179688,20.));
#83892=CARTESIAN_POINT('Ctrl Pts',(2.48706861295929,225.820450582116,20.));
#83893=CARTESIAN_POINT('Ctrl Pts',(2.49529968930897,225.801635180991,20.));
#83894=CARTESIAN_POINT('Ctrl Pts',(2.53185203011613,225.718080257535,20.));
#83895=CARTESIAN_POINT('Ctrl Pts',(2.56414446983256,225.6328418152,20.));
#83896=CARTESIAN_POINT('Ctrl Pts',(2.59215295014503,225.546318858556,20.));
#83897=CARTESIAN_POINT('Ctrl Pts',(2.62062462394071,225.458365018508,20.));
#83898=CARTESIAN_POINT('Ctrl Pts',(2.64466996545821,225.369083071526,20.));
#83899=CARTESIAN_POINT('Ctrl Pts',(2.66422459333411,225.278855014715,20.));
#83900=CARTESIAN_POINT('Ctrl Pts',(2.68343383284957,225.190220632855,20.));
#83901=CARTESIAN_POINT('Ctrl Pts',(2.69830984962651,225.100672357925,20.));
#83902=CARTESIAN_POINT('Ctrl Pts',(2.70874897441918,225.010549484523,20.));
#83903=CARTESIAN_POINT('Ctrl Pts',(2.71288502035126,224.974842243607,20.));
#83904=CARTESIAN_POINT('Ctrl Pts',(2.71632406879747,224.939044621295,20.));
#83905=CARTESIAN_POINT('Ctrl Pts',(2.7190576333604,224.903177183262,20.));
#83906=CARTESIAN_POINT('Ctrl Pts',(2.72067759764398,224.881921431946,20.));
#83907=CARTESIAN_POINT('Ctrl Pts',(2.72204977456521,224.860641157351,20.));
#83908=CARTESIAN_POINT('Ctrl Pts',(2.72317219338359,224.839340616697,20.));
#83909=CARTESIAN_POINT('Ctrl Pts',(2.72391521405841,224.825240049394,20.));
#83910=CARTESIAN_POINT('Ctrl Pts',(2.7245487028823,224.811130692204,20.));
#83911=CARTESIAN_POINT('Ctrl Pts',(2.72507174573303,224.797028170696,20.));
#83912=CARTESIAN_POINT('Ctrl Pts',(2.72860191891809,224.701846020323,20.));
#83913=CARTESIAN_POINT('Ctrl Pts',(2.72711407425655,224.606813701877,20.));
#83914=CARTESIAN_POINT('Ctrl Pts',(2.72054976732745,224.512330159547,20.));
#83915=CARTESIAN_POINT('Ctrl Pts',(2.71400763276353,224.418165755798,20.));
#83916=CARTESIAN_POINT('Ctrl Pts',(2.70242363100706,224.324545473338,20.));
#83917=CARTESIAN_POINT('Ctrl Pts',(2.68569190358529,224.23184632802,20.));
#83918=CARTESIAN_POINT('Ctrl Pts',(2.68378789808642,224.221297525857,20.));
#83919=CARTESIAN_POINT('Ctrl Pts',(2.6818171771052,224.210760641935,20.));
#83920=CARTESIAN_POINT('Ctrl Pts',(2.67977954180341,224.200236225707,20.));
#83921=CARTESIAN_POINT('Ctrl Pts',(2.66224892193235,224.109690316875,20.));
#83922=CARTESIAN_POINT('Ctrl Pts',(2.63976977371118,224.020066944523,20.));
#83923=CARTESIAN_POINT('Ctrl Pts',(2.61261721716453,223.93160392846,20.));
#83924=CARTESIAN_POINT('Ctrl Pts',(2.60191875644486,223.896748348623,20.));
#83925=CARTESIAN_POINT('Ctrl Pts',(2.590494190504,223.862072960234,20.));
#83926=CARTESIAN_POINT('Ctrl Pts',(2.57835818302837,223.827592647788,20.));
#83927=CARTESIAN_POINT('Ctrl Pts',(2.5730714188911,223.812572116558,20.));
#83928=CARTESIAN_POINT('Ctrl Pts',(2.56764962929132,223.797588608551,20.));
#83929=CARTESIAN_POINT('Ctrl Pts',(2.56209395823295,223.782643373109,20.));
#83930=CARTESIAN_POINT('Ctrl Pts',(2.55767501123199,223.770756023652,20.));
#83931=CARTESIAN_POINT('Ctrl Pts',(2.55317171629538,223.758893969826,20.));
#83932=CARTESIAN_POINT('Ctrl Pts',(2.54858843359649,223.747067146183,20.));
#83933=CARTESIAN_POINT('Ctrl Pts',(2.51483910385201,223.659979484958,20.));
#83934=CARTESIAN_POINT('Ctrl Pts',(2.47670633871247,223.574664722143,20.));
#83935=CARTESIAN_POINT('Ctrl Pts',(2.43452361875301,223.491353789882,20.));
#83936=CARTESIAN_POINT('Ctrl Pts',(2.39075605743655,223.404912793674,20.));
#83937=CARTESIAN_POINT('Ctrl Pts',(2.34262838247497,223.320628308811,20.));
#83938=CARTESIAN_POINT('Ctrl Pts',(2.29045699662235,223.238761286965,20.));
#83939=CARTESIAN_POINT('Ctrl Pts',(2.23768158870514,223.155946437364,20.));
#83940=CARTESIAN_POINT('Ctrl Pts',(2.18076788377723,223.075604536594,20.));
#83941=CARTESIAN_POINT('Ctrl Pts',(2.11999147971506,222.998020474552,20.));
#83942=CARTESIAN_POINT('Ctrl Pts',(2.07727586754496,222.94349189959,20.));
#83943=CARTESIAN_POINT('Ctrl Pts',(2.03265108574106,222.890325910386,20.));
#83944=CARTESIAN_POINT('Ctrl Pts',(1.98619948137722,222.838629076086,20.));
#83945=CARTESIAN_POINT('Ctrl Pts',(1.97483618125597,222.825982652964,20.));
#83946=CARTESIAN_POINT('Ctrl Pts',(1.96336276466422,222.81342349125,20.));
#83947=CARTESIAN_POINT('Ctrl Pts',(1.95179211158417,222.800965553175,20.));
#83948=CARTESIAN_POINT('Ctrl Pts',(1.88311823323209,222.727025480997,20.));
#83949=CARTESIAN_POINT('Ctrl Pts',(1.81093139290505,222.656546115043,20.));
#83950=CARTESIAN_POINT('Ctrl Pts',(1.73554501731834,222.589814716556,20.));
#83951=CARTESIAN_POINT('Ctrl Pts',(1.67071531821197,222.532428001103,20.));
#83952=CARTESIAN_POINT('Ctrl Pts',(1.60351838516032,222.477812989059,20.));
#83953=CARTESIAN_POINT('Ctrl Pts',(1.53412731892236,222.426167665699,20.));
#83954=CARTESIAN_POINT('Ctrl Pts',(1.50861557622552,222.407180175343,20.));
#83955=CARTESIAN_POINT('Ctrl Pts',(1.48280704293535,222.388594260749,20.));
#83956=CARTESIAN_POINT('Ctrl Pts',(1.4567096131704,222.370420411812,20.));
#83957=CARTESIAN_POINT('Ctrl Pts',(1.43999802584827,222.35878271928,20.));
#83958=CARTESIAN_POINT('Ctrl Pts',(1.42316691333928,222.347313414893,20.));
#83959=CARTESIAN_POINT('Ctrl Pts',(1.40623317545358,222.336024928434,20.));
#83960=CARTESIAN_POINT('Ctrl Pts',(1.32003063638968,222.278559990595,20.));
#83961=CARTESIAN_POINT('Ctrl Pts',(1.23108709539103,222.225717754617,20.));
#83962=CARTESIAN_POINT('Ctrl Pts',(1.13970924141191,222.177817900273,20.));
#83963=CARTESIAN_POINT('Ctrl Pts',(1.0483313874328,222.129918045928,20.));
#83964=CARTESIAN_POINT('Ctrl Pts',(0.954518581207992,222.086959670452,20.));
#83965=CARTESIAN_POINT('Ctrl Pts',(0.858539701362015,222.049302906438,20.));
#83966=CARTESIAN_POINT('Ctrl Pts',(0.83765419207808,222.041108596444,20.));
#83967=CARTESIAN_POINT('Ctrl Pts',(0.816665993434418,222.033165510218,20.));
#83968=CARTESIAN_POINT('Ctrl Pts',(0.795579197825938,222.025472417912,20.));
#83969=CARTESIAN_POINT('Ctrl Pts',(-0.793799282532863,222.030777046254,
20.));
#83970=CARTESIAN_POINT('Ctrl Pts',(-0.886846243364189,222.064814040164,
20.));
#83971=CARTESIAN_POINT('Ctrl Pts',(-0.977826097699112,222.103621433571,
20.));
#83972=CARTESIAN_POINT('Ctrl Pts',(-1.06653114531038,222.146870245696,20.));
#83973=CARTESIAN_POINT('Ctrl Pts',(-1.15720925843237,222.191081040729,20.));
#83974=CARTESIAN_POINT('Ctrl Pts',(-1.24551090929842,222.23993365004,20.));
#83975=CARTESIAN_POINT('Ctrl Pts',(-1.3311852948319,222.293122208313,20.));
#83976=CARTESIAN_POINT('Ctrl Pts',(-1.41411898609942,222.344609282814,20.));
#83977=CARTESIAN_POINT('Ctrl Pts',(-1.49459113824758,222.40016019587,20.));
#83978=CARTESIAN_POINT('Ctrl Pts',(-1.57234056875799,222.459528180822,20.));
#83979=CARTESIAN_POINT('Ctrl Pts',(-1.6403713204546,222.511475167654,20.));
#83980=CARTESIAN_POINT('Ctrl Pts',(-1.70631719179868,222.566345316816,20.));
#83981=CARTESIAN_POINT('Ctrl Pts',(-1.76997796704167,222.623986279521,20.));
#83982=CARTESIAN_POINT('Ctrl Pts',(-1.78334888221234,222.636092830529,20.));
#83983=CARTESIAN_POINT('Ctrl Pts',(-1.79662079780618,222.64832354999,20.));
#83984=CARTESIAN_POINT('Ctrl Pts',(-1.80977458978086,222.660660637269,20.));
#83985=CARTESIAN_POINT('Ctrl Pts',(-1.88220131303961,222.728590463733,20.));
#83986=CARTESIAN_POINT('Ctrl Pts',(-1.95116230195733,222.799841861522,20.));
#83987=CARTESIAN_POINT('Ctrl Pts',(-2.01641825200817,222.874123335633,20.));
#83988=CARTESIAN_POINT('Ctrl Pts',(-2.08131436524733,222.947995204048,20.));
#83989=CARTESIAN_POINT('Ctrl Pts',(-2.1425466731571,223.024864622427,20.));
#83990=CARTESIAN_POINT('Ctrl Pts',(-2.1998361920632,223.10447163777,20.));
#83991=CARTESIAN_POINT('Ctrl Pts',(-2.25566854673307,223.182053841282,20.));
#83992=CARTESIAN_POINT('Ctrl Pts',(-2.30775639825841,223.262236891238,20.));
#83993=CARTESIAN_POINT('Ctrl Pts',(-2.35579471799653,223.344794263963,20.));
#83994=CARTESIAN_POINT('Ctrl Pts',(-2.37650846819571,223.380392361587,20.));
#83995=CARTESIAN_POINT('Ctrl Pts',(-2.39646867876236,223.416432025931,20.));
#83996=CARTESIAN_POINT('Ctrl Pts',(-2.41564792066214,223.452895427602,20.));
#83997=CARTESIAN_POINT('Ctrl Pts',(-2.42885140531378,223.477997773503,20.));
#83998=CARTESIAN_POINT('Ctrl Pts',(-2.44168472738545,223.503300944244,20.));
#83999=CARTESIAN_POINT('Ctrl Pts',(-2.45413840792515,223.528799126159,20.));
#84000=CARTESIAN_POINT('Ctrl Pts',(-2.46035290716359,223.541522949576,20.));
#84001=CARTESIAN_POINT('Ctrl Pts',(-2.46647232871111,223.554294379828,20.));
#84002=CARTESIAN_POINT('Ctrl Pts',(-2.47249028915989,223.56710113792,20.));
#84003=CARTESIAN_POINT('Ctrl Pts',(-2.51269161001993,223.652653144387,20.));
#84004=CARTESIAN_POINT('Ctrl Pts',(-2.54843641035125,223.739916698538,20.));
#84005=CARTESIAN_POINT('Ctrl Pts',(-2.57947360880066,223.828654231103,20.));
#84006=CARTESIAN_POINT('Ctrl Pts',(-2.60982495439825,223.915430862143,20.));
#84007=CARTESIAN_POINT('Ctrl Pts',(-2.63567467167773,224.003617722926,20.));
#84008=CARTESIAN_POINT('Ctrl Pts',(-2.6567388257605,224.093001424021,20.));
#84009=CARTESIAN_POINT('Ctrl Pts',(-2.66036646980286,224.108394980747,20.));
#84010=CARTESIAN_POINT('Ctrl Pts',(-2.66385205248285,224.123824042632,20.));
#84011=CARTESIAN_POINT('Ctrl Pts',(-2.66719396486238,224.13928752477,20.));
#84012=CARTESIAN_POINT('Ctrl Pts',(-2.6873211089196,224.23241855194,20.));
#84013=CARTESIAN_POINT('Ctrl Pts',(-2.70224110124294,224.326799119115,20.));
#84014=CARTESIAN_POINT('Ctrl Pts',(-2.7120323266871,224.422020654949,20.));
#84015=CARTESIAN_POINT('Ctrl Pts',(-2.71529438038166,224.453744749603,20.));
#84016=CARTESIAN_POINT('Ctrl Pts',(-2.71798674853152,224.485562068786,20.));
#84017=CARTESIAN_POINT('Ctrl Pts',(-2.72011113094023,224.517457045106,20.));
#84018=CARTESIAN_POINT('Ctrl Pts',(-2.72133545868555,224.535838813042,20.));
#84019=CARTESIAN_POINT('Ctrl Pts',(-2.722371121112,224.554246369289,20.));
#84020=CARTESIAN_POINT('Ctrl Pts',(-2.7232183581693,224.572676685511,20.));
#84021=CARTESIAN_POINT('Ctrl Pts',(-2.72379264716902,224.585169443914,20.));
#84022=CARTESIAN_POINT('Ctrl Pts',(-2.72428024263059,224.597671042088,20.));
#84023=CARTESIAN_POINT('Ctrl Pts',(-2.7246810999333,224.610171143549,20.));
#84024=CARTESIAN_POINT('Ctrl Pts',(-2.72766946102712,224.703358461389,20.));
#84025=CARTESIAN_POINT('Ctrl Pts',(-2.72584881895818,224.796608735442,20.));
#84026=CARTESIAN_POINT('Ctrl Pts',(-2.71935806060957,224.88954711861,20.));
#84027=CARTESIAN_POINT('Ctrl Pts',(-2.71285445289211,224.982669486376,20.));
#84028=CARTESIAN_POINT('Ctrl Pts',(-2.70166183707515,225.075479708117,20.));
#84029=CARTESIAN_POINT('Ctrl Pts',(-2.68586888947921,225.167588686864,20.));
#84030=CARTESIAN_POINT('Ctrl Pts',(-2.67029900027931,225.258396725369,20.));
#84031=CARTESIAN_POINT('Ctrl Pts',(-2.65025734363534,225.348524036092,20.));
#84032=CARTESIAN_POINT('Ctrl Pts',(-2.62578584634267,225.437572618048,20.));
#84033=CARTESIAN_POINT('Ctrl Pts',(-2.61627032324279,225.472198363604,20.));
#84034=CARTESIAN_POINT('Ctrl Pts',(-2.60608459160239,225.506660669287,20.));
#84035=CARTESIAN_POINT('Ctrl Pts',(-2.59522954905329,225.540934672887,20.));
#84036=CARTESIAN_POINT('Ctrl Pts',(-2.58886565516187,225.561028202799,20.));
#84037=CARTESIAN_POINT('Ctrl Pts',(-2.5822717015305,225.581056995775,20.));
#84038=CARTESIAN_POINT('Ctrl Pts',(-2.57544773877719,225.601015886081,20.));
#84039=CARTESIAN_POINT('Ctrl Pts',(-2.57041723007358,225.615729238868,20.));
#84040=CARTESIAN_POINT('Ctrl Pts',(-2.56526191645706,225.630403812104,20.));
#84041=CARTESIAN_POINT('Ctrl Pts',(-2.5599864272113,225.645025393398,20.));
#84042=CARTESIAN_POINT('Ctrl Pts',(-2.52758251764902,225.734836285968,20.));
#84043=CARTESIAN_POINT('Ctrl Pts',(-2.49060722777199,225.822773889061,20.));
#84044=CARTESIAN_POINT('Ctrl Pts',(-2.44913270809182,225.90839658293,20.));
#84045=CARTESIAN_POINT('Ctrl Pts',(-2.41802681833168,225.972613603331,20.));
#84046=CARTESIAN_POINT('Ctrl Pts',(-2.38438897400814,226.035527952701,20.));
#84047=CARTESIAN_POINT('Ctrl Pts',(-2.34823239730369,226.096936292273,20.));
#84048=CARTESIAN_POINT('Ctrl Pts',(-2.33710865887614,226.115828852602,20.));
#84049=CARTESIAN_POINT('Ctrl Pts',(-2.32574642144184,226.134578744948,20.));
#84050=CARTESIAN_POINT('Ctrl Pts',(-2.31414581792787,226.153179704593,20.));
#84051=CARTESIAN_POINT('Ctrl Pts',(-2.30316198797025,226.170791700172,20.));
#84052=CARTESIAN_POINT('Ctrl Pts',(-2.29196345883308,226.188271460635,20.));
#84053=CARTESIAN_POINT('Ctrl Pts',(-2.28056228114764,226.205595973582,20.));
#84054=CARTESIAN_POINT('Ctrl Pts',(-2.23334092463296,226.277350578666,20.));
#84055=CARTESIAN_POINT('Ctrl Pts',(-2.18260256041263,226.346516008461,20.));
#84056=CARTESIAN_POINT('Ctrl Pts',(-2.12838300135328,226.41274085809,20.));
#84057=CARTESIAN_POINT('Ctrl Pts',(-2.07470009109681,226.47831023418,20.));
#84058=CARTESIAN_POINT('Ctrl Pts',(-2.01760419713431,226.540997538338,20.));
#84059=CARTESIAN_POINT('Ctrl Pts',(-1.95710196343274,226.600419914749,20.));
#84060=CARTESIAN_POINT('Ctrl Pts',(-1.94393772146859,226.613349198402,20.));
#84061=CARTESIAN_POINT('Ctrl Pts',(-1.93061211823694,226.626123733867,20.));
#84062=CARTESIAN_POINT('Ctrl Pts',(-1.91712853756743,226.638742124992,20.));
#84063=CARTESIAN_POINT('Origin',(160.,-225.,22.2084234471774));
#84064=CARTESIAN_POINT('Ctrl Pts',(156.923621975382,-224.997773684101,19.7084234471775));
#84065=CARTESIAN_POINT('Ctrl Pts',(156.922437084912,-224.853669211175,19.7009407276991));
#84066=CARTESIAN_POINT('Ctrl Pts',(156.997172963777,-223.691638871918,19.6405387198101));
#84067=CARTESIAN_POINT('Ctrl Pts',(158.478135150588,-221.701106223228,19.5272174235105));
#84068=CARTESIAN_POINT('Ctrl Pts',(161.945877027117,-221.932389138002,19.3684595582787));
#84069=CARTESIAN_POINT('Ctrl Pts',(163.63266934599,-224.970773983768,19.2097016930469));
#84070=CARTESIAN_POINT('Ctrl Pts',(161.994882807082,-228.036087395469,19.0509438278151));
#84071=CARTESIAN_POINT('Ctrl Pts',(158.531360332167,-228.322686556747,18.8921859625833));
#84072=CARTESIAN_POINT('Ctrl Pts',(157.007146995965,-226.341897506019,18.7780125023707));
#84073=CARTESIAN_POINT('Ctrl Pts',(156.922679362106,-225.163035208244,18.7167583305688));
#84074=CARTESIAN_POINT('Ctrl Pts',(156.924068591467,-225.002427532313,18.7084234471774));
#84075=CARTESIAN_POINT('Ctrl Pts',(156.929637641087,-225.003026239314,19.7915765528225));
#84076=CARTESIAN_POINT('Ctrl Pts',(156.934919294579,-224.29968971933,19.7552124583938));
#84077=CARTESIAN_POINT('Ctrl Pts',(157.522174149263,-222.562575364414,19.6659290755545));
#84078=CARTESIAN_POINT('Ctrl Pts',(160.407275465985,-221.390670340075,19.5237264043046));
#84079=CARTESIAN_POINT('Ctrl Pts',(163.253011317767,-223.383220872305,19.3649685390728));
#84080=CARTESIAN_POINT('Ctrl Pts',(163.122801873322,-226.856577342785,19.2062106738411));
#84081=CARTESIAN_POINT('Ctrl Pts',(160.134021031603,-228.6302491553,19.0474528086092));
#84082=CARTESIAN_POINT('Ctrl Pts',(157.42551199164,-227.28218313637,18.9092414349364));
#84083=CARTESIAN_POINT('Ctrl Pts',(156.933644953762,-225.625342150596,18.8239493496742));
#84084=CARTESIAN_POINT('Ctrl Pts',(156.93039533859,-224.998257313349,18.7915765528225));
#84085=CARTESIAN_POINT('Ctrl Pts',(161.913465996665,-223.364012796625,20.));
#84086=CARTESIAN_POINT('Ctrl Pts',(162.457434515453,-224.000243484621,19.9470807115894));
#84087=CARTESIAN_POINT('Ctrl Pts',(162.850433814982,-225.848044833187,19.8412421347682));
#84088=CARTESIAN_POINT('Ctrl Pts',(160.831717845445,-227.858697877144,19.6824842695364));
#84089=CARTESIAN_POINT('Ctrl Pts',(158.050453908468,-227.24740924583,19.5237264043046));
#84090=CARTESIAN_POINT('Ctrl Pts',(157.054009795468,-224.582054764982,19.3649685390728));
#84091=CARTESIAN_POINT('Ctrl Pts',(158.753442408201,-222.297880239784,19.206210673841));
#84092=CARTESIAN_POINT('Ctrl Pts',(161.593865435422,-222.48732378556,19.0474528086093));
#84093=CARTESIAN_POINT('Ctrl Pts',(162.975514910861,-224.976061006714,18.8886949433774));
#84094=CARTESIAN_POINT('Ctrl Pts',(161.634006008404,-227.486855382494,18.7299370781457));
#84095=CARTESIAN_POINT('Ctrl Pts',(158.79703908776,-227.72160839649,18.5711792129139));
#84096=CARTESIAN_POINT('Ctrl Pts',(157.061029552932,-225.465579927985,18.4124213476821));
#84097=CARTESIAN_POINT('Ctrl Pts',(158.014761990161,-222.783436142778,18.2536634824503));
#84098=CARTESIAN_POINT('Ctrl Pts',(160.785385942383,-222.129899504983,18.0949056172185));
#84099=CARTESIAN_POINT('Ctrl Pts',(162.837223859747,-224.10307487572,17.9361477519867));
#84100=CARTESIAN_POINT('Ctrl Pts',(162.29243502248,-226.897117941075,17.7773898867549));
#84101=CARTESIAN_POINT('Ctrl Pts',(159.649609545089,-227.954917846864,17.6186320215231));
#84102=CARTESIAN_POINT('Ctrl Pts',(157.327461493527,-226.30837748647,17.4598741562913));
#84103=CARTESIAN_POINT('Ctrl Pts',(157.451220532081,-223.464409894173,17.3011162910595));
#84104=CARTESIAN_POINT('Ctrl Pts',(159.907622461572,-222.025814406454,17.1423584258277));
#84105=CARTESIAN_POINT('Ctrl Pts',(162.448568299937,-223.309193408747,16.9836005605959));
#84106=CARTESIAN_POINT('Ctrl Pts',(162.748584531626,-226.139998560115,16.8248426953641));
#84107=CARTESIAN_POINT('Ctrl Pts',(160.53309630558,-227.927477062891,16.6660848301324));
#84108=CARTESIAN_POINT('Ctrl Pts',(157.829718362824,-227.035728678229,16.5073269649006));
#84109=CARTESIAN_POINT('Ctrl Pts',(157.112582088492,-224.280881484703,16.3485690996688));
#84110=CARTESIAN_POINT('Ctrl Pts',(159.038010573505,-222.184171529352,16.189811234437));
#84111=CARTESIAN_POINT('Ctrl Pts',(161.843851743683,-222.664507679004,16.0310533692052));
#84112=CARTESIAN_POINT('Ctrl Pts',(162.962199870615,-225.282286309282,15.8722955039734));
#84113=CARTESIAN_POINT('Ctrl Pts',(161.369542792414,-227.641716520265,15.7135376387416));
#84114=CARTESIAN_POINT('Ctrl Pts',(158.523480204468,-227.583447875852,15.5547797735098));
#84115=CARTESIAN_POINT('Ctrl Pts',(157.028728475322,-225.160807837019,15.396021908278));
#84116=CARTESIAN_POINT('Ctrl Pts',(158.253284328723,-222.590996472085,15.2372640430462));
#84117=CARTESIAN_POINT('Ctrl Pts',(161.076434295787,-222.22590504116,15.0785061778144));
#84118=CARTESIAN_POINT('Ctrl Pts',(162.914431637677,-224.39966520748,14.9197483125826));
#84119=CARTESIAN_POINT('Ctrl Pts',(162.085141259372,-227.122851752306,14.7609904473509));
#84120=CARTESIAN_POINT('Ctrl Pts',(159.347529682486,-227.903204456901,14.6022325821191));
#84121=CARTESIAN_POINT('Ctrl Pts',(157.207058914531,-226.026544556706,14.4434747168873));
#84122=CARTESIAN_POINT('Ctrl Pts',(157.622687718167,-223.210391118582,14.2847168516555));
#84123=CARTESIAN_POINT('Ctrl Pts',(160.214032628651,-222.032087658357,14.1259589864237));
#84124=CARTESIAN_POINT('Ctrl Pts',(162.609494885811,-223.570017456494,13.9672011211919));
#84125=CARTESIAN_POINT('Ctrl Pts',(162.616747526092,-226.416667222215,13.8084432559601));
#84126=CARTESIAN_POINT('Ctrl Pts',(160.229152933395,-227.966783201874,13.6496853907283));
#84127=CARTESIAN_POINT('Ctrl Pts',(157.631837585066,-226.801699311844,13.4909275254965));
#84128=CARTESIAN_POINT('Ctrl Pts',(157.201864385759,-223.987700282465,13.3321696602647));
#84129=CARTESIAN_POINT('Ctrl Pts',(159.332744790571,-222.100157914766,13.1734117950329));
#84130=CARTESIAN_POINT('Ctrl Pts',(162.074297136814,-222.86655090944,13.0146539298011));
#84131=CARTESIAN_POINT('Ctrl Pts',(162.917452825014,-225.585476427899,12.8558960645693));
#84132=CARTESIAN_POINT('Ctrl Pts',(161.090555802487,-227.768573942568,12.6971381993376));
#84133=CARTESIAN_POINT('Ctrl Pts',(158.26558215241,-227.417872693871,12.5383803341057));
#84134=CARTESIAN_POINT('Ctrl Pts',(157.027947648243,-224.854334450823,12.379622468874));
#84135=CARTESIAN_POINT('Ctrl Pts',(158.51033533953,-222.424109312655,12.2208646036422));
#84136=CARTESIAN_POINT('Ctrl Pts',(161.356064069501,-222.35133923025,12.0621067384104));
#84137=CARTESIAN_POINT('Ctrl Pts',(162.96072301639,-224.702623380164,11.9033488731786));
#84138=CARTESIAN_POINT('Ctrl Pts',(161.855728375107,-227.326066600858,11.7445910079468));
#84139=CARTESIAN_POINT('Ctrl Pts',(159.052371197901,-227.820693759917,11.585833142715));
#84140=CARTESIAN_POINT('Ctrl Pts',(157.116283863111,-225.733822100821,11.4270752774832));
#84141=CARTESIAN_POINT('Ctrl Pts',(157.819373423403,-222.97535648391,11.2683174122514));
#84142=CARTESIAN_POINT('Ctrl Pts',(160.518172340845,-222.069844533308,11.1095595470196));
#84143=CARTESIAN_POINT('Ctrl Pts',(162.742739952322,-223.846010750597,10.9508016817878));
#84144=CARTESIAN_POINT('Ctrl Pts',(162.457152067289,-226.67830788356,10.792043816556));
#84145=CARTESIAN_POINT('Ctrl Pts',(159.922778706899,-227.974617707487,10.6332859513243));
#84146=CARTESIAN_POINT('Ctrl Pts',(157.459078270917,-226.548557522496,10.4745280860924));
#84147=CARTESIAN_POINT('Ctrl Pts',(157.320829301473,-223.705257553812,10.3157702208607));
#84148=CARTESIAN_POINT('Ctrl Pts',(159.634557249965,-222.046905820965,10.1570123556289));
#84149=CARTESIAN_POINT('Ctrl Pts',(162.282738388918,-223.091225764643,9.99825449039707));
#84150=CARTESIAN_POINT('Ctrl Pts',(162.8417574441,-225.882455813459,9.83949662516529));
#84151=CARTESIAN_POINT('Ctrl Pts',(160.800000198191,-227.866062336499,9.68073875993349));
#84152=CARTESIAN_POINT('Ctrl Pts',(158.026082802357,-227.226648721881,9.52198089470171));
#84153=CARTESIAN_POINT('Ctrl Pts',(157.058694348183,-224.549406284558,9.36322302946991));
#84154=CARTESIAN_POINT('Ctrl Pts',(158.783188710889,-222.284547197889,9.20446516423812));
#84155=CARTESIAN_POINT('Ctrl Pts',(161.621308717539,-222.504870408929,9.04570729900632));
#84156=CARTESIAN_POINT('Ctrl Pts',(162.975607049654,-225.008736123599,8.88694943377453));
#84157=CARTESIAN_POINT('Ctrl Pts',(161.606629926939,-227.504606538295,8.72819156854274));
#84158=CARTESIAN_POINT('Ctrl Pts',(158.767265158268,-227.708261147634,8.56943370331095));
#84159=CARTESIAN_POINT('Ctrl Pts',(157.056099268275,-225.433315261159,8.41067583807915));
#84160=CARTESIAN_POINT('Ctrl Pts',(158.03919121219,-222.76179926471,8.25191797284736));
#84161=CARTESIAN_POINT('Ctrl Pts',(160.816815281602,-222.138684493184,8.09316010761556));
#84162=CARTESIAN_POINT('Ctrl Pts',(162.846890037412,-224.134245560977,7.93440224238378));
#84163=CARTESIAN_POINT('Ctrl Pts',(162.271491142934,-226.922145057319,7.77564437715198));
#84164=CARTESIAN_POINT('Ctrl Pts',(159.617223643767,-227.950897472789,7.6168865119202));
#84165=CARTESIAN_POINT('Ctrl Pts',(157.313273050772,-226.278988637203,7.45812864668839));
#84166=CARTESIAN_POINT('Ctrl Pts',(157.468214856058,-223.436549451145,7.29937078145661));
#84167=CARTESIAN_POINT('Ctrl Pts',(159.940246325519,-222.024980145917,7.14061291622482));
#84168=CARTESIAN_POINT('Ctrl Pts',(162.466964355516,-223.336148894156,6.98185505099302));
#84169=CARTESIAN_POINT('Ctrl Pts',(162.735916704355,-226.170074109035,6.82309718576123));
#84170=CARTESIAN_POINT('Ctrl Pts',(160.500958192956,-227.933147545337,6.66433932052944));
#84171=CARTESIAN_POINT('Ctrl Pts',(157.807522763063,-227.01180446349,6.50558145529765));
#84172=CARTESIAN_POINT('Ctrl Pts',(157.120642414198,-224.249258015769,6.34682359006585));
#84173=CARTESIAN_POINT('Ctrl Pts',(159.06895001463,-222.173790602495,6.18806572483406));
#84174=CARTESIAN_POINT('Ctrl Pts',(161.869354525061,-222.684869918679,6.02930785960226));
#84175=CARTESIAN_POINT('Ctrl Pts',(162.958925847666,-225.314756194248,5.87054999437047));
#84176=CARTESIAN_POINT('Ctrl Pts',(161.340488350845,-227.656577613219,5.71179212913869));
#84177=CARTESIAN_POINT('Ctrl Pts',(158.495235968043,-227.567099305039,5.55303426390689));
#84178=CARTESIAN_POINT('Ctrl Pts',(157.027143568115,-225.128211813837,5.3942763986751));
#84179=CARTESIAN_POINT('Ctrl Pts',(158.279809257744,-222.571984875653,5.2355185334433));
#84180=CARTESIAN_POINT('Ctrl Pts',(161.10679344704,-222.237877283792,5.07676066821151));
#84181=CARTESIAN_POINT('Ctrl Pts',(162.920840317129,-224.431664293187,4.91800280297972));
#84182=CARTESIAN_POINT('Ctrl Pts',(162.061734243841,-227.145592119108,4.75924493774793));
#84183=CARTESIAN_POINT('Ctrl Pts',(159.315729071664,-227.895874121996,4.60048707251614));
#84184=CARTESIAN_POINT('Ctrl Pts',(157.195968626195,-225.995852242308,4.44172920728434));
#84185=CARTESIAN_POINT('Ctrl Pts',(157.64245758376,-223.184426429626,4.28297134205255));
#84186=CARTESIAN_POINT('Ctrl Pts',(160.246569267972,-222.034613477144,4.12421347682076));
#84187=CARTESIAN_POINT('Ctrl Pts',(162.625020767807,-223.598722153791,3.96545561158897));
#84188=CARTESIAN_POINT('Ctrl Pts',(162.601053364222,-226.445280260137,3.80669774635717));
#84189=CARTESIAN_POINT('Ctrl Pts',(160.19660202388,-227.969117929339,3.64793988112538));
#84190=CARTESIAN_POINT('Ctrl Pts',(157.612220519232,-226.775618986163,3.48918201589359));
#84191=CARTESIAN_POINT('Ctrl Pts',(157.213134701033,-223.957073617098,3.3304241506618));
#84192=CARTESIAN_POINT('Ctrl Pts',(159.364587895797,-222.093014431776,3.17166628543));
#84193=CARTESIAN_POINT('Ctrl Pts',(162.097570221393,-222.889428325998,3.01290842019821));
#84194=CARTESIAN_POINT('Ctrl Pts',(162.910856366896,-225.617437329495,2.85415055496642));
#84195=CARTESIAN_POINT('Ctrl Pts',(161.060126871497,-227.78036772115,2.69539268973463));
#84196=CARTESIAN_POINT('Ctrl Pts',(158.239169322395,-227.398705667494,2.53663482450284));
#84197=CARTESIAN_POINT('Ctrl Pts',(157.02972390408,-224.821748314993,2.37787695927104));
#84198=CARTESIAN_POINT('Ctrl Pts',(158.538675126888,-222.407926827632,2.21911909403925));
#84199=CARTESIAN_POINT('Ctrl Pts',(161.385030660596,-222.366370750881,2.06036122880746));
#84200=CARTESIAN_POINT('Ctrl Pts',(162.96380651088,-224.735111758081,1.90160336357567));
#84201=CARTESIAN_POINT('Ctrl Pts',(161.830106089352,-227.346279099041,1.74284549834387));
#84202=CARTESIAN_POINT('Ctrl Pts',(159.021494036293,-227.810130603545,1.58408763311208));
#84203=CARTESIAN_POINT('Ctrl Pts',(157.108407719473,-225.702153382141,1.42532976788029));
#84204=CARTESIAN_POINT('Ctrl Pts',(157.841712527075,-222.951559827016,1.2665719026485));
#84205=CARTESIAN_POINT('Ctrl Pts',(160.55026952987,-222.07571022901,1.1078140374167));
#84206=CARTESIAN_POINT('Ctrl Pts',(162.755245642935,-223.876146461489,0.94905617218491));
#84207=CARTESIAN_POINT('Ctrl Pts',(162.438567593097,-226.705183319779,0.790298306953122));
#84208=CARTESIAN_POINT('Ctrl Pts',(159.890223508887,-227.973532899909,0.631540441721324));
#84209=CARTESIAN_POINT('Ctrl Pts',(157.442116673283,-226.520720196198,0.472782576489534));
#84210=CARTESIAN_POINT('Ctrl Pts',(157.335462206895,-223.675698352418,0.314024711257741));
#84211=CARTESIAN_POINT('Ctrl Pts',(159.666401148433,-222.043601838811,0.155266846025946));
#84212=CARTESIAN_POINT('Ctrl Pts',(162.304705428334,-223.115261021833,-0.0034910192058423));
#84213=CARTESIAN_POINT('Ctrl Pts',(162.829415850734,-225.915728625906,-0.162248884437638));
#84214=CARTESIAN_POINT('Ctrl Pts',(161.458872983031,-227.215894200354,-0.268087461258832));
#84215=CARTESIAN_POINT('Ctrl Pts',(160.650199997975,-227.432086802035,-0.32100674966943));
#84216=CARTESIAN_POINT('Ctrl Pts',(162.054331550342,-223.243574678773,20.1070022498898));
#84217=CARTESIAN_POINT('Ctrl Pts',(162.638345947507,-223.926643402192,20.0540829614792));
#84218=CARTESIAN_POINT('Ctrl Pts',(163.060277072331,-225.910476203892,19.948244384658));
#84219=CARTESIAN_POINT('Ctrl Pts',(160.892947255847,-228.069149518281,19.7894865194262));
#84220=CARTESIAN_POINT('Ctrl Pts',(157.906932210104,-227.412859036056,19.6307286541944));
#84221=CARTESIAN_POINT('Ctrl Pts',(156.837131867137,-224.551286469627,19.4719707889626));
#84222=CARTESIAN_POINT('Ctrl Pts',(158.66167332233,-222.098955567599,19.3132129237308));
#84223=CARTESIAN_POINT('Ctrl Pts',(161.711202632654,-222.302345569707,19.1544550584991));
#84224=CARTESIAN_POINT('Ctrl Pts',(163.194566389237,-224.974298665732,18.9956971932673));
#84225=CARTESIAN_POINT('Ctrl Pts',(161.75429827463,-227.669932720152,18.8369393280355));
#84226=CARTESIAN_POINT('Ctrl Pts',(158.708479502562,-227.921967783242,18.6781814628037));
#84227=CARTESIAN_POINT('Ctrl Pts',(156.844668405157,-225.499854994514,18.5194235975719));
#84228=CARTESIAN_POINT('Ctrl Pts',(157.868612723895,-222.620257128595,18.3606657323401));
#84229=CARTESIAN_POINT('Ctrl Pts',(160.843204490409,-221.918608425839,18.2019078671083));
#84230=CARTESIAN_POINT('Ctrl Pts',(163.046094626516,-224.037045035389,18.0431500018765));
#84231=CARTESIAN_POINT('Ctrl Pts',(162.461199520659,-227.036779983476,17.8843921366447));
#84232=CARTESIAN_POINT('Ctrl Pts',(159.623814498028,-228.172453010433,17.7256342714129));
#84233=CARTESIAN_POINT('Ctrl Pts',(157.130714534295,-226.404697629797,17.5668764061811));
#84234=CARTESIAN_POINT('Ctrl Pts',(157.26358446665,-223.35136281058,17.4081185409493));
#84235=CARTESIAN_POINT('Ctrl Pts',(159.900821811276,-221.806860789769,17.2493606757176));
#84236=CARTESIAN_POINT('Ctrl Pts',(162.628827018873,-223.184719596799,17.0906028104858));
#84237=CARTESIAN_POINT('Ctrl Pts',(162.950929847691,-226.223922982415,16.931844945254));
#84238=CARTESIAN_POINT('Ctrl Pts',(160.572341793286,-228.142992090625,16.7730870800222));
#84239=CARTESIAN_POINT('Ctrl Pts',(157.669946553453,-227.185594966888,16.6143292147904));
#84240=CARTESIAN_POINT('Ctrl Pts',(156.900016135656,-224.227941412607,16.4555713495586));
#84241=CARTESIAN_POINT('Ctrl Pts',(158.9671908289,-221.976875848494,16.2968134843268));
#84242=CARTESIAN_POINT('Ctrl Pts',(161.979592434777,-222.492573388309,16.138055619095));
#84243=CARTESIAN_POINT('Ctrl Pts',(163.180271122261,-225.303067664855,15.9792977538632));
#84244=CARTESIAN_POINT('Ctrl Pts',(161.47036580368,-227.836194426292,15.8205398886314));
#84245=CARTESIAN_POINT('Ctrl Pts',(158.414781759407,-227.77363616039,15.6617820233996));
#84246=CARTESIAN_POINT('Ctrl Pts',(156.80998938658,-225.172646189535,15.5030241581678));
#84247=CARTESIAN_POINT('Ctrl Pts',(158.124694601715,-222.413650432824,15.344266292936));
#84248=CARTESIAN_POINT('Ctrl Pts',(161.155679243613,-222.021681698278,15.1855084277043));
#84249=CARTESIAN_POINT('Ctrl Pts',(163.128986287204,-224.355469756353,15.0267505624724));
#84250=CARTESIAN_POINT('Ctrl Pts',(162.238645203789,-227.279131868066,14.8679926972407));
#84251=CARTESIAN_POINT('Ctrl Pts',(159.2994961179,-228.116932583751,14.7092348320089));
#84252=CARTESIAN_POINT('Ctrl Pts',(157.001448157361,-226.102116721357,14.5504769667771));
#84253=CARTESIAN_POINT('Ctrl Pts',(157.447674725291,-223.078643678917,14.3917191015453));
#84254=CARTESIAN_POINT('Ctrl Pts',(160.229789284266,-221.813595865977,14.2329612363135));
#84255=CARTESIAN_POINT('Ctrl Pts',(162.801600699318,-223.464744991192,14.0742033710817));
#84256=CARTESIAN_POINT('Ctrl Pts',(162.809387264524,-226.520959440096,13.9154455058499));
#84257=CARTESIAN_POINT('Ctrl Pts',(160.246022715714,-228.185191869234,13.7566876406181));
#84258=CARTESIAN_POINT('Ctrl Pts',(157.457498187158,-226.934336824904,13.5979297753863));
#84259=CARTESIAN_POINT('Ctrl Pts',(156.995871217733,-223.913176794487,13.4391719101545));
#84260=CARTESIAN_POINT('Ctrl Pts',(159.283622791705,-221.886677319018,13.2804140449227));
#84261=CARTESIAN_POINT('Ctrl Pts',(162.227002758537,-222.709490638754,13.1216561796909));
#84262=CARTESIAN_POINT('Ctrl Pts',(163.132229888331,-225.628578035831,12.9628983144592));
#84263=CARTESIAN_POINT('Ctrl Pts',(161.170840347497,-227.972390839234,12.8041404492274));
#84264=CARTESIAN_POINT('Ctrl Pts',(158.137897766675,-227.595871663456,12.6453825839956));
#84265=CARTESIAN_POINT('Ctrl Pts',(156.809151076567,-224.843610843364,12.4866247187638));
#84266=CARTESIAN_POINT('Ctrl Pts',(158.400669195708,-222.234477373275,12.327866853532));
#84267=CARTESIAN_POINT('Ctrl Pts',(161.455894804045,-222.156350102414,12.1691089883002));
#84268=CARTESIAN_POINT('Ctrl Pts',(163.178685544971,-224.680731106,12.0103511230684));
#84269=CARTESIAN_POINT('Ctrl Pts',(161.992343400139,-227.49730698882,11.8515932578366));
#84270=CARTESIAN_POINT('Ctrl Pts',(158.982608653847,-228.028347613676,11.6928353926048));
#84271=CARTESIAN_POINT('Ctrl Pts',(156.903990427546,-225.787844621583,11.534077527373));
#84272=CARTESIAN_POINT('Ctrl Pts',(157.658840040207,-222.826306262798,11.3753196621412));
#84273=CARTESIAN_POINT('Ctrl Pts',(160.556319156007,-221.854132326822,11.2165617969094));
#84274=CARTESIAN_POINT('Ctrl Pts',(162.944655002106,-223.76105636163,11.0578039316776));
#84275=CARTESIAN_POINT('Ctrl Pts',(162.638042706073,-226.801861565554,10.8990460664459));
#84276=CARTESIAN_POINT('Ctrl Pts',(159.917093829181,-228.193603135539,10.7402882012141));
#84277=CARTESIAN_POINT('Ctrl Pts',(157.272020676562,-226.662559241464,10.5815303359823));
#84278=CARTESIAN_POINT('Ctrl Pts',(157.123594093479,-223.60994119498,10.4227724707505));
#84279=CARTESIAN_POINT('Ctrl Pts',(159.607654082932,-221.829504912187,10.2640146055187));
#84280=CARTESIAN_POINT('Ctrl Pts',(162.450789040257,-222.950705609084,10.1052567402869));
#84281=CARTESIAN_POINT('Ctrl Pts',(163.050961964314,-225.94742045196,9.9464988750551));
#84282=CARTESIAN_POINT('Ctrl Pts',(160.858894618607,-228.077056134459,9.7877410098233));
#84283=CARTESIAN_POINT('Ctrl Pts',(157.880766951726,-227.390570163703,9.62898314459151));
#84284=CARTESIAN_POINT('Ctrl Pts',(156.842161287288,-224.516234473133,9.47022527935971));
#84285=CARTESIAN_POINT('Ctrl Pts',(158.693609488546,-222.084640973728,9.31146741412793));
#84286=CARTESIAN_POINT('Ctrl Pts',(161.740666234513,-222.321183940523,9.15270954889614));
#84287=CARTESIAN_POINT('Ctrl Pts',(163.194665311105,-225.00937925961,8.99395168366434));
#84288=CARTESIAN_POINT('Ctrl Pts',(161.7249068206,-227.688990680671,8.83519381843255));
#84289=CARTESIAN_POINT('Ctrl Pts',(158.676513675713,-227.907637936523,8.67643595320076));
#84290=CARTESIAN_POINT('Ctrl Pts',(156.839375162768,-225.46521506721,8.51767808796896));
#84291=CARTESIAN_POINT('Ctrl Pts',(157.89484037657,-222.59702738668,8.35892022273718));
#84292=CARTESIAN_POINT('Ctrl Pts',(160.876947594951,-221.928040147366,8.20016235750537));
#84293=CARTESIAN_POINT('Ctrl Pts',(163.056472408918,-224.070510444381,8.04140449227359));
#84294=CARTESIAN_POINT('Ctrl Pts',(162.438713794436,-227.063649546147,7.88264662704179));
#84295=CARTESIAN_POINT('Ctrl Pts',(159.589044411186,-228.16813666443,7.72388876181001));
#84296=CARTESIAN_POINT('Ctrl Pts',(157.115481566658,-226.373145232011,7.56513089657821));
#84297=CARTESIAN_POINT('Ctrl Pts',(157.281829878894,-223.321451337253,7.40637303134642));
#84298=CARTESIAN_POINT('Ctrl Pts',(159.935847379076,-221.805965112634,7.24761516611462));
#84299=CARTESIAN_POINT('Ctrl Pts',(162.648577355406,-223.213659491329,7.08885730088284));
#84300=CARTESIAN_POINT('Ctrl Pts',(162.937329440221,-226.256212633314,6.93009943565103));
#84301=CARTESIAN_POINT('Ctrl Pts',(160.537837736853,-228.149080022689,6.77134157041925));
#84302=CARTESIAN_POINT('Ctrl Pts',(157.646116957868,-227.159909499134,6.61258370518745));
#84303=CARTESIAN_POINT('Ctrl Pts',(156.908669846477,-224.193989886907,6.45382583995567));
#84304=CARTESIAN_POINT('Ctrl Pts',(159.000407970027,-221.965730698488,6.29506797472386));
#84305=CARTESIAN_POINT('Ctrl Pts',(162.0069726801,-222.514434655492,6.13631010949208));
#84306=CARTESIAN_POINT('Ctrl Pts',(163.176756072268,-225.337927918048,5.97755224426028));
#84307=CARTESIAN_POINT('Ctrl Pts',(161.439172432019,-227.852149563295,5.8187943790285));
#84308=CARTESIAN_POINT('Ctrl Pts',(158.38445823858,-227.756084040372,5.66003651379669));
#84309=CARTESIAN_POINT('Ctrl Pts',(156.808287801664,-225.137650512081,5.50127864856492));
#84310=CARTESIAN_POINT('Ctrl Pts',(158.153172243153,-222.393239240547,5.34252078333311));
#84311=CARTESIAN_POINT('Ctrl Pts',(161.188273375084,-222.034535313555,5.18376291810133));
#84312=CARTESIAN_POINT('Ctrl Pts',(163.135866760866,-224.389824550984,5.02500505286953));
#84313=CARTESIAN_POINT('Ctrl Pts',(162.213515010418,-227.303546335358,4.86624718763774));
#84314=CARTESIAN_POINT('Ctrl Pts',(159.265354409479,-228.109062604197,4.70748932240594));
#84315=CARTESIAN_POINT('Ctrl Pts',(156.989541424098,-226.069164899934,4.54873145717415));
#84316=CARTESIAN_POINT('Ctrl Pts',(157.468900008993,-223.050767521301,4.38997359194236));
#84317=CARTESIAN_POINT('Ctrl Pts',(160.264721206137,-221.816307630509,4.23121572671057));
#84318=CARTESIAN_POINT('Ctrl Pts',(162.818269565808,-223.495562871105,4.07245786147878));
#84319=CARTESIAN_POINT('Ctrl Pts',(162.792537729731,-226.551678912853,3.91369999624698));
#84320=CARTESIAN_POINT('Ctrl Pts',(160.211075473106,-228.187698474683,3.75494213101519));
#84321=CARTESIAN_POINT('Ctrl Pts',(157.436436952028,-226.906336517617,3.5961842657834));
#84322=CARTESIAN_POINT('Ctrl Pts',(157.007971231159,-223.880295455047,3.43742640055161));
#84323=CARTESIAN_POINT('Ctrl Pts',(159.317810122882,-221.879007947045,3.27866853531981));
#84324=CARTESIAN_POINT('Ctrl Pts',(162.251989161226,-222.734052245131,3.11991067008802));
#84325=CARTESIAN_POINT('Ctrl Pts',(163.125147812112,-225.662891835315,2.96115280485623));
#84326=CARTESIAN_POINT('Ctrl Pts',(161.138171299243,-227.985052852294,2.80239493962444));
#84327=CARTESIAN_POINT('Ctrl Pts',(158.109540476748,-227.575293598792,2.64363707439265));
#84328=CARTESIAN_POINT('Ctrl Pts',(156.81105809682,-224.808625781148,2.48487920916085));
#84329=CARTESIAN_POINT('Ctrl Pts',(158.431095301738,-222.217103565952,2.32612134392906));
#84330=CARTESIAN_POINT('Ctrl Pts',(161.486993857854,-222.17248821364,2.16736347869727));
#84331=CARTESIAN_POINT('Ctrl Pts',(163.181996040181,-224.715611213558,2.00860561346547));
#84332=CARTESIAN_POINT('Ctrl Pts',(161.964834852766,-227.519007490841,1.84984774823368));
#84333=CARTESIAN_POINT('Ctrl Pts',(158.949458377131,-228.017006818781,1.69108988300189));
#84334=CARTESIAN_POINT('Ctrl Pts',(156.895534457907,-225.753844514941,1.5323320177701));
#84335=CARTESIAN_POINT('Ctrl Pts',(157.682823704176,-222.800757743443,1.37357415253831));
#84336=CARTESIAN_POINT('Ctrl Pts',(160.590779276128,-221.860429843354,1.21481628730651));
#84337=CARTESIAN_POINT('Ctrl Pts',(162.958081336741,-223.793410603506,1.05605842207472));
#84338=CARTESIAN_POINT('Ctrl Pts',(162.618090079924,-226.830715517833,0.897300556842932));
#84339=CARTESIAN_POINT('Ctrl Pts',(159.882141982365,-228.192438466589,0.738542691611134));
#84340=CARTESIAN_POINT('Ctrl Pts',(157.253810399909,-226.632672586676,0.579784826379344));
#84341=CARTESIAN_POINT('Ctrl Pts',(157.139304244238,-223.578205904082,0.421026961147551));
#84342=CARTESIAN_POINT('Ctrl Pts',(159.641842265749,-221.825957697451,0.262269095915756));
#84343=CARTESIAN_POINT('Ctrl Pts',(162.474373249341,-222.976510294013,0.103511230683968));
#84344=CARTESIAN_POINT('Ctrl Pts',(163.037711807438,-225.983142742557,-0.055246634547828));
#84345=CARTESIAN_POINT('Ctrl Pts',(161.56627230492,-227.379023915733,-0.161085211369022));
#84346=CARTESIAN_POINT('Ctrl Pts',(160.698066426161,-227.611132185939,-0.21400449977962));
#84347=CARTESIAN_POINT('Ctrl Pts',(162.195197104019,-223.123136560921,20.2140044997796));
#84348=CARTESIAN_POINT('Ctrl Pts',(162.819257379562,-223.853043319762,20.161085211369));
#84349=CARTESIAN_POINT('Ctrl Pts',(163.270120329681,-225.972907574598,20.0552466345478));
#84350=CARTESIAN_POINT('Ctrl Pts',(160.95417666625,-228.279601159419,19.896488769316));
#84351=CARTESIAN_POINT('Ctrl Pts',(157.76341051174,-227.578308826282,19.7377309040842));
#84352=CARTESIAN_POINT('Ctrl Pts',(156.620253938806,-224.520518174272,19.5789730388525));
#84353=CARTESIAN_POINT('Ctrl Pts',(158.569904236459,-221.900030895413,19.4202151736206));
#84354=CARTESIAN_POINT('Ctrl Pts',(161.828539829886,-222.117367353854,19.2614573083889));
#84355=CARTESIAN_POINT('Ctrl Pts',(163.413617867613,-224.97253632475,19.1026994431571));
#84356=CARTESIAN_POINT('Ctrl Pts',(161.874590540856,-227.853010057811,18.9439415779253));
#84357=CARTESIAN_POINT('Ctrl Pts',(158.619919917364,-228.122327169995,18.7851837126935));
#84358=CARTESIAN_POINT('Ctrl Pts',(156.628307257382,-225.534130061043,18.6264258474617));
#84359=CARTESIAN_POINT('Ctrl Pts',(157.722463457629,-222.457078114412,18.4676679822299));
#84360=CARTESIAN_POINT('Ctrl Pts',(160.901023038434,-221.707317346696,18.3089101169981));
#84361=CARTESIAN_POINT('Ctrl Pts',(163.254965393284,-223.971015195058,18.1501522517663));
#84362=CARTESIAN_POINT('Ctrl Pts',(162.629964018838,-227.176442025878,17.9913943865345));
#84363=CARTESIAN_POINT('Ctrl Pts',(159.598019450966,-228.389988174002,17.8326365213027));
#84364=CARTESIAN_POINT('Ctrl Pts',(156.933967575063,-226.501017773124,17.6738786560709));
#84365=CARTESIAN_POINT('Ctrl Pts',(157.07594840122,-223.238315726986,17.5151207908392));
#84366=CARTESIAN_POINT('Ctrl Pts',(159.894021160979,-221.587907173084,17.3563629256074));
#84367=CARTESIAN_POINT('Ctrl Pts',(162.80908573781,-223.060245784851,17.1976050603756));
#84368=CARTESIAN_POINT('Ctrl Pts',(163.153275163757,-226.307847404716,17.0388471951438));
#84369=CARTESIAN_POINT('Ctrl Pts',(160.611587280992,-228.358507118361,16.880089329912));
#84370=CARTESIAN_POINT('Ctrl Pts',(157.510174744083,-227.335461255546,16.7213314646802));
#84371=CARTESIAN_POINT('Ctrl Pts',(156.687450182819,-224.175001340511,16.5625735994484));
#84372=CARTESIAN_POINT('Ctrl Pts',(158.896371084294,-221.769580167636,16.4038157342166));
#84373=CARTESIAN_POINT('Ctrl Pts',(162.115333125871,-222.320639097614,16.2450578689848));
#84374=CARTESIAN_POINT('Ctrl Pts',(163.398342373908,-225.323849020427,16.086300003753));
#84375=CARTESIAN_POINT('Ctrl Pts',(161.571188814945,-228.030672332319,15.9275421385212));
#84376=CARTESIAN_POINT('Ctrl Pts',(158.306083314347,-227.963824444928,15.7687842732894));
#84377=CARTESIAN_POINT('Ctrl Pts',(156.591250297839,-225.184484542052,15.6100264080576));
#84378=CARTESIAN_POINT('Ctrl Pts',(157.996104874706,-222.236304393562,15.4512685428259));
#84379=CARTESIAN_POINT('Ctrl Pts',(161.23492419144,-221.817458355396,15.2925106775941));
#84380=CARTESIAN_POINT('Ctrl Pts',(163.34354093673,-224.311274305225,15.1337528123623));
#84381=CARTESIAN_POINT('Ctrl Pts',(162.392149148207,-227.435411983827,14.9749949471305));
#84382=CARTESIAN_POINT('Ctrl Pts',(159.251462553313,-228.330660710601,14.8162370818987));
#84383=CARTESIAN_POINT('Ctrl Pts',(156.795837400192,-226.177688886008,14.6574792166669));
#84384=CARTESIAN_POINT('Ctrl Pts',(157.272661732414,-222.946896239252,14.4987213514351));
#84385=CARTESIAN_POINT('Ctrl Pts',(160.245545939881,-221.595104073596,14.3399634862033));
#84386=CARTESIAN_POINT('Ctrl Pts',(162.993706512824,-223.359472525891,14.1812056209715));
#84387=CARTESIAN_POINT('Ctrl Pts',(163.002027002956,-226.625251657978,14.0224477557397));
#84388=CARTESIAN_POINT('Ctrl Pts',(160.262892498034,-228.403600536596,13.8636898905079));
#84389=CARTESIAN_POINT('Ctrl Pts',(157.283158789249,-227.066974337964,13.7049320252761));
#84390=CARTESIAN_POINT('Ctrl Pts',(156.789878049707,-223.83865330651,13.5461741600443));
#84391=CARTESIAN_POINT('Ctrl Pts',(159.234500792838,-221.673196723269,13.3874162948126));
#84392=CARTESIAN_POINT('Ctrl Pts',(162.379708380261,-222.552430368069,13.2286584295807));
#84393=CARTESIAN_POINT('Ctrl Pts',(163.347006951649,-225.671679643764,13.069900564349));
#84394=CARTESIAN_POINT('Ctrl Pts',(161.251124892506,-228.176207735899,12.9111426991172));
#84395=CARTESIAN_POINT('Ctrl Pts',(158.010213380941,-227.773870633041,12.7523848338854));
#84396=CARTESIAN_POINT('Ctrl Pts',(156.590354504892,-224.832887235903,12.5936269686536));
#84397=CARTESIAN_POINT('Ctrl Pts',(158.291003051885,-222.044845433895,12.4348691034218));
#84398=CARTESIAN_POINT('Ctrl Pts',(161.555725538588,-221.961360974578,12.27611123819));
#84399=CARTESIAN_POINT('Ctrl Pts',(163.396648073553,-224.658838831835,12.1173533729582));
#84400=CARTESIAN_POINT('Ctrl Pts',(162.128958425172,-227.668547376781,11.9585955077264));
#84401=CARTESIAN_POINT('Ctrl Pts',(158.912846109793,-228.236001467435,11.7998376424946));
#84402=CARTESIAN_POINT('Ctrl Pts',(156.69169699198,-225.841867142345,11.6410797772628));
#84403=CARTESIAN_POINT('Ctrl Pts',(157.498306657011,-222.677256041687,11.482321912031));
#84404=CARTESIAN_POINT('Ctrl Pts',(160.594465971169,-221.638420120337,11.3235640467992));
#84405=CARTESIAN_POINT('Ctrl Pts',(163.14657005189,-223.676101972664,11.1648061815675));
#84406=CARTESIAN_POINT('Ctrl Pts',(162.818933344857,-226.925415247548,11.0060483163357));
#84407=CARTESIAN_POINT('Ctrl Pts',(159.911408951463,-228.412588563591,10.8472904511039));
#84408=CARTESIAN_POINT('Ctrl Pts',(157.084963082206,-226.776560960433,10.6885325858721));
#84409=CARTESIAN_POINT('Ctrl Pts',(156.926358885484,-223.514624836148,10.5297747206403));
#84410=CARTESIAN_POINT('Ctrl Pts',(159.580750915898,-221.612104003409,10.3710168554085));
#84411=CARTESIAN_POINT('Ctrl Pts',(162.618839691596,-222.810185453525,10.2122589901767));
#84412=CARTESIAN_POINT('Ctrl Pts',(163.260166484529,-226.012385090462,10.0535011249449));
#84413=CARTESIAN_POINT('Ctrl Pts',(160.917789039023,-228.288049932419,9.89474325971311));
#84414=CARTESIAN_POINT('Ctrl Pts',(157.735451101095,-227.554491605526,9.73598539448133));
#84415=CARTESIAN_POINT('Ctrl Pts',(156.625628226393,-224.483062661708,9.57722752924952));
#84416=CARTESIAN_POINT('Ctrl Pts',(158.604030266202,-221.884734749567,9.41846966401774));
#84417=CARTESIAN_POINT('Ctrl Pts',(161.860023751488,-222.137497472117,9.25971179878594));
#84418=CARTESIAN_POINT('Ctrl Pts',(163.413723572555,-225.010022395621,9.10095393355415));
#84419=CARTESIAN_POINT('Ctrl Pts',(161.843183714261,-227.873374823046,8.94219606832236));
#84420=CARTESIAN_POINT('Ctrl Pts',(158.585762193157,-228.107014725413,8.78343820309056));
#84421=CARTESIAN_POINT('Ctrl Pts',(156.622651057262,-225.497114873262,8.62468033785878));
#84422=CARTESIAN_POINT('Ctrl Pts',(157.750489540949,-222.43225550865,8.46592247262698));
#84423=CARTESIAN_POINT('Ctrl Pts',(160.937079908301,-221.717395801548,8.30716460739519));
#84424=CARTESIAN_POINT('Ctrl Pts',(163.266054780425,-224.006775327784,8.14840674216339));
#84425=CARTESIAN_POINT('Ctrl Pts',(162.605936445939,-227.205154034974,7.9896488769316));
#84426=CARTESIAN_POINT('Ctrl Pts',(159.560865178606,-228.385375856072,7.83089101169981));
#84427=CARTESIAN_POINT('Ctrl Pts',(156.917690082544,-226.467301826819,7.67213314646802));
#84428=CARTESIAN_POINT('Ctrl Pts',(157.095444901729,-223.206353223362,7.51337528123623));
#84429=CARTESIAN_POINT('Ctrl Pts',(159.931448432633,-221.58695007935,7.35461741600444));
#84430=CARTESIAN_POINT('Ctrl Pts',(162.830190355295,-223.091170088503,7.19585955077264));
#84431=CARTESIAN_POINT('Ctrl Pts',(163.138742176086,-226.342351157594,7.03710168554085));
#84432=CARTESIAN_POINT('Ctrl Pts',(160.574717280751,-228.365012500042,6.87834382030906));
#84433=CARTESIAN_POINT('Ctrl Pts',(157.484711152673,-227.308014534778,6.71958595507727));
#84434=CARTESIAN_POINT('Ctrl Pts',(156.696697278757,-224.138721758045,6.56082808984547));
#84435=CARTESIAN_POINT('Ctrl Pts',(158.931865925424,-221.757670794481,6.40207022461368));
#84436=CARTESIAN_POINT('Ctrl Pts',(162.144590835139,-222.343999392306,6.24331235938189));
#84437=CARTESIAN_POINT('Ctrl Pts',(163.394586296869,-225.361099641848,6.08455449415009));
#84438=CARTESIAN_POINT('Ctrl Pts',(161.537856513193,-228.047721513371,5.9257966289183));
#84439=CARTESIAN_POINT('Ctrl Pts',(158.273680509117,-227.945068775705,5.76703876368651));
#84440=CARTESIAN_POINT('Ctrl Pts',(156.589432035212,-225.147089210326,5.60828089845471));
#84441=CARTESIAN_POINT('Ctrl Pts',(158.026535228563,-222.214493605441,5.44952303322293));
#84442=CARTESIAN_POINT('Ctrl Pts',(161.269753303129,-221.831193343318,5.29076516799113));
#84443=CARTESIAN_POINT('Ctrl Pts',(163.350893204603,-224.347984808781,5.13200730275934));
#84444=CARTESIAN_POINT('Ctrl Pts',(162.365295776996,-227.461500551607,4.97324943752755));
#84445=CARTESIAN_POINT('Ctrl Pts',(159.214979747294,-228.322251086399,4.81449157229575));
#84446=CARTESIAN_POINT('Ctrl Pts',(156.783114222002,-226.142477557561,4.65573370706396));
#84447=CARTESIAN_POINT('Ctrl Pts',(157.295342434226,-222.917108612975,4.49697584183217));
#84448=CARTESIAN_POINT('Ctrl Pts',(160.282873144302,-221.598001783875,4.33821797660038));
#84449=CARTESIAN_POINT('Ctrl Pts',(163.011518363809,-223.392403588418,4.17946011136858));
#84450=CARTESIAN_POINT('Ctrl Pts',(162.984022095241,-226.658077565569,4.0207022461368));
#84451=CARTESIAN_POINT('Ctrl Pts',(160.225548922332,-228.406279020027,3.861944380905));
#84452=CARTESIAN_POINT('Ctrl Pts',(157.260653384824,-227.037054049071,3.70318651567321));
#84453=CARTESIAN_POINT('Ctrl Pts',(156.802807761284,-223.803517292995,3.54442865044142));
#84454=CARTESIAN_POINT('Ctrl Pts',(159.271032349968,-221.665001462314,3.38567078520962));
#84455=CARTESIAN_POINT('Ctrl Pts',(162.40640810106,-222.578676164264,3.22691291997783));
#84456=CARTESIAN_POINT('Ctrl Pts',(163.339439257329,-225.708346341134,3.06815505474604));
#84457=CARTESIAN_POINT('Ctrl Pts',(161.216215726989,-228.189737983437,2.90939718951425));
#84458=CARTESIAN_POINT('Ctrl Pts',(157.979911631102,-227.75188153009,2.75063932428245));
#84459=CARTESIAN_POINT('Ctrl Pts',(156.59239228956,-224.795503247303,2.59188145905066));
#84460=CARTESIAN_POINT('Ctrl Pts',(158.323515476587,-222.026280304273,2.43312359381887));
#84461=CARTESIAN_POINT('Ctrl Pts',(161.588957055112,-221.978605676399,2.27436572858708));
#84462=CARTESIAN_POINT('Ctrl Pts',(163.400185569483,-224.696110669036,2.11560786335528));
#84463=CARTESIAN_POINT('Ctrl Pts',(162.099563616179,-227.691735882641,1.95684999812349));
#84464=CARTESIAN_POINT('Ctrl Pts',(158.877422717969,-228.223883034018,1.7980921328917));
#84465=CARTESIAN_POINT('Ctrl Pts',(156.682661196342,-225.80553564774,1.63933426765991));
#84466=CARTESIAN_POINT('Ctrl Pts',(157.523934881276,-222.649955659871,1.48057640242812));
#84467=CARTESIAN_POINT('Ctrl Pts',(160.631289022385,-221.645149457697,1.32181853719632));
#84468=CARTESIAN_POINT('Ctrl Pts',(163.160917030547,-223.710674745524,1.16306067196453));
#84469=CARTESIAN_POINT('Ctrl Pts',(162.797612566751,-226.956247715886,1.00430280673274));
#84470=CARTESIAN_POINT('Ctrl Pts',(159.874060455843,-228.411344033269,0.845544941500945));
#84471=CARTESIAN_POINT('Ctrl Pts',(157.065504126535,-226.744624977154,0.686787076269154));
#84472=CARTESIAN_POINT('Ctrl Pts',(156.943146281581,-223.480713455746,0.528029211037361));
#84473=CARTESIAN_POINT('Ctrl Pts',(159.617283383065,-221.608313556091,0.369271345805566));
#84474=CARTESIAN_POINT('Ctrl Pts',(162.644041070348,-222.837759566193,0.210513480573778));
#84475=CARTESIAN_POINT('Ctrl Pts',(163.246007764142,-226.050556859208,0.0517556153419821));
#84476=CARTESIAN_POINT('Ctrl Pts',(161.673671626809,-227.542153631111,-0.0540829614792118));
#84477=CARTESIAN_POINT('Ctrl Pts',(160.745932854347,-227.790177569842,-0.10700224988981));
#84478=CARTESIAN_POINT('Ctrl Pts',(162.336062657696,-223.002698443069,20.3210067496694));
#84479=CARTESIAN_POINT('Ctrl Pts',(163.000168811616,-223.779443237332,20.2680874612588));
#84480=CARTESIAN_POINT('Ctrl Pts',(163.47996358703,-226.035338945303,20.1622488844376));
#84481=CARTESIAN_POINT('Ctrl Pts',(161.015406076653,-228.490052800557,20.0034910192058));
#84482=CARTESIAN_POINT('Ctrl Pts',(157.619888813377,-227.743758616508,19.844733153974));
#84483=CARTESIAN_POINT('Ctrl Pts',(156.403376010475,-224.489749878917,19.6859752887423));
#84484=CARTESIAN_POINT('Ctrl Pts',(158.478135150588,-221.701106223228,19.5272174235105));
#84485=CARTESIAN_POINT('Ctrl Pts',(161.945877027117,-221.932389138002,19.3684595582787));
#84486=CARTESIAN_POINT('Ctrl Pts',(163.63266934599,-224.970773983768,19.2097016930469));
#84487=CARTESIAN_POINT('Ctrl Pts',(161.994882807082,-228.036087395469,19.0509438278151));
#84488=CARTESIAN_POINT('Ctrl Pts',(158.531360332167,-228.322686556747,18.8921859625833));
#84489=CARTESIAN_POINT('Ctrl Pts',(156.411946109607,-225.568405127571,18.7334280973515));
#84490=CARTESIAN_POINT('Ctrl Pts',(157.576314191364,-222.293899100229,18.5746702321197));
#84491=CARTESIAN_POINT('Ctrl Pts',(160.95884158646,-221.496026267553,18.4159123668879));
#84492=CARTESIAN_POINT('Ctrl Pts',(163.463836160053,-223.904985354727,18.2571545016561));
#84493=CARTESIAN_POINT('Ctrl Pts',(162.798728517017,-227.31610406828,18.0983966364243));
#84494=CARTESIAN_POINT('Ctrl Pts',(159.572224403905,-228.607523337571,17.9396387711925));
#84495=CARTESIAN_POINT('Ctrl Pts',(156.737220615831,-226.597337916451,17.7808809059608));
#84496=CARTESIAN_POINT('Ctrl Pts',(156.88831233579,-223.125268643393,17.622123040729));
#84497=CARTESIAN_POINT('Ctrl Pts',(159.887220510682,-221.3689535564,17.4633651754972));
#84498=CARTESIAN_POINT('Ctrl Pts',(162.989344456746,-222.935771972903,17.3046073102654));
#84499=CARTESIAN_POINT('Ctrl Pts',(163.355620479822,-226.391771827016,17.1458494450336));
#84500=CARTESIAN_POINT('Ctrl Pts',(160.650832768699,-228.574022146095,16.9870915798018));
#84501=CARTESIAN_POINT('Ctrl Pts',(157.350402934712,-227.485327544205,16.82833371457));
#84502=CARTESIAN_POINT('Ctrl Pts',(156.474884229982,-224.122061268415,16.6695758493382));
#84503=CARTESIAN_POINT('Ctrl Pts',(158.825551339689,-221.562284486778,16.5108179841064));
#84504=CARTESIAN_POINT('Ctrl Pts',(162.251073816965,-222.14870480692,16.3520601188746));
#84505=CARTESIAN_POINT('Ctrl Pts',(163.616413625555,-225.344630375999,16.1933022536428));
#84506=CARTESIAN_POINT('Ctrl Pts',(161.672011826211,-228.225150238345,16.034544388411));
#84507=CARTESIAN_POINT('Ctrl Pts',(158.197384869287,-228.154012729466,15.8757865231792));
#84508=CARTESIAN_POINT('Ctrl Pts',(156.372511209097,-225.196322894569,15.7170286579475));
#84509=CARTESIAN_POINT('Ctrl Pts',(157.867515147698,-222.058958354301,15.5582707927157));
#84510=CARTESIAN_POINT('Ctrl Pts',(161.314169139266,-221.613235012514,15.3995129274839));
#84511=CARTESIAN_POINT('Ctrl Pts',(163.558095586257,-224.267078854098,15.2407550622521));
#84512=CARTESIAN_POINT('Ctrl Pts',(162.545653092624,-227.591692099587,15.0819971970203));
#84513=CARTESIAN_POINT('Ctrl Pts',(159.203428988727,-228.544388837452,14.9232393317885));
#84514=CARTESIAN_POINT('Ctrl Pts',(156.590226643023,-226.253261050659,14.7644814665567));
#84515=CARTESIAN_POINT('Ctrl Pts',(157.097648739538,-222.815148799587,14.6057236013249));
#84516=CARTESIAN_POINT('Ctrl Pts',(160.261302595496,-221.376612281216,14.4469657360931));
#84517=CARTESIAN_POINT('Ctrl Pts',(163.185812326331,-223.254200060589,14.2882078708613));
#84518=CARTESIAN_POINT('Ctrl Pts',(163.194666741387,-226.72954387586,14.1294500056295));
#84519=CARTESIAN_POINT('Ctrl Pts',(160.279762280353,-228.622009203956,13.9706921403977));
#84520=CARTESIAN_POINT('Ctrl Pts',(157.108819391341,-227.199611851024,13.8119342751659));
#84521=CARTESIAN_POINT('Ctrl Pts',(156.583884881681,-223.764129818532,13.6531764099342));
#84522=CARTESIAN_POINT('Ctrl Pts',(159.185378793971,-221.459716127521,13.4944185447024));
#84523=CARTESIAN_POINT('Ctrl Pts',(162.532414001985,-222.395370097384,13.3356606794706));
#84524=CARTESIAN_POINT('Ctrl Pts',(163.561784014967,-225.714781251697,13.1769028142388));
#84525=CARTESIAN_POINT('Ctrl Pts',(161.331409437515,-228.380024632565,13.018144949007));
#84526=CARTESIAN_POINT('Ctrl Pts',(157.882528995206,-227.951869602626,12.8593870837752));
#84527=CARTESIAN_POINT('Ctrl Pts',(156.371557933217,-224.822163628443,12.7006292185434));
#84528=CARTESIAN_POINT('Ctrl Pts',(158.181336908062,-221.855213494516,12.5418713533116));
#84529=CARTESIAN_POINT('Ctrl Pts',(161.655556273132,-221.766371846742,12.3831134880798));
#84530=CARTESIAN_POINT('Ctrl Pts',(163.614610602134,-224.63694655767,12.224355622848));
#84531=CARTESIAN_POINT('Ctrl Pts',(162.265573450205,-227.839787764742,12.0655977576162));
#84532=CARTESIAN_POINT('Ctrl Pts',(158.843083565739,-228.443655321194,11.9068398923844));
#84533=CARTESIAN_POINT('Ctrl Pts',(156.479403556414,-225.895889663108,11.7480820271526));
#84534=CARTESIAN_POINT('Ctrl Pts',(157.337773273815,-222.528205820575,11.5893241619208));
#84535=CARTESIAN_POINT('Ctrl Pts',(160.632612786331,-221.422707913851,11.4305662966891));
#84536=CARTESIAN_POINT('Ctrl Pts',(163.348485101673,-223.591147583697,11.2718084314573));
#84537=CARTESIAN_POINT('Ctrl Pts',(162.99982398364,-227.048968929542,11.1130505662255));
#84538=CARTESIAN_POINT('Ctrl Pts',(159.905724073745,-228.631573991643,10.9542927009937));
#84539=CARTESIAN_POINT('Ctrl Pts',(156.897905487851,-226.890562679401,10.7955348357619));
#84540=CARTESIAN_POINT('Ctrl Pts',(156.729123677489,-223.419308477316,10.6367769705301));
#84541=CARTESIAN_POINT('Ctrl Pts',(159.553847748865,-221.394703094632,10.4780191052983));
#84542=CARTESIAN_POINT('Ctrl Pts',(162.786890342936,-222.669665297966,10.3192612400665));
#84543=CARTESIAN_POINT('Ctrl Pts',(163.469371004743,-226.077349728964,10.1605033748347));
#84544=CARTESIAN_POINT('Ctrl Pts',(160.97668345944,-228.499043730379,10.0017455096029));
#84545=CARTESIAN_POINT('Ctrl Pts',(157.590135250464,-227.718413047349,9.84298764437114));
#84546=CARTESIAN_POINT('Ctrl Pts',(156.409095165498,-224.449890850283,9.68422977913933));
#84547=CARTESIAN_POINT('Ctrl Pts',(158.514451043859,-221.684828525406,9.52547191390756));
#84548=CARTESIAN_POINT('Ctrl Pts',(161.979381268463,-221.953811003712,9.36671404867575));
#84549=CARTESIAN_POINT('Ctrl Pts',(163.632781834006,-225.010665531631,9.20795618344396));
#84550=CARTESIAN_POINT('Ctrl Pts',(161.961460607923,-228.057758965422,9.04919831821217));
#84551=CARTESIAN_POINT('Ctrl Pts',(158.495010710601,-228.306391514302,8.89044045298037));
#84552=CARTESIAN_POINT('Ctrl Pts',(156.405926951755,-225.529014679313,8.73168258774859));
#84553=CARTESIAN_POINT('Ctrl Pts',(157.606138705329,-222.26748363062,8.5729247225168));
#84554=CARTESIAN_POINT('Ctrl Pts',(160.99721222165,-221.50675145573,8.41416685728499));
#84555=CARTESIAN_POINT('Ctrl Pts',(163.475637151931,-223.943040211187,8.25540899205321));
#84556=CARTESIAN_POINT('Ctrl Pts',(162.773159097441,-227.346658523802,8.09665112682141));
#84557=CARTESIAN_POINT('Ctrl Pts',(159.532685946025,-228.602615047713,7.93789326158963));
#84558=CARTESIAN_POINT('Ctrl Pts',(156.71989859843,-226.561458421627,7.77913539635782));
#84559=CARTESIAN_POINT('Ctrl Pts',(156.909059924565,-223.091255109471,7.62037753112604));
#84560=CARTESIAN_POINT('Ctrl Pts',(159.92704948619,-221.367935046067,7.46161966589424));
#84561=CARTESIAN_POINT('Ctrl Pts',(163.011803355185,-222.968680685676,7.30286180066245));
#84562=CARTESIAN_POINT('Ctrl Pts',(163.340154911951,-226.428489681874,7.14410393543066));
#84563=CARTESIAN_POINT('Ctrl Pts',(160.611596824648,-228.580944977395,6.98534607019887));
#84564=CARTESIAN_POINT('Ctrl Pts',(157.323305347477,-227.456119570422,6.82658820496707));
#84565=CARTESIAN_POINT('Ctrl Pts',(156.484724711037,-224.083453629183,6.66783033973528));
#84566=CARTESIAN_POINT('Ctrl Pts',(158.863323880821,-221.549610890473,6.50907247450349));
#84567=CARTESIAN_POINT('Ctrl Pts',(162.282208990179,-222.17356412912,6.3503146092717));
#84568=CARTESIAN_POINT('Ctrl Pts',(163.61241652147,-225.384271365649,6.19155674403991));
#84569=CARTESIAN_POINT('Ctrl Pts',(161.636540594368,-228.243293463447,6.03279887880811));
#84570=CARTESIAN_POINT('Ctrl Pts',(158.162902779655,-228.134053511038,5.87404101357632));
#84571=CARTESIAN_POINT('Ctrl Pts',(156.37057626876,-225.156527908571,5.71528314834453));
#84572=CARTESIAN_POINT('Ctrl Pts',(157.899898213972,-222.035747970335,5.55652528311273));
#84573=CARTESIAN_POINT('Ctrl Pts',(161.351233231173,-221.627851373082,5.39776741788094));
#84574=CARTESIAN_POINT('Ctrl Pts',(163.56591964834,-224.306145066578,5.23900955264915));
#84575=CARTESIAN_POINT('Ctrl Pts',(162.517076543573,-227.619454767856,5.08025168741736));
#84576=CARTESIAN_POINT('Ctrl Pts',(159.164605085109,-228.535439568601,4.92149382218557));
#84577=CARTESIAN_POINT('Ctrl Pts',(156.576687019905,-226.215790215187,4.76273595695377));
#84578=CARTESIAN_POINT('Ctrl Pts',(157.121784859459,-222.78344970465,4.60397809172198));
#84579=CARTESIAN_POINT('Ctrl Pts',(160.301025082467,-221.37969593724,4.44522022649019));
#84580=CARTESIAN_POINT('Ctrl Pts',(163.20476716181,-223.289244305731,4.2864623612584));
#84581=CARTESIAN_POINT('Ctrl Pts',(163.17550646075,-226.764476218285,4.1277044960266));
#84582=CARTESIAN_POINT('Ctrl Pts',(160.240022371557,-228.624859565371,3.96894663079482));
#84583=CARTESIAN_POINT('Ctrl Pts',(157.08486981762,-227.167771580525,3.81018876556302));
#84584=CARTESIAN_POINT('Ctrl Pts',(156.59764429141,-223.726739130944,3.65143090033123));
#84585=CARTESIAN_POINT('Ctrl Pts',(159.224254577053,-221.450994977583,3.49267303509943));
#84586=CARTESIAN_POINT('Ctrl Pts',(162.560827040894,-222.423300083398,3.33391516986764));
#84587=CARTESIAN_POINT('Ctrl Pts',(163.553730702545,-225.753800846953,3.17515730463585));
#84588=CARTESIAN_POINT('Ctrl Pts',(161.294260154735,-228.39442311458,3.01639943940406));
#84589=CARTESIAN_POINT('Ctrl Pts',(157.850282785455,-227.928469461388,2.85764157417226));
#84590=CARTESIAN_POINT('Ctrl Pts',(156.3737264823,-224.782380713458,2.69888370894047));
#84591=CARTESIAN_POINT('Ctrl Pts',(158.215935651436,-221.835457042593,2.54012584370868));
#84592=CARTESIAN_POINT('Ctrl Pts',(161.69092025237,-221.784723139159,2.38136797847689));
#84593=CARTESIAN_POINT('Ctrl Pts',(163.618375098784,-224.676610124513,2.22261011324509));
#84594=CARTESIAN_POINT('Ctrl Pts',(162.234292379592,-227.864464274441,2.0638522480133));
#84595=CARTESIAN_POINT('Ctrl Pts',(158.805387058807,-228.430759249254,1.90509438278151));
#84596=CARTESIAN_POINT('Ctrl Pts',(156.469787934776,-225.85722678054,1.74633651754972));
#84597=CARTESIAN_POINT('Ctrl Pts',(157.365046058377,-222.499153576299,1.58757865231793));
#84598=CARTESIAN_POINT('Ctrl Pts',(160.671798768642,-221.429869072041,1.42882078708613));
#84599=CARTESIAN_POINT('Ctrl Pts',(163.363752724354,-223.627938887541,1.27006292185434));
#84600=CARTESIAN_POINT('Ctrl Pts',(162.977135053578,-227.081779913939,1.11130505662255));
#84601=CARTESIAN_POINT('Ctrl Pts',(159.865978929321,-228.630249599949,0.952547191390754));
#84602=CARTESIAN_POINT('Ctrl Pts',(156.877197853162,-226.856577367632,0.793789326158964));
#84603=CARTESIAN_POINT('Ctrl Pts',(156.746988318924,-223.38322100741,0.635031460927171));
#84604=CARTESIAN_POINT('Ctrl Pts',(159.592724500381,-221.390669414731,0.476273595695376));
#84605=CARTESIAN_POINT('Ctrl Pts',(162.813708891355,-222.699008838373,0.317515730463588));
#84606=CARTESIAN_POINT('Ctrl Pts',(163.454303720846,-226.117970975858,0.158757865231792));
#84607=CARTESIAN_POINT('Ctrl Pts',(161.781070948697,-227.70528334649,0.0529192884105984));
#84608=CARTESIAN_POINT('Ctrl Pts',(160.793799282533,-227.969222953746,0.));
#84609=CARTESIAN_POINT('Ctrl Pts',(160.793799282533,-227.969222953746,0.));
#84610=CARTESIAN_POINT('Ctrl Pts',(160.886835131854,-227.935190024475,-3.02457214913811E-16));
#84611=CARTESIAN_POINT('Ctrl Pts',(160.977803977775,-227.896385137717,-1.37333377546448E-15));
#84612=CARTESIAN_POINT('Ctrl Pts',(161.066498279727,-227.853137686896,-6.66133814775094E-16));
#84613=CARTESIAN_POINT('Ctrl Pts',(161.157170911953,-227.808925599797,5.68402718963673E-17));
#84614=CARTESIAN_POINT('Ctrl Pts',(161.245467067815,-227.7600699377,-1.69277578169131E-15));
#84615=CARTESIAN_POINT('Ctrl Pts',(161.331136079803,-227.706877059437,-1.27675647831893E-15));
#84616=CARTESIAN_POINT('Ctrl Pts',(161.414071319396,-227.655381612005,-8.7401271135087E-16));
#84617=CARTESIAN_POINT('Ctrl Pts',(161.494544733236,-227.599820476436,1.75893653509998E-15));
#84618=CARTESIAN_POINT('Ctrl Pts',(161.572295205067,-227.540440925299,1.88737914186277E-15));
#84619=CARTESIAN_POINT('Ctrl Pts',(161.640326867919,-227.488483818054,1.9997664227802E-15));
#84620=CARTESIAN_POINT('Ctrl Pts',(161.70627348163,-227.433602519189,4.82523262324037E-15));
#84621=CARTESIAN_POINT('Ctrl Pts',(161.769934874098,-227.375949718044,5.32907051820075E-15));
#84622=CARTESIAN_POINT('Ctrl Pts',(161.783313679488,-227.363833652454,5.43495493077293E-15));
#84623=CARTESIAN_POINT('Ctrl Pts',(161.79659337319,-227.351593235715,6.17321314109589E-15));
#84624=CARTESIAN_POINT('Ctrl Pts',(161.809754802739,-227.339246301387,6.0507154842071E-15));
#84625=CARTESIAN_POINT('Ctrl Pts',(161.882179710651,-227.271303409741,5.37663357792855E-15));
#84626=CARTESIAN_POINT('Ctrl Pts',(161.951138858742,-227.200038396299,1.6501302217819E-15));
#84627=CARTESIAN_POINT('Ctrl Pts',(162.016393029598,-227.125743280976,1.83186799063151E-15));
#84628=CARTESIAN_POINT('Ctrl Pts',(162.081289564234,-227.051855352256,2.01260971573651E-15));
#84629=CARTESIAN_POINT('Ctrl Pts',(162.142522107232,-226.974969645043,4.08055444834208E-16));
#84630=CARTESIAN_POINT('Ctrl Pts',(162.199811733062,-226.895346657282,-8.60422844084496E-16));
#84631=CARTESIAN_POINT('Ctrl Pts',(162.255642444754,-226.817751315904,-2.09659858463182E-15));
#84632=CARTESIAN_POINT('Ctrl Pts',(162.307728765594,-226.737555590414,-1.2543397869325E-15));
#84633=CARTESIAN_POINT('Ctrl Pts',(162.355765747154,-226.65498650143,-1.36002320516582E-15));
#84634=CARTESIAN_POINT('Ctrl Pts',(162.376479635949,-226.619382121811,-1.40559464828665E-15));
#84635=CARTESIAN_POINT('Ctrl Pts',(162.396439968897,-226.583336323596,-1.93777603934293E-15));
#84636=CARTESIAN_POINT('Ctrl Pts',(162.415619320772,-226.546866979337,-2.02615701994091E-15));
#84637=CARTESIAN_POINT('Ctrl Pts',(162.428829664771,-226.521747643385,-2.08703202574327E-15));
#84638=CARTESIAN_POINT('Ctrl Pts',(162.441669459883,-226.496427366951,-3.53414151482419E-15));
#84639=CARTESIAN_POINT('Ctrl Pts',(162.454129213649,-226.470911987081,-3.1641356201817E-15));
#84640=CARTESIAN_POINT('Ctrl Pts',(162.460341854643,-226.45818959321,-2.97964451127121E-15));
#84641=CARTESIAN_POINT('Ctrl Pts',(162.466459455713,-226.445419669975,-1.69354284525896E-15));
#84642=CARTESIAN_POINT('Ctrl Pts',(162.472475650985,-226.432614465927,-1.63757896132211E-15));
#84643=CARTESIAN_POINT('Ctrl Pts',(162.512676180897,-226.347049426042,-1.26362537626533E-15));
#84644=CARTESIAN_POINT('Ctrl Pts',(162.548420108931,-226.259774184938,-2.83979563700065E-18));
#84645=CARTESIAN_POINT('Ctrl Pts',(162.579456396658,-226.171026817168,-7.7715611723761E-16));
#84646=CARTESIAN_POINT('Ctrl Pts',(162.609806651508,-226.084241140585,-1.53435678186565E-15));
#84647=CARTESIAN_POINT('Ctrl Pts',(162.635655300542,-225.996047022835,-1.68477216875799E-15));
#84648=CARTESIAN_POINT('Ctrl Pts',(162.656718450553,-225.906658343455,-1.9151347174784E-15));
#84649=CARTESIAN_POINT('Ctrl Pts',(162.660341355547,-225.891283307301,-1.95475754824121E-15));
#84650=CARTESIAN_POINT('Ctrl Pts',(162.66382255848,-225.875872922801,-1.31552826697175E-15));
#84651=CARTESIAN_POINT('Ctrl Pts',(162.667160456718,-225.860428273356,-1.30451205393456E-15));
#84652=CARTESIAN_POINT('Ctrl Pts',(162.687288048911,-225.767296732645,-1.2092570774105E-15));
#84653=CARTESIAN_POINT('Ctrl Pts',(162.70220900913,-225.672918237907,3.95464250160003E-15));
#84654=CARTESIAN_POINT('Ctrl Pts',(162.71200163869,-225.577700926241,5.27355936696949E-15));
#84655=CARTESIAN_POINT('Ctrl Pts',(162.71526433647,-225.545976524792,5.71299466904966E-15));
#84656=CARTESIAN_POINT('Ctrl Pts',(162.717957335588,-225.514159127666,1.08684253548423E-14));
#84657=CARTESIAN_POINT('Ctrl Pts',(162.720082333063,-225.482264288845,1.15463194561016E-14));
#84658=CARTESIAN_POINT('Ctrl Pts',(162.721307135479,-225.463880796112,1.19370429005596E-14));
#84659=CARTESIAN_POINT('Ctrl Pts',(162.722343230258,-225.445471581581,4.25907006365195E-15));
#84660=CARTESIAN_POINT('Ctrl Pts',(162.723190856866,-225.427039671918,4.35762537165374E-15));
#84661=CARTESIAN_POINT('Ctrl Pts',(162.723765383164,-225.414546415178,4.42442673887179E-15));
#84662=CARTESIAN_POINT('Ctrl Pts',(162.724253204013,-225.40204435614,3.39829207989485E-15));
#84663=CARTESIAN_POINT('Ctrl Pts',(162.724654274891,-225.389543824009,3.19189119579733E-15));
#84664=CARTESIAN_POINT('Ctrl Pts',(162.727643921145,-225.296362864977,1.65334610634577E-15));
#84665=CARTESIAN_POINT('Ctrl Pts',(162.725824895213,-225.203120691748,6.39634240367912E-16));
#84666=CARTESIAN_POINT('Ctrl Pts',(162.719335998398,-225.110191721826,2.4980018054066E-16));
#84667=CARTESIAN_POINT('Ctrl Pts',(162.712834250128,-225.017078703282,-1.40805957372921E-16));
#84668=CARTESIAN_POINT('Ctrl Pts',(162.701643731984,-224.924279149824,1.77023230634299E-15));
#84669=CARTESIAN_POINT('Ctrl Pts',(162.685853037124,-224.8321817391,1.60982338570648E-15));
#84670=CARTESIAN_POINT('Ctrl Pts',(162.670284969111,-224.741382773839,1.45167600786084E-15));
#84671=CARTESIAN_POINT('Ctrl Pts',(162.650245055058,-224.651265446538,2.60240118438736E-15));
#84672=CARTESIAN_POINT('Ctrl Pts',(162.625775144772,-224.562227386308,4.16333634234434E-15));
#84673=CARTESIAN_POINT('Ctrl Pts',(162.616258304647,-224.527598694405,4.77041541085431E-15));
#84674=CARTESIAN_POINT('Ctrl Pts',(162.606070959923,-224.493133590178,6.71445756624556E-15));
#84675=CARTESIAN_POINT('Ctrl Pts',(162.595214003931,-224.45885692894,6.66133814775094E-15));
#84676=CARTESIAN_POINT('Ctrl Pts',(162.589230527729,-224.439966405027,6.63206301974616E-15));
#84677=CARTESIAN_POINT('Ctrl Pts',(162.583043654131,-224.421133133431,-2.06375398258952E-15));
#84678=CARTESIAN_POINT('Ctrl Pts',(162.576653426697,-224.402361401392,-1.97064586870965E-15));
#84679=CARTESIAN_POINT('Ctrl Pts',(162.57141710462,-224.386979345604,-1.8943506073516E-15));
#84680=CARTESIAN_POINT('Ctrl Pts',(162.566043962058,-224.371638089573,6.8029554114436E-15));
#84681=CARTESIAN_POINT('Ctrl Pts',(162.560539518476,-224.356354677768,6.38378239159465E-15));
#84682=CARTESIAN_POINT('Ctrl Pts',(162.528144500718,-224.266408002972,3.91684504924636E-15));
#84683=CARTESIAN_POINT('Ctrl Pts',(162.491164517742,-224.178337626994,4.67507282145047E-15));
#84684=CARTESIAN_POINT('Ctrl Pts',(162.449672187927,-224.092586398355,7.09848846369709E-15));
#84685=CARTESIAN_POINT('Ctrl Pts',(162.418552940565,-224.028272976875,8.91605019538206E-15));
#84686=CARTESIAN_POINT('Ctrl Pts',(162.384894352882,-223.965264611358,4.96167796900426E-15));
#84687=CARTESIAN_POINT('Ctrl Pts',(162.348709733279,-223.903765223849,5.12090370108353E-15));
#84688=CARTESIAN_POINT('Ctrl Pts',(162.334283097957,-223.879245711253,5.18438624133952E-15));
#84689=CARTESIAN_POINT('Ctrl Pts',(162.319454775845,-223.854966251689,1.42974040300608E-15));
#84690=CARTESIAN_POINT('Ctrl Pts',(162.304225021793,-223.830940576599,6.80011602582908E-16));
#84691=CARTESIAN_POINT('Ctrl Pts',(162.293795413291,-223.814487363743,1.66583884431403E-16));
#84692=CARTESIAN_POINT('Ctrl Pts',(162.28318192805,-223.798160209656,4.27605544559612E-15));
#84693=CARTESIAN_POINT('Ctrl Pts',(162.272389031914,-223.781969041488,4.02455846426619E-15));
#84694=CARTESIAN_POINT('Ctrl Pts',(162.224799336923,-223.710576456493,2.91561935445547E-15));
#84695=CARTESIAN_POINT('Ctrl Pts',(162.173700478564,-223.641787621303,5.11345936751299E-15));
#84696=CARTESIAN_POINT('Ctrl Pts',(162.119126329557,-223.575955009348,4.88151186139874E-15));
#84697=CARTESIAN_POINT('Ctrl Pts',(162.068157476713,-223.514471453999,4.66488735104534E-15));
#84698=CARTESIAN_POINT('Ctrl Pts',(162.014156816139,-223.45556630499,3.49062128769292E-15));
#84699=CARTESIAN_POINT('Ctrl Pts',(161.957129225973,-223.39956097681,4.09394740330526E-15));
#84700=CARTESIAN_POINT('Ctrl Pts',(161.943965194155,-223.386632920057,4.23408426879927E-15));
#84701=CARTESIAN_POINT('Ctrl Pts',(161.930639785301,-223.373859540263,5.90640714698764E-16));
#84702=CARTESIAN_POINT('Ctrl Pts',(161.9171563836,-223.361242235853,7.21644966006352E-16));
#84703=CARTESIAN_POINT('Ctrl Pts',(157.480508436316,-225.001988388677,18.387416697508));
#84704=CARTESIAN_POINT('Ctrl Pts',(157.479370520287,-225.133541934848,18.3957515808994));
#84705=CARTESIAN_POINT('Ctrl Pts',(157.488784872591,-225.264932202126,18.4040864642907));
#84706=CARTESIAN_POINT('Ctrl Pts',(157.509319881608,-225.394560708534,18.4124213476821));
#84707=CARTESIAN_POINT('Ctrl Pts',(157.639699397875,-226.217589417486,18.4653406360927));
#84708=CARTESIAN_POINT('Ctrl Pts',(158.218369242817,-226.969598906988,18.5182599245033));
#84709=CARTESIAN_POINT('Ctrl Pts',(158.980531985396,-227.306478149406,18.5711792129139));
#84710=CARTESIAN_POINT('Ctrl Pts',(159.742694727975,-227.643357391824,18.6240985013245));
#84711=CARTESIAN_POINT('Ctrl Pts',(160.688350368189,-227.565106387159,18.6770177897351));
#84712=CARTESIAN_POINT('Ctrl Pts',(161.384763005373,-227.10751515553,18.7299370781457));
#84713=CARTESIAN_POINT('Ctrl Pts',(162.081175642556,-226.6499239239,18.7828563665563));
#84714=CARTESIAN_POINT('Ctrl Pts',(162.528345276708,-225.812992465307,18.8357756549668));
#84715=CARTESIAN_POINT('Ctrl Pts',(162.521655181211,-224.979737199152,18.8886949433774));
#84716=CARTESIAN_POINT('Ctrl Pts',(162.514965085714,-224.146481932996,18.941614231788));
#84717=CARTESIAN_POINT('Ctrl Pts',(162.054415260568,-223.316902859278,18.9945335201987));
#84718=CARTESIAN_POINT('Ctrl Pts',(161.350736510125,-222.870539398123,19.0474528086093));
#84719=CARTESIAN_POINT('Ctrl Pts',(160.647057759681,-222.424175936968,19.1003720970199));
#84720=CARTESIAN_POINT('Ctrl Pts',(159.700250083941,-222.361028088376,19.1532913854304));
#84721=CARTESIAN_POINT('Ctrl Pts',(158.943607477282,-222.71014991828,19.206210673841));
#84722=CARTESIAN_POINT('Ctrl Pts',(158.186964870623,-223.059271748183,19.2591299622516));
#84723=CARTESIAN_POINT('Ctrl Pts',(157.620487333045,-223.820663256583,19.3120492506622));
#84724=CARTESIAN_POINT('Ctrl Pts',(157.50332258309,-224.64558475759,19.3649685390728));
#84725=CARTESIAN_POINT('Ctrl Pts',(157.486755637785,-224.762227599343,19.3724512585512));
#84726=CARTESIAN_POINT('Ctrl Pts',(157.479172071341,-224.880140634173,19.3799339780296));
#84727=CARTESIAN_POINT('Ctrl Pts',(157.48014261364,-224.998176427436,19.387416697508));
#84728=CARTESIAN_POINT('Ctrl Pts',(159.206200717467,-227.969222953746,20.));
#84729=CARTESIAN_POINT('Ctrl Pts',(158.218929051303,-227.70528334649,19.9470807115894));
#84730=CARTESIAN_POINT('Ctrl Pts',(156.545695841364,-226.117974132338,19.8412421347682));
#84731=CARTESIAN_POINT('Ctrl Pts',(157.186291485908,-222.699008209422,19.6824842695364));
#84732=CARTESIAN_POINT('Ctrl Pts',(160.407275465985,-221.390670340075,19.5237264043046));
#84733=CARTESIAN_POINT('Ctrl Pts',(163.253011317767,-223.383220872305,19.3649685390728));
#84734=CARTESIAN_POINT('Ctrl Pts',(163.122801873322,-226.856577342785,19.2062106738411));
#84735=CARTESIAN_POINT('Ctrl Pts',(160.134021031603,-228.6302491553,19.0474528086092));
#84736=CARTESIAN_POINT('Ctrl Pts',(157.022865258248,-227.081779751736,18.8886949433775));
#84737=CARTESIAN_POINT('Ctrl Pts',(156.636247599646,-223.627939000525,18.7299370781456));
#84738=CARTESIAN_POINT('Ctrl Pts',(159.328201303672,-221.429869438357,18.5711792129139));
#84739=CARTESIAN_POINT('Ctrl Pts',(162.634953676974,-222.499153818262,18.4124213476821));
#84740=CARTESIAN_POINT('Ctrl Pts',(163.530211716637,-225.857226698665,18.2536634824503));
#84741=CARTESIAN_POINT('Ctrl Pts',(161.194612821702,-228.430758907163,18.0949056172185));
#84742=CARTESIAN_POINT('Ctrl Pts',(157.765707842634,-227.864463991016,17.9361477519867));
#84743=CARTESIAN_POINT('Ctrl Pts',(156.381625260024,-224.676610156181,17.7773898867549));
#84744=CARTESIAN_POINT('Ctrl Pts',(158.309079915571,-221.784723458447,17.6186320215231));
#84745=CARTESIAN_POINT('Ctrl Pts',(161.784064171446,-221.835457356522,17.4598741562913));
#84746=CARTESIAN_POINT('Ctrl Pts',(163.626273157879,-224.782380735109,17.3011162910595));
#84747=CARTESIAN_POINT('Ctrl Pts',(162.149717001196,-227.928469170749,17.1423584258277));
#84748=CARTESIAN_POINT('Ctrl Pts',(158.705739973713,-228.394422777744,16.983600560596));
#84749=CARTESIAN_POINT('Ctrl Pts',(156.44626965011,-225.753800772142,16.8248426953641));
#84750=CARTESIAN_POINT('Ctrl Pts',(157.439173213236,-222.423300339104,16.6660848301324));
#84751=CARTESIAN_POINT('Ctrl Pts',(160.775745345963,-221.450995329772,16.5073269649006));
#84752=CARTESIAN_POINT('Ctrl Pts',(163.402355370953,-223.726739257298,16.3485690996688));
#84753=CARTESIAN_POINT('Ctrl Pts',(162.915129893092,-227.167771365402,16.189811234437));
#84754=CARTESIAN_POINT('Ctrl Pts',(159.759977652262,-228.624859205653,16.0310533692052));
#84755=CARTESIAN_POINT('Ctrl Pts',(156.824493854376,-226.764476043185,15.8722955039734));
#84756=CARTESIAN_POINT('Ctrl Pts',(156.79523315622,-223.2892444755,15.7135376387416));
#84757=CARTESIAN_POINT('Ctrl Pts',(159.698974947405,-221.379696296506,15.5547797735098));
#84758=CARTESIAN_POINT('Ctrl Pts',(162.878214854917,-222.783449924613,15.396021908278));
#84759=CARTESIAN_POINT('Ctrl Pts',(163.423312640378,-226.215790094536,15.2372640430462));
#84760=CARTESIAN_POINT('Ctrl Pts',(160.83539483199,-228.535439217757,15.0785061778144));
#84761=CARTESIAN_POINT('Ctrl Pts',(157.482923706213,-227.619454507911,14.9197483125826));
#84762=CARTESIAN_POINT('Ctrl Pts',(156.43408070553,-224.306145135434,14.7609904473509));
#84763=CARTESIAN_POINT('Ctrl Pts',(158.648766902918,-221.627851707722,14.6022325821191));
#84764=CARTESIAN_POINT('Ctrl Pts',(162.100101577621,-222.035748264497,14.4434747168873));
#84765=CARTESIAN_POINT('Ctrl Pts',(163.629423371069,-225.156527893037,14.2847168516555));
#84766=CARTESIAN_POINT('Ctrl Pts',(161.837097038039,-228.134053200026,14.1259589864237));
#84767=CARTESIAN_POINT('Ctrl Pts',(158.363459568037,-228.243293141594,13.9672011211919));
#84768=CARTESIAN_POINT('Ctrl Pts',(156.387583837013,-225.384271327515,13.8084432559601));
#84769=CARTESIAN_POINT('Ctrl Pts',(157.7177912363,-222.173564409605,13.6496853907283));
#84770=CARTESIAN_POINT('Ctrl Pts',(161.136676006379,-221.549611232878,13.4909275254965));
#84771=CARTESIAN_POINT('Ctrl Pts',(163.515274940119,-224.083453720138,13.3321696602647));
#84772=CARTESIAN_POINT('Ctrl Pts',(162.676694386897,-227.456119326685,13.1734117950329));
#84773=CARTESIAN_POINT('Ctrl Pts',(159.388403236045,-228.580944622035,13.0146539298011));
#84774=CARTESIAN_POINT('Ctrl Pts',(156.659845419514,-226.428489540116,12.8558960645693));
#84775=CARTESIAN_POINT('Ctrl Pts',(156.988196943696,-222.968680887257,12.6971381993375));
#84776=CARTESIAN_POINT('Ctrl Pts',(160.072950506571,-221.367935406501,12.5383803341058));
#84777=CARTESIAN_POINT('Ctrl Pts',(163.090939768701,-223.091255298888,12.379622468874));
#84778=CARTESIAN_POINT('Ctrl Pts',(163.280101076064,-226.561458266673,12.2208646036422));
#84779=CARTESIAN_POINT('Ctrl Pts',(160.467314007601,-228.602614690202,12.0621067384104));
#84780=CARTESIAN_POINT('Ctrl Pts',(157.226841177757,-227.346658290928,11.9033488731786));
#84781=CARTESIAN_POINT('Ctrl Pts',(156.524363192979,-223.943040316076,11.7445910079468));
#84782=CARTESIAN_POINT('Ctrl Pts',(159.00278787731,-221.506751802388,11.585833142715));
#84783=CARTESIAN_POINT('Ctrl Pts',(162.393861057113,-222.267483901785,11.4270752774832));
#84784=CARTESIAN_POINT('Ctrl Pts',(163.594072691582,-225.529014626816,11.2683174122514));
#84785=CARTESIAN_POINT('Ctrl Pts',(161.504989140049,-228.306391186187,11.1095595470196));
#84786=CARTESIAN_POINT('Ctrl Pts',(158.038539586726,-228.057758661981,10.9508016817878));
#84787=CARTESIAN_POINT('Ctrl Pts',(156.367218526498,-225.010665530573,10.792043816556));
#84788=CARTESIAN_POINT('Ctrl Pts',(158.020618927964,-221.953811306005,10.6332859513243));
#84789=CARTESIAN_POINT('Ctrl Pts',(161.48554880872,-221.684828854392,10.4745280860924));
#84790=CARTESIAN_POINT('Ctrl Pts',(163.590904478153,-224.449890904874,10.3157702208607));
#84791=CARTESIAN_POINT('Ctrl Pts',(162.40986451039,-227.718412777583,10.1570123556289));
#84792=CARTESIAN_POINT('Ctrl Pts',(159.023316637483,-228.499043383147,9.99825449039708));
#84793=CARTESIAN_POINT('Ctrl Pts',(156.530629339545,-226.077349622051,9.83949662516528));
#84794=CARTESIAN_POINT('Ctrl Pts',(157.213109933626,-222.66966552922,9.6807387599335));
#84795=CARTESIAN_POINT('Ctrl Pts',(160.44615220686,-221.394703452409,9.52198089470169));
#84796=CARTESIAN_POINT('Ctrl Pts',(163.270875997921,-223.419308634178,9.36322302946991));
#84797=CARTESIAN_POINT('Ctrl Pts',(163.102094204308,-226.890562491788,9.20446516423811));
#84798=CARTESIAN_POINT('Ctrl Pts',(160.0942759169,-228.631573631259,9.04570729900633));
#84799=CARTESIAN_POINT('Ctrl Pts',(157.000176314052,-227.048968726209,8.88694943377452));
#84800=CARTESIAN_POINT('Ctrl Pts',(156.651515230618,-223.591147723507,8.72819156854274));
#84801=CARTESIAN_POINT('Ctrl Pts',(159.367387276447,-221.422708268849,8.56943370331094));
#84802=CARTESIAN_POINT('Ctrl Pts',(162.662226461995,-222.528206065867,8.41067583807915));
#84803=CARTESIAN_POINT('Ctrl Pts',(163.520596094214,-225.895889574202,8.25191797284736));
#84804=CARTESIAN_POINT('Ctrl Pts',(161.156916319453,-228.443654979458,8.09316010761556));
#84805=CARTESIAN_POINT('Ctrl Pts',(157.734426774623,-227.839787482932,7.93440224238378));
#84806=CARTESIAN_POINT('Ctrl Pts',(156.385389756567,-224.636946593699,7.77564437715197));
#84807=CARTESIAN_POINT('Ctrl Pts',(158.344443891159,-221.766372167636,7.6168865119202));
#84808=CARTESIAN_POINT('Ctrl Pts',(161.81866291146,-221.855213806593,7.45812864668839));
#84809=CARTESIAN_POINT('Ctrl Pts',(163.628441706709,-224.822163646091,7.29937078145661));
#84810=CARTESIAN_POINT('Ctrl Pts',(162.117470794664,-227.951869309693,7.14061291622481));
#84811=CARTESIAN_POINT('Ctrl Pts',(158.668590694609,-228.380024297143,6.98185505099302));
#84812=CARTESIAN_POINT('Ctrl Pts',(156.438216338492,-225.714781180764,6.82309718576122));
#84813=CARTESIAN_POINT('Ctrl Pts',(157.467586249323,-222.395370355858,6.66433932052943));
#84814=CARTESIAN_POINT('Ctrl Pts',(160.814621125189,-221.459716478846,6.50558145529765));
#84815=CARTESIAN_POINT('Ctrl Pts',(163.416114779316,-223.764129941176,6.34682359006585));
#84816=CARTESIAN_POINT('Ctrl Pts',(162.891180321749,-227.199611632742,6.18806572483406));
#84817=CARTESIAN_POINT('Ctrl Pts',(159.72023774741,-228.622008844521,6.02930785960227));
#84818=CARTESIAN_POINT('Ctrl Pts',(156.80533357564,-226.729543704226,5.87054999437047));
#84819=CARTESIAN_POINT('Ctrl Pts',(156.814187989818,-223.254200233836,5.71179212913868));
#84820=CARTESIAN_POINT('Ctrl Pts',(159.738697430435,-221.376612640788,5.55303426390689));
#84821=CARTESIAN_POINT('Ctrl Pts',(162.902350972443,-222.815149016404,5.39427639867509));
#84822=CARTESIAN_POINT('Ctrl Pts',(163.409773018603,-226.25326092629,5.23551853344331));
#84823=CARTESIAN_POINT('Ctrl Pts',(160.796570932224,-228.544388485719,5.07676066821151));
#84824=CARTESIAN_POINT('Ctrl Pts',(157.454347159998,-227.591691842397,4.91800280297972));
#84825=CARTESIAN_POINT('Ctrl Pts',(156.441904766836,-224.26707892683,4.75924493774792));
#84826=CARTESIAN_POINT('Ctrl Pts',(158.685830991148,-221.613235348605,4.60048707251613));
#84827=CARTESIAN_POINT('Ctrl Pts',(162.132484640682,-222.05895864616,4.44172920728435));
#84828=CARTESIAN_POINT('Ctrl Pts',(163.627488430923,-225.196322875086,4.28297134205254));
#84829=CARTESIAN_POINT('Ctrl Pts',(161.802614951828,-228.154012416474,4.12421347682076));
#84830=CARTESIAN_POINT('Ctrl Pts',(158.327988339714,-228.225149918293,3.96545561158896));
#84831=CARTESIAN_POINT('Ctrl Pts',(156.383586733325,-225.344630341799,3.80669774635717));
#84832=CARTESIAN_POINT('Ctrl Pts',(157.748926406423,-222.148705089872,3.64793988112538));
#84833=CARTESIAN_POINT('Ctrl Pts',(161.174448543763,-221.562284827925,3.48918201589358));
#84834=CARTESIAN_POINT('Ctrl Pts',(163.525115420198,-224.122061355537,3.33042415066179));
#84835=CARTESIAN_POINT('Ctrl Pts',(162.649596802351,-227.485327297572,3.17166628543));
#84836=CARTESIAN_POINT('Ctrl Pts',(159.349167295888,-228.574021791418,3.01290842019821));
#84837=CARTESIAN_POINT('Ctrl Pts',(156.644379853178,-226.39177168891,2.85415055496641));
#84838=CARTESIAN_POINT('Ctrl Pts',(157.010655839907,-222.935772177733,2.69539268973463));
#84839=CARTESIAN_POINT('Ctrl Pts',(160.112779478126,-221.368953916766,2.53663482450283));
#84840=CARTESIAN_POINT('Ctrl Pts',(163.111687355417,-223.125268829368,2.37787695927104));
#84841=CARTESIAN_POINT('Ctrl Pts',(163.262779060384,-226.597337758068,2.21911909403925));
#84842=CARTESIAN_POINT('Ctrl Pts',(160.427775553637,-228.607522979317,2.06036122880745));
#84843=CARTESIAN_POINT('Ctrl Pts',(157.201271760739,-227.316103838939,1.90160336357566));
#84844=CARTESIAN_POINT('Ctrl Pts',(156.536164183628,-223.904985462419,1.74284549834387));
#84845=CARTESIAN_POINT('Ctrl Pts',(159.041158508843,-221.496026617155,1.58408763311207));
#84846=CARTESIAN_POINT('Ctrl Pts',(162.423685567743,-222.293899365156,1.42532976788028));
#84847=CARTESIAN_POINT('Ctrl Pts',(163.588053535237,-225.568405078077,1.26657190264849));
#84848=CARTESIAN_POINT('Ctrl Pts',(161.468639519931,-228.322686213904,1.1078140374167));
#84849=CARTESIAN_POINT('Ctrl Pts',(158.005117395928,-228.036087118832,0.949056172184905));
#84850=CARTESIAN_POINT('Ctrl Pts',(156.367331002864,-224.970773940809,0.790298306953113));
#84851=CARTESIAN_POINT('Ctrl Pts',(158.054123192547,-221.932389526572,0.631540441721319));
#84852=CARTESIAN_POINT('Ctrl Pts',(161.52186463808,-221.701106398635,0.472782576489526));
#84853=CARTESIAN_POINT('Ctrl Pts',(163.596623766652,-224.489750196051,0.314024711257736));
#84854=CARTESIAN_POINT('Ctrl Pts',(162.380110634752,-227.743757872981,0.15526684602594));
#84855=CARTESIAN_POINT('Ctrl Pts',(158.984594590514,-228.490053105179,-0.00349101920584808));
#84856=CARTESIAN_POINT('Ctrl Pts',(156.520034264226,-226.035336592024,-0.162248884437644));
#84857=CARTESIAN_POINT('Ctrl Pts',(156.999831188384,-223.779443237332,-0.268087461258838));
#84858=CARTESIAN_POINT('Ctrl Pts',(157.663937342304,-223.002698443069,-0.321006749669435));
#84859=CARTESIAN_POINT('Ctrl Pts',(159.254067145653,-227.790177569842,20.1070022498898));
#84860=CARTESIAN_POINT('Ctrl Pts',(158.326328373192,-227.542153631111,20.0540829614792));
#84861=CARTESIAN_POINT('Ctrl Pts',(156.753991824467,-226.05055982535,19.948244384658));
#84862=CARTESIAN_POINT('Ctrl Pts',(157.355959284165,-222.837758975168,19.7894865194262));
#84863=CARTESIAN_POINT('Ctrl Pts',(160.382716585329,-221.608314425637,19.6307286541944));
#84864=CARTESIAN_POINT('Ctrl Pts',(163.056853377018,-223.480713328787,19.4719707889626));
#84865=CARTESIAN_POINT('Ctrl Pts',(162.934495616441,-226.744624953805,19.3132129237309));
#84866=CARTESIAN_POINT('Ctrl Pts',(160.125939507437,-228.411343615433,19.154455058499));
#84867=CARTESIAN_POINT('Ctrl Pts',(157.202387726272,-226.956247563464,18.9956971932673));
#84868=CARTESIAN_POINT('Ctrl Pts',(156.839083273915,-223.710674851695,18.8369393280355));
#84869=CARTESIAN_POINT('Ctrl Pts',(159.368711045569,-221.645149801924,18.6781814628037));
#84870=CARTESIAN_POINT('Ctrl Pts',(162.476064870033,-222.649955887244,18.5194235975719));
#84871=CARTESIAN_POINT('Ctrl Pts',(163.317338476092,-225.805535570802,18.3606657323401));
#84872=CARTESIAN_POINT('Ctrl Pts',(161.122577169746,-228.223882712554,18.2019078671083));
#84873=CARTESIAN_POINT('Ctrl Pts',(157.900436592647,-227.691735616307,18.0431500018765));
#84874=CARTESIAN_POINT('Ctrl Pts',(156.599814767689,-224.696110698794,17.8843921366447));
#84875=CARTESIAN_POINT('Ctrl Pts',(158.411043102702,-221.978605976434,17.7256342714129));
#84876=CARTESIAN_POINT('Ctrl Pts',(161.676484356976,-222.026280599272,17.5668764061811));
#84877=CARTESIAN_POINT('Ctrl Pts',(163.407607372316,-224.795503267648,17.4081185409493));
#84878=CARTESIAN_POINT('Ctrl Pts',(162.020088168414,-227.751881256977,17.2493606757175));
#84879=CARTESIAN_POINT('Ctrl Pts',(158.783784393714,-228.189737666912,17.0906028104858));
#84880=CARTESIAN_POINT('Ctrl Pts',(156.66056107406,-225.708346270834,16.9318449452539));
#84881=CARTESIAN_POINT('Ctrl Pts',(157.593592137746,-222.578676404551,16.7730870800222));
#84882=CARTESIAN_POINT('Ctrl Pts',(160.728967577691,-221.665001793266,16.6143292147904));
#84883=CARTESIAN_POINT('Ctrl Pts',(163.197191921438,-223.803517411731,16.4555713495586));
#84884=CARTESIAN_POINT('Ctrl Pts',(162.739346343332,-227.03705384692,16.2968134843268));
#84885=CARTESIAN_POINT('Ctrl Pts',(159.774451100051,-228.406278682,16.138055619095));
#84886=CARTESIAN_POINT('Ctrl Pts',(157.015978200883,-226.658077401028,15.9792977538632));
#84887=CARTESIAN_POINT('Ctrl Pts',(156.988481935044,-223.39240374795,15.8205398886314));
#84888=CARTESIAN_POINT('Ctrl Pts',(159.717126883769,-221.598002121477,15.6617820233996));
#84889=CARTESIAN_POINT('Ctrl Pts',(162.704657297373,-222.917108819674,15.5030241581678));
#84890=CARTESIAN_POINT('Ctrl Pts',(163.216885458766,-226.142477444185,15.344266292936));
#84891=CARTESIAN_POINT('Ctrl Pts',(160.785020174804,-228.322250756711,15.1855084277043));
#84892=CARTESIAN_POINT('Ctrl Pts',(157.634704457728,-227.461500307336,15.0267505624724));
#84893=CARTESIAN_POINT('Ctrl Pts',(156.649107127928,-224.347984873485,14.8679926972407));
#84894=CARTESIAN_POINT('Ctrl Pts',(158.730246822877,-221.83119365778,14.7092348320089));
#84895=CARTESIAN_POINT('Ctrl Pts',(161.973464575598,-222.214493881865,14.5504769667771));
#84896=CARTESIAN_POINT('Ctrl Pts',(163.410567626335,-225.147089195729,14.3917191015453));
#84897=CARTESIAN_POINT('Ctrl Pts',(161.726319319569,-227.945068483447,14.2329612363135));
#84898=CARTESIAN_POINT('Ctrl Pts',(158.462143639418,-228.047721210926,14.0742033710817));
#84899=CARTESIAN_POINT('Ctrl Pts',(156.605414039998,-225.361099606014,13.9154455058499));
#84900=CARTESIAN_POINT('Ctrl Pts',(157.855409377682,-222.343999655878,13.7566876406181));
#84901=CARTESIAN_POINT('Ctrl Pts',(161.068133968578,-221.757671116238,13.5979297753863));
#84902=CARTESIAN_POINT('Ctrl Pts',(163.303302393434,-224.138721843515,13.4391719101545));
#84903=CARTESIAN_POINT('Ctrl Pts',(162.515288597719,-227.308014305738,13.2804140449227));
#84904=CARTESIAN_POINT('Ctrl Pts',(159.425282776282,-228.36501216611,13.1216561796909));
#84905=CARTESIAN_POINT('Ctrl Pts',(156.861258135392,-226.342351024384,12.9628983144591));
#84906=CARTESIAN_POINT('Ctrl Pts',(157.169809925563,-223.091170277928,12.8041404492273));
#84907=CARTESIAN_POINT('Ctrl Pts',(160.068551560564,-221.586950418049,12.6453825839956));
#84908=CARTESIAN_POINT('Ctrl Pts',(162.904554810033,-223.206353401357,12.4866247187638));
#84909=CARTESIAN_POINT('Ctrl Pts',(163.082309611578,-226.467301681209,12.327866853532));
#84910=CARTESIAN_POINT('Ctrl Pts',(160.439134777816,-228.385375520119,12.1691089883002));
#84911=CARTESIAN_POINT('Ctrl Pts',(157.394063812665,-227.205153816143,12.0103511230684));
#84912=CARTESIAN_POINT('Ctrl Pts',(156.733945543687,-224.006775426348,11.8515932578366));
#84913=CARTESIAN_POINT('Ctrl Pts',(159.062920184692,-221.717396127302,11.6928353926048));
#84914=CARTESIAN_POINT('Ctrl Pts',(162.249510235817,-222.432255763464,11.534077527373));
#84915=CARTESIAN_POINT('Ctrl Pts',(163.377348607582,-225.49711482393,11.3753196621412));
#84916=CARTESIAN_POINT('Ctrl Pts',(161.414237666499,-228.107014417083,11.2165617969094));
#84917=CARTESIAN_POINT('Ctrl Pts',(158.15681646865,-227.873374537903,11.0578039316776));
#84918=CARTESIAN_POINT('Ctrl Pts',(156.586276766211,-225.010022394626,10.8990460664458));
#84919=CARTESIAN_POINT('Ctrl Pts',(158.139976433094,-222.137497756182,10.7402882012141));
#84920=CARTESIAN_POINT('Ctrl Pts',(161.395969595266,-221.884735058715,10.5815303359823));
#84921=CARTESIAN_POINT('Ctrl Pts',(163.374371438746,-224.483062713007,10.4227724707505));
#84922=CARTESIAN_POINT('Ctrl Pts',(162.264548674179,-227.554491352027,10.2640146055187));
#84923=CARTESIAN_POINT('Ctrl Pts',(159.082211052055,-228.288049606125,10.1052567402869));
#84924=CARTESIAN_POINT('Ctrl Pts',(156.739833838999,-226.012384989997,9.94649887505509));
#84925=CARTESIAN_POINT('Ctrl Pts',(157.381160568288,-222.810185670835,9.78774100982331));
#84926=CARTESIAN_POINT('Ctrl Pts',(160.419249042497,-221.612104339612,9.6289831445915));
#84927=CARTESIAN_POINT('Ctrl Pts',(163.073640809499,-223.514624983551,9.47022527935972));
#84928=CARTESIAN_POINT('Ctrl Pts',(162.915036628516,-226.776560784133,9.31146741412792));
#84929=CARTESIAN_POINT('Ctrl Pts',(160.088591039746,-228.412588224938,9.15270954889613));
#84930=CARTESIAN_POINT('Ctrl Pts',(157.181066934884,-226.925415056476,8.99395168366434));
#84931=CARTESIAN_POINT('Ctrl Pts',(156.853430260365,-223.676102104043,8.83519381843255));
#84932=CARTESIAN_POINT('Ctrl Pts',(159.405534087823,-221.638420453928,8.67643595320075));
#84933=CARTESIAN_POINT('Ctrl Pts',(162.501693094729,-222.677256272187,8.51767808796897));
#84934=CARTESIAN_POINT('Ctrl Pts',(163.308302679716,-225.841867058801,8.35892022273717));
#84935=CARTESIAN_POINT('Ctrl Pts',(161.087153782322,-228.236001146306,8.20016235750538));
#84936=CARTESIAN_POINT('Ctrl Pts',(157.871041786099,-227.668547111964,8.04140449227359));
#84937=CARTESIAN_POINT('Ctrl Pts',(156.603352263518,-224.658838865691,7.88264662704179));
#84938=CARTESIAN_POINT('Ctrl Pts',(158.444274615796,-221.961361276122,7.72388876181));
#84939=CARTESIAN_POINT('Ctrl Pts',(161.70899677852,-222.044845727154,7.56513089657821));
#84940=CARTESIAN_POINT('Ctrl Pts',(163.409645156747,-224.832887252487,7.40637303134642));
#84941=CARTESIAN_POINT('Ctrl Pts',(161.9897864216,-227.773870357772,7.24761516611462));
#84942=CARTESIAN_POINT('Ctrl Pts',(158.748875231651,-228.176207420704,7.08885730088284));
#84943=CARTESIAN_POINT('Ctrl Pts',(156.652993380496,-225.671679577109,6.93009943565103));
#84944=CARTESIAN_POINT('Ctrl Pts',(157.620291855893,-222.552430610957,6.77134157041925));
#84945=CARTESIAN_POINT('Ctrl Pts',(160.765499131197,-221.673197053409,6.61258370518745));
#84946=CARTESIAN_POINT('Ctrl Pts',(163.210121631732,-223.838653421758,6.45382583995566));
#84947=CARTESIAN_POINT('Ctrl Pts',(162.716840941141,-227.066974132844,6.29506797472387));
#84948=CARTESIAN_POINT('Ctrl Pts',(159.737107528055,-228.403600198834,6.13631010949207));
#84949=CARTESIAN_POINT('Ctrl Pts',(156.997973294955,-226.625251496694,5.97755224426028));
#84950=CARTESIAN_POINT('Ctrl Pts',(157.006293784261,-223.359472688691,5.81879437902849));
#84951=CARTESIAN_POINT('Ctrl Pts',(159.754454084486,-221.595104411486,5.6600365137967));
#84952=CARTESIAN_POINT('Ctrl Pts',(162.727337996934,-222.946896442995,5.5012786485649));
#84953=CARTESIAN_POINT('Ctrl Pts',(163.204162281838,-226.177688769139,5.34252078333312));
#84954=CARTESIAN_POINT('Ctrl Pts',(160.748537372404,-228.330660380078,5.18376291810132));
#84955=CARTESIAN_POINT('Ctrl Pts',(157.607851089182,-227.435411742145,5.02500505286953));
#84956=CARTESIAN_POINT('Ctrl Pts',(156.656459395071,-224.311274373572,4.86624718763773));
#84957=CARTESIAN_POINT('Ctrl Pts',(158.76507593111,-221.81745867122,4.70748932240594));
#84958=CARTESIAN_POINT('Ctrl Pts',(162.003894926434,-222.236304667822,4.54873145717415));
#84959=CARTESIAN_POINT('Ctrl Pts',(163.408749363889,-225.184484523744,4.38997359194236));
#84960=CARTESIAN_POINT('Ctrl Pts',(161.693916517555,-227.963824150809,4.23121572671057));
#84961=CARTESIAN_POINT('Ctrl Pts',(158.428811340974,-228.030672031565,4.07245786147877));
#84962=CARTESIAN_POINT('Ctrl Pts',(156.601657963332,-225.323848988289,3.91369999624698));
#84963=CARTESIAN_POINT('Ctrl Pts',(157.884667084047,-222.320639363504,3.75494213101519));
#84964=CARTESIAN_POINT('Ctrl Pts',(161.103628806185,-221.769580488212,3.5961842657834));
#84965=CARTESIAN_POINT('Ctrl Pts',(163.312549488455,-224.17500142238,3.4374264005516));
#84966=CARTESIAN_POINT('Ctrl Pts',(162.489825008836,-227.335461023785,3.27866853531981));
#84967=CARTESIAN_POINT('Ctrl Pts',(159.3884127797,-228.35850678507,3.11991067008802));
#84968=CARTESIAN_POINT('Ctrl Pts',(156.846725149163,-226.307847274938,2.96115280485623));
#84969=CARTESIAN_POINT('Ctrl Pts',(157.190914540955,-223.060245977329,2.80239493962443));
#84970=CARTESIAN_POINT('Ctrl Pts',(160.105978828504,-221.58790751172,2.64363707439264));
#84971=CARTESIAN_POINT('Ctrl Pts',(162.924051308607,-223.238315901747,2.48487920916085));
#84972=CARTESIAN_POINT('Ctrl Pts',(163.066032120677,-226.501017624291,2.32612134392906));
#84973=CARTESIAN_POINT('Ctrl Pts',(160.401980509136,-228.38998783735,2.16736347869726));
#84974=CARTESIAN_POINT('Ctrl Pts',(157.37003624217,-227.176441810367,2.00860561346547));
#84975=CARTESIAN_POINT('Ctrl Pts',(156.745034929673,-223.971015296256,1.84984774823368));
#84976=CARTESIAN_POINT('Ctrl Pts',(159.098977051121,-221.707317675217,1.69108988300188));
#84977=CARTESIAN_POINT('Ctrl Pts',(162.277536316003,-222.457078363364,1.53233201777009));
#84978=CARTESIAN_POINT('Ctrl Pts',(163.371692408878,-225.534130014532,1.3735741525383));
#84979=CARTESIAN_POINT('Ctrl Pts',(161.380079943652,-228.122326847825,1.21481628730651));
#84980=CARTESIAN_POINT('Ctrl Pts',(158.125409649912,-227.853009797855,1.05605842207471));
#84981=CARTESIAN_POINT('Ctrl Pts',(156.586382460205,-224.972536284381,0.897300556842924));
#84982=CARTESIAN_POINT('Ctrl Pts',(158.171460376533,-222.117367718994,0.738542691611129));
#84983=CARTESIAN_POINT('Ctrl Pts',(161.430095564953,-221.900031060243,0.579784826379336));
#84984=CARTESIAN_POINT('Ctrl Pts',(163.37974585176,-224.520518472282,0.421026961147546));
#84985=CARTESIAN_POINT('Ctrl Pts',(162.236588969666,-227.57830812759,0.26226909591575));
#84986=CARTESIAN_POINT('Ctrl Pts',(159.045823960686,-228.279601445673,0.103511230683962));
#84987=CARTESIAN_POINT('Ctrl Pts',(156.729877651146,-225.972905363223,-0.0552466345478339));
#84988=CARTESIAN_POINT('Ctrl Pts',(157.180742620438,-223.853043319762,-0.161085211369028));
#84989=CARTESIAN_POINT('Ctrl Pts',(157.804802895981,-223.123136560921,-0.214004499779625));
#84990=CARTESIAN_POINT('Ctrl Pts',(159.301933573839,-227.611132185939,20.2140044997796));
#84991=CARTESIAN_POINT('Ctrl Pts',(158.43372769508,-227.379023915733,20.161085211369));
#84992=CARTESIAN_POINT('Ctrl Pts',(156.96228780757,-225.983145518363,20.0552466345478));
#84993=CARTESIAN_POINT('Ctrl Pts',(157.525627082423,-222.976509740914,19.896488769316));
#84994=CARTESIAN_POINT('Ctrl Pts',(160.358157704673,-221.825958511198,19.7377309040842));
#84995=CARTESIAN_POINT('Ctrl Pts',(162.860695436269,-223.57820578527,19.5789730388524));
#84996=CARTESIAN_POINT('Ctrl Pts',(162.746189359561,-226.632672564826,19.4202151736207));
#84997=CARTESIAN_POINT('Ctrl Pts',(160.117857983271,-228.192438075565,19.2614573083889));
#84998=CARTESIAN_POINT('Ctrl Pts',(157.381910194295,-226.830715375192,19.1026994431571));
#84999=CARTESIAN_POINT('Ctrl Pts',(157.041918948184,-223.793410702864,18.9439415779253));
#85000=CARTESIAN_POINT('Ctrl Pts',(159.409220787465,-221.860430165491,18.7851837126935));
#85001=CARTESIAN_POINT('Ctrl Pts',(162.317176063092,-222.800757956226,18.6264258474617));
#85002=CARTESIAN_POINT('Ctrl Pts',(163.104465235546,-225.75384444294,18.4676679822299));
#85003=CARTESIAN_POINT('Ctrl Pts',(161.050541517789,-228.017006517946,18.3089101169981));
#85004=CARTESIAN_POINT('Ctrl Pts',(158.03516534266,-227.519007241598,18.1501522517663));
#85005=CARTESIAN_POINT('Ctrl Pts',(156.818004275354,-224.715611241407,17.9913943865345));
#85006=CARTESIAN_POINT('Ctrl Pts',(158.513006289833,-222.172488494422,17.8326365213027));
#85007=CARTESIAN_POINT('Ctrl Pts',(161.568904542505,-222.217103842021,17.673878656071));
#85008=CARTESIAN_POINT('Ctrl Pts',(163.188941586754,-224.808625800187,17.5151207908391));
#85009=CARTESIAN_POINT('Ctrl Pts',(161.890459335632,-227.575293343204,17.3563629256074));
#85010=CARTESIAN_POINT('Ctrl Pts',(158.861828813714,-227.98505255608,17.1976050603756));
#85011=CARTESIAN_POINT('Ctrl Pts',(156.874852498011,-225.662891769525,17.0388471951438));
#85012=CARTESIAN_POINT('Ctrl Pts',(157.748011062256,-222.734052469999,16.880089329912));
#85013=CARTESIAN_POINT('Ctrl Pts',(160.682189809418,-221.87900825676,16.7213314646802));
#85014=CARTESIAN_POINT('Ctrl Pts',(162.992028471923,-223.880295566163,16.5625735994484));
#85015=CARTESIAN_POINT('Ctrl Pts',(162.563562793573,-226.906336328438,16.4038157342166));
#85016=CARTESIAN_POINT('Ctrl Pts',(159.788924547841,-228.187698158347,16.2450578689848));
#85017=CARTESIAN_POINT('Ctrl Pts',(157.20746254739,-226.55167875887,16.086300003753));
#85018=CARTESIAN_POINT('Ctrl Pts',(157.181730713867,-223.4955630204,15.9275421385212));
#85019=CARTESIAN_POINT('Ctrl Pts',(159.735278820133,-221.816307946447,15.7687842732894));
#85020=CARTESIAN_POINT('Ctrl Pts',(162.531099739829,-223.050767714736,15.6100264080576));
#85021=CARTESIAN_POINT('Ctrl Pts',(163.010458277155,-226.069164793834,15.4512685428258));
#85022=CARTESIAN_POINT('Ctrl Pts',(160.734645517617,-228.109062295665,15.2925106775941));
#85023=CARTESIAN_POINT('Ctrl Pts',(157.786485209243,-227.303546106762,15.1337528123623));
#85024=CARTESIAN_POINT('Ctrl Pts',(156.864133550327,-224.389824611536,14.9749949471305));
#85025=CARTESIAN_POINT('Ctrl Pts',(158.811726742836,-222.034535607837,14.8162370818987));
#85026=CARTESIAN_POINT('Ctrl Pts',(161.846827573574,-222.393239499232,14.6574792166669));
#85027=CARTESIAN_POINT('Ctrl Pts',(163.191711881602,-225.137650498421,14.4987213514351));
#85028=CARTESIAN_POINT('Ctrl Pts',(161.615541601099,-227.756083766868,14.3399634862033));
#85029=CARTESIAN_POINT('Ctrl Pts',(158.5608277108,-227.852149280258,14.1812056209715));
#85030=CARTESIAN_POINT('Ctrl Pts',(156.823244242982,-225.337927884513,14.0224477557397));
#85031=CARTESIAN_POINT('Ctrl Pts',(157.993027519065,-222.514434902151,13.8636898905079));
#85032=CARTESIAN_POINT('Ctrl Pts',(160.999591930777,-221.965730999598,13.7049320252761));
#85033=CARTESIAN_POINT('Ctrl Pts',(163.09132984675,-224.193989966893,13.5461741600443));
#85034=CARTESIAN_POINT('Ctrl Pts',(162.353882808541,-227.159909284792,13.3874162948125));
#85035=CARTESIAN_POINT('Ctrl Pts',(159.46216231652,-228.149079710186,13.2286584295808));
#85036=CARTESIAN_POINT('Ctrl Pts',(157.06267085127,-226.256212508652,13.069900564349));
#85037=CARTESIAN_POINT('Ctrl Pts',(157.35142290743,-223.2136596686,12.9111426991172));
#85038=CARTESIAN_POINT('Ctrl Pts',(160.064152614558,-221.805965429598,12.7523848338854));
#85039=CARTESIAN_POINT('Ctrl Pts',(162.718169851365,-223.321451503826,12.5936269686536));
#85040=CARTESIAN_POINT('Ctrl Pts',(162.884518147092,-226.373145095745,12.4348691034218));
#85041=CARTESIAN_POINT('Ctrl Pts',(160.410955548032,-228.168136350036,12.27611123819));
#85042=CARTESIAN_POINT('Ctrl Pts',(157.561286447573,-227.063649341357,12.1173533729582));
#85043=CARTESIAN_POINT('Ctrl Pts',(156.943527894395,-224.07051053662,11.9585955077264));
#85044=CARTESIAN_POINT('Ctrl Pts',(159.123052492074,-221.928040452216,11.7998376424946));
#85045=CARTESIAN_POINT('Ctrl Pts',(162.105159414521,-222.597027625143,11.6410797772628));
#85046=CARTESIAN_POINT('Ctrl Pts',(163.160624523583,-225.465215021044,11.482321912031));
#85047=CARTESIAN_POINT('Ctrl Pts',(161.323486192949,-227.90763764798,11.3235640467992));
#85048=CARTESIAN_POINT('Ctrl Pts',(158.275093350574,-227.688990413825,11.1648061815675));
#85049=CARTESIAN_POINT('Ctrl Pts',(156.805335005923,-225.009379258679,11.0060483163357));
#85050=CARTESIAN_POINT('Ctrl Pts',(158.259333938224,-222.32118420636,10.8472904511039));
#85051=CARTESIAN_POINT('Ctrl Pts',(161.306390381813,-222.084641263038,10.6885325858721));
#85052=CARTESIAN_POINT('Ctrl Pts',(163.157838399339,-224.51623452114,10.5297747206403));
#85053=CARTESIAN_POINT('Ctrl Pts',(162.119232837969,-227.390569926471,10.3710168554085));
#85054=CARTESIAN_POINT('Ctrl Pts',(159.141105466627,-228.077055829103,10.2122589901767));
#85055=CARTESIAN_POINT('Ctrl Pts',(156.949038338452,-225.947420357942,10.0535011249449));
#85056=CARTESIAN_POINT('Ctrl Pts',(157.54921120295,-222.950705812449,9.89474325971312));
#85057=CARTESIAN_POINT('Ctrl Pts',(160.392345878133,-221.829505226816,9.73598539448132));
#85058=CARTESIAN_POINT('Ctrl Pts',(162.876405621077,-223.609941332924,9.57722752924953));
#85059=CARTESIAN_POINT('Ctrl Pts',(162.727979052723,-226.662559076478,9.41846966401773));
#85060=CARTESIAN_POINT('Ctrl Pts',(160.082906162592,-228.193602818617,9.25971179878594));
#85061=CARTESIAN_POINT('Ctrl Pts',(157.361957555717,-226.801861386744,9.10095393355414));
#85062=CARTESIAN_POINT('Ctrl Pts',(157.055345290111,-223.761056484579,8.94219606832236));
#85063=CARTESIAN_POINT('Ctrl Pts',(159.4436808992,-221.854132639007,8.78343820309056));
#85064=CARTESIAN_POINT('Ctrl Pts',(162.341159727464,-222.826306478508,8.62468033785878));
#85065=CARTESIAN_POINT('Ctrl Pts',(163.096009265217,-225.7878445434,8.46592247262697));
#85066=CARTESIAN_POINT('Ctrl Pts',(161.017391245191,-228.028347313154,8.30716460739519));
#85067=CARTESIAN_POINT('Ctrl Pts',(158.007656797574,-227.497306740996,8.1484067421634));
#85068=CARTESIAN_POINT('Ctrl Pts',(156.82131477047,-224.680731137683,7.9896488769316));
#85069=CARTESIAN_POINT('Ctrl Pts',(158.544105340433,-222.156350384608,7.83089101169981));
#85070=CARTESIAN_POINT('Ctrl Pts',(161.59933064558,-222.234477647715,7.67213314646802));
#85071=CARTESIAN_POINT('Ctrl Pts',(163.190848606784,-224.843610858883,7.51337528123622));
#85072=CARTESIAN_POINT('Ctrl Pts',(161.862102048537,-227.595871405851,7.35461741600443));
#85073=CARTESIAN_POINT('Ctrl Pts',(158.829159768693,-227.972390544264,7.19585955077264));
#85074=CARTESIAN_POINT('Ctrl Pts',(156.8677704225,-225.628577973453,7.03710168554085));
#85075=CARTESIAN_POINT('Ctrl Pts',(157.772997462463,-222.709490866057,6.87834382030905));
#85076=CARTESIAN_POINT('Ctrl Pts',(160.716377137205,-221.886677627973,6.71958595507726));
#85077=CARTESIAN_POINT('Ctrl Pts',(163.004128484148,-223.91317690234,6.56082808984547));
#85078=CARTESIAN_POINT('Ctrl Pts',(162.542501560533,-226.934336632947,6.40207022461368));
#85079=CARTESIAN_POINT('Ctrl Pts',(159.7539773087,-228.185191553147,6.24331235938189));
#85080=CARTESIAN_POINT('Ctrl Pts',(157.19061301427,-226.520959289162,6.08455449415009));
#85081=CARTESIAN_POINT('Ctrl Pts',(157.198399578703,-223.464745143546,5.9257966289183));
#85082=CARTESIAN_POINT('Ctrl Pts',(159.770210738537,-221.813596182184,5.76703876368651));
#85083=CARTESIAN_POINT('Ctrl Pts',(162.552325021425,-223.078643869585,5.60828089845471));
#85084=CARTESIAN_POINT('Ctrl Pts',(162.998551545073,-226.102116611987,5.44952303322292));
#85085=CARTESIAN_POINT('Ctrl Pts',(160.700503812585,-228.116932274438,5.29076516799113));
#85086=CARTESIAN_POINT('Ctrl Pts',(157.761355018366,-227.279131641893,5.13200730275934));
#85087=CARTESIAN_POINT('Ctrl Pts',(156.871014023306,-224.355469820314,4.97324943752755));
#85088=CARTESIAN_POINT('Ctrl Pts',(158.844320871072,-222.021681993836,4.81449157229575));
#85089=CARTESIAN_POINT('Ctrl Pts',(161.875305212187,-222.413650689484,4.65573370706397));
#85090=CARTESIAN_POINT('Ctrl Pts',(163.190010296854,-225.172646172402,4.49697584183216));
#85091=CARTESIAN_POINT('Ctrl Pts',(161.585218083281,-227.773635885145,4.33821797660038));
#85092=CARTESIAN_POINT('Ctrl Pts',(158.529634342234,-227.836194144838,4.17946011136858));
#85093=CARTESIAN_POINT('Ctrl Pts',(156.819729193338,-225.303067634779,4.02070224613679));
#85094=CARTESIAN_POINT('Ctrl Pts',(158.020407761671,-222.492573637137,3.861944380905));
#85095=CARTESIAN_POINT('Ctrl Pts',(161.032809068608,-221.976876148499,3.70318651567321));
#85096=CARTESIAN_POINT('Ctrl Pts',(163.099983556713,-224.227941489222,3.54442865044141));
#85097=CARTESIAN_POINT('Ctrl Pts',(162.33005321532,-227.185594749999,3.38567078520962));
#85098=CARTESIAN_POINT('Ctrl Pts',(159.427658263512,-228.142991778722,3.22691291997783));
#85099=CARTESIAN_POINT('Ctrl Pts',(157.049070445148,-226.223922860965,3.06815505474604));
#85100=CARTESIAN_POINT('Ctrl Pts',(157.371173242002,-223.184719776926,2.90939718951424));
#85101=CARTESIAN_POINT('Ctrl Pts',(160.099178178882,-221.806861106675,2.75063932428245));
#85102=CARTESIAN_POINT('Ctrl Pts',(162.736415261797,-223.351362974126,2.59188145905066));
#85103=CARTESIAN_POINT('Ctrl Pts',(162.869285180969,-226.404697490515,2.43312359381887));
#85104=CARTESIAN_POINT('Ctrl Pts',(160.376185464635,-228.172452695384,2.27436572858707));
#85105=CARTESIAN_POINT('Ctrl Pts',(157.5388007236,-227.036779781794,2.11560786335528));
#85106=CARTESIAN_POINT('Ctrl Pts',(156.953905675717,-224.037045130094,1.95684999812349));
#85107=CARTESIAN_POINT('Ctrl Pts',(159.156795593401,-221.918608733279,1.79809213289169));
#85108=CARTESIAN_POINT('Ctrl Pts',(162.131387064264,-222.620257361572,1.6393342676599));
#85109=CARTESIAN_POINT('Ctrl Pts',(163.155331282519,-225.499854950988,1.48057640242811));
#85110=CARTESIAN_POINT('Ctrl Pts',(161.291520367372,-227.921967481746,1.32181853719632));
#85111=CARTESIAN_POINT('Ctrl Pts',(158.245701903897,-227.669932476878,1.16306067196452));
#85112=CARTESIAN_POINT('Ctrl Pts',(156.805433917545,-224.974298627954,1.00430280673273));
#85113=CARTESIAN_POINT('Ctrl Pts',(158.28879756052,-222.302345911416,0.845544941500939));
#85114=CARTESIAN_POINT('Ctrl Pts',(161.338326491825,-222.098955721852,0.686787076269146));
#85115=CARTESIAN_POINT('Ctrl Pts',(163.162867936868,-224.551286748514,0.528029211037356));
#85116=CARTESIAN_POINT('Ctrl Pts',(162.093067304581,-227.412858382199,0.36927134580556));
#85117=CARTESIAN_POINT('Ctrl Pts',(159.107053330859,-228.069149786166,0.210513480573772));
#85118=CARTESIAN_POINT('Ctrl Pts',(156.939721038065,-225.910474134421,0.0517556153419763));
#85119=CARTESIAN_POINT('Ctrl Pts',(157.361654052493,-223.926643402192,-0.0540829614792177));
#85120=CARTESIAN_POINT('Ctrl Pts',(157.945668449658,-223.243574678773,-0.107002249889815));
#85121=CARTESIAN_POINT('Ctrl Pts',(159.349800002025,-227.432086802035,20.3210067496694));
#85122=CARTESIAN_POINT('Ctrl Pts',(158.541127016969,-227.215894200354,20.2680874612588));
#85123=CARTESIAN_POINT('Ctrl Pts',(157.170583790673,-225.915731211375,20.1622488844376));
#85124=CARTESIAN_POINT('Ctrl Pts',(157.695294880681,-223.11526050666,20.0034910192058));
#85125=CARTESIAN_POINT('Ctrl Pts',(160.333598824017,-222.043602596759,19.8447331539741));
#85126=CARTESIAN_POINT('Ctrl Pts',(162.664537495519,-223.675698241753,19.6859752887422));
#85127=CARTESIAN_POINT('Ctrl Pts',(162.55788310268,-226.520720175846,19.5272174235105));
#85128=CARTESIAN_POINT('Ctrl Pts',(160.109776459105,-227.973532535698,19.3684595582787));
#85129=CARTESIAN_POINT('Ctrl Pts',(157.561432662319,-226.705183186919,19.2097016930469));
#85130=CARTESIAN_POINT('Ctrl Pts',(157.244754622453,-223.876146554034,19.0509438278151));
#85131=CARTESIAN_POINT('Ctrl Pts',(159.449730529362,-222.075710529059,18.8921859625833));
#85132=CARTESIAN_POINT('Ctrl Pts',(162.158287256151,-222.951560025208,18.7334280973515));
#85133=CARTESIAN_POINT('Ctrl Pts',(162.891591995001,-225.702153315077,18.5746702321197));
#85134=CARTESIAN_POINT('Ctrl Pts',(160.978505865832,-227.810130323338,18.4159123668879));
#85135=CARTESIAN_POINT('Ctrl Pts',(158.169894092673,-227.346278866889,18.2571545016561));
#85136=CARTESIAN_POINT('Ctrl Pts',(157.03619378302,-224.73511178402,18.0983966364243));
#85137=CARTESIAN_POINT('Ctrl Pts',(158.614969476964,-222.366371012409,17.9396387711925));
#85138=CARTESIAN_POINT('Ctrl Pts',(161.461324728035,-222.407927084771,17.7808809059608));
#85139=CARTESIAN_POINT('Ctrl Pts',(162.970275801191,-224.821748332727,17.622123040729));
#85140=CARTESIAN_POINT('Ctrl Pts',(161.76083050285,-227.398705429432,17.4633651754972));
#85141=CARTESIAN_POINT('Ctrl Pts',(158.939873233715,-227.780367445248,17.3046073102654));
#85142=CARTESIAN_POINT('Ctrl Pts',(157.089143921962,-225.617437268217,17.1458494450336));
#85143=CARTESIAN_POINT('Ctrl Pts',(157.902429986765,-222.889428535446,16.9870915798018));
#85144=CARTESIAN_POINT('Ctrl Pts',(160.635412041146,-222.093014720254,16.82833371457));
#85145=CARTESIAN_POINT('Ctrl Pts',(162.786865022409,-223.957073720595,16.6695758493382));
#85146=CARTESIAN_POINT('Ctrl Pts',(162.387779243813,-226.775618809956,16.5108179841064));
#85147=CARTESIAN_POINT('Ctrl Pts',(159.80339799563,-227.969117634694,16.3520601188746));
#85148=CARTESIAN_POINT('Ctrl Pts',(157.398946893897,-226.445280116713,16.1933022536428));
#85149=CARTESIAN_POINT('Ctrl Pts',(157.37497949269,-223.598722292849,16.034544388411));
#85150=CARTESIAN_POINT('Ctrl Pts',(159.753430756497,-222.034613771418,15.8757865231792));
#85151=CARTESIAN_POINT('Ctrl Pts',(162.357542182285,-223.184426609798,15.7170286579475));
#85152=CARTESIAN_POINT('Ctrl Pts',(162.804031095543,-225.995852143483,15.5582707927156));
#85153=CARTESIAN_POINT('Ctrl Pts',(160.684270860431,-227.89587383462,15.3995129274839));
#85154=CARTESIAN_POINT('Ctrl Pts',(157.938265960758,-227.145591906187,15.2407550622521));
#85155=CARTESIAN_POINT('Ctrl Pts',(157.079159972725,-224.431664349587,15.0819971970203));
#85156=CARTESIAN_POINT('Ctrl Pts',(158.893206662794,-222.237877557895,14.9232393317885));
#85157=CARTESIAN_POINT('Ctrl Pts',(161.720190571551,-222.5719851166,14.7644814665567));
#85158=CARTESIAN_POINT('Ctrl Pts',(162.972856136869,-225.128211801113,14.6057236013249));
#85159=CARTESIAN_POINT('Ctrl Pts',(161.504763882629,-227.567099050289,14.4469657360931));
#85160=CARTESIAN_POINT('Ctrl Pts',(158.659511782181,-227.65657734959,14.2882078708613));
#85161=CARTESIAN_POINT('Ctrl Pts',(157.041074445967,-225.314756163012,14.1294500056295));
#85162=CARTESIAN_POINT('Ctrl Pts',(158.130645660447,-222.684870148424,13.9706921403977));
#85163=CARTESIAN_POINT('Ctrl Pts',(160.931049892975,-222.173790882957,13.8119342751659));
#85164=CARTESIAN_POINT('Ctrl Pts',(162.879357300065,-224.24925809027,13.6531764099341));
#85165=CARTESIAN_POINT('Ctrl Pts',(162.192477019363,-227.011804263845,13.4944185447023));
#85166=CARTESIAN_POINT('Ctrl Pts',(159.499041856757,-227.933147254261,13.3356606794706));
#85167=CARTESIAN_POINT('Ctrl Pts',(157.264083567147,-226.170073992921,13.1769028142388));
#85168=CARTESIAN_POINT('Ctrl Pts',(157.533035889297,-223.336149059271,13.018144949007));
#85169=CARTESIAN_POINT('Ctrl Pts',(160.059753668551,-222.024980441147,12.8593870837752));
#85170=CARTESIAN_POINT('Ctrl Pts',(162.531784892697,-223.436549606296,12.7006292185434));
#85171=CARTESIAN_POINT('Ctrl Pts',(162.686726682607,-226.278988510281,12.5418713533116));
#85172=CARTESIAN_POINT('Ctrl Pts',(160.382776318248,-227.950897179953,12.3831134880798));
#85173=CARTESIAN_POINT('Ctrl Pts',(157.728509082481,-226.922144866572,12.224355622848));
#85174=CARTESIAN_POINT('Ctrl Pts',(157.153110245103,-224.134245646892,12.0655977576162));
#85175=CARTESIAN_POINT('Ctrl Pts',(159.183184799456,-222.138684777131,11.9068398923844));
#85176=CARTESIAN_POINT('Ctrl Pts',(161.960808593226,-222.761799486821,11.7480820271526));
#85177=CARTESIAN_POINT('Ctrl Pts',(162.943900439583,-225.433315218158,11.5893241619209));
#85178=CARTESIAN_POINT('Ctrl Pts',(161.232734719399,-227.708260878876,11.4305662966891));
#85179=CARTESIAN_POINT('Ctrl Pts',(158.393370232498,-227.504606289747,11.2718084314573));
#85180=CARTESIAN_POINT('Ctrl Pts',(157.024393245635,-225.008736122732,11.1130505662255));
#85181=CARTESIAN_POINT('Ctrl Pts',(158.378691443354,-222.504870656537,10.9542927009937));
#85182=CARTESIAN_POINT('Ctrl Pts',(161.216811168359,-222.28454746736,10.7955348357619));
#85183=CARTESIAN_POINT('Ctrl Pts',(162.941305359932,-224.549406329273,10.6367769705301));
#85184=CARTESIAN_POINT('Ctrl Pts',(161.973917001759,-227.226648500916,10.4780191052983));
#85185=CARTESIAN_POINT('Ctrl Pts',(159.199999881199,-227.866062052082,10.3192612400665));
#85186=CARTESIAN_POINT('Ctrl Pts',(157.158242837906,-225.882455725887,10.1605033748347));
#85187=CARTESIAN_POINT('Ctrl Pts',(157.717261837613,-223.091225954063,10.0017455096029));
#85188=CARTESIAN_POINT('Ctrl Pts',(160.36544271377,-222.046906114019,9.84298764437113));
#85189=CARTESIAN_POINT('Ctrl Pts',(162.679170432655,-223.705257682298,9.68422977913934));
#85190=CARTESIAN_POINT('Ctrl Pts',(162.540921476931,-226.548557368823,9.52547191390755));
#85191=CARTESIAN_POINT('Ctrl Pts',(160.077221285438,-227.974617412297,9.36671404867575));
#85192=CARTESIAN_POINT('Ctrl Pts',(157.54284817655,-226.678307717011,9.20795618344396));
#85193=CARTESIAN_POINT('Ctrl Pts',(157.257260319857,-223.846010865114,9.04919831821217));
#85194=CARTESIAN_POINT('Ctrl Pts',(159.481827710576,-222.069844824086,8.89044045298037));
#85195=CARTESIAN_POINT('Ctrl Pts',(162.180626360199,-222.975356684828,8.73168258774859));
#85196=CARTESIAN_POINT('Ctrl Pts',(162.883715850719,-225.733822027999,8.57292472251678));
#85197=CARTESIAN_POINT('Ctrl Pts',(160.94762870806,-227.820693480001,8.414166857285));
#85198=CARTESIAN_POINT('Ctrl Pts',(158.144271809049,-227.326066370028,8.2554089920532));
#85199=CARTESIAN_POINT('Ctrl Pts',(157.039277277422,-224.702623409675,8.09665112682141));
#85200=CARTESIAN_POINT('Ctrl Pts',(158.64393606507,-222.351339493094,7.93789326158962));
#85201=CARTESIAN_POINT('Ctrl Pts',(161.48966451264,-222.424109568277,7.77913539635783));
#85202=CARTESIAN_POINT('Ctrl Pts',(162.972052056822,-224.854334465279,7.62037753112604));
#85203=CARTESIAN_POINT('Ctrl Pts',(161.734417675473,-227.417872453929,7.46161966589424));
#85204=CARTESIAN_POINT('Ctrl Pts',(158.909444305736,-227.768573667824,7.30286180066245));
#85205=CARTESIAN_POINT('Ctrl Pts',(157.082547464504,-225.585476369798,7.14410393543066));
#85206=CARTESIAN_POINT('Ctrl Pts',(157.925703069032,-222.866551121156,6.98534607019886));
#85207=CARTESIAN_POINT('Ctrl Pts',(160.667255143213,-222.100158202536,6.82658820496708));
#85208=CARTESIAN_POINT('Ctrl Pts',(162.798135336563,-223.987700382922,6.66783033973528));
#85209=CARTESIAN_POINT('Ctrl Pts',(162.368162179926,-226.80169913305,6.50907247450349));
#85210=CARTESIAN_POINT('Ctrl Pts',(159.770847089346,-227.966782907461,6.3503146092717));
#85211=CARTESIAN_POINT('Ctrl Pts',(157.383252733585,-226.41666708163,6.19155674403991));
#85212=CARTESIAN_POINT('Ctrl Pts',(157.390505373146,-223.5700175984,6.03279887880811));
#85213=CARTESIAN_POINT('Ctrl Pts',(159.785967392588,-222.032087952882,5.87404101357632));
#85214=CARTESIAN_POINT('Ctrl Pts',(162.377312045917,-223.210391296176,5.71528314834452));
#85215=CARTESIAN_POINT('Ctrl Pts',(162.792940808308,-226.026544454835,5.55652528311274));
#85216=CARTESIAN_POINT('Ctrl Pts',(160.652470252765,-227.903204168797,5.39776741788094));
#85217=CARTESIAN_POINT('Ctrl Pts',(157.91485894755,-227.122851541641,5.23900955264915));
#85218=CARTESIAN_POINT('Ctrl Pts',(157.085568651541,-224.399665267055,5.08025168741735));
#85219=CARTESIAN_POINT('Ctrl Pts',(158.923565811034,-222.225905316451,4.92149382218556));
#85220=CARTESIAN_POINT('Ctrl Pts',(161.746715497939,-222.590996711146,4.76273595695377));
#85221=CARTESIAN_POINT('Ctrl Pts',(162.971271229819,-225.16080782106,4.60397809172198));
#85222=CARTESIAN_POINT('Ctrl Pts',(161.476519649008,-227.58344761948,4.44522022649019));
#85223=CARTESIAN_POINT('Ctrl Pts',(158.630457343494,-227.64171625811,4.28646236125839));
#85224=CARTESIAN_POINT('Ctrl Pts',(157.037800423344,-225.282286281269,4.1277044960266));
#85225=CARTESIAN_POINT('Ctrl Pts',(158.156148439294,-222.66450791077,3.96894663079481));
#85226=CARTESIAN_POINT('Ctrl Pts',(160.961989331031,-222.184171808785,3.81018876556301));
#85227=CARTESIAN_POINT('Ctrl Pts',(162.887417624971,-224.280881556065,3.65143090033122));
#85228=CARTESIAN_POINT('Ctrl Pts',(162.170281421805,-227.035728476212,3.49267303509943));
#85229=CARTESIAN_POINT('Ctrl Pts',(159.466903747323,-227.927476772375,3.33391516986764));
#85230=CARTESIAN_POINT('Ctrl Pts',(157.251415741134,-226.139998446992,3.17515730463585));
#85231=CARTESIAN_POINT('Ctrl Pts',(157.55143194305,-223.309193576523,3.01639943940405));
#85232=CARTESIAN_POINT('Ctrl Pts',(160.09237752926,-222.025814701629,2.85764157417226));
#85233=CARTESIAN_POINT('Ctrl Pts',(162.548779214987,-223.464410046505,2.69888370894047));
#85234=CARTESIAN_POINT('Ctrl Pts',(162.672538241262,-226.308377356738,2.54012584370868));
#85235=CARTESIAN_POINT('Ctrl Pts',(160.350390420134,-227.954917553418,2.38136797847688));
#85236=CARTESIAN_POINT('Ctrl Pts',(157.70756520503,-226.897117753222,2.22261011324509));
#85237=CARTESIAN_POINT('Ctrl Pts',(157.162776421762,-224.103074963931,2.0638522480133));
#85238=CARTESIAN_POINT('Ctrl Pts',(159.214614135679,-222.129899791342,1.90509438278151));
#85239=CARTESIAN_POINT('Ctrl Pts',(161.985237812524,-222.783436359779,1.74633651754971));
#85240=CARTESIAN_POINT('Ctrl Pts',(162.93897015616,-225.465579887444,1.58757865231792));
#85241=CARTESIAN_POINT('Ctrl Pts',(161.202960791094,-227.721608115667,1.42882078708613));
#85242=CARTESIAN_POINT('Ctrl Pts',(158.365994157881,-227.4868551559,1.27006292185433));
#85243=CARTESIAN_POINT('Ctrl Pts',(157.024485374886,-224.976060971526,1.11130505662254));
#85244=CARTESIAN_POINT('Ctrl Pts',(158.406134744506,-222.487324103837,0.952547191390749));
#85245=CARTESIAN_POINT('Ctrl Pts',(161.246557418698,-222.29788038346,0.793789326158957));
#85246=CARTESIAN_POINT('Ctrl Pts',(162.945990021977,-224.582055024746,0.635031460927165));
#85247=CARTESIAN_POINT('Ctrl Pts',(161.949545639495,-227.247408636808,0.47627359569537));
#85248=CARTESIAN_POINT('Ctrl Pts',(159.168282701031,-227.85869812666,0.317515730463582));
#85249=CARTESIAN_POINT('Ctrl Pts',(157.149564424984,-225.848042905619,0.158757865231786));
#85250=CARTESIAN_POINT('Ctrl Pts',(157.542565484547,-224.000243484621,0.0529192884105924));
#85251=CARTESIAN_POINT('Ctrl Pts',(158.086534003335,-223.364012796625,-4.44089209850063E-15));
#85252=CARTESIAN_POINT('Ctrl Pts',(158.086534003335,-223.364012796625,-4.44089209850063E-15));
#85253=CARTESIAN_POINT('Ctrl Pts',(158.024938131872,-223.421897790789,-4.02047441971943E-15));
#85254=CARTESIAN_POINT('Ctrl Pts',(157.966714212982,-223.482934468891,-1.25170609456878E-15));
#85255=CARTESIAN_POINT('Ctrl Pts',(157.911858615954,-223.546737772691,-1.38777878078145E-15));
#85256=CARTESIAN_POINT('Ctrl Pts',(157.855548999771,-223.612232266285,-1.52745825104056E-15));
#85257=CARTESIAN_POINT('Ctrl Pts',(157.802788200628,-223.680642427049,-1.1358963542259E-14));
#85258=CARTESIAN_POINT('Ctrl Pts',(157.753597853786,-223.751600310779,-1.22124532708767E-14));
#85259=CARTESIAN_POINT('Ctrl Pts',(157.702709598817,-223.825007454886,-1.30954029899182E-14));
#85260=CARTESIAN_POINT('Ctrl Pts',(157.655641951551,-223.90114175895,-2.81027041762154E-15));
#85261=CARTESIAN_POINT('Ctrl Pts',(157.612453799623,-223.979639850734,-1.49880108324396E-15));
#85262=CARTESIAN_POINT('Ctrl Pts',(157.593558983155,-224.013982765889,-9.25033249453769E-16));
#85263=CARTESIAN_POINT('Ctrl Pts',(157.575407220319,-224.048778631187,-8.43275911610205E-15));
#85264=CARTESIAN_POINT('Ctrl Pts',(157.55800588697,-224.083999106998,-8.38218383591993E-15));
#85265=CARTESIAN_POINT('Ctrl Pts',(157.548477933598,-224.103283781599,-8.35449176763588E-15));
#85266=CARTESIAN_POINT('Ctrl Pts',(157.539174987618,-224.122695774927,-8.94435754255875E-16));
#85267=CARTESIAN_POINT('Ctrl Pts',(157.530098465041,-224.142230564629,-3.88578058618805E-16));
#85268=CARTESIAN_POINT('Ctrl Pts',(157.521442320672,-224.16086060256,9.38508900182872E-17));
#85269=CARTESIAN_POINT('Ctrl Pts',(157.512989615474,-224.179608342932,-5.5821178937832E-15));
#85270=CARTESIAN_POINT('Ctrl Pts',(157.504755700859,-224.198437010398,-5.49560397189452E-15));
#85271=CARTESIAN_POINT('Ctrl Pts',(157.468216216528,-224.281992625442,-5.11168280667383E-15));
#85272=CARTESIAN_POINT('Ctrl Pts',(157.435936147707,-224.367231893099,-3.02367079316581E-15));
#85273=CARTESIAN_POINT('Ctrl Pts',(157.407939191047,-224.453755565247,-3.69149155687865E-15));
#85274=CARTESIAN_POINT('Ctrl Pts',(157.379477689978,-224.541714896589,-4.37039325364763E-15));
#85275=CARTESIAN_POINT('Ctrl Pts',(157.355442125594,-224.631002365215,-7.11283600949192E-15));
#85276=CARTESIAN_POINT('Ctrl Pts',(157.33589650728,-224.721235656857,-7.35522753814166E-15));
#85277=CARTESIAN_POINT('Ctrl Pts',(157.31669447316,-224.809882775465,-7.59335816818749E-15));
#85278=CARTESIAN_POINT('Ctrl Pts',(157.301825663592,-224.899443667177,-6.01491689603108E-15));
#85279=CARTESIAN_POINT('Ctrl Pts',(157.291393417184,-224.989578650944,-6.13398221105399E-15));
#85280=CARTESIAN_POINT('Ctrl Pts',(157.287259487947,-225.025295948072,-6.18116357234791E-15));
#85281=CARTESIAN_POINT('Ctrl Pts',(157.28382270983,-225.061103573716,-5.15113929225242E-15));
#85282=CARTESIAN_POINT('Ctrl Pts',(157.281091552527,-225.096980929019,-5.6621374255883E-15));
#85283=CARTESIAN_POINT('Ctrl Pts',(157.279473342812,-225.118238249062,-5.96490363479611E-15));
#85284=CARTESIAN_POINT('Ctrl Pts',(157.278102868135,-225.139520052234,-6.46012964232343E-15));
#85285=CARTESIAN_POINT('Ctrl Pts',(157.276982094653,-225.160822076977,-6.60582699651968E-15));
#85286=CARTESIAN_POINT('Ctrl Pts',(157.276240093157,-225.174924957255,-6.7022850735275E-15));
#85287=CARTESIAN_POINT('Ctrl Pts',(157.27560761903,-225.18903661353,-1.04645236124941E-14));
#85288=CARTESIAN_POINT('Ctrl Pts',(157.275085584502,-225.203141411304,-1.02418074021671E-14));
#85289=CARTESIAN_POINT('Ctrl Pts',(157.271562563848,-225.298329547766,-8.73877691854704E-15));
#85290=CARTESIAN_POINT('Ctrl Pts',(157.273056291674,-225.393366882897,-1.25249371125912E-14));
#85291=CARTESIAN_POINT('Ctrl Pts',(157.279624839535,-225.487854119313,-1.19904086659517E-14));
#85292=CARTESIAN_POINT('Ctrl Pts',(157.286171652655,-225.582028705859,-1.14576489264445E-14));
#85293=CARTESIAN_POINT('Ctrl Pts',(157.297759397958,-225.675657782649,-1.02581785354216E-14));
#85294=CARTESIAN_POINT('Ctrl Pts',(157.314493581616,-225.768363904367,-1.11854969730985E-14));
#85295=CARTESIAN_POINT('Ctrl Pts',(157.316397869106,-225.778913514163,-1.12910223417952E-14));
#85296=CARTESIAN_POINT('Ctrl Pts',(157.318368855583,-225.789451182139,-9.70347588764154E-15));
#85297=CARTESIAN_POINT('Ctrl Pts',(157.320406739366,-225.799976358203,-9.93649607039515E-15));
#85298=CARTESIAN_POINT('Ctrl Pts',(157.337939942263,-225.890531103766,-1.1971137394992E-14));
#85299=CARTESIAN_POINT('Ctrl Pts',(157.36042066591,-225.980161474788,-5.38012735527091E-15));
#85300=CARTESIAN_POINT('Ctrl Pts',(157.387574007674,-226.068629871038,-4.8017145815038E-15));
#85301=CARTESIAN_POINT('Ctrl Pts',(157.398274256088,-226.103492387221,-4.57378092902809E-15));
#85302=CARTESIAN_POINT('Ctrl Pts',(157.409700687624,-226.138174410619,-6.81791231009982E-15));
#85303=CARTESIAN_POINT('Ctrl Pts',(157.421838645824,-226.172661063201,-7.04991620636974E-15));
#85304=CARTESIAN_POINT('Ctrl Pts',(157.42714896822,-226.187748876204,-7.15141725505753E-15));
#85305=CARTESIAN_POINT('Ctrl Pts',(157.432595494617,-226.20279929086,-9.33337609025355E-15));
#85306=CARTESIAN_POINT('Ctrl Pts',(157.438177066941,-226.217811042138,-9.29811783123569E-15));
#85307=CARTESIAN_POINT('Ctrl Pts',(157.44259780243,-226.229700699347,-9.27019246758084E-15));
#85308=CARTESIAN_POINT('Ctrl Pts',(157.447102851067,-226.241564891189,-9.32321973403198E-15));
#85309=CARTESIAN_POINT('Ctrl Pts',(157.451687905131,-226.253393829545,-9.43689570931383E-15));
#85310=CARTESIAN_POINT('Ctrl Pts',(157.485446240419,-226.34048664493,-1.02738567645768E-14));
#85311=CARTESIAN_POINT('Ctrl Pts',(157.523587548176,-226.425804632643,-1.06218398729921E-14));
#85312=CARTESIAN_POINT('Ctrl Pts',(157.565778560797,-226.509117057952,-9.78384040450919E-15));
#85313=CARTESIAN_POINT('Ctrl Pts',(157.609551906108,-226.595554034339,-8.91441258505656E-15));
#85314=CARTESIAN_POINT('Ctrl Pts',(157.657684534616,-226.679832913129,-6.08329446841785E-15));
#85315=CARTESIAN_POINT('Ctrl Pts',(157.709860342191,-226.761692981327,-5.20417042793042E-15));
#85316=CARTESIAN_POINT('Ctrl Pts',(157.762637853889,-226.844497079773,-4.31490811485777E-15));
#85317=CARTESIAN_POINT('Ctrl Pts',(157.819552746941,-226.924827072195,-8.96093847127932E-15));
#85318=CARTESIAN_POINT('Ctrl Pts',(157.880329760087,-227.002398324715,-7.64666108210577E-15));
#85319=CARTESIAN_POINT('Ctrl Pts',(157.92312880423,-227.057023836714,-6.7211497237137E-15));
#85320=CARTESIAN_POINT('Ctrl Pts',(157.967844154052,-227.110281017477,-8.49846093585579E-15));
#85321=CARTESIAN_POINT('Ctrl Pts',(158.014393105504,-227.162062750717,-9.13158437754191E-15));
#85322=CARTESIAN_POINT('Ctrl Pts',(158.02559966715,-227.174529093515,-9.28400750754482E-15));
#85323=CARTESIAN_POINT('Ctrl Pts',(158.036913147564,-227.186910416437,-1.3469166115988E-14));
#85324=CARTESIAN_POINT('Ctrl Pts',(158.048321150992,-227.199193291615,-1.33087985076941E-14));
#85325=CARTESIAN_POINT('Ctrl Pts',(158.116987457225,-227.273125568526,-1.23435243147714E-14));
#85326=CARTESIAN_POINT('Ctrl Pts',(158.189166708083,-227.343596762759,-3.71230618695111E-15));
#85327=CARTESIAN_POINT('Ctrl Pts',(158.264545772445,-227.410319899525,-7.56339435525888E-15));
#85328=CARTESIAN_POINT('Ctrl Pts',(158.329365760519,-227.467696479694,-1.08750232704468E-14));
#85329=CARTESIAN_POINT('Ctrl Pts',(158.3965529381,-227.522301582086,-9.56933057703736E-15));
#85330=CARTESIAN_POINT('Ctrl Pts',(158.465934417848,-227.573937429872,-6.84868828315643E-15));
#85331=CARTESIAN_POINT('Ctrl Pts',(158.491454071548,-227.592929947167,-5.84799113118415E-15));
#85332=CARTESIAN_POINT('Ctrl Pts',(158.517270804806,-227.611520587321,-1.17738964924128E-14));
#85333=CARTESIAN_POINT('Ctrl Pts',(158.543376723496,-227.629698856678,-1.18516307878735E-14));
#85334=CARTESIAN_POINT('Ctrl Pts',(158.560069303013,-227.641322359009,-1.19013354515399E-14));
#85335=CARTESIAN_POINT('Ctrl Pts',(158.57688116617,-227.652777833288,-1.23844299269826E-14));
#85336=CARTESIAN_POINT('Ctrl Pts',(158.593795463636,-227.664052888908,-1.19002030452009E-14));
#85337=CARTESIAN_POINT('Ctrl Pts',(158.679989147357,-227.721509521675,-9.43262797853806E-15));
#85338=CARTESIAN_POINT('Ctrl Pts',(158.768924488191,-227.774344032196,-5.88836659555711E-15));
#85339=CARTESIAN_POINT('Ctrl Pts',(158.86029512281,-227.822237061513,-2.13370987545147E-15));
#85340=CARTESIAN_POINT('Ctrl Pts',(158.951665757429,-227.870130090831,1.62094684465417E-15));
#85341=CARTESIAN_POINT('Ctrl Pts',(159.045472324464,-227.913082541088,-5.46458148948038E-15));
#85342=CARTESIAN_POINT('Ctrl Pts',(159.141446274327,-227.95073460326,-7.40379979546901E-15));
#85343=CARTESIAN_POINT('Ctrl Pts',(159.162330716372,-227.958927892287,-7.86016396636461E-15));
#85344=CARTESIAN_POINT('Ctrl Pts',(159.183317909858,-227.966870015372,8.49377045481285E-16));
#85345=CARTESIAN_POINT('Ctrl Pts',(159.204403760484,-227.974562200359,8.32667268468867E-16));
#85346=CARTESIAN_POINT('Ctrl Pts',(157.485690666959,-224.998572567547,19.112583302492));
#85347=CARTESIAN_POINT('Ctrl Pts',(157.484001293575,-224.6725707558,19.092036810933));
#85348=CARTESIAN_POINT('Ctrl Pts',(157.542838236001,-224.347153873571,19.071490319374));
#85349=CARTESIAN_POINT('Ctrl Pts',(157.665030280249,-224.047579988685,19.0509438278151));
#85350=CARTESIAN_POINT('Ctrl Pts',(157.979746591422,-223.276001212375,18.9980245394045));
#85351=CARTESIAN_POINT('Ctrl Pts',(158.714738560392,-222.675855870717,18.9451052509939));
#85352=CARTESIAN_POINT('Ctrl Pts',(159.533660666009,-222.521758115913,18.8921859625833));
#85353=CARTESIAN_POINT('Ctrl Pts',(160.352582771625,-222.367660361109,18.8392666741727));
#85354=CARTESIAN_POINT('Ctrl Pts',(161.255435013888,-222.659610193158,18.7863473857621));
#85355=CARTESIAN_POINT('Ctrl Pts',(161.829078591495,-223.264017324161,18.7334280973515));
#85356=CARTESIAN_POINT('Ctrl Pts',(162.402722169101,-223.868424455164,18.6805088089409));
#85357=CARTESIAN_POINT('Ctrl Pts',(162.647157082051,-224.785288885121,18.6275895205303));
#85358=CARTESIAN_POINT('Ctrl Pts',(162.450526850331,-225.595050601476,18.5746702321197));
#85359=CARTESIAN_POINT('Ctrl Pts',(162.253896618611,-226.404812317831,18.5217509437091));
#85360=CARTESIAN_POINT('Ctrl Pts',(161.616201242222,-227.107471320585,18.4688316552985));
#85361=CARTESIAN_POINT('Ctrl Pts',(160.829251591834,-227.381492245887,18.4159123668879));
#85362=CARTESIAN_POINT('Ctrl Pts',(160.042301941446,-227.655513171189,18.3629930784773));
#85363=CARTESIAN_POINT('Ctrl Pts',(159.10609801706,-227.500896019039,18.3100737900667));
#85364=CARTESIAN_POINT('Ctrl Pts',(158.449046003258,-226.988392929152,18.2571545016561));
#85365=CARTESIAN_POINT('Ctrl Pts',(157.850708419101,-226.521687319499,18.2089641019347));
#85366=CARTESIAN_POINT('Ctrl Pts',(157.483861600094,-225.758199612281,18.1607737022134));
#85367=CARTESIAN_POINT('Ctrl Pts',(157.479093605947,-224.998703157778,18.112583302492));
#85368=CARTESIAN_POINT('Origin',(-160.,-225.,22.2084234471774));
#85369=CARTESIAN_POINT('Ctrl Pts',(-163.076377950168,-224.997773694264,
19.7084234471775));
#85370=CARTESIAN_POINT('Ctrl Pts',(-163.077562842917,-224.85366922826,19.7009407276991));
#85371=CARTESIAN_POINT('Ctrl Pts',(-163.002826982104,-223.691638940026,
19.6405387198101));
#85372=CARTESIAN_POINT('Ctrl Pts',(-161.521864797362,-221.70110626648,19.5272174235105));
#85373=CARTESIAN_POINT('Ctrl Pts',(-158.054123026994,-221.932389233715,
19.3684595582787));
#85374=CARTESIAN_POINT('Ctrl Pts',(-156.367330739964,-224.970773973196,
19.2097016930469));
#85375=CARTESIAN_POINT('Ctrl Pts',(-158.005117242933,-228.036087327305,
19.0509438278151));
#85376=CARTESIAN_POINT('Ctrl Pts',(-161.468639631394,-228.322686472282,
18.8921859625833));
#85377=CARTESIAN_POINT('Ctrl Pts',(-162.992852930873,-226.341897473527,
18.7780125023707));
#85378=CARTESIAN_POINT('Ctrl Pts',(-163.077320562719,-225.163035204797,
18.7167583305688));
#85379=CARTESIAN_POINT('Ctrl Pts',(-163.075931333395,-225.0024275328,18.7084234471774));
#85380=CARTESIAN_POINT('Ctrl Pts',(-163.070362267144,-225.003024949566,
19.7915765528225));
#85381=CARTESIAN_POINT('Ctrl Pts',(-163.065080691912,-224.299688720016,
19.7552124583938));
#85382=CARTESIAN_POINT('Ctrl Pts',(-162.477826131062,-222.562575755896,
19.6659290755545));
#85383=CARTESIAN_POINT('Ctrl Pts',(-159.592724505823,-221.390669564417,
19.5237264043046));
#85384=CARTESIAN_POINT('Ctrl Pts',(-156.746988377721,-223.383220985595,
19.3649685390728));
#85385=CARTESIAN_POINT('Ctrl Pts',(-156.877197897433,-226.856577363582,
19.206210673841));
#85386=CARTESIAN_POINT('Ctrl Pts',(-159.865978935642,-228.630249528,19.0474528086092));
#85387=CARTESIAN_POINT('Ctrl Pts',(-162.574488231656,-227.282183302953,
18.9092414349364));
#85388=CARTESIAN_POINT('Ctrl Pts',(-163.066355304625,-225.625342192633,
18.8239493496742));
#85389=CARTESIAN_POINT('Ctrl Pts',(-163.069604917803,-224.99825730896,18.7915765528225));
#85390=CARTESIAN_POINT('Ctrl Pts',(-158.086534003335,-223.364012796625,
20.));
#85391=CARTESIAN_POINT('Ctrl Pts',(-157.542565484547,-224.000243484621,
19.9470807115894));
#85392=CARTESIAN_POINT('Ctrl Pts',(-157.14956575156,-225.848044358444,19.8412421347682));
#85393=CARTESIAN_POINT('Ctrl Pts',(-159.168282289031,-227.858697938457,
19.6824842695364));
#85394=CARTESIAN_POINT('Ctrl Pts',(-161.949545980211,-227.24740909585,19.5237264043046));
#85395=CARTESIAN_POINT('Ctrl Pts',(-162.945990159525,-224.582054828932,
19.3649685390728));
#85396=CARTESIAN_POINT('Ctrl Pts',(-161.246557549164,-222.297880275211,
19.206210673841));
#85397=CARTESIAN_POINT('Ctrl Pts',(-158.406134608902,-222.487323863959,
19.0474528086093));
#85398=CARTESIAN_POINT('Ctrl Pts',(-157.024485159544,-224.976060998054,
18.8886949433774));
#85399=CARTESIAN_POINT('Ctrl Pts',(-158.365994032564,-227.486855326661,
18.7299370781457));
#85400=CARTESIAN_POINT('Ctrl Pts',(-161.202960882393,-227.721608327304,
18.5711792129139));
#85401=CARTESIAN_POINT('Ctrl Pts',(-162.938970375395,-225.465579917995,
18.4124213476821));
#85402=CARTESIAN_POINT('Ctrl Pts',(-161.985237961226,-222.783436196243,
18.2536634824503));
#85403=CARTESIAN_POINT('Ctrl Pts',(-159.21461407685,-222.129899575534,18.0949056172185));
#85404=CARTESIAN_POINT('Ctrl Pts',(-157.16277620961,-224.103074897453,17.9361477519867));
#85405=CARTESIAN_POINT('Ctrl Pts',(-157.707565033574,-226.897117894792,
17.7773898867549));
#85406=CARTESIAN_POINT('Ctrl Pts',(-160.350390446343,-227.954917774566,
17.6186320215231));
#85407=CARTESIAN_POINT('Ctrl Pts',(-162.672538441131,-226.308377454507,
17.4598741562913));
#85408=CARTESIAN_POINT('Ctrl Pts',(-162.548779405603,-223.464409931704,
17.3011162910595));
#85409=CARTESIAN_POINT('Ctrl Pts',(-160.092377536169,-222.025814479178,
17.1423584258277));
#85410=CARTESIAN_POINT('Ctrl Pts',(-157.551431759929,-223.309193450083,
16.9836005605959));
#85411=CARTESIAN_POINT('Ctrl Pts',(-157.251415535576,-226.139998532244,
16.8248426953642));
#85412=CARTESIAN_POINT('Ctrl Pts',(-159.466903707454,-227.927476991314,
16.6660848301324));
#85413=CARTESIAN_POINT('Ctrl Pts',(-162.170281584114,-227.035728628457,
16.5073269649006));
#85414=CARTESIAN_POINT('Ctrl Pts',(-162.887417840912,-224.280881502285,
16.3485690996688));
#85415=CARTESIAN_POINT('Ctrl Pts',(-160.961989402975,-222.184171598198,
16.189811234437));
#85416=CARTESIAN_POINT('Ctrl Pts',(-158.156148301398,-222.664507736106,
16.0310533692052));
#85417=CARTESIAN_POINT('Ctrl Pts',(-157.03780020181,-225.28228630238,15.8722955039734));
#85418=CARTESIAN_POINT('Ctrl Pts',(-158.63045724107,-227.641716455676,15.7135376387416));
#85419=CARTESIAN_POINT('Ctrl Pts',(-161.476519759432,-227.583447812688,
15.5547797735098));
#85420=CARTESIAN_POINT('Ctrl Pts',(-162.971271452032,-225.160807833087,
15.396021908278));
#85421=CARTESIAN_POINT('Ctrl Pts',(-161.746715628571,-222.590996530984,
15.2372640430462));
#85422=CARTESIAN_POINT('Ctrl Pts',(-158.923565730531,-222.225905108985,
15.0785061778144));
#85423=CARTESIAN_POINT('Ctrl Pts',(-157.085568433579,-224.399665222158,
14.9197483125826));
#85424=CARTESIAN_POINT('Ctrl Pts',(-157.914858791609,-227.122851700403,
14.7609904473509));
#85425=CARTESIAN_POINT('Ctrl Pts',(-160.652470301561,-227.903204385919,
14.6022325821191));
#85426=CARTESIAN_POINT('Ctrl Pts',(-162.792941017183,-226.026544531607,
14.4434747168873));
#85427=CARTESIAN_POINT('Ctrl Pts',(-162.377312223709,-223.210391162337,
14.2847168516555));
#85428=CARTESIAN_POINT('Ctrl Pts',(-159.785967376581,-222.032087730921,
14.1259589864237));
#85429=CARTESIAN_POINT('Ctrl Pts',(-157.39050517799,-223.570017491456,13.9672011211919));
#85430=CARTESIAN_POINT('Ctrl Pts',(-157.383252537887,-226.416667187578,
13.8084432559601));
#85431=CARTESIAN_POINT('Ctrl Pts',(-159.770847072208,-227.966783129337,
13.6496853907283));
#85432=CARTESIAN_POINT('Ctrl Pts',(-162.368162357033,-226.801699267793,
13.4909275254965));
#85433=CARTESIAN_POINT('Ctrl Pts',(-162.798135545827,-223.987700307215,
13.3321696602647));
#85434=CARTESIAN_POINT('Ctrl Pts',(-160.667255193115,-222.100157985666,
13.1734117950329));
#85435=CARTESIAN_POINT('Ctrl Pts',(-157.925702913902,-222.866550961602,
13.0146539298011));
#85436=CARTESIAN_POINT('Ctrl Pts',(-157.082547246317,-225.585476413584,
12.8558960645693));
#85437=CARTESIAN_POINT('Ctrl Pts',(-158.909444224176,-227.768573874878,
12.6971381993376));
#85438=CARTESIAN_POINT('Ctrl Pts',(-161.734417805185,-227.417872634754,
12.5383803341058));
#85439=CARTESIAN_POINT('Ctrl Pts',(-162.972052279092,-224.854334454385,
12.379622468874));
#85440=CARTESIAN_POINT('Ctrl Pts',(-161.489664624048,-222.424109375634,
12.2208646036422));
#85441=CARTESIAN_POINT('Ctrl Pts',(-158.643935963655,-222.351339295008,
12.0621067384104));
#85442=CARTESIAN_POINT('Ctrl Pts',(-157.039277055999,-224.702623387435,
11.9033488731786));
#85443=CARTESIAN_POINT('Ctrl Pts',(-158.144271670265,-227.326066543987,
11.7445910079468));
#85444=CARTESIAN_POINT('Ctrl Pts',(-160.94762877893,-227.820693690952,11.585833142715));
#85445=CARTESIAN_POINT('Ctrl Pts',(-162.883716066383,-225.733822082879,
11.4270752774832));
#85446=CARTESIAN_POINT('Ctrl Pts',(-162.180626523281,-222.975356533412,
11.2683174122514));
#85447=CARTESIAN_POINT('Ctrl Pts',(-159.481827671824,-222.069844604949,
11.1095595470196));
#85448=CARTESIAN_POINT('Ctrl Pts',(-157.257260114736,-223.846010778811,
10.9508016817878));
#85449=CARTESIAN_POINT('Ctrl Pts',(-157.542847992787,-226.678307842526,
10.792043816556));
#85450=CARTESIAN_POINT('Ctrl Pts',(-160.077221291214,-227.974617634759,
10.6332859513242));
#85451=CARTESIAN_POINT('Ctrl Pts',(-162.540921666958,-226.548557484635,
10.4745280860925));
#85452=CARTESIAN_POINT('Ctrl Pts',(-162.679170633022,-223.705257585468,
10.3157702208607));
#85453=CARTESIAN_POINT('Ctrl Pts',(-160.3654427411,-222.046905893167,10.1570123556289));
#85454=CARTESIAN_POINT('Ctrl Pts',(-157.717261666894,-223.091225811312,
9.99825449039707));
#85455=CARTESIAN_POINT('Ctrl Pts',(-157.15824262538,-225.882455791883,9.83949662516529));
#85456=CARTESIAN_POINT('Ctrl Pts',(-159.199999821369,-227.866062266425,
9.68073875993349));
#85457=CARTESIAN_POINT('Ctrl Pts',(-161.973917149382,-227.22664866744,9.5219808947017));
#85458=CARTESIAN_POINT('Ctrl Pts',(-162.941305579903,-224.549406295574,
9.36322302946991));
#85459=CARTESIAN_POINT('Ctrl Pts',(-161.216811259361,-222.28454726428,9.20446516423811));
#85460=CARTESIAN_POINT('Ctrl Pts',(-158.378691322102,-222.504870469934,
9.04570729900632));
#85461=CARTESIAN_POINT('Ctrl Pts',(-157.024393023099,-225.008736123386,
8.88694943377453));
#85462=CARTESIAN_POINT('Ctrl Pts',(-158.393370112343,-227.504606477058,
8.72819156854273));
#85463=CARTESIAN_POINT('Ctrl Pts',(-161.232734811591,-227.708261081419,
8.56943370331094));
#85464=CARTESIAN_POINT('Ctrl Pts',(-162.943900659748,-225.433315250564,
8.41067583807915));
#85465=CARTESIAN_POINT('Ctrl Pts',(-161.960808739869,-222.761799319433,
8.25191797284736));
#85466=CARTESIAN_POINT('Ctrl Pts',(-159.183184738369,-222.138684563142,
8.09316010761556));
#85467=CARTESIAN_POINT('Ctrl Pts',(-157.153110032193,-224.134245582145,
7.93440224238378));
#85468=CARTESIAN_POINT('Ctrl Pts',(-157.728508912603,-226.922145010324,
7.77564437715198));
#85469=CARTESIAN_POINT('Ctrl Pts',(-160.382776346874,-227.950897400641,
7.61688651192019));
#85470=CARTESIAN_POINT('Ctrl Pts',(-162.686726883539,-226.278988605933,
7.45812864668839));
#85471=CARTESIAN_POINT('Ctrl Pts',(-162.531785082041,-223.43654948937,7.2993707814566));
#85472=CARTESIAN_POINT('Ctrl Pts',(-160.05975367302,-222.024980218655,7.14061291622481));
#85473=CARTESIAN_POINT('Ctrl Pts',(-157.5330357048,-223.336148934837,6.98185505099302));
#85474=CARTESIAN_POINT('Ctrl Pts',(-157.264083362536,-226.170074080427,
6.82309718576123));
#85475=CARTESIAN_POINT('Ctrl Pts',(-159.499041819292,-227.933147473623,
6.66433932052943));
#85476=CARTESIAN_POINT('Ctrl Pts',(-162.192477183332,-227.011804414302,
6.50558145529764));
#85477=CARTESIAN_POINT('Ctrl Pts',(-162.879357515403,-224.249258034125,
6.34682359006585));
#85478=CARTESIAN_POINT('Ctrl Pts',(-160.931049962606,-222.173790671594,
6.18806572483405));
#85479=CARTESIAN_POINT('Ctrl Pts',(-158.130645520644,-222.684869975283,
6.02930785960226));
#85480=CARTESIAN_POINT('Ctrl Pts',(-157.041074224678,-225.314756186552,
5.87054999437047));
#85481=CARTESIAN_POINT('Ctrl Pts',(-158.65951168193,-227.656577548267,5.71179212913868));
#85482=CARTESIAN_POINT('Ctrl Pts',(-161.504763995166,-227.567099242275,
5.55303426390689));
#85483=CARTESIAN_POINT('Ctrl Pts',(-162.972856359199,-225.128211810702,
5.3942763986751));
#85484=CARTESIAN_POINT('Ctrl Pts',(-161.720190700198,-222.571984935017,
5.2355185334433));
#85485=CARTESIAN_POINT('Ctrl Pts',(-158.89320658002,-222.237877351324,5.07676066821151));
#85486=CARTESIAN_POINT('Ctrl Pts',(-157.079159754285,-224.431664307083,
4.91800280297972));
#85487=CARTESIAN_POINT('Ctrl Pts',(-157.938265806568,-227.145592066649,
4.75924493774793));
#85488=CARTESIAN_POINT('Ctrl Pts',(-160.684270911606,-227.895874051193,
4.60048707251613));
#85489=CARTESIAN_POINT('Ctrl Pts',(-162.804031305248,-225.99585221796,4.44172920728434));
#85490=CARTESIAN_POINT('Ctrl Pts',(-162.357542358599,-223.184426474016,
4.28297134205255));
#85491=CARTESIAN_POINT('Ctrl Pts',(-159.753430738056,-222.034613549646,
4.12421347682075));
#85492=CARTESIAN_POINT('Ctrl Pts',(-157.374979296373,-223.598722188052,
3.96545561158896));
#85493=CARTESIAN_POINT('Ctrl Pts',(-157.398946699372,-226.445280224801,
3.80669774635717));
#85494=CARTESIAN_POINT('Ctrl Pts',(-159.803397980927,-227.969117856745,
3.64793988112538));
#85495=CARTESIAN_POINT('Ctrl Pts',(-162.387779422388,-226.77561894275,3.48918201589358));
#85496=CARTESIAN_POINT('Ctrl Pts',(-162.786865230829,-223.957073642597,
3.3304241506618));
#85497=CARTESIAN_POINT('Ctrl Pts',(-160.635412088667,-222.093014502851,
3.17166628543));
#85498=CARTESIAN_POINT('Ctrl Pts',(-157.902429829893,-222.889428377601,
3.01290842019821));
#85499=CARTESIAN_POINT('Ctrl Pts',(-157.089143704272,-225.617437314398,
2.85415055496641));
#85500=CARTESIAN_POINT('Ctrl Pts',(-158.939873154425,-227.780367653174,
2.69539268973462));
#85501=CARTESIAN_POINT('Ctrl Pts',(-161.760830634549,-227.398705608841,
2.53663482450283));
#85502=CARTESIAN_POINT('Ctrl Pts',(-162.970276023305,-224.821748319362,
2.37787695927104));
#85503=CARTESIAN_POINT('Ctrl Pts',(-161.461324837368,-222.407926890985,
2.21911909403925));
#85504=CARTESIAN_POINT('Ctrl Pts',(-158.614969373296,-222.366370815315,
2.06036122880745));
#85505=CARTESIAN_POINT('Ctrl Pts',(-157.03619356153,-224.735111764472,1.90160336357566));
#85506=CARTESIAN_POINT('Ctrl Pts',(-158.169893955495,-227.346279041844,
1.74284549834387));
#85507=CARTESIAN_POINT('Ctrl Pts',(-160.978505939593,-227.810130534509,
1.58408763311208));
#85508=CARTESIAN_POINT('Ctrl Pts',(-162.89159221018,-225.702153365617,1.42532976788028));
#85509=CARTESIAN_POINT('Ctrl Pts',(-162.158287419518,-222.951559875847,
1.26657190264849));
#85510=CARTESIAN_POINT('Ctrl Pts',(-159.449730484722,-222.075710302932,
1.1078140374167));
#85511=CARTESIAN_POINT('Ctrl Pts',(-157.244754422452,-223.876146484295,
0.949056172184905));
#85512=CARTESIAN_POINT('Ctrl Pts',(-157.561432469829,-226.705183287036,
0.790298306953112));
#85513=CARTESIAN_POINT('Ctrl Pts',(-160.109776483231,-227.973532810194,
0.631540441721317));
#85514=CARTESIAN_POINT('Ctrl Pts',(-162.557883271515,-226.520720191152,
0.472782576489527));
#85515=CARTESIAN_POINT('Ctrl Pts',(-162.66453771979,-223.67569832521,0.314024711257735));
#85516=CARTESIAN_POINT('Ctrl Pts',(-160.333598844781,-222.043602025466,
0.15526684602594));
#85517=CARTESIAN_POINT('Ctrl Pts',(-157.695294647756,-223.115260895132,
-0.00349101920584827));
#85518=CARTESIAN_POINT('Ctrl Pts',(-157.170584060966,-225.915729262672,
-0.162248884437644));
#85519=CARTESIAN_POINT('Ctrl Pts',(-158.541127016969,-227.215894200354,
-0.268087461258838));
#85520=CARTESIAN_POINT('Ctrl Pts',(-159.349800002025,-227.432086802035,
-0.321006749669435));
#85521=CARTESIAN_POINT('Ctrl Pts',(-157.945668449658,-223.243574678773,
20.1070022498898));
#85522=CARTESIAN_POINT('Ctrl Pts',(-157.361654052493,-223.926643402192,
20.0540829614792));
#85523=CARTESIAN_POINT('Ctrl Pts',(-156.9397224623,-225.9104756942,19.948244384658));
#85524=CARTESIAN_POINT('Ctrl Pts',(-159.107052888527,-228.069149584109,
19.7894865194262));
#85525=CARTESIAN_POINT('Ctrl Pts',(-162.09306767038,-227.412858875035,19.6307286541944));
#85526=CARTESIAN_POINT('Ctrl Pts',(-163.162868084542,-224.551286538285,
19.4719707889626));
#85527=CARTESIAN_POINT('Ctrl Pts',(-161.338326631897,-222.098955605634,
19.3132129237308));
#85528=CARTESIAN_POINT('Ctrl Pts',(-158.288797414932,-222.302345653878,
19.1544550584991));
#85529=CARTESIAN_POINT('Ctrl Pts',(-156.805433686351,-224.974298656435,
18.9956971932672));
#85530=CARTESIAN_POINT('Ctrl Pts',(-158.245701769353,-227.669932660209,
18.8369393280355));
#85531=CARTESIAN_POINT('Ctrl Pts',(-161.291520465393,-227.921967708964,
18.6781814628037));
#85532=CARTESIAN_POINT('Ctrl Pts',(-163.155331517893,-225.499854983788,
18.5194235975719));
#85533=CARTESIAN_POINT('Ctrl Pts',(-162.131387223912,-222.620257185996,
18.3606657323401));
#85534=CARTESIAN_POINT('Ctrl Pts',(-159.15679553024,-221.918608501585,18.2019078671083));
#85535=CARTESIAN_POINT('Ctrl Pts',(-156.953905447948,-224.037045058722,
18.0431500018765));
#85536=CARTESIAN_POINT('Ctrl Pts',(-157.538800539521,-227.036779933787,
17.8843921366447));
#85537=CARTESIAN_POINT('Ctrl Pts',(-160.376185492774,-228.172452932812,
17.7256342714129));
#85538=CARTESIAN_POINT('Ctrl Pts',(-162.869285395553,-226.404697595481,
17.5668764061811));
#85539=CARTESIAN_POINT('Ctrl Pts',(-162.736415466445,-223.351362850873,
17.4081185409494));
#85540=CARTESIAN_POINT('Ctrl Pts',(-160.0991781863,-221.806860867848,17.2493606757175));
#85541=CARTESIAN_POINT('Ctrl Pts',(-157.3711730454,-223.184719641178,17.0906028104858));
#85542=CARTESIAN_POINT('Ctrl Pts',(-157.049070224458,-226.223922952493,
16.931844945254));
#85543=CARTESIAN_POINT('Ctrl Pts',(-159.427658220708,-228.14299201378,16.7730870800222));
#85544=CARTESIAN_POINT('Ctrl Pts',(-162.330053389578,-227.185594913451,
16.6143292147904));
#85545=CARTESIAN_POINT('Ctrl Pts',(-163.099983788551,-224.227941431483,
16.4555713495586));
#85546=CARTESIAN_POINT('Ctrl Pts',(-161.032809145849,-221.976875922408,
16.2968134843268));
#85547=CARTESIAN_POINT('Ctrl Pts',(-158.020407613623,-222.492573449615,
16.138055619095));
#85548=CARTESIAN_POINT('Ctrl Pts',(-156.819728955495,-225.303067657444,
15.9792977538632));
#85549=CARTESIAN_POINT('Ctrl Pts',(-158.52963423227,-227.836194356948,15.8205398886314));
#85550=CARTESIAN_POINT('Ctrl Pts',(-161.585218201835,-227.773636092576,
15.6617820233996));
#85551=CARTESIAN_POINT('Ctrl Pts',(-163.190010535425,-225.172646185314,
15.5030241581678));
#85552=CARTESIAN_POINT('Ctrl Pts',(-161.875305352435,-222.413650496059,
15.344266292936));
#85553=CARTESIAN_POINT('Ctrl Pts',(-158.844320784643,-222.021681771096,
15.1855084277042));
#85554=CARTESIAN_POINT('Ctrl Pts',(-156.871013789299,-224.355469772111,
15.0267505624725));
#85555=CARTESIAN_POINT('Ctrl Pts',(-157.761354850944,-227.279131812342,
14.8679926972407));
#85556=CARTESIAN_POINT('Ctrl Pts',(-160.700503864973,-228.116932507544,
14.7092348320089));
#85557=CARTESIAN_POINT('Ctrl Pts',(-162.998551769325,-226.10211669441,14.5504769667771));
#85558=CARTESIAN_POINT('Ctrl Pts',(-162.552325212306,-223.078643725893,
14.3917191015453));
#85559=CARTESIAN_POINT('Ctrl Pts',(-159.770210721352,-221.813595943883,
14.2329612363135));
#85560=CARTESIAN_POINT('Ctrl Pts',(-157.198399369181,-223.464745028728,
14.0742033710817));
#85561=CARTESIAN_POINT('Ctrl Pts',(-157.190612804165,-226.52095940291,13.9154455058499));
#85562=CARTESIAN_POINT('Ctrl Pts',(-159.753977290301,-228.185191791358,
13.7566876406181));
#85563=CARTESIAN_POINT('Ctrl Pts',(-162.542501750679,-226.93433677761,13.5979297753863));
#85564=CARTESIAN_POINT('Ctrl Pts',(-163.004128708817,-223.913176821059,
13.4391719101545));
#85565=CARTESIAN_POINT('Ctrl Pts',(-160.71637719078,-221.886677395137,13.2804140449227));
#85566=CARTESIAN_POINT('Ctrl Pts',(-157.772997295912,-222.709490694757,
13.1216561796909));
#85567=CARTESIAN_POINT('Ctrl Pts',(-156.86777018825,-225.628578020463,12.9628983144592));
#85568=CARTESIAN_POINT('Ctrl Pts',(-158.82915968113,-227.97239076656,12.8041404492274));
#85569=CARTESIAN_POINT('Ctrl Pts',(-161.862102187797,-227.595871599988,
12.6453825839956));
#85570=CARTESIAN_POINT('Ctrl Pts',(-163.190848845418,-224.843610847187,
12.4866247187638));
#85571=CARTESIAN_POINT('Ctrl Pts',(-161.599330765189,-222.234477440891,
12.327866853532));
#85572=CARTESIAN_POINT('Ctrl Pts',(-158.544105231552,-222.15635017194,12.1691089883002));
#85573=CARTESIAN_POINT('Ctrl Pts',(-156.821314532746,-224.680731113806,
12.0103511230684));
#85574=CARTESIAN_POINT('Ctrl Pts',(-158.007656648573,-227.497306927762,
11.8515932578366));
#85575=CARTESIAN_POINT('Ctrl Pts',(-161.017391321278,-228.028347539634,
11.6928353926048));
#85576=CARTESIAN_POINT('Ctrl Pts',(-163.096009496758,-225.78784460232,11.534077527373));
#85577=CARTESIAN_POINT('Ctrl Pts',(-162.341159902552,-222.826306315944,
11.3753196621412));
#85578=CARTESIAN_POINT('Ctrl Pts',(-159.443680857594,-221.854132403737,
11.2165617969094));
#85579=CARTESIAN_POINT('Ctrl Pts',(-157.055345069889,-223.761056391922,
11.0578039316776));
#85580=CARTESIAN_POINT('Ctrl Pts',(-157.361957358426,-226.801861521499,
10.8990460664459));
#85581=CARTESIAN_POINT('Ctrl Pts',(-160.082906168792,-228.193603057457,
10.740288201214));
#85582=CARTESIAN_POINT('Ctrl Pts',(-162.72797925674,-226.662559200816,10.5815303359823));
#85583=CARTESIAN_POINT('Ctrl Pts',(-162.876405836195,-223.609941228966,
10.4227724707505));
#85584=CARTESIAN_POINT('Ctrl Pts',(-160.392345907475,-221.829504989705,
10.2640146055187));
#85585=CARTESIAN_POINT('Ctrl Pts',(-157.549211019663,-222.950705659188,
10.1052567402869));
#85586=CARTESIAN_POINT('Ctrl Pts',(-156.94903811028,-225.947420428797,9.9464988750551));
#85587=CARTESIAN_POINT('Ctrl Pts',(-159.141105402393,-228.077056059227,
9.7877410098233));
#85588=CARTESIAN_POINT('Ctrl Pts',(-162.11923299646,-227.390570105255,9.62898314459151));
#85589=CARTESIAN_POINT('Ctrl Pts',(-163.157838635504,-224.516234484961,
9.47022527935971));
#85590=CARTESIAN_POINT('Ctrl Pts',(-161.306390479514,-222.084641045007,
9.31146741412792));
#85591=CARTESIAN_POINT('Ctrl Pts',(-158.259333808045,-222.321184006019,
9.15270954889613));
#85592=CARTESIAN_POINT('Ctrl Pts',(-156.805334767004,-225.009379259381,
8.99395168366434));
#85593=CARTESIAN_POINT('Ctrl Pts',(-158.275093221573,-227.688990614926,
8.83519381843254));
#85594=CARTESIAN_POINT('Ctrl Pts',(-161.323486291929,-227.907637865433,
8.67643595320076));
#85595=CARTESIAN_POINT('Ctrl Pts',(-163.160624759956,-225.465215055836,
8.51767808796896));
#85596=CARTESIAN_POINT('Ctrl Pts',(-162.10515957196,-222.597027445432,8.35892022273717));
#85597=CARTESIAN_POINT('Ctrl Pts',(-159.12305242649,-221.928040222474,8.20016235750537));
#85598=CARTESIAN_POINT('Ctrl Pts',(-156.943527665811,-224.070510467106,
8.04140449227359));
#85599=CARTESIAN_POINT('Ctrl Pts',(-157.561286265189,-227.063649495691,
7.88264662704179));
#85600=CARTESIAN_POINT('Ctrl Pts',(-160.410955578766,-228.168136586971,
7.72388876181));
#85601=CARTESIAN_POINT('Ctrl Pts',(-162.884518362817,-226.373145198439,
7.56513089657821));
#85602=CARTESIAN_POINT('Ctrl Pts',(-162.718170054648,-223.321451378293,
7.40637303134641));
#85603=CARTESIAN_POINT('Ctrl Pts',(-160.064152619355,-221.805965190726,
7.24761516611462));
#85604=CARTESIAN_POINT('Ctrl Pts',(-157.351422709351,-223.213659535005,
7.08885730088283));
#85605=CARTESIAN_POINT('Ctrl Pts',(-157.062670631596,-226.256212602601,
6.93009943565104));
#85606=CARTESIAN_POINT('Ctrl Pts',(-159.462162276297,-228.149079945696,
6.77134157041924));
#85607=CARTESIAN_POINT('Ctrl Pts',(-162.353882984581,-227.159909446325,
6.61258370518746));
#85608=CARTESIAN_POINT('Ctrl Pts',(-163.091330077941,-224.193989906614,
6.45382583995566));
#85609=CARTESIAN_POINT('Ctrl Pts',(-160.999592005533,-221.965730772674,
6.29506797472387));
#85610=CARTESIAN_POINT('Ctrl Pts',(-157.993027368969,-222.514434716263,
6.13631010949207));
#85611=CARTESIAN_POINT('Ctrl Pts',(-156.823244005403,-225.337927909786,
5.97755224426028));
#85612=CARTESIAN_POINT('Ctrl Pts',(-158.560827603168,-227.852149493561,
5.8187943790285));
#85613=CARTESIAN_POINT('Ctrl Pts',(-161.61554172192,-227.756083972987,5.6600365137967));
#85614=CARTESIAN_POINT('Ctrl Pts',(-163.1917121203,-225.137650508716,5.50127864856491));
#85615=CARTESIAN_POINT('Ctrl Pts',(-161.846827711693,-222.393239304281,
5.34252078333311));
#85616=CARTESIAN_POINT('Ctrl Pts',(-158.811726653968,-222.034535386059,
5.18376291810132));
#85617=CARTESIAN_POINT('Ctrl Pts',(-156.864133315805,-224.389824565903,
5.02500505286953));
#85618=CARTESIAN_POINT('Ctrl Pts',(-157.786485043701,-227.303546279037,
4.86624718763773));
#85619=CARTESIAN_POINT('Ctrl Pts',(-160.734645572559,-228.109062528182,
4.70748932240594));
#85620=CARTESIAN_POINT('Ctrl Pts',(-163.010458502297,-226.069164873794,
4.54873145717415));
#85621=CARTESIAN_POINT('Ctrl Pts',(-162.531099929123,-223.050767568959,
4.38997359194236));
#85622=CARTESIAN_POINT('Ctrl Pts',(-159.735278800335,-221.816307708349,
4.23121572671057));
#85623=CARTESIAN_POINT('Ctrl Pts',(-157.181730503097,-223.495562907887,
4.07245786147877));
#85624=CARTESIAN_POINT('Ctrl Pts',(-157.207462338545,-226.551678874916,
3.91369999624698));
#85625=CARTESIAN_POINT('Ctrl Pts',(-159.788924532055,-228.187698396745,
3.75494213101518));
#85626=CARTESIAN_POINT('Ctrl Pts',(-162.563562985294,-226.906336471008,
3.5961842657834));
#85627=CARTESIAN_POINT('Ctrl Pts',(-162.992028695687,-223.880295482423,
3.4374264005516));
#85628=CARTESIAN_POINT('Ctrl Pts',(-160.682189860438,-221.879008023352,
3.27866853531981));
#85629=CARTESIAN_POINT('Ctrl Pts',(-157.748010893835,-222.734052300533,
3.11991067008802));
#85630=CARTESIAN_POINT('Ctrl Pts',(-156.874852264295,-225.662891819106,
2.96115280485622));
#85631=CARTESIAN_POINT('Ctrl Pts',(-158.861828728588,-227.985052779313,
2.80239493962443));
#85632=CARTESIAN_POINT('Ctrl Pts',(-161.890459477026,-227.575293535821,
2.64363707439264));
#85633=CARTESIAN_POINT('Ctrl Pts',(-163.18894182522,-224.808625785839,2.48487920916085));
#85634=CARTESIAN_POINT('Ctrl Pts',(-161.568904659887,-222.217103633969,
2.32612134392905));
#85635=CARTESIAN_POINT('Ctrl Pts',(-158.513006178533,-222.172488282818,
2.16736347869726));
#85636=CARTESIAN_POINT('Ctrl Pts',(-156.81800403756,-224.71561122042,2.00860561346547));
#85637=CARTESIAN_POINT('Ctrl Pts',(-158.035165195383,-227.519007429433,
1.84984774823368));
#85638=CARTESIAN_POINT('Ctrl Pts',(-161.05054159698,-228.017006744663,1.69108988300188));
#85639=CARTESIAN_POINT('Ctrl Pts',(-163.104465466566,-225.7538444972,1.53233201777009));
#85640=CARTESIAN_POINT('Ctrl Pts',(-162.317176238485,-222.80075779587,1.3735741525383));
#85641=CARTESIAN_POINT('Ctrl Pts',(-159.409220739539,-221.860429922718,
1.21481628730651));
#85642=CARTESIAN_POINT('Ctrl Pts',(-157.04191873346,-223.793410627992,1.05605842207472));
#85643=CARTESIAN_POINT('Ctrl Pts',(-157.381909987635,-226.830715482678,
0.897300556842923));
#85644=CARTESIAN_POINT('Ctrl Pts',(-160.117858009173,-228.192438370269,
0.738542691611127));
#85645=CARTESIAN_POINT('Ctrl Pts',(-162.746189540825,-226.632672581258,
0.579784826379337));
#85646=CARTESIAN_POINT('Ctrl Pts',(-162.86069567705,-223.578205874871,0.421026961147545));
#85647=CARTESIAN_POINT('Ctrl Pts',(-160.358157726966,-221.825957897847,
0.26226909591575));
#85648=CARTESIAN_POINT('Ctrl Pts',(-157.525626832351,-222.976510157985,
0.103511230683962));
#85649=CARTESIAN_POINT('Ctrl Pts',(-156.962288097762,-225.983143426199,
-0.0552466345478338));
#85650=CARTESIAN_POINT('Ctrl Pts',(-158.43372769508,-227.379023915733,-0.161085211369028));
#85651=CARTESIAN_POINT('Ctrl Pts',(-159.301933573839,-227.611132185939,
-0.214004499779625));
#85652=CARTESIAN_POINT('Ctrl Pts',(-157.804802895981,-223.123136560921,
20.2140044997796));
#85653=CARTESIAN_POINT('Ctrl Pts',(-157.180742620438,-223.853043319762,
20.161085211369));
#85654=CARTESIAN_POINT('Ctrl Pts',(-156.729879173041,-225.972907029956,
20.0552466345478));
#85655=CARTESIAN_POINT('Ctrl Pts',(-159.045823488024,-228.27960122976,19.896488769316));
#85656=CARTESIAN_POINT('Ctrl Pts',(-162.236589360548,-227.57830865422,19.7377309040842));
#85657=CARTESIAN_POINT('Ctrl Pts',(-163.37974600956,-224.520518247638,19.5789730388525));
#85658=CARTESIAN_POINT('Ctrl Pts',(-161.430095714629,-221.900030936057,
19.4202151736207));
#85659=CARTESIAN_POINT('Ctrl Pts',(-158.171460220963,-222.117367443797,
19.2614573083889));
#85660=CARTESIAN_POINT('Ctrl Pts',(-156.586382213157,-224.972536314815,
19.1026994431571));
#85661=CARTESIAN_POINT('Ctrl Pts',(-158.125409506143,-227.853009993757,
18.9439415779253));
#85662=CARTESIAN_POINT('Ctrl Pts',(-161.380080048394,-228.122327090623,
18.7851837126935));
#85663=CARTESIAN_POINT('Ctrl Pts',(-163.371692660391,-225.534130049582,
18.6264258474617));
#85664=CARTESIAN_POINT('Ctrl Pts',(-162.277536486599,-222.457078175749,
18.4676679822299));
#85665=CARTESIAN_POINT('Ctrl Pts',(-159.09897698363,-221.707317427635,18.3089101169981));
#85666=CARTESIAN_POINT('Ctrl Pts',(-156.745034686285,-223.971015219991,
18.1501522517663));
#85667=CARTESIAN_POINT('Ctrl Pts',(-157.370036045468,-227.176441972781,
17.9913943865345));
#85668=CARTESIAN_POINT('Ctrl Pts',(-160.401980539204,-228.389988091059,
17.8326365213027));
#85669=CARTESIAN_POINT('Ctrl Pts',(-163.066032349974,-226.501017736455,
17.6738786560709));
#85670=CARTESIAN_POINT('Ctrl Pts',(-162.924051527288,-223.238315770043,
17.5151207908391));
#85671=CARTESIAN_POINT('Ctrl Pts',(-160.10597883643,-221.587907256516,17.3563629256074));
#85672=CARTESIAN_POINT('Ctrl Pts',(-157.190914330871,-223.060245832273,
17.1976050603756));
#85673=CARTESIAN_POINT('Ctrl Pts',(-156.84672491334,-226.307847372741,17.0388471951438));
#85674=CARTESIAN_POINT('Ctrl Pts',(-159.388412733961,-228.358507036245,
16.880089329912));
#85675=CARTESIAN_POINT('Ctrl Pts',(-162.489825195042,-227.335461198446,
16.7213314646802));
#85676=CARTESIAN_POINT('Ctrl Pts',(-163.312549736191,-224.175001360682,
16.5625735994484));
#85677=CARTESIAN_POINT('Ctrl Pts',(-161.103628888722,-221.769580246619,
16.4038157342166));
#85678=CARTESIAN_POINT('Ctrl Pts',(-157.884666925848,-222.320639163124,
16.2450578689848));
#85679=CARTESIAN_POINT('Ctrl Pts',(-156.60165770918,-225.323849012509,16.086300003753));
#85680=CARTESIAN_POINT('Ctrl Pts',(-158.42881122347,-228.03067225822,15.9275421385212));
#85681=CARTESIAN_POINT('Ctrl Pts',(-161.693916644237,-227.963824372464,
15.7687842732894));
#85682=CARTESIAN_POINT('Ctrl Pts',(-163.408749618819,-225.184484537541,
15.6100264080576));
#85683=CARTESIAN_POINT('Ctrl Pts',(-162.003895076299,-222.236304461133,
15.4512685428259));
#85684=CARTESIAN_POINT('Ctrl Pts',(-158.765075838754,-221.817458433208,
15.292510677594));
#85685=CARTESIAN_POINT('Ctrl Pts',(-156.656459145018,-224.311274322064,
15.1337528123623));
#85686=CARTESIAN_POINT('Ctrl Pts',(-157.60785091028,-227.435411924282,14.9749949471305));
#85687=CARTESIAN_POINT('Ctrl Pts',(-160.748537428385,-228.330660629168,
14.8162370818987));
#85688=CARTESIAN_POINT('Ctrl Pts',(-163.204162521467,-226.177688857214,
14.6574792166669));
#85689=CARTESIAN_POINT('Ctrl Pts',(-162.727338200903,-222.94689628945,14.4987213514351));
#85690=CARTESIAN_POINT('Ctrl Pts',(-159.754454066123,-221.595104156844,
14.3399634862033));
#85691=CARTESIAN_POINT('Ctrl Pts',(-157.00629356037,-223.359472566001,14.1812056209715));
#85692=CARTESIAN_POINT('Ctrl Pts',(-156.997973070443,-226.625251618241,
14.0224477557397));
#85693=CARTESIAN_POINT('Ctrl Pts',(-159.737107508394,-228.403600453379,
13.8636898905079));
#85694=CARTESIAN_POINT('Ctrl Pts',(-162.716841144325,-227.066974287427,
13.7049320252761));
#85695=CARTESIAN_POINT('Ctrl Pts',(-163.210121871807,-223.838653334904,
13.5461741600443));
#85696=CARTESIAN_POINT('Ctrl Pts',(-160.765499188446,-221.673196804608,
13.3874162948125));
#85697=CARTESIAN_POINT('Ctrl Pts',(-157.620291677922,-222.552430427911,
13.2286584295807));
#85698=CARTESIAN_POINT('Ctrl Pts',(-156.652993130184,-225.671679627342,
13.069900564349));
#85699=CARTESIAN_POINT('Ctrl Pts',(-158.748875138084,-228.176207658242,
12.9111426991172));
#85700=CARTESIAN_POINT('Ctrl Pts',(-161.98978657041,-227.773870565221,12.7523848338854));
#85701=CARTESIAN_POINT('Ctrl Pts',(-163.409645411744,-224.832887239989,
12.5936269686536));
#85702=CARTESIAN_POINT('Ctrl Pts',(-161.70899690633,-222.044845506148,12.4348691034218));
#85703=CARTESIAN_POINT('Ctrl Pts',(-158.444274499449,-221.961361048871,
12.27611123819));
#85704=CARTESIAN_POINT('Ctrl Pts',(-156.603352009494,-224.658838840176,
12.1173533729582));
#85705=CARTESIAN_POINT('Ctrl Pts',(-157.87104162688,-227.668547311536,11.9585955077264));
#85706=CARTESIAN_POINT('Ctrl Pts',(-161.087153863627,-228.236001388316,
11.7998376424946));
#85707=CARTESIAN_POINT('Ctrl Pts',(-163.308302927133,-225.841867121762,
11.6410797772628));
#85708=CARTESIAN_POINT('Ctrl Pts',(-162.501693281823,-222.677256098477,
11.482321912031));
#85709=CARTESIAN_POINT('Ctrl Pts',(-159.405534043365,-221.638420202526,
11.3235640467992));
#85710=CARTESIAN_POINT('Ctrl Pts',(-156.853430025042,-223.676102005032,
11.1648061815675));
#85711=CARTESIAN_POINT('Ctrl Pts',(-157.181066724065,-226.925415200472,
11.0060483163357));
#85712=CARTESIAN_POINT('Ctrl Pts',(-160.088591046371,-228.412588480155,
10.8472904511039));
#85713=CARTESIAN_POINT('Ctrl Pts',(-162.915036846522,-226.776560916997,
10.6885325858721));
#85714=CARTESIAN_POINT('Ctrl Pts',(-163.073641039367,-223.514624872465,
10.5297747206403));
#85715=CARTESIAN_POINT('Ctrl Pts',(-160.419249073851,-221.612104086242,
10.3710168554085));
#85716=CARTESIAN_POINT('Ctrl Pts',(-157.381160372433,-222.810185507065,
10.2122589901767));
#85717=CARTESIAN_POINT('Ctrl Pts',(-156.739833595181,-226.01238506571,10.0535011249449));
#85718=CARTESIAN_POINT('Ctrl Pts',(-159.082210983416,-228.288049852028,
9.89474325971311));
#85719=CARTESIAN_POINT('Ctrl Pts',(-162.264548843538,-227.554491543069,
9.73598539448133));
#85720=CARTESIAN_POINT('Ctrl Pts',(-163.374371691105,-224.483062674347,
9.57722752924952));
#85721=CARTESIAN_POINT('Ctrl Pts',(-161.395969699666,-221.884734825734,
9.41846966401773));
#85722=CARTESIAN_POINT('Ctrl Pts',(-158.139976293989,-222.137497542104,
9.25971179878595));
#85723=CARTESIAN_POINT('Ctrl Pts',(-156.586276510909,-225.010022395376,
9.10095393355415));
#85724=CARTESIAN_POINT('Ctrl Pts',(-158.156816330804,-227.873374752793,
8.94219606832236));
#85725=CARTESIAN_POINT('Ctrl Pts',(-161.414237772266,-228.107014649447,
8.78343820309056));
#85726=CARTESIAN_POINT('Ctrl Pts',(-163.377348860164,-225.497114861107,
8.62468033785877));
#85727=CARTESIAN_POINT('Ctrl Pts',(-162.249510404051,-222.432255571431,
8.46592247262698));
#85728=CARTESIAN_POINT('Ctrl Pts',(-159.062920114611,-221.717395881806,
8.30716460739519));
#85729=CARTESIAN_POINT('Ctrl Pts',(-156.733945299429,-224.006775352068,
8.1484067421634));
#85730=CARTESIAN_POINT('Ctrl Pts',(-157.394063617775,-227.205153981059,
7.9896488769316));
#85731=CARTESIAN_POINT('Ctrl Pts',(-160.439134810658,-228.385375773301,
7.83089101169981));
#85732=CARTESIAN_POINT('Ctrl Pts',(-163.082309842095,-226.467301790944,
7.67213314646802));
#85733=CARTESIAN_POINT('Ctrl Pts',(-162.904555027255,-223.206353267216,
7.51337528123622));
#85734=CARTESIAN_POINT('Ctrl Pts',(-160.068551565691,-221.586950162798,
7.35461741600443));
#85735=CARTESIAN_POINT('Ctrl Pts',(-157.169809713902,-223.091170135173,
7.19585955077264));
#85736=CARTESIAN_POINT('Ctrl Pts',(-156.861257900655,-226.342351124774,
7.03710168554085));
#85737=CARTESIAN_POINT('Ctrl Pts',(-159.425282733301,-228.365012417769,
6.87834382030906));
#85738=CARTESIAN_POINT('Ctrl Pts',(-162.51528878583,-227.308014478348,6.71958595507726));
#85739=CARTESIAN_POINT('Ctrl Pts',(-163.303302640478,-224.138721779103,
6.56082808984547));
#85740=CARTESIAN_POINT('Ctrl Pts',(-161.06813404846,-221.757670873754,6.40207022461368));
#85741=CARTESIAN_POINT('Ctrl Pts',(-157.855409217295,-222.343999457244,
6.24331235938189));
#85742=CARTESIAN_POINT('Ctrl Pts',(-156.605413786127,-225.36109963302,6.08455449415009));
#85743=CARTESIAN_POINT('Ctrl Pts',(-158.462143524407,-228.047721438856,
5.9257966289183));
#85744=CARTESIAN_POINT('Ctrl Pts',(-161.726319448675,-227.945068703699,
5.76703876368651));
#85745=CARTESIAN_POINT('Ctrl Pts',(-163.410567881401,-225.14708920673,5.60828089845471));
#85746=CARTESIAN_POINT('Ctrl Pts',(-161.973464723187,-222.214493673545,
5.44952303322292));
#85747=CARTESIAN_POINT('Ctrl Pts',(-158.730246727916,-221.831193420794,
5.29076516799113));
#85748=CARTESIAN_POINT('Ctrl Pts',(-156.649106877325,-224.347984824723,
5.13200730275933));
#85749=CARTESIAN_POINT('Ctrl Pts',(-157.634704280835,-227.461500491424,
4.97324943752755));
#85750=CARTESIAN_POINT('Ctrl Pts',(-160.785020233513,-228.322251005172,
4.81449157229575));
#85751=CARTESIAN_POINT('Ctrl Pts',(-163.216885699347,-226.142477529628,
4.65573370706396));
#85752=CARTESIAN_POINT('Ctrl Pts',(-162.704657499646,-222.917108663901,
4.49697584183216));
#85753=CARTESIAN_POINT('Ctrl Pts',(-159.717126862614,-221.598001867052,
4.33821797660038));
#85754=CARTESIAN_POINT('Ctrl Pts',(-156.988481709821,-223.392403627723,
4.17946011136858));
#85755=CARTESIAN_POINT('Ctrl Pts',(-157.015977977717,-226.65807752503,4.02070224613679));
#85756=CARTESIAN_POINT('Ctrl Pts',(-159.774451083183,-228.406278936745,
3.861944380905));
#85757=CARTESIAN_POINT('Ctrl Pts',(-162.7393465482,-227.037053999266,3.70318651567321));
#85758=CARTESIAN_POINT('Ctrl Pts',(-163.197192160546,-223.803517322249,
3.54442865044141));
#85759=CARTESIAN_POINT('Ctrl Pts',(-160.728967632209,-221.665001543853,
3.38567078520962));
#85760=CARTESIAN_POINT('Ctrl Pts',(-157.593591957777,-222.578676223465,
3.22691291997783));
#85761=CARTESIAN_POINT('Ctrl Pts',(-156.660560824318,-225.708346323814,
3.06815505474603));
#85762=CARTESIAN_POINT('Ctrl Pts',(-158.78378430275,-228.189737905452,2.90939718951424));
#85763=CARTESIAN_POINT('Ctrl Pts',(-162.020088319504,-227.751881462801,
2.75063932428245));
#85764=CARTESIAN_POINT('Ctrl Pts',(-163.407607627134,-224.795503252315,
2.59188145905066));
#85765=CARTESIAN_POINT('Ctrl Pts',(-161.676484482407,-222.026280376954,
2.43312359381886));
#85766=CARTESIAN_POINT('Ctrl Pts',(-158.41104298377,-221.978605750321,2.27436572858707));
#85767=CARTESIAN_POINT('Ctrl Pts',(-156.599814513589,-224.696110676368,
2.11560786335528));
#85768=CARTESIAN_POINT('Ctrl Pts',(-157.900436435271,-227.691735817022,
1.95684999812349));
#85769=CARTESIAN_POINT('Ctrl Pts',(-161.122577254367,-228.223882954817,
1.7980921328917));
#85770=CARTESIAN_POINT('Ctrl Pts',(-163.317338722953,-225.805535628783,
1.6393342676599));
#85771=CARTESIAN_POINT('Ctrl Pts',(-162.476065057453,-222.649955715892,
1.48057640242811));
#85772=CARTESIAN_POINT('Ctrl Pts',(-159.368710994356,-221.645149542503,
1.32181853719632));
#85773=CARTESIAN_POINT('Ctrl Pts',(-156.839083044467,-223.710674771688,
1.16306067196453));
#85774=CARTESIAN_POINT('Ctrl Pts',(-157.20238750544,-226.956247678321,1.00430280673273));
#85775=CARTESIAN_POINT('Ctrl Pts',(-160.125939535115,-228.411343930344,
0.845544941500937));
#85776=CARTESIAN_POINT('Ctrl Pts',(-162.934495810134,-226.744624971365,
0.686787076269146));
#85777=CARTESIAN_POINT('Ctrl Pts',(-163.05685363431,-223.480713424532,0.528029211037356));
#85778=CARTESIAN_POINT('Ctrl Pts',(-160.38271660915,-221.608313770228,0.36927134580556));
#85779=CARTESIAN_POINT('Ctrl Pts',(-157.355959016946,-222.837759420837,
0.210513480573772));
#85780=CARTESIAN_POINT('Ctrl Pts',(-156.753992134557,-226.050557589728,
0.0517556153419762));
#85781=CARTESIAN_POINT('Ctrl Pts',(-158.326328373192,-227.542153631111,
-0.0540829614792177));
#85782=CARTESIAN_POINT('Ctrl Pts',(-159.254067145653,-227.790177569842,
-0.107002249889815));
#85783=CARTESIAN_POINT('Ctrl Pts',(-157.663937342304,-223.002698443069,
20.3210067496694));
#85784=CARTESIAN_POINT('Ctrl Pts',(-156.999831188384,-223.779443237332,
20.2680874612588));
#85785=CARTESIAN_POINT('Ctrl Pts',(-156.520035883781,-226.035338365711,
20.1622488844376));
#85786=CARTESIAN_POINT('Ctrl Pts',(-158.984594087522,-228.490052875411,
20.0034910192058));
#85787=CARTESIAN_POINT('Ctrl Pts',(-162.380111050717,-227.743758433405,
19.844733153974));
#85788=CARTESIAN_POINT('Ctrl Pts',(-163.596623934578,-224.489749956991,
19.6859752887423));
#85789=CARTESIAN_POINT('Ctrl Pts',(-161.521864797362,-221.70110626648,19.5272174235105));
#85790=CARTESIAN_POINT('Ctrl Pts',(-158.054123026994,-221.932389233715,
19.3684595582787));
#85791=CARTESIAN_POINT('Ctrl Pts',(-156.367330739964,-224.970773973196,
19.2097016930469));
#85792=CARTESIAN_POINT('Ctrl Pts',(-158.005117242933,-228.036087327305,
19.0509438278151));
#85793=CARTESIAN_POINT('Ctrl Pts',(-161.468639631394,-228.322686472282,
18.8921859625833));
#85794=CARTESIAN_POINT('Ctrl Pts',(-163.58805380289,-225.568405115375,18.7334280973515));
#85795=CARTESIAN_POINT('Ctrl Pts',(-162.423685749286,-222.293899165502,
18.5746702321197));
#85796=CARTESIAN_POINT('Ctrl Pts',(-159.04115843702,-221.496026353686,18.4159123668879));
#85797=CARTESIAN_POINT('Ctrl Pts',(-156.536163924622,-223.90498538126,18.2571545016561));
#85798=CARTESIAN_POINT('Ctrl Pts',(-157.201271551415,-227.316104011775,
18.0983966364243));
#85799=CARTESIAN_POINT('Ctrl Pts',(-160.427775585634,-228.607523249306,
17.9396387711926));
#85800=CARTESIAN_POINT('Ctrl Pts',(-163.262779304396,-226.597337877429,
17.7808809059607));
#85801=CARTESIAN_POINT('Ctrl Pts',(-163.111687588131,-223.125268689213,
17.622123040729));
#85802=CARTESIAN_POINT('Ctrl Pts',(-160.11277948656,-221.368953645186,17.4633651754972));
#85803=CARTESIAN_POINT('Ctrl Pts',(-157.010655616342,-222.935772023368,
17.3046073102654));
#85804=CARTESIAN_POINT('Ctrl Pts',(-156.644379602221,-226.39177179299,17.1458494450336));
#85805=CARTESIAN_POINT('Ctrl Pts',(-159.349167247214,-228.574022058711,
16.9870915798018));
#85806=CARTESIAN_POINT('Ctrl Pts',(-162.649597000506,-227.48532748344,16.82833371457));
#85807=CARTESIAN_POINT('Ctrl Pts',(-163.52511568383,-224.12206128988,16.6695758493382));
#85808=CARTESIAN_POINT('Ctrl Pts',(-161.174448631596,-221.562284570829,
16.5108179841064));
#85809=CARTESIAN_POINT('Ctrl Pts',(-157.748926238073,-222.148704876632,
16.3520601188746));
#85810=CARTESIAN_POINT('Ctrl Pts',(-156.383586462865,-225.344630367573,
16.1933022536428));
#85811=CARTESIAN_POINT('Ctrl Pts',(-158.327988214669,-228.225150159492,
16.034544388411));
#85812=CARTESIAN_POINT('Ctrl Pts',(-161.80261508664,-228.154012652352,15.8757865231792));
#85813=CARTESIAN_POINT('Ctrl Pts',(-163.627488702212,-225.196322889768,
15.7170286579475));
#85814=CARTESIAN_POINT('Ctrl Pts',(-162.132484800163,-222.058958426208,
15.5582707927157));
#85815=CARTESIAN_POINT('Ctrl Pts',(-158.685830892865,-221.613235095319,
15.3995129274839));
#85816=CARTESIAN_POINT('Ctrl Pts',(-156.441904500737,-224.267078872017,
15.2407550622521));
#85817=CARTESIAN_POINT('Ctrl Pts',(-157.454346969616,-227.591692036222,
15.0819971970203));
#85818=CARTESIAN_POINT('Ctrl Pts',(-160.796570991797,-228.544388750793,
14.9232393317885));
#85819=CARTESIAN_POINT('Ctrl Pts',(-163.409773273609,-226.253261020018,
14.7644814665567));
#85820=CARTESIAN_POINT('Ctrl Pts',(-162.902351189501,-222.815148853006,
14.6057236013249));
#85821=CARTESIAN_POINT('Ctrl Pts',(-159.738697410893,-221.376612369806,
14.4469657360931));
#85822=CARTESIAN_POINT('Ctrl Pts',(-156.814187751561,-223.254200103273,
14.2882078708613));
#85823=CARTESIAN_POINT('Ctrl Pts',(-156.805333336721,-226.729543833573,
14.1294500056295));
#85824=CARTESIAN_POINT('Ctrl Pts',(-159.720237726487,-228.622009115399,
13.9706921403977));
#85825=CARTESIAN_POINT('Ctrl Pts',(-162.891180537971,-227.199611797244,
13.8119342751659));
#85826=CARTESIAN_POINT('Ctrl Pts',(-163.416115034797,-223.764129848749,
13.6531764099341));
#85827=CARTESIAN_POINT('Ctrl Pts',(-160.814621186112,-221.459716214079,
13.4944185447024));
#85828=CARTESIAN_POINT('Ctrl Pts',(-157.467586059932,-222.395370161066,
13.3356606794706));
#85829=CARTESIAN_POINT('Ctrl Pts',(-156.438216072117,-225.714781234221,
13.1769028142388));
#85830=CARTESIAN_POINT('Ctrl Pts',(-158.668590595037,-228.380024549925,
13.018144949007));
#85831=CARTESIAN_POINT('Ctrl Pts',(-162.117470953023,-227.951869530454,
12.8593870837752));
#85832=CARTESIAN_POINT('Ctrl Pts',(-163.628441978069,-224.822163632791,
12.7006292185434));
#85833=CARTESIAN_POINT('Ctrl Pts',(-161.818663047472,-221.855213571405,
12.5418713533116));
#85834=CARTESIAN_POINT('Ctrl Pts',(-158.344443767345,-221.766371925803,
12.3831134880798));
#85835=CARTESIAN_POINT('Ctrl Pts',(-156.385389486241,-224.636946566547,
12.224355622848));
#85836=CARTESIAN_POINT('Ctrl Pts',(-157.734426605188,-227.839787695311,
12.0655977576162));
#85837=CARTESIAN_POINT('Ctrl Pts',(-161.156916405975,-228.443655236998,
11.9068398923844));
#85838=CARTESIAN_POINT('Ctrl Pts',(-163.520596357509,-225.895889641203,
11.7480820271526));
#85839=CARTESIAN_POINT('Ctrl Pts',(-162.662226661094,-222.528205881009,
11.5893241619208));
#85840=CARTESIAN_POINT('Ctrl Pts',(-159.367387229136,-221.422708001315,
11.4305662966891));
#85841=CARTESIAN_POINT('Ctrl Pts',(-156.651514980196,-223.591147618143,
11.2718084314573));
#85842=CARTESIAN_POINT('Ctrl Pts',(-157.000176089704,-227.048968879445,
11.1130505662255));
#85843=CARTESIAN_POINT('Ctrl Pts',(-160.09427592395,-228.631573902853,10.9542927009937));
#85844=CARTESIAN_POINT('Ctrl Pts',(-163.102094436304,-226.890562633178,
10.7955348357619));
#85845=CARTESIAN_POINT('Ctrl Pts',(-163.27087624254,-223.419308515963,10.6367769705301));
#85846=CARTESIAN_POINT('Ctrl Pts',(-160.446152240227,-221.39470318278,10.4780191052983));
#85847=CARTESIAN_POINT('Ctrl Pts',(-157.213109725203,-222.669665354942,
10.3192612400665));
#85848=CARTESIAN_POINT('Ctrl Pts',(-156.530629080082,-226.077349702623,
10.1605033748347));
#85849=CARTESIAN_POINT('Ctrl Pts',(-159.02331656444,-228.499043644829,10.0017455096029));
#85850=CARTESIAN_POINT('Ctrl Pts',(-162.409864690616,-227.718412980884,
9.84298764437113));
#85851=CARTESIAN_POINT('Ctrl Pts',(-163.590904746706,-224.449890863733,
9.68422977913934));
#85852=CARTESIAN_POINT('Ctrl Pts',(-161.48554891982,-221.684828606461,9.52547191390754));
#85853=CARTESIAN_POINT('Ctrl Pts',(-158.020618779932,-221.953811078189,
9.36671404867575));
#85854=CARTESIAN_POINT('Ctrl Pts',(-156.367218254814,-225.010665531371,
9.20795618344397));
#85855=CARTESIAN_POINT('Ctrl Pts',(-158.038539440034,-228.057758890661,
9.04919831821217));
#85856=CARTESIAN_POINT('Ctrl Pts',(-161.504989252603,-228.306391433462,
8.89044045298037));
#85857=CARTESIAN_POINT('Ctrl Pts',(-163.594072960372,-225.529014666379,
8.73168258774858));
#85858=CARTESIAN_POINT('Ctrl Pts',(-162.393861236142,-222.267483697429,
8.5729247225168));
#85859=CARTESIAN_POINT('Ctrl Pts',(-159.002787802732,-221.506751541139,
8.41416685728499));
#85860=CARTESIAN_POINT('Ctrl Pts',(-156.524362933047,-223.943040237029,
8.25540899205321));
#85861=CARTESIAN_POINT('Ctrl Pts',(-157.226840970362,-227.346658466427,
8.09665112682141));
#85862=CARTESIAN_POINT('Ctrl Pts',(-160.46731404255,-228.602614959631,7.93789326158962));
#85863=CARTESIAN_POINT('Ctrl Pts',(-163.280101321373,-226.56145838345,7.77913539635782));
#85864=CARTESIAN_POINT('Ctrl Pts',(-163.090939999863,-223.091255156139,
7.62037753112604));
#85865=CARTESIAN_POINT('Ctrl Pts',(-160.072950512026,-221.36793513487,7.46161966589424));
#85866=CARTESIAN_POINT('Ctrl Pts',(-156.988196718452,-222.968680735341,
7.30286180066245));
#85867=CARTESIAN_POINT('Ctrl Pts',(-156.659845169714,-226.428489646948,
7.14410393543065));
#85868=CARTESIAN_POINT('Ctrl Pts',(-159.388403190305,-228.580944889843,
6.98534607019887));
#85869=CARTESIAN_POINT('Ctrl Pts',(-162.676694587079,-227.45611951037,6.82658820496707));
#85870=CARTESIAN_POINT('Ctrl Pts',(-163.515275203016,-224.083453651592,
6.66783033973528));
#85871=CARTESIAN_POINT('Ctrl Pts',(-161.136676091388,-221.549610974834,
6.50907247450348));
#85872=CARTESIAN_POINT('Ctrl Pts',(-157.71779106562,-222.173564198225,6.3503146092717));
#85873=CARTESIAN_POINT('Ctrl Pts',(-156.387583566852,-225.384271356254,
6.1915567440399));
#85874=CARTESIAN_POINT('Ctrl Pts',(-158.363459445645,-228.24329338415,6.03279887880811));
#85875=CARTESIAN_POINT('Ctrl Pts',(-161.837097175429,-228.134053434412,
5.87404101357632));
#85876=CARTESIAN_POINT('Ctrl Pts',(-163.629423642502,-225.156527904744,
5.71528314834452));
#85877=CARTESIAN_POINT('Ctrl Pts',(-162.100101734681,-222.03574804281,5.55652528311273));
#85878=CARTESIAN_POINT('Ctrl Pts',(-158.648766801864,-221.627851455529,
5.39776741788094));
#85879=CARTESIAN_POINT('Ctrl Pts',(-156.434080438846,-224.306145083543,
5.23900955264915));
#85880=CARTESIAN_POINT('Ctrl Pts',(-157.482923517968,-227.619454703812,
5.08025168741736));
#85881=CARTESIAN_POINT('Ctrl Pts',(-160.835394894467,-228.535439482161,
4.92149382218556));
#85882=CARTESIAN_POINT('Ctrl Pts',(-163.423312896397,-226.215790185461,
4.76273595695377));
#85883=CARTESIAN_POINT('Ctrl Pts',(-162.87821507017,-222.783449758844,4.60397809172198));
#85884=CARTESIAN_POINT('Ctrl Pts',(-159.698974924892,-221.379696025755,
4.44522022649019));
#85885=CARTESIAN_POINT('Ctrl Pts',(-156.795232916545,-223.289244347558,
4.28646236125839));
#85886=CARTESIAN_POINT('Ctrl Pts',(-156.82449361689,-226.764476175145,4.1277044960266));
#85887=CARTESIAN_POINT('Ctrl Pts',(-159.759977634311,-228.624859476745,
3.96894663079481));
#85888=CARTESIAN_POINT('Ctrl Pts',(-162.915130111106,-227.167771527524,
3.81018876556301));
#85889=CARTESIAN_POINT('Ctrl Pts',(-163.402355625404,-223.726739162074,
3.65143090033122));
#85890=CARTESIAN_POINT('Ctrl Pts',(-160.77574540398,-221.450995064354,3.49267303509943));
#85891=CARTESIAN_POINT('Ctrl Pts',(-157.439173021718,-222.423300146398,
3.33391516986764));
#85892=CARTESIAN_POINT('Ctrl Pts',(-156.446269384341,-225.753800828521,
3.17515730463584));
#85893=CARTESIAN_POINT('Ctrl Pts',(-158.705739876912,-228.394423031591,
3.01639943940405));
#85894=CARTESIAN_POINT('Ctrl Pts',(-162.149717161981,-227.928469389781,
2.85764157417226));
#85895=CARTESIAN_POINT('Ctrl Pts',(-163.626273429048,-224.782380718792,
2.69888370894047));
#85896=CARTESIAN_POINT('Ctrl Pts',(-161.784064304926,-221.835457119938,
2.54012584370867));
#85897=CARTESIAN_POINT('Ctrl Pts',(-158.309079789007,-221.784723217824,
2.38136797847688));
#85898=CARTESIAN_POINT('Ctrl Pts',(-156.381624989618,-224.676610132315,
2.22261011324509));
#85899=CARTESIAN_POINT('Ctrl Pts',(-157.765707675159,-227.864464204611,
2.0638522480133));
#85900=CARTESIAN_POINT('Ctrl Pts',(-161.194612911753,-228.430759164971,
1.90509438278151));
#85901=CARTESIAN_POINT('Ctrl Pts',(-163.53021197934,-225.857226760367,1.74633651754971));
#85902=CARTESIAN_POINT('Ctrl Pts',(-162.63495387642,-222.499153635915,1.58757865231792));
#85903=CARTESIAN_POINT('Ctrl Pts',(-159.328201249173,-221.429869162289,
1.42882078708612));
#85904=CARTESIAN_POINT('Ctrl Pts',(-156.636247355474,-223.627938915385,
1.27006292185434));
#85905=CARTESIAN_POINT('Ctrl Pts',(-157.022865023245,-227.081779873964,
1.11130505662254));
#85906=CARTESIAN_POINT('Ctrl Pts',(-160.134021061057,-228.63024949042,0.952547191390747));
#85907=CARTESIAN_POINT('Ctrl Pts',(-163.122802079444,-226.856577361471,
0.793789326158957));
#85908=CARTESIAN_POINT('Ctrl Pts',(-163.253011591569,-223.383220974194,
0.635031460927165));
#85909=CARTESIAN_POINT('Ctrl Pts',(-160.407275491335,-221.390669642609,
0.47627359569537));
#85910=CARTESIAN_POINT('Ctrl Pts',(-157.18629120154,-222.69900868369,0.317515730463582));
#85911=CARTESIAN_POINT('Ctrl Pts',(-156.545696171353,-226.117971753255,
0.158757865231786));
#85912=CARTESIAN_POINT('Ctrl Pts',(-158.218929051303,-227.70528334649,0.0529192884105924));
#85913=CARTESIAN_POINT('Ctrl Pts',(-159.206200717467,-227.969222953746,
-4.44089209850063E-15));
#85914=CARTESIAN_POINT('Ctrl Pts',(-159.206200717467,-227.969222953746,
-4.44089209850063E-15));
#85915=CARTESIAN_POINT('Ctrl Pts',(-159.113164853268,-227.935190019033,
-4.15823203790848E-15));
#85916=CARTESIAN_POINT('Ctrl Pts',(-159.022195992629,-227.896385128928,
-5.66635079944646E-15));
#85917=CARTESIAN_POINT('Ctrl Pts',(-158.933501676326,-227.853137676309,
-5.99520433297585E-15));
#85918=CARTESIAN_POINT('Ctrl Pts',(-158.842829036744,-227.808925590939,
-6.33139293179453E-15));
#85919=CARTESIAN_POINT('Ctrl Pts',(-158.754532873528,-227.760069932939,
-5.08640997726718E-15));
#85920=CARTESIAN_POINT('Ctrl Pts',(-158.668863854363,-227.706877060488,
-4.6074255521944E-15));
#85921=CARTESIAN_POINT('Ctrl Pts',(-158.585928616916,-227.655381624328,
-4.14372598595588E-15));
#85922=CARTESIAN_POINT('Ctrl Pts',(-158.505455204851,-227.59982050253,-6.97772062172547E-16));
#85923=CARTESIAN_POINT('Ctrl Pts',(-158.427704734505,-227.540440966992,
1.16573417585641E-15));
#85924=CARTESIAN_POINT('Ctrl Pts',(-158.359673072952,-227.488483873397,
2.79630213413175E-15));
#85925=CARTESIAN_POINT('Ctrl Pts',(-158.29372646032,-227.433602589581,-2.63172470389904E-15));
#85926=CARTESIAN_POINT('Ctrl Pts',(-158.230065068767,-227.375949804433,
-3.1641356201817E-15));
#85927=CARTESIAN_POINT('Ctrl Pts',(-158.216686274063,-227.363833751708,
-3.2760247286858E-15));
#85928=CARTESIAN_POINT('Ctrl Pts',(-158.203406590895,-227.351593348083,
3.2015646022047E-15));
#85929=CARTESIAN_POINT('Ctrl Pts',(-158.190245171691,-227.339246427072,
2.99760216648792E-15));
#85930=CARTESIAN_POINT('Ctrl Pts',(-158.117820261348,-227.271303553023,
1.8752337583938E-15));
#85931=CARTESIAN_POINT('Ctrl Pts',(-158.048861110802,-227.200038557941,
-1.25208198436776E-15));
#85932=CARTESIAN_POINT('Ctrl Pts',(-157.983606937581,-227.125743461044,
-1.36002320516582E-15));
#85933=CARTESIAN_POINT('Ctrl Pts',(-157.918710403508,-227.051855553971,
-1.46737283151989E-15));
#85934=CARTESIAN_POINT('Ctrl Pts',(-157.857477860833,-226.974969868741,
-3.36873373652266E-15));
#85935=CARTESIAN_POINT('Ctrl Pts',(-157.800188235161,-226.895346902578,
-3.80251385934116E-15));
#85936=CARTESIAN_POINT('Ctrl Pts',(-157.744357521391,-226.817751579147,
-4.22524753218019E-15));
#85937=CARTESIAN_POINT('Ctrl Pts',(-157.692271198614,-226.737555871033,
-4.98425732962394E-15));
#85938=CARTESIAN_POINT('Ctrl Pts',(-157.644234215362,-226.654986798192,
-4.69069227904129E-15));
#85939=CARTESIAN_POINT('Ctrl Pts',(-157.623520326731,-226.619382427072,
-4.56410494253316E-15));
#85940=CARTESIAN_POINT('Ctrl Pts',(-157.603559993929,-226.583336637164,
-9.73322648313371E-15));
#85941=CARTESIAN_POINT('Ctrl Pts',(-157.584380642184,-226.546867300965,
-1.06303854607859E-14));
#85942=CARTESIAN_POINT('Ctrl Pts',(-157.571170306177,-226.521747985591,
-1.12483297846706E-14));
#85943=CARTESIAN_POINT('Ctrl Pts',(-157.558330518607,-226.496427729856,
3.35764189332899E-15));
#85944=CARTESIAN_POINT('Ctrl Pts',(-157.545870771917,-226.47091237078,4.05231403988182E-15));
#85945=CARTESIAN_POINT('Ctrl Pts',(-157.539658128808,-226.458189975719,
4.39868947045594E-15));
#85946=CARTESIAN_POINT('Ctrl Pts',(-157.533540525665,-226.445420051201,
-7.52285493344474E-16));
#85947=CARTESIAN_POINT('Ctrl Pts',(-157.527524328383,-226.432614845812,
-1.0547118733939E-15));
#85948=CARTESIAN_POINT('Ctrl Pts',(-157.48732379761,-226.34704982372,-3.0755400524729E-15));
#85949=CARTESIAN_POINT('Ctrl Pts',(-157.451579868608,-226.259774598662,
-4.13920845915888E-15));
#85950=CARTESIAN_POINT('Ctrl Pts',(-157.42054357986,-226.17102724452,-5.19029264012261E-15));
#85951=CARTESIAN_POINT('Ctrl Pts',(-157.390193323743,-226.084241580497,
-6.21814343603167E-15));
#85952=CARTESIAN_POINT('Ctrl Pts',(-157.364344673472,-225.996047472969,
-2.30602227738755E-15));
#85953=CARTESIAN_POINT('Ctrl Pts',(-157.343281522306,-225.906658800827,
-1.83186799063151E-15));
#85954=CARTESIAN_POINT('Ctrl Pts',(-157.33965861153,-225.891283742224,-1.75031235532725E-15));
#85955=CARTESIAN_POINT('Ctrl Pts',(-157.336177403255,-225.875873335079,
-1.11974478500717E-14));
#85956=CARTESIAN_POINT('Ctrl Pts',(-157.332839500122,-225.860428662792,
-1.13520304267922E-14));
#85957=CARTESIAN_POINT('Ctrl Pts',(-157.312711908479,-225.767297123485,
-1.22863078582233E-14));
#85958=CARTESIAN_POINT('Ctrl Pts',(-157.297790949491,-225.672918626754,
-2.72065433198562E-15));
#85959=CARTESIAN_POINT('Ctrl Pts',(-157.287998321733,-225.577701310259,
-2.55351295663786E-15));
#85960=CARTESIAN_POINT('Ctrl Pts',(-157.284735624775,-225.545976909347,
-2.49782497680672E-15));
#85961=CARTESIAN_POINT('Ctrl Pts',(-157.282042626464,-225.514159512456,
-7.4552035416634E-15));
#85962=CARTESIAN_POINT('Ctrl Pts',(-157.27991762978,-225.482264673585,-8.13238365537927E-15));
#85963=CARTESIAN_POINT('Ctrl Pts',(-157.278692828001,-225.463881183537,
-8.52269551529948E-15));
#85964=CARTESIAN_POINT('Ctrl Pts',(-157.277656733797,-225.445471971603,
-5.44258673003032E-15));
#85965=CARTESIAN_POINT('Ctrl Pts',(-157.276809107702,-225.427040064452,
-5.13478148889135E-15));
#85966=CARTESIAN_POINT('Ctrl Pts',(-157.27623458174,-225.41454680917,-4.92614928261313E-15));
#85967=CARTESIAN_POINT('Ctrl Pts',(-157.275746761203,-225.402044751541,
-4.56125519357613E-15));
#85968=CARTESIAN_POINT('Ctrl Pts',(-157.27534569061,-225.389544220778,-4.52415882534751E-15));
#85969=CARTESIAN_POINT('Ctrl Pts',(-157.272356045913,-225.296363254102,
-4.24763653062282E-15));
#85970=CARTESIAN_POINT('Ctrl Pts',(-157.274175073836,-225.203121070918,
-5.75556499322864E-15));
#85971=CARTESIAN_POINT('Ctrl Pts',(-157.280663972965,-225.11019208928,-6.96664947952286E-15));
#85972=CARTESIAN_POINT('Ctrl Pts',(-157.287165723555,-225.017079059002,
-8.18013255502608E-15));
#85973=CARTESIAN_POINT('Ctrl Pts',(-157.298356244342,-224.924279492042,
-6.82012577763791E-15));
#85974=CARTESIAN_POINT('Ctrl Pts',(-157.314146942062,-224.832182066588,
-6.50868248186498E-15));
#85975=CARTESIAN_POINT('Ctrl Pts',(-157.329715012396,-224.741383089712,
-6.20163011344484E-15));
#85976=CARTESIAN_POINT('Ctrl Pts',(-157.349754928696,-224.651265749557,
-6.37045444938708E-15));
#85977=CARTESIAN_POINT('Ctrl Pts',(-157.374224841053,-224.562227675715,
-8.40993941153556E-15));
#85978=CARTESIAN_POINT('Ctrl Pts',(-157.383741679345,-224.527598988116,
-9.20313590120162E-15));
#85979=CARTESIAN_POINT('Ctrl Pts',(-157.393929021839,-224.493133887988,
-9.22030469681423E-15));
#85980=CARTESIAN_POINT('Ctrl Pts',(-157.404785975198,-224.458857230651,
-9.67281810204668E-15));
#85981=CARTESIAN_POINT('Ctrl Pts',(-157.410769888121,-224.439965325527,
-9.92222516164008E-15));
#85982=CARTESIAN_POINT('Ctrl Pts',(-157.416957228107,-224.421130681043,
-1.27377712901384E-14));
#85983=CARTESIAN_POINT('Ctrl Pts',(-157.423347951588,-224.402357585388,
-1.29757316003065E-14));
#85984=CARTESIAN_POINT('Ctrl Pts',(-157.428583915131,-224.38697665947,-1.3170694113126E-14));
#85985=CARTESIAN_POINT('Ctrl Pts',(-157.433956678714,-224.371636528744,
-1.35354925628854E-14));
#85986=CARTESIAN_POINT('Ctrl Pts',(-157.439460724043,-224.356354233907,
-1.27953203588049E-14));
#85987=CARTESIAN_POINT('Ctrl Pts',(-157.471855748141,-224.266407607404,
-8.438907038856E-15));
#85988=CARTESIAN_POINT('Ctrl Pts',(-157.508835731473,-224.178337278242,
-9.18892624322844E-15));
#85989=CARTESIAN_POINT('Ctrl Pts',(-157.550328055791,-224.092586094792,
-7.72298891504875E-15));
#85990=CARTESIAN_POINT('Ctrl Pts',(-157.581447299029,-224.028272707204,
-6.62353591891397E-15));
#85991=CARTESIAN_POINT('Ctrl Pts',(-157.615105879293,-223.965264374664,
-8.64296102576464E-15));
#85992=CARTESIAN_POINT('Ctrl Pts',(-157.651290488186,-223.90376501913,-7.66053886991358E-15));
#85993=CARTESIAN_POINT('Ctrl Pts',(-157.665717481941,-223.879244902832,
-7.26884199267624E-15));
#85994=CARTESIAN_POINT('Ctrl Pts',(-157.680546182159,-223.854964851476,
-4.75898920195301E-15));
#85995=CARTESIAN_POINT('Ctrl Pts',(-157.695776333974,-223.830938597538,
-3.14331893846997E-15));
#85996=CARTESIAN_POINT('Ctrl Pts',(-157.706205612398,-223.814485938704,
-2.03694290071405E-15));
#85997=CARTESIAN_POINT('Ctrl Pts',(-157.716818754359,-223.798159331959,
-6.56110042008239E-15));
#85998=CARTESIAN_POINT('Ctrl Pts',(-157.727611295651,-223.781968701565,
-6.58501031480796E-15));
#85999=CARTESIAN_POINT('Ctrl Pts',(-157.775201002763,-223.710576122415,
-6.69044098737037E-15));
#86000=CARTESIAN_POINT('Ctrl Pts',(-157.826299872079,-223.641787294174,
-3.28198090435521E-15));
#86001=CARTESIAN_POINT('Ctrl Pts',(-157.880874030867,-223.575954690689,
-3.53883589099269E-16));
#86002=CARTESIAN_POINT('Ctrl Pts',(-157.931842788648,-223.514471268944,
2.38077116575345E-15));
#86003=CARTESIAN_POINT('Ctrl Pts',(-157.985843340743,-223.455566244336,
-2.7573366700933E-15));
#86004=CARTESIAN_POINT('Ctrl Pts',(-158.04287080899,-223.399561029707,-6.05418493115906E-16));
#86005=CARTESIAN_POINT('Ctrl Pts',(-158.056034841079,-223.38663297126,-1.05207374013562E-16));
#86006=CARTESIAN_POINT('Ctrl Pts',(-158.069360250185,-223.373859589861,
6.80932906126852E-16));
#86007=CARTESIAN_POINT('Ctrl Pts',(-158.082843652116,-223.361242283932,
8.04911692853238E-16));
#86008=CARTESIAN_POINT('Ctrl Pts',(-162.519491502139,-225.001988389076,
18.3874166975081));
#86009=CARTESIAN_POINT('Ctrl Pts',(-162.520629418137,-225.133541932024,
18.3957515808994));
#86010=CARTESIAN_POINT('Ctrl Pts',(-162.511215066058,-225.264932196066,
18.4040864642908));
#86011=CARTESIAN_POINT('Ctrl Pts',(-162.490680057533,-225.394560699254,
18.4124213476821));
#86012=CARTESIAN_POINT('Ctrl Pts',(-162.360300544394,-226.217589387765,
18.4653406360927));
#86013=CARTESIAN_POINT('Ctrl Pts',(-161.781630713394,-226.969598857535,
18.5182599245033));
#86014=CARTESIAN_POINT('Ctrl Pts',(-161.019467989588,-227.306478092312,
18.5711792129139));
#86015=CARTESIAN_POINT('Ctrl Pts',(-160.257305265783,-227.64335732709,18.6240985013245));
#86016=CARTESIAN_POINT('Ctrl Pts',(-159.311649649173,-227.565106326875,
18.6770177897351));
#86017=CARTESIAN_POINT('Ctrl Pts',(-158.615237028698,-227.107515105334,
18.7299370781457));
#86018=CARTESIAN_POINT('Ctrl Pts',(-157.918824408224,-226.649923883792,
18.7828563665563));
#86019=CARTESIAN_POINT('Ctrl Pts',(-157.471654783884,-225.812992440923,
18.8357756549669));
#86020=CARTESIAN_POINT('Ctrl Pts',(-157.47834487994,-224.97973719714,18.8886949433775));
#86021=CARTESIAN_POINT('Ctrl Pts',(-157.485034975996,-224.146481953356,
18.9416142317881));
#86022=CARTESIAN_POINT('Ctrl Pts',(-157.945584792449,-223.316902908658,
18.9945335201987));
#86023=CARTESIAN_POINT('Ctrl Pts',(-158.649263524052,-222.87053945485,19.0474528086093));
#86024=CARTESIAN_POINT('Ctrl Pts',(-159.352942255656,-222.424176001043,
19.1003720970199));
#86025=CARTESIAN_POINT('Ctrl Pts',(-160.29974990241,-222.361028138127,19.1532913854305));
#86026=CARTESIAN_POINT('Ctrl Pts',(-161.056392494181,-222.710149965623,
19.2062106738411));
#86027=CARTESIAN_POINT('Ctrl Pts',(-161.813035085951,-223.059271793118,
19.2591299622517));
#86028=CARTESIAN_POINT('Ctrl Pts',(-162.379512622738,-223.820663311025,
19.3120492506623));
#86029=CARTESIAN_POINT('Ctrl Pts',(-162.496677361246,-224.645584781132,
19.3649685390729));
#86030=CARTESIAN_POINT('Ctrl Pts',(-162.513244304932,-224.762227618515,
19.3724512585513));
#86031=CARTESIAN_POINT('Ctrl Pts',(-162.520827869545,-224.880140648168,
19.3799339780297));
#86032=CARTESIAN_POINT('Ctrl Pts',(-162.519857325378,-224.99817643576,19.3874166975081));
#86033=CARTESIAN_POINT('Ctrl Pts',(-160.793799282533,-227.969222953746,
20.));
#86034=CARTESIAN_POINT('Ctrl Pts',(-161.781070948697,-227.70528334649,19.9470807115894));
#86035=CARTESIAN_POINT('Ctrl Pts',(-163.454303791657,-226.117971486511,
19.8412421347682));
#86036=CARTESIAN_POINT('Ctrl Pts',(-162.813708830336,-222.699008736782,
19.6824842695364));
#86037=CARTESIAN_POINT('Ctrl Pts',(-159.592724505823,-221.390669564417,
19.5237264043046));
#86038=CARTESIAN_POINT('Ctrl Pts',(-156.746988377721,-223.383220985595,
19.3649685390728));
#86039=CARTESIAN_POINT('Ctrl Pts',(-156.877197897433,-226.856577363582,
19.206210673841));
#86040=CARTESIAN_POINT('Ctrl Pts',(-159.865978935642,-228.630249528,19.0474528086092));
#86041=CARTESIAN_POINT('Ctrl Pts',(-162.977135003112,-227.081779887678,
18.8886949433775));
#86042=CARTESIAN_POINT('Ctrl Pts',(-163.363752671914,-223.627938905832,
18.7299370781457));
#86043=CARTESIAN_POINT('Ctrl Pts',(-160.671798756939,-221.429869131324,
18.5711792129139));
#86044=CARTESIAN_POINT('Ctrl Pts',(-157.365046101209,-222.499153615461,
18.4124213476821));
#86045=CARTESIAN_POINT('Ctrl Pts',(-156.469787991194,-225.857226767288,
18.2536634824503));
#86046=CARTESIAN_POINT('Ctrl Pts',(-158.805387078146,-228.430759193889,
18.0949056172185));
#86047=CARTESIAN_POINT('Ctrl Pts',(-162.234292343626,-227.864464228569,
17.9361477519867));
#86048=CARTESIAN_POINT('Ctrl Pts',(-163.618375040713,-224.676610129639,
17.7773898867549));
#86049=CARTESIAN_POINT('Ctrl Pts',(-161.690920225189,-221.784723190834,
17.6186320215231));
#86050=CARTESIAN_POINT('Ctrl Pts',(-158.215935680102,-221.835457093401,
17.4598741562913));
#86051=CARTESIAN_POINT('Ctrl Pts',(-156.373726540536,-224.782380716962,
17.3011162910595));
#86052=CARTESIAN_POINT('Ctrl Pts',(-157.850282819984,-227.928469414349,
17.1423584258277));
#86053=CARTESIAN_POINT('Ctrl Pts',(-161.294260133946,-228.394423060065,
16.9836005605959));
#86054=CARTESIAN_POINT('Ctrl Pts',(-163.553730645469,-225.753800834845,
16.8248426953641));
#86055=CARTESIAN_POINT('Ctrl Pts',(-162.560826999764,-222.423300124782,
16.6660848301324));
#86056=CARTESIAN_POINT('Ctrl Pts',(-159.224254589513,-221.450995034583,
16.5073269649006));
#86057=CARTESIAN_POINT('Ctrl Pts',(-156.597644346055,-223.726739151393,
16.3485690996688));
#86058=CARTESIAN_POINT('Ctrl Pts',(-157.08486986444,-227.167771545708,16.189811234437));
#86059=CARTESIAN_POINT('Ctrl Pts',(-160.240022367702,-228.624859507152,
16.0310533692052));
#86060=CARTESIAN_POINT('Ctrl Pts',(-163.175506409748,-226.764476189946,
15.8722955039734));
#86061=CARTESIAN_POINT('Ctrl Pts',(-163.204767110338,-223.289244333207,
15.7135376387416));
#86062=CARTESIAN_POINT('Ctrl Pts',(-160.301025077633,-221.379695995386,
15.5547797735098));
#86063=CARTESIAN_POINT('Ctrl Pts',(-157.121784905686,-222.78344974025,15.396021908278));
#86064=CARTESIAN_POINT('Ctrl Pts',(-156.576687074886,-226.21579019566,15.2372640430462));
#86065=CARTESIAN_POINT('Ctrl Pts',(-159.164605098526,-228.535439511819,
15.0785061778144));
#86066=CARTESIAN_POINT('Ctrl Pts',(-162.517076503146,-227.619454725785,
14.9197483125826));
#86067=CARTESIAN_POINT('Ctrl Pts',(-163.565919591067,-224.306145077722,
14.7609904473508));
#86068=CARTESIAN_POINT('Ctrl Pts',(-161.351233209471,-221.627851427242,
14.6022325821191));
#86069=CARTESIAN_POINT('Ctrl Pts',(-157.899898247702,-222.035748017944,
14.4434747168873));
#86070=CARTESIAN_POINT('Ctrl Pts',(-156.370576327052,-225.156527906056,
14.2847168516555));
#86071=CARTESIAN_POINT('Ctrl Pts',(-158.16290280916,-228.134053460702,14.1259589864237));
#86072=CARTESIAN_POINT('Ctrl Pts',(-161.636540568083,-228.243293411356,
13.9672011211919));
#86073=CARTESIAN_POINT('Ctrl Pts',(-163.612416463452,-225.384271359477,
13.8084432559601));
#86074=CARTESIAN_POINT('Ctrl Pts',(-162.282208953524,-222.173564174515,
13.6496853907283));
#86075=CARTESIAN_POINT('Ctrl Pts',(-158.863323899077,-221.54961094589,13.4909275254965));
#86076=CARTESIAN_POINT('Ctrl Pts',(-156.484724767496,-224.083453643903,
13.3321696602647));
#86077=CARTESIAN_POINT('Ctrl Pts',(-157.323305390468,-227.456119530974,
13.1734117950329));
#86078=CARTESIAN_POINT('Ctrl Pts',(-160.611596814825,-228.580944919882,
13.0146539298011));
#86079=CARTESIAN_POINT('Ctrl Pts',(-163.340154858305,-226.428489658931,
12.8558960645694));
#86080=CARTESIAN_POINT('Ctrl Pts',(-163.011803306812,-222.968680718301,
12.6971381993375));
#86081=CARTESIAN_POINT('Ctrl Pts',(-159.927049487362,-221.367935104402,
12.5383803341058));
#86082=CARTESIAN_POINT('Ctrl Pts',(-156.909059974209,-223.091255140127,
12.379622468874));
#86083=CARTESIAN_POINT('Ctrl Pts',(-156.719898651112,-226.561458396548,
12.2208646036422));
#86084=CARTESIAN_POINT('Ctrl Pts',(-159.53268595353,-228.602614989851,12.0621067384104));
#86085=CARTESIAN_POINT('Ctrl Pts',(-162.773159052901,-227.346658486112,
11.9033488731786));
#86086=CARTESIAN_POINT('Ctrl Pts',(-163.475637096109,-223.943040228163,
11.7445910079468));
#86087=CARTESIAN_POINT('Ctrl Pts',(-160.997212205634,-221.506751511835,
11.585833142715));
#86088=CARTESIAN_POINT('Ctrl Pts',(-157.606138743777,-222.267483674507,
11.4270752774832));
#86089=CARTESIAN_POINT('Ctrl Pts',(-156.405927009479,-225.529014670817,
11.2683174122514));
#86090=CARTESIAN_POINT('Ctrl Pts',(-158.495010734773,-228.306391461198,
11.1095595470196));
#86091=CARTESIAN_POINT('Ctrl Pts',(-161.96146057642,-228.057758916311,10.9508016817878));
#86092=CARTESIAN_POINT('Ctrl Pts',(-163.63278177566,-225.01066553146,10.792043816556));
#86093=CARTESIAN_POINT('Ctrl Pts',(-161.979381236672,-221.953811052636,
10.6332859513243));
#86094=CARTESIAN_POINT('Ctrl Pts',(-158.514451067719,-221.684828578651,
10.4745280860924));
#86095=CARTESIAN_POINT('Ctrl Pts',(-156.409095223172,-224.449890859119,
10.3157702208607));
#86096=CARTESIAN_POINT('Ctrl Pts',(-157.590135289169,-227.718413003688,
10.1570123556289));
#86097=CARTESIAN_POINT('Ctrl Pts',(-160.976683443753,-228.499043674182,
9.99825449039708));
#86098=CARTESIAN_POINT('Ctrl Pts',(-163.469370949022,-226.07734971166,9.83949662516527));
#86099=CARTESIAN_POINT('Ctrl Pts',(-162.786890298175,-222.669665335394,
9.6807387599335));
#86100=CARTESIAN_POINT('Ctrl Pts',(-159.553847756031,-221.394703152536,
9.5219808947017));
#86101=CARTESIAN_POINT('Ctrl Pts',(-156.729123730022,-223.419308502703,
9.3632230294699));
#86102=CARTESIAN_POINT('Ctrl Pts',(-156.897905537673,-226.890562649037,
9.20446516423812));
#86103=CARTESIAN_POINT('Ctrl Pts',(-159.905724075259,-228.631573933316,
9.04570729900632));
#86104=CARTESIAN_POINT('Ctrl Pts',(-162.99982393546,-227.048968896633,8.88694943377453));
#86105=CARTESIAN_POINT('Ctrl Pts',(-163.348485047893,-223.591147606325,
8.72819156854274));
#86106=CARTESIAN_POINT('Ctrl Pts',(-160.632612776171,-221.422707971306,
8.56943370331094));
#86107=CARTESIAN_POINT('Ctrl Pts',(-157.337773316573,-222.528205860274,
8.41067583807916));
#86108=CARTESIAN_POINT('Ctrl Pts',(-156.479403612958,-225.895889648718,
8.25191797284736));
#86109=CARTESIAN_POINT('Ctrl Pts',(-158.84308358432,-228.443655265885,8.09316010761556));
#86110=CARTESIAN_POINT('Ctrl Pts',(-162.265573413817,-227.839787719132,
7.93440224238377));
#86111=CARTESIAN_POINT('Ctrl Pts',(-163.61461054408,-224.636946563501,7.77564437715198));
#86112=CARTESIAN_POINT('Ctrl Pts',(-161.655556246542,-221.766371898677,
7.61688651192019));
#86113=CARTESIAN_POINT('Ctrl Pts',(-158.181336937272,-221.855213545024,
7.4581286466884));
#86114=CARTESIAN_POINT('Ctrl Pts',(-156.371557991493,-224.822163631299,
7.29937078145661));
#86115=CARTESIAN_POINT('Ctrl Pts',(-157.882529029215,-227.951869555216,
7.14061291622481));
#86116=CARTESIAN_POINT('Ctrl Pts',(-161.331409416131,-228.380024578279,
6.98185505099302));
#86117=CARTESIAN_POINT('Ctrl Pts',(-163.561783957761,-225.714781240217,
6.82309718576123));
#86118=CARTESIAN_POINT('Ctrl Pts',(-162.532413961312,-222.395370139217,
6.66433932052944));
#86119=CARTESIAN_POINT('Ctrl Pts',(-159.185378807054,-221.459716184381,
6.50558145529764));
#86120=CARTESIAN_POINT('Ctrl Pts',(-156.583884936547,-223.764129838381,
6.34682359006585));
#86121=CARTESIAN_POINT('Ctrl Pts',(-157.108819437776,-227.199611815696,
6.18806572483406));
#86122=CARTESIAN_POINT('Ctrl Pts',(-160.27976227586,-228.622009145783,6.02930785960227));
#86123=CARTESIAN_POINT('Ctrl Pts',(-163.194666690078,-226.729543848082,
5.87054999437047));
#86124=CARTESIAN_POINT('Ctrl Pts',(-163.185812275164,-223.254200088628,
5.71179212913868));
#86125=CARTESIAN_POINT('Ctrl Pts',(-160.261302591299,-221.376612339411,
5.55303426390689));
#86126=CARTESIAN_POINT('Ctrl Pts',(-157.097648786153,-222.815148834678,
5.3942763986751));
#86127=CARTESIAN_POINT('Ctrl Pts',(-156.590226697787,-226.253261030531,
5.2355185334433));
#86128=CARTESIAN_POINT('Ctrl Pts',(-159.203429001521,-228.544388780525,
5.07676066821151));
#86129=CARTESIAN_POINT('Ctrl Pts',(-162.545653051738,-227.591692057962,
4.91800280297972));
#86130=CARTESIAN_POINT('Ctrl Pts',(-163.55809552911,-224.267078865869,4.75924493774792));
#86131=CARTESIAN_POINT('Ctrl Pts',(-161.314169118159,-221.613235066909,
4.60048707251614));
#86132=CARTESIAN_POINT('Ctrl Pts',(-157.867515181948,-222.058958401537,
4.44172920728434));
#86133=CARTESIAN_POINT('Ctrl Pts',(-156.372511267358,-225.196322891415,
4.28297134205255));
#86134=CARTESIAN_POINT('Ctrl Pts',(-158.197384898239,-228.15401267881,4.12421347682076));
#86135=CARTESIAN_POINT('Ctrl Pts',(-161.672011799357,-228.225150186546,
3.96545561158896));
#86136=CARTESIAN_POINT('Ctrl Pts',(-163.616413567471,-225.344630370464,
3.80669774635717));
#86137=CARTESIAN_POINT('Ctrl Pts',(-162.251073780811,-222.148704852714,
3.64793988112538));
#86138=CARTESIAN_POINT('Ctrl Pts',(-158.825551358552,-221.562284541991,
3.48918201589359));
#86139=CARTESIAN_POINT('Ctrl Pts',(-156.474884286599,-224.122061282515,
3.3304241506618));
#86140=CARTESIAN_POINT('Ctrl Pts',(-157.350402977267,-227.485327504289,
3.17166628543));
#86141=CARTESIAN_POINT('Ctrl Pts',(-160.650832758246,-228.574022088692,
3.01290842019821));
#86142=CARTESIAN_POINT('Ctrl Pts',(-163.355620425927,-226.391771804664,
2.85415055496642));
#86143=CARTESIAN_POINT('Ctrl Pts',(-162.989344408734,-222.935772006054,
2.69539268973463));
#86144=CARTESIAN_POINT('Ctrl Pts',(-159.887220512494,-221.368953614723,
2.53663482450283));
#86145=CARTESIAN_POINT('Ctrl Pts',(-156.888312385766,-223.125268673492,
2.37787695927104));
#86146=CARTESIAN_POINT('Ctrl Pts',(-156.737220668234,-226.597337890817,
2.21911909403925));
#86147=CARTESIAN_POINT('Ctrl Pts',(-159.572224410776,-228.60752327959,2.06036122880746));
#86148=CARTESIAN_POINT('Ctrl Pts',(-162.798728472064,-227.316104031162,
1.90160336357566));
#86149=CARTESIAN_POINT('Ctrl Pts',(-163.46383610443,-223.904985372157,1.74284549834387));
#86150=CARTESIAN_POINT('Ctrl Pts',(-160.958841571036,-221.496026324134,
1.58408763311208));
#86151=CARTESIAN_POINT('Ctrl Pts',(-157.576314230351,-222.293899143107,
1.42532976788029));
#86152=CARTESIAN_POINT('Ctrl Pts',(-156.411946167088,-225.568405119559,
1.2665719026485));
#86153=CARTESIAN_POINT('Ctrl Pts',(-158.531360356103,-228.322686501262,
1.1078140374167));
#86154=CARTESIAN_POINT('Ctrl Pts',(-161.994882774227,-228.036087350692,
0.94905617218491));
#86155=CARTESIAN_POINT('Ctrl Pts',(-163.632669289527,-224.970773976824,
0.790298306953122));
#86156=CARTESIAN_POINT('Ctrl Pts',(-161.945876991572,-221.932389200875,
0.631540441721325));
#86157=CARTESIAN_POINT('Ctrl Pts',(-158.478135184779,-221.701106251642,
0.472782576489533));
#86158=CARTESIAN_POINT('Ctrl Pts',(-156.403376046572,-224.489749930199,
0.314024711257741));
#86159=CARTESIAN_POINT('Ctrl Pts',(-157.619888902649,-227.743758496233,
0.155266846025946));
#86160=CARTESIAN_POINT('Ctrl Pts',(-161.015405968821,-228.490052849714,
-0.00349101920584225));
#86161=CARTESIAN_POINT('Ctrl Pts',(-163.47996393464,-226.035338564583,-0.162248884437638));
#86162=CARTESIAN_POINT('Ctrl Pts',(-163.000168811616,-223.779443237332,
-0.268087461258832));
#86163=CARTESIAN_POINT('Ctrl Pts',(-162.336062657696,-223.002698443069,
-0.32100674966943));
#86164=CARTESIAN_POINT('Ctrl Pts',(-160.745932854347,-227.790177569842,
20.1070022498898));
#86165=CARTESIAN_POINT('Ctrl Pts',(-161.673671626808,-227.542153631111,
20.0540829614792));
#86166=CARTESIAN_POINT('Ctrl Pts',(-163.246007830683,-226.050557339068,
19.948244384658));
#86167=CARTESIAN_POINT('Ctrl Pts',(-162.644041013008,-222.837759470728,
19.7894865194262));
#86168=CARTESIAN_POINT('Ctrl Pts',(-159.617283388179,-221.608313696751,
19.6307286541944));
#86169=CARTESIAN_POINT('Ctrl Pts',(-156.943146336833,-223.480713435247,
19.4719707889626));
#86170=CARTESIAN_POINT('Ctrl Pts',(-157.065504168138,-226.744624973348,
19.3132129237308));
#86171=CARTESIAN_POINT('Ctrl Pts',(-159.874060461782,-228.411343965659,
19.1544550584991));
#86172=CARTESIAN_POINT('Ctrl Pts',(-162.797612519329,-226.956247691209,
18.9956971932673));
#86173=CARTESIAN_POINT('Ctrl Pts',(-163.16091698127,-223.710674762712,18.8369393280355));
#86174=CARTESIAN_POINT('Ctrl Pts',(-160.631289011388,-221.645149513406,
18.6781814628037));
#86175=CARTESIAN_POINT('Ctrl Pts',(-157.523934921525,-222.649955696672,
18.5194235975719));
#86176=CARTESIAN_POINT('Ctrl Pts',(-156.682661249357,-225.805535635287,
18.3606657323401));
#86177=CARTESIAN_POINT('Ctrl Pts',(-158.877422736142,-228.223882981991,
18.2019078671083));
#86178=CARTESIAN_POINT('Ctrl Pts',(-162.099563582381,-227.691735839536,
18.0431500018765));
#86179=CARTESIAN_POINT('Ctrl Pts',(-163.400185514913,-224.696110673852,
17.8843921366447));
#86180=CARTESIAN_POINT('Ctrl Pts',(-161.58895702957,-221.978605724959,17.7256342714129));
#86181=CARTESIAN_POINT('Ctrl Pts',(-158.323515503524,-222.026280352017,
17.5668764061811));
#86182=CARTESIAN_POINT('Ctrl Pts',(-156.592392344284,-224.795503250595,
17.4081185409494));
#86183=CARTESIAN_POINT('Ctrl Pts',(-157.979911663549,-227.751881485888,
17.2493606757175));
#86184=CARTESIAN_POINT('Ctrl Pts',(-161.216215707453,-228.189737932209,
17.0906028104858));
#86185=CARTESIAN_POINT('Ctrl Pts',(-163.339439203695,-225.708346329756,
16.931844945254));
#86186=CARTESIAN_POINT('Ctrl Pts',(-162.40640806241,-222.578676203153,16.7730870800222));
#86187=CARTESIAN_POINT('Ctrl Pts',(-159.271032361676,-221.665001515877,
16.6143292147904));
#86188=CARTESIAN_POINT('Ctrl Pts',(-156.802807812634,-223.803517312212,
16.4555713495586));
#86189=CARTESIAN_POINT('Ctrl Pts',(-157.260653428821,-227.037054016354,
16.2968134843268));
#86190=CARTESIAN_POINT('Ctrl Pts',(-160.225548918709,-228.406278965319,
16.138055619095));
#86191=CARTESIAN_POINT('Ctrl Pts',(-162.984022047315,-226.658077538939,
15.9792977538632));
#86192=CARTESIAN_POINT('Ctrl Pts',(-163.011518315441,-223.392403614237,
15.8205398886314));
#86193=CARTESIAN_POINT('Ctrl Pts',(-160.282873139759,-221.598001838514,
15.6617820233996));
#86194=CARTESIAN_POINT('Ctrl Pts',(-157.295342477666,-222.917108646428,
15.5030241581678));
#86195=CARTESIAN_POINT('Ctrl Pts',(-156.783114273668,-226.142477539211,
15.344266292936));
#86196=CARTESIAN_POINT('Ctrl Pts',(-159.214979759902,-228.322251033041,
15.1855084277042));
#86197=CARTESIAN_POINT('Ctrl Pts',(-162.365295739007,-227.461500512073,
15.0267505624725));
#86198=CARTESIAN_POINT('Ctrl Pts',(-163.350893150784,-224.347984819253,
14.8679926972406));
#86199=CARTESIAN_POINT('Ctrl Pts',(-161.269753282735,-221.831193394213,
14.7092348320089));
#86200=CARTESIAN_POINT('Ctrl Pts',(-158.026535260259,-222.214493650178,
14.5504769667771));
#86201=CARTESIAN_POINT('Ctrl Pts',(-156.589432089989,-225.147089207964,
14.3917191015453));
#86202=CARTESIAN_POINT('Ctrl Pts',(-158.273680536844,-227.945068728404,
14.2329612363135));
#86203=CARTESIAN_POINT('Ctrl Pts',(-161.537856488493,-228.047721464422,
14.0742033710817));
#86204=CARTESIAN_POINT('Ctrl Pts',(-163.394586242349,-225.361099636049,
13.9154455058499));
#86205=CARTESIAN_POINT('Ctrl Pts',(-162.144590800695,-222.343999434964,
13.7566876406181));
#86206=CARTESIAN_POINT('Ctrl Pts',(-158.93186594258,-221.757670846556,13.5979297753863));
#86207=CARTESIAN_POINT('Ctrl Pts',(-156.696697331812,-224.138721771878,
13.4391719101545));
#86208=CARTESIAN_POINT('Ctrl Pts',(-157.484711193071,-227.308014497709,
13.2804140449227));
#86209=CARTESIAN_POINT('Ctrl Pts',(-160.57471727152,-228.365012445997,13.1216561796909));
#86210=CARTESIAN_POINT('Ctrl Pts',(-163.138742125675,-226.342351136035,
12.9628983144591));
#86211=CARTESIAN_POINT('Ctrl Pts',(-162.83019030984,-223.09117011916,12.8041404492274));
#86212=CARTESIAN_POINT('Ctrl Pts',(-159.931448433734,-221.586950134167,
12.6453825839956));
#86213=CARTESIAN_POINT('Ctrl Pts',(-157.095444948379,-223.206353252169,
12.4866247187638));
#86214=CARTESIAN_POINT('Ctrl Pts',(-156.917690132049,-226.467301803253,
12.327866853532));
#86215=CARTESIAN_POINT('Ctrl Pts',(-159.560865185658,-228.385375801699,
12.1691089883002));
#86216=CARTESIAN_POINT('Ctrl Pts',(-162.605936404085,-227.205153999557,
12.0103511230684));
#86217=CARTESIAN_POINT('Ctrl Pts',(-163.266054727969,-224.006775343736,
11.8515932578366));
#86218=CARTESIAN_POINT('Ctrl Pts',(-160.93707989325,-221.71739585427,11.6928353926048));
#86219=CARTESIAN_POINT('Ctrl Pts',(-157.750489577079,-222.432255549891,
11.534077527373));
#86220=CARTESIAN_POINT('Ctrl Pts',(-156.622651111505,-225.497114865277,
11.3753196621412));
#86221=CARTESIAN_POINT('Ctrl Pts',(-158.585762215871,-228.107014675511,
11.2165617969094));
#86222=CARTESIAN_POINT('Ctrl Pts',(-161.843183684658,-227.873374776897,
11.0578039316776));
#86223=CARTESIAN_POINT('Ctrl Pts',(-163.413723517728,-225.01002239546,10.8990460664458));
#86224=CARTESIAN_POINT('Ctrl Pts',(-161.860023721614,-222.137497518092,
10.7402882012141));
#86225=CARTESIAN_POINT('Ctrl Pts',(-158.604030288623,-221.884734799601,
10.5815303359823));
#86226=CARTESIAN_POINT('Ctrl Pts',(-156.625628280589,-224.483062670011,
10.4227724707505));
#86227=CARTESIAN_POINT('Ctrl Pts',(-157.735451137466,-227.554491564498,
10.2640146055187));
#86228=CARTESIAN_POINT('Ctrl Pts',(-160.917789024283,-228.28804987961,10.1052567402869));
#86229=CARTESIAN_POINT('Ctrl Pts',(-163.260166432167,-226.012385074202,
9.94649887505509));
#86230=CARTESIAN_POINT('Ctrl Pts',(-162.618839649535,-222.810185488696,
9.78774100982331));
#86231=CARTESIAN_POINT('Ctrl Pts',(-159.580750922632,-221.612104057822,
9.62898314459151));
#86232=CARTESIAN_POINT('Ctrl Pts',(-156.926358934849,-223.514624860004,
9.47022527935972));
#86233=CARTESIAN_POINT('Ctrl Pts',(-157.084963129025,-226.776560931899,
9.31146741412793));
#86234=CARTESIAN_POINT('Ctrl Pts',(-159.911408952885,-228.412588508782,
9.15270954889613));
#86235=CARTESIAN_POINT('Ctrl Pts',(-162.818933299582,-226.925415216624,
8.99395168366434));
#86236=CARTESIAN_POINT('Ctrl Pts',(-163.146570001353,-223.676101993927,
8.83519381843255));
#86237=CARTESIAN_POINT('Ctrl Pts',(-160.594465961621,-221.638420174327,
8.67643595320076));
#86238=CARTESIAN_POINT('Ctrl Pts',(-157.498306697191,-222.677256078992,
8.51767808796897));
#86239=CARTESIAN_POINT('Ctrl Pts',(-156.691697045115,-225.841867128824,
8.35892022273717));
#86240=CARTESIAN_POINT('Ctrl Pts',(-158.912846127253,-228.236001415462,
8.20016235750538));
#86241=CARTESIAN_POINT('Ctrl Pts',(-162.128958390979,-227.668547333921,
8.04140449227359));
#86242=CARTESIAN_POINT('Ctrl Pts',(-163.396648018999,-224.658838837315,
7.88264662704179));
#86243=CARTESIAN_POINT('Ctrl Pts',(-161.555725513602,-221.961361023381,
7.72388876181));
#86244=CARTESIAN_POINT('Ctrl Pts',(-158.291003079333,-222.044845481358,
7.56513089657821));
#86245=CARTESIAN_POINT('Ctrl Pts',(-156.590354559654,-224.832887238587,
7.40637303134642));
#86246=CARTESIAN_POINT('Ctrl Pts',(-158.010213412898,-227.77387058849,7.24761516611462));
#86247=CARTESIAN_POINT('Ctrl Pts',(-161.251124872411,-228.176207684886,
7.08885730088284));
#86248=CARTESIAN_POINT('Ctrl Pts',(-163.347006897893,-225.671679632976,
6.93009943565103));
#86249=CARTESIAN_POINT('Ctrl Pts',(-162.37970834204,-222.552430407379,6.77134157041925));
#86250=CARTESIAN_POINT('Ctrl Pts',(-159.234500805133,-221.673196776701,
6.61258370518745));
#86251=CARTESIAN_POINT('Ctrl Pts',(-156.789878101265,-223.838653325162,
6.45382583995566));
#86252=CARTESIAN_POINT('Ctrl Pts',(-157.283158832885,-227.066974304766,
6.29506797472387));
#86253=CARTESIAN_POINT('Ctrl Pts',(-160.262892493811,-228.40360048193,6.13631010949208));
#86254=CARTESIAN_POINT('Ctrl Pts',(-163.00202695474,-226.625251631875,5.97755224426028));
#86255=CARTESIAN_POINT('Ctrl Pts',(-162.993706464743,-223.359472552239,
5.81879437902849));
#86256=CARTESIAN_POINT('Ctrl Pts',(-160.245545935937,-221.595104128282,
5.6600365137967));
#86257=CARTESIAN_POINT('Ctrl Pts',(-157.272661776218,-222.946896272227,
5.50127864856491));
#86258=CARTESIAN_POINT('Ctrl Pts',(-156.795837451654,-226.177688867093,
5.34252078333311));
#86259=CARTESIAN_POINT('Ctrl Pts',(-159.251462565336,-228.330660657108,
5.18376291810132));
#86260=CARTESIAN_POINT('Ctrl Pts',(-162.392149109786,-227.435411944712,
5.02500505286953));
#86261=CARTESIAN_POINT('Ctrl Pts',(-163.34354088303,-224.311274316287,4.86624718763774));
#86262=CARTESIAN_POINT('Ctrl Pts',(-161.234924171605,-221.817458406511,
4.70748932240595));
#86263=CARTESIAN_POINT('Ctrl Pts',(-157.996104906891,-222.23630443795,4.54873145717415));
#86264=CARTESIAN_POINT('Ctrl Pts',(-156.591250352587,-225.184484539089,
4.38997359194236));
#86265=CARTESIAN_POINT('Ctrl Pts',(-158.306083341553,-227.963824397327,
4.23121572671057));
#86266=CARTESIAN_POINT('Ctrl Pts',(-161.57118878971,-228.030672283643,4.07245786147877));
#86267=CARTESIAN_POINT('Ctrl Pts',(-163.398342319327,-225.323849015226,
3.91369999624698));
#86268=CARTESIAN_POINT('Ctrl Pts',(-162.115333091897,-222.320639140647,
3.75494213101519));
#86269=CARTESIAN_POINT('Ctrl Pts',(-158.89637110202,-221.76958021952,3.5961842657834));
#86270=CARTESIAN_POINT('Ctrl Pts',(-156.687450236022,-224.175001353761,
3.4374264005516));
#86271=CARTESIAN_POINT('Ctrl Pts',(-157.510174784072,-227.335461218037,
3.27866853531981));
#86272=CARTESIAN_POINT('Ctrl Pts',(-160.611587271169,-228.358507064419,
3.11991067008802));
#86273=CARTESIAN_POINT('Ctrl Pts',(-163.153275113112,-226.307847383712,
2.96115280485622));
#86274=CARTESIAN_POINT('Ctrl Pts',(-162.809085692693,-223.060245816003,
2.80239493962444));
#86275=CARTESIAN_POINT('Ctrl Pts',(-159.894021162681,-221.587907227891,
2.64363707439264));
#86276=CARTESIAN_POINT('Ctrl Pts',(-157.075948448183,-223.23831575527,2.48487920916085));
#86277=CARTESIAN_POINT('Ctrl Pts',(-156.933967624306,-226.501017749036,
2.32612134392906));
#86278=CARTESIAN_POINT('Ctrl Pts',(-159.598019457423,-228.389988119517,
2.16736347869727));
#86279=CARTESIAN_POINT('Ctrl Pts',(-162.629963976595,-227.176441990998,
2.00860561346547));
#86280=CARTESIAN_POINT('Ctrl Pts',(-163.254965341015,-223.971015211437,
1.84984774823368));
#86281=CARTESIAN_POINT('Ctrl Pts',(-160.90102302394,-221.707317399865,1.69108988300189));
#86282=CARTESIAN_POINT('Ctrl Pts',(-157.722463494266,-222.457078154705,
1.5323320177701));
#86283=CARTESIAN_POINT('Ctrl Pts',(-156.628307311397,-225.534130053513,
1.37357415253831));
#86284=CARTESIAN_POINT('Ctrl Pts',(-158.619919939858,-228.122327117855,
1.21481628730651));
#86285=CARTESIAN_POINT('Ctrl Pts',(-161.874590509982,-227.853010015733,
1.05605842207472));
#86286=CARTESIAN_POINT('Ctrl Pts',(-163.413617814555,-224.972536318225,
0.897300556842931));
#86287=CARTESIAN_POINT('Ctrl Pts',(-161.828539796483,-222.117367412936,
0.738542691611136));
#86288=CARTESIAN_POINT('Ctrl Pts',(-158.569904268588,-221.900030922114,
0.579784826379343));
#86289=CARTESIAN_POINT('Ctrl Pts',(-156.620253972727,-224.520518222462,
0.421026961147552));
#86290=CARTESIAN_POINT('Ctrl Pts',(-157.76341059563,-227.57830871326,0.262269095915756));
#86291=CARTESIAN_POINT('Ctrl Pts',(-160.954176564921,-228.279601205613,
0.103511230683968));
#86292=CARTESIAN_POINT('Ctrl Pts',(-163.270120656329,-225.972907216835,
-0.055246634547828));
#86293=CARTESIAN_POINT('Ctrl Pts',(-162.819257379562,-223.853043319762,
-0.161085211369022));
#86294=CARTESIAN_POINT('Ctrl Pts',(-162.195197104019,-223.123136560921,
-0.21400449977962));
#86295=CARTESIAN_POINT('Ctrl Pts',(-160.698066426161,-227.611132185939,
20.2140044997796));
#86296=CARTESIAN_POINT('Ctrl Pts',(-161.56627230492,-227.379023915733,20.161085211369));
#86297=CARTESIAN_POINT('Ctrl Pts',(-163.037711869709,-225.983143191625,
20.0552466345478));
#86298=CARTESIAN_POINT('Ctrl Pts',(-162.474373195681,-222.976510204674,
19.896488769316));
#86299=CARTESIAN_POINT('Ctrl Pts',(-159.641842270535,-221.825957829085,
19.7377309040843));
#86300=CARTESIAN_POINT('Ctrl Pts',(-157.139304295944,-223.578205884898,
19.5789730388525));
#86301=CARTESIAN_POINT('Ctrl Pts',(-157.253810438842,-226.632672583114,
19.4202151736207));
#86302=CARTESIAN_POINT('Ctrl Pts',(-159.882141987924,-228.192438403318,
19.2614573083889));
#86303=CARTESIAN_POINT('Ctrl Pts',(-162.618090035545,-226.830715494739,
19.1026994431571));
#86304=CARTESIAN_POINT('Ctrl Pts',(-162.958081290626,-223.793410619591,
18.9439415779253));
#86305=CARTESIAN_POINT('Ctrl Pts',(-160.590779265836,-221.860429895488,
18.7851837126935));
#86306=CARTESIAN_POINT('Ctrl Pts',(-157.682823741842,-222.800757777882,
18.6264258474617));
#86307=CARTESIAN_POINT('Ctrl Pts',(-156.895534507521,-225.753844503286,
18.4676679822299));
#86308=CARTESIAN_POINT('Ctrl Pts',(-158.949458394138,-228.017006770093,
18.3089101169981));
#86309=CARTESIAN_POINT('Ctrl Pts',(-161.964834821137,-227.519007450502,
18.1501522517663));
#86310=CARTESIAN_POINT('Ctrl Pts',(-163.181995989113,-224.715611218066,
17.9913943865345));
#86311=CARTESIAN_POINT('Ctrl Pts',(-161.486993833951,-222.172488259083,
17.8326365213027));
#86312=CARTESIAN_POINT('Ctrl Pts',(-158.431095326946,-222.217103610633,
17.6738786560709));
#86313=CARTESIAN_POINT('Ctrl Pts',(-156.811058148032,-224.808625784229,
17.5151207908392));
#86314=CARTESIAN_POINT('Ctrl Pts',(-158.109540507114,-227.575293557426,
17.3563629256073));
#86315=CARTESIAN_POINT('Ctrl Pts',(-161.138171280961,-227.985052804353,
17.1976050603756));
#86316=CARTESIAN_POINT('Ctrl Pts',(-163.12514776192,-225.662891824667,17.0388471951438));
#86317=CARTESIAN_POINT('Ctrl Pts',(-162.251989125057,-222.734052281524,
16.880089329912));
#86318=CARTESIAN_POINT('Ctrl Pts',(-159.317810133839,-221.879007997171,
16.7213314646802));
#86319=CARTESIAN_POINT('Ctrl Pts',(-157.007971279214,-223.88029547303,16.5625735994484));
#86320=CARTESIAN_POINT('Ctrl Pts',(-157.436436993201,-226.906336486999,
16.4038157342166));
#86321=CARTESIAN_POINT('Ctrl Pts',(-160.211075469716,-228.187698423485,
16.2450578689848));
#86322=CARTESIAN_POINT('Ctrl Pts',(-162.792537684881,-226.551678887932,
16.086300003753));
#86323=CARTESIAN_POINT('Ctrl Pts',(-162.818269520544,-223.495562895267,
15.9275421385212));
#86324=CARTESIAN_POINT('Ctrl Pts',(-160.264721201885,-221.816307681643,
15.7687842732894));
#86325=CARTESIAN_POINT('Ctrl Pts',(-157.468900049645,-223.050767552607,
15.6100264080577));
#86326=CARTESIAN_POINT('Ctrl Pts',(-156.989541472449,-226.069164882762,
15.4512685428258));
#86327=CARTESIAN_POINT('Ctrl Pts',(-159.265354421278,-228.109062554263,
15.2925106775941));
#86328=CARTESIAN_POINT('Ctrl Pts',(-162.213514974867,-227.30354629836,15.1337528123623));
#86329=CARTESIAN_POINT('Ctrl Pts',(-163.135866710501,-224.389824560784,
14.9749949471305));
#86330=CARTESIAN_POINT('Ctrl Pts',(-161.188273356,-222.034535361183,14.8162370818987));
#86331=CARTESIAN_POINT('Ctrl Pts',(-158.153172272815,-222.393239282414,
14.6574792166669));
#86332=CARTESIAN_POINT('Ctrl Pts',(-156.808287852926,-225.13765050987,14.4987213514351));
#86333=CARTESIAN_POINT('Ctrl Pts',(-158.384458264527,-227.756083996107,
14.3399634862033));
#86334=CARTESIAN_POINT('Ctrl Pts',(-161.439172408904,-227.852149517486,
14.1812056209715));
#86335=CARTESIAN_POINT('Ctrl Pts',(-163.176756021246,-225.337927912621,
14.0224477557397));
#86336=CARTESIAN_POINT('Ctrl Pts',(-162.006972647866,-222.514434695413,
13.8636898905079));
#86337=CARTESIAN_POINT('Ctrl Pts',(-159.000407986082,-221.965730747221,
13.7049320252761));
#86338=CARTESIAN_POINT('Ctrl Pts',(-156.908669896127,-224.193989899852,
13.5461741600443));
#86339=CARTESIAN_POINT('Ctrl Pts',(-157.646116995673,-227.159909464444,
13.3874162948125));
#86340=CARTESIAN_POINT('Ctrl Pts',(-160.537837728215,-228.149079972112,
13.2286584295808));
#86341=CARTESIAN_POINT('Ctrl Pts',(-162.937329393044,-226.256212613139,
13.069900564349));
#86342=CARTESIAN_POINT('Ctrl Pts',(-162.648577312867,-223.21365952002,12.9111426991172));
#86343=CARTESIAN_POINT('Ctrl Pts',(-159.935847380107,-221.805965163933,
12.7523848338854));
#86344=CARTESIAN_POINT('Ctrl Pts',(-157.28182992255,-223.321451364212,12.5936269686536));
#86345=CARTESIAN_POINT('Ctrl Pts',(-157.115481612986,-226.373145209957,
12.4348691034218));
#86346=CARTESIAN_POINT('Ctrl Pts',(-159.589044417786,-228.168136613547,
12.27611123819));
#86347=CARTESIAN_POINT('Ctrl Pts',(-162.438713755268,-227.063649513002,
12.1173533729582));
#86348=CARTESIAN_POINT('Ctrl Pts',(-163.056472359829,-224.070510459309,
11.9585955077264));
#86349=CARTESIAN_POINT('Ctrl Pts',(-160.876947580867,-221.928040196705,
11.7998376424946));
#86350=CARTESIAN_POINT('Ctrl Pts',(-157.894840410381,-222.597027425275,
11.6410797772628));
#86351=CARTESIAN_POINT('Ctrl Pts',(-156.839375213531,-225.465215059738,
11.482321912031));
#86352=CARTESIAN_POINT('Ctrl Pts',(-158.676513696969,-227.907637889824,
11.3235640467992));
#86353=CARTESIAN_POINT('Ctrl Pts',(-161.724906792896,-227.688990637483,
11.1648061815674));
#86354=CARTESIAN_POINT('Ctrl Pts',(-163.194665259795,-225.00937925946,11.0060483163357));
#86355=CARTESIAN_POINT('Ctrl Pts',(-161.740666206557,-222.321183983548,
10.8472904511039));
#86356=CARTESIAN_POINT('Ctrl Pts',(-158.693609509527,-222.084641020551,
10.6885325858721));
#86357=CARTESIAN_POINT('Ctrl Pts',(-156.842161338006,-224.516234480902,
10.5297747206403));
#86358=CARTESIAN_POINT('Ctrl Pts',(-157.880766985763,-227.390570125308,
10.3710168554085));
#86359=CARTESIAN_POINT('Ctrl Pts',(-160.858894604812,-228.077056085039,
10.2122589901767));
#86360=CARTESIAN_POINT('Ctrl Pts',(-163.050961915313,-225.947420436744,
10.0535011249449));
#86361=CARTESIAN_POINT('Ctrl Pts',(-162.450789000895,-222.950705641998,
9.89474325971312));
#86362=CARTESIAN_POINT('Ctrl Pts',(-159.607654089233,-221.829504963108,
9.73598539448133));
#86363=CARTESIAN_POINT('Ctrl Pts',(-157.123594139676,-223.609941217306,
9.57722752924952));
#86364=CARTESIAN_POINT('Ctrl Pts',(-157.272020720376,-226.662559214762,
9.41846966401774));
#86365=CARTESIAN_POINT('Ctrl Pts',(-159.917093830512,-228.193603084247,
9.25971179878594));
#86366=CARTESIAN_POINT('Ctrl Pts',(-162.638042663704,-226.801861536614,
9.10095393355416));
#86367=CARTESIAN_POINT('Ctrl Pts',(-162.944654954812,-223.761056381529,
8.94219606832235));
#86368=CARTESIAN_POINT('Ctrl Pts',(-160.556319147072,-221.854132377348,
8.78343820309057));
#86369=CARTESIAN_POINT('Ctrl Pts',(-157.658840077809,-222.82630629771,8.62468033785877));
#86370=CARTESIAN_POINT('Ctrl Pts',(-156.903990477271,-225.787844608929,
8.46592247262698));
#86371=CARTESIAN_POINT('Ctrl Pts',(-158.982608670187,-228.028347565038,
8.30716460739519));
#86372=CARTESIAN_POINT('Ctrl Pts',(-161.99234336814,-227.49730694871,8.1484067421634));
#86373=CARTESIAN_POINT('Ctrl Pts',(-163.178685493918,-224.680731111127,
7.9896488769316));
#86374=CARTESIAN_POINT('Ctrl Pts',(-161.455894780662,-222.156350148086,
7.83089101169981));
#86375=CARTESIAN_POINT('Ctrl Pts',(-158.400669221395,-222.234477417692,
7.67213314646802));
#86376=CARTESIAN_POINT('Ctrl Pts',(-156.809151127816,-224.843610845875,
7.51337528123623));
#86377=CARTESIAN_POINT('Ctrl Pts',(-158.137897796582,-227.595871621763,
7.35461741600443));
#86378=CARTESIAN_POINT('Ctrl Pts',(-161.170840328692,-227.972390791494,
7.19585955077265));
#86379=CARTESIAN_POINT('Ctrl Pts',(-163.132229838025,-225.628578025736,
7.03710168554084));
#86380=CARTESIAN_POINT('Ctrl Pts',(-162.227002722769,-222.709490675542,
6.87834382030906));
#86381=CARTESIAN_POINT('Ctrl Pts',(-159.283622803211,-221.886677369021,
6.71958595507727));
#86382=CARTESIAN_POINT('Ctrl Pts',(-156.995871265982,-223.913176811942,
6.56082808984547));
#86383=CARTESIAN_POINT('Ctrl Pts',(-157.457498227993,-226.934336793837,
6.40207022461368));
#86384=CARTESIAN_POINT('Ctrl Pts',(-160.246022711763,-228.185191818077,
6.24331235938188));
#86385=CARTESIAN_POINT('Ctrl Pts',(-162.809387219402,-226.520959415668,
6.0845544941501));
#86386=CARTESIAN_POINT('Ctrl Pts',(-162.801600654321,-223.46474501585,5.9257966289183));
#86387=CARTESIAN_POINT('Ctrl Pts',(-160.229789280576,-221.813595917153,
5.76703876368651));
#86388=CARTESIAN_POINT('Ctrl Pts',(-157.447674766284,-223.078643709776,
5.60828089845472));
#86389=CARTESIAN_POINT('Ctrl Pts',(-157.001448205521,-226.102116703656,
5.44952303322292));
#86390=CARTESIAN_POINT('Ctrl Pts',(-159.299496129151,-228.11693253369,5.29076516799113));
#86391=CARTESIAN_POINT('Ctrl Pts',(-162.238645167834,-227.279131831461,
5.13200730275934));
#86392=CARTESIAN_POINT('Ctrl Pts',(-163.128986236949,-224.355469766705,
4.97324943752754));
#86393=CARTESIAN_POINT('Ctrl Pts',(-161.155679225052,-222.021681746113,
4.81449157229576));
#86394=CARTESIAN_POINT('Ctrl Pts',(-158.124694631834,-222.413650474363,
4.65573370706396));
#86395=CARTESIAN_POINT('Ctrl Pts',(-156.809989437815,-225.172646186762,
4.49697584183217));
#86396=CARTESIAN_POINT('Ctrl Pts',(-158.414781784868,-227.773636115843,
4.33821797660038));
#86397=CARTESIAN_POINT('Ctrl Pts',(-161.470365780064,-227.83619438074,4.17946011136858));
#86398=CARTESIAN_POINT('Ctrl Pts',(-163.180271071183,-225.303067659987,
4.0207022461368));
#86399=CARTESIAN_POINT('Ctrl Pts',(-161.979592402983,-222.492573428581,
3.861944380905));
#86400=CARTESIAN_POINT('Ctrl Pts',(-158.967190845488,-221.976875897049,
3.70318651567321));
#86401=CARTESIAN_POINT('Ctrl Pts',(-156.900016185444,-224.227941425007,
3.54442865044141));
#86402=CARTESIAN_POINT('Ctrl Pts',(-157.669946590876,-227.185594931785,
3.38567078520963));
#86403=CARTESIAN_POINT('Ctrl Pts',(-160.572341784094,-228.142992040145,
3.22691291997783));
#86404=CARTESIAN_POINT('Ctrl Pts',(-162.950929800296,-226.223922962759,
3.06815505474604));
#86405=CARTESIAN_POINT('Ctrl Pts',(-162.628826976652,-223.184719625952,
2.90939718951425));
#86406=CARTESIAN_POINT('Ctrl Pts',(-159.900821812869,-221.806860841059,
2.75063932428245));
#86407=CARTESIAN_POINT('Ctrl Pts',(-157.2635845106,-223.351362837049,2.59188145905066));
#86408=CARTESIAN_POINT('Ctrl Pts',(-157.130714580378,-226.404697607255,
2.43312359381887));
#86409=CARTESIAN_POINT('Ctrl Pts',(-159.62381450407,-228.172452959444,2.27436572858708));
#86410=CARTESIAN_POINT('Ctrl Pts',(-162.461199481127,-227.036779950835,
2.11560786335528));
#86411=CARTESIAN_POINT('Ctrl Pts',(-163.046094577601,-224.037045050717,
1.95684999812349));
#86412=CARTESIAN_POINT('Ctrl Pts',(-160.843204476844,-221.918608475596,
1.7980921328917));
#86413=CARTESIAN_POINT('Ctrl Pts',(-157.868612758181,-222.620257166302,
1.6393342676599));
#86414=CARTESIAN_POINT('Ctrl Pts',(-156.844668455705,-225.499854987468,
1.48057640242812));
#86415=CARTESIAN_POINT('Ctrl Pts',(-158.708479523612,-227.921967734449,
1.32181853719632));
#86416=CARTESIAN_POINT('Ctrl Pts',(-161.754298245737,-227.669932680775,
1.16306067196453));
#86417=CARTESIAN_POINT('Ctrl Pts',(-163.194566339583,-224.974298659625,
1.00430280673274));
#86418=CARTESIAN_POINT('Ctrl Pts',(-161.711202601395,-222.302345624998,
0.845544941500946));
#86419=CARTESIAN_POINT('Ctrl Pts',(-158.661673352397,-222.098955592586,
0.686787076269153));
#86420=CARTESIAN_POINT('Ctrl Pts',(-156.837131898881,-224.551286514725,
0.528029211037362));
#86421=CARTESIAN_POINT('Ctrl Pts',(-157.90693228861,-227.412858930286,0.369271345805565));
#86422=CARTESIAN_POINT('Ctrl Pts',(-160.89294716102,-228.069149561511,0.210513480573778));
#86423=CARTESIAN_POINT('Ctrl Pts',(-163.060277378019,-225.910475869087,
0.0517556153419819));
#86424=CARTESIAN_POINT('Ctrl Pts',(-162.638345947507,-223.926643402192,
-0.0540829614792118));
#86425=CARTESIAN_POINT('Ctrl Pts',(-162.054331550342,-223.243574678773,
-0.10700224988981));
#86426=CARTESIAN_POINT('Ctrl Pts',(-160.650199997975,-227.432086802035,
20.3210067496694));
#86427=CARTESIAN_POINT('Ctrl Pts',(-161.458872983031,-227.215894200354,
20.2680874612588));
#86428=CARTESIAN_POINT('Ctrl Pts',(-162.829415908735,-225.915729044181,
20.1622488844376));
#86429=CARTESIAN_POINT('Ctrl Pts',(-162.304705378354,-223.11526093862,20.0034910192058));
#86430=CARTESIAN_POINT('Ctrl Pts',(-159.666401152891,-222.043601961419,
19.8447331539741));
#86431=CARTESIAN_POINT('Ctrl Pts',(-157.335462255055,-223.675698334549,
19.6859752887423));
#86432=CARTESIAN_POINT('Ctrl Pts',(-157.442116709546,-226.52072019288,19.5272174235105));
#86433=CARTESIAN_POINT('Ctrl Pts',(-159.890223514064,-227.973532840977,
19.3684595582787));
#86434=CARTESIAN_POINT('Ctrl Pts',(-162.438567551761,-226.705183298269,
19.2097016930469));
#86435=CARTESIAN_POINT('Ctrl Pts',(-162.755245599982,-223.876146476471,
19.0509438278151));
#86436=CARTESIAN_POINT('Ctrl Pts',(-160.550269520285,-222.075710277569,
18.8921859625833));
#86437=CARTESIAN_POINT('Ctrl Pts',(-157.841712562158,-222.951559859093,
18.7334280973515));
#86438=CARTESIAN_POINT('Ctrl Pts',(-157.108407765684,-225.702153371286,
18.5746702321197));
#86439=CARTESIAN_POINT('Ctrl Pts',(-159.021494052134,-227.810130558195,
18.4159123668879));
#86440=CARTESIAN_POINT('Ctrl Pts',(-161.830106059892,-227.346279061469,
18.2571545016561));
#86441=CARTESIAN_POINT('Ctrl Pts',(-162.963806463313,-224.735111762279,
18.0983966364243));
#86442=CARTESIAN_POINT('Ctrl Pts',(-161.385030638332,-222.366370793208,
17.9396387711925));
#86443=CARTESIAN_POINT('Ctrl Pts',(-158.538675150368,-222.407926869249,
17.7808809059607));
#86444=CARTESIAN_POINT('Ctrl Pts',(-157.029723951781,-224.821748317863,
17.622123040729));
#86445=CARTESIAN_POINT('Ctrl Pts',(-158.239169350678,-227.398705628965,
17.4633651754972));
#86446=CARTESIAN_POINT('Ctrl Pts',(-161.060126854468,-227.780367676496,
17.3046073102654));
#86447=CARTESIAN_POINT('Ctrl Pts',(-162.910856320146,-225.617437319578,
17.1458494450336));
#86448=CARTESIAN_POINT('Ctrl Pts',(-162.097570187703,-222.889428359895,
16.9870915798018));
#86449=CARTESIAN_POINT('Ctrl Pts',(-159.364587906002,-222.093014478465,
16.82833371457));
#86450=CARTESIAN_POINT('Ctrl Pts',(-157.213134745793,-223.957073633848,
16.6695758493382));
#86451=CARTESIAN_POINT('Ctrl Pts',(-157.612220557582,-226.775618957645,
16.5108179841064));
#86452=CARTESIAN_POINT('Ctrl Pts',(-160.196602020722,-227.969117881651,
16.3520601188746));
#86453=CARTESIAN_POINT('Ctrl Pts',(-162.601053322447,-226.445280236925,
16.1933022536428));
#86454=CARTESIAN_POINT('Ctrl Pts',(-162.625020725647,-223.598722176297,
16.0345443884111));
#86455=CARTESIAN_POINT('Ctrl Pts',(-160.246569264012,-222.034613524771,
15.8757865231792));
#86456=CARTESIAN_POINT('Ctrl Pts',(-157.642457621625,-223.184426458786,
15.7170286579475));
#86457=CARTESIAN_POINT('Ctrl Pts',(-157.19596867123,-225.995852226314,15.5582707927157));
#86458=CARTESIAN_POINT('Ctrl Pts',(-159.315729082654,-227.895874075485,
15.3995129274839));
#86459=CARTESIAN_POINT('Ctrl Pts',(-162.061734210728,-227.145592084648,
15.2407550622521));
#86460=CARTESIAN_POINT('Ctrl Pts',(-162.920840270217,-224.431664302315,
15.0819971970203));
#86461=CARTESIAN_POINT('Ctrl Pts',(-161.106793429264,-222.237877328154,
14.9232393317885));
#86462=CARTESIAN_POINT('Ctrl Pts',(-158.279809285372,-222.571984914649,
14.7644814665567));
#86463=CARTESIAN_POINT('Ctrl Pts',(-157.027143615862,-225.128211811777,
14.6057236013249));
#86464=CARTESIAN_POINT('Ctrl Pts',(-158.495235992211,-227.567099263809,
14.4469657360931));
#86465=CARTESIAN_POINT('Ctrl Pts',(-161.340488329315,-227.656577570551,
14.2882078708613));
#86466=CARTESIAN_POINT('Ctrl Pts',(-162.958925800143,-225.314756189193,
14.1294500056295));
#86467=CARTESIAN_POINT('Ctrl Pts',(-161.869354495037,-222.684869955862,
13.9706921403977));
#86468=CARTESIAN_POINT('Ctrl Pts',(-159.068950029584,-222.173790647886,
13.811934275166));
#86469=CARTESIAN_POINT('Ctrl Pts',(-157.120642460443,-224.249258027827,
13.6531764099341));
#86470=CARTESIAN_POINT('Ctrl Pts',(-157.807522798276,-227.011804431178,
13.4944185447024));
#86471=CARTESIAN_POINT('Ctrl Pts',(-160.50095818491,-227.933147498227,13.3356606794706));
#86472=CARTESIAN_POINT('Ctrl Pts',(-162.735916660414,-226.170074090242,
13.1769028142388));
#86473=CARTESIAN_POINT('Ctrl Pts',(-162.466964315894,-223.336148920879,
13.018144949007));
#86474=CARTESIAN_POINT('Ctrl Pts',(-159.940246326479,-222.024980193698,
12.8593870837752));
#86475=CARTESIAN_POINT('Ctrl Pts',(-157.468214896721,-223.436549476255,
12.7006292185434));
#86476=CARTESIAN_POINT('Ctrl Pts',(-157.313273093923,-226.278988616662,
12.5418713533116));
#86477=CARTESIAN_POINT('Ctrl Pts',(-159.617223649915,-227.950897425395,
12.3831134880798));
#86478=CARTESIAN_POINT('Ctrl Pts',(-162.271491106452,-226.922145026448,
12.224355622848));
#86479=CARTESIAN_POINT('Ctrl Pts',(-162.846889991688,-224.134245574882,
12.0655977576162));
#86480=CARTESIAN_POINT('Ctrl Pts',(-160.816815268483,-222.13868453914,11.9068398923844));
#86481=CARTESIAN_POINT('Ctrl Pts',(-158.039191243683,-222.761799300658,
11.7480820271526));
#86482=CARTESIAN_POINT('Ctrl Pts',(-157.056099315557,-225.433315254199,
11.5893241619208));
#86483=CARTESIAN_POINT('Ctrl Pts',(-158.767265178067,-227.708261104137,
11.4305662966891));
#86484=CARTESIAN_POINT('Ctrl Pts',(-161.606629901135,-227.504606498068,
11.2718084314573));
#86485=CARTESIAN_POINT('Ctrl Pts',(-162.975607001862,-225.008736123459,
11.1130505662255));
#86486=CARTESIAN_POINT('Ctrl Pts',(-161.621308691499,-222.504870449003,
10.9542927009937));
#86487=CARTESIAN_POINT('Ctrl Pts',(-158.783188730432,-222.284547241501,
10.7955348357619));
#86488=CARTESIAN_POINT('Ctrl Pts',(-157.058694395424,-224.549406291795,
10.6367769705301));
#86489=CARTESIAN_POINT('Ctrl Pts',(-158.026082834059,-227.226648686118,
10.4780191052983));
#86490=CARTESIAN_POINT('Ctrl Pts',(-160.800000185342,-227.866062290468,
10.3192612400665));
#86491=CARTESIAN_POINT('Ctrl Pts',(-162.841757398458,-225.882455799286,
10.1605033748347));
#86492=CARTESIAN_POINT('Ctrl Pts',(-162.282738352255,-223.0912257953,10.0017455096029));
#86493=CARTESIAN_POINT('Ctrl Pts',(-159.634557255835,-222.046905868394,
9.84298764437113));
#86494=CARTESIAN_POINT('Ctrl Pts',(-157.320829344503,-223.705257574607,
9.68422977913933));
#86495=CARTESIAN_POINT('Ctrl Pts',(-157.459078311727,-226.548557497625,
9.52547191390755));
#86496=CARTESIAN_POINT('Ctrl Pts',(-159.922778708139,-227.974617659712,
9.36671404867574));
#86497=CARTESIAN_POINT('Ctrl Pts',(-162.457152027825,-226.678307856605,
9.20795618344397));
#86498=CARTESIAN_POINT('Ctrl Pts',(-162.742739908271,-223.846010769131,
9.04919831821216));
#86499=CARTESIAN_POINT('Ctrl Pts',(-160.518172332523,-222.069844580369,
8.89044045298038));
#86500=CARTESIAN_POINT('Ctrl Pts',(-157.819373458426,-222.975356516428,
8.73168258774858));
#86501=CARTESIAN_POINT('Ctrl Pts',(-157.116283909427,-225.733822089035,
8.57292472251679));
#86502=CARTESIAN_POINT('Ctrl Pts',(-159.05237121312,-227.820693714614,8.414166857285));
#86503=CARTESIAN_POINT('Ctrl Pts',(-161.855728345302,-227.3260665635,8.2554089920532));
#86504=CARTESIAN_POINT('Ctrl Pts',(-162.960722968838,-224.70262338494,8.09665112682141));
#86505=CARTESIAN_POINT('Ctrl Pts',(-161.356064047721,-222.35133927279,7.93789326158962));
#86506=CARTESIAN_POINT('Ctrl Pts',(-158.510335363456,-222.424109354026,
7.77913539635782));
#86507=CARTESIAN_POINT('Ctrl Pts',(-157.027947695977,-224.854334453163,
7.62037753112604));
#86508=CARTESIAN_POINT('Ctrl Pts',(-158.265582180266,-227.417872655037,
7.46161966589424));
#86509=CARTESIAN_POINT('Ctrl Pts',(-161.090555784972,-227.768573898102,
7.30286180066245));
#86510=CARTESIAN_POINT('Ctrl Pts',(-162.917452778156,-225.585476418495,
7.14410393543066));
#86511=CARTESIAN_POINT('Ctrl Pts',(-162.074297103498,-222.866550943705,
6.98534607019887));
#86512=CARTESIAN_POINT('Ctrl Pts',(-159.332744801288,-222.10015796134,6.82658820496707));
#86513=CARTESIAN_POINT('Ctrl Pts',(-157.2018644307,-223.987700298723,6.66783033973528));
#86514=CARTESIAN_POINT('Ctrl Pts',(-157.631837623101,-226.801699282907,
6.50907247450349));
#86515=CARTESIAN_POINT('Ctrl Pts',(-160.229152929714,-227.966783154224,
6.3503146092717));
#86516=CARTESIAN_POINT('Ctrl Pts',(-162.616747484064,-226.416667199462,
6.1915567440399));
#86517=CARTESIAN_POINT('Ctrl Pts',(-162.6094948439,-223.570017479461,6.03279887880812));
#86518=CARTESIAN_POINT('Ctrl Pts',(-160.214032625214,-222.032087706024,
5.87404101357632));
#86519=CARTESIAN_POINT('Ctrl Pts',(-157.622687756349,-223.210391147325,
5.71528314834453));
#86520=CARTESIAN_POINT('Ctrl Pts',(-157.207058959388,-226.026544540218,
5.55652528311273));
#86521=CARTESIAN_POINT('Ctrl Pts',(-159.347529692965,-227.903204410272,
5.39776741788094));
#86522=CARTESIAN_POINT('Ctrl Pts',(-162.085141225883,-227.122851718211,
5.23900955264915));
#86523=CARTESIAN_POINT('Ctrl Pts',(-162.914431590869,-224.399665217122,
5.08025168741736));
#86524=CARTESIAN_POINT('Ctrl Pts',(-161.076434278499,-222.225905085714,
4.92149382218557));
#86525=CARTESIAN_POINT('Ctrl Pts',(-158.253284356777,-222.590996510776,
4.76273595695377));
#86526=CARTESIAN_POINT('Ctrl Pts',(-157.028728523044,-225.160807834436,
4.60397809172198));
#86527=CARTESIAN_POINT('Ctrl Pts',(-158.523480228182,-227.583447834359,
4.44522022649019));
#86528=CARTESIAN_POINT('Ctrl Pts',(-161.369542770418,-227.641716477836,
4.2864623612584));
#86529=CARTESIAN_POINT('Ctrl Pts',(-162.962199823039,-225.282286304748,
4.1277044960266));
#86530=CARTESIAN_POINT('Ctrl Pts',(-161.843851714069,-222.664507716515,
3.96894663079481));
#86531=CARTESIAN_POINT('Ctrl Pts',(-159.038010588956,-222.184171574577,
3.81018876556302));
#86532=CARTESIAN_POINT('Ctrl Pts',(-157.112582134867,-224.280881496252,
3.65143090033122));
#86533=CARTESIAN_POINT('Ctrl Pts',(-157.829718397681,-227.035728645533,
3.49267303509944));
#86534=CARTESIAN_POINT('Ctrl Pts',(-160.533096297017,-227.927477015872,
3.33391516986764));
#86535=CARTESIAN_POINT('Ctrl Pts',(-162.748584487481,-226.139998541806,
3.17515730463585));
#86536=CARTESIAN_POINT('Ctrl Pts',(-162.448568260611,-223.309193435901,
3.01639943940406));
#86537=CARTESIAN_POINT('Ctrl Pts',(-159.907622463056,-222.025814454227,
2.85764157417227));
#86538=CARTESIAN_POINT('Ctrl Pts',(-157.451220573017,-223.464409918827,
2.69888370894047));
#86539=CARTESIAN_POINT('Ctrl Pts',(-157.32746153645,-226.308377465473,2.54012584370868));
#86540=CARTESIAN_POINT('Ctrl Pts',(-159.649609550717,-227.954917799371,
2.38136797847689));
#86541=CARTESIAN_POINT('Ctrl Pts',(-162.292434985658,-226.897117910672,
2.22261011324509));
#86542=CARTESIAN_POINT('Ctrl Pts',(-162.837223814186,-224.103074889997,
2.06385224801331));
#86543=CARTESIAN_POINT('Ctrl Pts',(-160.785385929749,-222.129899551328,
1.90509438278151));
#86544=CARTESIAN_POINT('Ctrl Pts',(-158.014762022095,-222.783436177899,
1.74633651754972));
#86545=CARTESIAN_POINT('Ctrl Pts',(-157.061029600014,-225.465579921422,
1.58757865231793));
#86546=CARTESIAN_POINT('Ctrl Pts',(-158.797039107366,-227.721608351042,
1.42882078708613));
#86547=CARTESIAN_POINT('Ctrl Pts',(-161.634005981492,-227.486855345816,
1.27006292185434));
#86548=CARTESIAN_POINT('Ctrl Pts',(-162.975514864611,-224.976061001026,
1.11130505662255));
#86549=CARTESIAN_POINT('Ctrl Pts',(-161.593865406306,-222.487323837059,
0.952547191390755));
#86550=CARTESIAN_POINT('Ctrl Pts',(-158.753442436207,-222.297880263058,
0.793789326158963));
#86551=CARTESIAN_POINT('Ctrl Pts',(-157.054009825035,-224.582054806988,
0.635031460927172));
#86552=CARTESIAN_POINT('Ctrl Pts',(-158.050453981591,-227.247409147313,
0.476273595695376));
#86553=CARTESIAN_POINT('Ctrl Pts',(-160.83171775712,-227.858697917409,0.317515730463588));
#86554=CARTESIAN_POINT('Ctrl Pts',(-162.850434099709,-225.84804452134,0.158757865231792));
#86555=CARTESIAN_POINT('Ctrl Pts',(-162.457434515453,-224.000243484622,
0.0529192884105984));
#86556=CARTESIAN_POINT('Ctrl Pts',(-161.913465996665,-223.364012796625,
0.));
#86557=CARTESIAN_POINT('Ctrl Pts',(-161.913465996665,-223.364012796625,
0.));
#86558=CARTESIAN_POINT('Ctrl Pts',(-161.975061821414,-223.421897746888,
-3.51911852623003E-16));
#86559=CARTESIAN_POINT('Ctrl Pts',(-162.033285691278,-223.482934384445,
4.3246434463342E-16));
#86560=CARTESIAN_POINT('Ctrl Pts',(-162.08814123845,-223.546737650339,6.66133814775094E-16));
#86561=CARTESIAN_POINT('Ctrl Pts',(-162.144450808367,-223.612232110736,
9.059970199533E-16));
#86562=CARTESIAN_POINT('Ctrl Pts',(-162.197211559747,-223.680642241593,
-9.91859996330672E-16));
#86563=CARTESIAN_POINT('Ctrl Pts',(-162.246401858891,-223.751600097819,
-1.38777878078145E-15));
#86564=CARTESIAN_POINT('Ctrl Pts',(-162.297290107341,-223.82500727525,-1.79736387824417E-15));
#86565=CARTESIAN_POINT('Ctrl Pts',(-162.344357741728,-223.901141619796,
4.27848227219236E-15));
#86566=CARTESIAN_POINT('Ctrl Pts',(-162.387545875999,-223.979639757331,
4.9960036108132E-15));
#86567=CARTESIAN_POINT('Ctrl Pts',(-162.406440684742,-224.013982692503,
5.30991919645982E-15));
#86568=CARTESIAN_POINT('Ctrl Pts',(-162.424592438936,-224.048778578827,
5.06079435892012E-15));
#86569=CARTESIAN_POINT('Ctrl Pts',(-162.441993762856,-224.083999076523,
5.27355936696949E-15));
#86570=CARTESIAN_POINT('Ctrl Pts',(-162.451521735226,-224.103283812009,
5.39005734880947E-15));
#86571=CARTESIAN_POINT('Ctrl Pts',(-162.460824698828,-224.122695867125,
-1.80422085998584E-15));
#86572=CARTESIAN_POINT('Ctrl Pts',(-162.469901237658,-224.142230719459,
-2.16493489801906E-15));
#86573=CARTESIAN_POINT('Ctrl Pts',(-162.478557397273,-224.160860816575,
-2.50894249247741E-15));
#86574=CARTESIAN_POINT('Ctrl Pts',(-162.487010116501,-224.17960861694,1.52748735518423E-15));
#86575=CARTESIAN_POINT('Ctrl Pts',(-162.495244043881,-224.198437344968,
1.49880108324396E-15));
#86576=CARTESIAN_POINT('Ctrl Pts',(-162.531783468902,-224.281992963608,
1.37150097062534E-15));
#86577=CARTESIAN_POINT('Ctrl Pts',(-162.564063480614,-224.367232235573,
-3.46659333174283E-15));
#86578=CARTESIAN_POINT('Ctrl Pts',(-162.592060384007,-224.45375591163,-1.30451205393456E-15));
#86579=CARTESIAN_POINT('Ctrl Pts',(-162.620521837946,-224.541715268642,
8.93444478518701E-16));
#86580=CARTESIAN_POINT('Ctrl Pts',(-162.644557356984,-224.631002763181,
4.3432970000933E-16));
#86581=CARTESIAN_POINT('Ctrl Pts',(-162.664102933426,-224.721236079534,
1.02695629777827E-15));
#86582=CARTESIAN_POINT('Ctrl Pts',(-162.683304934146,-224.809883258132,
1.60916559670726E-15));
#86583=CARTESIAN_POINT('Ctrl Pts',(-162.698173710175,-224.899444209412,
4.52079509896306E-15));
#86584=CARTESIAN_POINT('Ctrl Pts',(-162.708605924403,-224.989579250553,
5.16253706450698E-15));
#86585=CARTESIAN_POINT('Ctrl Pts',(-162.712739843743,-225.025296595084,
5.41683681955754E-15));
#86586=CARTESIAN_POINT('Ctrl Pts',(-162.716176611214,-225.061104267913,
1.34242000952038E-14));
#86587=CARTESIAN_POINT('Ctrl Pts',(-162.718907757196,-225.096981670027,
1.38500322321988E-14));
#86588=CARTESIAN_POINT('Ctrl Pts',(-162.720525958649,-225.118238997391,
1.41023373770799E-14));
#86589=CARTESIAN_POINT('Ctrl Pts',(-162.721896425303,-225.139520807707,
3.52876023556576E-15));
#86590=CARTESIAN_POINT('Ctrl Pts',(-162.723017191021,-225.160822839396,
3.3584246494911E-15));
#86591=CARTESIAN_POINT('Ctrl Pts',(-162.723759187735,-225.174925731069,
3.24565492153553E-15));
#86592=CARTESIAN_POINT('Ctrl Pts',(-162.72439165709,-225.189037398679,3.64992830526776E-15));
#86593=CARTESIAN_POINT('Ctrl Pts',(-162.724913686862,-225.203142207687,
3.69149155687865E-15));
#86594=CARTESIAN_POINT('Ctrl Pts',(-162.728436673681,-225.298330372776,
3.97198664573279E-15));
#86595=CARTESIAN_POINT('Ctrl Pts',(-162.726942917764,-225.39336773222,1.17756522009375E-14));
#86596=CARTESIAN_POINT('Ctrl Pts',(-162.720374349249,-225.487854987023,
1.06303854607859E-14));
#86597=CARTESIAN_POINT('Ctrl Pts',(-162.71382751348,-225.58202962157,9.48890794684939E-15));
#86598=CARTESIAN_POINT('Ctrl Pts',(-162.702239749738,-225.675658740134,
2.24970435481665E-15));
#86599=CARTESIAN_POINT('Ctrl Pts',(-162.685505553451,-225.768364895442,
2.91433543964104E-15));
#86600=CARTESIAN_POINT('Ctrl Pts',(-162.683601264249,-225.778914510579,
2.9899679812951E-15));
#86601=CARTESIAN_POINT('Ctrl Pts',(-162.681630276117,-225.789452183786,
5.32923785720578E-15));
#86602=CARTESIAN_POINT('Ctrl Pts',(-162.679592390737,-225.799977364968,
5.38458166943201E-15));
#86603=CARTESIAN_POINT('Ctrl Pts',(-162.662059174472,-225.890532152657,
5.863838114987E-15));
#86604=CARTESIAN_POINT('Ctrl Pts',(-162.63957844198,-225.980162557517,1.21988532545923E-14));
#86605=CARTESIAN_POINT('Ctrl Pts',(-162.612425094939,-226.068630980284,
1.37667655053519E-14));
#86606=CARTESIAN_POINT('Ctrl Pts',(-162.60172483783,-226.10349352847,1.43846290851872E-14));
#86607=CARTESIAN_POINT('Ctrl Pts',(-162.590298397256,-226.138175582511,
9.10155007490613E-15));
#86608=CARTESIAN_POINT('Ctrl Pts',(-162.578160429641,-226.172662264402,
9.74220704108575E-15));
#86609=CARTESIAN_POINT('Ctrl Pts',(-162.572850001538,-226.187750378864,
1.00224980144874E-14));
#86610=CARTESIAN_POINT('Ctrl Pts',(-162.567403364151,-226.202801093293,
1.26710079476777E-14));
#86611=CARTESIAN_POINT('Ctrl Pts',(-162.561821675617,-226.217813142587,
1.301736496373E-14));
#86612=CARTESIAN_POINT('Ctrl Pts',(-162.557400927301,-226.229702822785,
1.32916828849232E-14));
#86613=CARTESIAN_POINT('Ctrl Pts',(-162.552895865822,-226.241567036791,
-2.18922818415383E-15));
#86614=CARTESIAN_POINT('Ctrl Pts',(-162.548310798671,-226.253395997137,
-1.85962356624714E-15));
#86615=CARTESIAN_POINT('Ctrl Pts',(-162.514552420086,-226.340488837539,
5.67149501155898E-16));
#86616=CARTESIAN_POINT('Ctrl Pts',(-162.476411071193,-226.425806841494,
7.30675670375641E-15));
#86617=CARTESIAN_POINT('Ctrl Pts',(-162.434220018652,-226.509119275137,
8.24340595784179E-15));
#86618=CARTESIAN_POINT('Ctrl Pts',(-162.390446644469,-226.595556235402,
9.21518304820882E-15));
#86619=CARTESIAN_POINT('Ctrl Pts',(-162.342313990897,-226.679835090795,
1.02191638285051E-14));
#86620=CARTESIAN_POINT('Ctrl Pts',(-162.290138160741,-226.761695129367,
1.04777297948999E-14));
#86621=CARTESIAN_POINT('Ctrl Pts',(-162.237360636907,-226.844499181049,
1.07392775539542E-14));
#86622=CARTESIAN_POINT('Ctrl Pts',(-162.18044573594,-226.924829121338,9.48127483138641E-15));
#86623=CARTESIAN_POINT('Ctrl Pts',(-162.119668717606,-227.002400317474,
1.01307850997046E-14));
#86624=CARTESIAN_POINT('Ctrl Pts',(-162.076869286147,-227.057026279444,
1.05881729573591E-14));
#86625=CARTESIAN_POINT('Ctrl Pts',(-162.032153516023,-227.110283883549,
1.04004194029648E-14));
#86626=CARTESIAN_POINT('Ctrl Pts',(-161.985604112955,-227.162066010945,
1.1518563880486E-14));
#86627=CARTESIAN_POINT('Ctrl Pts',(-161.974398233174,-227.174531569172,
1.17877358089457E-14));
#86628=CARTESIAN_POINT('Ctrl Pts',(-161.963085448517,-227.186912117143,
1.11605785323705E-14));
#86629=CARTESIAN_POINT('Ctrl Pts',(-161.951678152587,-227.199194229367,
1.11993747609063E-14));
#86630=CARTESIAN_POINT('Ctrl Pts',(-161.883011874223,-227.273126469054,
1.14329088643908E-14));
#86631=CARTESIAN_POINT('Ctrl Pts',(-161.810832651604,-227.343597623949,
1.49981926778286E-14));
#86632=CARTESIAN_POINT('Ctrl Pts',(-161.735453614524,-227.410320720505,
1.35447209004269E-14));
#86633=CARTESIAN_POINT('Ctrl Pts',(-161.670633677549,-227.467697241631,
1.2294851538123E-14));
#86634=CARTESIAN_POINT('Ctrl Pts',(-161.603446552378,-227.522302286696,
8.96312012513312E-15));
#86635=CARTESIAN_POINT('Ctrl Pts',(-161.534065125301,-227.573938079886,
7.79931674799172E-15));
#86636=CARTESIAN_POINT('Ctrl Pts',(-161.508545380815,-227.592930659083,
7.37124880434049E-15));
#86637=CARTESIAN_POINT('Ctrl Pts',(-161.482728554244,-227.611521358039,
6.88696359544211E-15));
#86638=CARTESIAN_POINT('Ctrl Pts',(-161.456622539761,-227.629699683014,
6.67521593555875E-15));
#86639=CARTESIAN_POINT('Ctrl Pts',(-161.439930141174,-227.64132305227,6.53982275476302E-15));
#86640=CARTESIAN_POINT('Ctrl Pts',(-161.423118461496,-227.652778396977,
1.59935197070125E-14));
#86641=CARTESIAN_POINT('Ctrl Pts',(-161.406204349576,-227.664053326898,
1.52794443764037E-14));
#86642=CARTESIAN_POINT('Ctrl Pts',(-161.320010703824,-227.721509924092,
1.16405447178875E-14));
#86643=CARTESIAN_POINT('Ctrl Pts',(-161.23107539812,-227.774344401213,5.94975413786717E-15));
#86644=CARTESIAN_POINT('Ctrl Pts',(-161.139704794375,-227.822237400702,
6.55031584528842E-15));
#86645=CARTESIAN_POINT('Ctrl Pts',(-161.04833419063,-227.87013040019,7.15087755270967E-15));
#86646=CARTESIAN_POINT('Ctrl Pts',(-160.954527650215,-227.913082824186,
1.10522651367167E-15));
#86647=CARTESIAN_POINT('Ctrl Pts',(-160.858553721283,-227.95073486507,-2.17837900495788E-15));
#86648=CARTESIAN_POINT('Ctrl Pts',(-160.837669284134,-227.95892814933,-2.89637846893106E-15));
#86649=CARTESIAN_POINT('Ctrl Pts',(-160.816682095278,-227.966870267892,
8.4228218624679E-16));
#86650=CARTESIAN_POINT('Ctrl Pts',(-160.795596249024,-227.974562448592,
6.93889390390723E-16));
#86651=CARTESIAN_POINT('Ctrl Pts',(-162.514309543052,-224.998572563953,
19.1125833024919));
#86652=CARTESIAN_POINT('Ctrl Pts',(-162.515998915399,-224.67257072807,19.092036810933));
#86653=CARTESIAN_POINT('Ctrl Pts',(-162.457161966883,-224.347153821985,
19.071490319374));
#86654=CARTESIAN_POINT('Ctrl Pts',(-162.334969911996,-224.04757991362,19.0509438278151));
#86655=CARTESIAN_POINT('Ctrl Pts',(-162.020253573416,-223.276001076837,
18.9980245394045));
#86656=CARTESIAN_POINT('Ctrl Pts',(-161.28526154685,-222.675855677203,18.9451052509939));
#86657=CARTESIAN_POINT('Ctrl Pts',(-160.46633937388,-222.52175790764,18.8921859625832));
#86658=CARTESIAN_POINT('Ctrl Pts',(-159.647417200909,-222.367660138077,
18.8392666741726));
#86659=CARTESIAN_POINT('Ctrl Pts',(-158.744564881534,-222.659609998585,
18.7863473857621));
#86660=CARTESIAN_POINT('Ctrl Pts',(-158.170921255767,-223.264017180871,
18.7334280973515));
#86661=CARTESIAN_POINT('Ctrl Pts',(-157.59727763,-223.868424363157,18.6805088089409));
#86662=CARTESIAN_POINT('Ctrl Pts',(-157.352842697842,-224.785288867222,
18.6275895205303));
#86663=CARTESIAN_POINT('Ctrl Pts',(-157.549472946172,-225.595050650405,
18.5746702321197));
#86664=CARTESIAN_POINT('Ctrl Pts',(-157.746103194501,-226.404812433589,
18.5217509437091));
#86665=CARTESIAN_POINT('Ctrl Pts',(-158.383798623317,-227.107471495892,
18.4688316552985));
#86666=CARTESIAN_POINT('Ctrl Pts',(-159.170748339018,-227.381492444256,
18.4159123668879));
#86667=CARTESIAN_POINT('Ctrl Pts',(-159.95769805472,-227.65551339262,18.3629930784773));
#86668=CARTESIAN_POINT('Ctrl Pts',(-160.893902057306,-227.500896227044,
18.3100737900667));
#86669=CARTESIAN_POINT('Ctrl Pts',(-161.550954125836,-226.988393094392,
18.2571545016561));
#86670=CARTESIAN_POINT('Ctrl Pts',(-162.14929175983,-226.521687445794,18.2089641019347));
#86671=CARTESIAN_POINT('Ctrl Pts',(-162.51613860921,-225.7581996753,18.1607737022133));
#86672=CARTESIAN_POINT('Ctrl Pts',(-162.520906603697,-224.998703157721,
18.112583302492));
#86673=CARTESIAN_POINT('Origin',(-160.,225.,22.2084234471774));
#86674=CARTESIAN_POINT('Ctrl Pts',(-163.076377868511,225.002226294578,19.7084234471774));
#86675=CARTESIAN_POINT('Ctrl Pts',(-163.077562763763,225.146330752986,19.7009407276991));
#86676=CARTESIAN_POINT('Ctrl Pts',(-163.00282692276,226.308360985244,19.6405387198101));
#86677=CARTESIAN_POINT('Ctrl Pts',(-161.521864740257,228.298893686106,19.5272174235105));
#86678=CARTESIAN_POINT('Ctrl Pts',(-158.054123086354,228.067610661284,19.3684595582787));
#86679=CARTESIAN_POINT('Ctrl Pts',(-156.367330834239,225.02922603841,19.2097016930469));
#86680=CARTESIAN_POINT('Ctrl Pts',(-158.005117297794,221.963912747455,19.0509438278151));
#86681=CARTESIAN_POINT('Ctrl Pts',(-161.468639591425,221.677313620367,18.8921859625833));
#86682=CARTESIAN_POINT('Ctrl Pts',(-162.992852850625,223.658102562111,18.7780125023707));
#86683=CARTESIAN_POINT('Ctrl Pts',(-163.077320480262,224.836964798983,18.7167583305688));
#86684=CARTESIAN_POINT('Ctrl Pts',(-163.07593125098,224.997572466666,18.7084234471774));
#86685=CARTESIAN_POINT('Ctrl Pts',(-163.070362295124,224.996974657089,19.7915765528225));
#86686=CARTESIAN_POINT('Ctrl Pts',(-163.065080696031,225.700310975174,19.7552124583938));
#86687=CARTESIAN_POINT('Ctrl Pts',(-162.477826045596,227.437424363323,19.6659290755545));
#86688=CARTESIAN_POINT('Ctrl Pts',(-159.59272451442,228.609330199079,19.5237264043046));
#86689=CARTESIAN_POINT('Ctrl Pts',(-156.746988470599,226.616779048904,19.3649685390728));
#86690=CARTESIAN_POINT('Ctrl Pts',(-156.877197967362,223.143422642792,19.2062106738411));
#86691=CARTESIAN_POINT('Ctrl Pts',(-159.865978945628,221.369750585662,19.0474528086092));
#86692=CARTESIAN_POINT('Ctrl Pts',(-162.574488163549,222.717816747864,18.9092414349364));
#86693=CARTESIAN_POINT('Ctrl Pts',(-163.066355225813,224.374657820191,18.8239493496742));
#86694=CARTESIAN_POINT('Ctrl Pts',(-163.069604839599,225.001742689702,18.7915765528225));
#86695=CARTESIAN_POINT('Ctrl Pts',(-158.086534003335,226.635987203375,20.));
#86696=CARTESIAN_POINT('Ctrl Pts',(-157.542565484547,225.999756515379,19.9470807115894));
#86697=CARTESIAN_POINT('Ctrl Pts',(-157.149565275988,224.151956162406,19.8412421347682));
#86698=CARTESIAN_POINT('Ctrl Pts',(-159.168282436654,222.141301994169,19.6824842695364));
#86699=CARTESIAN_POINT('Ctrl Pts',(-161.94954585807,222.752591068708,19.5237264043046));
#86700=CARTESIAN_POINT('Ctrl Pts',(-162.945990110181,225.417945100886,19.3649685390728));
#86701=CARTESIAN_POINT('Ctrl Pts',(-161.24655750239,227.702119685951,19.206210673841));
#86702=CARTESIAN_POINT('Ctrl Pts',(-158.406134657523,227.512676050035,19.0474528086092));
#86703=CARTESIAN_POINT('Ctrl Pts',(-157.024485236765,225.023939011451,18.8886949433775));
#86704=CARTESIAN_POINT('Ctrl Pts',(-158.3659940775,222.513144734576,18.7299370781456));
#86705=CARTESIAN_POINT('Ctrl Pts',(-161.202960849655,222.278391748584,18.5711792129139));
#86706=CARTESIAN_POINT('Ctrl Pts',(-162.938970296779,224.534420092962,18.4124213476821));
#86707=CARTESIAN_POINT('Ctrl Pts',(-161.985237907903,227.216563745114,18.2536634824503));
#86708=CARTESIAN_POINT('Ctrl Pts',(-159.214614097946,227.87010034708,18.0949056172185));
#86709=CARTESIAN_POINT('Ctrl Pts',(-157.162776285685,225.896925078708,17.9361477519867));
#86710=CARTESIAN_POINT('Ctrl Pts',(-157.707565095056,223.102882155973,17.7773898867549));
#86711=CARTESIAN_POINT('Ctrl Pts',(-160.350390436945,222.045082304735,17.6186320215231));
#86712=CARTESIAN_POINT('Ctrl Pts',(-162.67253836946,223.691622580552,17.4598741562913));
#86713=CARTESIAN_POINT('Ctrl Pts',(-162.54877933725,226.535590027129,17.3011162910595));
#86714=CARTESIAN_POINT('Ctrl Pts',(-160.092377533692,227.974185441053,17.1423584258277));
#86715=CARTESIAN_POINT('Ctrl Pts',(-157.551431825594,226.690806504577,16.9836005605959));
#86716=CARTESIAN_POINT('Ctrl Pts',(-157.251415609286,223.860001498326,16.8248426953641));
#86717=CARTESIAN_POINT('Ctrl Pts',(-159.466903721751,222.072523087195,16.6660848301324));
#86718=CARTESIAN_POINT('Ctrl Pts',(-162.170281525912,222.964271426136,16.5073269649006));
#86719=CARTESIAN_POINT('Ctrl Pts',(-162.887417763478,225.71911847843,16.3485690996688));
#86720=CARTESIAN_POINT('Ctrl Pts',(-160.961989377177,227.815828326288,16.189811234437));
#86721=CARTESIAN_POINT('Ctrl Pts',(-158.156148350846,227.335492201262,16.0310533692052));
#86722=CARTESIAN_POINT('Ctrl Pts',(-157.037800281249,224.71771370519,15.8722955039734));
#86723=CARTESIAN_POINT('Ctrl Pts',(-158.630457277798,222.358283615169,15.7135376387416));
#86724=CARTESIAN_POINT('Ctrl Pts',(-161.476519719835,222.416552256594,15.5547797735098));
#86725=CARTESIAN_POINT('Ctrl Pts',(-162.971271372349,224.839192171226,15.396021908278));
#86726=CARTESIAN_POINT('Ctrl Pts',(-161.746715581728,227.409003404412,15.2372640430462));
#86727=CARTESIAN_POINT('Ctrl Pts',(-158.923565759399,227.77409481662,15.0785061778144));
#86728=CARTESIAN_POINT('Ctrl Pts',(-157.085568511738,225.600334761742,14.9197483125827));
#86729=CARTESIAN_POINT('Ctrl Pts',(-157.914858847527,222.877148356527,14.7609904473508));
#86730=CARTESIAN_POINT('Ctrl Pts',(-160.652470284063,222.096795691938,14.6022325821191));
#86731=CARTESIAN_POINT('Ctrl Pts',(-162.792940942283,223.973455495923,14.4434747168873));
#86732=CARTESIAN_POINT('Ctrl Pts',(-162.377312159954,226.78960878967,14.2847168516555));
#86733=CARTESIAN_POINT('Ctrl Pts',(-159.785967382321,227.967912189486,14.1259589864237));
#86734=CARTESIAN_POINT('Ctrl Pts',(-157.390505247971,226.429982470195,13.9672011211919));
#86735=CARTESIAN_POINT('Ctrl Pts',(-157.383252608062,223.583332850414,13.8084432559601));
#86736=CARTESIAN_POINT('Ctrl Pts',(-159.770847078353,222.033216950225,13.6496853907283));
#86737=CARTESIAN_POINT('Ctrl Pts',(-162.368162293525,223.198300780524,13.4909275254965));
#86738=CARTESIAN_POINT('Ctrl Pts',(-162.798135470788,226.012299665637,13.3321696602647));
#86739=CARTESIAN_POINT('Ctrl Pts',(-160.66725517522,227.899841936567,13.1734117950329));
#86740=CARTESIAN_POINT('Ctrl Pts',(-157.92570296953,227.133448981184,13.0146539298011));
#86741=CARTESIAN_POINT('Ctrl Pts',(-157.082547324556,224.414523602118,12.8558960645693));
#86742=CARTESIAN_POINT('Ctrl Pts',(-158.909444253422,222.231426199369,12.6971381993375));
#86743=CARTESIAN_POINT('Ctrl Pts',(-161.734417758671,222.582127430087,12.5383803341058));
#86744=CARTESIAN_POINT('Ctrl Pts',(-162.972052199389,225.145665541708,12.379622468874));
#86745=CARTESIAN_POINT('Ctrl Pts',(-161.489664584098,227.575890555287,12.2208646036422));
#86746=CARTESIAN_POINT('Ctrl Pts',(-158.643936000021,227.648660633961,12.0621067384104));
#86747=CARTESIAN_POINT('Ctrl Pts',(-157.039277135399,225.29737660459,11.9033488731786));
#86748=CARTESIAN_POINT('Ctrl Pts',(-158.144271720032,222.673933518393,11.7445910079468));
#86749=CARTESIAN_POINT('Ctrl Pts',(-160.947628753517,222.179306384692,11.585833142715));
#86750=CARTESIAN_POINT('Ctrl Pts',(-162.883715989048,224.2661779368,11.4270752774832));
#86751=CARTESIAN_POINT('Ctrl Pts',(-162.180626464802,227.024643412292,11.2683174122514));
#86752=CARTESIAN_POINT('Ctrl Pts',(-159.48182768572,227.930155316471,11.1095595470196));
#86753=CARTESIAN_POINT('Ctrl Pts',(-157.25726018829,226.153989190242,10.9508016817878));
#86754=CARTESIAN_POINT('Ctrl Pts',(-157.542848058682,223.321692202482,10.792043816556));
#86755=CARTESIAN_POINT('Ctrl Pts',(-160.077221289143,222.025382445013,10.6332859513242));
#86756=CARTESIAN_POINT('Ctrl Pts',(-162.540921598817,223.451442556894,10.4745280860925));
#86757=CARTESIAN_POINT('Ctrl Pts',(-162.679170561173,226.29474237981,10.3157702208607));
#86758=CARTESIAN_POINT('Ctrl Pts',(-160.3654427313,227.953094027638,10.1570123556289));
#86759=CARTESIAN_POINT('Ctrl Pts',(-157.717261728112,226.9087741375,9.99825449039708));
#86760=CARTESIAN_POINT('Ctrl Pts',(-157.158242701589,224.117544231782,9.83949662516528));
#86761=CARTESIAN_POINT('Ctrl Pts',(-159.199999842823,222.133937810436,9.6807387599335));
#86762=CARTESIAN_POINT('Ctrl Pts',(-161.973917096446,222.773351392274,9.5219808947017));
#86763=CARTESIAN_POINT('Ctrl Pts',(-162.941305501024,225.450593692342,9.36322302946991));
#86764=CARTESIAN_POINT('Ctrl Pts',(-161.216811226729,227.715452662898,9.20446516423812));
#86765=CARTESIAN_POINT('Ctrl Pts',(-158.378691365582,227.495129463153,9.04570729900632));
#86766=CARTESIAN_POINT('Ctrl Pts',(-157.024393102897,224.991263876849,8.88694943377453));
#86767=CARTESIAN_POINT('Ctrl Pts',(-158.393370155429,222.495393590109,8.72819156854274));
#86768=CARTESIAN_POINT('Ctrl Pts',(-161.232734778532,222.291738991211,8.56943370331094));
#86769=CARTESIAN_POINT('Ctrl Pts',(-162.943900580799,224.566684761056,8.41067583807915));
#86770=CARTESIAN_POINT('Ctrl Pts',(-161.960808687285,227.238200620543,8.25191797284736));
#86771=CARTESIAN_POINT('Ctrl Pts',(-159.183184760274,227.861315360124,8.09316010761557));
#86772=CARTESIAN_POINT('Ctrl Pts',(-157.15311010854,225.865754394638,7.93440224238377));
#86773=CARTESIAN_POINT('Ctrl Pts',(-157.728508973519,223.077855041224,7.77564437715198));
#86774=CARTESIAN_POINT('Ctrl Pts',(-160.382776336609,222.049102678496,7.6168865119202));
#86775=CARTESIAN_POINT('Ctrl Pts',(-162.686726811487,223.721011428366,7.4581286466884));
#86776=CARTESIAN_POINT('Ctrl Pts',(-162.531785014145,226.563450468702,7.29937078145661));
#86777=CARTESIAN_POINT('Ctrl Pts',(-160.059753671418,227.975019701562,7.14061291622482));
#86778=CARTESIAN_POINT('Ctrl Pts',(-157.533035770958,226.663851020543,6.98185505099302));
#86779=CARTESIAN_POINT('Ctrl Pts',(-157.264083435908,223.829925950952,6.82309718576123));
#86780=CARTESIAN_POINT('Ctrl Pts',(-159.499041832727,222.066852605038,6.66433932052944));
#86781=CARTESIAN_POINT('Ctrl Pts',(-162.192477124534,222.98819563965,6.50558145529764));
#86782=CARTESIAN_POINT('Ctrl Pts',(-162.879357438186,225.750741945742,6.34682359006585));
#86783=CARTESIAN_POINT('Ctrl Pts',(-160.931049937637,227.826209252613,6.18806572483406));
#86784=CARTESIAN_POINT('Ctrl Pts',(-158.130645570776,227.315129962631,6.02930785960227));
#86785=CARTESIAN_POINT('Ctrl Pts',(-157.04107430403,224.685243821889,5.87054999437047));
#86786=CARTESIAN_POINT('Ctrl Pts',(-158.659511717879,222.343422522977,5.71179212913868));
#86787=CARTESIAN_POINT('Ctrl Pts',(-161.504763954812,222.432900826569,5.55303426390689));
#86788=CARTESIAN_POINT('Ctrl Pts',(-162.972856279474,224.871788192736,5.39427639867509));
#86789=CARTESIAN_POINT('Ctrl Pts',(-161.720190654067,227.42801499987,5.23551853344331));
#86790=CARTESIAN_POINT('Ctrl Pts',(-158.893206609702,227.762122574602,5.07676066821151));
#86791=CARTESIAN_POINT('Ctrl Pts',(-157.079159832615,225.568335677676,4.91800280297972));
#86792=CARTESIAN_POINT('Ctrl Pts',(-157.938265861858,222.854407990891,4.75924493774793));
#86793=CARTESIAN_POINT('Ctrl Pts',(-160.684270893255,222.104126026468,4.60048707251613));
#86794=CARTESIAN_POINT('Ctrl Pts',(-162.80403123005,224.004147808747,4.44172920728434));
#86795=CARTESIAN_POINT('Ctrl Pts',(-162.357542295375,226.815573477294,4.28297134205255));
#86796=CARTESIAN_POINT('Ctrl Pts',(-159.753430744669,227.965386370829,4.12421347682076));
#86797=CARTESIAN_POINT('Ctrl Pts',(-157.37497936677,226.401277774369,3.96545561158896));
#86798=CARTESIAN_POINT('Ctrl Pts',(-157.398946769126,223.554719813958,3.80669774635717));
#86799=CARTESIAN_POINT('Ctrl Pts',(-159.803397986199,222.03088222288,3.64793988112538));
#86800=CARTESIAN_POINT('Ctrl Pts',(-162.387779358353,223.224381104868,3.48918201589359));
#86801=CARTESIAN_POINT('Ctrl Pts',(-162.786865156092,226.042926329434,3.3304241506618));
#86802=CARTESIAN_POINT('Ctrl Pts',(-160.635412071627,227.906985419191,3.17166628543));
#86803=CARTESIAN_POINT('Ctrl Pts',(-157.902429886146,227.110571565798,3.01290842019822));
#86804=CARTESIAN_POINT('Ctrl Pts',(-157.089143782333,224.382562702162,2.85415055496642));
#86805=CARTESIAN_POINT('Ctrl Pts',(-158.939873182857,222.219632421386,2.69539268973463));
#86806=CARTESIAN_POINT('Ctrl Pts',(-161.760830587323,222.601294455492,2.53663482450283));
#86807=CARTESIAN_POINT('Ctrl Pts',(-162.970275943658,225.178251675845,2.37787695927104));
#86808=CARTESIAN_POINT('Ctrl Pts',(-161.461324798163,227.592073039525,2.21911909403925));
#86809=CARTESIAN_POINT('Ctrl Pts',(-158.61496941047,227.633629114009,2.06036122880746));
#86810=CARTESIAN_POINT('Ctrl Pts',(-157.036193640954,225.264888228518,1.90160336357567));
#86811=CARTESIAN_POINT('Ctrl Pts',(-158.169894004685,222.653721020893,1.74284549834387));
#86812=CARTESIAN_POINT('Ctrl Pts',(-160.978505913143,222.189869541214,1.58408763311208));
#86813=CARTESIAN_POINT('Ctrl Pts',(-162.891592133019,224.297846652507,1.42532976788028));
#86814=CARTESIAN_POINT('Ctrl Pts',(-162.158287360937,227.048440070593,1.2665719026485));
#86815=CARTESIAN_POINT('Ctrl Pts',(-159.449730500729,227.924289615984,1.1078140374167));
#86816=CARTESIAN_POINT('Ctrl Pts',(-157.244754494171,226.123853490694,0.94905617218491));
#86817=CARTESIAN_POINT('Ctrl Pts',(-157.561432538852,223.294816748872,0.790298306953121));
#86818=CARTESIAN_POINT('Ctrl Pts',(-160.109776474582,222.026467288224,0.631540441721325));
#86819=CARTESIAN_POINT('Ctrl Pts',(-162.557883210969,223.479279814359,0.472782576489533));
#86820=CARTESIAN_POINT('Ctrl Pts',(-162.664537639372,226.324301704676,0.314024711257741));
#86821=CARTESIAN_POINT('Ctrl Pts',(-160.333598837337,227.956397769736,0.155266846025946));
#86822=CARTESIAN_POINT('Ctrl Pts',(-157.69529473125,226.88473924401,-0.00349101920584214));
#86823=CARTESIAN_POINT('Ctrl Pts',(-157.170583964077,224.084270038712,-0.162248884437638));
#86824=CARTESIAN_POINT('Ctrl Pts',(-158.541127016969,222.784105799646,-0.268087461258832));
#86825=CARTESIAN_POINT('Ctrl Pts',(-159.349800002025,222.567913197965,-0.32100674966943));
#86826=CARTESIAN_POINT('Ctrl Pts',(-157.945668449658,226.756425321227,20.1070022498898));
#86827=CARTESIAN_POINT('Ctrl Pts',(-157.361654052493,226.073356597808,20.0540829614792));
#86828=CARTESIAN_POINT('Ctrl Pts',(-156.939721951717,224.089524864994,19.948244384658));
#86829=CARTESIAN_POINT('Ctrl Pts',(-159.107053047018,221.930850343558,19.7894865194262));
#86830=CARTESIAN_POINT('Ctrl Pts',(-162.093067539247,222.587141301637,19.6307286541944));
#86831=CARTESIAN_POINT('Ctrl Pts',(-163.162868031566,225.448713386366,19.4719707889626));
#86832=CARTESIAN_POINT('Ctrl Pts',(-161.338326581679,227.90104435267,19.3132129237309));
#86833=CARTESIAN_POINT('Ctrl Pts',(-158.288797467133,227.697654253785,19.1544550584991));
#86834=CARTESIAN_POINT('Ctrl Pts',(-156.805433769257,225.025701353771,18.9956971932673));
#86835=CARTESIAN_POINT('Ctrl Pts',(-158.245701817598,222.330067405536,18.8369393280355));
#86836=CARTESIAN_POINT('Ctrl Pts',(-161.291520430245,222.078032372512,18.6781814628037));
#86837=CARTESIAN_POINT('Ctrl Pts',(-163.155331433491,224.500145027974,18.5194235975719));
#86838=CARTESIAN_POINT('Ctrl Pts',(-162.131387166664,227.379742751044,18.3606657323401));
#86839=CARTESIAN_POINT('Ctrl Pts',(-159.156795552889,228.081391415333,18.2019078671083));
#86840=CARTESIAN_POINT('Ctrl Pts',(-156.953905529623,225.962954915685,18.0431500018765));
#86841=CARTESIAN_POINT('Ctrl Pts',(-157.538800605529,222.963220120716,17.8843921366447));
#86842=CARTESIAN_POINT('Ctrl Pts',(-160.376185482683,221.827547152327,17.7256342714129));
#86843=CARTESIAN_POINT('Ctrl Pts',(-162.869285318606,223.595302442159,17.5668764061811));
#86844=CARTESIAN_POINT('Ctrl Pts',(-162.736415393061,226.648637104929,17.4081185409493));
#86845=CARTESIAN_POINT('Ctrl Pts',(-160.09917818364,228.193139046512,17.2493606757176));
#86846=CARTESIAN_POINT('Ctrl Pts',(-157.3711731159,226.815280310145,17.0906028104857));
#86847=CARTESIAN_POINT('Ctrl Pts',(-157.049070303595,223.776077080328,16.931844945254));
#86848=CARTESIAN_POINT('Ctrl Pts',(-159.427658236056,221.857008070509,16.7730870800222));
#86849=CARTESIAN_POINT('Ctrl Pts',(-162.330053327091,222.814405145161,16.6143292147904));
#86850=CARTESIAN_POINT('Ctrl Pts',(-163.099983705417,225.772058547812,16.4555713495586));
#86851=CARTESIAN_POINT('Ctrl Pts',(-161.032809118151,228.023123996518,16.2968134843268));
#86852=CARTESIAN_POINT('Ctrl Pts',(-158.020407666711,227.507426483142,16.138055619095));
#86853=CARTESIAN_POINT('Ctrl Pts',(-156.819729040783,224.696932350683,15.9792977538632));
#86854=CARTESIAN_POINT('Ctrl Pts',(-158.529634271702,222.163805719112,15.8205398886314));
#86855=CARTESIAN_POINT('Ctrl Pts',(-161.585218159323,222.226363981806,15.6617820233996));
#86856=CARTESIAN_POINT('Ctrl Pts',(-163.190010449876,224.827353819316,15.5030241581678));
#86857=CARTESIAN_POINT('Ctrl Pts',(-161.875305302144,227.586349434581,15.3442662929361));
#86858=CARTESIAN_POINT('Ctrl Pts',(-158.844320815635,227.978318149032,15.1855084277042));
#86859=CARTESIAN_POINT('Ctrl Pts',(-156.871013873211,225.644530210604,15.0267505624725));
#86860=CARTESIAN_POINT('Ctrl Pts',(-157.76135491098,222.720868248779,14.8679926972406));
#86861=CARTESIAN_POINT('Ctrl Pts',(-160.700503846187,221.883067576046,14.7092348320089));
#86862=CARTESIAN_POINT('Ctrl Pts',(-162.998551688911,223.897883335145,14.5504769667771));
#86863=CARTESIAN_POINT('Ctrl Pts',(-162.552325143858,226.92135622258,14.3917191015453));
#86864=CARTESIAN_POINT('Ctrl Pts',(-159.770210727515,228.186403970666,14.2329612363135));
#86865=CARTESIAN_POINT('Ctrl Pts',(-157.198399444313,226.535254930099,14.0742033710817));
#86866=CARTESIAN_POINT('Ctrl Pts',(-157.190612879506,223.479040637879,13.9154455058499));
#86867=CARTESIAN_POINT('Ctrl Pts',(-159.753977296899,221.814808294061,13.7566876406181));
#86868=CARTESIAN_POINT('Ctrl Pts',(-162.542501682495,223.065663274264,13.5979297753863));
#86869=CARTESIAN_POINT('Ctrl Pts',(-163.004128628254,226.086823149794,13.4391719101545));
#86870=CARTESIAN_POINT('Ctrl Pts',(-160.716377171569,228.113322521371,13.2804140449227));
#86871=CARTESIAN_POINT('Ctrl Pts',(-157.772997355635,227.290509243817,13.1216561796909));
#86872=CARTESIAN_POINT('Ctrl Pts',(-156.867770272249,224.371421996394,12.9628983144592));
#86873=CARTESIAN_POINT('Ctrl Pts',(-158.829159712529,222.027609313153,12.8041404492274));
#86874=CARTESIAN_POINT('Ctrl Pts',(-161.86210213786,222.404128469628,12.6453825839956));
#86875=CARTESIAN_POINT('Ctrl Pts',(-163.190848759847,225.156389148619,12.4866247187638));
#86876=CARTESIAN_POINT('Ctrl Pts',(-161.599330722299,227.765522484944,12.327866853532));
#86877=CARTESIAN_POINT('Ctrl Pts',(-158.544105270595,227.8436497518,12.1691089883002));
#86878=CARTESIAN_POINT('Ctrl Pts',(-156.821314617991,225.319268877632,12.0103511230684));
#86879=CARTESIAN_POINT('Ctrl Pts',(-158.007656702003,222.50269313921,11.8515932578366));
#86880=CARTESIAN_POINT('Ctrl Pts',(-161.017391293994,221.971652541579,11.6928353926048));
#86881=CARTESIAN_POINT('Ctrl Pts',(-163.09600941373,224.212155418808,11.534077527373));
#86882=CARTESIAN_POINT('Ctrl Pts',(-162.341159839768,227.173693625762,11.3753196621412));
#86883=CARTESIAN_POINT('Ctrl Pts',(-159.443680872514,228.145867511898,11.2165617969094));
#86884=CARTESIAN_POINT('Ctrl Pts',(-157.055345148858,226.238943574853,11.0578039316776));
#86885=CARTESIAN_POINT('Ctrl Pts',(-157.361957429172,223.198138526823,10.8990460664458));
#86886=CARTESIAN_POINT('Ctrl Pts',(-160.082906166569,221.806397028188,10.7402882012141));
#86887=CARTESIAN_POINT('Ctrl Pts',(-162.727979183582,223.33744084377,10.5815303359823));
#86888=CARTESIAN_POINT('Ctrl Pts',(-162.876405759056,226.390058733755,10.4227724707505));
#86889=CARTESIAN_POINT('Ctrl Pts',(-160.392345896954,228.17049492527,10.2640146055187));
#86890=CARTESIAN_POINT('Ctrl Pts',(-157.549211085388,227.049294285855,10.1052567402869));
#86891=CARTESIAN_POINT('Ctrl Pts',(-156.9490381921,224.052579596611,9.94649887505509));
#86892=CARTESIAN_POINT('Ctrl Pts',(-159.141105425426,221.922944023293,9.7877410098233));
#86893=CARTESIAN_POINT('Ctrl Pts',(-162.119232939627,222.609429958855,9.62898314459152));
#86894=CARTESIAN_POINT('Ctrl Pts',(-163.157838550818,225.483765502066,9.47022527935971));
#86895=CARTESIAN_POINT('Ctrl Pts',(-161.306390444479,227.91535887681,9.31146741412793));
#86896=CARTESIAN_POINT('Ctrl Pts',(-158.259333854726,227.678815922141,9.15270954889614));
#86897=CARTESIAN_POINT('Ctrl Pts',(-156.805334852677,224.990620740871,8.99395168366434));
#86898=CARTESIAN_POINT('Ctrl Pts',(-158.275093267831,222.311009457187,8.83519381843255));
#86899=CARTESIAN_POINT('Ctrl Pts',(-161.323486256436,222.092362212543,8.67643595320076));
#86900=CARTESIAN_POINT('Ctrl Pts',(-163.160624675195,224.53478495664,8.51767808796896));
#86901=CARTESIAN_POINT('Ctrl Pts',(-162.105159515504,227.402972490126,8.35892022273717));
#86902=CARTESIAN_POINT('Ctrl Pts',(-159.123052450008,228.071959695143,8.20016235750538));
#86903=CARTESIAN_POINT('Ctrl Pts',(-156.943527747778,225.929489507967,8.04140449227359));
#86904=CARTESIAN_POINT('Ctrl Pts',(-157.56128633059,222.936350559651,7.88264662704179));
#86905=CARTESIAN_POINT('Ctrl Pts',(-160.410955567745,221.831863497991,7.72388876181));
#86906=CARTESIAN_POINT('Ctrl Pts',(-162.884518285461,223.626854838386,7.56513089657821));
#86907=CARTESIAN_POINT('Ctrl Pts',(-162.718169981753,226.678548576692,7.40637303134641));
#86908=CARTESIAN_POINT('Ctrl Pts',(-160.064152617635,228.194034723617,7.24761516611462));
#86909=CARTESIAN_POINT('Ctrl Pts',(-157.35142278038,226.78634041709,7.08885730088283));
#86910=CARTESIAN_POINT('Ctrl Pts',(-157.062670710368,223.743787431088,6.93009943565105));
#86911=CARTESIAN_POINT('Ctrl Pts',(-159.46216229072,221.850920138755,6.77134157041924));
#86912=CARTESIAN_POINT('Ctrl Pts',(-162.353882921455,222.840090611599,6.61258370518746));
#86913=CARTESIAN_POINT('Ctrl Pts',(-163.091329995038,225.806010071771,6.45382583995566));
#86914=CARTESIAN_POINT('Ctrl Pts',(-160.999591978726,228.034269145954,6.29506797472387));
#86915=CARTESIAN_POINT('Ctrl Pts',(-157.993027422792,227.48556521708,6.13631010949207));
#86916=CARTESIAN_POINT('Ctrl Pts',(-156.823244090596,224.662072099277,5.97755224426028));
#86917=CARTESIAN_POINT('Ctrl Pts',(-158.560827641764,222.147850582927,5.81879437902849));
#86918=CARTESIAN_POINT('Ctrl Pts',(-161.615541678595,222.243916100925,5.6600365137967));
#86919=CARTESIAN_POINT('Ctrl Pts',(-163.191712034706,224.862349494975,5.50127864856491));
#86920=CARTESIAN_POINT('Ctrl Pts',(-161.846827662165,227.606760625812,5.34252078333311));
#86921=CARTESIAN_POINT('Ctrl Pts',(-158.811726685835,227.965464534414,5.18376291810132));
#86922=CARTESIAN_POINT('Ctrl Pts',(-156.864133399902,225.610175417734,5.02500505286953));
#86923=CARTESIAN_POINT('Ctrl Pts',(-157.786485103062,222.696453782739,4.86624718763774));
#86924=CARTESIAN_POINT('Ctrl Pts',(-160.734645552858,221.890937555196,4.70748932240594));
#86925=CARTESIAN_POINT('Ctrl Pts',(-163.010458421564,223.930835154879,4.54873145717415));
#86926=CARTESIAN_POINT('Ctrl Pts',(-162.531099861244,226.949232378767,4.38997359194236));
#86927=CARTESIAN_POINT('Ctrl Pts',(-159.735278807435,228.183692206272,4.23121572671057));
#86928=CARTESIAN_POINT('Ctrl Pts',(-157.181730578677,226.504437051767,4.07245786147877));
#86929=CARTESIAN_POINT('Ctrl Pts',(-157.207462413434,223.448321166697,3.91369999624699));
#86930=CARTESIAN_POINT('Ctrl Pts',(-159.788924537715,221.812301688742,3.75494213101519));
#86931=CARTESIAN_POINT('Ctrl Pts',(-162.563562916545,223.093663580116,3.5961842657834));
#86932=CARTESIAN_POINT('Ctrl Pts',(-162.992028615448,226.119704487549,3.4374264005516));
#86933=CARTESIAN_POINT('Ctrl Pts',(-160.682189842143,228.120991892951,3.27866853531981));
#86934=CARTESIAN_POINT('Ctrl Pts',(-157.748010954229,227.265947638699,3.11991067008802));
#86935=CARTESIAN_POINT('Ctrl Pts',(-156.874852348103,224.337108198673,2.96115280485623));
#86936=CARTESIAN_POINT('Ctrl Pts',(-158.861828759113,222.014947300736,2.80239493962444));
#86937=CARTESIAN_POINT('Ctrl Pts',(-161.890459426324,222.424706533249,2.64363707439264));
#86938=CARTESIAN_POINT('Ctrl Pts',(-163.188941739709,225.191374209016,2.48487920916085));
#86939=CARTESIAN_POINT('Ctrl Pts',(-161.568904617796,227.782896291425,2.32612134392906));
#86940=CARTESIAN_POINT('Ctrl Pts',(-158.513006218444,227.827511641304,2.16736347869727));
#86941=CARTESIAN_POINT('Ctrl Pts',(-156.81800412283,225.284388772055,2.00860561346547));
#86942=CARTESIAN_POINT('Ctrl Pts',(-158.035165248194,222.480992637923,1.84984774823368));
#86943=CARTESIAN_POINT('Ctrl Pts',(-161.050541568583,221.982993336634,1.69108988300189));
#86944=CARTESIAN_POINT('Ctrl Pts',(-163.104465383725,224.246155522258,1.5323320177701));
#86945=CARTESIAN_POINT('Ctrl Pts',(-162.317176175592,227.199242146627,1.37357415253831));
#86946=CARTESIAN_POINT('Ctrl Pts',(-159.409220756724,228.139569990229,1.21481628730651));
#86947=CARTESIAN_POINT('Ctrl Pts',(-157.041918810458,226.206589345156,1.05605842207472));
#86948=CARTESIAN_POINT('Ctrl Pts',(-157.381910061739,223.169284555873,0.897300556842932));
#86949=CARTESIAN_POINT('Ctrl Pts',(-160.117857999888,221.807561735395,0.738542691611135));
#86950=CARTESIAN_POINT('Ctrl Pts',(-162.746189475821,223.367327424658,0.579784826379343));
#86951=CARTESIAN_POINT('Ctrl Pts',(-162.860695590711,226.421794157215,0.421026961147551));
#86952=CARTESIAN_POINT('Ctrl Pts',(-160.358157718974,228.174041882278,0.262269095915756));
#86953=CARTESIAN_POINT('Ctrl Pts',(-157.525626921991,227.023489991401,0.103511230683968));
#86954=CARTESIAN_POINT('Ctrl Pts',(-156.96228799374,224.016855823753,-0.055246634547828));
#86955=CARTESIAN_POINT('Ctrl Pts',(-158.43372769508,222.620976084267,-0.161085211369022));
#86956=CARTESIAN_POINT('Ctrl Pts',(-159.301933573839,222.388867814061,-0.21400449977962));
#86957=CARTESIAN_POINT('Ctrl Pts',(-157.804802895981,226.876863439079,20.2140044997796));
#86958=CARTESIAN_POINT('Ctrl Pts',(-157.180742620438,226.146956680238,20.161085211369));
#86959=CARTESIAN_POINT('Ctrl Pts',(-156.729878627447,224.027093567582,20.0552466345478));
#86960=CARTESIAN_POINT('Ctrl Pts',(-159.045823657383,221.720398692947,19.896488769316));
#86961=CARTESIAN_POINT('Ctrl Pts',(-162.236589220423,222.421691534567,19.7377309040842));
#86962=CARTESIAN_POINT('Ctrl Pts',(-163.379745952951,225.479481671847,19.5789730388525));
#86963=CARTESIAN_POINT('Ctrl Pts',(-161.430095660968,228.099969019388,19.4202151736207));
#86964=CARTESIAN_POINT('Ctrl Pts',(-158.171460276744,227.882632457535,19.2614573083889));
#86965=CARTESIAN_POINT('Ctrl Pts',(-156.586382301748,225.02746369609,19.1026994431571));
#86966=CARTESIAN_POINT('Ctrl Pts',(-158.125409557696,222.146990076495,18.9439415779253));
#86967=CARTESIAN_POINT('Ctrl Pts',(-161.380080010835,221.877672996439,18.7851837126935));
#86968=CARTESIAN_POINT('Ctrl Pts',(-163.371692570201,224.465869962988,18.6264258474617));
#86969=CARTESIAN_POINT('Ctrl Pts',(-162.277536425426,227.542921756974,18.4676679822299));
#86970=CARTESIAN_POINT('Ctrl Pts',(-159.098977007832,228.292682483585,18.3089101169981));
#86971=CARTESIAN_POINT('Ctrl Pts',(-156.745034773561,226.028984752661,18.1501522517663));
#86972=CARTESIAN_POINT('Ctrl Pts',(-157.370036116003,222.823558085459,17.9913943865345));
#86973=CARTESIAN_POINT('Ctrl Pts',(-160.401980528422,221.610011999918,17.8326365213027));
#86974=CARTESIAN_POINT('Ctrl Pts',(-163.066032267751,223.498982303766,17.6738786560709));
#86975=CARTESIAN_POINT('Ctrl Pts',(-162.924051448872,226.761684182729,17.5151207908392));
#86976=CARTESIAN_POINT('Ctrl Pts',(-160.105978833588,228.412092651971,17.3563629256073));
#86977=CARTESIAN_POINT('Ctrl Pts',(-157.190914406205,226.939754115711,17.1976050603756));
#86978=CARTESIAN_POINT('Ctrl Pts',(-156.846724997903,223.69215266233,17.0388471951438));
#86979=CARTESIAN_POINT('Ctrl Pts',(-159.388412750362,221.641493053823,16.880089329912));
#86980=CARTESIAN_POINT('Ctrl Pts',(-162.489825128271,222.664538864185,16.7213314646802));
#86981=CARTESIAN_POINT('Ctrl Pts',(-163.312549647356,225.824998617194,16.5625735994484));
#86982=CARTESIAN_POINT('Ctrl Pts',(-161.103628859126,228.230419666749,16.4038157342166));
#86983=CARTESIAN_POINT('Ctrl Pts',(-157.884666982576,227.679360765022,16.2450578689848));
#86984=CARTESIAN_POINT('Ctrl Pts',(-156.601657800316,224.676150996176,16.086300003753));
#86985=CARTESIAN_POINT('Ctrl Pts',(-158.428811265605,221.969327823056,15.9275421385212));
#86986=CARTESIAN_POINT('Ctrl Pts',(-161.69391659881,222.036175707019,15.7687842732894));
#86987=CARTESIAN_POINT('Ctrl Pts',(-163.408749527404,224.815515467406,15.6100264080576));
#86988=CARTESIAN_POINT('Ctrl Pts',(-162.00389502256,227.763695464751,15.4512685428258));
#86989=CARTESIAN_POINT('Ctrl Pts',(-158.765075871872,228.182541481444,15.2925106775941));
#86990=CARTESIAN_POINT('Ctrl Pts',(-156.656459234684,225.688725659466,15.1337528123623));
#86991=CARTESIAN_POINT('Ctrl Pts',(-157.607850974432,222.56458814103,14.9749949471305));
#86992=CARTESIAN_POINT('Ctrl Pts',(-160.748537408311,221.669339460152,14.8162370818987));
#86993=CARTESIAN_POINT('Ctrl Pts',(-163.204162435539,223.822311174369,14.6574792166669));
#86994=CARTESIAN_POINT('Ctrl Pts',(-162.727338127762,227.053103655491,14.4987213514351));
#86995=CARTESIAN_POINT('Ctrl Pts',(-159.754454072708,228.404895751845,14.3399634862033));
#86996=CARTESIAN_POINT('Ctrl Pts',(-157.006293640655,226.640527390004,14.1812056209715));
#86997=CARTESIAN_POINT('Ctrl Pts',(-156.99797315095,223.374748425344,14.0224477557397));
#86998=CARTESIAN_POINT('Ctrl Pts',(-159.737107515444,221.596399637898,13.8636898905079));
#86999=CARTESIAN_POINT('Ctrl Pts',(-162.716841071466,222.933025768004,13.7049320252761));
#87000=CARTESIAN_POINT('Ctrl Pts',(-163.210121785719,226.161346633951,13.5461741600443));
#87001=CARTESIAN_POINT('Ctrl Pts',(-160.765499167917,228.326803106175,13.3874162948126));
#87002=CARTESIAN_POINT('Ctrl Pts',(-157.62029174174,227.447569506451,13.2286584295807));
#87003=CARTESIAN_POINT('Ctrl Pts',(-156.652993219943,224.328320390671,13.069900564349));
#87004=CARTESIAN_POINT('Ctrl Pts',(-158.748875171636,221.823792426936,12.9111426991172));
#87005=CARTESIAN_POINT('Ctrl Pts',(-161.989786517048,222.226129509168,12.7523848338854));
#87006=CARTESIAN_POINT('Ctrl Pts',(-163.409645320305,225.167112755529,12.5936269686536));
#87007=CARTESIAN_POINT('Ctrl Pts',(-161.708996860499,227.955154414602,12.4348691034218));
#87008=CARTESIAN_POINT('Ctrl Pts',(-158.444274541169,228.038638869639,12.27611123819));
#87009=CARTESIAN_POINT('Ctrl Pts',(-156.603352100584,225.341161150675,12.1173533729582));
#87010=CARTESIAN_POINT('Ctrl Pts',(-157.871041683974,222.331452760028,11.9585955077264));
#87011=CARTESIAN_POINT('Ctrl Pts',(-161.087153834472,221.763998698466,11.7998376424946));
#87012=CARTESIAN_POINT('Ctrl Pts',(-163.308302838412,224.158132900815,11.6410797772628));
#87013=CARTESIAN_POINT('Ctrl Pts',(-162.501693214734,227.322743839232,11.482321912031));
#87014=CARTESIAN_POINT('Ctrl Pts',(-159.405534059307,228.361579707324,11.3235640467992));
#87015=CARTESIAN_POINT('Ctrl Pts',(-156.853430109426,226.323897959464,11.1648061815675));
#87016=CARTESIAN_POINT('Ctrl Pts',(-157.181066799662,223.074584851163,11.0060483163356));
#87017=CARTESIAN_POINT('Ctrl Pts',(-160.088591043995,221.587411611363,10.8472904511039));
#87018=CARTESIAN_POINT('Ctrl Pts',(-162.915036768348,223.223439130646,10.6885325858721));
#87019=CARTESIAN_POINT('Ctrl Pts',(-163.073640956939,226.485375087701,10.5297747206403));
#87020=CARTESIAN_POINT('Ctrl Pts',(-160.419249062608,228.387895822902,10.3710168554085));
#87021=CARTESIAN_POINT('Ctrl Pts',(-157.381160442664,227.189814434209,10.2122589901767));
#87022=CARTESIAN_POINT('Ctrl Pts',(-156.739833682611,223.98761496144,10.0535011249449));
#87023=CARTESIAN_POINT('Ctrl Pts',(-159.082211008029,221.71195023615,9.89474325971311));
#87024=CARTESIAN_POINT('Ctrl Pts',(-162.264548782808,222.445508525436,9.73598539448133));
#87025=CARTESIAN_POINT('Ctrl Pts',(-163.374371600612,225.51693731179,9.57722752924952));
#87026=CARTESIAN_POINT('Ctrl Pts',(-161.39596966223,228.115265090722,9.41846966401774));
#87027=CARTESIAN_POINT('Ctrl Pts',(-158.13997634387,227.86250238113,9.25971179878594));
#87028=CARTESIAN_POINT('Ctrl Pts',(-156.586276602457,224.989977604893,9.10095393355415));
#87029=CARTESIAN_POINT('Ctrl Pts',(-158.156816380233,222.126625324264,8.94219606832236));
#87030=CARTESIAN_POINT('Ctrl Pts',(-161.414237734339,221.892985433876,8.78343820309056));
#87031=CARTESIAN_POINT('Ctrl Pts',(-163.377348769591,224.502885152224,8.62468033785878));
#87032=CARTESIAN_POINT('Ctrl Pts',(-162.249510343725,227.567744359708,8.46592247262697));
#87033=CARTESIAN_POINT('Ctrl Pts',(-159.062920139741,228.282604030162,8.30716460739519));
#87034=CARTESIAN_POINT('Ctrl Pts',(-156.733945387017,225.993224621296,8.14840674216339));
#87035=CARTESIAN_POINT('Ctrl Pts',(-157.39406368766,222.794846078078,7.98964887693161));
#87036=CARTESIAN_POINT('Ctrl Pts',(-160.439134798881,221.614624317487,7.83089101169981));
#87037=CARTESIAN_POINT('Ctrl Pts',(-163.082309759434,223.532698248405,7.67213314646802));
#87038=CARTESIAN_POINT('Ctrl Pts',(-162.904554949362,226.793646684682,7.51337528123623));
#87039=CARTESIAN_POINT('Ctrl Pts',(-160.068551563853,228.413049745672,7.35461741600443));
#87040=CARTESIAN_POINT('Ctrl Pts',(-157.169809789801,226.908829813637,7.19585955077264));
#87041=CARTESIAN_POINT('Ctrl Pts',(-156.861257984829,223.657648911225,7.03710168554085));
#87042=CARTESIAN_POINT('Ctrl Pts',(-159.425282748714,221.634987672473,6.87834382030905));
#87043=CARTESIAN_POINT('Ctrl Pts',(-162.515288718375,222.691985583548,6.71958595507727));
#87044=CARTESIAN_POINT('Ctrl Pts',(-163.303302551891,225.861278197799,6.56082808984547));
#87045=CARTESIAN_POINT('Ctrl Pts',(-161.068134019816,228.242329039294,6.40207022461368));
#87046=CARTESIAN_POINT('Ctrl Pts',(-157.855409274808,227.656000471528,6.24331235938189));
#87047=CARTESIAN_POINT('Ctrl Pts',(-156.605413877162,224.638900376664,6.08455449415009));
#87048=CARTESIAN_POINT('Ctrl Pts',(-158.462143565649,221.952278642878,5.92579662891831));
#87049=CARTESIAN_POINT('Ctrl Pts',(-161.726319402379,222.05493137528,5.7670387636865));
#87050=CARTESIAN_POINT('Ctrl Pts',(-163.410567789938,224.852910797215,5.60828089845472));
#87051=CARTESIAN_POINT('Ctrl Pts',(-161.973464670263,227.785506251754,5.44952303322292));
#87052=CARTESIAN_POINT('Ctrl Pts',(-158.730246761968,228.168806494225,5.29076516799113));
#87053=CARTESIAN_POINT('Ctrl Pts',(-156.649106967188,225.652015157792,5.13200730275933));
#87054=CARTESIAN_POINT('Ctrl Pts',(-157.634704344266,222.538499574588,4.97324943752755));
#87055=CARTESIAN_POINT('Ctrl Pts',(-160.78502021246,221.677749083923,4.81449157229575));
#87056=CARTESIAN_POINT('Ctrl Pts',(-163.216885613078,223.857522501011,4.65573370706397));
#87057=CARTESIAN_POINT('Ctrl Pts',(-162.704657427114,227.08289128024,4.49697584183217));
#87058=CARTESIAN_POINT('Ctrl Pts',(-159.7171268702,228.401998041715,4.33821797660038));
#87059=CARTESIAN_POINT('Ctrl Pts',(-156.988481790584,226.607596329165,4.17946011136858));
#87060=CARTESIAN_POINT('Ctrl Pts',(-157.015978057742,223.341922519436,4.02070224613679));
#87061=CARTESIAN_POINT('Ctrl Pts',(-159.774451089232,221.593721154604,3.861944380905));
#87062=CARTESIAN_POINT('Ctrl Pts',(-162.739346474737,222.962946055363,3.70318651567321));
#87063=CARTESIAN_POINT('Ctrl Pts',(-163.197192074805,226.196482645664,3.54442865044142));
#87064=CARTESIAN_POINT('Ctrl Pts',(-160.728967612659,228.33499836671,3.38567078520962));
#87065=CARTESIAN_POINT('Ctrl Pts',(-157.593592022312,227.4213237116,3.22691291997783));
#87066=CARTESIAN_POINT('Ctrl Pts',(-156.660560913873,224.291653695184,3.06815505474604));
#87067=CARTESIAN_POINT('Ctrl Pts',(-158.783784335368,221.810262180086,2.90939718951425));
#87068=CARTESIAN_POINT('Ctrl Pts',(-162.020088265325,222.248118611005,2.75063932428246));
#87069=CARTESIAN_POINT('Ctrl Pts',(-163.407607535759,225.204496742187,2.59188145905066));
#87070=CARTESIAN_POINT('Ctrl Pts',(-161.676484437429,227.973719543325,2.43312359381887));
#87071=CARTESIAN_POINT('Ctrl Pts',(-158.411043026418,228.021394168598,2.27436572858708));
#87072=CARTESIAN_POINT('Ctrl Pts',(-156.599814604706,225.303889315591,2.11560786335528));
#87073=CARTESIAN_POINT('Ctrl Pts',(-157.900436491704,222.308264254952,1.95684999812349));
#87074=CARTESIAN_POINT('Ctrl Pts',(-161.122577224023,221.776117132055,1.7980921328917));
#87075=CARTESIAN_POINT('Ctrl Pts',(-163.317338634431,224.194464392009,1.6393342676599));
#87076=CARTESIAN_POINT('Ctrl Pts',(-162.476064990247,227.350044222662,1.48057640242812));
#87077=CARTESIAN_POINT('Ctrl Pts',(-159.36871101272,228.354850364474,1.32181853719632));
#87078=CARTESIAN_POINT('Ctrl Pts',(-156.839083126746,226.289325199618,1.16306067196453));
#87079=CARTESIAN_POINT('Ctrl Pts',(-157.202387584625,223.043752362873,1.00430280673274));
#87080=CARTESIAN_POINT('Ctrl Pts',(-160.125939525193,221.588656182565,0.845544941500944));
#87081=CARTESIAN_POINT('Ctrl Pts',(-162.934495740674,223.255375034957,0.686787076269154));
#87082=CARTESIAN_POINT('Ctrl Pts',(-163.056853542051,226.519286609754,0.528029211037361));
#87083=CARTESIAN_POINT('Ctrl Pts',(-160.38271660061,228.39168599482,0.369271345805566));
#87084=CARTESIAN_POINT('Ctrl Pts',(-157.355959112733,227.162240738792,0.210513480573778));
#87085=CARTESIAN_POINT('Ctrl Pts',(-156.753992023402,223.949441608794,0.0517556153419821));
#87086=CARTESIAN_POINT('Ctrl Pts',(-158.326328373191,222.457846368889,-0.0540829614792118));
#87087=CARTESIAN_POINT('Ctrl Pts',(-159.254067145653,222.209822430158,-0.10700224988981));
#87088=CARTESIAN_POINT('Ctrl Pts',(-157.663937342304,226.997301556931,20.3210067496694));
#87089=CARTESIAN_POINT('Ctrl Pts',(-156.999831188384,226.220556762668,20.2680874612588));
#87090=CARTESIAN_POINT('Ctrl Pts',(-156.520035303177,223.96466227017,20.1622488844377));
#87091=CARTESIAN_POINT('Ctrl Pts',(-158.984594267748,221.509947042336,20.0034910192058));
#87092=CARTESIAN_POINT('Ctrl Pts',(-162.3801109016,222.256241767497,19.8447331539741));
#87093=CARTESIAN_POINT('Ctrl Pts',(-163.596623874336,225.510249957328,19.6859752887423));
#87094=CARTESIAN_POINT('Ctrl Pts',(-161.521864740257,228.298893686106,19.5272174235105));
#87095=CARTESIAN_POINT('Ctrl Pts',(-158.054123086354,228.067610661284,19.3684595582787));
#87096=CARTESIAN_POINT('Ctrl Pts',(-156.367330834239,225.02922603841,19.2097016930469));
#87097=CARTESIAN_POINT('Ctrl Pts',(-158.005117297794,221.963912747455,19.0509438278151));
#87098=CARTESIAN_POINT('Ctrl Pts',(-161.468639591425,221.677313620367,18.8921859625833));
#87099=CARTESIAN_POINT('Ctrl Pts',(-163.588053706912,224.431594898001,18.7334280973515));
#87100=CARTESIAN_POINT('Ctrl Pts',(-162.423685684187,227.706100762903,18.5746702321197));
#87101=CARTESIAN_POINT('Ctrl Pts',(-159.041158462775,228.503973551838,18.4159123668879));
#87102=CARTESIAN_POINT('Ctrl Pts',(-156.536164017499,226.095014589637,18.2571545016561));
#87103=CARTESIAN_POINT('Ctrl Pts',(-157.201271626476,222.683896050202,18.0983966364243));
#87104=CARTESIAN_POINT('Ctrl Pts',(-160.427775574161,221.392476847509,17.9396387711926));
#87105=CARTESIAN_POINT('Ctrl Pts',(-163.262779216896,223.402662165373,17.7808809059608));
#87106=CARTESIAN_POINT('Ctrl Pts',(-163.111687504683,226.874731260529,17.622123040729));
#87107=CARTESIAN_POINT('Ctrl Pts',(-160.112779483536,228.631046257429,17.4633651754972));
#87108=CARTESIAN_POINT('Ctrl Pts',(-157.01065569651,227.064227921279,17.3046073102654));
#87109=CARTESIAN_POINT('Ctrl Pts',(-156.644379692211,223.608228244332,17.1458494450336));
#87110=CARTESIAN_POINT('Ctrl Pts',(-159.349167264668,221.425978037138,16.9870915798018));
#87111=CARTESIAN_POINT('Ctrl Pts',(-162.64959692945,222.514672583209,16.82833371457));
#87112=CARTESIAN_POINT('Ctrl Pts',(-163.525115589295,225.877938686576,16.6695758493382));
#87113=CARTESIAN_POINT('Ctrl Pts',(-161.1744486001,228.437715336979,16.5108179841064));
#87114=CARTESIAN_POINT('Ctrl Pts',(-157.748926298441,227.851295046903,16.3520601188746));
#87115=CARTESIAN_POINT('Ctrl Pts',(-156.383586559849,224.655369641669,16.1933022536428));
#87116=CARTESIAN_POINT('Ctrl Pts',(-158.327988259509,221.774849926999,16.034544388411));
#87117=CARTESIAN_POINT('Ctrl Pts',(-161.802615038297,221.845987432231,15.8757865231792));
#87118=CARTESIAN_POINT('Ctrl Pts',(-163.627488604931,224.803677115496,15.7170286579474));
#87119=CARTESIAN_POINT('Ctrl Pts',(-162.132484742975,227.94104149492,15.5582707927157));
#87120=CARTESIAN_POINT('Ctrl Pts',(-158.685830928108,228.386764813856,15.3995129274839));
#87121=CARTESIAN_POINT('Ctrl Pts',(-156.441904596157,225.732921108328,15.2407550622521));
#87122=CARTESIAN_POINT('Ctrl Pts',(-157.454347037885,222.408308033282,15.0819971970203));
#87123=CARTESIAN_POINT('Ctrl Pts',(-160.796570970435,221.455611344259,14.9232393317885));
#87124=CARTESIAN_POINT('Ctrl Pts',(-163.409773182167,223.746739013592,14.7644814665567));
#87125=CARTESIAN_POINT('Ctrl Pts',(-162.902351111666,227.184851088401,14.6057236013249));
#87126=CARTESIAN_POINT('Ctrl Pts',(-159.738697417901,228.623387533023,14.4469657360931));
#87127=CARTESIAN_POINT('Ctrl Pts',(-156.814187836997,226.745799849908,14.2882078708613));
#87128=CARTESIAN_POINT('Ctrl Pts',(-156.805333422394,223.270456212809,14.1294500056295));
#87129=CARTESIAN_POINT('Ctrl Pts',(-159.720237733989,221.377990981734,13.9706921403977));
#87130=CARTESIAN_POINT('Ctrl Pts',(-162.891180460436,222.800388261744,13.8119342751659));
#87131=CARTESIAN_POINT('Ctrl Pts',(-163.416114943184,226.235870118108,13.6531764099341));
#87132=CARTESIAN_POINT('Ctrl Pts',(-160.814621164266,228.540283690979,13.4944185447024));
#87133=CARTESIAN_POINT('Ctrl Pts',(-157.467586127845,227.604629769084,13.3356606794706));
#87134=CARTESIAN_POINT('Ctrl Pts',(-156.438216167636,224.285218784948,13.1769028142388));
#87135=CARTESIAN_POINT('Ctrl Pts',(-158.668590630742,221.61997554072,13.018144949007));
#87136=CARTESIAN_POINT('Ctrl Pts',(-162.117470896237,222.048130548708,12.8593870837752));
#87137=CARTESIAN_POINT('Ctrl Pts',(-163.628441880763,225.17783636244,12.7006292185434));
#87138=CARTESIAN_POINT('Ctrl Pts',(-161.8186629987,228.14478634426,12.5418713533116));
#87139=CARTESIAN_POINT('Ctrl Pts',(-158.344443811744,228.233627987479,12.3831134880798));
#87140=CARTESIAN_POINT('Ctrl Pts',(-156.385389583177,225.363053423717,12.224355622848));
#87141=CARTESIAN_POINT('Ctrl Pts',(-157.734426665945,222.160212380846,12.0655977576162));
#87142=CARTESIAN_POINT('Ctrl Pts',(-161.156916374949,221.556344855353,11.9068398923844));
#87143=CARTESIAN_POINT('Ctrl Pts',(-163.520596263094,224.104110382822,11.7480820271526));
#87144=CARTESIAN_POINT('Ctrl Pts',(-162.6622265897,227.471794052703,11.5893241619208));
#87145=CARTESIAN_POINT('Ctrl Pts',(-159.367387246101,228.577291902751,11.4305662966891));
#87146=CARTESIAN_POINT('Ctrl Pts',(-156.651515069994,226.408852344075,11.2718084314573));
#87147=CARTESIAN_POINT('Ctrl Pts',(-157.000176170152,222.951031175503,11.1130505662255));
#87148=CARTESIAN_POINT('Ctrl Pts',(-160.094275921422,221.368426194538,10.9542927009937));
#87149=CARTESIAN_POINT('Ctrl Pts',(-163.102094353113,223.109437417523,10.7955348357619));
#87150=CARTESIAN_POINT('Ctrl Pts',(-163.270876154823,226.580691441646,10.6367769705301));
#87151=CARTESIAN_POINT('Ctrl Pts',(-160.446152228262,228.605296720535,10.4780191052983));
#87152=CARTESIAN_POINT('Ctrl Pts',(-157.213109799941,227.330334582564,10.3192612400665));
#87153=CARTESIAN_POINT('Ctrl Pts',(-156.530629173122,223.922650326269,10.1605033748347));
#87154=CARTESIAN_POINT('Ctrl Pts',(-159.023316590632,221.500956449007,10.0017455096029));
#87155=CARTESIAN_POINT('Ctrl Pts',(-162.409864625989,222.281587092017,9.84298764437113));
#87156=CARTESIAN_POINT('Ctrl Pts',(-163.590904650406,225.550109121514,9.68422977913934));
#87157=CARTESIAN_POINT('Ctrl Pts',(-161.485548879981,228.315171304634,9.52547191390754));
#87158=CARTESIAN_POINT('Ctrl Pts',(-158.020618833015,228.046188840119,9.36671404867576));
#87159=CARTESIAN_POINT('Ctrl Pts',(-156.367218352237,224.989334468915,9.20795618344395));
#87160=CARTESIAN_POINT('Ctrl Pts',(-158.038539492636,221.942241191341,9.04919831821217));
#87161=CARTESIAN_POINT('Ctrl Pts',(-161.504989212242,221.693608655208,8.89044045298038));
#87162=CARTESIAN_POINT('Ctrl Pts',(-163.594072863987,224.470985347808,8.73168258774859));
#87163=CARTESIAN_POINT('Ctrl Pts',(-162.393861171944,227.732516229291,8.57292472251679));
#87164=CARTESIAN_POINT('Ctrl Pts',(-159.002787829475,228.493248365181,8.414166857285));
#87165=CARTESIAN_POINT('Ctrl Pts',(-156.524363026255,226.056959734625,8.2554089920532));
#87166=CARTESIAN_POINT('Ctrl Pts',(-157.226841044731,222.653341596505,8.09665112682142));
#87167=CARTESIAN_POINT('Ctrl Pts',(-160.467314030017,221.397385136983,7.93789326158962));
#87168=CARTESIAN_POINT('Ctrl Pts',(-163.280101233408,223.438541658425,7.77913539635783));
#87169=CARTESIAN_POINT('Ctrl Pts',(-163.090939916971,226.908744792673,7.62037753112604));
#87170=CARTESIAN_POINT('Ctrl Pts',(-160.07295051007,228.632064767727,7.46161966589424));
#87171=CARTESIAN_POINT('Ctrl Pts',(-156.988196799222,227.031319210184,7.30286180066245));
#87172=CARTESIAN_POINT('Ctrl Pts',(-156.65984525929,223.571510391361,7.14410393543066));
#87173=CARTESIAN_POINT('Ctrl Pts',(-159.388403206707,221.41905520619,6.98534607019887));
#87174=CARTESIAN_POINT('Ctrl Pts',(-162.676694515296,222.543880555497,6.82658820496707));
#87175=CARTESIAN_POINT('Ctrl Pts',(-163.515275108744,225.916546323828,6.66783033973529));
#87176=CARTESIAN_POINT('Ctrl Pts',(-161.136676060905,228.450388932634,6.50907247450349));
#87177=CARTESIAN_POINT('Ctrl Pts',(-157.717791126824,227.826435725977,6.3503146092717));
#87178=CARTESIAN_POINT('Ctrl Pts',(-156.387583663728,224.615728654052,6.1915567440399));
#87179=CARTESIAN_POINT('Ctrl Pts',(-158.363459489534,221.756706702828,6.03279887880811));
#87180=CARTESIAN_POINT('Ctrl Pts',(-161.837097126162,221.865946649636,5.87404101357632));
#87181=CARTESIAN_POINT('Ctrl Pts',(-163.62942354517,224.843472099454,5.71528314834452));
#87182=CARTESIAN_POINT('Ctrl Pts',(-162.100101678361,227.964251877696,5.55652528311274));
#87183=CARTESIAN_POINT('Ctrl Pts',(-158.648766838101,228.372148454037,5.39776741788094));
#87184=CARTESIAN_POINT('Ctrl Pts',(-156.434080534475,225.69385489785,5.23900955264915));
#87185=CARTESIAN_POINT('Ctrl Pts',(-157.48292358547,222.380545366436,5.08025168741736));
#87186=CARTESIAN_POINT('Ctrl Pts',(-160.835394872063,221.464560612651,4.92149382218557));
#87187=CARTESIAN_POINT('Ctrl Pts',(-163.423312804591,223.784209847143,4.76273595695377));
#87188=CARTESIAN_POINT('Ctrl Pts',(-162.878214992983,227.216550181714,4.60397809172198));
#87189=CARTESIAN_POINT('Ctrl Pts',(-159.698974932965,228.620303877157,4.44522022649019));
#87190=CARTESIAN_POINT('Ctrl Pts',(-156.79523300249,226.710755606563,4.28646236125839));
#87191=CARTESIAN_POINT('Ctrl Pts',(-156.82449370205,223.235523872175,4.1277044960266));
#87192=CARTESIAN_POINT('Ctrl Pts',(-159.759977640748,221.375140620465,3.96894663079481));
#87193=CARTESIAN_POINT('Ctrl Pts',(-162.915130032929,222.832228530611,3.81018876556302));
#87194=CARTESIAN_POINT('Ctrl Pts',(-163.402355534161,226.273260803779,3.65143090033122));
#87195=CARTESIAN_POINT('Ctrl Pts',(-160.775745383176,228.54900484047,3.49267303509943));
#87196=CARTESIAN_POINT('Ctrl Pts',(-157.439173090395,227.576699784501,3.33391516986764));
#87197=CARTESIAN_POINT('Ctrl Pts',(-156.446269479642,224.246199191696,3.17515730463585));
#87198=CARTESIAN_POINT('Ctrl Pts',(-158.705739911624,221.605577059435,3.01639943940406));
#87199=CARTESIAN_POINT('Ctrl Pts',(-162.149717104325,222.071530688761,2.85764157417226));
#87200=CARTESIAN_POINT('Ctrl Pts',(-163.62627333181,225.217619275357,2.69888370894047));
#87201=CARTESIAN_POINT('Ctrl Pts',(-161.784064257062,228.164542795226,2.54012584370868));
#87202=CARTESIAN_POINT('Ctrl Pts',(-158.309079834391,228.215276695892,2.38136797847689));
#87203=CARTESIAN_POINT('Ctrl Pts',(-156.381625086582,225.323389859127,2.22261011324509));
#87204=CARTESIAN_POINT('Ctrl Pts',(-157.765707735213,222.135535871982,2.0638522480133));
#87205=CARTESIAN_POINT('Ctrl Pts',(-161.194612879462,221.569240927476,1.90509438278151));
#87206=CARTESIAN_POINT('Ctrl Pts',(-163.530211885137,224.14277326176,1.74633651754971));
#87207=CARTESIAN_POINT('Ctrl Pts',(-162.634953804902,227.500846298696,1.58757865231793));
#87208=CARTESIAN_POINT('Ctrl Pts',(-159.328201268715,228.570130738719,1.42882078708613));
#87209=CARTESIAN_POINT('Ctrl Pts',(-156.636247443033,226.37206105408,1.27006292185434));
#87210=CARTESIAN_POINT('Ctrl Pts',(-157.022865107512,222.918220169874,1.11130505662255));
#87211=CARTESIAN_POINT('Ctrl Pts',(-160.134021050498,221.369750629735,0.952547191390755));
#87212=CARTESIAN_POINT('Ctrl Pts',(-163.122802005527,223.143422645256,0.793789326158964));
#87213=CARTESIAN_POINT('Ctrl Pts',(-163.25301149339,226.616779062293,0.635031460927171));
#87214=CARTESIAN_POINT('Ctrl Pts',(-160.407275482247,228.609330107362,0.476273595695376));
#87215=CARTESIAN_POINT('Ctrl Pts',(-157.186291303474,227.300991486183,0.317515730463588));
#87216=CARTESIAN_POINT('Ctrl Pts',(-156.545696053065,223.882027393836,0.158757865231792));
#87217=CARTESIAN_POINT('Ctrl Pts',(-158.218929051303,222.29471665351,0.0529192884105984));
#87218=CARTESIAN_POINT('Ctrl Pts',(-159.206200717467,222.030777046254,0.));
#87219=CARTESIAN_POINT('Ctrl Pts',(-159.206200717467,222.030777046254,0.));
#87220=CARTESIAN_POINT('Ctrl Pts',(-159.113164836944,222.064809986938,4.63034655208678E-16));
#87221=CARTESIAN_POINT('Ctrl Pts',(-159.022195960155,222.103614880716,2.71860146874827E-18));
#87222=CARTESIAN_POINT('Ctrl Pts',(-158.933501628106,222.146862335309,5.55111512312578E-17));
#87223=CARTESIAN_POINT('Ctrl Pts',(-158.842828980427,222.191074418795,1.09481232003075E-16));
#87224=CARTESIAN_POINT('Ctrl Pts',(-158.754532809116,222.239930072316,3.09433814103877E-15));
#87225=CARTESIAN_POINT('Ctrl Pts',(-158.668863782053,222.29312293841,2.55351295663786E-15));
#87226=CARTESIAN_POINT('Ctrl Pts',(-158.585928546965,222.344618362203,2.02994609300867E-15));
#87227=CARTESIAN_POINT('Ctrl Pts',(-158.50545513685,222.400179468892,-1.45413356794216E-15));
#87228=CARTESIAN_POINT('Ctrl Pts',(-158.427704668138,222.459558987316,-2.4980018054066E-15));
#87229=CARTESIAN_POINT('Ctrl Pts',(-158.359673008016,222.511516065936,-3.41138651318799E-15));
#87230=CARTESIAN_POINT('Ctrl Pts',(-158.293726396571,222.566397333241,3.31443200639852E-15));
#87231=CARTESIAN_POINT('Ctrl Pts',(-158.230065006024,222.624050100838,4.49640324973188E-15));
#87232=CARTESIAN_POINT('Ctrl Pts',(-158.216686222763,222.636166139703,4.74480085697196E-15));
#87233=CARTESIAN_POINT('Ctrl Pts',(-158.203406550876,222.648406529201,-1.97156843780396E-16));
#87234=CARTESIAN_POINT('Ctrl Pts',(-158.19024514275,222.660753435868,0.));
#87235=CARTESIAN_POINT('Ctrl Pts',(-158.117820229753,222.72869629065,1.08491941895841E-15));
#87236=CARTESIAN_POINT('Ctrl Pts',(-158.048861076532,222.799961265629,3.84701060022766E-15));
#87237=CARTESIAN_POINT('Ctrl Pts',(-157.983606900735,222.874256342348,3.85802501057242E-15));
#87238=CARTESIAN_POINT('Ctrl Pts',(-157.91871036732,222.94814422569,3.86897905359346E-15));
#87239=CARTESIAN_POINT('Ctrl Pts',(-157.857477825039,223.025029886816,6.98233960792838E-15));
#87240=CARTESIAN_POINT('Ctrl Pts',(-157.800188199579,223.104652829295,6.9111383282916E-15));
#87241=CARTESIAN_POINT('Ctrl Pts',(-157.744357483621,223.182248132977,6.84175022551745E-15));
#87242=CARTESIAN_POINT('Ctrl Pts',(-157.692271158803,223.262443821962,-5.23084561579274E-16));
#87243=CARTESIAN_POINT('Ctrl Pts',(-157.644234173771,223.345012877019,-4.16333634234434E-16));
#87244=CARTESIAN_POINT('Ctrl Pts',(-157.623520285302,223.380617238873,-3.70301877629731E-16));
#87245=CARTESIAN_POINT('Ctrl Pts',(-157.603559952642,223.416663019726,-2.91706587269718E-15));
#87246=CARTESIAN_POINT('Ctrl Pts',(-157.584380601027,223.453132347144,-3.46944695195361E-15));
#87247=CARTESIAN_POINT('Ctrl Pts',(-157.571170272066,223.478251643241,-3.84991527617551E-15));
#87248=CARTESIAN_POINT('Ctrl Pts',(-157.558330491145,223.503571879617,3.30872527225209E-15));
#87249=CARTESIAN_POINT('Ctrl Pts',(-157.545870750695,223.529087219283,3.52495810318487E-15));
#87250=CARTESIAN_POINT('Ctrl Pts',(-157.539658105459,223.541809615391,3.6327755872119E-15));
#87251=CARTESIAN_POINT('Ctrl Pts',(-157.533540500235,223.554579541051,5.24877045946864E-16));
#87252=CARTESIAN_POINT('Ctrl Pts',(-157.527524300936,223.567384747645,2.4980018054066E-16));
#87253=CARTESIAN_POINT('Ctrl Pts',(-157.487323769582,223.652949750335,-1.58827658575181E-15));
#87254=CARTESIAN_POINT('Ctrl Pts',(-157.451579839888,223.7402249579,-8.46591886096976E-15));
#87255=CARTESIAN_POINT('Ctrl Pts',(-157.420543550398,223.828972297192,-5.57887069874141E-15));
#87256=CARTESIAN_POINT('Ctrl Pts',(-157.390193293269,223.915757947517,-2.75563842743794E-15));
#87257=CARTESIAN_POINT('Ctrl Pts',(-157.364344642025,224.003952043901,3.01207522017872E-16));
#87258=CARTESIAN_POINT('Ctrl Pts',(-157.343281489985,224.093340708165,7.21644966006352E-16));
#87259=CARTESIAN_POINT('Ctrl Pts',(-157.339658573778,224.108715787825,7.93961285378772E-16));
#87260=CARTESIAN_POINT('Ctrl Pts',(-157.336177360488,224.124126216227,3.93408136349463E-15));
#87261=CARTESIAN_POINT('Ctrl Pts',(-157.332839452763,224.139570909969,3.99680288865056E-15));
#87262=CARTESIAN_POINT('Ctrl Pts',(-157.312711861727,224.232702447729,4.37608524451406E-15));
#87263=CARTESIAN_POINT('Ctrl Pts',(-157.29779090409,224.327080946637,-3.10799959844018E-16));
#87264=CARTESIAN_POINT('Ctrl Pts',(-157.28799827831,224.422298268421,-1.4432899320127E-15));
#87265=CARTESIAN_POINT('Ctrl Pts',(-157.284735582254,224.454022668725,-1.82061166869276E-15));
#87266=CARTESIAN_POINT('Ctrl Pts',(-157.282042584831,224.48584006534,8.80200877206319E-15));
#87267=CARTESIAN_POINT('Ctrl Pts',(-157.279917589015,224.517734904248,9.15933995315754E-15));
#87268=CARTESIAN_POINT('Ctrl Pts',(-157.278692787876,224.536118392216,9.36529783516321E-15));
#87269=CARTESIAN_POINT('Ctrl Pts',(-157.277656694263,224.554527602168,6.51887382620648E-15));
#87270=CARTESIAN_POINT('Ctrl Pts',(-157.276809068708,224.572959507432,6.77236045021345E-15));
#87271=CARTESIAN_POINT('Ctrl Pts',(-157.276234543042,224.585452762959,6.94417519866532E-15));
#87272=CARTESIAN_POINT('Ctrl Pts',(-157.275746722798,224.597954820887,4.16905420329119E-15));
#87273=CARTESIAN_POINT('Ctrl Pts',(-157.275345652497,224.610455351992,4.16333634234434E-15));
#87274=CARTESIAN_POINT('Ctrl Pts',(-157.272356009785,224.703636327093,4.12071448459771E-15));
#87275=CARTESIAN_POINT('Ctrl Pts',(-157.274175040167,224.796878521229,3.65420848031107E-15));
#87276=CARTESIAN_POINT('Ctrl Pts',(-157.28066394211,224.889807515738,4.37150315946155E-15));
#87277=CARTESIAN_POINT('Ctrl Pts',(-157.287165695516,224.982920558858,5.09021846185362E-15));
#87278=CARTESIAN_POINT('Ctrl Pts',(-157.29835621947,225.075720140589,3.27636343276335E-15));
#87279=CARTESIAN_POINT('Ctrl Pts',(-157.314146920592,225.16781758215,2.5951463200613E-15));
#87280=CARTESIAN_POINT('Ctrl Pts',(-157.329714993719,225.258616571636,1.92353346735484E-15));
#87281=CARTESIAN_POINT('Ctrl Pts',(-157.349754912718,225.34873392575,5.78387140447215E-15));
#87282=CARTESIAN_POINT('Ctrl Pts',(-157.374224827573,225.437772014373,5.70377078901174E-15));
#87283=CARTESIAN_POINT('Ctrl Pts',(-157.383741664711,225.472400699991,5.67261806467303E-15));
#87284=CARTESIAN_POINT('Ctrl Pts',(-157.393929005722,225.506865798334,1.39646007254645E-15));
#87285=CARTESIAN_POINT('Ctrl Pts',(-157.404785957261,225.541142454069,2.4980018054066E-16));
#87286=CARTESIAN_POINT('Ctrl Pts',(-157.410770219746,225.560035465086,-3.82229330717133E-16));
#87287=CARTESIAN_POINT('Ctrl Pts',(-157.416957933028,225.578871208808,4.76239706612756E-15));
#87288=CARTESIAN_POINT('Ctrl Pts',(-157.423349053532,225.597645396291,4.94049245958195E-15));
#87289=CARTESIAN_POINT('Ctrl Pts',(-157.428584730572,225.613025419601,5.08639018779692E-15));
#87290=CARTESIAN_POINT('Ctrl Pts',(-157.433957191302,225.628364651371,1.41988730813603E-15));
#87291=CARTESIAN_POINT('Ctrl Pts',(-157.439460918369,225.64364605392,1.66533453693773E-15));
#87292=CARTESIAN_POINT('Ctrl Pts',(-157.471855948626,225.733592646819,3.1100410614556E-15));
#87293=CARTESIAN_POINT('Ctrl Pts',(-157.508835933315,225.821662943619,3.31193101344564E-15));
#87294=CARTESIAN_POINT('Ctrl Pts',(-157.550328254259,225.907414095892,3.49026363366534E-15));
#87295=CARTESIAN_POINT('Ctrl Pts',(-157.581447494966,225.971727460097,3.62401309883011E-15));
#87296=CARTESIAN_POINT('Ctrl Pts',(-157.615106070035,226.034735769921,1.73102608059913E-15));
#87297=CARTESIAN_POINT('Ctrl Pts',(-157.651290671058,226.096235103398,7.49400541621981E-16));
#87298=CARTESIAN_POINT('Ctrl Pts',(-157.665717951457,226.120755703417,3.58013418418384E-16));
#87299=CARTESIAN_POINT('Ctrl Pts',(-157.680546954031,226.145036228956,4.50893100540133E-15));
#87300=CARTESIAN_POINT('Ctrl Pts',(-157.695777423898,226.169062946708,4.2257863874795E-15));
#87301=CARTESIAN_POINT('Ctrl Pts',(-157.706206438561,226.185515163475,4.03190403206177E-15));
#87302=CARTESIAN_POINT('Ctrl Pts',(-157.716819306202,226.201841333482,9.48857707092389E-15));
#87303=CARTESIAN_POINT('Ctrl Pts',(-157.727611563923,226.218031534773,9.45771239102555E-15));
#87304=CARTESIAN_POINT('Ctrl Pts',(-157.775201280265,226.28942411146,9.32161099321723E-15));
#87305=CARTESIAN_POINT('Ctrl Pts',(-157.826300157625,226.358212936193,2.36509029748788E-15));
#87306=CARTESIAN_POINT('Ctrl Pts',(-157.880874323238,226.424045534683,1.60982338570648E-15));
#87307=CARTESIAN_POINT('Ctrl Pts',(-157.931843006989,226.48552885477,9.04453730645144E-16));
#87308=CARTESIAN_POINT('Ctrl Pts',(-157.985843474429,226.544433784549,2.05927059619376E-15));
#87309=CARTESIAN_POINT('Ctrl Pts',(-158.042870847355,226.600438912347,4.47124975933022E-16));
#87310=CARTESIAN_POINT('Ctrl Pts',(-158.056034879742,226.613366972652,7.5849346180632E-17));
#87311=CARTESIAN_POINT('Ctrl Pts',(-158.069360289123,226.626140355812,9.46940075139361E-16));
#87312=CARTESIAN_POINT('Ctrl Pts',(-158.082843691308,226.638757663408,7.49400541621981E-16));
#87313=CARTESIAN_POINT('Ctrl Pts',(-162.519491434632,224.998011610487,18.387416697508));
#87314=CARTESIAN_POINT('Ctrl Pts',(-162.520629350597,224.866458071072,18.3957515808994));
#87315=CARTESIAN_POINT('Ctrl Pts',(-162.511214998764,224.735067810581,18.4040864642907));
#87316=CARTESIAN_POINT('Ctrl Pts',(-162.490679990779,224.605439310924,18.4124213476821));
#87317=CARTESIAN_POINT('Ctrl Pts',(-162.360300481071,223.782410644836,18.4653406360927));
#87318=CARTESIAN_POINT('Ctrl Pts',(-161.781630665363,223.03040119671,18.5182599245033));
#87319=CARTESIAN_POINT('Ctrl Pts',(-161.01946796215,222.693521970312,18.5711792129139));
#87320=CARTESIAN_POINT('Ctrl Pts',(-160.257305258936,222.356642743915,18.6240985013245));
#87321=CARTESIAN_POINT('Ctrl Pts',(-159.311649668218,222.434893739245,18.6770177897351));
#87322=CARTESIAN_POINT('Ctrl Pts',(-158.61523706607,222.892484949723,18.7299370781457));
#87323=CARTESIAN_POINT('Ctrl Pts',(-157.918824463922,223.350076160201,18.7828563665563));
#87324=CARTESIAN_POINT('Ctrl Pts',(-157.471654850343,224.187007585826,18.8357756549669));
#87325=CARTESIAN_POINT('Ctrl Pts',(-157.478344947014,225.020262805069,18.8886949433775));
#87326=CARTESIAN_POINT('Ctrl Pts',(-157.485035043684,225.853518024313,18.9416142317881));
#87327=CARTESIAN_POINT('Ctrl Pts',(-157.945584850604,226.683097037174,18.9945335201987));
#87328=CARTESIAN_POINT('Ctrl Pts',(-158.649263561541,227.129460482924,19.0474528086093));
#87329=CARTESIAN_POINT('Ctrl Pts',(-159.352942272479,227.575823928674,19.1003720970199));
#87330=CARTESIAN_POINT('Ctrl Pts',(-160.299749887435,227.638971807313,19.1532913854305));
#87331=CARTESIAN_POINT('Ctrl Pts',(-161.056392462878,227.289849982455,19.2062106738411));
#87332=CARTESIAN_POINT('Ctrl Pts',(-161.813035038321,226.940728157596,19.2591299622517));
#87333=CARTESIAN_POINT('Ctrl Pts',(-162.379512574251,226.179336629241,19.3120492506623));
#87334=CARTESIAN_POINT('Ctrl Pts',(-162.496677300197,225.354415193034,19.3649685390729));
#87335=CARTESIAN_POINT('Ctrl Pts',(-162.513244242107,225.237772360444,19.3724512585512));
#87336=CARTESIAN_POINT('Ctrl Pts',(-162.520827804709,225.119859336471,19.3799339780296));
#87337=CARTESIAN_POINT('Ctrl Pts',(-162.519857258493,225.0018235551,19.387416697508));
#87338=CARTESIAN_POINT('Ctrl Pts',(-160.793799282533,222.030777046254,20.));
#87339=CARTESIAN_POINT('Ctrl Pts',(-161.781070948697,222.29471665351,19.9470807115894));
#87340=CARTESIAN_POINT('Ctrl Pts',(-163.454303903543,223.882027706698,19.8412421347682));
#87341=CARTESIAN_POINT('Ctrl Pts',(-162.813708733919,227.30099142385,19.6824842695364));
#87342=CARTESIAN_POINT('Ctrl Pts',(-159.59272451442,228.609330199079,19.5237264043046));
#87343=CARTESIAN_POINT('Ctrl Pts',(-156.746988470599,226.616779048904,19.3649685390728));
#87344=CARTESIAN_POINT('Ctrl Pts',(-156.877197967362,223.143422642792,19.2062106738411));
#87345=CARTESIAN_POINT('Ctrl Pts',(-159.865978945628,221.369750585662,19.0474528086092));
#87346=CARTESIAN_POINT('Ctrl Pts',(-162.977134923396,222.918220153796,18.8886949433775));
#87347=CARTESIAN_POINT('Ctrl Pts',(-163.363752589082,226.372061065279,18.7299370781457));
#87348=CARTESIAN_POINT('Ctrl Pts',(-160.671798738453,228.570130775029,18.5711792129139));
#87349=CARTESIAN_POINT('Ctrl Pts',(-157.365046168866,227.50084632268,18.4124213476821));
#87350=CARTESIAN_POINT('Ctrl Pts',(-156.469788080311,224.142773253644,18.2536634824503));
#87351=CARTESIAN_POINT('Ctrl Pts',(-158.805387108694,221.569240893567,18.0949056172185));
#87352=CARTESIAN_POINT('Ctrl Pts',(-162.234292286814,222.135535843889,17.9361477519867));
#87353=CARTESIAN_POINT('Ctrl Pts',(-163.618374948983,225.323389862265,17.7773898867549));
#87354=CARTESIAN_POINT('Ctrl Pts',(-161.690920182255,228.21527672754,17.6186320215231));
#87355=CARTESIAN_POINT('Ctrl Pts',(-158.215935725382,228.164542826343,17.4598741562913));
#87356=CARTESIAN_POINT('Ctrl Pts',(-156.373726632524,225.217619277503,17.3011162910595));
#87357=CARTESIAN_POINT('Ctrl Pts',(-157.850282874527,222.071530659953,17.1423584258277));
#87358=CARTESIAN_POINT('Ctrl Pts',(-161.294260101108,221.605577026048,16.9836005605959));
#87359=CARTESIAN_POINT('Ctrl Pts',(-163.553730555313,224.24619918428,16.8248426953642));
#87360=CARTESIAN_POINT('Ctrl Pts',(-162.560826934795,227.576699809846,16.6660848301323));
#87361=CARTESIAN_POINT('Ctrl Pts',(-159.224254609194,228.54900487538,16.5073269649006));
#87362=CARTESIAN_POINT('Ctrl Pts',(-156.597644432372,226.273260816304,16.3485690996688));
#87363=CARTESIAN_POINT('Ctrl Pts',(-157.084869938397,222.832228509288,16.189811234437));
#87364=CARTESIAN_POINT('Ctrl Pts',(-160.240022361613,221.37514058481,16.0310533692052));
#87365=CARTESIAN_POINT('Ctrl Pts',(-163.175506329186,223.235523854818,15.8722955039734));
#87366=CARTESIAN_POINT('Ctrl Pts',(-163.204767029033,226.710755623391,15.7135376387416));
#87367=CARTESIAN_POINT('Ctrl Pts',(-160.301025069996,228.620303912768,15.5547797735098));
#87368=CARTESIAN_POINT('Ctrl Pts',(-157.121784978706,227.216550203517,15.396021908278));
#87369=CARTESIAN_POINT('Ctrl Pts',(-156.576687161735,223.784209835184,15.2372640430462));
#87370=CARTESIAN_POINT('Ctrl Pts',(-159.164605119719,221.464560577875,15.0785061778144));
#87371=CARTESIAN_POINT('Ctrl Pts',(-162.517076439288,222.38054534067,14.9197483125826));
#87372=CARTESIAN_POINT('Ctrl Pts',(-163.565919500601,225.693854904675,14.7609904473509));
#87373=CARTESIAN_POINT('Ctrl Pts',(-161.35123317519,228.372148487207,14.602232582119));
#87374=CARTESIAN_POINT('Ctrl Pts',(-157.899898300982,227.964251906854,14.4434747168873));
#87375=CARTESIAN_POINT('Ctrl Pts',(-156.37057641913,224.843472097915,14.2847168516555));
#87376=CARTESIAN_POINT('Ctrl Pts',(-158.162902855767,221.865946618808,14.1259589864237));
#87377=CARTESIAN_POINT('Ctrl Pts',(-161.636540526564,221.756706670925,13.9672011211919));
#87378=CARTESIAN_POINT('Ctrl Pts',(-163.612416371805,224.615728650272,13.8084432559601));
#87379=CARTESIAN_POINT('Ctrl Pts',(-162.282208895625,227.826435753778,13.6496853907283));
#87380=CARTESIAN_POINT('Ctrl Pts',(-158.863323927915,228.450388966574,13.4909275254965));
#87381=CARTESIAN_POINT('Ctrl Pts',(-156.484724856678,225.916546332844,13.3321696602647));
#87382=CARTESIAN_POINT('Ctrl Pts',(-157.323305458375,222.543880531338,13.1734117950329));
#87383=CARTESIAN_POINT('Ctrl Pts',(-160.611596799308,221.419055170966,13.0146539298011));
#87384=CARTESIAN_POINT('Ctrl Pts',(-163.340154773566,223.57151037731,12.8558960645693));
#87385=CARTESIAN_POINT('Ctrl Pts',(-163.011803230403,227.031319230165,12.6971381993375));
#87386=CARTESIAN_POINT('Ctrl Pts',(-159.927049489213,228.632064803453,12.5383803341058));
#87387=CARTESIAN_POINT('Ctrl Pts',(-156.909060052626,226.908744811449,12.379622468874));
#87388=CARTESIAN_POINT('Ctrl Pts',(-156.719898734327,223.438541643066,12.2208646036422));
#87389=CARTESIAN_POINT('Ctrl Pts',(-159.532685965386,221.397385101546,12.0621067384104));
#87390=CARTESIAN_POINT('Ctrl Pts',(-162.773158982547,222.653341573422,11.9033488731786));
#87391=CARTESIAN_POINT('Ctrl Pts',(-163.475637007933,226.056959745022,11.7445910079468));
#87392=CARTESIAN_POINT('Ctrl Pts',(-160.997212180335,228.493248399541,11.585833142715));
#87393=CARTESIAN_POINT('Ctrl Pts',(-157.606138804509,227.732516256169,11.4270752774832));
#87394=CARTESIAN_POINT('Ctrl Pts',(-156.40592710066,224.470985342605,11.2683174122514));
#87395=CARTESIAN_POINT('Ctrl Pts',(-158.495010772954,221.693608622685,11.1095595470196));
#87396=CARTESIAN_POINT('Ctrl Pts',(-161.961460526658,221.942241161264,10.9508016817878));
#87397=CARTESIAN_POINT('Ctrl Pts',(-163.632781683497,224.98933446881,10.792043816556));
#87398=CARTESIAN_POINT('Ctrl Pts',(-161.979381186455,228.046188870082,10.6332859513243));
#87399=CARTESIAN_POINT('Ctrl Pts',(-158.514451105407,228.315171337243,10.4745280860925));
#87400=CARTESIAN_POINT('Ctrl Pts',(-156.409095314272,225.550109126926,10.3157702208607));
#87401=CARTESIAN_POINT('Ctrl Pts',(-157.590135350307,222.281587065278,10.1570123556289));
#87402=CARTESIAN_POINT('Ctrl Pts',(-160.976683418975,221.500956414589,9.99825449039708));
#87403=CARTESIAN_POINT('Ctrl Pts',(-163.469370861004,223.922650315672,9.83949662516528));
#87404=CARTESIAN_POINT('Ctrl Pts',(-162.786890227472,227.330334605486,9.68073875993349));
#87405=CARTESIAN_POINT('Ctrl Pts',(-159.55384776735,228.605296755998,9.52198089470171));
#87406=CARTESIAN_POINT('Ctrl Pts',(-156.729123813004,226.580691457195,9.36322302946991));
#87407=CARTESIAN_POINT('Ctrl Pts',(-156.897905616373,223.109437398927,9.20446516423812));
#87408=CARTESIAN_POINT('Ctrl Pts',(-159.90572407765,221.368426158816,9.04570729900633));
#87409=CARTESIAN_POINT('Ctrl Pts',(-162.999823859355,222.951031155348,8.88694943377453));
#87410=CARTESIAN_POINT('Ctrl Pts',(-163.348484962943,226.408852357933,8.72819156854274));
#87411=CARTESIAN_POINT('Ctrl Pts',(-160.632612760122,228.577291937938,8.56943370331094));
#87412=CARTESIAN_POINT('Ctrl Pts',(-157.337773384114,227.471794077016,8.41067583807916));
#87413=CARTESIAN_POINT('Ctrl Pts',(-156.479403702276,224.10411037401,8.25191797284736));
#87414=CARTESIAN_POINT('Ctrl Pts',(-158.843083613671,221.55634482148,8.09316010761557));
#87415=CARTESIAN_POINT('Ctrl Pts',(-162.26557335634,222.160212352913,7.93440224238377));
#87416=CARTESIAN_POINT('Ctrl Pts',(-163.614610452378,225.363053427288,7.77564437715199));
#87417=CARTESIAN_POINT('Ctrl Pts',(-161.655556204541,228.233628019286,7.61688651192019));
#87418=CARTESIAN_POINT('Ctrl Pts',(-158.181336983412,228.144786375193,7.45812864668841));
#87419=CARTESIAN_POINT('Ctrl Pts',(-156.371558083546,225.177836364189,7.2993707814566));
#87420=CARTESIAN_POINT('Ctrl Pts',(-157.882529082935,222.048130519673,7.14061291622482));
#87421=CARTESIAN_POINT('Ctrl Pts',(-161.331409382354,221.619975507472,6.98185505099302));
#87422=CARTESIAN_POINT('Ctrl Pts',(-163.561783867399,224.285218777917,6.82309718576123));
#87423=CARTESIAN_POINT('Ctrl Pts',(-162.532413897065,227.604629794704,6.66433932052944));
#87424=CARTESIAN_POINT('Ctrl Pts',(-159.185378827721,228.540283725802,6.50558145529764));
#87425=CARTESIAN_POINT('Ctrl Pts',(-156.583885023213,226.235870130265,6.34682359006585));
#87426=CARTESIAN_POINT('Ctrl Pts',(-157.108819511125,222.800388240108,6.18806572483406));
#87427=CARTESIAN_POINT('Ctrl Pts',(-160.279762268762,221.377990946107,6.02930785960227));
#87428=CARTESIAN_POINT('Ctrl Pts',(-163.19466660903,223.270456195797,5.87054999437048));
#87429=CARTESIAN_POINT('Ctrl Pts',(-163.18581219434,226.745799867081,5.71179212913868));
#87430=CARTESIAN_POINT('Ctrl Pts',(-160.26130258467,228.623387568664,5.5530342639069));
#87431=CARTESIAN_POINT('Ctrl Pts',(-157.097648859785,227.184851109893,5.39427639867509));
#87432=CARTESIAN_POINT('Ctrl Pts',(-156.590226784293,223.746739001265,5.23551853344331));
#87433=CARTESIAN_POINT('Ctrl Pts',(-159.203429021729,221.455611309395,5.07676066821151));
#87434=CARTESIAN_POINT('Ctrl Pts',(-162.545652987155,222.408308007789,4.91800280297972));
#87435=CARTESIAN_POINT('Ctrl Pts',(-163.558095438842,225.732921115537,4.75924493774792));
#87436=CARTESIAN_POINT('Ctrl Pts',(-161.314169084819,228.386764847169,4.60048707251614));
#87437=CARTESIAN_POINT('Ctrl Pts',(-157.867515236049,227.941041523849,4.44172920728434));
#87438=CARTESIAN_POINT('Ctrl Pts',(-156.372511359387,224.803677113565,4.28297134205255));
#87439=CARTESIAN_POINT('Ctrl Pts',(-158.197384943971,221.845987401207,4.12421347682076));
#87440=CARTESIAN_POINT('Ctrl Pts',(-161.672011756938,221.774849895275,3.96545561158897));
#87441=CARTESIAN_POINT('Ctrl Pts',(-163.616413475723,224.655369638279,3.80669774635717));
#87442=CARTESIAN_POINT('Ctrl Pts',(-162.251073723701,227.851295074949,3.64793988112539));
#87443=CARTESIAN_POINT('Ctrl Pts',(-158.825551388348,228.437715370794,3.48918201589359));
#87444=CARTESIAN_POINT('Ctrl Pts',(-156.474884376031,225.877938695212,3.3304241506618));
#87445=CARTESIAN_POINT('Ctrl Pts',(-157.350403044487,222.514672558763,3.17166628543001));
#87446=CARTESIAN_POINT('Ctrl Pts',(-160.650832741734,221.425978001981,3.01290842019821));
#87447=CARTESIAN_POINT('Ctrl Pts',(-163.355620340796,223.608228230643,2.85415055496642));
#87448=CARTESIAN_POINT('Ctrl Pts',(-162.989344332895,227.064227941581,2.69539268973463));
#87449=CARTESIAN_POINT('Ctrl Pts',(-159.887220515355,228.631046293149,2.53663482450283));
#87450=CARTESIAN_POINT('Ctrl Pts',(-156.88831246471,226.874731278963,2.37787695927104));
#87451=CARTESIAN_POINT('Ctrl Pts',(-156.73722075101,223.402662149674,2.21911909403925));
#87452=CARTESIAN_POINT('Ctrl Pts',(-159.572224421631,221.392476811998,2.06036122880746));
#87453=CARTESIAN_POINT('Ctrl Pts',(-162.798728401055,222.68389602747,1.90160336357567));
#87454=CARTESIAN_POINT('Ctrl Pts',(-163.463836016567,226.095014600311,1.74284549834387));
#87455=CARTESIAN_POINT('Ctrl Pts',(-160.958841546672,228.50397358649,1.58408763311208));
#87456=CARTESIAN_POINT('Ctrl Pts',(-157.576314291936,227.706100789163,1.42532976788028));
#87457=CARTESIAN_POINT('Ctrl Pts',(-156.411946257884,224.431594893095,1.2665719026485));
#87458=CARTESIAN_POINT('Ctrl Pts',(-158.531360393914,221.677313586384,1.1078140374167));
#87459=CARTESIAN_POINT('Ctrl Pts',(-161.994882722329,221.963912720035,0.949056172184911));
#87460=CARTESIAN_POINT('Ctrl Pts',(-163.632669200339,225.029226034151,0.79029830695312));
#87461=CARTESIAN_POINT('Ctrl Pts',(-161.945876935419,228.067610699799,0.631540441721325));
#87462=CARTESIAN_POINT('Ctrl Pts',(-158.478135238796,228.298893703494,0.472782576489533));
#87463=CARTESIAN_POINT('Ctrl Pts',(-156.403376103572,225.51024998876,0.314024711257742));
#87464=CARTESIAN_POINT('Ctrl Pts',(-157.6198890437,222.256241693801,0.155266846025946));
#87465=CARTESIAN_POINT('Ctrl Pts',(-161.015405798375,221.509947072523,-0.00349101920584216));
#87466=CARTESIAN_POINT('Ctrl Pts',(-163.479964483845,223.964662036918,-0.162248884437638));
#87467=CARTESIAN_POINT('Ctrl Pts',(-163.000168811616,226.220556762668,-0.268087461258832));
#87468=CARTESIAN_POINT('Ctrl Pts',(-162.336062657696,226.997301556931,-0.32100674966943));
#87469=CARTESIAN_POINT('Ctrl Pts',(-160.745932854347,222.209822430158,20.1070022498898));
#87470=CARTESIAN_POINT('Ctrl Pts',(-161.673671626808,222.457846368889,20.0540829614792));
#87471=CARTESIAN_POINT('Ctrl Pts',(-163.246007935822,223.949441902791,19.948244384658));
#87472=CARTESIAN_POINT('Ctrl Pts',(-162.644040922406,227.162240680218,19.7894865194262));
#87473=CARTESIAN_POINT('Ctrl Pts',(-159.617283396257,228.391686081006,19.6307286541944));
#87474=CARTESIAN_POINT('Ctrl Pts',(-156.94314642411,226.519286597172,19.4719707889626));
#87475=CARTESIAN_POINT('Ctrl Pts',(-157.065504233849,223.255375032642,19.3132129237309));
#87476=CARTESIAN_POINT('Ctrl Pts',(-159.874060471167,221.588656141149,19.154455058499));
#87477=CARTESIAN_POINT('Ctrl Pts',(-162.797612444419,223.043752347765,18.9956971932673));
#87478=CARTESIAN_POINT('Ctrl Pts',(-163.160916903433,226.289325210142,18.8369393280355));
#87479=CARTESIAN_POINT('Ctrl Pts',(-160.631288994016,228.354850398594,18.6781814628037));
#87480=CARTESIAN_POINT('Ctrl Pts',(-157.523934985103,227.350044245199,18.5194235975719));
#87481=CARTESIAN_POINT('Ctrl Pts',(-156.6826613331,224.194464384383,18.3606657323401));
#87482=CARTESIAN_POINT('Ctrl Pts',(-158.877422764847,221.776117100191,18.2019078671083));
#87483=CARTESIAN_POINT('Ctrl Pts',(-162.099563528995,222.308264228553,18.0431500018765));
#87484=CARTESIAN_POINT('Ctrl Pts',(-163.400185428714,225.30388931854,17.8843921366447));
#87485=CARTESIAN_POINT('Ctrl Pts',(-161.588956989225,228.021394198337,17.7256342714129));
#87486=CARTESIAN_POINT('Ctrl Pts',(-158.323515546074,227.973719572567,17.5668764061811));
#87487=CARTESIAN_POINT('Ctrl Pts',(-156.592392430726,225.204496744203,17.4081185409493));
#87488=CARTESIAN_POINT('Ctrl Pts',(-157.979911714803,222.248118583934,17.2493606757176));
#87489=CARTESIAN_POINT('Ctrl Pts',(-161.216215676596,221.810262148711,17.0906028104857));
#87490=CARTESIAN_POINT('Ctrl Pts',(-163.339439118975,224.291653688216,16.931844945254));
#87491=CARTESIAN_POINT('Ctrl Pts',(-162.406408001359,227.421323735417,16.7730870800222));
#87492=CARTESIAN_POINT('Ctrl Pts',(-159.27103238017,228.334998399515,16.6143292147904));
#87493=CARTESIAN_POINT('Ctrl Pts',(-156.802807893747,226.196482657433,16.4555713495586));
#87494=CARTESIAN_POINT('Ctrl Pts',(-157.260653498318,222.962946035326,16.2968134843268));
#87495=CARTESIAN_POINT('Ctrl Pts',(-160.225548912986,221.593721121098,16.138055619095));
#87496=CARTESIAN_POINT('Ctrl Pts',(-162.98402197161,223.341922503126,15.9792977538632));
#87497=CARTESIAN_POINT('Ctrl Pts',(-163.011518239039,226.607596344978,15.8205398886314));
#87498=CARTESIAN_POINT('Ctrl Pts',(-160.282873132583,228.401998075178,15.6617820233996));
#87499=CARTESIAN_POINT('Ctrl Pts',(-157.295342546282,227.082891300729,15.5030241581678));
#87500=CARTESIAN_POINT('Ctrl Pts',(-156.78311435528,223.857522489773,15.344266292936));
#87501=CARTESIAN_POINT('Ctrl Pts',(-159.214979779818,221.677749051244,15.1855084277043));
#87502=CARTESIAN_POINT('Ctrl Pts',(-162.365295678999,222.538499550375,15.0267505624724));
#87503=CARTESIAN_POINT('Ctrl Pts',(-163.350893065773,225.652015164205,14.8679926972407));
#87504=CARTESIAN_POINT('Ctrl Pts',(-161.269753250522,228.168806525395,14.7092348320089));
#87505=CARTESIAN_POINT('Ctrl Pts',(-158.026535310325,227.785506279153,14.5504769667771));
#87506=CARTESIAN_POINT('Ctrl Pts',(-156.589432176514,224.852910795768,14.3917191015453));
#87507=CARTESIAN_POINT('Ctrl Pts',(-158.27368058064,222.054931346312,14.2329612363135));
#87508=CARTESIAN_POINT('Ctrl Pts',(-161.537856449478,221.952278612899,14.0742033710817));
#87509=CARTESIAN_POINT('Ctrl Pts',(-163.394586156228,224.638900373112,13.9154455058499));
#87510=CARTESIAN_POINT('Ctrl Pts',(-162.144590746287,227.656000497653,13.7566876406181));
#87511=CARTESIAN_POINT('Ctrl Pts',(-158.931865969678,228.242329071187,13.5979297753863));
#87512=CARTESIAN_POINT('Ctrl Pts',(-156.696697415616,225.861278206272,13.4391719101545));
#87513=CARTESIAN_POINT('Ctrl Pts',(-157.484711256883,222.691985560846,13.2804140449227));
#87514=CARTESIAN_POINT('Ctrl Pts',(-160.574717256939,221.634987639373,13.1216561796909));
#87515=CARTESIAN_POINT('Ctrl Pts',(-163.138742046045,223.65764889802,12.9628983144591));
#87516=CARTESIAN_POINT('Ctrl Pts',(-162.830190238038,226.908829832413,12.8041404492274));
#87517=CARTESIAN_POINT('Ctrl Pts',(-159.931448435473,228.413049779244,12.6453825839956));
#87518=CARTESIAN_POINT('Ctrl Pts',(-157.095445022068,226.793646702326,12.4866247187638));
#87519=CARTESIAN_POINT('Ctrl Pts',(-156.917690210247,223.532698233973,12.327866853532));
#87520=CARTESIAN_POINT('Ctrl Pts',(-159.560865196799,221.614624284187,12.1691089883002));
#87521=CARTESIAN_POINT('Ctrl Pts',(-162.605936337972,222.794846056387,12.0103511230684));
#87522=CARTESIAN_POINT('Ctrl Pts',(-163.266054645109,225.993224631066,11.8515932578366));
#87523=CARTESIAN_POINT('Ctrl Pts',(-160.937079869477,228.282604062451,11.6928353926048));
#87524=CARTESIAN_POINT('Ctrl Pts',(-157.750489634149,227.567744384966,11.534077527373));
#87525=CARTESIAN_POINT('Ctrl Pts',(-156.622651197188,224.502885147334,11.3753196621412));
#87526=CARTESIAN_POINT('Ctrl Pts',(-158.58576225175,221.892985403314,11.2165617969094));
#87527=CARTESIAN_POINT('Ctrl Pts',(-161.843183637897,222.126625296,11.0578039316776));
#87528=CARTESIAN_POINT('Ctrl Pts',(-163.413723431122,224.989977604794,10.8990460664458));
#87529=CARTESIAN_POINT('Ctrl Pts',(-161.860023674426,227.862502409287,10.7402882012141));
#87530=CARTESIAN_POINT('Ctrl Pts',(-158.604030324039,228.115265121365,10.5815303359823));
#87531=CARTESIAN_POINT('Ctrl Pts',(-156.625628366196,225.516937316875,10.4227724707505));
#87532=CARTESIAN_POINT('Ctrl Pts',(-157.735451194917,222.445508500309,10.2640146055187));
#87533=CARTESIAN_POINT('Ctrl Pts',(-160.917789000998,221.711950203807,10.1052567402869));
#87534=CARTESIAN_POINT('Ctrl Pts',(-163.260166349457,223.987614951482,9.9464988750551));
#87535=CARTESIAN_POINT('Ctrl Pts',(-162.618839583096,227.189814455749,9.78774100982331));
#87536=CARTESIAN_POINT('Ctrl Pts',(-159.580750933268,228.387895856227,9.62898314459151));
#87537=CARTESIAN_POINT('Ctrl Pts',(-156.926359012827,226.485375102312,9.47022527935972));
#87538=CARTESIAN_POINT('Ctrl Pts',(-157.084963202979,223.223439113172,9.31146741412793));
#87539=CARTESIAN_POINT('Ctrl Pts',(-159.911408955133,221.587411577795,9.15270954889613));
#87540=CARTESIAN_POINT('Ctrl Pts',(-162.818933228066,223.074584832224,8.99395168366434));
#87541=CARTESIAN_POINT('Ctrl Pts',(-163.146569921525,226.323897972486,8.83519381843255));
#87542=CARTESIAN_POINT('Ctrl Pts',(-160.59446594654,228.36157974039,8.67643595320076));
#87543=CARTESIAN_POINT('Ctrl Pts',(-157.498306760659,227.32274386208,8.51767808796897));
#87544=CARTESIAN_POINT('Ctrl Pts',(-156.691697129046,224.158132892534,8.35892022273717));
#87545=CARTESIAN_POINT('Ctrl Pts',(-158.912846154834,221.763998666635,8.20016235750538));
#87546=CARTESIAN_POINT('Ctrl Pts',(-162.128958336967,222.331452733779,8.04140449227358));
#87547=CARTESIAN_POINT('Ctrl Pts',(-163.396647932827,225.34116115403,7.8826466270418));
#87548=CARTESIAN_POINT('Ctrl Pts',(-161.555725474133,228.038638899528,7.72388876181));
#87549=CARTESIAN_POINT('Ctrl Pts',(-158.291003122691,227.95515444367,7.56513089657821));
#87550=CARTESIAN_POINT('Ctrl Pts',(-156.590354646156,225.167112757173,7.40637303134641));
#87551=CARTESIAN_POINT('Ctrl Pts',(-158.010213463379,222.226129481883,7.24761516611463));
#87552=CARTESIAN_POINT('Ctrl Pts',(-161.251124840671,221.823792395694,7.08885730088283));
#87553=CARTESIAN_POINT('Ctrl Pts',(-163.34700681298,224.328320384064,6.93009943565104));
#87554=CARTESIAN_POINT('Ctrl Pts',(-162.379708281668,227.447569530526,6.77134157041925));
#87555=CARTESIAN_POINT('Ctrl Pts',(-159.234500824553,228.326803138899,6.61258370518746));
#87556=CARTESIAN_POINT('Ctrl Pts',(-156.789878182705,226.161346645375,6.45382583995566));
#87557=CARTESIAN_POINT('Ctrl Pts',(-157.28315890181,222.933025747673,6.29506797472387));
#87558=CARTESIAN_POINT('Ctrl Pts',(-160.262892487142,221.596399604419,6.13631010949208));
#87559=CARTESIAN_POINT('Ctrl Pts',(-163.002026878579,223.374748409357,5.97755224426028));
#87560=CARTESIAN_POINT('Ctrl Pts',(-162.993706388793,226.640527406141,5.8187943790285));
#87561=CARTESIAN_POINT('Ctrl Pts',(-160.245545929708,228.404895785336,5.6600365137967));
#87562=CARTESIAN_POINT('Ctrl Pts',(-157.27266184541,227.053103675686,5.50127864856491));
#87563=CARTESIAN_POINT('Ctrl Pts',(-156.795837532943,223.822311162785,5.34252078333311));
#87564=CARTESIAN_POINT('Ctrl Pts',(-159.251462584326,221.669339427391,5.18376291810132));
#87565=CARTESIAN_POINT('Ctrl Pts',(-162.392149049098,222.564588117074,5.02500505286953));
#87566=CARTESIAN_POINT('Ctrl Pts',(-163.343540798205,225.68872566624,4.86624718763774));
#87567=CARTESIAN_POINT('Ctrl Pts',(-161.234924140276,228.182541512748,4.70748932240595));
#87568=CARTESIAN_POINT('Ctrl Pts',(-157.99610495773,227.763695491936,4.54873145717415));
#87569=CARTESIAN_POINT('Ctrl Pts',(-156.591250439066,224.815515465591,4.38997359194236));
#87570=CARTESIAN_POINT('Ctrl Pts',(-158.306083384528,222.036175677865,4.23121572671057));
#87571=CARTESIAN_POINT('Ctrl Pts',(-161.571188749849,221.969327793245,4.07245786147877));
#87572=CARTESIAN_POINT('Ctrl Pts',(-163.398342233112,224.67615099299,3.91369999624699));
#87573=CARTESIAN_POINT('Ctrl Pts',(-162.115333038231,227.679360791378,3.75494213101519));
#87574=CARTESIAN_POINT('Ctrl Pts',(-158.896371130019,228.230419698525,3.5961842657834));
#87575=CARTESIAN_POINT('Ctrl Pts',(-156.687450320061,225.824998625309,3.4374264005516));
#87576=CARTESIAN_POINT('Ctrl Pts',(-157.510174847238,222.664538841213,3.27866853531982));
#87577=CARTESIAN_POINT('Ctrl Pts',(-160.611587255653,221.641493020787,3.11991067008802));
#87578=CARTESIAN_POINT('Ctrl Pts',(-163.153275033114,223.692152649466,2.96115280485623));
#87579=CARTESIAN_POINT('Ctrl Pts',(-162.809085621427,226.93975413479,2.80239493962444));
#87580=CARTESIAN_POINT('Ctrl Pts',(-159.89402116537,228.412092685536,2.64363707439264));
#87581=CARTESIAN_POINT('Ctrl Pts',(-157.075948522366,226.761684200052,2.48487920916085));
#87582=CARTESIAN_POINT('Ctrl Pts',(-156.933967702091,223.498982289014,2.32612134392906));
#87583=CARTESIAN_POINT('Ctrl Pts',(-159.598019467623,221.610011966548,2.16736347869727));
#87584=CARTESIAN_POINT('Ctrl Pts',(-162.629963909868,222.823558064097,2.00860561346547));
#87585=CARTESIAN_POINT('Ctrl Pts',(-163.254965258451,226.028984762691,1.84984774823368));
#87586=CARTESIAN_POINT('Ctrl Pts',(-160.901023001045,228.292682516148,1.69108988300189));
#87587=CARTESIAN_POINT('Ctrl Pts',(-157.722463552137,227.54292178165,1.5323320177701));
#87588=CARTESIAN_POINT('Ctrl Pts',(-156.628307396718,224.465869958378,1.37357415253831));
#87589=CARTESIAN_POINT('Ctrl Pts',(-158.619919975389,221.877672964505,1.21481628730651));
#87590=CARTESIAN_POINT('Ctrl Pts',(-161.874590461213,222.146990050728,1.05605842207472));
#87591=CARTESIAN_POINT('Ctrl Pts',(-163.413617730746,225.027463692089,0.897300556842931));
#87592=CARTESIAN_POINT('Ctrl Pts',(-161.828539743717,227.882632493727,0.738542691611135));
#87593=CARTESIAN_POINT('Ctrl Pts',(-158.569904319348,228.099969035727,0.579784826379343));
#87594=CARTESIAN_POINT('Ctrl Pts',(-156.620254026289,225.479481701384,0.421026961147552));
#87595=CARTESIAN_POINT('Ctrl Pts',(-157.763410728175,222.421691465315,0.262269095915756));
#87596=CARTESIAN_POINT('Ctrl Pts',(-160.954176404753,221.720398721314,0.103511230683968));
#87597=CARTESIAN_POINT('Ctrl Pts',(-163.270121172418,224.027093348395,-0.055246634547828));
#87598=CARTESIAN_POINT('Ctrl Pts',(-162.819257379562,226.146956680238,-0.161085211369022));
#87599=CARTESIAN_POINT('Ctrl Pts',(-162.195197104019,226.876863439079,-0.21400449977962));
#87600=CARTESIAN_POINT('Ctrl Pts',(-160.698066426161,222.388867814061,20.2140044997796));
#87601=CARTESIAN_POINT('Ctrl Pts',(-161.56627230492,222.620976084267,20.161085211369));
#87602=CARTESIAN_POINT('Ctrl Pts',(-163.037711968101,224.016856098884,20.0552466345478));
#87603=CARTESIAN_POINT('Ctrl Pts',(-162.474373110892,227.023489936586,19.896488769316));
#87604=CARTESIAN_POINT('Ctrl Pts',(-159.641842278095,228.174041962934,19.7377309040842));
#87605=CARTESIAN_POINT('Ctrl Pts',(-157.139304377621,226.421794145441,19.5789730388524));
#87606=CARTESIAN_POINT('Ctrl Pts',(-157.253810500337,223.367327422492,19.4202151736207));
#87607=CARTESIAN_POINT('Ctrl Pts',(-159.882141996706,221.807561696636,19.2614573083889));
#87608=CARTESIAN_POINT('Ctrl Pts',(-162.618089965442,223.169284541734,19.1026994431571));
#87609=CARTESIAN_POINT('Ctrl Pts',(-162.958081217784,226.206589355004,18.9439415779253));
#87610=CARTESIAN_POINT('Ctrl Pts',(-160.590779249579,228.139570022159,18.7851837126935));
#87611=CARTESIAN_POINT('Ctrl Pts',(-157.68282380134,227.199242167719,18.6264258474617));
#87612=CARTESIAN_POINT('Ctrl Pts',(-156.89553458589,224.246155515121,18.4676679822299));
#87613=CARTESIAN_POINT('Ctrl Pts',(-158.949458421001,221.982993306815,18.3089101169981));
#87614=CARTESIAN_POINT('Ctrl Pts',(-161.964834771176,222.480992613217,18.1501522517663));
#87615=CARTESIAN_POINT('Ctrl Pts',(-163.181995908446,225.284388774815,17.9913943865345));
#87616=CARTESIAN_POINT('Ctrl Pts',(-161.486993796195,227.827511669135,17.8326365213027));
#87617=CARTESIAN_POINT('Ctrl Pts',(-158.431095366766,227.78289631879,17.673878656071));
#87618=CARTESIAN_POINT('Ctrl Pts',(-156.811058228927,225.191374210904,17.5151207908391));
#87619=CARTESIAN_POINT('Ctrl Pts',(-158.109540555079,222.424706507915,17.3563629256074));
#87620=CARTESIAN_POINT('Ctrl Pts',(-161.138171252083,222.014947271375,17.1976050603756));
#87621=CARTESIAN_POINT('Ctrl Pts',(-163.125147682637,224.337108192152,17.0388471951438));
#87622=CARTESIAN_POINT('Ctrl Pts',(-162.251989067923,227.265947660988,16.880089329912));
#87623=CARTESIAN_POINT('Ctrl Pts',(-159.317810151146,228.12099192365,16.7213314646802));
#87624=CARTESIAN_POINT('Ctrl Pts',(-157.007971355121,226.119704498563,16.5625735994484));
#87625=CARTESIAN_POINT('Ctrl Pts',(-157.436437058239,223.093663561365,16.4038157342166));
#87626=CARTESIAN_POINT('Ctrl Pts',(-160.211075464361,221.812301657386,16.2450578689848));
#87627=CARTESIAN_POINT('Ctrl Pts',(-162.792537614034,223.448321151434,16.086300003753));
#87628=CARTESIAN_POINT('Ctrl Pts',(-162.818269449045,226.504437066565,15.9275421385212));
#87629=CARTESIAN_POINT('Ctrl Pts',(-160.26472119517,228.183692237588,15.7687842732894));
#87630=CARTESIAN_POINT('Ctrl Pts',(-157.468900113859,226.949232397941,15.6100264080576));
#87631=CARTESIAN_POINT('Ctrl Pts',(-156.989541548824,223.930835144362,15.4512685428259));
#87632=CARTESIAN_POINT('Ctrl Pts',(-159.265354439916,221.890937524614,15.292510677594));
#87633=CARTESIAN_POINT('Ctrl Pts',(-162.21351491871,222.69645376008,15.1337528123623));
#87634=CARTESIAN_POINT('Ctrl Pts',(-163.135866630944,225.610175423736,14.9749949471305));
#87635=CARTESIAN_POINT('Ctrl Pts',(-161.188273325853,227.965464563583,14.8162370818987));
#87636=CARTESIAN_POINT('Ctrl Pts',(-158.153172319669,227.606760651453,14.6574792166669));
#87637=CARTESIAN_POINT('Ctrl Pts',(-156.808287933899,224.862349493622,14.4987213514351));
#87638=CARTESIAN_POINT('Ctrl Pts',(-158.384458305513,222.243916073815,14.3399634862033));
#87639=CARTESIAN_POINT('Ctrl Pts',(-161.439172372392,222.147850554872,14.1812056209715));
#87640=CARTESIAN_POINT('Ctrl Pts',(-163.176755940652,224.662072095952,14.0224477557397));
#87641=CARTESIAN_POINT('Ctrl Pts',(-162.00697259695,227.485565241528,13.8636898905079));
#87642=CARTESIAN_POINT('Ctrl Pts',(-159.000408011441,228.0342691758,13.7049320252761));
#87643=CARTESIAN_POINT('Ctrl Pts',(-156.908669974554,225.806010079699,13.5461741600444));
#87644=CARTESIAN_POINT('Ctrl Pts',(-157.646117055391,222.840090590353,13.3874162948125));
#87645=CARTESIAN_POINT('Ctrl Pts',(-160.53783771457,221.85092010778,13.2286584295808));
#87646=CARTESIAN_POINT('Ctrl Pts',(-162.937329318524,223.743787418731,13.069900564349));
#87647=CARTESIAN_POINT('Ctrl Pts',(-162.648577245673,226.786340434661,12.9111426991172));
#87648=CARTESIAN_POINT('Ctrl Pts',(-159.935847381734,228.194034755035,12.7523848338854));
#87649=CARTESIAN_POINT('Ctrl Pts',(-157.28182999151,226.678548593203,12.5936269686536));
#87650=CARTESIAN_POINT('Ctrl Pts',(-157.115481686166,223.626854824879,12.4348691034218));
#87651=CARTESIAN_POINT('Ctrl Pts',(-159.589044428212,221.831863466828,12.27611123819));
#87652=CARTESIAN_POINT('Ctrl Pts',(-162.438713693398,222.936350539352,12.1173533729582));
#87653=CARTESIAN_POINT('Ctrl Pts',(-163.056472282286,225.92948951711,11.9585955077264));
#87654=CARTESIAN_POINT('Ctrl Pts',(-160.876947558619,228.07195972536,11.7998376424946));
#87655=CARTESIAN_POINT('Ctrl Pts',(-157.894840463788,227.402972513763,11.6410797772628));
#87656=CARTESIAN_POINT('Ctrl Pts',(-156.839375293716,224.534784952064,11.482321912031));
#87657=CARTESIAN_POINT('Ctrl Pts',(-158.676513730546,222.092362183943,11.3235640467992));
#87658=CARTESIAN_POINT('Ctrl Pts',(-161.724906749135,222.311009430736,11.1648061815675));
#87659=CARTESIAN_POINT('Ctrl Pts',(-163.194665178747,224.990620740778,11.0060483163357));
#87660=CARTESIAN_POINT('Ctrl Pts',(-161.740666162396,227.678815948491,10.8472904511039));
#87661=CARTESIAN_POINT('Ctrl Pts',(-158.693609542671,227.915358905487,10.6885325858721));
#87662=CARTESIAN_POINT('Ctrl Pts',(-156.84216141812,225.483765506824,10.5297747206403));
#87663=CARTESIAN_POINT('Ctrl Pts',(-157.880767039527,222.60942993534,10.3710168554085));
#87664=CARTESIAN_POINT('Ctrl Pts',(-160.858894583022,221.922943993026,10.2122589901767));
#87665=CARTESIAN_POINT('Ctrl Pts',(-163.05096183791,224.052579587292,10.0535011249449));
#87666=CARTESIAN_POINT('Ctrl Pts',(-162.450788938719,227.049294306012,9.89474325971312));
#87667=CARTESIAN_POINT('Ctrl Pts',(-159.607654099187,228.170494956457,9.73598539448132));
#87668=CARTESIAN_POINT('Ctrl Pts',(-157.123594212651,226.390058747429,9.57722752924954));
#87669=CARTESIAN_POINT('Ctrl Pts',(-157.272020789584,223.337440827417,9.41846966401773));
#87670=CARTESIAN_POINT('Ctrl Pts',(-159.917093832615,221.806396996775,9.25971179878595));
#87671=CARTESIAN_POINT('Ctrl Pts',(-162.638042596777,223.198138509099,9.10095393355415));
#87672=CARTESIAN_POINT('Ctrl Pts',(-162.944654880107,226.238943587039,8.94219606832235));
#87673=CARTESIAN_POINT('Ctrl Pts',(-160.556319132959,228.145867542842,8.78343820309057));
#87674=CARTESIAN_POINT('Ctrl Pts',(-157.658840137204,227.173693647144,8.62468033785877));
#87675=CARTESIAN_POINT('Ctrl Pts',(-156.903990555816,224.212155411058,8.46592247262698));
#87676=CARTESIAN_POINT('Ctrl Pts',(-158.982608695998,221.971652511791,8.30716460739519));
#87677=CARTESIAN_POINT('Ctrl Pts',(-161.992343317594,222.502693114646,8.1484067421634));
#87678=CARTESIAN_POINT('Ctrl Pts',(-163.178685413276,225.319268880773,7.98964887693161));
#87679=CARTESIAN_POINT('Ctrl Pts',(-161.455894743725,227.843649779771,7.83089101169981));
#87680=CARTESIAN_POINT('Ctrl Pts',(-158.40066926197,227.765522512147,7.67213314646803));
#87681=CARTESIAN_POINT('Ctrl Pts',(-156.809151208767,225.156389150158,7.51337528123622));
#87682=CARTESIAN_POINT('Ctrl Pts',(-158.137897843824,222.404128444094,7.35461741600444));
#87683=CARTESIAN_POINT('Ctrl Pts',(-161.170840298987,222.027609283915,7.19585955077264));
#87684=CARTESIAN_POINT('Ctrl Pts',(-163.13222975856,224.371421990211,7.03710168554085));
#87685=CARTESIAN_POINT('Ctrl Pts',(-162.227002666271,227.290509266348,6.87834382030905));
#87686=CARTESIAN_POINT('Ctrl Pts',(-159.283622821385,228.113322551995,6.71958595507727));
#87687=CARTESIAN_POINT('Ctrl Pts',(-156.995871342197,226.086823160485,6.56082808984547));
#87688=CARTESIAN_POINT('Ctrl Pts',(-157.457498292496,223.065663255237,6.40207022461368));
#87689=CARTESIAN_POINT('Ctrl Pts',(-160.246022705521,221.814808262731,6.24331235938189));
#87690=CARTESIAN_POINT('Ctrl Pts',(-162.809387148128,223.479040622918,6.08455449415009));
#87691=CARTESIAN_POINT('Ctrl Pts',(-162.801600583245,226.535254945201,5.9257966289183));
#87692=CARTESIAN_POINT('Ctrl Pts',(-160.229789274746,228.186404002008,5.76703876368651));
#87693=CARTESIAN_POINT('Ctrl Pts',(-157.447674831036,226.92135624148,5.60828089845472));
#87694=CARTESIAN_POINT('Ctrl Pts',(-157.001448281594,223.897883324305,5.44952303322293));
#87695=CARTESIAN_POINT('Ctrl Pts',(-159.299496146922,221.883067545386,5.29076516799113));
#87696=CARTESIAN_POINT('Ctrl Pts',(-162.23864511104,222.72086822636,5.13200730275934));
#87697=CARTESIAN_POINT('Ctrl Pts',(-163.128986157567,225.644530216944,4.97324943752755));
#87698=CARTESIAN_POINT('Ctrl Pts',(-161.155679195733,227.978318178328,4.81449157229575));
#87699=CARTESIAN_POINT('Ctrl Pts',(-158.12469467941,227.586349460022,4.65573370706397));
#87700=CARTESIAN_POINT('Ctrl Pts',(-156.809989518745,224.827353817618,4.49697584183217));
#87701=CARTESIAN_POINT('Ctrl Pts',(-158.414781825084,222.226363954524,4.33821797660038));
#87702=CARTESIAN_POINT('Ctrl Pts',(-161.470365742761,222.163805691214,4.17946011136859));
#87703=CARTESIAN_POINT('Ctrl Pts',(-163.1802709905,224.696932347702,4.02070224613679));
#87704=CARTESIAN_POINT('Ctrl Pts',(-161.979592352761,227.507426507806,3.861944380905));
#87705=CARTESIAN_POINT('Ctrl Pts',(-158.96719087169,228.023124026255,3.70318651567321));
#87706=CARTESIAN_POINT('Ctrl Pts',(-156.900016264091,225.772058555407,3.54442865044142));
#87707=CARTESIAN_POINT('Ctrl Pts',(-157.669946649989,222.814405123663,3.38567078520962));
#87708=CARTESIAN_POINT('Ctrl Pts',(-160.572341769573,221.857008039592,3.22691291997783));
#87709=CARTESIAN_POINT('Ctrl Pts',(-162.950929725432,223.77607706829,3.06815505474604));
#87710=CARTESIAN_POINT('Ctrl Pts',(-162.628826909959,226.815280327998,2.90939718951425));
#87711=CARTESIAN_POINT('Ctrl Pts',(-159.900821815385,228.193139077924,2.75063932428246));
#87712=CARTESIAN_POINT('Ctrl Pts',(-157.263584580022,226.64863712114,2.59188145905066));
#87713=CARTESIAN_POINT('Ctrl Pts',(-157.130714653171,223.595302428353,2.43312359381887));
#87714=CARTESIAN_POINT('Ctrl Pts',(-159.623814513615,221.827547121098,2.27436572858708));
#87715=CARTESIAN_POINT('Ctrl Pts',(-162.461199418682,222.963220100725,2.11560786335528));
#87716=CARTESIAN_POINT('Ctrl Pts',(-163.046094500334,225.962954925072,1.95684999812349));
#87717=CARTESIAN_POINT('Ctrl Pts',(-160.843204455419,228.081391445806,1.7980921328917));
#87718=CARTESIAN_POINT('Ctrl Pts',(-157.868612812338,227.379742774137,1.63933426765991));
#87719=CARTESIAN_POINT('Ctrl Pts',(-156.844668535551,224.50014502366,1.48057640242812));
#87720=CARTESIAN_POINT('Ctrl Pts',(-158.708479556863,222.078032342627,1.32181853719632));
#87721=CARTESIAN_POINT('Ctrl Pts',(-161.754298200098,222.330067381422,1.16306067196453));
#87722=CARTESIAN_POINT('Ctrl Pts',(-163.194566261152,225.025701350026,1.00430280673274));
#87723=CARTESIAN_POINT('Ctrl Pts',(-161.711202552014,227.697654287655,0.845544941500945));
#87724=CARTESIAN_POINT('Ctrl Pts',(-158.6616733999,227.90104436796,0.686787076269153));
#87725=CARTESIAN_POINT('Ctrl Pts',(-156.837131949006,225.448713414009,0.528029211037362));
#87726=CARTESIAN_POINT('Ctrl Pts',(-157.90693241265,222.587141236829,0.369271345805566));
#87727=CARTESIAN_POINT('Ctrl Pts',(-160.89294701113,221.930850370105,0.210513480573778));
#87728=CARTESIAN_POINT('Ctrl Pts',(-163.06027786099,224.089524659872,0.051755615341982));
#87729=CARTESIAN_POINT('Ctrl Pts',(-162.638345947507,226.073356597808,-0.0540829614792118));
#87730=CARTESIAN_POINT('Ctrl Pts',(-162.054331550342,226.756425321227,-0.10700224988981));
#87731=CARTESIAN_POINT('Ctrl Pts',(-160.650199997975,222.567913197965,20.3210067496694));
#87732=CARTESIAN_POINT('Ctrl Pts',(-161.458872983031,222.784105799646,20.2680874612588));
#87733=CARTESIAN_POINT('Ctrl Pts',(-162.82941600038,224.084270294977,20.1622488844376));
#87734=CARTESIAN_POINT('Ctrl Pts',(-162.304705299379,226.884739192954,20.0034910192058));
#87735=CARTESIAN_POINT('Ctrl Pts',(-159.666401159932,227.956397844861,19.8447331539741));
#87736=CARTESIAN_POINT('Ctrl Pts',(-157.335462331131,226.324301693709,19.6859752887422));
#87737=CARTESIAN_POINT('Ctrl Pts',(-157.442116766824,223.479279812341,19.5272174235105));
#87738=CARTESIAN_POINT('Ctrl Pts',(-159.890223522245,222.026467252124,19.3684595582787));
#87739=CARTESIAN_POINT('Ctrl Pts',(-162.438567486465,223.294816735702,19.2097016930469));
#87740=CARTESIAN_POINT('Ctrl Pts',(-162.755245532134,226.123853499867,19.0509438278151));
#87741=CARTESIAN_POINT('Ctrl Pts',(-160.550269505142,227.924289645724,18.8921859625833));
#87742=CARTESIAN_POINT('Ctrl Pts',(-157.841712617577,227.048440090238,18.7334280973515));
#87743=CARTESIAN_POINT('Ctrl Pts',(-157.10840783868,224.29784664586,18.5746702321197));
#87744=CARTESIAN_POINT('Ctrl Pts',(-159.021494077155,222.189869513439,18.4159123668879));
#87745=CARTESIAN_POINT('Ctrl Pts',(-161.830106013357,222.653720997882,18.2571545016561));
#87746=CARTESIAN_POINT('Ctrl Pts',(-162.963806388178,225.264888231089,18.0983966364243));
#87747=CARTESIAN_POINT('Ctrl Pts',(-161.385030603165,227.633629139932,17.9396387711925));
#87748=CARTESIAN_POINT('Ctrl Pts',(-158.538675187457,227.592073065013,17.7808809059608));
#87749=CARTESIAN_POINT('Ctrl Pts',(-157.029724027129,225.178251677604,17.622123040729));
#87750=CARTESIAN_POINT('Ctrl Pts',(-158.239169395355,222.601294431896,17.4633651754972));
#87751=CARTESIAN_POINT('Ctrl Pts',(-161.060126827571,222.219632394038,17.3046073102654));
#87752=CARTESIAN_POINT('Ctrl Pts',(-162.910856246299,224.382562696088,17.1458494450336));
#87753=CARTESIAN_POINT('Ctrl Pts',(-162.097570134487,227.110571586559,16.9870915798018));
#87754=CARTESIAN_POINT('Ctrl Pts',(-159.364587922123,227.906985447785,16.82833371457));
#87755=CARTESIAN_POINT('Ctrl Pts',(-157.213134816495,226.042926339693,16.6695758493382));
#87756=CARTESIAN_POINT('Ctrl Pts',(-157.61222061816,223.224381087403,16.5108179841064));
#87757=CARTESIAN_POINT('Ctrl Pts',(-160.196602015734,222.030882193675,16.3520601188746));
#87758=CARTESIAN_POINT('Ctrl Pts',(-162.601053256459,223.554719799741,16.1933022536428));
#87759=CARTESIAN_POINT('Ctrl Pts',(-162.62502065905,226.401277788152,16.034544388411));
#87760=CARTESIAN_POINT('Ctrl Pts',(-160.246569257757,227.965386399998,15.8757865231792));
#87761=CARTESIAN_POINT('Ctrl Pts',(-157.642457681435,226.815573495153,15.7170286579474));
#87762=CARTESIAN_POINT('Ctrl Pts',(-157.195968742368,224.004147798951,15.5582707927157));
#87763=CARTESIAN_POINT('Ctrl Pts',(-159.315729100014,222.104125997983,15.3995129274839));
#87764=CARTESIAN_POINT('Ctrl Pts',(-162.061734158422,222.854407969786,15.2407550622521));
#87765=CARTESIAN_POINT('Ctrl Pts',(-162.920840196116,225.568335683266,15.0819971970203));
#87766=CARTESIAN_POINT('Ctrl Pts',(-161.106793401185,227.762122601771,14.9232393317885));
#87767=CARTESIAN_POINT('Ctrl Pts',(-158.279809329013,227.428015023753,14.7644814665567));
#87768=CARTESIAN_POINT('Ctrl Pts',(-157.027143691284,224.871788191475,14.6057236013249));
#87769=CARTESIAN_POINT('Ctrl Pts',(-158.495236030387,222.432900801318,14.4469657360931));
#87770=CARTESIAN_POINT('Ctrl Pts',(-161.340488295306,222.343422496845,14.2882078708613));
#87771=CARTESIAN_POINT('Ctrl Pts',(-162.958925725075,224.685243818793,14.1294500056295));
#87772=CARTESIAN_POINT('Ctrl Pts',(-161.869354447612,227.315129985403,13.9706921403977));
#87773=CARTESIAN_POINT('Ctrl Pts',(-159.068950053205,227.826209280413,13.8119342751659));
#87774=CARTESIAN_POINT('Ctrl Pts',(-157.120642533492,225.750741953127,13.6531764099342));
#87775=CARTESIAN_POINT('Ctrl Pts',(-157.807522853899,222.988195619861,13.4944185447023));
#87776=CARTESIAN_POINT('Ctrl Pts',(-160.500958172201,222.066852576186,13.3356606794706));
#87777=CARTESIAN_POINT('Ctrl Pts',(-162.735916591004,223.829925939442,13.1769028142388));
#87778=CARTESIAN_POINT('Ctrl Pts',(-162.466964253308,226.663851036909,13.018144949007));
#87779=CARTESIAN_POINT('Ctrl Pts',(-159.940246327995,227.975019730826,12.8593870837752));
#87780=CARTESIAN_POINT('Ctrl Pts',(-157.468214960952,226.563450484081,12.7006292185434));
#87781=CARTESIAN_POINT('Ctrl Pts',(-157.313273162085,223.721011415786,12.5418713533116));
#87782=CARTESIAN_POINT('Ctrl Pts',(-159.617223659625,222.049102649469,12.3831134880798));
#87783=CARTESIAN_POINT('Ctrl Pts',(-162.271491048824,223.077855022317,12.224355622848));
#87784=CARTESIAN_POINT('Ctrl Pts',(-162.846889919463,225.865754403154,12.0655977576162));
#87785=CARTESIAN_POINT('Ctrl Pts',(-160.816815247761,227.861315388269,11.9068398923844));
#87786=CARTESIAN_POINT('Ctrl Pts',(-158.039191293428,227.238200642559,11.7480820271526));
#87787=CARTESIAN_POINT('Ctrl Pts',(-157.056099390243,224.566684756794,11.5893241619209));
#87788=CARTESIAN_POINT('Ctrl Pts',(-158.767265209342,222.291738964571,11.4305662966891));
#87789=CARTESIAN_POINT('Ctrl Pts',(-161.606629860374,222.495393565473,11.2718084314573));
#87790=CARTESIAN_POINT('Ctrl Pts',(-162.975606926372,224.991263876762,11.1130505662255));
#87791=CARTESIAN_POINT('Ctrl Pts',(-161.621308650367,227.495129487696,10.9542927009937));
#87792=CARTESIAN_POINT('Ctrl Pts',(-158.783188761302,227.715452689608,10.7955348357619));
#87793=CARTESIAN_POINT('Ctrl Pts',(-157.058694470044,225.450593696774,10.6367769705301));
#87794=CARTESIAN_POINT('Ctrl Pts',(-158.026082884138,222.773351370371,10.4780191052983));
#87795=CARTESIAN_POINT('Ctrl Pts',(-160.800000165046,222.133937782244,10.3192612400665));
#87796=CARTESIAN_POINT('Ctrl Pts',(-162.841757326363,224.117544223102,10.1605033748347));
#87797=CARTESIAN_POINT('Ctrl Pts',(-162.282738294342,226.908774156275,10.0017455096029));
#87798=CARTESIAN_POINT('Ctrl Pts',(-159.634557265106,227.953094056686,9.84298764437113));
#87799=CARTESIAN_POINT('Ctrl Pts',(-157.320829412474,226.294742392546,9.68422977913935));
#87800=CARTESIAN_POINT('Ctrl Pts',(-157.45907837619,223.451442541662,9.52547191390754));
#87801=CARTESIAN_POINT('Ctrl Pts',(-159.922778710098,222.025382415754,9.36671404867576));
#87802=CARTESIAN_POINT('Ctrl Pts',(-162.457151965487,223.321692185974,9.20795618344396));
#87803=CARTESIAN_POINT('Ctrl Pts',(-162.742739838688,226.153989201593,9.04919831821217));
#87804=CARTESIAN_POINT('Ctrl Pts',(-160.518172319377,227.930155345293,8.89044045298038));
#87805=CARTESIAN_POINT('Ctrl Pts',(-157.819373513749,227.024643432207,8.73168258774858));
#87806=CARTESIAN_POINT('Ctrl Pts',(-157.116283982586,224.266177929582,8.5729247225168));
#87807=CARTESIAN_POINT('Ctrl Pts',(-159.052371237161,222.179306356947,8.41416685728499));
#87808=CARTESIAN_POINT('Ctrl Pts',(-161.855728298222,222.673933495512,8.25540899205321));
#87809=CARTESIAN_POINT('Ctrl Pts',(-162.960722893725,225.297376607515,8.09665112682141));
#87810=CARTESIAN_POINT('Ctrl Pts',(-161.356064013318,227.648660660014,7.93789326158962));
#87811=CARTESIAN_POINT('Ctrl Pts',(-158.510335401249,227.575890580624,7.77913539635783));
#87812=CARTESIAN_POINT('Ctrl Pts',(-157.027947771377,225.145665543142,7.62037753112604));
#87813=CARTESIAN_POINT('Ctrl Pts',(-158.265582224268,222.582127406304,7.46161966589425));
#87814=CARTESIAN_POINT('Ctrl Pts',(-161.090555757304,222.231426172136,7.30286180066245));
#87815=CARTESIAN_POINT('Ctrl Pts',(-162.917452704141,224.414523596358,7.14410393543066));
#87816=CARTESIAN_POINT('Ctrl Pts',(-162.074297050874,227.133449002169,6.98534607019887));
#87817=CARTESIAN_POINT('Ctrl Pts',(-159.332744818217,227.899841965091,6.82658820496707));
#87818=CARTESIAN_POINT('Ctrl Pts',(-157.201864501689,226.012299675595,6.66783033973529));
#87819=CARTESIAN_POINT('Ctrl Pts',(-157.631837683181,223.198300762802,6.50907247450349));
#87820=CARTESIAN_POINT('Ctrl Pts',(-160.229152923901,222.033216921042,6.3503146092717));
#87821=CARTESIAN_POINT('Ctrl Pts',(-162.616747417678,223.583332836479,6.1915567440399));
#87822=CARTESIAN_POINT('Ctrl Pts',(-162.609494777697,226.429982484261,6.03279887880811));
#87823=CARTESIAN_POINT('Ctrl Pts',(-160.214032619784,227.96791221868,5.87404101357632));
#87824=CARTESIAN_POINT('Ctrl Pts',(-157.622687816661,226.789608807273,5.71528314834453));
#87825=CARTESIAN_POINT('Ctrl Pts',(-157.207059030245,223.973455485825,5.55652528311273));
#87826=CARTESIAN_POINT('Ctrl Pts',(-159.347529709518,222.096795663381,5.39776741788095));
#87827=CARTESIAN_POINT('Ctrl Pts',(-162.085141172983,222.877148335646,5.23900955264915));
#87828=CARTESIAN_POINT('Ctrl Pts',(-162.91443151693,225.600334767647,5.08025168741736));
#87829=CARTESIAN_POINT('Ctrl Pts',(-161.07643425119,227.774094843907,4.92149382218557));
#87830=CARTESIAN_POINT('Ctrl Pts',(-158.253284401091,227.409003428108,4.76273595695378));
#87831=CARTESIAN_POINT('Ctrl Pts',(-157.028728598424,224.839192169644,4.60397809172198));
#87832=CARTESIAN_POINT('Ctrl Pts',(-158.523480265641,222.416552231182,4.44522022649019));
#87833=CARTESIAN_POINT('Ctrl Pts',(-161.369542735673,222.358283589184,4.28646236125839));
#87834=CARTESIAN_POINT('Ctrl Pts',(-162.962199747888,224.717713702413,4.12770449602661));
#87835=CARTESIAN_POINT('Ctrl Pts',(-161.843851667291,227.335492224234,3.96894663079481));
#87836=CARTESIAN_POINT('Ctrl Pts',(-159.038010613361,227.815828353986,3.81018876556302));
#87837=CARTESIAN_POINT('Ctrl Pts',(-157.112582208121,225.719118485504,3.65143090033122));
#87838=CARTESIAN_POINT('Ctrl Pts',(-157.82971845274,222.964271406113,3.49267303509944));
#87839=CARTESIAN_POINT('Ctrl Pts',(-160.533096283493,222.072523058399,3.33391516986764));
#87840=CARTESIAN_POINT('Ctrl Pts',(-162.74858441775,223.860001487113,3.17515730463585));
#87841=CARTESIAN_POINT('Ctrl Pts',(-162.448568198491,226.690806521207,3.01639943940406));
#87842=CARTESIAN_POINT('Ctrl Pts',(-159.9076224654,227.974185470311,2.85764157417226));
#87843=CARTESIAN_POINT('Ctrl Pts',(-157.451220637679,226.535590042229,2.69888370894047));
#87844=CARTESIAN_POINT('Ctrl Pts',(-157.327461604252,223.691622567693,2.54012584370868));
#87845=CARTESIAN_POINT('Ctrl Pts',(-159.649609559608,222.045082275649,2.38136797847689));
#87846=CARTESIAN_POINT('Ctrl Pts',(-162.292434927495,223.102882137353,2.2226101132451));
#87847=CARTESIAN_POINT('Ctrl Pts',(-162.837223742218,225.896925087452,2.0638522480133));
#87848=CARTESIAN_POINT('Ctrl Pts',(-160.785385909792,227.870100375464,1.90509438278151));
#87849=CARTESIAN_POINT('Ctrl Pts',(-158.014762072539,227.216563766624,1.74633651754972));
#87850=CARTESIAN_POINT('Ctrl Pts',(-157.061029674385,224.534420088943,1.58757865231793));
#87851=CARTESIAN_POINT('Ctrl Pts',(-158.797039138337,222.278391720749,1.42882078708613));
#87852=CARTESIAN_POINT('Ctrl Pts',(-161.634005938982,222.513144712115,1.27006292185434));
#87853=CARTESIAN_POINT('Ctrl Pts',(-162.975514791558,225.023939007964,1.11130505662255));
#87854=CARTESIAN_POINT('Ctrl Pts',(-161.593865360312,227.512676081583,0.952547191390756));
#87855=CARTESIAN_POINT('Ctrl Pts',(-158.753442480452,227.702119700194,0.793789326158963));
#87856=CARTESIAN_POINT('Ctrl Pts',(-157.054009871723,225.417945126632,0.635031460927172));
#87857=CARTESIAN_POINT('Ctrl Pts',(-158.050454097125,222.752591008343,0.476273595695375));
#87858=CARTESIAN_POINT('Ctrl Pts',(-160.831717617507,222.141302018896,0.317515730463588));
#87859=CARTESIAN_POINT('Ctrl Pts',(-162.850434549562,224.151955971349,0.158757865231792));
#87860=CARTESIAN_POINT('Ctrl Pts',(-162.457434515453,225.999756515378,0.0529192884105984));
#87861=CARTESIAN_POINT('Ctrl Pts',(-161.913465996665,226.635987203375,0.));
#87862=CARTESIAN_POINT('Ctrl Pts',(-161.913465996665,226.635987203375,0.));
#87863=CARTESIAN_POINT('Ctrl Pts',(-161.975061835647,226.578102239736,-1.1918084162755E-16));
#87864=CARTESIAN_POINT('Ctrl Pts',(-162.03328572045,226.517065589828,-7.91451747642661E-15));
#87865=CARTESIAN_POINT('Ctrl Pts',(-162.088141282815,226.453262312389,-5.71764857681956E-15));
#87866=CARTESIAN_POINT('Ctrl Pts',(-162.144450866834,226.387767841878,-3.46254866446102E-15));
#87867=CARTESIAN_POINT('Ctrl Pts',(-162.197211632774,226.319357701911,2.40033719953046E-15));
#87868=CARTESIAN_POINT('Ctrl Pts',(-162.246401946459,226.248399837308,1.66533453693773E-15));
#87869=CARTESIAN_POINT('Ctrl Pts',(-162.297290196901,226.174992670038,9.0496126895645E-16));
#87870=CARTESIAN_POINT('Ctrl Pts',(-162.344357835219,226.098858337835,3.49623503131884E-15));
#87871=CARTESIAN_POINT('Ctrl Pts',(-162.387545974877,226.02036021425,4.05231403988182E-15));
#87872=CARTESIAN_POINT('Ctrl Pts',(-162.406440785977,225.986017285181,4.29559860612813E-15));
#87873=CARTESIAN_POINT('Ctrl Pts',(-162.424592542808,225.951221405267,1.66664251847669E-15));
#87874=CARTESIAN_POINT('Ctrl Pts',(-162.441993869605,225.916000914244,1.66533453693773E-15));
#87875=CARTESIAN_POINT('Ctrl Pts',(-162.451521836186,225.896716197316,1.66461836141054E-15));
#87876=CARTESIAN_POINT('Ctrl Pts',(-162.460824794419,225.877304161032,1.76785945204013E-15));
#87877=CARTESIAN_POINT('Ctrl Pts',(-162.469901328297,225.857769327789,1.60982338570648E-15));
#87878=CARTESIAN_POINT('Ctrl Pts',(-162.478557483357,225.83913924852,1.45910674500921E-15));
#87879=CARTESIAN_POINT('Ctrl Pts',(-162.487010198395,225.820391466247,1.64355834195759E-15));
#87880=CARTESIAN_POINT('Ctrl Pts',(-162.495244121967,225.801562756482,1.55431223447522E-15));
#87881=CARTESIAN_POINT('Ctrl Pts',(-162.531783565047,225.718007138947,1.15826737976362E-15));
#87882=CARTESIAN_POINT('Ctrl Pts',(-162.564063594148,225.632767868306,-2.35018207924615E-16));
#87883=CARTESIAN_POINT('Ctrl Pts',(-162.592060513761,225.546244193452,1.60982338570648E-15));
#87884=CARTESIAN_POINT('Ctrl Pts',(-162.620521982054,225.458284844261,3.48527615872856E-15));
#87885=CARTESIAN_POINT('Ctrl Pts',(-162.644557514902,225.368997357617,3.19370643993033E-15));
#87886=CARTESIAN_POINT('Ctrl Pts',(-162.664103104093,225.278764048794,1.74860126378462E-15));
#87887=CARTESIAN_POINT('Ctrl Pts',(-162.68330511497,225.190116888533,3.28898586209486E-16));
#87888=CARTESIAN_POINT('Ctrl Pts',(-162.698173901202,225.100555955463,9.49040340436925E-15));
#87889=CARTESIAN_POINT('Ctrl Pts',(-162.708606125223,225.010420931865,9.54791801177635E-15));
#87890=CARTESIAN_POINT('Ctrl Pts',(-162.712740047564,224.974703601891,9.57070902163041E-15));
#87891=CARTESIAN_POINT('Ctrl Pts',(-162.716176818268,224.938895943555,8.03528719691709E-15));
#87892=CARTESIAN_POINT('Ctrl Pts',(-162.718907967693,224.90301855582,8.40993941153556E-15));
#87893=CARTESIAN_POINT('Ctrl Pts',(-162.720526171663,224.881761230701,8.63192056555412E-15));
#87894=CARTESIAN_POINT('Ctrl Pts',(-162.721896640762,224.860479422577,7.91625006826265E-15));
#87895=CARTESIAN_POINT('Ctrl Pts',(-162.723017408846,224.839177393018,8.07687250414801E-15));
#87896=CARTESIAN_POINT('Ctrl Pts',(-162.723759407018,224.825074504822,8.18321167943288E-15));
#87897=CARTESIAN_POINT('Ctrl Pts',(-162.724391877827,224.810962840671,-1.70682398921736E-15));
#87898=CARTESIAN_POINT('Ctrl Pts',(-162.72491390905,224.796858035091,-1.2490009027033E-15));
#87899=CARTESIAN_POINT('Ctrl Pts',(-162.728436906185,224.701669878708,1.84067908658679E-15));
#87900=CARTESIAN_POINT('Ctrl Pts',(-162.726943158831,224.606632526655,3.561771636142E-15));
#87901=CARTESIAN_POINT('Ctrl Pts',(-162.720374596608,224.512145277437,4.24660306919122E-15));
#87902=CARTESIAN_POINT('Ctrl Pts',(-162.713827767741,224.417970657526,4.92916860522656E-15));
#87903=CARTESIAN_POINT('Ctrl Pts',(-162.702240009616,224.324341551697,7.98702549658127E-15));
#87904=CARTESIAN_POINT('Ctrl Pts',(-162.685505817175,224.23163540663,7.88258347483861E-15));
#87905=CARTESIAN_POINT('Ctrl Pts',(-162.683601528504,224.221085793176,7.87069836240063E-15));
#87906=CARTESIAN_POINT('Ctrl Pts',(-162.681630540887,224.210548121617,1.13803607953457E-14));
#87907=CARTESIAN_POINT('Ctrl Pts',(-162.679592656004,224.20002294205,1.14908083048704E-14));
#87908=CARTESIAN_POINT('Ctrl Pts',(-162.662059443819,224.109468167218,1.24420909448365E-14));
#87909=CARTESIAN_POINT('Ctrl Pts',(-162.639578714029,224.019837772689,9.58219353840262E-15));
#87910=CARTESIAN_POINT('Ctrl Pts',(-162.612425368603,223.931369358019,1.01585406753202E-14));
#87911=CARTESIAN_POINT('Ctrl Pts',(-162.60172511415,223.896506819604,1.03856604250736E-14));
#87912=CARTESIAN_POINT('Ctrl Pts',(-162.590298676337,223.86182477492,8.90058523051191E-15));
#87913=CARTESIAN_POINT('Ctrl Pts',(-162.578160711599,223.827338101979,8.90953977261688E-15));
#87914=CARTESIAN_POINT('Ctrl Pts',(-162.572850315517,223.812250078835,8.91345741172205E-15));
#87915=CARTESIAN_POINT('Ctrl Pts',(-162.56740371175,223.797199455213,5.91681775914833E-15));
#87916=CARTESIAN_POINT('Ctrl Pts',(-162.561822058418,223.782187496193,5.82867087928207E-15));
#87917=CARTESIAN_POINT('Ctrl Pts',(-162.55740131404,223.770297823102,5.75885736698703E-15));
#87918=CARTESIAN_POINT('Ctrl Pts',(-162.552896256506,223.758433615952,6.99654648590045E-15));
#87919=CARTESIAN_POINT('Ctrl Pts',(-162.548311193376,223.746604662409,7.105427357601E-15));
#87920=CARTESIAN_POINT('Ctrl Pts',(-162.514552827935,223.659511829625,7.9070826788108E-15));
#87921=CARTESIAN_POINT('Ctrl Pts',(-162.476411491524,223.574193830615,9.12682322584472E-15));
#87922=CARTESIAN_POINT('Ctrl Pts',(-162.434220451094,223.490881399508,8.42381719934338E-15));
#87923=CARTESIAN_POINT('Ctrl Pts',(-162.390447085663,223.404444434346,7.69444576443903E-15));
#87924=CARTESIAN_POINT('Ctrl Pts',(-162.342314439683,223.320165571839,1.09227548171616E-14));
#87925=CARTESIAN_POINT('Ctrl Pts',(-162.290138616362,223.238305524255,9.53404022396853E-15));
#87926=CARTESIAN_POINT('Ctrl Pts',(-162.237361096172,223.155501458327,8.12931083370241E-15));
#87927=CARTESIAN_POINT('Ctrl Pts',(-162.180446197562,223.075171502158,1.26107348299605E-14));
#87928=CARTESIAN_POINT('Ctrl Pts',(-162.119669180754,222.997600288849,1.22402088464924E-14));
#87929=CARTESIAN_POINT('Ctrl Pts',(-162.076869866936,222.94297446356,1.19792836040716E-14));
#87930=CARTESIAN_POINT('Ctrl Pts',(-162.032154224472,222.889716988046,9.06583501434719E-15));
#87931=CARTESIAN_POINT('Ctrl Pts',(-161.985604958578,222.837934980372,8.52096171399808E-15));
#87932=CARTESIAN_POINT('Ctrl Pts',(-161.9743988715,222.825469183633,8.38979106001418E-15));
#87933=CARTESIAN_POINT('Ctrl Pts',(-161.963085875323,222.813088400073,5.60125771483385E-15));
#87934=CARTESIAN_POINT('Ctrl Pts',(-161.951678364305,222.800806055908,5.71764857681956E-15));
#87935=CARTESIAN_POINT('Ctrl Pts',(-161.883012077408,222.726873804882,6.41825086494875E-15));
#87936=CARTESIAN_POINT('Ctrl Pts',(-161.810832846144,222.656402638005,1.24845656601378E-14));
#87937=CARTESIAN_POINT('Ctrl Pts',(-161.73545380071,222.589679529204,1.12479470182336E-14));
#87938=CARTESIAN_POINT('Ctrl Pts',(-161.670633848202,222.532302990158,1.01845538540404E-14));
#87939=CARTESIAN_POINT('Ctrl Pts',(-161.603446707105,222.477697927691,1.0704076426586E-14));
#87940=CARTESIAN_POINT('Ctrl Pts',(-161.534065264026,222.426062117926,1.09842690498851E-14));
#87941=CARTESIAN_POINT('Ctrl Pts',(-161.508545546914,222.407069557385,1.10873288331103E-14));
#87942=CARTESIAN_POINT('Ctrl Pts',(-161.482728748481,222.38847887615,5.71429167113529E-15));
#87943=CARTESIAN_POINT('Ctrl Pts',(-161.456622762885,222.370300567934,5.88418203051333E-15));
#87944=CARTESIAN_POINT('Ctrl Pts',(-161.439930310342,222.358677158962,5.99281178329901E-15));
#87945=CARTESIAN_POINT('Ctrl Pts',(-161.423118575947,222.347221775582,1.01871413174874E-14));
#87946=CARTESIAN_POINT('Ctrl Pts',(-161.406204408697,222.335946808143,9.91567938868343E-15));
#87947=CARTESIAN_POINT('Ctrl Pts',(-161.320010751063,222.278490199795,8.53232446466678E-15));
#87948=CARTESIAN_POINT('Ctrl Pts',(-161.231075434318,222.225655712217,6.65843379994348E-15));
#87949=CARTESIAN_POINT('Ctrl Pts',(-161.139704820809,222.177762703399,5.31519273039294E-15));
#87950=CARTESIAN_POINT('Ctrl Pts',(-161.0483342073,222.129869694581,3.97195166084239E-15));
#87951=CARTESIAN_POINT('Ctrl Pts',(-160.954527658396,222.086917262382,1.53223770557588E-16));
#87952=CARTESIAN_POINT('Ctrl Pts',(-160.858553722692,222.049265214854,1.94115556961805E-15));
#87953=CARTESIAN_POINT('Ctrl Pts',(-160.837669284051,222.04107192914,2.34062737524038E-15));
#87954=CARTESIAN_POINT('Ctrl Pts',(-160.816682093783,222.033129809198,7.10494195145333E-16));
#87955=CARTESIAN_POINT('Ctrl Pts',(-160.795596246196,222.025437627191,7.49400541621981E-16));
#87956=CARTESIAN_POINT('Ctrl Pts',(-162.514309478995,225.001427434952,19.112583302492));
#87957=CARTESIAN_POINT('Ctrl Pts',(-162.515998851658,225.327429263472,19.092036810933));
#87958=CARTESIAN_POINT('Ctrl Pts',(-162.457161905,225.65284616228,19.071490319374));
#87959=CARTESIAN_POINT('Ctrl Pts',(-162.334969853357,225.952420063482,19.050943827815));
#87960=CARTESIAN_POINT('Ctrl Pts',(-162.020253523137,226.723998881819,18.9980245394044));
#87961=CARTESIAN_POINT('Ctrl Pts',(-161.28526151414,227.324144263772,18.9451052509938));
#87962=CARTESIAN_POINT('Ctrl Pts',(-160.466339361713,227.478242028834,18.8921859625833));
#87963=CARTESIAN_POINT('Ctrl Pts',(-159.647417209287,227.632339793896,18.8392666741727));
#87964=CARTESIAN_POINT('Ctrl Pts',(-158.744564913432,227.340389942067,18.7863473857621));
#87965=CARTESIAN_POINT('Ctrl Pts',(-158.170921302355,226.735982775423,18.7334280973515));
#87966=CARTESIAN_POINT('Ctrl Pts',(-157.597277691277,226.131575608779,18.6805088089409));
#87967=CARTESIAN_POINT('Ctrl Pts',(-157.352842764978,225.214711127319,18.6275895205303));
#87968=CARTESIAN_POINT('Ctrl Pts',(-157.549473008242,224.404949364519,18.5746702321197));
#87969=CARTESIAN_POINT('Ctrl Pts',(-157.746103251505,223.595187601719,18.5217509437091));
#87970=CARTESIAN_POINT('Ctrl Pts',(-158.38379866433,222.892528557579,18.4688316552985));
#87971=CARTESIAN_POINT('Ctrl Pts',(-159.170748360109,222.61850761625,18.4159123668879));
#87972=CARTESIAN_POINT('Ctrl Pts',(-159.957698055889,222.34448667492,18.3629930784773));
#87973=CARTESIAN_POINT('Ctrl Pts',(-160.893902034623,222.499103836401,18.3100737900667));
#87974=CARTESIAN_POINT('Ctrl Pts',(-161.55095408646,223.011606956009,18.2571545016561));
#87975=CARTESIAN_POINT('Ctrl Pts',(-162.149291705253,223.478312592728,18.2089641019347));
#87976=CARTESIAN_POINT('Ctrl Pts',(-162.516138545369,224.241800343922,18.1607737022133));
#87977=CARTESIAN_POINT('Ctrl Pts',(-162.520906539752,225.001296842262,18.1125833024919));
#87978=CARTESIAN_POINT('Origin',(160.,225.,22.2084234471774));
#87979=CARTESIAN_POINT('Ctrl Pts',(156.923621908153,225.002226325067,19.7084234471775));
#87980=CARTESIAN_POINT('Ctrl Pts',(156.922437019742,225.146330804243,19.7009407276991));
#87981=CARTESIAN_POINT('Ctrl Pts',(156.9971729149,226.308361189561,19.6405387198101));
#87982=CARTESIAN_POINT('Ctrl Pts',(158.478135103599,228.298893815846,19.5272174235105));
#87983=CARTESIAN_POINT('Ctrl Pts',(161.945877075973,228.067610948411,19.3684595582787));
#87984=CARTESIAN_POINT('Ctrl Pts',(163.632669423604,225.029226006693,19.2097016930469));
#87985=CARTESIAN_POINT('Ctrl Pts',(161.994882852242,221.963912542979,19.0509438278151));
#87986=CARTESIAN_POINT('Ctrl Pts',(158.531360299265,221.677313366987,18.8921859625833));
#87987=CARTESIAN_POINT('Ctrl Pts',(157.007146929903,223.658102464642,18.7780125023707));
#87988=CARTESIAN_POINT('Ctrl Pts',(156.922679294227,224.836964788643,18.7167583305688));
#87989=CARTESIAN_POINT('Ctrl Pts',(156.924068523622,224.997572468126,18.7084234471774));
#87990=CARTESIAN_POINT('Ctrl Pts',(156.929637674279,224.99697422706,19.7915765528225));
#87991=CARTESIAN_POINT('Ctrl Pts',(156.934919299465,225.700310641978,19.7552124583938));
#87992=CARTESIAN_POINT('Ctrl Pts',(157.522174047868,227.437424493836,19.6659290755545));
#87993=CARTESIAN_POINT('Ctrl Pts',(160.40727547618,228.609329940462,19.5237264043046));
#87994=CARTESIAN_POINT('Ctrl Pts',(163.25301142787,226.616779086673,19.3649685390728));
#87995=CARTESIAN_POINT('Ctrl Pts',(163.122801956202,223.143422649729,19.2062106738411));
#87996=CARTESIAN_POINT('Ctrl Pts',(160.13402104345,221.369750709928,19.0474528086092));
#87997=CARTESIAN_POINT('Ctrl Pts',(157.425511910903,222.717816803407,18.9092414349364));
#87998=CARTESIAN_POINT('Ctrl Pts',(156.933644860339,224.374657834208,18.8239493496742));
#87999=CARTESIAN_POINT('Ctrl Pts',(156.930395245889,225.001742688239,18.7915765528225));
#88000=CARTESIAN_POINT('Ctrl Pts',(161.913465996665,226.635987203375,20.));
#88001=CARTESIAN_POINT('Ctrl Pts',(162.457434515453,225.999756515379,19.9470807115894));
#88002=CARTESIAN_POINT('Ctrl Pts',(162.85043342369,224.151954738239,19.8412421347682));
#88003=CARTESIAN_POINT('Ctrl Pts',(160.831717966777,222.141302178128,19.6824842695364));
#88004=CARTESIAN_POINT('Ctrl Pts',(158.050453807979,222.752590618786,19.5237264043046));
#88005=CARTESIAN_POINT('Ctrl Pts',(157.054009754812,225.417945292734,19.3649685390728));
#88006=CARTESIAN_POINT('Ctrl Pts',(158.753442369712,227.702119792221,19.206210673841));
#88007=CARTESIAN_POINT('Ctrl Pts',(161.593865475439,227.512676285221,19.0474528086092));
#88008=CARTESIAN_POINT('Ctrl Pts',(162.975514974434,225.023938985472,18.8886949433775));
#88009=CARTESIAN_POINT('Ctrl Pts',(161.634006045394,222.51314456709,18.7299370781457));
#88010=CARTESIAN_POINT('Ctrl Pts',(158.79703906081,222.278391541041,18.5711792129139));
#88011=CARTESIAN_POINT('Ctrl Pts',(157.061029488215,224.534420062994,18.4124213476821));
#88012=CARTESIAN_POINT('Ctrl Pts',(158.014761946265,227.216563905499,18.2536634824503));
#88013=CARTESIAN_POINT('Ctrl Pts',(160.785385959748,227.870100558722,18.0949056172185));
#88014=CARTESIAN_POINT('Ctrl Pts',(162.837223922373,225.896925143905,17.9361477519867));
#88015=CARTESIAN_POINT('Ctrl Pts',(162.292435073093,223.102882017134,17.7773898867549));
#88016=CARTESIAN_POINT('Ctrl Pts',(159.649609537352,222.045082087855,17.6186320215231));
#88017=CARTESIAN_POINT('Ctrl Pts',(157.327461434526,223.691622484669,17.4598741562913));
#88018=CARTESIAN_POINT('Ctrl Pts',(157.451220475812,226.535590139715,17.3011162910595));
#88019=CARTESIAN_POINT('Ctrl Pts',(159.907622459533,227.974185659212,17.1423584258277));
#88020=CARTESIAN_POINT('Ctrl Pts',(162.448568353993,226.690806628577,16.983600560596));
#88021=CARTESIAN_POINT('Ctrl Pts',(162.748584592305,223.86000141472,16.8248426953641));
#88022=CARTESIAN_POINT('Ctrl Pts',(160.533096317349,222.07252287248,16.6660848301324));
#88023=CARTESIAN_POINT('Ctrl Pts',(157.829718314911,222.96427127683,16.5073269649006));
#88024=CARTESIAN_POINT('Ctrl Pts',(157.112582024748,225.719118531172,16.3485690996688));
#88025=CARTESIAN_POINT('Ctrl Pts',(159.038010552267,227.815828532812,16.189811234437));
#88026=CARTESIAN_POINT('Ctrl Pts',(161.843851784389,227.335492372555,16.0310533692052));
#88027=CARTESIAN_POINT('Ctrl Pts',(162.96219993601,224.717713684486,15.8722955039734));
#88028=CARTESIAN_POINT('Ctrl Pts',(161.369542822649,222.358283421415,15.7135376387416));
#88029=CARTESIAN_POINT('Ctrl Pts',(158.523480171871,222.416552067114,15.5547797735098));
#88030=CARTESIAN_POINT('Ctrl Pts',(157.028728409726,224.839192159431,15.396021908278));
#88031=CARTESIAN_POINT('Ctrl Pts',(158.253284290161,227.409003581098,15.2372640430462));
#88032=CARTESIAN_POINT('Ctrl Pts',(161.076434319551,227.774095020083,15.0785061778144));
#88033=CARTESIAN_POINT('Ctrl Pts',(162.914431702018,225.600334805773,14.9197483125826));
#88034=CARTESIAN_POINT('Ctrl Pts',(162.085141305405,222.877148200829,14.7609904473508));
#88035=CARTESIAN_POINT('Ctrl Pts',(159.347529668082,222.096795479006,14.6022325821191));
#88036=CARTESIAN_POINT('Ctrl Pts',(157.207058852872,223.973455420632,14.4434747168873));
#88037=CARTESIAN_POINT('Ctrl Pts',(157.622687665684,226.789608920927,14.2847168516555));
#88038=CARTESIAN_POINT('Ctrl Pts',(160.214032633376,227.967912407165,14.1259589864237));
#88039=CARTESIAN_POINT('Ctrl Pts',(162.609494943419,226.429982575076,13.9672011211919));
#88040=CARTESIAN_POINT('Ctrl Pts',(162.616747583861,223.58333274651,13.8084432559601));
#88041=CARTESIAN_POINT('Ctrl Pts',(160.229152938454,222.03321673263,13.6496853907283));
#88042=CARTESIAN_POINT('Ctrl Pts',(157.631837532785,223.19830064838,13.4909275254965));
#88043=CARTESIAN_POINT('Ctrl Pts',(157.201864323986,226.012299739883,13.3321696602647));
#88044=CARTESIAN_POINT('Ctrl Pts',(159.33274477584,227.899842149253,13.1734117950329));
#88045=CARTESIAN_POINT('Ctrl Pts',(162.074297182607,227.133449137659,13.0146539298011));
#88046=CARTESIAN_POINT('Ctrl Pts',(162.917452889421,224.414523559176,12.8558960645693));
#88047=CARTESIAN_POINT('Ctrl Pts',(161.090555826563,222.231425996311,12.6971381993376));
#88048=CARTESIAN_POINT('Ctrl Pts',(158.26558211412,222.582127252751,12.5383803341057));
#88049=CARTESIAN_POINT('Ctrl Pts',(157.02794758263,225.145665552392,12.379622468874));
#88050=CARTESIAN_POINT('Ctrl Pts',(158.510335306644,227.575890744212,12.2208646036422));
#88051=CARTESIAN_POINT('Ctrl Pts',(161.356064099438,227.648660828224,12.0621067384104));
#88052=CARTESIAN_POINT('Ctrl Pts',(162.960723081753,225.297376626401,11.9033488731786));
#88053=CARTESIAN_POINT('Ctrl Pts',(161.855728416075,222.67393334779,11.7445910079468));
#88054=CARTESIAN_POINT('Ctrl Pts',(159.05237117698,222.179306177811,11.585833142715));
#88055=CARTESIAN_POINT('Ctrl Pts',(157.116283799449,224.266177882979,11.4270752774832));
#88056=CARTESIAN_POINT('Ctrl Pts',(157.819373375262,227.024643560787,11.2683174122514));
#88057=CARTESIAN_POINT('Ctrl Pts',(160.518172352285,227.93015553138,11.1095595470196));
#88058=CARTESIAN_POINT('Ctrl Pts',(162.742740012873,226.15398927488,10.9508016817878));
#88059=CARTESIAN_POINT('Ctrl Pts',(162.457152121535,223.321692079389,10.792043816556));
#88060=CARTESIAN_POINT('Ctrl Pts',(159.922778705194,222.025382226843,10.6332859513242));
#88061=CARTESIAN_POINT('Ctrl Pts',(157.459078214822,223.451442443317,10.4745280860925));
#88062=CARTESIAN_POINT('Ctrl Pts',(157.320829242326,226.294742474771,10.3157702208606));
#88063=CARTESIAN_POINT('Ctrl Pts',(159.634557241897,227.95309424423,10.1570123556289));
#88064=CARTESIAN_POINT('Ctrl Pts',(162.282738439313,226.908774277497,9.99825449039706));
#88065=CARTESIAN_POINT('Ctrl Pts',(162.841757506836,224.117544167059,9.83949662516529));
#88066=CARTESIAN_POINT('Ctrl Pts',(160.800000215852,222.133937600228,9.68073875993349));
#88067=CARTESIAN_POINT('Ctrl Pts',(158.026082758779,222.773351228962,9.52198089470171));
#88068=CARTESIAN_POINT('Ctrl Pts',(157.058694283249,225.45059372539,9.3632230294699));
#88069=CARTESIAN_POINT('Ctrl Pts',(158.783188684025,227.715452862059,9.20446516423811));
#88070=CARTESIAN_POINT('Ctrl Pts',(161.621308753332,227.495129646155,9.04570729900632));
#88071=CARTESIAN_POINT('Ctrl Pts',(162.975607115345,224.991263876208,8.88694943377453));
#88072=CARTESIAN_POINT('Ctrl Pts',(161.606629962408,222.495393406412,8.72819156854274));
#88073=CARTESIAN_POINT('Ctrl Pts',(158.767265131054,222.291738792576,8.56943370331094));
#88074=CARTESIAN_POINT('Ctrl Pts',(157.056099203283,224.566684729275,8.41067583807915));
#88075=CARTESIAN_POINT('Ctrl Pts',(158.039191168902,227.238200784702,8.25191797284736));
#88076=CARTESIAN_POINT('Ctrl Pts',(160.816815299634,227.861315569984,8.09316010761556));
#88077=CARTESIAN_POINT('Ctrl Pts',(162.846890100262,225.865754458136,7.93440224238378));
#88078=CARTESIAN_POINT('Ctrl Pts',(162.271491193081,223.077854900246,7.77564437715198));
#88079=CARTESIAN_POINT('Ctrl Pts',(159.617223635317,222.049102462065,7.61688651192019));
#88080=CARTESIAN_POINT('Ctrl Pts',(157.313272991458,223.72101133456,7.4581286466884));
#88081=CARTESIAN_POINT('Ctrl Pts',(157.468214800164,226.563450583371,7.2993707814566));
#88082=CARTESIAN_POINT('Ctrl Pts',(159.9402463242,227.975019919762,7.14061291622481));
#88083=CARTESIAN_POINT('Ctrl Pts',(162.466964409978,226.663851142576,6.98185505099302));
#88084=CARTESIAN_POINT('Ctrl Pts',(162.735916764755,223.829925865134,6.82309718576123));
#88085=CARTESIAN_POINT('Ctrl Pts',(160.500958204016,222.066852389909,6.66433932052943));
#88086=CARTESIAN_POINT('Ctrl Pts',(157.807522714661,222.988195492096,6.50558145529764));
#88087=CARTESIAN_POINT('Ctrl Pts',(157.120642350631,225.750742000804,6.34682359006585));
#88088=CARTESIAN_POINT('Ctrl Pts',(159.068949994076,227.826209459899,6.18806572483406));
#88089=CARTESIAN_POINT('Ctrl Pts',(161.86935456633,227.315130132432,6.02930785960226));
#88090=CARTESIAN_POINT('Ctrl Pts',(162.958925912989,224.685243798804,5.87054999437047));
#88091=CARTESIAN_POINT('Ctrl Pts',(161.340488380438,222.343422328133,5.71179212913868));
#88092=CARTESIAN_POINT('Ctrl Pts',(158.495235934823,222.432900638288,5.55303426390689));
#88093=CARTESIAN_POINT('Ctrl Pts',(157.027143502485,224.871788183333,5.39427639867509));
#88094=CARTESIAN_POINT('Ctrl Pts',(158.279809219768,227.42801517795,5.2355185334433));
#88095=CARTESIAN_POINT('Ctrl Pts',(161.106793471474,227.762122777187,5.07676066821151));
#88096=CARTESIAN_POINT('Ctrl Pts',(162.920840381611,225.56833571936,4.91800280297972));
#88097=CARTESIAN_POINT('Ctrl Pts',(162.061734289357,222.854407833525,4.75924493774793));
#88098=CARTESIAN_POINT('Ctrl Pts',(159.315729056558,222.104125814073,4.60048707251613));
#88099=CARTESIAN_POINT('Ctrl Pts',(157.195968564291,224.004147735707,4.44172920728434));
#88100=CARTESIAN_POINT('Ctrl Pts',(157.642457531714,226.815573610455,4.28297134205255));
#88101=CARTESIAN_POINT('Ctrl Pts',(160.246569273415,227.965386588322,4.12421347682076));
#88102=CARTESIAN_POINT('Ctrl Pts',(162.625020825759,226.401277877144,3.96545561158896));
#88103=CARTESIAN_POINT('Ctrl Pts',(162.601053421645,223.554719707956,3.80669774635717));
#88104=CARTESIAN_POINT('Ctrl Pts',(160.196602028221,222.030882005113,3.64793988112538));
#88105=CARTESIAN_POINT('Ctrl Pts',(157.612220466518,223.224380974637,3.48918201589359));
#88106=CARTESIAN_POINT('Ctrl Pts',(157.213134639509,226.042926405927,3.33042415066179));
#88107=CARTESIAN_POINT('Ctrl Pts',(159.364587881769,227.9069856324,3.17166628543));
#88108=CARTESIAN_POINT('Ctrl Pts',(162.0975702677,227.110571720598,3.01290842019821));
#88109=CARTESIAN_POINT('Ctrl Pts',(162.910856431158,224.382562656872,2.85415055496641));
#88110=CARTESIAN_POINT('Ctrl Pts',(161.060126894903,222.219632217471,2.69539268973462));
#88111=CARTESIAN_POINT('Ctrl Pts',(158.239169283519,222.601294279545,2.53663482450283));
#88112=CARTESIAN_POINT('Ctrl Pts',(157.029723838513,225.178251688952,2.37787695927104));
#88113=CARTESIAN_POINT('Ctrl Pts',(158.538675094614,227.592073229572,2.21911909403925));
#88114=CARTESIAN_POINT('Ctrl Pts',(161.385030691198,227.6336293073,2.06036122880745));
#88115=CARTESIAN_POINT('Ctrl Pts',(162.963806576262,225.26488824769,1.90160336357566));
#88116=CARTESIAN_POINT('Ctrl Pts',(161.830106129847,222.653720849312,1.74284549834387));
#88117=CARTESIAN_POINT('Ctrl Pts',(159.02149401452,222.189869334119,1.58408763311208));
#88118=CARTESIAN_POINT('Ctrl Pts',(157.108407655953,224.297846602939,1.42532976788028));
#88119=CARTESIAN_POINT('Ctrl Pts',(157.841712478851,227.048440217077,1.26657190264849));
#88120=CARTESIAN_POINT('Ctrl Pts',(160.550269543046,227.924289837736,1.1078140374167));
#88121=CARTESIAN_POINT('Ctrl Pts',(162.755245701977,226.123853559107,0.949056172184904));
#88122=CARTESIAN_POINT('Ctrl Pts',(162.438567649914,223.29481665065,0.790298306953114));
#88123=CARTESIAN_POINT('Ctrl Pts',(159.890223501773,222.026467019093,0.631540441721318));
#88124=CARTESIAN_POINT('Ctrl Pts',(157.442116623435,223.479279799228,0.472782576489526));
#88125=CARTESIAN_POINT('Ctrl Pts',(157.335462140697,226.324301623048,0.314024711257735));
#88126=CARTESIAN_POINT('Ctrl Pts',(159.666401142308,227.95639832968,0.15526684602594));
#88127=CARTESIAN_POINT('Ctrl Pts',(162.304705497016,226.88473886389,-0.00349101920584817));
#88128=CARTESIAN_POINT('Ctrl Pts',(162.829415771032,224.084271948927,-0.162248884437644));
#88129=CARTESIAN_POINT('Ctrl Pts',(161.458872983031,222.784105799646,-0.268087461258838));
#88130=CARTESIAN_POINT('Ctrl Pts',(160.650199997975,222.567913197965,-0.321006749669435));
#88131=CARTESIAN_POINT('Ctrl Pts',(162.054331550342,226.756425321227,20.1070022498898));
#88132=CARTESIAN_POINT('Ctrl Pts',(162.638345947507,226.073356597808,20.0540829614792));
#88133=CARTESIAN_POINT('Ctrl Pts',(163.060276652233,224.089523335983,19.948244384658));
#88134=CARTESIAN_POINT('Ctrl Pts',(160.892947386112,221.93085054106,19.7894865194262));
#88135=CARTESIAN_POINT('Ctrl Pts',(157.906932102218,222.587140818593,19.6307286541944));
#88136=CARTESIAN_POINT('Ctrl Pts',(156.837131823488,225.448713592338,19.4719707889627));
#88137=CARTESIAN_POINT('Ctrl Pts',(158.661673281008,227.901044466763,19.3132129237308));
#88138=CARTESIAN_POINT('Ctrl Pts',(161.711202675617,227.697654506284,19.1544550584991));
#88139=CARTESIAN_POINT('Ctrl Pts',(163.194566457491,225.025701325879,18.9956971932673));
#88140=CARTESIAN_POINT('Ctrl Pts',(161.754298314344,222.33006722572,18.8369393280355));
#88141=CARTESIAN_POINT('Ctrl Pts',(158.708479473629,222.07803214969,18.6781814628037));
#88142=CARTESIAN_POINT('Ctrl Pts',(156.844668335675,224.500144995801,18.5194235975719));
#88143=CARTESIAN_POINT('Ctrl Pts',(157.868612676768,227.379742923236,18.3606657323401));
#88144=CARTESIAN_POINT('Ctrl Pts',(160.843204509053,228.081391642555,18.2019078671083));
#88145=CARTESIAN_POINT('Ctrl Pts',(163.046094693752,225.96295498568,18.0431500018765));
#88146=CARTESIAN_POINT('Ctrl Pts',(162.461199574998,222.963219971656,17.8843921366447));
#88147=CARTESIAN_POINT('Ctrl Pts',(159.623814489722,221.82754691948,17.7256342714129));
#88148=CARTESIAN_POINT('Ctrl Pts',(157.130714470951,223.595302339218,17.5668764061811));
#88149=CARTESIAN_POINT('Ctrl Pts',(157.26358440624,226.648637225804,17.4081185409493));
#88150=CARTESIAN_POINT('Ctrl Pts',(159.900821809086,228.193139280731,17.2493606757175));
#88151=CARTESIAN_POINT('Ctrl Pts',(162.628827076909,226.815280443273,17.0906028104858));
#88152=CARTESIAN_POINT('Ctrl Pts',(162.950929912838,223.776076990567,16.9318449452539));
#88153=CARTESIAN_POINT('Ctrl Pts',(160.572341805922,221.857007839987,16.7730870800222));
#88154=CARTESIAN_POINT('Ctrl Pts',(157.669946502014,222.814404984862,16.6143292147904));
#88155=CARTESIAN_POINT('Ctrl Pts',(156.900016067218,225.772058604437,16.4555713495586));
#88156=CARTESIAN_POINT('Ctrl Pts',(158.967190806099,228.023124218246,16.2968134843268));
#88157=CARTESIAN_POINT('Ctrl Pts',(161.97959247848,227.507426667046,16.138055619095));
#88158=CARTESIAN_POINT('Ctrl Pts',(163.180271192471,224.696932328455,15.9792977538632));
#88159=CARTESIAN_POINT('Ctrl Pts',(161.470365836141,222.163805511095,15.8205398886314));
#88160=CARTESIAN_POINT('Ctrl Pts',(158.414781724411,222.226363778377,15.6617820233996));
#88161=CARTESIAN_POINT('Ctrl Pts',(156.809989316156,224.827353806653,15.5030241581678));
#88162=CARTESIAN_POINT('Ctrl Pts',(158.124694560314,227.586349624274,15.344266292936));
#88163=CARTESIAN_POINT('Ctrl Pts',(161.155679269127,227.978318367473,15.1855084277042));
#88164=CARTESIAN_POINT('Ctrl Pts',(163.128986356281,225.644530257876,15.0267505624725));
#88165=CARTESIAN_POINT('Ctrl Pts',(162.238645253212,222.720868081619,14.8679926972407));
#88166=CARTESIAN_POINT('Ctrl Pts',(159.299496102435,221.883067347437,14.7092348320089));
#88167=CARTESIAN_POINT('Ctrl Pts',(157.001448091164,223.897883254312,14.5504769667771));
#88168=CARTESIAN_POINT('Ctrl Pts',(157.447674668944,226.9213563635,14.3917191015453));
#88169=CARTESIAN_POINT('Ctrl Pts',(160.229789289339,228.186404204368,14.2329612363135));
#88170=CARTESIAN_POINT('Ctrl Pts',(162.801600761167,226.535255042701,14.0742033710817));
#88171=CARTESIAN_POINT('Ctrl Pts',(162.809387326546,223.479040526326,13.9154455058499));
#88172=CARTESIAN_POINT('Ctrl Pts',(160.246022721146,221.814808060447,13.7566876406181));
#88173=CARTESIAN_POINT('Ctrl Pts',(157.457498131028,223.065663132392,13.5979297753863));
#88174=CARTESIAN_POINT('Ctrl Pts',(156.995871151412,226.086823229506,13.4391719101545));
#88175=CARTESIAN_POINT('Ctrl Pts',(159.283622775889,228.113322749714,13.2804140449227));
#88176=CARTESIAN_POINT('Ctrl Pts',(162.227002807702,227.290509411812,13.1216561796909));
#88177=CARTESIAN_POINT('Ctrl Pts',(163.132229957481,224.371421950292,12.9628983144592));
#88178=CARTESIAN_POINT('Ctrl Pts',(161.170840373345,222.027609095146,12.8041404492274));
#88179=CARTESIAN_POINT('Ctrl Pts',(158.137897725566,222.404128279236,12.6453825839956));
#88180=CARTESIAN_POINT('Ctrl Pts',(156.809151006124,225.156389160089,12.4866247187638));
#88181=CARTESIAN_POINT('Ctrl Pts',(158.4006691604,227.765522687778,12.327866853532));
#88182=CARTESIAN_POINT('Ctrl Pts',(161.455894836186,227.843649960364,12.1691089883002));
#88183=CARTESIAN_POINT('Ctrl Pts',(163.178685615146,225.319268901049,12.0103511230684));
#88184=CARTESIAN_POINT('Ctrl Pts',(161.992343444123,222.502692956048,11.8515932578366));
#88185=CARTESIAN_POINT('Ctrl Pts',(158.982608631386,221.971652319468,11.6928353926048));
#88186=CARTESIAN_POINT('Ctrl Pts',(156.903990359196,224.212155361024,11.534077527373));
#88187=CARTESIAN_POINT('Ctrl Pts',(157.658839988522,227.173693785189,11.3753196621412));
#88188=CARTESIAN_POINT('Ctrl Pts',(160.556319168289,228.145867742628,11.2165617969094));
#88189=CARTESIAN_POINT('Ctrl Pts',(162.944655067114,226.238943665722,11.0578039316776));
#88190=CARTESIAN_POINT('Ctrl Pts',(162.638042764312,223.198138394667,10.8990460664458));
#88191=CARTESIAN_POINT('Ctrl Pts',(159.917093827351,221.806396793957,10.740288201214));
#88192=CARTESIAN_POINT('Ctrl Pts',(157.272020616337,223.337440721832,10.5815303359823));
#88193=CARTESIAN_POINT('Ctrl Pts',(157.123594029977,226.390058835707,10.4227724707505));
#88194=CARTESIAN_POINT('Ctrl Pts',(159.60765407427,228.170495157807,10.2640146055187));
#88195=CARTESIAN_POINT('Ctrl Pts',(162.450789094363,227.049294436158,10.1052567402869));
#88196=CARTESIAN_POINT('Ctrl Pts',(163.050962031669,224.052579527124,9.94649887505509));
#88197=CARTESIAN_POINT('Ctrl Pts',(160.858894637569,221.92294379761,9.78774100982331));
#88198=CARTESIAN_POINT('Ctrl Pts',(157.88076690494,222.609429783521,9.62898314459151));
#88199=CARTESIAN_POINT('Ctrl Pts',(156.842161217574,225.483765537547,9.47022527935972));
#88200=CARTESIAN_POINT('Ctrl Pts',(158.693609459705,227.915359090634,9.31146741412792));
#88201=CARTESIAN_POINT('Ctrl Pts',(161.740666272941,227.678816118616,9.15270954889613));
#88202=CARTESIAN_POINT('Ctrl Pts',(163.194665381632,224.990620740183,8.99395168366434));
#88203=CARTESIAN_POINT('Ctrl Pts',(161.72490685868,222.311009259966,8.83519381843255));
#88204=CARTESIAN_POINT('Ctrl Pts',(158.676513646495,222.092361999286,8.67643595320076));
#88205=CARTESIAN_POINT('Ctrl Pts',(156.839375092992,224.534784922519,8.51767808796896));
#88206=CARTESIAN_POINT('Ctrl Pts',(157.894840330095,227.402972666369,8.35892022273717));
#88207=CARTESIAN_POINT('Ctrl Pts',(160.876947614311,228.071959920453,8.20016235750538));
#88208=CARTESIAN_POINT('Ctrl Pts',(163.056472476395,225.92948957614,8.04140449227359));
#88209=CARTESIAN_POINT('Ctrl Pts',(162.438713848275,222.936350408295,7.88264662704179));
#88210=CARTESIAN_POINT('Ctrl Pts',(159.589044402114,221.831863265628,7.72388876181));
#88211=CARTESIAN_POINT('Ctrl Pts',(157.115481502978,223.626854737674,7.56513089657821));
#88212=CARTESIAN_POINT('Ctrl Pts',(157.281829818885,226.678548699803,7.40637303134641));
#88213=CARTESIAN_POINT('Ctrl Pts',(159.93584737766,228.19403495788,7.24761516611462));
#88214=CARTESIAN_POINT('Ctrl Pts',(162.648577413877,226.786340548107,7.08885730088283));
#88215=CARTESIAN_POINT('Ctrl Pts',(162.937329505067,223.743787338953,6.93009943565104));
#88216=CARTESIAN_POINT('Ctrl Pts',(160.537837748727,221.85091990779,6.77134157041924));
#88217=CARTESIAN_POINT('Ctrl Pts',(157.646116905902,222.840090453183,6.61258370518745));
#88218=CARTESIAN_POINT('Ctrl Pts',(156.908669778231,225.806010130887,6.45382583995566));
#88219=CARTESIAN_POINT('Ctrl Pts',(159.000407947959,228.034269368499,6.29506797472387));
#88220=CARTESIAN_POINT('Ctrl Pts',(162.006972724407,227.485565399381,6.13631010949207));
#88221=CARTESIAN_POINT('Ctrl Pts',(163.1767561424,224.662072074492,5.97755224426028));
#88222=CARTESIAN_POINT('Ctrl Pts',(161.439172463791,222.147850373739,5.81879437902849));
#88223=CARTESIAN_POINT('Ctrl Pts',(158.384458202915,222.243915898783,5.6600365137967));
#88224=CARTESIAN_POINT('Ctrl Pts',(156.808287731201,224.86234948488,5.50127864856491));
#88225=CARTESIAN_POINT('Ctrl Pts',(158.153172202382,227.606760817002,5.34252078333311));
#88226=CARTESIAN_POINT('Ctrl Pts',(161.188273401317,227.965464751912,5.18376291810132));
#88227=CARTESIAN_POINT('Ctrl Pts',(163.135866830095,225.610175462486,5.02500505286953));
#88228=CARTESIAN_POINT('Ctrl Pts',(162.213515059285,222.696453613788,4.86624718763774));
#88229=CARTESIAN_POINT('Ctrl Pts',(159.265354393261,221.890937327165,4.70748932240594));
#88230=CARTESIAN_POINT('Ctrl Pts',(156.989541357638,223.930835076462,4.54873145717415));
#88231=CARTESIAN_POINT('Ctrl Pts',(157.468899953115,226.949232521731,4.38997359194236));
#88232=CARTESIAN_POINT('Ctrl Pts',(160.264721211981,228.183692439776,4.23121572671057));
#88233=CARTESIAN_POINT('Ctrl Pts',(162.818269628026,226.504437162108,4.07245786147877));
#88234=CARTESIAN_POINT('Ctrl Pts',(162.792537791381,223.448321052891,3.91369999624698));
#88235=CARTESIAN_POINT('Ctrl Pts',(160.211075477766,221.812301454944,3.75494213101519));
#88236=CARTESIAN_POINT('Ctrl Pts',(157.436436895433,223.093663440297,3.5961842657834));
#88237=CARTESIAN_POINT('Ctrl Pts',(157.007971165105,226.119704569673,3.4374264005516));
#88238=CARTESIAN_POINT('Ctrl Pts',(159.317810107821,228.120992121855,3.27866853531981));
#88239=CARTESIAN_POINT('Ctrl Pts',(162.251989210943,227.265947804894,3.11991067008802));
#88240=CARTESIAN_POINT('Ctrl Pts',(163.125147881105,224.33710815005,2.96115280485623));
#88241=CARTESIAN_POINT('Ctrl Pts',(161.138171324371,222.014947081809,2.80239493962443));
#88242=CARTESIAN_POINT('Ctrl Pts',(158.10954043501,222.424706344349,2.64363707439264));
#88243=CARTESIAN_POINT('Ctrl Pts',(156.811058026427,225.191374223088,2.48487920916085));
#88244=CARTESIAN_POINT('Ctrl Pts',(158.431095267087,227.782896495463,2.32612134392906));
#88245=CARTESIAN_POINT('Ctrl Pts',(161.486993890709,227.827511848824,2.16736347869726));
#88246=CARTESIAN_POINT('Ctrl Pts',(163.181996110377,225.284388792637,2.00860561346547));
#88247=CARTESIAN_POINT('Ctrl Pts',(161.964834896241,222.480992453711,1.84984774823368));
#88248=CARTESIAN_POINT('Ctrl Pts',(158.949458353755,221.982993114294,1.69108988300189));
#88249=CARTESIAN_POINT('Ctrl Pts',(156.895534389711,224.246155469041,1.53233201777009));
#88250=CARTESIAN_POINT('Ctrl Pts',(157.682823652402,227.199242303896,1.3735741525383));
#88251=CARTESIAN_POINT('Ctrl Pts',(160.590779290273,228.139570228306,1.21481628730651));
#88252=CARTESIAN_POINT('Ctrl Pts',(162.95808140013,226.206589418606,1.05605842207471));
#88253=CARTESIAN_POINT('Ctrl Pts',(162.618090140923,223.169284450419,0.897300556842924));
#88254=CARTESIAN_POINT('Ctrl Pts',(159.882141974727,221.80756144645,0.738542691611128));
#88255=CARTESIAN_POINT('Ctrl Pts',(157.253810346392,223.367327408414,0.579784826379337));
#88256=CARTESIAN_POINT('Ctrl Pts',(157.139304173167,226.421794069577,0.421026961147545));
#88257=CARTESIAN_POINT('Ctrl Pts',(159.641842259173,228.174042483444,0.26226909591575));
#88258=CARTESIAN_POINT('Ctrl Pts',(162.474373323079,227.023489583297,0.103511230683962));
#88259=CARTESIAN_POINT('Ctrl Pts',(163.037711721868,224.016857874595,-0.0552466345478338));
#88260=CARTESIAN_POINT('Ctrl Pts',(161.56627230492,222.620976084267,-0.161085211369028));
#88261=CARTESIAN_POINT('Ctrl Pts',(160.698066426161,222.388867814061,-0.214004499779625));
#88262=CARTESIAN_POINT('Ctrl Pts',(162.195197104019,226.876863439079,20.2140044997796));
#88263=CARTESIAN_POINT('Ctrl Pts',(162.819257379562,226.146956680238,20.161085211369));
#88264=CARTESIAN_POINT('Ctrl Pts',(163.270119880776,224.027091933727,20.0552466345478));
#88265=CARTESIAN_POINT('Ctrl Pts',(160.954176805447,221.720398903991,19.8964887693161));
#88266=CARTESIAN_POINT('Ctrl Pts',(157.763410396457,222.4216910184,19.7377309040842));
#88267=CARTESIAN_POINT('Ctrl Pts',(156.620253892164,225.479481891942,19.5789730388525));
#88268=CARTESIAN_POINT('Ctrl Pts',(158.569904192303,228.099969141304,19.4202151736207));
#88269=CARTESIAN_POINT('Ctrl Pts',(161.828539875795,227.882632727348,19.2614573083889));
#88270=CARTESIAN_POINT('Ctrl Pts',(163.413617940547,225.027463666286,19.1026994431571));
#88271=CARTESIAN_POINT('Ctrl Pts',(161.874590583293,222.146989884349,18.9439415779253));
#88272=CARTESIAN_POINT('Ctrl Pts',(158.619919886447,221.877672758339,18.7851837126935));
#88273=CARTESIAN_POINT('Ctrl Pts',(156.628307183136,224.465869928608,18.6264258474617));
#88274=CARTESIAN_POINT('Ctrl Pts',(157.722463407271,227.542921940972,18.4676679822299));
#88275=CARTESIAN_POINT('Ctrl Pts',(160.901023058357,228.292682726388,18.3089101169981));
#88276=CARTESIAN_POINT('Ctrl Pts',(163.254965465131,226.028984827456,18.1501522517663));
#88277=CARTESIAN_POINT('Ctrl Pts',(162.629964076903,222.823557926178,17.9913943865345));
#88278=CARTESIAN_POINT('Ctrl Pts',(159.598019442091,221.610011751104,17.8326365213027));
#88279=CARTESIAN_POINT('Ctrl Pts',(156.933967507375,223.498982193766,17.673878656071));
#88280=CARTESIAN_POINT('Ctrl Pts',(157.075948336667,226.761684311892,17.5151207908391));
#88281=CARTESIAN_POINT('Ctrl Pts',(159.894021158639,228.41209290225,17.3563629256074));
#88282=CARTESIAN_POINT('Ctrl Pts',(162.809085799825,226.939754257969,17.1976050603756));
#88283=CARTESIAN_POINT('Ctrl Pts',(163.15327523337,223.692152566413,17.0388471951438));
#88284=CARTESIAN_POINT('Ctrl Pts',(160.611587294494,221.641492807494,16.880089329912));
#88285=CARTESIAN_POINT('Ctrl Pts',(157.510174689116,222.664538692895,16.7213314646802));
#88286=CARTESIAN_POINT('Ctrl Pts',(156.687450109689,225.824998677702,16.5625735994484));
#88287=CARTESIAN_POINT('Ctrl Pts',(158.89637105993,228.230419903681,16.4038157342166));
#88288=CARTESIAN_POINT('Ctrl Pts',(162.11533317257,227.679360961537,16.2450578689848));
#88289=CARTESIAN_POINT('Ctrl Pts',(163.398342448932,224.676150972424,16.086300003753));
#88290=CARTESIAN_POINT('Ctrl Pts',(161.571188849632,221.969327600774,15.9275421385212));
#88291=CARTESIAN_POINT('Ctrl Pts',(158.306083276952,222.03617548964,15.7687842732894));
#88292=CARTESIAN_POINT('Ctrl Pts',(156.591250222585,224.815515453875,15.6100264080576));
#88293=CARTESIAN_POINT('Ctrl Pts',(157.996104830467,227.763695667451,15.4512685428258));
#88294=CARTESIAN_POINT('Ctrl Pts',(161.234924218702,228.182541714864,15.2925106775941));
#88295=CARTESIAN_POINT('Ctrl Pts',(163.343541010544,225.68872570998,15.1337528123623));
#88296=CARTESIAN_POINT('Ctrl Pts',(162.392149201018,222.564587962408,14.9749949471305));
#88297=CARTESIAN_POINT('Ctrl Pts',(159.251462536788,221.669339215869,14.8162370818987));
#88298=CARTESIAN_POINT('Ctrl Pts',(156.795837329455,223.822311087992,14.6574792166669));
#88299=CARTESIAN_POINT('Ctrl Pts',(157.272661672204,227.053103806073,14.4987213514351));
#88300=CARTESIAN_POINT('Ctrl Pts',(160.245545945302,228.404896001573,14.3399634862033));
#88301=CARTESIAN_POINT('Ctrl Pts',(162.993706578915,226.640527510327,14.1812056209715));
#88302=CARTESIAN_POINT('Ctrl Pts',(163.00202706923,223.374748306142,14.0224477557397));
#88303=CARTESIAN_POINT('Ctrl Pts',(160.262892503838,221.596399388265,13.8636898905079));
#88304=CARTESIAN_POINT('Ctrl Pts',(157.283158729271,222.933025616404,13.7049320252761));
#88305=CARTESIAN_POINT('Ctrl Pts',(156.789877978838,226.161346719129,13.5461741600443));
#88306=CARTESIAN_POINT('Ctrl Pts',(159.234500775938,228.326803350176,13.3874162948126));
#88307=CARTESIAN_POINT('Ctrl Pts',(162.379708432797,227.447569685965,13.2286584295807));
#88308=CARTESIAN_POINT('Ctrl Pts',(163.34700702554,224.328320341408,13.069900564349));
#88309=CARTESIAN_POINT('Ctrl Pts',(161.251124920127,221.823792193981,12.9111426991172));
#88310=CARTESIAN_POINT('Ctrl Pts',(158.010213337013,222.226129305721,12.7523848338854));
#88311=CARTESIAN_POINT('Ctrl Pts',(156.590354429619,225.167112767786,12.5936269686536));
#88312=CARTESIAN_POINT('Ctrl Pts',(158.291003014156,227.955154631344,12.4348691034218));
#88313=CARTESIAN_POINT('Ctrl Pts',(161.555725572934,228.038639092505,12.27611123819));
#88314=CARTESIAN_POINT('Ctrl Pts',(163.396648148539,225.341161175697,12.1173533729582));
#88315=CARTESIAN_POINT('Ctrl Pts',(162.128958472172,222.331452564307,11.9585955077264));
#88316=CARTESIAN_POINT('Ctrl Pts',(158.912846085792,221.763998461125,11.7998376424946));
#88317=CARTESIAN_POINT('Ctrl Pts',(156.691696918944,224.158132839069,11.6410797772628));
#88318=CARTESIAN_POINT('Ctrl Pts',(157.498306601782,227.322744009591,11.482321912031));
#88319=CARTESIAN_POINT('Ctrl Pts',(160.594465984293,228.361579953876,11.3235640467992));
#88320=CARTESIAN_POINT('Ctrl Pts',(163.146570121355,226.323898056563,11.1648061815674));
#88321=CARTESIAN_POINT('Ctrl Pts',(162.818933407089,223.074584709946,11.0060483163357));
#88322=CARTESIAN_POINT('Ctrl Pts',(159.911408949507,221.58741136107,10.8472904511039));
#88323=CARTESIAN_POINT('Ctrl Pts',(157.084963017852,223.223439000347,10.6885325858721));
#88324=CARTESIAN_POINT('Ctrl Pts',(156.926358817628,226.485375196644,10.5297747206403));
#88325=CARTESIAN_POINT('Ctrl Pts',(159.580750906643,228.387896071384,10.3710168554085));
#88326=CARTESIAN_POINT('Ctrl Pts',(162.618839749411,227.189814594819,10.2122589901767));
#88327=CARTESIAN_POINT('Ctrl Pts',(163.260166556502,223.987614887188,10.0535011249449));
#88328=CARTESIAN_POINT('Ctrl Pts',(160.917789059285,221.711949994992,9.89474325971312));
#88329=CARTESIAN_POINT('Ctrl Pts',(157.735451051101,222.445508338079,9.73598539448132));
#88330=CARTESIAN_POINT('Ctrl Pts',(156.625628151898,225.516937349704,9.57722752924952));
#88331=CARTESIAN_POINT('Ctrl Pts',(158.604030235384,228.115265319207,9.41846966401773));
#88332=CARTESIAN_POINT('Ctrl Pts',(161.860023792551,227.862502591077,9.25971179878595));
#88333=CARTESIAN_POINT('Ctrl Pts',(163.413723647919,224.989977604158,9.10095393355415));
#88334=CARTESIAN_POINT('Ctrl Pts',(161.843183754953,222.126625113519,8.94219606832236));
#88335=CARTESIAN_POINT('Ctrl Pts',(158.585762161935,221.892985205995,8.78343820309056));
#88336=CARTESIAN_POINT('Ctrl Pts',(156.622650982701,224.502885115764,8.62468033785877));
#88337=CARTESIAN_POINT('Ctrl Pts',(157.750489491288,227.567744548037,8.46592247262698));
#88338=CARTESIAN_POINT('Ctrl Pts',(160.937079928988,228.282604270921,8.30716460739519));
#88339=CARTESIAN_POINT('Ctrl Pts',(163.266054852528,225.993224694143,8.1484067421634));
#88340=CARTESIAN_POINT('Ctrl Pts',(162.605936503469,222.794845916344,7.9896488769316));
#88341=CARTESIAN_POINT('Ctrl Pts',(159.560865168911,221.614624069191,7.83089101169982));
#88342=CARTESIAN_POINT('Ctrl Pts',(156.917690014497,223.532698140788,7.67213314646801));
#88343=CARTESIAN_POINT('Ctrl Pts',(157.095444837606,226.793646816236,7.51337528123623));
#88344=CARTESIAN_POINT('Ctrl Pts',(159.93144843112,228.413049995998,7.35461741600443));
#88345=CARTESIAN_POINT('Ctrl Pts',(162.830190417776,226.908829953638,7.19585955077264));
#88346=CARTESIAN_POINT('Ctrl Pts',(163.138742245379,223.657648812771,7.03710168554085));
#88347=CARTESIAN_POINT('Ctrl Pts',(160.574717293439,221.63498742567,6.87834382030906));
#88348=CARTESIAN_POINT('Ctrl Pts',(157.484711097144,222.691985414269,6.71958595507726));
#88349=CARTESIAN_POINT('Ctrl Pts',(156.696697205832,225.861278260969,6.56082808984547));
#88350=CARTESIAN_POINT('Ctrl Pts',(158.931865901843,228.242329277099,6.40207022461368));
#88351=CARTESIAN_POINT('Ctrl Pts',(162.144590882485,227.65600066633,6.24331235938188));
#88352=CARTESIAN_POINT('Ctrl Pts',(163.39458637181,224.63890035018,6.08455449415009));
#88353=CARTESIAN_POINT('Ctrl Pts',(161.537856547144,221.952278419346,5.92579662891829));
#88354=CARTESIAN_POINT('Ctrl Pts',(158.273680471006,222.054931159278,5.76703876368651));
#88355=CARTESIAN_POINT('Ctrl Pts',(156.589431959918,224.852910786426,5.60828089845471));
#88356=CARTESIAN_POINT('Ctrl Pts',(158.026535184995,227.785506456054,5.44952303322292));
#88357=CARTESIAN_POINT('Ctrl Pts',(161.269753331161,228.168806726638,5.29076516799113));
#88358=CARTESIAN_POINT('Ctrl Pts',(163.350893278579,225.652015205613,5.13200730275933));
#88359=CARTESIAN_POINT('Ctrl Pts',(162.365295829214,222.538499394052,4.97324943752755));
#88360=CARTESIAN_POINT('Ctrl Pts',(159.214979729963,221.677748840256,4.81449157229575));
#88361=CARTESIAN_POINT('Ctrl Pts',(156.783114150984,223.857522417217,4.65573370706396));
#88362=CARTESIAN_POINT('Ctrl Pts',(157.295342374516,227.082891433008,4.49697584183217));
#88363=CARTESIAN_POINT('Ctrl Pts',(160.282873150547,228.40199829123,4.33821797660038));
#88364=CARTESIAN_POINT('Ctrl Pts',(163.011518430293,226.607596447073,4.17946011136858));
#88365=CARTESIAN_POINT('Ctrl Pts',(162.984022161118,223.341922397826,4.02070224613679));
#88366=CARTESIAN_POINT('Ctrl Pts',(160.225548927311,221.593720904774,3.861944380905));
#88367=CARTESIAN_POINT('Ctrl Pts',(157.260653324349,222.962945905958,3.7031865156732));
#88368=CARTESIAN_POINT('Ctrl Pts',(156.802807690702,226.196482733419,3.54442865044142));
#88369=CARTESIAN_POINT('Ctrl Pts',(159.271032333874,228.334998611311,3.38567078520962));
#88370=CARTESIAN_POINT('Ctrl Pts',(162.406408154186,227.421323889191,3.22691291997783));
#88371=CARTESIAN_POINT('Ctrl Pts',(163.339439331051,224.291653643227,3.06815505474604));
#88372=CARTESIAN_POINT('Ctrl Pts',(161.216215753841,221.810261946147,2.90939718951424));
#88373=CARTESIAN_POINT('Ctrl Pts',(157.979911586501,222.248118409152,2.75063932428245));
#88374=CARTESIAN_POINT('Ctrl Pts',(156.59239221434,225.204496757223,2.59188145905066));
#88375=CARTESIAN_POINT('Ctrl Pts',(158.323515439561,227.973719761354,2.43312359381887));
#88376=CARTESIAN_POINT('Ctrl Pts',(161.58895709022,228.021394390348,2.27436572858707));
#88377=CARTESIAN_POINT('Ctrl Pts',(163.400185644492,225.303889337585,2.11560786335528));
#88378=CARTESIAN_POINT('Ctrl Pts',(162.099563662636,222.308264058109,1.95684999812349));
#88379=CARTESIAN_POINT('Ctrl Pts',(158.87742269299,221.776116894469,1.7980921328917));
#88380=CARTESIAN_POINT('Ctrl Pts',(156.682661123469,224.194464335143,1.6393342676599));
#88381=CARTESIAN_POINT('Ctrl Pts',(157.523934825953,227.350044390714,1.48057640242811));
#88382=CARTESIAN_POINT('Ctrl Pts',(160.6312890375,228.354850618877,1.32181853719632));
#88383=CARTESIAN_POINT('Ctrl Pts',(163.160917098283,226.289325278104,1.16306067196453));
#88384=CARTESIAN_POINT('Ctrl Pts',(162.797612631933,223.043752250189,1.00430280673273));
#88385=CARTESIAN_POINT('Ctrl Pts',(159.874060447681,221.588655873807,0.845544941500939));
#88386=CARTESIAN_POINT('Ctrl Pts',(157.065504069348,223.255375017599,0.686787076269146));
#88387=CARTESIAN_POINT('Ctrl Pts',(156.943146205637,226.519286516107,0.528029211037356));
#88388=CARTESIAN_POINT('Ctrl Pts',(159.617283376038,228.391686637208,0.36927134580556));
#88389=CARTESIAN_POINT('Ctrl Pts',(162.644041149142,227.162240302705,0.210513480573772));
#88390=CARTESIAN_POINT('Ctrl Pts',(163.246007672705,223.949443800262,0.0517556153419762));
#88391=CARTESIAN_POINT('Ctrl Pts',(161.673671626809,222.457846368889,-0.0540829614792177));
#88392=CARTESIAN_POINT('Ctrl Pts',(160.745932854347,222.209822430158,-0.107002249889815));
#88393=CARTESIAN_POINT('Ctrl Pts',(162.336062657696,226.997301556931,20.3210067496694));
#88394=CARTESIAN_POINT('Ctrl Pts',(163.000168811616,226.220556762668,20.2680874612588));
#88395=CARTESIAN_POINT('Ctrl Pts',(163.479963109319,223.96466053147,20.1622488844376));
#88396=CARTESIAN_POINT('Ctrl Pts',(161.015406224782,221.509947266923,20.0034910192059));
#88397=CARTESIAN_POINT('Ctrl Pts',(157.619888690695,222.256241218208,19.844733153974));
#88398=CARTESIAN_POINT('Ctrl Pts',(156.40337596084,225.510250191546,19.6859752887423));
#88399=CARTESIAN_POINT('Ctrl Pts',(158.478135103599,228.298893815846,19.5272174235105));
#88400=CARTESIAN_POINT('Ctrl Pts',(161.945877075973,228.067610948411,19.3684595582787));
#88401=CARTESIAN_POINT('Ctrl Pts',(163.632669423604,225.029226006693,19.2097016930469));
#88402=CARTESIAN_POINT('Ctrl Pts',(161.994882852242,221.963912542979,19.0509438278151));
#88403=CARTESIAN_POINT('Ctrl Pts',(158.531360299265,221.677313366987,18.8921859625833));
#88404=CARTESIAN_POINT('Ctrl Pts',(156.411946030597,224.431594861414,18.7334280973515));
#88405=CARTESIAN_POINT('Ctrl Pts',(157.576314137774,227.706100958709,18.5746702321197));
#88406=CARTESIAN_POINT('Ctrl Pts',(160.958841607661,228.503973810221,18.4159123668879));
#88407=CARTESIAN_POINT('Ctrl Pts',(163.46383623651,226.095014669232,18.2571545016561));
#88408=CARTESIAN_POINT('Ctrl Pts',(162.798728578809,222.6838958807,18.0983966364243));
#88409=CARTESIAN_POINT('Ctrl Pts',(159.57222439446,221.39247658273,17.9396387711925));
#88410=CARTESIAN_POINT('Ctrl Pts',(156.7372205438,223.402662048314,17.7808809059608));
#88411=CARTESIAN_POINT('Ctrl Pts',(156.888312267094,226.87473139798,17.622123040729));
#88412=CARTESIAN_POINT('Ctrl Pts',(159.887220508192,228.631046523769,17.4633651754972));
#88413=CARTESIAN_POINT('Ctrl Pts',(162.98934452274,227.064228072664,17.3046073102654));
#88414=CARTESIAN_POINT('Ctrl Pts',(163.355620553903,223.60822814226,17.1458494450336));
#88415=CARTESIAN_POINT('Ctrl Pts',(160.650832783067,221.425977775001,16.9870915798018));
#88416=CARTESIAN_POINT('Ctrl Pts',(157.350402876218,222.514672400928,16.82833371457));
#88417=CARTESIAN_POINT('Ctrl Pts',(156.47488415216,225.877938750967,16.6695758493382));
#88418=CARTESIAN_POINT('Ctrl Pts',(158.825551313761,228.437715589115,16.5108179841064));
#88419=CARTESIAN_POINT('Ctrl Pts',(162.251073866661,227.851295256028,16.3520601188746));
#88420=CARTESIAN_POINT('Ctrl Pts',(163.616413705393,224.655369616393,16.1933022536428));
#88421=CARTESIAN_POINT('Ctrl Pts',(161.672011863123,221.774849690454,16.034544388411));
#88422=CARTESIAN_POINT('Ctrl Pts',(158.197384829492,221.845987200903,15.8757865231793));
#88423=CARTESIAN_POINT('Ctrl Pts',(156.372511129014,224.803677101097,15.7170286579474));
#88424=CARTESIAN_POINT('Ctrl Pts',(157.86751510062,227.941041710627,15.5582707927157));
#88425=CARTESIAN_POINT('Ctrl Pts',(161.314169168278,228.386765062254,15.3995129274839));
#88426=CARTESIAN_POINT('Ctrl Pts',(163.558095664808,225.732921162083,15.2407550622521));
#88427=CARTESIAN_POINT('Ctrl Pts',(162.545653148823,222.408307843197,15.0819971970203));
#88428=CARTESIAN_POINT('Ctrl Pts',(159.203428971142,221.4556110843,14.9232393317885));
#88429=CARTESIAN_POINT('Ctrl Pts',(156.590226567747,223.746738921673,14.7644814665567));
#88430=CARTESIAN_POINT('Ctrl Pts',(157.097648675464,227.184851248647,14.6057236013249));
#88431=CARTESIAN_POINT('Ctrl Pts',(160.261302601264,228.623387798777,14.4469657360931));
#88432=CARTESIAN_POINT('Ctrl Pts',(163.185812396663,226.745799977952,14.2882078708613));
#88433=CARTESIAN_POINT('Ctrl Pts',(163.194666811915,223.270456085958,14.1294500056295));
#88434=CARTESIAN_POINT('Ctrl Pts',(160.27976228653,221.377990716082,13.9706921403978));
#88435=CARTESIAN_POINT('Ctrl Pts',(157.108819327513,222.800388100416,13.8119342751659));
#88436=CARTESIAN_POINT('Ctrl Pts',(156.583884806264,226.235870208751,13.6531764099342));
#88437=CARTESIAN_POINT('Ctrl Pts',(159.185378775986,228.540283950637,13.4944185447024));
#88438=CARTESIAN_POINT('Ctrl Pts',(162.532414057892,227.604629960118,13.3356606794706));
#88439=CARTESIAN_POINT('Ctrl Pts',(163.561784093599,224.285218732523,13.1769028142388));
#88440=CARTESIAN_POINT('Ctrl Pts',(161.331409466909,221.619975292816,13.018144949007));
#88441=CARTESIAN_POINT('Ctrl Pts',(157.882528948459,222.048130332206,12.8593870837752));
#88442=CARTESIAN_POINT('Ctrl Pts',(156.371557853113,225.177836375483,12.7006292185434));
#88443=CARTESIAN_POINT('Ctrl Pts',(158.181336867912,228.14478657491,12.5418713533116));
#88444=CARTESIAN_POINT('Ctrl Pts',(161.655556309681,228.233628224646,12.3831134880798));
#88445=CARTESIAN_POINT('Ctrl Pts',(163.614610681933,225.363053450345,12.224355622848));
#88446=CARTESIAN_POINT('Ctrl Pts',(162.265573500221,222.160212172565,12.0655977576162));
#88447=CARTESIAN_POINT('Ctrl Pts',(158.843083540198,221.556344602782,11.9068398923844));
#88448=CARTESIAN_POINT('Ctrl Pts',(156.479403478692,224.104110317114,11.7480820271526));
#88449=CARTESIAN_POINT('Ctrl Pts',(157.337773215042,227.471794233994,11.5893241619208));
#88450=CARTESIAN_POINT('Ctrl Pts',(160.632612800297,228.577292165123,11.4305662966891));
#88451=CARTESIAN_POINT('Ctrl Pts',(163.348485175597,226.408852447405,11.2718084314573));
#88452=CARTESIAN_POINT('Ctrl Pts',(162.999824049866,222.951031025224,11.1130505662255));
#88453=CARTESIAN_POINT('Ctrl Pts',(159.905724071664,221.368425928184,10.9542927009937));
#88454=CARTESIAN_POINT('Ctrl Pts',(156.897905419367,223.109437278862,10.7955348357619));
#88455=CARTESIAN_POINT('Ctrl Pts',(156.729123605279,226.580691557581,10.6367769705301));
#88456=CARTESIAN_POINT('Ctrl Pts',(159.553847739015,228.605296984961,10.4780191052983));
#88457=CARTESIAN_POINT('Ctrl Pts',(162.786890404461,227.33033475348,10.3192612400665));
#88458=CARTESIAN_POINT('Ctrl Pts',(163.469371081335,223.922650247252,10.1605033748347));
#88459=CARTESIAN_POINT('Ctrl Pts',(160.976683481002,221.500956192374,10.0017455096029));
#88460=CARTESIAN_POINT('Ctrl Pts',(157.590135197262,222.281586892638,9.84298764437113));
#88461=CARTESIAN_POINT('Ctrl Pts',(156.409095086223,225.550109161861,9.68422977913934));
#88462=CARTESIAN_POINT('Ctrl Pts',(158.514451011063,228.315171547782,9.52547191390754));
#88463=CARTESIAN_POINT('Ctrl Pts',(161.979381312161,228.046189063538,9.36671404867575));
#88464=CARTESIAN_POINT('Ctrl Pts',(163.632781914206,224.989334468133,9.20795618344396));
#88465=CARTESIAN_POINT('Ctrl Pts',(161.961460651225,221.942240967073,9.04919831821217));
#88466=CARTESIAN_POINT('Ctrl Pts',(158.495010677376,221.693608412704,8.89044045298037));
#88467=CARTESIAN_POINT('Ctrl Pts',(156.40592687241,224.470985309008,8.73168258774858));
#88468=CARTESIAN_POINT('Ctrl Pts',(157.606138652481,227.732516429704,8.57292472251679));
#88469=CARTESIAN_POINT('Ctrl Pts',(160.997212243665,228.493248621389,8.414166857285));
#88470=CARTESIAN_POINT('Ctrl Pts',(163.475637228661,226.056959812147,8.2554089920532));
#88471=CARTESIAN_POINT('Ctrl Pts',(162.773159158663,222.653341424392,8.09665112682142));
#88472=CARTESIAN_POINT('Ctrl Pts',(159.532685935708,221.397384872754,7.93789326158962));
#88473=CARTESIAN_POINT('Ctrl Pts',(156.719898526016,223.438541543901,7.77913539635783));
#88474=CARTESIAN_POINT('Ctrl Pts',(156.909059856328,226.908744932668,7.62037753112604));
#88475=CARTESIAN_POINT('Ctrl Pts',(159.927049484579,228.632065034116,7.46161966589424));
#88476=CARTESIAN_POINT('Ctrl Pts',(163.011803421676,227.031319359169,7.30286180066245));
#88477=CARTESIAN_POINT('Ctrl Pts',(163.34015498569,223.57151028659,7.14410393543066));
#88478=CARTESIAN_POINT('Ctrl Pts',(160.61159683815,221.41905494355,6.98534607019886));
#88479=CARTESIAN_POINT('Ctrl Pts',(157.323305288385,222.543880375355,6.82658820496707));
#88480=CARTESIAN_POINT('Ctrl Pts',(156.484724633432,225.916546391051,6.66783033973528));
#88481=CARTESIAN_POINT('Ctrl Pts',(158.863323855727,228.450389185699,6.50907247450349));
#88482=CARTESIAN_POINT('Ctrl Pts',(162.282209040562,227.826435933279,6.35031460927169));
#88483=CARTESIAN_POINT('Ctrl Pts',(163.612416601221,224.615728625868,6.1915567440399));
#88484=CARTESIAN_POINT('Ctrl Pts',(161.636540630497,221.756706464952,6.03279887880811));
#88485=CARTESIAN_POINT('Ctrl Pts',(158.162902739098,221.865946419773,5.87404101357632));
#88486=CARTESIAN_POINT('Ctrl Pts',(156.370576188634,224.843472087974,5.71528314834453));
#88487=CARTESIAN_POINT('Ctrl Pts',(157.899898167609,227.964252095106,5.55652528311273));
#88488=CARTESIAN_POINT('Ctrl Pts',(161.351233261004,228.372148701364,5.39776741788094));
#88489=CARTESIAN_POINT('Ctrl Pts',(163.565919727063,225.69385494874,5.23900955264914));
#88490=CARTESIAN_POINT('Ctrl Pts',(162.517076599142,222.380545174315,5.08025168741736));
#88491=CARTESIAN_POINT('Ctrl Pts',(159.164605066666,221.464560353348,4.92149382218556));
#88492=CARTESIAN_POINT('Ctrl Pts',(156.57668694433,223.784209757972,4.76273595695378));
#88493=CARTESIAN_POINT('Ctrl Pts',(157.121784795917,227.216550344284,4.60397809172198));
#88494=CARTESIAN_POINT('Ctrl Pts',(160.301025089113,228.620304142684,4.44522022649019));
#88495=CARTESIAN_POINT('Ctrl Pts',(163.20476723256,226.710755732037,4.28646236125839));
#88496=CARTESIAN_POINT('Ctrl Pts',(163.175506530854,223.235523742761,4.1277044960266));
#88497=CARTESIAN_POINT('Ctrl Pts',(160.240022376856,221.375140354604,3.96894663079481));
#88498=CARTESIAN_POINT('Ctrl Pts',(157.084869753264,222.832228371618,3.81018876556302));
#88499=CARTESIAN_POINT('Ctrl Pts',(156.597644216298,226.273260897166,3.65143090033123));
#88500=CARTESIAN_POINT('Ctrl Pts',(159.224254559927,228.549005100767,3.49267303509943));
#88501=CARTESIAN_POINT('Ctrl Pts',(162.560827097429,227.576699973488,3.33391516986764));
#88502=CARTESIAN_POINT('Ctrl Pts',(163.553730780998,224.246199136404,3.17515730463585));
#88503=CARTESIAN_POINT('Ctrl Pts',(161.29426018331,221.605576810485,3.01639943940405));
#88504=CARTESIAN_POINT('Ctrl Pts',(157.850282737992,222.071530473955,2.85764157417226));
#88505=CARTESIAN_POINT('Ctrl Pts',(156.373726402253,225.217619291359,2.69888370894047));
#88506=CARTESIAN_POINT('Ctrl Pts',(158.215935612034,228.164543027245,2.54012584370868));
#88507=CARTESIAN_POINT('Ctrl Pts',(161.69092028973,228.215276931872,2.38136797847688));
#88508=CARTESIAN_POINT('Ctrl Pts',(163.618375178607,225.323389882532,2.22261011324509));
#88509=CARTESIAN_POINT('Ctrl Pts',(162.23429242903,222.135535662507,2.0638522480133));
#88510=CARTESIAN_POINT('Ctrl Pts',(158.805387032225,221.569240674643,1.90509438278151));
#88511=CARTESIAN_POINT('Ctrl Pts',(156.469787857227,224.142773201245,1.74633651754971));
#88512=CARTESIAN_POINT('Ctrl Pts',(157.365045999503,227.500846477532,1.58757865231792));
#88513=CARTESIAN_POINT('Ctrl Pts',(160.671798784727,228.570131009447,1.42882078708613));
#88514=CARTESIAN_POINT('Ctrl Pts',(163.363752796435,226.372061137603,1.27006292185433));
#88515=CARTESIAN_POINT('Ctrl Pts',(162.977135122943,222.918220049959,1.11130505662254));
#88516=CARTESIAN_POINT('Ctrl Pts',(159.865978920635,221.369750301164,0.952547191390749));
#88517=CARTESIAN_POINT('Ctrl Pts',(156.877197792305,223.143422626784,0.793789326158956));
#88518=CARTESIAN_POINT('Ctrl Pts',(156.746988238107,226.616778962636,0.635031460927165));
#88519=CARTESIAN_POINT('Ctrl Pts',(159.592724492903,228.609330790972,0.47627359569537));
#88520=CARTESIAN_POINT('Ctrl Pts',(162.813708975205,227.300991022112,0.317515730463582));
#88521=CARTESIAN_POINT('Ctrl Pts',(163.454303623542,223.882029725929,0.158757865231786));
#88522=CARTESIAN_POINT('Ctrl Pts',(161.781070948697,222.29471665351,0.0529192884105924));
#88523=CARTESIAN_POINT('Ctrl Pts',(160.793799282533,222.030777046254,-4.44089209850063E-15));
#88524=CARTESIAN_POINT('Ctrl Pts',(160.793799282533,222.030777046254,-4.44089209850063E-15));
#88525=CARTESIAN_POINT('Ctrl Pts',(160.886835118416,222.064809970609,-5.00621204762829E-15));
#88526=CARTESIAN_POINT('Ctrl Pts',(160.977803951042,222.103614854342,-3.61054845394339E-15));
#88527=CARTESIAN_POINT('Ctrl Pts',(161.066498240031,222.146862303535,-3.38618022510673E-15));
#88528=CARTESIAN_POINT('Ctrl Pts',(161.157170865599,222.191074392185,-3.15680743645755E-15));
#88529=CARTESIAN_POINT('Ctrl Pts',(161.245467014803,222.239930057968,-6.14220668071666E-15));
#88530=CARTESIAN_POINT('Ctrl Pts',(161.331136020296,222.293122941464,-6.10622663543836E-15));
#88531=CARTESIAN_POINT('Ctrl Pts',(161.414071261832,222.344618399072,-6.07139474112087E-15));
#88532=CARTESIAN_POINT('Ctrl Pts',(161.494544677277,222.400179547073,-6.69073627993026E-15));
#88533=CARTESIAN_POINT('Ctrl Pts',(161.572295150453,222.459559112292,-6.43929354282591E-15));
#88534=CARTESIAN_POINT('Ctrl Pts',(161.640326814483,222.511516231859,-6.2192811478596E-15));
#88535=CARTESIAN_POINT('Ctrl Pts',(161.706273429172,222.56639754431,-2.90661151556184E-15));
#88536=CARTESIAN_POINT('Ctrl Pts',(161.769934822469,222.624050359897,-2.1094237467878E-15));
#88537=CARTESIAN_POINT('Ctrl Pts',(161.783313637273,222.63616643689,-1.94189006632134E-15));
#88538=CARTESIAN_POINT('Ctrl Pts',(161.796593340256,222.64840686525,-6.04831299584486E-15));
#88539=CARTESIAN_POINT('Ctrl Pts',(161.809754778918,222.660753811381,-5.88418203051333E-15));
#88540=CARTESIAN_POINT('Ctrl Pts',(161.882179684673,222.728696718903,-4.9810003950793E-15));
#88541=CARTESIAN_POINT('Ctrl Pts',(161.951138830584,222.799961748911,-2.73633371429518E-15));
#88542=CARTESIAN_POINT('Ctrl Pts',(162.016392999341,222.874256880864,-3.24740234702858E-15));
#88543=CARTESIAN_POINT('Ctrl Pts',(162.081289534507,222.948144829102,-3.75567000453203E-15));
#88544=CARTESIAN_POINT('Ctrl Pts',(162.142522077819,223.025030556139,-1.03735117717522E-14));
#88545=CARTESIAN_POINT('Ctrl Pts',(162.199811703815,223.104653563377,-1.15740750317173E-14));
#88546=CARTESIAN_POINT('Ctrl Pts',(162.255642413703,223.182248921006,-1.27440651984299E-14));
#88547=CARTESIAN_POINT('Ctrl Pts',(162.307728732862,223.262444662234,-8.20072163964933E-15));
#88548=CARTESIAN_POINT('Ctrl Pts',(162.355765712955,223.34501376585,-9.57567358739198E-15));
#88549=CARTESIAN_POINT('Ctrl Pts',(162.376479601884,223.380618153094,-1.01685626880933E-14));
#88550=CARTESIAN_POINT('Ctrl Pts',(162.396439934948,223.416663958761,-2.61105265973387E-15));
#88551=CARTESIAN_POINT('Ctrl Pts',(162.415619286929,223.453133310247,-2.55351295663786E-15));
#88552=CARTESIAN_POINT('Ctrl Pts',(162.428829636786,223.478252662175,-2.51388077254134E-15));
#88553=CARTESIAN_POINT('Ctrl Pts',(162.441669437427,223.503572954656,-7.17365798022769E-15));
#88554=CARTESIAN_POINT('Ctrl Pts',(162.45412919638,223.529088350617,-7.57727214306669E-15));
#88555=CARTESIAN_POINT('Ctrl Pts',(162.460341835531,223.541810743441,-7.77852075142854E-15));
#88556=CARTESIAN_POINT('Ctrl Pts',(162.466459434798,223.554580665549,4.45523880766167E-15));
#88557=CARTESIAN_POINT('Ctrl Pts',(162.472475628322,223.567385868417,4.13558076672871E-15));
#88558=CARTESIAN_POINT('Ctrl Pts',(162.512676157777,223.652950924293,1.99960850495947E-15));
#88559=CARTESIAN_POINT('Ctrl Pts',(162.548420085257,223.74022617982,-7.11576176770946E-15));
#88560=CARTESIAN_POINT('Ctrl Pts',(162.57945637239,223.828973559839,-6.57807142090405E-15));
#88561=CARTESIAN_POINT('Ctrl Pts',(162.609806626417,223.915759247713,-6.05226630304389E-15));
#88562=CARTESIAN_POINT('Ctrl Pts',(162.635655274658,224.003953374654,-8.47510144726437E-15));
#88563=CARTESIAN_POINT('Ctrl Pts',(162.656718423957,224.093342060539,-8.60422844084496E-15));
#88564=CARTESIAN_POINT('Ctrl Pts',(162.660341324486,224.108717079385,-8.62643852191117E-15));
#88565=CARTESIAN_POINT('Ctrl Pts',(162.663822523297,224.124127446413,-7.27321386741096E-15));
#88566=CARTESIAN_POINT('Ctrl Pts',(162.66716041776,224.139572078222,-7.41073868937292E-15));
#88567=CARTESIAN_POINT('Ctrl Pts',(162.687288010448,224.232703620192,-8.24215987393993E-15));
#88568=CARTESIAN_POINT('Ctrl Pts',(162.702208971776,224.327082113126,-4.25211970581271E-15));
#88569=CARTESIAN_POINT('Ctrl Pts',(162.712001602964,224.422299420426,-4.49640324973188E-15));
#88570=CARTESIAN_POINT('Ctrl Pts',(162.715264301484,224.454023822342,-4.57779338298299E-15));
#88571=CARTESIAN_POINT('Ctrl Pts',(162.71795730133,224.485841219662,-6.6124359778604E-15));
#88572=CARTESIAN_POINT('Ctrl Pts',(162.720082299518,224.51773605842,-6.77236045021345E-15));
#88573=CARTESIAN_POINT('Ctrl Pts',(162.721307102418,224.536119552202,-6.86453744993252E-15));
#88574=CARTESIAN_POINT('Ctrl Pts',(162.722343197653,224.554528767701,-5.15903927657121E-15));
#88575=CARTESIAN_POINT('Ctrl Pts',(162.723190824689,224.572960678251,-5.16253706450698E-15));
#88576=CARTESIAN_POINT('Ctrl Pts',(162.723765351252,224.585453935017,-5.16490788562594E-15));
#88577=CARTESIAN_POINT('Ctrl Pts',(162.72425317236,224.597955994038,-6.09967805737917E-15));
#88578=CARTESIAN_POINT('Ctrl Pts',(162.724654243491,224.610456526116,-6.16173778666962E-15));
#88579=CARTESIAN_POINT('Ctrl Pts',(162.727643891428,224.703637478209,-6.62434086836518E-15));
#88580=CARTESIAN_POINT('Ctrl Pts',(162.725824867569,224.796879642422,-1.66933774719167E-14));
#88581=CARTESIAN_POINT('Ctrl Pts',(162.71933597312,224.889808601752,-1.62370117351429E-14));
#88582=CARTESIAN_POINT('Ctrl Pts',(162.712834227217,224.982921609736,-1.57797421520312E-14));
#88583=CARTESIAN_POINT('Ctrl Pts',(162.701643711728,225.075721151049,-6.75753491926581E-15));
#88584=CARTESIAN_POINT('Ctrl Pts',(162.685853019716,225.167818548531,-6.63358257213531E-15));
#88585=CARTESIAN_POINT('Ctrl Pts',(162.670284954048,225.258617503434,-6.5113777771573E-15));
#88586=CARTESIAN_POINT('Ctrl Pts',(162.650245042262,225.34873481927,-7.10343674945186E-15));
#88587=CARTESIAN_POINT('Ctrl Pts',(162.625775134076,225.437772867359,-5.16253706450698E-15));
#88588=CARTESIAN_POINT('Ctrl Pts',(162.616258293167,225.472401560365,-4.40768202457879E-15));
#88589=CARTESIAN_POINT('Ctrl Pts',(162.606070947409,225.506866665537,-1.0540714498591E-14));
#88590=CARTESIAN_POINT('Ctrl Pts',(162.595213990126,225.541143327577,-1.07136521876328E-14));
#88591=CARTESIAN_POINT('Ctrl Pts',(162.589230777255,225.560033018317,-1.08089572514558E-14));
#88592=CARTESIAN_POINT('Ctrl Pts',(162.583044184862,225.578865461749,-9.70376744646794E-15));
#88593=CARTESIAN_POINT('Ctrl Pts',(162.5766542565,225.597636371203,-9.83935155574045E-15));
#88594=CARTESIAN_POINT('Ctrl Pts',(162.57141771802,225.61301910855,-9.95046256750947E-15));
#88595=CARTESIAN_POINT('Ctrl Pts',(162.566044346708,225.628361043375,-6.98833070421156E-15));
#88596=CARTESIAN_POINT('Ctrl Pts',(162.560539662732,225.643645128936,-7.14706072102445E-15));
#88597=CARTESIAN_POINT('Ctrl Pts',(162.528144649867,225.733591827165,-8.08118536097141E-15));
#88598=CARTESIAN_POINT('Ctrl Pts',(162.491164668217,225.821662225634,-4.71317433233986E-15));
#88599=CARTESIAN_POINT('Ctrl Pts',(162.449672336204,225.907413475919,-6.89032164657988E-15));
#88600=CARTESIAN_POINT('Ctrl Pts',(162.418553087193,225.971726913633,-8.52318213225989E-15));
#88601=CARTESIAN_POINT('Ctrl Pts',(162.384894495877,226.034735294909,-7.87655847841885E-15));
#88602=CARTESIAN_POINT('Ctrl Pts',(162.348709870643,226.096234697731,-9.87404602525999E-15));
#88603=CARTESIAN_POINT('Ctrl Pts',(162.334283447985,226.120753851172,-1.06704229234161E-14));
#88604=CARTESIAN_POINT('Ctrl Pts',(162.319455350187,226.14503295866,-1.36977293069563E-14));
#88605=CARTESIAN_POINT('Ctrl Pts',(162.304225832086,226.169058289372,-1.48908663177849E-14));
#88606=CARTESIAN_POINT('Ctrl Pts',(162.293796027918,226.185511829972,-1.57079759128285E-14));
#88607=CARTESIAN_POINT('Ctrl Pts',(162.283182339175,226.20183930785,-9.08136479655679E-15));
#88608=CARTESIAN_POINT('Ctrl Pts',(162.272389232672,226.21803079415,-8.60422844084496E-15));
#88609=CARTESIAN_POINT('Ctrl Pts',(162.224799544389,226.289423380297,-6.5004068553228E-15));
#88610=CARTESIAN_POINT('Ctrl Pts',(162.173700691787,226.358212217461,-5.45208773016714E-15));
#88611=CARTESIAN_POINT('Ctrl Pts',(162.119126547549,226.424044832575,-1.50227053019591E-15));
#88612=CARTESIAN_POINT('Ctrl Pts',(162.068157640418,226.485528461734,2.18661674160883E-15));
#88613=CARTESIAN_POINT('Ctrl Pts',(162.014156917713,226.544433679649,7.08152378222129E-16));
#88614=CARTESIAN_POINT('Ctrl Pts',(161.957129257532,226.600439071007,2.34621350125863E-16));
#88615=CARTESIAN_POINT('Ctrl Pts',(161.943965225959,226.613367126231,1.07305421308585E-16));
#88616=CARTESIAN_POINT('Ctrl Pts',(161.930639817331,226.626140504577,1.02173491822713E-15));
#88617=CARTESIAN_POINT('Ctrl Pts',(161.917156415839,226.638757807614,8.32667268468867E-16));
#88618=CARTESIAN_POINT('Ctrl Pts',(157.480508380744,224.998011611683,18.387416697508));
#88619=CARTESIAN_POINT('Ctrl Pts',(157.479370464687,224.866458062603,18.3957515808994));
#88620=CARTESIAN_POINT('Ctrl Pts',(157.488784817194,224.735067792401,18.4040864642907));
#88621=CARTESIAN_POINT('Ctrl Pts',(157.509319826656,224.605439283086,18.4124213476821));
#88622=CARTESIAN_POINT('Ctrl Pts',(157.639699345747,223.782410555676,18.4653406360927));
#88623=CARTESIAN_POINT('Ctrl Pts',(158.218369203279,223.030401048359,18.5182599245033));
#88624=CARTESIAN_POINT('Ctrl Pts',(158.980531962808,222.693521799041,18.5711792129139));
#88625=CARTESIAN_POINT('Ctrl Pts',(159.742694722338,222.356642549724,18.6240985013245));
#88626=CARTESIAN_POINT('Ctrl Pts',(160.688350383866,222.434893558407,18.6770177897351));
#88627=CARTESIAN_POINT('Ctrl Pts',(161.384763036137,222.892484799145,18.7299370781456));
#88628=CARTESIAN_POINT('Ctrl Pts',(162.081175688407,223.350076039884,18.7828563665562));
#88629=CARTESIAN_POINT('Ctrl Pts',(162.528345331421,224.187007512678,18.8357756549668));
#88630=CARTESIAN_POINT('Ctrl Pts',(162.521655236428,225.020262799033,18.8886949433774));
#88631=CARTESIAN_POINT('Ctrl Pts',(162.514965141436,225.853518085388,18.941614231788));
#88632=CARTESIAN_POINT('Ctrl Pts',(162.054415308437,226.683097185305,18.9945335201986));
#88633=CARTESIAN_POINT('Ctrl Pts',(161.350736540984,227.129460653096,19.0474528086092));
#88634=CARTESIAN_POINT('Ctrl Pts',(160.64705777353,227.575824120888,19.1003720970198));
#88635=CARTESIAN_POINT('Ctrl Pts',(159.700250071621,227.638971956554,19.1532913854304));
#88636=CARTESIAN_POINT('Ctrl Pts',(158.943607451517,227.289850124473,19.206210673841));
#88637=CARTESIAN_POINT('Ctrl Pts',(158.186964831412,226.940728292392,19.2591299622516));
#88638=CARTESIAN_POINT('Ctrl Pts',(157.620487293112,226.179336792563,19.3120492506622));
#88639=CARTESIAN_POINT('Ctrl Pts',(157.503322532823,225.354415263657,19.3649685390728));
#88640=CARTESIAN_POINT('Ctrl Pts',(157.486755586057,225.23777241796,19.3724512585512));
#88641=CARTESIAN_POINT('Ctrl Pts',(157.47917201796,225.119859378455,19.3799339780296));
#88642=CARTESIAN_POINT('Ctrl Pts',(157.480142558574,225.001823580074,19.387416697508));
#88643=CARTESIAN_POINT('Ctrl Pts',(159.206200717467,222.030777046254,20.));
#88644=CARTESIAN_POINT('Ctrl Pts',(158.218929051303,222.29471665351,19.9470807115894));
#88645=CARTESIAN_POINT('Ctrl Pts',(156.545695974101,223.882026824534,19.8412421347682));
#88646=CARTESIAN_POINT('Ctrl Pts',(157.18629137152,227.300991599666,19.6824842695364));
#88647=CARTESIAN_POINT('Ctrl Pts',(160.40727547618,228.609329940462,19.5237264043046));
#88648=CARTESIAN_POINT('Ctrl Pts',(163.25301142787,226.616779086673,19.3649685390728));
#88649=CARTESIAN_POINT('Ctrl Pts',(163.122801956202,223.143422649729,19.2062106738411));
#88650=CARTESIAN_POINT('Ctrl Pts',(160.13402104345,221.369750709928,19.0474528086092));
#88651=CARTESIAN_POINT('Ctrl Pts',(157.022865163748,222.918220199123,18.8886949433775));
#88652=CARTESIAN_POINT('Ctrl Pts',(156.636247501462,226.372061033706,18.7299370781457));
#88653=CARTESIAN_POINT('Ctrl Pts',(159.328201281756,228.570130672657,18.5711792129139));
#88654=CARTESIAN_POINT('Ctrl Pts',(162.634953757174,227.500846255061,18.4124213476821));
#88655=CARTESIAN_POINT('Ctrl Pts',(163.530211822273,224.142773276525,18.2536634824503));
#88656=CARTESIAN_POINT('Ctrl Pts',(161.194612857913,221.569240989169,18.0949056172185));
#88657=CARTESIAN_POINT('Ctrl Pts',(157.76570777529,222.135535923095,17.9361477519867));
#88658=CARTESIAN_POINT('Ctrl Pts',(156.38162515129,225.323389853416,17.7773898867549));
#88659=CARTESIAN_POINT('Ctrl Pts',(158.309079864678,228.215276638311,17.6186320215231));
#88660=CARTESIAN_POINT('Ctrl Pts',(161.78406422512,228.164542738612,17.4598741562913));
#88661=CARTESIAN_POINT('Ctrl Pts',(163.62627326692,225.217619271453,17.3011162910595));
#88662=CARTESIAN_POINT('Ctrl Pts',(162.14971706585,222.071530741175,17.1423584258277));
#88663=CARTESIAN_POINT('Ctrl Pts',(158.705739934788,221.605577120181,16.9836005605959));
#88664=CARTESIAN_POINT('Ctrl Pts',(156.44626954324,224.246199205187,16.8248426953641));
#88665=CARTESIAN_POINT('Ctrl Pts',(157.439173136224,227.576699738386,16.6660848301324));
#88666=CARTESIAN_POINT('Ctrl Pts',(160.775745369292,228.549004776956,16.5073269649006));
#88667=CARTESIAN_POINT('Ctrl Pts',(163.402355473271,226.273260780993,16.3485690996688));
#88668=CARTESIAN_POINT('Ctrl Pts',(162.915129980759,222.832228569406,16.189811234437));
#88669=CARTESIAN_POINT('Ctrl Pts',(159.759977645044,221.375140685337,16.0310533692052));
#88670=CARTESIAN_POINT('Ctrl Pts',(156.82449375888,223.235523903752,15.8722955039734));
#88671=CARTESIAN_POINT('Ctrl Pts',(156.795233059844,226.710755575947,15.7135376387416));
#88672=CARTESIAN_POINT('Ctrl Pts',(159.698974938352,228.620303812367,15.5547797735098));
#88673=CARTESIAN_POINT('Ctrl Pts',(162.878214941473,227.216550142046,15.396021908278));
#88674=CARTESIAN_POINT('Ctrl Pts',(163.423312743327,223.784209868902,15.2372640430462));
#88675=CARTESIAN_POINT('Ctrl Pts',(160.835394857113,221.464560675923,15.0785061778144));
#88676=CARTESIAN_POINT('Ctrl Pts',(157.482923630517,222.380545413314,14.9197483125826));
#88677=CARTESIAN_POINT('Ctrl Pts',(156.434080598292,225.693854885432,14.7609904473509));
#88678=CARTESIAN_POINT('Ctrl Pts',(158.648766862283,228.372148393688,14.6022325821191));
#88679=CARTESIAN_POINT('Ctrl Pts',(162.100101640777,227.964251824647,14.4434747168873));
#88680=CARTESIAN_POINT('Ctrl Pts',(163.629423480216,224.843472102255,14.2847168516555));
#88681=CARTESIAN_POINT('Ctrl Pts',(161.837097093285,221.865946705725,14.1259589864237));
#88682=CARTESIAN_POINT('Ctrl Pts',(158.363459518822,221.756706760871,13.9672011211919));
#88683=CARTESIAN_POINT('Ctrl Pts',(156.387583728377,224.615728660929,13.8084432559601));
#88684=CARTESIAN_POINT('Ctrl Pts',(157.717791167667,227.826435675394,13.6496853907283));
#88685=CARTESIAN_POINT('Ctrl Pts',(161.136676040562,228.450388870885,13.4909275254965));
#88686=CARTESIAN_POINT('Ctrl Pts',(163.515275045834,225.916546307426,13.3321696602647));
#88687=CARTESIAN_POINT('Ctrl Pts',(162.676694467393,222.543880599453,13.1734117950329));
#88688=CARTESIAN_POINT('Ctrl Pts',(159.388403217653,221.419055270276,13.0146539298011));
#88689=CARTESIAN_POINT('Ctrl Pts',(156.659845319066,223.571510416925,12.8558960645693));
#88690=CARTESIAN_POINT('Ctrl Pts',(156.988196853122,227.031319173831,12.6971381993375));
#88691=CARTESIAN_POINT('Ctrl Pts',(160.072950508764,228.632064702726,12.5383803341058));
#88692=CARTESIAN_POINT('Ctrl Pts',(163.090939861654,226.908744758514,12.379622468874));
#88693=CARTESIAN_POINT('Ctrl Pts',(163.280101174706,223.438541686369,12.2208646036422));
#88694=CARTESIAN_POINT('Ctrl Pts',(160.467314021654,221.397385201457,12.0621067384104));
#88695=CARTESIAN_POINT('Ctrl Pts',(157.226841094361,222.653341638501,11.9033488731786));
#88696=CARTESIAN_POINT('Ctrl Pts',(156.524363088457,226.05695971571,11.7445910079468));
#88697=CARTESIAN_POINT('Ctrl Pts',(159.002787847321,228.493248302664,11.585833142715));
#88698=CARTESIAN_POINT('Ctrl Pts',(162.393861129102,227.732516180389,11.4270752774832));
#88699=CARTESIAN_POINT('Ctrl Pts',(163.594072799666,224.470985357276,11.2683174122514));
#88700=CARTESIAN_POINT('Ctrl Pts',(161.504989185309,221.693608714381,11.1095595470196));
#88701=CARTESIAN_POINT('Ctrl Pts',(158.038539527739,221.942241246064,10.9508016817878));
#88702=CARTESIAN_POINT('Ctrl Pts',(156.36721841725,224.989334469106,10.792043816556));
#88703=CARTESIAN_POINT('Ctrl Pts',(158.020618868438,228.046188785603,10.6332859513243));
#88704=CARTESIAN_POINT('Ctrl Pts',(161.485548853394,228.315171245305,10.4745280860925));
#88705=CARTESIAN_POINT('Ctrl Pts',(163.590904586142,225.55010911167,10.3157702208607));
#88706=CARTESIAN_POINT('Ctrl Pts',(162.409864582861,222.281587140667,10.1570123556289));
#88707=CARTESIAN_POINT('Ctrl Pts',(159.023316608111,221.500956511627,9.99825449039707));
#88708=CARTESIAN_POINT('Ctrl Pts',(156.530629235211,223.922650345549,9.83949662516529));
#88709=CARTESIAN_POINT('Ctrl Pts',(157.213109849816,227.330334540859,9.68073875993349));
#88710=CARTESIAN_POINT('Ctrl Pts',(160.446152220277,228.605296656013,9.52198089470171));
#88711=CARTESIAN_POINT('Ctrl Pts',(163.270876096285,226.580691413359,9.3632230294699));
#88712=CARTESIAN_POINT('Ctrl Pts',(163.102094297597,223.109437451357,9.20446516423812));
#88713=CARTESIAN_POINT('Ctrl Pts',(160.094275919735,221.36842625953,9.04570729900632));
#88714=CARTESIAN_POINT('Ctrl Pts',(157.000176223839,222.951031212172,8.88694943377453));
#88715=CARTESIAN_POINT('Ctrl Pts',(156.65151512992,226.408852318861,8.72819156854274));
#88716=CARTESIAN_POINT('Ctrl Pts',(159.367387257422,228.57729183873,8.56943370331094));
#88717=CARTESIAN_POINT('Ctrl Pts',(162.662226542055,227.471794008467,8.41067583807916));
#88718=CARTESIAN_POINT('Ctrl Pts',(163.520596200089,224.104110398856,8.25191797284736));
#88719=CARTESIAN_POINT('Ctrl Pts',(161.156916354245,221.556344916982,8.09316010761557));
#88720=CARTESIAN_POINT('Ctrl Pts',(157.734426706491,222.160212431668,7.93440224238377));
#88721=CARTESIAN_POINT('Ctrl Pts',(156.385389647865,225.363053417219,7.77564437715199));
#88722=CARTESIAN_POINT('Ctrl Pts',(158.344443841372,228.233627929609,7.61688651192019));
#88723=CARTESIAN_POINT('Ctrl Pts',(161.818662966152,228.144786287979,7.4581286466884));
#88724=CARTESIAN_POINT('Ctrl Pts',(163.628441815827,225.177836359257,7.29937078145661));
#88725=CARTESIAN_POINT('Ctrl Pts',(162.117470858342,222.048130601536,7.14061291622482));
#88726=CARTESIAN_POINT('Ctrl Pts',(158.66859065457,221.61997560121,6.98185505099302));
#88727=CARTESIAN_POINT('Ctrl Pts',(156.438216231379,224.28521879774,6.82309718576123));
#88728=CARTESIAN_POINT('Ctrl Pts',(157.467586173166,227.604629722471,6.66433932052944));
#88729=CARTESIAN_POINT('Ctrl Pts',(160.814621149687,228.540283627621,6.50558145529764));
#88730=CARTESIAN_POINT('Ctrl Pts',(163.416114882048,226.235870095991,6.34682359006586));
#88731=CARTESIAN_POINT('Ctrl Pts',(162.891180408695,222.800388301109,6.18806572483405));
#88732=CARTESIAN_POINT('Ctrl Pts',(159.720237738997,221.377991046555,6.02930785960227));
#88733=CARTESIAN_POINT('Ctrl Pts',(156.805333479567,223.270456243762,5.87054999437047));
#88734=CARTESIAN_POINT('Ctrl Pts',(156.814187894011,226.745799818665,5.71179212913869));
#88735=CARTESIAN_POINT('Ctrl Pts',(159.738697422576,228.623387468178,5.55303426390689));
#88736=CARTESIAN_POINT('Ctrl Pts',(162.902351059725,227.184851049301,5.3942763986751));
#88737=CARTESIAN_POINT('Ctrl Pts',(163.409773121145,223.746739036021,5.2355185334433));
#88738=CARTESIAN_POINT('Ctrl Pts',(160.796570956179,221.455611407691,5.07676066821152));
#88739=CARTESIAN_POINT('Ctrl Pts',(157.454347083443,222.408308079663,4.91800280297972));
#88740=CARTESIAN_POINT('Ctrl Pts',(156.441904659834,225.732921095211,4.75924493774793));
#88741=CARTESIAN_POINT('Ctrl Pts',(158.685830951627,228.386764753245,4.60048707251613));
#88742=CARTESIAN_POINT('Ctrl Pts',(162.132484704811,227.941041442286,4.44172920728434));
#88743=CARTESIAN_POINT('Ctrl Pts',(163.627488540013,224.80367711901,4.28297134205255));
#88744=CARTESIAN_POINT('Ctrl Pts',(161.802615006038,221.845987488677,4.12421347682076));
#88745=CARTESIAN_POINT('Ctrl Pts',(158.327988289432,221.774849984717,3.96545561158897));
#88746=CARTESIAN_POINT('Ctrl Pts',(156.38358662457,224.655369647836,3.80669774635717));
#88747=CARTESIAN_POINT('Ctrl Pts',(157.748926338727,227.851294995875,3.64793988112539));
#88748=CARTESIAN_POINT('Ctrl Pts',(161.174448579081,228.437715275457,3.48918201589359));
#88749=CARTESIAN_POINT('Ctrl Pts',(163.525115526208,225.877938670865,3.3304241506618));
#88750=CARTESIAN_POINT('Ctrl Pts',(162.649596882032,222.514672627688,3.17166628543));
#88751=CARTESIAN_POINT('Ctrl Pts',(159.349167276316,221.4259781011,3.01290842019821));
#88752=CARTESIAN_POINT('Ctrl Pts',(156.644379752265,223.608228269237,2.85415055496642));
#88753=CARTESIAN_POINT('Ctrl Pts',(157.010655750008,227.064227884339,2.69539268973463));
#88754=CARTESIAN_POINT('Ctrl Pts',(160.112779481517,228.63104619244,2.53663482450283));
#88755=CARTESIAN_POINT('Ctrl Pts',(163.111687448995,226.874731226991,2.37787695927104));
#88756=CARTESIAN_POINT('Ctrl Pts',(163.262779158505,223.402662193936,2.21911909403925));
#88757=CARTESIAN_POINT('Ctrl Pts',(160.427775566504,221.392476912117,2.06036122880746));
#88758=CARTESIAN_POINT('Ctrl Pts',(157.201271676567,222.683896091561,1.90160336357566));
#88759=CARTESIAN_POINT('Ctrl Pts',(156.536164079478,226.095014570215,1.74284549834387));
#88760=CARTESIAN_POINT('Ctrl Pts',(159.041158479961,228.50397348879,1.58408763311208));
#88761=CARTESIAN_POINT('Ctrl Pts',(162.423685640744,227.706100715127,1.42532976788028));
#88762=CARTESIAN_POINT('Ctrl Pts',(163.588053642863,224.431594906927,1.2665719026485));
#88763=CARTESIAN_POINT('Ctrl Pts',(161.468639564753,221.677313682196,1.1078140374167));
#88764=CARTESIAN_POINT('Ctrl Pts',(158.005117334405,221.963912797343,0.949056172184911));
#88765=CARTESIAN_POINT('Ctrl Pts',(156.367330897151,225.029226046159,0.790298306953121));
#88766=CARTESIAN_POINT('Ctrl Pts',(158.05412312597,228.067610591205,0.631540441721325));
#88767=CARTESIAN_POINT('Ctrl Pts',(161.521864702141,228.298893654481,0.472782576489533));
#88768=CARTESIAN_POINT('Ctrl Pts',(163.59662383415,225.510249900124,0.314024711257741));
#88769=CARTESIAN_POINT('Ctrl Pts',(162.380110802063,222.256241901603,0.155266846025946));
#88770=CARTESIAN_POINT('Ctrl Pts',(158.984594388107,221.509946987359,-0.00349101920584297));
#88771=CARTESIAN_POINT('Ctrl Pts',(156.520034915627,223.964662694603,-0.162248884437635));
#88772=CARTESIAN_POINT('Ctrl Pts',(156.999831188384,226.220556762667,-0.268087461258832));
#88773=CARTESIAN_POINT('Ctrl Pts',(157.663937342304,226.99730155693,-0.32100674966943));
#88774=CARTESIAN_POINT('Ctrl Pts',(159.254067145653,222.209822430158,20.1070022498898));
#88775=CARTESIAN_POINT('Ctrl Pts',(158.326328373192,222.457846368889,20.0540829614792));
#88776=CARTESIAN_POINT('Ctrl Pts',(156.7539919492,223.949441073822,19.948244384658));
#88777=CARTESIAN_POINT('Ctrl Pts',(157.355959176676,227.162240845431,19.7894865194262));
#88778=CARTESIAN_POINT('Ctrl Pts',(160.38271659491,228.391685837985,19.6307286541944));
#88779=CARTESIAN_POINT('Ctrl Pts',(163.056853480481,226.519286632664,19.4719707889626));
#88780=CARTESIAN_POINT('Ctrl Pts',(162.934495694324,223.255375039161,19.3132129237308));
#88781=CARTESIAN_POINT('Ctrl Pts',(160.12593951857,221.588656257922,19.1544550584991));
#88782=CARTESIAN_POINT('Ctrl Pts',(157.20238763747,223.043752390359,18.9956971932673));
#88783=CARTESIAN_POINT('Ctrl Pts',(156.839083181652,226.289325180472,18.8369393280355));
#88784=CARTESIAN_POINT('Ctrl Pts',(159.368711024974,228.354850302395,18.6781814628037));
#88785=CARTESIAN_POINT('Ctrl Pts',(162.476064945398,227.350044181658,18.5194235975719));
#88786=CARTESIAN_POINT('Ctrl Pts',(163.317338575358,224.194464405884,18.3606657323401));
#88787=CARTESIAN_POINT('Ctrl Pts',(161.122577203773,221.776117190028,18.2019078671083));
#88788=CARTESIAN_POINT('Ctrl Pts',(157.900436529364,222.308264302983,18.0431500018765));
#88789=CARTESIAN_POINT('Ctrl Pts',(156.599814665512,225.303889310224,17.8843921366447));
#88790=CARTESIAN_POINT('Ctrl Pts',(158.411043054878,228.021394114489,17.7256342714129));
#88791=CARTESIAN_POINT('Ctrl Pts',(161.676484407413,227.973719490126,17.5668764061811));
#88792=CARTESIAN_POINT('Ctrl Pts',(163.407607474782,225.204496738517,17.4081185409493));
#88793=CARTESIAN_POINT('Ctrl Pts',(162.020088229169,222.248118660259,17.2493606757175));
#88794=CARTESIAN_POINT('Ctrl Pts',(158.783784357136,221.810262237168,17.0906028104858));
#88795=CARTESIAN_POINT('Ctrl Pts',(156.660560973636,224.291653707862,16.9318449452539));
#88796=CARTESIAN_POINT('Ctrl Pts',(157.593592065377,227.421323668266,16.7730870800222));
#88797=CARTESIAN_POINT('Ctrl Pts',(160.728967599613,228.334998307027,16.6143292147904));
#88798=CARTESIAN_POINT('Ctrl Pts',(163.197192017586,226.196482624251,16.4555713495586));
#88799=CARTESIAN_POINT('Ctrl Pts',(162.739346425713,222.96294609182,16.2968134843268));
#88800=CARTESIAN_POINT('Ctrl Pts',(159.774451093269,221.593721215564,16.138055619095));
#88801=CARTESIAN_POINT('Ctrl Pts',(157.015978111145,223.341922549109,15.9792977538632));
#88802=CARTESIAN_POINT('Ctrl Pts',(156.988481844478,226.607596300395,15.8205398886314));
#88803=CARTESIAN_POINT('Ctrl Pts',(159.717126875262,228.401997980831,15.6617820233996));
#88804=CARTESIAN_POINT('Ctrl Pts',(162.70465737871,227.082891242965,15.5030241581678));
#88805=CARTESIAN_POINT('Ctrl Pts',(163.216885555507,223.857522521458,15.344266292936));
#88806=CARTESIAN_POINT('Ctrl Pts',(160.785020198412,221.67774914338,15.1855084277043));
#88807=CARTESIAN_POINT('Ctrl Pts',(157.634704386597,222.538499618639,15.0267505624724));
#88808=CARTESIAN_POINT('Ctrl Pts',(156.649107027157,225.652015146123,14.8679926972407));
#88809=CARTESIAN_POINT('Ctrl Pts',(158.730246784692,228.168806437515,14.7092348320089));
#88810=CARTESIAN_POINT('Ctrl Pts',(161.973464634945,227.785506201904,14.5504769667771));
#88811=CARTESIAN_POINT('Ctrl Pts',(163.410567728901,224.852910799848,14.3917191015453));
#88812=CARTESIAN_POINT('Ctrl Pts',(161.726319371484,222.054931427987,14.2329612363135));
#88813=CARTESIAN_POINT('Ctrl Pts',(158.462143593171,221.95227869742,14.0742033710817));
#88814=CARTESIAN_POINT('Ctrl Pts',(156.605413937913,224.638900383126,13.9154455058499));
#88815=CARTESIAN_POINT('Ctrl Pts',(157.855409313188,227.656000423995,13.7566876406181));
#88816=CARTESIAN_POINT('Ctrl Pts',(161.0681340007,228.242328981268,13.5979297753863));
#88817=CARTESIAN_POINT('Ctrl Pts',(163.303302492774,225.861278182386,13.4391719101545));
#88818=CARTESIAN_POINT('Ctrl Pts',(162.515288673361,222.691985624853,13.2804140449227));
#88819=CARTESIAN_POINT('Ctrl Pts',(159.425282758999,221.634987732694,13.1216561796909));
#88820=CARTESIAN_POINT('Ctrl Pts',(156.861258041001,223.657648935247,12.9628983144592));
#88821=CARTESIAN_POINT('Ctrl Pts',(157.169809840451,226.908829779476,12.8041404492274));
#88822=CARTESIAN_POINT('Ctrl Pts',(160.068551562625,228.413049684591,12.6453825839956));
#88823=CARTESIAN_POINT('Ctrl Pts',(162.904554897381,226.793646652583,12.4866247187638));
#88824=CARTESIAN_POINT('Ctrl Pts',(163.082309704272,223.532698274665,12.327866853532));
#88825=CARTESIAN_POINT('Ctrl Pts',(160.439134791023,221.614624378073,12.1691089883002));
#88826=CARTESIAN_POINT('Ctrl Pts',(157.394063734297,222.794846117542,12.0103511230684));
#88827=CARTESIAN_POINT('Ctrl Pts',(156.733945445467,225.993224603521,11.8515932578366));
#88828=CARTESIAN_POINT('Ctrl Pts',(159.062920156511,228.282603971415,11.6928353926048));
#88829=CARTESIAN_POINT('Ctrl Pts',(162.249510303466,227.567744313755,11.534077527373));
#88830=CARTESIAN_POINT('Ctrl Pts',(163.377348709149,224.502885161121,11.3753196621412));
#88831=CARTESIAN_POINT('Ctrl Pts',(161.41423770903,221.89298548948,11.2165617969094));
#88832=CARTESIAN_POINT('Ctrl Pts',(158.15681641322,222.126625375687,11.0578039316776));
#88833=CARTESIAN_POINT('Ctrl Pts',(156.58627666355,224.989977605072,10.8990460664458));
#88834=CARTESIAN_POINT('Ctrl Pts',(158.139976377158,227.862502329901,10.7402882012141));
#88835=CARTESIAN_POINT('Ctrl Pts',(161.395969637247,228.11526503497,10.5815303359823));
#88836=CARTESIAN_POINT('Ctrl Pts',(163.374371540223,225.516937302539,10.4227724707505));
#88837=CARTESIAN_POINT('Ctrl Pts',(162.264548742281,222.445508571152,10.2640146055187));
#88838=CARTESIAN_POINT('Ctrl Pts',(159.082211024455,221.711950294994,10.1052567402869));
#88839=CARTESIAN_POINT('Ctrl Pts',(156.739833740956,223.987614979558,9.9464988750551));
#88840=CARTESIAN_POINT('Ctrl Pts',(157.381160489532,227.189814395019,9.7877410098233));
#88841=CARTESIAN_POINT('Ctrl Pts',(160.419249055105,228.387895762271,9.62898314459152));
#88842=CARTESIAN_POINT('Ctrl Pts',(163.073640901932,226.485375061119,9.47022527935972));
#88843=CARTESIAN_POINT('Ctrl Pts',(162.915036716179,223.223439162441,9.31146741412793));
#88844=CARTESIAN_POINT('Ctrl Pts',(160.08859104241,221.587411672436,9.15270954889613));
#88845=CARTESIAN_POINT('Ctrl Pts',(157.181066850111,223.074584885621,8.99395168366435));
#88846=CARTESIAN_POINT('Ctrl Pts',(156.853430165738,226.32389793577,8.83519381843254));
#88847=CARTESIAN_POINT('Ctrl Pts',(159.405534069946,228.361579647164,8.67643595320076));
#88848=CARTESIAN_POINT('Ctrl Pts',(162.501693169962,227.322743797664,8.51767808796897));
#88849=CARTESIAN_POINT('Ctrl Pts',(163.308302779206,224.158132915882,8.35892022273717));
#88850=CARTESIAN_POINT('Ctrl Pts',(161.087153815016,221.763998756378,8.20016235750538));
#88851=CARTESIAN_POINT('Ctrl Pts',(157.871041722075,222.331452807785,8.04140449227359));
#88852=CARTESIAN_POINT('Ctrl Pts',(156.603352161372,225.341161144569,7.88264662704179));
#88853=CARTESIAN_POINT('Ctrl Pts',(158.444274569011,228.038638815259,7.72388876181));
#88854=CARTESIAN_POINT('Ctrl Pts',(161.708996829914,227.955154361715,7.56513089657821));
#88855=CARTESIAN_POINT('Ctrl Pts',(163.409645259285,225.167112752539,7.40637303134642));
#88856=CARTESIAN_POINT('Ctrl Pts',(161.989786481439,222.22612955881,7.24761516611462));
#88857=CARTESIAN_POINT('Ctrl Pts',(158.748875194027,221.823792483779,7.08885730088284));
#88858=CARTESIAN_POINT('Ctrl Pts',(156.652993279842,224.328320402691,6.93009943565103));
#88859=CARTESIAN_POINT('Ctrl Pts',(157.620291784328,227.447569462648,6.77134157041925));
#88860=CARTESIAN_POINT('Ctrl Pts',(160.765499154218,228.326803046637,6.61258370518745));
#88861=CARTESIAN_POINT('Ctrl Pts',(163.210121728269,226.161346613168,6.45382583995566));
#88862=CARTESIAN_POINT('Ctrl Pts',(162.716841022844,222.933025804996,6.29506797472387));
#88863=CARTESIAN_POINT('Ctrl Pts',(159.737107520149,221.59639969881,6.13631010949208));
#88864=CARTESIAN_POINT('Ctrl Pts',(156.997973204676,223.37474845443,5.97755224426028));
#88865=CARTESIAN_POINT('Ctrl Pts',(157.006293694231,226.640527360644,5.81879437902849));
#88866=CARTESIAN_POINT('Ctrl Pts',(159.754454077101,228.404895690909,5.66003651379671));
#88867=CARTESIAN_POINT('Ctrl Pts',(162.727338078953,227.053103618748,5.50127864856491));
#88868=CARTESIAN_POINT('Ctrl Pts',(163.204162378196,223.822311195445,5.34252078333312));
#88869=CARTESIAN_POINT('Ctrl Pts',(160.748537394915,221.669339519759,5.18376291810132));
#88870=CARTESIAN_POINT('Ctrl Pts',(157.607851017243,222.564588184615,5.02500505286953));
#88871=CARTESIAN_POINT('Ctrl Pts',(156.656459294521,225.68872564714,4.86624718763774));
#88872=CARTESIAN_POINT('Ctrl Pts',(158.765075893972,228.182541424488,4.70748932240594));
#88873=CARTESIAN_POINT('Ctrl Pts',(162.003894986697,227.763695415291,4.54873145717415));
#88874=CARTESIAN_POINT('Ctrl Pts',(163.4087494664,224.815515470708,4.38997359194236));
#88875=CARTESIAN_POINT('Ctrl Pts',(161.693916568495,222.036175760061,4.23121572671057));
#88876=CARTESIAN_POINT('Ctrl Pts',(158.428811293724,221.969327877293,4.07245786147877));
#88877=CARTESIAN_POINT('Ctrl Pts',(156.601657861134,224.676151001972,3.91369999624698));
#88878=CARTESIAN_POINT('Ctrl Pts',(157.884667020433,227.679360717071,3.75494213101519));
#88879=CARTESIAN_POINT('Ctrl Pts',(161.103628839374,228.230419608936,3.5961842657834));
#88880=CARTESIAN_POINT('Ctrl Pts',(163.312549588073,225.82499860243,3.43742640055161));
#88881=CARTESIAN_POINT('Ctrl Pts',(162.489825083712,222.664538905981,3.27866853531981));
#88882=CARTESIAN_POINT('Ctrl Pts',(159.388412761308,221.641493113929,3.11991067008802));
#88883=CARTESIAN_POINT('Ctrl Pts',(156.846725054335,223.692152685734,2.96115280485623));
#88884=CARTESIAN_POINT('Ctrl Pts',(157.190914456477,226.939754080999,2.80239493962444));
#88885=CARTESIAN_POINT('Ctrl Pts',(160.105978831691,228.412092590901,2.64363707439264));
#88886=CARTESIAN_POINT('Ctrl Pts',(162.924051396542,226.761684151213,2.48487920916085));
#88887=CARTESIAN_POINT('Ctrl Pts',(163.06603221288,223.498982330607,2.32612134392906));
#88888=CARTESIAN_POINT('Ctrl Pts',(160.401980521227,221.61001206063,2.16736347869727));
#88889=CARTESIAN_POINT('Ctrl Pts',(157.370036163074,222.823558124324,2.00860561346547));
#88890=CARTESIAN_POINT('Ctrl Pts',(156.745034831803,226.028984734411,1.84984774823368));
#88891=CARTESIAN_POINT('Ctrl Pts',(159.098977023982,228.292682424339,1.69108988300189));
#88892=CARTESIAN_POINT('Ctrl Pts',(162.277536384602,227.542921712078,1.53233201777009));
#88893=CARTESIAN_POINT('Ctrl Pts',(163.371692510015,224.465869971375,1.37357415253831));
#88894=CARTESIAN_POINT('Ctrl Pts',(161.380079985771,221.87767305454,1.21481628730651));
#88895=CARTESIAN_POINT('Ctrl Pts',(158.1254095921,222.146990123374,1.05605842207472));
#88896=CARTESIAN_POINT('Ctrl Pts',(156.586382360866,225.027463703372,0.89730055684293));
#88897=CARTESIAN_POINT('Ctrl Pts',(158.171460313971,227.882632391681,0.738542691611135));
#88898=CARTESIAN_POINT('Ctrl Pts',(161.430095625151,228.099968989669,0.579784826379343));
#88899=CARTESIAN_POINT('Ctrl Pts',(163.379745915188,225.479481618092,0.421026961147551));
#88900=CARTESIAN_POINT('Ctrl Pts',(162.236589126888,222.421691660586,0.262269095915756));
#88901=CARTESIAN_POINT('Ctrl Pts',(159.045823770485,221.720398641285,0.103511230683967));
#88902=CARTESIAN_POINT('Ctrl Pts',(156.729878263267,224.027093966422,-0.0552466345478245));
#88903=CARTESIAN_POINT('Ctrl Pts',(157.180742620438,226.146956680238,-0.161085211369022));
#88904=CARTESIAN_POINT('Ctrl Pts',(157.804802895981,226.876863439079,-0.21400449977962));
#88905=CARTESIAN_POINT('Ctrl Pts',(159.301933573839,222.388867814061,20.2140044997796));
#88906=CARTESIAN_POINT('Ctrl Pts',(158.433727695081,222.620976084267,20.161085211369));
#88907=CARTESIAN_POINT('Ctrl Pts',(156.962287924299,224.01685532311,20.0552466345478));
#88908=CARTESIAN_POINT('Ctrl Pts',(157.525626981831,227.023490091198,19.896488769316));
#88909=CARTESIAN_POINT('Ctrl Pts',(160.358157713639,228.174041735507,19.7377309040842));
#88910=CARTESIAN_POINT('Ctrl Pts',(162.860695533093,226.421794178655,19.5789730388525));
#88911=CARTESIAN_POINT('Ctrl Pts',(162.746189432446,223.367327428592,19.4202151736207));
#88912=CARTESIAN_POINT('Ctrl Pts',(160.11785799369,221.807561805916,19.2614573083889));
#88913=CARTESIAN_POINT('Ctrl Pts',(157.381910111192,223.169284581594,19.1026994431571));
#88914=CARTESIAN_POINT('Ctrl Pts',(157.041918861842,226.206589327239,18.9439415779253));
#88915=CARTESIAN_POINT('Ctrl Pts',(159.409220768192,228.139569932133,18.7851837126935));
#88916=CARTESIAN_POINT('Ctrl Pts',(162.317176133621,227.199242108255,18.6264258474617));
#88917=CARTESIAN_POINT('Ctrl Pts',(163.104465328442,224.246155535242,18.4676679822299));
#88918=CARTESIAN_POINT('Ctrl Pts',(161.050541549633,221.982993390887,18.3089101169981));
#88919=CARTESIAN_POINT('Ctrl Pts',(158.035165283438,222.480992682871,18.1501522517663));
#88920=CARTESIAN_POINT('Ctrl Pts',(156.818004179734,225.284388767032,17.9913943865345));
#88921=CARTESIAN_POINT('Ctrl Pts',(158.513006245078,227.827511590667,17.8326365213027));
#88922=CARTESIAN_POINT('Ctrl Pts',(161.568904589706,227.782896241639,17.673878656071));
#88923=CARTESIAN_POINT('Ctrl Pts',(163.188941682644,225.191374205583,17.5151207908391));
#88924=CARTESIAN_POINT('Ctrl Pts',(161.890459392489,222.424706579342,17.3563629256074));
#88925=CARTESIAN_POINT('Ctrl Pts',(158.861828779484,222.014947354155,17.1976050603756));
#88926=CARTESIAN_POINT('Ctrl Pts',(156.874852404031,224.337108210537,17.0388471951438));
#88927=CARTESIAN_POINT('Ctrl Pts',(157.748010994531,227.265947598146,16.880089329912));
#88928=CARTESIAN_POINT('Ctrl Pts',(160.682189829934,228.120991837097,16.7213314646802));
#88929=CARTESIAN_POINT('Ctrl Pts',(162.992028561902,226.11970446751,16.5625735994484));
#88930=CARTESIAN_POINT('Ctrl Pts',(162.563562870667,223.093663614233,16.4038157342166));
#88931=CARTESIAN_POINT('Ctrl Pts',(159.788924541493,221.81230174579,16.2450578689848));
#88932=CARTESIAN_POINT('Ctrl Pts',(157.20746246341,223.448321194466,16.086300003753));
#88933=CARTESIAN_POINT('Ctrl Pts',(157.181730629114,226.504437024843,15.9275421385212));
#88934=CARTESIAN_POINT('Ctrl Pts',(159.735278812172,228.183692149295,15.7687842732894));
#88935=CARTESIAN_POINT('Ctrl Pts',(162.531099815947,226.949232343883,15.6100264080576));
#88936=CARTESIAN_POINT('Ctrl Pts',(163.010458367688,223.930835174013,15.4512685428259));
#88937=CARTESIAN_POINT('Ctrl Pts',(160.73464553971,221.890937610836,15.292510677594));
#88938=CARTESIAN_POINT('Ctrl Pts',(157.786485142676,222.696453823964,15.1337528123623));
#88939=CARTESIAN_POINT('Ctrl Pts',(156.864133456022,225.610175406814,14.9749949471305));
#88940=CARTESIAN_POINT('Ctrl Pts',(158.811726707101,227.965464481343,14.8162370818987));
#88941=CARTESIAN_POINT('Ctrl Pts',(161.846827629113,227.606760579161,14.6574792166669));
#88942=CARTESIAN_POINT('Ctrl Pts',(163.191711977586,224.862349497439,14.4987213514351));
#88943=CARTESIAN_POINT('Ctrl Pts',(161.615541649683,222.243916150249,14.3399634862033));
#88944=CARTESIAN_POINT('Ctrl Pts',(158.56082766752,222.14785063397,14.1812056209715));
#88945=CARTESIAN_POINT('Ctrl Pts',(156.823244147448,224.662072105324,14.0224477557397));
#88946=CARTESIAN_POINT('Ctrl Pts',(157.993027458709,227.485565172597,13.8636898905079));
#88947=CARTESIAN_POINT('Ctrl Pts',(160.999591960837,228.034269091652,13.7049320252761));
#88948=CARTESIAN_POINT('Ctrl Pts',(163.091329939715,225.806010057346,13.5461741600443));
#88949=CARTESIAN_POINT('Ctrl Pts',(162.353882879329,222.840090650254,13.3874162948126));
#88950=CARTESIAN_POINT('Ctrl Pts',(159.462162300346,221.850920195112,13.2286584295807));
#88951=CARTESIAN_POINT('Ctrl Pts',(157.062670762936,223.74378745357,13.069900564349));
#88952=CARTESIAN_POINT('Ctrl Pts',(157.351422827779,226.786340385121,12.9111426991172));
#88953=CARTESIAN_POINT('Ctrl Pts',(160.064152616487,228.194034666456,12.7523848338854));
#88954=CARTESIAN_POINT('Ctrl Pts',(162.718169933108,226.678548546653,12.5936269686536));
#88955=CARTESIAN_POINT('Ctrl Pts',(162.884518233838,223.62685486296,12.4348691034218));
#88956=CARTESIAN_POINT('Ctrl Pts',(160.410955560391,221.83186355469,12.27611123819));
#88957=CARTESIAN_POINT('Ctrl Pts',(157.561286374234,222.936350596582,12.1173533729582));
#88958=CARTESIAN_POINT('Ctrl Pts',(156.943527802478,225.929489491333,11.9585955077264));
#88959=CARTESIAN_POINT('Ctrl Pts',(159.123052465701,228.071959640166,11.7998376424946));
#88960=CARTESIAN_POINT('Ctrl Pts',(162.10515947783,227.402972447122,11.6410797772628));
#88961=CARTESIAN_POINT('Ctrl Pts',(163.160624618632,224.534784964966,11.482321912031));
#88962=CARTESIAN_POINT('Ctrl Pts',(161.32348623275,222.092362264579,11.3235640467992));
#88963=CARTESIAN_POINT('Ctrl Pts',(158.275093298701,222.31100950531,11.1648061815674));
#88964=CARTESIAN_POINT('Ctrl Pts',(156.80533490985,224.990620741038,11.0060483163357));
#88965=CARTESIAN_POINT('Ctrl Pts',(158.259333885877,227.6788158742,10.8472904511039));
#88966=CARTESIAN_POINT('Ctrl Pts',(161.306390421099,227.915358824636,10.6885325858721));
#88967=CARTESIAN_POINT('Ctrl Pts',(163.157838494304,225.483765493408,10.5297747206403));
#88968=CARTESIAN_POINT('Ctrl Pts',(162.119232901701,222.609430001637,10.3710168554085));
#88969=CARTESIAN_POINT('Ctrl Pts',(159.141105440797,221.922944078361,10.2122589901767));
#88970=CARTESIAN_POINT('Ctrl Pts',(156.949038246701,224.052579613566,10.0535011249449));
#88971=CARTESIAN_POINT('Ctrl Pts',(157.549211129248,227.049294249179,9.89474325971311));
#88972=CARTESIAN_POINT('Ctrl Pts',(160.392345889932,228.17049486853,9.73598539448132));
#88973=CARTESIAN_POINT('Ctrl Pts',(162.876405707579,226.390058708879,9.57722752924953));
#88974=CARTESIAN_POINT('Ctrl Pts',(162.727979134762,223.337440873524,9.41846966401773));
#88975=CARTESIAN_POINT('Ctrl Pts',(160.082906165086,221.806397085342,9.25971179878595));
#88976=CARTESIAN_POINT('Ctrl Pts',(157.361957476384,223.198138559069,9.10095393355415));
#88977=CARTESIAN_POINT('Ctrl Pts',(157.055345201557,226.23894355268,8.94219606832236));
#88978=CARTESIAN_POINT('Ctrl Pts',(159.443680882469,228.145867455598,8.78343820309056));
#88979=CARTESIAN_POINT('Ctrl Pts',(162.341159797869,227.173693586861,8.62468033785878));
#88980=CARTESIAN_POINT('Ctrl Pts',(163.096009358323,224.212155432907,8.46592247262698));
#88981=CARTESIAN_POINT('Ctrl Pts',(161.017391275787,221.971652595775,8.30716460739519));
#88982=CARTESIAN_POINT('Ctrl Pts',(158.007656737659,222.502693183903,8.1484067421634));
#88983=CARTESIAN_POINT('Ctrl Pts',(156.821314674878,225.319268871918,7.98964887693161));
#88984=CARTESIAN_POINT('Ctrl Pts',(158.54410529665,227.843649700909,7.83089101169981));
#88985=CARTESIAN_POINT('Ctrl Pts',(161.599330693676,227.765522435452,7.67213314646802));
#88986=CARTESIAN_POINT('Ctrl Pts',(163.190848702742,225.156389145821,7.51337528123624));
#88987=CARTESIAN_POINT('Ctrl Pts',(161.862102104535,222.404128516084,7.35461741600443));
#88988=CARTESIAN_POINT('Ctrl Pts',(158.829159733483,222.027609366348,7.19585955077264));
#88989=CARTESIAN_POINT('Ctrl Pts',(156.867770328305,224.371422007643,7.03710168554085));
#88990=CARTESIAN_POINT('Ctrl Pts',(157.77299739549,227.290509202825,6.87834382030906));
#88991=CARTESIAN_POINT('Ctrl Pts',(160.716377158748,228.113322465654,6.71958595507727));
#88992=CARTESIAN_POINT('Ctrl Pts',(163.00412857449,226.086823130344,6.56082808984547));
#88993=CARTESIAN_POINT('Ctrl Pts',(162.542501636994,223.065663308882,6.40207022461368));
#88994=CARTESIAN_POINT('Ctrl Pts',(159.753977301302,221.814808351065,6.24331235938189));
#88995=CARTESIAN_POINT('Ctrl Pts',(157.190612929784,223.479040665098,6.08455449415009));
#88996=CARTESIAN_POINT('Ctrl Pts',(157.198399494451,226.535254902624,5.92579662891831));
#88997=CARTESIAN_POINT('Ctrl Pts',(159.770210731627,228.18640391364,5.76703876368651));
#88998=CARTESIAN_POINT('Ctrl Pts',(162.552325098181,226.921356188195,5.60828089845472));
#88999=CARTESIAN_POINT('Ctrl Pts',(162.998551635248,223.89788335487,5.44952303322292));
#89000=CARTESIAN_POINT('Ctrl Pts',(160.700503833651,221.883067631827,5.29076516799114));
#89001=CARTESIAN_POINT('Ctrl Pts',(157.761354951043,222.720868289566,5.13200730275934));
#89002=CARTESIAN_POINT('Ctrl Pts',(156.871013929208,225.644530199069,4.97324943752755));
#89003=CARTESIAN_POINT('Ctrl Pts',(158.844320836317,227.978318095731,4.81449157229576));
#89004=CARTESIAN_POINT('Ctrl Pts',(161.875305268582,227.586349388296,4.65573370706397));
#89005=CARTESIAN_POINT('Ctrl Pts',(163.190010392787,224.827353822406,4.49697584183217));
#89006=CARTESIAN_POINT('Ctrl Pts',(161.585218130953,222.226364031445,4.33821797660038));
#89007=CARTESIAN_POINT('Ctrl Pts',(158.529634298016,222.163805769869,4.17946011136858));
#89008=CARTESIAN_POINT('Ctrl Pts',(156.819729097698,224.696932356107,4.0207022461368));
#89009=CARTESIAN_POINT('Ctrl Pts',(158.020407702139,227.507426438268,3.861944380905));
#89010=CARTESIAN_POINT('Ctrl Pts',(161.032809099667,228.023123942415,3.70318651567321));
#89011=CARTESIAN_POINT('Ctrl Pts',(163.099983649938,225.772058533996,3.54442865044141));
#89012=CARTESIAN_POINT('Ctrl Pts',(162.330053285392,222.814405184275,3.38567078520963));
#89013=CARTESIAN_POINT('Ctrl Pts',(159.4276582463,221.857008126758,3.22691291997783));
#89014=CARTESIAN_POINT('Ctrl Pts',(157.049070356406,223.77607710223,3.06815505474604));
#89015=CARTESIAN_POINT('Ctrl Pts',(157.371173162946,226.81528027766,2.90939718951425));
#89016=CARTESIAN_POINT('Ctrl Pts',(160.099178181865,228.193138989361,2.75063932428246));
#89017=CARTESIAN_POINT('Ctrl Pts',(162.736415344089,226.648637075436,2.59188145905066));
#89018=CARTESIAN_POINT('Ctrl Pts',(162.869285267256,223.595302467277,2.43312359381887));
#89019=CARTESIAN_POINT('Ctrl Pts',(160.37618547595,221.827547209143,2.27436572858708));
#89020=CARTESIAN_POINT('Ctrl Pts',(157.538800649579,222.963220157087,2.11560786335528));
#89021=CARTESIAN_POINT('Ctrl Pts',(156.953905584128,225.962954898605,1.95684999812349));
#89022=CARTESIAN_POINT('Ctrl Pts',(159.156795568002,228.081391359888,1.7980921328917));
#89023=CARTESIAN_POINT('Ctrl Pts',(162.131387128461,227.37974270903,1.63933426765991));
#89024=CARTESIAN_POINT('Ctrl Pts',(163.155331377166,224.500145035824,1.48057640242812));
#89025=CARTESIAN_POINT('Ctrl Pts',(161.291520406789,222.078032426884,1.32181853719632));
#89026=CARTESIAN_POINT('Ctrl Pts',(158.245701849794,222.330067449406,1.16306067196453));
#89027=CARTESIAN_POINT('Ctrl Pts',(156.805433824581,225.025701360586,1.00430280673274));
#89028=CARTESIAN_POINT('Ctrl Pts',(158.288797501971,227.697654192157,0.845544941500946));
#89029=CARTESIAN_POINT('Ctrl Pts',(161.33832654816,227.901044324858,0.686787076269153));
#89030=CARTESIAN_POINT('Ctrl Pts',(163.162867996227,225.448713336061,0.528029211037362));
#89031=CARTESIAN_POINT('Ctrl Pts',(162.093067451714,222.58714141957,0.369271345805566));
#89032=CARTESIAN_POINT('Ctrl Pts',(159.107053152862,221.930850295212,0.210513480573777));
#89033=CARTESIAN_POINT('Ctrl Pts',(156.939721610906,224.08952523824,0.0517556153419854));
#89034=CARTESIAN_POINT('Ctrl Pts',(157.361654052493,226.073356597808,-0.0540829614792118));
#89035=CARTESIAN_POINT('Ctrl Pts',(157.945668449658,226.756425321227,-0.10700224988981));
#89036=CARTESIAN_POINT('Ctrl Pts',(159.349800002025,222.567913197965,20.3210067496694));
#89037=CARTESIAN_POINT('Ctrl Pts',(158.541127016969,222.784105799646,20.2680874612588));
#89038=CARTESIAN_POINT('Ctrl Pts',(157.170583899398,224.084269572398,20.1622488844377));
#89039=CARTESIAN_POINT('Ctrl Pts',(157.695294786986,226.884739336963,20.0034910192058));
#89040=CARTESIAN_POINT('Ctrl Pts',(160.333598832368,227.956397633029,19.8447331539741));
#89041=CARTESIAN_POINT('Ctrl Pts',(162.664537585704,226.324301724646,19.6859752887423));
#89042=CARTESIAN_POINT('Ctrl Pts',(162.557883170567,223.479279818023,19.5272174235105));
#89043=CARTESIAN_POINT('Ctrl Pts',(160.10977646881,222.02646735391,19.3684595582787));
#89044=CARTESIAN_POINT('Ctrl Pts',(157.561432584915,223.29481677283,19.2097016930469));
#89045=CARTESIAN_POINT('Ctrl Pts',(157.244754542031,226.123853474005,19.0509438278151));
#89046=CARTESIAN_POINT('Ctrl Pts',(159.449730511411,227.924289561872,18.8921859625833));
#89047=CARTESIAN_POINT('Ctrl Pts',(162.158287321844,227.048440034851,18.7334280973515));
#89048=CARTESIAN_POINT('Ctrl Pts',(162.891592081527,224.297846664601,18.5746702321197));
#89049=CARTESIAN_POINT('Ctrl Pts',(160.978505895493,222.189869591746,18.4159123668879));
#89050=CARTESIAN_POINT('Ctrl Pts',(158.169894037512,222.653721062759,18.2571545016561));
#89051=CARTESIAN_POINT('Ctrl Pts',(157.036193693956,225.26488822384,18.0983966364243));
#89052=CARTESIAN_POINT('Ctrl Pts',(158.614969435278,227.633629066845,17.9396387711925));
#89053=CARTESIAN_POINT('Ctrl Pts',(161.461324771999,227.592072993153,17.7808809059608));
#89054=CARTESIAN_POINT('Ctrl Pts',(162.970275890506,225.178251672648,17.622123040729));
#89055=CARTESIAN_POINT('Ctrl Pts',(161.760830555808,222.601294498425,17.4633651754972));
#89056=CARTESIAN_POINT('Ctrl Pts',(158.939873201832,222.219632471142,17.3046073102654));
#89057=CARTESIAN_POINT('Ctrl Pts',(157.089143834426,224.382562713212,17.1458494450336));
#89058=CARTESIAN_POINT('Ctrl Pts',(157.902429923685,227.110571528026,16.9870915798018));
#89059=CARTESIAN_POINT('Ctrl Pts',(160.635412060255,227.906985367167,16.82833371457));
#89060=CARTESIAN_POINT('Ctrl Pts',(162.786865106217,226.042926310769,16.6695758493382));
#89061=CARTESIAN_POINT('Ctrl Pts',(162.387779315621,223.224381136646,16.5108179841064));
#89062=CARTESIAN_POINT('Ctrl Pts',(159.803397989718,222.030882276016,16.3520601188746));
#89063=CARTESIAN_POINT('Ctrl Pts',(157.398946815676,223.554719839823,16.1933022536428));
#89064=CARTESIAN_POINT('Ctrl Pts',(157.374979413748,226.401277749291,16.034544388411));
#89065=CARTESIAN_POINT('Ctrl Pts',(159.753430749081,227.965386317759,15.8757865231793));
#89066=CARTESIAN_POINT('Ctrl Pts',(162.357542253183,226.815573444802,15.7170286579474));
#89067=CARTESIAN_POINT('Ctrl Pts',(162.804031179868,224.004147826569,15.5582707927157));
#89068=CARTESIAN_POINT('Ctrl Pts',(160.684270881009,222.104126078293,15.3995129274839));
#89069=CARTESIAN_POINT('Ctrl Pts',(157.938265898756,222.854408029289,15.2407550622521));
#89070=CARTESIAN_POINT('Ctrl Pts',(157.079159884887,225.568335667504,15.0819971970203));
#89071=CARTESIAN_POINT('Ctrl Pts',(158.89320662951,227.76212252517,14.9232393317885));
#89072=CARTESIAN_POINT('Ctrl Pts',(161.720190623281,227.428014956417,14.7644814665567));
#89073=CARTESIAN_POINT('Ctrl Pts',(162.972856226271,224.871788195031,14.6057236013249));
#89074=CARTESIAN_POINT('Ctrl Pts',(161.504763927882,222.432900872511,14.4469657360931));
#89075=CARTESIAN_POINT('Ctrl Pts',(158.659511741869,222.34342257052,14.2882078708613));
#89076=CARTESIAN_POINT('Ctrl Pts',(157.041074356984,224.685243827522,14.1294500056295));
#89077=CARTESIAN_POINT('Ctrl Pts',(158.13064560423,227.315129921198,13.9706921403977));
#89078=CARTESIAN_POINT('Ctrl Pts',(160.931049920975,227.826209202034,13.8119342751659));
#89079=CARTESIAN_POINT('Ctrl Pts',(162.879357386656,225.750741932307,13.6531764099341));
#89080=CARTESIAN_POINT('Ctrl Pts',(162.192477085297,222.988195675654,13.4944185447024));
#89081=CARTESIAN_POINT('Ctrl Pts',(159.499041841692,222.06685265753,13.3356606794706));
#89082=CARTESIAN_POINT('Ctrl Pts',(157.26408348487,223.829925971892,13.1769028142388));
#89083=CARTESIAN_POINT('Ctrl Pts',(157.533035815108,226.663850990766,13.018144949007));
#89084=CARTESIAN_POINT('Ctrl Pts',(160.059753670348,227.97501964832,12.8593870837752));
#89085=CARTESIAN_POINT('Ctrl Pts',(162.531784968835,226.563450440722,12.7006292185434));
#89086=CARTESIAN_POINT('Ctrl Pts',(162.686726763404,223.721011451256,12.5418713533116));
#89087=CARTESIAN_POINT('Ctrl Pts',(160.382776329759,222.049102731306,12.3831134880798));
#89088=CARTESIAN_POINT('Ctrl Pts',(157.728509014171,223.077855075623,12.224355622848));
#89089=CARTESIAN_POINT('Ctrl Pts',(157.153110159489,225.865754379144,12.0655977576162));
#89090=CARTESIAN_POINT('Ctrl Pts',(159.183184774892,227.861315308917,11.9068398923844));
#89091=CARTESIAN_POINT('Ctrl Pts',(161.960808652193,227.238200580488,11.7480820271526));
#89092=CARTESIAN_POINT('Ctrl Pts',(162.943900528114,224.566684768811,11.5893241619208));
#89093=CARTESIAN_POINT('Ctrl Pts',(161.232734756471,222.291739039679,11.4305662966891));
#89094=CARTESIAN_POINT('Ctrl Pts',(158.393370184182,222.495393634933,11.2718084314573));
#89095=CARTESIAN_POINT('Ctrl Pts',(157.02439315615,224.991263877004,11.1130505662255));
#89096=CARTESIAN_POINT('Ctrl Pts',(158.378691394597,227.495129418499,10.9542927009937));
#89097=CARTESIAN_POINT('Ctrl Pts',(161.216811204952,227.715452614301,10.7955348357619));
#89098=CARTESIAN_POINT('Ctrl Pts',(162.941305448385,225.450593684278,10.6367769705301));
#89099=CARTESIAN_POINT('Ctrl Pts',(161.97391706112,222.773351432123,10.4780191052983));
#89100=CARTESIAN_POINT('Ctrl Pts',(159.19999985714,222.133937861728,10.3192612400665));
#89101=CARTESIAN_POINT('Ctrl Pts',(157.158242752446,224.117544247575,10.1605033748347));
#89102=CARTESIAN_POINT('Ctrl Pts',(157.717261768964,226.908774103339,10.0017455096029));
#89103=CARTESIAN_POINT('Ctrl Pts',(160.365442724759,227.953093974789,9.84298764437114));
#89104=CARTESIAN_POINT('Ctrl Pts',(162.679170513225,226.294742356639,9.68422977913933));
#89105=CARTESIAN_POINT('Ctrl Pts',(162.540921553344,223.451442584608,9.52547191390755));
#89106=CARTESIAN_POINT('Ctrl Pts',(160.077221287761,222.025382498248,9.36671404867575));
#89107=CARTESIAN_POINT('Ctrl Pts',(157.542848102656,223.321692232518,9.20795618344397));
#89108=CARTESIAN_POINT('Ctrl Pts',(157.257260237375,226.153989169589,9.04919831821217));
#89109=CARTESIAN_POINT('Ctrl Pts',(159.481827694993,227.930155264032,8.89044045298037));
#89110=CARTESIAN_POINT('Ctrl Pts',(162.180626425776,227.024643376059,8.73168258774859));
#89111=CARTESIAN_POINT('Ctrl Pts',(162.88371593744,224.266177949933,8.57292472251679));
#89112=CARTESIAN_POINT('Ctrl Pts',(160.947628736558,222.179306435172,8.41416685728499));
#89113=CARTESIAN_POINT('Ctrl Pts',(158.144271753243,222.67393356002,8.25540899205321));
#89114=CARTESIAN_POINT('Ctrl Pts',(157.039277188385,225.297376599268,8.09665112682141));
#89115=CARTESIAN_POINT('Ctrl Pts',(158.643936024289,227.648660586559,7.93789326158962));
#89116=CARTESIAN_POINT('Ctrl Pts',(161.489664557439,227.575890509188,7.77913539635783));
#89117=CARTESIAN_POINT('Ctrl Pts',(162.9720521462,225.145665539102,7.62037753112604));
#89118=CARTESIAN_POINT('Ctrl Pts',(161.734417727632,222.582127473359,7.46161966589424));
#89119=CARTESIAN_POINT('Ctrl Pts',(158.90944427294,222.231426248916,7.30286180066245));
#89120=CARTESIAN_POINT('Ctrl Pts',(157.082547376768,224.414523612595,7.14410393543066));
#89121=CARTESIAN_POINT('Ctrl Pts',(157.925703006652,227.133448943003,6.98534607019887));
#89122=CARTESIAN_POINT('Ctrl Pts',(160.667255163279,227.899841884671,6.82658820496708));
#89123=CARTESIAN_POINT('Ctrl Pts',(162.798135420711,226.012299647521,6.66783033973528));
#89124=CARTESIAN_POINT('Ctrl Pts',(162.368162251143,223.198300812768,6.50907247450349));
#89125=CARTESIAN_POINT('Ctrl Pts',(159.770847082455,222.03321700332,6.3503146092717));
#89126=CARTESIAN_POINT('Ctrl Pts',(157.383252654892,223.583332875767,6.1915567440399));
#89127=CARTESIAN_POINT('Ctrl Pts',(157.390505294671,226.429982444603,6.03279887880811));
#89128=CARTESIAN_POINT('Ctrl Pts',(159.785967386151,227.967912136371,5.87404101357632));
#89129=CARTESIAN_POINT('Ctrl Pts',(162.377312117409,226.789608757643,5.71528314834453));
#89130=CARTESIAN_POINT('Ctrl Pts',(162.792940892299,223.973455514294,5.55652528311274));
#89131=CARTESIAN_POINT('Ctrl Pts',(160.652470272387,222.096795743895,5.39776741788094));
#89132=CARTESIAN_POINT('Ctrl Pts',(157.914858884844,222.877148394518,5.23900955264915));
#89133=CARTESIAN_POINT('Ctrl Pts',(157.085568563895,225.600334750998,5.08025168741735));
#89134=CARTESIAN_POINT('Ctrl Pts',(158.923565778663,227.774094766974,4.92149382218557));
#89135=CARTESIAN_POINT('Ctrl Pts',(161.746715550468,227.4090033613,4.76273595695377));
#89136=CARTESIAN_POINT('Ctrl Pts',(162.971271319174,224.839192174104,4.60397809172198));
#89137=CARTESIAN_POINT('Ctrl Pts',(161.476519693411,222.416552302829,4.44522022649019));
#89138=CARTESIAN_POINT('Ctrl Pts',(158.630457302308,222.358283662445,4.28646236125839));
#89139=CARTESIAN_POINT('Ctrl Pts',(157.037800334262,224.717713710242,4.1277044960266));
#89140=CARTESIAN_POINT('Ctrl Pts',(158.156148383844,227.335492159465,3.96894663079481));
#89141=CARTESIAN_POINT('Ctrl Pts',(160.96198935996,227.815828275895,3.81018876556302));
#89142=CARTESIAN_POINT('Ctrl Pts',(162.887417711804,225.719118465561,3.65143090033123));
#89143=CARTESIAN_POINT('Ctrl Pts',(162.170281487072,222.964271462568,3.49267303509943));
#89144=CARTESIAN_POINT('Ctrl Pts',(159.466903731292,222.072523139587,3.33391516986765));
#89145=CARTESIAN_POINT('Ctrl Pts',(157.251415658476,223.860001518727,3.17515730463585));
#89146=CARTESIAN_POINT('Ctrl Pts',(157.551431869414,226.69080647432,3.01639943940406));
#89147=CARTESIAN_POINT('Ctrl Pts',(160.092377532038,227.974185387821,2.85764157417226));
#89148=CARTESIAN_POINT('Ctrl Pts',(162.548779291636,226.535589999658,2.69888370894047));
#89149=CARTESIAN_POINT('Ctrl Pts',(162.672538321632,223.691622603948,2.54012584370868));
#89150=CARTESIAN_POINT('Ctrl Pts',(160.350390430673,222.045082357655,2.38136797847689));
#89151=CARTESIAN_POINT('Ctrl Pts',(157.707565136085,223.102882189851,2.22261011324509));
#89152=CARTESIAN_POINT('Ctrl Pts',(157.162776336452,225.8969250628,2.0638522480133));
#89153=CARTESIAN_POINT('Ctrl Pts',(159.214614112023,227.870100295438,1.90509438278151));
#89154=CARTESIAN_POINT('Ctrl Pts',(161.985237872319,227.216563705981,1.74633651754972));
#89155=CARTESIAN_POINT('Ctrl Pts',(162.938970244317,224.534420100273,1.58757865231793));
#89156=CARTESIAN_POINT('Ctrl Pts',(161.202960827807,222.278391799228,1.42882078708613));
#89157=CARTESIAN_POINT('Ctrl Pts',(158.365994107488,222.513144775438,1.27006292185434));
#89158=CARTESIAN_POINT('Ctrl Pts',(157.024485288296,225.023939017799,1.11130505662255));
#89159=CARTESIAN_POINT('Ctrl Pts',(158.406134689972,227.512675992633,0.952547191390755));
#89160=CARTESIAN_POINT('Ctrl Pts',(161.24655747117,227.702119660047,0.793789326158964));
#89161=CARTESIAN_POINT('Ctrl Pts',(162.945990077265,225.41794505403,0.635031460927171));
#89162=CARTESIAN_POINT('Ctrl Pts',(161.949545776539,222.752591178553,0.476273595695376));
#89163=CARTESIAN_POINT('Ctrl Pts',(159.16828253524,222.141301949138,0.317515730463587));
#89164=CARTESIAN_POINT('Ctrl Pts',(157.149564958546,224.151956510058,0.158757865231795));
#89165=CARTESIAN_POINT('Ctrl Pts',(157.542565484547,225.999756515378,0.0529192884105984));
#89166=CARTESIAN_POINT('Ctrl Pts',(158.086534003335,226.635987203375,0.));
#89167=CARTESIAN_POINT('Ctrl Pts',(158.086534003335,226.635987203375,0.));
#89168=CARTESIAN_POINT('Ctrl Pts',(158.02493814877,226.578102225091,3.88510873360859E-16));
#89169=CARTESIAN_POINT('Ctrl Pts',(157.966714247614,226.517065561656,3.25162993585481E-15));
#89170=CARTESIAN_POINT('Ctrl Pts',(157.911858668619,226.45326227157,2.88657986402541E-15));
#89171=CARTESIAN_POINT('Ctrl Pts',(157.855549069167,226.38776778998,2.51185365200075E-15));
#89172=CARTESIAN_POINT('Ctrl Pts',(157.802788287295,226.31935764003,1.57974842293527E-15));
#89173=CARTESIAN_POINT('Ctrl Pts',(157.753597957701,226.248399766245,4.16333634234434E-15));
#89174=CARTESIAN_POINT('Ctrl Pts',(157.70270970509,226.174992610086,6.83610303803933E-15));
#89175=CARTESIAN_POINT('Ctrl Pts',(157.655642062481,226.098858291382,5.567414283278E-15));
#89176=CARTESIAN_POINT('Ctrl Pts',(157.612453916939,226.020360183052,6.60582699651968E-15));
#89177=CARTESIAN_POINT('Ctrl Pts',(157.593559103265,225.986017260658,7.06013255856292E-15));
#89178=CARTESIAN_POINT('Ctrl Pts',(157.575407343554,225.951221387756,1.38955512833555E-15));
#89179=CARTESIAN_POINT('Ctrl Pts',(157.558006013615,225.91600090403,1.0547118733939E-15));
#89180=CARTESIAN_POINT('Ctrl Pts',(157.548478053374,225.896716207413,8.71371103972259E-16));
#89181=CARTESIAN_POINT('Ctrl Pts',(157.539175101023,225.877304191743,3.02150505445988E-15));
#89182=CARTESIAN_POINT('Ctrl Pts',(157.53009857257,225.857769379394,3.21964677141295E-15));
#89183=CARTESIAN_POINT('Ctrl Pts',(157.521442422622,225.839139319921,3.40861157460151E-15));
#89184=CARTESIAN_POINT('Ctrl Pts',(157.51298971229,225.820391557714,6.07713703975296E-15));
#89185=CARTESIAN_POINT('Ctrl Pts',(157.504755793001,225.801562868206,5.71764857681956E-15));
#89186=CARTESIAN_POINT('Ctrl Pts',(157.468216330129,225.718007251847,4.1223553897749E-15));
#89187=CARTESIAN_POINT('Ctrl Pts',(157.435936281972,225.632767982619,4.36828787014081E-15));
#89188=CARTESIAN_POINT('Ctrl Pts',(157.407939344588,225.546244309043,4.8017145815038E-15));
#89189=CARTESIAN_POINT('Ctrl Pts',(157.379477860582,225.458284968426,5.24233304072434E-15));
#89190=CARTESIAN_POINT('Ctrl Pts',(157.355442312615,225.368997490439,6.89313887191085E-16));
#89191=CARTESIAN_POINT('Ctrl Pts',(157.335896709461,225.278764189872,1.33226762955019E-15));
#89192=CARTESIAN_POINT('Ctrl Pts',(157.316694687441,225.190117049601,1.96391925071255E-15));
#89193=CARTESIAN_POINT('Ctrl Pts',(157.30182589002,225.100556136381,8.25976945391393E-15));
#89194=CARTESIAN_POINT('Ctrl Pts',(157.291393655264,225.010421131899,9.07607322631065E-15));
#89195=CARTESIAN_POINT('Ctrl Pts',(157.287259729619,224.974703817709,9.39954553855482E-15));
#89196=CARTESIAN_POINT('Ctrl Pts',(157.283822955362,224.938896175082,7.48833909922335E-15));
#89197=CARTESIAN_POINT('Ctrl Pts',(157.28109180216,224.903018802931,7.88258347483861E-15));
#89198=CARTESIAN_POINT('Ctrl Pts',(157.279473595435,224.881761480246,8.1161730441672E-15));
#89199=CARTESIAN_POINT('Ctrl Pts',(157.27810312366,224.860479674496,9.69815673100317E-15));
#89200=CARTESIAN_POINT('Ctrl Pts',(157.276982352986,224.839177647246,1.01030295240889E-14));
#89201=CARTESIAN_POINT('Ctrl Pts',(157.276240353188,224.825074762242,1.03710732353788E-14));
#89202=CARTESIAN_POINT('Ctrl Pts',(157.275607880765,224.810963101263,1.12280289430315E-14));
#89203=CARTESIAN_POINT('Ctrl Pts',(157.275085847944,224.796858298822,1.10467190950203E-14));
#89204=CARTESIAN_POINT('Ctrl Pts',(157.271562839589,224.701670151936,9.82312532148025E-15));
#89205=CARTESIAN_POINT('Ctrl Pts',(157.273056577644,224.606632807943,6.53173546723879E-15));
#89206=CARTESIAN_POINT('Ctrl Pts',(157.279625133053,224.512145564813,7.105427357601E-15));
#89207=CARTESIAN_POINT('Ctrl Pts',(157.286171954436,224.417970960931,7.6772210170925E-15));
#89208=CARTESIAN_POINT('Ctrl Pts',(157.29775970648,224.324341869061,8.22264820408673E-15));
#89209=CARTESIAN_POINT('Ctrl Pts',(157.314493894775,224.231635735225,9.79771819231701E-15));
#89210=CARTESIAN_POINT('Ctrl Pts',(157.316398182771,224.221086124168,9.97695526191135E-15));
#89211=CARTESIAN_POINT('Ctrl Pts',(157.318369169726,224.210548454971,6.40383101223916E-15));
#89212=CARTESIAN_POINT('Ctrl Pts',(157.320407053956,224.200023277725,6.38378239159465E-15));
#89213=CARTESIAN_POINT('Ctrl Pts',(157.337940261685,224.109468516937,6.21335718039711E-15));
#89214=CARTESIAN_POINT('Ctrl Pts',(157.360420988526,224.019838133689,1.13008504771569E-14));
#89215=CARTESIAN_POINT('Ctrl Pts',(157.387574332193,223.931369727859,1.29896093881143E-14));
#89216=CARTESIAN_POINT('Ctrl Pts',(157.398274583748,223.896507200109,1.36550944711156E-14));
#89217=CARTESIAN_POINT('Ctrl Pts',(157.40970101855,223.861825165636,7.03342696341441E-15));
#89218=CARTESIAN_POINT('Ctrl Pts',(157.421838980151,223.827338502461,7.41073868937292E-15));
#89219=CARTESIAN_POINT('Ctrl Pts',(157.427149340729,223.812250580568,7.57581264337371E-15));
#89220=CARTESIAN_POINT('Ctrl Pts',(157.432595907216,223.79720005763,6.38525469805514E-15));
#89221=CARTESIAN_POINT('Ctrl Pts',(157.438177521516,223.782188198706,6.32827124036339E-15));
#89222=CARTESIAN_POINT('Ctrl Pts',(157.442598261446,223.770298533707,6.28313930661066E-15));
#89223=CARTESIAN_POINT('Ctrl Pts',(157.447103314523,223.75843433437,5.8191034780375E-15));
#89224=CARTESIAN_POINT('Ctrl Pts',(157.451688373109,223.746605388579,6.07847105982273E-15));
#89225=CARTESIAN_POINT('Ctrl Pts',(157.485446723974,223.659512564152,7.98811336120978E-15));
#89226=CARTESIAN_POINT('Ctrl Pts',(157.523588046527,223.574194570567,1.3532532634904E-14));
#89227=CARTESIAN_POINT('Ctrl Pts',(157.565779073504,223.490882142242,1.33643096589253E-14));
#89228=CARTESIAN_POINT('Ctrl Pts',(157.609552429182,223.404445171664,1.31897776627071E-14));
#89229=CARTESIAN_POINT('Ctrl Pts',(157.657685066682,223.320166301312,1.07282401440124E-14));
#89230=CARTESIAN_POINT('Ctrl Pts',(157.709860882353,223.238306243802,1.13520304267922E-14));
#89231=CARTESIAN_POINT('Ctrl Pts',(157.762638398375,223.15550216223,1.19830143648678E-14));
#89232=CARTESIAN_POINT('Ctrl Pts',(157.819553294228,223.075172188621,1.73211728058691E-14));
#89233=CARTESIAN_POINT('Ctrl Pts',(157.88033030919,222.99760095645,1.5931700403371E-14));
#89234=CARTESIAN_POINT('Ctrl Pts',(157.92312949277,222.942975282447,1.495323371707E-14));
#89235=CARTESIAN_POINT('Ctrl Pts',(157.967844993907,222.889717949271,1.86083952223982E-14));
#89236=CARTESIAN_POINT('Ctrl Pts',(158.014394107949,222.83793607413,1.92346139016308E-14));
#89237=CARTESIAN_POINT('Ctrl Pts',(158.025600423893,222.825470014036,1.9385370892694E-14));
#89238=CARTESIAN_POINT('Ctrl Pts',(158.036913653601,222.81308897035,1.06179758662295E-14));
#89239=CARTESIAN_POINT('Ctrl Pts',(158.048321402091,222.800806370086,1.10883524584438E-14));
#89240=CARTESIAN_POINT('Ctrl Pts',(158.116987698191,222.726874106645,1.39196752552947E-14));
#89241=CARTESIAN_POINT('Ctrl Pts',(158.189166938781,222.656402926642,2.01694406300404E-14));
#89242=CARTESIAN_POINT('Ctrl Pts',(158.26454599322,222.589679804418,1.73125402902485E-14));
#89243=CARTESIAN_POINT('Ctrl Pts',(158.329365962863,222.532303245515,1.48558340516762E-14));
#89244=CARTESIAN_POINT('Ctrl Pts',(158.396553121545,222.477698163774,1.06264985383864E-14));
#89245=CARTESIAN_POINT('Ctrl Pts',(158.465934582306,222.426062335657,8.84015083357781E-15));
#89246=CARTESIAN_POINT('Ctrl Pts',(158.491454268484,222.407069796228,8.1831016401346E-15));
#89247=CARTESIAN_POINT('Ctrl Pts',(158.517271035126,222.38847913505,6.96638787698447E-15));
#89248=CARTESIAN_POINT('Ctrl Pts',(158.543376988089,222.370300845808,5.81479309147426E-15));
#89249=CARTESIAN_POINT('Ctrl Pts',(158.560069502231,222.358677391546,5.07844716031687E-15));
#89250=CARTESIAN_POINT('Ctrl Pts',(158.576881299093,222.347221964069,1.4774855333679E-14));
#89251=CARTESIAN_POINT('Ctrl Pts',(158.593795529517,222.335946953852,1.42247325030098E-14));
#89252=CARTESIAN_POINT('Ctrl Pts',(158.679989199738,222.278490333717,1.14213471488789E-14));
#89253=CARTESIAN_POINT('Ctrl Pts',(158.768924528117,222.225655835067,3.46784439453926E-15));
#89254=CARTESIAN_POINT('Ctrl Pts',(158.860295151837,222.17776281636,2.90739654573713E-15));
#89255=CARTESIAN_POINT('Ctrl Pts',(158.951665775557,222.129869797652,2.346948696935E-15));
#89256=CARTESIAN_POINT('Ctrl Pts',(159.045472333248,222.086917356743,2.82861414654592E-16));
#89257=CARTESIAN_POINT('Ctrl Pts',(159.141446275838,222.049265302153,-1.79847456371895E-15));
#89258=CARTESIAN_POINT('Ctrl Pts',(159.162330716112,222.04107201485,-2.25850751576755E-15));
#89259=CARTESIAN_POINT('Ctrl Pts',(159.183317907923,222.033129893401,-3.50002483407811E-15));
#89260=CARTESIAN_POINT('Ctrl Pts',(159.204403756968,222.025437709964,-3.71924713249427E-15));
#89261=CARTESIAN_POINT('Ctrl Pts',(157.485690591028,225.001427433753,19.112583302492));
#89262=CARTESIAN_POINT('Ctrl Pts',(157.484001218019,225.327429254226,19.092036810933));
#89263=CARTESIAN_POINT('Ctrl Pts',(157.542838162647,225.652846145079,19.071490319374));
#89264=CARTESIAN_POINT('Ctrl Pts',(157.665030210741,225.952420038454,19.0509438278151));
#89265=CARTESIAN_POINT('Ctrl Pts',(157.979746531824,226.723998836627,18.9980245394045));
#89266=CARTESIAN_POINT('Ctrl Pts',(158.714738521617,227.32414419925,18.9451052509939));
#89267=CARTESIAN_POINT('Ctrl Pts',(159.533660651586,227.478241959391,18.8921859625833));
#89268=CARTESIAN_POINT('Ctrl Pts',(160.352582781555,227.632339719532,18.8392666741727));
#89269=CARTESIAN_POINT('Ctrl Pts',(161.255435051699,227.340389877191,18.7863473857621));
#89270=CARTESIAN_POINT('Ctrl Pts',(161.829078646719,226.735982727646,18.7334280973515));
#89271=CARTESIAN_POINT('Ctrl Pts',(162.402722241738,226.131575578101,18.6805088089409));
#89272=CARTESIAN_POINT('Ctrl Pts',(162.647157161632,225.214711121351,18.6275895205303));
#89273=CARTESIAN_POINT('Ctrl Pts',(162.450526923907,224.404949380834,18.5746702321197));
#89274=CARTESIAN_POINT('Ctrl Pts',(162.253896686182,223.595187640316,18.5217509437091));
#89275=CARTESIAN_POINT('Ctrl Pts',(161.616201290837,222.892528616031,18.4688316552985));
#89276=CARTESIAN_POINT('Ctrl Pts',(160.829251616835,222.618507682391,18.4159123668879));
#89277=CARTESIAN_POINT('Ctrl Pts',(160.042301942833,222.344486748751,18.3629930784773));
#89278=CARTESIAN_POINT('Ctrl Pts',(159.106097990172,222.499103905755,18.3100737900667));
#89279=CARTESIAN_POINT('Ctrl Pts',(158.449045956583,223.011607011104,18.2571545016561));
#89280=CARTESIAN_POINT('Ctrl Pts',(157.850708354407,223.478312634838,18.2089641019347));
#89281=CARTESIAN_POINT('Ctrl Pts',(157.483861524418,224.241800364934,18.1607737022134));
#89282=CARTESIAN_POINT('Ctrl Pts',(157.479093530148,225.001296842243,18.112583302492));
#89283=CARTESIAN_POINT('Origin',(0.,225.,22.2084234471774));
#89284=CARTESIAN_POINT('Ctrl Pts',(-3.07632864029364,225.002216919788,19.7084234471775));
#89285=CARTESIAN_POINT('Ctrl Pts',(-3.07751543998229,225.146316230092,19.7009407276991));
#89286=CARTESIAN_POINT('Ctrl Pts',(-3.002794304667,226.308308938777,19.6405387198101));
#89287=CARTESIAN_POINT('Ctrl Pts',(-1.52182622034608,228.298871155631,19.5272174235105));
#89288=CARTESIAN_POINT('Ctrl Pts',(1.94583867854751,228.067542026651,19.3684595582787));
#89289=CARTESIAN_POINT('Ctrl Pts',(3.63261192033118,225.029235473214,19.2097016930469));
#89290=CARTESIAN_POINT('Ctrl Pts',(1.99484850327397,221.96395749968,19.0509438278151));
#89291=CARTESIAN_POINT('Ctrl Pts',(-1.46861477289244,221.67737141594,18.8921859625833));
#89292=CARTESIAN_POINT('Ctrl Pts',(-2.99280343380595,223.658124429256,18.7780125023708));
#89293=CARTESIAN_POINT('Ctrl Pts',(-3.07726971933124,224.836966997831,18.7167583305688));
#89294=CARTESIAN_POINT('Ctrl Pts',(-3.07588051624417,224.997572007392,18.7084234471775));
#89295=CARTESIAN_POINT('Ctrl Pts',(-3.07038312444426,224.996706709974,19.7915765528225));
#89296=CARTESIAN_POINT('Ctrl Pts',(-3.06508366964555,225.700112229625,19.7552124583938));
#89297=CARTESIAN_POINT('Ctrl Pts',(-2.47776202454432,227.437543589317,19.6659290755545));
#89298=CARTESIAN_POINT('Ctrl Pts',(0.407268901123991,228.609154817042,19.5237264043046));
#89299=CARTESIAN_POINT('Ctrl Pts',(3.25295011294267,226.616814793291,19.3649685390728));
#89300=CARTESIAN_POINT('Ctrl Pts',(3.12275731293263,223.14341933887,19.206210673841));
#89301=CARTESIAN_POINT('Ctrl Pts',(0.134013646578404,221.369829208712,19.0474528086092));
#89302=CARTESIAN_POINT('Ctrl Pts',(-2.57444317314689,222.717848478559,18.9092414349364));
#89303=CARTESIAN_POINT('Ctrl Pts',(-3.06630351957984,224.374665598836,18.8239493496742));
#89304=CARTESIAN_POINT('Ctrl Pts',(-3.06955363737172,225.001741577652,18.7915765528225));
#89305=CARTESIAN_POINT('Ctrl Pts',(1.91346599666507,226.635987203375,20.));
#89306=CARTESIAN_POINT('Ctrl Pts',(2.45743451545281,225.999756515378,19.9470807115894));
#89307=CARTESIAN_POINT('Ctrl Pts',(2.85075747508451,224.152305503521,19.8412421347682));
#89308=CARTESIAN_POINT('Ctrl Pts',(0.831598276500719,222.14123234529,19.6824842695364));
#89309=CARTESIAN_POINT('Ctrl Pts',(-1.94946050932766,222.75270577452,19.5237264043046));
#89310=CARTESIAN_POINT('Ctrl Pts',(-2.9459653310193,225.417892776033,19.3649685390728));
#89311=CARTESIAN_POINT('Ctrl Pts',(-1.24652595077964,227.702101231267,19.206210673841));
#89312=CARTESIAN_POINT('Ctrl Pts',(1.59383402415598,227.512619831493,19.0474528086093));
#89313=CARTESIAN_POINT('Ctrl Pts',(2.97546787357532,225.023946739488,18.8886949433774));
#89314=CARTESIAN_POINT('Ctrl Pts',(1.63397791019756,222.513181391067,18.7299370781457));
#89315=CARTESIAN_POINT('Ctrl Pts',(-1.20294052082536,222.278439088866,18.5711792129139));
#89316=CARTESIAN_POINT('Ctrl Pts',(-2.93892195162375,224.5344265124,18.4124213476821));
#89317=CARTESIAN_POINT('Ctrl Pts',(-1.9852050243123,227.216527803386,18.2536634824503));
#89318=CARTESIAN_POINT('Ctrl Pts',(0.785372889255974,227.870052581747,18.0949056172185));
#89319=CARTESIAN_POINT('Ctrl Pts',(2.83717686333081,225.896910448037,17.9361477519867));
#89320=CARTESIAN_POINT('Ctrl Pts',(2.29239702935025,223.102913397598,17.7773898867549));
#89321=CARTESIAN_POINT('Ctrl Pts',(-0.350384645949477,222.04513116686,17.6186320215231));
#89322=CARTESIAN_POINT('Ctrl Pts',(-2.67249422325434,223.691644167573,17.4598741562913));
#89323=CARTESIAN_POINT('Ctrl Pts',(-2.54873723378948,226.535564674241,17.3011162910595));
#89324=CARTESIAN_POINT('Ctrl Pts',(-0.0923760078729938,227.974136303935,
17.1423584258278));
#89325=CARTESIAN_POINT('Ctrl Pts',(2.44852772681453,226.690778577842,16.9836005605959));
#89326=CARTESIAN_POINT('Ctrl Pts',(2.74853898713179,223.860020328042,16.8248426953642));
#89327=CARTESIAN_POINT('Ctrl Pts',(0.533087472085183,222.072571446793,16.6660848301324));
#89328=CARTESIAN_POINT('Ctrl Pts',(-2.17024567525691,222.964305053653,16.5073269649006));
#89329=CARTESIAN_POINT('Ctrl Pts',(-2.88737006653445,225.719106599626,16.3485690996688));
#89330=CARTESIAN_POINT('Ctrl Pts',(-0.961973486173353,227.815781811798,
16.189811234437));
#89331=CARTESIAN_POINT('Ctrl Pts',(1.84382119076242,227.335453621575,16.0310533692052));
#89332=CARTESIAN_POINT('Ctrl Pts',(2.96215078648909,224.717718368216,15.8722955039734));
#89333=CARTESIAN_POINT('Ctrl Pts',(1.36952009887017,222.358327253417,15.7135376387416));
#89334=CARTESIAN_POINT('Ctrl Pts',(-1.47649532936267,222.416594932285,15.5547797735098));
#89335=CARTESIAN_POINT('Ctrl Pts',(-2.97122229023292,224.839194827597,15.396021908278));
#89336=CARTESIAN_POINT('Ctrl Pts',(-1.74668672791837,227.408963610339,15.2372640430462));
#89337=CARTESIAN_POINT('Ctrl Pts',(1.07641645909825,227.774048991643,15.0785061778144));
#89338=CARTESIAN_POINT('Ctrl Pts',(2.91438334507821,225.600324844875,14.9197483125826));
#89339=CARTESIAN_POINT('Ctrl Pts',(2.08510670824745,222.877183423688,14.7609904473508));
#89340=CARTESIAN_POINT('Ctrl Pts',(-0.652459505976317,222.096843649662,
14.6022325821191));
#89341=CARTESIAN_POINT('Ctrl Pts',(-2.79289480598801,223.973472453302,14.4434747168873));
#89342=CARTESIAN_POINT('Ctrl Pts',(-2.37727288938734,226.789579227313,14.2847168516555));
#89343=CARTESIAN_POINT('Ctrl Pts',(0.214029082096596,227.96786316286,14.1259589864237));
#89344=CARTESIAN_POINT('Ctrl Pts',(2.60945164606224,226.429958848466,13.9672011211919));
#89345=CARTESIAN_POINT('Ctrl Pts',(2.61670416616591,223.583356252188,13.8084432559601));
#89346=CARTESIAN_POINT('Ctrl Pts',(0.229149136293932,222.033265958199,13.6496853907283));
#89347=CARTESIAN_POINT('Ctrl Pts',(-2.36812317410319,223.198330542602,13.4909275254965));
#89348=CARTESIAN_POINT('Ctrl Pts',(-2.79808924868524,226.012282943567,13.3321696602647));
#89349=CARTESIAN_POINT('Ctrl Pts',(-0.667244152902773,227.899794034386,
13.1734117950329));
#89350=CARTESIAN_POINT('Ctrl Pts',(2.07426276537758,227.133413738967,13.0146539298011));
#89351=CARTESIAN_POINT('Ctrl Pts',(2.91740448235278,224.41453327354,12.8558960645693));
#89352=CARTESIAN_POINT('Ctrl Pts',(1.09053773180285,222.231471933146,12.6971381993376));
#89353=CARTESIAN_POINT('Ctrl Pts',(-1.73438910800869,222.582167370667,12.5383803341058));
#89354=CARTESIAN_POINT('Ctrl Pts',(-2.97200310437387,225.145663135475,12.379622468874));
#89355=CARTESIAN_POINT('Ctrl Pts',(-1.48963997648728,227.575848004424,12.2208646036422));
#89356=CARTESIAN_POINT('Ctrl Pts',(1.35604159930179,227.648616881017,12.0621067384104));
#89357=CARTESIAN_POINT('Ctrl Pts',(2.96067395673492,225.297371692257,11.9033488731786));
#89358=CARTESIAN_POINT('Ctrl Pts',(1.85569762538991,222.673971942438,11.7445910079468));
#89359=CARTESIAN_POINT('Ctrl Pts',(-0.947613099738392,222.17935297943,11.585833142715));
#89360=CARTESIAN_POINT('Ctrl Pts',(-2.8836683532501,224.266190058729,11.4270752774832));
#89361=CARTESIAN_POINT('Ctrl Pts',(-2.18059044326484,227.024609967423,11.2683174122514));
#89362=CARTESIAN_POINT('Ctrl Pts',(0.518163754646772,227.930106913546,11.1095595470196));
#89363=CARTESIAN_POINT('Ctrl Pts',(2.74269450468196,226.153970127617,10.9508016817878));
#89364=CARTESIAN_POINT('Ctrl Pts',(2.45711135188605,223.321719926271,10.792043816556));
#89365=CARTESIAN_POINT('Ctrl Pts',(-0.0772200135324106,222.025431582405,
10.6332859513243));
#89366=CARTESIAN_POINT('Ctrl Pts',(-2.5408796256026,223.45146813735,10.4745280860925));
#89367=CARTESIAN_POINT('Ctrl Pts',(-2.67912630423898,226.294720992098,10.3157702208607));
#89368=CARTESIAN_POINT('Ctrl Pts',(-0.365436694589916,227.953045245792,
10.1570123556289));
#89369=CARTESIAN_POINT('Ctrl Pts',(2.28270056357738,226.908742606662,9.99825449039707));
#89370=CARTESIAN_POINT('Ctrl Pts',(2.84171035572368,224.117558808975,9.83949662516529));
#89371=CARTESIAN_POINT('Ctrl Pts',(0.799986942059197,222.133985154613,9.68073875993349));
#89372=CARTESIAN_POINT('Ctrl Pts',(-1.97388448951912,222.773388174046,9.5219808947017));
#89373=CARTESIAN_POINT('Ctrl Pts',(-2.94125691391068,225.450586249032,9.36322302946991));
#89374=CARTESIAN_POINT('Ctrl Pts',(-1.21679112635331,227.715407806623,9.20446516423812));
#89375=CARTESIAN_POINT('Ctrl Pts',(1.62128185219347,227.495088246374,9.04570729900632));
#89376=CARTESIAN_POINT('Ctrl Pts',(2.97555774336814,224.99126402116,8.88694943377453));
#89377=CARTESIAN_POINT('Ctrl Pts',(1.60660330482325,222.495434963437,8.72819156854274));
#89378=CARTESIAN_POINT('Ctrl Pts',(-1.23271441511773,222.291783728687,8.56943370331094));
#89379=CARTESIAN_POINT('Ctrl Pts',(-2.94385195081828,224.566691918945,8.41067583807916));
#89380=CARTESIAN_POINT('Ctrl Pts',(-1.96077629689413,227.238163647945,8.25191797284736));
#89381=CARTESIAN_POINT('Ctrl Pts',(0.816801746841883,227.861268094359,8.09316010761557));
#89382=CARTESIAN_POINT('Ctrl Pts',(2.84684286398815,225.865740093333,7.93440224238377));
#89383=CARTESIAN_POINT('Ctrl Pts',(2.27145350396183,223.077886792932,7.77564437715199));
#89384=CARTESIAN_POINT('Ctrl Pts',(-0.38277001356761,222.049151424055,7.61688651192019));
#89385=CARTESIAN_POINT('Ctrl Pts',(-2.68668242973203,223.721032555843,7.45812864668841));
#89386=CARTESIAN_POINT('Ctrl Pts',(-2.53174319185694,226.563424642229,7.2993707814566));
#89387=CARTESIAN_POINT('Ctrl Pts',(-0.0597526843527511,227.974970557528,
7.14061291622481));
#89388=CARTESIAN_POINT('Ctrl Pts',(2.46692347752136,226.663823535564,6.98185505099302));
#89389=CARTESIAN_POINT('Ctrl Pts',(2.73587136977733,223.829945279281,6.82309718576122));
#89390=CARTESIAN_POINT('Ctrl Pts',(0.500949891998614,222.066901057388,6.66433932052944));
#89391=CARTESIAN_POINT('Ctrl Pts',(-2.19244090723784,222.988228872432,6.50558145529764));
#89392=CARTESIAN_POINT('Ctrl Pts',(-2.87930987438589,225.750729544315,6.34682359006585));
#89393=CARTESIAN_POINT('Ctrl Pts',(-0.931034557722079,227.826162566763,
6.18806572483406));
#89394=CARTESIAN_POINT('Ctrl Pts',(1.86932354955694,227.315091719245,6.02930785960227));
#89395=CARTESIAN_POINT('Ctrl Pts',(2.95887681779079,224.685249021313,5.87054999437047));
#89396=CARTESIAN_POINT('Ctrl Pts',(1.34046613873754,222.343466406698,5.71179212913869));
#89397=CARTESIAN_POINT('Ctrl Pts',(-1.50473909777578,222.432943232208,5.55303426390689));
#89398=CARTESIAN_POINT('Ctrl Pts',(-2.97280717117708,224.871790310653,5.3942763986751));
#89399=CARTESIAN_POINT('Ctrl Pts',(-1.72016223842006,227.427974891748,5.23551853344331));
#89400=CARTESIAN_POINT('Ctrl Pts',(1.10677510729556,227.762076947392,5.07676066821151));
#89401=CARTESIAN_POINT('Ctrl Pts',(2.92079191833656,225.568326289399,4.91800280297972));
#89402=CARTESIAN_POINT('Ctrl Pts',(2.06170008057449,222.854443433697,4.75924493774793));
#89403=CARTESIAN_POINT('Ctrl Pts',(-0.68425958985738,222.104173863102,4.60048707251613));
#89404=CARTESIAN_POINT('Ctrl Pts',(-2.80398491055471,224.004164259125,4.44172920728435));
#89405=CARTESIAN_POINT('Ctrl Pts',(-2.35750335138642,226.815543486026,4.28297134205255));
#89406=CARTESIAN_POINT('Ctrl Pts',(0.24656518228451,227.965337385933,4.12421347682076));
#89407=CARTESIAN_POINT('Ctrl Pts',(2.62497727078325,226.401254626798,3.96545561158896));
#89408=CARTESIAN_POINT('Ctrl Pts',(2.60101026436985,223.554743688413,3.80669774635717));
#89409=CARTESIAN_POINT('Ctrl Pts',(0.196598766116914,222.030931269372,3.64793988112538));
#89410=CARTESIAN_POINT('Ctrl Pts',(-2.38773991480887,223.224410436226,3.48918201589359));
#89411=CARTESIAN_POINT('Ctrl Pts',(-2.78681912030052,226.042909101251,3.33042415066179));
#89412=CARTESIAN_POINT('Ctrl Pts',(-0.635401575053557,227.90693739939,3.17166628543));
#89413=CARTESIAN_POINT('Ctrl Pts',(2.09753546379433,227.110536700736,3.01290842019821));
#89414=CARTESIAN_POINT('Ctrl Pts',(2.91080813455441,224.38257290303,2.85415055496642));
#89415=CARTESIAN_POINT('Ctrl Pts',(1.06010930306564,222.219678347057,2.69539268973462));
#89416=CARTESIAN_POINT('Ctrl Pts',(-1.76080149659037,222.6013340852,2.53663482450284));
#89417=CARTESIAN_POINT('Ctrl Pts',(-2.97022688518523,225.178248720063,2.37787695927104));
#89418=CARTESIAN_POINT('Ctrl Pts',(-1.46130064497296,227.592030243376,2.21911909403925));
#89419=CARTESIAN_POINT('Ctrl Pts',(1.38500768436501,227.633585566377,2.06036122880745));
#89420=CARTESIAN_POINT('Ctrl Pts',(2.96375744914242,225.264883936543,1.90160336357567));
#89421=CARTESIAN_POINT('Ctrl Pts',(1.83007567274748,222.6537596164,1.74284549834387));
#89422=CARTESIAN_POINT('Ctrl Pts',(-0.978489580748851,222.189916275707,
1.58408763311209));
#89423=CARTESIAN_POINT('Ctrl Pts',(-2.89154467470074,224.297857645524,1.42532976788028));
#89424=CARTESIAN_POINT('Ctrl Pts',(-2.15825115583635,227.048407395618,1.2665719026485));
#89425=CARTESIAN_POINT('Ctrl Pts',(0.550259436798537,227.924239087672,1.1078140374167));
#89426=CARTESIAN_POINT('Ctrl Pts',(2.75520165707748,226.123839149338,0.94905617218491));
#89427=CARTESIAN_POINT('Ctrl Pts',(2.43852444180769,223.294836940432,0.790298306953122));
#89428=CARTESIAN_POINT('Ctrl Pts',(-0.10977043955631,222.026531358032,0.631540441721324));
#89429=CARTESIAN_POINT('Ctrl Pts',(-2.55784675572612,223.479277150759,0.472782576489534));
#89430=CARTESIAN_POINT('Ctrl Pts',(-2.66448757984816,226.324330789744,0.314024711257741));
#89431=CARTESIAN_POINT('Ctrl Pts',(-0.33359347540508,227.956254895383,0.155266846025945));
#89432=CARTESIAN_POINT('Ctrl Pts',(2.30464641624464,226.884864210807,-0.00349101920584165));
#89433=CARTESIAN_POINT('Ctrl Pts',(2.82948413440186,224.083799326414,-0.162248884437639));
#89434=CARTESIAN_POINT('Ctrl Pts',(1.45887298303089,222.784105799646,-0.268087461258832));
#89435=CARTESIAN_POINT('Ctrl Pts',(0.65019999797512,222.567913197965,-0.32100674966943));
#89436=CARTESIAN_POINT('Ctrl Pts',(2.0543315503421,226.756425321227,20.1070022498898));
#89437=CARTESIAN_POINT('Ctrl Pts',(2.63834594750733,226.073356597808,20.0540829614792));
#89438=CARTESIAN_POINT('Ctrl Pts',(3.06062455964552,224.089899923906,19.948244384658));
#89439=CARTESIAN_POINT('Ctrl Pts',(0.892818884476147,221.930775567268,19.7894865194262));
#89440=CARTESIAN_POINT('Ctrl Pts',(-2.0929759073,222.587264451862,19.6307286541944));
#89441=CARTESIAN_POINT('Ctrl Pts',(-3.16284142821185,225.448657209463,19.4719707889627));
#89442=CARTESIAN_POINT('Ctrl Pts',(-1.33829270730179,227.901024539389,19.3132129237308));
#89443=CARTESIAN_POINT('Ctrl Pts',(1.71116890895316,227.697593896546,19.1544550584991));
#89444=CARTESIAN_POINT('Ctrl Pts',(3.19451588916061,225.02570965073,18.9956971932673));
#89445=CARTESIAN_POINT('Ctrl Pts',(1.75426810788969,222.330106760605,18.8369393280355));
#89446=CARTESIAN_POINT('Ctrl Pts',(-1.29149860484772,222.078083197891,18.6781814628037));
#89447=CARTESIAN_POINT('Ctrl Pts',(-3.15527952926067,224.50015192,18.5194235975719));
#89448=CARTESIAN_POINT('Ctrl Pts',(-2.1313518622491,227.379704163357,18.3606657323401));
#89449=CARTESIAN_POINT('Ctrl Pts',(0.843190476336583,228.081340133611,18.2019078671083));
#89450=CARTESIAN_POINT('Ctrl Pts',(3.04604417031683,225.962939207932,18.0431500018765));
#89451=CARTESIAN_POINT('Ctrl Pts',(2.46115873055101,222.963253662288,17.8843921366447));
#89452=CARTESIAN_POINT('Ctrl Pts',(-0.376179265366609,221.827599611583,
17.7256342714129));
#89453=CARTESIAN_POINT('Ctrl Pts',(-2.86923792244393,223.595325618373,17.5668764061811));
#89454=CARTESIAN_POINT('Ctrl Pts',(-2.73637019002741,226.648609885612,17.4081185409494));
#89455=CARTESIAN_POINT('Ctrl Pts',(-0.0991765454933055,228.193086292017,
17.2493606757175));
#89456=CARTESIAN_POINT('Ctrl Pts',(2.62878345883821,226.815250327498,17.0906028104858));
#89457=CARTESIAN_POINT('Ctrl Pts',(2.9508809503023,223.77609729625,16.931844945254));
#89458=CARTESIAN_POINT('Ctrl Pts',(0.572332309487286,221.857059990244,16.7730870800222));
#89459=CARTESIAN_POINT('Ctrl Pts',(-2.33001483718247,222.814441248269,16.6143292147904));
#89460=CARTESIAN_POINT('Ctrl Pts',(-3.09993249711944,225.772045794514,16.4555713495586));
#89461=CARTESIAN_POINT('Ctrl Pts',(-1.0327920572839,228.023074057724,16.2968134843268));
#89462=CARTESIAN_POINT('Ctrl Pts',(1.97955963261133,227.507385063296,16.138055619095));
#89463=CARTESIAN_POINT('Ctrl Pts',(3.18021842466029,224.696937356992,15.9792977538632));
#89464=CARTESIAN_POINT('Ctrl Pts',(1.47034143948213,222.163852569921,15.8205398886314));
#89465=CARTESIAN_POINT('Ctrl Pts',(-1.58519197327205,222.226409799197,15.6617820233996));
#89466=CARTESIAN_POINT('Ctrl Pts',(-3.18995775443279,224.827356671244,15.5030241581678));
#89467=CARTESIAN_POINT('Ctrl Pts',(-1.87527432417426,227.586306710948,15.344266292936));
#89468=CARTESIAN_POINT('Ctrl Pts',(1.15566009382299,227.978268950512,15.1855084277043));
#89469=CARTESIAN_POINT('Ctrl Pts',(3.12893443939975,225.644519563677,15.0267505624724));
#89470=CARTESIAN_POINT('Ctrl Pts',(2.2386081090797,222.720905897514,14.8679926972407));
#89471=CARTESIAN_POINT('Ctrl Pts',(-0.70049227463872,221.883119064321,14.7092348320089));
#89472=CARTESIAN_POINT('Ctrl Pts',(-2.99850215615409,223.897901540894,14.5504769667771));
#89473=CARTESIAN_POINT('Ctrl Pts',(-2.55228298227041,226.921324483901,14.3917191015453));
#89474=CARTESIAN_POINT('Ctrl Pts',(0.229785476621013,228.186351334796,14.2329612363135));
#89475=CARTESIAN_POINT('Ctrl Pts',(2.801554276345,226.535229569386,14.0742033710817));
#89476=CARTESIAN_POINT('Ctrl Pts',(2.80934071252649,223.479065762445,13.9154455058499));
#89477=CARTESIAN_POINT('Ctrl Pts',(0.246018639078369,221.814860909905,13.7566876406181));
#89478=CARTESIAN_POINT('Ctrl Pts',(-2.54245968317983,223.065695227367,13.5979297753863));
#89479=CARTESIAN_POINT('Ctrl Pts',(-3.00407900337164,226.086805196678,13.4391719101545));
#89480=CARTESIAN_POINT('Ctrl Pts',(-0.716365337810284,228.113271092727,
13.2804140449227));
#89481=CARTESIAN_POINT('Ctrl Pts',(2.22696585674466,227.290471407138,13.1216561796909));
#89482=CARTESIAN_POINT('Ctrl Pts',(3.13217798678021,224.371432379807,12.9628983144591));
#89483=CARTESIAN_POINT('Ctrl Pts',(1.17082094648441,222.027658413759,12.8041404492274));
#89484=CARTESIAN_POINT('Ctrl Pts',(-1.86207137799251,222.404171350554,12.6453825839956));
#89485=CARTESIAN_POINT('Ctrl Pts',(-3.19079605055485,225.156386565244,12.4866247187638));
#89486=CARTESIAN_POINT('Ctrl Pts',(-1.59930430312442,227.765476801572,12.327866853532));
#89487=CARTESIAN_POINT('Ctrl Pts',(1.45587067963436,227.843602777852,12.1691089883002));
#89488=CARTESIAN_POINT('Ctrl Pts',(3.17863287364251,225.319263603663,12.0103511230684));
#89489=CARTESIAN_POINT('Ctrl Pts',(1.99231038668972,222.502734391957,11.8515932578366));
#89490=CARTESIAN_POINT('Ctrl Pts',(-1.01737448781578,221.971702566529,11.6928353926048));
#89491=CARTESIAN_POINT('Ctrl Pts',(-3.09595827107957,224.212168433128,11.534077527373));
#89492=CARTESIAN_POINT('Ctrl Pts',(-2.34112116639695,227.173657718748,11.3753196621412));
#89493=CARTESIAN_POINT('Ctrl Pts',(0.556309937709806,228.145815545646,11.2165617969094));
#89494=CARTESIAN_POINT('Ctrl Pts',(2.94460620870091,226.238923108876,11.0578039316776));
#89495=CARTESIAN_POINT('Ctrl Pts',(2.63799899328275,223.198168291581,10.8990460664458));
#89496=CARTESIAN_POINT('Ctrl Pts',(-0.0829047970509779,221.806449782977,
10.7402882012141));
#89497=CARTESIAN_POINT('Ctrl Pts',(-2.7279341203838,223.337468307408,10.5815303359823));
#89498=CARTESIAN_POINT('Ctrl Pts',(-2.8763582440148,226.390035771523,10.4227724707505));
#89499=CARTESIAN_POINT('Ctrl Pts',(-0.392339415833482,228.170442552201,
10.2640146055187));
#89500=CARTESIAN_POINT('Ctrl Pts',(2.45074843029026,227.04926043378,10.1052567402869));
#89501=CARTESIAN_POINT('Ctrl Pts',(3.05091140938569,224.052595246948,9.9464988750551));
#89502=CARTESIAN_POINT('Ctrl Pts',(0.858880386585508,221.922994852854,9.7877410098233));
#89503=CARTESIAN_POINT('Ctrl Pts',(-2.11919793224307,222.609469448427,9.62898314459151));
#89504=CARTESIAN_POINT('Ctrl Pts',(-3.15778638681823,225.483757510795,9.47022527935972));
#89505=CARTESIAN_POINT('Ctrl Pts',(-1.3063688643543,227.915310718306,9.31146741412792));
#89506=CARTESIAN_POINT('Ctrl Pts',(1.74063739139499,227.678771671066,9.15270954889614));
#89507=CARTESIAN_POINT('Ctrl Pts',(3.19461237498849,224.990620895806,8.99395168366434));
#89508=CARTESIAN_POINT('Ctrl Pts',(1.72487823861759,222.311053876336,8.83519381843255));
#89509=CARTESIAN_POINT('Ctrl Pts',(-1.32346439390693,222.092410243503,8.67643595320076));
#89510=CARTESIAN_POINT('Ctrl Pts',(-3.1605724651718,224.534792641478,8.51767808796896));
#89511=CARTESIAN_POINT('Ctrl Pts',(-2.10512474059796,227.402932795679,8.35892022273718));
#89512=CARTESIAN_POINT('Ctrl Pts',(0.876933063789126,228.071908949767,8.20016235750537));
#89513=CARTESIAN_POINT('Ctrl Pts',(3.05642176268095,225.929474153829,8.04140449227359));
#89514=CARTESIAN_POINT('Ctrl Pts',(2.43867338455803,222.936384648857,7.88264662704178));
#89515=CARTESIAN_POINT('Ctrl Pts',(-0.410948779213894,221.831915832102,
7.72388876181));
#89516=CARTESIAN_POINT('Ctrl Pts',(-2.88447063640942,223.626877521225,7.56513089657821));
#89517=CARTESIAN_POINT('Ctrl Pts',(-2.71812508059212,226.678520848926,7.40637303134642));
#89518=CARTESIAN_POINT('Ctrl Pts',(-0.064151557904577,228.193981961697,
7.24761516611462));
#89519=CARTESIAN_POINT('Ctrl Pts',(2.64853346805454,226.786310908722,7.08885730088283));
#89520=CARTESIAN_POINT('Ctrl Pts',(2.93728076820118,223.74380818233,6.93009943565104));
#89521=CARTESIAN_POINT('Ctrl Pts',(0.537828824795869,221.850972158071,6.77134157041925));
#89522=CARTESIAN_POINT('Ctrl Pts',(-2.35384403791301,222.840126290913,6.61258370518745));
#89523=CARTESIAN_POINT('Ctrl Pts',(-3.09127892968659,225.805996757376,6.45382583995566));
#89524=CARTESIAN_POINT('Ctrl Pts',(-0.999575466572595,228.034219023184,
6.29506797472387));
#89525=CARTESIAN_POINT('Ctrl Pts',(2.0069394242413,227.485524158292,6.13631010949207));
#89526=CARTESIAN_POINT('Ctrl Pts',(3.17670343291052,224.662077681472,5.97755224426029));
#89527=CARTESIAN_POINT('Ctrl Pts',(1.43914858470087,222.14789769728,5.81879437902849));
#89528=CARTESIAN_POINT('Ctrl Pts',(-1.61551499163388,222.243961628382,5.6600365137967));
#89529=CARTESIAN_POINT('Ctrl Pts',(-3.19165931115384,224.86235176881,5.50127864856491));
#89530=CARTESIAN_POINT('Ctrl Pts',(-1.84679715461491,227.60671756501,5.34252078333311));
#89531=CARTESIAN_POINT('Ctrl Pts',(1.18825368520437,227.96541554822,5.18376291810132));
#89532=CARTESIAN_POINT('Ctrl Pts',(3.13581479905091,225.610165338311,5.02500505286953));
#89533=CARTESIAN_POINT('Ctrl Pts',(2.21347833212026,222.696491834775,4.86624718763774));
#89534=CARTESIAN_POINT('Ctrl Pts',(-0.734633417326518,221.890988913467,
4.70748932240595));
#89535=CARTESIAN_POINT('Ctrl Pts',(-3.01040869211954,223.930852816301,4.54873145717415));
#89536=CARTESIAN_POINT('Ctrl Pts',(-2.53105805027697,226.949200179601,4.38997359194236));
#89537=CARTESIAN_POINT('Ctrl Pts',(0.264716819669501,228.183639615205,4.23121572671057));
#89538=CARTESIAN_POINT('Ctrl Pts',(2.81822286661979,226.504412200118,4.07245786147877));
#89539=CARTESIAN_POINT('Ctrl Pts',(2.79249145695371,223.448346798741,3.91369999624699));
#89540=CARTESIAN_POINT('Ctrl Pts',(0.211071975512616,221.812354345939,3.75494213101519));
#89541=CARTESIAN_POINT('Ctrl Pts',(-2.56352056924564,223.09369507079,3.5961842657834));
#89542=CARTESIAN_POINT('Ctrl Pts',(-2.99197919059342,226.119685991062,3.43742640055161));
#89543=CARTESIAN_POINT('Ctrl Pts',(-0.682178572833074,228.120940338027,
3.27866853531981));
#89544=CARTESIAN_POINT('Ctrl Pts',(2.25195184484294,227.26591020694,3.11991067008802));
#89545=CARTESIAN_POINT('Ctrl Pts',(3.12509602900158,224.337119150509,2.96115280485623));
#89546=CARTESIAN_POINT('Ctrl Pts',(1.13815243745883,222.014996607363,2.80239493962443));
#89547=CARTESIAN_POINT('Ctrl Pts',(-1.89042819398914,222.424749080416,2.64363707439265));
#89548=CARTESIAN_POINT('Ctrl Pts',(-3.18888906964905,225.191371035635,2.48487920916085));
#89549=CARTESIAN_POINT('Ctrl Pts',(-1.5688786864963,227.782850344709,2.32612134392906));
#89550=CARTESIAN_POINT('Ctrl Pts',(1.48696919015871,227.827464887782,2.16736347869726));
#89551=CARTESIAN_POINT('Ctrl Pts',(3.18194336661653,225.284384164112,2.00860561346548));
#89552=CARTESIAN_POINT('Ctrl Pts',(1.96480219695107,222.481034074754,1.84984774823368));
#89553=CARTESIAN_POINT('Ctrl Pts',(-1.05052403383013,221.983043511628,1.69108988300189));
#89554=CARTESIAN_POINT('Ctrl Pts',(-3.10441443162012,224.246167324559,1.53233201777009));
#89555=CARTESIAN_POINT('Ctrl Pts',(-2.31713730514386,227.199207066186,1.37357415253831));
#89556=CARTESIAN_POINT('Ctrl Pts',(0.59076844002395,228.139515742124,1.21481628730651));
#89557=CARTESIAN_POINT('Ctrl Pts',(2.95803411273257,226.206573948019,1.05605842207472));
#89558=CARTESIAN_POINT('Ctrl Pts',(2.6180437519229,223.169306233895,0.897300556842932));
#89559=CARTESIAN_POINT('Ctrl Pts',(-0.117851520574949,221.807630521893,
0.738542691611135));
#89560=CARTESIAN_POINT('Ctrl Pts',(-2.74615033681632,223.367324564969,0.579784826379343));
#89561=CARTESIAN_POINT('Ctrl Pts',(-2.86064184590518,226.421825383467,0.421026961147552));
#89562=CARTESIAN_POINT('Ctrl Pts',(-0.3581519623068,228.173888489799,0.262269095915755));
#89563=CARTESIAN_POINT('Ctrl Pts',(2.47430989289899,227.023624158005,0.103511230683968));
#89564=CARTESIAN_POINT('Ctrl Pts',(3.03778511801357,224.016350458554,-0.0552466345478283));
#89565=CARTESIAN_POINT('Ctrl Pts',(1.56627230491969,222.620976084267,-0.161085211369022));
#89566=CARTESIAN_POINT('Ctrl Pts',(0.698066426161045,222.388867814061,-0.21400449977962));
#89567=CARTESIAN_POINT('Ctrl Pts',(2.19519710401913,226.876863439079,20.2140044997796));
#89568=CARTESIAN_POINT('Ctrl Pts',(2.81925737956185,226.146956680238,20.161085211369));
#89569=CARTESIAN_POINT('Ctrl Pts',(3.27049164420653,224.027494344291,20.0552466345478));
#89570=CARTESIAN_POINT('Ctrl Pts',(0.954039492451579,221.720318789244,19.896488769316));
#89571=CARTESIAN_POINT('Ctrl Pts',(-2.23649130527235,222.421823129205,19.7377309040842));
#89572=CARTESIAN_POINT('Ctrl Pts',(-3.3797175254044,225.479421642892,19.5789730388525));
#89573=CARTESIAN_POINT('Ctrl Pts',(-1.43005946382394,228.09994784751,19.4202151736207));
#89574=CARTESIAN_POINT('Ctrl Pts',(1.82850379375034,227.882567961598,19.2614573083888));
#89575=CARTESIAN_POINT('Ctrl Pts',(3.41356390474589,225.027472561972,19.1026994431571));
#89576=CARTESIAN_POINT('Ctrl Pts',(1.87455830558183,222.147032130142,18.9439415779253));
#89577=CARTESIAN_POINT('Ctrl Pts',(-1.38005668887008,221.877727306915,18.7851837126935));
#89578=CARTESIAN_POINT('Ctrl Pts',(-3.37163710689758,224.465877327599,18.6264258474617));
#89579=CARTESIAN_POINT('Ctrl Pts',(-2.27749870018589,227.542880523328,18.4676679822299));
#89580=CARTESIAN_POINT('Ctrl Pts',(0.90100806341719,228.292627685475,18.3089101169981));
#89581=CARTESIAN_POINT('Ctrl Pts',(3.25491147730285,226.028967967827,18.1501522517663));
#89582=CARTESIAN_POINT('Ctrl Pts',(2.62992043175177,222.823593926977,17.9913943865345));
#89583=CARTESIAN_POINT('Ctrl Pts',(-0.401973884783737,221.610068056307,
17.8326365213027));
#89584=CARTESIAN_POINT('Ctrl Pts',(-3.06598162163353,223.499007069173,17.6738786560709));
#89585=CARTESIAN_POINT('Ctrl Pts',(-2.92400314626534,226.761655096983,17.5151207908392));
#89586=CARTESIAN_POINT('Ctrl Pts',(-0.105977083113621,228.412036280099,
17.3563629256073));
#89587=CARTESIAN_POINT('Ctrl Pts',(2.8090391908619,226.939722077155,17.1976050603756));
#89588=CARTESIAN_POINT('Ctrl Pts',(3.15322291347281,223.692174264458,17.0388471951438));
#89589=CARTESIAN_POINT('Ctrl Pts',(0.611577146889394,221.641548533695,16.880089329912));
#89590=CARTESIAN_POINT('Ctrl Pts',(-2.48978399910804,222.664577442884,16.7213314646802));
#89591=CARTESIAN_POINT('Ctrl Pts',(-3.31249492770443,225.824984989402,16.5625735994484));
#89592=CARTESIAN_POINT('Ctrl Pts',(-1.10361062839445,228.230366303651,16.4038157342166));
#89593=CARTESIAN_POINT('Ctrl Pts',(2.11529807446024,227.679316505017,16.2450578689848));
#89594=CARTESIAN_POINT('Ctrl Pts',(3.39828606283148,224.676156345768,16.086300003753));
#89595=CARTESIAN_POINT('Ctrl Pts',(1.5711627800941,221.969377886425,15.9275421385212));
#89596=CARTESIAN_POINT('Ctrl Pts',(-1.69388861718143,222.036224666109,15.7687842732894));
#89597=CARTESIAN_POINT('Ctrl Pts',(-3.40869321863266,224.815518514891,15.6100264080576));
#89598=CARTESIAN_POINT('Ctrl Pts',(-2.00386192043016,227.763649811556,15.4512685428258));
#89599=CARTESIAN_POINT('Ctrl Pts',(1.23490372854773,228.18248890938,15.2925106775941));
#89600=CARTESIAN_POINT('Ctrl Pts',(3.3434855337213,225.688714282479,15.1337528123623));
#89601=CARTESIAN_POINT('Ctrl Pts',(2.39210950991196,222.56462837134,14.9749949471305));
#89602=CARTESIAN_POINT('Ctrl Pts',(-0.748525043301124,221.66939447898,14.8162370818987));
#89603=CARTESIAN_POINT('Ctrl Pts',(-3.20410950632018,223.822330628485,14.6574792166669));
#89604=CARTESIAN_POINT('Ctrl Pts',(-2.72729307515348,227.05306974049,14.4987213514351));
#89605=CARTESIAN_POINT('Ctrl Pts',(0.245541871145432,228.404839506733,14.3399634862033));
#89606=CARTESIAN_POINT('Ctrl Pts',(2.99365690662777,226.640500290306,14.1812056209715));
#89607=CARTESIAN_POINT('Ctrl Pts',(3.00197725888707,223.374775272702,14.0224477557397));
#89608=CARTESIAN_POINT('Ctrl Pts',(0.262888141862807,221.596455861611,13.8636898905079));
#89609=CARTESIAN_POINT('Ctrl Pts',(-2.71679619225647,222.933059912132,13.7049320252761));
#89610=CARTESIAN_POINT('Ctrl Pts',(-3.21006875805803,226.161327449789,13.5461741600443));
#89611=CARTESIAN_POINT('Ctrl Pts',(-0.765486522717795,228.326748151068,
13.3874162948126));
#89612=CARTESIAN_POINT('Ctrl Pts',(2.37966894811175,227.44752907531,13.2286584295807));
#89613=CARTESIAN_POINT('Ctrl Pts',(3.34695149120764,224.328331486075,13.069900564349));
#89614=CARTESIAN_POINT('Ctrl Pts',(1.25110416116596,221.823844894372,12.9111426991172));
#89615=CARTESIAN_POINT('Ctrl Pts',(-1.98975364797633,222.22617533044,12.7523848338854));
#89616=CARTESIAN_POINT('Ctrl Pts',(-3.40958899673583,225.167109995012,12.5936269686536));
#89617=CARTESIAN_POINT('Ctrl Pts',(-1.70896862976155,227.95510559872,12.4348691034218));
#89618=CARTESIAN_POINT('Ctrl Pts',(1.55569975996694,228.038588674687,12.27611123819));
#89619=CARTESIAN_POINT('Ctrl Pts',(3.39659179055011,225.34115551507,12.1173533729582));
#89620=CARTESIAN_POINT('Ctrl Pts',(2.12892314798953,222.331496841476,11.9585955077264));
#89621=CARTESIAN_POINT('Ctrl Pts',(-1.08713587589318,221.764052153628,11.7998376424946));
#89622=CARTESIAN_POINT('Ctrl Pts',(-3.30824818890903,224.158146807528,11.6410797772628));
#89623=CARTESIAN_POINT('Ctrl Pts',(-2.50165188952906,227.322705470074,11.482321912031));
#89624=CARTESIAN_POINT('Ctrl Pts',(0.594456120772842,228.361524177746,11.3235640467992));
#89625=CARTESIAN_POINT('Ctrl Pts',(3.14651791271986,226.323876090134,11.1648061815675));
#89626=CARTESIAN_POINT('Ctrl Pts',(2.81888663467947,223.074616656891,11.0060483163356));
#89627=CARTESIAN_POINT('Ctrl Pts',(-0.0885895805695465,221.587467983548,
10.8472904511039));
#89628=CARTESIAN_POINT('Ctrl Pts',(-2.914988615165,223.223468477467,10.6885325858721));
#89629=CARTESIAN_POINT('Ctrl Pts',(-3.07359018379062,226.485350550948,10.5297747206403));
#89630=CARTESIAN_POINT('Ctrl Pts',(-0.419242137077048,228.387839858611,
10.3710168554085));
#89631=CARTESIAN_POINT('Ctrl Pts',(2.61879629700314,227.189778260897,10.2122589901767));
#89632=CARTESIAN_POINT('Ctrl Pts',(3.26011246304771,223.987631684921,10.0535011249449));
#89633=CARTESIAN_POINT('Ctrl Pts',(0.917773831111815,221.712004551095,9.89474325971311));
#89634=CARTESIAN_POINT('Ctrl Pts',(-2.26451137496702,222.445550722809,9.73598539448132));
#89635=CARTESIAN_POINT('Ctrl Pts',(-3.37431585972579,225.516928772558,9.57722752924953));
#89636=CARTESIAN_POINT('Ctrl Pts',(-1.39594660235529,228.115213629989,9.41846966401773));
#89637=CARTESIAN_POINT('Ctrl Pts',(1.85999293059652,227.862455095757,9.25971179878594));
#89638=CARTESIAN_POINT('Ctrl Pts',(3.41366700660884,224.989977770452,9.10095393355415));
#89639=CARTESIAN_POINT('Ctrl Pts',(1.84315317241193,222.126672789235,8.94219606832236));
#89640=CARTESIAN_POINT('Ctrl Pts',(-1.41421437269613,221.893036758319,8.78343820309056));
#89641=CARTESIAN_POINT('Ctrl Pts',(-3.37729297952532,224.502893364011,8.62468033785877));
#89642=CARTESIAN_POINT('Ctrl Pts',(-2.24947318430178,227.567701943412,8.46592247262699));
#89643=CARTESIAN_POINT('Ctrl Pts',(0.937064380736367,228.282549805174,8.30716460739518));
#89644=CARTESIAN_POINT('Ctrl Pts',(3.26600066137376,225.993208214324,8.14840674216341));
#89645=CARTESIAN_POINT('Ctrl Pts',(2.60589326515423,222.794882504782,7.98964887693159));
#89646=CARTESIAN_POINT('Ctrl Pts',(-0.439127544860177,221.614680240149,
7.83089101169981));
#89647=CARTESIAN_POINT('Ctrl Pts',(-3.08225884308682,223.532722486607,7.67213314646803));
#89648=CARTESIAN_POINT('Ctrl Pts',(-2.90450696932731,226.793617055623,7.51337528123622));
#89649=CARTESIAN_POINT('Ctrl Pts',(-0.0685504314564027,228.412993365865,
7.35461741600444));
#89650=CARTESIAN_POINT('Ctrl Pts',(2.83014345858772,226.90879828188,7.19585955077264));
#89651=CARTESIAN_POINT('Ctrl Pts',(3.13869016662505,223.65767108538,7.03710168554085));
#89652=CARTESIAN_POINT('Ctrl Pts',(0.574707757593123,221.635043258754,6.87834382030906));
#89653=CARTESIAN_POINT('Ctrl Pts',(-2.51524716858818,222.692023709393,6.71958595507726));
#89654=CARTESIAN_POINT('Ctrl Pts',(-3.30324798498729,225.861263970437,6.56082808984547));
#89655=CARTESIAN_POINT('Ctrl Pts',(-1.06811637542311,228.242275479605,6.40207022461368));
#89656=CARTESIAN_POINT('Ctrl Pts',(2.14455529892566,227.655956597338,6.24331235938189));
#89657=CARTESIAN_POINT('Ctrl Pts',(3.39453004803023,224.63890634163,6.08455449415009));
#89658=CARTESIAN_POINT('Ctrl Pts',(1.53783103066421,221.952328987863,5.9257966289183));
#89659=CARTESIAN_POINT('Ctrl Pts',(-1.72629088549199,222.054980024556,5.76703876368652));
#89660=CARTESIAN_POINT('Ctrl Pts',(-3.41051145113059,224.852913226966,5.60828089845471));
#89661=CARTESIAN_POINT('Ctrl Pts',(-1.97343207080975,227.785460238272,5.44952303322293));
#89662=CARTESIAN_POINT('Ctrl Pts',(1.26973226311318,228.168754149048,5.29076516799113));
#89663=CARTESIAN_POINT('Ctrl Pts',(3.35083767976526,225.652004387222,5.13200730275934));
#89664=CARTESIAN_POINT('Ctrl Pts',(2.36525658366603,222.538540235852,4.97324943752754));
#89665=CARTESIAN_POINT('Ctrl Pts',(-0.785007244795656,221.677803963833,
4.81449157229576));
#89666=CARTESIAN_POINT('Ctrl Pts',(-3.21683247368438,223.857541373477,4.65573370706396));
#89667=CARTESIAN_POINT('Ctrl Pts',(-2.70461274916752,227.082856873177,4.49697584183217));
#89668=CARTESIAN_POINT('Ctrl Pts',(0.282868457054493,228.401941844477,4.33821797660038));
#89669=CARTESIAN_POINT('Ctrl Pts',(3.01146846245633,226.607569773438,4.17946011136859));
#89670=CARTESIAN_POINT('Ctrl Pts',(2.98397264953758,223.34194990907,4.02070224613679));
#89671=CARTESIAN_POINT('Ctrl Pts',(0.225545184908317,221.593777422506,3.861944380905));
#89672=CARTESIAN_POINT('Ctrl Pts',(-2.73930122368241,222.962979705353,3.70318651567321));
#89673=CARTESIAN_POINT('Ctrl Pts',(-3.19713926088632,226.196462880873,3.54442865044142));
#89674=CARTESIAN_POINT('Ctrl Pts',(-0.728955570612594,228.334943276665,
3.38567078520962));
#89675=CARTESIAN_POINT('Ctrl Pts',(2.40636822589155,227.421283713145,3.22691291997783));
#89676=CARTESIAN_POINT('Ctrl Pts',(3.33938392344875,224.291665397987,3.06815505474604));
#89677=CARTESIAN_POINT('Ctrl Pts',(1.21619557185201,221.81031486767,2.90939718951424));
#89678=CARTESIAN_POINT('Ctrl Pts',(-2.02005489138791,222.248164075633,2.75063932428246));
#89679=CARTESIAN_POINT('Ctrl Pts',(-3.40755125411287,225.204493351206,2.59188145905066));
#89680=CARTESIAN_POINT('Ctrl Pts',(-1.67645672801963,227.973670446042,2.43312359381887));
#89681=CARTESIAN_POINT('Ctrl Pts',(1.58893069595241,228.021344209186,2.27436572858707));
#89682=CARTESIAN_POINT('Ctrl Pts',(3.40012928409063,225.303884391681,2.11560786335529));
#89683=CARTESIAN_POINT('Ctrl Pts',(2.09952872115466,222.308308533108,1.95684999812349));
#89684=CARTESIAN_POINT('Ctrl Pts',(-1.1225584869114,221.776170747549,1.7980921328917));
#89685=CARTESIAN_POINT('Ctrl Pts',(-3.3172841885395,224.194477003594,1.6393342676599));
#89686=CARTESIAN_POINT('Ctrl Pts',(-2.47602345445138,227.350006736754,1.48057640242812));
#89687=CARTESIAN_POINT('Ctrl Pts',(0.631277443249367,228.354792396575,1.32181853719632));
#89688=CARTESIAN_POINT('Ctrl Pts',(3.16086656838766,226.289308746699,1.16306067196453));
#89689=CARTESIAN_POINT('Ctrl Pts',(2.7975630620381,223.043775527358,1.00430280673274));
#89690=CARTESIAN_POINT('Ctrl Pts',(-0.125932601593587,221.588729685755,
0.845544941500944));
#89691=CARTESIAN_POINT('Ctrl Pts',(-2.93445391790652,223.255371979179,0.686787076269154));
#89692=CARTESIAN_POINT('Ctrl Pts',(-3.05679611196219,226.519319977191,0.528029211037361));
#89693=CARTESIAN_POINT('Ctrl Pts',(-0.382710449208524,228.391522084216,
0.369271345805566));
#89694=CARTESIAN_POINT('Ctrl Pts',(2.64397336955335,227.162384105202,0.210513480573778));
#89695=CARTESIAN_POINT('Ctrl Pts',(3.24608610162528,223.948901590694,0.0517556153419817));
#89696=CARTESIAN_POINT('Ctrl Pts',(1.6736716268085,222.457846368889,-0.0540829614792118));
#89697=CARTESIAN_POINT('Ctrl Pts',(0.745932854346969,222.209822430158,-0.10700224988981));
#89698=CARTESIAN_POINT('Ctrl Pts',(2.33606265769616,226.997301556931,20.3210067496694));
#89699=CARTESIAN_POINT('Ctrl Pts',(3.00016881161637,226.220556762668,20.2680874612588));
#89700=CARTESIAN_POINT('Ctrl Pts',(3.48035872876753,223.965088764676,20.1622488844376));
#89701=CARTESIAN_POINT('Ctrl Pts',(1.01526010042701,221.509862011222,20.0034910192058));
#89702=CARTESIAN_POINT('Ctrl Pts',(-2.3800067032447,222.256381806548,19.844733153974));
#89703=CARTESIAN_POINT('Ctrl Pts',(-3.59659362259695,225.510186076321,19.6859752887423));
#89704=CARTESIAN_POINT('Ctrl Pts',(-1.52182622034608,228.298871155631,19.5272174235105));
#89705=CARTESIAN_POINT('Ctrl Pts',(1.94583867854751,228.067542026651,19.3684595582787));
#89706=CARTESIAN_POINT('Ctrl Pts',(3.63261192033118,225.029235473214,19.2097016930469));
#89707=CARTESIAN_POINT('Ctrl Pts',(1.99484850327397,221.96395749968,19.0509438278151));
#89708=CARTESIAN_POINT('Ctrl Pts',(-1.46861477289244,221.67737141594,18.8921859625833));
#89709=CARTESIAN_POINT('Ctrl Pts',(-3.5879946845345,224.431602735199,18.7334280973515));
#89710=CARTESIAN_POINT('Ctrl Pts',(-2.42364553812269,227.7060568833,18.5746702321197));
#89711=CARTESIAN_POINT('Ctrl Pts',(0.958825650497796,228.503915237338,18.4159123668879));
#89712=CARTESIAN_POINT('Ctrl Pts',(3.46377878428887,226.094996727722,18.2571545016561));
#89713=CARTESIAN_POINT('Ctrl Pts',(2.79868213295254,222.683934191666,18.0983966364244));
#89714=CARTESIAN_POINT('Ctrl Pts',(-0.427768504200867,221.39253650103,17.9396387711925));
#89715=CARTESIAN_POINT('Ctrl Pts',(-3.26272532082312,223.402688519974,17.7808809059608));
#89716=CARTESIAN_POINT('Ctrl Pts',(-3.11163610250327,226.874700308353,17.622123040729));
#89717=CARTESIAN_POINT('Ctrl Pts',(-0.112777620733934,228.630986268181,
17.4633651754972));
#89718=CARTESIAN_POINT('Ctrl Pts',(2.98929492288558,227.064193826811,17.3046073102654));
#89719=CARTESIAN_POINT('Ctrl Pts',(3.35556487664332,223.608251232666,17.1458494450336));
#89720=CARTESIAN_POINT('Ctrl Pts',(0.650821984291496,221.426037077147,16.9870915798018));
#89721=CARTESIAN_POINT('Ctrl Pts',(-2.6495531610336,222.514713637499,16.82833371457));
#89722=CARTESIAN_POINT('Ctrl Pts',(-3.52505735828943,225.87792418429,16.6695758493382));
#89723=CARTESIAN_POINT('Ctrl Pts',(-1.174429199505,228.437658549578,16.5108179841064));
#89724=CARTESIAN_POINT('Ctrl Pts',(2.25103651630915,227.851247946737,16.3520601188746));
#89725=CARTESIAN_POINT('Ctrl Pts',(3.61635370100267,224.655375334543,16.1933022536428));
#89726=CARTESIAN_POINT('Ctrl Pts',(1.67198412070606,221.77490320293,16.034544388411));
#89727=CARTESIAN_POINT('Ctrl Pts',(-1.80258526109082,221.84603953302,15.8757865231792));
#89728=CARTESIAN_POINT('Ctrl Pts',(-3.62742868283253,224.803680358538,15.7170286579475));
#89729=CARTESIAN_POINT('Ctrl Pts',(-2.13244951668605,227.940992912165,15.5582707927156));
#89730=CARTESIAN_POINT('Ctrl Pts',(1.31414736327247,228.386708868249,15.3995129274839));
#89731=CARTESIAN_POINT('Ctrl Pts',(3.55803662804284,225.732909001281,15.2407550622521));
#89732=CARTESIAN_POINT('Ctrl Pts',(2.54561091074421,222.408350845166,15.0819971970203));
#89733=CARTESIAN_POINT('Ctrl Pts',(-0.796557811963526,221.455669893639,
14.9232393317885));
#89734=CARTESIAN_POINT('Ctrl Pts',(-3.40971685648626,223.746759716077,14.7644814665567));
#89735=CARTESIAN_POINT('Ctrl Pts',(-2.90230316803655,227.184814997078,14.6057236013249));
#89736=CARTESIAN_POINT('Ctrl Pts',(0.261298265669851,228.62332767867,14.4469657360931));
#89737=CARTESIAN_POINT('Ctrl Pts',(3.18575953691054,226.745771011226,14.2882078708613));
#89738=CARTESIAN_POINT('Ctrl Pts',(3.19461380524764,223.270484782959,14.1294500056295));
#89739=CARTESIAN_POINT('Ctrl Pts',(0.279757644647243,221.378050813317,13.9706921403977));
#89740=CARTESIAN_POINT('Ctrl Pts',(-2.89113270133312,222.800424596897,13.8119342751659));
#89741=CARTESIAN_POINT('Ctrl Pts',(-3.41605851274443,226.235849702901,13.6531764099342));
#89742=CARTESIAN_POINT('Ctrl Pts',(-0.814607707625303,228.540225209408,
13.4944185447024));
#89743=CARTESIAN_POINT('Ctrl Pts',(2.53237203947883,227.604586743482,13.3356606794706));
#89744=CARTESIAN_POINT('Ctrl Pts',(3.56172499563507,224.285230592343,13.1769028142388));
#89745=CARTESIAN_POINT('Ctrl Pts',(1.33138737584751,221.620031374985,13.018144949007));
#89746=CARTESIAN_POINT('Ctrl Pts',(-2.11743591796015,222.048179310326,12.8593870837752));
#89747=CARTESIAN_POINT('Ctrl Pts',(-3.62838194291682,225.17783342478,12.7006292185434));
#89748=CARTESIAN_POINT('Ctrl Pts',(-1.81863295639868,228.144734395868,12.5418713533116));
#89749=CARTESIAN_POINT('Ctrl Pts',(1.65552884029951,228.233574571522,12.3831134880798));
#89750=CARTESIAN_POINT('Ctrl Pts',(3.6145507074577,225.363047426476,12.224355622848));
#89751=CARTESIAN_POINT('Ctrl Pts',(2.26553590928934,222.160259290996,12.0655977576162));
#89752=CARTESIAN_POINT('Ctrl Pts',(-1.15689726397057,221.556401740727,11.9068398923844));
#89753=CARTESIAN_POINT('Ctrl Pts',(-3.5205381067385,224.104125181928,11.7480820271526));
#89754=CARTESIAN_POINT('Ctrl Pts',(-2.66218261266118,227.471753221399,11.5893241619208));
#89755=CARTESIAN_POINT('Ctrl Pts',(0.632602303835877,228.577232809845,11.430566296689));
#89756=CARTESIAN_POINT('Ctrl Pts',(3.34842961673882,226.408829071393,11.2718084314573));
#89757=CARTESIAN_POINT('Ctrl Pts',(2.99977427607618,222.951065022201,11.1130505662255));
#89758=CARTESIAN_POINT('Ctrl Pts',(-0.0942743640881148,221.36848618412,
10.9542927009937));
#89759=CARTESIAN_POINT('Ctrl Pts',(-3.10204310994621,223.109468647525,10.7955348357619));
#89760=CARTESIAN_POINT('Ctrl Pts',(-3.27082212356644,226.580665330373,10.6367769705301));
#89761=CARTESIAN_POINT('Ctrl Pts',(-0.446144858320614,228.605237165021,
10.4780191052983));
#89762=CARTESIAN_POINT('Ctrl Pts',(2.78684416371602,227.330296088014,10.3192612400665));
#89763=CARTESIAN_POINT('Ctrl Pts',(3.46931351670972,223.922668122894,10.1605033748347));
#89764=CARTESIAN_POINT('Ctrl Pts',(0.976667275638124,221.501014249336,10.0017455096029));
#89765=CARTESIAN_POINT('Ctrl Pts',(-2.40982481769097,222.281631997191,9.84298764437114));
#89766=CARTESIAN_POINT('Ctrl Pts',(-3.59084533263335,225.55010003432,9.68422977913934));
#89767=CARTESIAN_POINT('Ctrl Pts',(-1.48552434035628,228.315116541671,9.52547191390755));
#89768=CARTESIAN_POINT('Ctrl Pts',(1.97934846979805,228.046138520449,9.36671404867575));
#89769=CARTESIAN_POINT('Ctrl Pts',(3.63272163822919,224.989334645098,9.20795618344396));
#89770=CARTESIAN_POINT('Ctrl Pts',(1.96142810620627,221.942291702134,9.04919831821217));
#89771=CARTESIAN_POINT('Ctrl Pts',(-1.50496435148532,221.693663273135,8.89044045298037));
#89772=CARTESIAN_POINT('Ctrl Pts',(-3.59401349387884,224.470994086545,8.73168258774859));
#89773=CARTESIAN_POINT('Ctrl Pts',(-2.39382162800561,227.732471091145,8.57292472251679));
#89774=CARTESIAN_POINT('Ctrl Pts',(0.997195697683612,228.493190660582,8.41416685728499));
#89775=CARTESIAN_POINT('Ctrl Pts',(3.47557956006656,226.05694227482,8.25540899205321));
#89776=CARTESIAN_POINT('Ctrl Pts',(2.77311314575043,222.653380360706,8.09665112682141));
#89777=CARTESIAN_POINT('Ctrl Pts',(-0.467306310506461,221.397444648195,
7.93789326158963));
#89778=CARTESIAN_POINT('Ctrl Pts',(-3.28004704976421,223.43856745199,7.77913539635783));
#89779=CARTESIAN_POINT('Ctrl Pts',(-3.09088885806249,226.90871326232,7.62037753112604));
#89780=CARTESIAN_POINT('Ctrl Pts',(-0.0729493050082294,228.632004770035,
7.46161966589425));
#89781=CARTESIAN_POINT('Ctrl Pts',(3.01175344912091,227.031285655038,7.30286180066245));
#89782=CARTESIAN_POINT('Ctrl Pts',(3.3400995650489,223.571533988429,7.14410393543066));
#89783=CARTESIAN_POINT('Ctrl Pts',(0.611586690390379,221.419114359437,6.98534607019887));
#89784=CARTESIAN_POINT('Ctrl Pts',(-2.67665029926335,222.543921127873,6.82658820496707));
#89785=CARTESIAN_POINT('Ctrl Pts',(-3.51521704028799,225.916531183497,6.66783033973528));
#89786=CARTESIAN_POINT('Ctrl Pts',(-1.13665728427362,228.450331936026,6.50907247450349));
#89787=CARTESIAN_POINT('Ctrl Pts',(2.28217117361002,227.826389036385,6.3503146092717));
#89788=CARTESIAN_POINT('Ctrl Pts',(3.61235666314995,224.615735001789,6.1915567440399));
#89789=CARTESIAN_POINT('Ctrl Pts',(1.63651347662755,221.756760278445,6.03279887880811));
#89790=CARTESIAN_POINT('Ctrl Pts',(-1.83706677935009,221.865998420731,5.87404101357633));
#89791=CARTESIAN_POINT('Ctrl Pts',(-3.62936359110735,224.843474685122,5.71528314834452));
#89792=CARTESIAN_POINT('Ctrl Pts',(-2.1000669870046,227.964202911534,5.55652528311274));
#89793=CARTESIAN_POINT('Ctrl Pts',(1.35121084102199,228.372092749875,5.39776741788093));
#89794=CARTESIAN_POINT('Ctrl Pts',(3.56586056047961,225.693843436134,5.23900955264916));
#89795=CARTESIAN_POINT('Ctrl Pts',(2.51703483521181,222.380588636929,5.08025168741735));
#89796=CARTESIAN_POINT('Ctrl Pts',(-0.835381072264795,221.464619014198,
4.92149382218557));
#89797=CARTESIAN_POINT('Ctrl Pts',(-3.42325625524921,223.784229930654,4.76273595695377));
#89798=CARTESIAN_POINT('Ctrl Pts',(-2.87816744805807,227.216513566753,4.60397809172198));
#89799=CARTESIAN_POINT('Ctrl Pts',(0.301020094439488,228.620244073749,4.44522022649019));
#89800=CARTESIAN_POINT('Ctrl Pts',(3.20471405829287,226.710727346758,4.28646236125839));
#89801=CARTESIAN_POINT('Ctrl Pts',(3.17545384212145,223.235553019399,4.12770449602661));
#89802=CARTESIAN_POINT('Ctrl Pts',(0.24001839430402,221.375200499072,3.96894663079481));
#89803=CARTESIAN_POINT('Ctrl Pts',(-2.91508187811918,222.832264339917,3.81018876556302));
#89804=CARTESIAN_POINT('Ctrl Pts',(-3.40229933117922,226.273239770683,3.65143090033123));
#89805=CARTESIAN_POINT('Ctrl Pts',(-0.77573256839211,228.548946215303,3.49267303509943));
#89806=CARTESIAN_POINT('Ctrl Pts',(2.56078460694016,227.576657219349,3.33391516986764));
#89807=CARTESIAN_POINT('Ctrl Pts',(3.55367181789592,224.246211645467,3.17515730463585));
#89808=CARTESIAN_POINT('Ctrl Pts',(1.2942387062452,221.605633127976,3.01639943940405));
#89809=CARTESIAN_POINT('Ctrl Pts',(-2.14968158878668,222.071579070849,2.85764157417227));
#89810=CARTESIAN_POINT('Ctrl Pts',(-3.62621343857669,225.217615666778,2.69888370894047));
#89811=CARTESIAN_POINT('Ctrl Pts',(-1.78403476954297,228.164490547375,2.54012584370868));
#89812=CARTESIAN_POINT('Ctrl Pts',(1.69089220174611,228.21522353059,2.38136797847689));
#89813=CARTESIAN_POINT('Ctrl Pts',(3.61831520156474,225.323384619251,2.22261011324509));
#89814=CARTESIAN_POINT('Ctrl Pts',(2.23425524535826,222.135582991462,2.0638522480133));
#89815=CARTESIAN_POINT('Ctrl Pts',(-1.19459293999268,221.56929798347,1.90509438278151));
#89816=CARTESIAN_POINT('Ctrl Pts',(-3.53015394545888,224.142786682629,1.74633651754971));
#89817=CARTESIAN_POINT('Ctrl Pts',(-2.6349096037589,227.500806407321,1.58757865231793));
#89818=CARTESIAN_POINT('Ctrl Pts',(0.671786446474784,228.570069051027,1.42882078708613));
#89819=CARTESIAN_POINT('Ctrl Pts',(3.36369902404275,226.372043545379,1.27006292185434));
#89820=CARTESIAN_POINT('Ctrl Pts',(2.97708237215331,222.918244820821,1.11130505662255));
#89821=CARTESIAN_POINT('Ctrl Pts',(-0.134013682612229,221.369828849617,
0.952547191390754));
#89822=CARTESIAN_POINT('Ctrl Pts',(-3.12275749899671,223.143419393389,0.793789326158964));
#89823=CARTESIAN_POINT('Ctrl Pts',(-3.25295037801921,226.616814570914,0.635031460927171));
#89824=CARTESIAN_POINT('Ctrl Pts',(-0.407268936110244,228.609155678633,
0.476273595695376));
#89825=CARTESIAN_POINT('Ctrl Pts',(2.8136368462077,227.3011440524,0.317515730463589));
#89826=CARTESIAN_POINT('Ctrl Pts',(3.45438708523699,223.881452722834,0.158757865231792));
#89827=CARTESIAN_POINT('Ctrl Pts',(1.7810709486973,222.29471665351,0.0529192884105984));
#89828=CARTESIAN_POINT('Ctrl Pts',(0.793799282532894,222.030777046254,0.));
#89829=CARTESIAN_POINT('Ctrl Pts',(0.793799282532894,222.030777046254,0.));
#89830=CARTESIAN_POINT('Ctrl Pts',(0.886846191183898,222.064814021077,-1.38596869938627E-16));
#89831=CARTESIAN_POINT('Ctrl Pts',(0.977825993756427,222.103621402683,2.39308088689558E-15));
#89832=CARTESIAN_POINT('Ctrl Pts',(1.06653099078737,222.146870208338,1.49880108324396E-15));
#89833=CARTESIAN_POINT('Ctrl Pts',(1.1572090782491,222.191081009455,5.84629560049093E-16));
#89834=CARTESIAN_POINT('Ctrl Pts',(1.24551070332407,222.239933633085,-4.06870172435856E-15));
#89835=CARTESIAN_POINT('Ctrl Pts',(1.33118506358561,222.293122211572,-4.44089209850063E-15));
#89836=CARTESIAN_POINT('Ctrl Pts',(1.41411876188254,222.344609325192,-4.80117636679151E-15));
#89837=CARTESIAN_POINT('Ctrl Pts',(1.49459091967829,222.400160285979,-9.26260121771311E-16));
#89838=CARTESIAN_POINT('Ctrl Pts',(1.57234035477895,222.459528324875,-1.77635683940025E-15));
#89839=CARTESIAN_POINT('Ctrl Pts',(1.64037111049203,222.511475358909,-2.52019146732557E-15));
#89840=CARTESIAN_POINT('Ctrl Pts',(1.70631698504278,222.566345560034,-2.4936108625525E-15));
#89841=CARTESIAN_POINT('Ctrl Pts',(1.76997776289673,222.623986577848,-4.71844785465692E-15));
#89842=CARTESIAN_POINT('Ctrl Pts',(1.78334871497265,222.63609317335,-5.18574011530746E-15));
#89843=CARTESIAN_POINT('Ctrl Pts',(1.79662066694636,222.648323938157,-1.20584228596178E-15));
#89844=CARTESIAN_POINT('Ctrl Pts',(1.80977449464236,222.660661071479,-1.22124532708767E-15));
#89845=CARTESIAN_POINT('Ctrl Pts',(1.88220120936656,222.728590958986,-1.30605650838734E-15));
#89846=CARTESIAN_POINT('Ctrl Pts',(1.95116218959374,222.799842420315,8.00223029047533E-15));
#89847=CARTESIAN_POINT('Ctrl Pts',(2.01641813121821,222.874123957972,6.85562717706034E-15));
#89848=CARTESIAN_POINT('Ctrl Pts',(2.08131424640546,222.947995901339,5.71534652414354E-15));
#89849=CARTESIAN_POINT('Ctrl Pts',(2.14254655535901,223.024865395635,-1.30534801110875E-16));
#89850=CARTESIAN_POINT('Ctrl Pts',(2.19983607468768,223.104472485275,-8.32667268468867E-16));
#89851=CARTESIAN_POINT('Ctrl Pts',(2.25566842116609,223.182054749239,-1.51694082584268E-15));
#89852=CARTESIAN_POINT('Ctrl Pts',(2.30775626506218,223.262237857311,-5.95467361534588E-15));
#89853=CARTESIAN_POINT('Ctrl Pts',(2.35579457812553,223.344795283462,-8.90953977261688E-15));
#89854=CARTESIAN_POINT('Ctrl Pts',(2.37650832906487,223.380393410341,-1.01836553220135E-14));
#89855=CARTESIAN_POINT('Ctrl Pts',(2.39646854028631,223.416433103221,2.5576910520071E-15));
#89856=CARTESIAN_POINT('Ctrl Pts',(2.41564778277341,223.452896532503,3.02535774210355E-15));
#89857=CARTESIAN_POINT('Ctrl Pts',(2.42885130513818,223.477998968344,3.34731245987215E-15));
#89858=CARTESIAN_POINT('Ctrl Pts',(2.44168466279926,223.503302229722,-4.14100659545732E-15));
#89859=CARTESIAN_POINT('Ctrl Pts',(2.45413837672965,223.528800502852,-4.32986979603811E-15));
#89860=CARTESIAN_POINT('Ctrl Pts',(2.46035286582353,223.541524316901,-4.42411383494947E-15));
#89861=CARTESIAN_POINT('Ctrl Pts',(2.46647227743221,223.554295737379,2.15191029731381E-15));
#89862=CARTESIAN_POINT('Ctrl Pts',(2.47249022824328,223.56710248546,2.3037127760972E-15));
#89863=CARTESIAN_POINT('Ctrl Pts',(2.51269154441903,223.652654552092,3.31778876930894E-15));
#89864=CARTESIAN_POINT('Ctrl Pts',(2.5484363396718,223.739918159891,6.98524591958814E-16));
#89865=CARTESIAN_POINT('Ctrl Pts',(2.57947353285492,223.82865573719,2.77555756156289E-17));
#89866=CARTESIAN_POINT('Ctrl Pts',(2.60982487234774,223.915432409246,-6.28190921098164E-16));
#89867=CARTESIAN_POINT('Ctrl Pts',(2.63567458362555,224.003619302437,5.15344782426835E-15));
#89868=CARTESIAN_POINT('Ctrl Pts',(2.65673873200962,224.093003025007,6.60582699651968E-15));
#89869=CARTESIAN_POINT('Ctrl Pts',(2.66036635111496,224.108396483778,6.85595239145078E-15));
#89870=CARTESIAN_POINT('Ctrl Pts',(2.66385191074304,224.123825446915,3.8409637378969E-15));
#89871=CARTESIAN_POINT('Ctrl Pts',(2.66719380198884,224.13928882952,3.99680288865056E-15));
#89872=CARTESIAN_POINT('Ctrl Pts',(2.6873209483154,224.232419856686,4.90868829782107E-15));
#89873=CARTESIAN_POINT('Ctrl Pts',(2.70224094539991,224.326800411483,3.07486859462122E-15));
#89874=CARTESIAN_POINT('Ctrl Pts',(2.71203217769051,224.422021924685,4.13558076672871E-15));
#89875=CARTESIAN_POINT('Ctrl Pts',(2.71529423454605,224.453746020357,4.48896870709092E-15));
#89876=CARTESIAN_POINT('Ctrl Pts',(2.71798660578109,224.485563339469,2.05641129816516E-15));
#89877=CARTESIAN_POINT('Ctrl Pts',(2.72011099118565,224.517458314697,2.05391259555654E-15));
#89878=CARTESIAN_POINT('Ctrl Pts',(2.72133532130525,224.535840091728,2.05247253818413E-15));
#89879=CARTESIAN_POINT('Ctrl Pts',(2.7223709858767,224.554247656756,7.55656642889705E-15));
#89880=CARTESIAN_POINT('Ctrl Pts',(2.72321822484737,224.572677981456,8.13238365537927E-15));
#89881=CARTESIAN_POINT('Ctrl Pts',(2.72379251502994,224.585170743124,8.52269405370954E-15));
#89882=CARTESIAN_POINT('Ctrl Pts',(2.72428011160068,224.597672344381,8.79861093759093E-15));
#89883=CARTESIAN_POINT('Ctrl Pts',(2.72468096993961,224.610172448783,8.57647286522933E-15));
#89884=CARTESIAN_POINT('Ctrl Pts',(2.72766933700557,224.703359733888,6.92045118606972E-15));
#89885=CARTESIAN_POINT('Ctrl Pts',(2.72584870249446,224.796609966936,-5.66219201085476E-16));
#89886=CARTESIAN_POINT('Ctrl Pts',(2.71935795287165,224.889548302923,8.46545056276682E-16));
#89887=CARTESIAN_POINT('Ctrl Pts',(2.71285435385017,224.982670624088,2.2621060893908E-15));
#89888=CARTESIAN_POINT('Ctrl Pts',(2.70166174783478,225.07548079302,5.9470159394075E-15));
#89889=CARTESIAN_POINT('Ctrl Pts',(2.68586881074027,225.167589714791,5.89805981832114E-15));
#89890=CARTESIAN_POINT('Ctrl Pts',(2.67029892991559,225.258397708661,5.84979514365098E-15));
#89891=CARTESIAN_POINT('Ctrl Pts',(2.65025728119255,225.348524970524,1.95015538798884E-16));
#89892=CARTESIAN_POINT('Ctrl Pts',(2.62578579099026,225.437573501206,8.88178419700125E-16));
#89893=CARTESIAN_POINT('Ctrl Pts',(2.61627026001682,225.472199265507,1.15770891450574E-15));
#89894=CARTESIAN_POINT('Ctrl Pts',(2.60608451887964,225.506661589206,3.62406394873002E-15));
#89895=CARTESIAN_POINT('Ctrl Pts',(2.59522946518981,225.540935610117,4.08006961549745E-15));
#89896=CARTESIAN_POINT('Ctrl Pts',(2.58886805642713,225.561021282946,4.34730352583022E-15));
#89897=CARTESIAN_POINT('Ctrl Pts',(2.58227676746916,225.581042269272,7.67942111821871E-15));
#89898=CARTESIAN_POINT('Ctrl Pts',(2.57545564888798,225.600993409454,8.14626144318709E-15));
#89899=CARTESIAN_POINT('Ctrl Pts',(2.57042451361342,225.615709014225,8.49059453145984E-15));
#89900=CARTESIAN_POINT('Ctrl Pts',(2.56526853205797,225.630385839234,1.02262120206335E-15));
#89901=CARTESIAN_POINT('Ctrl Pts',(2.5599923386753,225.645009655912,1.77635683940025E-15));
#89902=CARTESIAN_POINT('Ctrl Pts',(2.52758850675101,225.73482207622,6.40543715094128E-15));
#89903=CARTESIAN_POINT('Ctrl Pts',(2.4906131496606,225.822761175715,9.4868431892647E-15));
#89904=CARTESIAN_POINT('Ctrl Pts',(2.44913842341953,225.90838531885,8.70137295549966E-15));
#89905=CARTESIAN_POINT('Ctrl Pts',(2.41803237873873,225.972603426202,8.11227028017589E-15));
#89906=CARTESIAN_POINT('Ctrl Pts',(2.38439430103246,226.035518835997,2.83514090577719E-15));
#89907=CARTESIAN_POINT('Ctrl Pts',(2.34823741362777,226.09692820208,3.10862446895044E-15));
#89908=CARTESIAN_POINT('Ctrl Pts',(2.33712251184633,226.115805907587,3.19269539323893E-15));
#89909=CARTESIAN_POINT('Ctrl Pts',(2.32576948659689,226.134541170905,6.20229766951161E-15));
#89910=CARTESIAN_POINT('Ctrl Pts',(2.31417847054799,226.153127742234,6.19643225618915E-15));
#89911=CARTESIAN_POINT('Ctrl Pts',(2.30318790659673,226.17075146909,6.19087069023592E-15));
#89912=CARTESIAN_POINT('Ctrl Pts',(2.29198235378028,226.18824280901,8.27692394682741E-16));
#89913=CARTESIAN_POINT('Ctrl Pts',(2.28057388545861,226.205578703977,1.50573997714787E-15));
#89914=CARTESIAN_POINT('Ctrl Pts',(2.23335304213644,226.277333785992,4.31224982174617E-15));
#89915=CARTESIAN_POINT('Ctrl Pts',(2.18261517567617,226.346499716342,-4.49298739505873E-15));
#89916=CARTESIAN_POINT('Ctrl Pts',(2.12839610130427,226.412725093439,-3.25087179398054E-15));
#89917=CARTESIAN_POINT('Ctrl Pts',(2.0747094208182,226.478300183044,-2.02095291073937E-15));
#89918=CARTESIAN_POINT('Ctrl Pts',(2.0176092036947,226.54099277136,5.93088889512619E-15));
#89919=CARTESIAN_POINT('Ctrl Pts',(1.95710209621334,226.600419913581,4.67247768254353E-15));
#89920=CARTESIAN_POINT('Ctrl Pts',(1.9439378552628,226.613349191673,4.39195893259633E-15));
#89921=CARTESIAN_POINT('Ctrl Pts',(1.93061225296776,226.626123721938,9.20546864075757E-16));
#89922=CARTESIAN_POINT('Ctrl Pts',(1.91712867315962,226.638742108209,9.43689570931383E-16));
#89923=CARTESIAN_POINT('Ctrl Pts',(-2.51944987787367,224.998011234297,18.387416697508));
#89924=CARTESIAN_POINT('Ctrl Pts',(-2.52058777238211,224.866459872146,18.3957515808994));
#89925=CARTESIAN_POINT('Ctrl Pts',(-2.51117357035687,224.735071803788,18.4040864642907));
#89926=CARTESIAN_POINT('Ctrl Pts',(-2.49063889193878,224.605445490309,18.4124213476821));
#89927=CARTESIAN_POINT('Ctrl Pts',(-2.36026147469096,223.782430704556,18.4653406360927));
#89928=CARTESIAN_POINT('Ctrl Pts',(-1.78160099775816,223.030434896711,18.5182599245033));
#89929=CARTESIAN_POINT('Ctrl Pts',(-1.01945102078794,222.693560709822,18.5711792129139));
#89930=CARTESIAN_POINT('Ctrl Pts',(-0.257301043817723,222.356686522933,
18.6240985013245));
#89931=CARTESIAN_POINT('Ctrl Pts',(0.688338433189915,222.434933957,18.6770177897351));
#89932=CARTESIAN_POINT('Ctrl Pts',(1.3847398322567,222.892518565437,18.7299370781457));
#89933=CARTESIAN_POINT('Ctrl Pts',(2.08114123132348,223.350103173874,18.7828563665563));
#89934=CARTESIAN_POINT('Ctrl Pts',(2.5283045524494,224.187024956681,18.8357756549668));
#89935=CARTESIAN_POINT('Ctrl Pts',(2.5216139047758,225.020264696752,18.8886949433774));
#89936=CARTESIAN_POINT('Ctrl Pts',(2.51492325710221,225.853504436823,18.941614231788));
#89937=CARTESIAN_POINT('Ctrl Pts',(2.05437864062909,226.683062134158,18.9945335201987));
#89938=CARTESIAN_POINT('Ctrl Pts',(1.3507130032366,227.129421216121,19.0474528086093));
#89939=CARTESIAN_POINT('Ctrl Pts',(0.647047365844105,227.575780298084,19.1003720970199));
#89940=CARTESIAN_POINT('Ctrl Pts',(-0.299739292467768,227.638940764676,
19.1532913854304));
#89941=CARTESIAN_POINT('Ctrl Pts',(-1.05637251833031,227.289819588766,19.206210673841));
#89942=CARTESIAN_POINT('Ctrl Pts',(-1.81300574419286,226.940698412856,19.2591299622516));
#89943=CARTESIAN_POINT('Ctrl Pts',(-2.37948553760609,226.179295594445,19.3120492506622));
#89944=CARTESIAN_POINT('Ctrl Pts',(-2.49664129736409,225.354396351653,19.3649685390728));
#89945=CARTESIAN_POINT('Ctrl Pts',(-2.51320697146662,225.237756657184,19.3724512585512));
#89946=CARTESIAN_POINT('Ctrl Pts',(-2.52078904185958,225.119847440786,19.3799339780296));
#89947=CARTESIAN_POINT('Ctrl Pts',(-2.51981693572124,225.001815876221,19.387416697508));
#89948=CARTESIAN_POINT('Ctrl Pts',(-0.793799282532863,222.030777046254,
20.));
#89949=CARTESIAN_POINT('Ctrl Pts',(-1.78107094869726,222.29471665351,19.9470807115894));
#89950=CARTESIAN_POINT('Ctrl Pts',(-3.45438749280176,223.881450010451,19.8412421347682));
#89951=CARTESIAN_POINT('Ctrl Pts',(-2.81363649299402,227.301144948027,19.6824842695364));
#89952=CARTESIAN_POINT('Ctrl Pts',(0.407268901123991,228.609154817042,19.5237264043046));
#89953=CARTESIAN_POINT('Ctrl Pts',(3.25295011294267,226.616814793291,19.3649685390728));
#89954=CARTESIAN_POINT('Ctrl Pts',(3.12275731293263,223.14341933887,19.206210673841));
#89955=CARTESIAN_POINT('Ctrl Pts',(0.134013646578404,221.369829208712,19.0474528086092));
#89956=CARTESIAN_POINT('Ctrl Pts',(-2.97708214348246,222.918244913477,18.8886949433774));
#89957=CARTESIAN_POINT('Ctrl Pts',(-3.36369879634767,226.37204347757,18.7299370781457));
#89958=CARTESIAN_POINT('Ctrl Pts',(-0.671786392406203,228.570068782136,
18.5711792129139));
#89959=CARTESIAN_POINT('Ctrl Pts',(2.6349094131999,227.500806238298,18.4124213476821));
#89960=CARTESIAN_POINT('Ctrl Pts',(3.53015369719777,224.142786739032,18.2536634824503));
#89961=CARTESIAN_POINT('Ctrl Pts',(1.19459285411968,221.569298229067,18.0949056172185));
#89962=CARTESIAN_POINT('Ctrl Pts',(-2.23425508627908,222.135583193393,17.9361477519867));
#89963=CARTESIAN_POINT('Ctrl Pts',(-3.61831494530944,225.323384596945,17.7773898867549));
#89964=CARTESIAN_POINT('Ctrl Pts',(-1.69089208164927,228.215223302252,17.6186320215231));
#89965=CARTESIAN_POINT('Ctrl Pts',(1.7840346429268,228.164490323129,17.4598741562913));
#89966=CARTESIAN_POINT('Ctrl Pts',(3.6262131814702,225.217615651258,17.3011162910595));
#89967=CARTESIAN_POINT('Ctrl Pts',(2.14968143631101,222.071579278568,17.1423584258277));
#89968=CARTESIAN_POINT('Ctrl Pts',(-1.29423861444767,221.60563336867,16.9836005605959));
#89969=CARTESIAN_POINT('Ctrl Pts',(-3.55367156588917,224.246211698934,16.8248426953642));
#89970=CARTESIAN_POINT('Ctrl Pts',(-2.56078442533408,227.576657036616,16.6660848301324));
#89971=CARTESIAN_POINT('Ctrl Pts',(0.77573251337774,228.548945963627,16.5073269649006));
#89972=CARTESIAN_POINT('Ctrl Pts',(3.40229908990077,226.273239680388,16.3485690996688));
#89973=CARTESIAN_POINT('Ctrl Pts',(2.91508167139093,222.832264493646,16.189811234437));
#89974=CARTESIAN_POINT('Ctrl Pts',(-0.24001837728243,221.37520075613,16.0310533692052));
#89975=CARTESIAN_POINT('Ctrl Pts',(-3.17545361692919,223.235553144528,15.8722955039734));
#89976=CARTESIAN_POINT('Ctrl Pts',(-3.20471383102538,226.710727225439,15.7135376387416));
#89977=CARTESIAN_POINT('Ctrl Pts',(-0.301020073092202,228.620243817014,
15.5547797735098));
#89978=CARTESIAN_POINT('Ctrl Pts',(2.87816724394823,227.216513409565,15.396021908278));
#89979=CARTESIAN_POINT('Ctrl Pts',(3.4232560124835,223.784230016872,15.2372640430462));
#89980=CARTESIAN_POINT('Ctrl Pts',(0.835381013022407,221.464619264915,15.0785061778144));
#89981=CARTESIAN_POINT('Ctrl Pts',(-2.51703465671226,222.380588822689,14.9197483125826));
#89982=CARTESIAN_POINT('Ctrl Pts',(-3.56586030760089,225.693843386929,14.7609904473508));
#89983=CARTESIAN_POINT('Ctrl Pts',(-1.35121074519871,228.372092510738,14.6022325821191));
#89984=CARTESIAN_POINT('Ctrl Pts',(2.10006683807499,227.964202701323,14.4434747168873));
#89985=CARTESIAN_POINT('Ctrl Pts',(3.62936333372522,224.843474696222,14.2847168516555));
#89986=CARTESIAN_POINT('Ctrl Pts',(1.83706664907154,221.865998642983,14.1259589864237));
#89987=CARTESIAN_POINT('Ctrl Pts',(-1.6365133605716,221.756760508445,13.9672011211919));
#89988=CARTESIAN_POINT('Ctrl Pts',(-3.61235640697389,224.61573502904,13.8084432559601));
#89989=CARTESIAN_POINT('Ctrl Pts',(-2.2821710117662,227.826388835947,13.6496853907283));
#89990=CARTESIAN_POINT('Ctrl Pts',(1.13665720366575,228.45033169134,13.4909275254965));
#89991=CARTESIAN_POINT('Ctrl Pts',(3.51521679100075,225.9165311185,13.3321696602647));
#89992=CARTESIAN_POINT('Ctrl Pts',(2.6766501094444,222.54392130205,13.1734117950329));
#89993=CARTESIAN_POINT('Ctrl Pts',(-0.611586647018769,221.419114613381,
13.0146539298011));
#89994=CARTESIAN_POINT('Ctrl Pts',(-3.3400993281804,223.571534089731,12.8558960645693));
#89995=CARTESIAN_POINT('Ctrl Pts',(-3.01175323553757,227.031285510986,12.6971381993375));
#89996=CARTESIAN_POINT('Ctrl Pts',(0.0729492998349137,228.632004512465,
12.5383803341058));
#89997=CARTESIAN_POINT('Ctrl Pts',(3.09088863886716,226.908713126961,12.3796224688739));
#89998=CARTESIAN_POINT('Ctrl Pts',(3.28004681715442,223.438567562721,12.2208646036422));
#89999=CARTESIAN_POINT('Ctrl Pts',(0.46730627736665,221.397444903677,12.0621067384104));
#90000=CARTESIAN_POINT('Ctrl Pts',(-2.7731129490907,222.65338052712,11.9033488731786));
#90001=CARTESIAN_POINT('Ctrl Pts',(-3.47557931359025,226.056942199865,11.7445910079468));
#90002=CARTESIAN_POINT('Ctrl Pts',(-0.997195626965866,228.493190412856,
11.585833142715));
#90003=CARTESIAN_POINT('Ctrl Pts',(2.39382145824392,227.732470897368,11.4270752774832));
#90004=CARTESIAN_POINT('Ctrl Pts',(3.59401323900362,224.47099412406,11.2683174122514));
#90005=CARTESIAN_POINT('Ctrl Pts',(1.50496424475834,221.69366350761,11.1095595470196));
#90006=CARTESIAN_POINT('Ctrl Pts',(-1.9614279671085,221.942291918976,10.9508016817878));
#90007=CARTESIAN_POINT('Ctrl Pts',(-3.6327213806089,224.989334645854,10.792043816556));
#90008=CARTESIAN_POINT('Ctrl Pts',(-1.97934832942936,228.046138304427,10.6332859513243));
#90009=CARTESIAN_POINT('Ctrl Pts',(1.48552423500794,228.315116306574,10.4745280860925));
#90010=CARTESIAN_POINT('Ctrl Pts',(3.59084507798282,225.550099995309,10.3157702208607));
#90011=CARTESIAN_POINT('Ctrl Pts',(2.40982464679436,222.281632189969,10.1570123556289));
#90012=CARTESIAN_POINT('Ctrl Pts',(-0.976667206376252,221.501014497472,
9.99825449039707));
#90013=CARTESIAN_POINT('Ctrl Pts',(-3.4693132706778,223.922668199295,9.83949662516529));
#90014=CARTESIAN_POINT('Ctrl Pts',(-2.78684396608248,227.330295922758,9.68073875993348));
#90015=CARTESIAN_POINT('Ctrl Pts',(0.446144826681538,228.60523690935,9.5219808947017));
#90016=CARTESIAN_POINT('Ctrl Pts',(3.27082189161085,226.580665218277,9.36322302946991));
#90017=CARTESIAN_POINT('Ctrl Pts',(3.10204288995985,223.109468781596,9.20446516423812));
#90018=CARTESIAN_POINT('Ctrl Pts',(0.094274357402458,221.368486441654,9.04570729900631));
#90019=CARTESIAN_POINT('Ctrl Pts',(-2.9997740633424,222.951065167505,8.88694943377453));
#90020=CARTESIAN_POINT('Ctrl Pts',(-3.34842937927955,226.408828971483,8.72819156854274));
#90021=CARTESIAN_POINT('Ctrl Pts',(-0.632602258973873,228.57723255616,8.56943370331094));
#90022=CARTESIAN_POINT('Ctrl Pts',(2.66218242386824,227.471753046111,8.41067583807915));
#90023=CARTESIAN_POINT('Ctrl Pts',(3.52053785707391,224.10412524546,8.25191797284736));
#90024=CARTESIAN_POINT('Ctrl Pts',(1.15689718192732,221.556401984935,8.09316010761557));
#90025=CARTESIAN_POINT('Ctrl Pts',(-2.26553574862528,222.160259492381,7.93440224238377));
#90026=CARTESIAN_POINT('Ctrl Pts',(-3.61455045112604,225.36304740073,7.77564437715198));
#90027=CARTESIAN_POINT('Ctrl Pts',(-1.65552872289502,228.233574342207,7.61688651192019));
#90028=CARTESIAN_POINT('Ctrl Pts',(1.81863282742744,228.144734172854,7.4581286466884));
#90029=CARTESIAN_POINT('Ctrl Pts',(3.62838168560431,225.177833412168,7.2993707814566));
#90030=CARTESIAN_POINT('Ctrl Pts',(2.11743576779875,222.048179519659,7.14061291622482));
#90031=CARTESIAN_POINT('Ctrl Pts',(-1.33138728143009,221.620031614681,6.98185505099302));
#90032=CARTESIAN_POINT('Ctrl Pts',(-3.56172474304964,224.285230643032,6.82309718576122));
#90033=CARTESIAN_POINT('Ctrl Pts',(-2.53237185989158,227.604586558773,6.66433932052944));
#90034=CARTESIAN_POINT('Ctrl Pts',(0.814607649856128,228.540224958348,6.50558145529764));
#90035=CARTESIAN_POINT('Ctrl Pts',(3.41605827048919,226.235849615258,6.34682359006585));
#90036=CARTESIAN_POINT('Ctrl Pts',(2.89113249630378,222.800424752883,6.18806572483406));
#90037=CARTESIAN_POINT('Ctrl Pts',(-0.279757624807835,221.378051070173,
6.02930785960226));
#90038=CARTESIAN_POINT('Ctrl Pts',(-3.19461357869652,223.270484905611,5.87054999437047));
#90039=CARTESIAN_POINT('Ctrl Pts',(-3.18575931098727,226.745770887422,5.71179212913868));
#90040=CARTESIAN_POINT('Ctrl Pts',(-0.261298247139434,228.623327421715,
5.55303426390689));
#90041=CARTESIAN_POINT('Ctrl Pts',(2.9023029622151,227.184814842139,5.39427639867509));
#90042=CARTESIAN_POINT('Ctrl Pts',(3.40971661468071,223.746759804953,5.2355185334433));
#90043=CARTESIAN_POINT('Ctrl Pts',(0.796557755474301,221.455670144991,5.07676066821152));
#90044=CARTESIAN_POINT('Ctrl Pts',(-2.54561073021817,222.408351028957,4.91800280297971));
#90045=CARTESIAN_POINT('Ctrl Pts',(-3.55803637571897,225.732908949305,4.75924493774792));
#90046=CARTESIAN_POINT('Ctrl Pts',(-1.31414727007755,228.386708628075,4.60048707251613));
#90047=CARTESIAN_POINT('Ctrl Pts',(2.13244936546002,227.9409927036,4.44172920728434));
#90048=CARTESIAN_POINT('Ctrl Pts',(3.62742842558762,224.80368037246,4.28297134205255));
#90049=CARTESIAN_POINT('Ctrl Pts',(1.80258513325755,221.846039756688,4.12421347682075));
#90050=CARTESIAN_POINT('Ctrl Pts',(-1.67198400213467,221.774903431643,3.96545561158896));
#90051=CARTESIAN_POINT('Ctrl Pts',(-3.61635344454317,224.655375358983,3.80669774635717));
#90052=CARTESIAN_POINT('Ctrl Pts',(-2.25103635667323,227.851247744537,3.64793988112538));
#90053=CARTESIAN_POINT('Ctrl Pts',(1.17442911621855,228.437658305789,3.48918201589358));
#90054=CARTESIAN_POINT('Ctrl Pts',(3.52505710830432,225.877924122033,3.33042415066179));
#90055=CARTESIAN_POINT('Ctrl Pts',(2.64955297313634,222.514713813743,3.17166628543));
#90056=CARTESIAN_POINT('Ctrl Pts',(-0.650821938137665,221.426037330607,
3.01290842019821));
#90057=CARTESIAN_POINT('Ctrl Pts',(-3.35556463867761,223.60825133135,2.85415055496642));
#90058=CARTESIAN_POINT('Ctrl Pts',(-2.98929471089608,227.064193680453,2.69539268973462));
#90059=CARTESIAN_POINT('Ctrl Pts',(0.112777612738978,228.630986010631,2.53663482450283));
#90060=CARTESIAN_POINT('Ctrl Pts',(3.11163588183028,226.874700175507,2.37787695927104));
#90061=CARTESIAN_POINT('Ctrl Pts',(3.26272508945618,223.402688633055,2.21911909403925));
#90062=CARTESIAN_POINT('Ctrl Pts',(0.42776847383237,221.392536757232,2.06036122880745));
#90063=CARTESIAN_POINT('Ctrl Pts',(-2.7986819344071,222.683934355202,1.90160336357566));
#90064=CARTESIAN_POINT('Ctrl Pts',(-3.46377853880955,226.09499665142,1.74284549834387));
#90065=CARTESIAN_POINT('Ctrl Pts',(-0.958825582149559,228.5039149863,1.58408763311207));
#90066=CARTESIAN_POINT('Ctrl Pts',(2.42364536547895,227.706056696193,1.42532976788028));
#90067=CARTESIAN_POINT('Ctrl Pts',(3.58799443175235,224.431602766551,1.26657190264849));
#90068=CARTESIAN_POINT('Ctrl Pts',(1.46861466513916,221.677371668161,1.1078140374167));
#90069=CARTESIAN_POINT('Ctrl Pts',(-1.99484835403995,221.963957684538,0.949056172184904));
#90070=CARTESIAN_POINT('Ctrl Pts',(-3.63261167939862,225.029235526384,0.790298306953113));
#90071=CARTESIAN_POINT('Ctrl Pts',(-1.94583850483642,228.067541710309,0.631540441721317));
#90072=CARTESIAN_POINT('Ctrl Pts',(1.52182603612892,228.298871095165,0.472782576489527));
#90073=CARTESIAN_POINT('Ctrl Pts',(3.59659353011021,225.51018574291,0.314024711257735));
#90074=CARTESIAN_POINT('Ctrl Pts',(2.38000618637172,222.256382496769,0.155266846025939));
#90075=CARTESIAN_POINT('Ctrl Pts',(-1.01525930202285,221.509861473209,-0.00349101920584771));
#90076=CARTESIAN_POINT('Ctrl Pts',(-3.48036060104862,223.965090769095,-0.162248884437644));
#90077=CARTESIAN_POINT('Ctrl Pts',(-3.00016881161633,226.220556762668,-0.268087461258838));
#90078=CARTESIAN_POINT('Ctrl Pts',(-2.33606265769611,226.997301556931,-0.321006749669435));
#90079=CARTESIAN_POINT('Ctrl Pts',(-0.745932854346946,222.209822430158,
20.1070022498898));
#90080=CARTESIAN_POINT('Ctrl Pts',(-1.67367162680846,222.457846368889,20.0540829614792));
#90081=CARTESIAN_POINT('Ctrl Pts',(-3.24608648461372,223.948899041869,19.948244384658));
#90082=CARTESIAN_POINT('Ctrl Pts',(-2.64397303763859,227.162384946822,19.7894865194262));
#90083=CARTESIAN_POINT('Ctrl Pts',(0.382710416331961,228.39152127458,19.6307286541944));
#90084=CARTESIAN_POINT('Ctrl Pts',(3.05679586286989,226.519320186158,19.4719707889626));
#90085=CARTESIAN_POINT('Ctrl Pts',(2.93445374306217,223.255371927948,19.3132129237308));
#90086=CARTESIAN_POINT('Ctrl Pts',(0.125932567732614,221.588730023197,19.1544550584991));
#90087=CARTESIAN_POINT('Ctrl Pts',(-2.79756284715621,223.043775614427,18.9956971932672));
#90088=CARTESIAN_POINT('Ctrl Pts',(-3.16086635442269,226.289308682979,18.8369393280355));
#90089=CARTESIAN_POINT('Ctrl Pts',(-0.631277392441138,228.354792143898,
18.6781814628037));
#90090=CARTESIAN_POINT('Ctrl Pts',(2.47602327538317,227.350006577922,18.5194235975719));
#90091=CARTESIAN_POINT('Ctrl Pts',(3.31728395524864,224.194477056596,18.3606657323401));
#90092=CARTESIAN_POINT('Ctrl Pts',(1.12255840621658,221.776170978336,18.2019078671083));
#90093=CARTESIAN_POINT('Ctrl Pts',(-2.09952857166804,222.308308722862,18.0431500018765));
#90094=CARTESIAN_POINT('Ctrl Pts',(-3.40012904328763,225.30388437072,17.8843921366447));
#90095=CARTESIAN_POINT('Ctrl Pts',(-1.58893058309745,228.021343994616,17.7256342714129));
#90096=CARTESIAN_POINT('Ctrl Pts',(1.67645660903848,227.973670235318,17.5668764061811));
#90097=CARTESIAN_POINT('Ctrl Pts',(3.40755101251001,225.204493336622,17.4081185409494));
#90098=CARTESIAN_POINT('Ctrl Pts',(2.02005474810658,222.248164270826,17.2493606757175));
#90099=CARTESIAN_POINT('Ctrl Pts',(-1.21619548558992,221.81031509385,17.0906028104858));
#90100=CARTESIAN_POINT('Ctrl Pts',(-3.33938368663811,224.291665448231,16.931844945254));
#90101=CARTESIAN_POINT('Ctrl Pts',(-2.40636805523639,227.42128354143,16.7730870800222));
#90102=CARTESIAN_POINT('Ctrl Pts',(0.728955518915619,228.334943040165,16.6143292147904));
#90103=CARTESIAN_POINT('Ctrl Pts',(3.19713903415707,226.196462796022,16.4555713495586));
#90104=CARTESIAN_POINT('Ctrl Pts',(2.73930102941996,222.962979849813,16.2968134843268));
#90105=CARTESIAN_POINT('Ctrl Pts',(-0.225545168913144,221.593777664063,
16.138055619095));
#90106=CARTESIAN_POINT('Ctrl Pts',(-2.98397243792452,223.341950026654,15.9792977538632));
#90107=CARTESIAN_POINT('Ctrl Pts',(-3.01146824889316,226.607569659434,15.8205398886314));
#90108=CARTESIAN_POINT('Ctrl Pts',(-0.282868436994453,228.401941603223,
15.6617820233996));
#90109=CARTESIAN_POINT('Ctrl Pts',(2.7046125573656,227.082856725468,15.5030241581678));
#90110=CARTESIAN_POINT('Ctrl Pts',(3.21683224555754,223.857541454497,15.344266292936));
#90111=CARTESIAN_POINT('Ctrl Pts',(0.785007189125602,221.677804199431,15.1855084277042));
#90112=CARTESIAN_POINT('Ctrl Pts',(-2.36525641593009,222.538540410411,15.0267505624725));
#90113=CARTESIAN_POINT('Ctrl Pts',(-3.35083744213523,225.652004340984,14.8679926972406));
#90114=CARTESIAN_POINT('Ctrl Pts',(-1.26973217306808,228.168753924331,14.7092348320089));
#90115=CARTESIAN_POINT('Ctrl Pts',(1.97343193086066,227.785460040736,14.5504769667771));
#90116=CARTESIAN_POINT('Ctrl Pts',(3.41051120926871,224.852913237397,14.3917191015453));
#90117=CARTESIAN_POINT('Ctrl Pts',(1.72629076306928,222.054980233407,14.2329612363135));
#90118=CARTESIAN_POINT('Ctrl Pts',(-1.53783092160648,221.952329203993,14.0742033710817));
#90119=CARTESIAN_POINT('Ctrl Pts',(-3.3945298073017,224.638906367238,13.9154455058499));
#90120=CARTESIAN_POINT('Ctrl Pts',(-2.14455514684108,227.655956408987,13.7566876406181));
#90121=CARTESIAN_POINT('Ctrl Pts',(1.06811629967593,228.242275249674,13.5979297753863));
#90122=CARTESIAN_POINT('Ctrl Pts',(3.30324775073217,225.861263909359,13.4391719101545));
#90123=CARTESIAN_POINT('Ctrl Pts',(2.51524699021539,222.692023873067,13.2804140449227));
#90124=CARTESIAN_POINT('Ctrl Pts',(-0.574707716836846,221.635043497385,
13.1216561796909));
#90125=CARTESIAN_POINT('Ctrl Pts',(-3.13868994403982,223.657671180573,12.9628983144591));
#90126=CARTESIAN_POINT('Ctrl Pts',(-2.83014325788355,226.908798146515,12.8041404492274));
#90127=CARTESIAN_POINT('Ctrl Pts',(0.068550426595048,228.412993123827,12.6453825839956));
#90128=CARTESIAN_POINT('Ctrl Pts',(2.90450676334955,226.793616928427,12.4866247187638));
#90129=CARTESIAN_POINT('Ctrl Pts',(3.08225862450349,223.532722590661,12.327866853532));
#90130=CARTESIAN_POINT('Ctrl Pts',(0.439127513718703,221.614680480224,12.1691089883002));
#90131=CARTESIAN_POINT('Ctrl Pts',(-2.60589308035317,222.794882661161,12.0103511230684));
#90132=CARTESIAN_POINT('Ctrl Pts',(-3.26600042976007,225.993208143889,11.8515932578366));
#90133=CARTESIAN_POINT('Ctrl Pts',(-0.937064314282925,228.282549572387,
11.6928353926048));
#90134=CARTESIAN_POINT('Ctrl Pts',(2.2494730247768,227.567701761319,11.534077527373));
#90135=CARTESIAN_POINT('Ctrl Pts',(3.37729274001918,224.502893399264,11.3753196621412));
#90136=CARTESIAN_POINT('Ctrl Pts',(1.41421427240481,221.893036978655,11.2165617969094));
#90137=CARTESIAN_POINT('Ctrl Pts',(-1.84315304170182,222.126672993002,11.0578039316776));
#90138=CARTESIAN_POINT('Ctrl Pts',(-3.41366676452317,224.989977771163,10.8990460664458));
#90139=CARTESIAN_POINT('Ctrl Pts',(-1.85999279869212,227.862454892762,10.7402882012141));
#90140=CARTESIAN_POINT('Ctrl Pts',(1.39594650335951,228.115213409068,10.5815303359823));
#90141=CARTESIAN_POINT('Ctrl Pts',(3.37431562043079,225.516928735899,10.4227724707505));
#90142=CARTESIAN_POINT('Ctrl Pts',(2.26451121437554,222.445550903962,10.2640146055187));
#90143=CARTESIAN_POINT('Ctrl Pts',(-0.91777376602647,221.712004784268,10.1052567402869));
#90144=CARTESIAN_POINT('Ctrl Pts',(-3.26011223185162,223.987631756715,9.9464988750551));
#90145=CARTESIAN_POINT('Ctrl Pts',(-2.61879611128699,227.189778105605,9.7877410098233));
#90146=CARTESIAN_POINT('Ctrl Pts',(0.419242107345829,228.387839618357,9.62898314459151));
#90147=CARTESIAN_POINT('Ctrl Pts',(3.07358996582205,226.485350445612,9.47022527935971));
#90148=CARTESIAN_POINT('Ctrl Pts',(2.91498840844391,223.223468603453,9.31146741412792));
#90149=CARTESIAN_POINT('Ctrl Pts',(0.0885895742870307,221.587468225553,
9.15270954889613));
#90150=CARTESIAN_POINT('Ctrl Pts',(-2.81888643477362,223.074616793433,8.99395168366434));
#90151=CARTESIAN_POINT('Ctrl Pts',(-3.14651768957949,226.323875996249,8.83519381843255));
#90152=CARTESIAN_POINT('Ctrl Pts',(-0.594456078616027,228.361523939358,
8.67643595320075));
#90153=CARTESIAN_POINT('Ctrl Pts',(2.50165171212042,227.322705305355,8.51767808796897));
#90154=CARTESIAN_POINT('Ctrl Pts',(3.30824795429932,224.158146867229,8.35892022273716));
#90155=CARTESIAN_POINT('Ctrl Pts',(1.08713579879716,221.76405238311,8.20016235750538));
#90156=CARTESIAN_POINT('Ctrl Pts',(-2.12892299701359,222.331497030718,8.04140449227358));
#90157=CARTESIAN_POINT('Ctrl Pts',(-3.39659154967535,225.341155490876,7.88264662704179));
#90158=CARTESIAN_POINT('Ctrl Pts',(-1.55569964964197,228.0385884592,7.72388876181));
#90159=CARTESIAN_POINT('Ctrl Pts',(1.70896850856733,227.955105389154,7.5651308965782));
#90160=CARTESIAN_POINT('Ctrl Pts',(3.40958875493938,225.167109983161,7.40637303134642));
#90161=CARTESIAN_POINT('Ctrl Pts',(1.98975350686972,222.22617552715,7.24761516611462));
#90162=CARTESIAN_POINT('Ctrl Pts',(-1.25110407244195,221.823845119614,7.08885730088283));
#90163=CARTESIAN_POINT('Ctrl Pts',(-3.34695125385322,224.328331533708,6.93009943565103));
#90164=CARTESIAN_POINT('Ctrl Pts',(-2.37966877935368,227.447528901739,6.77134157041924));
#90165=CARTESIAN_POINT('Ctrl Pts',(0.765486468432129,228.326747915146,6.61258370518745));
#90166=CARTESIAN_POINT('Ctrl Pts',(3.21006853041089,226.161327367432,6.45382583995566));
#90167=CARTESIAN_POINT('Ctrl Pts',(2.71679599959049,222.933060058712,6.29506797472387));
#90168=CARTESIAN_POINT('Ctrl Pts',(-0.26288812321973,221.596456102979,6.13631010949208));
#90169=CARTESIAN_POINT('Ctrl Pts',(-3.00197704599707,223.374775387958,5.97755224426028));
#90170=CARTESIAN_POINT('Ctrl Pts',(-2.99365669432777,226.640500173968,5.81879437902849));
#90171=CARTESIAN_POINT('Ctrl Pts',(-0.245541853732399,228.404839265273,
5.66003651379669));
#90172=CARTESIAN_POINT('Ctrl Pts',(2.72729288174315,227.053069594893,5.50127864856491));
#90173=CARTESIAN_POINT('Ctrl Pts',(3.2041092790956,223.822330712001,5.34252078333311));
#90174=CARTESIAN_POINT('Ctrl Pts',(0.748524990218216,221.669394715176,5.18376291810132));
#90175=CARTESIAN_POINT('Ctrl Pts',(-2.39210934027172,222.564628544048,5.02500505286953));
#90176=CARTESIAN_POINT('Ctrl Pts',(-3.34348529661266,225.688714233638,4.86624718763773));
#90177=CARTESIAN_POINT('Ctrl Pts',(-1.2349036409725,228.182488683689,4.70748932240594));
#90178=CARTESIAN_POINT('Ctrl Pts',(2.00386177832312,227.763649615568,4.54873145717415));
#90179=CARTESIAN_POINT('Ctrl Pts',(3.40869297689972,224.815518527974,4.38997359194236));
#90180=CARTESIAN_POINT('Ctrl Pts',(1.69388849705656,222.036224876289,4.23121572671056));
#90181=CARTESIAN_POINT('Ctrl Pts',(-1.57116266867262,221.969378101347,4.07245786147877));
#90182=CARTESIAN_POINT('Ctrl Pts',(-3.39828582183659,224.676156368734,3.91369999624698));
#90183=CARTESIAN_POINT('Ctrl Pts',(-2.11529792445043,227.679316315009,3.75494213101518));
#90184=CARTESIAN_POINT('Ctrl Pts',(1.10361055013022,228.230366074564,3.5961842657834));
#90185=CARTESIAN_POINT('Ctrl Pts',(3.31249469279354,225.824984930898,3.4374264005516));
#90186=CARTESIAN_POINT('Ctrl Pts',(2.48978382254105,222.664577608501,3.27866853531981));
#90187=CARTESIAN_POINT('Ctrl Pts',(-0.611577103518663,221.641548771872,
3.11991067008801));
#90188=CARTESIAN_POINT('Ctrl Pts',(-3.15322268985653,223.692174357191,2.96115280485623));
#90189=CARTESIAN_POINT('Ctrl Pts',(-2.80903899165545,226.939721939622,2.80239493962443));
#90190=CARTESIAN_POINT('Ctrl Pts',(0.105977075600772,228.41203603808,2.64363707439264));
#90191=CARTESIAN_POINT('Ctrl Pts',(2.92400293889902,226.761654972147,2.48487920916085));
#90192=CARTESIAN_POINT('Ctrl Pts',(3.06598140421811,223.499007175436,2.32612134392906));
#90193=CARTESIAN_POINT('Ctrl Pts',(0.401973856246465,221.610068297059,2.16736347869726));
#90194=CARTESIAN_POINT('Ctrl Pts',(-2.62992024517871,222.823594080652,2.00860561346547));
#90195=CARTESIAN_POINT('Ctrl Pts',(-3.25491124662603,226.028967896126,1.84984774823368));
#90196=CARTESIAN_POINT('Ctrl Pts',(-0.901007999190373,228.292627449574,
1.69108988300189));
#90197=CARTESIAN_POINT('Ctrl Pts',(2.27749853795265,227.542880347504,1.53233201777009));
#90198=CARTESIAN_POINT('Ctrl Pts',(3.3716368693583,224.465877357061,1.3735741525383));
#90199=CARTESIAN_POINT('Ctrl Pts',(1.38005658761437,221.877727543927,1.2148162873065));
#90200=CARTESIAN_POINT('Ctrl Pts',(-1.8745581653467,222.147032303853,1.05605842207472));
#90201=CARTESIAN_POINT('Ctrl Pts',(-3.41356367834167,225.027472611936,0.897300556842921));
#90202=CARTESIAN_POINT('Ctrl Pts',(-1.82850363051409,227.882567664331,0.738542691611129));
#90203=CARTESIAN_POINT('Ctrl Pts',(1.43005929071516,228.09994779069,0.579784826379336));
#90204=CARTESIAN_POINT('Ctrl Pts',(3.37971743849465,225.479421329585,0.421026961147546));
#90205=CARTESIAN_POINT('Ctrl Pts',(2.23649081956702,222.421823777806,0.262269095915749));
#90206=CARTESIAN_POINT('Ctrl Pts',(-0.954038742191529,221.720318283674,
0.103511230683963));
#90207=CARTESIAN_POINT('Ctrl Pts',(-3.27049340358829,224.027496227842,-0.0552466345478343));
#90208=CARTESIAN_POINT('Ctrl Pts',(-2.81925737956181,226.146956680238,-0.161085211369028));
#90209=CARTESIAN_POINT('Ctrl Pts',(-2.19519710401908,226.876863439079,-0.214004499779625));
#90210=CARTESIAN_POINT('Ctrl Pts',(-0.698066426161029,222.388867814061,
20.2140044997796));
#90211=CARTESIAN_POINT('Ctrl Pts',(-1.56627230491966,222.620976084267,20.161085211369));
#90212=CARTESIAN_POINT('Ctrl Pts',(-3.03778547642569,224.016348073287,20.0552466345478));
#90213=CARTESIAN_POINT('Ctrl Pts',(-2.47430958228317,227.023624945618,19.896488769316));
#90214=CARTESIAN_POINT('Ctrl Pts',(0.358151931539931,228.173887732117,19.7377309040843));
#90215=CARTESIAN_POINT('Ctrl Pts',(2.86064161279711,226.421825579025,19.5789730388524));
#90216=CARTESIAN_POINT('Ctrl Pts',(2.74615017319171,223.367324517025,19.4202151736207));
#90217=CARTESIAN_POINT('Ctrl Pts',(0.117851488886823,221.807630837682,19.2614573083889));
#90218=CARTESIAN_POINT('Ctrl Pts',(-2.61804355082996,223.169306315376,19.1026994431571));
#90219=CARTESIAN_POINT('Ctrl Pts',(-2.9580339124977,226.206573888388,18.9439415779253));
#90220=CARTESIAN_POINT('Ctrl Pts',(-0.590768392476075,228.139515505661,
18.7851837126935));
#90221=CARTESIAN_POINT('Ctrl Pts',(2.31713713756645,227.199206917547,18.6264258474617));
#90222=CARTESIAN_POINT('Ctrl Pts',(3.10441421329951,224.24616737416,18.4676679822299));
#90223=CARTESIAN_POINT('Ctrl Pts',(1.05052395831347,221.983043727605,18.3089101169981));
#90224=CARTESIAN_POINT('Ctrl Pts',(-1.96480205705699,222.481034252332,18.1501522517663));
#90225=CARTESIAN_POINT('Ctrl Pts',(-3.18194314126583,225.284384144496,17.9913943865345));
#90226=CARTESIAN_POINT('Ctrl Pts',(-1.48696908454564,227.827464686981,17.8326365213028));
#90227=CARTESIAN_POINT('Ctrl Pts',(1.56887857515016,227.782850147507,17.6738786560709));
#90228=CARTESIAN_POINT('Ctrl Pts',(3.18888884354982,225.191371021987,17.5151207908392));
#90229=CARTESIAN_POINT('Ctrl Pts',(1.89042805990215,222.424749263084,17.3563629256074));
#90230=CARTESIAN_POINT('Ctrl Pts',(-1.13815235673217,222.01499681903,17.1976050603756));
#90231=CARTESIAN_POINT('Ctrl Pts',(-3.12509580738706,224.337119197528,17.0388471951438));
#90232=CARTESIAN_POINT('Ctrl Pts',(-2.2519516851387,227.265910046244,16.880089329912));
#90233=CARTESIAN_POINT('Ctrl Pts',(0.682178524453497,228.120940116704,16.7213314646802));
#90234=CARTESIAN_POINT('Ctrl Pts',(2.99197897841337,226.119685911656,16.5625735994484));
#90235=CARTESIAN_POINT('Ctrl Pts',(2.56352038744898,223.093695205979,16.4038157342166));
#90236=CARTESIAN_POINT('Ctrl Pts',(-0.211071960543857,221.812354571995,
16.2450578689848));
#90237=CARTESIAN_POINT('Ctrl Pts',(-2.79249125891984,223.44834690878,16.086300003753));
#90238=CARTESIAN_POINT('Ctrl Pts',(-2.81822266676094,226.50441209343,15.9275421385212));
#90239=CARTESIAN_POINT('Ctrl Pts',(-0.264716800896706,228.183639389432,
15.7687842732894));
#90240=CARTESIAN_POINT('Ctrl Pts',(2.53105787078296,226.949200041371,15.6100264080576));
#90241=CARTESIAN_POINT('Ctrl Pts',(3.01040847863157,223.930852892121,15.4512685428258));
#90242=CARTESIAN_POINT('Ctrl Pts',(0.734633365228797,221.890989133948,15.292510677594));
#90243=CARTESIAN_POINT('Ctrl Pts',(-2.21347817514792,222.696491998132,15.1337528123623));
#90244=CARTESIAN_POINT('Ctrl Pts',(-3.13581457666957,225.61016529504,14.9749949471305));
#90245=CARTESIAN_POINT('Ctrl Pts',(-1.18825360093744,227.965415337923,14.8162370818987));
#90246=CARTESIAN_POINT('Ctrl Pts',(1.84679702364634,227.60671738015,14.6574792166669));
#90247=CARTESIAN_POINT('Ctrl Pts',(3.19165908481221,224.862351778571,14.4987213514351));
#90248=CARTESIAN_POINT('Ctrl Pts',(1.61551487706703,222.243961823831,14.3399634862033));
#90249=CARTESIAN_POINT('Ctrl Pts',(-1.43914848264138,222.147897899542,14.1812056209715));
#90250=CARTESIAN_POINT('Ctrl Pts',(-3.1767032076295,224.662077705436,14.0224477557397));
#90251=CARTESIAN_POINT('Ctrl Pts',(-2.00693928191597,227.485523982027,13.8636898905079));
#90252=CARTESIAN_POINT('Ctrl Pts',(0.999575395686113,228.034218808007,13.7049320252761));
#90253=CARTESIAN_POINT('Ctrl Pts',(3.0912787104636,225.805996700218,13.5461741600443));
#90254=CARTESIAN_POINT('Ctrl Pts',(2.35384387098638,222.840126444083,13.3874162948126));
#90255=CARTESIAN_POINT('Ctrl Pts',(-0.537828786654925,221.850972381389,
13.2286584295807));
#90256=CARTESIAN_POINT('Ctrl Pts',(-2.93728055989923,223.743808271415,13.069900564349));
#90257=CARTESIAN_POINT('Ctrl Pts',(-2.64853328022953,226.786310782043,12.9111426991172));
#90258=CARTESIAN_POINT('Ctrl Pts',(0.0641515533551816,228.19398173519,12.7523848338854));
#90259=CARTESIAN_POINT('Ctrl Pts',(2.71812488783194,226.678520729892,12.5936269686536));
#90260=CARTESIAN_POINT('Ctrl Pts',(2.88447043185256,223.626877618602,12.4348691034218));
#90261=CARTESIAN_POINT('Ctrl Pts',(0.410948750070758,221.831916056771,12.27611123819));
#90262=CARTESIAN_POINT('Ctrl Pts',(-2.43867321161564,222.936384795201,12.1173533729582));
#90263=CARTESIAN_POINT('Ctrl Pts',(-3.05642154592989,225.929474087914,11.9585955077264));
#90264=CARTESIAN_POINT('Ctrl Pts',(-0.876933001599986,228.071908731918,
11.7998376424946));
#90265=CARTESIAN_POINT('Ctrl Pts',(2.10512459130967,227.402932625271,11.6410797772628));
#90266=CARTESIAN_POINT('Ctrl Pts',(3.16057224103474,224.534792674469,11.482321912031));
#90267=CARTESIAN_POINT('Ctrl Pts',(1.32346430005129,222.092410449699,11.3235640467992));
#90268=CARTESIAN_POINT('Ctrl Pts',(-1.72487811629514,222.311054067027,11.1648061815675));
#90269=CARTESIAN_POINT('Ctrl Pts',(-3.19461214843743,224.990620896471,11.0060483163357));
#90270=CARTESIAN_POINT('Ctrl Pts',(-1.74063726795488,227.678771481096,10.8472904511039));
#90271=CARTESIAN_POINT('Ctrl Pts',(1.30636877171108,227.915310511562,10.6885325858721));
#90272=CARTESIAN_POINT('Ctrl Pts',(3.15778616287877,225.483757476488,10.5297747206403));
#90273=CARTESIAN_POINT('Ctrl Pts',(2.11919778195673,222.609469617956,10.3710168554085));
#90274=CARTESIAN_POINT('Ctrl Pts',(-0.858880325676687,221.922995071065,
10.2122589901767));
#90275=CARTESIAN_POINT('Ctrl Pts',(-3.05091119302543,224.052595314135,10.0535011249449));
#90276=CARTESIAN_POINT('Ctrl Pts',(-2.45074825649149,227.049260288453,9.8947432597131));
#90277=CARTESIAN_POINT('Ctrl Pts',(0.392339388010119,228.170442327365,9.73598539448133));
#90278=CARTESIAN_POINT('Ctrl Pts',(2.87635804003325,226.390035672946,9.57722752924952));
#90279=CARTESIAN_POINT('Ctrl Pts',(2.72793392692798,223.33746842531,9.41846966401774));
#90280=CARTESIAN_POINT('Ctrl Pts',(0.0829047911716047,221.806450009452,
9.25971179878593));
#90281=CARTESIAN_POINT('Ctrl Pts',(-2.63799880620485,223.198168419361,9.10095393355416));
#90282=CARTESIAN_POINT('Ctrl Pts',(-2.94460599987943,226.238923021015,8.94219606832235));
#90283=CARTESIAN_POINT('Ctrl Pts',(-0.556309898258184,228.145815322556,
8.78343820309056));
#90284=CARTESIAN_POINT('Ctrl Pts',(2.34112100037261,227.1736575646,8.62468033785877));
#90285=CARTESIAN_POINT('Ctrl Pts',(3.09595805152473,224.212168488999,8.46592247262698));
#90286=CARTESIAN_POINT('Ctrl Pts',(1.017374415667,221.971702781286,8.30716460739518));
#90287=CARTESIAN_POINT('Ctrl Pts',(-1.99231024540189,222.502734569055,8.1484067421634));
#90288=CARTESIAN_POINT('Ctrl Pts',(-3.17863264822466,225.319263581023,7.9896488769316));
#90289=CARTESIAN_POINT('Ctrl Pts',(-1.45587057638894,227.843602576193,7.83089101169981));
#90290=CARTESIAN_POINT('Ctrl Pts',(1.59930418970722,227.765476605454,7.67213314646802));
#90291=CARTESIAN_POINT('Ctrl Pts',(3.19079582427445,225.156386554153,7.51337528123622));
#90292=CARTESIAN_POINT('Ctrl Pts',(1.86207124594069,222.404171534641,7.35461741600444));
#90293=CARTESIAN_POINT('Ctrl Pts',(-1.17082086345382,222.027658624547,7.19585955077263));
#90294=CARTESIAN_POINT('Ctrl Pts',(-3.1321777646568,224.371432424383,7.03710168554085));
#90295=CARTESIAN_POINT('Ctrl Pts',(-2.22696569881578,227.290471244706,6.87834382030905));
#90296=CARTESIAN_POINT('Ctrl Pts',(0.71636528700813,228.113270871944,6.71958595507726));
#90297=CARTESIAN_POINT('Ctrl Pts',(3.00407879033259,226.086805119606,6.56082808984547));
#90298=CARTESIAN_POINT('Ctrl Pts',(2.54245950287719,223.065695364541,6.40207022461367));
#90299=CARTESIAN_POINT('Ctrl Pts',(-0.246018621631624,221.814861135784,
6.24331235938189));
#90300=CARTESIAN_POINT('Ctrl Pts',(-2.80934051329762,223.479065870305,6.08455449415009));
#90301=CARTESIAN_POINT('Ctrl Pts',(-2.80155407766827,226.535229460513,5.9257966289183));
#90302=CARTESIAN_POINT('Ctrl Pts',(-0.229785460325367,228.186351108831,
5.7670387636865));
#90303=CARTESIAN_POINT('Ctrl Pts',(2.55228280127121,226.921324347647,5.60828089845472));
#90304=CARTESIAN_POINT('Ctrl Pts',(2.99850194351049,223.897901619051,5.44952303322292));
#90305=CARTESIAN_POINT('Ctrl Pts',(0.700492224962129,221.88311928536,5.29076516799113));
#90306=CARTESIAN_POINT('Ctrl Pts',(-2.23860795032526,222.72090605914,5.13200730275934));
#90307=CARTESIAN_POINT('Ctrl Pts',(-3.12893421750635,225.64451951797,4.97324943752754));
#90308=CARTESIAN_POINT('Ctrl Pts',(-1.15566001186744,227.978268739303,4.81449157229575));
#90309=CARTESIAN_POINT('Ctrl Pts',(1.87527419118623,227.586306527535,4.65573370706396));
#90310=CARTESIAN_POINT('Ctrl Pts',(3.18995752821183,224.827356683487,4.49697584183217));
#90311=CARTESIAN_POINT('Ctrl Pts',(1.58519186085557,222.22640999589,4.33821797660037));
#90312=CARTESIAN_POINT('Ctrl Pts',(-1.47034133521057,222.163852771051,4.17946011136858));
#90313=CARTESIAN_POINT('Ctrl Pts',(-3.18021819913001,224.696937378484,4.02070224613679));
#90314=CARTESIAN_POINT('Ctrl Pts',(-1.97955949222763,227.507384885481,3.86194438090499));
#90315=CARTESIAN_POINT('Ctrl Pts',(1.03279198404188,228.023073843338,3.70318651567321));
#90316=CARTESIAN_POINT('Ctrl Pts',(3.09993227728275,225.772045739765,3.54442865044141));
#90317=CARTESIAN_POINT('Ctrl Pts',(2.33001467194577,222.814441403258,3.38567078520962));
#90318=CARTESIAN_POINT('Ctrl Pts',(-0.57233226889966,221.857060213137,3.22691291997783));
#90319=CARTESIAN_POINT('Ctrl Pts',(-2.95088074103546,223.776097383032,3.06815505474604));
#90320=CARTESIAN_POINT('Ctrl Pts',(-2.62878327241482,226.815250198791,2.90939718951424));
#90321=CARTESIAN_POINT('Ctrl Pts',(0.0991765384625657,228.193086065528,
2.75063932428245));
#90322=CARTESIAN_POINT('Ctrl Pts',(2.73636999596777,226.648609768787,2.59188145905066));
#90323=CARTESIAN_POINT('Ctrl Pts',(2.86923771898004,223.595325717816,2.43312359381887));
#90324=CARTESIAN_POINT('Ctrl Pts',(0.376179238660561,221.827599836887,2.27436572858707));
#90325=CARTESIAN_POINT('Ctrl Pts',(-2.46115855595033,222.963253806101,2.11560786335528));
#90326=CARTESIAN_POINT('Ctrl Pts',(-3.04604395444252,225.962939140832,1.95684999812349));
#90327=CARTESIAN_POINT('Ctrl Pts',(-0.843190416231185,228.081339912848,
1.7980921328917));
#90328=CARTESIAN_POINT('Ctrl Pts',(2.13135171042635,227.379703998816,1.6393342676599));
#90329=CARTESIAN_POINT('Ctrl Pts',(3.15527930696426,224.500151947571,1.48057640242811));
#90330=CARTESIAN_POINT('Ctrl Pts',(1.29149851008957,222.078083419693,1.32181853719631));
#90331=CARTESIAN_POINT('Ctrl Pts',(-1.75426797665344,222.330106923169,1.16306067196453));
#90332=CARTESIAN_POINT('Ctrl Pts',(-3.19451567728472,225.025709697487,1.00430280673273));
#90333=CARTESIAN_POINT('Ctrl Pts',(-1.71116875619176,227.697593618355,0.845544941500938));
#90334=CARTESIAN_POINT('Ctrl Pts',(1.33829254530139,227.901024486215,0.686787076269146));
#90335=CARTESIAN_POINT('Ctrl Pts',(3.16284134687909,225.448656916261,0.528029211037355));
#90336=CARTESIAN_POINT('Ctrl Pts',(2.09297545276232,222.587265058842,0.36927134580556));
#90337=CARTESIAN_POINT('Ctrl Pts',(-0.892818182360209,221.930775094139,
0.210513480573772));
#90338=CARTESIAN_POINT('Ctrl Pts',(-3.06062620612795,224.08990168659,0.0517556153419759));
#90339=CARTESIAN_POINT('Ctrl Pts',(-2.63834594750729,226.073356597808,-0.0540829614792177));
#90340=CARTESIAN_POINT('Ctrl Pts',(-2.05433155034205,226.756425321227,-0.107002249889815));
#90341=CARTESIAN_POINT('Ctrl Pts',(-0.650199997975112,222.567913197965,
20.3210067496694));
#90342=CARTESIAN_POINT('Ctrl Pts',(-1.45887298303087,222.784105799646,20.2680874612588));
#90343=CARTESIAN_POINT('Ctrl Pts',(-2.82948446823766,224.083797104705,20.1622488844376));
#90344=CARTESIAN_POINT('Ctrl Pts',(-2.30464612692774,226.884864944414,20.0034910192058));
#90345=CARTESIAN_POINT('Ctrl Pts',(0.3335934467479,227.956254189655,19.8447331539741));
#90346=CARTESIAN_POINT('Ctrl Pts',(2.66448736272432,226.324330971892,19.6859752887423));
#90347=CARTESIAN_POINT('Ctrl Pts',(2.55784660332125,223.479277106103,19.5272174235105));
#90348=CARTESIAN_POINT('Ctrl Pts',(0.109770410041031,222.026531652166,19.3684595582787));
#90349=CARTESIAN_POINT('Ctrl Pts',(-2.4385242545037,223.294837016326,19.2097016930469));
#90350=CARTESIAN_POINT('Ctrl Pts',(-2.75520147057272,226.123839093796,19.0509438278151));
#90351=CARTESIAN_POINT('Ctrl Pts',(-0.550259392511009,227.924238867424,
18.8921859625833));
#90352=CARTESIAN_POINT('Ctrl Pts',(2.15825099974972,227.048407257171,18.7334280973515));
#90353=CARTESIAN_POINT('Ctrl Pts',(2.89154447135037,224.297857691724,18.5746702321197));
#90354=CARTESIAN_POINT('Ctrl Pts',(0.97848951041037,222.189916476875,18.4159123668879));
#90355=CARTESIAN_POINT('Ctrl Pts',(-1.83007554244595,222.653759781801,18.2571545016561));
#90356=CARTESIAN_POINT('Ctrl Pts',(-2.96375723924402,225.264883918272,18.0983966364243));
#90357=CARTESIAN_POINT('Ctrl Pts',(-1.38500758599382,227.633585379346,17.9396387711926));
#90358=CARTESIAN_POINT('Ctrl Pts',(1.46130054126183,227.592030059696,17.7808809059607));
#90359=CARTESIAN_POINT('Ctrl Pts',(2.97022667458963,225.178248707351,17.622123040729));
#90360=CARTESIAN_POINT('Ctrl Pts',(1.76080137169772,222.601334255342,17.4633651754972));
#90361=CARTESIAN_POINT('Ctrl Pts',(-1.06010922787442,222.219678544209,17.3046073102654));
#90362=CARTESIAN_POINT('Ctrl Pts',(-2.910807928136,224.382572946825,17.1458494450336));
#90363=CARTESIAN_POINT('Ctrl Pts',(-2.09753531504101,227.110536551059,16.9870915798018));
#90364=CARTESIAN_POINT('Ctrl Pts',(0.635401529991375,227.906937193242,16.82833371457));
#90365=CARTESIAN_POINT('Ctrl Pts',(2.78681892266966,226.04290902729,16.6695758493382));
#90366=CARTESIAN_POINT('Ctrl Pts',(2.38773974547801,223.224410562146,16.5108179841064));
#90367=CARTESIAN_POINT('Ctrl Pts',(-0.196598752174572,222.030931479928,
16.3520601188746));
#90368=CARTESIAN_POINT('Ctrl Pts',(-2.60101007991516,223.554743790905,16.1933022536428));
#90369=CARTESIAN_POINT('Ctrl Pts',(-2.62497708462872,226.401254527426,16.034544388411));
#90370=CARTESIAN_POINT('Ctrl Pts',(-0.246565164798955,227.965337175641,
15.8757865231793));
#90371=CARTESIAN_POINT('Ctrl Pts',(2.35750318420032,226.815543357274,15.7170286579475));
#90372=CARTESIAN_POINT('Ctrl Pts',(2.80398471170561,224.004164329746,15.5582707927157));
#90373=CARTESIAN_POINT('Ctrl Pts',(0.68425954133199,222.104174068464,15.3995129274838));
#90374=CARTESIAN_POINT('Ctrl Pts',(-2.06169993436575,222.854443585853,15.2407550622521));
#90375=CARTESIAN_POINT('Ctrl Pts',(-2.92079171120392,225.568326249095,15.0819971970203));
#90376=CARTESIAN_POINT('Ctrl Pts',(-1.10677502880681,227.762076751515,14.9232393317885));
#90377=CARTESIAN_POINT('Ctrl Pts',(1.72016211643202,227.427974719564,14.7644814665567));
#90378=CARTESIAN_POINT('Ctrl Pts',(2.9728069603557,224.871790319746,14.6057236013249));
#90379=CARTESIAN_POINT('Ctrl Pts',(1.50473899106477,222.432943414254,14.4469657360931));
#90380=CARTESIAN_POINT('Ctrl Pts',(-1.34046604367627,222.34346659509,14.2882078708613));
#90381=CARTESIAN_POINT('Ctrl Pts',(-2.95887660795731,224.685249043634,14.1294500056295));
#90382=CARTESIAN_POINT('Ctrl Pts',(-1.86932341699085,227.315091555066,13.9706921403977));
#90383=CARTESIAN_POINT('Ctrl Pts',(0.931034491696291,227.826162366341,13.8119342751659));
#90384=CARTESIAN_POINT('Ctrl Pts',(2.87930967019502,225.750729491076,13.6531764099342));
#90385=CARTESIAN_POINT('Ctrl Pts',(2.19244075175736,222.9882290151,13.4944185447024));
#90386=CARTESIAN_POINT('Ctrl Pts',(-0.500949856473002,222.066901265393,
13.3356606794706));
#90387=CARTESIAN_POINT('Ctrl Pts',(-2.73587117575864,223.829945362257,13.1769028142388));
#90388=CARTESIAN_POINT('Ctrl Pts',(-2.46692330257551,226.663823417572,13.018144949007));
#90389=CARTESIAN_POINT('Ctrl Pts',(0.0597526801153146,227.974970346553,
12.8593870837752));
#90390=CARTESIAN_POINT('Ctrl Pts',(2.53174301231433,226.563424531357,12.7006292185434));
#90391=CARTESIAN_POINT('Ctrl Pts',(2.68668223920164,223.721032646543,12.5418713533116));
#90392=CARTESIAN_POINT('Ctrl Pts',(0.382769986422813,222.049151633319,12.3831134880798));
#90393=CARTESIAN_POINT('Ctrl Pts',(-2.27145334287811,223.077886929242,12.224355622848));
#90394=CARTESIAN_POINT('Ctrl Pts',(-2.84684266209971,225.865740031938,12.0655977576162));
#90395=CARTESIAN_POINT('Ctrl Pts',(-0.816801688917045,227.861267891448,
11.9068398923844));
#90396=CARTESIAN_POINT('Ctrl Pts',(1.96077615784255,227.238163489222,11.7480820271526));
#90397=CARTESIAN_POINT('Ctrl Pts',(2.9438517420503,224.566691949673,11.5893241619208));
#90398=CARTESIAN_POINT('Ctrl Pts',(1.23271432769777,222.291783920744,11.4305662966891));
#90399=CARTESIAN_POINT('Ctrl Pts',(-1.60660319088846,222.495435141052,11.2718084314573));
#90400=CARTESIAN_POINT('Ctrl Pts',(-2.97555753235169,224.991264021779,11.1130505662255));
#90401=CARTESIAN_POINT('Ctrl Pts',(-1.62128173721763,227.495088069431,10.9542927009937));
#90402=CARTESIAN_POINT('Ctrl Pts',(1.21679104006264,227.715407614056,10.7955348357619));
#90403=CARTESIAN_POINT('Ctrl Pts',(2.94125670532674,225.450586217078,10.6367769705301));
#90404=CARTESIAN_POINT('Ctrl Pts',(1.97388434953791,222.773388331949,10.4780191052983));
#90405=CARTESIAN_POINT('Ctrl Pts',(-0.799986885326904,222.133985357861,
10.3192612400665));
#90406=CARTESIAN_POINT('Ctrl Pts',(-2.84171015419925,224.117558871555,10.1605033748347));
#90407=CARTESIAN_POINT('Ctrl Pts',(-2.28270040169599,226.908742471301,10.0017455096029));
#90408=CARTESIAN_POINT('Ctrl Pts',(0.365436668674411,227.953045036372,9.84298764437113));
#90409=CARTESIAN_POINT('Ctrl Pts',(2.67912611424445,226.29472090028,9.68422977913933));
#90410=CARTESIAN_POINT('Ctrl Pts',(2.54087944541204,223.451468247167,9.52547191390754));
#90411=CARTESIAN_POINT('Ctrl Pts',(0.0772200080561768,222.025431793351,
9.36671404867575));
#90412=CARTESIAN_POINT('Ctrl Pts',(-2.45711117763608,223.321720045289,9.20795618344396));
#90413=CARTESIAN_POINT('Ctrl Pts',(-2.74269431017936,226.153970045781,9.04919831821217));
#90414=CARTESIAN_POINT('Ctrl Pts',(-0.51816371790034,227.930106705753,8.89044045298038));
#90415=CARTESIAN_POINT('Ctrl Pts',(2.18059028862479,227.024609823844,8.73168258774858));
#90416=CARTESIAN_POINT('Ctrl Pts',(2.88366814875014,224.266190110768,8.57292472251679));
#90417=CARTESIAN_POINT('Ctrl Pts',(0.947613032536847,222.179353179461,8.41416685728499));
#90418=CARTESIAN_POINT('Ctrl Pts',(-1.8556974937902,222.673972107392,8.25540899205321));
#90419=CARTESIAN_POINT('Ctrl Pts',(-2.96067374677397,225.297371671169,8.0966511268214));
#90420=CARTESIAN_POINT('Ctrl Pts',(-1.3560415031359,227.648616693186,7.93789326158962));
#90421=CARTESIAN_POINT('Ctrl Pts',(1.48963987084711,227.575847821754,7.77913539635783));
#90422=CARTESIAN_POINT('Ctrl Pts',(2.97200289360952,225.145663125145,7.62037753112604));
#90423=CARTESIAN_POINT('Ctrl Pts',(1.73438898501166,222.582167542132,7.46161966589423));
#90424=CARTESIAN_POINT('Ctrl Pts',(-1.09053765446568,222.23147212948,7.30286180066245));
#90425=CARTESIAN_POINT('Ctrl Pts',(-2.91740427546038,224.414533315059,7.14410393543066));
#90426=CARTESIAN_POINT('Ctrl Pts',(-2.07426261827787,227.133413587672,6.98534607019886));
#90427=CARTESIAN_POINT('Ctrl Pts',(0.667244105584131,227.899793828743,6.82658820496708));
#90428=CARTESIAN_POINT('Ctrl Pts',(2.79808905025428,226.012282871779,6.66783033973528));
#90429=CARTESIAN_POINT('Ctrl Pts',(2.3681230061639,223.19833067037,6.50907247450349));
#90430=CARTESIAN_POINT('Ctrl Pts',(-0.229149120043518,222.03326616859,6.35031460927169));
#90431=CARTESIAN_POINT('Ctrl Pts',(-2.61670398059818,223.583356352652,6.1915567440399));
#90432=CARTESIAN_POINT('Ctrl Pts',(-2.60945146100876,226.429958747059,6.03279887880811));
#90433=CARTESIAN_POINT('Ctrl Pts',(-0.214029066918333,227.967862952389,
5.87404101357631));
#90434=CARTESIAN_POINT('Ctrl Pts',(2.37727272079926,226.789579100402,5.71528314834453));
#90435=CARTESIAN_POINT('Ctrl Pts',(2.79289460792538,223.9734725261,5.55652528311272));
#90436=CARTESIAN_POINT('Ctrl Pts',(0.652459459706044,222.096843855544,5.39776741788095));
#90437=CARTESIAN_POINT('Ctrl Pts',(-2.08510656037881,222.877183574231,5.23900955264914));
#90438=CARTESIAN_POINT('Ctrl Pts',(-2.91438313840003,225.600324802303,5.08025168741736));
#90439=CARTESIAN_POINT('Ctrl Pts',(-1.07641638276239,227.774048794917,4.92149382218556));
#90440=CARTESIAN_POINT('Ctrl Pts',(1.74668660404933,227.408963439503,4.76273595695377));
#90441=CARTESIAN_POINT('Ctrl Pts',(2.97122207952394,224.839194839001,4.60397809172198));
#90442=CARTESIAN_POINT('Ctrl Pts',(1.47649522465458,222.416595115491,4.44522022649018));
#90443=CARTESIAN_POINT('Ctrl Pts',(-1.36952000174851,222.358327440755,4.28646236125839));
#90444=CARTESIAN_POINT('Ctrl Pts',(-2.96215057642344,224.717718388235,4.1277044960266));
#90445=CARTESIAN_POINT('Ctrl Pts',(-1.84382106000483,227.335453455953,3.96894663079481));
#90446=CARTESIAN_POINT('Ctrl Pts',(0.96197341795355,227.815781612112,3.81018876556301));
#90447=CARTESIAN_POINT('Ctrl Pts',(2.88736986177197,225.719106548631,3.65143090033122));
#90448=CARTESIAN_POINT('Ctrl Pts',(2.17024552135048,222.964305198015,3.49267303509943));
#90449=CARTESIAN_POINT('Ctrl Pts',(-0.533087434280658,222.072571654402,
3.33391516986763));
#90450=CARTESIAN_POINT('Ctrl Pts',(-2.74853879221438,223.860020408874,3.17515730463585));
#90451=CARTESIAN_POINT('Ctrl Pts',(-2.44852755317419,226.69077845796,3.01639943940405));
#90452=CARTESIAN_POINT('Ctrl Pts',(0.0923760013243574,227.974136092977,
2.85764157417226));
#90453=CARTESIAN_POINT('Ctrl Pts',(2.54873705303652,226.535564565427,2.69888370894047));
#90454=CARTESIAN_POINT('Ctrl Pts',(2.67249403374196,223.691644260197,2.54012584370867));
#90455=CARTESIAN_POINT('Ctrl Pts',(0.350384621074658,222.045131376714,2.38136797847688));
#90456=CARTESIAN_POINT('Ctrl Pts',(-2.29239686672194,223.102913531551,2.22261011324509));
#90457=CARTESIAN_POINT('Ctrl Pts',(-2.837176662259,225.896910385537,2.0638522480133));
#90458=CARTESIAN_POINT('Ctrl Pts',(-0.785372833271999,227.870052376122,
1.90509438278151));
#90459=CARTESIAN_POINT('Ctrl Pts',(1.98520488290005,227.216527650127,1.74633651754971));
#90460=CARTESIAN_POINT('Ctrl Pts',(2.93892174457021,224.534426538081,1.58757865231792));
#90461=CARTESIAN_POINT('Ctrl Pts',(1.20294043256477,222.27843929546,1.42882078708613));
#90462=CARTESIAN_POINT('Ctrl Pts',(-1.63397778796018,222.513181542484,1.27006292185433));
#90463=CARTESIAN_POINT('Ctrl Pts',(-2.97546767622777,225.023946783039,1.11130505662254));
#90464=CARTESIAN_POINT('Ctrl Pts',(-1.59383388186942,227.512619572377,0.952547191390748));
#90465=CARTESIAN_POINT('Ctrl Pts',(1.24652579988762,227.70210118174,0.793789326158957));
#90466=CARTESIAN_POINT('Ctrl Pts',(2.94596525526353,225.417892502936,0.635031460927166));
#90467=CARTESIAN_POINT('Ctrl Pts',(1.94946008595763,222.752706339879,0.47627359569537));
#90468=CARTESIAN_POINT('Ctrl Pts',(-0.83159762252889,222.141231904605,0.317515730463582));
#90469=CARTESIAN_POINT('Ctrl Pts',(-2.85075900866762,224.152307145338,0.158757865231786));
#90470=CARTESIAN_POINT('Ctrl Pts',(-2.45743451545277,225.999756515379,0.0529192884105924));
#90471=CARTESIAN_POINT('Ctrl Pts',(-1.91346599666502,226.635987203375,-4.44089209850063E-15));
#90472=CARTESIAN_POINT('Ctrl Pts',(-1.91346599666502,226.635987203375,-4.44089209850063E-15));
#90473=CARTESIAN_POINT('Ctrl Pts',(-1.97507207771062,226.578092614711,-4.89329144937181E-15));
#90474=CARTESIAN_POINT('Ctrl Pts',(-2.03330671663252,226.517047060303,-8.96290615499113E-15));
#90475=CARTESIAN_POINT('Ctrl Pts',(-2.0881732164084,226.453235441036,-9.04831765069503E-15));
#90476=CARTESIAN_POINT('Ctrl Pts',(-2.14449293498847,226.387733678504,-9.13599139371118E-15));
#90477=CARTESIAN_POINT('Ctrl Pts',(-2.1972641669798,226.3193169524,-4.39530143014281E-15));
#90478=CARTESIAN_POINT('Ctrl Pts',(-2.24646493105837,226.24835301163,-4.05231403988182E-15));
#90479=CARTESIAN_POINT('Ctrl Pts',(-2.29735461880039,226.174953078634,-3.69755285849117E-15));
#90480=CARTESIAN_POINT('Ctrl Pts',(-2.34442508449272,226.09882752961,-3.93155570548555E-15));
#90481=CARTESIAN_POINT('Ctrl Pts',(-2.38761709048648,226.020339322605,-4.27435864480685E-15));
#90482=CARTESIAN_POINT('Ctrl Pts',(-2.40651359310875,225.98600073204,-4.42433493075992E-15));
#90483=CARTESIAN_POINT('Ctrl Pts',(-2.42466724057222,225.951209407906,-7.20234639837333E-15));
#90484=CARTESIAN_POINT('Ctrl Pts',(-2.44207062867183,225.915993656427,-7.32747196252603E-15));
#90485=CARTESIAN_POINT('Ctrl Pts',(-2.45159445688031,225.896722192423,-7.39594566262734E-15));
#90486=CARTESIAN_POINT('Ctrl Pts',(-2.46089357651441,225.877323604807,-4.29996776038342E-15));
#90487=CARTESIAN_POINT('Ctrl Pts',(-2.46996656934727,225.857802403079,-4.38538094726937E-15));
#90488=CARTESIAN_POINT('Ctrl Pts',(-2.4786193151025,225.839185393399,-4.46683792666765E-15));
#90489=CARTESIAN_POINT('Ctrl Pts',(-2.48706888952069,225.820450858377,-5.8504930511398E-15));
#90490=CARTESIAN_POINT('Ctrl Pts',(-2.49529995223353,225.801635520385,-5.99520433297585E-15));
#90491=CARTESIAN_POINT('Ctrl Pts',(-2.53185235388015,225.718080599787,-6.6378364062587E-15));
#90492=CARTESIAN_POINT('Ctrl Pts',(-2.56414485209629,225.632842160853,-7.06865270289981E-15));
#90493=CARTESIAN_POINT('Ctrl Pts',(-2.5921533868293,225.546319206983,-7.91033905045424E-15));
#90494=CARTESIAN_POINT('Ctrl Pts',(-2.62062510855391,225.458365392588,-8.76594466122256E-15));
#90495=CARTESIAN_POINT('Ctrl Pts',(-2.64467049608575,225.369083471302,-1.42490890091117E-14));
#90496=CARTESIAN_POINT('Ctrl Pts',(-2.66422516627309,225.278855438708,-1.57374113740616E-14));
#90497=CARTESIAN_POINT('Ctrl Pts',(-2.6834344396825,225.190221116027,-1.71994453002682E-14));
#90498=CARTESIAN_POINT('Ctrl Pts',(-2.69831049024112,225.100672899581,-4.96279256628846E-15));
#90499=CARTESIAN_POINT('Ctrl Pts',(-2.70874964711037,225.010550082124,-3.58046925441613E-15));
#90500=CARTESIAN_POINT('Ctrl Pts',(-2.71288570289571,224.974842888027,-3.03278457040537E-15));
#90501=CARTESIAN_POINT('Ctrl Pts',(-2.71632476189001,224.939045312261,-1.00261591147195E-14));
#90502=CARTESIAN_POINT('Ctrl Pts',(-2.71905833761488,224.903177920343,-1.0019762797242E-14));
#90503=CARTESIAN_POINT('Ctrl Pts',(-2.72067831003024,224.88192217645,-1.00159722097785E-14));
#90504=CARTESIAN_POINT('Ctrl Pts',(-2.72205049483485,224.860641909081,-1.11437171572486E-14));
#90505=CARTESIAN_POINT('Ctrl Pts',(-2.72317292126621,224.839341375436,-1.16573417585641E-14));
#90506=CARTESIAN_POINT('Ctrl Pts',(-2.72391594666752,224.825240818715,-1.19973516824731E-14));
#90507=CARTESIAN_POINT('Ctrl Pts',(-2.72454944019077,224.811131472036,-1.79062259471769E-16));
#90508=CARTESIAN_POINT('Ctrl Pts',(-2.72507248770474,224.797028960929,-3.05311331771918E-16));
#90509=CARTESIAN_POINT('Ctrl Pts',(-2.72860269395363,224.701846837876,-1.15740459682122E-15));
#90510=CARTESIAN_POINT('Ctrl Pts',(-2.72711487623298,224.606814542,-1.19300801555276E-14));
#90511=CARTESIAN_POINT('Ctrl Pts',(-2.72055058832908,224.512331015797,-1.1740608485411E-14));
#90512=CARTESIAN_POINT('Ctrl Pts',(-2.71400847489059,224.418166659277,-1.15517768592805E-14));
#90513=CARTESIAN_POINT('Ctrl Pts',(-2.70242448973437,224.324546417287,-5.8005117148528E-15));
#90514=CARTESIAN_POINT('Ctrl Pts',(-2.6856927726943,224.231847303625,-5.05151476204446E-15));
#90515=CARTESIAN_POINT('Ctrl Pts',(-2.68378876806322,224.221298503326,-4.96628180816443E-15));
#90516=CARTESIAN_POINT('Ctrl Pts',(-2.68181804784731,224.210761621159,-1.04055797883408E-14));
#90517=CARTESIAN_POINT('Ctrl Pts',(-2.67978041320572,224.200237206572,-1.04083408558608E-14));
#90518=CARTESIAN_POINT('Ctrl Pts',(-2.66224980411456,224.109691338203,-1.04064054973758E-14));
#90519=CARTESIAN_POINT('Ctrl Pts',(-2.63977066177727,224.020067997417,-6.8127980350163E-15));
#90520=CARTESIAN_POINT('Ctrl Pts',(-2.61261810729545,223.931605005111,-6.07847105982273E-15));
#90521=CARTESIAN_POINT('Ctrl Pts',(-2.60191965458823,223.896749458088,-5.78913686767505E-15));
#90522=CARTESIAN_POINT('Ctrl Pts',(-2.59049509704381,223.862074101058,-7.49266670012035E-15));
#90523=CARTESIAN_POINT('Ctrl Pts',(-2.57835909838488,223.827593818547,-7.04991620636974E-15));
#90524=CARTESIAN_POINT('Ctrl Pts',(-2.57307244820024,223.812573613203,-6.85704646030921E-15));
#90525=CARTESIAN_POINT('Ctrl Pts',(-2.56765077825727,223.797590429269,-9.27411057059242E-15));
#90526=CARTESIAN_POINT('Ctrl Pts',(-2.562095232492,223.782645516012,-9.32587340685131E-15));
#90527=CARTESIAN_POINT('Ctrl Pts',(-2.55767628878723,223.7707581636,-9.36704615010494E-15));
#90528=CARTESIAN_POINT('Ctrl Pts',(-2.55317299678642,223.758896106066,-8.65625838009356E-15));
#90529=CARTESIAN_POINT('Ctrl Pts',(-2.5485897169222,223.747069278679,-8.60422844084496E-15));
#90530=CARTESIAN_POINT('Ctrl Pts',(-2.51484042770109,223.659981640598,-8.2211024874061E-15));
#90531=CARTESIAN_POINT('Ctrl Pts',(-2.4767077009188,223.574666891679,-1.01908969297783E-14));
#90532=CARTESIAN_POINT('Ctrl Pts',(-2.43452501819882,223.49135596505,-1.10744746706359E-14));
#90533=CARTESIAN_POINT('Ctrl Pts',(-2.39075748174647,223.404914947481,-1.19912494817165E-14));
#90534=CARTESIAN_POINT('Ctrl Pts',(-2.34262982770305,223.320630433717,-1.39073301009351E-14));
#90535=CARTESIAN_POINT('Ctrl Pts',(-2.29045846029114,223.23876337662,-1.66533453693773E-14));
#90536=CARTESIAN_POINT('Ctrl Pts',(-2.23768305960534,223.155948473434,-1.94311536437352E-14));
#90537=CARTESIAN_POINT('Ctrl Pts',(-2.1807693575821,223.075606513649,-1.23608385957802E-14));
#90538=CARTESIAN_POINT('Ctrl Pts',(-2.11999295375159,222.998022388435,-1.25177646026486E-14));
#90539=CARTESIAN_POINT('Ctrl Pts',(-2.07727773114182,222.94349426616,-1.26280562437161E-14));
#90540=CARTESIAN_POINT('Ctrl Pts',(-2.03265337236878,222.890328702756,-1.32724496364774E-14));
#90541=CARTESIAN_POINT('Ctrl Pts',(-1.98620222285849,222.838632264833,-1.29063426612674E-14));
#90542=CARTESIAN_POINT('Ctrl Pts',(-1.9748381431076,222.825984947176,-1.28167761186198E-14));
#90543=CARTESIAN_POINT('Ctrl Pts',(-1.96336393095075,222.813424902219,-1.62360964966543E-14));
#90544=CARTESIAN_POINT('Ctrl Pts',(-1.95179246873506,222.8009660948,-1.60427227058335E-14));
#90545=CARTESIAN_POINT('Ctrl Pts',(-1.8831185473061,222.727025987158,-1.48950944917225E-14));
#90546=CARTESIAN_POINT('Ctrl Pts',(-1.8109316641223,222.656546584352,-2.25517043828303E-15));
#90547=CARTESIAN_POINT('Ctrl Pts',(-1.735545247337,222.589815149064,-6.30745455865167E-15));
#90548=CARTESIAN_POINT('Ctrl Pts',(-1.67071550898282,222.532428398584,-9.7922802137621E-15));
#90549=CARTESIAN_POINT('Ctrl Pts',(-1.60351853762922,222.477813351873,-1.37421915177158E-14));
#90550=CARTESIAN_POINT('Ctrl Pts',(-1.5341274349756,222.426167995139,-1.41275879883551E-14));
#90551=CARTESIAN_POINT('Ctrl Pts',(-1.50861567308636,222.407180488193,-1.4269279683917E-14));
#90552=CARTESIAN_POINT('Ctrl Pts',(-1.4828071207238,222.388594557367,-1.78319144411338E-14));
#90553=CARTESIAN_POINT('Ctrl Pts',(-1.45670967205871,222.370420692607,-1.85407245112401E-14));
#90554=CARTESIAN_POINT('Ctrl Pts',(-1.43999809309774,222.358783004194,-1.89946131501996E-14));
#90555=CARTESIAN_POINT('Ctrl Pts',(-1.42316698931895,222.347313703686,-1.1605964273452E-14));
#90556=CARTESIAN_POINT('Ctrl Pts',(-1.40623326051012,222.336025220852,-1.15879528195251E-14));
#90557=CARTESIAN_POINT('Ctrl Pts',(-1.32003067627284,222.278560240554,-1.14962639840711E-14));
#90558=CARTESIAN_POINT('Ctrl Pts',(-1.2310870933596,222.225717965425,-7.07423916875325E-15));
#90559=CARTESIAN_POINT('Ctrl Pts',(-1.13970920235716,222.177818076848,-3.37230243729891E-15));
#90560=CARTESIAN_POINT('Ctrl Pts',(-1.04833131135472,222.129918188271,3.29634294155433E-16));
#90561=CARTESIAN_POINT('Ctrl Pts',(-0.954518472994722,222.086959783478,
-9.90042614199229E-16));
#90562=CARTESIAN_POINT('Ctrl Pts',(-0.858539567548663,222.049302996692,
1.81105130891979E-15));
#90563=CARTESIAN_POINT('Ctrl Pts',(-0.837654053215665,222.041108681946,
2.43149121055914E-15));
#90564=CARTESIAN_POINT('Ctrl Pts',(-0.816665849837719,222.033165591267,
1.08805921371938E-15));
#90565=CARTESIAN_POINT('Ctrl Pts',(-0.795579049799863,222.025472494795,
1.02695629777827E-15));
#90566=CARTESIAN_POINT('Ctrl Pts',(-2.51426753931457,225.001426524072,19.112583302492));
#90567=CARTESIAN_POINT('Ctrl Pts',(-2.51595717399498,225.327423730599,19.092036810933));
#90568=CARTESIAN_POINT('Ctrl Pts',(-2.45712149670304,225.65283607352,19.071490319374));
#90569=CARTESIAN_POINT('Ctrl Pts',(-2.33493158821761,225.952405376489,19.0509438278151));
#90570=CARTESIAN_POINT('Ctrl Pts',(-2.0202207778855,226.723972351672,18.9980245394045));
#90571=CARTESIAN_POINT('Ctrl Pts',(-1.28524008519825,227.324105609548,18.9451052509939));
#90572=CARTESIAN_POINT('Ctrl Pts',(-0.466331340144507,227.478200303444,
18.8921859625833));
#90573=CARTESIAN_POINT('Ctrl Pts',(0.352577404909238,227.632294997339,18.8392666741727));
#90574=CARTESIAN_POINT('Ctrl Pts',(1.25541420232948,227.340351127255,18.7863473857621));
#90575=CARTESIAN_POINT('Ctrl Pts',(1.82904817963972,226.735954264639,18.7334280973515));
#90576=CARTESIAN_POINT('Ctrl Pts',(2.40268215694995,226.131557402022,18.6805088089409));
#90577=CARTESIAN_POINT('Ctrl Pts',(2.64711331415017,225.214707546873,18.6275895205303));
#90578=CARTESIAN_POINT('Ctrl Pts',(2.45048639926028,224.40495908349,18.5746702321197));
#90579=CARTESIAN_POINT('Ctrl Pts',(2.25385948437039,223.595210620107,18.5217509437091));
#90580=CARTESIAN_POINT('Ctrl Pts',(1.61617449739038,222.892563548491,18.4688316552985));
#90581=CARTESIAN_POINT('Ctrl Pts',(0.829237828424323,222.618547230171,18.4159123668879));
#90582=CARTESIAN_POINT('Ctrl Pts',(0.0423011594582637,222.34453091185,18.3629930784773));
#90583=CARTESIAN_POINT('Ctrl Pts',(-0.893887191493852,222.499145346826,
18.3100737900667));
#90584=CARTESIAN_POINT('Ctrl Pts',(-1.55092831643626,223.011639920392,18.2571545016561));
#90585=CARTESIAN_POINT('Ctrl Pts',(-2.14925598476556,223.478337774746,18.2089641019347));
#90586=CARTESIAN_POINT('Ctrl Pts',(-2.51609677269774,224.24181291764,18.1607737022134));
#90587=CARTESIAN_POINT('Ctrl Pts',(-2.52086470301557,225.001296835693,18.112583302492));
#90588=CARTESIAN_POINT('Origin',(0.,225.,10.));
#90589=CARTESIAN_POINT('Origin',(160.,-225.,10.));
#90590=CARTESIAN_POINT('Origin',(-160.,-225.,10.));
#90591=CARTESIAN_POINT('Origin',(0.,-225.,10.));
#90592=CARTESIAN_POINT('Origin',(-160.,225.,10.));
#90593=CARTESIAN_POINT('Origin',(160.,225.,10.));
#90594=CARTESIAN_POINT('Origin',(325.,275.,0.));
#90595=CARTESIAN_POINT('',(325.,275.,0.));
#90596=CARTESIAN_POINT('',(-325.,275.,0.));
#90597=CARTESIAN_POINT('',(325.,275.,0.));
#90598=CARTESIAN_POINT('',(-325.,275.,0.));
#90599=CARTESIAN_POINT('',(325.,275.,0.));
#90600=CARTESIAN_POINT('Origin',(325.,-275.,0.));
#90601=CARTESIAN_POINT('',(325.,-275.,0.));
#90602=CARTESIAN_POINT('',(325.,-275.,0.));
#90603=CARTESIAN_POINT('',(325.,-275.,0.));
#90604=CARTESIAN_POINT('Origin',(-325.,-275.,0.));
#90605=CARTESIAN_POINT('',(-325.,-275.,0.));
#90606=CARTESIAN_POINT('',(-325.,-275.,0.));
#90607=CARTESIAN_POINT('',(-325.,-275.,0.));
#90608=CARTESIAN_POINT('Origin',(-325.,275.,0.));
#90609=CARTESIAN_POINT('',(-325.,275.,0.));
#90610=CARTESIAN_POINT('Origin',(0.,0.,0.));
#90611=CARTESIAN_POINT('',(0.,0.,0.));
#90612=CARTESIAN_POINT('Origin',(0.,0.,0.));
#90613=CARTESIAN_POINT('',(-2.94572833338121,0.00181828527978219,0.322176117089595));
#90614=CARTESIAN_POINT('',(-2.94480724771071,0.00314787458853884,0.177823882910503));
#90615=CARTESIAN_POINT('',(-2.942,-3.60291088309151E-16,0.));
#90616=CARTESIAN_POINT('',(1.28892185405323,2.64462557919718,0.));
#90617=CARTESIAN_POINT('Ctrl Pts',(-2.94572833338121,0.00181828527978219,
0.322176117089595));
#90618=CARTESIAN_POINT('Ctrl Pts',(-2.94634360469406,0.0948282274037363,
0.317125952852808));
#90619=CARTESIAN_POINT('Ctrl Pts',(-2.9423230955825,0.187780597515525,0.31207578861602));
#90620=CARTESIAN_POINT('Ctrl Pts',(-2.93349332836829,0.280269293446551,
0.307025624379232));
#90621=CARTESIAN_POINT('Ctrl Pts',(-2.84078967180988,1.2513073848389,0.254003989763848));
#90622=CARTESIAN_POINT('Ctrl Pts',(-2.21796709303351,2.17123521104683,0.200982355148463));
#90623=CARTESIAN_POINT('Ctrl Pts',(-1.35083655151447,2.61872799079034,0.147960720533078));
#90624=CARTESIAN_POINT('Ctrl Pts',(-0.544239642849529,3.03498168675485,
0.0986404803553854));
#90625=CARTESIAN_POINT('Ctrl Pts',(0.473745963287759,3.04245857499168,0.0493202401776924));
#90626=CARTESIAN_POINT('Ctrl Pts',(1.29201570592007,2.64858957748139,-3.98986399474666E-16));
#90627=CARTESIAN_POINT('',(-1.28892185405285,2.64462557919736,0.));
#90628=CARTESIAN_POINT('Origin',(0.,0.,0.));
#90629=CARTESIAN_POINT('Ctrl Pts',(-1.28892185405285,2.64462557919736,-2.24820162486594E-14));
#90630=CARTESIAN_POINT('Ctrl Pts',(-2.17016087157859,2.21513255860965,0.0530334224957372));
#90631=CARTESIAN_POINT('Ctrl Pts',(-2.81210852573283,1.31417567340568,0.106066844991497));
#90632=CARTESIAN_POINT('Ctrl Pts',(-2.92616511686446,0.346700093493863,
0.159100267487257));
#90633=CARTESIAN_POINT('Ctrl Pts',(-2.93958779542159,0.232843335263716,
0.165341472628339));
#90634=CARTESIAN_POINT('Ctrl Pts',(-2.9456993876071,0.118065318924837,0.171582677769421));
#90635=CARTESIAN_POINT('Ctrl Pts',(-2.94480724771071,0.00314787458853884,
0.177823882910503));
#90636=CARTESIAN_POINT('Origin',(0.,0.,0.));
#90637=CARTESIAN_POINT('',(-2.93822341007844,0.00177250923968975,1.3221761170896));
#90638=CARTESIAN_POINT('',(-2.93786545338865,0.00151834006811738,1.17782388291051));
#90639=CARTESIAN_POINT('',(-2.942,-3.60291088309151E-16,0.));
#90640=CARTESIAN_POINT('Ctrl Pts',(-2.93822341007844,0.00177250923968975,
1.3221761170896));
#90641=CARTESIAN_POINT('Ctrl Pts',(-2.94027489500473,0.377271029867399,
1.30192242721178));
#90642=CARTESIAN_POINT('Ctrl Pts',(-2.87355216442792,0.752067251550473,
1.28166873733397));
#90643=CARTESIAN_POINT('Ctrl Pts',(-2.73470753731878,1.09790711585681,1.26141504745616));
#90644=CARTESIAN_POINT('Ctrl Pts',(-2.37122961644105,2.00327275694782,1.20839341284077));
#90645=CARTESIAN_POINT('Ctrl Pts',(-1.51348078456157,2.71019263013704,1.15537177822539));
#90646=CARTESIAN_POINT('Ctrl Pts',(-0.555353735968972,2.89405691690588,
1.10235014361));
#90647=CARTESIAN_POINT('Ctrl Pts',(0.402773312623631,3.07792120367472,1.04932850899462));
#90648=CARTESIAN_POINT('Ctrl Pts',(1.46127857792935,2.73872990402317,0.996306874379233));
#90649=CARTESIAN_POINT('Ctrl Pts',(2.13406540677062,2.03220287366626,0.943285239763848));
#90650=CARTESIAN_POINT('Ctrl Pts',(2.80685223561189,1.32567584330935,0.890263605148464));
#90651=CARTESIAN_POINT('Ctrl Pts',(3.09392062798872,0.251813082247085,0.837241970533078));
#90652=CARTESIAN_POINT('Ctrl Pts',(2.86345785963421,-0.696160052250375,
0.784220335917694));
#90653=CARTESIAN_POINT('Ctrl Pts',(2.63299509127969,-1.64413318674784,0.731198701302309));
#90654=CARTESIAN_POINT('Ctrl Pts',(1.88500116219385,-2.46621669468049,0.678177066686924));
#90655=CARTESIAN_POINT('Ctrl Pts',(0.962941916531661,-2.78505266672784,
0.62515543207154));
#90656=CARTESIAN_POINT('Ctrl Pts',(0.0408826708694723,-3.1038886387752,
0.572133797456155));
#90657=CARTESIAN_POINT('Ctrl Pts',(-1.05524189136906,-2.91947707493725,
0.51911216284077));
#90658=CARTESIAN_POINT('Ctrl Pts',(-1.8220118053181,-2.3161971147299,0.466090528225386));
#90659=CARTESIAN_POINT('Ctrl Pts',(-2.51574900299274,-1.77037790430724,
0.418119057846789));
#90660=CARTESIAN_POINT('Ctrl Pts',(-2.93988387601795,-0.881682423669888,
0.370147587468192));
#90661=CARTESIAN_POINT('Ctrl Pts',(-2.94572833338121,0.00181828527978219,
0.322176117089595));
#90662=CARTESIAN_POINT('Ctrl Pts',(-2.94480724771071,0.00314787458853884,
0.177823882910503));
#90663=CARTESIAN_POINT('Ctrl Pts',(-2.93811860296998,-0.85842323414381,
0.22461610026518));
#90664=CARTESIAN_POINT('Ctrl Pts',(-2.53775312306778,-1.72783153197978,
0.271408317619858));
#90665=CARTESIAN_POINT('Ctrl Pts',(-1.87323616063333,-2.27559789904567,
0.318200534974535));
#90666=CARTESIAN_POINT('Ctrl Pts',(-1.12008508516153,-2.89642603705373,
0.371233957470294));
#90667=CARTESIAN_POINT('Ctrl Pts',(-0.0276174061089035,-3.10408803845018,
0.424267379966054));
#90668=CARTESIAN_POINT('Ctrl Pts',(0.901529172781748,-2.8053109028385,0.477300802461814));
#90669=CARTESIAN_POINT('Ctrl Pts',(1.8306757516724,-2.50653376722683,0.530334224957574));
#90670=CARTESIAN_POINT('Ctrl Pts',(2.59650123040107,-1.70131749460704,0.583367647453334));
#90671=CARTESIAN_POINT('Ctrl Pts',(2.8475652442623,-0.758507527336255,0.636401069949093));
#90672=CARTESIAN_POINT('Ctrl Pts',(3.09862925812353,0.184302439934527,0.689434492444853));
#90673=CARTESIAN_POINT('Ctrl Pts',(2.83493180711731,1.2647061018563,0.742467914940612));
#90674=CARTESIAN_POINT('Ctrl Pts',(2.17741585189684,1.98579598787704,0.795501337436372));
#90675=CARTESIAN_POINT('Ctrl Pts',(1.51989989667636,2.70688587389778,0.848534759932131));
#90676=CARTESIAN_POINT('Ctrl Pts',(0.468565437241616,3.06866198401749,0.901568182427891));
#90677=CARTESIAN_POINT('Ctrl Pts',(-0.493489605026679,2.90521466357553,
0.954601604923651));
#90678=CARTESIAN_POINT('Ctrl Pts',(-1.45554464729497,2.74176734313358,1.00763502741941));
#90679=CARTESIAN_POINT('Ctrl Pts',(-2.32832027239682,2.05309659212996,1.06066844991517));
#90680=CARTESIAN_POINT('Ctrl Pts',(-2.71091124967939,1.15542995337685,1.11370187241093));
#90681=CARTESIAN_POINT('Ctrl Pts',(-2.86510648171644,0.793644328850147,
1.13507587591079));
#90682=CARTESIAN_POINT('Ctrl Pts',(-2.93967988512601,0.397911017809249,
1.15644987941065));
#90683=CARTESIAN_POINT('Ctrl Pts',(-2.93786545338865,0.00151834006811738,
1.17782388291051));
#90684=CARTESIAN_POINT('Origin',(0.,0.,0.));
#90685=CARTESIAN_POINT('',(-2.93928862718909,-0.00231022146983534,2.3221761170896));
#90686=CARTESIAN_POINT('',(-2.93977341269383,-0.00246746851037129,2.1778238829105));
#90687=CARTESIAN_POINT('',(-2.942,-3.60291088309151E-16,0.));
#90688=CARTESIAN_POINT('Ctrl Pts',(-2.93928862718909,-0.00231022146983534,
2.3221761170896));
#90689=CARTESIAN_POINT('Ctrl Pts',(-2.93448895843968,0.654458709996738,
2.28671890157076));
#90690=CARTESIAN_POINT('Ctrl Pts',(-2.71712890865226,1.31410884872896,2.25126168605192));
#90691=CARTESIAN_POINT('Ctrl Pts',(-2.31282889140208,1.82615547188083,2.21580447053308));
#90692=CARTESIAN_POINT('Ctrl Pts',(-1.70825102266775,2.59185431657369,2.16278283591769));
#90693=CARTESIAN_POINT('Ctrl Pts',(-0.685651158909644,3.02749257073117,
2.10976120130231));
#90694=CARTESIAN_POINT('Ctrl Pts',(0.28537070618245,2.93301616105637,2.05673956668693));
#90695=CARTESIAN_POINT('Ctrl Pts',(1.25639257127454,2.83853975138157,2.00371793207154));
#90696=CARTESIAN_POINT('Ctrl Pts',(2.17583643770061,2.21394867787448,1.95069629745616));
#90697=CARTESIAN_POINT('Ctrl Pts',(2.621473533489,1.34606781880211,1.89767466284077));
#90698=CARTESIAN_POINT('Ctrl Pts',(3.0671106292774,0.478186959729728,1.84465302822539));
#90699=CARTESIAN_POINT('Ctrl Pts',(3.03894095442811,-0.632983684907954,
1.79163139361));
#90700=CARTESIAN_POINT('Ctrl Pts',(2.54990095382167,-1.47716865811546,1.73860975899462));
#90701=CARTESIAN_POINT('Ctrl Pts',(2.06086095321523,-2.32135363132295,1.68558812437923));
#90702=CARTESIAN_POINT('Ctrl Pts',(1.11095062685165,-2.89855293310027,1.63256648976385));
#90703=CARTESIAN_POINT('Ctrl Pts',(0.136388833930434,-2.9437074353793,1.57954485514846));
#90704=CARTESIAN_POINT('Ctrl Pts',(-0.838172958990785,-2.98886193765833,
1.52652322053308));
#90705=CARTESIAN_POINT('Ctrl Pts',(-1.83738621846964,-2.50197164043906,
1.47350158591769));
#90706=CARTESIAN_POINT('Ctrl Pts',(-2.40238934327107,-1.70662078733303,
1.42047995130231));
#90707=CARTESIAN_POINT('Ctrl Pts',(-2.75156739680238,-1.21508534164919,
1.38771200656474));
#90708=CARTESIAN_POINT('Ctrl Pts',(-2.93490436327265,-0.605737275258753,
1.35494406182717));
#90709=CARTESIAN_POINT('Ctrl Pts',(-2.93822341007844,0.00177250923968975,
1.3221761170896));
#90710=CARTESIAN_POINT('Ctrl Pts',(-2.93786545338865,0.00151834006811738,
1.17782388291051));
#90711=CARTESIAN_POINT('Ctrl Pts',(-2.9351778963003,-0.585623038082895,
1.20948330190641));
#90712=CARTESIAN_POINT('Ctrl Pts',(-2.76489639151172,-1.17421105846512,
1.24114272090231));
#90713=CARTESIAN_POINT('Ctrl Pts',(-2.43753063936175,-1.65606669470434,
1.27280213989821));
#90714=CARTESIAN_POINT('Ctrl Pts',(-1.88915272229826,-2.46323417752985,
1.32583556239397));
#90715=CARTESIAN_POINT('Ctrl Pts',(-0.899990558707984,-2.97090661667828,
1.37886898488973));
#90716=CARTESIAN_POINT('Ctrl Pts',(0.07551096328437,-2.94589715015884,1.43190240738549));
#90717=CARTESIAN_POINT('Ctrl Pts',(1.05101248527673,-2.92088768363939,1.48493582988125));
#90718=CARTESIAN_POINT('Ctrl Pts',(2.01285336567117,-2.36319631145207,1.53796925237701));
#90719=CARTESIAN_POINT('Ctrl Pts',(2.51916357038756,-1.52900912719568,1.59100267487277));
#90720=CARTESIAN_POINT('Ctrl Pts',(3.02547377510396,-0.694821942939303,
1.64403609736853));
#90721=CARTESIAN_POINT('Ctrl Pts',(3.0762533041423,0.415861053386139,1.69706951986429));
#90722=CARTESIAN_POINT('Ctrl Pts',(2.6481694163222,1.29277087678848,1.75010294236005));
#90723=CARTESIAN_POINT('Ctrl Pts',(2.22008552850209,2.16968070019081,1.80313636485581));
#90724=CARTESIAN_POINT('Ctrl Pts',(1.31313822382353,2.81281735067005,1.85616978735156));
#90725=CARTESIAN_POINT('Ctrl Pts',(0.343989133332744,2.92672437389905,1.90920320984732));
#90726=CARTESIAN_POINT('Ctrl Pts',(-0.625159957158049,3.04063139712806,
1.96223663234308));
#90727=CARTESIAN_POINT('Ctrl Pts',(-1.65651083346107,2.62530879310683,2.01527005483884));
#90728=CARTESIAN_POINT('Ctrl Pts',(-2.27625313257342,1.8715561682732,2.0683034773346));
#90729=CARTESIAN_POINT('Ctrl Pts',(-2.70286729874226,1.35269284717742,2.10481027919324));
#90730=CARTESIAN_POINT('Ctrl Pts',(-2.9344374252303,0.673461734771185,2.14131708105187));
#90731=CARTESIAN_POINT('Ctrl Pts',(-2.93977341269383,-0.00246746851037129,
2.1778238829105));
#90732=CARTESIAN_POINT('Origin',(0.,0.,0.));
#90733=CARTESIAN_POINT('',(-2.94660142545168,-0.00080359277598141,3.32217611708959));
#90734=CARTESIAN_POINT('',(-2.94677574562124,-0.00048046415745224,3.1778238829105));
#90735=CARTESIAN_POINT('',(-2.942,-3.60291088309151E-16,0.));
#90736=CARTESIAN_POINT('Ctrl Pts',(-2.94660142545168,-0.00080359277598141,
3.32217611708959));
#90737=CARTESIAN_POINT('Ctrl Pts',(-2.9432210210648,0.931587450945792,3.27151537592973));
#90738=CARTESIAN_POINT('Ctrl Pts',(-2.4632020008259,1.86697373967705,3.22085463476987));
#90739=CARTESIAN_POINT('Ctrl Pts',(-1.70229822738816,2.40545252134969,3.17019389361));
#90740=CARTESIAN_POINT('Ctrl Pts',(-0.905934792329565,2.96902550816978,
3.11717225899462));
#90741=CARTESIAN_POINT('Ctrl Pts',(0.198103007440144,3.09783561201883,3.06415062437924));
#90742=CARTESIAN_POINT('Ctrl Pts',(1.10281702258816,2.73273044381862,3.01112898976385));
#90743=CARTESIAN_POINT('Ctrl Pts',(2.00753103773617,2.36762527561841,2.95810735514846));
#90744=CARTESIAN_POINT('Ctrl Pts',(2.71292126826249,1.50860483536893,2.90508572053308));
#90745=CARTESIAN_POINT('Ctrl Pts',(2.89505718696188,0.550149958862014,2.85206408591769));
#90746=CARTESIAN_POINT('Ctrl Pts',(3.07719310566127,-0.40830491764491,2.79904245130231));
#90747=CARTESIAN_POINT('Ctrl Pts',(2.73607471253372,-1.46619423040927,2.74602081668693));
#90748=CARTESIAN_POINT('Ctrl Pts',(2.02835099365646,-2.13771218014694,2.69299918207154));
#90749=CARTESIAN_POINT('Ctrl Pts',(1.3206272747792,-2.8092301298846,2.63997754745616));
#90750=CARTESIAN_POINT('Ctrl Pts',(0.246298230152233,-3.09437671659557,
2.58695591284077));
#90751=CARTESIAN_POINT('Ctrl Pts',(-0.70128090767504,-2.86220649994471,
2.53393427822538));
#90752=CARTESIAN_POINT('Ctrl Pts',(-1.64886004550232,-2.63003628329385,
2.48091264361));
#90753=CARTESIAN_POINT('Ctrl Pts',(-2.4696892765299,-1.88054926328115,2.42789100899462));
#90754=CARTESIAN_POINT('Ctrl Pts',(-2.78682595518842,-0.957926035660687,
2.37486937437924));
#90755=CARTESIAN_POINT('Ctrl Pts',(-2.89188347699535,-0.65228964486123,
2.35730495528269));
#90756=CARTESIAN_POINT('Ctrl Pts',(-2.94166623615261,-0.327653444085288,
2.33974053618614));
#90757=CARTESIAN_POINT('Ctrl Pts',(-2.93928862718909,-0.00231022146983534,
2.3221761170896));
#90758=CARTESIAN_POINT('Ctrl Pts',(-2.93977341269383,-0.00246746851037129,
2.1778238829105));
#90759=CARTESIAN_POINT('Ctrl Pts',(-2.94218901296677,-0.308460460266985,
2.19435050354763));
#90760=CARTESIAN_POINT('Ctrl Pts',(-2.89824084993499,-0.613776768417091,
2.21087712418476));
#90761=CARTESIAN_POINT('Ctrl Pts',(-2.80503526316264,-0.903231941911796,
2.22740374482188));
#90762=CARTESIAN_POINT('Ctrl Pts',(-2.50594137271785,-1.83208478161718,
2.28043716731764));
#90763=CARTESIAN_POINT('Ctrl Pts',(-1.69961986990659,-2.59760781538194,
2.3334705898134));
#90764=CARTESIAN_POINT('Ctrl Pts',(-0.75650214363239,-2.84811401666259,
2.38650401230916));
#90765=CARTESIAN_POINT('Ctrl Pts',(0.186615582641814,-3.09862021794324,
2.43953743480492));
#90766=CARTESIAN_POINT('Ctrl Pts',(1.26652953237896,-2.83410958673978,2.49257085730068));
#90767=CARTESIAN_POINT('Ctrl Pts',(1.98711806191723,-2.17610013539117,2.54560427979644));
#90768=CARTESIAN_POINT('Ctrl Pts',(2.7077065914555,-1.51809068404256,2.5986377022922));
#90769=CARTESIAN_POINT('Ctrl Pts',(3.06896970079488,-0.466582412548801,
2.65167112478796));
#90770=CARTESIAN_POINT('Ctrl Pts',(2.90493990584006,0.495352443093267,2.70470454728372));
#90771=CARTESIAN_POINT('Ctrl Pts',(2.74091011088523,1.45728729873534,2.75773796977948));
#90772=CARTESIAN_POINT('Ctrl Pts',(2.0515874116362,2.32964873852571,2.81077139227524));
#90773=CARTESIAN_POINT('Ctrl Pts',(1.15365266405868,2.71166649769722,2.863804814771));
#90774=CARTESIAN_POINT('Ctrl Pts',(0.255717916481151,3.09368425686873,2.91683823726676));
#90775=CARTESIAN_POINT('Ctrl Pts',(-0.85082887942487,2.98535833542137,2.96987165976252));
#90776=CARTESIAN_POINT('Ctrl Pts',(-1.65763057826024,2.4364545324485,3.02290508225827));
#90777=CARTESIAN_POINT('Ctrl Pts',(-2.44322794727629,1.90197699716214,3.07454468247568));
#90778=CARTESIAN_POINT('Ctrl Pts',(-2.9446289500562,0.949775755309008,3.12618428269309));
#90779=CARTESIAN_POINT('Ctrl Pts',(-2.94677574562124,-0.00048046415745224,
3.1778238829105));
#90780=CARTESIAN_POINT('Origin',(0.,0.,0.));
#90781=CARTESIAN_POINT('',(-2.94172250344281,0.00271694754677573,4.3221761170896));
#90782=CARTESIAN_POINT('',(-2.94122604762498,0.00270348896235926,4.17782388291051));
#90783=CARTESIAN_POINT('',(-2.942,-3.60291088309151E-16,0.));
#90784=CARTESIAN_POINT('Ctrl Pts',(-2.94172250344281,0.00271694754677573,
4.3221761170896));
#90785=CARTESIAN_POINT('Ctrl Pts',(-2.9438999436428,0.240100699663681,4.30933348490409));
#90786=CARTESIAN_POINT('Ctrl Pts',(-2.91758898170167,0.477007792036415,
4.29649085271859));
#90787=CARTESIAN_POINT('Ctrl Pts',(-2.86094144805788,0.706424172715316,
4.28364822053308));
#90788=CARTESIAN_POINT('Ctrl Pts',(-2.62706845478522,1.65358448498141,4.2306265859177));
#90789=CARTESIAN_POINT('Ctrl Pts',(-1.87610725072441,2.47306528404282,4.17760495130231));
#90790=CARTESIAN_POINT('Ctrl Pts',(-0.952915541058148,2.78854317750225,
4.12458331668693));
#90791=CARTESIAN_POINT('Ctrl Pts',(-0.0297238313918914,3.10402107096167,
4.07156168207154));
#90792=CARTESIAN_POINT('Ctrl Pts',(1.06569838387982,2.91549605881912,4.01854004745616));
#90793=CARTESIAN_POINT('Ctrl Pts',(1.8303094172875,2.30954292397576,3.96551841284077));
#90794=CARTESIAN_POINT('Ctrl Pts',(2.5949204506952,1.7035897891324,3.91249677822539));
#90795=CARTESIAN_POINT('Ctrl Pts',(3.02872030223887,0.680208531588234,3.85947514361001));
#90796=CARTESIAN_POINT('Ctrl Pts',(2.93249865246612,-0.290641934962542,
3.80645350899462));
#90797=CARTESIAN_POINT('Ctrl Pts',(2.83627700269337,-1.26149240151332,3.75343187437924));
#90798=CARTESIAN_POINT('Ctrl Pts',(2.21003385160419,-2.1798120770707,3.70041023976385));
#90799=CARTESIAN_POINT('Ctrl Pts',(1.3413536641399,-2.6238886084906,3.64738860514846));
#90800=CARTESIAN_POINT('Ctrl Pts',(0.472673476675607,-3.06796513991049,
3.59436697053308));
#90801=CARTESIAN_POINT('Ctrl Pts',(-0.638443747163792,-3.03779852719289,
3.5413453359177));
#90802=CARTESIAN_POINT('Ctrl Pts',(-1.48174883110658,-2.54724193593031,
3.48832370130231));
#90803=CARTESIAN_POINT('Ctrl Pts',(-2.32505391504936,-2.05668534466774,
3.43530206668693));
#90804=CARTESIAN_POINT('Ctrl Pts',(-2.90054685909553,-1.10573877486018,
3.38228043207154));
#90805=CARTESIAN_POINT('Ctrl Pts',(-2.94394879594488,-0.131097555060847,
3.32925879745616));
#90806=CARTESIAN_POINT('Ctrl Pts',(-2.94588135327563,-0.0876997214407355,
3.32689790400064));
#90807=CARTESIAN_POINT('Ctrl Pts',(-2.94675895916341,-0.0442549095690453,
3.32453701054511));
#90808=CARTESIAN_POINT('Ctrl Pts',(-2.94660142545168,-0.00080359277598141,
3.32217611708959));
#90809=CARTESIAN_POINT('Ctrl Pts',(-2.94677574562124,-0.00048046415745224,
3.1778238829105));
#90810=CARTESIAN_POINT('Ctrl Pts',(-2.94683369052153,-0.0261291578587509,
3.17921770518885));
#90811=CARTESIAN_POINT('Ctrl Pts',(-2.9465279123969,-0.0517764345476016,
3.1806115274672));
#90812=CARTESIAN_POINT('Ctrl Pts',(-2.94585418233316,-0.0774140418253259,
3.18200534974556));
#90813=CARTESIAN_POINT('Ctrl Pts',(-2.92021948580598,-1.0528971286279,3.23503877224132));
#90814=CARTESIAN_POINT('Ctrl Pts',(-2.36189349098687,-2.01438161773467,
3.28807219473707));
#90815=CARTESIAN_POINT('Ctrl Pts',(-1.52737599577425,-2.52015323654691,
3.34110561723283));
#90816=CARTESIAN_POINT('Ctrl Pts',(-0.69285850056163,-3.02592485535916,
3.39413903972859));
#90817=CARTESIAN_POINT('Ctrl Pts',(0.417850495044496,-3.0759836038769,3.44717246222435));
#90818=CARTESIAN_POINT('Ctrl Pts',(1.29448167466864,-2.64733205050477,3.50020588472011));
#90819=CARTESIAN_POINT('Ctrl Pts',(2.17111285429278,-2.21868049713266,3.55323930721587));
#90820=CARTESIAN_POINT('Ctrl Pts',(2.81366621793492,-1.31131864187067,3.60627272971163));
#90821=CARTESIAN_POINT('Ctrl Pts',(2.92694719068011,-0.342096374378361,
3.65930615220739));
#90822=CARTESIAN_POINT('Ctrl Pts',(3.04022816342529,0.627125893113943,3.71233957470315));
#90823=CARTESIAN_POINT('Ctrl Pts',(2.62423674527353,1.65820857283657,3.76537299719891));
#90824=CARTESIAN_POINT('Ctrl Pts',(1.87008299284461,2.27746336585166,3.81840641969467));
#90825=CARTESIAN_POINT('Ctrl Pts',(1.11592924041568,2.89671815886675,3.87143984219043));
#90826=CARTESIAN_POINT('Ctrl Pts',(0.0236131537096002,3.1041450651743,3.92447326468619));
#90827=CARTESIAN_POINT('Ctrl Pts',(-0.905045809395506,2.80445036847489,
3.97750668718195));
#90828=CARTESIAN_POINT('Ctrl Pts',(-1.83370477250061,2.50475567177548,4.03054010967771));
#90829=CARTESIAN_POINT('Ctrl Pts',(-2.59870661200473,1.69793937206912,4.08357353217347));
#90830=CARTESIAN_POINT('Ctrl Pts',(-2.84860286558964,0.754659856831406,
4.13660695466923));
#90831=CARTESIAN_POINT('Ctrl Pts',(-2.9133416376511,0.510291417324331,4.15034593074966));
#90832=CARTESIAN_POINT('Ctrl Pts',(-2.94350990785796,0.256764463573631,
4.16408490683008));
#90833=CARTESIAN_POINT('Ctrl Pts',(-2.94122604762498,0.00270348896235926,
4.17782388291051));
#90834=CARTESIAN_POINT('Origin',(0.,0.,0.));
#90835=CARTESIAN_POINT('',(-2.93720214312355,-0.000469105519047275,5.3221761170896));
#90836=CARTESIAN_POINT('',(-2.93728841713612,-0.000715510856791167,5.17782388291051));
#90837=CARTESIAN_POINT('',(-2.942,-3.60291088309151E-16,0.));
#90838=CARTESIAN_POINT('Ctrl Pts',(-2.93720214312355,-0.000469105519047275,
5.3221761170896));
#90839=CARTESIAN_POINT('Ctrl Pts',(-2.93646371746741,0.51995090163242,5.29412995926307));
#90840=CARTESIAN_POINT('Ctrl Pts',(-2.80485920517972,1.04071981632219,5.26608380143654));
#90841=CARTESIAN_POINT('Ctrl Pts',(-2.54457459694768,1.48632472952113,5.23803764361001));
#90842=CARTESIAN_POINT('Ctrl Pts',(-2.05250308116121,2.32874674813021,5.18501600899462));
#90843=CARTESIAN_POINT('Ctrl Pts',(-1.10052368210578,2.9025295761171,5.13199437437923));
#90844=CARTESIAN_POINT('Ctrl Pts',(-0.125806028712567,2.94417966913734,
5.07897273976385));
#90845=CARTESIAN_POINT('Ctrl Pts',(0.848911624680633,2.98582976215758,5.02595110514846));
#90846=CARTESIAN_POINT('Ctrl Pts',(1.84636753241161,2.49534712021119,4.97292947053308));
#90847=CARTESIAN_POINT('Ctrl Pts',(2.40850826444871,1.69797203189426,4.9199078359177));
#90848=CARTESIAN_POINT('Ctrl Pts',(2.97064899648583,0.90059694357731,4.86688620130232));
#90849=CARTESIAN_POINT('Ctrl Pts',(3.09747455282905,-0.203670591110202,
4.81386456668693));
#90850=CARTESIAN_POINT('Ctrl Pts',(2.73074388176872,-1.10772692176276,4.76084293207154));
#90851=CARTESIAN_POINT('Ctrl Pts',(2.36401321070839,-2.01178325241532,4.70782129745616));
#90852=CARTESIAN_POINT('Ctrl Pts',(1.50372631224452,-2.71562837903293,4.65479966284077));
#90853=CARTESIAN_POINT('Ctrl Pts',(0.544945626332551,-2.8960413231487,4.60177802822539));
#90854=CARTESIAN_POINT('Ctrl Pts',(-0.413835059579424,-3.07645426726447,
4.54875639361));
#90855=CARTESIAN_POINT('Ctrl Pts',(-1.47110953293949,-2.73343502887838,
4.49573475899462));
#90856=CARTESIAN_POINT('Ctrl Pts',(-2.14135437837727,-2.02450549694995,
4.44271312437924));
#90857=CARTESIAN_POINT('Ctrl Pts',(-2.64925590704205,-1.48728929091278,
4.40253412194936));
#90858=CARTESIAN_POINT('Ctrl Pts',(-2.93491024145304,-0.739953419037798,
4.36235511951948));
#90859=CARTESIAN_POINT('Ctrl Pts',(-2.94172250344281,0.00271694754677573,
4.3221761170896));
#90860=CARTESIAN_POINT('Ctrl Pts',(-2.94122604762498,0.00270348896235926,
4.17782388291051));
#90861=CARTESIAN_POINT('Ctrl Pts',(-2.93469404531129,-0.723928924883364,
4.21711832932584));
#90862=CARTESIAN_POINT('Ctrl Pts',(-2.66270342590315,-1.45492963249676,
4.25641277574117));
#90863=CARTESIAN_POINT('Ctrl Pts',(-2.17481432996248,-1.98852518595228,
4.2957072221565));
#90864=CARTESIAN_POINT('Ctrl Pts',(-1.51633887308468,-2.70868798272918,
4.34874064465227));
#90865=CARTESIAN_POINT('Ctrl Pts',(-0.464597291663352,-3.0692708455139,
4.40177406714803));
#90866=CARTESIAN_POINT('Ctrl Pts',(0.497231234682031,-2.90461888803337,
4.45480748964379));
#90867=CARTESIAN_POINT('Ctrl Pts',(1.45905976102742,-2.73996693055284,4.50784091213955));
#90868=CARTESIAN_POINT('Ctrl Pts',(2.33097523229686,-2.05008015280707,4.5608743346353));
#90869=CARTESIAN_POINT('Ctrl Pts',(2.71241213919701,-1.15189850786832,4.61390775713106));
#90870=CARTESIAN_POINT('Ctrl Pts',(3.09384904609714,-0.253716862929587,
4.66694117962682));
#90871=CARTESIAN_POINT('Ctrl Pts',(2.984807388628,0.852759649202112,4.71997460212259));
#90872=CARTESIAN_POINT('Ctrl Pts',(2.43538184742155,1.65920614828456,4.77300802461835));
#90873=CARTESIAN_POINT('Ctrl Pts',(1.88595630621511,2.46565264736702,4.82604144711411));
#90874=CARTESIAN_POINT('Ctrl Pts',(0.896146881271349,2.97206913340023,4.87907486960986));
#90875=CARTESIAN_POINT('Ctrl Pts',(-0.0793194161058163,2.94580349235183,
4.93210829210562));
#90876=CARTESIAN_POINT('Ctrl Pts',(-1.05478571348298,2.91953785130342,4.98514171460138));
#90877=CARTESIAN_POINT('Ctrl Pts',(-2.01590888329356,2.36059008317341,5.03817513709714));
#90878=CARTESIAN_POINT('Ctrl Pts',(-2.52114062795194,1.52574562735251,5.0912085595929));
#90879=CARTESIAN_POINT('Ctrl Pts',(-2.79619240256571,1.0712503357804,5.1200803340321));
#90880=CARTESIAN_POINT('Ctrl Pts',(-2.93612746598571,0.53498501956348,5.14895210847131));
#90881=CARTESIAN_POINT('Ctrl Pts',(-2.93728841713612,-0.000715510856791167,
5.17782388291051));
#90882=CARTESIAN_POINT('Origin',(0.,0.,0.));
#90883=CARTESIAN_POINT('',(-2.94344957106371,-0.00254475878011751,6.32217611708959));
#90884=CARTESIAN_POINT('',(-2.94385951897541,-0.00245237012002547,6.17782388291051));
#90885=CARTESIAN_POINT('',(-2.942,-3.60291088309151E-16,0.));
#90886=CARTESIAN_POINT('Ctrl Pts',(-2.94344957106371,-0.00254475878011751,
6.32217611708959));
#90887=CARTESIAN_POINT('Ctrl Pts',(-2.93616232120099,0.795681372462419,
6.27892643362204));
#90888=CARTESIAN_POINT('Ctrl Pts',(-2.59990813395451,1.59931200027747,6.23567675015448));
#90889=CARTESIAN_POINT('Ctrl Pts',(-2.02065345820614,2.14498966963894,6.19242706668693));
#90890=CARTESIAN_POINT('Ctrl Pts',(-1.31052040509786,2.81395923618761,6.13940543207154));
#90891=CARTESIAN_POINT('Ctrl Pts',(-0.235173278132946,3.0952421301662,6.08638379745616));
#90892=CARTESIAN_POINT('Ctrl Pts',(0.711565152013647,2.85966713368149,6.03336216284077));
#90893=CARTESIAN_POINT('Ctrl Pts',(1.65830358216024,2.62409213719678,5.98034052822539));
#90894=CARTESIAN_POINT('Ctrl Pts',(2.47643331548851,1.87165925024877,5.92731889361));
#90895=CARTESIAN_POINT('Ctrl Pts',(2.79025139845639,0.947902006765649,5.87429725899462));
#90896=CARTESIAN_POINT('Ctrl Pts',(3.10406948142426,0.024144763282521,5.82127562437923));
#90897=CARTESIAN_POINT('Ctrl Pts',(2.91357591403173,-1.07093683673572,5.76825398976385));
#90898=CARTESIAN_POINT('Ctrl Pts',(2.30624948232532,-1.83445752370893,5.71523235514847));
#90899=CARTESIAN_POINT('Ctrl Pts',(1.6989230506189,-2.59797821068214,5.66221072053309));
#90900=CARTESIAN_POINT('Ctrl Pts',(0.674763754598609,-3.02993798461032,
5.6091890859177));
#90901=CARTESIAN_POINT('Ctrl Pts',(-0.29591219946945,-2.93197152974308,
5.55616745130231));
#90902=CARTESIAN_POINT('Ctrl Pts',(-1.26658815353752,-2.83400507487583,
5.50314581668693));
#90903=CARTESIAN_POINT('Ctrl Pts',(-2.18378076565335,-2.20611239121314,
5.45012418207154));
#90904=CARTESIAN_POINT('Ctrl Pts',(-2.6262952554525,-1.33663544476617,5.39710254745616));
#90905=CARTESIAN_POINT('Ctrl Pts',(-2.83473866631452,-0.927074301433759,
5.37212707066731));
#90906=CARTESIAN_POINT('Ctrl Pts',(-2.93785972099746,-0.463910047749339,
5.34715159387845));
#90907=CARTESIAN_POINT('Ctrl Pts',(-2.93720214312355,-0.000469105519047275,
5.3221761170896));
#90908=CARTESIAN_POINT('Ctrl Pts',(-2.93728841713612,-0.000715510856791167,
5.17782388291051));
#90909=CARTESIAN_POINT('Ctrl Pts',(-2.93825997131497,-0.449022133194243,
5.20198553096707));
#90910=CARTESIAN_POINT('Ctrl Pts',(-2.84204308495302,-0.896933215975224,
5.22614717902362));
#90911=CARTESIAN_POINT('Ctrl Pts',(-2.64649421691623,-1.29619371435045,
5.25030882708018));
#90912=CARTESIAN_POINT('Ctrl Pts',(-2.21727574171593,-2.17254745672079,
5.30334224957594));
#90913=CARTESIAN_POINT('Ctrl Pts',(-1.30949847180912,-2.81451379794974,
5.3563756720717));
#90914=CARTESIAN_POINT('Ctrl Pts',(-0.34020313693593,-2.92716784809496,
5.40940909456746));
#90915=CARTESIAN_POINT('Ctrl Pts',(0.629092197937262,-3.03982189824018,
5.46244251706321));
#90916=CARTESIAN_POINT('Ctrl Pts',(1.65990559777684,-2.62316365730168,5.51547593955898));
#90917=CARTESIAN_POINT('Ctrl Pts',(2.2786724705311,-1.86860952511248,5.56850936205474));
#90918=CARTESIAN_POINT('Ctrl Pts',(2.89743934328536,-1.11405539292327,5.6215427845505));
#90919=CARTESIAN_POINT('Ctrl Pts',(3.1041596889543,-0.0216053694833598,
5.67457620704626));
#90920=CARTESIAN_POINT('Ctrl Pts',(2.80386439268148,0.90685955514088,5.72760962954202));
#90921=CARTESIAN_POINT('Ctrl Pts',(2.50356909640867,1.8353244797651,5.78064305203778));
#90922=CARTESIAN_POINT('Ctrl Pts',(1.69625815819413,2.59980430557365,5.83367647453354));
#90923=CARTESIAN_POINT('Ctrl Pts',(0.752817206002227,2.84909038811436,5.8867098970293));
#90924=CARTESIAN_POINT('Ctrl Pts',(-0.190623746189707,3.09837647065508,
5.93974331952506));
#90925=CARTESIAN_POINT('Ctrl Pts',(-1.27019471235901,2.83246880992794,5.99277674202081));
#90926=CARTESIAN_POINT('Ctrl Pts',(-1.98993145274738,2.17352768527678,6.04581016451657));
#90927=CARTESIAN_POINT('Ctrl Pts',(-2.5871342410519,1.62677016285567,6.08981473731455));
#90928=CARTESIAN_POINT('Ctrl Pts',(-2.93659552111978,0.809413858651952,
6.13381931011253));
#90929=CARTESIAN_POINT('Ctrl Pts',(-2.94385951897541,-0.00245237012002547,
6.17782388291051));
#90930=CARTESIAN_POINT('Origin',(0.,0.,0.));
#90931=CARTESIAN_POINT('',(-2.94561041112727,0.0017180900162133,7.3221761170896));
#90932=CARTESIAN_POINT('',(-2.94532408079935,0.00188850225021302,7.17782388291051));
#90933=CARTESIAN_POINT('',(-2.942,-3.60291088309151E-16,0.));
#90934=CARTESIAN_POINT('Ctrl Pts',(-2.94561041112727,0.0017180900162133,
7.3221761170896));
#90935=CARTESIAN_POINT('Ctrl Pts',(-2.94630377550943,0.101773161046659,
7.3167445425964));
#90936=CARTESIAN_POINT('Ctrl Pts',(-2.94164939634066,0.201762961465683,
7.3113129681032));
#90937=CARTESIAN_POINT('Ctrl Pts',(-2.93143493536931,0.301181507922605,
7.30588139361001));
#90938=CARTESIAN_POINT('Ctrl Pts',(-2.83172399186774,1.271679813862,7.25285975899462));
#90939=CARTESIAN_POINT('Ctrl Pts',(-2.20218380394821,2.18774239999403,7.19983812437924));
#90940=CARTESIAN_POINT('Ctrl Pts',(-1.33191290738037,2.62869341844419,7.14681648976385));
#90941=CARTESIAN_POINT('Ctrl Pts',(-0.46164201081253,3.06964443689435,7.09379485514847));
#90942=CARTESIAN_POINT('Ctrl Pts',(0.649359594403592,3.03548388766263,7.04077322053308));
#90943=CARTESIAN_POINT('Ctrl Pts',(1.49089582631948,2.54189903735011,6.9877515859177));
#90944=CARTESIAN_POINT('Ctrl Pts',(2.33243205823535,2.04831418703759,6.93472995130231));
#90945=CARTESIAN_POINT('Ctrl Pts',(2.90450291685098,1.09530503564424,6.88170831668693));
#90946=CARTESIAN_POINT('Ctrl Pts',(2.94440103136477,0.120514096753516,6.82868668207154));
#90947=CARTESIAN_POINT('Ctrl Pts',(2.98429914587856,-0.85427684213721,6.77566504745616));
#90948=CARTESIAN_POINT('Ctrl Pts',(2.49202451629054,-1.85084956852532,6.72264341284077));
#90949=CARTESIAN_POINT('Ctrl Pts',(1.69364035086188,-2.41155622844475,6.66962177822539));
#90950=CARTESIAN_POINT('Ctrl Pts',(0.895256185433229,-2.97226288836418,
6.61660014361));
#90951=CARTESIAN_POINT('Ctrl Pts',(-0.209237515836049,-3.09710348181494,
6.56357850899462));
#90952=CARTESIAN_POINT('Ctrl Pts',(-1.11263324192275,-2.72874849518725,
6.51055687437924));
#90953=CARTESIAN_POINT('Ctrl Pts',(-2.01602896800946,-2.36039350855957,
6.45753523976386));
#90954=CARTESIAN_POINT('Ctrl Pts',(-2.71832671891359,-1.49884294185344,
6.40451360514847));
#90955=CARTESIAN_POINT('Ctrl Pts',(-2.89701610473984,-0.539739538940995,
6.35149197053308));
#90956=CARTESIAN_POINT('Ctrl Pts',(-2.9299487738587,-0.362975626116294,
6.34172001938525));
#90957=CARTESIAN_POINT('Ctrl Pts',(-2.9450960721234,-0.182898142528554,
6.33194806823742));
#90958=CARTESIAN_POINT('Ctrl Pts',(-2.94344957106371,-0.00254475878011751,
6.32217611708959));
#90959=CARTESIAN_POINT('Ctrl Pts',(-2.94385951897541,-0.00245237012002547,
6.17782388291051));
#90960=CARTESIAN_POINT('Ctrl Pts',(-2.94534994464423,-0.169030925215637,
6.18685273260829));
#90961=CARTESIAN_POINT('Ctrl Pts',(-2.93243429156208,-0.335378354983467,
6.19588158230608));
#90962=CARTESIAN_POINT('Ctrl Pts',(-2.90429666833196,-0.499109855256177,
6.20491043200386));
#90963=CARTESIAN_POINT('Ctrl Pts',(-2.73902262892075,-1.46083168256277,
6.25794385449962));
#90964=CARTESIAN_POINT('Ctrl Pts',(-2.04857203549091,-2.33230074860083,
6.31097727699537));
#90965=CARTESIAN_POINT('Ctrl Pts',(-1.15014386281302,-2.71315662653886,
6.36401069949113));
#90966=CARTESIAN_POINT('Ctrl Pts',(-0.251715690135105,-3.09401250447689,
6.41704412198689));
#90967=CARTESIAN_POINT('Ctrl Pts',(0.854690061790863,-2.98425519431488,
6.47007754448265));
#90968=CARTESIAN_POINT('Ctrl Pts',(1.66078102051885,-2.43430815370249,6.52311096697841));
#90969=CARTESIAN_POINT('Ctrl Pts',(2.46687197924684,-1.8843611130901,6.57614438947417));
#90970=CARTESIAN_POINT('Ctrl Pts',(2.97264814477684,-0.89422434202733,6.62917781196992));
#90971=CARTESIAN_POINT('Ctrl Pts',(2.94575157188272,0.0812247625331604,
6.68221123446569));
#90972=CARTESIAN_POINT('Ctrl Pts',(2.91885499898859,1.05667386709364,6.73524465696145));
#90973=CARTESIAN_POINT('Ctrl Pts',(2.35928568767037,2.01743530515185,6.78827807945721));
#90974=CARTESIAN_POINT('Ctrl Pts',(1.52411461962062,2.52212696182345,6.84131150195297));
#90975=CARTESIAN_POINT('Ctrl Pts',(0.688943551570855,3.02681861849506,6.89434492444873));
#90976=CARTESIAN_POINT('Ctrl Pts',(-0.421829273210428,3.07544049378006,
6.94737834694448));
#90977=CARTESIAN_POINT('Ctrl Pts',(-1.29790521123388,2.64565527761082,7.00041176944024));
#90978=CARTESIAN_POINT('Ctrl Pts',(-2.17398114925735,2.21587006144158,7.053445191936));
#90979=CARTESIAN_POINT('Ctrl Pts',(-2.81536020052296,1.30767775381808,7.10647861443177));
#90980=CARTESIAN_POINT('Ctrl Pts',(-2.92738728118153,0.338309756398913,
7.15951203692753));
#90981=CARTESIAN_POINT('Ctrl Pts',(-2.94028117934613,0.226739123929774,
7.16561598558852));
#90982=CARTESIAN_POINT('Ctrl Pts',(-2.94616267287143,0.114358087958319,
7.17171993424952));
#90983=CARTESIAN_POINT('Ctrl Pts',(-2.94532408079935,0.00188850225021302,
7.17782388291051));
#90984=CARTESIAN_POINT('Origin',(0.,0.,0.));
#90985=CARTESIAN_POINT('',(-2.93809888154578,0.00167770611676693,8.3221761170896));
#90986=CARTESIAN_POINT('',(-2.93791306433702,0.00153065962940209,8.17782388291051));
#90987=CARTESIAN_POINT('',(-2.942,-3.60291088309151E-16,0.));
#90988=CARTESIAN_POINT('Ctrl Pts',(-2.93809888154578,0.00167770611676693,
8.3221761170896));
#90989=CARTESIAN_POINT('Ctrl Pts',(-2.94007633420882,0.384287406036693,
8.30154101695538));
#90990=CARTESIAN_POINT('Ctrl Pts',(-2.87073335467684,0.766208258950615,
8.28090591682115));
#90991=CARTESIAN_POINT('Ctrl Pts',(-2.72674429344234,1.11753596774236,8.26027081668693));
#90992=CARTESIAN_POINT('Ctrl Pts',(-2.35676618120986,2.02026817086468,8.20724918207155));
#90993=CARTESIAN_POINT('Ctrl Pts',(-1.49395472948062,2.72101627730632,8.15422754745616));
#90994=CARTESIAN_POINT('Ctrl Pts',(-0.534531707931531,2.89798152758675,
8.10120591284077));
#90995=CARTESIAN_POINT('Ctrl Pts',(0.424891313617566,3.07494677786719,8.04818427822539));
#90996=CARTESIAN_POINT('Ctrl Pts',(1.48092590498651,2.72812917198643,7.99516264361001));
#90997=CARTESIAN_POINT('Ctrl Pts',(2.14861803155556,2.0167948917757,7.94214100899462));
#90998=CARTESIAN_POINT('Ctrl Pts',(2.81631015812461,1.30546061156497,7.88911937437924));
#90999=CARTESIAN_POINT('Ctrl Pts',(3.09565981989376,0.229609657024259,7.83609773976385));
#91000=CARTESIAN_POINT('Ctrl Pts',(2.85838358121436,-0.716703832599229,
7.78307610514847));
#91001=CARTESIAN_POINT('Ctrl Pts',(2.62110734253496,-1.6630173222227,7.73005447053308));
#91002=CARTESIAN_POINT('Ctrl Pts',(1.86720520340702,-2.47979334692897,7.6770328359177));
#91003=CARTESIAN_POINT('Ctrl Pts',(0.942885410290185,-2.79195060559462,
7.62401120130232));
#91004=CARTESIAN_POINT('Ctrl Pts',(0.0185656171733344,-3.10410786426027,
7.57098956668693));
#91005=CARTESIAN_POINT('Ctrl Pts',(-1.07617182993241,-2.91164635688529,
7.51796793207155));
#91006=CARTESIAN_POINT('Ctrl Pts',(-1.83859970394347,-2.30294859032442,
7.46494629745616));
#91007=CARTESIAN_POINT('Ctrl Pts',(-2.52292391662041,-1.75660626200873,
7.41735623733397));
#91008=CARTESIAN_POINT('Ctrl Pts',(-2.93953533056363,-0.874938734231028,
7.36976617721179));
#91009=CARTESIAN_POINT('Ctrl Pts',(-2.94561041112727,0.0017180900162133,
7.3221761170896));
#91010=CARTESIAN_POINT('Ctrl Pts',(-2.94532408079935,0.00188850225021302,
7.17782388291051));
#91011=CARTESIAN_POINT('Ctrl Pts',(-2.93887666669244,-0.862820356365606,
7.22475335674527));
#91012=CARTESIAN_POINT('Ctrl Pts',(-2.53519706632201,-1.73276349436296,
7.27168283058004));
#91013=CARTESIAN_POINT('Ctrl Pts',(-1.8671352754884,-2.27988062150739,7.3186123044148));
#91014=CARTESIAN_POINT('Ctrl Pts',(-1.11218107908521,-2.89815931477968,
7.37164572691056));
#91015=CARTESIAN_POINT('Ctrl Pts',(-0.0195975762272904,-3.10417301410946,
7.42467914940632));
#91016=CARTESIAN_POINT('Ctrl Pts',(0.908672921418664,-2.80327724408032,
7.47771257190208));
#91017=CARTESIAN_POINT('Ctrl Pts',(1.83694341906463,-2.50238147405117,7.53074599439785));
#91018=CARTESIAN_POINT('Ctrl Pts',(2.60090091149863,-1.69457623466311,7.5837794168936));
#91019=CARTESIAN_POINT('Ctrl Pts',(2.84957671873934,-0.750974240115352,
7.63681283938936));
#91020=CARTESIAN_POINT('Ctrl Pts',(3.09825252598004,0.192627754432404,7.68984626188512));
#91021=CARTESIAN_POINT('Ctrl Pts',(2.83164664802746,1.27202650413984,7.74287968438088));
#91022=CARTESIAN_POINT('Ctrl Pts',(2.17224013125782,1.99133688698097,7.79591310687664));
#91023=CARTESIAN_POINT('Ctrl Pts',(1.51283361448819,2.71064726982209,7.8489465293724));
#91024=CARTESIAN_POINT('Ctrl Pts',(0.460626458901515,3.06986928579691,7.90197995186816));
#91025=CARTESIAN_POINT('Ctrl Pts',(-0.500988267012792,2.90397323362554,
7.95501337436392));
#91026=CARTESIAN_POINT('Ctrl Pts',(-1.46260299292711,2.73807718145418,8.00804679685968));
#91027=CARTESIAN_POINT('Ctrl Pts',(-2.33362528916906,2.04706306113661,8.06108021935544));
#91028=CARTESIAN_POINT('Ctrl Pts',(-2.71389997881596,1.14838873656999,8.1141136418512));
#91029=CARTESIAN_POINT('Ctrl Pts',(-2.86617748613125,0.788522856039455,
8.13535038887097));
#91030=CARTESIAN_POINT('Ctrl Pts',(-2.93976221721368,0.395358070397946,
8.15658713589074));
#91031=CARTESIAN_POINT('Ctrl Pts',(-2.93791306433702,0.00153065962940209,
8.17782388291051));
#91032=CARTESIAN_POINT('Origin',(0.,0.,0.));
#91033=CARTESIAN_POINT('',(-2.93946271110901,-0.00237070406174211,9.3221761170896));
#91034=CARTESIAN_POINT('',(-2.93970717506282,-0.00244914695740897,9.1778238829105));
#91035=CARTESIAN_POINT('',(-2.942,-3.60291088309151E-16,0.));
#91036=CARTESIAN_POINT('Ctrl Pts',(-2.93946271110901,-0.00237070406174211,
9.3221761170896));
#91037=CARTESIAN_POINT('Ctrl Pts',(-2.93446464588925,0.661363954518237,
9.28633749131435));
#91038=CARTESIAN_POINT('Ctrl Pts',(-2.71199962688196,1.32813253283145,9.2504988655391));
#91039=CARTESIAN_POINT('Ctrl Pts',(-2.29964025869718,1.84273594462077,9.21466023976385));
#91040=CARTESIAN_POINT('Ctrl Pts',(-1.68957312366702,2.60406854266272,9.16163860514847));
#91041=CARTESIAN_POINT('Ctrl Pts',(-0.663867679221267,3.03234398107946,
9.10861697053308));
#91042=CARTESIAN_POINT('Ctrl Pts',(0.306449843415351,2.93088887105754,9.0555953359177));
#91043=CARTESIAN_POINT('Ctrl Pts',(1.27676736605195,2.82943376103562,9.00257370130232));
#91044=CARTESIAN_POINT('Ctrl Pts',(2.19169696687942,2.19824810257508,8.94955206668694));
#91045=CARTESIAN_POINT('Ctrl Pts',(2.63108308949774,1.32718606727815,8.89653043207155));
#91046=CARTESIAN_POINT('Ctrl Pts',(3.07046921211607,0.456124031981203,8.84350879745617));
#91047=CARTESIAN_POINT('Ctrl Pts',(3.03431185652521,-0.654814380152138,
8.79048716284078));
#91048=CARTESIAN_POINT('Ctrl Pts',(2.53921526620191,-1.49546210681027,8.73746552822539));
#91049=CARTESIAN_POINT('Ctrl Pts',(2.04411867587862,-2.33610983346839,8.68444389361001));
#91050=CARTESIAN_POINT('Ctrl Pts',(1.09008285082291,-2.90646687465129,8.63142225899462));
#91051=CARTESIAN_POINT('Ctrl Pts',(0.115221775476145,-2.94461288176806,
8.57840062437923));
#91052=CARTESIAN_POINT('Ctrl Pts',(-0.85963929987063,-2.98275888888482,
8.52537898976385));
#91053=CARTESIAN_POINT('Ctrl Pts',(-1.85532562550848,-2.48869386193542,
8.47235735514847));
#91054=CARTESIAN_POINT('Ctrl Pts',(-2.41459640195952,-1.6893031985592,8.41933572053308));
#91055=CARTESIAN_POINT('Ctrl Pts',(-2.75620869696377,-1.20102150993995,
8.38694918605192));
#91056=CARTESIAN_POINT('Ctrl Pts',(-2.9349952940449,-0.598823486447531,
8.35456265157076));
#91057=CARTESIAN_POINT('Ctrl Pts',(-2.93809888154578,0.00167770611676693,
8.3221761170896));
#91058=CARTESIAN_POINT('Ctrl Pts',(-2.93791306433702,0.00153065962940209,
8.17782388291051));
#91059=CARTESIAN_POINT('Ctrl Pts',(-2.9351444240236,-0.588126615192338,
8.2096205583865));
#91060=CARTESIAN_POINT('Ctrl Pts',(-2.7632717718794,-1.17926933079271,8.24141723386249));
#91061=CARTESIAN_POINT('Ctrl Pts',(-2.4332334415684,-1.66235519794395,8.27321390933847));
#91062=CARTESIAN_POINT('Ctrl Pts',(-1.88276513162211,-2.46809027907558,
8.32624733183424));
#91063=CARTESIAN_POINT('Ctrl Pts',(-0.892301428677693,-2.97322591252315,
8.37928075433));
#91064=CARTESIAN_POINT('Ctrl Pts',(0.0831300749779144,-2.94569841903957,
8.43231417682576));
#91065=CARTESIAN_POINT('Ctrl Pts',(1.0585615786335,-2.91817092555599,8.48534759932152));
#91066=CARTESIAN_POINT('Ctrl Pts',(2.01896088300028,-2.35798030514126,8.53838102181727));
#91067=CARTESIAN_POINT('Ctrl Pts',(2.52311224054409,-1.52248297426101,8.59141444431303));
#91068=CARTESIAN_POINT('Ctrl Pts',(3.02726359808791,-0.686985643380747,
8.64444786680879));
#91069=CARTESIAN_POINT('Ctrl Pts',(3.07516700880875,0.423818397965051,8.69748128930456));
#91070=CARTESIAN_POINT('Ctrl Pts',(2.64481523147421,1.29961616512727,8.75051471180032));
#91071=CARTESIAN_POINT('Ctrl Pts',(2.21446345413967,2.17541393228948,8.80354813429608));
#91072=CARTESIAN_POINT('Ctrl Pts',(1.30585648874975,2.81620542526811,8.85658155679183));
#91073=CARTESIAN_POINT('Ctrl Pts',(0.336416234327566,2.92760548957316,8.90961497928759));
#91074=CARTESIAN_POINT('Ctrl Pts',(-0.633024020094595,3.03900555387821,
8.96264840178335));
#91075=CARTESIAN_POINT('Ctrl Pts',(-1.66329756354901,2.62101418950972,9.01568182427912));
#91076=CARTESIAN_POINT('Ctrl Pts',(-2.2810878186777,1.86566024473329,9.06871524677488));
#91077=CARTESIAN_POINT('Ctrl Pts',(-2.70475933865403,1.34764955866819,9.10508479215342));
#91078=CARTESIAN_POINT('Ctrl Pts',(-2.93443931783068,0.67097671916862,9.14145433753196));
#91079=CARTESIAN_POINT('Ctrl Pts',(-2.93970717506282,-0.00244914695740897,
9.1778238829105));
#91080=CARTESIAN_POINT('Origin',(0.,0.,0.));
#91081=CARTESIAN_POINT('',(-2.94667766504495,-0.000677344457850615,10.3221761170896));
#91082=CARTESIAN_POINT('',(-2.94675654686086,-0.000527081537143387,10.1778238829105));
#91083=CARTESIAN_POINT('',(-2.942,-3.60291088309151E-16,0.));
#91084=CARTESIAN_POINT('Ctrl Pts',(-2.94667766504495,-0.000677344457850615,
10.3221761170896));
#91085=CARTESIAN_POINT('Ctrl Pts',(-2.9437606123768,0.938668430873604,10.2711339656733));
#91086=CARTESIAN_POINT('Ctrl Pts',(-2.45547363684786,1.8806215504616,10.2200918142571));
#91087=CARTESIAN_POINT('Ctrl Pts',(-1.68496058899857,2.41762877517203,10.1690496628408));
#91088=CARTESIAN_POINT('Ctrl Pts',(-0.884566010089308,2.97546186144238,
10.1160280282254));
#91089=CARTESIAN_POINT('Ctrl Pts',(0.22036931948501,3.09633132563897,10.06300639361));
#91090=CARTESIAN_POINT('Ctrl Pts',(1.12243508338583,2.72473128300808,10.0099847589946));
#91091=CARTESIAN_POINT('Ctrl Pts',(2.02450084728663,2.35313124037721,9.95696312437924));
#91092=CARTESIAN_POINT('Ctrl Pts',(2.72369704551392,1.48906169091887,9.90394148976386));
#91093=CARTESIAN_POINT('Ctrl Pts',(2.89893758856608,0.529322150128768,9.85091985514847));
#91094=CARTESIAN_POINT('Ctrl Pts',(3.07417813161823,-0.430417390661342,
9.79789822053309));
#91095=CARTESIAN_POINT('Ctrl Pts',(2.72546301949522,-1.48582692278323,9.7448765859177));
#91096=CARTESIAN_POINT('Ctrl Pts',(2.01292981013226,-2.15223945240745,9.69185495130231));
#91097=CARTESIAN_POINT('Ctrl Pts',(1.30039660076932,-2.81865198203167,9.63883331668693));
#91098=CARTESIAN_POINT('Ctrl Pts',(0.22404529416644,-3.09606750915824,9.58581168207154));
#91099=CARTESIAN_POINT('Ctrl Pts',(-0.721840197888351,-2.85709079479997,
9.53279004745616));
#91100=CARTESIAN_POINT('Ctrl Pts',(-1.66772568994314,-2.6181140804417,9.47976841284078));
#91101=CARTESIAN_POINT('Ctrl Pts',(-2.48314536744984,-1.8627451245986,9.42674677822539));
#91102=CARTESIAN_POINT('Ctrl Pts',(-2.79364079339589,-0.937865767843463,
9.37372514361001));
#91103=CARTESIAN_POINT('Ctrl Pts',(-2.89426473091789,-0.638135096043858,
9.35654213476987));
#91104=CARTESIAN_POINT('Ctrl Pts',(-2.94185905854134,-0.320601614404311,
9.33935912592974));
#91105=CARTESIAN_POINT('Ctrl Pts',(-2.93946271110901,-0.00237070406174211,
9.3221761170896));
#91106=CARTESIAN_POINT('Ctrl Pts',(-2.93970717506282,-0.00244914695740897,
9.1778238829105));
#91107=CARTESIAN_POINT('Ctrl Pts',(-2.94212081330531,-0.311000869666037,
9.19448776002772));
#91108=CARTESIAN_POINT('Ctrl Pts',(-2.89742341321448,-0.618870952337822,
9.21115163714493));
#91109=CARTESIAN_POINT('Ctrl Pts',(-2.80268892270593,-0.91048590754583,
9.22781551426215));
#91110=CARTESIAN_POINT('Ctrl Pts',(-2.50119280480251,-1.83856158986408,
9.28084893675791));
#91111=CARTESIAN_POINT('Ctrl Pts',(-1.69289360219275,-2.6019964293162,9.33388235925367));
#91112=CARTESIAN_POINT('Ctrl Pts',(-0.749130960052534,-2.8500618572215,
9.38691578174943));
#91113=CARTESIAN_POINT('Ctrl Pts',(0.194631682087679,-3.09812728512679,
9.43994920424519));
#91114=CARTESIAN_POINT('Ctrl Pts',(1.27385776375836,-2.83082330148527,9.49298262674095));
#91115=CARTESIAN_POINT('Ctrl Pts',(1.99274148812309,-2.17095166846502,9.54601604923671));
#91116=CARTESIAN_POINT('Ctrl Pts',(2.71162521248781,-1.51108003544478,9.59904947173247));
#91117=CARTESIAN_POINT('Ctrl Pts',(3.07016657954661,-0.458640753045832,
9.65208289422823));
#91118=CARTESIAN_POINT('Ctrl Pts',(2.90364858401899,0.50286646917705,9.70511631672399));
#91119=CARTESIAN_POINT('Ctrl Pts',(2.73713058849137,1.46437369139994,9.75814973921975));
#91120=CARTESIAN_POINT('Ctrl Pts',(2.04555323037731,2.33494885344676,9.8111831617155));
#91121=CARTESIAN_POINT('Ctrl Pts',(1.14663312988947,2.71464219571161,9.86421658421126));
#91122=CARTESIAN_POINT('Ctrl Pts',(0.247713029401628,3.09433553797646,9.91725000670703));
#91123=CARTESIAN_POINT('Ctrl Pts',(-0.858549813459989,2.98314706045934,
9.9702834292028));
#91124=CARTESIAN_POINT('Ctrl Pts',(-1.66392867990964,2.4321577114719,10.0233168516986));
#91125=CARTESIAN_POINT('Ctrl Pts',(-2.44605620000286,1.89707546499944,10.0748191954359));
#91126=CARTESIAN_POINT('Ctrl Pts',(-2.94442204707364,0.947219947536058,
10.1263215391732));
#91127=CARTESIAN_POINT('Ctrl Pts',(-2.94675654686086,-0.000527081537143387,
10.1778238829105));
#91128=CARTESIAN_POINT('Origin',(0.,0.,0.));
#91129=CARTESIAN_POINT('',(-2.94150967972677,0.00271347918382847,11.3221761170896));
#91130=CARTESIAN_POINT('',(-2.94130162828673,0.0027079682416201,11.1778238829105));
#91131=CARTESIAN_POINT('',(-2.942,-3.60291088309151E-16,0.));
#91132=CARTESIAN_POINT('Ctrl Pts',(-2.94150967972677,0.00271347918382847,
11.3221761170896));
#91133=CARTESIAN_POINT('Ctrl Pts',(-2.94373491656768,0.247192333748545,
11.3089520746477));
#91134=CARTESIAN_POINT('Ctrl Pts',(-2.9158155052491,0.491169927694146,11.2957280322058));
#91135=CARTESIAN_POINT('Ctrl Pts',(-2.85578877861464,0.726974231288132,
11.2825039897639));
#91136=CARTESIAN_POINT('Ctrl Pts',(-2.61511236058667,1.67242867011129,11.2294823551485));
#91137=CARTESIAN_POINT('Ctrl Pts',(-1.85827902823171,2.48648936622251,11.1764607205331));
#91138=CARTESIAN_POINT('Ctrl Pts',(-0.932843095641359,2.7953219564001,11.1234390859177));
#91139=CARTESIAN_POINT('Ctrl Pts',(-0.00740716305097949,3.1041545465777,
11.0704174513023));
#91140=CARTESIAN_POINT('Ctrl Pts',(1.08663136977481,2.90775903082164,11.0173958166869));
#91141=CARTESIAN_POINT('Ctrl Pts',(1.8468662323789,2.29632449813104,10.9643741820716));
#91142=CARTESIAN_POINT('Ctrl Pts',(2.60710109498298,1.68488996544046,10.9113525474562));
#91143=CARTESIAN_POINT('Ctrl Pts',(3.03353228736538,0.658416415815393,10.8583309128408));
#91144=CARTESIAN_POINT('Ctrl Pts',(2.93033333857171,-0.311717188928345,
10.8053092782254));
#91145=CARTESIAN_POINT('Ctrl Pts',(2.82713438977805,-1.28185079367208,10.75228764361));
#91146=CARTESIAN_POINT('Ctrl Pts',(2.19430529980826,-2.1956444535345,10.6992660089946));
#91147=CARTESIAN_POINT('Ctrl Pts',(1.32245493972955,-2.63346426089346,10.6462443743792));
#91148=CARTESIAN_POINT('Ctrl Pts',(0.450604579650845,-3.07128406825242,
10.5932227397639));
#91149=CARTESIAN_POINT('Ctrl Pts',(-0.66026705053676,-3.03313002310796,
10.5402011051485));
#91150=CARTESIAN_POINT('Ctrl Pts',(-1.50002355624255,-2.53652329217291,
10.4871794705331));
#91151=CARTESIAN_POINT('Ctrl Pts',(-2.33978006194835,-2.03991656123784,
10.4341578359177));
#91152=CARTESIAN_POINT('Ctrl Pts',(-2.90842144317229,-1.08485714451215,
10.3811362013023));
#91153=CARTESIAN_POINT('Ctrl Pts',(-2.94481521966216,-0.109929081977263,
10.3281145666869));
#91154=CARTESIAN_POINT('Ctrl Pts',(-2.94617392671893,-0.0735316050958383,
10.3261350834878));
#91155=CARTESIAN_POINT('Ctrl Pts',(-2.94679079226602,-0.0371064354900674,
10.3241556002887));
#91156=CARTESIAN_POINT('Ctrl Pts',(-2.94667766504495,-0.000677344457850615,
10.3221761170896));
#91157=CARTESIAN_POINT('Ctrl Pts',(-2.94675654686086,-0.000527081537143387,
10.1778238829105));
#91158=CARTESIAN_POINT('Ctrl Pts',(-2.94682594764491,-0.0287020195940664,
10.1793549616689));
#91159=CARTESIAN_POINT('Ctrl Pts',(-2.94645696896677,-0.0568750942243903,
10.1808860404274));
#91160=CARTESIAN_POINT('Ctrl Pts',(-2.94564403384026,-0.0850353526445027,
10.1824171191858));
#91161=CARTESIAN_POINT('Ctrl Pts',(-2.91748563128357,-1.06044884731575,
10.2354505416816));
#91162=CARTESIAN_POINT('Ctrl Pts',(-2.35667393613251,-2.02048561620049,
10.2884839641773));
#91163=CARTESIAN_POINT('Ctrl Pts',(-1.52085069195865,-2.52409646370082,
10.3415173866731));
#91164=CARTESIAN_POINT('Ctrl Pts',(-0.685027447784799,-3.02770731120113,
10.3945508091689));
#91165=CARTESIAN_POINT('Ctrl Pts',(0.425807345411858,-3.07489223731705,
10.4475842316646));
#91166=CARTESIAN_POINT('Ctrl Pts',(1.30132657531592,-2.6439740788583,10.5006176541604));
#91167=CARTESIAN_POINT('Ctrl Pts',(2.17684580522,-2.21305592039955,10.5536510766561));
#91168=CARTESIAN_POINT('Ctrl Pts',(2.81704947183149,-1.3040346773661,10.6066844991519));
#91169=CARTESIAN_POINT('Ctrl Pts',(2.92782247317795,-0.334522571513875,
10.6597179216477));
#91170=CARTESIAN_POINT('Ctrl Pts',(3.0385954745244,0.634989534338361,10.7127513441434));
#91171=CARTESIAN_POINT('Ctrl Pts',(2.61993781060583,1.66499250300936,10.7657847666392));
#91172=CARTESIAN_POINT('Ctrl Pts',(1.8641844334644,2.28229406153701,10.8188181891349));
#91173=CARTESIAN_POINT('Ctrl Pts',(1.10843105632298,2.89959562006465,10.8718516116307));
#91174=CARTESIAN_POINT('Ctrl Pts',(0.0155819659587191,3.10419576844893,
10.9248850341265));
#91175=CARTESIAN_POINT('Ctrl Pts',(-0.912298512764032,2.80209942880452,
10.9779184566222));
#91176=CARTESIAN_POINT('Ctrl Pts',(-1.84017899148677,2.50000308916011,11.030951879118));
#91177=CARTESIAN_POINT('Ctrl Pts',(-2.60309085856801,1.69121026148702,11.0839853016137));
#91178=CARTESIAN_POINT('Ctrl Pts',(-2.85054580335778,0.747287366584909,
11.1370187241095));
#91179=CARTESIAN_POINT('Ctrl Pts',(-2.91401168231396,0.505195230407465,
11.1506204437098));
#91180=CARTESIAN_POINT('Ctrl Pts',(-2.94357123776359,0.254214351879716,
11.1642221633102));
#91181=CARTESIAN_POINT('Ctrl Pts',(-2.94130162828673,0.0027079682416201,
11.1778238829105));
#91182=CARTESIAN_POINT('Origin',(0.,0.,0.));
#91183=CARTESIAN_POINT('',(-2.937239763848,-0.000584049131356901,12.3221761170896));
#91184=CARTESIAN_POINT('',(-2.93727053600114,-0.00067468657406146,12.1778238829105));
#91185=CARTESIAN_POINT('',(-2.942,-3.60291088309151E-16,0.));
#91186=CARTESIAN_POINT('Ctrl Pts',(-2.937239763848,-0.000584049131356901,
12.3221761170896));
#91187=CARTESIAN_POINT('Ctrl Pts',(-2.93630723827878,0.526896498967096,
12.2937485490067));
#91188=CARTESIAN_POINT('Ctrl Pts',(-2.80088780003305,1.05482369633564,12.2653209809237));
#91189=CARTESIAN_POINT('Ctrl Pts',(-2.53382312395941,1.50458015988076,12.2368934128408));
#91190=CARTESIAN_POINT('Ctrl Pts',(-2.03570785669002,2.34344273181871,12.1838717782254));
#91191=CARTESIAN_POINT('Ctrl Pts',(-1.07962793359348,2.91036661609979,12.13085014361));
#91192=CARTESIAN_POINT('Ctrl Pts',(-0.104636033354822,2.94500804439343,
12.0778285089946));
#91193=CARTESIAN_POINT('Ctrl Pts',(0.870355866883847,2.97964947268707,12.0248068743792));
#91194=CARTESIAN_POINT('Ctrl Pts',(1.86425974426462,2.48200844499326,11.9717852397639));
#91195=CARTESIAN_POINT('Ctrl Pts',(2.42065333828634,1.68061253620858,11.9187636051485));
#91196=CARTESIAN_POINT('Ctrl Pts',(2.97704693230805,0.879216627423909,11.8657419705331));
#91197=CARTESIAN_POINT('Ctrl Pts',(3.09593024297072,-0.22593416245163,11.8127203359177));
#91198=CARTESIAN_POINT('Ctrl Pts',(2.72270947038747,-1.12733057302667,11.7596987013023));
#91199=CARTESIAN_POINT('Ctrl Pts',(2.34948869780421,-2.02872698360171,11.7066770666869));
#91200=CARTESIAN_POINT('Ctrl Pts',(1.48416384197505,-2.72636901487625,11.6536554320716));
#91201=CARTESIAN_POINT('Ctrl Pts',(0.524110882362077,-2.89988428458928,
11.6006337974562));
#91202=CARTESIAN_POINT('Ctrl Pts',(-0.435942077250893,-3.07339955430231,
11.5476121628408));
#91203=CARTESIAN_POINT('Ctrl Pts',(-1.49072314064766,-2.72278806245382,
11.4945905282254));
#91204=CARTESIAN_POINT('Ctrl Pts',(-2.15585392049559,-2.00905822576202,
11.44156889361));
#91205=CARTESIAN_POINT('Ctrl Pts',(-2.6550954793503,-1.47333862434378,11.4017713014365));
#91206=CARTESIAN_POINT('Ctrl Pts',(-2.93481285697586,-0.733042609904606,
11.3619737092631));
#91207=CARTESIAN_POINT('Ctrl Pts',(-2.94150967972677,0.00271347918382847,
11.3221761170896));
#91208=CARTESIAN_POINT('Ctrl Pts',(-2.94130162828673,0.0027079682416201,
11.1778238829105));
#91209=CARTESIAN_POINT('Ctrl Pts',(-2.9347219773889,-0.726414913814524,
11.2172555858059));
#91210=CARTESIAN_POINT('Ctrl Pts',(-2.66063931527267,-1.45995431762841,
11.2566872887014));
#91211=CARTESIAN_POINT('Ctrl Pts',(-2.16966229743749,-1.99414525558605,
11.2961189915968));
#91212=CARTESIAN_POINT('Ctrl Pts',(-1.50932582422915,-2.71260202072372,
11.3491524140925));
#91213=CARTESIAN_POINT('Ctrl Pts',(-0.456654855314183,-3.0704625888679,
11.4021858365883));
#91214=CARTESIAN_POINT('Ctrl Pts',(0.504744460963153,-2.90332271964814,
11.4552192590841));
#91215=CARTESIAN_POINT('Ctrl Pts',(1.46614377724048,-2.73618285042839,11.5082526815798));
#91216=CARTESIAN_POINT('Ctrl Pts',(2.33627144088016,-2.04404254384471,11.5612861040756));
#91217=CARTESIAN_POINT('Ctrl Pts',(2.71538327691526,-1.14487704350598,11.6143195265713));
#91218=CARTESIAN_POINT('Ctrl Pts',(3.09449511295038,-0.245711543167243,
11.6673529490671));
#91219=CARTESIAN_POINT('Ctrl Pts',(2.98259112138089,0.860479150926533,11.7203863715629));
#91220=CARTESIAN_POINT('Ctrl Pts',(2.43108096386306,1.6655014657576,11.7734197940586));
#91221=CARTESIAN_POINT('Ctrl Pts',(1.87957080634523,2.47052378058866,11.8264532165544));
#91222=CARTESIAN_POINT('Ctrl Pts',(0.88845448287903,2.97437771615703,11.8794866390501));
#91223=CARTESIAN_POINT('Ctrl Pts',(-0.0869405947359189,2.94558841630752,
11.9325200615459));
#91224=CARTESIAN_POINT('Ctrl Pts',(-1.06233567235088,2.916799116458,11.9855534840417));
#91225=CARTESIAN_POINT('Ctrl Pts',(-2.02200950411461,2.35536658119062,12.0385869065374));
#91226=CARTESIAN_POINT('Ctrl Pts',(-2.52507963088188,1.5192177733964,12.0916203290332));
#91227=CARTESIAN_POINT('Ctrl Pts',(-2.79765260301929,1.0661764307228,12.1203548469923));
#91228=CARTESIAN_POINT('Ctrl Pts',(-2.93618139806878,0.532487217082399,
12.1490893649514));
#91229=CARTESIAN_POINT('Ctrl Pts',(-2.93727053600114,-0.00067468657406146,
12.1778238829105));
#91230=CARTESIAN_POINT('Origin',(0.,0.,0.));
#91231=CARTESIAN_POINT('',(-2.94365959218558,-0.00249856367199902,13.3221761170896));
#91232=CARTESIAN_POINT('',(-2.94378501997585,-0.00247147196094728,13.1778238829105));
#91233=CARTESIAN_POINT('',(-2.942,-3.60291088309151E-16,0.));
#91234=CARTESIAN_POINT('Ctrl Pts',(-2.94365959218558,-0.00249856367199902,
13.3221761170896));
#91235=CARTESIAN_POINT('Ctrl Pts',(-2.93637971808012,0.802618607647404,
13.2785450233656));
#91236=CARTESIAN_POINT('Ctrl Pts',(-2.59348572085056,1.61318695127993,13.2349139296417));
#91237=CARTESIAN_POINT('Ctrl Pts',(-2.00518015117195,2.15946142414359,13.1912828359177));
#91238=CARTESIAN_POINT('Ctrl Pts',(-1.29025599284032,2.82330830552441,13.1382612013023));
#91239=CARTESIAN_POINT('Ctrl Pts',(-0.212914415108081,3.0968528810621,13.0852395666869));
#91240=CARTESIAN_POINT('Ctrl Pts',(0.732105916213065,2.85447753686451,13.0322179320716));
#91241=CARTESIAN_POINT('Ctrl Pts',(1.6771262475342,2.61210219266691,12.9791962974562));
#91242=CARTESIAN_POINT('Ctrl Pts',(2.48982533244424,1.85380692873404,12.9261746628408));
#91243=CARTESIAN_POINT('Ctrl Pts',(2.79699408917628,0.927817409909507,12.8731530282254));
#91244=CARTESIAN_POINT('Ctrl Pts',(3.10416284590832,0.00182789108496756,
12.82013139361));
#91245=CARTESIAN_POINT('Ctrl Pts',(2.90580127446235,-1.09185588263124,12.7671097589946));
#91246=CARTESIAN_POINT('Ctrl Pts',(2.29300131933759,-1.85099055387495,12.7140881243793));
#91247=CARTESIAN_POINT('Ctrl Pts',(1.68020136421283,-2.61012522511867,12.6610664897639));
#91248=CARTESIAN_POINT('Ctrl Pts',(0.652963025409289,-3.03471079388989,
12.6080448551485));
#91249=CARTESIAN_POINT('Ctrl Pts',(-0.316983527445643,-2.92976833970646,
12.5550232205331));
#91250=CARTESIAN_POINT('Ctrl Pts',(-1.28693008030059,-2.82482588552303,
12.5020015859177));
#91251=CARTESIAN_POINT('Ctrl Pts',(-2.19958484720692,-2.19035540838494,
12.4489799513023));
#91252=CARTESIAN_POINT('Ctrl Pts',(-2.63583692493897,-1.31771954001848,
12.3959583166869));
#91253=CARTESIAN_POINT('Ctrl Pts',(-2.83819229746733,-0.912947699978407,
12.3713642501545));
#91254=CARTESIAN_POINT('Ctrl Pts',(-2.93804653690103,-0.456933028989684,
12.346770183622));
#91255=CARTESIAN_POINT('Ctrl Pts',(-2.937239763848,-0.000584049131356901,
12.3221761170896));
#91256=CARTESIAN_POINT('Ctrl Pts',(-2.93727053600114,-0.00067468657406146,
12.1778238829105));
#91257=CARTESIAN_POINT('Ctrl Pts',(-2.93819154879431,-0.451534875631614,
12.2021227874472));
#91258=CARTESIAN_POINT('Ctrl Pts',(-2.84082973894426,-0.902017986379197,
12.2264216919838));
#91259=CARTESIAN_POINT('Ctrl Pts',(-2.64313182011494,-1.30303644108441,
12.2507205965204));
#91260=CARTESIAN_POINT('Ctrl Pts',(-2.21164746080996,-2.17827676744996,
12.3037540190162));
#91261=CARTESIAN_POINT('Ctrl Pts',(-1.30221232042921,-2.81789233986001,
12.356787441512));
#91262=CARTESIAN_POINT('Ctrl Pts',(-0.332628768749986,-2.9280382319051,
12.4098208640077));
#91263=CARTESIAN_POINT('Ctrl Pts',(0.636954782929239,-3.03818412395018,
12.4628542865035));
#91264=CARTESIAN_POINT('Ctrl Pts',(1.66668674590694,-2.61886033563027,12.5158877089993));
#91265=CARTESIAN_POINT('Ctrl Pts',(2.28349934958056,-1.86270784229927,12.568921131495));
#91266=CARTESIAN_POINT('Ctrl Pts',(2.90031195325417,-1.10655534896829,12.6219545539908));
#91267=CARTESIAN_POINT('Ctrl Pts',(3.10420519762372,-0.0135741506262503,
12.6749879764865));
#91268=CARTESIAN_POINT('Ctrl Pts',(2.80150876262273,0.914110736314876,12.7280213989823));
#91269=CARTESIAN_POINT('Ctrl Pts',(2.49881232762173,1.84179562325603,12.781054821478));
#91270=CARTESIAN_POINT('Ctrl Pts',(1.68952621325013,2.60418419879625,12.8340882439738));
#91271=CARTESIAN_POINT('Ctrl Pts',(0.745443460483677,2.85102855694575,12.8871216664696));
#91272=CARTESIAN_POINT('Ctrl Pts',(-0.198639292282781,3.09787291509526,
12.9401550889653));
#91273=CARTESIAN_POINT('Ctrl Pts',(-1.27751868344409,2.82917305585407,12.9931885114611));
#91274=CARTESIAN_POINT('Ctrl Pts',(-1.99554818878264,2.16837201871459,13.0462219339568));
#91275=CARTESIAN_POINT('Ctrl Pts',(-2.58947605453147,1.62178145836176,13.0900892502747));
#91276=CARTESIAN_POINT('Ctrl Pts',(-2.93651056908799,0.806915424962724,
13.1339565665926));
#91277=CARTESIAN_POINT('Ctrl Pts',(-2.94378501997585,-0.00247147196094728,
13.1778238829105));
#91278=CARTESIAN_POINT('Origin',(0.,0.,0.));
#91279=CARTESIAN_POINT('',(-2.94544838002636,0.00181532900233754,14.3221761170896));
#91280=CARTESIAN_POINT('',(-2.94538511207558,0.00185514841678406,14.1778238829105));
#91281=CARTESIAN_POINT('',(-2.942,-3.60291088309151E-16,0.));
#91282=CARTESIAN_POINT('Ctrl Pts',(-2.94544838002636,0.00181532900233754,
14.3221761170896));
#91283=CARTESIAN_POINT('Ctrl Pts',(-2.94622316443012,0.108911839184011,
14.31636313234));
#91284=CARTESIAN_POINT('Ctrl Pts',(-2.94089026946329,0.215930373720906,
14.3105501475904));
#91285=CARTESIAN_POINT('Ctrl Pts',(-2.929193876287,0.322248841954449,14.3047371628408));
#91286=CARTESIAN_POINT('Ctrl Pts',(-2.82250825572816,1.2920052095289,14.2517155282254));
#91287=CARTESIAN_POINT('Ctrl Pts',(-2.18639844106512,2.20351813516736,14.19869389361));
#91288=CARTESIAN_POINT('Ctrl Pts',(-1.3129798834425,2.63820107396945,14.1456722589946));
#91289=CARTESIAN_POINT('Ctrl Pts',(-0.439561325819871,3.07288401277154,
14.0926506243793));
#91290=CARTESIAN_POINT('Ctrl Pts',(0.67116597476233,3.03073696473725,14.0396289897639));
#91291=CARTESIAN_POINT('Ctrl Pts',(1.50913190300478,2.53111477028431,13.9866073551485));
#91292=CARTESIAN_POINT('Ctrl Pts',(2.34709783124724,2.03149257583137,13.9335857205331));
#91293=CARTESIAN_POINT('Ctrl Pts',(2.91230238714993,1.07439523495978,13.8805640859177));
#91294=CARTESIAN_POINT('Ctrl Pts',(2.94519135533895,0.0993426467079052,
13.8275424513023));
#91295=CARTESIAN_POINT('Ctrl Pts',(2.97808032352798,-0.875709941543982,
13.7745208166869));
#91296=CARTESIAN_POINT('Ctrl Pts',(2.47865370400332,-1.86871777717613,13.7214991820716));
#91297=CARTESIAN_POINT('Ctrl Pts',(1.67625905423563,-2.42367008153158,13.6684775474562));
#91298=CARTESIAN_POINT('Ctrl Pts',(0.873864404467956,-2.97862238588703,
13.6154559128408));
#91299=CARTESIAN_POINT('Ctrl Pts',(-0.231498275542777,-3.09551915896577,
13.5624342782254));
#91300=CARTESIAN_POINT('Ctrl Pts',(-1.13222242085015,-2.72067886211189,
13.50941264361));
#91301=CARTESIAN_POINT('Ctrl Pts',(-2.03294656615752,-2.34583856525801,
13.4563910089946));
#91302=CARTESIAN_POINT('Ctrl Pts',(-2.72903217676157,-1.47926119847154,
13.4033693743792));
#91303=CARTESIAN_POINT('Ctrl Pts',(-2.90082161259808,-0.518897921466346,
13.3503477397639));
#91304=CARTESIAN_POINT('Ctrl Pts',(-2.93124684813898,-0.348810169763627,
13.3409571988724));
#91305=CARTESIAN_POINT('Ctrl Pts',(-2.9452264095545,-0.17578062181818,13.331566657981));
#91306=CARTESIAN_POINT('Ctrl Pts',(-2.94365959218558,-0.00249856367199902,
13.3221761170896));
#91307=CARTESIAN_POINT('Ctrl Pts',(-2.94378501997585,-0.00247147196094728,
13.1778238829105));
#91308=CARTESIAN_POINT('Ctrl Pts',(-2.94530502153557,-0.171593425590788,
13.1869899890884));
#91309=CARTESIAN_POINT('Ctrl Pts',(-2.93199096538639,-0.340476157971982,
13.1961560952663));
#91310=CARTESIAN_POINT('Ctrl Pts',(-2.90299564064934,-0.506622241585387,
13.2053222014441));
#91311=CARTESIAN_POINT('Ctrl Pts',(-2.73523396766174,-1.46791324970816,
13.2583556239399));
#91312=CARTESIAN_POINT('Ctrl Pts',(-2.04253100217075,-2.33759305091599,
13.3113890464356));
#91313=CARTESIAN_POINT('Ctrl Pts',(-1.14312047815411,-2.71612322211692,
13.3644224689314));
#91314=CARTESIAN_POINT('Ctrl Pts',(-0.243709954137437,-3.09465339331786,
13.4174558914272));
#91315=CARTESIAN_POINT('Ctrl Pts',(0.862408128404901,-2.98203393451191,
13.4704893139229));
#91316=CARTESIAN_POINT('Ctrl Pts',(1.66707355482995,-2.43000319919227,13.5235227364187));
#91317=CARTESIAN_POINT('Ctrl Pts',(2.47173898125499,-1.87797246387265,13.5765561589144));
#91318=CARTESIAN_POINT('Ctrl Pts',(2.97495175156274,-0.886530452039386,
13.6295895814102));
#91319=CARTESIAN_POINT('Ctrl Pts',(2.94553156646463,0.0888458004550528,
13.682623003906));
#91320=CARTESIAN_POINT('Ctrl Pts',(2.91611138136652,1.06422205294949,13.7356564264017));
#91321=CARTESIAN_POINT('Ctrl Pts',(2.35405824086255,2.02353254610508,13.7886898488975));
#91322=CARTESIAN_POINT('Ctrl Pts',(1.51758421925744,2.52606174167593,13.8417232713932));
#91323=CARTESIAN_POINT('Ctrl Pts',(0.68111019765233,3.02859093724679,13.894756693889));
#91324=CARTESIAN_POINT('Ctrl Pts',(-0.429784705053949,3.07433883523289,
13.9477901163848));
#91325=CARTESIAN_POINT('Ctrl Pts',(-1.30474576171729,2.64228845559656,14.0008235388805));
#91326=CARTESIAN_POINT('Ctrl Pts',(-2.17970681838062,2.21023807596023,14.0538569613763));
#91327=CARTESIAN_POINT('Ctrl Pts',(-2.81873402900105,1.30038941870153,14.106890383872));
#91328=CARTESIAN_POINT('Ctrl Pts',(-2.92825276566436,0.330734826828228,
14.1599238063678));
#91329=CARTESIAN_POINT('Ctrl Pts',(-2.94057451596746,0.221640783878745,
14.1658904985487));
#91330=CARTESIAN_POINT('Ctrl Pts',(-2.94619370378806,0.111789712414528,
14.1718571907296));
#91331=CARTESIAN_POINT('Ctrl Pts',(-2.94538511207558,0.00185514841678406,
14.1778238829105));
#91332=CARTESIAN_POINT('Origin',(0.,0.,0.));
#91333=CARTESIAN_POINT('',(-2.93798069771247,0.00158343123380422,15.3221761170896));
#91334=CARTESIAN_POINT('',(-2.93795334773476,0.00156554691536136,15.1778238829105));
#91335=CARTESIAN_POINT('',(-2.942,-3.60291088309151E-16,0.));
#91336=CARTESIAN_POINT('Ctrl Pts',(-2.93798069771247,0.00158343123380422,
15.3221761170896));
#91337=CARTESIAN_POINT('Ctrl Pts',(-2.93987699576759,0.391304358149722,
15.301159606699));
#91338=CARTESIAN_POINT('Ctrl Pts',(-2.86785867215597,0.780352682464874,
15.2801430963083));
#91339=CARTESIAN_POINT('Ctrl Pts',(-2.71863946474125,1.13711061105315,15.2591265859177));
#91340=CARTESIAN_POINT('Ctrl Pts',(-2.34218085453035,2.03715958132271,15.2061049513023));
#91341=CARTESIAN_POINT('Ctrl Pts',(-1.47435377624626,2.73168652256657,15.1530833166869));
#91342=CARTESIAN_POINT('Ctrl Pts',(-0.513683284281933,2.90174956956447,
15.1000616820716));
#91343=CARTESIAN_POINT('Ctrl Pts',(0.446987207682398,3.07181261656237,15.0470400474562));
#91344=CARTESIAN_POINT('Ctrl Pts',(1.50050111332698,2.71741176931431,14.9940184128408));
#91345=CARTESIAN_POINT('Ctrl Pts',(2.16306195169747,2.00129559889012,14.9409967782254));
#91346=CARTESIAN_POINT('Ctrl Pts',(2.82562279006796,1.28517942846593,14.88797514361));
#91347=CARTESIAN_POINT('Ctrl Pts',(3.09723056116435,0.207347934865625,14.8349535089946));
#91348=CARTESIAN_POINT('Ctrl Pts',(2.85315707378551,-0.737235236085434,
14.7819318743792));
#91349=CARTESIAN_POINT('Ctrl Pts',(2.60908358640667,-1.68181840703649,14.7289102397639));
#91350=CARTESIAN_POINT('Ctrl Pts',(1.84932884055259,-2.49315325533829,14.6758886051485));
#91351=CARTESIAN_POINT('Ctrl Pts',(0.922788726883278,-2.79865718632264,
14.6228669705331));
#91352=CARTESIAN_POINT('Ctrl Pts',(-0.00375138678601547,-3.104161117307,
14.5698453359177));
#91353=CARTESIAN_POINT('Ctrl Pts',(-1.09707686827054,-2.90383413097393,
14.5168237013023));
#91354=CARTESIAN_POINT('Ctrl Pts',(-1.85510889578549,-2.2896707330522,14.4638020666869));
#91355=CARTESIAN_POINT('Ctrl Pts',(-2.53003468473154,-1.74284065089456,
14.4165934168212));
#91356=CARTESIAN_POINT('Ctrl Pts',(-2.93915616918906,-0.86794123647866,
14.3693847669554));
#91357=CARTESIAN_POINT('Ctrl Pts',(-2.94544838002636,0.00181532900233754,
14.3221761170896));
#91358=CARTESIAN_POINT('Ctrl Pts',(-2.94538511207558,0.00185514841678406,
14.1778238829105));
#91359=CARTESIAN_POINT('Ctrl Pts',(-2.93900674246776,-0.865335636541155,
14.2248906132254));
#91360=CARTESIAN_POINT('Ctrl Pts',(-2.5326635796891,-1.73772169519058,14.2719573435402));
#91361=CARTESIAN_POINT('Ctrl Pts',(-1.86123047185566,-2.28470368230412,
14.3190240738551));
#91362=CARTESIAN_POINT('Ctrl Pts',(-1.10467917867744,-2.90102707307532,
14.3720574963508));
#91363=CARTESIAN_POINT('Ctrl Pts',(-0.0115663296148442,-3.10421332812979,
14.4250909188466));
#91364=CARTESIAN_POINT('Ctrl Pts',(0.915922577440401,-2.80091692440761,
14.4781243413424));
#91365=CARTESIAN_POINT('Ctrl Pts',(1.84341148449563,-2.49762052068544,14.5311577638381));
#91366=CARTESIAN_POINT('Ctrl Pts',(2.60527644954349,-1.6878414581866,14.5841911863339));
#91367=CARTESIAN_POINT('Ctrl Pts',(2.85151011778344,-0.743599242520295,
14.6372246088296));
#91368=CARTESIAN_POINT('Ctrl Pts',(3.09774378602338,0.200642973145996,14.6902580313254));
#91369=CARTESIAN_POINT('Ctrl Pts',(2.82834615745544,1.27934834197977,14.7432914538212));
#91370=CARTESIAN_POINT('Ctrl Pts',(2.16708083283619,1.99695028712587,14.7963248763169));
#91371=CARTESIAN_POINT('Ctrl Pts',(1.50581550821692,2.71455223227199,14.8493582988127));
#91372=CARTESIAN_POINT('Ctrl Pts',(0.452682487546306,3.07105075373044,14.9023917213084));
#91373=CARTESIAN_POINT('Ctrl Pts',(-0.508499810258251,2.9026673471594,14.9554251438042));
#91374=CARTESIAN_POINT('Ctrl Pts',(-1.46968210806282,2.73428394058836,15.0084585663));
#91375=CARTESIAN_POINT('Ctrl Pts',(-2.33891368300132,2.04101860598786,15.0614919887957));
#91376=CARTESIAN_POINT('Ctrl Pts',(-2.716862031007,1.14136343456876,15.1145254112915));
#91377=CARTESIAN_POINT('Ctrl Pts',(-2.86722980321464,0.783433191996738,
15.1356249018312));
#91378=CARTESIAN_POINT('Ctrl Pts',(-2.9398339382908,0.392834167959925,15.1567243923708));
#91379=CARTESIAN_POINT('Ctrl Pts',(-2.93795334773476,0.00156554691536136,
15.1778238829105));
#91380=CARTESIAN_POINT('Origin',(0.,0.,0.));
#91381=CARTESIAN_POINT('',(-2.93964177839095,-0.00242668875790442,16.3221761170896));
#91382=CARTESIAN_POINT('',(-2.93964149763041,-0.00243012038732958,16.1778238829105));
#91383=CARTESIAN_POINT('',(-2.942,-3.60291088309151E-16,0.));
#91384=CARTESIAN_POINT('Ctrl Pts',(-2.93964177839095,-0.00242668875790442,
16.3221761170896));
#91385=CARTESIAN_POINT('Ctrl Pts',(-2.93444969551508,0.668268699559762,
16.2859560810579));
#91386=CARTESIAN_POINT('Ctrl Pts',(-2.70680889432787,1.34215078748866,16.2497360450263));
#91387=CARTESIAN_POINT('Ctrl Pts',(-2.28633275003428,1.85922124480626,16.2135160089946));
#91388=CARTESIAN_POINT('Ctrl Pts',(-1.67080789335733,2.61614817978613,16.1604943743792));
#91389=CARTESIAN_POINT('Ctrl Pts',(-0.642049934071474,3.03703839245773,
16.1074727397639));
#91390=CARTESIAN_POINT('Ctrl Pts',(0.327513115445196,2.92860995016913,16.0544511051485));
#91391=CARTESIAN_POINT('Ctrl Pts',(1.29707616496187,2.82018150788052,16.0014294705331));
#91392=CARTESIAN_POINT('Ctrl Pts',(2.20744430470937,2.18243441063176,15.9484078359177));
#91393=CARTESIAN_POINT('Ctrl Pts',(2.64055670034754,1.30823598531302,15.8953862013023));
#91394=CARTESIAN_POINT('Ctrl Pts',(3.07366909598573,0.434037559994252,15.8423645666869));
#91395=CARTESIAN_POINT('Ctrl Pts',(3.02952574751452,-0.676612193394493,
15.7893429320716));
#91396=CARTESIAN_POINT('Ctrl Pts',(2.52839823989685,-1.51367877091038,15.7363212974562));
#91397=CARTESIAN_POINT('Ctrl Pts',(2.0272707322792,-2.35074534842623,15.6832996628408));
#91398=CARTESIAN_POINT('Ctrl Pts',(1.06915906551514,-2.91422875006925,15.6302780282254));
#91399=CARTESIAN_POINT('Ctrl Pts',(0.0940489391366825,-2.94536515190655,
15.57725639361));
#91400=CARTESIAN_POINT('Ctrl Pts',(-0.8810611872418,-2.97650155374385,15.5242347589946));
#91401=CARTESIAN_POINT('Ctrl Pts',(-1.87316977323467,-2.47529095577539,
15.4712131243793));
#91402=CARTESIAN_POINT('Ctrl Pts',(-2.42667899516226,-1.67190015714352,
15.4181914897639));
#91403=CARTESIAN_POINT('Ctrl Pts',(-2.76079037320335,-1.18695429499211,
15.3861863655391));
#91404=CARTESIAN_POINT('Ctrl Pts',(-2.93509290836528,-0.591905518505825,
15.3541812413144));
#91405=CARTESIAN_POINT('Ctrl Pts',(-2.93798069771247,0.00158343123380422,
15.3221761170896));
#91406=CARTESIAN_POINT('Ctrl Pts',(-2.93795334773476,0.00156554691536136,
15.1778238829105));
#91407=CARTESIAN_POINT('Ctrl Pts',(-2.93510708702808,-0.590616785519977,
15.2097578148666));
#91408=CARTESIAN_POINT('Ctrl Pts',(-2.76164155797149,-1.1843329378168,15.2416917468227));
#91409=CARTESIAN_POINT('Ctrl Pts',(-2.42892441791055,-1.66864494646884,
15.2736256787788));
#91410=CARTESIAN_POINT('Ctrl Pts',(-1.87637333573557,-2.47295314784975,
15.3266591012745));
#91411=CARTESIAN_POINT('Ctrl Pts',(-0.884606050312744,-2.97552454237392,
15.3796925237703));
#91412=CARTESIAN_POINT('Ctrl Pts',(0.0907509690048441,-2.94547348433537,
15.432725946266));
#91413=CARTESIAN_POINT('Ctrl Pts',(1.06610798832242,-2.91542242629683,15.4857593687618));
#91414=CARTESIAN_POINT('Ctrl Pts',(2.02505474153477,-2.35274891569562,15.5387927912575));
#91415=CARTESIAN_POINT('Ctrl Pts',(2.52704279567215,-1.51595003022512,15.5918262137533));
#91416=CARTESIAN_POINT('Ctrl Pts',(3.02903084980954,-0.679151144754612,
15.6448596362491));
#91417=CARTESIAN_POINT('Ctrl Pts',(3.07406020487193,0.431773115585177,15.6978930587448));
#91418=CARTESIAN_POINT('Ctrl Pts',(2.64144398565597,1.30645453649945,15.7509264812406));
#91419=CARTESIAN_POINT('Ctrl Pts',(2.20882776644001,2.1811359574137,15.8039599037363));
#91420=CARTESIAN_POINT('Ctrl Pts',(1.2985659729457,2.81957453890244,15.8569933262321));
#91421=CARTESIAN_POINT('Ctrl Pts',(0.328840746540987,2.92846607436597,15.9100267487279));
#91422=CARTESIAN_POINT('Ctrl Pts',(-0.640884479863755,3.0373576098295,15.9630601712236));
#91423=CARTESIAN_POINT('Ctrl Pts',(-1.67007313917891,2.6167020992678,16.0160935937194));
#91424=CARTESIAN_POINT('Ctrl Pts',(-2.2859070592039,1.85975232275157,16.0691270162151));
#91425=CARTESIAN_POINT('Ctrl Pts',(-2.70664310552638,1.34260631003568,16.1053593051136));
#91426=CARTESIAN_POINT('Ctrl Pts',(-2.93444231580981,0.668492091843893,
16.1415915940121));
#91427=CARTESIAN_POINT('Ctrl Pts',(-2.93964149763041,-0.00243012038732958,
16.1778238829105));
#91428=CARTESIAN_POINT('Origin',(0.,0.,0.));
#91429=CARTESIAN_POINT('',(-2.94674177077904,-0.000549249277246588,17.3221761170896));
#91430=CARTESIAN_POINT('',(-2.94673569549022,-0.000573513903422574,17.1778238829105));
#91431=CARTESIAN_POINT('',(-2.942,-3.60291088309151E-16,0.));
#91432=CARTESIAN_POINT('Ctrl Pts',(-2.94674177077904,-0.000549249277246588,
17.3221761170896));
#91433=CARTESIAN_POINT('Ctrl Pts',(-2.94431894621181,0.945760599581783,
17.2707525554169));
#91434=CARTESIAN_POINT('Ctrl Pts',(-2.4476760535182,1.89425494672401,17.2193289937442));
#91435=CARTESIAN_POINT('Ctrl Pts',(-1.66753585901357,2.42968006945814,17.1679054320716));
#91436=CARTESIAN_POINT('Ctrl Pts',(-0.863151506854386,2.98174442085811,
17.1148837974562));
#91437=CARTESIAN_POINT('Ctrl Pts',(0.242624240201871,3.09466699229011,17.0618621628408));
#91438=CARTESIAN_POINT('Ctrl Pts',(1.14199512784458,2.71659128486371,17.0088405282254));
#91439=CARTESIAN_POINT('Ctrl Pts',(2.04136601548729,2.33851557743732,16.95581889361));
#91440=CARTESIAN_POINT('Ctrl Pts',(2.73433204371645,1.46944159115252,16.9027972589946));
#91441=CARTESIAN_POINT('Ctrl Pts',(2.90266815249068,0.508466987654616,16.8497756243792));
#91442=CARTESIAN_POINT('Ctrl Pts',(3.07100426126492,-0.452507615843304,
16.7967539897639));
#91443=CARTESIAN_POINT('Ctrl Pts',(2.7147104505842,-1.50538283655434,16.7437323551485));
#91444=CARTESIAN_POINT('Ctrl Pts',(1.99740458146546,-2.16665549152582,16.6907107205331));
#91445=CARTESIAN_POINT('Ctrl Pts',(1.28009871234673,-2.8279281464973,16.6376890859177));
#91446=CARTESIAN_POINT('Ctrl Pts',(0.20178078478999,-3.09759823572925,16.5846674513023));
#91447=CARTESIAN_POINT('Ctrl Pts',(-0.742362174335158,-2.85182739364335,
16.5316458166869));
#91448=CARTESIAN_POINT('Ctrl Pts',(-1.68650513346031,-2.60605655155744,
16.4786241820716));
#91449=CARTESIAN_POINT('Ctrl Pts',(-2.49647312415386,-1.84484477815369,
16.4256025474562));
#91450=CARTESIAN_POINT('Ctrl Pts',(-2.80031124246659,-0.917757062807729,
16.3725809128408));
#91451=CARTESIAN_POINT('Ctrl Pts',(-2.89659205567343,-0.623979706486333,
16.3557793142571));
#91452=CARTESIAN_POINT('Ctrl Pts',(-2.94205026004507,-0.313546055856832,
16.3389777156733));
#91453=CARTESIAN_POINT('Ctrl Pts',(-2.93964177839095,-0.00242668875790442,
16.3221761170896));
#91454=CARTESIAN_POINT('Ctrl Pts',(-2.93964149763041,-0.00243012038732958,
16.1778238829105));
#91455=CARTESIAN_POINT('Ctrl Pts',(-2.94205238998694,-0.313540846863508,
16.1946250165078));
#91456=CARTESIAN_POINT('Ctrl Pts',(-2.89659907789882,-0.623965217516017,
16.2114261501051));
#91457=CARTESIAN_POINT('Ctrl Pts',(-2.80032391440682,-0.91773403538245,
16.2282272837024));
#91458=CARTESIAN_POINT('Ctrl Pts',(-2.49642766884992,-1.84502657452947,
16.2812607061982));
#91459=CARTESIAN_POINT('Ctrl Pts',(-1.68615599700128,-2.60636761035277,
16.3342941286939));
#91460=CARTESIAN_POINT('Ctrl Pts',(-0.741754713466301,-2.85199048566937,
16.3873275511897));
#91461=CARTESIAN_POINT('Ctrl Pts',(0.202646570068678,-3.09761336098597,
16.4403609736855));
#91462=CARTESIAN_POINT('Ctrl Pts',(1.28117746528998,-2.82751807579589,16.4933943961812));
#91463=CARTESIAN_POINT('Ctrl Pts',(1.99835155002923,-2.16578874034239,16.546427818677));
#91464=CARTESIAN_POINT('Ctrl Pts',(2.71552563476848,-1.50405940488887,16.5994612411727));
#91465=CARTESIAN_POINT('Ctrl Pts',(3.07134290902563,-0.450696019171894,
16.6524946636685));
#91466=CARTESIAN_POINT('Ctrl Pts',(2.90233783931567,0.51037716619625,16.7055280861643));
#91467=CARTESIAN_POINT('Ctrl Pts',(2.73333276960572,1.47145035156437,16.75856150866));
#91468=CARTESIAN_POINT('Ctrl Pts',(2.03950535592868,2.34023333658368,16.8115949311558));
#91469=CARTESIAN_POINT('Ctrl Pts',(1.13960591348502,2.71759970327641,16.8646283536515));
#91470=CARTESIAN_POINT('Ctrl Pts',(0.23970647104136,3.09496606996915,16.9176617761473));
#91471=CARTESIAN_POINT('Ctrl Pts',(-0.866265000168904,2.98091581833532,
16.9706951986431));
#91472=CARTESIAN_POINT('Ctrl Pts',(-1.67021564001697,2.4278446204691,17.0237286211388));
#91473=CARTESIAN_POINT('Ctrl Pts',(-2.44887545156518,1.89217203889788,17.0750937083961));
#91474=CARTESIAN_POINT('Ctrl Pts',(-2.94421760130182,0.944665652976608,
17.1264587956533));
#91475=CARTESIAN_POINT('Ctrl Pts',(-2.94673569549022,-0.000573513903422574,
17.1778238829105));
#91476=CARTESIAN_POINT('Origin',(0.,0.,0.));
#91477=CARTESIAN_POINT('',(-2.94129852510877,0.00270460087765087,18.3221761170896));
#91478=CARTESIAN_POINT('',(-2.94137747154633,0.00271175267126415,18.1778238829105));
#91479=CARTESIAN_POINT('',(-2.942,-3.60291088309151E-16,0.));
#91480=CARTESIAN_POINT('Ctrl Pts',(-2.94129852510877,0.00270460087765087,
18.3221761170896));
#91481=CARTESIAN_POINT('Ctrl Pts',(-2.94356667986702,0.254280750264864,
18.3085706643913));
#91482=CARTESIAN_POINT('Ctrl Pts',(-2.91398910889245,0.50533156988729,18.294965211693));
#91483=CARTESIAN_POINT('Ctrl Pts',(-2.85048850073354,0.747486714399695,
18.2813597589946));
#91484=CARTESIAN_POINT('Ctrl Pts',(-2.60302109789805,1.6911864116652,18.2283381243792));
#91485=CARTESIAN_POINT('Ctrl Pts',(-1.84035475602305,2.49978492816616,18.1753164897639));
#91486=CARTESIAN_POINT('Ctrl Pts',(-0.912722433937579,2.80195625226471,
18.1222948551485));
#91487=CARTESIAN_POINT('Ctrl Pts',(0.0149098881479351,3.10412757636327,
18.0692732205331));
#91488=CARTESIAN_POINT('Ctrl Pts',(1.10750819044393,2.89987170805936,18.0162515859177));
#91489=CARTESIAN_POINT('Ctrl Pts',(1.8633275876524,2.28298738106712,17.9632299513023));
#91490=CARTESIAN_POINT('Ctrl Pts',(2.61914698486086,1.6661030540749,17.9102083166869));
#91491=CARTESIAN_POINT('Ctrl Pts',(3.03818747698181,0.636590268394331,17.8571866820716));
#91492=CARTESIAN_POINT('Ctrl Pts',(2.9280165632392,-0.3327763309118,17.8041650474562));
#91493=CARTESIAN_POINT('Ctrl Pts',(2.8178456494966,-1.30214293021795,17.7511434128408));
#91494=CARTESIAN_POINT('Ctrl Pts',(2.17846332989048,-2.21136334314964,17.6981217782254));
#91495=CARTESIAN_POINT('Ctrl Pts',(1.30348786095498,-2.64290379646351,17.64510014361));
#91496=CARTESIAN_POINT('Ctrl Pts',(0.428512392019511,-3.07444424977737,
17.5920785089946));
#91497=CARTESIAN_POINT('Ctrl Pts',(-0.682056226245346,-3.02830474347338,
17.5390568743792));
#91498=CARTESIAN_POINT('Ctrl Pts',(-1.51822074890888,-2.52567354157278,
17.4860352397639));
#91499=CARTESIAN_POINT('Ctrl Pts',(-2.35438527157246,-2.02304233967215,
17.4330136051485));
#91500=CARTESIAN_POINT('Ctrl Pts',(-2.91614569863472,-1.06391944217489,
17.3799919705331));
#91501=CARTESIAN_POINT('Ctrl Pts',(-2.94552943353478,-0.0887549277422849,
17.3269703359177));
#91502=CARTESIAN_POINT('Ctrl Pts',(-2.94641505978979,-0.0593634531772387,
17.325372262975));
#91503=CARTESIAN_POINT('Ctrl Pts',(-2.94681706409323,-0.0299574060769884,
17.3237741900323));
#91504=CARTESIAN_POINT('Ctrl Pts',(-2.94674177077904,-0.000549249277246588,
17.3221761170896));
#91505=CARTESIAN_POINT('Ctrl Pts',(-2.94673569549022,-0.000573513903422574,
17.1778238829105));
#91506=CARTESIAN_POINT('Ctrl Pts',(-2.94681748305241,-0.0312748305982578,
17.179492218149));
#91507=CARTESIAN_POINT('Ctrl Pts',(-2.94637936742245,-0.0619737554974743,
17.1811605533876));
#91508=CARTESIAN_POINT('Ctrl Pts',(-2.94541416994405,-0.092656099588213,
17.1828288886261));
#91509=CARTESIAN_POINT('Ctrl Pts',(-2.91473225153718,-1.06799347768063,
17.2358623111219));
#91510=CARTESIAN_POINT('Ctrl Pts',(-2.35143860623763,-2.02657608976683,
17.2888957336176));
#91511=CARTESIAN_POINT('Ctrl Pts',(-1.51431520698315,-2.52802279246008,
17.3419291561134));
#91512=CARTESIAN_POINT('Ctrl Pts',(-0.677191807728671,-3.02946949515333,
17.3949625786091));
#91513=CARTESIAN_POINT('Ctrl Pts',(0.433761345480731,-3.07378028845364,
17.4479960011049));
#91514=CARTESIAN_POINT('Ctrl Pts',(1.30816276471605,-2.64059841064645,17.5010294236007));
#91515=CARTESIAN_POINT('Ctrl Pts',(2.18256418395138,-2.20741653283925,17.5540628460964));
#91516=CARTESIAN_POINT('Ctrl Pts',(2.82041386921262,-1.29674198392452,17.6070962685922));
#91517=CARTESIAN_POINT('Ctrl Pts',(2.92867815792071,-0.326946528680541,
17.6601296910879));
#91518=CARTESIAN_POINT('Ctrl Pts',(3.03694244662878,0.642848926563412,17.7131631135837));
#91519=CARTESIAN_POINT('Ctrl Pts',(2.61562133878374,1.67176528813662,17.7661965360794));
#91520=CARTESIAN_POINT('Ctrl Pts',(1.85827339560542,2.28710947977642,17.8192299585752));
#91521=CARTESIAN_POINT('Ctrl Pts',(1.10092545242709,2.90245367141623,17.872263381071));
#91522=CARTESIAN_POINT('Ctrl Pts',(0.00755067391547432,3.10422569312265,
17.9252968035667));
#91523=CARTESIAN_POINT('Ctrl Pts',(-0.919545109383185,2.79972973286843,
17.9783302260625));
#91524=CARTESIAN_POINT('Ctrl Pts',(-1.84664089268186,2.49523377261421,18.0313636485583));
#91525=CARTESIAN_POINT('Ctrl Pts',(-2.60745768076757,1.68446983039934,18.084397071054));
#91526=CARTESIAN_POINT('Ctrl Pts',(-2.85246966040257,0.739909874093412,
18.1374304935498));
#91527=CARTESIAN_POINT('Ctrl Pts',(-2.91467486249146,0.500098975644197,
18.15089495667));
#91528=CARTESIAN_POINT('Ctrl Pts',(-2.94363216926481,0.251663815076334,
18.1643594197903));
#91529=CARTESIAN_POINT('Ctrl Pts',(-2.94137747154633,0.00271175267126415,
18.1778238829105));
#91530=CARTESIAN_POINT('Origin',(0.,0.,0.));
#91531=CARTESIAN_POINT('',(-2.9372855915547,-0.000697940546887099,19.3221761170896));
#91532=CARTESIAN_POINT('',(-2.93725371205965,-0.00063370482881248,19.1778238829105));
#91533=CARTESIAN_POINT('',(-2.942,-3.60291088309151E-16,0.));
#91534=CARTESIAN_POINT('Ctrl Pts',(-2.9372855915547,-0.000697940546887099,
19.3221761170896));
#91535=CARTESIAN_POINT('Ctrl Pts',(-2.93615528736924,0.533838969154223,
19.2933671387503));
#91536=CARTESIAN_POINT('Ctrl Pts',(-2.7968583901853,1.06892457674313,19.2645581604109));
#91537=CARTESIAN_POINT('Ctrl Pts',(-2.5229406841141,1.52275782232767,19.2357491820716));
#91538=CARTESIAN_POINT('Ctrl Pts',(-2.01880741166991,2.35801758892721,19.1827275474562));
#91539=CARTESIAN_POINT('Ctrl Pts',(-1.0586763818656,2.91805322665358,19.1297059128408));
#91540=CARTESIAN_POINT('Ctrl Pts',(-0.0834606296271075,2.94568419969291,
19.0766842782254));
#91541=CARTESIAN_POINT('Ctrl Pts',(0.891755122611403,2.97331517273224,19.02366264361));
#91542=CARTESIAN_POINT('Ctrl Pts',(1.88205559728409,2.46854148108454,18.9706410089946));
#91543=CARTESIAN_POINT('Ctrl Pts',(2.43267329472432,1.66316617394455,18.9176193743793));
#91544=CARTESIAN_POINT('Ctrl Pts',(2.98329099216454,0.857790866804561,18.8645977397639));
#91545=CARTESIAN_POINT('Ctrl Pts',(3.09422591237229,-0.248186055827714,
18.8115761051485));
#91546=CARTESIAN_POINT('Ctrl Pts',(2.71453432909591,-1.14687595544508,18.7585544705331));
#91547=CARTESIAN_POINT('Ctrl Pts',(2.33484274581953,-2.04556585506245,18.7055328359177));
#91548=CARTESIAN_POINT('Ctrl Pts',(1.46452465905902,-2.73696873166493,18.6525112013023));
#91549=CARTESIAN_POINT('Ctrl Pts',(0.503249048435527,-2.90357735840927,
18.5994895666869));
#91550=CARTESIAN_POINT('Ctrl Pts',(-0.458026562188004,-3.07018598515363,
18.5464679320716));
#91551=CARTESIAN_POINT('Ctrl Pts',(-1.5102596966745,-2.71200036203983,18.4934462974562));
#91552=CARTESIAN_POINT('Ctrl Pts',(-2.17024203201977,-1.99350711146786,
18.4404246628408));
#91553=CARTESIAN_POINT('Ctrl Pts',(-2.66087163973964,-1.45938060110743,
18.4010084809237));
#91554=CARTESIAN_POINT('Ctrl Pts',(-2.93472748314863,-0.726133423854732,
18.3615922990067));
#91555=CARTESIAN_POINT('Ctrl Pts',(-2.94129852510877,0.00270460087765087,
18.3221761170896));
#91556=CARTESIAN_POINT('Ctrl Pts',(-2.94137747154633,0.00271175267126415,
18.1778238829105));
#91557=CARTESIAN_POINT('Ctrl Pts',(-2.93475143368432,-0.728901082967289,
18.217392842286));
#91558=CARTESIAN_POINT('Ctrl Pts',(-2.65856701665389,-1.46497807346214,
18.2569618016615));
#91559=CARTESIAN_POINT('Ctrl Pts',(-2.16449574177378,-1.99975197690645,
18.296530761037));
#91560=CARTESIAN_POINT('Ctrl Pts',(-1.50230267232571,-2.7164979012034,18.3495641835328));
#91561=CARTESIAN_POINT('Ctrl Pts',(-0.448709362245287,-3.07163377940028,
18.4025976060286));
#91562=CARTESIAN_POINT('Ctrl Pts',(0.512254308613893,-2.90200711725602,
18.4556310285243));
#91563=CARTESIAN_POINT('Ctrl Pts',(1.47321797947303,-2.73238045511176,18.5086644510201));
#91564=CARTESIAN_POINT('Ctrl Pts',(2.34155201111092,-2.03799125262641,18.5616978735158));
#91565=CARTESIAN_POINT('Ctrl Pts',(2.71833623861653,-1.13784791563819,18.6147312960116));
#91566=CARTESIAN_POINT('Ctrl Pts',(3.09512046612215,-0.23770457864997,18.6677647185074));
#91567=CARTESIAN_POINT('Ctrl Pts',(2.98035488949546,0.868192892841143,18.7207981410031));
#91568=CARTESIAN_POINT('Ctrl Pts',(2.42676380731967,1.67178563481728,18.7738315634989));
#91569=CARTESIAN_POINT('Ctrl Pts',(1.87317272514386,2.47537837679345,18.8268649859946));
#91570=CARTESIAN_POINT('Ctrl Pts',(0.880756137418969,2.97666638925464,18.8798984084904));
#91571=CARTESIAN_POINT('Ctrl Pts',(-0.094561191408211,2.94535362331546,
18.9329318309862));
#91572=CARTESIAN_POINT('Ctrl Pts',(-1.06987852023536,2.91404085737629,18.9859652534819));
#91573=CARTESIAN_POINT('Ctrl Pts',(-2.02809659016481,2.35012731303673,19.0389986759777));
#91574=CARTESIAN_POINT('Ctrl Pts',(-2.52900173162973,1.51267975021546,19.0920320984734));
#91575=CARTESIAN_POINT('Ctrl Pts',(-2.79910527450039,1.06110212610704,19.1206293599525));
#91576=CARTESIAN_POINT('Ctrl Pts',(-2.936235941417,0.529989017990088,19.1492266214315));
#91577=CARTESIAN_POINT('Ctrl Pts',(-2.93725371205965,-0.00063370482881248,
19.1778238829105));
#91578=CARTESIAN_POINT('Origin',(0.,0.,0.));
#91579=CARTESIAN_POINT('',(-2.94386718000102,-0.00244699584354052,20.3221761170896));
#91580=CARTESIAN_POINT('',(-2.94371017125697,-0.00248988210239957,20.1778238829105));
#91581=CARTESIAN_POINT('',(-2.942,-3.60291088309151E-16,0.));
#91582=CARTESIAN_POINT('Ctrl Pts',(-2.94386718000102,-0.00244699584354052,
20.3221761170896));
#91583=CARTESIAN_POINT('Ctrl Pts',(-2.93661160233715,0.809560164967209,
20.2781636131092));
#91584=CARTESIAN_POINT('Ctrl Pts',(-2.58699792073722,1.62705246749167,20.2341511091289));
#91585=CARTESIAN_POINT('Ctrl Pts',(-1.98960320148806,2.17382156159301,20.1901386051485));
#91586=CARTESIAN_POINT('Ctrl Pts',(-1.26992489054007,2.83251144525318,20.1371169705331));
#91587=CARTESIAN_POINT('Ctrl Pts',(-0.190644547079911,3.0983035635283,20.0840953359177));
#91588=CARTESIAN_POINT('Ctrl Pts',(0.752608839724244,2.84914039938139,20.0310737013023));
#91589=CARTESIAN_POINT('Ctrl Pts',(1.6958622265284,2.59997723523449,19.9780520666869));
#91590=CARTESIAN_POINT('Ctrl Pts',(2.50308865667655,1.83585878866557,19.9250304320716));
#91591=CARTESIAN_POINT('Ctrl Pts',(2.80359221040288,0.907684856536971,19.8720087974562));
#91592=CARTESIAN_POINT('Ctrl Pts',(3.10409576412921,-0.0204890755916505,
19.8189871628408));
#91593=CARTESIAN_POINT('Ctrl Pts',(2.89787644143367,-1.11271849327995,19.7659655282254));
#91594=CARTESIAN_POINT('Ctrl Pts',(2.27963463695782,-1.86742791105854,19.71294389361));
#91595=CARTESIAN_POINT('Ctrl Pts',(1.66139283248197,-2.6221373288371,19.6599222589946));
#91596=CARTESIAN_POINT('Ctrl Pts',(0.63112854622583,-3.03932674670597,19.6069006243792));
#91597=CARTESIAN_POINT('Ctrl Pts',(-0.338038471351601,-2.92741371741415,
19.5538789897639));
#91598=CARTESIAN_POINT('Ctrl Pts',(-1.30720548892903,-2.81550068812232,
19.5008573551485));
#91599=CARTESIAN_POINT('Ctrl Pts',(-2.21527523782775,-2.1744852116698,19.4478357205331));
#91600=CARTESIAN_POINT('Ctrl Pts',(-2.64524235473507,-1.29873552570718,
19.3948140859177));
#91601=CARTESIAN_POINT('Ctrl Pts',(-2.84158948901698,-0.898819033432462,
19.3706014296417));
#91602=CARTESIAN_POINT('Ctrl Pts',(-2.93823556160944,-0.449952277475836,
19.3463887733656));
#91603=CARTESIAN_POINT('Ctrl Pts',(-2.9372855915547,-0.000697940546887099,
19.3221761170896));
#91604=CARTESIAN_POINT('Ctrl Pts',(-2.93725371205965,-0.00063370482881248,
19.1778238829105));
#91605=CARTESIAN_POINT('Ctrl Pts',(-2.93812338999438,-0.454047130567155,
19.2022600439273));
#91606=CARTESIAN_POINT('Ctrl Pts',(-2.83960909846098,-0.907102497379243,
19.226696204944));
#91607=CARTESIAN_POINT('Ctrl Pts',(-2.63975173092173,-1.30987044565247,
19.2511323659607));
#91608=CARTESIAN_POINT('Ctrl Pts',(-2.20600437574835,-2.18399149739613,
19.3041657884565));
#91609=CARTESIAN_POINT('Ctrl Pts',(-1.29491745240111,-2.82125201958039,
19.3571992109522));
#91610=CARTESIAN_POINT('Ctrl Pts',(-0.325052174039479,-2.92888901623983,
19.410232633448));
#91611=CARTESIAN_POINT('Ctrl Pts',(0.6448131043221,-3.03652601289925,19.4632660559438));
#91612=CARTESIAN_POINT('Ctrl Pts',(1.67345673769806,-2.6145394840339,19.5162994784395));
#91613=CARTESIAN_POINT('Ctrl Pts',(2.2883109435186,-1.85679369103599,19.5693329009353));
#91614=CARTESIAN_POINT('Ctrl Pts',(2.90316514933918,-1.09904789803805,19.622366323431));
#91615=CARTESIAN_POINT('Ctrl Pts',(3.10422992760428,-0.00554284090747439,
19.6753997459268));
#91616=CARTESIAN_POINT('Ctrl Pts',(2.79913438004101,0.921355798685008,19.7284331684226));
#91617=CARTESIAN_POINT('Ctrl Pts',(2.49403883247774,1.8482544382775,19.7814665909183));
#91618=CARTESIAN_POINT('Ctrl Pts',(1.6827829590861,2.60854666033193,19.8345000134141));
#91619=CARTESIAN_POINT('Ctrl Pts',(0.738064725173308,2.8529476417826,19.8875334359098));
#91620=CARTESIAN_POINT('Ctrl Pts',(-0.206653508739454,3.09734862323327,
19.9405668584056));
#91621=CARTESIAN_POINT('Ctrl Pts',(-1.28483410317334,2.82585836408022,19.9936002809014));
#91622=CARTESIAN_POINT('Ctrl Pts',(-2.00115156717165,2.16320183767131,20.0466337033971));
#91623=CARTESIAN_POINT('Ctrl Pts',(-2.59180938424943,1.6167915139912,20.0903637632349));
#91624=CARTESIAN_POINT('Ctrl Pts',(-2.93642751257773,0.804417574374107,
20.1340938230727));
#91625=CARTESIAN_POINT('Ctrl Pts',(-2.94371017125697,-0.00248988210239957,
20.1778238829105));
#91626=CARTESIAN_POINT('Origin',(0.,0.,0.));
#91627=CARTESIAN_POINT('',(-2.94527945804905,0.00190826819681383,21.3221761170896));
#91628=CARTESIAN_POINT('',(-2.94544527640723,0.00182122834732236,21.1778238829105));
#91629=CARTESIAN_POINT('',(-2.942,-3.60291088309151E-16,0.));
#91630=CARTESIAN_POINT('Ctrl Pts',(-2.94527945804905,0.00190826819681383,
21.3221761170896));
#91631=CARTESIAN_POINT('Ctrl Pts',(-2.94613741111825,0.116048922849094,
21.3159817220836));
#91632=CARTESIAN_POINT('Ctrl Pts',(-2.94007944024821,0.230097659896368,
21.3097873270776));
#91633=CARTESIAN_POINT('Ctrl Pts',(-2.92680141464145,0.343299519765235,
21.3035929320716));
#91634=CARTESIAN_POINT('Ctrl Pts',(-2.81314663133309,1.31226382474057,21.2505712974562));
#91635=CARTESIAN_POINT('Ctrl Pts',(-2.17050006882104,2.21917997610633,21.1975496628408));
#91636=CARTESIAN_POINT('Ctrl Pts',(-1.29397899492201,2.64757236760752,21.1445280282254));
#91637=CARTESIAN_POINT('Ctrl Pts',(-0.417457921022976,3.0759647591087,21.09150639361));
#91638=CARTESIAN_POINT('Ctrl Pts',(0.692937664263023,3.02583339074529,21.0384847589946));
#91639=CARTESIAN_POINT('Ctrl Pts',(1.52728997650969,2.52019967634933,20.9854631243793));
#91640=CARTESIAN_POINT('Ctrl Pts',(2.36164228875633,2.01456596195338,20.9324414897639));
#91641=CARTESIAN_POINT('Ctrl Pts',(2.91995132796366,1.05342990152483,20.8794198551485));
#91642=CARTESIAN_POINT('Ctrl Pts',(2.945829449881,0.078166061894146,20.8263982205331));
#91643=CARTESIAN_POINT('Ctrl Pts',(2.97170757179833,-0.897097777736566,
20.7733765859177));
#91644=CARTESIAN_POINT('Ctrl Pts',(2.46515477642569,-1.88648939656947,20.7203549513023));
#91645=CARTESIAN_POINT('Ctrl Pts',(1.65879111605267,-2.43565866129123,20.6673333166869));
#91646=CARTESIAN_POINT('Ctrl Pts',(0.852427455679624,-2.984827926013,20.6143116820716));
#91647=CARTESIAN_POINT('Ctrl Pts',(-0.253747069693798,-3.09377483662359,
20.5612900474562));
#91648=CARTESIAN_POINT('Ctrl Pts',(-1.15175307808728,-2.71246860408277,
20.5082684128408));
#91649=CARTESIAN_POINT('Ctrl Pts',(-2.04975908648074,-2.33116237154196,
20.4552467782254));
#91650=CARTESIAN_POINT('Ctrl Pts',(-2.73959657789424,-1.45960299584977,
20.40222514361));
#91651=CARTESIAN_POINT('Ctrl Pts',(-2.90447718438307,-0.498029483481065,
20.3492035089946));
#91652=CARTESIAN_POINT('Ctrl Pts',(-2.93249274697017,-0.334644452994275,
20.3401943783596));
#91653=CARTESIAN_POINT('Ctrl Pts',(-2.94535235900914,-0.168660638029602,
20.3311852477246));
#91654=CARTESIAN_POINT('Ctrl Pts',(-2.94386718000102,-0.00244699584354052,
20.3221761170896));
#91655=CARTESIAN_POINT('Ctrl Pts',(-2.94371017125697,-0.00248988210239957,
20.1778238829105));
#91656=CARTESIAN_POINT('Ctrl Pts',(-2.94525952232254,-0.174155613337497,
20.1871272455685));
#91657=CARTESIAN_POINT('Ctrl Pts',(-2.93154088692244,-0.345573928578387,
20.1964306082264));
#91658=CARTESIAN_POINT('Ctrl Pts',(-2.9016751811188,-0.514131236725823,
20.2057339708844));
#91659=CARTESIAN_POINT('Ctrl Pts',(-2.73142699750492,-1.47498499104929,
20.2587673933802));
#91660=CARTESIAN_POINT('Ctrl Pts',(-2.03647629671438,-2.34286970603145,
20.3118008158759));
#91661=CARTESIAN_POINT('Ctrl Pts',(-1.13608944176364,-2.71907163671928,
20.3648342383717));
#91662=CARTESIAN_POINT('Ctrl Pts',(-0.235702586812923,-3.0952735674071,
20.4178676608674));
#91663=CARTESIAN_POINT('Ctrl Pts',(0.870120422298012,-2.97979271380062,
20.4709010833632));
#91664=CARTESIAN_POINT('Ctrl Pts',(1.67335493021286,-2.42568197891447,20.523934505859));
#91665=CARTESIAN_POINT('Ctrl Pts',(2.47658943812775,-1.87157124402828,20.5769679283547));
#91666=CARTESIAN_POINT('Ctrl Pts',(2.97723544484651,-0.878830627862415,
20.6300013508505));
#91667=CARTESIAN_POINT('Ctrl Pts',(2.94529184447496,0.0964662436678312,
20.6830347733462));
#91668=CARTESIAN_POINT('Ctrl Pts',(2.9133482441034,1.07176311519802,20.736068195842));
#91669=CARTESIAN_POINT('Ctrl Pts',(2.34881503664154,2.02961624209257,20.7891016183377));
#91670=CARTESIAN_POINT('Ctrl Pts',(1.51104366060626,2.52997961277156,20.8421350408335));
#91671=CARTESIAN_POINT('Ctrl Pts',(0.67327228457098,3.03034298345054,20.8951684633293));
#91672=CARTESIAN_POINT('Ctrl Pts',(-0.437737260037742,3.07321659791399,
20.948201885825));
#91673=CARTESIAN_POINT('Ctrl Pts',(-1.31157757859425,2.63890394683606,21.0012353083208));
#91674=CARTESIAN_POINT('Ctrl Pts',(-2.18541789715079,2.20459129575811,21.0542687308166));
#91675=CARTESIAN_POINT('Ctrl Pts',(-2.82208898965512,1.29309237913876,21.1073021533123));
#91676=CARTESIAN_POINT('Ctrl Pts',(-2.92909864923512,0.323157683410274,
21.1603355758081));
#91677=CARTESIAN_POINT('Ctrl Pts',(-2.94086115485009,0.216542426904973,
21.1661650115089));
#91678=CARTESIAN_POINT('Ctrl Pts',(-2.94622407160623,0.109221125107908,
21.1719944472097));
#91679=CARTESIAN_POINT('Ctrl Pts',(-2.94544527640723,0.00182122834732236,
21.1778238829105));
#91680=CARTESIAN_POINT('Origin',(0.,0.,0.));
#91681=CARTESIAN_POINT('',(-2.93786968250863,0.00148626117932052,22.3221761170896));
#91682=CARTESIAN_POINT('',(-2.93799456442315,0.00160006380599582,22.1778238829105));
#91683=CARTESIAN_POINT('',(-2.942,-3.60291088309151E-16,0.));
#91684=CARTESIAN_POINT('Ctrl Pts',(-2.93786968250863,0.00148626117932052,
22.3221761170896));
#91685=CARTESIAN_POINT('Ctrl Pts',(-2.93967789259735,0.398317401179163,
22.3007781964426));
#91686=CARTESIAN_POINT('Ctrl Pts',(-2.86492885207122,0.794495709771153,
22.2793802757955));
#91687=CARTESIAN_POINT('Ctrl Pts',(-2.71039411649762,1.15662648001562,22.2579823551485));
#91688=CARTESIAN_POINT('Ctrl Pts',(-2.32747446649407,2.05394569619588,22.2049607205331));
#91689=CARTESIAN_POINT('Ctrl Pts',(-1.45467661742421,2.74221557391513,22.1519390859177));
#91690=CARTESIAN_POINT('Ctrl Pts',(-0.492808309653051,2.90536762750519,
22.0989174513023));
#91691=CARTESIAN_POINT('Ctrl Pts',(0.469059998118109,3.06851968109525,22.045895816687));
#91692=CARTESIAN_POINT('Ctrl Pts',(1.51999876459057,2.70655391055611,21.9928741820716));
#91693=CARTESIAN_POINT('Ctrl Pts',(2.17739406868201,1.98569286413751,21.9398525474562));
#91694=CARTESIAN_POINT('Ctrl Pts',(2.83478937277347,1.26483181771889,21.8868309128408));
#91695=CARTESIAN_POINT('Ctrl Pts',(3.0986412144839,0.185075495420776,21.8338092782254));
#91696=CARTESIAN_POINT('Ctrl Pts',(2.84778309394186,-0.757728533762051,
21.78078764361));
#91697=CARTESIAN_POINT('Ctrl Pts',(2.59692497339982,-1.70053256294485,21.7277660089946));
#91698=CARTESIAN_POINT('Ctrl Pts',(1.83135689060535,-2.50638429901237,21.6747443743793));
#91699=CARTESIAN_POINT('Ctrl Pts',(0.90264434687977,-2.80521911159614,21.6217227397639));
#91700=CARTESIAN_POINT('Ctrl Pts',(-0.0260681968458087,-3.1040539241799,
21.5687011051485));
#91701=CARTESIAN_POINT('Ctrl Pts',(-1.11792520150249,-2.89587181327991,
21.5156794705331));
#91702=CARTESIAN_POINT('Ctrl Pts',(-1.87152220177849,-2.27627452853746,
21.4626578359177));
#91703=CARTESIAN_POINT('Ctrl Pts',(-2.53707820654536,-1.72906336229535,
21.4158305963083));
#91704=CARTESIAN_POINT('Ctrl Pts',(-2.93879366340633,-0.860951103764374,
21.369003356699));
#91705=CARTESIAN_POINT('Ctrl Pts',(-2.94527945804905,0.00190826819681383,
21.3221761170896));
#91706=CARTESIAN_POINT('Ctrl Pts',(-2.94544527640723,0.00182122834732236,
21.1778238829105));
#91707=CARTESIAN_POINT('Ctrl Pts',(-2.93913896475443,-0.867851853003506,
21.2250278697055));
#91708=CARTESIAN_POINT('Ctrl Pts',(-2.53012139393514,-1.74267839595515,
21.2722318565004));
#91709=CARTESIAN_POINT('Ctrl Pts',(-1.85531320966215,-2.28951144992795,
21.3194358432953));
#91710=CARTESIAN_POINT('Ctrl Pts',(-1.09716988385351,-2.90387541270011,
21.3724692657911));
#91711=CARTESIAN_POINT('Ctrl Pts',(-0.00353500558054817,-3.10423286340682,
21.4255026882869));
#91712=CARTESIAN_POINT('Ctrl Pts',(0.923166102530367,-2.79853785617364,
21.4785361107826));
#91713=CARTESIAN_POINT('Ctrl Pts',(1.84986721064131,-2.49284284894045,21.5315695332784));
#91714=CARTESIAN_POINT('Ctrl Pts',(2.60963454859019,-1.68109538376735,21.5846029557741));
#91715=CARTESIAN_POINT('Ctrl Pts',(2.85342442960947,-0.736219267478046,
21.6376363782699));
#91716=CARTESIAN_POINT('Ctrl Pts',(3.09721431062875,0.208656848811227,21.6906698007657));
#91717=CARTESIAN_POINT('Ctrl Pts',(2.82502673471846,1.28666161621668,21.7437032232614));
#91718=CARTESIAN_POINT('Ctrl Pts',(2.16190702857628,2.00255032023931,21.7967366457572));
#91719=CARTESIAN_POINT('Ctrl Pts',(1.49878732243405,2.71843902426198,21.849770068253));
#91720=CARTESIAN_POINT('Ctrl Pts',(0.444735486059899,3.07221166490178,21.9028034907487));
#91721=CARTESIAN_POINT('Ctrl Pts',(-0.51600794974714,2.90134203104285,21.9558369132445));
#91722=CARTESIAN_POINT('Ctrl Pts',(-1.4767513855541,2.73047239718393,22.0088703357402));
#91723=CARTESIAN_POINT('Ctrl Pts',(-2.34418642079396,2.03496048882639,22.061903758236));
#91724=CARTESIAN_POINT('Ctrl Pts',(-2.71980589727694,1.13433049259714,22.1149371807317));
#91725=CARTESIAN_POINT('Ctrl Pts',(-2.86827497607355,0.778343345368319,
22.1358994147913));
#91726=CARTESIAN_POINT('Ctrl Pts',(-2.93990569515241,0.390309758900483,
22.1568616488509));
#91727=CARTESIAN_POINT('Ctrl Pts',(-2.93799456442315,0.00160006380599582,
22.1778238829105));
#91728=CARTESIAN_POINT('Origin',(0.,0.,0.));
#91729=CARTESIAN_POINT('',(-2.93982555808591,-0.00247806991730104,23.3221761170896));
#91730=CARTESIAN_POINT('',(-2.93957643049581,-0.00241049697055628,23.1778238829105));
#91731=CARTESIAN_POINT('',(-2.942,-3.60291088309151E-16,0.));
#91732=CARTESIAN_POINT('Ctrl Pts',(-2.93982555808591,-0.00247806991730104,
23.3221761170896));
#91733=CARTESIAN_POINT('Ctrl Pts',(-2.9344443745828,0.675173062708582,23.2855746708015));
#91734=CARTESIAN_POINT('Ctrl Pts',(-2.70155654492499,1.35616333535824,23.2489732245135));
#91735=CARTESIAN_POINT('Ctrl Pts',(-2.27290706666078,1.87561044658578,23.2123717782254));
#91736=CARTESIAN_POINT('Ctrl Pts',(-1.65195630324756,2.62809259488021,23.15935014361));
#91737=CARTESIAN_POINT('Ctrl Pts',(-0.620199002997637,3.04157582706469,
23.1063285089946));
#91738=CARTESIAN_POINT('Ctrl Pts',(0.348559459157085,2.92617965689914,23.0533068743793));
#91739=CARTESIAN_POINT('Ctrl Pts',(1.31731792131181,2.81078348673359,23.0002852397639));
#91740=CARTESIAN_POINT('Ctrl Pts',(2.22307754537133,2.16650791421801,22.9472636051485));
#91741=CARTESIAN_POINT('Ctrl Pts',(2.64989382755387,1.28921828396519,22.8942419705331));
#91742=CARTESIAN_POINT('Ctrl Pts',(3.07671010973638,0.411928653712412,22.8412203359177));
#91743=CARTESIAN_POINT('Ctrl Pts',(3.02458305004197,-0.698375034277577,
22.7881987013023));
#91744=CARTESIAN_POINT('Ctrl Pts',(2.5174505271332,-1.53181719681397,22.7351770666869));
#91745=CARTESIAN_POINT('Ctrl Pts',(2.0103180042244,-2.36525935935041,22.6821554320716));
#91746=CARTESIAN_POINT('Ctrl Pts',(1.04818001810119,-2.92183999643322,22.6291337974562));
#91747=CARTESIAN_POINT('Ctrl Pts',(0.0728712416473015,-2.94596518362981,
22.5761121628408));
#91748=CARTESIAN_POINT('Ctrl Pts',(-0.902437534806564,-2.9700903708264,
22.5230905282254));
#91749=CARTESIAN_POINT('Ctrl Pts',(-1.89091710159111,-2.4617601081368,22.47006889361));
#91750=CARTESIAN_POINT('Ctrl Pts',(-2.43863615951476,-1.65441069947136,
22.4170472589946));
#91751=CARTESIAN_POINT('Ctrl Pts',(-2.76531244832466,-1.17288298050626,
22.3854235450263));
#91752=CARTESIAN_POINT('Ctrl Pts',(-2.93519735188436,-0.584985418573476,
22.3537998310579));
#91753=CARTESIAN_POINT('Ctrl Pts',(-2.93786968250863,0.00148626117932052,
22.3221761170896));
#91754=CARTESIAN_POINT('Ctrl Pts',(-2.93799456442315,0.00160006380599582,
22.1778238829105));
#91755=CARTESIAN_POINT('Ctrl Pts',(-2.93507062828303,-0.593106676081661,
22.2098950713467));
#91756=CARTESIAN_POINT('Ctrl Pts',(-2.76000362972722,-1.18939601703009,
22.2419662597829));
#91757=CARTESIAN_POINT('Ctrl Pts',(-2.42459913570607,-1.67492352554719,
22.274037448219));
#91758=CARTESIAN_POINT('Ctrl Pts',(-1.86996897992613,-2.47779946336128,
22.3270708707148));
#91759=CARTESIAN_POINT('Ctrl Pts',(-0.87690475064014,-2.97780325488844,
22.3801042932106));
#91760=CARTESIAN_POINT('Ctrl Pts',(0.0983712555699952,-2.94522883344837,
22.4331377157063));
#91761=CARTESIAN_POINT('Ctrl Pts',(1.0736472617801,-2.91265441200831,22.4861711382021));
#91762=CARTESIAN_POINT('Ctrl Pts',(2.03113504491436,-2.34750177760105,22.5392045606978));
#91763=CARTESIAN_POINT('Ctrl Pts',(2.53095643547645,-1.50940693884003,22.5922379831936));
#91764=CARTESIAN_POINT('Ctrl Pts',(3.03077782603854,-0.671312100078998,
22.6452714056893));
#91765=CARTESIAN_POINT('Ctrl Pts',(3.07293282402846,0.439724943035805,22.6983048281851));
#91766=CARTESIAN_POINT('Ctrl Pts',(2.63805505874409,1.31328416282721,22.7513382506809));
#91767=CARTESIAN_POINT('Ctrl Pts',(2.20317729345972,2.18684338261864,22.8043716731766));
#91768=CARTESIAN_POINT('Ctrl Pts',(1.29126676490102,2.82292477908666,22.8574050956724));
#91769=CARTESIAN_POINT('Ctrl Pts',(0.321263057585504,2.92930705681888,22.9104385181681));
#91770=CARTESIAN_POINT('Ctrl Pts',(-0.648740649729987,3.0356893345511,22.9634719406639));
#91771=CARTESIAN_POINT('Ctrl Pts',(-1.6768375358023,2.61237249354755,23.0165053631597));
#91772=CARTESIAN_POINT('Ctrl Pts',(-2.29071099850207,1.85383195210346,23.0695387856554));
#91773=CARTESIAN_POINT('Ctrl Pts',(-2.70851889198083,1.33756232164056,23.1056338180738));
#91774=CARTESIAN_POINT('Ctrl Pts',(-2.93444656187858,0.666007415259461,
23.1417288504922));
#91775=CARTESIAN_POINT('Ctrl Pts',(-2.93957643049581,-0.00241049697055628,
23.1778238829105));
#91776=CARTESIAN_POINT('Origin',(0.,0.,0.));
#91777=CARTESIAN_POINT('',(-2.94679320362931,-0.000419630752076516,24.3221761170896));
#91778=CARTESIAN_POINT('',(-2.94671321490455,-0.00061974086392264,24.1778238829105));
#91779=CARTESIAN_POINT('',(-2.942,-3.60291088309151E-16,0.));
#91780=CARTESIAN_POINT('Ctrl Pts',(-2.94679320362931,-0.000419630752076516,
24.3221761170896));
#91781=CARTESIAN_POINT('Ctrl Pts',(-2.94489621355737,0.952864368939043,
24.2703711451605));
#91782=CARTESIAN_POINT('Ctrl Pts',(-2.43980905770987,1.90787363364129,24.2185661732314));
#91783=CARTESIAN_POINT('Ctrl Pts',(-1.65002493835147,2.44160577977619,24.1667612013023));
#91784=CARTESIAN_POINT('Ctrl Pts',(-0.841692389518663,2.98787286150696,
24.1137395666869));
#91785=CARTESIAN_POINT('Ctrl Pts',(0.264866620290473,3.09284270349453,24.0607179320716));
#91786=CARTESIAN_POINT('Ctrl Pts',(1.16149614548691,2.70831087304196,24.0076962974562));
#91787=CARTESIAN_POINT('Ctrl Pts',(2.05812567068335,2.32377904258938,23.9546746628408));
#91788=CARTESIAN_POINT('Ctrl Pts',(2.74482571126712,1.44974553969667,23.9016530282254));
#91789=CARTESIAN_POINT('Ctrl Pts',(2.90624868489911,0.487585543818128,23.84863139361));
#91790=CARTESIAN_POINT('Ctrl Pts',(3.0676716585311,-0.474574452060386,23.7956097589946));
#91791=CARTESIAN_POINT('Ctrl Pts',(2.70381756521139,-1.52486094092468,23.7425881243793));
#91792=CARTESIAN_POINT('Ctrl Pts',(1.98177611204847,-2.18095954174586,23.6895664897639));
#91793=CARTESIAN_POINT('Ctrl Pts',(1.25973465888552,-2.83705814256706,23.6365448551485));
#91794=CARTESIAN_POINT('Ctrl Pts',(0.179505845879314,-3.09896885534504,
23.5835232205331));
#91795=CARTESIAN_POINT('Ctrl Pts',(-0.762845779973811,-2.84641658879975,
23.5305015859177));
#91796=CARTESIAN_POINT('Ctrl Pts',(-1.70519740582696,-2.59386432225444,
23.4774799513023));
#91797=CARTESIAN_POINT('Ctrl Pts',(-2.50967184452705,-1.82684907638581,
23.4244583166869));
#91798=CARTESIAN_POINT('Ctrl Pts',(-2.8068369505888,-0.897600921249319,
23.3714366820716));
#91799=CARTESIAN_POINT('Ctrl Pts',(-2.89886555440755,-0.609823491887907,
23.3550164937442));
#91800=CARTESIAN_POINT('Ctrl Pts',(-2.94223967161163,-0.306486800347378,
23.3385963054169));
#91801=CARTESIAN_POINT('Ctrl Pts',(-2.93982555808591,-0.00247806991730104,
23.3221761170896));
#91802=CARTESIAN_POINT('Ctrl Pts',(-2.93957643049581,-0.00241049697055628,
23.1778238829105));
#91803=CARTESIAN_POINT('Ctrl Pts',(-2.94198373448926,-0.316080344966286,
23.1947622729879));
#91804=CARTESIAN_POINT('Ctrl Pts',(-2.89576777188966,-0.629059375834195,
23.2117006630653));
#91805=CARTESIAN_POINT('Ctrl Pts',(-2.79794016151588,-0.924976020161902,
23.2286390531427));
#91806=CARTESIAN_POINT('Ctrl Pts',(-2.4916458225027,-1.85147920909858,23.2816724756384));
#91807=CARTESIAN_POINT('Ctrl Pts',(-1.67940710514908,-2.61072134508725,
23.3347058981342));
#91808=CARTESIAN_POINT('Ctrl Pts',(-0.734373501779644,-2.85390002368373,
23.38773932063));
#91809=CARTESIAN_POINT('Ctrl Pts',(0.210660101589743,-3.09707870228019,
23.4407727431257));
#91810=CARTESIAN_POINT('Ctrl Pts',(1.28848859097492,-2.8241939234845,23.4938061656215));
#91811=CARTESIAN_POINT('Ctrl Pts',(2.00394823552418,-2.16061131503044,23.5468395881172));
#91812=CARTESIAN_POINT('Ctrl Pts',(2.71940788007347,-1.49702870657636,23.599873010613));
#91813=CARTESIAN_POINT('Ctrl Pts',(3.07249867978681,-0.442748268463822,
23.6529064331088));
#91814=CARTESIAN_POINT('Ctrl Pts',(2.90100766716762,0.517884446892132,23.7059398556045));
#91815=CARTESIAN_POINT('Ctrl Pts',(2.72951665454842,1.47851716224811,23.7589732781003));
#91816=CARTESIAN_POINT('Ctrl Pts',(2.03344382959672,2.34550215484754,23.812006700596));
#91817=CARTESIAN_POINT('Ctrl Pts',(1.13257106887453,2.72053901998234,23.8650401230918));
#91818=CARTESIAN_POINT('Ctrl Pts',(0.231698308152341,3.09557588511714,23.9180735455876));
#91819=CARTESIAN_POINT('Ctrl Pts',(-0.873974388340304,2.97866462278731,
23.9711069680833));
#91820=CARTESIAN_POINT('Ctrl Pts',(-1.67649142016412,2.42351527814746,24.0241403905791));
#91821=CARTESIAN_POINT('Ctrl Pts',(-2.4516857177852,1.88726671365922,24.0753682213562));
#91822=CARTESIAN_POINT('Ctrl Pts',(-2.94401560406121,0.942112851897334,
24.1265960521334));
#91823=CARTESIAN_POINT('Ctrl Pts',(-2.94671321490455,-0.00061974086392264,
24.1778238829105));
#91824=CARTESIAN_POINT('Origin',(0.,0.,0.));
#91825=CARTESIAN_POINT('',(-2.94108940257125,0.00269036361580877,25.3221761170896));
#91826=CARTESIAN_POINT('',(-2.94145356055697,0.00271483987803603,25.1778238829105));
#91827=CARTESIAN_POINT('',(-2.942,-3.60291088309151E-16,0.));
#91828=CARTESIAN_POINT('Ctrl Pts',(-2.94108940257125,0.00269036361580877,
25.3221761170896));
#91829=CARTESIAN_POINT('Ctrl Pts',(-2.94339537070129,0.261365886758737,
25.3081892541349));
#91830=CARTESIAN_POINT('Ctrl Pts',(-2.91210970553165,0.519492689068858,
25.2942023911801));
#91831=CARTESIAN_POINT('Ctrl Pts',(-2.84504088836942,0.767960561828773,
25.2802155282254));
#91832=CARTESIAN_POINT('Ctrl Pts',(-2.59079529168549,1.70985674010536,25.22719389361));
#91833=CARTESIAN_POINT('Ctrl Pts',(-1.82233536056913,2.51295128260037,25.1741722589946));
#91834=CARTESIAN_POINT('Ctrl Pts',(-0.892554595938133,2.80844572215451,
25.1211506243792));
#91835=CARTESIAN_POINT('Ctrl Pts',(0.037226168692838,3.10394016170864,25.0681289897638));
#91836=CARTESIAN_POINT('Ctrl Pts',(1.12832776683841,2.89183449832193,25.0151073551485));
#91837=CARTESIAN_POINT('Ctrl Pts',(1.87969263227361,2.26953226220615,24.9620857205331));
#91838=CARTESIAN_POINT('Ctrl Pts',(2.63105749770886,1.64723002609033,24.9090640859177));
#91839=CARTESIAN_POINT('Ctrl Pts',(3.04268563043366,0.614731217245394,24.8560424513023));
#91840=CARTESIAN_POINT('Ctrl Pts',(2.92554844619577,-0.353818272535112,
24.8030208166869));
#91841=CARTESIAN_POINT('Ctrl Pts',(2.80841126195789,-1.32236776231556,24.7499991820715));
#91842=CARTESIAN_POINT('Ctrl Pts',(2.16250876075731,-2.22696793303165,24.6969775474562));
#91843=CARTESIAN_POINT('Ctrl Pts',(1.28445340821624,-2.65220672707463,24.6439559128408));
#91844=CARTESIAN_POINT('Ctrl Pts',(0.406398055675107,-3.07744552111764,
24.5909342782254));
#91845=CARTESIAN_POINT('Ctrl Pts',(-0.703810148206556,-3.02332293848755,
24.53791264361));
#91846=CARTESIAN_POINT('Ctrl Pts',(-1.53633946861557,-2.51469324534669,
24.4848910089946));
#91847=CARTESIAN_POINT('Ctrl Pts',(-2.36886878902454,-2.00606355220585,
24.4318693743792));
#91848=CARTESIAN_POINT('Ctrl Pts',(-2.92371922596088,-1.04292674855432,
24.3788477397639));
#91849=CARTESIAN_POINT('Ctrl Pts',(-2.94609140050085,-0.067576185991548,
24.3258261051485));
#91850=CARTESIAN_POINT('Ctrl Pts',(-2.94660476434132,-0.0451952721601265,
24.3246094424622));
#91851=CARTESIAN_POINT('Ctrl Pts',(-2.94683775528045,-0.0228079272548677,
24.3233927797759));
#91852=CARTESIAN_POINT('Ctrl Pts',(-2.94679320362931,-0.000419630752076516,
24.3221761170896));
#91853=CARTESIAN_POINT('Ctrl Pts',(-2.94671321490455,-0.00061974086392264,
24.1778238829105));
#91854=CARTESIAN_POINT('Ctrl Pts',(-2.94680829571755,-0.0338475808200229,
24.1796294746291));
#91855=CARTESIAN_POINT('Ctrl Pts',(-2.94629510538745,-0.0670724128288604,
24.1814350663477));
#91856=CARTESIAN_POINT('Ctrl Pts',(-2.94516459026207,-0.100276226317684,
24.1832406580664));
#91857=CARTESIAN_POINT('Ctrl Pts',(-2.91195936138129,-1.07553095919334,
24.2362740805621));
#91858=CARTESIAN_POINT('Ctrl Pts',(-2.34618753646466,-2.03265299799483,
24.2893075030579));
#91859=CARTESIAN_POINT('Ctrl Pts',(-1.50776958560142,-2.53193219933579,
24.3423409255536));
#91860=CARTESIAN_POINT('Ctrl Pts',(-0.66935163473825,-3.03121140067672,
24.3953743480494));
#91861=CARTESIAN_POINT('Ctrl Pts',(0.441712442071503,-3.07264776455723,
24.4484077705452));
#91862=CARTESIAN_POINT('Ctrl Pts',(1.31499019763738,-2.63720506700099,24.5014411930409));
#91863=CARTESIAN_POINT('Ctrl Pts',(2.18826795320328,-2.20176236944474,24.5544746155367));
#91864=CARTESIAN_POINT('Ctrl Pts',(2.82375938752531,-1.28944061045169,24.6075080380325));
#91865=CARTESIAN_POINT('Ctrl Pts',(2.92951423890392,-0.319368297357882,
24.6605414605282));
#91866=CARTESIAN_POINT('Ctrl Pts',(3.03526909028253,0.650704015735951,24.713574883024));
#91867=CARTESIAN_POINT('Ctrl Pts',(2.61128735871772,1.67852688293051,24.7666083055197));
#91868=CARTESIAN_POINT('Ctrl Pts',(1.85234991897961,2.29190958873912,24.8196417280155));
#91869=CARTESIAN_POINT('Ctrl Pts',(1.09341247924151,2.90529229454771,24.8726751505112));
#91870=CARTESIAN_POINT('Ctrl Pts',(-0.000480668669881057,3.1042348389703,
24.925708573007));
#91871=CARTESIAN_POINT('Ctrl Pts',(-0.926785550822343,2.79734129631781,
24.9787419955028));
#91872=CARTESIAN_POINT('Ctrl Pts',(-1.85309043297486,2.4904477536653,25.0317754179985));
#91873=CARTESIAN_POINT('Ctrl Pts',(-2.61180704936844,1.67771812393763,25.0848088404943));
#91874=CARTESIAN_POINT('Ctrl Pts',(-2.85437442380639,0.732527428850295,
25.13784226299));
#91875=CARTESIAN_POINT('Ctrl Pts',(-2.91533118222703,0.495002654566948,
25.1511694696302));
#91876=CARTESIAN_POINT('Ctrl Pts',(-2.94369269586688,0.249112856181335,
25.1644966762703));
#91877=CARTESIAN_POINT('Ctrl Pts',(-2.94145356055697,0.00271483987803603,
25.1778238829105));
#91878=CARTESIAN_POINT('Origin',(0.,0.,0.));
#91879=CARTESIAN_POINT('',(-2.93733956291468,-0.000810573463508324,26.3221761170896));
#91880=CARTESIAN_POINT('',(-2.93723794832128,-0.000592575232268764,26.1778238829105));
#91881=CARTESIAN_POINT('',(-2.942,-3.60291088309151E-16,0.));
#91882=CARTESIAN_POINT('Ctrl Pts',(-2.93733956291468,-0.000810573463508324,
26.3221761170896));
#91883=CARTESIAN_POINT('Ctrl Pts',(-2.93600810479843,0.540778397853635,
26.2929857284938));
#91884=CARTESIAN_POINT('Ctrl Pts',(-2.79277081125737,1.0830223511668,26.2637953398981));
#91885=CARTESIAN_POINT('Ctrl Pts',(-2.5119278398973,1.54085677730512,26.2346049513023));
#91886=CARTESIAN_POINT('Ctrl Pts',(-2.00180261964182,2.3724705661185,26.1815833166869));
#91887=CARTESIAN_POINT('Ctrl Pts',(-1.03767010985474,2.92558901047594,26.1285616820716));
#91888=CARTESIAN_POINT('Ctrl Pts',(-0.0622809120321974,2.94620810008639,
26.0755400474562));
#91889=CARTESIAN_POINT('Ctrl Pts',(0.913108285790287,2.96682718969685,26.0225184128408));
#91890=CARTESIAN_POINT('Ctrl Pts',(1.89975417164822,2.4549469245604,25.9694967782254));
#91891=CARTESIAN_POINT('Ctrl Pts',(2.44456751248201,1.64563384686137,25.91647514361));
#91892=CARTESIAN_POINT('Ctrl Pts',(2.98938085331583,0.836320769162291,25.8634535089946));
#91893=CARTESIAN_POINT('Ctrl Pts',(3.09236164912545,-0.270425121099402,
25.8104318743793));
#91894=CARTESIAN_POINT('Ctrl Pts',(2.70621888044578,-1.16636205876949,25.7574102397639));
#91895=CARTESIAN_POINT('Ctrl Pts',(2.32007611176614,-2.06229899643953,25.7043886051485));
#91896=CARTESIAN_POINT('Ctrl Pts',(1.44480977859727,-2.747426981518,25.6513669705331));
#91897=CARTESIAN_POINT('Ctrl Pts',(0.482361202848739,-2.90712035371853,
25.5983453359177));
#91898=CARTESIAN_POINT('Ctrl Pts',(-0.480087372899792,-3.06681372591906,
25.5453237013023));
#91899=CARTESIAN_POINT('Ctrl Pts',(-1.52971819122799,-2.70107248524166,
25.4923020666869));
#91900=CARTESIAN_POINT('Ctrl Pts',(-2.18451796926637,-1.97785295787391,
25.4392804320716));
#91901=CARTESIAN_POINT('Ctrl Pts',(-2.66658458234967,-1.44541541014243,
25.4002456604109));
#91902=CARTESIAN_POINT('Ctrl Pts',(-2.93465386804832,-0.719225623747977,
25.3612108887503));
#91903=CARTESIAN_POINT('Ctrl Pts',(-2.94108940257125,0.00269036361580877,
25.3221761170896));
#91904=CARTESIAN_POINT('Ctrl Pts',(-2.94145356055697,0.00271483987803603,
25.1778238829105));
#91905=CARTESIAN_POINT('Ctrl Pts',(-2.93478242591144,-0.731387443210676,
25.2175300987661));
#91906=CARTESIAN_POINT('Ctrl Pts',(-2.65648652101379,-1.47000089125401,
25.2572363146217));
#91907=CARTESIAN_POINT('Ctrl Pts',(-2.15931469757571,-2.00534531244163,
25.2969425304773));
#91908=CARTESIAN_POINT('Ctrl Pts',(-1.4952694644247,-2.72037559819935,25.3499759529731));
#91909=CARTESIAN_POINT('Ctrl Pts',(-0.440760865640405,-3.07278440926782,
25.4030093754689));
#91910=CARTESIAN_POINT('Ctrl Pts',(0.519760727376244,-2.90067208963292,
25.4560427979646));
#91911=CARTESIAN_POINT('Ctrl Pts',(1.48028232039289,-2.72855976999802,25.5090762204604));
#91912=CARTESIAN_POINT('Ctrl Pts',(2.34681690764188,-2.03192631965965,25.5621096429561));
#91913=CARTESIAN_POINT('Ctrl Pts',(2.72127100452882,-1.1308111713318,25.6151430654519));
#91914=CARTESIAN_POINT('Ctrl Pts',(3.09572510141573,-0.229696023004005,
25.6681764879476));
#91915=CARTESIAN_POINT('Ctrl Pts',(2.97809870794077,0.875900823313237,25.7212099104434));
#91916=CARTESIAN_POINT('Ctrl Pts',(2.42243040669225,1.67805861340744,25.7742433329392));
#91917=CARTESIAN_POINT('Ctrl Pts',(1.8667621054437,2.48021640350168,25.8272767554349));
#91918=CARTESIAN_POINT('Ctrl Pts',(0.873051896421506,2.97893513737279,25.8803101779307));
#91919=CARTESIAN_POINT('Ctrl Pts',(-0.102181155114106,2.94509911494293,
25.9333436004265));
#91920=CARTESIAN_POINT('Ctrl Pts',(-1.07741420664972,2.91126309251307,25.9863770229222));
#91921=CARTESIAN_POINT('Ctrl Pts',(-2.03417010069878,2.34487231378225,26.039410445418));
#91922=CARTESIAN_POINT('Ctrl Pts',(-2.53290690394125,1.50613160157566,26.0924438679137));
#91923=CARTESIAN_POINT('Ctrl Pts',(-2.80055042467695,1.05602742690899,26.1209038729126));
#91924=CARTESIAN_POINT('Ctrl Pts',(-2.93629108483062,0.527490418271314,
26.1493638779116));
#91925=CARTESIAN_POINT('Ctrl Pts',(-2.93723794832128,-0.000592575232268764,
26.1778238829105));
#91926=CARTESIAN_POINT('Origin',(0.,0.,0.));
#91927=CARTESIAN_POINT('',(-2.94407188513322,-0.00239011867426281,27.3221761170896));
#91928=CARTESIAN_POINT('',(-2.94363499374191,-0.002507597635829,27.1778238829105));
#91929=CARTESIAN_POINT('',(-2.942,-3.60291088309151E-16,0.));
#91930=CARTESIAN_POINT('Ctrl Pts',(-2.94407188513322,-0.00239011867426281,
27.3221761170896));
#91931=CARTESIAN_POINT('Ctrl Pts',(-2.93685821302976,0.816506344639196,
27.2777822028528));
#91932=CARTESIAN_POINT('Ctrl Pts',(-2.58044453554868,1.64090832397564,27.233388288616));
#91933=CARTESIAN_POINT('Ctrl Pts',(-1.97392341428739,2.18806933974823,27.1889943743792));
#91934=CARTESIAN_POINT('Ctrl Pts',(-1.24952814906002,2.84156817968708,27.1359727397639));
#91935=CARTESIAN_POINT('Ctrl Pts',(-0.168364825121207,3.09959410258269,
27.0829511051485));
#91936=CARTESIAN_POINT('Ctrl Pts',(0.773072862803339,2.84365599709516,27.0299294705331));
#91937=CARTESIAN_POINT('Ctrl Pts',(1.71451055072783,2.58771789160765,26.9769078359177));
#91938=CARTESIAN_POINT('Ctrl Pts',(2.51622260263805,1.81781575773695,26.9238862013023));
#91939=CARTESIAN_POINT('Ctrl Pts',(2.81004542109612,0.887505387248421,26.870864566687));
#91940=CARTESIAN_POINT('Ctrl Pts',(3.1038682395542,-0.0428049832401568,
26.8178429320716));
#91941=CARTESIAN_POINT('Ctrl Pts',(2.88980182456017,-1.13352359034658,26.7648212974562));
#91942=CARTESIAN_POINT('Ctrl Pts',(2.26615012607589,-1.88376874565444,26.7117996628408));
#91943=CARTESIAN_POINT('Ctrl Pts',(1.6424984275916,-2.63401390096229,26.6587780282254));
#91944=CARTESIAN_POINT('Ctrl Pts',(0.609261445617043,-3.04378560447153,
26.60575639361));
#91945=CARTESIAN_POINT('Ctrl Pts',(-0.359075942910748,-2.92490778457048,
26.5527347589946));
#91946=CARTESIAN_POINT('Ctrl Pts',(-1.32741333143854,-2.80602996466943,
26.4997131243793));
#91947=CARTESIAN_POINT('Ctrl Pts',(-2.23085112651959,-2.1585026213581,26.4466914897639));
#91948=CARTESIAN_POINT('Ctrl Pts',(-2.65451105869814,-1.27968438306777,
26.3936698551485));
#91949=CARTESIAN_POINT('Ctrl Pts',(-2.84493038744279,-0.884688381998503,
26.3698386091289));
#91950=CARTESIAN_POINT('Ctrl Pts',(-2.93842657502584,-0.442967757313165,
26.3460073631092));
#91951=CARTESIAN_POINT('Ctrl Pts',(-2.93733956291468,-0.000810573463508324,
26.3221761170896));
#91952=CARTESIAN_POINT('Ctrl Pts',(-2.93723794832128,-0.000592575232268764,
26.1778238829105));
#91953=CARTESIAN_POINT('Ctrl Pts',(-2.93805550516533,-0.456558899652427,
26.2023973004073));
#91954=CARTESIAN_POINT('Ctrl Pts',(-2.83838115668472,-0.91218674524788,
26.2269707179042));
#91955=CARTESIAN_POINT('Ctrl Pts',(-2.63635397196237,-1.31669568231095,
26.251544135401));
#91956=CARTESIAN_POINT('Ctrl Pts',(-2.20034652430512,-2.18969160830876,
26.3045775578967));
#91957=CARTESIAN_POINT('Ctrl Pts',(-1.2876139165547,-2.82459281462198,26.3576109803925));
#91958=CARTESIAN_POINT('Ctrl Pts',(-0.31747340351993,-2.92972019540357,
26.4106444028883));
#91959=CARTESIAN_POINT('Ctrl Pts',(0.652667109514815,-3.03484757618516,
26.463677825384));
#91960=CARTESIAN_POINT('Ctrl Pts',(1.68021552783393,-2.61020113143511,26.5167112478798));
#91961=CARTESIAN_POINT('Ctrl Pts',(2.29310722013781,-1.85086711091042,26.5697446703756));
#91962=CARTESIAN_POINT('Ctrl Pts',(2.9059989124417,-1.09153309038574,26.6227780928713));
#91963=CARTESIAN_POINT('Ctrl Pts',(3.10423387873042,0.00248850591357333,
26.6758115153671));
#91964=CARTESIAN_POINT('Ctrl Pts',(2.79674126082988,0.928594693754894,26.7288449378628));
#91965=CARTESIAN_POINT('Ctrl Pts',(2.48924864292936,1.85470088159619,26.7818783603586));
#91966=CARTESIAN_POINT('Ctrl Pts',(1.67602844083961,2.61289166097947,26.8349117828543));
#91967=CARTESIAN_POINT('Ctrl Pts',(0.73068104946248,2.85484762977895,26.8879452053501));
#91968=CARTESIAN_POINT('Ctrl Pts',(-0.214666341914737,3.09680359857845,
26.9409786278459));
#91969=CARTESIAN_POINT('Ctrl Pts',(-1.29214092257942,2.82252475679402,26.9940120503416));
#91970=CARTESIAN_POINT('Ctrl Pts',(-2.00674155040704,2.15801717675463,27.0470454728374));
#91971=CARTESIAN_POINT('Ctrl Pts',(-2.59413423943573,1.61180034021774,27.0906382761951));
#91972=CARTESIAN_POINT('Ctrl Pts',(-2.93634634043979,0.801920292911836,
27.1342310795528));
#91973=CARTESIAN_POINT('Ctrl Pts',(-2.94363499374191,-0.002507597635829,
27.1778238829105));
#91974=CARTESIAN_POINT('Origin',(0.,0.,0.));
#91975=CARTESIAN_POINT('',(-2.94510414404698,0.00199674015882861,28.3221761170896));
#91976=CARTESIAN_POINT('',(-2.94550455047329,0.00178675002179936,28.1778238829105));
#91977=CARTESIAN_POINT('',(-2.942,-3.60291088309151E-16,0.));
#91978=CARTESIAN_POINT('Ctrl Pts',(-2.94510414404698,0.00199674015882861,
28.3221761170896));
#91979=CARTESIAN_POINT('Ctrl Pts',(-2.94604657952822,0.123184313699714,
28.3156003118272));
#91980=CARTESIAN_POINT('Ctrl Pts',(-2.93921686867972,0.244264808562547,
28.3090245065647));
#91981=CARTESIAN_POINT('Ctrl Pts',(-2.92425767409291,0.364332453299115,
28.3024487013023));
#91982=CARTESIAN_POINT('Ctrl Pts',(-2.80363960256099,1.33245461238088,28.2494270666869));
#91983=CARTESIAN_POINT('Ctrl Pts',(-2.15448950896227,2.23472711329033,28.1964054320716));
#91984=CARTESIAN_POINT('Ctrl Pts',(-1.27491122392638,2.65680681498011,28.1433837974562));
#91985=CARTESIAN_POINT('Ctrl Pts',(-0.395332938890521,3.07888651666988,
28.0903621628408));
#91986=CARTESIAN_POINT('Ctrl Pts',(0.714673537582494,3.02077341913999,28.0373405282254));
#91987=CARTESIAN_POINT('Ctrl Pts',(1.54536910828959,2.50915431971859,27.98431889361));
#91988=CARTESIAN_POINT('Ctrl Pts',(2.37606467899674,1.99753522029717,27.9312972589946));
#91989=CARTESIAN_POINT('Ctrl Pts',(2.92744934393793,1.03241011898417,27.8782756243793));
#91990=CARTESIAN_POINT('Ctrl Pts',(2.94631528200943,0.0569854368759391,
27.8252539897639));
#91991=CARTESIAN_POINT('Ctrl Pts',(2.96518122008093,-0.918439245232291,
27.7722323551485));
#91992=CARTESIAN_POINT('Ctrl Pts',(2.45152843128275,-1.90416350813576,27.7192107205331));
#91993=CARTESIAN_POINT('Ctrl Pts',(1.64123743918605,-2.44752134806466,27.6661890859177));
#91994=CARTESIAN_POINT('Ctrl Pts',(0.830946447089397,-2.99087918799354,
27.6131674513023));
#91995=CARTESIAN_POINT('Ctrl Pts',(-0.275982748305732,-3.09187060494792,
27.5601458166869));
#91996=CARTESIAN_POINT('Ctrl Pts',(-1.17122420414422,-2.7041181454672,27.5071241820716));
#91997=CARTESIAN_POINT('Ctrl Pts',(-2.06646565998275,-2.31636568598647,
27.4541025474562));
#91998=CARTESIAN_POINT('Ctrl Pts',(-2.75001937626462,-1.43986935007058,
27.4010809128408));
#91999=CARTESIAN_POINT('Ctrl Pts',(-2.90798263114761,-0.477135303621595,
27.3480592782254));
#92000=CARTESIAN_POINT('Ctrl Pts',(-2.93368653113318,-0.320478493397227,
27.3394315578468));
#92001=CARTESIAN_POINT('Ctrl Pts',(-2.94547382381967,-0.161538277289376,
27.3308038374682));
#92002=CARTESIAN_POINT('Ctrl Pts',(-2.94407188513322,-0.00239011867426281,
27.3221761170896));
#92003=CARTESIAN_POINT('Ctrl Pts',(-2.94363499374191,-0.002507597635829,
27.1778238829105));
#92004=CARTESIAN_POINT('Ctrl Pts',(-2.94521345152747,-0.176717484446133,
27.1872645020486));
#92005=CARTESIAN_POINT('Ctrl Pts',(-2.93108405332729,-0.350671665978835,
27.1967051211866));
#92006=CARTESIAN_POINT('Ctrl Pts',(-2.90033529857916,-0.521636790414356,
27.2061457403247));
#92007=CARTESIAN_POINT('Ctrl Pts',(-2.72760174393312,-1.48204685924987,
27.2591791628204));
#92008=CARTESIAN_POINT('Ctrl Pts',(-2.03040795965037,-2.34813067862668,
27.3122125853162));
#92009=CARTESIAN_POINT('Ctrl Pts',(-1.12905080070553,-2.72200185061,27.365246007812));
#92010=CARTESIAN_POINT('Ctrl Pts',(-0.227693641760674,-3.09587302259333,
27.4182794303077));
#92011=CARTESIAN_POINT('Ctrl Pts',(0.877826891846307,-2.97753154718315,
27.4713128528035));
#92012=CARTESIAN_POINT('Ctrl Pts',(1.6796251046219,-2.42134452179403,27.5243462752992));
#92013=CARTESIAN_POINT('Ctrl Pts',(2.48142331739747,-1.86515749640492,27.577379697795));
#92014=CARTESIAN_POINT('Ctrl Pts',(2.9794992093417,-0.871124921036897,27.6304131202907));
#92015=CARTESIAN_POINT('Ctrl Pts',(2.94503240751833,0.104086041162237,27.6834465427865));
#92016=CARTESIAN_POINT('Ctrl Pts',(2.91056560569497,1.07929700336143,27.7364799652823));
#92017=CARTESIAN_POINT('Ctrl Pts',(2.343556110104,2.03568635239166,27.789513387778));
#92018=CARTESIAN_POINT('Ctrl Pts',(1.50449298744779,2.53388054888515,27.8425468102738));
#92019=CARTESIAN_POINT('Ctrl Pts',(0.665429864791645,3.0320747453786,27.8955802327695));
#92020=CARTESIAN_POINT('Ctrl Pts',(-0.445686884929689,3.0720737893353,27.9486136552653));
#92021=CARTESIAN_POINT('Ctrl Pts',(-1.31840061613457,2.63550177398424,28.0016470777611));
#92022=CARTESIAN_POINT('Ctrl Pts',(-2.1911143473395,2.19892975863315,28.0546805002568));
#92023=CARTESIAN_POINT('Ctrl Pts',(-2.82542506002796,1.28578668397422,28.1077139227526));
#92024=CARTESIAN_POINT('Ctrl Pts',(-2.92992492623167,0.315578376864476,
28.1607473452483));
#92025=CARTESIAN_POINT('Ctrl Pts',(-2.94114109782648,0.211444053533942,
28.1664395244691));
#92026=CARTESIAN_POINT('Ctrl Pts',(-2.94625377339621,0.106652330639497,
28.1721317036898));
#92027=CARTESIAN_POINT('Ctrl Pts',(-2.94550455047329,0.00178675002179936,
28.1778238829105));
#92028=CARTESIAN_POINT('Origin',(0.,0.,0.));
#92029=CARTESIAN_POINT('',(-2.93776599353799,0.00138637979514328,29.3221761170896));
#92030=CARTESIAN_POINT('',(-2.9380367068104,0.00163420181435583,29.1778238829105));
#92031=CARTESIAN_POINT('',(-2.942,-3.60291088309151E-16,0.));
#92032=CARTESIAN_POINT('Ctrl Pts',(-2.93776599353799,0.00138637979514328,
29.3221761170896));
#92033=CARTESIAN_POINT('Ctrl Pts',(-2.93947922483499,0.405326537383405,
29.3003967861861));
#92034=CARTESIAN_POINT('Ctrl Pts',(-2.86194376351095,0.808637278136982,
29.2786174552827));
#92035=CARTESIAN_POINT('Ctrl Pts',(-2.7020086748925,1.17608256590425,29.2568381243793));
#92036=CARTESIAN_POINT('Ctrl Pts',(-2.31264777723671,2.07062564785274,29.2038164897639));
#92037=CARTESIAN_POINT('Ctrl Pts',(-1.43492427007663,2.7526028871322,29.1507948551485));
#92038=CARTESIAN_POINT('Ctrl Pts',(-0.471907863019101,2.90883551440073,
29.0977732205331));
#92039=CARTESIAN_POINT('Ctrl Pts',(0.491108544038425,3.06506814166927,29.0447515859177));
#92040=CARTESIAN_POINT('Ctrl Pts',(1.53941785099337,2.69555615692688,28.9917299513023));
#92041=CARTESIAN_POINT('Ctrl Pts',(2.1916136417186,1.96998749398345,28.9387083166869));
#92042=CARTESIAN_POINT('Ctrl Pts',(2.84380943244382,1.24441883104002,28.8856866820716));
#92043=CARTESIAN_POINT('Ctrl Pts',(3.09989170693931,0.162793489895487,28.8326650474562));
#92044=CARTESIAN_POINT('Ctrl Pts',(2.84226191945076,-0.778182666382572,
28.7796434128408));
#92045=CARTESIAN_POINT('Ctrl Pts',(2.58463213196221,-1.71915882266066,28.7266217782254));
#92046=CARTESIAN_POINT('Ctrl Pts',(1.81329028248965,-2.5194857940723,28.67360014361));
#92047=CARTESIAN_POINT('Ctrl Pts',(0.882453311491304,-2.81163604224591,
28.6205785089946));
#92048=CARTESIAN_POINT('Ctrl Pts',(-0.048383659506986,-3.10378629041951,
28.5675568743793));
#92049=CARTESIAN_POINT('Ctrl Pts',(-1.138715752031,-2.88775981535513,28.5145352397639));
#92050=CARTESIAN_POINT('Ctrl Pts',(-1.88783877356046,-2.26276066919592,
28.4615136051485));
#92051=CARTESIAN_POINT('Ctrl Pts',(-2.54405468004333,-1.71527464959593,
28.4150677757955));
#92052=CARTESIAN_POINT('Ctrl Pts',(-2.93844759085073,-0.853967987469306,
28.3686219464425));
#92053=CARTESIAN_POINT('Ctrl Pts',(-2.94510414404698,0.00199674015882861,
28.3221761170896));
#92054=CARTESIAN_POINT('Ctrl Pts',(-2.94550455047329,0.00178675002179936,
28.1778238829105));
#92055=CARTESIAN_POINT('Ctrl Pts',(-2.93927334388506,-0.870369022082387,
28.2251651261855));
#92056=CARTESIAN_POINT('Ctrl Pts',(-2.52757049983615,-1.74763358479836,
28.2725063694606));
#92057=CARTESIAN_POINT('Ctrl Pts',(-1.84938352851645,-2.29430389219696,
28.3198476127356));
#92058=CARTESIAN_POINT('Ctrl Pts',(-1.08965324487858,-2.90670431458808,
28.3728810352314));
#92059=CARTESIAN_POINT('Ctrl Pts',(0.00449634211611205,-3.10423161980979,
28.4259144577271));
#92060=CARTESIAN_POINT('Ctrl Pts',(0.930403448202452,-2.79614005530321,
28.4789478802229));
#92061=CARTESIAN_POINT('Ctrl Pts',(1.85631055428879,-2.48804849079663,28.5319813027187));
#92062=CARTESIAN_POINT('Ctrl Pts',(2.61397517946678,-1.67433805656175,28.5850147252144));
#92063=CARTESIAN_POINT('Ctrl Pts',(2.85531964140355,-0.72883436438824,28.6380481477102));
#92064=CARTESIAN_POINT('Ctrl Pts',(3.09666410334032,0.2166693277853,28.6910815702059));
#92065=CARTESIAN_POINT('Ctrl Pts',(2.82168840203584,1.29396627789748,28.7441149927017));
#92066=CARTESIAN_POINT('Ctrl Pts',(2.15671875311016,2.00813694883617,28.7971484151975));
#92067=CARTESIAN_POINT('Ctrl Pts',(1.4917491041845,2.72230761977483,28.8501818376932));
#92068=CARTESIAN_POINT('Ctrl Pts',(0.436785507637672,3.07335201154002,28.903215260189));
#92069=CARTESIAN_POINT('Ctrl Pts',(-0.523512635221601,2.89999729414725,
28.9562486826847));
#92070=CARTESIAN_POINT('Ctrl Pts',(-1.48381077808087,2.72664257675449,29.0092821051805));
#92071=CARTESIAN_POINT('Ctrl Pts',(-2.34944346725259,2.02888875020379,29.0623155276763));
#92072=CARTESIAN_POINT('Ctrl Pts',(-2.7227315579203,1.1272899577318,29.115348950172));
#92073=CARTESIAN_POINT('Ctrl Pts',(-2.86931301076673,0.773253319036106,
29.1361739277515));
#92074=CARTESIAN_POINT('Ctrl Pts',(-2.93997747852574,0.387784843198274,
29.156998905331));
#92075=CARTESIAN_POINT('Ctrl Pts',(-2.9380367068104,0.00163420181435583,
29.1778238829105));
#92076=CARTESIAN_POINT('Origin',(0.,0.,0.));
#92077=CARTESIAN_POINT('',(-2.94001376569275,-0.00252472911655227,30.3221761170896));
#92078=CARTESIAN_POINT('',(-2.9395119866127,-0.0023902824457737,30.1778238829105));
#92079=CARTESIAN_POINT('',(-2.942,-3.60291088309151E-16,0.));
#92080=CARTESIAN_POINT('Ctrl Pts',(-2.94001376569275,-0.00252472911655227,
30.3221761170896));
#92081=CARTESIAN_POINT('Ctrl Pts',(-2.93444893807589,0.682077234566173,
30.2851932605451));
#92082=CARTESIAN_POINT('Ctrl Pts',(-2.69624239041632,1.37017001338517,30.2482104040006));
#92083=CARTESIAN_POINT('Ctrl Pts',(-2.25936390251588,1.89190270284348,30.2112275474562));
#92084=CARTESIAN_POINT('Ctrl Pts',(-1.63301932772814,2.63990117056867,30.1582059128408));
#92085=CARTESIAN_POINT('Ctrl Pts',(-0.598316015418425,3.04595605037192,
30.1051842782254));
#92086=CARTESIAN_POINT('Ctrl Pts',(0.369587786719338,2.92359811686322,30.05216264361));
#92087=CARTESIAN_POINT('Ctrl Pts',(1.33749158885707,2.80124018335451,29.9991410089947));
#92088=CARTESIAN_POINT('Ctrl Pts',(2.23859588082286,2.15046943653388,29.9461193743793));
#92089=CARTESIAN_POINT('Ctrl Pts',(2.65909398850434,1.2701339462113,29.8930977397639));
#92090=CARTESIAN_POINT('Ctrl Pts',(3.07959209618584,0.389798455888696,29.8400761051485));
#92091=CARTESIAN_POINT('Ctrl Pts',(3.019484019583,-0.720101777935874,29.7870544705331));
#92092=CARTESIAN_POINT('Ctrl Pts',(2.50637269377013,-1.54987644699237,29.7340328359177));
#92093=CARTESIAN_POINT('Ctrl Pts',(1.99326136795729,-2.37965111604882,29.6810112013023));
#92094=CARTESIAN_POINT('Ctrl Pts',(1.02714679293448,-2.92930022033724,29.627989566687));
#92095=CARTESIAN_POINT('Ctrl Pts',(0.0516897776292723,-2.94641294592372,
29.5749679320716));
#92096=CARTESIAN_POINT('Ctrl Pts',(-0.923767237675969,-2.9635256715102,
29.5219462974562));
#92097=CARTESIAN_POINT('Ctrl Pts',(-1.90856669326362,-2.4481020183947,29.4689246628408));
#92098=CARTESIAN_POINT('Ctrl Pts',(-2.45046727698169,-1.63683572952821,
29.4159030282254));
#92099=CARTESIAN_POINT('Ctrl Pts',(-2.76977509804398,-1.15880769489887,
29.3846607245135));
#92100=CARTESIAN_POINT('Ctrl Pts',(-2.93530837476417,-0.578063059711174,
29.3534184208015));
#92101=CARTESIAN_POINT('Ctrl Pts',(-2.93776599353799,0.00138637979514328,
29.3221761170896));
#92102=CARTESIAN_POINT('Ctrl Pts',(-2.9380367068104,0.00163420181435583,
29.1778238829105));
#92103=CARTESIAN_POINT('Ctrl Pts',(-2.93503505945448,-0.595596292908616,
29.2100323278268));
#92104=CARTESIAN_POINT('Ctrl Pts',(-2.75835797892961,-1.19445856238458,
29.242240772743));
#92105=CARTESIAN_POINT('Ctrl Pts',(-2.42025762390727,-1.68119089315188,
29.2744492176593));
#92106=CARTESIAN_POINT('Ctrl Pts',(-1.86355210706285,-2.48262919317022,
29.3274826401551));
#92107=CARTESIAN_POINT('Ctrl Pts',(-0.869197581210329,-2.98006203481362,
29.3805160626508));
#92108=CARTESIAN_POINT('Ctrl Pts',(0.105990883665151,-2.9449644680162,29.4335494851466));
#92109=CARTESIAN_POINT('Ctrl Pts',(1.0811793485406,-2.90986690121879,29.4865829076423));
#92110=CARTESIAN_POINT('Ctrl Pts',(2.03720175243902,-2.34223892598059,29.5396163301381));
#92111=CARTESIAN_POINT('Ctrl Pts',(2.53485313376005,-1.50285374390355,29.5926497526339));
#92112=CARTESIAN_POINT('Ctrl Pts',(3.03250451508113,-0.663468561826437,
29.6456831751296));
#92113=CARTESIAN_POINT('Ctrl Pts',(3.07178487382474,0.447673827089566,29.6987165976254));
#92114=CARTESIAN_POINT('Ctrl Pts',(2.63464847342311,1.32010499839496,29.7517500201211));
#92115=CARTESIAN_POINT('Ctrl Pts',(2.1975120730215,2.19253616970031,29.8047834426169));
#92116=CARTESIAN_POINT('Ctrl Pts',(1.28395891347472,2.82625612339508,29.8578168651127));
#92117=CARTESIAN_POINT('Ctrl Pts',(0.313683218184318,2.93012843130256,29.9108502876084));
#92118=CARTESIAN_POINT('Ctrl Pts',(-0.656592477106082,3.03400073921004,
29.9638837101042));
#92119=CARTESIAN_POINT('Ctrl Pts',(-1.6835907081401,2.60802540133023,30.0169171325999));
#92120=CARTESIAN_POINT('Ctrl Pts',(-2.29549960441592,1.84789917241835,30.0699505550957));
#92121=CARTESIAN_POINT('Ctrl Pts',(-2.71038670676496,1.33251760099142,30.1059083310339));
#92122=CARTESIAN_POINT('Ctrl Pts',(-2.93445204415044,0.663522680698212,
30.1418661069722));
#92123=CARTESIAN_POINT('Ctrl Pts',(-2.9395119866127,-0.0023902824457737,
30.1778238829105));
#92124=CARTESIAN_POINT('Origin',(0.,0.,0.));
#92125=CARTESIAN_POINT('',(-2.94683142262726,-0.000288828235917582,31.3221761170896));
#92126=CARTESIAN_POINT('',(-2.94668913024009,-0.0006657472057589,31.1778238829105));
#92127=CARTESIAN_POINT('',(-2.942,-3.60291088309151E-16,0.));
#92128=CARTESIAN_POINT('Ctrl Pts',(-2.94683142262726,-0.000288828235917582,
31.3221761170896));
#92129=CARTESIAN_POINT('Ctrl Pts',(-2.94549260199717,0.959980156645984,
31.2699897349041));
#92130=CARTESIAN_POINT('Ctrl Pts',(-2.43187245641912,1.92147731567173,31.2178033527186));
#92131=CARTESIAN_POINT('Ctrl Pts',(-1.63242873210736,2.45340528971644,31.1656169705331));
#92132=CARTESIAN_POINT('Ctrl Pts',(-0.820189767249493,2.99384686662539,
31.1125953359177));
#92133=CARTESIAN_POINT('Ctrl Pts',(0.287095310098538,3.09085855354509,31.0595737013023));
#92134=CARTESIAN_POINT('Ctrl Pts',(1.18093712835462,2.69989047553633,31.0065520666869));
#92135=CARTESIAN_POINT('Ctrl Pts',(2.07477894661068,2.30892239752758,30.9535304320716));
#92136=CARTESIAN_POINT('Ctrl Pts',(2.75517750577479,1.42997455459038,30.9005087974562));
#92137=CARTESIAN_POINT('Ctrl Pts',(2.9096790007227,0.466678897928309,30.8474871628408));
#92138=CARTESIAN_POINT('Ctrl Pts',(3.06418049567062,-0.496616758733819,
30.7944655282254));
#92139=CARTESIAN_POINT('Ctrl Pts',(2.69278492640225,-1.54426022912084,30.74144389361));
#92140=CARTESIAN_POINT('Ctrl Pts',(1.96604520967682,-2.19515086372784,30.6884222589947));
#92141=CARTESIAN_POINT('Ctrl Pts',(1.23930549295141,-2.84604149833482,30.6354006243793));
#92142=CARTESIAN_POINT('Ctrl Pts',(0.157221628768963,-3.10017929716181,
30.5823789897638));
#92143=CARTESIAN_POINT('Ctrl Pts',(-0.783289956059199,-2.84085865993981,
30.5293573551485));
#92144=CARTESIAN_POINT('Ctrl Pts',(-1.72380154088736,-2.58153802271781,
30.4763357205331));
#92145=CARTESIAN_POINT('Ctrl Pts',(-2.52274084636124,-1.80875894944683,
30.4233140859177));
#92146=CARTESIAN_POINT('Ctrl Pts',(-2.8132175804653,-0.877398384987801,
30.3702924513024));
#92147=CARTESIAN_POINT('Ctrl Pts',(-2.9010853330696,-0.595666493737709,
30.3542536732314));
#92148=CARTESIAN_POINT('Ctrl Pts',(-2.94242712808519,-0.299423886952565,
30.3382148951605));
#92149=CARTESIAN_POINT('Ctrl Pts',(-2.94001376569275,-0.00252472911655227,
30.3221761170896));
#92150=CARTESIAN_POINT('Ctrl Pts',(-2.9395119866127,-0.0023902824457737,
30.1778238829105));
#92151=CARTESIAN_POINT('Ctrl Pts',(-2.94191485461085,-0.318619362248227,
30.194899529468));
#92152=CARTESIAN_POINT('Ctrl Pts',(-2.89492949018049,-0.634153425308857,
30.2119751760255));
#92153=CARTESIAN_POINT('Ctrl Pts',(-2.79553767998929,-0.932211813408388,
30.229050822583));
#92154=CARTESIAN_POINT('Ctrl Pts',(-2.4868472977692,-1.85791945037922,30.2820842450787));
#92155=CARTESIAN_POINT('Ctrl Pts',(-1.67264697181141,-2.61505760437691,
30.3351176675745));
#92156=CARTESIAN_POINT('Ctrl Pts',(-0.726987374400473,-2.85579045848262,
30.3881510900703));
#92157=CARTESIAN_POINT('Ctrl Pts',(0.218672223010494,-3.09652331258834,
30.441184512566));
#92158=CARTESIAN_POINT('Ctrl Pts',(1.29579109187459,-2.82085086680205,30.4942179350618));
#92159=CARTESIAN_POINT('Ctrl Pts',(2.00953150714542,-2.15541942718533,30.5472513575575));
#92160=CARTESIAN_POINT('Ctrl Pts',(2.72327192241621,-1.48998798756864,30.6002847800533));
#92161=CARTESIAN_POINT('Ctrl Pts',(3.07363388409376,-0.434797554121506,
30.653318202549));
#92162=CARTESIAN_POINT('Ctrl Pts',(2.8996580764786,0.525388261013206,30.7063516250448));
#92163=CARTESIAN_POINT('Ctrl Pts',(2.72568226886344,1.48557407614795,30.7593850475406));
#92164=CARTESIAN_POINT('Ctrl Pts',(2.02736869195559,2.35075527297029,30.8124184700363));
#92165=CARTESIAN_POINT('Ctrl Pts',(1.12552864314742,2.72346012615438,30.8654518925321));
#92166=CARTESIAN_POINT('Ctrl Pts',(0.223688594339212,3.09616497933847,30.9184853150278));
#92167=CARTESIAN_POINT('Ctrl Pts',(-0.881677926369304,2.97639348888425,
30.9715187375236));
#92168=CARTESIAN_POINT('Ctrl Pts',(-1.68275597834239,2.41916971348664,31.0245521600194));
#92169=CARTESIAN_POINT('Ctrl Pts',(-2.45448700768209,1.88235950291979,31.0756427343164));
#92170=CARTESIAN_POINT('Ctrl Pts',(-2.94381604647467,0.939561525051785,
31.1267333086134));
#92171=CARTESIAN_POINT('Ctrl Pts',(-2.94668913024009,-0.0006657472057589,
31.1778238829105));
#92172=CARTESIAN_POINT('Origin',(0.,0.,0.));
#92173=CARTESIAN_POINT('',(-2.94088266626002,0.00267082732003945,32.3221761170896));
#92174=CARTESIAN_POINT('',(-2.94152987837198,0.00271722750875524,32.1778238829105));
#92175=CARTESIAN_POINT('',(-2.942,-3.60291088309151E-16,0.));
#92176=CARTESIAN_POINT('Ctrl Pts',(-2.94088266626002,0.00267082732003945,
32.3221761170896));
#92177=CARTESIAN_POINT('Ctrl Pts',(-2.943221129712,0.268447683304989,32.3078078438784));
#92178=CARTESIAN_POINT('Ctrl Pts',(-2.91017720576495,0.533653254375284,
32.2934395706673));
#92179=CARTESIAN_POINT('Ctrl Pts',(-2.83944622309545,0.78839471533439,32.2790712974562));
#92180=CARTESIAN_POINT('Ctrl Pts',(-2.57843557386977,1.72843869041002,32.2260496628408));
#92181=CARTESIAN_POINT('Ctrl Pts',(-1.80422177324665,2.52598774898972,32.1730280282254));
#92182=CARTESIAN_POINT('Ctrl Pts',(-0.872340624067349,2.81479003064528,
32.12000639361));
#92183=CARTESIAN_POINT('Ctrl Pts',(0.0595405251119813,3.10359231230084,
32.0669847589946));
#92184=CARTESIAN_POINT('Ctrl Pts',(1.14908902284753,2.88364781703224,32.0139631243793));
#92185=CARTESIAN_POINT('Ctrl Pts',(1.89596052037525,2.25595983700877,31.9609414897639));
#92186=CARTESIAN_POINT('Ctrl Pts',(2.64283201790295,1.62827185698532,31.9079198551485));
#92187=CARTESIAN_POINT('Ctrl Pts',(3.04702651522286,0.592840392207089,31.8548982205331));
#92188=CARTESIAN_POINT('Ctrl Pts',(2.9229291150121,-0.374841926194006,31.8018765859177));
#92189=CARTESIAN_POINT('Ctrl Pts',(2.79883171480133,-1.3425242445951,31.7488549513023));
#92190=CARTESIAN_POINT('Ctrl Pts',(2.14644241705985,-2.24245741661903,31.695833316687));
#92191=CARTESIAN_POINT('Ctrl Pts',(1.26535256535564,-2.66137257188206,31.6428116820716));
#92192=CARTESIAN_POINT('Ctrl Pts',(0.384262713651435,-3.08028772714509,
31.5897900474562));
#92193=CARTESIAN_POINT('Ctrl Pts',(-0.725527692015529,-3.01818486564724,
31.5367684128408));
#92194=CARTESIAN_POINT('Ctrl Pts',(-1.55437877885202,-2.50358297103825,
31.4837467782254));
#92195=CARTESIAN_POINT('Ctrl Pts',(-2.38322986568854,-1.98898107642925,
31.43072514361));
#92196=CARTESIAN_POINT('Ctrl Pts',(-2.93114163369459,-1.02188014870908,
31.3777035089946));
#92197=CARTESIAN_POINT('Ctrl Pts',(-2.94650109151376,-0.0463939513998811,
31.3246818743793));
#92198=CARTESIAN_POINT('Ctrl Pts',(-2.94674304981169,-0.0310270691349388,
31.3238466219494));
#92199=CARTESIAN_POINT('Ctrl Pts',(-2.94685285069216,-0.0156581059935221,
31.3230113695195));
#92200=CARTESIAN_POINT('Ctrl Pts',(-2.94683142262726,-0.000288828235917582,
31.3221761170896));
#92201=CARTESIAN_POINT('Ctrl Pts',(-2.94668913024009,-0.0006657472057589,
31.1778238829105));
#92202=CARTESIAN_POINT('Ctrl Pts',(-2.94679838651085,-0.0364202652831939,
31.1797667311092));
#92203=CARTESIAN_POINT('Ctrl Pts',(-2.94620418231902,-0.0721710658817098,
31.1817095793079));
#92204=CARTESIAN_POINT('Ctrl Pts',(-2.94489529646495,-0.107895681825943,
31.1836524275066));
#92205=CARTESIAN_POINT('Ctrl Pts',(-2.90916697937683,-1.08306124139995,
31.2366858500024));
#92206=CARTESIAN_POINT('Ctrl Pts',(-2.34092076196299,-2.03871630020705,
31.2897192724982));
#92207=CARTESIAN_POINT('Ctrl Pts',(-1.50121387162844,-2.53582465815924,
31.3427526949939));
#92208=CARTESIAN_POINT('Ctrl Pts',(-0.661506981293825,-3.03293301611147,
31.3957861174897));
#92209=CARTESIAN_POINT('Ctrl Pts',(0.449660581961557,-3.07149467320871,
31.4488195399855));
#92210=CARTESIAN_POINT('Ctrl Pts',(1.32180882837894,-2.63379407063604,31.5018529624812));
#92211=CARTESIAN_POINT('Ctrl Pts',(2.19395707479628,-2.1960934680634,31.5548863849769));
#92212=CARTESIAN_POINT('Ctrl Pts',(2.82708600437565,-1.2821306058209,31.6079198074727));
#92213=CARTESIAN_POINT('Ctrl Pts',(2.9303307105311,-0.31178792827231,31.6609532299685));
#92214=CARTESIAN_POINT('Ctrl Pts',(3.03357541668656,0.658554749276281,31.7139866524642));
#92215=CARTESIAN_POINT('Ctrl Pts',(2.60693589941809,1.68527724213097,31.76702007496));
#92216=CARTESIAN_POINT('Ctrl Pts',(1.84641404323699,2.29669435629457,31.8200534974558));
#92217=CARTESIAN_POINT('Ctrl Pts',(1.08589218705586,2.90811147045818,31.8730869199515));
#92218=CARTESIAN_POINT('Ctrl Pts',(-0.00851200803791696,3.10422320593068,
31.9261203424473));
#92219=CARTESIAN_POINT('Ctrl Pts',(-0.934019788616158,2.79493413514013,
31.979153764943));
#92220=CARTESIAN_POINT('Ctrl Pts',(-1.85952756919437,2.48564506434958,32.0321871874388));
#92221=CARTESIAN_POINT('Ctrl Pts',(-2.61613893525706,1.67095518729601,32.0852206099346));
#92222=CARTESIAN_POINT('Ctrl Pts',(-2.85626008081923,0.725140080271805,
32.1382540324303));
#92223=CARTESIAN_POINT('Ctrl Pts',(-2.91598064557429,0.489906268550998,
32.1514439825904));
#92224=CARTESIAN_POINT('Ctrl Pts',(-2.94375281118411,0.246561478114943,
32.1646339327504));
#92225=CARTESIAN_POINT('Ctrl Pts',(-2.94152987837198,0.00271722750875524,
32.1778238829105));
#92226=CARTESIAN_POINT('Origin',(0.,0.,0.));
#92227=CARTESIAN_POINT('',(-2.93740160319918,-0.000921743247123685,33.3221761170896));
#92228=CARTESIAN_POINT('',(-2.93722324760469,-0.000551307423291771,33.1778238829105));
#92229=CARTESIAN_POINT('',(-2.942,-3.60291088309151E-16,0.));
#92230=CARTESIAN_POINT('Ctrl Pts',(-2.93740160319918,-0.000921743247123685,
33.3221761170896));
#92231=CARTESIAN_POINT('Ctrl Pts',(-2.93586593204594,0.54771487550154,33.2926043182374));
#92232=CARTESIAN_POINT('Ctrl Pts',(-2.78862489741151,1.09711691069357,33.2630325193853));
#92233=CARTESIAN_POINT('Ctrl Pts',(-2.50078516053484,1.55887608932429,33.2334607205331));
#92234=CARTESIAN_POINT('Ctrl Pts',(-1.98469435954012,2.386800916355,33.1804390859177));
#92235=CARTESIAN_POINT('Ctrl Pts',(-1.01661020332163,2.93297357806132,33.1274174513023));
#92236=CARTESIAN_POINT('Ctrl Pts',(-0.0410979752959005,2.94657971849479,
33.074395816687));
#92237=CARTESIAN_POINT('Ctrl Pts',(0.934414252729828,2.96018585892825,33.0213741820716));
#92238=CARTESIAN_POINT('Ctrl Pts',(1.91735455256277,2.44122547808888,32.9683525474562));
#92239=CARTESIAN_POINT('Ctrl Pts',(2.45633537677761,1.62801646116033,32.9153309128408));
#92240=CARTESIAN_POINT('Ctrl Pts',(2.99531620099246,0.814807444231778,32.8623092782254));
#92241=CARTESIAN_POINT('Ctrl Pts',(3.0903375495892,-0.292650208786009,32.80928764361));
#92242=CARTESIAN_POINT('Ctrl Pts',(2.6977635542415,-1.18578787581275,32.7562660089946));
#92243=CARTESIAN_POINT('Ctrl Pts',(2.30518955889379,-2.07892554283951,32.7032443743793));
#92244=CARTESIAN_POINT('Ctrl Pts',(1.42502021960166,-2.75774322387527,32.6502227397639));
#92245=CARTESIAN_POINT('Ctrl Pts',(0.461448425241032,-2.91051308738868,
32.5972011051485));
#92246=CARTESIAN_POINT('Ctrl Pts',(-0.502123369119543,-3.06328295090209,
32.5441794705331));
#92247=CARTESIAN_POINT('Ctrl Pts',(-1.54909761854858,-2.69000499689322,
32.4911578359177));
#92248=CARTESIAN_POINT('Ctrl Pts',(-2.19868099434898,-1.96209657410302,
32.4381362013023));
#92249=CARTESIAN_POINT('Ctrl Pts',(-2.67223450074586,-1.43144323722631,
32.3994828398981));
#92250=CARTESIAN_POINT('Ctrl Pts',(-2.93459175909169,-0.712318978087848,
32.3608294784938));
#92251=CARTESIAN_POINT('Ctrl Pts',(-2.94088266626002,0.00267082732003945,
32.3221761170896));
#92252=CARTESIAN_POINT('Ctrl Pts',(-2.94152987837198,0.00271722750875524,
32.1778238829105));
#92253=CARTESIAN_POINT('Ctrl Pts',(-2.93481496581132,-0.733874005615878,
32.2176673552462));
#92254=CARTESIAN_POINT('Ctrl Pts',(-2.65439781930278,-1.47502276218687,
32.2575108275819));
#92255=CARTESIAN_POINT('Ctrl Pts',(-2.15411919952377,-2.01092522475132,
32.2973542999176));
#92256=CARTESIAN_POINT('Ctrl Pts',(-1.48822624760452,-2.72423508575532,
32.3503877224134));
#92257=CARTESIAN_POINT('Ctrl Pts',(-0.432809418704383,-3.07391447076852,
32.4034211449091));
#92258=CARTESIAN_POINT('Ctrl Pts',(0.527263667004487,-2.89931764571512,
32.4564545674049));
#92259=CARTESIAN_POINT('Ctrl Pts',(1.48733675271336,-2.72472082066171,32.5094879899006));
#92260=CARTESIAN_POINT('Ctrl Pts',(2.35206609523099,-2.0258477855417,32.5625214123964));
#92261=CARTESIAN_POINT('Ctrl Pts',(2.72418755500742,-1.12376685768925,32.6155548348921));
#92262=CARTESIAN_POINT('Ctrl Pts',(3.09630901478386,-0.221685929836773,
32.6685882573879));
#92263=CARTESIAN_POINT('Ctrl Pts',(2.97582259181911,0.883602890748098,32.7216216798837));
#92264=CARTESIAN_POINT('Ctrl Pts',(2.41808079098732,1.68432035953859,32.7746551023794));
#92265=CARTESIAN_POINT('Ctrl Pts',(1.86033899015554,2.48503782832908,32.8276885248752));
#92266=CARTESIAN_POINT('Ctrl Pts',(0.865341811456686,2.98118394532513,32.880721947371));
#92267=CARTESIAN_POINT('Ctrl Pts',(-0.109800434847724,2.94482489289352,
32.9337553698667));
#92268=CARTESIAN_POINT('Ctrl Pts',(-1.08494268115213,2.90846584046192,32.9867887923625));
#92269=CARTESIAN_POINT('Ctrl Pts',(-2.04022999506213,2.33960161860266,33.0398222148582));
#92270=CARTESIAN_POINT('Ctrl Pts',(-2.53679512167625,1.49957337130853,33.092855637354));
#92271=CARTESIAN_POINT('Ctrl Pts',(-2.80198806119353,1.05095233805867,33.1211783858728));
#92272=CARTESIAN_POINT('Ctrl Pts',(-2.93634681713537,0.524991413987441,
33.1495011343917));
#92273=CARTESIAN_POINT('Ctrl Pts',(-2.93722324760469,-0.000551307423291771,
33.1778238829105));
#92274=CARTESIAN_POINT('Origin',(0.,0.,0.));
#92275=CARTESIAN_POINT('',(-2.94427325151691,-0.00232800721794407,34.3221761170896));
#92276=CARTESIAN_POINT('',(-2.94355950823906,-0.00252461584680807,34.1778238829105));
#92277=CARTESIAN_POINT('',(-2.942,-3.60291088309151E-16,0.));
#92278=CARTESIAN_POINT('Ctrl Pts',(-2.94427325151691,-0.00232800721794407,
34.3221761170896));
#92279=CARTESIAN_POINT('Ctrl Pts',(-2.93711978754248,0.823457452646246,
34.2774007925964));
#92280=CARTESIAN_POINT('Ctrl Pts',(-2.57382536708779,1.65475429244643,34.2326254681032));
#92281=CARTESIAN_POINT('Ctrl Pts',(-1.95814160001811,2.20220402217795,34.18785014361));
#92282=CARTESIAN_POINT('Ctrl Pts',(-1.22906682265575,2.85047804070656,34.1348285089946));
#92283=CARTESIAN_POINT('Ctrl Pts',(-0.146076400813901,3.10072443152059,
34.0818068743793));
#92284=CARTESIAN_POINT('Ctrl Pts',(0.79349692771717,2.83802461348059,34.0287852397639));
#92285=CARTESIAN_POINT('Ctrl Pts',(1.73307025624827,2.57532479544058,33.9757636051485));
#92286=CARTESIAN_POINT('Ctrl Pts',(2.52922649146857,1.79967876854651,33.9227419705331));
#92287=CARTESIAN_POINT('Ctrl Pts',(2.81635338770602,0.867280045069095,33.8697203359177));
#92288=CARTESIAN_POINT('Ctrl Pts',(3.10348028394345,-0.0651186784082651,
33.8166987013023));
#92289=CARTESIAN_POINT('Ctrl Pts',(2.88157784119809,-1.15427009846895,33.7636770666869));
#92290=CARTESIAN_POINT('Ctrl Pts',(2.25254848367163,-1.90001221304677,33.7106554320716));
#92291=CARTESIAN_POINT('Ctrl Pts',(1.62351912614512,-2.64575432762465,33.6576337974562));
#92292=CARTESIAN_POINT('Ctrl Pts',(0.587362853837422,-3.04808713671961,
33.6046121628408));
#92293=CARTESIAN_POINT('Ctrl Pts',(-0.380094854749983,-2.92225067070072,
33.5515905282254));
#92294=CARTESIAN_POINT('Ctrl Pts',(-1.34755256333731,-2.79641420468185,
33.49856889361));
#92295=CARTESIAN_POINT('Ctrl Pts',(-2.24631170820435,-2.14240846354924,
33.4455472589947));
#92296=CARTESIAN_POINT('Ctrl Pts',(-2.66364255775242,-1.2605670968054,33.3925256243793));
#92297=CARTESIAN_POINT('Ctrl Pts',(-2.84821513745164,-0.870555823683219,
33.369075788616));
#92298=CARTESIAN_POINT('Ctrl Pts',(-2.93861935922781,-0.435979436817632,
33.3456259528528));
#92299=CARTESIAN_POINT('Ctrl Pts',(-2.93740160319918,-0.000921743247123685,
33.3221761170896));
#92300=CARTESIAN_POINT('Ctrl Pts',(-2.93722324760469,-0.000551307423291771,
33.1778238829105));
#92301=CARTESIAN_POINT('Ctrl Pts',(-2.93798790459327,-0.459070184611203,
33.2025345568874));
#92302=CARTESIAN_POINT('Ctrl Pts',(-2.83714590676715,-0.917270726220104,
33.2272452308643));
#92303=CARTESIAN_POINT('Ctrl Pts',(-2.63293856598045,-1.32351210537377,
33.2519559048413));
#92304=CARTESIAN_POINT('Ctrl Pts',(-2.19467394435226,-2.195377062033,33.304989327337));
#92305=CARTESIAN_POINT('Ctrl Pts',(-1.28030176177763,-2.82791470262249,
33.3580227498328));
#92306=CARTESIAN_POINT('Ctrl Pts',(-0.309892507921363,-2.93053176383268,
33.4110561723285));
#92307=CARTESIAN_POINT('Ctrl Pts',(0.660516745934904,-3.03314882504287,
33.4640895948243));
#92308=CARTESIAN_POINT('Ctrl Pts',(1.68696307107281,-2.60584530687375,33.5171230173201));
#92309=CARTESIAN_POINT('Ctrl Pts',(2.29788814733301,-1.84492814159374,33.5701564398158));
#92310=CARTESIAN_POINT('Ctrl Pts',(2.90881322359324,-1.08401097631369,33.6231898623116));
#92311=CARTESIAN_POINT('Ctrl Pts',(3.10421705097572,0.0105198360772893,
33.6762232848074));
#92312=CARTESIAN_POINT('Ctrl Pts',(2.7943294210082,0.935827373069456,33.7292567073031));
#92313=CARTESIAN_POINT('Ctrl Pts',(2.48444179104069,1.86113491006157,33.7822901297989));
#92314=CARTESIAN_POINT('Ctrl Pts',(1.66926270372325,2.6172191716549,33.8353235522946));
#92315=CARTESIAN_POINT('Ctrl Pts',(0.723292482774982,2.85672850821692,33.8883569747904));
#92316=CARTESIAN_POINT('Ctrl Pts',(-0.222677738173258,3.09623784477894,
33.9413903972861));
#92317=CARTESIAN_POINT('Ctrl Pts',(-1.29943909275232,2.81917225630971,33.9944238197819));
#92318=CARTESIAN_POINT('Ctrl Pts',(-2.01231810107072,2.15281807066951,34.0474572422777));
#92319=CARTESIAN_POINT('Ctrl Pts',(-2.59645062931776,1.60680794745917,34.0909127891553));
#92320=CARTESIAN_POINT('Ctrl Pts',(-2.93626704149822,0.799423566697762,
34.1343683360329));
#92321=CARTESIAN_POINT('Ctrl Pts',(-2.94355950823906,-0.00252461584680807,
34.1778238829105));
#92322=CARTESIAN_POINT('Origin',(0.,0.,0.));
#92323=CARTESIAN_POINT('',(-2.94492293178134,0.00208059058526368,35.3221761170896));
#92324=CARTESIAN_POINT('',(-2.94556291087109,0.0017517216428375,35.1778238829105));
#92325=CARTESIAN_POINT('',(-2.942,-3.60291088309151E-16,0.));
#92326=CARTESIAN_POINT('Ctrl Pts',(-2.94492293178134,0.00208059058526368,
35.3221761170896));
#92327=CARTESIAN_POINT('Ctrl Pts',(-2.94595073758724,0.130317914585527,
35.3152189015707));
#92328=CARTESIAN_POINT('Ctrl Pts',(-2.9383025122363,0.258431807689072,35.3082616860519));
#92329=CARTESIAN_POINT('Ctrl Pts',(-2.92156278612083,0.385346555417464,
35.3013044705331));
#92330=CARTESIAN_POINT('Ctrl Pts',(-2.79398766080593,1.35257652883955,35.2482828359177));
#92331=CARTESIAN_POINT('Ctrl Pts',(-2.13836758903384,2.25015874312748,35.1952612013023));
#92332=CARTESIAN_POINT('Ctrl Pts',(-1.25577755602009,2.6659039387822,35.142239566687));
#92333=CARTESIAN_POINT('Ctrl Pts',(-0.373187523006309,3.08164913443693,
35.0892179320716));
#92334=CARTESIAN_POINT('Ctrl Pts',(0.73637247124921,3.01555731145834,35.0361962974562));
#92335=CARTESIAN_POINT('Ctrl Pts',(1.56336836388063,2.49797927129819,34.9831746628408));
#92336=CARTESIAN_POINT('Ctrl Pts',(2.39036425651199,1.98040123113808,34.9301530282254));
#92337=CARTESIAN_POINT('Ctrl Pts',(2.93479604751941,1.01133697379647,34.87713139361));
#92338=CARTESIAN_POINT('Ctrl Pts',(2.94664882661281,0.0358018664257049,
34.8241097589947));
#92339=CARTESIAN_POINT('Ctrl Pts',(2.95850160570621,-0.939733240945092,
34.7710881243793));
#92340=CARTESIAN_POINT('Ctrl Pts',(2.43777537288558,-1.92173919834509,34.7180664897639));
#92341=CARTESIAN_POINT('Ctrl Pts',(1.62359893094074,-2.45925752869974,34.6650448551485));
#92342=CARTESIAN_POINT('Ctrl Pts',(0.809422488995877,-2.9967758590544,34.6120232205331));
#92343=CARTESIAN_POINT('Ctrl Pts',(-0.298204162073124,-3.08980656236369,
34.5590015859177));
#92344=CARTESIAN_POINT('Ctrl Pts',(-1.19063479260833,-2.69562791787901,
34.5059799513024));
#92345=CARTESIAN_POINT('Ctrl Pts',(-2.08306542314352,-2.30144927339435,
34.452958316687));
#92346=CARTESIAN_POINT('Ctrl Pts',(-2.76030003314485,-1.42006128111569,
34.3999366820716));
#92347=CARTESIAN_POINT('Ctrl Pts',(-2.91133777170409,-0.456216461854777,
34.3469150474562));
#92348=CARTESIAN_POINT('Ctrl Pts',(-2.93482825896181,-0.306312307692763,
34.338668737334));
#92349=CARTESIAN_POINT('Ctrl Pts',(-2.9455907111456,-0.154413627445788,
34.3304224272118));
#92350=CARTESIAN_POINT('Ctrl Pts',(-2.94427325151691,-0.00232800721794407,
34.3221761170896));
#92351=CARTESIAN_POINT('Ctrl Pts',(-2.94355950823906,-0.00252461584680807,
34.1778238829105));
#92352=CARTESIAN_POINT('Ctrl Pts',(-2.94516681373656,-0.179279034937491,
34.1874017585286));
#92353=CARTESIAN_POINT('Ctrl Pts',(-2.93062046171695,-0.355769369334824,
34.1969796341468));
#92354=CARTESIAN_POINT('Ctrl Pts',(-2.89897600199921,-0.529138852410934,
34.2065575097649));
#92355=CARTESIAN_POINT('Ctrl Pts',(-2.72375823255149,-1.4890988070398,34.2595909322607));
#92356=CARTESIAN_POINT('Ctrl Pts',(-2.02432603159842,-2.35337593348627,
34.3126243547565));
#92357=CARTESIAN_POINT('Ctrl Pts',(-1.12200460209435,-2.72491384417511,
34.3656577772522));
#92358=CARTESIAN_POINT('Ctrl Pts',(-0.219683172590273,-3.09645175486395,
34.418691199748));
#92359=CARTESIAN_POINT('Ctrl Pts',(0.885527485464739,-2.97525044979509,
34.4717246222437));
#92360=CARTESIAN_POINT('Ctrl Pts',(1.68588403608615,-2.41699085686478,34.5247580447395));
#92361=CARTESIAN_POINT('Ctrl Pts',(2.48624058670757,-1.85873126393446,34.5777914672353));
#92362=CARTESIAN_POINT('Ctrl Pts',(2.98174302989538,-0.863413383142613,
34.630824889731));
#92363=CARTESIAN_POINT('Ctrl Pts',(2.94475325733136,0.111705141933711,34.6838583122268));
#92364=CARTESIAN_POINT('Ctrl Pts',(2.90776348476734,1.08682366701001,34.7368917347225));
#92365=CARTESIAN_POINT('Ctrl Pts',(2.33828149645164,2.04174283637074,34.7899251572183));
#92366=CARTESIAN_POINT('Ctrl Pts',(1.49793224363048,2.53776452390489,34.8429585797141));
#92367=CARTESIAN_POINT('Ctrl Pts',(0.657582990809354,3.03378621143902,34.8959920022098));
#92368=CARTESIAN_POINT('Ctrl Pts',(-0.453633526517266,3.07091041714649,
34.9490254247056));
#92369=CARTESIAN_POINT('Ctrl Pts',(-1.3252148286668,2.63208195981427,35.0020588472013));
#92370=CARTESIAN_POINT('Ctrl Pts',(-2.1967961308164,2.193253502482,35.0550922696971));
#92371=CARTESIAN_POINT('Ctrl Pts',(-2.82874221778894,1.27847238211,35.1081256921929));
#92372=CARTESIAN_POINT('Ctrl Pts',(-2.93073159112318,0.307996957924358,
35.1611591146886));
#92373=CARTESIAN_POINT('Ctrl Pts',(-2.94141434668702,0.20634566428115,35.1667140374292));
#92374=CARTESIAN_POINT('Ctrl Pts',(-2.94628280629519,0.104083333628536,
35.1722689601699));
#92375=CARTESIAN_POINT('Ctrl Pts',(-2.94556291087109,0.0017517216428375,
35.1778238829105));
#92376=CARTESIAN_POINT('Origin',(0.,0.,0.));
#92377=CARTESIAN_POINT('',(-2.93766977734024,0.00128397461115384,36.3221761170896));
#92378=CARTESIAN_POINT('',(-2.9380797671204,0.00166795251978762,36.1778238829105));
#92379=CARTESIAN_POINT('',(-2.942,-3.60291088309151E-16,0.));
#92380=CARTESIAN_POINT('Ctrl Pts',(-2.93766977734024,0.00128397461115384,
36.3221761170896));
#92381=CARTESIAN_POINT('Ctrl Pts',(-2.93928119520059,0.412331772833426,
36.3000153759297));
#92382=CARTESIAN_POINT('Ctrl Pts',(-2.85890327362297,0.822777322858098,
36.2778546347699));
#92383=CARTESIAN_POINT('Ctrl Pts',(-2.69348357334797,1.19547786308358,36.25569389361));
#92384=CARTESIAN_POINT('Ctrl Pts',(-2.29770155311203,2.08719857414911,36.2026722589947));
#92385=CARTESIAN_POINT('Ctrl Pts',(-1.41509775515192,2.76284792532406,36.1496506243793));
#92386=CARTESIAN_POINT('Ctrl Pts',(-0.450983024670797,2.91215305100488,
36.0966289897639));
#92387=CARTESIAN_POINT('Ctrl Pts',(0.513131705810276,3.06145817668569,36.0436073551485));
#92388=CARTESIAN_POINT('Ctrl Pts',(1.55875736881236,2.68441907687241,35.9905857205331));
#92389=CARTESIAN_POINT('Ctrl Pts',(2.20571993583375,1.95418030019847,35.9375640859177));
#92390=CARTESIAN_POINT('Ctrl Pts',(2.85268250285517,1.22394152352449,35.8845424513023));
#92391=CARTESIAN_POINT('Ctrl Pts',(3.10098197389584,0.140503069989798,35.831520816687));
#92392=CARTESIAN_POINT('Ctrl Pts',(2.83659383568765,-0.79859657672511,35.7784991820716));
#92393=CARTESIAN_POINT('Ctrl Pts',(2.57220569747947,-1.73769622343999,35.7254775474562));
#92394=CARTESIAN_POINT('Ctrl Pts',(1.79512995002246,-2.5324570633351,35.6724559128408));
#92395=CARTESIAN_POINT('Ctrl Pts',(0.862216664341213,-2.81790764659713,
35.6194342782254));
#92396=CARTESIAN_POINT('Ctrl Pts',(-0.0706966213400306,-3.10335822985915,
35.56641264361));
#92397=CARTESIAN_POINT('Ctrl Pts',(-1.15944744524551,-2.87949855648811,
35.5133910089947));
#92398=CARTESIAN_POINT('Ctrl Pts',(-1.90405776776943,-2.2491298535245,35.4603693743793));
#92399=CARTESIAN_POINT('Ctrl Pts',(-2.55096430335971,-1.70147476274293,
35.4143049552827));
#92400=CARTESIAN_POINT('Ctrl Pts',(-2.93811772684485,-0.846991544752816,
35.3682405361861));
#92401=CARTESIAN_POINT('Ctrl Pts',(-2.94492293178134,0.00208059058526368,
35.3221761170896));
#92402=CARTESIAN_POINT('Ctrl Pts',(-2.94556291087109,0.0017517216428375,
35.1778238829105));
#92403=CARTESIAN_POINT('Ctrl Pts',(-2.9394098901518,-0.872887160204899,
35.2253023826656));
#92404=CARTESIAN_POINT('Ctrl Pts',(-2.5250108881712,-1.75258724980421,35.2727808824207));
#92405=CARTESIAN_POINT('Ctrl Pts',(-1.84344146811026,-2.29908097703182,
35.3202593821759));
#92406=CARTESIAN_POINT('Ctrl Pts',(-1.08212931206705,-2.90951375980329,
35.3732928046716));
#92407=CARTESIAN_POINT('Ctrl Pts',(0.0125276597154277,-3.10420959734703,
35.4263262271674));
#92408=CARTESIAN_POINT('Ctrl Pts',(0.937634566011756,-2.79372353784658,
35.4793596496632));
#92409=CARTESIAN_POINT('Ctrl Pts',(1.86274147230814,-2.48323747834612,35.5323930721589));
#92410=CARTESIAN_POINT('Ctrl Pts',(2.61829831311838,-1.66756952180139,35.5854264946547));
#92411=CARTESIAN_POINT('Ctrl Pts',(2.85719574047968,-0.721444582683122,
35.6384599171505));
#92412=CARTESIAN_POINT('Ctrl Pts',(3.09609316784096,0.22468035643506,35.6914933396462));
#92413=CARTESIAN_POINT('Ctrl Pts',(2.81833118175345,1.30126227812671,35.744526762142));
#92414=CARTESIAN_POINT('Ctrl Pts',(2.15151604116683,2.01371013552097,35.7975601846377));
#92415=CARTESIAN_POINT('Ctrl Pts',(1.48470090058019,2.72615799291525,35.8505936071335));
#92416=CARTESIAN_POINT('Ctrl Pts',(0.428832605494414,3.07447178601207,35.9036270296292));
#92417=CARTESIAN_POINT('Ctrl Pts',(-0.53101381644764,2.89863314547388,35.956660452125));
#92418=CARTESIAN_POINT('Ctrl Pts',(-1.49086023838975,2.72279450493568,36.0096938746208));
#92419=CARTESIAN_POINT('Ctrl Pts',(-2.35468478718815,2.02280343076241,36.0627272971166));
#92420=CARTESIAN_POINT('Ctrl Pts',(-2.72563899335359,1.12024187709997,36.1157607196123));
#92421=CARTESIAN_POINT('Ctrl Pts',(-2.87034391332007,0.768163115849085,
36.1364484407117));
#92422=CARTESIAN_POINT('Ctrl Pts',(-2.94004927918245,0.385259420894169,
36.1571361618111));
#92423=CARTESIAN_POINT('Ctrl Pts',(-2.9380797671204,0.00166795251978762,
36.1778238829105));
#92424=CARTESIAN_POINT('Origin',(0.,0.,0.));
#92425=CARTESIAN_POINT('',(-2.94020610685266,-0.00256655506160552,37.3221761170895));
#92426=CARTESIAN_POINT('',(-2.93944817876675,-0.00236948266595389,37.1778238829104));
#92427=CARTESIAN_POINT('',(-2.942,-3.60291088309151E-16,0.));
#92428=CARTESIAN_POINT('Ctrl Pts',(-2.94020610685266,-0.00256655506160552,
37.3221761170895));
#92429=CARTESIAN_POINT('Ctrl Pts',(-2.93446364090639,0.688981411203281,
37.2848118502887));
#92430=CARTESIAN_POINT('Ctrl Pts',(-2.69086624171657,1.3841706554978,37.2474475834878));
#92431=CARTESIAN_POINT('Ctrl Pts',(-2.24570395761129,1.90809717147404,37.210083316687));
#92432=CARTESIAN_POINT('Ctrl Pts',(-1.61399794560321,2.65157329649626,37.1570616820716));
#92433=CARTESIAN_POINT('Ctrl Pts',(-0.576402102409894,3.05017883597682,
37.1040400474562));
#92434=CARTESIAN_POINT('Ctrl Pts',(0.390597011231107,2.92086546349461,37.0510184128408));
#92435=CARTESIAN_POINT('Ctrl Pts',(1.35759612487211,2.7915520910124,36.9979967782254));
#92436=CARTESIAN_POINT('Ctrl Pts',(2.25399850896079,2.13431980656741,36.94497514361));
#92437=CARTESIAN_POINT('Ctrl Pts',(2.66815670766614,1.25098395847206,36.8919535089947));
#92438=CARTESIAN_POINT('Ctrl Pts',(3.08231490637149,0.367648110376697,36.8389318743793));
#92439=CARTESIAN_POINT('Ctrl Pts',(3.0142289196935,-0.74179130136904,36.7859102397639));
#92440=CARTESIAN_POINT('Ctrl Pts',(2.49516531239286,-1.56785558800856,36.7328886051485));
#92441=CARTESIAN_POINT('Ctrl Pts',(1.97610170509222,-2.39391987464807,36.6798669705331));
#92442=CARTESIAN_POINT('Ctrl Pts',(1.00606047716893,-2.93660903618137,36.6268453359177));
#92443=CARTESIAN_POINT('Ctrl Pts',(0.0305056418984252,-2.94670841564458,
36.5738237013023));
#92444=CARTESIAN_POINT('Ctrl Pts',(-0.945049193372081,-2.9568077951078,
36.520802066687));
#92445=CARTESIAN_POINT('Ctrl Pts',(-1.92611763598987,-2.43431739250088,
36.4677804320716));
#92446=CARTESIAN_POINT('Ctrl Pts',(-2.4621717360428,-1.61917615571939,36.4147587974562));
#92447=CARTESIAN_POINT('Ctrl Pts',(-2.77417849683287,-1.14472856386347,
36.3838979040006));
#92448=CARTESIAN_POINT('Ctrl Pts',(-2.93542572807573,-0.571138320048433,
36.3530370105451));
#92449=CARTESIAN_POINT('Ctrl Pts',(-2.93766977734024,0.00128397461115384,
36.3221761170896));
#92450=CARTESIAN_POINT('Ctrl Pts',(-2.9380797671204,0.00166795251978762,
36.1778238829105));
#92451=CARTESIAN_POINT('Ctrl Pts',(-2.93500039222214,-0.598085642118336,
36.2101695843068));
#92452=CARTESIAN_POINT('Ctrl Pts',(-2.75670459734122,-1.19952056778637,
36.2425152857032));
#92453=CARTESIAN_POINT('Ctrl Pts',(-2.41589991157505,-1.68744700733082,
36.2748609870995));
#92454=CARTESIAN_POINT('Ctrl Pts',(-1.85712276009852,-2.48744230494769,
36.3278944095953));
#92455=CARTESIAN_POINT('Ctrl Pts',(-0.861484593612878,-2.98230086702986,
36.3809278320911));
#92456=CARTESIAN_POINT('Ctrl Pts',(0.113609802286804,-2.94468038980845,
36.4339612545869));
#92457=CARTESIAN_POINT('Ctrl Pts',(1.08870419818649,-2.90705991258703,36.4869946770826));
#92458=CARTESIAN_POINT('Ctrl Pts',(2.04325482350024,-2.33696039606203,36.5400280995784));
#92459=CARTESIAN_POINT('Ctrl Pts',(2.5387328644398,-1.49629048928052,36.5930615220741));
#92460=CARTESIAN_POINT('Ctrl Pts',(3.03421090537933,-0.655620582499062,
36.6460949445699));
#92461=CARTESIAN_POINT('Ctrl Pts',(3.07061636194475,0.455619714538897,36.6991283670656));
#92462=CARTESIAN_POINT('Ctrl Pts',(2.6312242524958,1.32691699754582,36.7521617895614));
#92463=CARTESIAN_POINT('Ctrl Pts',(2.19183214304681,2.19821428055281,36.8051952120572));
#92464=CARTESIAN_POINT('Ctrl Pts',(1.27664246758345,2.82956854952869,36.8582286345529));
#92465=CARTESIAN_POINT('Ctrl Pts',(0.306101279074561,2.93093019231898,36.9112620570487));
#92466=CARTESIAN_POINT('Ctrl Pts',(-0.66443990943427,3.03229183510927,36.9642954795444));
#92467=CARTESIAN_POINT('Ctrl Pts',(-1.69033261098858,2.60366085171396,37.0173289020402));
#92468=CARTESIAN_POINT('Ctrl Pts',(-2.30027284489196,1.84195402340849,37.070362324536));
#92469=CARTESIAN_POINT('Ctrl Pts',(-2.71224655861185,1.32747215554647,37.1061828439941));
#92470=CARTESIAN_POINT('Ctrl Pts',(-2.93445875073954,0.661037879533799,
37.1420033634523));
#92471=CARTESIAN_POINT('Ctrl Pts',(-2.93944817876675,-0.00236948266595389,
37.1778238829104));
#92472=CARTESIAN_POINT('Origin',(0.,0.,0.));
#92473=CARTESIAN_POINT('',(-2.94685588500563,-0.000157196364489465,38.3221761170895));
#92474=CARTESIAN_POINT('',(-2.94666346659597,-0.000711517969463661,38.1778238829105));
#92475=CARTESIAN_POINT('',(-2.942,-3.60291088309151E-16,0.));
#92476=CARTESIAN_POINT('Ctrl Pts',(-2.94685588500563,-0.000157196364489465,
38.3221761170895));
#92477=CARTESIAN_POINT('Ctrl Pts',(-2.94610829565176,0.967108386057703,
38.2696083246476));
#92478=CARTESIAN_POINT('Ctrl Pts',(-2.42386605731926,1.93506569372811,38.2170405322057));
#92479=CARTESIAN_POINT('Ctrl Pts',(-1.61474814978403,2.46507798939248,38.1644727397639));
#92480=CARTESIAN_POINT('Ctrl Pts',(-0.798644751462322,2.99966612743237,
38.1114511051485));
#92481=CARTESIAN_POINT('Ctrl Pts',(0.309309160682091,3.08871464499743,38.0584294705331));
#92482=CARTESIAN_POINT('Ctrl Pts',(1.20031707159314,2.69133052757559,38.0054078359177));
#92483=CARTESIAN_POINT('Ctrl Pts',(2.09132498250417,2.29394641015376,37.9523862013024));
#92484=CARTESIAN_POINT('Ctrl Pts',(2.76538689218184,1.41012965774507,37.8993645666869));
#92485=CARTESIAN_POINT('Ctrl Pts',(2.91295892265725,0.445748130595928,37.8463429320716));
#92486=CARTESIAN_POINT('Ctrl Pts',(3.06053095313266,-0.518633396553271,
37.7933212974562));
#92487=CARTESIAN_POINT('Ctrl Pts',(2.68161310440574,-1.56357969844294,37.7402996628408));
#92488=CARTESIAN_POINT('Ctrl Pts',(1.95021268744095,-2.20922872395834,37.6872780282254));
#92489=CARTESIAN_POINT('Ctrl Pts',(1.2188122704762,-2.8548777494737,37.63425639361));
#92490=CARTESIAN_POINT('Ctrl Pts',(0.134929285273619,-3.10122949861485,
37.5812347589946));
#92491=CARTESIAN_POINT('Ctrl Pts',(-0.803693645883662,-2.8351538943388,
37.5282131243792));
#92492=CARTESIAN_POINT('Ctrl Pts',(-1.74231657704105,-2.56907829006272,
37.4751914897639));
#92493=CARTESIAN_POINT('Ctrl Pts',(-2.5356794541531,-1.79057533236931,37.4221698551485));
#92494=CARTESIAN_POINT('Ctrl Pts',(-2.81945280229766,-0.857150498240605,
37.3691482205331));
#92495=CARTESIAN_POINT('Ctrl Pts',(-2.90325149541768,-0.581508751976585,
37.3534908527186));
#92496=CARTESIAN_POINT('Ctrl Pts',(-2.94261246750633,-0.292357357779581,
37.3378334849041));
#92497=CARTESIAN_POINT('Ctrl Pts',(-2.94020610685266,-0.00256655506160552,
37.3221761170895));
#92498=CARTESIAN_POINT('Ctrl Pts',(-2.93944817876675,-0.00236948266595389,
37.1778238829104));
#92499=CARTESIAN_POINT('Ctrl Pts',(-2.94184575820291,-0.321157897035699,
37.195036785948));
#92500=CARTESIAN_POINT('Ctrl Pts',(-2.89408422772848,-0.639247363929739,
37.2122496889856));
#92501=CARTESIAN_POINT('Ctrl Pts',(-2.79311648590866,-0.939441366687316,
37.2294625920232));
#92502=CARTESIAN_POINT('Ctrl Pts',(-2.48203212676952,-1.86434725526213,
37.282496014519));
#92503=CARTESIAN_POINT('Ctrl Pts',(-1.66587564223875,-2.61937635919603,
37.3355294370148));
#92504=CARTESIAN_POINT('Ctrl Pts',(-0.719596380769393,-2.85766177741203,
37.3885628595105));
#92505=CARTESIAN_POINT('Ctrl Pts',(0.226682880699967,-3.09594719562802,
37.4415962820063));
#92506=CARTESIAN_POINT('Ctrl Pts',(1.30308491910795,-2.81748892812605,37.4946297045021));
#92507=CARTESIAN_POINT('Ctrl Pts',(2.01510132751988,-2.15021311156027,37.5476631269978));
#92508=CARTESIAN_POINT('Ctrl Pts',(2.72711773593179,-1.4829372949945,37.6006965494936));
#92509=CARTESIAN_POINT('Ctrl Pts',(3.07474851434775,-0.426843929364974,
37.6537299719893));
#92510=CARTESIAN_POINT('Ctrl Pts',(2.89828907628243,0.532888558330936,37.7067633944851));
#92511=CARTESIAN_POINT('Ctrl Pts',(2.72182963821711,1.49262104602685,37.7597968169808));
#92512=CARTESIAN_POINT('Ctrl Pts',(2.02127998367054,2.3559926557891,37.8128302394766));
#92513=CARTESIAN_POINT('Ctrl Pts',(1.11847868344357,2.72636300223951,37.8658636619724));
#92514=CARTESIAN_POINT('Ctrl Pts',(0.215677383216621,3.0967333486899,37.9188970844681));
#92515=CARTESIAN_POINT('Ctrl Pts',(-0.88937556269077,2.97410243182843,37.9719305069639));
#92516=CARTESIAN_POINT('Ctrl Pts',(-1.68900927261872,2.41480795557453,38.0249639294596));
#92517=CARTESIAN_POINT('Ctrl Pts',(-2.45727933028583,1.87745042025602,38.0759172472766));
#92518=CARTESIAN_POINT('Ctrl Pts',(-2.94361891960952,0.937011653288061,
38.1268705650935));
#92519=CARTESIAN_POINT('Ctrl Pts',(-2.94666346659597,-0.000711517969463661,
38.1778238829105));
#92520=CARTESIAN_POINT('Origin',(0.,0.,0.));
#92521=CARTESIAN_POINT('',(-2.940678661329,0.00264606062658684,39.3221761170896));
#92522=CARTESIAN_POINT('',(-2.9416064078984,0.00271891336319057,39.1778238829104));
#92523=CARTESIAN_POINT('',(-2.942,-3.60291088309151E-16,0.));
#92524=CARTESIAN_POINT('Ctrl Pts',(-2.940678661329,0.00264606062658684,
39.3221761170896));
#92525=CARTESIAN_POINT('Ctrl Pts',(-2.94304410098273,0.275526082595591,
39.307426433622));
#92526=CARTESIAN_POINT('Ctrl Pts',(-2.90819151789947,0.547813233612533,
39.2926767501545));
#92527=CARTESIAN_POINT('Ctrl Pts',(-2.8337047940856,0.808788118727334,39.277927066687));
#92528=CARTESIAN_POINT('Ctrl Pts',(-2.56594258329314,1.74693130212563,39.2249054320716));
#92529=CARTESIAN_POINT('Ctrl Pts',(-1.78601493030073,2.53889365351255,39.1718837974562));
#92530=CARTESIAN_POINT('Ctrl Pts',(-0.852081563133812,2.82098884981591,
39.1188621628408));
#92531=CARTESIAN_POINT('Ctrl Pts',(0.0818518040331556,3.10308404611928,
39.0658405282254));
#92532=CARTESIAN_POINT('Ctrl Pts',(1.16979088537462,2.87531208733904,39.01281889361));
#92533=CARTESIAN_POINT('Ctrl Pts',(1.91213041111138,2.24227080699929,38.9597972589946));
#92534=CARTESIAN_POINT('Ctrl Pts',(2.65446993684809,1.60922952665959,38.9067756243793));
#92535=CARTESIAN_POINT('Ctrl Pts',(3.05120990698014,0.570918924760407,38.8537539897639));
#92536=CARTESIAN_POINT('Ctrl Pts',(2.92015870507473,-0.395846205229427,
38.8007323551485));
#92537=CARTESIAN_POINT('Ctrl Pts',(2.7891075031693,-1.36261133521934,38.7477107205331));
#92538=CARTESIAN_POINT('Ctrl Pts',(2.13026512922635,-2.25783099329993,38.6946890859177));
#92539=CARTESIAN_POINT('Ctrl Pts',(1.246186319647,-2.67040085712668,38.6416674513023));
#92540=CARTESIAN_POINT('Ctrl Pts',(0.362107510067668,-3.08297072095342,
38.5886458166869));
#92541=CARTESIAN_POINT('Ctrl Pts',(-0.747207735148027,-3.01289079052633,
38.5356241820716));
#92542=CARTESIAN_POINT('Ctrl Pts',(-1.57233774721256,-2.49234329290906,
38.4826025474562));
#92543=CARTESIAN_POINT('Ctrl Pts',(-2.39746775927708,-1.97179579529179,
38.4295809128408));
#92544=CARTESIAN_POINT('Ctrl Pts',(-2.93841253819042,-1.00078073048434,
38.3765592782254));
#92545=CARTESIAN_POINT('Ctrl Pts',(-2.94675848539759,-0.0252093188232366,
38.32353764361));
#92546=CARTESIAN_POINT('Ctrl Pts',(-2.94682992308237,-0.0168588510740105,
38.3230838014365));
#92547=CARTESIAN_POINT('Ctrl Pts',(-2.94686233929183,-0.00850804949871229,
38.322629959263));
#92548=CARTESIAN_POINT('Ctrl Pts',(-2.94685588500563,-0.000157196364489465,
38.3221761170895));
#92549=CARTESIAN_POINT('Ctrl Pts',(-2.94666346659597,-0.000711517969463661,
38.1778238829105));
#92550=CARTESIAN_POINT('Ctrl Pts',(-2.94678775637145,-0.0389928790179145,
38.1799039875893));
#92551=CARTESIAN_POINT('Ctrl Pts',(-2.94610659763157,-0.0772697143163753,
38.1819840922681));
#92552=CARTESIAN_POINT('Ctrl Pts',(-2.94460629035526,-0.11551441511034,
38.1840641969469));
#92553=CARTESIAN_POINT('Ctrl Pts',(-2.90635512421528,-1.09058427389499,
38.2370976194427));
#92554=CARTESIAN_POINT('Ctrl Pts',(-2.33563831798667,-2.0447659558179,38.2901310419384));
#92555=CARTESIAN_POINT('Ctrl Pts',(-1.4946481089457,-2.53970014287575,38.3431644644342));
#92556=CARTESIAN_POINT('Ctrl Pts',(-0.653657899904804,-3.03463432993356,
38.3961978869299));
#92557=CARTESIAN_POINT('Ctrl Pts',(0.457605711948423,-3.07032102212643,
38.4492313094257));
#92558=CARTESIAN_POINT('Ctrl Pts',(1.32861861129864,-2.63036544438391,38.5022647319215));
#92559=CARTESIAN_POINT('Ctrl Pts',(2.19963151064891,-2.19040986664136,38.5552981544172));
#92560=CARTESIAN_POINT('Ctrl Pts',(2.83039369749616,-1.27481201896335,38.608331576913));
#92561=CARTESIAN_POINT('Ctrl Pts',(2.93112756733703,-0.304205472164799,
38.6613649994088));
#92562=CARTESIAN_POINT('Ctrl Pts',(3.03186143717789,0.666401074633756,38.7143984219045));
#92563=CARTESIAN_POINT('Ctrl Pts',(2.60256699001241,1.69201632055282,38.7674318444003));
#92564=CARTESIAN_POINT('Ctrl Pts',(1.84046580811073,2.30146375041481,38.820465266896));
#92565=CARTESIAN_POINT('Ctrl Pts',(1.07836462620906,2.91091118027678,38.8734986893918));
#92566=CARTESIAN_POINT('Ctrl Pts',(-0.0165432904288121,3.10419079408163,
38.9265321118876));
#92567=CARTESIAN_POINT('Ctrl Pts',(-0.941247774340326,2.79250826544837,
38.9795655343833));
#92568=CARTESIAN_POINT('Ctrl Pts',(-1.86595225825184,2.4808257368151,39.0325989568791));
#92569=CARTESIAN_POINT('Ctrl Pts',(-2.62045330943702,1.66418106574372,39.0856323793748));
#92570=CARTESIAN_POINT('Ctrl Pts',(-2.85812661881906,0.717747877806678,
39.1386658018706));
#92571=CARTESIAN_POINT('Ctrl Pts',(-2.9166232565481,0.484809818950013,39.1517184955505));
#92572=CARTESIAN_POINT('Ctrl Pts',(-2.94381250888963,0.244009683839058,
39.1647711892305));
#92573=CARTESIAN_POINT('Ctrl Pts',(-2.9416064078984,0.00271891336319057,
39.1778238829104));
#92574=CARTESIAN_POINT('Origin',(0.,0.,0.));
#92575=CARTESIAN_POINT('',(-2.93747162631023,-0.00103124720635284,40.3221761170895));
#92576=CARTESIAN_POINT('',(-2.93720961253691,-0.000509911063724039,40.1778238829105));
#92577=CARTESIAN_POINT('',(-2.942,-3.60291088309151E-16,0.));
#92578=CARTESIAN_POINT('Ctrl Pts',(-2.93747162631023,-0.00103124720635284,
40.3221761170895));
#92579=CARTESIAN_POINT('Ctrl Pts',(-2.93572901194389,0.554648497353495,
40.292222907981));
#92580=CARTESIAN_POINT('Ctrl Pts',(-2.78442048137917,1.11120814384935,40.2622696988724));
#92581=CARTESIAN_POINT('Ctrl Pts',(-2.48951322196339,1.57681482701289,40.2323164897639));
#92582=CARTESIAN_POINT('Ctrl Pts',(-1.96748351564707,2.40100789893758,40.1792948551485));
#92583=CARTESIAN_POINT('Ctrl Pts',(-0.995497750798812,2.94020654772044,
40.1262732205331));
#92584=CARTESIAN_POINT('Ctrl Pts',(-0.019912914309713,2.94679903571009,
40.0732515859177));
#92585=CARTESIAN_POINT('Ctrl Pts',(0.95567192217922,2.95339152369975,40.0202299513023));
#92586=CARTESIAN_POINT('Ctrl Pts',(1.93485583030902,2.42737785089641,39.967208316687));
#92587=CARTESIAN_POINT('Ctrl Pts',(2.46797627936023,1.61031492743918,39.9141866820716));
#92588=CARTESIAN_POINT('Ctrl Pts',(3.00109672841152,0.793252003981841,39.8611650474562));
#92589=CARTESIAN_POINT('Ctrl Pts',(3.08815371838411,-0.314860170129411,
39.8081434128408));
#92590=CARTESIAN_POINT('Ctrl Pts',(2.68916878751728,-1.20515240250397,39.7551217782254));
#92591=CARTESIAN_POINT('Ctrl Pts',(2.29018385665045,-2.09544463487851,39.70210014361));
#92592=CARTESIAN_POINT('Ctrl Pts',(1.4051570049442,-2.76791692551632,39.6490785089946));
#92593=CARTESIAN_POINT('Ctrl Pts',(0.440511796540892,-2.91375538405792,
39.5960568743793));
#92594=CARTESIAN_POINT('Ctrl Pts',(-0.52413341186236,-3.05959384259952,
39.5430352397639));
#92595=CARTESIAN_POINT('Ctrl Pts',(-1.56839697696268,-2.67879846904497,
39.4900136051485));
#92596=CARTESIAN_POINT('Ctrl Pts',(-2.2127303752166,-1.94623877456288,39.4369919705331));
#92597=CARTESIAN_POINT('Ctrl Pts',(-2.67782158788453,-1.41746426499749,
39.3987200193853));
#92598=CARTESIAN_POINT('Ctrl Pts',(-2.93454090311404,-0.705413260986069,
39.3604480682374));
#92599=CARTESIAN_POINT('Ctrl Pts',(-2.940678661329,0.00264606062658684,
39.3221761170896));
#92600=CARTESIAN_POINT('Ctrl Pts',(-2.9416064078984,0.00271891336319057,
39.1778238829104));
#92601=CARTESIAN_POINT('Ctrl Pts',(-2.93484906511283,-0.736360781348812,
39.2178046117262));
#92602=CARTESIAN_POINT('Ctrl Pts',(-2.65230090246203,-1.4800436773904,39.257785340542));
#92603=CARTESIAN_POINT('Ctrl Pts',(-2.14890928239526,-2.01649167648507,
39.2977660693579));
#92604=CARTESIAN_POINT('Ctrl Pts',(-1.48117306901056,-2.72807633803696,
39.3507994918536));
#92605=CARTESIAN_POINT('Ctrl Pts',(-0.424855074662313,-3.07502395633807,
39.4038329143494));
#92606=CARTESIAN_POINT('Ctrl Pts',(0.534763077275774,-2.89794379456894,
39.4568663368451));
#92607=CARTESIAN_POINT('Ctrl Pts',(1.49438122921394,-2.7208636327998,39.5098997593409));
#92608=CARTESIAN_POINT('Ctrl Pts',(2.35729953874191,-2.01975569096034,39.5629331818367));
#92609=CARTESIAN_POINT('Ctrl Pts',(2.72708587052995,-1.11671502186279,39.6159666043324));
#92610=CARTESIAN_POINT('Ctrl Pts',(3.09687220231795,-0.213674352765307,
39.6690000268282));
#92611=CARTESIAN_POINT('Ctrl Pts',(2.97352655636609,0.891299043590286,39.7220334493239));
#92612=CARTESIAN_POINT('Ctrl Pts',(2.41371498932006,1.69057083129627,39.7750668718197));
#92613=CARTESIAN_POINT('Ctrl Pts',(1.85390342227401,2.48984261900228,39.8281002943154));
#92614=CARTESIAN_POINT('Ctrl Pts',(0.857625934133788,2.98341279805871,39.8811337168112));
#92615=CARTESIAN_POINT('Ctrl Pts',(-0.117418979607592,2.9445309590028,39.934167139307));
#92616=CARTESIAN_POINT('Ctrl Pts',(-1.09246389334897,2.9056491199469,39.9872005618027));
#92617=CARTESIAN_POINT('Ctrl Pts',(-2.04627623269148,2.33431526277864,40.0402339842985));
#92618=CARTESIAN_POINT('Ctrl Pts',(-2.54066635880802,1.4930051033132,40.0932674067943));
#92619=CARTESIAN_POINT('Ctrl Pts',(-2.80341819166967,1.04587686444428,40.121452898833));
#92620=CARTESIAN_POINT('Ctrl Pts',(-2.93640312718175,0.522492001279797,
40.1496383908717));
#92621=CARTESIAN_POINT('Ctrl Pts',(-2.93720961253691,-0.000509911063724039,
40.1778238829105));
#92622=CARTESIAN_POINT('Origin',(0.,0.,0.));
#92623=CARTESIAN_POINT('',(-2.94447081660296,-0.00226074840892904,41.3221761170895));
#92624=CARTESIAN_POINT('',(-2.94348373544085,-0.00254093421303839,41.1778238829105));
#92625=CARTESIAN_POINT('',(-2.942,-3.60291088309151E-16,0.));
#92626=CARTESIAN_POINT('Ctrl Pts',(-2.94447081660296,-0.00226074840892904,
41.3221761170895));
#92627=CARTESIAN_POINT('Ctrl Pts',(-2.93739656150027,0.830413800742868,
41.27701938234));
#92628=CARTESIAN_POINT('Ctrl Pts',(-2.56714021706357,1.6685901412572,41.2318626475904));
#92629=CARTESIAN_POINT('Ctrl Pts',(-1.94225857440192,2.21622487829653,41.1867059128408));
#92630=CARTESIAN_POINT('Ctrl Pts',(-1.20854196892092,2.85924056778373,41.1336842782254));
#92631=CARTESIAN_POINT('Ctrl Pts',(-0.123780426189747,3.10169449191821,
41.08066264361));
#92632=CARTESIAN_POINT('Ctrl Pts',(0.813879978798057,2.83224653960949,41.0276410089946));
#92633=CARTESIAN_POINT('Ctrl Pts',(1.75154038378581,2.56279858730078,40.9746193743793));
#92634=CARTESIAN_POINT('Ctrl Pts',(2.54209965103021,1.78144875854892,40.9215977397639));
#92635=CARTESIAN_POINT('Ctrl Pts',(2.82251578418982,0.847009875395524,40.8685761051485));
#92636=CARTESIAN_POINT('Ctrl Pts',(3.10293191734945,-0.0874290077579226,
40.8155544705331));
#92637=CARTESIAN_POINT('Ctrl Pts',(2.87320491642424,-1.17495694531292,40.7625328359177));
#92638=CARTESIAN_POINT('Ctrl Pts',(2.23883041277921,-1.91615747365217,40.7095112013023));
#92639=CARTESIAN_POINT('Ctrl Pts',(1.60445590913423,-2.65735800199139,40.656489566687));
#92640=CARTESIAN_POINT('Ctrl Pts',(0.565433902769473,-3.05223112111489,
40.6034679320716));
#92641=CARTESIAN_POINT('Ctrl Pts',(-0.401094120455098,-2.91944251314435,
40.5504462974562));
#92642=CARTESIAN_POINT('Ctrl Pts',(-1.36762214367972,-2.7866539051738,40.4974246628408));
#92643=CARTESIAN_POINT('Ctrl Pts',(-2.26165618376416,-2.12620357010914,
40.4444030282254));
#92644=CARTESIAN_POINT('Ctrl Pts',(-2.67263637991414,-1.24138465504358,
40.39138139361));
#92645=CARTESIAN_POINT('Ctrl Pts',(-2.8514438819544,-0.856421434326478,
40.3683129681032));
#92646=CARTESIAN_POINT('Ctrl Pts',(-2.9388136985253,-0.428987288463168,
40.3452445425964));
#92647=CARTESIAN_POINT('Ctrl Pts',(-2.93747162631023,-0.00103124720635284,
40.3221761170895));
#92648=CARTESIAN_POINT('Ctrl Pts',(-2.93720961253691,-0.000509911063724039,
40.1778238829105));
#92649=CARTESIAN_POINT('Ctrl Pts',(-2.93792059859996,-0.461580987238054,
40.2026718133675));
#92650=CARTESIAN_POINT('Ctrl Pts',(-2.83590334183077,-0.922354436493001,
40.2275197438245));
#92651=CARTESIAN_POINT('Ctrl Pts',(-2.62950553583792,-1.33031966921331,
40.2523676742815));
#92652=CARTESIAN_POINT('Ctrl Pts',(-2.18898667386072,-2.20104782051176,
40.3054010967773));
#92653=CARTESIAN_POINT('Ctrl Pts',(-1.27298103701576,-2.83121766134602,
40.358434519273));
#92654=CARTESIAN_POINT('Ctrl Pts',(-0.30230953798844,-2.93132371609471,
40.4114679417688));
#92655=CARTESIAN_POINT('Ctrl Pts',(0.668361961038936,-3.0314297708434,40.4645013642645));
#92656=CARTESIAN_POINT('Ctrl Pts',(1.69369932224868,-2.60147203950645,40.5175347867603));
#92657=CARTESIAN_POINT('Ctrl Pts',(2.30265369310215,-1.83897682283957,40.5705682092561));
#92658=CARTESIAN_POINT('Ctrl Pts',(2.91160806395557,-1.07648160617274,40.6236016317518));
#92659=CARTESIAN_POINT('Ctrl Pts',(3.10417944445277,0.01855109582397,40.6766350542476));
#92660=CARTESIAN_POINT('Ctrl Pts',(2.79189887672024,0.943053788214828,40.7296684767434));
#92661=CARTESIAN_POINT('Ctrl Pts',(2.47961830898771,1.86755648060569,40.7827018992391));
#92662=CARTESIAN_POINT('Ctrl Pts',(1.66248579302546,2.62152916339069,40.8357353217349));
#92663=CARTESIAN_POINT('Ctrl Pts',(0.715899074568479,2.85859026450628,40.8887687442307));
#92664=CARTESIAN_POINT('Ctrl Pts',(-0.230687643888503,3.09565136562187,
40.9418021667264));
#92665=CARTESIAN_POINT('Ctrl Pts',(-1.30672856484022,2.81580088506805,40.9948355892222));
#92666=CARTESIAN_POINT('Ctrl Pts',(-2.01788118183506,2.14760455421709,41.0478690117179));
#92667=CARTESIAN_POINT('Ctrl Pts',(-2.59875856312033,1.60181434607681,41.0911873021154));
#92668=CARTESIAN_POINT('Ctrl Pts',(-2.9361896045507,0.796927381949951,41.1345055925129));
#92669=CARTESIAN_POINT('Ctrl Pts',(-2.94348373544085,-0.00254093421303839,
41.1778238829105));
#92670=CARTESIAN_POINT('Origin',(0.,0.,0.));
#92671=CARTESIAN_POINT('',(-2.94473630969457,0.00215967812386454,42.3221761170896));
#92672=CARTESIAN_POINT('',(-2.94562033411779,0.00171615163861752,42.1778238829104));
#92673=CARTESIAN_POINT('',(-2.942,-3.60291088309151E-16,0.));
#92674=CARTESIAN_POINT('Ctrl Pts',(-2.94473630969457,0.00215967812386454,
42.3221761170896));
#92675=CARTESIAN_POINT('Ctrl Pts',(-2.94584995717871,0.137449629621458,
42.3148374913143));
#92676=CARTESIAN_POINT('Ctrl Pts',(-2.93733632589731,0.27259864460851,42.3074988655391));
#92677=CARTESIAN_POINT('Ctrl Pts',(-2.91871689001713,0.406340739954757,
42.3001602397639));
#92678=CARTESIAN_POINT('Ctrl Pts',(-2.78419130495222,1.37262853406591,42.2471386051485));
#92679=CARTESIAN_POINT('Ctrl Pts',(-2.12213514233659,2.26547406799627,42.1941169705331));
#92680=CARTESIAN_POINT('Ctrl Pts',(-1.23657898017349,2.67486326880671,42.1410953359177));
#92681=CARTESIAN_POINT('Ctrl Pts',(-0.351022818010432,3.08425246961713,
42.0880737013023));
#92682=CARTESIAN_POINT('Ctrl Pts',(0.758033343700066,3.0101853373077,42.035052066687));
#92683=CARTESIAN_POINT('Ctrl Pts',(1.58128681294659,2.48667510869825,41.9820304320716));
#92684=CARTESIAN_POINT('Ctrl Pts',(2.40454028219315,1.96316488008877,41.9290087974562));
#92685=CARTESIAN_POINT('Ctrl Pts',(2.94199105897571,0.990211555179222,41.8759871628408));
#92686=CARTESIAN_POINT('Ctrl Pts',(2.94683006645108,0.0146164454682759,
41.8229655282254));
#92687=CARTESIAN_POINT('Ctrl Pts',(2.95166907392646,-0.960978664242615,
41.76994389361));
#92688=CARTESIAN_POINT('Ctrl Pts',(2.4238963120947,-1.9392155587549,41.7169222589946));
#92689=CARTESIAN_POINT('Ctrl Pts',(1.60587650300619,-2.47086659658324,41.6639006243793));
#92690=CARTESIAN_POINT('Ctrl Pts',(0.787856693917635,-3.00251763441161,
41.6108789897639));
#92691=CARTESIAN_POINT('Ctrl Pts',(-0.320410162427715,-3.08758281555597,
41.5578573551485));
#92692=CARTESIAN_POINT('Ctrl Pts',(-1.20998384019564,-2.68699836015649,
41.5048357205331));
#92693=CARTESIAN_POINT('Ctrl Pts',(-2.09955751796362,-2.28641390475698,
41.4518140859177));
#92694=CARTESIAN_POINT('Ctrl Pts',(-2.77043801715415,-1.40017981281356,
41.3987924513023));
#92695=CARTESIAN_POINT('Ctrl Pts',(-2.91454243263391,-0.43527403942188,
41.3457708166869));
#92696=CARTESIAN_POINT('Ctrl Pts',(-2.93591798633362,-0.292145911767843,
41.3379059168211));
#92697=CARTESIAN_POINT('Ctrl Pts',(-2.94570293199651,-0.147286777996668,
41.3300410169553));
#92698=CARTESIAN_POINT('Ctrl Pts',(-2.94447081660296,-0.00226074840892904,
41.3221761170895));
#92699=CARTESIAN_POINT('Ctrl Pts',(-2.94348373544085,-0.00254093421303839,
41.1778238829105));
#92700=CARTESIAN_POINT('Ctrl Pts',(-2.94511961359969,-0.181840260862772,
41.1875390150087));
#92701=CARTESIAN_POINT('Ctrl Pts',(-2.93015010916664,-0.360867037792384,
41.197254147107));
#92702=CARTESIAN_POINT('Ctrl Pts',(-2.89759730047774,-0.536637372498586,
41.2069692792052));
#92703=CARTESIAN_POINT('Ctrl Pts',(-2.71989648908757,-1.49614078721505,
41.260002701701));
#92704=CARTESIAN_POINT('Ctrl Pts',(-2.01823055326929,-2.3586054354999,41.3130361241967));
#92705=CARTESIAN_POINT('Ctrl Pts',(-1.11495089309546,-2.7278075979225,41.3660695466925));
#92706=CARTESIAN_POINT('Ctrl Pts',(-0.211671232921631,-3.0970097603451,
41.4191029691882));
#92707=CARTESIAN_POINT('Ctrl Pts',(0.893222151607806,-2.97294943690546,
41.472136391684));
#92708=CARTESIAN_POINT('Ctrl Pts',(1.69213168271017,-2.41262101326887,41.5251698141798));
#92709=CARTESIAN_POINT('Ctrl Pts',(2.49104121381259,-1.85229258963225,41.5782032366755));
#92710=CARTESIAN_POINT('Ctrl Pts',(2.9839668914879,-0.855696065798763,41.6312366591713));
#92711=CARTESIAN_POINT('Ctrl Pts',(2.94445439578259,0.119323494981688,41.684270081667));
#92712=CARTESIAN_POINT('Ctrl Pts',(2.90494190007729,1.09434305576208,41.7373035041628));
#92713=CARTESIAN_POINT('Ctrl Pts',(2.33299123099132,2.04778565348939,41.7903369266586));
#92714=CARTESIAN_POINT('Ctrl Pts',(1.49136147307008,2.54163151183257,41.8433703491543));
#92715=CARTESIAN_POINT('Ctrl Pts',(0.649731715148849,3.03547737017575,41.8964037716501));
#92716=CARTESIAN_POINT('Ctrl Pts',(-0.461577131607709,3.06972648913485,
41.9494371941458));
#92717=CARTESIAN_POINT('Ctrl Pts',(-1.33202017057833,2.6286445272175,42.0024706166416));
#92718=CARTESIAN_POINT('Ctrl Pts',(-2.20246320954901,2.18756256530014,42.0555040391373));
#92719=CARTESIAN_POINT('Ctrl Pts',(-2.83204044073378,1.27114952250626,42.1085374616331));
#92720=CARTESIAN_POINT('Ctrl Pts',(-2.93151863851002,0.300413477338171,
42.1615708841289));
#92721=CARTESIAN_POINT('Ctrl Pts',(-2.94168090317986,0.201247259653578,
42.1669885503894));
#92722=CARTESIAN_POINT('Ctrl Pts',(-2.94631116750731,0.101514138713564,
42.1724062166499));
#92723=CARTESIAN_POINT('Ctrl Pts',(-2.94562033411779,0.00171615163861752,
42.1778238829104));
#92724=CARTESIAN_POINT('Origin',(0.,0.,0.));
#92725=CARTESIAN_POINT('',(-2.93758116933064,0.00117923657373634,43.3221761170895));
#92726=CARTESIAN_POINT('',(-2.93812373739311,0.00170130757060122,43.1778238829105));
#92727=CARTESIAN_POINT('',(-2.942,-3.60291088309151E-16,0.));
#92728=CARTESIAN_POINT('Ctrl Pts',(-2.93758116933064,0.00117923657373634,
43.3221761170895));
#92729=CARTESIAN_POINT('Ctrl Pts',(-2.93908400894455,0.419333117468769,
43.2996339656733));
#92730=CARTESIAN_POINT('Ctrl Pts',(-2.85580724763625,0.836915777227387,
43.277091814257));
#92731=CARTESIAN_POINT('Ctrl Pts',(-2.68481925250477,1.21481136906017,43.2545496628408));
#92732=CARTESIAN_POINT('Ctrl Pts',(-2.28263656665219,2.10366361847272,43.2015280282254));
#92733=CARTESIAN_POINT('Ctrl Pts',(-1.39519809743223,2.77295015895075,43.1485063936101));
#92734=CARTESIAN_POINT('Ctrl Pts',(-0.430034876159872,2.91532006584257,
43.0954847589947));
#92735=CARTESIAN_POINT('Ctrl Pts',(0.535128345112486,3.05768997273439,43.0424631243793));
#92736=CARTESIAN_POINT('Ctrl Pts',(1.57801631843724,2.67314324604,42.9894414897639));
#92737=CARTESIAN_POINT('Ctrl Pts',(2.21971222190921,1.93827209981602,42.9364198551485));
#92738=CARTESIAN_POINT('Ctrl Pts',(2.86140812538118,1.20340095359203,42.8833982205331));
#92739=CARTESIAN_POINT('Ctrl Pts',(3.10191195900036,0.118205387838451,42.8303765859177));
#92740=CARTESIAN_POINT('Ctrl Pts',(2.83077913562125,-0.818969209646855,
42.7773549513024));
#92741=CARTESIAN_POINT('Ctrl Pts',(2.55964631224217,-1.75614380713211,42.724333316687));
#92742=CARTESIAN_POINT('Ctrl Pts',(1.77687683186485,-2.5452974363491,42.6713116820716));
#92743=CARTESIAN_POINT('Ctrl Pts',(0.841935451409881,-2.82403360048663,
42.6182900474562));
#92744=CARTESIAN_POINT('Ctrl Pts',(-0.0930059290451951,-3.10276976462418,
42.5652684128408));
#92745=CARTESIAN_POINT('Ctrl Pts',(-1.18011920957796,-2.87108846368215,
42.5122467782254));
#92746=CARTESIAN_POINT('Ctrl Pts',(-1.9201783460872,-2.23538278606508,42.45922514361));
#92747=CARTESIAN_POINT('Ctrl Pts',(-2.55780727474305,-1.68766394825522,
42.4135421347699));
#92748=CARTESIAN_POINT('Ctrl Pts',(-2.93780384448635,-0.840021438553098,
42.3678591259297));
#92749=CARTESIAN_POINT('Ctrl Pts',(-2.94473630969457,0.00215967812386454,
42.3221761170896));
#92750=CARTESIAN_POINT('Ctrl Pts',(-2.94562033411779,0.00171615163861752,
42.1778238829104));
#92751=CARTESIAN_POINT('Ctrl Pts',(-2.93954861380638,-0.875406283894391,
42.2254396391457));
#92752=CARTESIAN_POINT('Ctrl Pts',(-2.52244254972299,-1.75753937899873,
42.2730553953809));
#92753=CARTESIAN_POINT('Ctrl Pts',(-1.83748706821796,-2.30384267245614,
42.3206711516162));
#92754=CARTESIAN_POINT('Ctrl Pts',(-1.07459813578189,-2.91230372954013,
42.3737045741119));
#92755=CARTESIAN_POINT('Ctrl Pts',(0.0205588934579998,-3.10416679616593,
42.4267379966077));
#92756=CARTESIAN_POINT('Ctrl Pts',(0.944859407555178,-2.79128831997924,
42.4797714191034));
#92757=CARTESIAN_POINT('Ctrl Pts',(1.86915992165246,-2.47840984379252,42.5328048415992));
#92758=CARTESIAN_POINT('Ctrl Pts',(2.62260392060693,-1.66078982479322,42.5858382640949));
#92759=CARTESIAN_POINT('Ctrl Pts',(2.8590527142797,-0.714049971828252,42.6388716865907));
#92760=CARTESIAN_POINT('Ctrl Pts',(3.09550150795247,0.232689881136659,42.6919051090865));
#92761=CARTESIAN_POINT('Ctrl Pts',(2.81495509634351,1.30854956806729,42.7449385315822));
#92762=CARTESIAN_POINT('Ctrl Pts',(2.14629892757145,2.01926984298872,42.797971954078));
#92763=CARTESIAN_POINT('Ctrl Pts',(1.47764275879943,2.72999011791011,42.8510053765738));
#92764=CARTESIAN_POINT('Ctrl Pts',(0.420876832864394,3.07557098082247,42.9040387990695));
#92765=CARTESIAN_POINT('Ctrl Pts',(-0.538511443214592,2.89724959415391,
42.9570722215653));
#92766=CARTESIAN_POINT('Ctrl Pts',(-1.49789971929374,2.71892820748532,43.010105644061));
#92767=CARTESIAN_POINT('Ctrl Pts',(-2.35991034551675,2.01670457123563,43.0631390665568));
#92768=CARTESIAN_POINT('Ctrl Pts',(-2.72852818411529,1.11318629787948,43.1161724890526));
#92769=CARTESIAN_POINT('Ctrl Pts',(-2.87136768972636,0.76307273862408,43.1367229536719));
#92770=CARTESIAN_POINT('Ctrl Pts',(-2.94012108793881,0.382733492091749,
43.1572734182912));
#92771=CARTESIAN_POINT('Ctrl Pts',(-2.93812373739311,0.00170130757060122,
43.1778238829105));
#92772=CARTESIAN_POINT('Origin',(0.,0.,0.));
#92773=CARTESIAN_POINT('',(-2.94040227747744,-0.00260344384514166,44.3221761170895));
#92774=CARTESIAN_POINT('',(-2.93938501957473,-0.00234810359620528,44.1778238829104));
#92775=CARTESIAN_POINT('',(-2.942,-3.60291088309151E-16,0.));
#92776=CARTESIAN_POINT('Ctrl Pts',(-2.94040227747744,-0.00260344384514166,
44.3221761170895));
#92777=CARTESIAN_POINT('Ctrl Pts',(-2.93448873783951,0.695885794181435,
44.2844304400323));
#92778=CARTESIAN_POINT('Ctrl Pts',(-2.6854279089453,1.39816509258832,44.246684762975));
#92779=CARTESIAN_POINT('Ctrl Pts',(-2.23192793799287,1.92419301542808,44.2089390859177));
#92780=CARTESIAN_POINT('Ctrl Pts',(-1.59489314003593,2.66310836936333,44.1559174513024));
#92781=CARTESIAN_POINT('Ctrl Pts',(-0.554458396646493,3.05424396561426,
44.102895816687));
#92782=CARTESIAN_POINT('Ctrl Pts',(0.411586046778129,2.91798183803642,44.0498741820716));
#92783=CARTESIAN_POINT('Ctrl Pts',(1.37763049020286,2.78171971045856,43.9968525474562));
#92784=CARTESIAN_POINT('Ctrl Pts',(2.2692846336627,2.11805985905179,43.9438309128408));
#92785=CARTESIAN_POINT('Ctrl Pts',(2.67708151661102,1.23176931056174,43.8908092782254));
#92786=CARTESIAN_POINT('Ctrl Pts',(3.08487839955926,0.345478762071852,43.83778764361));
#92787=CARTESIAN_POINT('Ctrl Pts',(3.00881802199609,-0.763442483501333,
43.7847660089947));
#92788=CARTESIAN_POINT('Ctrl Pts',(2.48382896228187,-1.58575369056714,43.7317443743793));
#92789=CARTESIAN_POINT('Ctrl Pts',(1.95883990256756,-2.40806489763308,43.6787227397639));
#92790=CARTESIAN_POINT('Ctrl Pts',(0.984922160702103,-2.94376606619166,
43.6257011051484));
#92791=CARTESIAN_POINT('Ctrl Pts',(0.00931992940853922,-2.94685157752022,
43.572679470533));
#92792=CARTESIAN_POINT('Ctrl Pts',(-0.966282301884858,-2.94993708884877,
43.5196578359177));
#92793=CARTESIAN_POINT('Ctrl Pts',(-1.9435690226063,-2.42040694294752,43.4666362013024));
#92794=CARTESIAN_POINT('Ctrl Pts',(-2.47374893172442,-1.60143289082343,
43.413614566687));
#92795=CARTESIAN_POINT('Ctrl Pts',(-2.77852281788827,-1.13064571039558,
43.3831350834879));
#92796=CARTESIAN_POINT('Ctrl Pts',(-2.93554916387039,-0.564211082746676,
43.3526556002887));
#92797=CARTESIAN_POINT('Ctrl Pts',(-2.93758116933064,0.00117923657373634,
43.3221761170895));
#92798=CARTESIAN_POINT('Ctrl Pts',(-2.93812373739311,0.00170130757060122,
43.1778238829105));
#92799=CARTESIAN_POINT('Ctrl Pts',(-2.93496663827918,-0.600574729914202,
43.2103068407869));
#92800=CARTESIAN_POINT('Ctrl Pts',(-2.75504347670453,-1.20458202709536,
43.2427897986634));
#92801=CARTESIAN_POINT('Ctrl Pts',(-2.41152602787865,-1.69369182620744,
43.2752727565398));
#92802=CARTESIAN_POINT('Ctrl Pts',(-1.85068098206933,-2.49223876647609,
43.3283061790356));
#92803=CARTESIAN_POINT('Ctrl Pts',(-0.853765839476469,-2.98451973655098,
43.3813396015314));
#92804=CARTESIAN_POINT('Ctrl Pts',(0.121227960435853,-2.94437660072665,
43.4343730240271));
#92805=CARTESIAN_POINT('Ctrl Pts',(1.09622176034817,-2.90423346490231,43.4874064465229));
#92806=CARTESIAN_POINT('Ctrl Pts',(2.04929421758002,-2.33166622317874,43.5404398690186));
#92807=CARTESIAN_POINT('Ctrl Pts',(2.54259560154553,-1.48971721890414,43.5934732915144));
#92808=CARTESIAN_POINT('Ctrl Pts',(3.03589698551106,-0.647768214629499,
43.6465067140102));
#92809=CARTESIAN_POINT('Ctrl Pts',(3.06942729621027,0.463562552196082,43.6995401365059));
#92810=CARTESIAN_POINT('Ctrl Pts',(2.62778241888289,1.33372011468222,43.7525735590017));
#92811=CARTESIAN_POINT('Ctrl Pts',(2.18613754155555,2.20387767716831,43.8056069814974));
#92812=CARTESIAN_POINT('Ctrl Pts',(1.26931747620161,2.83286203531488,43.8586404039932));
#92813=CARTESIAN_POINT('Ctrl Pts',(0.298517291007927,2.93171233450133,43.911673826489));
#92814=CARTESIAN_POINT('Ctrl Pts',(-0.672282894185814,3.03056263368778,
43.9647072489847));
#92815=CARTESIAN_POINT('Ctrl Pts',(-1.69706319921938,2.59927887391403,44.0177406714805));
#92816=CARTESIAN_POINT('Ctrl Pts',(-2.30503068797946,1.83599654486918,44.0707740939763));
#92817=CARTESIAN_POINT('Ctrl Pts',(-2.71409845623966,1.32242599271415,44.1064573569543));
#92818=CARTESIAN_POINT('Ctrl Pts',(-2.93446666976082,0.658553003231076,
44.1421406199324));
#92819=CARTESIAN_POINT('Ctrl Pts',(-2.93938501957473,-0.00234810359620528,
44.1778238829104));
#92820=CARTESIAN_POINT('Origin',(0.,0.,0.));
#92821=CARTESIAN_POINT('',(-2.94686614867256,-2.51058573618992E-5,45.3221761170895));
#92822=CARTESIAN_POINT('',(-2.94663624902442,-0.000757038452637187,45.1778238829105));
#92823=CARTESIAN_POINT('',(-2.942,-3.60291088309151E-16,0.));
#92824=CARTESIAN_POINT('Ctrl Pts',(-2.94686604665161,-2.51053310065807E-5,
45.3221761170895));
#92825=CARTESIAN_POINT('Ctrl Pts',(-2.94674347542402,0.974249485910166,
45.2692269143912));
#92826=CARTESIAN_POINT('Ctrl Pts',(-2.41578966879103,1.94863846518009,45.216277711693));
#92827=CARTESIAN_POINT('Ctrl Pts',(-1.59698410515242,2.47662327554372,45.1633285089947));
#92828=CARTESIAN_POINT('Ctrl Pts',(-0.777058455588465,3.00533034327972,
45.1103068743793));
#92829=CARTESIAN_POINT('Ctrl Pts',(0.331507023858134,3.08641108866027,45.0572852397639));
#92830=CARTESIAN_POINT('Ctrl Pts',(1.21963497345379,2.68263147156411,45.0042636051485));
#92831=CARTESIAN_POINT('Ctrl Pts',(2.10776292304939,2.27885185446797,44.9512419705331));
#92832=CARTESIAN_POINT('Ctrl Pts',(2.77545334279413,1.39021187489515,44.8982203359177));
#92833=CARTESIAN_POINT('Ctrl Pts',(2.91608828119759,0.424794323698634,44.8451987013024));
#92834=CARTESIAN_POINT('Ctrl Pts',(3.05672321960106,-0.540623227497989,
44.792177066687));
#92835=CARTESIAN_POINT('Ctrl Pts',(2.67030267666323,-1.58281835031824,44.7391554320716));
#92836=CARTESIAN_POINT('Ctrl Pts',(1.93427936366993,-2.22319239479913,44.6861337974562));
#92837=CARTESIAN_POINT('Ctrl Pts',(1.19825605067672,-2.86356643927994,44.6331121628408));
#92838=CARTESIAN_POINT('Ctrl Pts',(0.112629967628113,-3.10211940542135,
44.5800905282254));
#92839=CARTESIAN_POINT('Ctrl Pts',(-0.82405579482585,-2.82930258685599,
44.52706889361));
#92840=CARTESIAN_POINT('Ctrl Pts',(-1.76074155727987,-2.55648576829062,
44.4740472589946));
#92841=CARTESIAN_POINT('Ctrl Pts',(-2.54848699913928,-1.77229916501841,
44.4210256243793));
#92842=CARTESIAN_POINT('Ctrl Pts',(-2.82554229380675,-0.836858307572525,
44.3680039897639));
#92843=CARTESIAN_POINT('Ctrl Pts',(-2.90536414300644,-0.567350305035001,
44.3527280322058));
#92844=CARTESIAN_POINT('Ctrl Pts',(-2.9427955311576,-0.285287257906869,
44.3374520746477));
#92845=CARTESIAN_POINT('Ctrl Pts',(-2.94040227747744,-0.00260344384514166,
44.3221761170895));
#92846=CARTESIAN_POINT('Ctrl Pts',(-2.93938501957473,-0.00234810359620528,
44.1778238829104));
#92847=CARTESIAN_POINT('Ctrl Pts',(-2.94177645316889,-0.323695947707879,
44.1951740424281));
#92848=CARTESIAN_POINT('Ctrl Pts',(-2.89323197945426,-0.644341189660126,
44.2125242019458));
#92849=CARTESIAN_POINT('Ctrl Pts',(-2.7906765954805,-0.946664631606558,
44.2298743614635));
#92850=CARTESIAN_POINT('Ctrl Pts',(-2.47720034173483,-1.87076258072161,
44.2829077839593));
#92851=CARTESIAN_POINT('Ctrl Pts',(-1.65909316175687,-2.6236775806358,44.335941206455));
#92852=CARTESIAN_POINT('Ctrl Pts',(-0.712200570359879,-2.85951396794568,
44.3889746289508));
#92853=CARTESIAN_POINT('Ctrl Pts',(0.234692021037057,-3.09535035525555,
44.4420080514465));
#92854=CARTESIAN_POINT('Ctrl Pts',(1.31037002385295,-2.81410812996117,44.4950414739423));
#92855=CARTESIAN_POINT('Ctrl Pts',(2.02065765936511,-2.14499240300543,44.548074896438));
#92856=CARTESIAN_POINT('Ctrl Pts',(2.73094529487735,-1.47587667604963,44.6011083189338));
#92857=CARTESIAN_POINT('Ctrl Pts',(3.07584256308573,-0.41888744743224,44.6541417414296));
#92858=CARTESIAN_POINT('Ctrl Pts',(2.89690067574173,0.54038528864112,44.7071751639254));
#92859=CARTESIAN_POINT('Ctrl Pts',(2.71795878839774,1.49965802471448,44.7602085864212));
#92860=CARTESIAN_POINT('Ctrl Pts',(2.01517774550148,2.36121426824389,44.8132420089169));
#92861=CARTESIAN_POINT('Ctrl Pts',(1.11142123695542,2.72924762880537,44.8662754314126));
#92862=CARTESIAN_POINT('Ctrl Pts',(0.207664728409461,3.0972809893668,44.9193088539084));
#92863=CARTESIAN_POINT('Ctrl Pts',(-0.897067245786189,2.97179146696041,
44.9723422764041));
#92864=CARTESIAN_POINT('Ctrl Pts',(-1.69525126113925,2.41043003361006,45.0253756988999));
#92865=CARTESIAN_POINT('Ctrl Pts',(-2.46006269463699,1.87253947918556,45.0761917602368));
#92866=CARTESIAN_POINT('Ctrl Pts',(-2.94342421446499,0.934463217541238,
45.1270078215736));
#92867=CARTESIAN_POINT('Ctrl Pts',(-2.94663624902442,-0.000757038452637187,
45.1778238829105));
#92868=CARTESIAN_POINT('Origin',(0.,0.,0.));
#92869=CARTESIAN_POINT('',(-2.94047772160941,0.00261614231624671,46.3221761170895));
#92870=CARTESIAN_POINT('',(-2.94168313190805,0.00271989540251569,46.1778238829104));
#92871=CARTESIAN_POINT('',(-2.942,-3.60291088309151E-16,0.));
#92872=CARTESIAN_POINT('Ctrl Pts',(-2.94047772160941,0.00261614231624671,
46.3221761170895));
#92873=CARTESIAN_POINT('Ctrl Pts',(-2.94286443428716,0.282601028255245,
46.3070450233656));
#92874=CARTESIAN_POINT('Ctrl Pts',(-2.90615255438172,0.561972588305002,
46.2919139296416));
#92875=CARTESIAN_POINT('Ctrl Pts',(-2.82781690667401,0.829139711354088,
46.2767828359177));
#92876=CARTESIAN_POINT('Ctrl Pts',(-2.55331698182402,1.76533360705024,46.2237612013023));
#92877=CARTESIAN_POINT('Ctrl Pts',(-1.76771577226658,2.55166832950176,46.170739566687));
#92878=CARTESIAN_POINT('Ctrl Pts',(-0.831778455781653,2.82704186270968,
46.1177179320716));
#92879=CARTESIAN_POINT('Ctrl Pts',(0.104158860703217,3.10241539591758,46.0646962974562));
#92880=CARTESIAN_POINT('Ctrl Pts',(1.19043228411555,2.86682773988194,46.0116746628408));
#92881=CARTESIAN_POINT('Ctrl Pts',(1.92820146634532,2.22846587792299,45.9586530282254));
#92882=CARTESIAN_POINT('Ctrl Pts',(2.66597064857513,1.590104015964,45.90563139361));
#92883=CARTESIAN_POINT('Ctrl Pts',(3.05523558962236,0.548967948081663,45.8526097589947));
#92884=CARTESIAN_POINT('Ctrl Pts',(2.91723736081436,-0.416830023037316,
45.7995881243793));
#92885=CARTESIAN_POINT('Ctrl Pts',(2.77923913200637,-1.38262799415624,45.7465664897639));
#92886=CARTESIAN_POINT('Ctrl Pts',(2.11397773334323,-2.27308786851182,45.6935448551485));
#92887=CARTESIAN_POINT('Ctrl Pts',(1.22695566109724,-2.67929111665561,45.6405232205331));
#92888=CARTESIAN_POINT('Ctrl Pts',(0.339933588851193,-3.08549436479943,
45.5875015859177));
#92889=CARTESIAN_POINT('Ctrl Pts',(-0.768849156977722,-3.00744098673142,
45.5344799513024));
#92890=CARTESIAN_POINT('Ctrl Pts',(-1.59021544510426,-2.48097479164936,
45.481458316687));
#92891=CARTESIAN_POINT('Ctrl Pts',(-2.41270378718693,-1.95378940041144,
45.4283642501545));
#92892=CARTESIAN_POINT('Ctrl Pts',(-2.94698895322209,-0.976965216459942,
45.375270183622));
#92893=CARTESIAN_POINT('Ctrl Pts',(-2.94686604665161,-2.51053310065807E-5,
45.3221761170895));
#92894=CARTESIAN_POINT('Ctrl Pts',(-2.94663624902442,-0.000757038452637187,
45.1778238829105));
#92895=CARTESIAN_POINT('Ctrl Pts',(-2.94677640629922,-0.0415654170659208,
45.1800412440694));
#92896=CARTESIAN_POINT('Ctrl Pts',(-2.94600235068899,-0.0823683577952838,
45.1822586052283));
#92897=CARTESIAN_POINT('Ctrl Pts',(-2.94429757386013,-0.123132375178255,
45.1844759663872));
#92898=CARTESIAN_POINT('Ctrl Pts',(-2.90352381471748,-1.09810000632183,
45.237509388883));
#92899=CARTESIAN_POINT('Ctrl Pts',(-2.33034023992174,-2.05080192431461,
45.2905428113787));
#92900=CARTESIAN_POINT('Ctrl Pts',(-1.48807234151735,-2.54355862753419,
45.3435762338744));
#92901=CARTESIAN_POINT('Ctrl Pts',(-0.645804443112948,-3.03631533075377,
45.3966096563702));
#92902=CARTESIAN_POINT('Ctrl Pts',(0.465547778900108,-3.06912681920016,
45.449643078866));
#92903=CARTESIAN_POINT('Ctrl Pts',(1.33541950084067,-2.62691921121265,45.5026765013617));
#92904=CARTESIAN_POINT('Ctrl Pts',(2.20529122278124,-2.18471160322514,45.5557099238575));
#92905=CARTESIAN_POINT('Ctrl Pts',(2.83368244464931,-1.26748489880373,45.6087433463532));
#92906=CARTESIAN_POINT('Ctrl Pts',(2.93190480393636,-0.296620979756358,
45.661776768849));
#92907=CARTESIAN_POINT('Ctrl Pts',(3.03012716322342,0.674242939291123,45.7148101913448));
#92908=CARTESIAN_POINT('Ctrl Pts',(2.59818065992933,1.69874407296457,45.7678436138406));
#92909=CARTESIAN_POINT('Ctrl Pts',(1.83450525351452,2.30621773911007,45.8208770363363));
#92910=CARTESIAN_POINT('Ctrl Pts',(1.07082984709984,2.91369140525546,45.8739104588321));
#92911=CARTESIAN_POINT('Ctrl Pts',(-0.0245744624354413,3.10413760387306,
45.9269438813278));
#92912=CARTESIAN_POINT('Ctrl Pts',(-0.948469459799883,2.79006370360431,
45.9799773038235));
#92913=CARTESIAN_POINT('Ctrl Pts',(-1.87236445716438,2.47598980333554,46.0330107263193));
#92914=CARTESIAN_POINT('Ctrl Pts',(-2.62475014235801,1.65739580418036,46.0860441488151));
#92915=CARTESIAN_POINT('Ctrl Pts',(-2.85997402495524,0.710350870700089,
46.1390775713109));
#92916=CARTESIAN_POINT('Ctrl Pts',(-2.9172590188444,0.479713306911208,46.1519930085107));
#92917=CARTESIAN_POINT('Ctrl Pts',(-2.94387178257188,0.241457476262084,
46.1649084457106));
#92918=CARTESIAN_POINT('Ctrl Pts',(-2.94168313190805,0.00271989540251569,
46.1778238829104));
#92919=CARTESIAN_POINT('Origin',(0.,0.,0.));
#92920=CARTESIAN_POINT('',(-2.93754881179149,-0.00113833082597881,47.3221761170895));
#92921=CARTESIAN_POINT('',(-2.93719707228474,-0.000468378137186533,47.1778238829104));
#92922=CARTESIAN_POINT('',(-2.942,-3.60291088309151E-16,0.));
#92923=CARTESIAN_POINT('Ctrl Pts',(-2.93754881179149,-0.00113833082597881,
47.3221761170895));
#92924=CARTESIAN_POINT('Ctrl Pts',(-2.93559720265068,0.561579659279432,
47.2918414977246));
#92925=CARTESIAN_POINT('Ctrl Pts',(-2.78015759911032,1.12529577977501,47.2615068783596));
#92926=CARTESIAN_POINT('Ctrl Pts',(-2.47811301989175,1.59467174661818,47.2311722589946));
#92927=CARTESIAN_POINT('Ctrl Pts',(-1.95017175502176,2.41509018377687,47.1781506243792));
#92928=CARTESIAN_POINT('Ctrl Pts',(-0.974333818001319,2.94728756516578,
47.1251289897639));
#92929=CARTESIAN_POINT('Ctrl Pts',(0.00127339248023564,2.94686620634015,
47.0721073551485));
#92930=CARTESIAN_POINT('Ctrl Pts',(0.976880602961791,2.94644484751451,47.0190857205331));
#92931=CARTESIAN_POINT('Ctrl Pts',(1.95225708690446,2.41340474847432,46.9660640859178));
#92932=CARTESIAN_POINT('Ctrl Pts',(2.47948950501506,1.59253007365169,46.9130424513024));
#92933=CARTESIAN_POINT('Ctrl Pts',(3.00672192312566,0.771655398829069,46.860020816687));
#92934=CARTESIAN_POINT('Ctrl Pts',(3.08581027540417,-0.337053851776008,
46.8069991820716));
#92935=CARTESIAN_POINT('Ctrl Pts',(2.68043508402907,-1.22445459233511,46.7539775474562));
#92936=CARTESIAN_POINT('Ctrl Pts',(2.27505989265393,-2.11185533289432,46.7009559128408));
#92937=CARTESIAN_POINT('Ctrl Pts',(1.38522115762505,-2.77794756340749,46.6479342782254));
#92938=CARTESIAN_POINT('Ctrl Pts',(0.419552367709688,-2.91684710004787,
46.59491264361));
#92939=CARTESIAN_POINT('Ctrl Pts',(-0.546116422205564,-3.05574663668823,
46.5418910089947));
#92940=CARTESIAN_POINT('Ctrl Pts',(-1.58761526700728,-2.6674534794559,46.4888693743793));
#92941=CARTESIAN_POINT('Ctrl Pts',(-2.22666536933688,-1.93028036636939,
46.4358477397639));
#92942=CARTESIAN_POINT('Ctrl Pts',(-2.68334600941247,-1.40347865253879,
46.3979571988724));
#92943=CARTESIAN_POINT('Ctrl Pts',(-2.93450103307901,-0.698508241896662,
46.360066657981));
#92944=CARTESIAN_POINT('Ctrl Pts',(-2.94047772160941,0.00261614231624671,
46.3221761170895));
#92945=CARTESIAN_POINT('Ctrl Pts',(-2.94168313190805,0.00271989540251569,
46.1778238829104));
#92946=CARTESIAN_POINT('Ctrl Pts',(-2.93488473602019,-0.738847781346994,
46.2179418682063));
#92947=CARTESIAN_POINT('Ctrl Pts',(-2.65019576255787,-1.48506362719018,
46.2580598535022));
#92948=CARTESIAN_POINT('Ctrl Pts',(-2.14368498174406,-2.02204462993227,
46.2981778387981));
#92949=CARTESIAN_POINT('Ctrl Pts',(-1.47410997593488,-2.73189932927898,
46.3512112612939));
#92950=CARTESIAN_POINT('Ctrl Pts',(-0.416897884315671,-3.07611286016707,
46.4042446837896));
#92951=CARTESIAN_POINT('Ctrl Pts',(0.542258909289073,-2.89655054624969,
46.4572781062854));
#92952=CARTESIAN_POINT('Ctrl Pts',(1.50141570289387,-2.7169882323323,46.5103115287812));
#92953=CARTESIAN_POINT('Ctrl Pts',(2.36251719848426,-2.01365007360937,46.5633449512769));
#92954=CARTESIAN_POINT('Ctrl Pts',(2.72996592922045,-1.10965570941658,46.6163783737727));
#92955=CARTESIAN_POINT('Ctrl Pts',(3.09741465995664,-0.205661345223792,
46.6694117962685));
#92956=CARTESIAN_POINT('Ctrl Pts',(2.97121062583871,0.898989224438765,46.7224452187642));
#92957=CARTESIAN_POINT('Ctrl Pts',(2.40933303563599,1.69680998371491,46.77547864126));
#92958=CARTESIAN_POINT('Ctrl Pts',(1.8474554454333,2.49463074299101,46.8285120637558));
#92959=CARTESIAN_POINT('Ctrl Pts',(0.849904299145825,2.98562169188063,46.8815454862515));
#92960=CARTESIAN_POINT('Ctrl Pts',(-0.125036747405431,2.94421732120279,
46.9345789087473));
#92961=CARTESIAN_POINT('Ctrl Pts',(-1.09997779395669,2.90281295052495,46.987612331243));
#92962=CARTESIAN_POINT('Ctrl Pts',(-2.05230874077178,2.32901326027967,47.0406457537388));
#92963=CARTESIAN_POINT('Ctrl Pts',(-2.54452057223983,1.48642683017747,47.0936791762345));
#92964=CARTESIAN_POINT('Ctrl Pts',(-2.80484081453354,1.04080100484249,47.1217274117932));
#92965=CARTESIAN_POINT('Ctrl Pts',(-2.93646001628066,0.519992184602745,
47.1497756473518));
#92966=CARTESIAN_POINT('Ctrl Pts',(-2.93719707228474,-0.000468378137186533,
47.1778238829104));
#92967=CARTESIAN_POINT('Origin',(0.,0.,0.));
#92968=CARTESIAN_POINT('',(-2.94461792262617,-0.00215304676840083,48.3221761170895));
#92969=CARTESIAN_POINT('',(-2.943409633743,-0.00255526730400832,48.1778238829104));
#92970=CARTESIAN_POINT('',(-2.942,-3.60291088309151E-16,0.));
#92971=CARTESIAN_POINT('Ctrl Pts',(-2.94461792262617,-0.00215304676840083,
48.3221761170895));
#92972=CARTESIAN_POINT('Ctrl Pts',(-2.93763702468649,0.837415355975283,
48.2766379720835));
#92973=CARTESIAN_POINT('Ctrl Pts',(-2.56039370972494,1.68241193941936,48.2310998270776));
#92974=CARTESIAN_POINT('Ctrl Pts',(-1.92629505958697,2.23011593323329,48.1855616820716));
#92975=CARTESIAN_POINT('Ctrl Pts',(-1.18799210646253,2.86782660488176,48.1325400474562));
#92976=CARTESIAN_POINT('Ctrl Pts',(-0.101476823706468,3.10250517619938,
48.0795184128408));
#92977=CARTESIAN_POINT('Ctrl Pts',(0.834231395674201,2.82633006893815,48.0264967782254));
#92978=CARTESIAN_POINT('Ctrl Pts',(1.76993961505482,2.55015496167694,47.97347514361));
#92979=CARTESIAN_POINT('Ctrl Pts',(2.55484077106006,1.76312617583694,47.9204535089946));
#92980=CARTESIAN_POINT('Ctrl Pts',(2.82852682256973,0.826691734777258,47.8674318743793));
#92981=CARTESIAN_POINT('Ctrl Pts',(3.10221287407942,-0.109742706282482,
47.8144102397639));
#92982=CARTESIAN_POINT('Ctrl Pts',(2.86468382109348,-1.19558280256193,47.7613886051485));
#92983=CARTESIAN_POINT('Ctrl Pts',(2.22499948973125,-1.93220149581064,47.7083669705331));
#92984=CARTESIAN_POINT('Ctrl Pts',(1.58531515836902,-2.66882018905935,47.6553453359178));
#92985=CARTESIAN_POINT('Ctrl Pts',(0.543475548630508,-3.05621747927732,
47.6023237013023));
#92986=CARTESIAN_POINT('Ctrl Pts',(-0.422074157754231,-2.91648460887001,
47.5493020666869));
#92987=CARTESIAN_POINT('Ctrl Pts',(-1.38762386413897,-2.77675173846269,
47.4962804320715));
#92988=CARTESIAN_POINT('Ctrl Pts',(-2.27688366716993,-2.10988870743008,
47.4432587974562));
#92989=CARTESIAN_POINT('Ctrl Pts',(-2.68149127232562,-1.2221374454495,47.3902371628408));
#92990=CARTESIAN_POINT('Ctrl Pts',(-2.8546156766408,-0.842284455905961,
47.3675501475904));
#92991=CARTESIAN_POINT('Ctrl Pts',(-2.9390084044044,-0.421990541615868,
47.34486313234));
#92992=CARTESIAN_POINT('Ctrl Pts',(-2.93754881179149,-0.00113833082597881,
47.3221761170895));
#92993=CARTESIAN_POINT('Ctrl Pts',(-2.93719707228474,-0.000468378137186533,
47.1778238829104));
#92994=CARTESIAN_POINT('Ctrl Pts',(-2.93785363700899,-0.464091283267131,
47.2028090698475));
#92995=CARTESIAN_POINT('Ctrl Pts',(-2.8346535013737,-0.9274378415004,47.2277942567846));
#92996=CARTESIAN_POINT('Ctrl Pts',(-2.62605493729491,-1.33711830655687,
47.2527794437218));
#92997=CARTESIAN_POINT('Ctrl Pts',(-2.18328475476092,-2.20670384322986,
47.3058128662175));
#92998=CARTESIAN_POINT('Ctrl Pts',(-1.26565167357192,-2.83450174661667,
47.3588462887133));
#92999=CARTESIAN_POINT('Ctrl Pts',(-0.294724481945897,-2.93209608829399,
47.4118797112091));
#93000=CARTESIAN_POINT('Ctrl Pts',(0.676202709680179,-3.02969042997131,
47.4649131337049));
#93001=CARTESIAN_POINT('Ctrl Pts',(1.70042401174323,-2.59708120993907,47.5179465562006));
#93002=CARTESIAN_POINT('Ctrl Pts',(2.30740370625557,-1.83301311549819,47.5709799786964));
#93003=CARTESIAN_POINT('Ctrl Pts',(2.91438340076788,-1.06894502105736,47.6240134011921));
#93004=CARTESIAN_POINT('Ctrl Pts',(3.10412148772949,0.0265819477921747,
47.6770468236879));
#93005=CARTESIAN_POINT('Ctrl Pts',(2.78944987179727,0.950273740143268,47.7300802461837));
#93006=CARTESIAN_POINT('Ctrl Pts',(2.47477825586507,1.87396553249431,47.7831136686794));
#93007=CARTESIAN_POINT('Ctrl Pts',(1.6556969370392,2.62582214834703,47.8361470911751));
#93008=CARTESIAN_POINT('Ctrl Pts',(0.708500440227379,2.86043317362063,47.8891805136709));
#93009=CARTESIAN_POINT('Ctrl Pts',(-0.238696056584552,3.09504419889426,
47.9422139361667));
#93010=CARTESIAN_POINT('Ctrl Pts',(-1.31400773138241,2.81240963358864,47.9952473586625));
#93011=CARTESIAN_POINT('Ctrl Pts',(-2.023429927351,2.14237611397396,48.0482807811582));
#93012=CARTESIAN_POINT('Ctrl Pts',(-2.60105781678863,1.5968193919164,48.0914618150756));
#93013=CARTESIAN_POINT('Ctrl Pts',(-2.93611593149267,0.794432991729182,
48.134642848993));
#93014=CARTESIAN_POINT('Ctrl Pts',(-2.943409633743,-0.00255526730400832,
48.1778238829104));
#93015=CARTESIAN_POINT('Origin',(0.,0.,-1.84858989190512));
#93016=CARTESIAN_POINT('',(-2.37386048877927,-0.00173572014615222,48.6514101080949));
#93017=CARTESIAN_POINT('',(-2.37475460450346,0.00138119150085991,48.8485898919049));
#93018=CARTESIAN_POINT('',(-2.37175,1.74448693060498E-12,-1.84858989190512));
#93019=CARTESIAN_POINT('',(-2.34668236863858,0.343918483395164,49.62825));
#93020=CARTESIAN_POINT('Ctrl Pts',(-2.37386048877927,-0.00173572014615207,
48.6514101080949));
#93021=CARTESIAN_POINT('Ctrl Pts',(-2.37478532824446,-0.112962957566302,
48.6588935977043));
#93022=CARTESIAN_POINT('Ctrl Pts',(-2.31708772079214,-1.01129619086623,
48.7193987219291));
#93023=CARTESIAN_POINT('Ctrl Pts',(-1.17033730995746,-2.54951603961395,
48.8329254807692));
#93024=CARTESIAN_POINT('Ctrl Pts',(1.51207452279905,-2.36256262295682,48.9919903846154));
#93025=CARTESIAN_POINT('Ctrl Pts',(2.80422967385422,-0.00687846186160384,
49.1510552884616));
#93026=CARTESIAN_POINT('Ctrl Pts',(1.52375565164409,2.35733202978189,49.3101201923077));
#93027=CARTESIAN_POINT('Ctrl Pts',(-1.16201321478499,2.55211054076708,49.4691850961539));
#93028=CARTESIAN_POINT('Ctrl Pts',(-2.23210772954909,1.12570340751462,49.5752283653847));
#93029=CARTESIAN_POINT('Ctrl Pts',(-2.34668236863857,0.343918483395232,
49.62825));
#93030=CARTESIAN_POINT('',(-0.43944522199609,2.33068358199152,49.6282500000002));
#93031=CARTESIAN_POINT('Origin',(0.,0.,49.62825));
#93032=CARTESIAN_POINT('Ctrl Pts',(-2.37475460450346,0.00138119150086006,
48.8485898919049));
#93033=CARTESIAN_POINT('Ctrl Pts',(-2.36985243589685,-0.707780462192968,
48.8963429046203));
#93034=CARTESIAN_POINT('Ctrl Pts',(-1.65515900824388,-2.21309514855009,
48.9971293398314));
#93035=CARTESIAN_POINT('Ctrl Pts',(0.905469678109174,-2.65425291543538,
49.1509491975383));
#93036=CARTESIAN_POINT('Ctrl Pts',(2.72507495425543,-0.67380191912698,49.3100494650256));
#93037=CARTESIAN_POINT('Ctrl Pts',(2.03481676979323,1.92982725944834,49.4691497325128));
#93038=CARTESIAN_POINT('Ctrl Pts',(0.337182413353676,2.47711500076564,49.5752165775044));
#93039=CARTESIAN_POINT('Ctrl Pts',(-0.43944522199609,2.33068358199152,49.6282500000002));
#93040=CARTESIAN_POINT('Origin',(0.,0.,-1.84858989190512));
#93041=CARTESIAN_POINT('',(-2.36816158883972,-0.000917687332811956,47.6514101080949));
#93042=CARTESIAN_POINT('',(-2.37288640340922,-0.00205997798142371,47.8485898919049));
#93043=CARTESIAN_POINT('',(-2.37175,1.74448693060498E-12,-1.84858989190512));
#93044=CARTESIAN_POINT('Ctrl Pts',(-2.36816158883972,-0.000917687332812299,
47.6514101080949));
#93045=CARTESIAN_POINT('Ctrl Pts',(-2.36933826755493,-0.340195807979261,
47.6740971233453));
#93046=CARTESIAN_POINT('Ctrl Pts',(-2.14229982249859,-1.47089603886295,
47.7498057732111));
#93047=CARTESIAN_POINT('Ctrl Pts',(-0.401765792635603,-2.77613641385121,
47.8785360576923));
#93048=CARTESIAN_POINT('Ctrl Pts',(2.11793144842226,-1.83921303886061,48.0376009615385));
#93049=CARTESIAN_POINT('Ctrl Pts',(2.69239732002637,0.78689972288376,48.1966658653846));
#93050=CARTESIAN_POINT('Ctrl Pts',(0.794107738018986,2.69033499428045,48.3557307692309));
#93051=CARTESIAN_POINT('Ctrl Pts',(-1.7100110252374,2.14946546110686,48.5073121834675));
#93052=CARTESIAN_POINT('Ctrl Pts',(-2.36823270336483,0.675098528394528,
48.6058719630889));
#93053=CARTESIAN_POINT('Ctrl Pts',(-2.37386048877927,-0.00173572014615207,
48.6514101080949));
#93054=CARTESIAN_POINT('Ctrl Pts',(-2.37288640340922,-0.00205997798142388,
47.8485898919049));
#93055=CARTESIAN_POINT('Ctrl Pts',(-2.37422800253445,-0.148657510252996,
47.8584422804833));
#93056=CARTESIAN_POINT('Ctrl Pts',(-2.29499082631282,-1.08291398552728,
47.9213280915575));
#93057=CARTESIAN_POINT('Ctrl Pts',(-1.05464278435862,-2.59947119907506,
48.0372473251273));
#93058=CARTESIAN_POINT('Ctrl Pts',(1.61673826111253,-2.29249989126509,48.1963475926147));
#93059=CARTESIAN_POINT('Ctrl Pts',(2.80269451719685,0.120818728651149,48.3554478601019));
#93060=CARTESIAN_POINT('Ctrl Pts',(1.41336773306382,2.42320569438391,48.5145481275892));
#93061=CARTESIAN_POINT('Ctrl Pts',(-1.27435908006578,2.49895924442061,48.6736483950764));
#93062=CARTESIAN_POINT('Ctrl Pts',(-2.33621967799716,0.945246301592545,
48.7849956498484));
#93063=CARTESIAN_POINT('Ctrl Pts',(-2.37529667415695,0.0797985293630277,
48.8433094821245));
#93064=CARTESIAN_POINT('Ctrl Pts',(-2.37475460450346,0.00138119150086006,
48.8485898919049));
#93065=CARTESIAN_POINT('Origin',(0.,0.,-1.84858989190512));
#93066=CARTESIAN_POINT('',(-2.37052278593716,0.00210905354912938,46.6514101080949));
#93067=CARTESIAN_POINT('',(-2.36787802725742,-0.000377592060197274,46.8485898919049));
#93068=CARTESIAN_POINT('',(-2.37175,1.74448693060498E-12,-1.84858989190512));
#93069=CARTESIAN_POINT('Ctrl Pts',(-2.37052278593716,0.00210905354912923,
46.6514101080949));
#93070=CARTESIAN_POINT('Ctrl Pts',(-2.36570456329227,-0.563115881276711,
46.6893006489864));
#93071=CARTESIAN_POINT('Ctrl Pts',(-1.87990249905625,-1.92672022299298,
46.7802128244932));
#93072=CARTESIAN_POINT('Ctrl Pts',(0.399362087284636,-2.7764790554831,46.9241466346154));
#93073=CARTESIAN_POINT('Ctrl Pts',(2.55144402454308,-1.16552978860435,47.0832115384616));
#93074=CARTESIAN_POINT('Ctrl Pts',(2.36016822626022,1.51589220166356,47.2422764423077));
#93075=CARTESIAN_POINT('Ctrl Pts',(0.00121257453600308,2.80505384839945,
47.4013413461539));
#93076=CARTESIAN_POINT('Ctrl Pts',(-2.02224819409324,1.70150941591366,47.5377192347496));
#93077=CARTESIAN_POINT('Ctrl Pts',(-2.36658826151806,0.452728265431197,
47.6210754887299));
#93078=CARTESIAN_POINT('Ctrl Pts',(-2.36816158883972,-0.000917687332812299,
47.6514101080949));
#93079=CARTESIAN_POINT('Ctrl Pts',(-2.36787802725742,-0.000377592060197413,
46.8485898919049));
#93080=CARTESIAN_POINT('Ctrl Pts',(-2.36840732956388,-0.374136132251743,
46.8735750788421));
#93081=CARTESIAN_POINT('Ctrl Pts',(-2.10861752023225,-1.54053686687448,
46.951593688275));
#93082=CARTESIAN_POINT('Ctrl Pts',(-0.280561895474226,-2.79119959037926,
47.0826457202037));
#93083=CARTESIAN_POINT('Ctrl Pts',(2.19652533073393,-1.74493080967452,47.241745987691));
#93084=CARTESIAN_POINT('Ctrl Pts',(2.65540837738748,0.904609729110513,47.4008462551782));
#93085=CARTESIAN_POINT('Ctrl Pts',(0.674453804384293,2.72298083242374,47.5599465226655));
#93086=CARTESIAN_POINT('Ctrl Pts',(-1.7651489471279,2.08175645129611,47.7091944015744));
#93087=CARTESIAN_POINT('Ctrl Pts',(-2.36700644477084,0.640447467076404,
47.8054088579876));
#93088=CARTESIAN_POINT('Ctrl Pts',(-2.37288640340922,-0.00205997798142388,
47.8485898919049));
#93089=CARTESIAN_POINT('Origin',(0.,0.,-1.84858989190512));
#93090=CARTESIAN_POINT('',(-2.3756729420957,-2.02395829644482E-5,45.6514101080949));
#93091=CARTESIAN_POINT('',(-2.37149455068082,0.00219269610015983,45.8485898919049));
#93092=CARTESIAN_POINT('',(-2.37175,1.74448693060498E-12,-1.84858989190512));
#93093=CARTESIAN_POINT('Ctrl Pts',(-2.37567285728959,-2.02391454256733E-5,
45.6514101080949));
#93094=CARTESIAN_POINT('Ctrl Pts',(-2.37567299246115,-0.00109466926018251,
45.651482540012));
#93095=CARTESIAN_POINT('Ctrl Pts',(-2.37518507362446,-0.788673641534315,
45.7045766065445));
#93096=CARTESIAN_POINT('Ctrl Pts',(-1.51368914530336,-2.36158227765018,
45.8106923076923));
#93097=CARTESIAN_POINT('Ctrl Pts',(1.16791059373771,-2.55035498271459,45.9697572115385));
#93098=CARTESIAN_POINT('Ctrl Pts',(2.77685048729278,-0.396770815138777,
46.1288221153846));
#93099=CARTESIAN_POINT('Ctrl Pts',(1.83541018417072,2.12122490443972,46.2878870192308));
#93100=CARTESIAN_POINT('Ctrl Pts',(-0.791750582632343,2.69099549234209,
46.446951923077));
#93101=CARTESIAN_POINT('Ctrl Pts',(-2.23914207963376,1.24225257134515,46.5681262860316));
#93102=CARTESIAN_POINT('Ctrl Pts',(-2.3724468803604,0.227824265386368,46.636279014371));
#93103=CARTESIAN_POINT('Ctrl Pts',(-2.37052278593716,0.00210905354912923,
46.6514101080949));
#93104=CARTESIAN_POINT('Ctrl Pts',(-2.37149455068082,0.00219269610015994,
45.8485898919049));
#93105=CARTESIAN_POINT('Ctrl Pts',(-2.36601389281351,-0.595636378451926,
45.8887078772009));
#93106=CARTESIAN_POINT('Ctrl Pts',(-1.83311208298173,-1.99245821506647,
45.9818592849926));
#93107=CARTESIAN_POINT('Ctrl Pts',(0.516201638739318,-2.75736203874416,
46.12804411528));
#93108=CARTESIAN_POINT('Ctrl Pts',(2.59878233775354,-1.05633320330836,46.2871443827674));
#93109=CARTESIAN_POINT('Ctrl Pts',(2.29355689460039,1.61527283537019,46.4462446502545));
#93110=CARTESIAN_POINT('Ctrl Pts',(-0.119028351361985,2.80273828373448,
46.6053449177419));
#93111=CARTESIAN_POINT('Ctrl Pts',(-2.06054937610219,1.63293049125855,46.7394599982919));
#93112=CARTESIAN_POINT('Ctrl Pts',(-2.36728383535441,0.419201721222213,
46.8205416563463));
#93113=CARTESIAN_POINT('Ctrl Pts',(-2.36787802725742,-0.000377592060197413,
46.8485898919049));
#93114=CARTESIAN_POINT('Origin',(0.,0.,-1.84858989190512));
#93115=CARTESIAN_POINT('',(-2.37046196519616,-0.00209881642975521,44.6514101080949));
#93116=CARTESIAN_POINT('',(-2.37548760150362,-0.000610301136611813,44.848589891905));
#93117=CARTESIAN_POINT('',(-2.37175,1.74448693060498E-12,-1.84858989190512));
#93118=CARTESIAN_POINT('Ctrl Pts',(-2.37046196519616,-0.00209881642975512,
44.6514101080949));
#93119=CARTESIAN_POINT('Ctrl Pts',(-2.37239133277476,-0.229989821189002,
44.666686065653));
#93120=CARTESIAN_POINT('Ctrl Pts',(-2.23747667874047,-1.24663494975249,
44.7349836578265));
#93121=CARTESIAN_POINT('Ctrl Pts',(-0.784399570615147,-2.69314741578982,
44.8563028846154));
#93122=CARTESIAN_POINT('Ctrl Pts',(1.84119559845759,-2.11620520221519,45.0153677884616));
#93123=CARTESIAN_POINT('Ctrl Pts',(2.7757567025159,0.404351850010035,45.1744326923077));
#93124=CARTESIAN_POINT('Ctrl Pts',(1.16094220248601,2.55353458782659,45.3334975961539));
#93125=CARTESIAN_POINT('Ctrl Pts',(-1.5189112200628,2.35752946495471,45.4924900680829));
#93126=CARTESIAN_POINT('Ctrl Pts',(-2.37557404413184,0.785409999391494,
45.5984609053966));
#93127=CARTESIAN_POINT('Ctrl Pts',(-2.37567285728959,-2.02391454256733E-5,
45.6514101080949));
#93128=CARTESIAN_POINT('Ctrl Pts',(-2.37548760150362,-0.000610301136611548,
44.848589891905));
#93129=CARTESIAN_POINT('Ctrl Pts',(-2.37560059199193,-0.0335087620399993,
44.8508072530639));
#93130=CARTESIAN_POINT('Ctrl Pts',(-2.3600516655157,-0.85314228325878,44.9060580367186));
#93131=CARTESIAN_POINT('Ctrl Pts',(-1.41656571057567,-2.42133250781507,
45.014342242869));
#93132=CARTESIAN_POINT('Ctrl Pts',(1.27124832670454,-2.50068734913707,45.1734425103564));
#93133=CARTESIAN_POINT('Ctrl Pts',(2.79101740943663,-0.282367393789022,
45.3325427778436));
#93134=CARTESIAN_POINT('Ctrl Pts',(1.74635141434428,2.19539660735637,45.4916430453309));
#93135=CARTESIAN_POINT('Ctrl Pts',(-0.902892471930827,2.65599222758591,
45.6507433128183));
#93136=CARTESIAN_POINT('Ctrl Pts',(-2.26370846509963,1.17542736851982,45.7697255950095));
#93137=CARTESIAN_POINT('Ctrl Pts',(-2.3732589735943,0.194655598004337,45.8356744547051));
#93138=CARTESIAN_POINT('Ctrl Pts',(-2.37149455068082,0.00219269610015994,
45.8485898919049));
#93139=CARTESIAN_POINT('Origin',(0.,0.,-1.84858989190512));
#93140=CARTESIAN_POINT('',(-2.36818767449352,0.000950664291755352,43.6514101080949));
#93141=CARTESIAN_POINT('',(-2.36964188313267,-0.00189296896605684,43.8485898919049));
#93142=CARTESIAN_POINT('',(-2.37175,1.74448693060498E-12,-1.84858989190512));
#93143=CARTESIAN_POINT('Ctrl Pts',(-2.36818767449352,0.000950664291755263,
43.6514101080949));
#93144=CARTESIAN_POINT('Ctrl Pts',(-2.36654953412987,-0.454849638172114,
43.681889591294));
#93145=CARTESIAN_POINT('Ctrl Pts',(-2.01974604676808,-1.70585947988162,
43.7653907091086));
#93146=CARTESIAN_POINT('Ctrl Pts',(0.00887142432873881,-2.80503956968683,
43.9019134615385));
#93147=CARTESIAN_POINT('Ctrl Pts',(2.36429909693514,-1.50944210551781,44.0609783653846));
#93148=CARTESIAN_POINT('Ctrl Pts',(2.54825171469771,1.17249259623757,44.2200432692308));
#93149=CARTESIAN_POINT('Ctrl Pts',(0.391779197956932,2.77755913523241,44.3791081730769));
#93150=CARTESIAN_POINT('Ctrl Pts',(-1.88286501107497,1.92244128703405,44.522897119365));
#93151=CARTESIAN_POINT('Ctrl Pts',(-2.36569465124747,0.56100174451135,44.6136644310376));
#93152=CARTESIAN_POINT('Ctrl Pts',(-2.37046196519616,-0.00209881642975512,
44.6514101080949));
#93153=CARTESIAN_POINT('Ctrl Pts',(-2.36964188313267,-0.00189296896605656,
43.8485898919049));
#93154=CARTESIAN_POINT('Ctrl Pts',(-2.37156978341398,-0.260953726706908,
43.8659400514226));
#93155=CARTESIAN_POINT('Ctrl Pts',(-2.21281240035297,-1.30957565229906,
43.9363236334361));
#93156=CARTESIAN_POINT('Ctrl Pts',(-0.677977057200952,-2.72210518454085,
44.0597406379455));
#93157=CARTESIAN_POINT('Ctrl Pts',(1.92355860205693,-2.04191866396806,44.2188409054326));
#93158=CARTESIAN_POINT('Ctrl Pts',(2.75769534156078,0.514418048784537,44.37794117292));
#93159=CARTESIAN_POINT('Ctrl Pts',(1.05801389510723,2.59809855924461,44.5370414404072));
#93160=CARTESIAN_POINT('Ctrl Pts',(-1.57655242741681,2.29883097463275,44.6939243467356));
#93161=CARTESIAN_POINT('Ctrl Pts',(-2.37289815793857,0.753335532361604,
44.7977738305682));
#93162=CARTESIAN_POINT('Ctrl Pts',(-2.37548760150362,-0.000610301136611548,
44.848589891905));
#93163=CARTESIAN_POINT('Origin',(0.,0.,-1.84858989190512));
#93164=CARTESIAN_POINT('',(-2.37395592879609,0.00174106614345369,42.6514101080949));
#93165=CARTESIAN_POINT('',(-2.36862507619379,0.00137154188862718,42.848589891905));
#93166=CARTESIAN_POINT('',(-2.37175,1.74448693060498E-12,-1.84858989190512));
#93167=CARTESIAN_POINT('Ctrl Pts',(-2.37395592879609,0.00174106614345361,
42.6514101080949));
#93168=CARTESIAN_POINT('Ctrl Pts',(-2.3683671883622,-0.677199472088916,
42.697093116935));
#93169=CARTESIAN_POINT('Ctrl Pts',(-1.70647264490752,-2.15366004211859,
42.7957977603907));
#93170=CARTESIAN_POINT('Ctrl Pts',(0.801418800438249,-2.68813199006011,
42.9475240384615));
#93171=CARTESIAN_POINT('Ctrl Pts',(2.69455290827499,-0.779557768345067,
43.1065889423078));
#93172=CARTESIAN_POINT('Ctrl Pts',(2.11289250645387,1.84499619128384,43.2656538461538));
#93173=CARTESIAN_POINT('Ctrl Pts',(-0.409340210132954,2.7750254561082,43.4247187500001));
#93174=CARTESIAN_POINT('Ctrl Pts',(-2.14435471179428,1.46651574667853,43.553304170647));
#93175=CARTESIAN_POINT('Ctrl Pts',(-2.36939921761179,0.33805347428917,43.6288679566786));
#93176=CARTESIAN_POINT('Ctrl Pts',(-2.36818767449352,0.000950664291755263,
43.6514101080949));
#93177=CARTESIAN_POINT('Ctrl Pts',(-2.36862507619379,0.00137154188862704,
42.848589891905));
#93178=CARTESIAN_POINT('Ctrl Pts',(-2.36607991989796,-0.484164893157661,
42.8810728497815));
#93179=CARTESIAN_POINT('Ctrl Pts',(-1.98421738068972,-1.76608856648426,
42.9665892301537));
#93180=CARTESIAN_POINT('Ctrl Pts',(0.11540256956664,-2.80288989664852,43.1051390330218));
#93181=CARTESIAN_POINT('Ctrl Pts',(2.42041575832236,-1.41813154631793,43.2642393005089));
#93182=CARTESIAN_POINT('Ctrl Pts',(2.50150907688241,1.26963060142386,43.4233395679963));
#93183=CARTESIAN_POINT('Ctrl Pts',(0.284172581298068,2.79083418888245,43.5824398354835));
#93184=CARTESIAN_POINT('Ctrl Pts',(-1.92398851613373,1.86151888529159,43.7241899434532));
#93185=CARTESIAN_POINT('Ctrl Pts',(-2.36567686064033,0.530905195587278,
43.8129066289269));
#93186=CARTESIAN_POINT('Ctrl Pts',(-2.36964188313267,-0.00189296896605656,
43.8485898919049));
#93187=CARTESIAN_POINT('Origin',(0.,0.,-1.84858989190512));
#93188=CARTESIAN_POINT('',(-2.37374189642354,-0.00182254589935643,41.6514101080949));
#93189=CARTESIAN_POINT('',(-2.37466860212234,0.00138350872013287,41.848589891905));
#93190=CARTESIAN_POINT('',(-2.37175,1.74448693060498E-12,-1.84858989190512));
#93191=CARTESIAN_POINT('Ctrl Pts',(-2.37374189642354,-0.0018225458993563,
41.6514101080949));
#93192=CARTESIAN_POINT('Ctrl Pts',(-2.37473518999418,-0.118738074680971,
41.6592750079607));
#93193=CARTESIAN_POINT('Ctrl Pts',(-2.31366732775003,-1.02280417077909,
41.7201615424419));
#93194=CARTESIAN_POINT('Ctrl Pts',(-1.15175551301023,-2.55769132772724,
41.8340697115385));
#93195=CARTESIAN_POINT('Ctrl Pts',(1.52859654328181,-2.35196052210647,41.9931346153846));
#93196=CARTESIAN_POINT('Ctrl Pts',(2.8050190938,0.0139130549425746,42.1521995192308));
#93197=CARTESIAN_POINT('Ctrl Pts',(1.50519018846317,2.36700827760163,42.311264423077));
#93198=CARTESIAN_POINT('Ctrl Pts',(-1.17707080902522,2.54614021613523,42.4703293269231));
#93199=CARTESIAN_POINT('Ctrl Pts',(-2.3184019631086,1.00694689508425,42.5837112219291));
#93200=CARTESIAN_POINT('Ctrl Pts',(-2.37485371717826,0.11080766793254,42.6440714823197));
#93201=CARTESIAN_POINT('Ctrl Pts',(-2.37395592879609,0.00174106614345361,
42.6514101080949));
#93202=CARTESIAN_POINT('Ctrl Pts',(-2.37466860212234,0.00138350872013286,
41.848589891905));
#93203=CARTESIAN_POINT('Ctrl Pts',(-2.36977376777603,-0.705725647118399,
41.8962056481402));
#93204=CARTESIAN_POINT('Ctrl Pts',(-1.65899852223576,-2.2089365118431,41.9968548268713));
#93205=CARTESIAN_POINT('Ctrl Pts',(0.899455893833502,-2.65715799696691,
42.1505374280981));
#93206=CARTESIAN_POINT('Ctrl Pts',(2.72166609558782,-0.679737589018599,
42.3096376955853));
#93207=CARTESIAN_POINT('Ctrl Pts',(2.04316240585326,1.92223747469062,42.4687379630726));
#93208=CARTESIAN_POINT('Ctrl Pts',(-0.512634247617058,2.75802749333056,
42.6278382305599));
#93209=CARTESIAN_POINT('Ctrl Pts',(-2.17177139308421,1.40643705594649,42.7544555401707));
#93210=CARTESIAN_POINT('Ctrl Pts',(-2.37023527883011,0.308547980922129,
42.8280394272857));
#93211=CARTESIAN_POINT('Ctrl Pts',(-2.36862507619379,0.00137154188862704,
42.848589891905));
#93212=CARTESIAN_POINT('Origin',(0.,0.,-1.84858989190512));
#93213=CARTESIAN_POINT('',(-2.36809936427644,-0.000831359809205589,40.6514101080949));
#93214=CARTESIAN_POINT('',(-2.37294614192107,-0.00204842308417053,40.848589891905));
#93215=CARTESIAN_POINT('',(-2.37175,1.74448693060498E-12,-1.84858989190512));
#93216=CARTESIAN_POINT('Ctrl Pts',(-2.36809936427644,-0.000831359809205547,
40.6514101080949));
#93217=CARTESIAN_POINT('Ctrl Pts',(-2.36918130165799,-0.345836370295785,
40.6744785336017));
#93218=CARTESIAN_POINT('Ctrl Pts',(-2.13685539616662,-1.48243054976489,
40.750568593724));
#93219=CARTESIAN_POINT('Ctrl Pts',(-0.381792176989602,-2.77894951794198,
40.8796802884616));
#93220=CARTESIAN_POINT('Ctrl Pts',(2.13109066828147,-1.82394579229869,41.0387451923077));
#93221=CARTESIAN_POINT('Ctrl Pts',(2.68668721598173,0.806249026765786,41.1978100961539));
#93222=CARTESIAN_POINT('Ctrl Pts',(0.774713447708398,2.69594969604779,41.356875));
#93223=CARTESIAN_POINT('Ctrl Pts',(-1.71907271573948,2.13856614449093,41.5080750039804));
#93224=CARTESIAN_POINT('Ctrl Pts',(-2.36803884933291,0.669454089705716,
41.6062533733453));
#93225=CARTESIAN_POINT('Ctrl Pts',(-2.37374189642354,-0.0018225458993563,
41.6514101080949));
#93226=CARTESIAN_POINT('Ctrl Pts',(-2.37294614192107,-0.00204842308417049,
40.848589891905));
#93227=CARTESIAN_POINT('Ctrl Pts',(-2.37426493662659,-0.1465940308283,40.8583050240033));
#93228=CARTESIAN_POINT('Ctrl Pts',(-2.29631986144691,-1.07877289148818,
40.9210535785973));
#93229=CARTESIAN_POINT('Ctrl Pts',(-1.0613739399866,-2.59672772645004,41.036835555687));
#93230=CARTESIAN_POINT('Ctrl Pts',(1.6108193483455,-2.29668686433149,41.1959358231744));
#93231=CARTESIAN_POINT('Ctrl Pts',(2.80296395340346,0.113589619763061,41.3550360906616));
#93232=CARTESIAN_POINT('Ctrl Pts',(1.41969678881716,2.41949799620072,41.514136358149));
#93233=CARTESIAN_POINT('Ctrl Pts',(-1.2680123450661,2.50232975815682,41.6732366256362));
#93234=CARTESIAN_POINT('Ctrl Pts',(-2.33495267914215,0.949290687493702,
41.7847211368882));
#93235=CARTESIAN_POINT('Ctrl Pts',(-2.37522553077338,0.0818375793671154,
41.8431722256445));
#93236=CARTESIAN_POINT('Ctrl Pts',(-2.37466860212234,0.00138350872013286,
41.848589891905));
#93237=CARTESIAN_POINT('Origin',(0.,0.,-1.84858989190512));
#93238=CARTESIAN_POINT('',(-2.37068477736474,0.00213317277161283,39.6514101080949));
#93239=CARTESIAN_POINT('',(-2.36788813682339,-0.000411074629237396,39.8485898919049));
#93240=CARTESIAN_POINT('',(-2.37175,1.74448693060498E-12,-1.84858989190512));
#93241=CARTESIAN_POINT('Ctrl Pts',(-2.37068477736474,0.00213317277161312,
39.6514101080949));
#93242=CARTESIAN_POINT('Ctrl Pts',(-2.36573670528941,-0.568682495493336,
39.6896820592428));
#93243=CARTESIAN_POINT('Ctrl Pts',(-1.87205793886815,-1.93797744307223,
39.780975645006));
#93244=CARTESIAN_POINT('Ctrl Pts',(0.419312947294725,-2.77353607186051,
39.9252908653846));
#93245=CARTESIAN_POINT('Ctrl Pts',(2.55975730711914,-1.14715657969204,40.0843557692308));
#93246=CARTESIAN_POINT('Ctrl Pts',(2.34920929627571,1.53282137640764,40.243420673077));
#93247=CARTESIAN_POINT('Ctrl Pts',(-0.0189546406110363,2.80498955635841,
40.4024855769231));
#93248=CARTESIAN_POINT('Ctrl Pts',(-2.02879098398741,1.6900544618181,40.5384820552624));
#93249=CARTESIAN_POINT('Ctrl Pts',(-2.36669452212011,0.447140575662978,
40.6214568989864));
#93250=CARTESIAN_POINT('Ctrl Pts',(-2.36809936427644,-0.000831359809205547,
40.6514101080949));
#93251=CARTESIAN_POINT('Ctrl Pts',(-2.36788813682339,-0.000411074629237465,
39.848589891905));
#93252=CARTESIAN_POINT('Ctrl Pts',(-2.36846131194098,-0.372112408727876,
39.873437822362));
#93253=CARTESIAN_POINT('Ctrl Pts',(-2.11068491643285,-1.5363911068291,39.9513191753148));
#93254=CARTESIAN_POINT('Ctrl Pts',(-0.287782598693457,-2.79046424483211,
40.0822339507635));
#93255=CARTESIAN_POINT('Ctrl Pts',(2.19200382528608,-1.7506081102658,40.2413342182507));
#93256=CARTESIAN_POINT('Ctrl Pts',(2.65773921450559,0.897737040271954,40.400434485738));
#93257=CARTESIAN_POINT('Ctrl Pts',(0.681497836463564,2.72122586800371,40.5595347532253));
#93258=CARTESIAN_POINT('Ctrl Pts',(-1.76200449819908,2.0857339556845,40.7089198886142));
#93259=CARTESIAN_POINT('Ctrl Pts',(-2.36706583772652,0.642458367826052,
40.8052716015075));
#93260=CARTESIAN_POINT('Ctrl Pts',(-2.37294614192107,-0.00204842308417049,
40.848589891905));
#93261=CARTESIAN_POINT('Origin',(0.,0.,-1.84858989190512));
#93262=CARTESIAN_POINT('',(-2.37566466528284,-0.000126726877739107,38.6514101080949));
#93263=CARTESIAN_POINT('',(-2.37143269814177,0.00219190441036694,38.8485898919049));
#93264=CARTESIAN_POINT('',(-2.37175,1.74448693060498E-12,-1.84858989190512));
#93265=CARTESIAN_POINT('Ctrl Pts',(-2.37566466528284,-0.000126726877739423,
38.6514101080949));
#93266=CARTESIAN_POINT('Ctrl Pts',(-2.37566986853005,-0.00685892807482193,
38.6518639502684));
#93267=CARTESIAN_POINT('Ctrl Pts',(-2.37259066578177,-0.800098223903023,
38.7053394270573));
#93268=CARTESIAN_POINT('Ctrl Pts',(-1.49667178065217,-2.37240369049618,
38.8118365384616));
#93269=CARTESIAN_POINT('Ctrl Pts',(1.18621581231896,-2.54189255010612,38.9709014423077));
#93270=CARTESIAN_POINT('Ctrl Pts',(2.77963124440541,-0.376796808380384,
39.1299663461539));
#93271=CARTESIAN_POINT('Ctrl Pts',(1.82011252500328,2.13436549962901,39.28903125));
#93272=CARTESIAN_POINT('Ctrl Pts',(-0.811076648523027,2.68523376261753,
39.4480961538463));
#93273=CARTESIAN_POINT('Ctrl Pts',(-2.24349225668707,1.23071521996542,39.5688891065444));
#93274=CARTESIAN_POINT('Ctrl Pts',(-2.37259172212968,0.222120661590212,
39.6366604246274));
#93275=CARTESIAN_POINT('Ctrl Pts',(-2.37068477736474,0.00213317277161312,
39.6514101080949));
#93276=CARTESIAN_POINT('Ctrl Pts',(-2.37143269814177,0.00219190441036694,
38.8485898919049));
#93277=CARTESIAN_POINT('Ctrl Pts',(-2.3659851360241,-0.593631435472327,
38.8885706207208));
#93278=CARTESIAN_POINT('Ctrl Pts',(-1.83605691347221,-1.98843277321527,
38.9815847720324));
#93279=CARTESIAN_POINT('Ctrl Pts',(0.509066002639091,-2.75868833519739,
39.1276323458398));
#93280=CARTESIAN_POINT('Ctrl Pts',(2.5960406803649,-1.06305329672964,39.286732613327));
#93281=CARTESIAN_POINT('Ctrl Pts',(2.29772827133774,1.60933350082956,39.4458328808143));
#93282=CARTESIAN_POINT('Ctrl Pts',(-0.111776622438346,2.80303683751629,
39.6049331483016));
#93283=CARTESIAN_POINT('Ctrl Pts',(-2.05830785667968,1.63706408555562,39.7391854853318));
#93284=CARTESIAN_POINT('Ctrl Pts',(-2.3672379731109,0.42121699661448,39.8204043998662));
#93285=CARTESIAN_POINT('Ctrl Pts',(-2.36788813682339,-0.000411074629237465,
39.848589891905));
#93286=CARTESIAN_POINT('Origin',(0.,0.,-1.84858989190512));
#93287=CARTESIAN_POINT('',(-2.37030381846627,-0.00206907782623366,37.6514101080949));
#93288=CARTESIAN_POINT('',(-2.37550954347348,-0.000573603921870391,37.848589891905));
#93289=CARTESIAN_POINT('',(-2.37175,1.74448693060498E-12,-1.84858989190512));
#93290=CARTESIAN_POINT('Ctrl Pts',(-2.37030381846627,-0.00206907782623399,
37.6514101080949));
#93291=CARTESIAN_POINT('Ctrl Pts',(-2.37224375248416,-0.235689518460821,
37.6670674759094));
#93292=CARTESIAN_POINT('Ctrl Pts',(-2.23305719905348,-1.25817407212943,
37.7357464783394));
#93293=CARTESIAN_POINT('Ctrl Pts',(-0.765017314006785,-2.69871713948505,
37.8574471153846));
#93294=CARTESIAN_POINT('Ctrl Pts',(1.8563621592982,-2.10291350825614,38.0165120192308));
#93295=CARTESIAN_POINT('Ctrl Pts',(2.77277793875275,0.424297292056489,38.175576923077));
#93296=CARTESIAN_POINT('Ctrl Pts',(1.14255394050895,2.56181501726957,38.3346418269231));
#93297=CARTESIAN_POINT('Ctrl Pts',(-1.5293958672604,2.34706495701738,38.4932528885958));
#93298=CARTESIAN_POINT('Ctrl Pts',(-2.37506198171684,0.77965306411788,38.598842315653));
#93299=CARTESIAN_POINT('Ctrl Pts',(-2.37566466528284,-0.000126726877739423,
38.6514101080949));
#93300=CARTESIAN_POINT('Ctrl Pts',(-2.37550954347348,-0.000573603921870361,
37.848589891905));
#93301=CARTESIAN_POINT('Ctrl Pts',(-2.3756097420714,-0.031434860913138,
37.8506699965838));
#93302=CARTESIAN_POINT('Ctrl Pts',(-2.3610602581339,-0.849024312195104,
37.9057835237585));
#93303=CARTESIAN_POINT('Ctrl Pts',(-1.42282549133698,-2.4176594356937,38.0139304734288));
#93304=CARTESIAN_POINT('Ctrl Pts',(1.26477424157903,-2.50396797975438,38.1730307409161));
#93305=CARTESIAN_POINT('Ctrl Pts',(2.79027752164898,-0.289587427174506,
38.3321310084034));
#93306=CARTESIAN_POINT('Ctrl Pts',(1.75202554503676,2.1908710631472,38.4912312758906));
#93307=CARTESIAN_POINT('Ctrl Pts',(-0.896017811135028,2.6583193201581,38.650331543378));
#93308=CARTESIAN_POINT('Ctrl Pts',(-2.26223403332359,1.17957625462007,38.7694510820493));
#93309=CARTESIAN_POINT('Ctrl Pts',(-2.37321118897298,0.196713109330291,
38.835537198225));
#93310=CARTESIAN_POINT('Ctrl Pts',(-2.37143269814177,0.00219190441036694,
38.8485898919049));
#93311=CARTESIAN_POINT('Origin',(0.,0.,-1.84858989190512));
#93312=CARTESIAN_POINT('',(-2.36825910754817,0.00103510087933,36.6514101080949));
#93313=CARTESIAN_POINT('',(-2.36969280013257,-0.00191020411530018,36.848589891905));
#93314=CARTESIAN_POINT('',(-2.37175,1.74448693060498E-12,-1.84858989190512));
#93315=CARTESIAN_POINT('Ctrl Pts',(-2.36825910754817,0.00103510087932999,
36.6514101080949));
#93316=CARTESIAN_POINT('Ctrl Pts',(-2.3664500239851,-0.460434164028738,
36.6822710015504));
#93317=CARTESIAN_POINT('Ctrl Pts',(-2.01311920287128,-1.71730605118079,
36.7661535296214));
#93318=CARTESIAN_POINT('Ctrl Pts',(0.0290376119636847,-2.8049032972229,
36.9030576923078));
#93319=CARTESIAN_POINT('Ctrl Pts',(2.37508990529535,-1.49240531741365,37.0621225961539));
#93320=CARTESIAN_POINT('Ctrl Pts',(2.53975639635982,1.19078257328104,37.2211875));
#93321=CARTESIAN_POINT('Ctrl Pts',(0.371800222537135,2.78030399132932,37.3802524038462));
#93322=CARTESIAN_POINT('Ctrl Pts',(-1.89062026807677,1.91116660406184,37.5236599398778));
#93323=CARTESIAN_POINT('Ctrl Pts',(-2.36567441887122,0.555435643107899,
37.6140458412941));
#93324=CARTESIAN_POINT('Ctrl Pts',(-2.37030381846627,-0.00206907782623399,
37.6514101080949));
#93325=CARTESIAN_POINT('Ctrl Pts',(-2.36969280013257,-0.00191020411530039,
36.848589891905));
#93326=CARTESIAN_POINT('Ctrl Pts',(-2.37162565500284,-0.258907628242798,
36.8658027949426));
#93327=CARTESIAN_POINT('Ctrl Pts',(-2.21449028033011,-1.30542157081352,
36.936049120476));
#93328=CARTESIAN_POINT('Ctrl Pts',(-0.685017475287161,-2.72034199768123,
37.0593288685051));
#93329=CARTESIAN_POINT('Ctrl Pts',(1.91826926971012,-2.04688850079404,37.2184291359924));
#93330=CARTESIAN_POINT('Ctrl Pts',(2.75901702502127,0.507281560319236,37.3775294034797));
#93331=CARTESIAN_POINT('Ctrl Pts',(1.06473220873587,2.59535254820565,37.536629670967));
#93332=CARTESIAN_POINT('Ctrl Pts',(-1.57290521304256,2.30264630586829,37.6936498337753));
#93333=CARTESIAN_POINT('Ctrl Pts',(-2.37305512324333,0.755390002953853,
37.7976365740881));
#93334=CARTESIAN_POINT('Ctrl Pts',(-2.37550954347348,-0.000573603921870361,
37.848589891905));
#93335=CARTESIAN_POINT('Origin',(0.,0.,-1.84858989190512));
#93336=CARTESIAN_POINT('',(-2.37410637778804,0.00167730819971897,35.6514101080949));
#93337=CARTESIAN_POINT('',(-2.36858962871103,0.00134465207171072,35.848589891905));
#93338=CARTESIAN_POINT('',(-2.37175,1.74448693060498E-12,-1.84858989190512));
#93339=CARTESIAN_POINT('Ctrl Pts',(-2.37410637778804,0.00167730819971894,
35.6514101080949));
#93340=CARTESIAN_POINT('Ctrl Pts',(-2.36862023067477,-0.682818557534048,
35.6974745271915));
#93341=CARTESIAN_POINT('Ctrl Pts',(-1.69725896922413,-2.16457461681033,
35.7965605809035));
#93342=CARTESIAN_POINT('Ctrl Pts',(0.820724015952912,-2.68230083684112,
35.9486682692308));
#93343=CARTESIAN_POINT('Ctrl Pts',(2.70008778620931,-0.760165532265031,
36.107733173077));
#93344=CARTESIAN_POINT('Ctrl Pts',(2.09957357433953,1.86013883772571,36.2667980769231));
#93345=CARTESIAN_POINT('Ctrl Pts',(-0.429280266134804,2.77201084824496,
36.4258629807693));
#93346=CARTESIAN_POINT('Ctrl Pts',(-2.14972422622322,1.45497952790296,36.5540669911599));
#93347=CARTESIAN_POINT('Ctrl Pts',(-2.36955818311237,0.332409205377294,
36.6292493669351));
#93348=CARTESIAN_POINT('Ctrl Pts',(-2.36825910754817,0.00103510087932999,
36.6514101080949));
#93349=CARTESIAN_POINT('Ctrl Pts',(-2.36858962871103,0.00134465207171076,
35.848589891905));
#93350=CARTESIAN_POINT('Ctrl Pts',(-2.36610713128963,-0.482158267059727,
35.8809355933014));
#93351=CARTESIAN_POINT('Ctrl Pts',(-1.98670264463906,-1.76198154825171,
35.9663147171935));
#93352=CARTESIAN_POINT('Ctrl Pts',(0.108150488259582,-2.80317908769424,
36.1047272635815));
#93353=CARTESIAN_POINT('Ctrl Pts',(2.41673863807743,-1.42438895004866,36.2638275310687));
#93354=CARTESIAN_POINT('Ctrl Pts',(2.50478551939227,1.26315439580437,36.422927798556));
#93355=CARTESIAN_POINT('Ctrl Pts',(0.291392134504392,2.79008963113125,36.5820280660433));
#93356=CARTESIAN_POINT('Ctrl Pts',(-1.92130639744127,1.86559611804953,36.723915430493));
#93357=CARTESIAN_POINT('Ctrl Pts',(-2.36567047656874,0.532908426508661,
36.8127693724468));
#93358=CARTESIAN_POINT('Ctrl Pts',(-2.36969280013257,-0.00191020411530039,
36.848589891905));
#93359=CARTESIAN_POINT('Origin',(0.,0.,-1.84858989190512));
#93360=CARTESIAN_POINT('',(-2.37358262552183,-0.00187676788449481,34.6514101080949));
#93361=CARTESIAN_POINT('',(-2.37462230926531,0.00141218416469555,34.848589891905));
#93362=CARTESIAN_POINT('',(-2.37175,1.74448693060498E-12,-1.84858989190512));
#93363=CARTESIAN_POINT('Ctrl Pts',(-2.37358262552183,-0.0018767678844951,
34.6514101080949));
#93364=CARTESIAN_POINT('Ctrl Pts',(-2.37464472099243,-0.12448352171728,
34.6596564182171));
#93365=CARTESIAN_POINT('Ctrl Pts',(-2.31018163025135,-1.0343001918437,34.7209243629547));
#93366=CARTESIAN_POINT('Ctrl Pts',(-1.13333760403503,-2.56590560328329,
34.8352139423077));
#93367=CARTESIAN_POINT('Ctrl Pts',(1.54546611079131,-2.34091012003366,34.9942788461539));
#93368=CARTESIAN_POINT('Ctrl Pts',(2.80484657580764,0.0340789650750163,
35.15334375));
#93369=CARTESIAN_POINT('Ctrl Pts',(1.48813403299161,2.37776844741717,35.3124086538462));
#93370=CARTESIAN_POINT('Ctrl Pts',(-1.1953454874454,2.53761203798461,35.4714735576924));
#93371=CARTESIAN_POINT('Ctrl Pts',(-2.32177929342658,0.99545829170247,35.5844740424419));
#93372=CARTESIAN_POINT('Ctrl Pts',(-2.37493496324691,0.105058298409406,
35.6444528925761));
#93373=CARTESIAN_POINT('Ctrl Pts',(-2.37410637778804,0.00167730819971894,
35.6514101080949));
#93374=CARTESIAN_POINT('Ctrl Pts',(-2.37462230926531,0.00141218416469564,
34.848589891905));
#93375=CARTESIAN_POINT('Ctrl Pts',(-2.36966193302837,-0.703694807005961,
34.8960683916601));
#93376=CARTESIAN_POINT('Ctrl Pts',(-1.66242402158611,-2.20504314783441,
34.9965803139111));
#93377=CARTESIAN_POINT('Ctrl Pts',(0.892578229012262,-2.65947619483432,
35.1501256586578));
#93378=CARTESIAN_POINT('Ctrl Pts',(2.71989835531262,-0.686776865193377,
35.3092259261451));
#93379=CARTESIAN_POINT('Ctrl Pts',(2.04812882046954,1.91694492893226,35.4683261936323));
#93380=CARTESIAN_POINT('Ctrl Pts',(-0.505496905774109,2.75934456058861,
35.6274264611197));
#93381=CARTESIAN_POINT('Ctrl Pts',(-2.16992769404118,1.41059069964949,35.7541810272105));
#93382=CARTESIAN_POINT('Ctrl Pts',(-2.37017738881721,0.310584307107474,
35.8279021708056));
#93383=CARTESIAN_POINT('Ctrl Pts',(-2.36858962871103,0.00134465207171076,
35.848589891905));
#93384=CARTESIAN_POINT('Origin',(0.,0.,-1.84858989190512));
#93385=CARTESIAN_POINT('',(-2.36804291379594,-0.000743081082047163,33.6514101080949));
#93386=CARTESIAN_POINT('',(-2.37300722762269,-0.00203526771887147,33.848589891905));
#93387=CARTESIAN_POINT('',(-2.37175,1.74448693060498E-12,-1.84858989190512));
#93388=CARTESIAN_POINT('Ctrl Pts',(-2.36804291379594,-0.000743081082047181,
33.6514101080949));
#93389=CARTESIAN_POINT('Ctrl Pts',(-2.36902463128789,-0.351473225448641,
33.6748599438582));
#93390=CARTESIAN_POINT('Ctrl Pts',(-2.13135450972719,-1.49396215643721,
33.7513314142368));
#93391=CARTESIAN_POINT('Ctrl Pts',(-0.361803463717808,-2.78162253789443,
33.8808245192308));
#93392=CARTESIAN_POINT('Ctrl Pts',(2.14414858133226,-1.80857749373683,34.039889423077));
#93393=CARTESIAN_POINT('Ctrl Pts',(2.68082137390367,0.825543730459955,34.1989543269231));
#93394=CARTESIAN_POINT('Ctrl Pts',(0.755311294824669,2.70144971035752,34.3580192307693));
#93395=CARTESIAN_POINT('Ctrl Pts',(-1.72812275275069,2.12760307727921,34.5088378244932));
#93396=CARTESIAN_POINT('Ctrl Pts',(-2.36781572267268,0.663846095620685,
34.6066347836017));
#93397=CARTESIAN_POINT('Ctrl Pts',(-2.37358262552183,-0.0018767678844951,
34.6514101080949));
#93398=CARTESIAN_POINT('Ctrl Pts',(-2.37300722762269,-0.00203526771887147,
33.848589891905));
#93399=CARTESIAN_POINT('Ctrl Pts',(-2.37430298792658,-0.144529249187231,
33.8581677675232));
#93400=CARTESIAN_POINT('Ctrl Pts',(-2.29764386443108,-1.07463147152998,
33.9207790656371));
#93401=CARTESIAN_POINT('Ctrl Pts',(-1.06808869572879,-2.59397302681686,
34.0364237862468));
#93402=CARTESIAN_POINT('Ctrl Pts',(1.60487192110541,-2.30084672297929,34.1955240537341));
#93403=CARTESIAN_POINT('Ctrl Pts',(2.80324845369984,0.106337352922497,34.3546243212214));
#93404=CARTESIAN_POINT('Ctrl Pts',(1.425951812856,2.41581682939948,34.5137245887086));
#93405=CARTESIAN_POINT('Ctrl Pts',(-1.26153402157907,2.50560201113339,34.672824856196));
#93406=CARTESIAN_POINT('Ctrl Pts',(-2.33380736810732,0.953419897021398,
34.784446623928));
#93407=CARTESIAN_POINT('Ctrl Pts',(-2.37520266683563,0.0839087853630068,
34.8430349691644));
#93408=CARTESIAN_POINT('Ctrl Pts',(-2.37462230926531,0.00141218416469564,
34.848589891905));
#93409=CARTESIAN_POINT('Origin',(0.,0.,-1.84858989190512));
#93410=CARTESIAN_POINT('',(-2.37084923987159,0.00215313891885895,32.6514101080949));
#93411=CARTESIAN_POINT('',(-2.36789912899606,-0.000444447102319612,32.848589891905));
#93412=CARTESIAN_POINT('',(-2.37175,1.74448693060498E-12,-1.84858989190512));
#93413=CARTESIAN_POINT('Ctrl Pts',(-2.37084923987159,0.00215313891885871,
32.6514101080949));
#93414=CARTESIAN_POINT('Ctrl Pts',(-2.36577770381593,-0.574249672426079,
32.6900634694992));
#93415=CARTESIAN_POINT('Ctrl Pts',(-1.86414833270866,-1.94922154145056,
32.7817384655188));
#93416=CARTESIAN_POINT('Ctrl Pts',(0.439242037856295,-2.77044980497037,
32.9264350961539));
#93417=CARTESIAN_POINT('Ctrl Pts',(2.56793846593204,-1.12872393651732,33.0855));
#93418=CARTESIAN_POINT('Ctrl Pts',(2.33812859149225,1.54967105520072,33.2445649038462));
#93419=CARTESIAN_POINT('Ctrl Pts',(-0.0391202080950587,2.80478079339528,
33.4036298076924));
#93420=CARTESIAN_POINT('Ctrl Pts',(-2.03527486879144,1.67859243755198,33.5392448757752));
#93421=CARTESIAN_POINT('Ctrl Pts',(-2.36680490289919,0.441550902778074,
33.6218383092428));
#93422=CARTESIAN_POINT('Ctrl Pts',(-2.36804291379594,-0.000743081082047181,
33.6514101080949));
#93423=CARTESIAN_POINT('Ctrl Pts',(-2.36789912899606,-0.000444447102319855,
32.848589891905));
#93424=CARTESIAN_POINT('Ctrl Pts',(-2.36851557196465,-0.370088276800515,
32.873300565882));
#93425=CARTESIAN_POINT('Ctrl Pts',(-2.11274503704775,-1.53224491940183,
32.9510446623547));
#93426=CARTESIAN_POINT('Ctrl Pts',(-0.295001182690674,-2.78971034840684,
33.0818221813231));
#93427=CARTESIAN_POINT('Ctrl Pts',(2.18746727921893,-1.75627344913702,33.2409224488105));
#93428=CARTESIAN_POINT('Ctrl Pts',(2.66005296337403,0.890857877465394,33.4000227162977));
#93429=CARTESIAN_POINT('Ctrl Pts',(0.688535967781046,2.71945357505306,33.559122983785));
#93430=CARTESIAN_POINT('Ctrl Pts',(-1.75884896300695,2.08970758428599,33.7086453756541));
#93431=CARTESIAN_POINT('Ctrl Pts',(-2.3671282650142,0.644470715268389,33.8051343450274));
#93432=CARTESIAN_POINT('Ctrl Pts',(-2.37300722762269,-0.00203526771887147,
33.848589891905));
#93433=CARTESIAN_POINT('Origin',(0.,0.,-1.84858989190512));
#93434=CARTESIAN_POINT('',(-2.37564494446506,-0.000232844447847634,31.6514101080949));
#93435=CARTESIAN_POINT('',(-2.37137100238912,0.00219054532625537,31.848589891905));
#93436=CARTESIAN_POINT('',(-2.37175,1.74448693060498E-12,-1.84858989190512));
#93437=CARTESIAN_POINT('Ctrl Pts',(-2.37564494446506,-0.000232844447847528,
31.6514101080949));
#93438=CARTESIAN_POINT('Ctrl Pts',(-2.37566221911256,-0.0126230839183631,
31.6522453605248));
#93439=CARTESIAN_POINT('Ctrl Pts',(-2.36995459238346,-0.811526557648796,
31.7061022475701));
#93440=CARTESIAN_POINT('Ctrl Pts',(-1.4795770558054,-2.38310247904171,31.8129807692308));
#93441=CARTESIAN_POINT('Ctrl Pts',(1.20445971643178,-2.53329873508307,31.972045673077));
#93442=CARTESIAN_POINT('Ctrl Pts',(2.78226833327609,-0.356803323035994,
32.1311105769231));
#93443=CARTESIAN_POINT('Ctrl Pts',(1.80472078159196,2.14739576933795,32.2901754807693));
#93444=CARTESIAN_POINT('Ctrl Pts',(-0.83036077806552,2.67933325062988,32.4492403846154));
#93445=CARTESIAN_POINT('Ctrl Pts',(-2.24779252756098,1.21917927701057,32.5696519270573));
#93446=CARTESIAN_POINT('Ctrl Pts',(-2.3727344372516,0.216414273582911,32.6370418348838));
#93447=CARTESIAN_POINT('Ctrl Pts',(-2.37084923987159,0.00215313891885871,
32.6514101080949));
#93448=CARTESIAN_POINT('Ctrl Pts',(-2.37137100238912,0.00219054532625535,
31.848589891905));
#93449=CARTESIAN_POINT('Ctrl Pts',(-2.36595764621499,-0.591626673288607,
31.8884333642407));
#93450=CARTESIAN_POINT('Ctrl Pts',(-1.83899320124287,-1.98440542455834,
31.9813102590722));
#93451=CARTESIAN_POINT('Ctrl Pts',(0.501926962994743,-2.75999616840604,
32.1272205763995));
#93452=CARTESIAN_POINT('Ctrl Pts',(2.59328163816445,-1.06976626931127,32.2863208438868));
#93453=CARTESIAN_POINT('Ctrl Pts',(2.30188428228449,1.60338338421251,32.445421111374));
#93454=CARTESIAN_POINT('Ctrl Pts',(-0.104524173098342,2.80331664694433,
32.6045213788614));
#93455=CARTESIAN_POINT('Ctrl Pts',(-2.05605868746136,1.64119699270093,32.7389109723716));
#93456=CARTESIAN_POINT('Ctrl Pts',(-2.36719257768177,0.423231946338964,
32.8202671433862));
#93457=CARTESIAN_POINT('Ctrl Pts',(-2.36789912899606,-0.000444447102319855,
32.848589891905));
#93458=CARTESIAN_POINT('Origin',(0.,0.,-1.84858989190512));
#93459=CARTESIAN_POINT('',(-2.3701487589333,-0.00203535903446658,30.6514101080949));
#93460=CARTESIAN_POINT('',(-2.37553023271479,-0.000536704938520205,30.848589891905));
#93461=CARTESIAN_POINT('',(-2.37175,1.74448693060498E-12,-1.84858989190512));
#93462=CARTESIAN_POINT('Ctrl Pts',(-2.3701487589333,-0.00203535903446656,
30.6514101080949));
#93463=CARTESIAN_POINT('Ctrl Pts',(-2.37209433753784,-0.241386337143971,
30.6674488861659));
#93464=CARTESIAN_POINT('Ctrl Pts',(-2.22858721340341,-1.26971431685246,
30.7365092988522));
#93465=CARTESIAN_POINT('Ctrl Pts',(-0.74559551558228,-2.70414737335524,
30.8585913461539));
#93466=CARTESIAN_POINT('Ctrl Pts',(1.87143276947021,-2.08951312009126,31.01765625));
#93467=CARTESIAN_POINT('Ctrl Pts',(2.76965585724649,0.444220803318177,31.1767211538462));
#93468=CARTESIAN_POINT('Ctrl Pts',(1.12410662268099,2.56996303291023,31.3357860576923));
#93469=CARTESIAN_POINT('Ctrl Pts',(-1.53980888886202,2.33657152166105,31.4940157091086));
#93470=CARTESIAN_POINT('Ctrl Pts',(-2.3745656284112,0.773906504598037,31.5992237259095));
#93471=CARTESIAN_POINT('Ctrl Pts',(-2.37564494446506,-0.000232844447847528,
31.6514101080949));
#93472=CARTESIAN_POINT('Ctrl Pts',(-2.37553023271479,-0.000536704938520552,
30.848589891905));
#93473=CARTESIAN_POINT('Ctrl Pts',(-2.37561831176314,-0.0293608987698828,
30.8505327401037));
#93474=CARTESIAN_POINT('Ctrl Pts',(-2.36206334805178,-0.844906819600521,
30.9055090107983));
#93475=CARTESIAN_POINT('Ctrl Pts',(-1.42907574814251,-2.41397018040158,
31.0135187039885));
#93476=CARTESIAN_POINT('Ctrl Pts',(1.25829169048848,-2.50723184955934,31.1726189714758));
#93477=CARTESIAN_POINT('Ctrl Pts',(2.78951895635884,-0.296805522037135,
31.3317192389631));
#93478=CARTESIAN_POINT('Ctrl Pts',(1.75768794845828,2.18633085365451,31.4908195064504));
#93479=CARTESIAN_POINT('Ctrl Pts',(-0.889137153221077,2.66062861905961,
31.6499197739376));
#93480=CARTESIAN_POINT('Ctrl Pts',(-2.26075327480318,1.18372539029748,31.7691765690892));
#93481=CARTESIAN_POINT('Ctrl Pts',(-2.37316306251715,0.198770287465469,
31.835399941745));
#93482=CARTESIAN_POINT('Ctrl Pts',(-2.37137100238912,0.00219054532625535,
31.848589891905));
#93483=CARTESIAN_POINT('Origin',(0.,0.,-1.84858989190512));
#93484=CARTESIAN_POINT('',(-2.36833667409033,0.00111765679201713,29.6514101080949));
#93485=CARTESIAN_POINT('',(-2.36974424005732,-0.00192697225866761,29.848589891905));
#93486=CARTESIAN_POINT('',(-2.37175,1.74448693060498E-12,-1.84858989190512));
#93487=CARTESIAN_POINT('Ctrl Pts',(-2.36833667409033,0.00111765679201677,
29.6514101080949));
#93488=CARTESIAN_POINT('Ctrl Pts',(-2.36635541735129,-0.466016676365621,
29.6826524118069));
#93489=CARTESIAN_POINT('Ctrl Pts',(-2.00643187356775,-1.72874566519355,
29.7669163501342));
#93490=CARTESIAN_POINT('Ctrl Pts',(0.0492022987188458,-2.80462204645853,
29.9042019230769));
#93491=CARTESIAN_POINT('Ctrl Pts',(2.38575795131293,-1.47529139068443,30.0632668269231));
#93492=CARTESIAN_POINT('Ctrl Pts',(2.53112980449082,1.20901100181045,30.2223317307692));
#93493=CARTESIAN_POINT('Ctrl Pts',(0.351802029708706,2.78290514059918,30.3813966346154));
#93494=CARTESIAN_POINT('Ctrl Pts',(-1.89831104124899,1.89987965715743,30.5244227603906));
#93495=CARTESIAN_POINT('Ctrl Pts',(-2.36566256590104,0.54986970805048,30.6144272515505));
#93496=CARTESIAN_POINT('Ctrl Pts',(-2.3701487589333,-0.00203535903446656,
30.6514101080949));
#93497=CARTESIAN_POINT('Ctrl Pts',(-2.36974424005732,-0.00192697225866751,
29.848589891905));
#93498=CARTESIAN_POINT('Ctrl Pts',(-2.37168135840376,-0.256861139499681,
29.8656655384625));
#93499=CARTESIAN_POINT('Ctrl Pts',(-2.21616148860617,-1.30126756262755,
29.9357746075158));
#93500=CARTESIAN_POINT('Ctrl Pts',(-0.692053308057238,-2.71856060160596,
30.0589170990649));
#93501=CARTESIAN_POINT('Ctrl Pts',(1.91296709700241,-2.05184463631711,30.2180173665521));
#93502=CARTESIAN_POINT('Ctrl Pts',(2.76032024038351,0.500141676254002,30.3771176340394));
#93503=CARTESIAN_POINT('Ctrl Pts',(1.07144339534857,2.59258916459223,30.5362179015267));
#93504=CARTESIAN_POINT('Ctrl Pts',(-1.56924879404274,2.30645815426358,30.6933753208152));
#93505=CARTESIAN_POINT('Ctrl Pts',(-2.37321404086479,0.757445631218895,
30.797499317608));
#93506=CARTESIAN_POINT('Ctrl Pts',(-2.37553023271479,-0.000536704938520552,
30.848589891905));
#93507=CARTESIAN_POINT('Origin',(0.,0.,-1.84858989190512));
#93508=CARTESIAN_POINT('',(-2.37425246554842,0.00160971056243236,28.6514101080949));
#93509=CARTESIAN_POINT('',(-2.36855491481223,0.00131744329006256,28.848589891905));
#93510=CARTESIAN_POINT('',(-2.37175,1.74448693060498E-12,-1.84858989190512));
#93511=CARTESIAN_POINT('Ctrl Pts',(-2.37425246554842,0.00160971056243232,
28.6514101080949));
#93512=CARTESIAN_POINT('Ctrl Pts',(-2.36888615690045,-0.688442751284159,
28.6978559374479));
#93513=CARTESIAN_POINT('Ctrl Pts',(-1.6879762329752,-2.17546809508341,28.7973234014163));
#93514=CARTESIAN_POINT('Ctrl Pts',(0.839986810335585,-2.67633104233065,
28.9498125000001));
#93515=CARTESIAN_POINT('Ctrl Pts',(2.70548310349,-0.740734005166865,29.1088774038461));
#93516=CARTESIAN_POINT('Ctrl Pts',(2.08614612062029,1.87518533833364,29.2679423076924));
#93517=CARTESIAN_POINT('Ctrl Pts',(-0.449198133734217,2.7688529622084,29.4270072115385));
#93518=CARTESIAN_POINT('Ctrl Pts',(-2.15503896555959,1.44344170040664,29.5548298116727));
#93519=CARTESIAN_POINT('Ctrl Pts',(-2.3697178285187,0.32676179981013,29.6296307771915));
#93520=CARTESIAN_POINT('Ctrl Pts',(-2.36833667409033,0.00111765679201677,
29.6514101080949));
#93521=CARTESIAN_POINT('Ctrl Pts',(-2.36855491481223,0.00131744329006263,
28.848589891905));
#93522=CARTESIAN_POINT('Ctrl Pts',(-2.3661350789471,-0.480151430218069,
28.8807983368213));
#93523=CARTESIAN_POINT('Ctrl Pts',(-1.98917995276845,-1.75787348496187,
28.9660402042334));
#93524=CARTESIAN_POINT('Ctrl Pts',(0.10089768302309,-2.80344951503636,29.1043154941412));
#93525=CARTESIAN_POINT('Ctrl Pts',(2.41304534085417,-1.43063681931478,29.2634157616285));
#93526=CARTESIAN_POINT('Ctrl Pts',(2.50804519556235,1.25666973497962,29.4225160291157));
#93527=CARTESIAN_POINT('Ctrl Pts',(0.298609737212693,2.78932639729359,29.581616296603));
#93528=CARTESIAN_POINT('Ctrl Pts',(-1.91861604566399,1.86967193881861,29.7236409175328));
#93529=CARTESIAN_POINT('Ctrl Pts',(-2.36566506992268,0.534911596855939,
29.8126321159668));
#93530=CARTESIAN_POINT('Ctrl Pts',(-2.36974424005732,-0.00192697225866751,
29.848589891905));
#93531=CARTESIAN_POINT('Origin',(0.,0.,-1.84858989190512));
#93532=CARTESIAN_POINT('',(-2.37342029013076,-0.00192684023212259,27.6514101080949));
#93533=CARTESIAN_POINT('',(-2.37457526090586,0.00144042296748297,27.848589891905));
#93534=CARTESIAN_POINT('',(-2.37175,1.74448693060498E-12,-1.84858989190512));
#93535=CARTESIAN_POINT('Ctrl Pts',(-2.37342029013076,-0.00192684023212316,
27.6514101080949));
#93536=CARTESIAN_POINT('Ctrl Pts',(-2.37455049002191,-0.130227195499285,
27.6600378284736));
#93537=CARTESIAN_POINT('Ctrl Pts',(-2.30665001943632,-1.04579922342617,
27.7216871834676));
#93538=CARTESIAN_POINT('Ctrl Pts',(-1.1148611157287,-2.57398725372069,27.8363581730769));
#93539=CARTESIAN_POINT('Ctrl Pts',(1.56225579709783,-2.32973872228513,27.9954230769231));
#93540=CARTESIAN_POINT('Ctrl Pts',(2.80452908244698,0.0542431137526706,
28.1544879807693));
#93541=CARTESIAN_POINT('Ctrl Pts',(1.47100095966601,2.38840571644395,28.3135528846154));
#93542=CARTESIAN_POINT('Ctrl Pts',(-1.21355838150491,2.52895269713762,28.4726177884615));
#93543=CARTESIAN_POINT('Ctrl Pts',(-2.3251114613213,0.98397290416047,28.5852368629547));
#93544=CARTESIAN_POINT('Ctrl Pts',(-2.37501222807476,0.0993074085722678,
28.6448343028325));
#93545=CARTESIAN_POINT('Ctrl Pts',(-2.37425246554842,0.00160971056243232,
28.6514101080949));
#93546=CARTESIAN_POINT('Ctrl Pts',(-2.37457526090586,0.0014404229674831,
27.848589891905));
#93547=CARTESIAN_POINT('Ctrl Pts',(-2.36955185362383,-0.701664761427417,
27.8959311351801));
#93548=CARTESIAN_POINT('Ctrl Pts',(-1.665840495116,-2.20114684206871,27.9963058009509));
#93549=CARTESIAN_POINT('Ctrl Pts',(0.885694589519864,-2.66177659090546,
28.1497138892175));
#93550=CARTESIAN_POINT('Ctrl Pts',(2.71811240879197,-0.693811544274251,
28.3088141567048));
#93551=CARTESIAN_POINT('Ctrl Pts',(2.05308152547941,1.91163955167607,28.4679144241921));
#93552=CARTESIAN_POINT('Ctrl Pts',(-0.498356180275029,2.76064315755925,
28.6270146916793));
#93553=CARTESIAN_POINT('Ctrl Pts',(-2.16807702738258,1.41474422731526,28.7539065142503));
#93554=CARTESIAN_POINT('Ctrl Pts',(-2.37011950533401,0.312620224969389,
28.8277649143255));
#93555=CARTESIAN_POINT('Ctrl Pts',(-2.36855491481223,0.00131744329006263,
28.848589891905));
#93556=CARTESIAN_POINT('Origin',(0.,0.,-1.84858989190512));
#93557=CARTESIAN_POINT('',(-2.36799289882491,-0.000653459418386054,26.6514101080949));
#93558=CARTESIAN_POINT('',(-2.37306808171561,-0.00202154815997113,26.848589891905));
#93559=CARTESIAN_POINT('',(-2.37175,1.74448693060498E-12,-1.84858989190512));
#93560=CARTESIAN_POINT('Ctrl Pts',(-2.36799289882491,-0.000653459418386224,
26.6514101080949));
#93561=CARTESIAN_POINT('Ctrl Pts',(-2.36886921458804,-0.357106994699224,
26.6752413541146));
#93562=CARTESIAN_POINT('Ctrl Pts',(-2.12579799293791,-1.50549148658124,
26.7520942347496));
#93563=CARTESIAN_POINT('Ctrl Pts',(-0.34179604974745,-2.78415178286989,
26.8819687500001));
#93564=CARTESIAN_POINT('Ctrl Pts',(2.15709566880955,-1.79311571441545,27.0410336538462));
#93565=CARTESIAN_POINT('Ctrl Pts',(2.67481696700378,0.844795763903405,27.2000985576923));
#93566=CARTESIAN_POINT('Ctrl Pts',(0.73587010182595,2.70681009361926,27.3591634615385));
#93567=CARTESIAN_POINT('Ctrl Pts',(-1.73710433416866,2.11662034428545,27.509600645006));
#93568=CARTESIAN_POINT('Ctrl Pts',(-2.36760484933805,0.65824232593481,27.6070161938582));
#93569=CARTESIAN_POINT('Ctrl Pts',(-2.37342029013076,-0.00192684023212316,
27.6514101080949));
#93570=CARTESIAN_POINT('Ctrl Pts',(-2.37306808171561,-0.00202154815997103,
26.848589891905));
#93571=CARTESIAN_POINT('Ctrl Pts',(-2.37434058588056,-0.142464205890787,
26.8580305110431));
#93572=CARTESIAN_POINT('Ctrl Pts',(-2.29896181857628,-1.07049040953162,
26.920504552677));
#93573=CARTESIAN_POINT('Ctrl Pts',(-1.07479630198138,-2.59120096384751,
27.0360120168066));
#93574=CARTESIAN_POINT('Ctrl Pts',(1.59891375129768,-2.30499118039708,27.1951122842938));
#93575=CARTESIAN_POINT('Ctrl Pts',(2.80351418982834,0.0990843742891699,
27.3542125517811));
#93576=CARTESIAN_POINT('Ctrl Pts',(1.43219729196881,2.41211949179022,27.5133128192684));
#93577=CARTESIAN_POINT('Ctrl Pts',(-1.25504725373308,2.50885749230484,27.6724130867557));
#93578=CARTESIAN_POINT('Ctrl Pts',(-2.33265631141876,0.957549547268701,
27.7841721109679));
#93579=CARTESIAN_POINT('Ctrl Pts',(-2.37517926140458,0.085979831814631,
27.8428977126843));
#93580=CARTESIAN_POINT('Ctrl Pts',(-2.37457526090586,0.0014404229674831,
27.848589891905));
#93581=CARTESIAN_POINT('Origin',(0.,0.,-1.84858989190512));
#93582=CARTESIAN_POINT('',(-2.37101590433324,0.00216888848020844,25.6514101080949));
#93583=CARTESIAN_POINT('',(-2.36791098026206,-0.000477715941999413,25.848589891905));
#93584=CARTESIAN_POINT('',(-2.37175,1.74448693060498E-12,-1.84858989190512));
#93585=CARTESIAN_POINT('Ctrl Pts',(-2.37101590433324,0.00216888848020831,
25.6514101080949));
#93586=CARTESIAN_POINT('Ctrl Pts',(-2.36582777414831,-0.579817597934016,
25.6904448797556));
#93587=CARTESIAN_POINT('Ctrl Pts',(-1.85617349906383,-1.96045219094367,
25.7825012860316));
#93588=CARTESIAN_POINT('Ctrl Pts',(0.459148425116812,-2.76722034059328,
25.9275793269231));
#93589=CARTESIAN_POINT('Ctrl Pts',(2.57598689455279,-1.11023295248012,26.0866442307693));
#93590=CARTESIAN_POINT('Ctrl Pts',(2.32692703480318,1.56644063544793,26.2457091346154));
#93591=CARTESIAN_POINT('Ctrl Pts',(-0.0592837535552358,2.80442705846396,
26.4047740384616));
#93592=CARTESIAN_POINT('Ctrl Pts',(-2.04169909775158,1.66712437431943,26.5400076962881));
#93593=CARTESIAN_POINT('Ctrl Pts',(-2.36691951820364,0.435958927638278,
26.6222197194992));
#93594=CARTESIAN_POINT('Ctrl Pts',(-2.36799289882491,-0.000653459418386224,
26.6514101080949));
#93595=CARTESIAN_POINT('Ctrl Pts',(-2.36791098026206,-0.000477715941999204,
25.848589891905));
#93596=CARTESIAN_POINT('Ctrl Pts',(-2.36857006946863,-0.36806375603213,
25.8731633094019));
#93597=CARTESIAN_POINT('Ctrl Pts',(-2.11479784456769,-1.52809834734262,
25.9507701493945));
#93598=CARTESIAN_POINT('Ctrl Pts',(-0.302217792031812,-2.78893777843403,
26.0814104118829));
#93599=CARTESIAN_POINT('Ctrl Pts',(2.18291609085233,-1.76192703200078,26.2405106793702));
#93600=CARTESIAN_POINT('Ctrl Pts',(2.66234890658549,0.883972751503175,26.3996109468574));
#93601=CARTESIAN_POINT('Ctrl Pts',(0.695569490229732,2.71766307883422,26.5587112143448));
#93602=CARTESIAN_POINT('Ctrl Pts',(-1.75568464583691,2.09367884994919,26.7083708626939));
#93603=CARTESIAN_POINT('Ctrl Pts',(-2.3671921933842,0.646483499224386,26.8049970885473));
#93604=CARTESIAN_POINT('Ctrl Pts',(-2.37306808171561,-0.00202154815997103,
26.848589891905));
#93605=CARTESIAN_POINT('Origin',(0.,0.,-1.84858989190512));
#93606=CARTESIAN_POINT('',(-2.37561413348328,-0.000338293417154348,24.6514101080949));
#93607=CARTESIAN_POINT('',(-2.3713094773117,0.00218862049173575,24.848589891905));
#93608=CARTESIAN_POINT('',(-2.37175,1.74448693060498E-12,-1.84858989190512));
#93609=CARTESIAN_POINT('Ctrl Pts',(-2.37561413348328,-0.00033829341715417,
24.6514101080949));
#93610=CARTESIAN_POINT('Ctrl Pts',(-2.37565004965548,-0.0183870501238682,
24.6526267707812));
#93611=CARTESIAN_POINT('Ctrl Pts',(-2.36727666328559,-0.822958632995309,
24.7068650680829));
#93612=CARTESIAN_POINT('Ctrl Pts',(-1.46240585539294,-2.39367809109597,
24.8141250000001));
#93613=CARTESIAN_POINT('Ctrl Pts',(1.2226413650927,-2.52457398030731,24.9731899038461));
#93614=CARTESIAN_POINT('Ctrl Pts',(2.78476161379025,-0.336791395437584,
25.1322548076924));
#93615=CARTESIAN_POINT('Ctrl Pts',(1.78923575676476,2.16031504563452,25.2913197115385));
#93616=CARTESIAN_POINT('Ctrl Pts',(-0.849601988376427,2.6732942507377,25.4503846153846));
#93617=CARTESIAN_POINT('Ctrl Pts',(-2.25204311898601,1.2076448752048,25.5704147475701));
#93618=CARTESIAN_POINT('Ctrl Pts',(-2.37287490498319,0.21070514681249,25.6374232451402));
#93619=CARTESIAN_POINT('Ctrl Pts',(-2.37101590433324,0.00216888848020831,
25.6514101080949));
#93620=CARTESIAN_POINT('Ctrl Pts',(-2.3713094773117,0.00218862049173589,
24.848589891905));
#93621=CARTESIAN_POINT('Ctrl Pts',(-2.36593141354757,-0.589622083083144,
24.8882961077606));
#93622=CARTESIAN_POINT('Ctrl Pts',(-1.84192095452906,-1.98037618738568,
24.981035746112));
#93623=CARTESIAN_POINT('Ctrl Pts',(0.494784563590454,-2.76128552696561,
25.1268088069592));
#93624=CARTESIAN_POINT('Ctrl Pts',(2.59050523725581,-1.07647208117411,25.2859090744465));
#93625=CARTESIAN_POINT('Ctrl Pts',(2.30602488505606,1.59742253499168,25.4450093419338));
#93626=CARTESIAN_POINT('Ctrl Pts',(-0.0972710241024927,2.80357769174802,
25.6041096094211));
#93627=CARTESIAN_POINT('Ctrl Pts',(-2.05380189715669,1.64532922764933,25.7386364594115));
#93628=CARTESIAN_POINT('Ctrl Pts',(-2.3671476480102,0.425246566804615,25.8201298869061));
#93629=CARTESIAN_POINT('Ctrl Pts',(-2.36791098026206,-0.000477715941999204,
25.848589891905));
#93630=CARTESIAN_POINT('Origin',(0.,0.,-1.84858989190512));
#93631=CARTESIAN_POINT('',(-2.3699970317438,-0.0019977438217458,23.6514101080949));
#93632=CARTESIAN_POINT('',(-2.37554964903122,-0.000499616039387474,23.848589891905));
#93633=CARTESIAN_POINT('',(-2.37175,1.74448693060498E-12,-1.84858989190512));
#93634=CARTESIAN_POINT('Ctrl Pts',(-2.3699970317438,-0.00199774382174632,
23.6514101080949));
#93635=CARTESIAN_POINT('Ctrl Pts',(-2.37194321588891,-0.247080240897932,
23.6678302964223));
#93636=CARTESIAN_POINT('Ctrl Pts',(-2.22406647554583,-1.28125555242059,
23.737272119365));
#93637=CARTESIAN_POINT('Ctrl Pts',(-0.726135179226555,-2.70943783674216,
23.8597355769231));
#93638=CARTESIAN_POINT('Ctrl Pts',(1.88640665005374,-2.07600473032059,24.0188004807692));
#93639=CARTESIAN_POINT('Ctrl Pts',(2.76639061929044,0.464121353939118,24.1778653846154));
#93640=CARTESIAN_POINT('Ctrl Pts',(1.10560120264771,2.57797821371406,24.3369302884615));
#93641=CARTESIAN_POINT('Ctrl Pts',(-1.55015041093734,2.32604964527379,24.4947785296214));
#93642=CARTESIAN_POINT('Ctrl Pts',(-2.3740848383765,0.768169975198311,24.5996051361658));
#93643=CARTESIAN_POINT('Ctrl Pts',(-2.37561413348328,-0.00033829341715417,
24.6514101080949));
#93644=CARTESIAN_POINT('Ctrl Pts',(-2.37554964903122,-0.000499616039387678,
23.848589891905));
#93645=CARTESIAN_POINT('Ctrl Pts',(-2.3756263002611,-0.02728687960757,23.8503954836237));
#93646=CARTESIAN_POINT('Ctrl Pts',(-2.36306094446354,-0.840789806362212,
23.9052344978381));
#93647=CARTESIAN_POINT('Ctrl Pts',(-1.43531643911124,-2.4102647666624,24.0131069345482));
#93648=CARTESIAN_POINT('Ctrl Pts',(1.2518007167422,-2.51047893664949,24.1722072020356));
#93649=CARTESIAN_POINT('Ctrl Pts',(2.78874171880229,-0.304021630165937,
24.3313074695228));
#93650=CARTESIAN_POINT('Ctrl Pts',(1.76333858640404,2.18177600946929,24.4904077370101));
#93651=CARTESIAN_POINT('Ctrl Pts',(-0.882250543669541,2.66292010845086,
24.6495080044974));
#93652=CARTESIAN_POINT('Ctrl Pts',(-2.25926617902281,1.18787477101089,24.768902056129));
#93653=CARTESIAN_POINT('Ctrl Pts',(-2.37311459939558,0.200827130065391,
24.8352626852649));
#93654=CARTESIAN_POINT('Ctrl Pts',(-2.3713094773117,0.00218862049173589,
24.848589891905));
#93655=CARTESIAN_POINT('Origin',(0.,0.,-1.84858989190512));
#93656=CARTESIAN_POINT('',(-2.36842026495236,0.00119817809484571,22.6514101080949));
#93657=CARTESIAN_POINT('',(-2.36979619273569,-0.00194326858727306,22.848589891905));
#93658=CARTESIAN_POINT('',(-2.37175,1.74448693060498E-12,-1.84858989190512));
#93659=CARTESIAN_POINT('Ctrl Pts',(-2.36842026495236,0.00119817809484543,
22.6514101080949));
#93660=CARTESIAN_POINT('Ctrl Pts',(-2.36626591411704,-0.471597269374344,
22.6830338220633));
#93661=CARTESIAN_POINT('Ctrl Pts',(-1.99968381525113,-1.74017804174392,
22.767679170647));
#93662=CARTESIAN_POINT('Ctrl Pts',(0.0693644423326341,-2.8041958319312,
22.9053461538462));
#93663=CARTESIAN_POINT('Ctrl Pts',(2.39630268358469,-1.45810120990461,23.0644110576923));
#93664=CARTESIAN_POINT('Ctrl Pts',(2.52237238497556,1.22717693964369,23.2234759615385));
#93665=CARTESIAN_POINT('Ctrl Pts',(0.331785653130296,2.78536244859756,23.3825408653846));
#93666=CARTESIAN_POINT('Ctrl Pts',(-1.90593755423956,1.88858078851823,23.5251855809035));
#93667=CARTESIAN_POINT('Ctrl Pts',(-2.36565888695313,0.544303776846138,
23.6148086618069));
#93668=CARTESIAN_POINT('Ctrl Pts',(-2.3699970317438,-0.00199774382174632,
23.6514101080949));
#93669=CARTESIAN_POINT('Ctrl Pts',(-2.36979619273569,-0.00194326858727323,
22.848589891905));
#93670=CARTESIAN_POINT('Ctrl Pts',(-2.37173688724524,-0.254814261784281,
22.8655282819824));
#93671=CARTESIAN_POINT('Ctrl Pts',(-2.21782603676459,-1.29711363442759,
22.9355000945556));
#93672=CARTESIAN_POINT('Ctrl Pts',(-0.699084508414374,-2.7167610082398,
23.0585053296246));
#93673=CARTESIAN_POINT('Ctrl Pts',(1.90765211942334,-2.05678703736111,23.2176055971119));
#93674=CARTESIAN_POINT('Ctrl Pts',(2.76160497892747,0.49299844437904,23.3767058645991));
#93675=CARTESIAN_POINT('Ctrl Pts',(1.07814741001629,2.5898084269058,23.5358061320864));
#93676=CARTESIAN_POINT('Ctrl Pts',(-1.56558316400954,2.31026649768087,23.693100807855));
#93677=CARTESIAN_POINT('Ctrl Pts',(-2.37337491805917,0.759502432526167,
23.7973620611279));
#93678=CARTESIAN_POINT('Ctrl Pts',(-2.37554964903122,-0.000499616039387678,
23.848589891905));
#93679=CARTESIAN_POINT('Origin',(0.,0.,-1.84858989190512));
#93680=CARTESIAN_POINT('',(-2.37439379830995,0.00153838718516934,21.6514101080949));
#93681=CARTESIAN_POINT('',(-2.36852094091456,0.00128992227662758,21.848589891905));
#93682=CARTESIAN_POINT('',(-2.37175,1.74448693060498E-12,-1.84858989190512));
#93683=CARTESIAN_POINT('Ctrl Pts',(-2.37439379830994,0.00153838718516921,
21.6514101080949));
#93684=CARTESIAN_POINT('Ctrl Pts',(-2.36916514996087,-0.694072325068264,
21.6982373477043));
#93685=CARTESIAN_POINT('Ctrl Pts',(-1.67862426279434,-2.18634004573506,
21.7980862219291));
#93686=CARTESIAN_POINT('Ctrl Pts',(0.859206187941647,-2.67022291509215,
21.9509567307692));
#93687=CARTESIAN_POINT('Ctrl Pts',(2.71073858124696,-0.721264191416516,
22.1100216346154));
#93688=CARTESIAN_POINT('Ctrl Pts',(2.07261083932685,1.89013491539238,22.2690865384616));
#93689=CARTESIAN_POINT('Ctrl Pts',(-0.469092783427355,2.76555196122163,
22.4281514423077));
#93690=CARTESIAN_POINT('Ctrl Pts',(-2.16029918274576,1.43190245360995,22.5555926321855));
#93691=CARTESIAN_POINT('Ctrl Pts',(-2.36987798836417,0.321111249574778,
22.6300121874479));
#93692=CARTESIAN_POINT('Ctrl Pts',(-2.36842026495236,0.00119817809484543,
22.6514101080949));
#93693=CARTESIAN_POINT('Ctrl Pts',(-2.36852094091456,0.00128992227662748,
21.848589891905));
#93694=CARTESIAN_POINT('Ctrl Pts',(-2.36616375344373,-0.478144377631666,
21.8806610803412));
#93695=CARTESIAN_POINT('Ctrl Pts',(-1.99164931628814,-1.75376439025444,
21.9657656912732));
#93696=CARTESIAN_POINT('Ctrl Pts',(0.0936442024055214,-2.80370117686478,
22.1039037247009));
#93697=CARTESIAN_POINT('Ctrl Pts',(2.40933589137447,-1.43687511229467,22.2630039921882));
#93698=CARTESIAN_POINT('Ctrl Pts',(2.51128808357329,1.25017666235613,22.4221042596755));
#93699=CARTESIAN_POINT('Ctrl Pts',(0.305825341110179,2.78854449247846,22.5812045271628));
#93700=CARTESIAN_POINT('Ctrl Pts',(-1.91591745013914,1.87374633225182,22.7233664045726));
#93701=CARTESIAN_POINT('Ctrl Pts',(-2.36566065028352,0.536914713509884,
22.8124948594867));
#93702=CARTESIAN_POINT('Ctrl Pts',(-2.36979619273569,-0.00194326858727323,
22.848589891905));
#93703=CARTESIAN_POINT('Origin',(0.,0.,-1.84858989190512));
#93704=CARTESIAN_POINT('',(-2.37325526314324,-0.00197269285830692,20.6514101080949));
#93705=CARTESIAN_POINT('',(-2.37452747597515,0.00146821833409135,20.848589891905));
#93706=CARTESIAN_POINT('',(-2.37175,1.74448693060498E-12,-1.84858989190512));
#93707=CARTESIAN_POINT('Ctrl Pts',(-2.37325526314324,-0.00197269285830694,
20.6514101080949));
#93708=CARTESIAN_POINT('Ctrl Pts',(-2.37445256882395,-0.135969023876453,
20.66041923873));
#93709=CARTESIAN_POINT('Ctrl Pts',(-2.30307226995662,-1.05730119808642,
20.7224500039804));
#93710=CARTESIAN_POINT('Ctrl Pts',(-1.09632700309372,-2.58193586131958,
20.8375024038462));
#93711=CARTESIAN_POINT('Ctrl Pts',(1.5789647343853,-2.31844690628189,20.9965673076923));
#93712=CARTESIAN_POINT('Ctrl Pts',(2.80406663012842,0.0744044587420362,
21.1556322115385));
#93713=CARTESIAN_POINT('Ctrl Pts',(1.4537918540513,2.39891953486867,21.3146971153846));
#93714=CARTESIAN_POINT('Ctrl Pts',(-1.23170854982573,2.52016264117351,21.4737620192308));
#93715=CARTESIAN_POINT('Ctrl Pts',(-2.32839868565871,0.972490786612713,
21.5859996834675));
#93716=CARTESIAN_POINT('Ctrl Pts',(-2.37508545371163,0.0935550757204803,
21.6452157130889));
#93717=CARTESIAN_POINT('Ctrl Pts',(-2.37439379830994,0.00153838718516921,
21.6514101080949));
#93718=CARTESIAN_POINT('Ctrl Pts',(-2.37452747597515,0.00146821833409142,
20.848589891905));
#93719=CARTESIAN_POINT('Ctrl Pts',(-2.36944352129783,-0.699635497062075,
20.8957938787));
#93720=CARTESIAN_POINT('Ctrl Pts',(-1.66924795052569,-2.19724761514887,
20.9960312879907));
#93721=CARTESIAN_POINT('Ctrl Pts',(0.878805021433445,-2.66405916978217,
21.1493021197773));
#93722=CARTESIAN_POINT('Ctrl Pts',(2.71630826798053,-0.70084157917304,21.3084023872645));
#93723=CARTESIAN_POINT('Ctrl Pts',(2.05802048773081,1.90632137843475,21.4675026547518));
#93724=CARTESIAN_POINT('Ctrl Pts',(-0.491212118917867,2.76192327555009,
21.6266029222391));
#93725=CARTESIAN_POINT('Ctrl Pts',(-2.16621938134231,1.41889763066239,21.7536320012902));
#93726=CARTESIAN_POINT('Ctrl Pts',(-2.37006163578416,0.31465573442438,21.8276276578455));
#93727=CARTESIAN_POINT('Ctrl Pts',(-2.36852094091456,0.00128992227662748,
21.848589891905));
#93728=CARTESIAN_POINT('Origin',(0.,0.,-1.84858989190512));
#93729=CARTESIAN_POINT('',(-2.3679493887729,-0.000562658222058198,19.651410108095));
#93730=CARTESIAN_POINT('',(-2.37312868751824,-0.00200726644127208,19.848589891905));
#93731=CARTESIAN_POINT('',(-2.37175,1.74448693060498E-12,-1.84858989190512));
#93732=CARTESIAN_POINT('Ctrl Pts',(-2.3679493887729,-0.000562658222058171,
19.651410108095));
#93733=CARTESIAN_POINT('Ctrl Pts',(-2.36871522544106,-0.362737700238317,
19.675622764371));
#93734=CARTESIAN_POINT('Ctrl Pts',(-2.12018559280303,-1.5170183344022,19.7528570552624));
#93735=CARTESIAN_POINT('Ctrl Pts',(-0.321770969210761,-2.78653712213808,
19.8831129807692));
#93736=CARTESIAN_POINT('Ctrl Pts',(2.16993126151137,-1.77756125351454,20.0421778846154));
#93737=CARTESIAN_POINT('Ctrl Pts',(2.66867430563458,0.864004132007661,20.2012427884615));
#93738=CARTESIAN_POINT('Ctrl Pts',(0.716390873577828,2.7120305687685,20.3603076923077));
#93739=CARTESIAN_POINT('Ctrl Pts',(-1.7460176444507,2.10561836082741,20.5103634655188));
#93740=CARTESIAN_POINT('Ctrl Pts',(-2.36740603937537,0.652642529321267,
20.6073976041146));
#93741=CARTESIAN_POINT('Ctrl Pts',(-2.37325526314324,-0.00197269285830694,
20.6514101080949));
#93742=CARTESIAN_POINT('Ctrl Pts',(-2.37312868751824,-0.00200726644127234,
19.848589891905));
#93743=CARTESIAN_POINT('Ctrl Pts',(-2.37437772673991,-0.140398904122633,
19.857893254563));
#93744=CARTESIAN_POINT('Ctrl Pts',(-2.300273734566,-1.0663497090457,19.9202300397168));
#93745=CARTESIAN_POINT('Ctrl Pts',(-1.08149671384552,-2.58841155609738,
20.0356002473663));
#93746=CARTESIAN_POINT('Ctrl Pts',(1.59294487880464,-2.30912020884302,20.1947005148536));
#93747=CARTESIAN_POINT('Ctrl Pts',(2.80376116001019,0.0918307324124995,
20.3538007823408));
#93748=CARTESIAN_POINT('Ctrl Pts',(1.43843318435008,2.40840600812187,20.5129010498282));
#93749=CARTESIAN_POINT('Ctrl Pts',(-1.24855208494876,2.51209617987991,20.6720013173154));
#93750=CARTESIAN_POINT('Ctrl Pts',(-2.33149949909663,0.961679636121884,
20.7838975980077));
#93751=CARTESIAN_POINT('Ctrl Pts',(-2.37515531673415,0.0880507149826994,
20.8427604562042));
#93752=CARTESIAN_POINT('Ctrl Pts',(-2.37452747597515,0.00146821833409142,
20.848589891905));
#93753=CARTESIAN_POINT('Origin',(0.,0.,-1.84858989190512));
#93754=CARTESIAN_POINT('',(-2.37118449249719,0.00218036612316423,18.651410108095));
#93755=CARTESIAN_POINT('',(-2.36792368850356,-0.000510873358860464,18.848589891905));
#93756=CARTESIAN_POINT('',(-2.37175,1.74448693060498E-12,-1.84858989190512));
#93757=CARTESIAN_POINT('Ctrl Pts',(-2.37118449249719,0.00218036612316402,
18.651410108095));
#93758=CARTESIAN_POINT('Ctrl Pts',(-2.36588712038017,-0.585386454121441,
18.690826290012));
#93759=CARTESIAN_POINT('Ctrl Pts',(-1.84813322168764,-1.97166903258445,
18.7832641065445));
#93760=CARTESIAN_POINT('Ctrl Pts',(0.479031080165797,-2.76384784565209,
18.9287235576923));
#93761=CARTESIAN_POINT('Ctrl Pts',(2.58390217697866,-1.09168458333227,19.0877884615385));
#93762=CARTESIAN_POINT('Ctrl Pts',(2.31560520518838,1.58312925037248,19.2468533653847));
#93763=CARTESIAN_POINT('Ctrl Pts',(-0.0794442347893398,2.80392836984813,
19.4059182692308));
#93764=CARTESIAN_POINT('Ctrl Pts',(-2.04806391798638,1.65565053536932,19.5407705168009));
#93765=CARTESIAN_POINT('Ctrl Pts',(-2.36703817226971,0.430364573451299,
19.6226011297556));
#93766=CARTESIAN_POINT('Ctrl Pts',(-2.3679493887729,-0.000562658222058171,
19.651410108095));
#93767=CARTESIAN_POINT('Ctrl Pts',(-2.36792368850356,-0.000510873358860013,
18.848589891905));
#93768=CARTESIAN_POINT('Ctrl Pts',(-2.3686247961319,-0.366038844975643,
18.8730260529218));
#93769=CARTESIAN_POINT('Ctrl Pts',(-2.11684335076948,-1.52395140070622,
18.9504956364343));
#93770=CARTESIAN_POINT('Ctrl Pts',(-0.309432378410861,-2.78814654008503,
19.0809986424426));
#93771=CARTESIAN_POINT('Ctrl Pts',(2.17835029065068,-1.76756882101353,19.2400989099299));
#93772=CARTESIAN_POINT('Ctrl Pts',(2.66462702877159,0.877081708472472,19.3991991774172));
#93773=CARTESIAN_POINT('Ctrl Pts',(0.702598356729098,2.71585439133226,19.5582994449045));
#93774=CARTESIAN_POINT('Ctrl Pts',(-1.75251153778358,2.09764773379169,19.7080963497337));
#93775=CARTESIAN_POINT('Ctrl Pts',(-2.3672576318676,0.648496730804293,19.8048598320673));
#93776=CARTESIAN_POINT('Ctrl Pts',(-2.37312868751824,-0.00200726644127234,
19.848589891905));
#93777=CARTESIAN_POINT('Origin',(0.,0.,-1.84858989190512));
#93778=CARTESIAN_POINT('',(-2.37557266989979,-0.000442787889473553,17.651410108095));
#93779=CARTESIAN_POINT('',(-2.37124813668935,0.00218613168039616,17.848589891905));
#93780=CARTESIAN_POINT('',(-2.37175,1.74448693060498E-12,-1.84858989190512));
#93781=CARTESIAN_POINT('Ctrl Pts',(-2.37557266989979,-0.000442787889474178,
17.651410108095));
#93782=CARTESIAN_POINT('Ctrl Pts',(-2.37563336905613,-0.0241507402655156,
17.6530081810377));
#93783=CARTESIAN_POINT('Ctrl Pts',(-2.36455668635702,-0.834394437625102,
17.7076278885958));
#93784=CARTESIAN_POINT('Ctrl Pts',(-1.44515906695039,-2.4041299800326,17.8152692307692));
#93785=CARTESIAN_POINT('Ctrl Pts',(1.24075981853869,-2.51571873673912,17.9743341346154));
#93786=CARTESIAN_POINT('Ctrl Pts',(2.78711095707658,-0.316762059950613,
18.1333990384615));
#93787=CARTESIAN_POINT('Ctrl Pts',(1.77365825090308,2.17312266075431,18.2924639423077));
#93788=CARTESIAN_POINT('Ctrl Pts',(-0.868799284926716,2.66711707508149,
18.4515288461538));
#93789=CARTESIAN_POINT('Ctrl Pts',(-2.25624427366724,1.19611213094849,18.5711775680829));
#93790=CARTESIAN_POINT('Ctrl Pts',(-2.37301300916873,0.204993327478883,
18.6378046553966));
#93791=CARTESIAN_POINT('Ctrl Pts',(-2.37118449249719,0.00218036612316402,
18.651410108095));
#93792=CARTESIAN_POINT('Ctrl Pts',(-2.37124813668935,0.00218613168039603,
17.848589891905));
#93793=CARTESIAN_POINT('Ctrl Pts',(-2.36590642856635,-0.587617655854367,
17.8881588512806));
#93794=CARTESIAN_POINT('Ctrl Pts',(-1.8448401832008,-1.97634507886242,17.9807612331519));
#93795=CARTESIAN_POINT('Ctrl Pts',(0.487638852235446,-2.7625564022455,18.1263970375189));
#93796=CARTESIAN_POINT('Ctrl Pts',(2.58771149622336,-1.08317068743137,18.2854973050062));
#93797=CARTESIAN_POINT('Ctrl Pts',(2.3101500519365,1.5914509930673,18.4445975724935));
#93798=CARTESIAN_POINT('Ctrl Pts',(-0.0900172240013499,2.80381997018001,
18.6036978399808));
#93799=CARTESIAN_POINT('Ctrl Pts',(-2.051537474168,1.649460778596,18.7383619464513));
#93800=CARTESIAN_POINT('Ctrl Pts',(-2.36710319308455,0.427260861122469,
18.819992630426));
#93801=CARTESIAN_POINT('Ctrl Pts',(-2.36792368850356,-0.000510873358860013,
18.848589891905));
#93802=CARTESIAN_POINT('Origin',(0.,0.,-1.84858989190512));
#93803=CARTESIAN_POINT('',(-2.36984887420079,-0.00195632190991676,16.651410108095));
#93804=CARTESIAN_POINT('',(-2.37556777218862,-0.000462349284400809,16.848589891905));
#93805=CARTESIAN_POINT('',(-2.37175,1.74448693060498E-12,-1.84858989190512));
#93806=CARTESIAN_POINT('Ctrl Pts',(-2.36984887420079,-0.00195632190991717,
16.651410108095));
#93807=CARTESIAN_POINT('Ctrl Pts',(-2.37179051810406,-0.252771195777155,
16.6682117066787));
#93808=CARTESIAN_POINT('Ctrl Pts',(-2.21949473853235,-1.29279764384103,
16.7380349398778));
#93809=CARTESIAN_POINT('Ctrl Pts',(-0.706637310794764,-2.71458825619525,
16.8608798076923));
#93810=CARTESIAN_POINT('Ctrl Pts',(1.9012830270871,-2.06238903715836,17.0199447115385));
#93811=CARTESIAN_POINT('Ctrl Pts',(2.76298239365644,0.483997915310618,17.1790096153846));
#93812=CARTESIAN_POINT('Ctrl Pts',(1.08703863690706,2.58586014539682,17.3380745192308));
#93813=CARTESIAN_POINT('Ctrl Pts',(-1.5604205625462,2.31549981116177,17.4955413501342));
#93814=CARTESIAN_POINT('Ctrl Pts',(-2.3736194631805,0.762443134622733,17.5999865464223));
#93815=CARTESIAN_POINT('Ctrl Pts',(-2.37557266989979,-0.000442787889474178,
17.651410108095));
#93816=CARTESIAN_POINT('Ctrl Pts',(-2.37556777218862,-0.000462349284400653,
16.848589891905));
#93817=CARTESIAN_POINT('Ctrl Pts',(-2.37563370680816,-0.0252128074327879,
16.8502582271436));
#93818=CARTESIAN_POINT('Ctrl Pts',(-2.36405305652946,-0.836673273324087,
16.9049599848779));
#93819=CARTESIAN_POINT('Ctrl Pts',(-1.44154752246972,-2.40654321927916,
17.012695165108));
#93820=CARTESIAN_POINT('Ctrl Pts',(1.24530136378902,-2.51370921928975,17.1717954325953));
#93821=CARTESIAN_POINT('Ctrl Pts',(2.78794581418191,-0.311235703258245,
17.3308957000825));
#93822=CARTESIAN_POINT('Ctrl Pts',(1.76897742105025,2.17720656108039,17.4899959675698));
#93823=CARTESIAN_POINT('Ctrl Pts',(-0.875358028577435,2.66519377299328,
17.6490962350571));
#93824=CARTESIAN_POINT('Ctrl Pts',(-2.25777273477332,1.19202439171433,17.7686275431688));
#93825=CARTESIAN_POINT('Ctrl Pts',(-2.37306580470883,0.202883634742145,
17.8351254287848));
#93826=CARTESIAN_POINT('Ctrl Pts',(-2.37124813668935,0.00218613168039603,
17.848589891905));
#93827=CARTESIAN_POINT('Origin',(0.,0.,-1.84858989190512));
#93828=CARTESIAN_POINT('',(-2.36850976199849,0.00127651360681889,15.651410108095));
#93829=CARTESIAN_POINT('',(-2.36984864786026,-0.00195908838300035,15.848589891905));
#93830=CARTESIAN_POINT('',(-2.37175,1.74448693060498E-12,-1.84858989190512));
#93831=CARTESIAN_POINT('Ctrl Pts',(-2.36850976199849,0.00127651360681887,
15.651410108095));
#93832=CARTESIAN_POINT('Ctrl Pts',(-2.3661817149612,-0.477176041303263,
15.6834152323197));
#93833=CARTESIAN_POINT('Ctrl Pts',(-1.99287478523265,-1.75160289678569,
15.7684419911599));
#93834=CARTESIAN_POINT('Ctrl Pts',(0.0895230006752742,-2.80362467567087,
15.9064903846154));
#93835=CARTESIAN_POINT('Ctrl Pts',(2.40672355708034,-1.44083566359076,16.0655552884616));
#93836=CARTESIAN_POINT('Ctrl Pts',(2.5134845904627,1.24527944782968,16.2246201923077));
#93837=CARTESIAN_POINT('Ctrl Pts',(0.311752127397432,2.78767578831249,16.3836850961539));
#93838=CARTESIAN_POINT('Ctrl Pts',(-1.91350003226281,1.8772703365023,16.5259484014163));
#93839=CARTESIAN_POINT('Ctrl Pts',(-2.36566317652526,0.538737691428593,
16.6151900720633));
#93840=CARTESIAN_POINT('Ctrl Pts',(-2.36984887420079,-0.00195632190991717,
16.651410108095));
#93841=CARTESIAN_POINT('Ctrl Pts',(-2.36984864786026,-0.00195908838300039,
15.848589891905));
#93842=CARTESIAN_POINT('Ctrl Pts',(-2.37179223519786,-0.252766996446055,
15.8653910255024));
#93843=CARTESIAN_POINT('Ctrl Pts',(-2.21948393637844,-1.29295979284088,
15.9352255815954));
#93844=CARTESIAN_POINT('Ctrl Pts',(-0.706111029293687,-2.71494322962874,
16.0580935601843));
#93845=CARTESIAN_POINT('Ctrl Pts',(1.90232437254992,-2.06171567084302,16.2171938276716));
#93846=CARTESIAN_POINT('Ctrl Pts',(2.7628712320534,0.485851912509174,16.3762940951588));
#93847=CARTESIAN_POINT('Ctrl Pts',(1.08484420786421,2.58701035375983,16.5353943626462));
#93848=CARTESIAN_POINT('Ctrl Pts',(-1.56190831659987,2.31407131393373,16.6928262948949));
#93849=CARTESIAN_POINT('Ctrl Pts',(-2.37353776202774,0.761560422315232,
16.7972248046478));
#93850=CARTESIAN_POINT('Ctrl Pts',(-2.37556777218862,-0.000462349284400653,
16.848589891905));
#93851=CARTESIAN_POINT('Origin',(0.,0.,-1.84858989190512));
#93852=CARTESIAN_POINT('',(-2.37452997801752,0.00146346246222767,14.651410108095));
#93853=CARTESIAN_POINT('',(-2.36848771328686,0.00126209581994427,14.848589891905));
#93854=CARTESIAN_POINT('',(-2.37175,1.74448693060498E-12,-1.84858989190512));
#93855=CARTESIAN_POINT('Ctrl Pts',(-2.37452997801752,0.00146346246222774,
14.651410108095));
#93856=CARTESIAN_POINT('Ctrl Pts',(-2.36945739098401,-0.699707555274035,
14.6986187579608));
#93857=CARTESIAN_POINT('Ctrl Pts',(-1.66920288796294,-2.19719003397587,
14.7988490424419));
#93858=CARTESIAN_POINT('Ctrl Pts',(0.878381155370515,-2.66397677083911,
14.9521009615385));
#93859=CARTESIAN_POINT('Ctrl Pts',(2.7158539478379,-0.701757097359029,15.1111658653846));
#93860=CARTESIAN_POINT('Ctrl Pts',(2.05896843006344,1.90498679619639,15.2702307692308));
#93861=CARTESIAN_POINT('Ctrl Pts',(-0.488963186910485,2.76210801590502,
15.429295673077));
#93862=CARTESIAN_POINT('Ctrl Pts',(-2.16550513060297,1.42036197322363,15.5563554526983));
#93863=CARTESIAN_POINT('Ctrl Pts',(-2.37003849922212,0.315457549776884,
15.6303935977043));
#93864=CARTESIAN_POINT('Ctrl Pts',(-2.36850976199849,0.00127651360681887,
15.651410108095));
#93865=CARTESIAN_POINT('Ctrl Pts',(-2.36848771328686,0.00126209581994444,
14.848589891905));
#93866=CARTESIAN_POINT('Ctrl Pts',(-2.36619314536369,-0.476137104368745,
14.8805238238611));
#93867=CARTESIAN_POINT('Ctrl Pts',(-1.99411074642562,-1.74965427770411,
14.965491178313));
#93868=CARTESIAN_POINT('Ctrl Pts',(0.0863900949595627,-2.8039340714949,
15.1034919552607));
#93869=CARTESIAN_POINT('Ctrl Pts',(2.40561031446837,-1.44310378723102,15.2625922227479));
#93870=CARTESIAN_POINT('Ctrl Pts',(2.51451416171814,1.24367522139665,15.4216924902352));
#93871=CARTESIAN_POINT('Ctrl Pts',(0.313038897897693,2.78774392191968,15.5807927577225));
#93872=CARTESIAN_POINT('Ctrl Pts',(-1.91321060022851,1.87781928293776,15.7230918916124));
#93873=CARTESIAN_POINT('Ctrl Pts',(-2.36565722723337,0.53891778342454,15.8123576030066));
#93874=CARTESIAN_POINT('Ctrl Pts',(-2.36984864786026,-0.00195908838300039,
15.848589891905));
#93875=CARTESIAN_POINT('Origin',(0.,0.,-1.84858989190512));
#93876=CARTESIAN_POINT('',(-2.37308791222507,-0.00201426525716621,13.651410108095));
#93877=CARTESIAN_POINT('',(-2.37447897333966,0.00149556365171458,13.848589891905));
#93878=CARTESIAN_POINT('',(-2.37175,1.74448693060498E-12,-1.84858989190512));
#93879=CARTESIAN_POINT('Ctrl Pts',(-2.37308791222507,-0.00201426525716633,
13.651410108095));
#93880=CARTESIAN_POINT('Ctrl Pts',(-2.37435103224372,-0.141708936028309,
13.6608006489864));
#93881=CARTESIAN_POINT('Ctrl Pts',(-2.29944815507118,-1.06880604528595,
13.7232128244932));
#93882=CARTESIAN_POINT('Ctrl Pts',(-1.07773622411112,-2.58975101523663,
13.8386466346154));
#93883=CARTESIAN_POINT('Ctrl Pts',(1.59559205901132,-2.30703525566917,13.9977115384616));
#93884=CARTESIAN_POINT('Ctrl Pts',(2.80345924275497,0.094561957954597,14.1567764423077));
#93885=CARTESIAN_POINT('Ctrl Pts',(1.43650760564222,2.40930935925889,14.3158413461539));
#93886=CARTESIAN_POINT('Ctrl Pts',(-1.24979505427195,2.51124232442785,14.47490625));
#93887=CARTESIAN_POINT('Ctrl Pts',(-2.33164118373885,0.961011990247127,
14.5867625039804));
#93888=CARTESIAN_POINT('Ctrl Pts',(-2.37515458539669,0.0878013781735994,
14.6455971233454));
#93889=CARTESIAN_POINT('Ctrl Pts',(-2.37452997801752,0.00146346246222774,
14.651410108095));
#93890=CARTESIAN_POINT('Ctrl Pts',(-2.37447897333966,0.00149556365171451,
13.848589891905));
#93891=CARTESIAN_POINT('Ctrl Pts',(-2.36933692775314,-0.69760700066698,
13.8956566222199));
#93892=CARTESIAN_POINT('Ctrl Pts',(-1.67264639556168,-2.19334548761835,
13.9957567750306));
#93893=CARTESIAN_POINT('Ctrl Pts',(0.87190957086987,-2.66632391618547,14.148890350337));
#93894=CARTESIAN_POINT('Ctrl Pts',(2.71448594495469,-0.707866922832642,
14.3079906178242));
#93895=CARTESIAN_POINT('Ctrl Pts',(2.06294567416375,1.90099044480665,14.4670908853115));
#93896=CARTESIAN_POINT('Ctrl Pts',(-0.484064769522908,2.76318490599233,
14.6261911527988));
#93897=CARTESIAN_POINT('Ctrl Pts',(-2.16435474415049,1.42305090134789,14.75335748833));
#93898=CARTESIAN_POINT('Ctrl Pts',(-2.37000378760724,0.31669083543954,14.8274904013654));
#93899=CARTESIAN_POINT('Ctrl Pts',(-2.36848771328686,0.00126209581994444,
14.848589891905));
#93900=CARTESIAN_POINT('Origin',(0.,0.,-1.84858989190512));
#93901=CARTESIAN_POINT('',(-2.36791244388392,-0.000470842462512318,12.651410108095));
#93902=CARTESIAN_POINT('',(-2.3731890282555,-0.00199242475106415,12.848589891905));
#93903=CARTESIAN_POINT('',(-2.37175,1.74448693060498E-12,-1.84858989190512));
#93904=CARTESIAN_POINT('Ctrl Pts',(-2.36791244388392,-0.000470842462512201,
12.651410108095));
#93905=CARTESIAN_POINT('Ctrl Pts',(-2.36856283952937,-0.368365367608508,
12.6760041746274));
#93906=CARTESIAN_POINT('Ctrl Pts',(-2.11451705642467,-1.52854249033973,
12.7536198757752));
#93907=CARTESIAN_POINT('Ctrl Pts',(-0.301729257152967,-2.78877843240699,
12.8842572115385));
#93908=CARTESIAN_POINT('Ctrl Pts',(2.18265469599876,-1.76191491500441,13.0433221153847));
#93909=CARTESIAN_POINT('Ctrl Pts',(2.66239370729449,0.88316784194122,13.2023870192308));
#93910=CARTESIAN_POINT('Ctrl Pts',(0.696874616911946,2.71711086597222,13.361451923077));
#93911=CARTESIAN_POINT('Ctrl Pts',(-1.75486287047061,2.09459753855825,13.5111262860316));
#93912=CARTESIAN_POINT('Ctrl Pts',(-2.36721910141259,0.647046459105955,
13.607779014371));
#93913=CARTESIAN_POINT('Ctrl Pts',(-2.37308791222507,-0.00201426525716633,
13.651410108095));
#93914=CARTESIAN_POINT('Ctrl Pts',(-2.3731890282555,-0.00199242475106441,
12.848589891905));
#93915=CARTESIAN_POINT('Ctrl Pts',(-2.37441440680738,-0.138333347090684,
12.8577559980829));
#93916=CARTESIAN_POINT('Ctrl Pts',(-2.30157962306162,-1.06220937357195,
12.9199555267566));
#93917=CARTESIAN_POINT('Ctrl Pts',(-1.08818988647055,-2.58560482223799,
13.035188477926));
#93918=CARTESIAN_POINT('Ctrl Pts',(1.58696534358022,-2.31323378067855,13.1942887454133));
#93919=CARTESIAN_POINT('Ctrl Pts',(2.80398936259225,0.0845764758463313,
13.3533890129006));
#93920=CARTESIAN_POINT('Ctrl Pts',(1.44465944825848,2.40467640325151,13.5124892803878));
#93921=CARTESIAN_POINT('Ctrl Pts',(-1.24204855870295,2.51531805217969,13.6715895478751));
#93922=CARTESIAN_POINT('Ctrl Pts',(-2.33033692113347,0.965810161418643,
13.7836230850475));
#93923=CARTESIAN_POINT('Ctrl Pts',(-2.37513083513226,0.0901214311432274,
13.8426231997242));
#93924=CARTESIAN_POINT('Ctrl Pts',(-2.37447897333966,0.00149556365171451,
13.848589891905));
#93925=CARTESIAN_POINT('Origin',(0.,0.,-1.84858989190512));
#93926=CARTESIAN_POINT('',(-2.37135471886199,0.00218752354069527,11.651410108095));
#93927=CARTESIAN_POINT('',(-2.36793725144823,-0.00054391158261724,11.848589891905));
#93928=CARTESIAN_POINT('',(-2.37175,1.74448693060498E-12,-1.84858989190512));
#93929=CARTESIAN_POINT('Ctrl Pts',(-2.37135471886199,0.0021875235406953,
11.651410108095));
#93930=CARTESIAN_POINT('Ctrl Pts',(-2.36595594613634,-0.590956427613617,
11.6912077002684));
#93931=CARTESIAN_POINT('Ctrl Pts',(-1.8400272861403,-1.98287170359581,11.7840269270573));
#93932=CARTESIAN_POINT('Ctrl Pts',(0.498888975319622,-2.76033249446239,
11.9298677884616));
#93933=CARTESIAN_POINT('Ctrl Pts',(2.59168390408889,-1.07307978779166,12.0889326923077));
#93934=CARTESIAN_POINT('Ctrl Pts',(2.30416368784436,1.59973603738241,12.2479975961539));
#93935=CARTESIAN_POINT('Ctrl Pts',(-0.0996006097535288,2.80328475332372,
12.4070625));
#93936=CARTESIAN_POINT('Ctrl Pts',(-2.054369577301,1.64417118009386,12.5415333373137));
#93937=CARTESIAN_POINT('Ctrl Pts',(-2.36716067042395,0.424767767310423,
12.622982540012));
#93938=CARTESIAN_POINT('Ctrl Pts',(-2.36791244388392,-0.000470842462512201,
12.651410108095));
#93939=CARTESIAN_POINT('Ctrl Pts',(-2.36793725144823,-0.000543911582617518,
11.848589891905));
#93940=CARTESIAN_POINT('Ctrl Pts',(-2.36867974366206,-0.364013542241654,
11.8728887964417));
#93941=CARTESIAN_POINT('Ctrl Pts',(-2.11888156743286,-1.51980408948385,
11.9502211234741));
#93942=CARTESIAN_POINT('Ctrl Pts',(-0.316644893535377,-2.78733663865617,
12.0805868730024));
#93943=CARTESIAN_POINT('Ctrl Pts',(2.17376990917619,-1.7731987784107,12.2396871404896));
#93944=CARTESIAN_POINT('Ctrl Pts',(2.66688731468318,0.870184794500003,12.3987874079769));
#93945=CARTESIAN_POINT('Ctrl Pts',(0.709622520229888,2.71402752465403,12.5578876754642));
#93946=CARTESIAN_POINT('Ctrl Pts',(-1.74932962998056,2.10161421686923,12.7078218367736));
#93947=CARTESIAN_POINT('Ctrl Pts',(-2.3673245894741,0.650510421196307,12.8047225755872));
#93948=CARTESIAN_POINT('Ctrl Pts',(-2.3731890282555,-0.00199242475106441,
12.848589891905));
#93949=CARTESIAN_POINT('Origin',(0.,0.,-1.84858989190512));
#93950=CARTESIAN_POINT('',(-2.37552098982677,-0.000546054288011158,10.651410108095));
#93951=CARTESIAN_POINT('',(-2.37118699418392,0.00218308078960436,10.848589891905));
#93952=CARTESIAN_POINT('',(-2.37175,1.74448693060498E-12,-1.84858989190512));
#93953=CARTESIAN_POINT('Ctrl Pts',(-2.37552098982677,-0.000546054288011466,
10.651410108095));
#93954=CARTESIAN_POINT('Ctrl Pts',(-2.3756121895163,-0.0299140681072457,
10.6533895912941));
#93955=CARTESIAN_POINT('Ctrl Pts',(-2.36179446748901,-0.845833956636457,
10.7083907091086));
#93956=CARTESIAN_POINT('Ctrl Pts',(-1.4278375819202,-2.4144576056201,10.8164134615385));
#93957=CARTESIAN_POINT('Ctrl Pts',(1.25881414027309,-2.50673346208347,10.9754783653846));
#93958=CARTESIAN_POINT('Ctrl Pts',(2.78931624170351,-0.296716351840369,
11.1345432692308));
#93959=CARTESIAN_POINT('Ctrl Pts',(1.75798906916851,2.18581795270431,11.2936081730769));
#93960=CARTESIAN_POINT('Ctrl Pts',(-0.887951675457031,2.66080204294372,
11.4526730769231));
#93961=CARTESIAN_POINT('Ctrl Pts',(-2.26039623340362,1.18458115724447,11.5719403885958));
#93962=CARTESIAN_POINT('Ctrl Pts',(-2.37314863642732,0.199278863891932,
11.638186065653));
#93963=CARTESIAN_POINT('Ctrl Pts',(-2.37135471886199,0.0021875235406953,
11.651410108095));
#93964=CARTESIAN_POINT('Ctrl Pts',(-2.37118699418392,0.00218308078960424,
10.848589891905));
#93965=CARTESIAN_POINT('Ctrl Pts',(-2.36588268180612,-0.585613382676844,
10.8880215948005));
#93966=CARTESIAN_POINT('Ctrl Pts',(-1.84775089715974,-1.97231211609,10.9804867201917));
#93967=CARTESIAN_POINT('Ctrl Pts',(0.480489876761207,-2.76380878573882,
11.1259852680787));
#93968=CARTESIAN_POINT('Ctrl Pts',(2.58490043376768,-1.08986204324435,11.2850855355659));
#93969=CARTESIAN_POINT('Ctrl Pts',(2.31425975531301,1.58546879841127,11.4441858030532));
#93970=CARTESIAN_POINT('Ctrl Pts',(-0.0827628213498791,2.80404348061853,
11.6032860705405));
#93971=CARTESIAN_POINT('Ctrl Pts',(-2.04926540690783,1.65359163367153,11.7380874334911));
#93972=CARTESIAN_POINT('Ctrl Pts',(-2.36705922191318,0.429274832467547,
11.8198553739459));
#93973=CARTESIAN_POINT('Ctrl Pts',(-2.36793725144823,-0.000543911582617518,
11.848589891905));
#93974=CARTESIAN_POINT('Origin',(0.,0.,-1.84858989190512));
#93975=CARTESIAN_POINT('',(-2.36970451566036,-0.00191118876816796,9.65141010809495));
#93976=CARTESIAN_POINT('',(-2.37558458192292,-0.000424916937384612,9.84858989190501));
#93977=CARTESIAN_POINT('',(-2.37175,1.74448693060498E-12,-1.84858989190512));
#93978=CARTESIAN_POINT('Ctrl Pts',(-2.36970451566036,-0.00191118876816797,
9.65141010809495));
#93979=CARTESIAN_POINT('Ctrl Pts',(-2.37163637732688,-0.25845917027921,
9.6685931169351));
#93980=CARTESIAN_POINT('Ctrl Pts',(-2.21487175474487,-1.30434045260947,
9.73879776039063));
#93981=CARTESIAN_POINT('Ctrl Pts',(-0.687102918082009,-2.71959836550246,
9.86202403846154));
#93982=CARTESIAN_POINT('Ctrl Pts',(1.91606113164826,-2.04866674436504,10.0210889423077));
#93983=CARTESIAN_POINT('Ctrl Pts',(2.75943135650696,0.503849460063841,10.1801538461539));
#93984=CARTESIAN_POINT('Ctrl Pts',(1.06841988491078,2.59360842056154,10.33921875));
#93985=CARTESIAN_POINT('Ctrl Pts',(-1.57061947598469,2.30492249930711,10.496304170647));
#93986=CARTESIAN_POINT('Ctrl Pts',(-2.37316935159884,0.756725646134099,
10.6003679566787));
#93987=CARTESIAN_POINT('Ctrl Pts',(-2.37552098982677,-0.000546054288011466,
10.651410108095));
#93988=CARTESIAN_POINT('Ctrl Pts',(-2.37558458192292,-0.000424916937384534,
9.84858989190501));
#93989=CARTESIAN_POINT('Ctrl Pts',(-2.37564053070254,-0.0231386862569469,
9.85012097066349));
#93990=CARTESIAN_POINT('Ctrl Pts',(-2.36503969337732,-0.832557221286051,
9.90468547191772));
#93991=CARTESIAN_POINT('Ctrl Pts',(-1.44776895650877,-2.4028055631629,10.0122833956677));
#93992=CARTESIAN_POINT('Ctrl Pts',(1.23879367513383,-2.51692267585747,10.171383663155));
#93993=CARTESIAN_POINT('Ctrl Pts',(2.78713124782529,-0.318447693025035,
10.3304839306423));
#93994=CARTESIAN_POINT('Ctrl Pts',(1.77460441465207,2.1726225390745,10.4895841981295));
#93995=CARTESIAN_POINT('Ctrl Pts',(-0.868459654081467,2.66744959746755,
10.6486844656168));
#93996=CARTESIAN_POINT('Ctrl Pts',(-2.25627293082936,1.19617424730534,10.7683530302087));
#93997=CARTESIAN_POINT('Ctrl Pts',(-2.3730166836048,0.204939799141744,10.8349881723047));
#93998=CARTESIAN_POINT('Ctrl Pts',(-2.37118699418392,0.00218308078960424,
10.848589891905));
#93999=CARTESIAN_POINT('Origin',(0.,0.,-1.84858989190512));
#94000=CARTESIAN_POINT('',(-2.36860503817343,0.00135251512067538,8.65141010809494));
#94001=CARTESIAN_POINT('',(-2.36990159498818,-0.00197442701926287,8.84858989190502));
#94002=CARTESIAN_POINT('',(-2.37175,1.74448693060498E-12,-1.84858989190512));
#94003=CARTESIAN_POINT('Ctrl Pts',(-2.36860503817343,0.00135251512067523,
8.65141010809494));
#94004=CARTESIAN_POINT('Ctrl Pts',(-2.36610302129555,-0.482753094486701,
8.68379664257612));
#94005=CARTESIAN_POINT('Ctrl Pts',(-1.98600454178426,-1.76301994240106,
8.76920481167267));
#94006=CARTESIAN_POINT('Ctrl Pts',(0.109676931802227,-2.80290860719912,
8.90763461538463));
#94007=CARTESIAN_POINT('Ctrl Pts',(2.41702003317145,-1.42349564415503,9.06669951923077));
#94008=CARTESIAN_POINT('Ctrl Pts',(2.50446688033972,1.26331759069596,9.22576442307694));
#94009=CARTESIAN_POINT('Ctrl Pts',(0.291702487991934,2.78984504017334,9.38482932692308));
#94010=CARTESIAN_POINT('Ctrl Pts',(-1.92099870206075,1.86594863561955,9.52671122192909));
#94011=CARTESIAN_POINT('Ctrl Pts',(-2.36567522905754,0.53317129814093,9.61557148231971));
#94012=CARTESIAN_POINT('Ctrl Pts',(-2.36970451566036,-0.00191118876816797,
9.65141010809495));
#94013=CARTESIAN_POINT('Ctrl Pts',(-2.36990159498818,-0.00197442701926287,
8.84858989190501));
#94014=CARTESIAN_POINT('Ctrl Pts',(-2.37184739597465,-0.250719344876404,
8.86525376902227));
#94015=CARTESIAN_POINT('Ctrl Pts',(-2.2211351990105,-1.28880604443534,8.93495106863528));
#94016=CARTESIAN_POINT('Ctrl Pts',(-0.713132823661497,-2.71310727794049,
9.05768179074405));
#94017=CARTESIAN_POINT('Ctrl Pts',(1.89698389204465,-2.06663050377184,9.21678205823132));
#94018=CARTESIAN_POINT('Ctrl Pts',(2.76411899128539,0.478702128481346,9.37588232571861));
#94019=CARTESIAN_POINT('Ctrl Pts',(1.09153374406576,2.5841949638839,9.53498259320587));
#94020=CARTESIAN_POINT('Ctrl Pts',(-1.558224245524,2.31787258077939,9.6925517819347));
#94021=CARTESIAN_POINT('Ctrl Pts',(-2.37370257992687,0.763619616102294,
9.79708754816773));
#94022=CARTESIAN_POINT('Ctrl Pts',(-2.37558458192292,-0.000424916937384534,
9.84858989190501));
#94023=CARTESIAN_POINT('Origin',(0.,0.,-1.84858989190512));
#94024=CARTESIAN_POINT('',(-2.37466060251227,0.00138507137951498,7.65141010809495));
#94025=CARTESIAN_POINT('',(-2.3684552380494,0.00123397076206691,7.84858989190501));
#94026=CARTESIAN_POINT('',(-2.37175,1.74448693060498E-12,-1.84858989190512));
#94027=CARTESIAN_POINT('Ctrl Pts',(-2.37466060251227,0.00138507137951483,
7.65141010809495));
#94028=CARTESIAN_POINT('Ctrl Pts',(-2.36976305923354,-0.705348722947108,
7.69900016821715));
#94029=CARTESIAN_POINT('Ctrl Pts',(-1.65971194045233,-2.20801762144576,
7.79961186295472));
#94030=CARTESIAN_POINT('Ctrl Pts',(0.897510721516925,-2.65759293241885,
7.9532451923077));
#94031=CARTESIAN_POINT('Ctrl Pts',(2.72082893886257,-0.682213731266401,
8.11231009615385));
#94032=CARTESIAN_POINT('Ctrl Pts',(2.04521959797142,1.91974021308981,8.27137500000001));
#94033=CARTESIAN_POINT('Ctrl Pts',(-0.508808317133133,2.75852130426731,
8.43043990384615));
#94034=CARTESIAN_POINT('Ctrl Pts',(-2.17065706179093,1.40882044126061,8.55711827321115));
#94035=CARTESIAN_POINT('Ctrl Pts',(-2.37019919974828,0.309800698596051,
8.63077500796074));
#94036=CARTESIAN_POINT('Ctrl Pts',(-2.36860503817343,0.00135251512067523,
8.65141010809494));
#94037=CARTESIAN_POINT('Ctrl Pts',(-2.3684552380494,0.00123397076206695,
7.84858989190502));
#94038=CARTESIAN_POINT('Ctrl Pts',(-2.36622324530222,-0.474129605566998,
7.88038656738104));
#94039=CARTESIAN_POINT('Ctrl Pts',(-1.99656425442517,-1.7455431608208,7.96521666535284));
#94040=CARTESIAN_POINT('Ctrl Pts',(0.0791354092423232,-2.80414819736781,
8.10308018582037));
#94041=CARTESIAN_POINT('Ctrl Pts',(2.40186863507383,-1.44932280243071,8.26218045330766));
#94042=CARTESIAN_POINT('Ctrl Pts',(2.51772340840239,1.23716545562014,8.42128072079493));
#94043=CARTESIAN_POINT('Ctrl Pts',(0.320250359289559,2.78692469097606,8.58038098828221));
#94044=CARTESIAN_POINT('Ctrl Pts',(-1.9104954853186,1.8818907754002,8.72281737865224));
#94045=CARTESIAN_POINT('Ctrl Pts',(-2.36565481035475,0.54092081362753,8.81222034652651));
#94046=CARTESIAN_POINT('Ctrl Pts',(-2.36990159498818,-0.00197442701926287,
8.84858989190501));
#94047=CARTESIAN_POINT('Origin',(0.,0.,-1.84858989190512));
#94048=CARTESIAN_POINT('',(-2.37291859965002,-0.00205150633385966,6.65141010809495));
#94049=CARTESIAN_POINT('',(-2.3744297718001,0.00152245248726483,6.84858989190502));
#94050=CARTESIAN_POINT('',(-2.37175,1.74448693060498E-12,-1.84858989190512));
#94051=CARTESIAN_POINT('Ctrl Pts',(-2.37291859965002,-0.00205150633385984,
6.65141010809495));
#94052=CARTESIAN_POINT('Ctrl Pts',(-2.3742459582117,-0.147446862522116,
6.66118205924279));
#94053=CARTESIAN_POINT('Ctrl Pts',(-2.29577744667903,-1.08031369136468,
6.72397564500602));
#94054=CARTESIAN_POINT('Ctrl Pts',(-1.05908973969091,-2.5974323115265,6.83979086538461));
#94055=CARTESIAN_POINT('Ctrl Pts',(1.61213691155191,-2.29550436028606,6.99885576923078));
#94056=CARTESIAN_POINT('Ctrl Pts',(2.80270695172092,0.114714569500639,7.15792067307693));
#94057=CARTESIAN_POINT('Ctrl Pts',(1.41914910781753,2.41957465259107,7.31698557692308));
#94058=CARTESIAN_POINT('Ctrl Pts',(-1.26781695999829,2.50219220796908,7.47605048076923));
#94059=CARTESIAN_POINT('Ctrl Pts',(-2.33483917126496,0.949536563310053,
7.5875253244932));
#94060=CARTESIAN_POINT('Ctrl Pts',(-2.37521957157186,0.0820463952122587,
7.64597853360177));
#94061=CARTESIAN_POINT('Ctrl Pts',(-2.37466060251227,0.00138507137951483,
7.65141010809495));
#94062=CARTESIAN_POINT('Ctrl Pts',(-2.3744297718001,0.00152245248726472,
6.84858989190502));
#94063=CARTESIAN_POINT('Ctrl Pts',(-2.36923206465993,-0.695579259077515,
6.89551936573982));
#94064=CARTESIAN_POINT('Ctrl Pts',(-1.67603583801615,-2.18944047996094,
6.99548226207037));
#94065=CARTESIAN_POINT('Ctrl Pts',(0.865008283985421,-2.66857081495577,
7.14847858089671));
#94066=CARTESIAN_POINT('Ctrl Pts',(2.71264545191261,-0.714887528227297,
7.30757884838397));
#94067=CARTESIAN_POINT('Ctrl Pts',(2.0678570518103,1.89564678647566,7.46667911587126));
#94068=CARTESIAN_POINT('Ctrl Pts',(-0.476914179932666,2.76442804044096,
7.62577938335854));
#94069=CARTESIAN_POINT('Ctrl Pts',(-2.162483104034,1.42720403096667,7.75308297536978));
#94070=CARTESIAN_POINT('Ctrl Pts',(-2.36994596827865,0.318725528032169,
7.82735314488528));
#94071=CARTESIAN_POINT('Ctrl Pts',(-2.3684552380494,0.00123397076206695,
7.84858989190502));
#94072=CARTESIAN_POINT('Origin',(0.,0.,-1.84858989190512));
#94073=CARTESIAN_POINT('',(-2.36788211521185,-0.000378178454202572,5.65141010809494));
#94074=CARTESIAN_POINT('',(-2.37324908705979,-0.00197702543379558,5.84858989190501));
#94075=CARTESIAN_POINT('',(-2.37175,1.74448693060498E-12,-1.84858989190512));
#94076=CARTESIAN_POINT('Ctrl Pts',(-2.36788211521185,-0.000378178454202779,
5.65141010809495));
#94077=CARTESIAN_POINT('Ctrl Pts',(-2.36841223428828,-0.373990025746932,
5.67638558488381));
#94078=CARTESIAN_POINT('Ctrl Pts',(-2.10879213104349,-1.54006374105855,
5.75438269628806));
#94079=CARTESIAN_POINT('Ctrl Pts',(-0.281671949479292,-2.79087559782923,
5.8854014423077));
#94080=CARTESIAN_POINT('Ctrl Pts',(2.19526531462978,-1.74617750760439,6.04446634615385));
#94081=CARTESIAN_POINT('Ctrl Pts',(2.65597549661169,0.902285903180645,6.20353125));
#94082=CARTESIAN_POINT('Ctrl Pts',(0.677322340573879,2.7220507226428,6.36259615384616));
#94083=CARTESIAN_POINT('Ctrl Pts',(-1.76364020147583,2.08355828545319,6.51188910654447));
#94084=CARTESIAN_POINT('Ctrl Pts',(-2.36704384272867,0.641453873263,6.6081604246274));
#94085=CARTESIAN_POINT('Ctrl Pts',(-2.37291859965002,-0.00205150633385984,
6.65141010809495));
#94086=CARTESIAN_POINT('Ctrl Pts',(-2.37324908705979,-0.00197702543379559,
5.84858989190501));
#94087=CARTESIAN_POINT('Ctrl Pts',(-2.37445062243721,-0.136267538027153,
5.85761874160283));
#94088=CARTESIAN_POINT('Ctrl Pts',(-2.302879494702,-1.05806940655756,5.91968101379641));
#94089=CARTESIAN_POINT('Ctrl Pts',(-1.09487577505419,-2.58278078105689,
6.03477670848575));
#94090=CARTESIAN_POINT('Ctrl Pts',(1.58097518564988,-2.31733186836853,6.19387697597303));
#94091=CARTESIAN_POINT('Ctrl Pts',(2.80419879604699,0.0773216531487339,
6.3529772434603));
#94092=CARTESIAN_POINT('Ctrl Pts',(1.45087604201706,2.40093070214407,6.51207751094759));
#94093=CARTESIAN_POINT('Ctrl Pts',(-1.23553671852851,2.51852308763786,6.67117777843485));
#94094=CARTESIAN_POINT('Ctrl Pts',(-2.32916856749468,0.969941120947585,
6.78334857208735));
#94095=CARTESIAN_POINT('Ctrl Pts',(-2.37510581896078,0.0921919765870843,
6.84248594324406));
#94096=CARTESIAN_POINT('Ctrl Pts',(-2.3744297718001,0.00152245248726472,
6.84858989190502));
#94097=CARTESIAN_POINT('Origin',(0.,0.,-1.84858989190512));
#94098=CARTESIAN_POINT('',(-2.37152629080235,0.002190319628347,4.65141010809494));
#94099=CARTESIAN_POINT('',(-2.36795166666981,-0.000576822865031718,4.84858989190501));
#94100=CARTESIAN_POINT('',(-2.37175,1.74448693060498E-12,-1.84858989190512));
#94101=CARTESIAN_POINT('Ctrl Pts',(-2.37152629080235,0.00219031962834669,
4.65141010809494));
#94102=CARTESIAN_POINT('Ctrl Pts',(-2.36603445450948,-0.596527709585613,
4.69158911052483));
#94103=CARTESIAN_POINT('Ctrl Pts',(-1.83185547982759,-1.99405983737433,
4.78478974757012));
#94104=CARTESIAN_POINT('Ctrl Pts',(0.518721084171678,-2.75667446873791,
4.93101201923077));
#94105=CARTESIAN_POINT('Ctrl Pts',(2.59933167366719,-1.05441952748531,5.09007692307692));
#94106=CARTESIAN_POINT('Ctrl Pts',(2.29260307415327,1.61626013811133,5.24914182692309));
#94107=CARTESIAN_POINT('Ctrl Pts',(-0.119751836615735,2.80249624215965,
5.40820673076923));
#94108=CARTESIAN_POINT('Ctrl Pts',(-2.06061632414504,1.63268656403164,5.54229615782653));
#94109=CARTESIAN_POINT('Ctrl Pts',(-2.36728681913762,0.419168440159318,
5.62336395026843));
#94110=CARTESIAN_POINT('Ctrl Pts',(-2.36788211521185,-0.000378178454202779,
5.65141010809495));
#94111=CARTESIAN_POINT('Ctrl Pts',(-2.36795166666981,-0.000576822865031856,
4.84858989190501));
#94112=CARTESIAN_POINT('Ctrl Pts',(-2.36873490379575,-0.361987846498752,
4.87275153996161));
#94113=CARTESIAN_POINT('Ctrl Pts',(-2.12091250633926,-1.5156564236008,4.94994661051396));
#94114=CARTESIAN_POINT('Ctrl Pts',(-0.323855289127461,-2.78650807957066,
5.08017510356208));
#94115=CARTESIAN_POINT('Ctrl Pts',(2.16917497708905,-1.77881686650588,5.23927537104935));
#94116=CARTESIAN_POINT('Ctrl Pts',(2.66912974919035,0.863282055751294,5.39837563853664));
#94117=CARTESIAN_POINT('Ctrl Pts',(0.716641933714364,2.71218249102838,5.55747590602391));
#94118=CARTESIAN_POINT('Ctrl Pts',(-1.74613891360093,2.10557828017548,5.70754732381337));
#94119=CARTESIAN_POINT('Ctrl Pts',(-2.36739307519176,0.652524581666242,
5.80458531910707));
#94120=CARTESIAN_POINT('Ctrl Pts',(-2.37324908705979,-0.00197702543379559,
5.84858989190501));
#94121=CARTESIAN_POINT('Origin',(0.,0.,-1.84858989190512));
#94122=CARTESIAN_POINT('',(-2.37545952780932,-0.000647831802807195,3.65141010809494));
#94123=CARTESIAN_POINT('',(-2.37112606337681,0.0021794697323349,3.84858989190501));
#94124=CARTESIAN_POINT('',(-2.37175,1.74448693060498E-12,-1.84858989190512));
#94125=CARTESIAN_POINT('Ctrl Pts',(-2.37545952780932,-0.000647831802807618,
3.65141010809494));
#94126=CARTESIAN_POINT('Ctrl Pts',(-2.37558652664713,-0.0356769482557227,
3.65377100155047));
#94127=CARTESIAN_POINT('Ctrl Pts',(-2.35898981085398,-0.857277173788602,
3.70915352962139));
#94128=CARTESIAN_POINT('Ctrl Pts',(-1.41044229536976,-2.42466043275193,
3.8175576923077));
#94129=CARTESIAN_POINT('Ctrl Pts',(1.27680339699028,-2.49761862144671,3.97662259615385));
#94130=CARTESIAN_POINT('Ctrl Pts',(2.79137735375039,-0.276655306861728,
4.1356875));
#94131=CARTESIAN_POINT('Ctrl Pts',(1.74222902142711,2.19840026511027,4.29475240384616));
#94132=CARTESIAN_POINT('Ctrl Pts',(-0.907058170011317,2.65434948083033,
4.45381730769232));
#94133=CARTESIAN_POINT('Ctrl Pts',(-2.26449923905453,1.17305206370316,4.57270320910857));
#94134=CARTESIAN_POINT('Ctrl Pts',(-2.37328167618444,0.193561806400188,
4.63856747590945));
#94135=CARTESIAN_POINT('Ctrl Pts',(-2.37152629080235,0.00219031962834669,
4.65141010809494));
#94136=CARTESIAN_POINT('Ctrl Pts',(-2.37112606337681,0.0021794697323349,
3.84858989190501));
#94137=CARTESIAN_POINT('Ctrl Pts',(-2.36586016382344,-0.583609254788488,
3.88788433832038));
#94138=CARTESIAN_POINT('Ctrl Pts',(-1.85065310628272,-1.96827731595091,
3.98021220723151));
#94139=CARTESIAN_POINT('Ctrl Pts',(0.473337684987186,-2.76504266915617,
4.12557349863841));
#94140=CARTESIAN_POINT('Ctrl Pts',(2.58207206872294,-1.09654610377387,4.28467376612568));
#94141=CARTESIAN_POINT('Ctrl Pts',(2.31835396766711,1.57947599104097,4.44377403361296));
#94142=CARTESIAN_POINT('Ctrl Pts',(-0.075507864702191,2.804248221581,4.60287430110024));
#94143=CARTESIAN_POINT('Ctrl Pts',(-2.04698568380069,1.65772178093785,4.73781292053093));
#94144=CARTESIAN_POINT('Ctrl Pts',(-2.36701574352502,0.431288484076751,
4.81971811746585));
#94145=CARTESIAN_POINT('Ctrl Pts',(-2.36795166666981,-0.000576822865031856,
4.84858989190501));
#94146=CARTESIAN_POINT('Origin',(0.,0.,-1.84858989190512));
#94147=CARTESIAN_POINT('',(-2.36956417455327,-0.00186242956101223,2.65141010809494));
#94148=CARTESIAN_POINT('',(-2.37560005937361,-0.000387335438401248,2.84858989190501));
#94149=CARTESIAN_POINT('',(-2.37175,1.74448693060498E-12,-1.84858989190512));
#94150=CARTESIAN_POINT('Ctrl Pts',(-2.36956417455326,-0.00186242956101212,
2.65141010809494));
#94151=CARTESIAN_POINT('Ctrl Pts',(-2.37148092984202,-0.264144138683627,
2.6689745271915));
#94152=CARTESIAN_POINT('Ctrl Pts',(-2.21019729025586,-1.31588391544579,
2.73956058090345));
#94153=CARTESIAN_POINT('Ctrl Pts',(-0.667532999398916,-2.7244678431737,
2.86316826923077));
#94154=CARTESIAN_POINT('Ctrl Pts',(1.93074019393295,-2.03483859399145,3.02223317307692));
#94155=CARTESIAN_POINT('Ctrl Pts',(2.75573769451142,0.523674979307748,3.18129807692308));
#94156=CARTESIAN_POINT('Ctrl Pts',(1.04974590737629,2.60122262971082,3.34036298076923));
#94157=CARTESIAN_POINT('Ctrl Pts',(-1.5807472859228,2.2943181908652,3.49706699115986));
#94158=CARTESIAN_POINT('Ctrl Pts',(-2.37273434966335,0.751017177696373,
3.60074936693509));
#94159=CARTESIAN_POINT('Ctrl Pts',(-2.37545952780932,-0.000647831802807618,
3.65141010809494));
#94160=CARTESIAN_POINT('Ctrl Pts',(-2.37560005937361,-0.000387335438401326,
2.84858989190501));
#94161=CARTESIAN_POINT('Ctrl Pts',(-2.37564677277175,-0.0210645241833399,
2.8499837141834));
#94162=CARTESIAN_POINT('Ctrl Pts',(-2.3660208670964,-0.828441659307457,
2.90441095895754));
#94163=CARTESIAN_POINT('Ctrl Pts',(-1.45398069647754,-2.39905181471807,
3.01187162622745));
#94164=CARTESIAN_POINT('Ctrl Pts',(1.23227769270891,-2.52011928935842,3.17097189371473));
#94165=CARTESIAN_POINT('Ctrl Pts',(2.78629802603849,-0.325657548824043,
3.330072161202));
#94166=CARTESIAN_POINT('Ctrl Pts',(1.78021952909652,2.16802397289482,3.48917242868929));
#94167=CARTESIAN_POINT('Ctrl Pts',(-0.861555466122802,2.66968756742434,
3.64827269617656));
#94168=CARTESIAN_POINT('Ctrl Pts',(-2.25476675598426,1.20032433252879,3.76807851724848));
#94169=CARTESIAN_POINT('Ctrl Pts',(-2.37296724131938,0.206995620831109,
3.83485091582462));
#94170=CARTESIAN_POINT('Ctrl Pts',(-2.37112606337681,0.0021794697323349,
3.84858989190501));
#94171=CARTESIAN_POINT('Origin',(0.,0.,-1.84858989190512));
#94172=CARTESIAN_POINT('',(-2.36870542925002,0.0014289424853233,1.65141010809494));
#94173=CARTESIAN_POINT('',(-2.36995499373098,-0.00198919729222008,1.84858989190501));
#94174=CARTESIAN_POINT('',(-2.37175,1.74448693060498E-12,-1.84858989190512));
#94175=CARTESIAN_POINT('Ctrl Pts',(-2.36870542925002,0.00142894248532303,
1.65141010809494));
#94176=CARTESIAN_POINT('Ctrl Pts',(-2.36602971570103,-0.488326778583579,
1.68417805283253));
#94177=CARTESIAN_POINT('Ctrl Pts',(-1.97907368647692,-1.77443351813344,
1.7699676321855));
#94178=CARTESIAN_POINT('Ctrl Pts',(0.12982574190393,-2.80204465094187,1.90877884615384));
#94179=CARTESIAN_POINT('Ctrl Pts',(2.42719129243389,-1.40608362715869,2.06784375));
#94180=CARTESIAN_POINT('Ctrl Pts',(2.49531987128246,1.28129126381962,2.22690865384615));
#94181=CARTESIAN_POINT('Ctrl Pts',(0.271637692292844,2.79186965803179,2.38597355769231));
#94182=CARTESIAN_POINT('Ctrl Pts',(-1.92843376376444,1.85461617100725,2.5274740424419));
#94183=CARTESIAN_POINT('Ctrl Pts',(-2.36569482908863,0.527604502187907,
2.61595289257612));
#94184=CARTESIAN_POINT('Ctrl Pts',(-2.36956417455326,-0.00186242956101212,
2.65141010809494));
#94185=CARTESIAN_POINT('Ctrl Pts',(-2.36995499373098,-0.00198919729222004,
1.84858989190501));
#94186=CARTESIAN_POINT('Ctrl Pts',(-2.37190237644613,-0.248671344879013,
1.86511651254217));
#94187=CARTESIAN_POINT('Ctrl Pts',(-2.22278002190394,-1.28465291067756,
1.93467655567509));
#94188=CARTESIAN_POINT('Ctrl Pts',(-0.720149694819682,-2.71125275032746,
2.05727002130378));
#94189=CARTESIAN_POINT('Ctrl Pts',(1.89163063518288,-2.07153172086814,2.21637028879105));
#94190=CARTESIAN_POINT('Ctrl Pts',(2.76534828940725,0.471549254232345,2.37547055627834));
#94191=CARTESIAN_POINT('Ctrl Pts',(1.09821595227919,2.58136221632247,2.53457082376561));
#94192=CARTESIAN_POINT('Ctrl Pts',(-1.55453093352958,2.3216703064687,2.69227726897451));
#94193=CARTESIAN_POINT('Ctrl Pts',(-2.37386937875385,0.765680029795463,
2.79695029168764));
#94194=CARTESIAN_POINT('Ctrl Pts',(-2.37560005937361,-0.000387335438401326,
2.84858989190501));
#94195=CARTESIAN_POINT('Origin',(0.,0.,-1.84858989190512));
#94196=CARTESIAN_POINT('',(-2.37475566780996,0.00146584572226412,0.651410108094944));
#94197=CARTESIAN_POINT('',(-2.36841685556579,0.00122403911035851,0.848589891905012));
#94198=CARTESIAN_POINT('',(-2.37175,1.74448693060498E-12,-1.84858989190512));
#94199=CARTESIAN_POINT('Ctrl Pts',(-2.37475566780996,0.00146584572226396,
0.651410108094944));
#94200=CARTESIAN_POINT('Ctrl Pts',(-2.37004404586893,-0.710785278156698,
0.699381578473552));
#94201=CARTESIAN_POINT('Ctrl Pts',(-1.65019917004401,-2.21908588862768,
0.800374683467544));
#94202=CARTESIAN_POINT('Ctrl Pts',(0.916620294059412,-2.65092658244327,
0.954389423076924));
#94203=CARTESIAN_POINT('Ctrl Pts',(2.72564945922899,-0.662711191614906,
1.11345432692308));
#94204=CARTESIAN_POINT('Ctrl Pts',(2.03137230801958,1.93443429127041,1.27251923076923));
#94205=CARTESIAN_POINT('Ctrl Pts',(-0.528630951316314,2.75477110121152,
1.43158413461539));
#94206=CARTESIAN_POINT('Ctrl Pts',(-2.17575442924696,1.39728243218704,1.55788109372396));
#94207=CARTESIAN_POINT('Ctrl Pts',(-2.37035927336069,0.304144311723338,
1.63115641821714));
#94208=CARTESIAN_POINT('Ctrl Pts',(-2.36870542925002,0.00142894248532303,
1.65141010809494));
#94209=CARTESIAN_POINT('Ctrl Pts',(-2.36841685556579,0.00122403911035841,
0.848589891905012));
#94210=CARTESIAN_POINT('Ctrl Pts',(-2.36625022962319,-0.472111298629738,
0.880249310900949));
#94211=CARTESIAN_POINT('Ctrl Pts',(-1.99902079532434,-1.74146140232311,
0.964942152392647));
#94212=CARTESIAN_POINT('Ctrl Pts',(0.0718874078444588,-2.8043235471302,
1.1026684163801));
#94213=CARTESIAN_POINT('Ctrl Pts',(2.39810709656883,-1.45554260356973,1.26176868386738));
#94214=CARTESIAN_POINT('Ctrl Pts',(2.52091778453322,1.23065290615308,1.42086895135466));
#94215=CARTESIAN_POINT('Ctrl Pts',(0.327458637825707,2.78608392325822,1.57996921884194));
#94216=CARTESIAN_POINT('Ctrl Pts',(-1.90777171460039,1.8859618485243,1.72254286569206));
#94217=CARTESIAN_POINT('Ctrl Pts',(-2.36565328459846,0.542924156848317,
1.81208309004641));
#94218=CARTESIAN_POINT('Ctrl Pts',(-2.36995499373098,-0.00198919729222004,
1.84858989190501));
#94219=CARTESIAN_POINT('Origin',(0.,0.,49.5));
#94220=CARTESIAN_POINT('',(-2.86956349206012,0.00162216627751805,49.1339652973708));
#94221=CARTESIAN_POINT('Ctrl Pts',(-0.439445221993838,2.33068358199194,
49.62825));
#94222=CARTESIAN_POINT('Ctrl Pts',(-0.359505261208484,2.34930630909117,
49.6247612467635));
#94223=CARTESIAN_POINT('Ctrl Pts',(-0.278760108098212,2.36340128745442,
49.6212867191599));
#94224=CARTESIAN_POINT('Ctrl Pts',(-0.197534229629186,2.37315541881725,
49.6178216918657));
#94225=CARTESIAN_POINT('Ctrl Pts',(-0.114150649388022,2.3831686610315,49.6142646188385));
#94226=CARTESIAN_POINT('Ctrl Pts',(-0.0302597106601846,2.38860739990529,
49.6107175575613));
#94227=CARTESIAN_POINT('Ctrl Pts',(0.0538029108463651,2.38962152881013,
49.6071753960455));
#94228=CARTESIAN_POINT('Ctrl Pts',(0.0939026325081102,2.3901052906306,49.605485706998));
#94229=CARTESIAN_POINT('Ctrl Pts',(0.134041570065805,2.38958147509166,49.6037971328912));
#94230=CARTESIAN_POINT('Ctrl Pts',(0.174183675497746,2.38806230251539,49.6021091188373));
#94231=CARTESIAN_POINT('Ctrl Pts',(0.198287612532619,2.3871500922631,49.6010955251549));
#94232=CARTESIAN_POINT('Ctrl Pts',(0.222392693138791,2.3858789481315,49.6000821334042));
#94233=CARTESIAN_POINT('Ctrl Pts',(0.24649108949659,2.38425107690571,49.5990688234506));
#94234=CARTESIAN_POINT('Ctrl Pts',(0.262231163126216,2.38318781889581,49.5984069713903));
#94235=CARTESIAN_POINT('Ctrl Pts',(0.277969056250135,2.38197221991301,49.5977451258474));
#94236=CARTESIAN_POINT('Ctrl Pts',(0.293686527897986,2.3806064861569,49.5970839288824));
#94237=CARTESIAN_POINT('Ctrl Pts',(0.379432205080258,2.37315581162149,49.5934768104613));
#94238=CARTESIAN_POINT('Ctrl Pts',(0.464683129359647,2.36123436880514,49.5898842179419));
#94239=CARTESIAN_POINT('Ctrl Pts',(0.549087259753569,2.34500689677144,49.5863009155998));
#94240=CARTESIAN_POINT('Ctrl Pts',(0.634238389507191,2.32863580722564,49.5826859000639));
#94241=CARTESIAN_POINT('Ctrl Pts',(0.71852862073425,2.30788198144388,49.5790803398741));
#94242=CARTESIAN_POINT('Ctrl Pts',(0.801595693877686,2.28286147762408,49.5754788590594));
#94243=CARTESIAN_POINT('Ctrl Pts',(0.854183456323832,2.26702159954283,49.5731988483359));
#94244=CARTESIAN_POINT('Ctrl Pts',(0.906280934573225,2.249470645855,49.5709204725652));
#94245=CARTESIAN_POINT('Ctrl Pts',(0.957793381125661,2.23022763047868,49.5686423677162));
#94246=CARTESIAN_POINT('Ctrl Pts',(0.971987759697525,2.22492517129849,49.5680146304446));
#94247=CARTESIAN_POINT('Ctrl Pts',(0.986130767173139,2.21949673426825,49.567387219577));
#94248=CARTESIAN_POINT('Ctrl Pts',(1.00021413720228,2.21394563250679,49.566760392062));
#94249=CARTESIAN_POINT('Ctrl Pts',(1.08183853281852,2.18177255707487,49.5631274251686));
#94250=CARTESIAN_POINT('Ctrl Pts',(1.16152778287534,2.1454580421936,49.5595110591734));
#94251=CARTESIAN_POINT('Ctrl Pts',(1.23892280784953,2.10514980872508,49.5559059771857));
#94252=CARTESIAN_POINT('Ctrl Pts',(1.31588775121095,2.06506556678656,49.5523209285203));
#94253=CARTESIAN_POINT('Ctrl Pts',(1.39058484076766,2.02103157966364,49.5487470388013));
#94254=CARTESIAN_POINT('Ctrl Pts',(1.46264758633523,1.97314377781481,49.5451790792837));
#94255=CARTESIAN_POINT('Ctrl Pts',(1.52263782893736,1.93327850723751,49.5422088516665));
#94256=CARTESIAN_POINT('Ctrl Pts',(1.58080248046675,1.89074157080871,49.5392427337394));
#94257=CARTESIAN_POINT('Ctrl Pts',(1.63691585662181,1.8455640580499,49.5362777089777));
#94258=CARTESIAN_POINT('Ctrl Pts',(1.66497254469934,1.82297530167049,49.5347951965969));
#94259=CARTESIAN_POINT('Ctrl Pts',(1.69251617012281,1.79972606657414,49.5333129575074));
#94260=CARTESIAN_POINT('Ctrl Pts',(1.71951680922542,1.77581828500007,49.5318306146436));
#94261=CARTESIAN_POINT('Ctrl Pts',(1.73353427516679,1.76340648568396,49.531061051726));
#94262=CARTESIAN_POINT('Ctrl Pts',(1.74740537466393,1.75081717401828,49.5302914608391));
#94263=CARTESIAN_POINT('Ctrl Pts',(1.76112577636582,1.7380504867577,49.5295217892232));
#94264=CARTESIAN_POINT('Ctrl Pts',(1.76984010737801,1.72994189481303,49.5290329425132));
#94265=CARTESIAN_POINT('Ctrl Pts',(1.77849214411516,1.72176307914284,49.5285441456439));
#94266=CARTESIAN_POINT('Ctrl Pts',(1.78707439365716,1.71352049619226,49.5280557560924));
#94267=CARTESIAN_POINT('Ctrl Pts',(1.79100755903657,1.70974299686188,49.5278319316899));
#94268=CARTESIAN_POINT('Ctrl Pts',(1.79492646082255,1.70595173973429,49.5276081707935));
#94269=CARTESIAN_POINT('Ctrl Pts',(1.79883101418844,1.70214675534458,49.5273844721621));
#94270=CARTESIAN_POINT('Ctrl Pts',(1.85864861208173,1.64385455009475,49.5239574182779));
#94271=CARTESIAN_POINT('Ctrl Pts',(1.91510096641586,1.58234433908994,49.5205449780736));
#94272=CARTESIAN_POINT('Ctrl Pts',(1.96816958093575,1.51800814503369,49.5171426893277));
#94273=CARTESIAN_POINT('Ctrl Pts',(2.02278845482118,1.45179253904477,49.5136410117049));
#94274=CARTESIAN_POINT('Ctrl Pts',(2.07382343813989,1.38258284038499,49.5101500872995));
#94275=CARTESIAN_POINT('Ctrl Pts',(2.12122068206654,1.31076313229951,49.5066650512987));
#94276=CARTESIAN_POINT('Ctrl Pts',(2.16728133943421,1.24096871616235,49.5032782921573));
#94277=CARTESIAN_POINT('Ctrl Pts',(2.20990663387466,1.16870853483454,49.4998970940011));
#94278=CARTESIAN_POINT('Ctrl Pts',(2.24901234132568,1.0943063482077,49.4965169920791));
#94279=CARTESIAN_POINT('Ctrl Pts',(2.2661210883355,1.06175539155845,49.4950381974882));
#94280=CARTESIAN_POINT('Ctrl Pts',(2.28255569813228,1.02879414143743,49.4935596127234));
#94281=CARTESIAN_POINT('Ctrl Pts',(2.29830685053076,0.995448545649893,49.4920808639053));
#94282=CARTESIAN_POINT('Ctrl Pts',(2.30471320039571,0.981886137791351,49.4914794233217));
#94283=CARTESIAN_POINT('Ctrl Pts',(2.31100647394448,0.96826014379224,49.4908779555999));
#94284=CARTESIAN_POINT('Ctrl Pts',(2.31718597494133,0.954572285797792,49.4902764355847));
#94285=CARTESIAN_POINT('Ctrl Pts',(2.32211929848942,0.943644763947515,49.4897962199723));
#94286=CARTESIAN_POINT('Ctrl Pts',(2.32697938553938,0.932679312829285,49.4893160377747));
#94287=CARTESIAN_POINT('Ctrl Pts',(2.33176231477172,0.921685451781552,49.4888362497009));
#94288=CARTESIAN_POINT('Ctrl Pts',(2.36731939269898,0.839955291244647,49.4852694267143));
#94289=CARTESIAN_POINT('Ctrl Pts',(2.3986749483017,0.756527190235498,49.4817186327847));
#94290=CARTESIAN_POINT('Ctrl Pts',(2.42577696253307,0.671808303375818,49.4781788484286));
#94291=CARTESIAN_POINT('Ctrl Pts',(2.45320047087974,0.586084449750662,49.4745970738414));
#94292=CARTESIAN_POINT('Ctrl Pts',(2.47626933263316,0.499038107217648,49.4710265715762));
#94293=CARTESIAN_POINT('Ctrl Pts',(2.49488476821487,0.411062505937825,49.4674621413933));
#94294=CARTESIAN_POINT('Ctrl Pts',(2.51281826366768,0.326309719005444,49.4640282871492));
#94295=CARTESIAN_POINT('Ctrl Pts',(2.52661866832979,0.240693578216629,49.4606000682581));
#94296=CARTESIAN_POINT('Ctrl Pts',(2.53615367370349,0.154552993143809,49.4571728353021));
#94297=CARTESIAN_POINT('Ctrl Pts',(2.53972930071863,0.122250273741502,49.4558876229436));
#94298=CARTESIAN_POINT('Ctrl Pts',(2.54270464826766,0.0898737425312771,
49.4546025492322));
#94299=CARTESIAN_POINT('Ctrl Pts',(2.54507104088501,0.0574411829209008,
49.4533173689837));
#94300=CARTESIAN_POINT('Ctrl Pts',(2.54659675859018,0.0365304810961177,
49.4524887565865));
#94301=CARTESIAN_POINT('Ctrl Pts',(2.54786931761251,0.0155964887192117,
49.4516600999024));
#94302=CARTESIAN_POINT('Ctrl Pts',(2.54888617789747,-0.00535601068066993,
49.4508313332178));
#94303=CARTESIAN_POINT('Ctrl Pts',(2.54959366579885,-0.0199338637528056,
49.4502547128));
#94304=CARTESIAN_POINT('Ctrl Pts',(2.55017695702511,-0.0345129004678059,
49.4496783466839));
#94305=CARTESIAN_POINT('Ctrl Pts',(2.5506354515805,-0.0490849422160798,
49.4491024711239));
#94306=CARTESIAN_POINT('Ctrl Pts',(2.55349263168339,-0.139892885849451,
49.4455138130422));
#94307=CARTESIAN_POINT('Ctrl Pts',(2.55151149704795,-0.230507570687691,
49.4419410548054));
#94308=CARTESIAN_POINT('Ctrl Pts',(2.54459631698184,-0.320534826816672,
49.4383790803832));
#94309=CARTESIAN_POINT('Ctrl Pts',(2.53778415703423,-0.409220885969587,
49.4348701711051));
#94310=CARTESIAN_POINT('Ctrl Pts',(2.52618405231378,-0.497337839177241,
49.4313717267274));
#94311=CARTESIAN_POINT('Ctrl Pts',(2.50965462981406,-0.584515376296054,
49.4278788564812));
#94312=CARTESIAN_POINT('Ctrl Pts',(2.50750901683598,-0.595831516048816,
49.4274254620731));
#94313=CARTESIAN_POINT('Ctrl Pts',(2.50528027513273,-0.607131824718634,
49.4269721615863));
#94314=CARTESIAN_POINT('Ctrl Pts',(2.50296803009266,-0.618415487757582,
49.4265189443241));
#94315=CARTESIAN_POINT('Ctrl Pts',(2.48519637484993,-0.705140452425336,
49.4230355674352));
#94316=CARTESIAN_POINT('Ctrl Pts',(2.46249614940113,-0.790883208828462,
49.4195571068563));
#94317=CARTESIAN_POINT('Ctrl Pts',(2.43513714111733,-0.8753863679234,49.416078705898));
#94318=CARTESIAN_POINT('Ctrl Pts',(2.42592803142475,-0.903830339773648,
49.414907867553));
#94319=CARTESIAN_POINT('Ctrl Pts',(2.4161906539963,-0.932133740819968,49.4137370359631));
#94320=CARTESIAN_POINT('Ctrl Pts',(2.40593406766555,-0.96028630774472,49.4125660259065));
#94321=CARTESIAN_POINT('Ctrl Pts',(2.39924822373631,-0.978637800395067,
49.4118026929392));
#94322=CARTESIAN_POINT('Ctrl Pts',(2.39233957405065,-0.996930415172384,
49.4110390638345));
#94323=CARTESIAN_POINT('Ctrl Pts',(2.38522272103957,-1.01513098367692,49.4102763599805));
#94324=CARTESIAN_POINT('Ctrl Pts',(2.35171164784641,-1.10083186612637,49.4066850219782));
#94325=CARTESIAN_POINT('Ctrl Pts',(2.31355264766449,-1.18460163813465,49.4031096924922));
#94326=CARTESIAN_POINT('Ctrl Pts',(2.27110938627169,-1.26617525182304,49.3995452516877));
#94327=CARTESIAN_POINT('Ctrl Pts',(2.2290466817146,-1.34701745620675,49.3960127705458));
#94328=CARTESIAN_POINT('Ctrl Pts',(2.18277549541836,-1.4257034416751,49.3924909836995));
#94329=CARTESIAN_POINT('Ctrl Pts',(2.13259475634065,-1.50196208234925,49.3889749078001));
#94330=CARTESIAN_POINT('Ctrl Pts',(2.08216402897786,-1.57860062509649,49.3854413156623));
#94331=CARTESIAN_POINT('Ctrl Pts',(2.02778413096789,-1.65278836814677,49.3819134915142));
#94332=CARTESIAN_POINT('Ctrl Pts',(1.96971197405773,-1.72422532172408,49.3783863771579));
#94333=CARTESIAN_POINT('Ctrl Pts',(1.94766500938463,-1.75134620160306,49.3770473160699));
#94334=CARTESIAN_POINT('Ctrl Pts',(1.92508543871163,-1.7780702874266,49.3757083572859));
#94335=CARTESIAN_POINT('Ctrl Pts',(1.90198583988356,-1.80437986478666,49.3743692240236));
#94336=CARTESIAN_POINT('Ctrl Pts',(1.88944491551879,-1.81866350764111,49.3736421997544));
#94337=CARTESIAN_POINT('Ctrl Pts',(1.87675070104281,-1.83282496139081,49.3729151240582));
#94338=CARTESIAN_POINT('Ctrl Pts',(1.86390512055704,-1.84686128720403,49.372187952644));
#94339=CARTESIAN_POINT('Ctrl Pts',(1.85444773605752,-1.85719534180929,49.3716525825478));
#94340=CARTESIAN_POINT('Ctrl Pts',(1.84491471803415,-1.86745454471056,49.3711175241102));
#94341=CARTESIAN_POINT('Ctrl Pts',(1.83530860507554,-1.87763647573028,49.3705828398716));
#94342=CARTESIAN_POINT('Ctrl Pts',(1.77156448674401,-1.94520159999665,49.3670347892161));
#94343=CARTESIAN_POINT('Ctrl Pts',(1.70458530858084,-2.00938821260543,49.363502069587));
#94344=CARTESIAN_POINT('Ctrl Pts',(1.63467500708789,-2.06992478749503,49.3599797407958));
#94345=CARTESIAN_POINT('Ctrl Pts',(1.5647324226398,-2.13048931677031,49.3564557854748));
#94346=CARTESIAN_POINT('Ctrl Pts',(1.49185537900294,-2.18740119976334,49.3529422305904));
#94347=CARTESIAN_POINT('Ctrl Pts',(1.4163068404822,-2.24035820837223,49.3494341291071));
#94348=CARTESIAN_POINT('Ctrl Pts',(1.34192288164103,-2.29249888542362,49.3459801049597));
#94349=CARTESIAN_POINT('Ctrl Pts',(1.26494848743881,-2.34080631444827,49.3425313673809));
#94350=CARTESIAN_POINT('Ctrl Pts',(1.18560428430781,-2.3849524025052,49.3390831946023));
#94351=CARTESIAN_POINT('Ctrl Pts',(1.1560523297861,-2.40139472765421,49.3377989136957));
#94352=CARTESIAN_POINT('Ctrl Pts',(1.12617137745806,-2.41725934019025,49.3365147111386));
#94353=CARTESIAN_POINT('Ctrl Pts',(1.095972007602,-2.43252757553188,49.3352303429717));
#94354=CARTESIAN_POINT('Ctrl Pts',(1.07971681644229,-2.4407458954946,49.3345390156303));
#94355=CARTESIAN_POINT('Ctrl Pts',(1.06336936453226,-2.44879141198345,49.3338476403074));
#94356=CARTESIAN_POINT('Ctrl Pts',(1.04693125869691,-2.45666108941232,49.3331561789576));
#94357=CARTESIAN_POINT('Ctrl Pts',(1.03431734823736,-2.46269994859887,49.3326255806247));
#94358=CARTESIAN_POINT('Ctrl Pts',(1.02165372665814,-2.46863344887536,49.3320950869736));
#94359=CARTESIAN_POINT('Ctrl Pts',(1.00894994693436,-2.47445653363982,49.3315650429079));
#94360=CARTESIAN_POINT('Ctrl Pts',(0.961614070867921,-2.49615407757779,
49.3295900322613));
#94361=CARTESIAN_POINT('Ctrl Pts',(0.91368552170473,-2.51633592893095,49.3276197738702));
#94362=CARTESIAN_POINT('Ctrl Pts',(0.865212251108304,-2.53495176364714,
49.3256534164861));
#94363=CARTESIAN_POINT('Ctrl Pts',(0.781689405409389,-2.56702815278748,
49.3222652447708));
#94364=CARTESIAN_POINT('Ctrl Pts',(0.69655068261115,-2.59445802060023,49.3188886550312));
#94365=CARTESIAN_POINT('Ctrl Pts',(0.610163038527935,-2.61737933997433,
49.3155192924974));
#94366=CARTESIAN_POINT('Ctrl Pts',(0.521562429201812,-2.64088782761347,
49.3120636180579));
#94367=CARTESIAN_POINT('Ctrl Pts',(0.431647336561218,-2.65965394393264,
49.308615545841));
#94368=CARTESIAN_POINT('Ctrl Pts',(0.340792399615863,-2.67377635564093,
49.305170377766));
#94369=CARTESIAN_POINT('Ctrl Pts',(0.251252423365253,-2.6876943710122,49.3017750722606));
#94370=CARTESIAN_POINT('Ctrl Pts',(0.16079875261803,-2.69710194612434,49.298382587441));
#94371=CARTESIAN_POINT('Ctrl Pts',(0.0697819260538942,-2.70204634331308,
49.2949884262775));
#94372=CARTESIAN_POINT('Ctrl Pts',(0.056678488182449,-2.7027581743428,49.2944997783911));
#94373=CARTESIAN_POINT('Ctrl Pts',(0.0435624055918989,-2.70337745931282,
49.2940110595948));
#94374=CARTESIAN_POINT('Ctrl Pts',(0.0304377310135361,-2.70390414115064,
49.2935223683404));
#94375=CARTESIAN_POINT('Ctrl Pts',(-0.0632353432642269,-2.70766316059304,
49.290034494268));
#94376=CARTESIAN_POINT('Ctrl Pts',(-0.156972776620133,-2.70669504074848,
49.2865618620568));
#94377=CARTESIAN_POINT('Ctrl Pts',(-0.250383234795894,-2.70113638510294,
49.2830997990332));
#94378=CARTESIAN_POINT('Ctrl Pts',(-0.345161089864368,-2.69549635860658,
49.2795870563073));
#94379=CARTESIAN_POINT('Ctrl Pts',(-0.43960325480989,-2.68513042806245,
49.2760851944697));
#94380=CARTESIAN_POINT('Ctrl Pts',(-0.533311979758323,-2.67012840852803,
49.2725893326246));
#94381=CARTESIAN_POINT('Ctrl Pts',(-0.626952633413095,-2.65513728666486,
49.2690960102211));
#94382=CARTESIAN_POINT('Ctrl Pts',(-0.719861888547964,-2.6355167074097,
49.2656086790962));
#94383=CARTESIAN_POINT('Ctrl Pts',(-0.811639396756275,-2.61130474078774,
49.262122468983));
#94384=CARTESIAN_POINT('Ctrl Pts',(-0.852869462444847,-2.6004277732849,
49.2605563263105));
#94385=CARTESIAN_POINT('Ctrl Pts',(-0.893870988019684,-2.58862350739258,
49.2589904098762));
#94386=CARTESIAN_POINT('Ctrl Pts',(-0.934606640503465,-2.57589208119221,
49.2574242781235));
#94387=CARTESIAN_POINT('Ctrl Pts',(-0.955365781692795,-2.56940406742735,
49.2566261676677));
#94388=CARTESIAN_POINT('Ctrl Pts',(-0.976055862454838,-2.562675238885,49.255828001294));
#94389=CARTESIAN_POINT('Ctrl Pts',(-0.996671844395906,-2.55570541111516,
49.2550297205652));
#94390=CARTESIAN_POINT('Ctrl Pts',(-1.01068707739322,-2.55096715705456,
49.2544870304113));
#94391=CARTESIAN_POINT('Ctrl Pts',(-1.02466976493489,-2.54611684946725,
49.2539442204075));
#94392=CARTESIAN_POINT('Ctrl Pts',(-1.03860223115708,-2.54116030770371,
49.2534019001196));
#94393=CARTESIAN_POINT('Ctrl Pts',(-1.12917963816755,-2.50893696019858,
49.2498761807911));
#94394=CARTESIAN_POINT('Ctrl Pts',(-1.21777942064694,-2.47218038079066,
49.2463655720126));
#94395=CARTESIAN_POINT('Ctrl Pts',(-1.30400292535831,-2.43098062826895,
49.242865238774));
#94396=CARTESIAN_POINT('Ctrl Pts',(-1.38886736099538,-2.39043027302829,
49.2394200783642));
#94397=CARTESIAN_POINT('Ctrl Pts',(-1.47143074991837,-2.34557546596676,
49.2359848721178));
#94398=CARTESIAN_POINT('Ctrl Pts',(-1.55130162346499,-2.29645380037892,
49.2325550100709));
#94399=CARTESIAN_POINT('Ctrl Pts',(-1.6116479732812,-2.25933998049077,49.2299635816101));
#94400=CARTESIAN_POINT('Ctrl Pts',(-1.6704571549813,-2.21978942207171,49.2273752039075));
#94401=CARTESIAN_POINT('Ctrl Pts',(-1.72755116942149,-2.17780075375096,
49.224787888648));
#94402=CARTESIAN_POINT('Ctrl Pts',(-1.76872966611956,-2.14751683946056,
49.2229218129497));
#94403=CARTESIAN_POINT('Ctrl Pts',(-1.80901576369452,-2.11596429670162,
49.2210562899208));
#94404=CARTESIAN_POINT('Ctrl Pts',(-1.84838795223496,-2.08320010102078,
49.2191905735852));
#94405=CARTESIAN_POINT('Ctrl Pts',(-1.87206203371001,-2.06349933591812,
49.2180687380415));
#94406=CARTESIAN_POINT('Ctrl Pts',(-1.89540563437032,-2.04336042988252,
49.2169468326079));
#94407=CARTESIAN_POINT('Ctrl Pts',(-1.91841351965119,-2.02279520631578,
49.2158246951126));
#94408=CARTESIAN_POINT('Ctrl Pts',(-1.93117286120055,-2.01139047666229,
49.2152023982177));
#94409=CARTESIAN_POINT('Ctrl Pts',(-1.94383029046328,-1.99985323695415,
49.2145799600185));
#94410=CARTESIAN_POINT('Ctrl Pts',(-1.95636866376425,-1.98820093939874,
49.2139581660398));
#94411=CARTESIAN_POINT('Ctrl Pts',(-2.02501357614443,-1.92440710223034,
49.2105539769829));
#94412=CARTESIAN_POINT('Ctrl Pts',(-2.09020338271483,-1.8570710837208,49.2071637169369));
#94413=CARTESIAN_POINT('Ctrl Pts',(-2.15185690424115,-1.78660322661286,
49.2037830333995));
#94414=CARTESIAN_POINT('Ctrl Pts',(-2.21484733000207,-1.71460733389174,
49.2003290426117));
#94415=CARTESIAN_POINT('Ctrl Pts',(-2.27414695035793,-1.63934166565729,
49.1968850481522));
#94416=CARTESIAN_POINT('Ctrl Pts',(-2.3296369179527,-1.5611981913315,49.1934464081936));
#94417=CARTESIAN_POINT('Ctrl Pts',(-2.38568234800599,-1.48227248972664,
49.1899733469605));
#94418=CARTESIAN_POINT('Ctrl Pts',(-2.43784197477932,-1.40041028970125,
49.1865057479634));
#94419=CARTESIAN_POINT('Ctrl Pts',(-2.48595320048127,-1.31598041155428,
49.1830388285787));
#94420=CARTESIAN_POINT('Ctrl Pts',(-2.51305842340654,-1.26841374420506,
49.1810856124339));
#94421=CARTESIAN_POINT('Ctrl Pts',(-2.53887790137548,-1.22003151950339,
49.1791326120012));
#94422=CARTESIAN_POINT('Ctrl Pts',(-2.56337609854124,-1.17089633028993,
49.1771789720447));
#94423=CARTESIAN_POINT('Ctrl Pts',(-2.56995917422177,-1.15769288242065,
49.1766539962843));
#94424=CARTESIAN_POINT('Ctrl Pts',(-2.57644782254101,-1.14443294732825,
49.1761288913047));
#94425=CARTESIAN_POINT('Ctrl Pts',(-2.58283802576922,-1.13112453966317,
49.1756039094184));
#94426=CARTESIAN_POINT('Ctrl Pts',(-2.62538221167359,-1.04252088347651,
49.1721087268444));
#94427=CARTESIAN_POINT('Ctrl Pts',(-2.66345146630088,-0.952014028769855,
49.168628527235));
#94428=CARTESIAN_POINT('Ctrl Pts',(-2.69692936295805,-0.860010437873625,
49.1651586115314));
#94429=CARTESIAN_POINT('Ctrl Pts',(-2.73050479700952,-0.767738795772912,
49.1616785862758));
#94430=CARTESIAN_POINT('Ctrl Pts',(-2.75946252850468,-0.673960808919952,
49.1582089049373));
#94431=CARTESIAN_POINT('Ctrl Pts',(-2.78364169059793,-0.579056964346966,
49.1547448272653));
#94432=CARTESIAN_POINT('Ctrl Pts',(-2.80735578926856,-0.48597850588979,
49.1513473778666));
#94433=CARTESIAN_POINT('Ctrl Pts',(-2.82647364105441,-0.391816203459708,
49.1479553186449));
#94434=CARTESIAN_POINT('Ctrl Pts',(-2.84079674623874,-0.296913748806167,
49.1445641776455));
#94435=CARTESIAN_POINT('Ctrl Pts',(-2.85209612830125,-0.222045968391273,
49.1418889338846));
#94436=CARTESIAN_POINT('Ctrl Pts',(-2.86041066761624,-0.146717119309908,
49.1392142615796));
#94437=CARTESIAN_POINT('Ctrl Pts',(-2.86561997416828,-0.0710943294859263,
49.1365379651472));
#94438=CARTESIAN_POINT('Ctrl Pts',(-2.86729088743676,-0.0468379103917938,
49.1356795285828));
#94439=CARTESIAN_POINT('Ctrl Pts',(-2.86864006663653,-0.0225815264959612,
49.1348219958472));
#94440=CARTESIAN_POINT('Ctrl Pts',(-2.86966548199755,0.0016690505250476,
49.1339652973708));
#94441=CARTESIAN_POINT('',(0.260874132846714,2.92567963864295,49.058));
#94442=CARTESIAN_POINT('Ctrl Pts',(0.260739855805342,2.92492329228914,49.058));
#94443=CARTESIAN_POINT('Ctrl Pts',(0.162865051941415,2.92111867579054,49.0703774519651));
#94444=CARTESIAN_POINT('Ctrl Pts',(0.0654587677403667,2.91267041664908,
49.0827990502223));
#94445=CARTESIAN_POINT('Ctrl Pts',(-0.0311012750313888,2.89958669379796,
49.0952843365015));
#94446=CARTESIAN_POINT('Ctrl Pts',(-0.129420938708193,2.88626454528355,
49.1079971430894));
#94447=CARTESIAN_POINT('Ctrl Pts',(-0.226864310025817,2.86813635666484,
49.1207759800322));
#94448=CARTESIAN_POINT('Ctrl Pts',(-0.323009383677986,2.84515947512996,
49.1336414769778));
#94449=CARTESIAN_POINT('Ctrl Pts',(-0.413314826332502,2.82357815661815,
49.1457255531816));
#94450=CARTESIAN_POINT('Ctrl Pts',(-0.502475357477472,2.79771863584763,
49.1578860820237));
#94451=CARTESIAN_POINT('Ctrl Pts',(-0.59011056116163,2.76750695016159,49.1701401578498));
#94452=CARTESIAN_POINT('Ctrl Pts',(-0.618328969582016,2.75777883121033,
49.1740859524842));
#94453=CARTESIAN_POINT('Ctrl Pts',(-0.646388950214392,2.74759918873813,
49.1780414463566));
#94454=CARTESIAN_POINT('Ctrl Pts',(-0.674276952688285,2.73696477818488,
49.1820072101754));
#94455=CARTESIAN_POINT('Ctrl Pts',(-0.694945139639471,2.72908346844834,
49.1849462929616));
#94456=CARTESIAN_POINT('Ctrl Pts',(-0.715518858776697,2.72095236969504,
49.1878910165143));
#94457=CARTESIAN_POINT('Ctrl Pts',(-0.735992427615463,2.71257003283589,
49.1908416131441));
#94458=CARTESIAN_POINT('Ctrl Pts',(-0.750134370446515,2.7067800052356,49.1928797125681));
#94459=CARTESIAN_POINT('Ctrl Pts',(-0.764229517079808,2.70086959326046,
49.1949207644322));
#94460=CARTESIAN_POINT('Ctrl Pts',(-0.778260340253251,2.69484524810002,
49.1969625551167));
#94461=CARTESIAN_POINT('Ctrl Pts',(-0.861823008089798,2.65896635864705,
49.2091227451959));
#94462=CARTESIAN_POINT('Ctrl Pts',(-0.943237200345705,2.6189972815904,49.2213278864296));
#94463=CARTESIAN_POINT('Ctrl Pts',(-1.02217019948904,2.57491088258204,49.2335969425659));
#94464=CARTESIAN_POINT('Ctrl Pts',(-1.06131160945252,2.5530492551749,49.2396809398966));
#94465=CARTESIAN_POINT('Ctrl Pts',(-1.09984243477703,2.53017455154342,49.2457806538004));
#94466=CARTESIAN_POINT('Ctrl Pts',(-1.13771892917144,2.50627986935387,49.2518983966494));
#94467=CARTESIAN_POINT('Ctrl Pts',(-1.21599994719749,2.45689567799419,49.2645422050562));
#94468=CARTESIAN_POINT('Ctrl Pts',(-1.29148891934137,2.40315618786065,49.2772630228555));
#94469=CARTESIAN_POINT('Ctrl Pts',(-1.36397315623523,2.34538874880156,49.2900812635639));
#94470=CARTESIAN_POINT('Ctrl Pts',(-1.43889280980964,2.28568036657046,49.3033301876675));
#94471=CARTESIAN_POINT('Ctrl Pts',(-1.5106031566708,2.22166779667127,49.3166831913371));
#94472=CARTESIAN_POINT('Ctrl Pts',(-1.57881491577384,2.15369213867893,49.3301628156358));
#94473=CARTESIAN_POINT('Ctrl Pts',(-1.59215311282773,2.1404001090774,49.3327986351408));
#94474=CARTESIAN_POINT('Ctrl Pts',(-1.6053573553333,2.12695651327283,49.3354392961489));
#94475=CARTESIAN_POINT('Ctrl Pts',(-1.61842521038769,2.11336386827515,49.3380849671945));
#94476=CARTESIAN_POINT('Ctrl Pts',(-1.62805298867044,2.1033494495531,49.3400341726402));
#94477=CARTESIAN_POINT('Ctrl Pts',(-1.63760069310815,2.09326038599484,49.3419848774496));
#94478=CARTESIAN_POINT('Ctrl Pts',(-1.64706556304477,2.08310024119305,49.3439367104448));
#94479=CARTESIAN_POINT('Ctrl Pts',(-1.70828813901715,2.01738034845456,49.3565619493159));
#94480=CARTESIAN_POINT('Ctrl Pts',(-1.76607890037575,1.94865710831166,49.3692405129108));
#94481=CARTESIAN_POINT('Ctrl Pts',(-1.82026814410794,1.87725108113391,49.3819940806871));
#94482=CARTESIAN_POINT('Ctrl Pts',(-1.87420815042845,1.80617347805226,49.3946889898441));
#94483=CARTESIAN_POINT('Ctrl Pts',(-1.92457998069414,1.73243671357817,49.4074582148224));
#94484=CARTESIAN_POINT('Ctrl Pts',(-1.97116800133376,1.65633974881965,49.4203231373166));
#94485=CARTESIAN_POINT('Ctrl Pts',(-2.01693944620795,1.5815765805262,49.4329625687126));
#94486=CARTESIAN_POINT('Ctrl Pts',(-2.05905869204356,1.50453433051914,49.4456943723306));
#94487=CARTESIAN_POINT('Ctrl Pts',(-2.09727163215101,1.42549384358289,49.4585388251477));
#94488=CARTESIAN_POINT('Ctrl Pts',(-2.1192404942794,1.38005296530499,49.4659231827046));
#94489=CARTESIAN_POINT('Ctrl Pts',(-2.13991732470015,1.33395165722691,49.4733447727726));
#94490=CARTESIAN_POINT('Ctrl Pts',(-2.15924596868274,1.28724457024862,49.4808074483121));
#94491=CARTESIAN_POINT('Ctrl Pts',(-2.16488416199063,1.27362004565863,49.4829843215228));
#94492=CARTESIAN_POINT('Ctrl Pts',(-2.17040807886406,1.25994255303091,49.4851649158573));
#94493=CARTESIAN_POINT('Ctrl Pts',(-2.17580969047169,1.24623072785564,49.4873465904162));
#94494=CARTESIAN_POINT('Ctrl Pts',(-2.20698364607134,1.16709659895971,49.4999375411865));
#94495=CARTESIAN_POINT('Ctrl Pts',(-2.23414211094401,1.08669178286697,49.5125848962906));
#94496=CARTESIAN_POINT('Ctrl Pts',(-2.25710446510236,1.00528373148052,49.5253107322942));
#94497=CARTESIAN_POINT('Ctrl Pts',(-2.27971678650434,0.925116645389746,
49.5378425786301));
#94498=CARTESIAN_POINT('Ctrl Pts',(-2.29826001442132,0.843975867542557,
49.5504505314132));
#94499=CARTESIAN_POINT('Ctrl Pts',(-2.31251203424867,0.762119412589603,
49.563155672931));
#94500=CARTESIAN_POINT('Ctrl Pts',(-2.32635004093017,0.682640841532014,
49.5754917372462));
#94501=CARTESIAN_POINT('Ctrl Pts',(-2.33614243912025,0.602486942314531,
49.5879194257547));
#94502=CARTESIAN_POINT('Ctrl Pts',(-2.34163918216539,0.521906755120729,
49.6004580363135));
#94503=CARTESIAN_POINT('Ctrl Pts',(-2.34567307551512,0.462771394677,49.6096597430938));
#94504=CARTESIAN_POINT('Ctrl Pts',(-2.34739252847471,0.403406675792388,
49.6189211885841));
#94505=CARTESIAN_POINT('Ctrl Pts',(-2.34668236863849,0.343918483395766,
49.62825));
#94506=CARTESIAN_POINT('',(-2.14330812717712,2.01108871876559,49.058));
#94507=CARTESIAN_POINT('Origin',(0.,0.,49.058));
#94508=CARTESIAN_POINT('Ctrl Pts',(-2.86966548199755,0.0016690505250476,
49.1339652973708));
#94509=CARTESIAN_POINT('Ctrl Pts',(-2.87368608546791,0.0967543767551498,
49.1306062245523));
#94510=CARTESIAN_POINT('Ctrl Pts',(-2.87273263089904,0.191749483183767,
49.1272599768048));
#94511=CARTESIAN_POINT('Ctrl Pts',(-2.86665574610838,0.286315728950319,
49.12392236081));
#94512=CARTESIAN_POINT('Ctrl Pts',(-2.86052341350175,0.381744833232796,
49.1205542911331));
#94513=CARTESIAN_POINT('Ctrl Pts',(-2.84917446165842,0.476738011679848,
49.1171950114464));
#94514=CARTESIAN_POINT('Ctrl Pts',(-2.83288404805877,0.57100164318236,49.1138402125967));
#94515=CARTESIAN_POINT('Ctrl Pts',(-2.81628545073246,0.667048563799475,
49.110421947316));
#94516=CARTESIAN_POINT('Ctrl Pts',(-2.79455638587865,0.762338849772889,
49.1070083340138));
#94517=CARTESIAN_POINT('Ctrl Pts',(-2.76793357574644,0.85655626228785,49.1035948143183));
#94518=CARTESIAN_POINT('Ctrl Pts',(-2.75923473119273,0.887341240344261,
49.1024794671004));
#94519=CARTESIAN_POINT('Ctrl Pts',(-2.75001301471277,0.918011581896025,
49.1013641298762));
#94520=CARTESIAN_POINT('Ctrl Pts',(-2.74027553745566,0.948555907391574,
49.1002486436324));
#94521=CARTESIAN_POINT('Ctrl Pts',(-2.73372252544349,0.969111265477753,
49.0994979569236));
#94522=CARTESIAN_POINT('Ctrl Pts',(-2.72693592120902,0.989609548497314,
49.0987472027259));
#94523=CARTESIAN_POINT('Ctrl Pts',(-2.71991775760214,1.01004722720839,49.0979963325757));
#94524=CARTESIAN_POINT('Ctrl Pts',(-2.71424481770592,1.0265674637604,49.0973893873019));
#94525=CARTESIAN_POINT('Ctrl Pts',(-2.70841986421024,1.0430497756366,49.0967823033947));
#94526=CARTESIAN_POINT('Ctrl Pts',(-2.70245178824862,1.05947149606707,49.0961758256804));
#94527=CARTESIAN_POINT('Ctrl Pts',(-2.66875576630627,1.15218925896325,49.0927516255701));
#94528=CARTESIAN_POINT('Ctrl Pts',(-2.6304519663529,1.24312504392082,49.0893412796056));
#94529=CARTESIAN_POINT('Ctrl Pts',(-2.58783597912855,1.33197382727985,49.085940362308));
#94530=CARTESIAN_POINT('Ctrl Pts',(-2.5446561368894,1.42199817491223,49.0824944472432));
#94531=CARTESIAN_POINT('Ctrl Pts',(-2.49704886581761,1.50988075199989,49.0790582119988));
#94532=CARTESIAN_POINT('Ctrl Pts',(-2.44526848354104,1.59529347018132,49.0756270531001));
#94533=CARTESIAN_POINT('Ctrl Pts',(-2.39355330634354,1.68059863135375,49.0722002149301));
#94534=CARTESIAN_POINT('Ctrl Pts',(-2.33767502868706,1.76344096821467,49.0687784403291));
#94535=CARTESIAN_POINT('Ctrl Pts',(-2.27784106807338,1.84347061755202,49.0653571431915));
#94536=CARTESIAN_POINT('Ctrl Pts',(-2.23495772093708,1.90082833210961,49.0629050796593));
#94537=CARTESIAN_POINT('Ctrl Pts',(-2.19004149603404,1.95674081908624,49.0604532613844));
#94538=CARTESIAN_POINT('Ctrl Pts',(-2.14315631774277,2.01106840053253,49.058));
#94539=CARTESIAN_POINT('',(-2.,-2.44929359829471E-16,50.));
#94540=CARTESIAN_POINT('',(-2.5,-3.06161699786838E-16,49.5));
#94541=CARTESIAN_POINT('Origin',(0.,0.,50.));
#94542=CARTESIAN_POINT('Ctrl Pts',(1.70810875200399,-2.39535560853235,-0.329233991005384));
#94543=CARTESIAN_POINT('Ctrl Pts',(2.50610891073096,-1.82630813584529,-0.276212356389999));
#94544=CARTESIAN_POINT('Ctrl Pts',(3.47463875979381,0.16229507325623,-0.17016908715923));
#94545=CARTESIAN_POINT('Ctrl Pts',(1.73917099852795,3.01633623709207,-0.0111041833130765));
#94546=CARTESIAN_POINT('Ctrl Pts',(-1.59514451425713,3.09116303725476,0.147960720533078));
#94547=CARTESIAN_POINT('Ctrl Pts',(-3.46361225058625,0.331379558630963,
0.307025624379232));
#94548=CARTESIAN_POINT('Ctrl Pts',(-2.15136645360759,-2.7350655110993,0.466090528225386));
#94549=CARTESIAN_POINT('Ctrl Pts',(1.137007233108,-3.28830020261314,0.62515543207154));
#94550=CARTESIAN_POINT('Ctrl Pts',(3.38098902036554,-0.822049678815183,
0.784220335917693));
#94551=CARTESIAN_POINT('Ctrl Pts',(2.51978384323507,2.39953860437162,0.943285239763849));
#94552=CARTESIAN_POINT('Ctrl Pts',(-0.655731952682091,3.41711250332626,
1.10235014361));
#94553=CARTESIAN_POINT('Ctrl Pts',(-3.22897844832054,1.2963528837586,1.26141504745616));
#94554=CARTESIAN_POINT('Ctrl Pts',(-2.83659947794847,-2.01508134321981,
1.42047995130231));
#94555=CARTESIAN_POINT('Ctrl Pts',(0.16104030048805,-3.47575223487759,1.57954485514846));
#94556=CARTESIAN_POINT('Ctrl Pts',(3.01077127957883,-1.74415432954563,1.73860975899462));
#94557=CARTESIAN_POINT('Ctrl Pts',(3.09528030412668,1.5893576043674,1.89767466284077));
#94558=CARTESIAN_POINT('Ctrl Pts',(0.336948704848476,3.46313082488865,2.05673956668693));
#94559=CARTESIAN_POINT('Ctrl Pts',(-2.73085088642586,2.15621606241621,2.21580447053308));
#94560=CARTESIAN_POINT('Ctrl Pts',(-3.29051850755748,-1.13106224326845,
2.37486937437924));
#94561=CARTESIAN_POINT('Ctrl Pts',(-0.828030814474741,-3.37952330330655,
2.53393427822538));
#94562=CARTESIAN_POINT('Ctrl Pts',(2.39495631940617,-2.52408354317363,2.69299918207155));
#94563=CARTESIAN_POINT('Ctrl Pts',(3.41831149878882,0.649584395119446,2.85206408591769));
#94564=CARTESIAN_POINT('Ctrl Pts',(1.30214080720984,3.22664571586789,3.01112898976385));
#94565=CARTESIAN_POINT('Ctrl Pts',(-2.00997259209927,2.84021540432072,3.17019389361));
#94566=CARTESIAN_POINT('Ctrl Pts',(-3.4760398031417,-0.154792205052638,
3.32925879745616));
#94567=CARTESIAN_POINT('Ctrl Pts',(-1.74956097100319,-3.00763191447529,
3.48832370130231));
#94568=CARTESIAN_POINT('Ctrl Pts',(1.583790700515,-3.09813175262809,3.64738860514846));
#94569=CARTESIAN_POINT('Ctrl Pts',(3.46252015378254,-0.343172725955958,
3.80645350899462));
#94570=CARTESIAN_POINT('Ctrl Pts',(2.16112059915153,2.72697104667658,3.96551841284077));
#94571=CARTESIAN_POINT('Ctrl Pts',(-1.12514604666361,3.29254608310422,4.12458331668693));
#94572=CARTESIAN_POINT('Ctrl Pts',(-3.37802965884603,0.83410368592,4.28364822053308));
#94573=CARTESIAN_POINT('Ctrl Pts',(-2.52838400629955,-2.39041579049229,
4.44271312437924));
#94574=CARTESIAN_POINT('Ctrl Pts',(0.643439413780638,-3.41947350565055,
4.60177802822539));
#94575=CARTESIAN_POINT('Ctrl Pts',(3.22430010917227,-1.3079381257977,4.76084293207155));
#94576=CARTESIAN_POINT('Ctrl Pts',(2.84382344014261,2.00486447826478,4.9199078359177));
#94577=CARTESIAN_POINT('Ctrl Pts',(-0.148544283050351,3.47631240410399,
5.07897273976384));
#94578=CARTESIAN_POINT('Ctrl Pts',(-3.00448248021664,1.75496392014332,5.23803764361001));
#94579=CARTESIAN_POINT('Ctrl Pts',(-3.10097337776917,-1.57821970755046,
5.39710254745616));
#94580=CARTESIAN_POINT('Ctrl Pts',(-0.349395541421692,-3.46189775853851,
5.55616745130231));
#94581=CARTESIAN_POINT('Ctrl Pts',(2.7230823466392,-2.16601843675395,5.71523235514847));
#94582=CARTESIAN_POINT('Ctrl Pts',(3.29456304881679,1.11922636330076,5.87429725899461));
#94583=CARTESIAN_POINT('Ctrl Pts',(0.840173848831963,3.3765250241448,6.03336216284078));
#94584=CARTESIAN_POINT('Ctrl Pts',(-2.38586753206279,2.53267634220902,6.19242706668693));
#94585=CARTESIAN_POINT('Ctrl Pts',(-3.42062446981773,-0.6372923751473,6.35149197053308));
#94586=CARTESIAN_POINT('Ctrl Pts',(-1.31373121710534,-3.2219440752657,6.51055687437924));
#94587=CARTESIAN_POINT('Ctrl Pts',(1.99974988670252,-2.84742229491342,6.66962177822538));
#94588=CARTESIAN_POINT('Ctrl Pts',(3.47657377546659,0.142295884250894,6.82868668207155));
#94589=CARTESIAN_POINT('Ctrl Pts',(1.76036119961975,3.00132333843091,6.98775158591769));
#94590=CARTESIAN_POINT('Ctrl Pts',(-1.57264361602868,3.10380498612606,7.14681648976386));
#94591=CARTESIAN_POINT('Ctrl Pts',(-3.46126417978726,0.35561722772998,7.30588139361));
#94592=CARTESIAN_POINT('Ctrl Pts',(-2.17090927703816,-2.71918484951032,
7.46494629745616));
#94593=CARTESIAN_POINT('Ctrl Pts',(1.11330306427908,-3.29656937163524,7.62401120130232));
#94594=CARTESIAN_POINT('Ctrl Pts',(3.37500948166289,-0.846241297516434,
7.78307610514846));
#94595=CARTESIAN_POINT('Ctrl Pts',(2.53696049635548,2.38131156610565,7.94214100899463));
#94596=CARTESIAN_POINT('Ctrl Pts',(-0.63114327775138,3.42176438374795,8.10120591284077));
#94597=CARTESIAN_POINT('Ctrl Pts',(-3.2195776329391,1.31952006442305,8.26027081668694));
#94598=CARTESIAN_POINT('Ctrl Pts',(-2.8510119511463,-1.99462883498604,8.41933572053308));
#94599=CARTESIAN_POINT('Ctrl Pts',(0.13604702576719,-3.47682391583421,8.57840062437923));
#94600=CARTESIAN_POINT('Ctrl Pts',(2.99815450093433,-1.76575279228548,8.73746552822539));
#94601=CARTESIAN_POINT('Ctrl Pts',(3.10662656770694,1.5670624441145,8.89653043207155));
#94602=CARTESIAN_POINT('Ctrl Pts',(0.361837765224454,3.46061941949619,9.0555953359177));
#94603=CARTESIAN_POINT('Ctrl Pts',(-2.71527856811274,2.17579310424599,9.21466023976385));
#94604=CARTESIAN_POINT('Ctrl Pts',(-3.29856504495654,-1.10737616875548,
9.37372514361001));
#94605=CARTESIAN_POINT('Ctrl Pts',(-0.852306012436442,-3.37348303628481,
9.53279004745616));
#94606=CARTESIAN_POINT('Ctrl Pts',(2.37674790737222,-2.54123645490509,9.69185495130231));
#94607=CARTESIAN_POINT('Ctrl Pts',(3.42289324374123,0.624992141460518,9.85091985514848));
#94608=CARTESIAN_POINT('Ctrl Pts',(1.32530464905932,3.21720078983556,10.0099847589946));
#94609=CARTESIAN_POINT('Ctrl Pts',(-1.98950133966361,2.85459239724579,10.1690496628408));
#94610=CARTESIAN_POINT('Ctrl Pts',(-3.47706282439622,-0.129797727786466,
10.3281145666869));
#94611=CARTESIAN_POINT('Ctrl Pts',(-1.77113868072445,-2.99497597796349,
10.4871794705331));
#94612=CARTESIAN_POINT('Ctrl Pts',(1.56147620983851,-3.10943811339688,10.6462443743792));
#94613=CARTESIAN_POINT('Ctrl Pts',(3.45996347974781,-0.368057133809716,
10.8053092782254));
#94614=CARTESIAN_POINT('Ctrl Pts',(2.18066990260054,2.71136351506559,10.9643741820716));
#94615=CARTESIAN_POINT('Ctrl Pts',(-1.10144569587676,3.30055006233375,11.1234390859177));
#94616=CARTESIAN_POINT('Ctrl Pts',(-3.37194569294167,0.858367974000013,
11.2825039897639));
#94617=CARTESIAN_POINT('Ctrl Pts',(-2.54550420404445,-2.37217657060532,
11.44156889361));
#94618=CARTESIAN_POINT('Ctrl Pts',(0.618838986145877,-3.42401104615079,
11.6006337974562));
#94619=CARTESIAN_POINT('Ctrl Pts',(3.21481355363338,-1.33108495232717,11.7596987013023));
#94620=CARTESIAN_POINT('Ctrl Pts',(2.85816362164538,1.98436741729946,11.9187636051485));
#94621=CARTESIAN_POINT('Ctrl Pts',(-0.123548010496914,3.47729050038087,
12.0778285089946));
#94622=CARTESIAN_POINT('Ctrl Pts',(-2.99178777978657,1.77651884753764,12.2368934128408));
#94623=CARTESIAN_POINT('Ctrl Pts',(-3.11223961411324,-1.55588493124686,
12.3959583166869));
#94624=CARTESIAN_POINT('Ctrl Pts',(-0.37427531339427,-3.45929636266111,
12.5550232205331));
#94625=CARTESIAN_POINT('Ctrl Pts',(2.70743970301638,-2.18553965634745,12.7140881243793));
#94626=CARTESIAN_POINT('Ctrl Pts',(3.30252441735429,1.09551166480118,12.8731530282254));
#94627=CARTESIAN_POINT('Ctrl Pts',(0.864427162624142,3.37039745659979,13.0322179320716));
#94628=CARTESIAN_POINT('Ctrl Pts',(-2.36759757057254,2.54976372998672,13.1912828359177));
#94629=CARTESIAN_POINT('Ctrl Pts',(-3.42511778736563,-0.612683831685064,
13.3503477397639));
#94630=CARTESIAN_POINT('Ctrl Pts',(-1.33686095555343,-3.21241593204452,
13.50941264361));
#94631=CARTESIAN_POINT('Ctrl Pts',(1.97922708447866,-2.86172561280827,13.6684775474562));
#94632=CARTESIAN_POINT('Ctrl Pts',(3.47750694305263,0.117297894088165,13.8275424513023));
#94633=CARTESIAN_POINT('Ctrl Pts',(1.78189327534454,2.98858991670296,13.9866073551485));
#94634=CARTESIAN_POINT('Ctrl Pts',(-1.55028862640208,3.11503106080583,14.1456722589946));
#94635=CARTESIAN_POINT('Ctrl Pts',(-3.45861807039121,0.380492283890413,
14.3047371628408));
#94636=CARTESIAN_POINT('Ctrl Pts',(-2.19040234975507,-2.70350714464087,
14.4638020666869));
#94637=CARTESIAN_POINT('Ctrl Pts',(1.0895740946985,-3.30448810364006,14.6228669705331));
#94638=CARTESIAN_POINT('Ctrl Pts',(3.36883833226074,-0.870483558734738,
14.7819318743792));
#94639=CARTESIAN_POINT('Ctrl Pts',(2.55401501897158,2.36301092206625,14.9409967782254));
#94640=CARTESIAN_POINT('Ctrl Pts',(-0.606526697962181,3.42621346381042,
15.1000616820716));
#94641=CARTESIAN_POINT('Ctrl Pts',(-3.21000793281444,1.34263264007885,15.2591265859177));
#94642=CARTESIAN_POINT('Ctrl Pts',(-2.86527835922753,-1.97408035780693,
15.4181914897639));
#94643=CARTESIAN_POINT('Ctrl Pts',(0.11104739875106,-3.4777121517123,15.57725639361));
#94644=CARTESIAN_POINT('Ctrl Pts',(2.9853823990433,-1.78726194678318,15.7363212974562));
#94645=CARTESIAN_POINT('Ctrl Pts',(3.11781244445693,1.54468731338294,15.8953862013023));
#94646=CARTESIAN_POINT('Ctrl Pts',(0.386708025214324,3.45792860512932,16.0544511051485));
#94647=CARTESIAN_POINT('Ctrl Pts',(-2.69956585264314,2.19525796711455,16.2135160089946));
#94648=CARTESIAN_POINT('Ctrl Pts',(-3.30644111484741,-1.08363300474993,
16.3725809128408));
#94649=CARTESIAN_POINT('Ctrl Pts',(-0.876537142766755,-3.3672683249612,
16.5316458166869));
#94650=CARTESIAN_POINT('Ctrl Pts',(2.35841663990349,-2.55825805726535,16.6907107205331));
#94651=CARTESIAN_POINT('Ctrl Pts',(3.42729807194563,0.600367604867713,16.8497756243792));
#94652=CARTESIAN_POINT('Ctrl Pts',(1.34839998725813,3.20758956372211,17.0088405282254));
#94653=CARTESIAN_POINT('Ctrl Pts',(-1.96892725391064,2.8688218494261,17.1679054320716));
#94654=CARTESIAN_POINT('Ctrl Pts',(-3.47790612569696,-0.104796544677688,
17.3269703359177));
#94655=CARTESIAN_POINT('Ctrl Pts',(-1.79262484451019,-2.98216523716939,
17.4860352397639));
#94656=CARTESIAN_POINT('Ctrl Pts',(1.53908101028433,-3.12058375608137,17.64510014361));
#94657=CARTESIAN_POINT('Ctrl Pts',(3.45722796910274,-0.392922517286194,
17.8041650474562));
#94658=CARTESIAN_POINT('Ctrl Pts',(2.20010649273994,2.69561583975543,17.9632299513023));
#94659=CARTESIAN_POINT('Ctrl Pts',(-1.077688414148,3.30838344466717,18.1222948551485));
#94660=CARTESIAN_POINT('Ctrl Pts',(-3.36568743977307,0.882587895164228,
18.2813597589946));
#94661=CARTESIAN_POINT('Ctrl Pts',(-2.56249283116099,-2.35381473892603,
18.4404246628408));
#94662=CARTESIAN_POINT('Ctrl Pts',(0.594206572298488,-3.42837160826742,
18.599489566687));
#94663=CARTESIAN_POINT('Ctrl Pts',(3.20516083258003,-1.35416297845998,18.7585544705331));
#94664=CARTESIAN_POINT('Ctrl Pts',(2.8723560719568,1.96376778943683,18.9176193743793));
#94665=CARTESIAN_POINT('Ctrl Pts',(-0.0985453520613107,3.47808886437995,
19.0766842782254));
#94666=CARTESIAN_POINT('Ctrl Pts',(-2.97893844147421,1.79798195120084,19.2357491820716));
#94667=CARTESIAN_POINT('Ctrl Pts',(-3.12334498672647,-1.53346973521728,
19.3948140859177));
#94668=CARTESIAN_POINT('Ctrl Pts',(-0.399135740030314,-3.45651616457484,
19.5538789897639));
#94669=CARTESIAN_POINT('Ctrl Pts',(2.69165711873815,-2.20494791096822,19.71294389361));
#94670=CARTESIAN_POINT('Ctrl Pts',(3.31031508682473,1.07174034209662,19.8720087974562));
#94671=CARTESIAN_POINT('Ctrl Pts',(0.888635796380244,3.36409568180341,20.0310737013023));
#94672=CARTESIAN_POINT('Ctrl Pts',(-2.34920523400022,2.56671932697806,20.1901386051485));
#94673=CARTESIAN_POINT('Ctrl Pts',(-3.42943406930774,-0.588043620157575,
20.3492035089946));
#94674=CARTESIAN_POINT('Ctrl Pts',(-1.3599215950672,-3.20272174723417,20.5082684128408));
#94675=CARTESIAN_POINT('Ctrl Pts',(1.95860198105303,-2.87588101540241,20.6673333166869));
#94676=CARTESIAN_POINT('Ctrl Pts',(3.47826036717098,0.0922938410963431,
20.8263982205331));
#94677=CARTESIAN_POINT('Ctrl Pts',(1.80333324954904,2.97570202238189,20.9854631243793));
#94678=CARTESIAN_POINT('Ctrl Pts',(-1.52785350630899,3.1260961274721,21.1445280282254));
#94679=CARTESIAN_POINT('Ctrl Pts',(-3.45579319384513,0.405347673374805,
21.3035929320716));
#94680=CARTESIAN_POINT('Ctrl Pts',(-2.20978220615917,-2.68768970237991,
21.4626578359177));
#94681=CARTESIAN_POINT('Ctrl Pts',(1.06578880781087,-3.3122360350799,21.6217227397639));
#94682=CARTESIAN_POINT('Ctrl Pts',(3.36249305619432,-0.894680826877306,
21.78078764361));
#94683=CARTESIAN_POINT('Ctrl Pts',(2.57093753106305,2.34458814001697,21.9398525474562));
#94684=CARTESIAN_POINT('Ctrl Pts',(-0.581878768354349,3.43048545163438,
22.0989174513023));
#94685=CARTESIAN_POINT('Ctrl Pts',(-3.20027231556393,1.36567581847664,22.2579823551485));
#94686=CARTESIAN_POINT('Ctrl Pts',(-2.87939666837566,-1.95342984544721,
22.4170472589946));
#94687=CARTESIAN_POINT('Ctrl Pts',(0.0860420319779839,-3.47842063351599,
22.5761121628408));
#94688=CARTESIAN_POINT('Ctrl Pts',(2.97245599034753,-1.80867872226767,22.735177066687));
#94689=CARTESIAN_POINT('Ctrl Pts',(3.12883716943083,1.52223234170245,22.8942419705331));
#94690=CARTESIAN_POINT('Ctrl Pts',(0.411558297252309,3.45505905924915,23.0533068743793));
#94691=CARTESIAN_POINT('Ctrl Pts',(-2.68371360349739,2.21460936269578,23.2123717782254));
#94692=CARTESIAN_POINT('Ctrl Pts',(-3.3141462832271,-1.05983383051717,23.3714366820716));
#94693=CARTESIAN_POINT('Ctrl Pts',(-0.90072296712697,-3.36087956812301,
23.5305015859177));
#94694=CARTESIAN_POINT('Ctrl Pts',(2.33996347189163,-2.57514742978914,23.6895664897639));
#94695=CARTESIAN_POINT('Ctrl Pts',(3.43152575185086,0.575712036804067,23.84863139361));
#94696=CARTESIAN_POINT('Ctrl Pts',(1.3714256300995,3.19781254548213,24.0076962974562));
#94697=CARTESIAN_POINT('Ctrl Pts',(-1.9482513993279,2.88290301951934,24.1667612013023));
#94698=CARTESIAN_POINT('Ctrl Pts',(-3.47856966289727,-0.0797899449027475,
24.3258261051485));
#94699=CARTESIAN_POINT('Ctrl Pts',(-1.81401835208813,-2.96920035585748,
24.4848910089946));
#94700=CARTESIAN_POINT('Ctrl Pts',(1.51660625955678,-3.13156810374769,24.6439559128408));
#94701=CARTESIAN_POINT('Ctrl Pts',(3.45431376315845,-0.417767591599538,
24.8030208166869));
#94702=CARTESIAN_POINT('Ctrl Pts',(2.21942936498409,2.67972883493518,24.9620857205332));
#94703=CARTESIAN_POINT('Ctrl Pts',(-1.05387542945276,3.31604582509538,25.1211506243792));
#94704=CARTESIAN_POINT('Ctrl Pts',(-3.35925522280188,0.906762197610325,
25.2802155282254));
#94705=CARTESIAN_POINT('Ctrl Pts',(-2.5793490095563,-2.3353312445642,25.4392804320715));
#94706=CARTESIAN_POINT('Ctrl Pts',(0.569543445428409,-3.43255496659649,
25.5983453359177));
#94707=CARTESIAN_POINT('Ctrl Pts',(3.19534244493507,-1.37717101136099,25.7574102397639));
#94708=CARTESIAN_POINT('Ctrl Pts',(2.88640005750619,1.94306665942397,25.91647514361));
#94709=CARTESIAN_POINT('Ctrl Pts',(-0.073537600067748,3.47870745483333,
26.0755400474562));
#94710=CARTESIAN_POINT('Ctrl Pts',(-2.96593512942888,1.81935212176105,26.2346049513023));
#94711=CARTESIAN_POINT('Ctrl Pts',(-3.13428892160056,-1.51097527804684,
26.3936698551485));
#94712=CARTESIAN_POINT('Ctrl Pts',(-0.42397553635747,-3.45355730798075,
26.5527347589946));
#94713=CARTESIAN_POINT('Ctrl Pts',(2.67573540956612,-2.22424219745308,26.7117996628408));
#94714=CARTESIAN_POINT('Ctrl Pts',(3.31793465454823,1.04791362386632,26.870864566687));
#94715=CARTESIAN_POINT('Ctrl Pts',(0.912798498817672,3.3576200254783,27.0299294705331));
#94716=CARTESIAN_POINT('Ctrl Pts',(-2.33069147299888,2.58354225679144,27.1889943743792));
#94717=CARTESIAN_POINT('Ctrl Pts',(-3.43357309254645,-0.563373014154682,
27.3480592782254));
#94718=CARTESIAN_POINT('Ctrl Pts',(-1.38291194370096,-3.19286202190228,
27.5071241820715));
#94719=CARTESIAN_POINT('Ctrl Pts',(1.93787564248457,-2.88988777103919,27.6661890859177));
#94720=CARTESIAN_POINT('Ctrl Pts',(3.4788340088791,0.0672850176711449,27.8252539897639));
#94721=CARTESIAN_POINT('Ctrl Pts',(1.82468001405561,2.96266032161008,27.98431889361));
#94722=CARTESIAN_POINT('Ctrl Pts',(-1.50533941536355,3.13699961419979,28.1433837974562));
#94723=CARTESIAN_POINT('Ctrl Pts',(-3.45278969615972,0.430182111471415,
28.3024487013023));
#94724=CARTESIAN_POINT('Ctrl Pts',(-2.22904784455505,-2.67173334029076,
28.4615136051485));
#94725=CARTESIAN_POINT('Ctrl Pts',(1.04194843301715,-3.3198127654839,28.6205785089947));
#94726=CARTESIAN_POINT('Ctrl Pts',(3.35597398143476,-0.918831851248986,
28.7796434128408));
#94727=CARTESIAN_POINT('Ctrl Pts',(2.58772715794839,2.32604417218444,28.9387083166869));
#94728=CARTESIAN_POINT('Ctrl Pts',(-0.557200762916511,3.43458012641168,
29.0977732205331));
#94729=CARTESIAN_POINT('Ctrl Pts',(-3.19037128439679,1.38864840857327,29.2568381243793));
#94730=CARTESIAN_POINT('Ctrl Pts',(-2.89336614885126,-1.93267836527921,
29.4159030282254));
#94731=CARTESIAN_POINT('Ctrl Pts',(0.061032217911679,-3.47894932462569,
29.5749679320716));
#94732=CARTESIAN_POINT('Ctrl Pts',(2.95937594298018,-1.83000201176034,29.7340328359177));
#94733=CARTESIAN_POINT('Ctrl Pts',(3.13970017278865,1.49969868971325,29.8930977397638));
#94734=CARTESIAN_POINT('Ctrl Pts',(0.436387296891261,3.45201093017516,30.0521626436101));
#94735=CARTESIAN_POINT('Ctrl Pts',(-2.66772264003783,2.23384629076543,30.2112275474561));
#94736=CARTESIAN_POINT('Ctrl Pts',(-3.32168015183512,-1.03597987617585,
30.3702924513024));
#94737=CARTESIAN_POINT('Ctrl Pts',(-0.924862235413484,-3.35431709598879,
30.5293573551484));
#94738=CARTESIAN_POINT('Ctrl Pts',(2.32138935713386,-2.59190369950783,30.6884222589947));
#94739=CARTESIAN_POINT('Ctrl Pts',(3.43557606493896,0.551026711653098,30.8474871628408));
#94740=CARTESIAN_POINT('Ctrl Pts',(1.39438038744657,3.1878702404648,31.0065520666869));
#94741=CARTESIAN_POINT('Ctrl Pts',(-1.92747484459752,2.89683517970569,31.1656169705331));
#94742=CARTESIAN_POINT('Ctrl Pts',(-3.47905340170063,-0.0547792209889362,
31.3246818743793));
#94743=CARTESIAN_POINT('Ctrl Pts',(-1.83531809768251,-2.95608200414939,
31.4837467782254));
#94744=CARTESIAN_POINT('Ctrl Pts',(1.49405311931838,-3.14239058864294,31.6428116820716));
#94745=CARTESIAN_POINT('Ctrl Pts',(3.45122101254281,-0.442591072571193,
31.8018765859177));
#94746=CARTESIAN_POINT('Ctrl Pts',(2.23863752058297,2.66370332176368,31.9609414897639));
#94747=CARTESIAN_POINT('Ctrl Pts',(-1.03000797262355,3.32353680756941,32.12000639361));
#94748=CARTESIAN_POINT('Ctrl Pts',(-3.35264937449288,0.930889631830323,
32.2790712974562));
#94749=CARTESIAN_POINT('Ctrl Pts',(-2.59607186797765,-2.31672704288437,
32.4381362013023));
#94750=CARTESIAN_POINT('Ctrl Pts',(0.544850880309637,-3.436560904911,32.5972011051485));
#94751=CARTESIAN_POINT('Ctrl Pts',(3.18535889818595,-1.40010786180367,32.7562660089947));
#94752=CARTESIAN_POINT('Ctrl Pts',(2.90029485239572,1.9222650972495,32.9153309128408));
#94753=CARTESIAN_POINT('Ctrl Pts',(-0.0485260471031247,3.47914623976763,
33.074395816687));
#94754=CARTESIAN_POINT('Ctrl Pts',(-2.95277851575862,1.84062825464868,33.2334607205331));
#94755=CARTESIAN_POINT('Ctrl Pts',(-3.14507085307143,-1.48840272241665,
33.3925256243793));
#94756=CARTESIAN_POINT('Ctrl Pts',(-0.44879341847017,-3.45041994581451,
33.5515905282254));
#94757=CARTESIAN_POINT('Ctrl Pts',(2.65967539845273,-2.24342151852971,33.7106554320715));
#94758=CARTESIAN_POINT('Ctrl Pts',(3.32538272668884,1.0240327416525,33.8697203359177));
#94759=CARTESIAN_POINT('Ctrl Pts',(0.936914021027954,3.35097082233462,34.0287852397639));
#94760=CARTESIAN_POINT('Ctrl Pts',(-2.31205724449761,2.60023164989254,34.18785014361));
#94761=CARTESIAN_POINT('Ctrl Pts',(-3.43753464314619,-0.538673288837053,
34.3469150474562));
#94762=CARTESIAN_POINT('Ctrl Pts',(-1.40583081314219,-3.18283726567299,
34.5059799513024));
#94763=CARTESIAN_POINT('Ctrl Pts',(1.91704914006494,-2.90374515574508,34.6650448551485));
#94764=CARTESIAN_POINT('Ctrl Pts',(3.47922783852685,0.0422727164548873,
34.8241097589947));
#94765=CARTESIAN_POINT('Ctrl Pts',(1.84593246550451,2.94946548847979,34.9831746628408));
#94766=CARTESIAN_POINT('Ctrl Pts',(-1.4827475172617,3.14774095741551,35.142239566687));
#94767=CARTESIAN_POINT('Ctrl Pts',(-3.44960773257809,0.454994314551468,
35.3013044705331));
#94768=CARTESIAN_POINT('Ctrl Pts',(-2.24819826915098,-2.65563888311707,
35.4603693743793));
#94769=CARTESIAN_POINT('Ctrl Pts',(1.01805420256545,-3.3272179032302,35.6194342782254));
#94770=CARTESIAN_POINT('Ctrl Pts',(3.34928144493648,-0.942935383544889,
35.7784991820716));
#94771=CARTESIAN_POINT('Ctrl Pts',(2.60438303181454,2.30737997705909,35.9375640859177));
#94772=CARTESIAN_POINT('Ctrl Pts',(-0.532493957191848,3.438497276499,36.0966289897639));
#94773=CARTESIAN_POINT('Ctrl Pts',(-3.1803053510721,1.41154922297418,36.25569389361));
#94774=CARTESIAN_POINT('Ctrl Pts',(-2.90718607860752,-1.91182698989406,
36.4147587974562));
#94775=CARTESIAN_POINT('Ctrl Pts',(0.0360192492456371,-3.47929819771466,
36.5738237013024));
#94776=CARTESIAN_POINT('Ctrl Pts',(2.94614293301552,-1.85123071311478,36.7328886051485));
#94777=CARTESIAN_POINT('Ctrl Pts',(3.15040089304948,1.47708752212243,36.8919535089947));
#94778=CARTESIAN_POINT('Ctrl Pts',(0.461193740783423,3.44878437545738,37.0510184128408));
#94779=CARTESIAN_POINT('Ctrl Pts',(-2.65159378879653,2.2529677570157,37.210083316687));
#94780=CARTESIAN_POINT('Ctrl Pts',(-3.32904233126504,-1.01207237467599,
37.3691482205331));
#94781=CARTESIAN_POINT('Ctrl Pts',(-0.948953699929094,-3.34758124775602,
37.5282131243792));
#94782=CARTESIAN_POINT('Ctrl Pts',(2.3026952556788,-2.60852600033258,37.6872780282255));
#94783=CARTESIAN_POINT('Ctrl Pts',(3.43944880185957,0.526312905336293,37.8463429320715));
#94784=CARTESIAN_POINT('Ctrl Pts',(1.4172630728265,3.17776316256248,38.0054078359178));
#94785=CARTESIAN_POINT('Ctrl Pts',(-1.90659866360674,2.91061760986732,38.1644727397638));
#94786=CARTESIAN_POINT('Ctrl Pts',(-3.47935731710377,-0.029765665676874,
38.32353764361));
#94787=CARTESIAN_POINT('Ctrl Pts',(-1.85652298036374,-2.94281086009925,
38.4826025474562));
#94788=CARTESIAN_POINT('Ctrl Pts',(1.47142275528341,-3.15305065138051,38.6416674513023));
#94789=CARTESIAN_POINT('Ctrl Pts',(3.44794987711221,-0.467391677138788,
38.8007323551485));
#94790=CARTESIAN_POINT('Ctrl Pts',(2.25772996671604,2.6475401285588,38.9597972589946));
#94791=CARTESIAN_POINT('Ctrl Pts',(-1.00608727730826,3.33085600489952,39.1188621628408));
#94792=CARTESIAN_POINT('Ctrl Pts',(-3.3458702362856,0.954968950738659,39.277927066687));
#94793=CARTESIAN_POINT('Ctrl Pts',(-2.61266054206305,-2.29800309549042,
39.4369919705331));
#94794=CARTESIAN_POINT('Ctrl Pts',(0.520130153238007,-3.44038921615408,
39.5960568743793));
#94795=CARTESIAN_POINT('Ctrl Pts',(3.1752107083567,-1.42297234424072,39.7551217782254));
#94796=CARTESIAN_POINT('Ctrl Pts',(2.91403973843892,1.90136417809308,39.9141866820716));
#94797=CARTESIAN_POINT('Ctrl Pts',(-0.023511985950815,3.47940519650318,
40.0732515859177));
#94798=CARTESIAN_POINT('Ctrl Pts',(-2.93946928049521,1.86180925015472,40.2323164897639));
#94799=CARTESIAN_POINT('Ctrl Pts',(-3.15569022384854,-1.46575323504451,
40.39138139361));
#94800=CARTESIAN_POINT('Ctrl Pts',(-0.473588103595339,-3.44710424023842,
40.5504462974562));
#94801=CARTESIAN_POINT('Ctrl Pts',(2.64347791549904,-2.26248488286786,40.7095112013023));
#94802=CARTESIAN_POINT('Ctrl Pts',(3.33265891827465,1.00009892979701,40.8685761051485));
#94803=CARTESIAN_POINT('Ctrl Pts',(0.960981116541363,3.34414841605268,41.0276410089946));
#94804=CARTESIAN_POINT('Ctrl Pts',(-2.29330351165203,2.61678664364926,41.1867059128408));
#94805=CARTESIAN_POINT('Ctrl Pts',(-3.44131851634454,-0.513945720870379,
41.3457708166869));
#94806=CARTESIAN_POINT('Ctrl Pts',(-1.42867701877307,-3.17264799670034,
41.5048357205332));
#94807=CARTESIAN_POINT('Ctrl Pts',(1.89612355026292,-2.91745245326724,41.6639006243792));
#94808=CARTESIAN_POINT('Ctrl Pts',(3.47944183575824,0.0172582302697266,
41.8229655282254));
#94809=CARTESIAN_POINT('Ctrl Pts',(1.86708950541063,2.93611820499827,41.9820304320716));
#94810=CARTESIAN_POINT('Ctrl Pts',(-1.46007897972099,3.15831960192657,42.1410953359177));
#94811=CARTESIAN_POINT('Ctrl Pts',(-3.44624746756781,0.479783000135612,
42.3001602397639));
#94812=CARTESIAN_POINT('Ctrl Pts',(-2.26723249011047,-2.6394071627402,42.45922514361));
#94813=CARTESIAN_POINT('Ctrl Pts',(0.994107351487493,-3.33445106556614,
42.6182900474562));
#94814=CARTESIAN_POINT('Ctrl Pts',(3.34241579261952,-0.966990177915068,
42.7773549513024));
#94815=CARTESIAN_POINT('Ctrl Pts',(2.620904291762,2.28859651934561,42.9364198551484));
#94816=CARTESIAN_POINT('Ctrl Pts',(-0.507759628212212,3.44223669942876,
43.0954847589948));
#94817=CARTESIAN_POINT('Ctrl Pts',(-3.17007503587205,1.43437707799479,43.2545496628407));
#94818=CARTESIAN_POINT('Ctrl Pts',(-2.92085574332787,-1.89087679704625,
43.4136145666871));
#94819=CARTESIAN_POINT('Ctrl Pts',(0.0110044188368612,-3.47946723475014,
43.572679470533));
#94820=CARTESIAN_POINT('Ctrl Pts',(2.93275764443294,-1.87236372907448,43.7317443743794));
#94821=CARTESIAN_POINT('Ctrl Pts',(3.16093877712245,1.45440000764499,43.8908092782254));
#94822=CARTESIAN_POINT('Ctrl Pts',(0.485976346743174,3.44537956186525,44.0498741820716));
#94823=CARTESIAN_POINT('Ctrl Pts',(-2.63532788342538,2.27197277311243,44.2089390859177));
#94824=CARTESIAN_POINT('Ctrl Pts',(-3.33623244099863,-0.988112561746271,
44.3680039897639));
#94825=CARTESIAN_POINT('Ctrl Pts',(-0.972996115420525,-3.34067237156277,
44.52706889361));
#94826=CARTESIAN_POINT('Ctrl Pts',(2.28388213372536,-2.62501347313853,44.6861337974562));
#94827=CARTESIAN_POINT('Ctrl Pts',(3.44314376253889,0.501571895322309,44.8451987013024));
#94828=CARTESIAN_POINT('Ctrl Pts',(1.44007250330464,3.16749183404082,45.0042636051485));
#94829=CARTESIAN_POINT('Ctrl Pts',(-1.88562393503503,2.92424959789918,45.1633285089947));
#94830=CARTESIAN_POINT('Ctrl Pts',(-3.47948139407905,-0.00475057237518032,
45.3223934128408));
#94831=CARTESIAN_POINT('Ctrl Pts',(-1.87763190280657,-2.92938760866342,
45.481458316687));
#94832=CARTESIAN_POINT('Ctrl Pts',(1.44871633468005,-3.16354774286744,45.6405232205331));
#94833=CARTESIAN_POINT('Ctrl Pts',(3.44450053066955,-0.492168119800616,
45.7995881243793));
#94834=CARTESIAN_POINT('Ctrl Pts',(2.27670570752794,2.63124008384628,45.9586530282254));
#94835=CARTESIAN_POINT('Ctrl Pts',(-0.982114562709173,3.33800305195324,
46.1177179320716));
#94836=CARTESIAN_POINT('Ctrl Pts',(-3.33891819138147,0.978998884598715,
46.2767828359177));
#94837=CARTESIAN_POINT('Ctrl Pts',(-2.62911411180905,-2.27916032222356,
46.4358477397639));
#94838=CARTESIAN_POINT('Ctrl Pts',(0.495382422596211,-3.44403979392057,
46.5949126436101));
#94839=CARTESIAN_POINT('Ctrl Pts',(3.16489862768261,-1.44576310238133,46.7539775474562));
#94840=CARTESIAN_POINT('Ctrl Pts',(2.92763357084724,1.88036464943404,46.9130424513024));
#94841=CARTESIAN_POINT('Ctrl Pts',(0.00150411901917797,3.47948494655473,
47.0721073551485));
#94842=CARTESIAN_POINT('Ctrl Pts',(-2.92600969204226,1.88289280238792,47.2311722589946));
#94843=CARTESIAN_POINT('Ctrl Pts',(-3.1661434702008,-1.44302567639757,47.3902371628409));
#94844=CARTESIAN_POINT('Ctrl Pts',(-0.498364061107948,-3.44361476949528,
47.5493020666869));
#94845=CARTESIAN_POINT('Ctrl Pts',(2.62715476810754,-2.28142289884137,47.7083669705332));
#94846=CARTESIAN_POINT('Ctrl Pts',(3.33974192706535,0.976097389996902,47.8674318743792));
#94847=CARTESIAN_POINT('Ctrl Pts',(0.98503845904953,3.33718374751698,48.0264967782254));
#94848=CARTESIAN_POINT('Ctrl Pts',(-2.27450738921853,2.63314803356416,48.1855616820716));
#94849=CARTESIAN_POINT('Ctrl Pts',(-3.44477925969703,-0.489080282373686,
48.3446265859177));
#94850=CARTESIAN_POINT('Ctrl Pts',(-1.45172651666228,-3.16250708908811,
48.5036914897639));
#94851=CARTESIAN_POINT('Ctrl Pts',(1.87562906970625,-2.930603662586,48.66275639361));
#94852=CARTESIAN_POINT('Ctrl Pts',(3.47846261219738,-0.00853227987589602,
48.8218212974562));
#94853=CARTESIAN_POINT('Ctrl Pts',(1.89011874233621,2.92411545551553,48.9808862013023));
#94854=CARTESIAN_POINT('Ctrl Pts',(-1.44140102367388,3.16572539725362,49.1399511051485));
#94855=CARTESIAN_POINT('Ctrl Pts',(-2.76878294100723,1.39636109408963,49.2459943743793));
#94856=CARTESIAN_POINT('Ctrl Pts',(-2.91090525077888,0.426608275808069,
49.2990160089947));
#94857=CARTESIAN_POINT('Ctrl Pts',(1.59774743137957,-2.24059110187418,-0.219489327336923));
#94858=CARTESIAN_POINT('Ctrl Pts',(2.34418860636375,-1.70830992437181,-0.166467692721538));
#94859=CARTESIAN_POINT('Ctrl Pts',(3.25014150704371,0.151809149222066,-0.0604244234907686));
#94860=CARTESIAN_POINT('Ctrl Pts',(1.6268027386243,2.82145002145618,0.0986404803553848));
#94861=CARTESIAN_POINT('Ctrl Pts',(-1.49208184042344,2.89144224391758,0.25770538420154));
#94862=CARTESIAN_POINT('Ctrl Pts',(-3.23982742326958,0.309969044999859,
0.416770288047693));
#94863=CARTESIAN_POINT('Ctrl Pts',(-2.01236614540808,-2.55835226526823,
0.575835191893847));
#94864=CARTESIAN_POINT('Ctrl Pts',(1.06354492009181,-3.07584232922318,0.73490009574));
#94865=CARTESIAN_POINT('Ctrl Pts',(3.16254249998669,-0.768936849748424,
0.893964999586155));
#94866=CARTESIAN_POINT('Ctrl Pts',(2.35697999816324,2.24450383333788,1.05302990343231));
#94867=CARTESIAN_POINT('Ctrl Pts',(-0.613364952226834,3.19633203595468,
1.21209480727846));
#94868=CARTESIAN_POINT('Ctrl Pts',(-3.02035336785881,1.21259520961831,1.37115971112462));
#94869=CARTESIAN_POINT('Ctrl Pts',(-2.65332609790095,-1.88488644904668,
1.53022461497077));
#94870=CARTESIAN_POINT('Ctrl Pts',(0.150635447626677,-3.25118304023235,
1.68928951881692));
#94871=CARTESIAN_POINT('Ctrl Pts',(2.81624461719718,-1.63146409541665,1.84835442266308));
#94872=CARTESIAN_POINT('Ctrl Pts',(2.89529349317861,1.48666882418481,2.00741932650923));
#94873=CARTESIAN_POINT('Ctrl Pts',(0.315178367329934,3.23937710260303,2.16648423035539));
#94874=CARTESIAN_POINT('Ctrl Pts',(-2.55440994851684,2.01690241981572,2.32554913420154));
#94875=CARTESIAN_POINT('Ctrl Pts',(-3.07791730894721,-1.05798403748725,
2.4846140380477));
#94876=CARTESIAN_POINT('Ctrl Pts',(-0.7745315427828,-3.16117148326227,2.64367894189385));
#94877=CARTESIAN_POINT('Ctrl Pts',(2.2402176109151,-2.36100189344623,2.80274384574));
#94878=CARTESIAN_POINT('Ctrl Pts',(3.19745356402969,0.607614589848881,2.96180874958616));
#94879=CARTESIAN_POINT('Ctrl Pts',(1.21800917393199,3.01817135381553,3.12087365343231));
#94880=CARTESIAN_POINT('Ctrl Pts',(-1.88010777557473,2.65670839839355,3.27993855727847));
#94881=CARTESIAN_POINT('Ctrl Pts',(-3.25145202864119,-0.144791043152296,
3.43900346112461));
#94882=CARTESIAN_POINT('Ctrl Pts',(-1.63652141245871,-2.81330808723417,
3.59806836497077));
#94883=CARTESIAN_POINT('Ctrl Pts',(1.48146159934009,-2.89796070890096,3.75713326881692));
#94884=CARTESIAN_POINT('Ctrl Pts',(3.23880588710515,-0.321000252924548,
3.91619817266308));
#94885=CARTESIAN_POINT('Ctrl Pts',(2.02149007324339,2.55078078615448,4.07526307650923));
#94886=CARTESIAN_POINT('Ctrl Pts',(-1.05245008777951,3.07981388234626,4.23432798035539));
#94887=CARTESIAN_POINT('Ctrl Pts',(-3.15977434353249,0.780212044531519,
4.39339288420154));
#94888=CARTESIAN_POINT('Ctrl Pts',(-2.36502450260688,-2.23597044667527,
4.5524577880477));
#94889=CARTESIAN_POINT('Ctrl Pts',(0.601866637244319,-3.19854049334634,
4.71152269189385));
#94890=CARTESIAN_POINT('Ctrl Pts',(3.01597729733724,-1.22343192636024,4.87058759574001));
#94891=CARTESIAN_POINT('Ctrl Pts',(2.66008331814616,1.87532969821363,5.02965249958615));
#94892=CARTESIAN_POINT('Ctrl Pts',(-0.138946800905478,3.25170701678921,
5.18871740343232));
#94893=CARTESIAN_POINT('Ctrl Pts',(-2.8103621386866,1.64157527574487,5.34778230727846));
#94894=CARTESIAN_POINT('Ctrl Pts',(-2.90061873595268,-1.47625054958176,
5.50684721112463));
#94895=CARTESIAN_POINT('Ctrl Pts',(-0.326821010774226,-3.23822370496875,
5.66591211497077));
#94896=CARTESIAN_POINT('Ctrl Pts',(2.5471433359694,-2.02607146037076,5.82497701881693));
#94897=CARTESIAN_POINT('Ctrl Pts',(3.08170053141509,1.04691287659405,5.98404192266308));
#94898=CARTESIAN_POINT('Ctrl Pts',(0.785890012745933,3.15836692364413,6.14310682650924));
#94899=CARTESIAN_POINT('Ctrl Pts',(-2.23171605232569,2.36903950965249,6.30217173035538));
#94900=CARTESIAN_POINT('Ctrl Pts',(-3.19961709343961,-0.596116760267523,
6.46123663420156));
#94901=CARTESIAN_POINT('Ctrl Pts',(-1.22885072463386,-3.01377348735263,
6.62030153804768));
#94902=CARTESIAN_POINT('Ctrl Pts',(1.87054556165231,-2.66344965003764,6.77936644189386));
#94903=CARTESIAN_POINT('Ctrl Pts',(3.2519515008847,0.133102112667476,6.93843134574));
#94904=CARTESIAN_POINT('Ctrl Pts',(1.64662383568568,2.80740710981763,7.09749624958616));
#94905=CARTESIAN_POINT('Ctrl Pts',(-1.47103473068521,2.90326739340707,7.25656115343231));
#94906=CARTESIAN_POINT('Ctrl Pts',(-3.23763106189424,0.33264071242159,7.41562605727848));
#94907=CARTESIAN_POINT('Ctrl Pts',(-2.03064630227834,-2.54349765707501,
7.57469096112461));
#94908=CARTESIAN_POINT('Ctrl Pts',(1.04137228335836,-3.08357722522978,7.73375586497078));
#94909=CARTESIAN_POINT('Ctrl Pts',(3.15694930072946,-0.791565442099757,
7.89282076881693));
#94910=CARTESIAN_POINT('Ctrl Pts',(2.37304686356079,2.2274544484337,8.05188567266308));
#94911=CARTESIAN_POINT('Ctrl Pts',(-0.590364957545297,3.2006833572544,8.21095057650924));
#94912=CARTESIAN_POINT('Ctrl Pts',(-3.01155994143853,1.23426555312279,8.37001548035538));
#94913=CARTESIAN_POINT('Ctrl Pts',(-2.66680737771094,-1.86575538232892,
8.52908038420155));
#94914=CARTESIAN_POINT('Ctrl Pts',(0.127256994445537,-3.25218547962251,
8.6881452880477));
#94915=CARTESIAN_POINT('Ctrl Pts',(2.80444301168003,-1.651667076242,8.84721019189386));
#94916=CARTESIAN_POINT('Ctrl Pts',(2.90590667191787,1.46581415964166,9.00627509574));
#94917=CARTESIAN_POINT('Ctrl Pts',(0.33845933948028,3.23702795972191,9.16533999958617));
#94918=CARTESIAN_POINT('Ctrl Pts',(-2.53984376146567,2.03521458422612,9.3244049034323));
#94919=CARTESIAN_POINT('Ctrl Pts',(-3.08544395761391,-1.03582832599161,
9.48346980727847));
#94920=CARTESIAN_POINT('Ctrl Pts',(-0.797238314318297,-3.15552147935736,
9.64253471112462));
#94921=CARTESIAN_POINT('Ctrl Pts',(2.22318564879756,-2.37704655139174,9.80159961497078));
#94922=CARTESIAN_POINT('Ctrl Pts',(3.20173928132981,0.584611247661624,9.96066451881693));
#94923=CARTESIAN_POINT('Ctrl Pts',(1.23967639434314,3.00933666674422,10.1197294226631));
#94924=CARTESIAN_POINT('Ctrl Pts',(-1.86095917572251,2.6701564903198,10.2787943265092));
#94925=CARTESIAN_POINT('Ctrl Pts',(-3.25240895224441,-0.121411465122582,
10.4378592303554));
#94926=CARTESIAN_POINT('Ctrl Pts',(-1.65670498112303,-2.80146985384903,
10.5969241342015));
#94927=CARTESIAN_POINT('Ctrl Pts',(1.4605888533167,-2.90853656295908,10.7559890380477));
#94928=CARTESIAN_POINT('Ctrl Pts',(3.23641440039971,-0.344276873153268,
10.9150539418939));
#94929=CARTESIAN_POINT('Ctrl Pts',(2.03977629145653,2.53618166094517,11.07411884574));
#94930=CARTESIAN_POINT('Ctrl Pts',(-1.03028102240352,3.08730072253707,11.2331837495862));
#94931=CARTESIAN_POINT('Ctrl Pts',(-3.15408346414037,0.80290861107543,11.3922486534323));
#94932=CARTESIAN_POINT('Ctrl Pts',(-2.38103856022442,-2.21890966720757,
11.5513135572785));
#94933=CARTESIAN_POINT('Ctrl Pts',(0.578855649203793,-3.20278486225466,
11.7103784611246));
#94934=CARTESIAN_POINT('Ctrl Pts',(3.00710367045189,-1.24508323081533,11.8694433649708));
#94935=CARTESIAN_POINT('Ctrl Pts',(2.67349697704504,1.85615695732711,12.0285082688169));
#94936=CARTESIAN_POINT('Ctrl Pts',(-0.115565543582453,3.25262191802848,
12.1875731726631));
#94937=CARTESIAN_POINT('Ctrl Pts',(-2.79848764592934,1.66173753405392,12.3466380765092));
#94938=CARTESIAN_POINT('Ctrl Pts',(-2.91115705803489,-1.45535882859056,
12.5057029803554));
#94939=CARTESIAN_POINT('Ctrl Pts',(-0.350093294647169,-3.23579038590974,
12.6647678842015));
#94940=CARTESIAN_POINT('Ctrl Pts',(2.53251136734384,-2.0443314092331,12.8238327880477));
#94941=CARTESIAN_POINT('Ctrl Pts',(3.08914751400102,1.02473039051453,12.9828976918939));
#94942=CARTESIAN_POINT('Ctrl Pts',(0.808576314053412,3.15263525972394,13.14196259574));
#94943=CARTESIAN_POINT('Ctrl Pts',(-2.21462651747716,2.38502287716278,13.3010274995862));
#94944=CARTESIAN_POINT('Ctrl Pts',(-3.20382009665126,-0.573098180765103,
13.4600924034323));
#94945=CARTESIAN_POINT('Ctrl Pts',(-1.25048604507266,-3.00486095977523,
13.6191573072785));
#94946=CARTESIAN_POINT('Ctrl Pts',(1.85134874265622,-2.67682882709524,13.7782222111246));
#94947=CARTESIAN_POINT('Ctrl Pts',(3.25282437628674,0.109719248710308,13.9372871149708));
#94948=CARTESIAN_POINT('Ctrl Pts',(1.6667647187771,2.79549639755494,14.0963520188169));
#94949=CARTESIAN_POINT('Ctrl Pts',(-1.45012410235871,2.91376814867984,14.2554169226631));
#94950=CARTESIAN_POINT('Ctrl Pts',(-3.23515591826786,0.355908585172157,
14.4144818265092));
#94951=CARTESIAN_POINT('Ctrl Pts',(-2.04887992284062,-2.52883289251848,
14.5735467303554));
#94952=CARTESIAN_POINT('Ctrl Pts',(1.01917644825584,-3.09098432603974,14.7326116342016));
#94953=CARTESIAN_POINT('Ctrl Pts',(3.15117687078646,-0.814241404942834,
14.8916765380477));
#94954=CARTESIAN_POINT('Ctrl Pts',(2.38899948933553,2.21033621344296,15.0507414418939));
#94955=CARTESIAN_POINT('Ctrl Pts',(-0.567338860944949,3.20484498117529,
15.20980634574));
#94956=CARTESIAN_POINT('Ctrl Pts',(-3.00260854195925,1.25588481966146,15.3688712495862));
#94957=CARTESIAN_POINT('Ctrl Pts',(-2.68015202970693,-1.84653454724265,
15.5279361534323));
#94958=CARTESIAN_POINT('Ctrl Pts',(0.103872599392466,-3.25301632636516,
15.6870010572785));
#94959=CARTESIAN_POINT('Ctrl Pts',(2.79249611838898,-1.67178651905237,15.8460659611246));
#94960=CARTESIAN_POINT('Ctrl Pts',(2.91636982645886,1.44488469153185,16.0051308649708));
#94961=CARTESIAN_POINT('Ctrl Pts',(0.361722725942028,3.23451099952371,16.1641957688169));
#94962=CARTESIAN_POINT('Ctrl Pts',(-2.52514624835235,2.05342181758519,16.3232606726631));
#94963=CARTESIAN_POINT('Ctrl Pts',(-3.09281115271945,-1.01361921356935,
16.4823255765092));
#94964=CARTESIAN_POINT('Ctrl Pts',(-0.81990386544276,-3.14970830203922,
16.6413904803554));
#94965=CARTESIAN_POINT('Ctrl Pts',(2.2060387689647,-2.39296838389635,16.8004553842016));
#94966=CARTESIAN_POINT('Ctrl Pts',(3.20585951251589,0.56157770834868,16.9595202880477));
#94967=CARTESIAN_POINT('Ctrl Pts',(1.26127953714111,3.00034642428035,17.1185851918939));
#94968=CARTESIAN_POINT('Ctrl Pts',(-1.84171438663855,2.6834665741446,17.27765009574));
#94969=CARTESIAN_POINT('Ctrl Pts',(-3.25319776764363,-0.0980256145163866,
17.4367149995862));
#94970=CARTESIAN_POINT('Ctrl Pts',(-1.67680291865692,-2.7894868181238,17.5957799034323));
#94971=CARTESIAN_POINT('Ctrl Pts',(1.43964061303579,-2.91896208296729,17.7548448072785));
#94972=CARTESIAN_POINT('Ctrl Pts',(3.23385563176069,-0.367535698174335,
17.9139097111246));
#94973=CARTESIAN_POINT('Ctrl Pts',(2.05795707879432,2.52145144675506,18.0729746149708));
#94974=CARTESIAN_POINT('Ctrl Pts',(-1.00805870440757,3.09462798813861,18.2320395188169));
#94975=CARTESIAN_POINT('Ctrl Pts',(-3.14822955822641,0.825563677260734,
18.3911044226631));
#94976=CARTESIAN_POINT('Ctrl Pts',(-2.3969295480238,-2.20173419792519,18.5501693265093));
#94977=CARTESIAN_POINT('Ctrl Pts',(0.55581474158759,-3.20686368739564,18.7092342303554));
#94978=CARTESIAN_POINT('Ctrl Pts',(2.99807461404624,-1.26667018008408,18.8682991342016));
#94979=CARTESIAN_POINT('Ctrl Pts',(2.68677244970067,1.83688827641538,19.0273640380477));
#94980=CARTESIAN_POINT('Ctrl Pts',(-0.0921783129706565,3.25336869953601,
19.1864289418939));
#94981=CARTESIAN_POINT('Ctrl Pts',(-2.78646850648086,1.68181390138538,19.34549384574));
#94982=CARTESIAN_POINT('Ctrl Pts',(-2.92154490983091,-1.43439188381135,
19.5045587495862));
#94983=CARTESIAN_POINT('Ctrl Pts',(-0.37334748309046,-3.23318981709592,
19.6636236534323));
#94984=CARTESIAN_POINT('Ctrl Pts',(2.51774849966255,-2.06248569181699,19.8226885572785));
#94985=CARTESIAN_POINT('Ctrl Pts',(3.09643482642802,1.00249493873363,19.9817534611246));
#94986=CARTESIAN_POINT('Ctrl Pts',(0.831220822112772,3.14674064412511,20.1408183649708));
#94987=CARTESIAN_POINT('Ctrl Pts',(-2.19742251423028,2.40088296892136,20.2998832688169));
#94988=CARTESIAN_POINT('Ctrl Pts',(-3.20785750257054,-0.550049979278808,
20.4589481726631));
#94989=CARTESIAN_POINT('Ctrl Pts',(-1.27205673107604,-2.99579311859597,
20.6180130765092));
#94990=CARTESIAN_POINT('Ctrl Pts',(1.83205623216379,-2.69006964569557,20.7770779803554));
#94991=CARTESIAN_POINT('Ctrl Pts',(3.25352912149012,0.0863307136449077,
20.9361428842016));
#94992=CARTESIAN_POINT('Ctrl Pts',(1.68681945104979,2.78344119321081,21.0952077880477));
#94993=CARTESIAN_POINT('Ctrl Pts',(-1.42913852081457,2.9241182987059,21.2542726918939));
#94994=CARTESIAN_POINT('Ctrl Pts',(-3.23251355768036,0.379158061915388,
21.41333759574));
#94995=CARTESIAN_POINT('Ctrl Pts',(-2.06700764202351,-2.51403741903719,
21.5724024995862));
#94996=CARTESIAN_POINT('Ctrl Pts',(0.996927934521134,-3.09823166175065,
21.7314674034323));
#94997=CARTESIAN_POINT('Ctrl Pts',(3.1452415645452,-0.836875281723708,21.8905323072785));
#94998=CARTESIAN_POINT('Ctrl Pts',(2.40482863381765,2.19310373180877,22.0495972111246));
#94999=CARTESIAN_POINT('Ctrl Pts',(-0.544283440045353,3.20884095483013,
22.2086621149708));
#95000=CARTESIAN_POINT('Ctrl Pts',(-2.99350194529984,1.27743917271579,22.367727018817));
#95001=CARTESIAN_POINT('Ctrl Pts',(-2.69335815147779,-1.82721826949352,
22.5267919226631));
#95002=CARTESIAN_POINT('Ctrl Pts',(0.0804828354295357,-3.25367903298773,
22.6858568265093));
#95003=CARTESIAN_POINT('Ctrl Pts',(2.78040488809325,-1.69181955147998,22.8449217303554));
#95004=CARTESIAN_POINT('Ctrl Pts',(2.92668224127907,1.42388054101619,23.0039866342016));
#95005=CARTESIAN_POINT('Ctrl Pts',(0.384967415878305,3.23182685569862,23.1630515380477));
#95006=CARTESIAN_POINT('Ctrl Pts',(-2.51031821686753,2.07152291480586,23.3221164418939));
#95007=CARTESIAN_POINT('Ctrl Pts',(-3.1000184883019,-0.991357709754248,
23.48118134574));
#95008=CARTESIAN_POINT('Ctrl Pts',(-0.84252703782683,-3.1437323243294,23.6402462495862));
#95009=CARTESIAN_POINT('Ctrl Pts',(2.18877786461233,-2.40876652996629,23.7993111534323));
#95010=CARTESIAN_POINT('Ctrl Pts',(3.20981404099739,0.538515142515751,23.9583760572785));
#95011=CARTESIAN_POINT('Ctrl Pts',(1.28281748761557,2.99120110155944,24.1174409611246));
#95012=CARTESIAN_POINT('Ctrl Pts',(-1.82237440403357,2.69663795642391,24.2765058649708));
#95013=CARTESIAN_POINT('Ctrl Pts',(-3.25381843354455,-0.074634697216143,
24.4355707688169));
#95014=CARTESIAN_POINT('Ctrl Pts',(-1.69681418652307,-2.77735960093697,
24.5946356726631));
#95015=CARTESIAN_POINT('Ctrl Pts',(1.41861796140208,-2.92923672926757,24.7537005765093));
#95016=CARTESIAN_POINT('Ctrl Pts',(3.23112971336905,-0.390775526212221,
24.9127654803554));
#95017=CARTESIAN_POINT('Ctrl Pts',(2.07603149557764,2.50659090516829,25.0718303842016));
#95018=CARTESIAN_POINT('Ctrl Pts',(-0.985784282427312,3.10179530030949,
25.2308952880477));
#95019=CARTESIAN_POINT('Ctrl Pts',(-3.14221292835331,0.848176072164354,
25.3899601918939));
#95020=CARTESIAN_POINT('Ctrl Pts',(-2.41269664464596,-2.18444492661569,
25.54902509574));
#95021=CARTESIAN_POINT('Ctrl Pts',(0.532745105324541,-3.21077675792875,
25.7080899995862));
#95022=CARTESIAN_POINT('Ctrl Pts',(2.98889059480765,-1.2881916584007,25.8671549034324));
#95023=CARTESIAN_POINT('Ctrl Pts',(2.69990904993852,1.81752465143196,26.0262198072784));
#95024=CARTESIAN_POINT('Ctrl Pts',(-0.0687863178969091,3.25394732271021,
26.1852847111247));
#95025=CARTESIAN_POINT('Ctrl Pts',(-2.77430534157964,1.70180334004416,26.3443496149708));
#95026=CARTESIAN_POINT('Ctrl Pts',(-2.93178175441925,-1.41335079897282,
26.503414518817));
#95027=CARTESIAN_POINT('Ctrl Pts',(-0.39658237415413,-3.23042213294379,
26.6624794226631));
#95028=CARTESIAN_POINT('Ctrl Pts',(2.50285549598059,-2.08053336977387,26.8215443265093));
#95029=CARTESIAN_POINT('Ctrl Pts',(3.10356209203342,0.980207670545344,26.9806092303554));
#95030=CARTESIAN_POINT('Ctrl Pts',(0.853822366487097,3.14068338152529,27.1396741342016));
#95031=CARTESIAN_POINT('Ctrl Pts',(-2.18010493181619,2.41661896516052,27.2987390380477));
#95032=CARTESIAN_POINT('Ctrl Pts',(-3.21172910251423,-0.526973347111528,
27.4578039418939));
#95033=CARTESIAN_POINT('Ctrl Pts',(-1.29356166771021,-2.98657043250842,
27.61686884574));
#95034=CARTESIAN_POINT('Ctrl Pts',(1.81266902735566,-2.7031714214545,27.7759337495863));
#95035=CARTESIAN_POINT('Ctrl Pts',(3.2540657000684,0.0629377163649865,27.9349986534323));
#95036=CARTESIAN_POINT('Ctrl Pts',(1.70678699592574,2.77124211988804,28.0940635572785));
#95037=CARTESIAN_POINT('Ctrl Pts',(-1.408079070744,2.9343173085124,28.2531284611246));
#95038=CARTESIAN_POINT('Ctrl Pts',(-3.22970411670864,0.402387940945082,
28.4121933649708));
#95039=CARTESIAN_POINT('Ctrl Pts',(-2.08502852285137,-2.49911200137148,
28.571258268817));
#95040=CARTESIAN_POINT('Ctrl Pts',(0.974627892123291,-3.10531885776615,
28.7303231726631));
#95041=CARTESIAN_POINT('Ctrl Pts',(3.13914368878651,-0.859465902554945,
28.8893880765092));
#95042=CARTESIAN_POINT('Ctrl Pts',(2.42053347883902,2.17575789423417,29.0484529803554));
#95043=CARTESIAN_POINT('Ctrl Pts',(-0.521199886522412,3.21267107167726,
29.2075178842015));
#95044=CARTESIAN_POINT('Ctrl Pts',(-2.98424062215708,1.29892749819622,29.3665827880478));
#95045=CARTESIAN_POINT('Ctrl Pts',(-2.70642506043275,-1.8078075474907,29.5256476918938));
#95046=CARTESIAN_POINT('Ctrl Pts',(0.0570889115140672,-3.25417356523664,
29.68471259574));
#95047=CARTESIAN_POINT('Ctrl Pts',(2.76816994575776,-1.71176513806837,29.8437774995862));
#95048=CARTESIAN_POINT('Ctrl Pts',(2.93684338335604,1.40280279374565,30.0028424034323));
#95049=CARTESIAN_POINT('Ctrl Pts',(0.40819220783041,3.22897566698317,30.1619073072785));
#95050=CARTESIAN_POINT('Ctrl Pts',(-2.49536043343434,2.08951694028864,30.3209722111246));
#95051=CARTESIAN_POINT('Ctrl Pts',(-3.10706559183244,-0.969044965186682,
30.4800371149708));
#95052=CARTESIAN_POINT('Ctrl Pts',(-0.865106662136416,-3.13759385511094,
30.6391020188169));
#95053=CARTESIAN_POINT('Ctrl Pts',(2.17140382791264,-2.42444017303564,30.7981669226631));
#95054=CARTESIAN_POINT('Ctrl Pts',(3.21360266237481,0.515424742208121,30.9572318265092));
#95055=CARTESIAN_POINT('Ctrl Pts',(1.30428913252471,2.98190117127995,31.1162967303554));
#95056=CARTESIAN_POINT('Ctrl Pts',(-1.80294022754192,2.70966995636255,31.2753616342015));
#95057=CARTESIAN_POINT('Ctrl Pts',(-3.25427091786653,-0.0512399222386381,
31.4344265380477));
#95058=CARTESIAN_POINT('Ctrl Pts',(-1.71673775039014,-2.7650888291135,31.5934914418938));
#95059=CARTESIAN_POINT('Ctrl Pts',(1.39752198502285,-2.93935997078965,31.7525563457401));
#95060=CARTESIAN_POINT('Ctrl Pts',(3.22823678612057,-0.41399515605946,31.9116212495861));
#95061=CARTESIAN_POINT('Ctrl Pts',(2.09399860758597,2.49160080428844,32.0706861534323));
#95062=CARTESIAN_POINT('Ctrl Pts',(-0.96345890777087,3.10880228858957,32.2297510572785));
#95063=CARTESIAN_POINT('Ctrl Pts',(-3.13603388550525,0.870744627009331,
32.3888159611247));
#95064=CARTESIAN_POINT('Ctrl Pts',(-2.42833903512999,-2.16704274691726,
32.5478808649708));
#95065=CARTESIAN_POINT('Ctrl Pts',(0.509647932825191,-3.21452387159745,
32.706945768817));
#95066=CARTESIAN_POINT('Ctrl Pts',(2.97955208743464,-1.30964655337489,32.8660106726631));
#95067=CARTESIAN_POINT('Ctrl Pts',(2.71290609876123,1.79806708323324,33.0250755765093));
#95068=CARTESIAN_POINT('Ctrl Pts',(-0.0453907674337705,3.25435775764352,
33.1841404803554));
#95069=CARTESIAN_POINT('Ctrl Pts',(-2.76199877990863,1.7217048168272,33.3432053842015));
#95070=CARTESIAN_POINT('Ctrl Pts',(-2.94186706268354,-1.39223666163496,
33.5022702880478));
#95071=CARTESIAN_POINT('Ctrl Pts',(-0.419796766886049,-3.22748747650781,
33.6613351918938));
#95072=CARTESIAN_POINT('Ctrl Pts',(2.48783312607924,-2.09847351026542,33.8204000957401));
#95073=CARTESIAN_POINT('Ctrl Pts',(3.11052894242712,0.957869737921647,33.9794649995861));
#95074=CARTESIAN_POINT('Ctrl Pts',(0.87637977896019,3.13446378500892,34.1385299034323));
#95075=CARTESIAN_POINT('Ctrl Pts',(-2.16267466533653,2.43223005252675,34.2975948072785));
#95076=CARTESIAN_POINT('Ctrl Pts',(-3.21543469636917,-0.5038694770355,34.4566597111246));
#95077=CARTESIAN_POINT('Ctrl Pts',(-1.3149997434398,-2.97719337820976,34.6157246149708));
#95078=CARTESIAN_POINT('Ctrl Pts',(1.79318813030706,-2.7161334771746,34.774789518817));
#95079=CARTESIAN_POINT('Ctrl Pts',(3.25443408428712,0.0395414659949287,
34.933854422663));
#95080=CARTESIAN_POINT('Ctrl Pts',(1.72666632133354,2.75889980812558,35.0929193265093));
#95081=CARTESIAN_POINT('Ctrl Pts',(-1.38694684065627,2.94436465093854,35.2519842303554));
#95082=CARTESIAN_POINT('Ctrl Pts',(-3.22672774056554,0.425597021568032,
35.4110491342015));
#95083=CARTESIAN_POINT('Ctrl Pts',(-2.10294163387085,-2.48405741097813,
35.5701140380478));
#95084=CARTESIAN_POINT('Ctrl Pts',(0.9522774736946,-3.11224554776717,35.7291789418938));
#95085=CARTESIAN_POINT('Ctrl Pts',(3.13288355869409,-0.882012099784934,
35.8882438457401));
#95086=CARTESIAN_POINT('Ctrl Pts',(2.43611321265621,2.15829959728129,36.0473087495861));
#95087=CARTESIAN_POINT('Ctrl Pts',(-0.498089393506169,3.21633513374765,
36.2063736534324));
#95088=CARTESIAN_POINT('Ctrl Pts',(-2.97482505122513,1.32034868542603,36.3654385572784));
#95089=CARTESIAN_POINT('Ctrl Pts',(-2.7193520811766,-1.78830338452491,36.5245034611247));
#95090=CARTESIAN_POINT('Ctrl Pts',(0.0336920368183218,-3.25449989755074,
36.6835683649708));
#95091=CARTESIAN_POINT('Ctrl Pts',(2.75579192377546,-1.73162224788107,36.842633268817));
#95092=CARTESIAN_POINT('Ctrl Pts',(2.94685272748626,1.3816525391753,37.0016981726631));
#95093=CARTESIAN_POINT('Ctrl Pts',(0.431395901367992,3.22595758074802,37.1607630765093));
#95094=CARTESIAN_POINT('Ctrl Pts',(-2.48027367118244,2.1074029639682,37.3198279803554));
#95095=CARTESIAN_POINT('Ctrl Pts',(-3.11395209906432,-0.946682133155469,
37.4788928842016));
#95096=CARTESIAN_POINT('Ctrl Pts',(-0.887641571288324,-3.1312932116657,
37.6379577880477));
#95097=CARTESIAN_POINT('Ctrl Pts',(2.15391755688526,-2.43998850297376,37.7970226918939));
#95098=CARTESIAN_POINT('Ctrl Pts',(3.21722518082396,0.49230770090969,37.95608759574));
#95099=CARTESIAN_POINT('Ctrl Pts',(1.32569336205399,2.97244711413151,38.1151524995862));
#95100=CARTESIAN_POINT('Ctrl Pts',(-1.7834128616667,2.72256190036968,38.2742174034323));
#95101=CARTESIAN_POINT('Ctrl Pts',(-3.25455519722178,-0.0278424988002109,
38.4332823072785));
#95102=CARTESIAN_POINT('Ctrl Pts',(-1.73657258045988,-2.75267513689822,
38.5923472111246));
#95103=CARTESIAN_POINT('Ctrl Pts',(1.37635377429526,-2.94933128428904,38.7514121149708));
#95104=CARTESIAN_POINT('Ctrl Pts',(3.22517699954328,-0.437193387552653,
38.910477018817));
#95105=CARTESIAN_POINT('Ctrl Pts',(2.11185748614512,2.47648191891553,39.0695419226631));
#95106=CARTESIAN_POINT('Ctrl Pts',(-0.941083734379852,3.11564859080552,
39.2286068265092));
#95107=CARTESIAN_POINT('Ctrl Pts',(-3.12969274906124,0.893268175284591,
39.3876717303555));
#95108=CARTESIAN_POINT('Ctrl Pts',(-2.44385591096055,-2.14952855830434,
39.5467366342015));
#95109=CARTESIAN_POINT('Ctrl Pts',(0.486524417923579,-3.21810483472289,
39.7058015380477));
#95110=CARTESIAN_POINT('Ctrl Pts',(2.97005957461085,-1.33103375605782,39.8648664418939));
#95111=CARTESIAN_POINT('Ctrl Pts',(2.72576292438452,1.77851657753127,40.02393134574));
#95112=CARTESIAN_POINT('Ctrl Pts',(-0.0219928708375552,3.25459998312159,
40.1829962495862));
#95113=CARTESIAN_POINT('Ctrl Pts',(-2.74954945756262,1.74151730307793,40.3420611534324));
#95114=CARTESIAN_POINT('Ctrl Pts',(-2.95180031333992,-1.37105056313366,
40.5011260572785));
#95115=CARTESIAN_POINT('Ctrl Pts',(-0.442989461393428,-3.22438599947294,
40.6601909611247));
#95116=CARTESIAN_POINT('Ctrl Pts',(2.47268216642652,-2.11630518601147,40.8192558649708));
#95117=CARTESIAN_POINT('Ctrl Pts',(3.11733501751034,0.935482295453273,40.978320768817));
#95118=CARTESIAN_POINT('Ctrl Pts',(0.898891893597044,3.12808217605105,41.1373856726631));
#95119=CARTESIAN_POINT('Ctrl Pts',(-2.14513261571724,2.44771542412284,41.2964505765093));
#95120=CARTESIAN_POINT('Ctrl Pts',(-3.21897409260272,-0.480739563230735,
41.4555154803553));
#95121=CARTESIAN_POINT('Ctrl Pts',(-1.33636985018545,-2.96766244037597,
41.6145803842017));
#95122=CARTESIAN_POINT('Ctrl Pts',(1.77361454793589,-2.72895514288032,41.7736452880476));
#95123=CARTESIAN_POINT('Ctrl Pts',(3.2546342551055,0.0161431718273427,41.9327101918939));
#95124=CARTESIAN_POINT('Ctrl Pts',(1.74645639976147,2.74641489586606,42.0917750957401));
#95125=CARTESIAN_POINT('Ctrl Pts',(-1.3657429228224,2.95425980666279,42.2508399995862));
#95126=CARTESIAN_POINT('Ctrl Pts',(-3.22358458309233,0.448784104166184,
42.4099049034324));
#95127=CARTESIAN_POINT('Ctrl Pts',(-2.120746049199,-2.46887442599044,42.5689698072784));
#95128=CARTESIAN_POINT('Ctrl Pts',(0.929877834471077,-3.1190113737308,42.7280347111247));
#95129=CARTESIAN_POINT('Ctrl Pts',(3.12646149783801,-0.904512708058399,
42.8870996149708));
#95130=CARTESIAN_POINT('Ctrl Pts',(2.45156702999263,2.14072974332502,43.0461645188169));
#95131=CARTESIAN_POINT('Ctrl Pts',(-0.474953155519126,3.21983295165524,
43.2052294226632));
#95132=CARTESIAN_POINT('Ctrl Pts',(-2.96525571917066,1.3417016271988,43.3642943265092));
#95133=CARTESIAN_POINT('Ctrl Pts',(-2.73213854554495,-1.7687067887167,43.5233592303554));
#95134=CARTESIAN_POINT('Ctrl Pts',(0.0102934206674854,-3.25465801306237,
43.6824241342016));
#95135=CARTESIAN_POINT('Ctrl Pts',(2.74327146193368,-1.75138985455559,43.8414890380477));
#95136=CARTESIAN_POINT('Ctrl Pts',(2.95670975631421,1.36043087050919,44.0005539418939));
#95137=CARTESIAN_POINT('Ctrl Pts',(0.45457729714776,3.22277275298764,44.1596188457401));
#95138=CARTESIAN_POINT('Ctrl Pts',(-2.46505870990123,2.12518006136686,44.3186837495862));
#95139=CARTESIAN_POINT('Ctrl Pts',(-3.12067765406467,-0.924270369548566,
44.4777486534324));
#95140=CARTESIAN_POINT('Ctrl Pts',(-0.910130600485398,-3.12483071963845,
44.6368135572785));
#95141=CARTESIAN_POINT('Ctrl Pts',(2.13631995530277,-2.45541071616408,44.7958784611246));
#95142=CARTESIAN_POINT('Ctrl Pts',(3.22068140919789,0.469165213551552,44.9549433649708));
#95143=CARTESIAN_POINT('Ctrl Pts',(1.34702906969843,2.96283941863608,45.114008268817));
#95144=CARTESIAN_POINT('Ctrl Pts',(-1.76379331539366,2.73531312234951,45.2730731726631));
#95145=CARTESIAN_POINT('Ctrl Pts',(-3.2546712575536,-0.00444363674203639,
45.4321380765093));
#95146=CARTESIAN_POINT('Ctrl Pts',(-1.7563176503055,-2.74011916499234,45.5912029803554));
#95147=CARTESIAN_POINT('Ctrl Pts',(1.3551144210326,-2.95915015614983,45.7502678842016));
#95148=CARTESIAN_POINT('Ctrl Pts',(3.22195051621063,-0.460369018246669,
45.9093327880477));
#95149=CARTESIAN_POINT('Ctrl Pts',(2.1296071997422,2.46123502404409,46.0683976918939));
#95150=CARTESIAN_POINT('Ctrl Pts',(-0.918659902683561,3.12233386541619,
46.22746259574));
#95151=CARTESIAN_POINT('Ctrl Pts',(-3.123189877464,0.915745529291522,46.3865274995862));
#95152=CARTESIAN_POINT('Ctrl Pts',(-2.45924641157584,-2.13190322118698,
46.5455924034324));
#95153=CARTESIAN_POINT('Ctrl Pts',(0.463375644159019,-3.22151954777474,
46.7046573072785));
#95154=CARTESIAN_POINT('Ctrl Pts',(2.96041375996944,-1.352351997789,46.8637222111247));
#95155=CARTESIAN_POINT('Ctrl Pts',(2.7384784559849,1.75887383351055,47.0227871149707));
#95156=CARTESIAN_POINT('Ctrl Pts',(0.00140693752478723,3.25467458050298,
47.1818520188171));
#95157=CARTESIAN_POINT('Ctrl Pts',(-2.7369594963831,1.76123864188931,47.340916922663));
#95158=CARTESIAN_POINT('Ctrl Pts',(-2.9615781729108,-1.34979143756155,47.4999818265093));
#95159=CARTESIAN_POINT('Ctrl Pts',(-0.466164638283834,-3.22112198428059,
47.6590467303553));
#95160=CARTESIAN_POINT('Ctrl Pts',(2.45741366154578,-2.13401961218112,47.8181116342016));
#95161=CARTESIAN_POINT('Ctrl Pts',(3.12396039138569,0.913031500959189,47.9771765380477));
#95162=CARTESIAN_POINT('Ctrl Pts',(0.921394885372682,3.12156749643814,48.1362414418939));
#95163=CARTESIAN_POINT('Ctrl Pts',(-2.12755091531158,2.46301970066826,48.2953063457401));
#95164=CARTESIAN_POINT('Ctrl Pts',(-3.22221123648809,-0.457480686744324,
48.4543712495861));
#95165=CARTESIAN_POINT('Ctrl Pts',(-1.35793011442734,-2.95817673926339,
48.6134361534324));
#95166=CARTESIAN_POINT('Ctrl Pts',(1.75444422073719,-2.74125664937627,48.7725010572784));
#95167=CARTESIAN_POINT('Ctrl Pts',(3.25371829941633,-0.00798100720446507,
48.9315659611247));
#95168=CARTESIAN_POINT('Ctrl Pts',(1.7679977121055,2.73518764693765,49.0906308649707));
#95169=CARTESIAN_POINT('Ctrl Pts',(-1.34827175404425,2.96118711175811,49.249695768817));
#95170=CARTESIAN_POINT('Ctrl Pts',(-2.58989120385452,1.30614186523129,49.3557390380477));
#95171=CARTESIAN_POINT('Ctrl Pts',(-2.72283095673211,0.399045011670457,
49.4087606726631));
#95172=CARTESIAN_POINT('Ctrl Pts',(1.48738611075516,-2.08582659521601,-0.109744663668461));
#95173=CARTESIAN_POINT('Ctrl Pts',(2.18226830199655,-1.59031171289833,-0.0567230290530766));
#95174=CARTESIAN_POINT('Ctrl Pts',(3.02564425429361,0.141323225187899,0.0493202401776927));
#95175=CARTESIAN_POINT('Ctrl Pts',(1.51443447872066,2.6265638058203,0.208385144023846));
#95176=CARTESIAN_POINT('Ctrl Pts',(-1.38901916658974,2.69172145058039,0.367450047870002));
#95177=CARTESIAN_POINT('Ctrl Pts',(-3.01604259595292,0.288558531368754,
0.526514951716154));
#95178=CARTESIAN_POINT('Ctrl Pts',(-1.87336583720858,-2.38163901943715,
0.685579855562309));
#95179=CARTESIAN_POINT('Ctrl Pts',(0.990082607075607,-2.86338445583323,
0.844644759408461));
#95180=CARTESIAN_POINT('Ctrl Pts',(2.94409597960784,-0.715824020681664,
1.00370966325462));
#95181=CARTESIAN_POINT('Ctrl Pts',(2.19417615309141,2.08946906230414,1.16277456710077));
#95182=CARTESIAN_POINT('Ctrl Pts',(-0.570997951771571,2.9755515685831,1.32183947094693));
#95183=CARTESIAN_POINT('Ctrl Pts',(-2.81172828739708,1.12883753547801,1.48090437479308));
#95184=CARTESIAN_POINT('Ctrl Pts',(-2.47005271785342,-1.75469155487355,
1.63996927863923));
#95185=CARTESIAN_POINT('Ctrl Pts',(0.140230594765303,-3.02661384558711,
1.79903418248539));
#95186=CARTESIAN_POINT('Ctrl Pts',(2.62171795481554,-1.51877386128767,1.95809908633154));
#95187=CARTESIAN_POINT('Ctrl Pts',(2.69530668223053,1.38398004400222,2.11716399017769));
#95188=CARTESIAN_POINT('Ctrl Pts',(0.293408029811388,3.01562338031741,2.27622889402385));
#95189=CARTESIAN_POINT('Ctrl Pts',(-2.37796901060781,1.87758877721523,2.43529379787));
#95190=CARTESIAN_POINT('Ctrl Pts',(-2.86531611033693,-0.984905831706037,
2.59435870171616));
#95191=CARTESIAN_POINT('Ctrl Pts',(-0.721032271090857,-2.94281966321798,
2.7534236055623));
#95192=CARTESIAN_POINT('Ctrl Pts',(2.08547890242402,-2.19792024371884,2.91248850940847));
#95193=CARTESIAN_POINT('Ctrl Pts',(2.97659562927056,0.565644784578315,3.07155341325461));
#95194=CARTESIAN_POINT('Ctrl Pts',(1.13387754065414,2.80969699176317,3.23061831710078));
#95195=CARTESIAN_POINT('Ctrl Pts',(-1.75024295905019,2.47320139246638,3.38968322094693));
#95196=CARTESIAN_POINT('Ctrl Pts',(-3.02686425414068,-0.134789881251951,
3.54874812479308));
#95197=CARTESIAN_POINT('Ctrl Pts',(-1.52348185391423,-2.61898425999305,
3.70781302863924));
#95198=CARTESIAN_POINT('Ctrl Pts',(1.37913249816518,-2.69778966517383,3.86687793248538));
#95199=CARTESIAN_POINT('Ctrl Pts',(3.01509162042777,-0.298827779893139,
4.02594283633155));
#95200=CARTESIAN_POINT('Ctrl Pts',(1.88185954733525,2.37459052563238,4.1850077401777));
#95201=CARTESIAN_POINT('Ctrl Pts',(-0.979754128895413,2.86708168158829,
4.34407264402385));
#95202=CARTESIAN_POINT('Ctrl Pts',(-2.94151902821897,0.726320403143036,
4.50313754787));
#95203=CARTESIAN_POINT('Ctrl Pts',(-2.20166499891421,-2.08152510285824,
4.66220245171616));
#95204=CARTESIAN_POINT('Ctrl Pts',(0.560293860707996,-2.97760748104212,
4.82126735556231));
#95205=CARTESIAN_POINT('Ctrl Pts',(2.80765448550222,-1.13892572692277,4.98033225940847));
#95206=CARTESIAN_POINT('Ctrl Pts',(2.47634319614971,1.74579491816248,5.13939716325462));
#95207=CARTESIAN_POINT('Ctrl Pts',(-0.129349318760607,3.02710162947443,
5.29846206710077));
#95208=CARTESIAN_POINT('Ctrl Pts',(-2.61624179715656,1.52818663134642,5.45752697094693));
#95209=CARTESIAN_POINT('Ctrl Pts',(-2.70026409413619,-1.37428139161307,
5.61659187479307));
#95210=CARTESIAN_POINT('Ctrl Pts',(-0.304246480126756,-3.01454965139899,
5.77565677863924));
#95211=CARTESIAN_POINT('Ctrl Pts',(2.37120432529958,-1.88612448398758,5.93472168248538));
#95212=CARTESIAN_POINT('Ctrl Pts',(2.86883801401339,0.974599389887348,6.09378658633155));
#95213=CARTESIAN_POINT('Ctrl Pts',(0.731606176659906,2.94020882314347,6.25285149017769));
#95214=CARTESIAN_POINT('Ctrl Pts',(-2.07756457258859,2.20540267709597,6.41191639402386));
#95215=CARTESIAN_POINT('Ctrl Pts',(-2.97860971706148,-0.554941145387749,
6.57098129787));
#95216=CARTESIAN_POINT('Ctrl Pts',(-1.14397023216239,-2.80560289943957,
6.73004620171617));
#95217=CARTESIAN_POINT('Ctrl Pts',(1.74134123660211,-2.47947700516185,6.88911110556231));
#95218=CARTESIAN_POINT('Ctrl Pts',(3.0273292263028,0.123908341084059,7.04817600940847));
#95219=CARTESIAN_POINT('Ctrl Pts',(1.5328864717516,2.61349088120435,7.20724091325462));
#95220=CARTESIAN_POINT('Ctrl Pts',(-1.36942584534175,2.70272980068808,7.36630581710077));
#95221=CARTESIAN_POINT('Ctrl Pts',(-3.01399794400122,0.309664197113199,
7.52537072094693));
#95222=CARTESIAN_POINT('Ctrl Pts',(-1.89038332751853,-2.36781046463971,
7.68443562479308));
#95223=CARTESIAN_POINT('Ctrl Pts',(0.969441502437645,-2.87058507882431,
7.84350052863925));
#95224=CARTESIAN_POINT('Ctrl Pts',(2.93888911979601,-0.736889586683079,
8.00256543248538));
#95225=CARTESIAN_POINT('Ctrl Pts',(2.2091332307661,2.07359733076176,8.16163033633156));
#95226=CARTESIAN_POINT('Ctrl Pts',(-0.549586637339215,2.97960233076085,
8.32069524017768));
#95227=CARTESIAN_POINT('Ctrl Pts',(-2.80354224993797,1.14901104182252,8.47976014402387));
#95228=CARTESIAN_POINT('Ctrl Pts',(-2.48260280427558,-1.7368819296718,8.63882504787));
#95229=CARTESIAN_POINT('Ctrl Pts',(0.118466963123882,-3.02754704341081,
8.79788995171617));
#95230=CARTESIAN_POINT('Ctrl Pts',(2.61073152242574,-1.53758136019852,8.95695485556231));
#95231=CARTESIAN_POINT('Ctrl Pts',(2.7051867761288,1.36456587516881,9.11601975940847));
#95232=CARTESIAN_POINT('Ctrl Pts',(0.315080913736107,3.01343649994762,9.27508466325462));
#95233=CARTESIAN_POINT('Ctrl Pts',(-2.3644089548186,1.89463606420625,9.43414956710077));
#95234=CARTESIAN_POINT('Ctrl Pts',(-2.87232287027127,-0.964280483227741,
9.59321447094693));
#95235=CARTESIAN_POINT('Ctrl Pts',(-0.742170616200155,-2.93755992242991,
9.75227937479308));
#95236=CARTESIAN_POINT('Ctrl Pts',(2.06962339022292,-2.21285664787839,9.91134427863924));
#95237=CARTESIAN_POINT('Ctrl Pts',(2.98058531891839,0.544230353862732,10.0704091824854));
#95238=CARTESIAN_POINT('Ctrl Pts',(1.15404813962696,2.80147254365288,10.2294740863316));
#95239=CARTESIAN_POINT('Ctrl Pts',(-1.73241701178142,2.48572058339382,10.3885389901777));
#95240=CARTESIAN_POINT('Ctrl Pts',(-3.02775508009259,-0.113025202458703,
10.5476038940239));
#95241=CARTESIAN_POINT('Ctrl Pts',(-1.54227128152162,-2.60796372973456,
10.70666879787));
#95242=CARTESIAN_POINT('Ctrl Pts',(1.3597014967949,-2.70763501252128,10.8657337017162));
#95243=CARTESIAN_POINT('Ctrl Pts',(3.01286532105161,-0.320496612496818,
11.0247986055623));
#95244=CARTESIAN_POINT('Ctrl Pts',(1.89888268031252,2.36099980682474,11.1838635094085));
#95245=CARTESIAN_POINT('Ctrl Pts',(-0.959116348930274,2.8740513827404,11.3429284132546));
#95246=CARTESIAN_POINT('Ctrl Pts',(-2.93622123533907,0.747449248150846,
11.5019933171008));
#95247=CARTESIAN_POINT('Ctrl Pts',(-2.2165729164044,-2.06564276380982,11.6610582209469));
#95248=CARTESIAN_POINT('Ctrl Pts',(0.538872312261706,-2.98155867835853,
11.8201231247931));
#95249=CARTESIAN_POINT('Ctrl Pts',(2.79939378727039,-1.15908150930349,11.9791880286392));
#95250=CARTESIAN_POINT('Ctrl Pts',(2.4888303324447,1.72794649735476,12.1382529324854));
#95251=CARTESIAN_POINT('Ctrl Pts',(-0.107583076667991,3.0279533356761,12.2973178363316));
#95252=CARTESIAN_POINT('Ctrl Pts',(-2.60518751207211,1.54695622057019,12.4563827401777));
#95253=CARTESIAN_POINT('Ctrl Pts',(-2.71007450195653,-1.35483272593425,
12.6154476440239));
#95254=CARTESIAN_POINT('Ctrl Pts',(-0.325911275900068,-3.01228440915837,
12.77451254787));
#95255=CARTESIAN_POINT('Ctrl Pts',(2.3575830316713,-1.90312316211876,12.9335774517162));
#95256=CARTESIAN_POINT('Ctrl Pts',(2.87577061064776,0.953949116227871,13.0926423555623));
#95257=CARTESIAN_POINT('Ctrl Pts',(0.752725465482682,2.93487306284808,13.2517072594085));
#95258=CARTESIAN_POINT('Ctrl Pts',(-2.06165546438178,2.22028202433883,13.4107721632546));
#95259=CARTESIAN_POINT('Ctrl Pts',(-2.98252240593688,-0.533512529845143,
13.5698370671008));
#95260=CARTESIAN_POINT('Ctrl Pts',(-1.16411113459189,-2.79730598750593,
13.728901970947));
#95261=CARTESIAN_POINT('Ctrl Pts',(1.72347040083377,-2.4919320413822,13.8879668747931));
#95262=CARTESIAN_POINT('Ctrl Pts',(3.02814180952086,0.102140603332451,14.0470317786392));
#95263=CARTESIAN_POINT('Ctrl Pts',(1.55163616220966,2.60240287840691,14.2060966824854));
#95264=CARTESIAN_POINT('Ctrl Pts',(-1.34995957831533,2.71250523655384,14.3651615863315));
#95265=CARTESIAN_POINT('Ctrl Pts',(-3.01169376614451,0.331324886453901,
14.5242264901777));
#95266=CARTESIAN_POINT('Ctrl Pts',(-1.90735749592618,-2.3541586403961,14.6832913940239));
#95267=CARTESIAN_POINT('Ctrl Pts',(0.948778801813178,-2.87748054843943,
14.84235629787));
#95268=CARTESIAN_POINT('Ctrl Pts',(2.93351540931218,-0.757999251150931,
15.0014212017162));
#95269=CARTESIAN_POINT('Ctrl Pts',(2.22398395969949,2.05766150481967,15.1604861055623));
#95270=CARTESIAN_POINT('Ctrl Pts',(-0.528151023927718,2.98347649854016,
15.3195510094085));
#95271=CARTESIAN_POINT('Ctrl Pts',(-2.79520915110406,1.16913699924407,15.4786159132546));
#95272=CARTESIAN_POINT('Ctrl Pts',(-2.49502570018633,-1.71898873667837,
15.6376808171008));
#95273=CARTESIAN_POINT('Ctrl Pts',(0.0966978000338692,-3.02832050101801,
15.7967457209469));
#95274=CARTESIAN_POINT('Ctrl Pts',(2.59960983773466,-1.55631109132156,15.9558106247931));
#95275=CARTESIAN_POINT('Ctrl Pts',(2.71492720846078,1.34508206968077,16.1148755286393));
#95276=CARTESIAN_POINT('Ctrl Pts',(0.336737426669731,3.0110933939181,16.2739404324854));
#95277=CARTESIAN_POINT('Ctrl Pts',(-2.35072664406156,1.91158566805583,16.4330053363316));
#95278=CARTESIAN_POINT('Ctrl Pts',(-2.87918119059149,-0.943605422388776,
16.5920702401777));
#95279=CARTESIAN_POINT('Ctrl Pts',(-0.763270588118764,-2.93214827911724,
16.7511351440239));
#95280=CARTESIAN_POINT('Ctrl Pts',(2.0536608980259,-2.22767871052736,16.91020004787));
#95281=CARTESIAN_POINT('Ctrl Pts',(2.98442095308616,0.52278781182965,17.0692649517162));
#95282=CARTESIAN_POINT('Ctrl Pts',(1.17415908702408,2.79310328483859,17.2283298555623));
#95283=CARTESIAN_POINT('Ctrl Pts',(-1.71450151936645,2.49811129886309,17.3873947594085));
#95284=CARTESIAN_POINT('Ctrl Pts',(-3.02848940959031,-0.0912546843550893,
17.5464596632546));
#95285=CARTESIAN_POINT('Ctrl Pts',(-1.56098099280365,-2.5968083990782,17.7055245671008));
#95286=CARTESIAN_POINT('Ctrl Pts',(1.34020021578723,-2.7173404098532,17.864589470947));
#95287=CARTESIAN_POINT('Ctrl Pts',(3.01048329441863,-0.342148879062476,
18.0236543747931));
#95288=CARTESIAN_POINT('Ctrl Pts',(1.9158076648487,2.34728705375469,18.1827192786393));
#95289=CARTESIAN_POINT('Ctrl Pts',(-0.938428994667144,2.88087253161005,
18.3417841824854));
#95290=CARTESIAN_POINT('Ctrl Pts',(-2.93077167667974,0.768539459357237,
18.5008490863316));
#95291=CARTESIAN_POINT('Ctrl Pts',(-2.23136626488662,-2.04965365692435,
18.6599139901777));
#95292=CARTESIAN_POINT('Ctrl Pts',(0.517422910876692,-2.98535576652387,
18.8189788940239));
#95293=CARTESIAN_POINT('Ctrl Pts',(2.79098839551245,-1.17917738170817,18.97804379787));
#95294=CARTESIAN_POINT('Ctrl Pts',(2.50118882744452,1.71000876339393,19.1371087017162));
#95295=CARTESIAN_POINT('Ctrl Pts',(-0.0858112738799978,3.02864853469207,
19.2961736055623));
#95296=CARTESIAN_POINT('Ctrl Pts',(-2.59399857148751,1.56564585156992,19.4552385094085));
#95297=CARTESIAN_POINT('Ctrl Pts',(-2.71974483293534,-1.33531403240542,
19.6143034132547));
#95298=CARTESIAN_POINT('Ctrl Pts',(-0.347559226150612,-3.009863469617,19.7733683171007));
#95299=CARTESIAN_POINT('Ctrl Pts',(2.34383988058696,-1.92002347266577,19.932433220947));
#95300=CARTESIAN_POINT('Ctrl Pts',(2.8825545660313,0.933249535370647,20.0914981247931));
#95301=CARTESIAN_POINT('Ctrl Pts',(0.773805847845303,2.92938560644681,20.2505630286393));
#95302=CARTESIAN_POINT('Ctrl Pts',(-2.04563979446034,2.23504661086466,20.4096279324854));
#95303=CARTESIAN_POINT('Ctrl Pts',(-2.98628093583334,-0.512056338400038,
20.5686928363316));
#95304=CARTESIAN_POINT('Ctrl Pts',(-1.18419186708488,-2.78886448995777,
20.7277577401777));
#95305=CARTESIAN_POINT('Ctrl Pts',(1.70551048327454,-2.50425827598873,20.8868226440239));
#95306=CARTESIAN_POINT('Ctrl Pts',(3.02879787580927,0.0803675861934736,
21.04588754787));
#95307=CARTESIAN_POINT('Ctrl Pts',(1.57030565255054,2.59118036403974,21.2049524517162));
#95308=CARTESIAN_POINT('Ctrl Pts',(-1.33042353532015,2.72214046993971,21.3640173555623));
#95309=CARTESIAN_POINT('Ctrl Pts',(-3.00923392151558,0.352968450455971,
21.5230822594085));
#95310=CARTESIAN_POINT('Ctrl Pts',(-1.92423307788785,-2.34038513569446,
21.6821471632546));
#95311=CARTESIAN_POINT('Ctrl Pts',(0.928067061231389,-2.8842272884214,21.8412120671008));
#95312=CARTESIAN_POINT('Ctrl Pts',(2.92799007289608,-0.779069736570111,
22.0002769709469));
#95313=CARTESIAN_POINT('Ctrl Pts',(2.23871973657225,2.04161932360058,22.1593418747931));
#95314=CARTESIAN_POINT('Ctrl Pts',(-0.506688111736351,2.98719645802588,
22.3184067786392));
#95315=CARTESIAN_POINT('Ctrl Pts',(-2.78673157503577,1.18920252695495,22.4774716824855));
#95316=CARTESIAN_POINT('Ctrl Pts',(-2.50731963457993,-1.70100669353983,
22.6365365863315));
#95317=CARTESIAN_POINT('Ctrl Pts',(0.0749236388810824,-3.02893743245946,
22.7956014901777));
#95318=CARTESIAN_POINT('Ctrl Pts',(2.58835378583897,-1.57496038069229,22.9546663940239));
#95319=CARTESIAN_POINT('Ctrl Pts',(2.72452731312732,1.32552874032994,23.11373129787));
#95320=CARTESIAN_POINT('Ctrl Pts',(0.3583765345043,3.00859465214809,23.2727962017162));
#95321=CARTESIAN_POINT('Ctrl Pts',(-2.33692283023767,1.92843646691595,23.4318611055623));
#95322=CARTESIAN_POINT('Ctrl Pts',(-2.88589069337668,-0.922881588991328,
23.5909260094085));
#95323=CARTESIAN_POINT('Ctrl Pts',(-0.784331108526694,-2.92658508053578,
23.7499909132546));
#95324=CARTESIAN_POINT('Ctrl Pts',(2.03759225733304,-2.24238563014344,23.9090558171008));
#95325=CARTESIAN_POINT('Ctrl Pts',(2.98810233014392,0.501318248227434,24.068120720947));
#95326=CARTESIAN_POINT('Ctrl Pts',(1.19420934513164,2.78458965763675,24.2271856247931));
#95327=CARTESIAN_POINT('Ctrl Pts',(-1.69649740873925,2.51037289332849,24.3862505286392));
#95328=CARTESIAN_POINT('Ctrl Pts',(-3.02906720419183,-0.0694794495295385,
24.5453154324854));
#95329=CARTESIAN_POINT('Ctrl Pts',(-1.57961002095801,-2.58551884601647,
24.7043803363315));
#95330=CARTESIAN_POINT('Ctrl Pts',(1.32062966324739,-2.72690535478744,24.8634452401778));
#95331=CARTESIAN_POINT('Ctrl Pts',(3.00794566357964,-0.363783460824903,
25.0225101440238));
#95332=CARTESIAN_POINT('Ctrl Pts',(1.9326336261712,2.33345297540141,25.1815750478701));
#95333=CARTESIAN_POINT('Ctrl Pts',(-0.91769313540187,2.88754477552359,25.3406399517161));
#95334=CARTESIAN_POINT('Ctrl Pts',(-2.92517063390475,0.78958994671838,25.4997048555623));
#95335=CARTESIAN_POINT('Ctrl Pts',(-2.24604427973561,-2.03355860866717,
25.6587697594085));
#95336=CARTESIAN_POINT('Ctrl Pts',(0.495946765220677,-2.98899854926102,
25.8178346632546));
#95337=CARTESIAN_POINT('Ctrl Pts',(2.78243874468022,-1.19921230544041,25.9768995671008));
#95338=CARTESIAN_POINT('Ctrl Pts',(2.51341804237085,1.69198264343994,26.135964470947));
#95339=CARTESIAN_POINT('Ctrl Pts',(-0.0640350357260733,3.02918719058709,
26.2950293747931));
#95340=CARTESIAN_POINT('Ctrl Pts',(-2.58267555373039,1.58425455832728,26.4540942786393));
#95341=CARTESIAN_POINT('Ctrl Pts',(-2.72927458723795,-1.31572631989881,
26.6131591824854));
#95342=CARTESIAN_POINT('Ctrl Pts',(-0.369189211950789,-3.00728695790684,
26.7722240863316));
#95343=CARTESIAN_POINT('Ctrl Pts',(2.32997558239507,-1.93682454209465,26.9312889901777));
#95344=CARTESIAN_POINT('Ctrl Pts',(2.8891895295186,0.912501717224372,27.0903538940239));
#95345=CARTESIAN_POINT('Ctrl Pts',(0.794846234156523,2.92374673757228,27.24941879787));
#95346=CARTESIAN_POINT('Ctrl Pts',(-2.02951839063349,2.2496956735296,27.4084837017162));
#95347=CARTESIAN_POINT('Ctrl Pts',(-2.989885112482,-0.490573680068375,27.5675486055623));
#95348=CARTESIAN_POINT('Ctrl Pts',(-1.20421139171946,-2.78027884311456,
27.7266135094085));
#95349=CARTESIAN_POINT('Ctrl Pts',(1.68746241222674,-2.51645507186982,27.8856784132547));
#95350=CARTESIAN_POINT('Ctrl Pts',(3.02929739125769,0.0585904150588297,
28.0447433171008));
#95351=CARTESIAN_POINT('Ctrl Pts',(1.58889397779588,2.57982391816599,28.203808220947));
#95352=CARTESIAN_POINT('Ctrl Pts',(-1.31081872612446,2.73163500282501,28.3628731247931));
#95353=CARTESIAN_POINT('Ctrl Pts',(-3.00661853725756,0.374593770418749,
28.5219380286392));
#95354=CARTESIAN_POINT('Ctrl Pts',(-1.9410092011477,-2.3264906624522,28.6810029324854));
#95355=CARTESIAN_POINT('Ctrl Pts',(0.907307351229441,-2.8908249500484,28.8400678363315));
#95356=CARTESIAN_POINT('Ctrl Pts',(2.92231339613825,-0.800099953860905,
28.9991327401777));
#95357=CARTESIAN_POINT('Ctrl Pts',(2.25333979972966,2.02547161628391,29.1581976440239));
#95358=CARTESIAN_POINT('Ctrl Pts',(-0.485199010128317,2.99076201694283,
29.31726254787));
#95359=CARTESIAN_POINT('Ctrl Pts',(-2.77810995991736,1.20920658781917,29.4763274517161));
#95360=CARTESIAN_POINT('Ctrl Pts',(-2.51948397201424,-1.68293672970218,
29.6353923555624));
#95361=CARTESIAN_POINT('Ctrl Pts',(0.0531456051164595,-3.02939780584758,
29.7944572594085));
#95362=CARTESIAN_POINT('Ctrl Pts',(2.57696394853534,-1.5935282643764,29.9535221632547));
#95363=CARTESIAN_POINT('Ctrl Pts',(2.73398659392343,1.30590689777805,30.1125870671008));
#95364=CARTESIAN_POINT('Ctrl Pts',(0.379997118769557,3.00594040379118,30.2716519709469));
#95365=CARTESIAN_POINT('Ctrl Pts',(-2.32299822683086,1.94518758981186,30.4307168747931));
#95366=CARTESIAN_POINT('Ctrl Pts',(-2.89245103182977,-0.902110054197515,
30.5897817786392));
#95367=CARTESIAN_POINT('Ctrl Pts',(-0.805351088859346,-2.92087061423309,
30.7488466824855));
#95368=CARTESIAN_POINT('Ctrl Pts',(2.02141829869142,-2.25697664656345,30.9079115863315));
#95369=CARTESIAN_POINT('Ctrl Pts',(2.99162925981065,0.479822772763149,31.0669764901778));
#95370=CARTESIAN_POINT('Ctrl Pts',(1.21419787760285,2.77593210209509,31.2260413940238));
#95371=CARTESIAN_POINT('Ctrl Pts',(-1.67840561048632,2.52250473301941,31.3851062978701));
#95372=CARTESIAN_POINT('Ctrl Pts',(-3.02948843403243,-0.0477006234883444,
31.5441712017161));
#95373=CARTESIAN_POINT('Ctrl Pts',(-1.59815740309777,-2.5740956540776,31.7032361055624));
#95374=CARTESIAN_POINT('Ctrl Pts',(1.30099085072732,-2.73632935293637,31.8623010094085));
#95375=CARTESIAN_POINT('Ctrl Pts',(3.00525255969833,-0.385399239547727,
32.0213659132547));
#95376=CARTESIAN_POINT('Ctrl Pts',(1.94935969458897,2.31949828681319,32.1804308171008));
#95377=CARTESIAN_POINT('Ctrl Pts',(-0.896909842918197,2.89406776960972,
32.339495720947));
#95378=CARTESIAN_POINT('Ctrl Pts',(-2.91941839651761,0.810599622188333,
32.4985606247931));
#95379=CARTESIAN_POINT('Ctrl Pts',(-2.26060620228232,-2.01735845095016,
32.6576255286393));
#95380=CARTESIAN_POINT('Ctrl Pts',(0.474444985340741,-2.99248683828391,
32.8166904324854));
#95381=CARTESIAN_POINT('Ctrl Pts',(2.77374527668334,-1.2191852449461,32.9757553363316));
#95382=CARTESIAN_POINT('Ctrl Pts',(2.52551734512674,1.67386906921698,33.1348202401777));
#95383=CARTESIAN_POINT('Ctrl Pts',(-0.0422554877644123,3.02956927551939,
33.2938851440239));
#95384=CARTESIAN_POINT('Ctrl Pts',(-2.57121904405865,1.60278137900572,33.45295004787));
#95385=CARTESIAN_POINT('Ctrl Pts',(-2.73866327229565,-1.29607060085328,
33.6120149517162));
#95386=CARTESIAN_POINT('Ctrl Pts',(-0.390800115301929,-3.00455500720112,
33.7710798555623));
#95387=CARTESIAN_POINT('Ctrl Pts',(2.31599085370575,-1.95352550200112,33.9301447594085));
#95388=CARTESIAN_POINT('Ctrl Pts',(2.8956751581654,0.891706734190801,34.0892096632547));
#95389=CARTESIAN_POINT('Ctrl Pts',(0.815845536892429,2.91795674768322,34.2482745671008));
#95390=CARTESIAN_POINT('Ctrl Pts',(-2.01329208617546,2.26422845516096,34.407339470947));
#95391=CARTESIAN_POINT('Ctrl Pts',(-2.99333474959216,-0.469065665233948,
34.5664043747931));
#95392=CARTESIAN_POINT('Ctrl Pts',(-1.22416867373741,-2.77154949074653,
34.7254692786393));
#95393=CARTESIAN_POINT('Ctrl Pts',(1.66932712054919,-2.52852179860413,34.8845341824854));
#95394=CARTESIAN_POINT('Ctrl Pts',(3.02964033004738,0.0368102155349702,
35.0435990863315));
#95395=CARTESIAN_POINT('Ctrl Pts',(1.60740017716258,2.56833412777138,35.2026639901778));
#95396=CARTESIAN_POINT('Ctrl Pts',(-1.29114616405084,2.74098834446158,35.3617288940238));
#95397=CARTESIAN_POINT('Ctrl Pts',(-3.00384774855298,0.396199728584597,
35.5207937978701));
#95398=CARTESIAN_POINT('Ctrl Pts',(-1.95768499859072,-2.31247593883919,
35.6798587017162));
#95399=CARTESIAN_POINT('Ctrl Pts',(0.88650074482376,-2.89727319230415,35.8389236055623));
#95400=CARTESIAN_POINT('Ctrl Pts',(2.91648567245169,-0.821088816024983,
35.9979885094085));
#95401=CARTESIAN_POINT('Ctrl Pts',(2.26784339349788,2.0092192175035,36.1570534132546));
#95402=CARTESIAN_POINT('Ctrl Pts',(-0.463684829820489,2.99417299099631,
36.3161183171008));
#95403=CARTESIAN_POINT('Ctrl Pts',(-2.76934475137816,1.22914814787788,36.4751832209469));
#95404=CARTESIAN_POINT('Ctrl Pts',(-2.53151808374568,-1.66477977915577,
36.6342481247931));
#95405=CARTESIAN_POINT('Ctrl Pts',(0.0313648243910064,-3.02970159738682,
36.7933130286392));
#95406=CARTESIAN_POINT('Ctrl Pts',(2.5654409145354,-1.61201378264736,36.9523779324855));
#95407=CARTESIAN_POINT('Ctrl Pts',(2.74330456192304,1.28621755622817,37.1114428363315));
#95408=CARTESIAN_POINT('Ctrl Pts',(0.401598061952563,3.00313078603868,37.2705077401778));
#95409=CARTESIAN_POINT('Ctrl Pts',(-2.30895355356834,1.96183817092069,37.4295726440238));
#95410=CARTESIAN_POINT('Ctrl Pts',(-2.8988618668636,-0.881291891634948,
37.5886375478701));
#95411=CARTESIAN_POINT('Ctrl Pts',(-0.826329442647554,-2.91500517557537,
37.7477024517162));
#95412=CARTESIAN_POINT('Ctrl Pts',(2.00513985809173,-2.27145100561495,37.9067673555623));
#95413=CARTESIAN_POINT('Ctrl Pts',(2.99500155978836,0.458302496483089,38.0658322594085));
#95414=CARTESIAN_POINT('Ctrl Pts',(1.23412365128147,2.76713106570055,38.2248971632546));
#95415=CARTESIAN_POINT('Ctrl Pts',(-1.66022705972667,2.53450619087203,38.3839620671008));
#95416=CARTESIAN_POINT('Ctrl Pts',(-3.0297530773398,-0.0259193319235489,
38.5430269709469));
#95417=CARTESIAN_POINT('Ctrl Pts',(-1.61662218055602,-2.5625394136972,38.7020918747932));
#95418=CARTESIAN_POINT('Ctrl Pts',(1.2812847933071,-2.74561191719758,38.8611567786392));
#95419=CARTESIAN_POINT('Ctrl Pts',(3.00240412197435,-0.406995097966519,
39.0202216824854));
#95420=CARTESIAN_POINT('Ctrl Pts',(1.9659850055742,2.30542370927227,39.1792865863316));
#95421=CARTESIAN_POINT('Ctrl Pts',(-0.876080191451438,2.90044117671153,
39.3383514901777));
#95422=CARTESIAN_POINT('Ctrl Pts',(-2.91351526183688,0.831567399830523,
39.4974163940239));
#95423=CARTESIAN_POINT('Ctrl Pts',(-2.27505127985805,-2.00105402111826,
39.6564812978701));
#95424=CARTESIAN_POINT('Ctrl Pts',(0.452918682609153,-2.99582045329171,
39.8155462017162));
#95425=CARTESIAN_POINT('Ctrl Pts',(2.764908440865,-1.23909516787493,39.9746111055624));
#95426=CARTESIAN_POINT('Ctrl Pts',(2.53748611033011,1.65566897696946,40.1336760094085));
#95427=CARTESIAN_POINT('Ctrl Pts',(-0.0204737557242954,3.02979476974,40.2927409132547));
#95428=CARTESIAN_POINT('Ctrl Pts',(-2.55962963463003,1.62122535600115,40.4518058171008));
#95429=CARTESIAN_POINT('Ctrl Pts',(-2.74791040283129,-1.2763478912228,40.6108707209469));
#95430=CARTESIAN_POINT('Ctrl Pts',(-0.412390819191514,-3.00166775870746,
40.7699356247932));
#95431=CARTESIAN_POINT('Ctrl Pts',(2.30188641735399,-1.97012548915508,40.9290005286392));
#95432=CARTESIAN_POINT('Ctrl Pts',(2.90201111674604,0.870865661109529,41.0880654324855));
#95433=CARTESIAN_POINT('Ctrl Pts',(0.836802670652721,2.91201593604942,41.2471303363315));
#95434=CARTESIAN_POINT('Ctrl Pts',(-1.99696171978245,2.27864420459642,41.4061952401778));
#95435=CARTESIAN_POINT('Ctrl Pts',(-2.9966296688609,-0.447533405591092,
41.5652601440238));
#95436=CARTESIAN_POINT('Ctrl Pts',(-1.24406268159784,-2.76267688405161,
41.7243250478701));
#95437=CARTESIAN_POINT('Ctrl Pts',(1.65110554560885,-2.54045783249339,41.8833899517162));
#95438=CARTESIAN_POINT('Ctrl Pts',(3.02982667445275,0.0150281133849578,
42.0424548555624));
#95439=CARTESIAN_POINT('Ctrl Pts',(1.62582329411232,2.55671158673385,42.2015197594085));
#95440=CARTESIAN_POINT('Ctrl Pts',(-1.27140686592381,2.75020001139901,42.3605846632546));
#95441=CARTESIAN_POINT('Ctrl Pts',(-3.00092169861683,0.417785208196757,
42.5196495671008));
#95442=CARTESIAN_POINT('Ctrl Pts',(-1.97425960828754,-2.29834168924068,
42.678714470947));
#95443=CARTESIAN_POINT('Ctrl Pts',(0.865648317454662,-2.90357168189545,
42.837779374793));
#95444=CARTESIAN_POINT('Ctrl Pts',(2.91050720305651,-0.842035238201733,
42.9968442786393));
#95445=CARTESIAN_POINT('Ctrl Pts',(2.28222976822325,1.99286296730443,43.1559091824854));
#95446=CARTESIAN_POINT('Ctrl Pts',(-0.442146682826039,2.99742920388172,
43.3149740863316));
#95447=CARTESIAN_POINT('Ctrl Pts',(-2.76043640246926,1.2490261764028,43.4740389901777));
#95448=CARTESIAN_POINT('Ctrl Pts',(-2.54342134776202,-1.64653678038715,
43.6331038940239));
#95449=CARTESIAN_POINT('Ctrl Pts',(0.00958242249811193,-3.0298487913746,
43.79216879787));
#95450=CARTESIAN_POINT('Ctrl Pts',(2.55378527943441,-1.63041598003669,43.9512337017162));
#95451=CARTESIAN_POINT('Ctrl Pts',(2.75248073550596,1.26646173337338,44.1102986055624));
#95452=CARTESIAN_POINT('Ctrl Pts',(0.423178247552346,3.00016594411002,44.2693635094084));
#95453=CARTESIAN_POINT('Ctrl Pts',(-2.29478953637709,1.97838734962128,44.4284284132547));
#95454=CARTESIAN_POINT('Ctrl Pts',(-2.9051228671307,-0.860428177350863,
44.5874933171007));
#95455=CARTESIAN_POINT('Ctrl Pts',(-0.847265085550273,-2.90898906771414,
44.746558220947));
#95456=CARTESIAN_POINT('Ctrl Pts',(1.98875777688018,-2.28580795918964,44.9056231247931));
#95457=CARTESIAN_POINT('Ctrl Pts',(2.9982190558569,0.436758531780793,45.0646880286392));
#95458=CARTESIAN_POINT('Ctrl Pts',(1.25398563609222,2.75818700323134,45.2237529324854));
#95459=CARTESIAN_POINT('Ctrl Pts',(-1.6419626957523,2.54637664679984,45.3828178363316));
#95460=CARTESIAN_POINT('Ctrl Pts',(-3.02986112102816,-0.00413670110889247,
45.5418827401778));
#95461=CARTESIAN_POINT('Ctrl Pts',(-1.63500339780443,-2.55085072132126,
45.7009476440238));
#95462=CARTESIAN_POINT('Ctrl Pts',(1.26151250738515,-2.75475256943221,45.8600125478701));
#95463=CARTESIAN_POINT('Ctrl Pts',(2.99940050175171,-0.428569916692723,
46.0190774517161));
#95464=CARTESIAN_POINT('Ctrl Pts',(1.98250869195646,2.29122996424191,46.1781423555624));
#95465=CARTESIAN_POINT('Ctrl Pts',(-0.855205242657951,2.90666467887914,
46.3372072594085));
#95466=CARTESIAN_POINT('Ctrl Pts',(-2.90746156354653,0.85249217398433,46.4962721632546));
#95467=CARTESIAN_POINT('Ctrl Pts',(-2.28937871134263,-1.98464612015039,
46.6553370671008));
#95468=CARTESIAN_POINT('Ctrl Pts',(0.431368865721828,-2.99899930162892,
46.8144019709469));
#95469=CARTESIAN_POINT('Ctrl Pts',(2.75592889225626,-1.25894089319667,46.9734668747932));
#95470=CARTESIAN_POINT('Ctrl Pts',(2.54932334112256,1.63738301758705,47.1325317786392));
#95471=CARTESIAN_POINT('Ctrl Pts',(0.00130975603039247,3.02986421445121,
47.2915966824855));
#95472=CARTESIAN_POINT('Ctrl Pts',(-2.54790930072394,1.6395844813907,47.4506615863315));
#95473=CARTESIAN_POINT('Ctrl Pts',(-2.75701287562081,-1.25655719872552,
47.6097264901778));
#95474=CARTESIAN_POINT('Ctrl Pts',(-0.433965215459717,-2.9986291990659,
47.7687913940238));
#95475=CARTESIAN_POINT('Ctrl Pts',(2.28767255498402,-1.98661632552086,47.9278562978701));
#95476=CARTESIAN_POINT('Ctrl Pts',(2.90817885570603,0.849965611921472,48.0869212017162));
#95477=CARTESIAN_POINT('Ctrl Pts',(0.857751311695834,2.90595124535929,48.2459861055623));
#95478=CARTESIAN_POINT('Ctrl Pts',(-1.98059444140463,2.29289136777236,48.4050510094085));
#95479=CARTESIAN_POINT('Ctrl Pts',(-2.99964321327916,-0.42588109111496,
48.5641159132546));
#95480=CARTESIAN_POINT('Ctrl Pts',(-1.2641337121924,-2.75384638943867,48.7231808171008));
#95481=CARTESIAN_POINT('Ctrl Pts',(1.63325937176812,-2.55190963616655,48.8822457209469));
#95482=CARTESIAN_POINT('Ctrl Pts',(3.02897398663527,-0.00742973453303311,
49.0413106247932));
#95483=CARTESIAN_POINT('Ctrl Pts',(1.6458766818748,2.54625983835977,49.2003755286392));
#95484=CARTESIAN_POINT('Ctrl Pts',(-1.25514248441462,2.75664882626259,49.3594404324855));
#95485=CARTESIAN_POINT('Ctrl Pts',(-2.41099946670181,1.21592263637295,49.4654837017162));
#95486=CARTESIAN_POINT('Ctrl Pts',(-2.53475666268534,0.371481747532844,
49.5185053363316));
#95487=CARTESIAN_POINT('Ctrl Pts',(1.37702479013074,-1.93106208855785,0.));
#95488=CARTESIAN_POINT('Ctrl Pts',(2.02034799762934,-1.47231350142485,0.0530216346153847));
#95489=CARTESIAN_POINT('Ctrl Pts',(2.80114700154351,0.130837301153735,0.159064903846153));
#95490=CARTESIAN_POINT('Ctrl Pts',(1.40206621881702,2.43167759018441,0.318129807692308));
#95491=CARTESIAN_POINT('Ctrl Pts',(-1.28595649275605,2.49200065724321,0.477194711538461));
#95492=CARTESIAN_POINT('Ctrl Pts',(-2.79225776863625,0.267148017737648,
0.636259615384617));
#95493=CARTESIAN_POINT('Ctrl Pts',(-1.73436552900908,-2.20492577360607,
0.795324519230768));
#95494=CARTESIAN_POINT('Ctrl Pts',(0.916620294059412,-2.65092658244327,
0.954389423076924));
#95495=CARTESIAN_POINT('Ctrl Pts',(2.72564945922899,-0.662711191614906,
1.11345432692308));
#95496=CARTESIAN_POINT('Ctrl Pts',(2.03137230801958,1.93443429127041,1.27251923076923));
#95497=CARTESIAN_POINT('Ctrl Pts',(-0.528630951316314,2.75477110121152,
1.43158413461539));
#95498=CARTESIAN_POINT('Ctrl Pts',(-2.60310320693535,1.04507986133772,1.59064903846154));
#95499=CARTESIAN_POINT('Ctrl Pts',(-2.2867793378059,-1.62449666070042,1.7497139423077));
#95500=CARTESIAN_POINT('Ctrl Pts',(0.12982574190393,-2.80204465094187,1.90877884615384));
#95501=CARTESIAN_POINT('Ctrl Pts',(2.42719129243389,-1.40608362715869,2.06784375));
#95502=CARTESIAN_POINT('Ctrl Pts',(2.49531987128246,1.28129126381962,2.22690865384615));
#95503=CARTESIAN_POINT('Ctrl Pts',(0.271637692292844,2.79186965803179,2.38597355769231));
#95504=CARTESIAN_POINT('Ctrl Pts',(-2.20152807269878,1.73827513461474,2.54503846153846));
#95505=CARTESIAN_POINT('Ctrl Pts',(-2.65271491172666,-0.911827625924829,
2.70410336538462));
#95506=CARTESIAN_POINT('Ctrl Pts',(-0.667532999398916,-2.7244678431737,
2.86316826923077));
#95507=CARTESIAN_POINT('Ctrl Pts',(1.93074019393295,-2.03483859399145,3.02223317307692));
#95508=CARTESIAN_POINT('Ctrl Pts',(2.75573769451142,0.523674979307748,3.18129807692308));
#95509=CARTESIAN_POINT('Ctrl Pts',(1.04974590737629,2.60122262971082,3.34036298076923));
#95510=CARTESIAN_POINT('Ctrl Pts',(-1.62037814252565,2.28969438653921,3.49942788461539));
#95511=CARTESIAN_POINT('Ctrl Pts',(-2.80227647964017,-0.124788719351607,
3.65849278846154));
#95512=CARTESIAN_POINT('Ctrl Pts',(-1.41044229536976,-2.42466043275193,
3.8175576923077));
#95513=CARTESIAN_POINT('Ctrl Pts',(1.27680339699028,-2.49761862144671,3.97662259615385));
#95514=CARTESIAN_POINT('Ctrl Pts',(2.79137735375039,-0.276655306861728,
4.1356875));
#95515=CARTESIAN_POINT('Ctrl Pts',(1.74222902142711,2.19840026511027,4.29475240384616));
#95516=CARTESIAN_POINT('Ctrl Pts',(-0.907058170011317,2.65434948083033,
4.45381730769232));
#95517=CARTESIAN_POINT('Ctrl Pts',(-2.72326371290543,0.672428761754554,
4.61288221153846));
#95518=CARTESIAN_POINT('Ctrl Pts',(-2.03830549522154,-1.92707975904121,
4.77194711538462));
#95519=CARTESIAN_POINT('Ctrl Pts',(0.518721084171678,-2.75667446873791,
4.93101201923077));
#95520=CARTESIAN_POINT('Ctrl Pts',(2.59933167366719,-1.05441952748531,5.09007692307692));
#95521=CARTESIAN_POINT('Ctrl Pts',(2.29260307415327,1.61626013811133,5.24914182692309));
#95522=CARTESIAN_POINT('Ctrl Pts',(-0.119751836615735,2.80249624215965,
5.40820673076923));
#95523=CARTESIAN_POINT('Ctrl Pts',(-2.42212145562652,1.41479798694797,5.5672716346154));
#95524=CARTESIAN_POINT('Ctrl Pts',(-2.4999094523197,-1.27231223364438,5.72633653846154));
#95525=CARTESIAN_POINT('Ctrl Pts',(-0.281671949479292,-2.79087559782923,
5.8854014423077));
#95526=CARTESIAN_POINT('Ctrl Pts',(2.19526531462978,-1.74617750760439,6.04446634615385));
#95527=CARTESIAN_POINT('Ctrl Pts',(2.65597549661169,0.902285903180645,6.20353125));
#95528=CARTESIAN_POINT('Ctrl Pts',(0.677322340573879,2.7220507226428,6.36259615384616));
#95529=CARTESIAN_POINT('Ctrl Pts',(-1.92341309285148,2.04176584453944,6.52166105769231));
#95530=CARTESIAN_POINT('Ctrl Pts',(-2.75760234068335,-0.513765530507972,
6.68072596153848));
#95531=CARTESIAN_POINT('Ctrl Pts',(-1.05908973969091,-2.5974323115265,6.83979086538461));
#95532=CARTESIAN_POINT('Ctrl Pts',(1.61213691155191,-2.29550436028606,6.99885576923078));
#95533=CARTESIAN_POINT('Ctrl Pts',(2.80270695172092,0.114714569500639,7.15792067307693));
#95534=CARTESIAN_POINT('Ctrl Pts',(1.41914910781753,2.41957465259107,7.31698557692308));
#95535=CARTESIAN_POINT('Ctrl Pts',(-1.26781695999829,2.50219220796908,7.47605048076923));
#95536=CARTESIAN_POINT('Ctrl Pts',(-2.7903648261082,0.286687681804811,7.6351153846154));
#95537=CARTESIAN_POINT('Ctrl Pts',(-1.75012035275872,-2.19212327220441,
7.79418028846153));
#95538=CARTESIAN_POINT('Ctrl Pts',(0.897510721516925,-2.65759293241885,
7.9532451923077));
#95539=CARTESIAN_POINT('Ctrl Pts',(2.72082893886257,-0.682213731266401,
8.11231009615385));
#95540=CARTESIAN_POINT('Ctrl Pts',(2.04521959797142,1.91974021308981,8.27137500000001));
#95541=CARTESIAN_POINT('Ctrl Pts',(-0.508808317133133,2.75852130426731,
8.43043990384615));
#95542=CARTESIAN_POINT('Ctrl Pts',(-2.59552455843741,1.06375653052225,8.58950480769233));
#95543=CARTESIAN_POINT('Ctrl Pts',(-2.29839823084021,-1.60800847701467,
8.74856971153845));
#95544=CARTESIAN_POINT('Ctrl Pts',(0.109676931802227,-2.80290860719912,
8.90763461538463));
#95545=CARTESIAN_POINT('Ctrl Pts',(2.41702003317145,-1.42349564415503,9.06669951923077));
#95546=CARTESIAN_POINT('Ctrl Pts',(2.50446688033972,1.26331759069596,9.22576442307694));
#95547=CARTESIAN_POINT('Ctrl Pts',(0.291702487991934,2.78984504017334,9.38482932692308));
#95548=CARTESIAN_POINT('Ctrl Pts',(-2.18897414817153,1.75405754418639,9.54389423076923));
#95549=CARTESIAN_POINT('Ctrl Pts',(-2.65920178292864,-0.892732640463869,
9.7029591346154));
#95550=CARTESIAN_POINT('Ctrl Pts',(-0.687102918082009,-2.71959836550246,
9.86202403846154));
#95551=CARTESIAN_POINT('Ctrl Pts',(1.91606113164826,-2.04866674436504,10.0210889423077));
#95552=CARTESIAN_POINT('Ctrl Pts',(2.75943135650696,0.503849460063841,10.1801538461539));
#95553=CARTESIAN_POINT('Ctrl Pts',(1.06841988491078,2.59360842056154,10.33921875));
#95554=CARTESIAN_POINT('Ctrl Pts',(-1.60387484784032,2.30128467646784,10.4982836538462));
#95555=CARTESIAN_POINT('Ctrl Pts',(-2.80310120794078,-0.104638939794822,
10.6573485576923));
#95556=CARTESIAN_POINT('Ctrl Pts',(-1.4278375819202,-2.4144576056201,10.8164134615385));
#95557=CARTESIAN_POINT('Ctrl Pts',(1.25881414027309,-2.50673346208347,10.9754783653846));
#95558=CARTESIAN_POINT('Ctrl Pts',(2.78931624170351,-0.296716351840369,
11.1345432692308));
#95559=CARTESIAN_POINT('Ctrl Pts',(1.75798906916851,2.18581795270431,11.2936081730769));
#95560=CARTESIAN_POINT('Ctrl Pts',(-0.887951675457031,2.66080204294372,
11.4526730769231));
#95561=CARTESIAN_POINT('Ctrl Pts',(-2.71835900653777,0.691989885226263,
11.6117379807692));
#95562=CARTESIAN_POINT('Ctrl Pts',(-2.05210727258437,-1.91237586041207,
11.7708028846154));
#95563=CARTESIAN_POINT('Ctrl Pts',(0.498888975319622,-2.76033249446239,
11.9298677884616));
#95564=CARTESIAN_POINT('Ctrl Pts',(2.59168390408889,-1.07307978779166,12.0889326923077));
#95565=CARTESIAN_POINT('Ctrl Pts',(2.30416368784436,1.59973603738241,12.2479975961539));
#95566=CARTESIAN_POINT('Ctrl Pts',(-0.0996006097535288,2.80328475332372,
12.4070625));
#95567=CARTESIAN_POINT('Ctrl Pts',(-2.41188737821489,1.43217490708647,12.5661274038462));
#95568=CARTESIAN_POINT('Ctrl Pts',(-2.50899194587818,-1.25430662327794,
12.7251923076923));
#95569=CARTESIAN_POINT('Ctrl Pts',(-0.301729257152967,-2.78877843240699,
12.8842572115385));
#95570=CARTESIAN_POINT('Ctrl Pts',(2.18265469599876,-1.76191491500441,13.0433221153847));
#95571=CARTESIAN_POINT('Ctrl Pts',(2.66239370729449,0.88316784194122,13.2023870192308));
#95572=CARTESIAN_POINT('Ctrl Pts',(0.696874616911946,2.71711086597222,13.361451923077));
#95573=CARTESIAN_POINT('Ctrl Pts',(-1.90868441128639,2.05554117151489,13.5205168269231));
#95574=CARTESIAN_POINT('Ctrl Pts',(-2.76122471522252,-0.493926878925183,
13.6795817307693));
#95575=CARTESIAN_POINT('Ctrl Pts',(-1.07773622411112,-2.58975101523663,
13.8386466346154));
#95576=CARTESIAN_POINT('Ctrl Pts',(1.59559205901132,-2.30703525566917,13.9977115384616));
#95577=CARTESIAN_POINT('Ctrl Pts',(2.80345924275497,0.094561957954597,14.1567764423077));
#95578=CARTESIAN_POINT('Ctrl Pts',(1.43650760564222,2.40930935925889,14.3158413461539));
#95579=CARTESIAN_POINT('Ctrl Pts',(-1.24979505427195,2.51124232442785,14.47490625));
#95580=CARTESIAN_POINT('Ctrl Pts',(-2.78823161402115,0.306741187735644,
14.6339711538462));
#95581=CARTESIAN_POINT('Ctrl Pts',(-1.76583506901173,-2.17948438827371,
14.7930360576923));
#95582=CARTESIAN_POINT('Ctrl Pts',(0.878381155370515,-2.66397677083911,
14.9521009615385));
#95583=CARTESIAN_POINT('Ctrl Pts',(2.7158539478379,-0.701757097359029,15.1111658653846));
#95584=CARTESIAN_POINT('Ctrl Pts',(2.05896843006344,1.90498679619639,15.2702307692308));
#95585=CARTESIAN_POINT('Ctrl Pts',(-0.488963186910485,2.76210801590502,
15.429295673077));
#95586=CARTESIAN_POINT('Ctrl Pts',(-2.58780976024888,1.08238917882668,15.5883605769231));
#95587=CARTESIAN_POINT('Ctrl Pts',(-2.30989937066573,-1.59144292611408,
15.7474254807692));
#95588=CARTESIAN_POINT('Ctrl Pts',(0.0895230006752742,-2.80362467567087,
15.9064903846154));
#95589=CARTESIAN_POINT('Ctrl Pts',(2.40672355708034,-1.44083566359076,16.0655552884616));
#95590=CARTESIAN_POINT('Ctrl Pts',(2.5134845904627,1.24527944782968,16.2246201923077));
#95591=CARTESIAN_POINT('Ctrl Pts',(0.311752127397432,2.78767578831249,16.3836850961539));
#95592=CARTESIAN_POINT('Ctrl Pts',(-2.17630703977077,1.76974951852646,16.54275));
#95593=CARTESIAN_POINT('Ctrl Pts',(-2.66555122846353,-0.873591631208197,
16.7018149038462));
#95594=CARTESIAN_POINT('Ctrl Pts',(-0.706637310794764,-2.71458825619525,
16.8608798076923));
#95595=CARTESIAN_POINT('Ctrl Pts',(1.9012830270871,-2.06238903715836,17.0199447115385));
#95596=CARTESIAN_POINT('Ctrl Pts',(2.76298239365644,0.483997915310618,17.1790096153846));
#95597=CARTESIAN_POINT('Ctrl Pts',(1.08703863690706,2.58586014539682,17.3380745192308));
#95598=CARTESIAN_POINT('Ctrl Pts',(-1.58728865209436,2.31275602358159,17.4971394230769));
#95599=CARTESIAN_POINT('Ctrl Pts',(-2.80378105153698,-0.0844837541937897,
17.6562043269231));
#95600=CARTESIAN_POINT('Ctrl Pts',(-1.44515906695039,-2.4041299800326,17.8152692307692));
#95601=CARTESIAN_POINT('Ctrl Pts',(1.24075981853869,-2.51571873673912,17.9743341346154));
#95602=CARTESIAN_POINT('Ctrl Pts',(2.78711095707658,-0.316762059950613,
18.1333990384615));
#95603=CARTESIAN_POINT('Ctrl Pts',(1.77365825090308,2.17312266075431,18.2924639423077));
#95604=CARTESIAN_POINT('Ctrl Pts',(-0.868799284926716,2.66711707508149,
18.4515288461538));
#95605=CARTESIAN_POINT('Ctrl Pts',(-2.71331379513307,0.711515241453737,
18.61059375));
#95606=CARTESIAN_POINT('Ctrl Pts',(-2.06580298174944,-1.8975731159235,18.7696586538462));
#95607=CARTESIAN_POINT('Ctrl Pts',(0.479031080165797,-2.76384784565209,
18.9287235576923));
#95608=CARTESIAN_POINT('Ctrl Pts',(2.58390217697866,-1.09168458333227,19.0877884615385));
#95609=CARTESIAN_POINT('Ctrl Pts',(2.31560520518838,1.58312925037248,19.2468533653847));
#95610=CARTESIAN_POINT('Ctrl Pts',(-0.0794442347893398,2.80392836984813,
19.4059182692308));
#95611=CARTESIAN_POINT('Ctrl Pts',(-2.40152863649417,1.44947780175445,19.5649831730769));
#95612=CARTESIAN_POINT('Ctrl Pts',(-2.51794475603978,-1.2362361809995,19.7240480769231));
#95613=CARTESIAN_POINT('Ctrl Pts',(-0.321770969210761,-2.78653712213808,
19.8831129807692));
#95614=CARTESIAN_POINT('Ctrl Pts',(2.16993126151137,-1.77756125351454,20.0421778846154));
#95615=CARTESIAN_POINT('Ctrl Pts',(2.66867430563458,0.864004132007661,20.2012427884615));
#95616=CARTESIAN_POINT('Ctrl Pts',(0.716390873577828,2.7120305687685,20.3603076923077));
#95617=CARTESIAN_POINT('Ctrl Pts',(-1.8938570746904,2.06921025280796,20.5193725961538));
#95618=CARTESIAN_POINT('Ctrl Pts',(-2.76470436909614,-0.474062697521268,
20.6784375));
#95619=CARTESIAN_POINT('Ctrl Pts',(-1.09632700309372,-2.58193586131958,
20.8375024038462));
#95620=CARTESIAN_POINT('Ctrl Pts',(1.5789647343853,-2.31844690628189,20.9965673076923));
#95621=CARTESIAN_POINT('Ctrl Pts',(2.80406663012842,0.0744044587420362,
21.1556322115385));
#95622=CARTESIAN_POINT('Ctrl Pts',(1.4537918540513,2.39891953486867,21.3146971153846));
#95623=CARTESIAN_POINT('Ctrl Pts',(-1.23170854982573,2.52016264117351,21.4737620192308));
#95624=CARTESIAN_POINT('Ctrl Pts',(-2.7859542853508,0.326778838996557,21.6328269230769));
#95625=CARTESIAN_POINT('Ctrl Pts',(-1.78145851375219,-2.16673285235174,
21.7918918269231));
#95626=CARTESIAN_POINT('Ctrl Pts',(0.859206187941647,-2.67022291509215,
21.9509567307692));
#95627=CARTESIAN_POINT('Ctrl Pts',(2.71073858124696,-0.721264191416516,
22.1100216346154));
#95628=CARTESIAN_POINT('Ctrl Pts',(2.07261083932685,1.89013491539238,22.2690865384616));
#95629=CARTESIAN_POINT('Ctrl Pts',(-0.469092783427355,2.76555196122163,
22.4281514423077));
#95630=CARTESIAN_POINT('Ctrl Pts',(-2.57996120477168,1.1009658811941,22.5872163461539));
#95631=CARTESIAN_POINT('Ctrl Pts',(-2.32128111768206,-1.57479511758614,
22.74628125));
#95632=CARTESIAN_POINT('Ctrl Pts',(0.0693644423326341,-2.8041958319312,
22.9053461538462));
#95633=CARTESIAN_POINT('Ctrl Pts',(2.39630268358469,-1.45810120990461,23.0644110576923));
#95634=CARTESIAN_POINT('Ctrl Pts',(2.52237238497556,1.22717693964369,23.2234759615385));
#95635=CARTESIAN_POINT('Ctrl Pts',(0.331785653130296,2.78536244859756,23.3825408653846));
#95636=CARTESIAN_POINT('Ctrl Pts',(-2.16352744360781,1.78535001902604,23.5416057692308));
#95637=CARTESIAN_POINT('Ctrl Pts',(-2.67176289845148,-0.854405468228408,
23.7006706730769));
#95638=CARTESIAN_POINT('Ctrl Pts',(-0.726135179226555,-2.70943783674216,
23.8597355769231));
#95639=CARTESIAN_POINT('Ctrl Pts',(1.88640665005374,-2.07600473032059,24.0188004807692));
#95640=CARTESIAN_POINT('Ctrl Pts',(2.76639061929044,0.464121353939118,24.1778653846154));
#95641=CARTESIAN_POINT('Ctrl Pts',(1.10560120264771,2.57797821371406,24.3369302884615));
#95642=CARTESIAN_POINT('Ctrl Pts',(-1.57062041344493,2.32410783023306,24.4959951923077));
#95643=CARTESIAN_POINT('Ctrl Pts',(-2.8043159748391,-0.0643242018429354,
24.6550600961538));
#95644=CARTESIAN_POINT('Ctrl Pts',(-1.46240585539294,-2.39367809109597,
24.8141250000001));
#95645=CARTESIAN_POINT('Ctrl Pts',(1.2226413650927,-2.52457398030731,24.9731899038461));
#95646=CARTESIAN_POINT('Ctrl Pts',(2.78476161379025,-0.336791395437584,
25.1322548076924));
#95647=CARTESIAN_POINT('Ctrl Pts',(1.78923575676476,2.16031504563452,25.2913197115385));
#95648=CARTESIAN_POINT('Ctrl Pts',(-0.849601988376427,2.6732942507377,25.4503846153846));
#95649=CARTESIAN_POINT('Ctrl Pts',(-2.70812833945618,0.731003821272407,
25.6094495192308));
#95650=CARTESIAN_POINT('Ctrl Pts',(-2.07939191482527,-1.88267229071865,
25.7685144230769));
#95651=CARTESIAN_POINT('Ctrl Pts',(0.459148425116812,-2.76722034059328,
25.9275793269231));
#95652=CARTESIAN_POINT('Ctrl Pts',(2.57598689455279,-1.11023295248012,26.0866442307693));
#95653=CARTESIAN_POINT('Ctrl Pts',(2.32692703480318,1.56644063544793,26.2457091346154));
#95654=CARTESIAN_POINT('Ctrl Pts',(-0.0592837535552358,2.80442705846396,
26.4047740384616));
#95655=CARTESIAN_POINT('Ctrl Pts',(-2.39104576588115,1.46670577661039,26.5638389423077));
#95656=CARTESIAN_POINT('Ctrl Pts',(-2.52676742005664,-1.21810184082479,
26.7229038461538));
#95657=CARTESIAN_POINT('Ctrl Pts',(-0.34179604974745,-2.78415178286989,
26.8819687500001));
#95658=CARTESIAN_POINT('Ctrl Pts',(2.15709566880955,-1.79311571441545,27.0410336538462));
#95659=CARTESIAN_POINT('Ctrl Pts',(2.67481696700378,0.844795763903405,27.2000985576923));
#95660=CARTESIAN_POINT('Ctrl Pts',(0.73587010182595,2.70681009361926,27.3591634615385));
#95661=CARTESIAN_POINT('Ctrl Pts',(-1.87893184945079,2.08277238189867,27.5182283653846));
#95662=CARTESIAN_POINT('Ctrl Pts',(-2.76804112244977,-0.454174013025224,
27.6772932692308));
#95663=CARTESIAN_POINT('Ctrl Pts',(-1.1148611157287,-2.57398725372069,27.8363581730769));
#95664=CARTESIAN_POINT('Ctrl Pts',(1.56225579709783,-2.32973872228513,27.9954230769231));
#95665=CARTESIAN_POINT('Ctrl Pts',(2.80452908244698,0.0542431137526706,
28.1544879807693));
#95666=CARTESIAN_POINT('Ctrl Pts',(1.47100095966601,2.38840571644395,28.3135528846154));
#95667=CARTESIAN_POINT('Ctrl Pts',(-1.21355838150491,2.52895269713762,28.4726177884615));
#95668=CARTESIAN_POINT('Ctrl Pts',(-2.78353295780648,0.34679959989242,28.6316826923077));
#95669=CARTESIAN_POINT('Ctrl Pts',(-1.79698987944403,-2.15386932353293,
28.7907475961538));
#95670=CARTESIAN_POINT('Ctrl Pts',(0.839986810335585,-2.67633104233065,
28.9498125000001));
#95671=CARTESIAN_POINT('Ctrl Pts',(2.70548310349,-0.740734005166865,29.1088774038461));
#95672=CARTESIAN_POINT('Ctrl Pts',(2.08614612062029,1.87518533833364,29.2679423076924));
#95673=CARTESIAN_POINT('Ctrl Pts',(-0.449198133734217,2.7688529622084,29.4270072115385));
#95674=CARTESIAN_POINT('Ctrl Pts',(-2.57197929767765,1.11948567744212,29.5860721153846));
#95675=CARTESIAN_POINT('Ctrl Pts',(-2.33254288359573,-1.55806591191366,
29.7451370192308));
#95676=CARTESIAN_POINT('Ctrl Pts',(0.0492022987188458,-2.80462204645853,
29.9042019230769));
#95677=CARTESIAN_POINT('Ctrl Pts',(2.38575795131293,-1.47529139068443,30.0632668269231));
#95678=CARTESIAN_POINT('Ctrl Pts',(2.53112980449082,1.20901100181045,30.2223317307692));
#95679=CARTESIAN_POINT('Ctrl Pts',(0.351802029708706,2.78290514059918,30.3813966346154));
#95680=CARTESIAN_POINT('Ctrl Pts',(-2.15063602022738,1.80085823933508,30.5404615384615));
#95681=CARTESIAN_POINT('Ctrl Pts',(-2.67783647182709,-0.835175143208346,
30.6995264423077));
#95682=CARTESIAN_POINT('Ctrl Pts',(-0.74559551558228,-2.70414737335524,
30.8585913461539));
#95683=CARTESIAN_POINT('Ctrl Pts',(1.87143276947021,-2.08951312009126,31.01765625));
#95684=CARTESIAN_POINT('Ctrl Pts',(2.76965585724649,0.444220803318177,31.1767211538462));
#95685=CARTESIAN_POINT('Ctrl Pts',(1.12410662268099,2.56996303291023,31.3357860576923));
#95686=CARTESIAN_POINT('Ctrl Pts',(-1.55387099343073,2.33533950967628,31.4948509615385));
#95687=CARTESIAN_POINT('Ctrl Pts',(-2.80470595019833,-0.0441613247380469,
31.6539158653847));
#95688=CARTESIAN_POINT('Ctrl Pts',(-1.4795770558054,-2.38310247904171,31.8129807692308));
#95689=CARTESIAN_POINT('Ctrl Pts',(1.20445971643178,-2.53329873508307,31.972045673077));
#95690=CARTESIAN_POINT('Ctrl Pts',(2.78226833327609,-0.356803323035994,
32.1311105769231));
#95691=CARTESIAN_POINT('Ctrl Pts',(1.80472078159196,2.14739576933795,32.2901754807693));
#95692=CARTESIAN_POINT('Ctrl Pts',(-0.83036077806552,2.67933325062988,32.4492403846154));
#95693=CARTESIAN_POINT('Ctrl Pts',(-2.70280290752998,0.750454617367339,
32.6083052884616));
#95694=CARTESIAN_POINT('Ctrl Pts',(-2.09287336943466,-1.86767415498305,
32.7673701923077));
#95695=CARTESIAN_POINT('Ctrl Pts',(0.439242037856295,-2.77044980497037,
32.9264350961539));
#95696=CARTESIAN_POINT('Ctrl Pts',(2.56793846593204,-1.12872393651732,33.0855));
#95697=CARTESIAN_POINT('Ctrl Pts',(2.33812859149225,1.54967105520072,33.2445649038462));
#95698=CARTESIAN_POINT('Ctrl Pts',(-0.0391202080950587,2.80478079339528,
33.4036298076924));
#95699=CARTESIAN_POINT('Ctrl Pts',(-2.38043930820866,1.48385794118423,33.5626947115384));
#95700=CARTESIAN_POINT('Ctrl Pts',(-2.53545948190777,-1.19990454007159,
33.7217596153847));
#95701=CARTESIAN_POINT('Ctrl Pts',(-0.361803463717808,-2.78162253789443,
33.8808245192308));
#95702=CARTESIAN_POINT('Ctrl Pts',(2.14414858133226,-1.80857749373683,34.039889423077));
#95703=CARTESIAN_POINT('Ctrl Pts',(2.68082137390367,0.825543730459955,34.1989543269231));
#95704=CARTESIAN_POINT('Ctrl Pts',(0.755311294824669,2.70144971035752,34.3580192307693));
#95705=CARTESIAN_POINT('Ctrl Pts',(-1.86390950701438,2.09622685779518,34.5170841346154));
#95706=CARTESIAN_POINT('Ctrl Pts',(-2.77123480281515,-0.4342618534324,34.6761490384615));
#95707=CARTESIAN_POINT('Ctrl Pts',(-1.13333760403503,-2.56590560328329,
34.8352139423077));
#95708=CARTESIAN_POINT('Ctrl Pts',(1.54546611079131,-2.34091012003366,34.9942788461539));
#95709=CARTESIAN_POINT('Ctrl Pts',(2.80484657580764,0.0340789650750163,
35.15334375));
#95710=CARTESIAN_POINT('Ctrl Pts',(1.48813403299161,2.37776844741717,35.3124086538462));
#95711=CARTESIAN_POINT('Ctrl Pts',(-1.1953454874454,2.53761203798461,35.4714735576924));
#95712=CARTESIAN_POINT('Ctrl Pts',(-2.78096775654043,0.36680243560116,35.6305384615384));
#95713=CARTESIAN_POINT('Ctrl Pts',(-1.81242836331058,-2.14089446670025,
35.7896033653847));
#95714=CARTESIAN_POINT('Ctrl Pts',(0.820724015952912,-2.68230083684112,
35.9486682692308));
#95715=CARTESIAN_POINT('Ctrl Pts',(2.70008778620931,-0.760165532265031,
36.107733173077));
#95716=CARTESIAN_POINT('Ctrl Pts',(2.09957357433953,1.86013883772571,36.2667980769231));
#95717=CARTESIAN_POINT('Ctrl Pts',(-0.429280266134804,2.77201084824496,
36.4258629807693));
#95718=CARTESIAN_POINT('Ctrl Pts',(-2.5638644515312,1.13794761032974,36.5849278846154));
#95719=CARTESIAN_POINT('Ctrl Pts',(-2.34368408631476,-1.54125617378662,
36.7439927884616));
#95720=CARTESIAN_POINT('Ctrl Pts',(0.0290376119636847,-2.8049032972229,
36.9030576923078));
#95721=CARTESIAN_POINT('Ctrl Pts',(2.37508990529535,-1.49240531741365,37.0621225961539));
#95722=CARTESIAN_POINT('Ctrl Pts',(2.53975639635982,1.19078257328104,37.2211875));
#95723=CARTESIAN_POINT('Ctrl Pts',(0.371800222537135,2.78030399132932,37.3802524038462));
#95724=CARTESIAN_POINT('Ctrl Pts',(-2.13763343595425,1.81627337787318,37.5393173076923));
#95725=CARTESIAN_POINT('Ctrl Pts',(-2.68377163466288,-0.81590165011443,
37.6983822115385));
#95726=CARTESIAN_POINT('Ctrl Pts',(-0.765017314006785,-2.69871713948505,
37.8574471153846));
#95727=CARTESIAN_POINT('Ctrl Pts',(1.8563621592982,-2.10291350825614,38.0165120192308));
#95728=CARTESIAN_POINT('Ctrl Pts',(2.77277793875275,0.424297292056489,38.175576923077));
#95729=CARTESIAN_POINT('Ctrl Pts',(1.14255394050895,2.56181501726957,38.3346418269231));
#95730=CARTESIAN_POINT('Ctrl Pts',(-1.53704125778664,2.34645048137439,38.4937067307693));
#95731=CARTESIAN_POINT('Ctrl Pts',(-2.80495095745781,-0.0239961650468875,
38.6527716346154));
#95732=CARTESIAN_POINT('Ctrl Pts',(-1.49667178065217,-2.37240369049618,
38.8118365384616));
#95733=CARTESIAN_POINT('Ctrl Pts',(1.18621581231896,-2.54189255010612,38.9709014423077));
#95734=CARTESIAN_POINT('Ctrl Pts',(2.77963124440541,-0.376796808380384,
39.1299663461539));
#95735=CARTESIAN_POINT('Ctrl Pts',(1.82011252500328,2.13436549962901,39.28903125));
#95736=CARTESIAN_POINT('Ctrl Pts',(-0.811076648523027,2.68523376261753,
39.4480961538463));
#95737=CARTESIAN_POINT('Ctrl Pts',(-2.69733777461252,0.769866624376458,
39.6071610576923));
#95738=CARTESIAN_POINT('Ctrl Pts',(-2.10624664875555,-1.85257948393219,
39.7662259615385));
#95739=CARTESIAN_POINT('Ctrl Pts',(0.419312947294725,-2.77353607186051,
39.9252908653846));
#95740=CARTESIAN_POINT('Ctrl Pts',(2.55975730711914,-1.14715657969204,40.0843557692308));
#95741=CARTESIAN_POINT('Ctrl Pts',(2.34920929627571,1.53282137640764,40.243420673077));
#95742=CARTESIAN_POINT('Ctrl Pts',(-0.0189546406110363,2.80498955635841,
40.4024855769231));
#95743=CARTESIAN_POINT('Ctrl Pts',(-2.36970981169745,1.50093340892436,40.5615504807693));
#95744=CARTESIAN_POINT('Ctrl Pts',(-2.54402049232267,-1.18164521931195,
40.7206153846154));
#95745=CARTESIAN_POINT('Ctrl Pts',(-0.381792176989602,-2.77894951794198,
40.8796802884616));
#95746=CARTESIAN_POINT('Ctrl Pts',(2.13109066828147,-1.82394579229869,41.0387451923077));
#95747=CARTESIAN_POINT('Ctrl Pts',(2.68668721598173,0.806249026765786,41.1978100961539));
#95748=CARTESIAN_POINT('Ctrl Pts',(0.774713447708398,2.69594969604779,41.356875));
#95749=CARTESIAN_POINT('Ctrl Pts',(-1.84879082384766,2.10957298506999,41.5159399038462));
#95750=CARTESIAN_POINT('Ctrl Pts',(-2.77428524511908,-0.41432724795145,
41.6750048076923));
#95751=CARTESIAN_POINT('Ctrl Pts',(-1.15175551301023,-2.55769132772724,
41.8340697115385));
#95752=CARTESIAN_POINT('Ctrl Pts',(1.52859654328181,-2.35196052210647,41.9931346153846));
#95753=CARTESIAN_POINT('Ctrl Pts',(2.8050190938,0.0139130549425746,42.1521995192308));
#95754=CARTESIAN_POINT('Ctrl Pts',(1.50519018846317,2.36700827760163,42.311264423077));
#95755=CARTESIAN_POINT('Ctrl Pts',(-1.17707080902522,2.54614021613523,42.4703293269231));
#95756=CARTESIAN_POINT('Ctrl Pts',(-2.77825881414133,0.386786312227329,
42.6293942307692));
#95757=CARTESIAN_POINT('Ctrl Pts',(-1.82777316737607,-2.12780895249092,
42.7884591346155));
#95758=CARTESIAN_POINT('Ctrl Pts',(0.801418800438249,-2.68813199006011,
42.9475240384615));
#95759=CARTESIAN_POINT('Ctrl Pts',(2.69455290827499,-0.779557768345067,
43.1065889423078));
#95760=CARTESIAN_POINT('Ctrl Pts',(2.11289250645387,1.84499619128384,43.2656538461538));
#95761=CARTESIAN_POINT('Ctrl Pts',(-0.409340210132954,2.7750254561082,43.4247187500001));
#95762=CARTESIAN_POINT('Ctrl Pts',(-2.55561708576786,1.15635072560681,43.5837836538462));
#95763=CARTESIAN_POINT('Ctrl Pts',(-2.3547041499791,-1.5243667720576,43.7428485576924));
#95764=CARTESIAN_POINT('Ctrl Pts',(0.00887142432873881,-2.80503956968683,
43.9019134615385));
#95765=CARTESIAN_POINT('Ctrl Pts',(2.36429909693514,-1.50944210551781,44.0609783653846));
#95766=CARTESIAN_POINT('Ctrl Pts',(2.54825171469771,1.17249259623757,44.2200432692308));
#95767=CARTESIAN_POINT('Ctrl Pts',(0.391779197956932,2.77755913523241,44.3791081730769));
#95768=CARTESIAN_POINT('Ctrl Pts',(-2.12452036285295,1.8315946378757,44.5381730769232));
#95769=CARTESIAN_POINT('Ctrl Pts',(-2.68956808019675,-0.796585985153158,
44.6972379807693));
#95770=CARTESIAN_POINT('Ctrl Pts',(-0.784399570615147,-2.69314741578982,
44.8563028846154));
#95771=CARTESIAN_POINT('Ctrl Pts',(1.84119559845759,-2.11620520221519,45.0153677884616));
#95772=CARTESIAN_POINT('Ctrl Pts',(2.7757567025159,0.404351850010035,45.1744326923077));
#95773=CARTESIAN_POINT('Ctrl Pts',(1.16094220248601,2.55353458782659,45.3334975961539));
#95774=CARTESIAN_POINT('Ctrl Pts',(-1.52013207611093,2.35744017125017,45.4925625));
#95775=CARTESIAN_POINT('Ctrl Pts',(-2.80505098450271,-0.00382976547574787,
45.6516274038463));
#95776=CARTESIAN_POINT('Ctrl Pts',(-1.51368914530336,-2.36158227765018,
45.8106923076923));
#95777=CARTESIAN_POINT('Ctrl Pts',(1.16791059373771,-2.55035498271459,45.9697572115385));
#95778=CARTESIAN_POINT('Ctrl Pts',(2.77685048729278,-0.396770815138777,
46.1288221153846));
#95779=CARTESIAN_POINT('Ctrl Pts',(1.83541018417072,2.12122490443972,46.2878870192308));
#95780=CARTESIAN_POINT('Ctrl Pts',(-0.791750582632343,2.69099549234209,
46.446951923077));
#95781=CARTESIAN_POINT('Ctrl Pts',(-2.69173324962905,0.789238818677136,
46.6060168269231));
#95782=CARTESIAN_POINT('Ctrl Pts',(-2.11951101110941,-1.83738901911381,
46.7650817307693));
#95783=CARTESIAN_POINT('Ctrl Pts',(0.399362087284636,-2.7764790554831,46.9241466346154));
#95784=CARTESIAN_POINT('Ctrl Pts',(2.55144402454308,-1.16552978860435,47.0832115384616));
#95785=CARTESIAN_POINT('Ctrl Pts',(2.36016822626022,1.51589220166356,47.2422764423077));
#95786=CARTESIAN_POINT('Ctrl Pts',(0.00121257453600308,2.80505384839945,
47.4013413461539));
#95787=CARTESIAN_POINT('Ctrl Pts',(-2.35885910506479,1.51793032089209,47.56040625));
#95788=CARTESIAN_POINT('Ctrl Pts',(-2.55244757833081,-1.16332295988949,
47.7194711538462));
#95789=CARTESIAN_POINT('Ctrl Pts',(-0.401765792635603,-2.77613641385121,
47.8785360576923));
#95790=CARTESIAN_POINT('Ctrl Pts',(2.11793144842226,-1.83921303886061,48.0376009615385));
#95791=CARTESIAN_POINT('Ctrl Pts',(2.69239732002637,0.78689972288376,48.1966658653846));
#95792=CARTESIAN_POINT('Ctrl Pts',(0.794107738018986,2.69033499428045,48.3557307692309));
#95793=CARTESIAN_POINT('Ctrl Pts',(-1.83363796749767,2.12276303487646,48.5147956730769));
#95794=CARTESIAN_POINT('Ctrl Pts',(-2.77707519007022,-0.394281495485595,
48.6738605769232));
#95795=CARTESIAN_POINT('Ctrl Pts',(-1.17033730995746,-2.54951603961395,
48.8329254807692));
#95796=CARTESIAN_POINT('Ctrl Pts',(1.51207452279905,-2.36256262295682,48.9919903846154));
#95797=CARTESIAN_POINT('Ctrl Pts',(2.80422967385422,-0.00687846186160384,
49.1510552884616));
#95798=CARTESIAN_POINT('Ctrl Pts',(1.52375565164409,2.35733202978189,49.3101201923077));
#95799=CARTESIAN_POINT('Ctrl Pts',(-1.16201321478499,2.55211054076708,49.4691850961539));
#95800=CARTESIAN_POINT('Ctrl Pts',(-2.23210772954909,1.12570340751462,49.5752283653847));
#95801=CARTESIAN_POINT('Ctrl Pts',(-2.34668236863857,0.343918483395232,
49.62825));
#95802=CARTESIAN_POINT('',(1.37702479013102,-1.93106208855765,0.));
#95803=CARTESIAN_POINT('Ctrl Pts',(1.37702479013074,-1.93106208855785,0.));
#95804=CARTESIAN_POINT('Ctrl Pts',(2.02034799762934,-1.47231350142485,0.0530216346153847));
#95805=CARTESIAN_POINT('Ctrl Pts',(2.80114700154351,0.130837301153735,0.159064903846153));
#95806=CARTESIAN_POINT('Ctrl Pts',(1.40206621881702,2.43167759018441,0.318129807692308));
#95807=CARTESIAN_POINT('Ctrl Pts',(-1.28595649275605,2.49200065724321,0.477194711538461));
#95808=CARTESIAN_POINT('Ctrl Pts',(-2.33798102191255,0.938128541486862,
0.588288145006008));
#95809=CARTESIAN_POINT('Ctrl Pts',(-2.37525168063667,0.0764476031090624,
0.646359943858168));
#95810=CARTESIAN_POINT('Ctrl Pts',(-2.37475566780996,0.00146584572226396,
0.651410108094944));
#95811=CARTESIAN_POINT('Ctrl Pts',(1.29201570592006,2.64858957748139,-1.12757025938492E-16));
#95812=CARTESIAN_POINT('Ctrl Pts',(1.35047965203311,2.6133373327088,-1.12757025938492E-16));
#95813=CARTESIAN_POINT('Ctrl Pts',(1.40754132366598,2.57595763103654,2.13489512922672E-16));
#95814=CARTESIAN_POINT('Ctrl Pts',(1.46306877857888,2.53644300429327,1.17961196366423E-16));
#95815=CARTESIAN_POINT('Ctrl Pts',(1.54265755239867,2.47980578410417,-2.28698325172702E-17));
#95816=CARTESIAN_POINT('Ctrl Pts',(1.61909632492994,2.4187835354811,-2.47637160981643E-16));
#95817=CARTESIAN_POINT('Ctrl Pts',(1.69220921223578,2.35375552712431,-3.40005801291454E-16));
#95818=CARTESIAN_POINT('Ctrl Pts',(1.73112408478278,2.31914389092118,-3.89169690141314E-16));
#95819=CARTESIAN_POINT('Ctrl Pts',(1.76909604502006,2.28339686212,-3.9497258110791E-16));
#95820=CARTESIAN_POINT('Ctrl Pts',(1.80609349552389,2.24656857838508,-2.70616862252382E-16));
#95821=CARTESIAN_POINT('Ctrl Pts',(1.82369497454583,2.229047580188,-2.11454824142015E-16));
#95822=CARTESIAN_POINT('Ctrl Pts',(1.8410758325068,2.21128182971957,-7.03914766414606E-16));
#95823=CARTESIAN_POINT('Ctrl Pts',(1.85823236581716,2.19327704183541,-7.07767178198537E-16));
#95824=CARTESIAN_POINT('Ctrl Pts',(1.8762119379848,2.17440852234662,-7.11804399147296E-16));
#95825=CARTESIAN_POINT('Ctrl Pts',(1.89394940284166,2.15527254575146,-2.20692458830647E-16));
#95826=CARTESIAN_POINT('Ctrl Pts',(1.91141683968546,2.13590224832762,-2.56739074444567E-16));
#95827=CARTESIAN_POINT('Ctrl Pts',(1.97654793536834,2.06367592764876,-3.91146634728832E-16));
#95828=CARTESIAN_POINT('Ctrl Pts',(2.03798087273529,1.98814233841135,-4.75975953068255E-17));
#95829=CARTESIAN_POINT('Ctrl Pts',(2.09554087281375,1.90967640222123,-3.46944695195361E-17));
#95830=CARTESIAN_POINT('Ctrl Pts',(2.14262943686529,1.8454851538349,-2.41387074578314E-17));
#95831=CARTESIAN_POINT('Ctrl Pts',(2.18712531645739,1.77933058201533,-9.28299200764564E-18));
#95832=CARTESIAN_POINT('Ctrl Pts',(2.22890868996356,1.71140843266836,-2.77555756156289E-17));
#95833=CARTESIAN_POINT('Ctrl Pts',(2.24792938225854,1.68048880616784,-3.61646938657112E-17));
#95834=CARTESIAN_POINT('Ctrl Pts',(2.26638765990956,1.64920281103461,-3.05448741047574E-16));
#95835=CARTESIAN_POINT('Ctrl Pts',(2.2842706081915,1.61756865561342,-2.91433543964104E-16));
#95836=CARTESIAN_POINT('Ctrl Pts',(2.29484156490064,1.59886909432101,-2.83148889817395E-16));
#95837=CARTESIAN_POINT('Ctrl Pts',(2.30521146927951,1.58004787629747,4.42982721947554E-17));
#95838=CARTESIAN_POINT('Ctrl Pts',(2.31537748039068,1.56110875696981,6.93889390390723E-17));
#95839=CARTESIAN_POINT('Ctrl Pts',(2.32260089416002,1.54765165035891,8.72170002504184E-17));
#95840=CARTESIAN_POINT('Ctrl Pts',(2.32972104671691,1.53413546224949,-2.90001761152889E-16));
#95841=CARTESIAN_POINT('Ctrl Pts',(2.33673088705629,1.52057364590497,-2.77555756156289E-16));
#95842=CARTESIAN_POINT('Ctrl Pts',(2.38039267025554,1.43610195234924,-2.00034051588298E-16));
#95843=CARTESIAN_POINT('Ctrl Pts',(2.41984393470611,1.34974138975305,-3.54536939389555E-16));
#95844=CARTESIAN_POINT('Ctrl Pts',(2.45491901736627,1.26183770540906,-3.60822483003176E-16));
#95845=CARTESIAN_POINT('Ctrl Pts',(2.49095039506518,1.17153739500316,-3.67279397108831E-16));
#95846=CARTESIAN_POINT('Ctrl Pts',(2.52236430096921,1.07960768483293,1.90948379502136E-16));
#95847=CARTESIAN_POINT('Ctrl Pts',(2.54892424395783,0.986413230220722,2.08166817117217E-16));
#95848=CARTESIAN_POINT('Ctrl Pts',(2.57369277004672,0.899504561727304,2.24223904342959E-16));
#95849=CARTESIAN_POINT('Ctrl Pts',(2.5942397122875,0.811495234712604,-2.90917053419974E-16));
#95850=CARTESIAN_POINT('Ctrl Pts',(2.61032409035078,0.722685000091402,-3.33066907387547E-16));
#95851=CARTESIAN_POINT('Ctrl Pts',(2.61939480520976,0.672600855610439,-3.5683713370175E-16));
#95852=CARTESIAN_POINT('Ctrl Pts',(2.62704538989607,0.622262130851272,-4.79791839152818E-16));
#95853=CARTESIAN_POINT('Ctrl Pts',(2.63322550736737,0.571724499349377,-4.9960036108132E-16));
#95854=CARTESIAN_POINT('Ctrl Pts',(2.63576498704184,0.550958019004824,-5.07739905200389E-16));
#95855=CARTESIAN_POINT('Ctrl Pts',(2.63805663524629,0.530151373647901,6.55971552207216E-16));
#95856=CARTESIAN_POINT('Ctrl Pts',(2.64009358497002,0.509344318092916,6.10622663543836E-16));
#95857=CARTESIAN_POINT('Ctrl Pts',(2.64878126462266,0.420601316206363,4.17207670174275E-16));
#95858=CARTESIAN_POINT('Ctrl Pts',(2.65285456203884,0.331754436353281,-3.00385640345007E-16));
#95859=CARTESIAN_POINT('Ctrl Pts',(2.65212953715791,0.243094007921421,-2.4980018054066E-16));
#95860=CARTESIAN_POINT('Ctrl Pts',(2.6518119314253,0.204255257601141,-2.27640620995021E-16));
#95861=CARTESIAN_POINT('Ctrl Pts',(2.65057287851832,0.165452331247355,1.32747360840593E-16));
#95862=CARTESIAN_POINT('Ctrl Pts',(2.64839376652478,0.126710099518821,1.11022302462516E-16));
#95863=CARTESIAN_POINT('Ctrl Pts',(2.64331550885207,0.0364242233839251,
3.36506741470677E-17));
#95864=CARTESIAN_POINT('Ctrl Pts',(2.6331350383468,-0.0535335684357302,
2.32891675937926E-17));
#95865=CARTESIAN_POINT('Ctrl Pts',(2.61804895698347,-0.142830691087905,
0.));
#95866=CARTESIAN_POINT('Ctrl Pts',(2.60250975672972,-0.234809902757026,
-2.39886707665931E-17));
#95867=CARTESIAN_POINT('Ctrl Pts',(2.58176536987519,-0.326089235663464,
-1.3663112480103E-16));
#95868=CARTESIAN_POINT('Ctrl Pts',(2.55598340453964,-0.41627347846358,0.));
#95869=CARTESIAN_POINT('Ctrl Pts',(2.55178247440597,-0.430968157407989,
2.22627639865488E-17));
#95870=CARTESIAN_POINT('Ctrl Pts',(2.54744770854094,-0.445633674797536,
-6.91067322917457E-17));
#95871=CARTESIAN_POINT('Ctrl Pts',(2.54297973154851,-0.460268213187004,
-5.55111512312578E-17));
#95872=CARTESIAN_POINT('Ctrl Pts',(2.5389302343891,-0.473532050878587,-4.31889600073214E-17));
#95873=CARTESIAN_POINT('Ctrl Pts',(2.53477298110434,-0.486764833902074,
-6.0951382644997E-16));
#95874=CARTESIAN_POINT('Ctrl Pts',(2.53051107740137,-0.499958263234954,
-5.82867087928207E-16));
#95875=CARTESIAN_POINT('Ctrl Pts',(2.5032317931632,-0.584405809198302,-4.12308575860242E-16));
#95876=CARTESIAN_POINT('Ctrl Pts',(2.47164137946824,-0.667333741906229,
-3.15553173727667E-16));
#95877=CARTESIAN_POINT('Ctrl Pts',(2.43595239984652,-0.748438750214095,
-1.94289029309402E-16));
#95878=CARTESIAN_POINT('Ctrl Pts',(2.40031431849794,-0.829428089626163,
-7.31978272282084E-17));
#95879=CARTESIAN_POINT('Ctrl Pts',(2.36058869270874,-0.908600483118366,
6.82754206395419E-17));
#95880=CARTESIAN_POINT('Ctrl Pts',(2.31694497829497,-0.985624034856247,
1.94289029309402E-16));
#95881=CARTESIAN_POINT('Ctrl Pts',(2.27399614291603,-1.06142124616893,3.18296296036431E-16));
#95882=CARTESIAN_POINT('Ctrl Pts',(2.22725231457587,-1.13513811558509,-6.23795482104556E-16));
#95883=CARTESIAN_POINT('Ctrl Pts',(2.17684411225952,-1.20641915833307,-7.21644966006352E-16));
#95884=CARTESIAN_POINT('Ctrl Pts',(2.16022671274044,-1.22991742867499,-7.5390169987135E-16));
#95885=CARTESIAN_POINT('Ctrl Pts',(2.14321088331498,-1.25315062930938,-3.34983149003289E-16));
#95886=CARTESIAN_POINT('Ctrl Pts',(2.12580073890458,-1.27610489756701,-3.33066907387547E-16));
#95887=CARTESIAN_POINT('Ctrl Pts',(2.11280904752226,-1.29323369110718,-3.31636981299695E-16));
#95888=CARTESIAN_POINT('Ctrl Pts',(2.09959778216782,-1.31020715351732,-5.6152853452759E-16));
#95889=CARTESIAN_POINT('Ctrl Pts',(2.08616856960686,-1.32701929923775,-6.10622663543836E-16));
#95890=CARTESIAN_POINT('Ctrl Pts',(2.07805318318902,-1.33717902069682,-6.40290659787479E-16));
#95891=CARTESIAN_POINT('Ctrl Pts',(2.06986448397218,-1.34727196523556,4.59211246770366E-16));
#95892=CARTESIAN_POINT('Ctrl Pts',(2.06160311038263,-1.35729714638091,4.44089209850063E-16));
#95893=CARTESIAN_POINT('Ctrl Pts',(2.00737870704495,-1.42309848801806,3.44834113785818E-16));
#95894=CARTESIAN_POINT('Ctrl Pts',(1.95002592106155,-1.48598389603456,6.1896723624897E-16));
#95895=CARTESIAN_POINT('Ctrl Pts',(1.8897024430572,-1.54565686846859,4.44089209850063E-16));
#95896=CARTESIAN_POINT('Ctrl Pts',(1.83033018451105,-1.60438887903527,2.71968772818087E-16));
#95897=CARTESIAN_POINT('Ctrl Pts',(1.76807954519956,-1.66000948217716,3.80823319481553E-16));
#95898=CARTESIAN_POINT('Ctrl Pts',(1.70307501002074,-1.71219354094858,4.44089209850063E-16));
#95899=CARTESIAN_POINT('Ctrl Pts',(1.64009787967249,-1.76275004846468,5.05381921402809E-16));
#95900=CARTESIAN_POINT('Ctrl Pts',(1.57453538849668,-1.81008131772167,1.79680524881221E-16));
#95901=CARTESIAN_POINT('Ctrl Pts',(1.50648507168998,-1.85384593634628,2.22044604925031E-16));
#95902=CARTESIAN_POINT('Ctrl Pts',(1.46428163718096,-1.88098787047103,2.48317953258481E-16));
#95903=CARTESIAN_POINT('Ctrl Pts',(1.42112105178449,-1.90675706879086,-1.67702223404997E-17));
#95904=CARTESIAN_POINT('Ctrl Pts',(1.37702479013074,-1.93106208855785,0.));
#95905=CARTESIAN_POINT('Ctrl Pts',(0.260739855805175,2.92492329228916,49.058));
#95906=CARTESIAN_POINT('Ctrl Pts',(0.736266525833309,2.88315289962924,49.0322954004341));
#95907=CARTESIAN_POINT('Ctrl Pts',(1.20206891229148,2.73208629432238,49.0065908008682));
#95908=CARTESIAN_POINT('Ctrl Pts',(1.59958942631121,2.47560915657343,48.9808862013024));
#95909=CARTESIAN_POINT('Ctrl Pts',(2.41956669895652,1.9465662103852,48.927864566687));
#95910=CARTESIAN_POINT('Ctrl Pts',(2.94901465557698,0.969016965254652,48.8748429320716));
#95911=CARTESIAN_POINT('Ctrl Pts',(2.94659971013865,-0.00676955442900931,
48.8218212974562));
#95912=CARTESIAN_POINT('Ctrl Pts',(2.94418476470032,-0.982556074112615,
48.7687996628408));
#95913=CARTESIAN_POINT('Ctrl Pts',(2.40990691720327,-1.95657986834934,48.7157780282254));
#95914=CARTESIAN_POINT('Ctrl Pts',(1.58820872905997,-2.48224233655137,48.66275639361));
#95915=CARTESIAN_POINT('Ctrl Pts',(0.766510540916721,-3.00790480475337,
48.6097347589946));
#95916=CARTESIAN_POINT('Ctrl Pts',(-0.342607987872747,-3.08520594692074,
48.5567131243793));
#95917=CARTESIAN_POINT('Ctrl Pts',(-1.22934270943994,-2.67828538355204,
48.5036914897639));
#95918=CARTESIAN_POINT('Ctrl Pts',(-2.11607743100718,-2.27136482018332,
48.4506698551485));
#95919=CARTESIAN_POINT('Ctrl Pts',(-2.78042834535212,-1.38022255127848,
48.3976482205331));
#95920=CARTESIAN_POINT('Ctrl Pts',(-2.91755849077816,-0.414280030836403,
48.3446265859177));
#95921=CARTESIAN_POINT('Ctrl Pts',(-2.93691308114256,-0.277946610197007,
48.3371430963083));
#95922=CARTESIAN_POINT('Ctrl Pts',(-2.94576512520083,-0.140123124765416,
48.3296596066989));
#95923=CARTESIAN_POINT('Ctrl Pts',(-2.94461792262617,-0.00215304676840083,
48.3221761170895));
#95924=CARTESIAN_POINT('Origin',(0.,0.,-1.84858989190512));
#95925=CARTESIAN_POINT('',(-1.37702479013129,-1.93106208855745,0.));
#95926=CARTESIAN_POINT('Ctrl Pts',(-1.38001442237635,-1.93381244560189,
4.37638206923774E-15));
#95927=CARTESIAN_POINT('Ctrl Pts',(-0.781458010274238,-2.35626571080451,
0.049355603818813));
#95928=CARTESIAN_POINT('Ctrl Pts',(0.901264645133876,-2.62481382078411,
0.151744630133381));
#95929=CARTESIAN_POINT('Ctrl Pts',(2.71060447735492,-0.722409270309101,
0.307167078943709));
#95930=CARTESIAN_POINT('Ctrl Pts',(2.07285013055992,1.89055543244044,0.466267346430989));
#95931=CARTESIAN_POINT('Ctrl Pts',(-0.469810478716988,2.76551378306258,
0.625367613918266));
#95932=CARTESIAN_POINT('Ctrl Pts',(-2.16059338637857,1.43138769003934,0.752808462409609));
#95933=CARTESIAN_POINT('Ctrl Pts',(-2.36987959467941,0.320783635789767,
0.82721588840519));
#95934=CARTESIAN_POINT('Ctrl Pts',(-2.36841685556579,0.00122403911035841,
0.848589891905012));
#95935=CARTESIAN_POINT('Origin',(0.,0.,0.));
#95936=CARTESIAN_POINT('Ctrl Pts',(-1.03908919352446,2.13201587949074,-0.329233991005407));
#95937=CARTESIAN_POINT('Ctrl Pts',(-1.74951701127321,1.7857718034953,-0.276200568509647));
#95938=CARTESIAN_POINT('Ctrl Pts',(-2.78455395807173,0.333124289911143,
-0.170133723518128));
#95939=CARTESIAN_POINT('Ctrl Pts',(-1.78369205252407,-2.16759894682849,
-0.0110334560308489));
#95940=CARTESIAN_POINT('Ctrl Pts',(0.858449569970475,-2.66983112066845,
0.14806681145643));
#95941=CARTESIAN_POINT('Ctrl Pts',(2.71060447735492,-0.722409270309101,
0.307167078943709));
#95942=CARTESIAN_POINT('Ctrl Pts',(2.07285013055992,1.89055543244044,0.466267346430989));
#95943=CARTESIAN_POINT('Ctrl Pts',(-0.469810478716988,2.76551378306258,
0.625367613918266));
#95944=CARTESIAN_POINT('Ctrl Pts',(-2.58062515122094,1.09995818786284,0.784467881405546));
#95945=CARTESIAN_POINT('Ctrl Pts',(-2.3204090178813,-1.57651378416218,0.943568148892824));
#95946=CARTESIAN_POINT('Ctrl Pts',(0.0718874078444588,-2.8043235471302,
1.1026684163801));
#95947=CARTESIAN_POINT('Ctrl Pts',(2.39810709656883,-1.45554260356973,1.26176868386738));
#95948=CARTESIAN_POINT('Ctrl Pts',(2.52091778453322,1.23065290615308,1.42086895135466));
#95949=CARTESIAN_POINT('Ctrl Pts',(0.327458637825707,2.78608392325822,1.57996921884194));
#95950=CARTESIAN_POINT('Ctrl Pts',(-2.16687151941952,1.7816229585196,1.73906948632922));
#95951=CARTESIAN_POINT('Ctrl Pts',(-2.67024455303756,-0.859829308452707,
1.8981697538165));
#95952=CARTESIAN_POINT('Ctrl Pts',(-0.720149694819682,-2.71125275032746,
2.05727002130378));
#95953=CARTESIAN_POINT('Ctrl Pts',(1.89163063518288,-2.07153172086814,2.21637028879105));
#95954=CARTESIAN_POINT('Ctrl Pts',(2.76534828940725,0.471549254232345,2.37547055627834));
#95955=CARTESIAN_POINT('Ctrl Pts',(1.09821595227919,2.58136221632247,2.53457082376561));
#95956=CARTESIAN_POINT('Ctrl Pts',(-1.5779761243933,2.31937512843085,2.69367109125289));
#95957=CARTESIAN_POINT('Ctrl Pts',(-2.80429647983432,-0.0736940611091368,
2.85277135874017));
#95958=CARTESIAN_POINT('Ctrl Pts',(-1.45398069647754,-2.39905181471807,
3.01187162622745));
#95959=CARTESIAN_POINT('Ctrl Pts',(1.23227769270891,-2.52011928935842,3.17097189371473));
#95960=CARTESIAN_POINT('Ctrl Pts',(2.78629802603849,-0.325657548824043,
3.330072161202));
#95961=CARTESIAN_POINT('Ctrl Pts',(1.78021952909652,2.16802397289482,3.48917242868929));
#95962=CARTESIAN_POINT('Ctrl Pts',(-0.861555466122802,2.66968756742434,
3.64827269617656));
#95963=CARTESIAN_POINT('Ctrl Pts',(-2.71171839560361,0.718396039047425,
3.80737296366385));
#95964=CARTESIAN_POINT('Ctrl Pts',(-2.07030755199707,-1.89297019654229,
3.96647323115112));
#95965=CARTESIAN_POINT('Ctrl Pts',(0.473337684987186,-2.76504266915617,
4.12557349863841));
#95966=CARTESIAN_POINT('Ctrl Pts',(2.58207206872294,-1.09654610377387,4.28467376612568));
#95967=CARTESIAN_POINT('Ctrl Pts',(2.31835396766711,1.57947599104097,4.44377403361296));
#95968=CARTESIAN_POINT('Ctrl Pts',(-0.075507864702191,2.804248221581,4.60287430110024));
#95969=CARTESIAN_POINT('Ctrl Pts',(-2.39999176476856,1.45242867461087,4.76197456858752));
#95970=CARTESIAN_POINT('Ctrl Pts',(-2.51932171322798,-1.23390746453664,
4.9210748360748));
#95971=CARTESIAN_POINT('Ctrl Pts',(-0.323855289127461,-2.78650807957066,
5.08017510356208));
#95972=CARTESIAN_POINT('Ctrl Pts',(2.16917497708905,-1.77881686650588,5.23927537104935));
#95973=CARTESIAN_POINT('Ctrl Pts',(2.66912974919035,0.863282055751294,5.39837563853664));
#95974=CARTESIAN_POINT('Ctrl Pts',(0.716641933714364,2.71218249102838,5.55747590602391));
#95975=CARTESIAN_POINT('Ctrl Pts',(-1.89430888784795,2.06908273474431,5.71657617351119));
#95976=CARTESIAN_POINT('Ctrl Pts',(-2.76473593307623,-0.475126031863108,
5.87567644099847));
#95977=CARTESIAN_POINT('Ctrl Pts',(-1.09487577505419,-2.58278078105689,
6.03477670848575));
#95978=CARTESIAN_POINT('Ctrl Pts',(1.58097518564988,-2.31733186836853,6.19387697597303));
#95979=CARTESIAN_POINT('Ctrl Pts',(2.80419879604699,0.0773216531487339,
6.3529772434603));
#95980=CARTESIAN_POINT('Ctrl Pts',(1.45087604201706,2.40093070214407,6.51207751094759));
#95981=CARTESIAN_POINT('Ctrl Pts',(-1.23553671852851,2.51852308763786,6.67117777843485));
#95982=CARTESIAN_POINT('Ctrl Pts',(-2.78671696819491,0.322052891574838,
6.83027804592215));
#95983=CARTESIAN_POINT('Ctrl Pts',(-1.77741345928775,-2.17032507255016,
6.98937831340941));
#95984=CARTESIAN_POINT('Ctrl Pts',(0.865008283985421,-2.66857081495577,
7.14847858089671));
#95985=CARTESIAN_POINT('Ctrl Pts',(2.71264545191261,-0.714887528227297,
7.30757884838397));
#95986=CARTESIAN_POINT('Ctrl Pts',(2.0678570518103,1.89564678647566,7.46667911587126));
#95987=CARTESIAN_POINT('Ctrl Pts',(-0.476914179932666,2.76442804044096,
7.62577938335854));
#95988=CARTESIAN_POINT('Ctrl Pts',(-2.58348841288175,1.09320498823544,7.78487965084581));
#95989=CARTESIAN_POINT('Ctrl Pts',(-2.31630879958662,-1.58247371881959,
7.94397991833311));
#95990=CARTESIAN_POINT('Ctrl Pts',(0.0791354092423232,-2.80414819736781,
8.10308018582037));
#95991=CARTESIAN_POINT('Ctrl Pts',(2.40186863507383,-1.44932280243071,8.26218045330766));
#95992=CARTESIAN_POINT('Ctrl Pts',(2.51772340840239,1.23716545562014,8.42128072079493));
#95993=CARTESIAN_POINT('Ctrl Pts',(0.320250359289559,2.78692469097606,8.58038098828221));
#95994=CARTESIAN_POINT('Ctrl Pts',(-2.17147426003902,1.77600930847366,8.73948125576949));
#95995=CARTESIAN_POINT('Ctrl Pts',(-2.66801076430334,-0.866734150335981,
8.89858152325677));
#95996=CARTESIAN_POINT('Ctrl Pts',(-0.713132823661497,-2.71310727794049,
9.05768179074405));
#95997=CARTESIAN_POINT('Ctrl Pts',(1.89698389204465,-2.06663050377184,9.21678205823132));
#95998=CARTESIAN_POINT('Ctrl Pts',(2.76411899128539,0.478702128481346,9.37588232571861));
#95999=CARTESIAN_POINT('Ctrl Pts',(1.09153374406576,2.5841949638839,9.53498259320587));
#96000=CARTESIAN_POINT('Ctrl Pts',(-1.58397158994894,2.31528476175863,9.69408286069318));
#96001=CARTESIAN_POINT('Ctrl Pts',(-2.8040964255511,-0.08094913222896,9.85318312818042));
#96002=CARTESIAN_POINT('Ctrl Pts',(-1.44776895650877,-2.4028055631629,10.0122833956677));
#96003=CARTESIAN_POINT('Ctrl Pts',(1.23879367513383,-2.51692267585747,10.171383663155));
#96004=CARTESIAN_POINT('Ctrl Pts',(2.78713124782529,-0.318447693025035,
10.3304839306423));
#96005=CARTESIAN_POINT('Ctrl Pts',(1.77460441465207,2.1726225390745,10.4895841981295));
#96006=CARTESIAN_POINT('Ctrl Pts',(-0.868459654081467,2.66744959746755,
10.6486844656168));
#96007=CARTESIAN_POINT('Ctrl Pts',(-2.71356796891854,0.711377820750957,
10.8077847331041));
#96008=CARTESIAN_POINT('Ctrl Pts',(-2.0654030911422,-1.89832020399546,10.9668850005914));
#96009=CARTESIAN_POINT('Ctrl Pts',(0.480489876761207,-2.76380878573882,
11.1259852680787));
#96010=CARTESIAN_POINT('Ctrl Pts',(2.58490043376768,-1.08986204324435,11.2850855355659));
#96011=CARTESIAN_POINT('Ctrl Pts',(2.31425975531301,1.58546879841127,11.4441858030532));
#96012=CARTESIAN_POINT('Ctrl Pts',(-0.0827628213498791,2.80404348061853,
11.6032860705405));
#96013=CARTESIAN_POINT('Ctrl Pts',(-2.40374148601931,1.44621450490125,11.7623863380278));
#96014=CARTESIAN_POINT('Ctrl Pts',(-2.5161208903381,-1.24042137638842,11.921486605515));
#96015=CARTESIAN_POINT('Ctrl Pts',(-0.316644893535377,-2.78733663865617,
12.0805868730024));
#96016=CARTESIAN_POINT('Ctrl Pts',(2.17376990917619,-1.7731987784107,12.2396871404896));
#96017=CARTESIAN_POINT('Ctrl Pts',(2.66688731468318,0.870184794500003,12.3987874079769));
#96018=CARTESIAN_POINT('Ctrl Pts',(0.709622520229888,2.71402752465403,12.5578876754642));
#96019=CARTESIAN_POINT('Ctrl Pts',(-1.89965572176903,2.06417481443488,12.7169879429515));
#96020=CARTESIAN_POINT('Ctrl Pts',(-2.76349742393105,-0.482277424024338,
12.8760882104387));
#96021=CARTESIAN_POINT('Ctrl Pts',(-1.08818988647055,-2.58560482223799,
13.035188477926));
#96022=CARTESIAN_POINT('Ctrl Pts',(1.58696534358022,-2.31323378067855,13.1942887454133));
#96023=CARTESIAN_POINT('Ctrl Pts',(2.80398936259225,0.0845764758463313,
13.3533890129006));
#96024=CARTESIAN_POINT('Ctrl Pts',(1.44465944825848,2.40467640325151,13.5124892803878));
#96025=CARTESIAN_POINT('Ctrl Pts',(-1.24204855870295,2.51531805217969,13.6715895478751));
#96026=CARTESIAN_POINT('Ctrl Pts',(-2.78754086338278,0.314841961574842,
13.8306898153624));
#96027=CARTESIAN_POINT('Ctrl Pts',(-1.77179240033766,-2.1749163698641,13.9897900828497));
#96028=CARTESIAN_POINT('Ctrl Pts',(0.87190957086987,-2.66632391618547,14.148890350337));
#96029=CARTESIAN_POINT('Ctrl Pts',(2.71448594495469,-0.707866922832642,
14.3079906178242));
#96030=CARTESIAN_POINT('Ctrl Pts',(2.06294567416375,1.90099044480665,14.4670908853115));
#96031=CARTESIAN_POINT('Ctrl Pts',(-0.484064769522908,2.76318490599233,
14.6261911527988));
#96032=CARTESIAN_POINT('Ctrl Pts',(-2.58630812900012,1.08651727444391,14.7852914202861));
#96033=CARTESIAN_POINT('Ctrl Pts',(-2.31220683828449,-1.58846122482972,
14.9443916877734));
#96034=CARTESIAN_POINT('Ctrl Pts',(0.0863900949595627,-2.8039340714949,
15.1034919552607));
#96035=CARTESIAN_POINT('Ctrl Pts',(2.40561031446837,-1.44310378723102,15.2625922227479));
#96036=CARTESIAN_POINT('Ctrl Pts',(2.51451416171814,1.24367522139665,15.4216924902352));
#96037=CARTESIAN_POINT('Ctrl Pts',(0.313038897897693,2.78774392191968,15.5807927577225));
#96038=CARTESIAN_POINT('Ctrl Pts',(-2.17606192065859,1.77038528102128,15.7398930252098));
#96039=CARTESIAN_POINT('Ctrl Pts',(-2.66575940221011,-0.873633982469486,
15.898993292697));
#96040=CARTESIAN_POINT('Ctrl Pts',(-0.706111029293687,-2.71494322962874,
16.0580935601843));
#96041=CARTESIAN_POINT('Ctrl Pts',(1.90232437254992,-2.06171567084302,16.2171938276716));
#96042=CARTESIAN_POINT('Ctrl Pts',(2.7628712320534,0.485851912509174,16.3762940951588));
#96043=CARTESIAN_POINT('Ctrl Pts',(1.08484420786421,2.58701035375983,16.5353943626462));
#96044=CARTESIAN_POINT('Ctrl Pts',(-1.58995644153392,2.31117892856046,16.6944946301334));
#96045=CARTESIAN_POINT('Ctrl Pts',(-2.80387760734961,-0.0882036779308033,
16.8535948976207));
#96046=CARTESIAN_POINT('Ctrl Pts',(-1.44154752246972,-2.40654321927916,
17.012695165108));
#96047=CARTESIAN_POINT('Ctrl Pts',(1.24530136378902,-2.51370921928975,17.1717954325953));
#96048=CARTESIAN_POINT('Ctrl Pts',(2.78794581418191,-0.311235703258245,
17.3308957000825));
#96049=CARTESIAN_POINT('Ctrl Pts',(1.76897742105025,2.17720656108039,17.4899959675698));
#96050=CARTESIAN_POINT('Ctrl Pts',(-0.875358028577435,2.66519377299328,
17.6490962350571));
#96051=CARTESIAN_POINT('Ctrl Pts',(-2.71539937848487,0.704354840347607,
17.8081965025444));
#96052=CARTESIAN_POINT('Ctrl Pts',(-2.06048480498726,-1.90365750444079,
17.9672967700317));
#96053=CARTESIAN_POINT('Ctrl Pts',(0.487638852235446,-2.7625564022455,18.1263970375189));
#96054=CARTESIAN_POINT('Ctrl Pts',(2.58771149622336,-1.08317068743137,18.2854973050062));
#96055=CARTESIAN_POINT('Ctrl Pts',(2.3101500519365,1.5914509930673,18.4445975724935));
#96056=CARTESIAN_POINT('Ctrl Pts',(-0.0900172240013499,2.80381997018001,
18.6036978399808));
#96057=CARTESIAN_POINT('Ctrl Pts',(-2.40747511729362,1.43999065462563,18.7627981074681));
#96058=CARTESIAN_POINT('Ctrl Pts',(-2.51290322523128,-1.24692698519977,
18.9218983749553));
#96059=CARTESIAN_POINT('Ctrl Pts',(-0.309432378410861,-2.78814654008503,
19.0809986424426));
#96060=CARTESIAN_POINT('Ctrl Pts',(2.17835029065068,-1.76756882101353,19.2400989099299));
#96061=CARTESIAN_POINT('Ctrl Pts',(2.66462702877159,0.877081708472472,19.3991991774172));
#96062=CARTESIAN_POINT('Ctrl Pts',(0.702598356729098,2.71585439133226,19.5582994449045));
#96063=CARTESIAN_POINT('Ctrl Pts',(-1.90498983992151,2.05925307711142,19.7173997123917));
#96064=CARTESIAN_POINT('Ctrl Pts',(-2.76224041670033,-0.489425587954166,
19.876499979879));
#96065=CARTESIAN_POINT('Ctrl Pts',(-1.08149671384552,-2.58841155609738,
20.0356002473663));
#96066=CARTESIAN_POINT('Ctrl Pts',(1.59294487880464,-2.30912020884302,20.1947005148536));
#96067=CARTESIAN_POINT('Ctrl Pts',(2.80376116001019,0.0918307324124995,
20.3538007823408));
#96068=CARTESIAN_POINT('Ctrl Pts',(1.43843318435008,2.40840600812187,20.5129010498282));
#96069=CARTESIAN_POINT('Ctrl Pts',(-1.24855208494876,2.51209617987991,20.6720013173154));
#96070=CARTESIAN_POINT('Ctrl Pts',(-2.78834609954504,0.307628924110014,
20.8311015848027));
#96071=CARTESIAN_POINT('Ctrl Pts',(-1.76615948150047,-2.17949310889092,
20.9902018522899));
#96072=CARTESIAN_POINT('Ctrl Pts',(0.878805021433445,-2.66405916978217,
21.1493021197773));
#96073=CARTESIAN_POINT('Ctrl Pts',(2.71630826798053,-0.70084157917304,21.3084023872645));
#96074=CARTESIAN_POINT('Ctrl Pts',(2.05802048773081,1.90632137843475,21.4675026547518));
#96075=CARTESIAN_POINT('Ctrl Pts',(-0.491212118917867,2.76192327555009,
21.6266029222391));
#96076=CARTESIAN_POINT('Ctrl Pts',(-2.589110533089,1.07982228780697,21.7857031897264));
#96077=CARTESIAN_POINT('Ctrl Pts',(-2.30808939971089,-1.59443809812089,
21.9448034572136));
#96078=CARTESIAN_POINT('Ctrl Pts',(0.0936442024055214,-2.80370117686478,
22.1039037247009));
#96079=CARTESIAN_POINT('Ctrl Pts',(2.40933589137447,-1.43687511229467,22.2630039921882));
#96080=CARTESIAN_POINT('Ctrl Pts',(2.51128808357329,1.25017666235613,22.4221042596755));
#96081=CARTESIAN_POINT('Ctrl Pts',(0.305825341110179,2.78854449247846,22.5812045271628));
#96082=CARTESIAN_POINT('Ctrl Pts',(-2.18063501532304,1.76474940310066,22.74030479465));
#96083=CARTESIAN_POINT('Ctrl Pts',(-2.66349019626259,-0.880527966739403,
22.8994050621373));
#96084=CARTESIAN_POINT('Ctrl Pts',(-0.699084508414374,-2.7167610082398,
23.0585053296246));
#96085=CARTESIAN_POINT('Ctrl Pts',(1.90765211942334,-2.05678703736111,23.2176055971119));
#96086=CARTESIAN_POINT('Ctrl Pts',(2.76160497892747,0.49299844437904,23.3767058645991));
#96087=CARTESIAN_POINT('Ctrl Pts',(1.07814741001629,2.5898084269058,23.5358061320864));
#96088=CARTESIAN_POINT('Ctrl Pts',(-1.59593065039136,2.30705762497135,23.6949063995737));
#96089=CARTESIAN_POINT('Ctrl Pts',(-2.80364002076886,-0.0954576332217178,
23.854006667061));
#96090=CARTESIAN_POINT('Ctrl Pts',(-1.43531643911124,-2.4102647666624,24.0131069345482));
#96091=CARTESIAN_POINT('Ctrl Pts',(1.2518007167422,-2.51047893664949,24.1722072020356));
#96092=CARTESIAN_POINT('Ctrl Pts',(2.78874171880229,-0.304021630165937,
24.3313074695228));
#96093=CARTESIAN_POINT('Ctrl Pts',(1.76333858640404,2.18177600946929,24.4904077370101));
#96094=CARTESIAN_POINT('Ctrl Pts',(-0.882250543669541,2.66292010845086,
24.6495080044974));
#96095=CARTESIAN_POINT('Ctrl Pts',(-2.71721261192068,0.697327145188193,
24.8086082719847));
#96096=CARTESIAN_POINT('Ctrl Pts',(-2.05555272651832,-1.90898206233064,
24.9677085394719));
#96097=CARTESIAN_POINT('Ctrl Pts',(0.494784563590454,-2.76128552696561,
25.1268088069592));
#96098=CARTESIAN_POINT('Ctrl Pts',(2.59050523725581,-1.07647208117411,25.2859090744465));
#96099=CARTESIAN_POINT('Ctrl Pts',(2.30602488505606,1.59742253499168,25.4450093419338));
#96100=CARTESIAN_POINT('Ctrl Pts',(-0.0972710241024927,2.80357769174802,
25.6041096094211));
#96101=CARTESIAN_POINT('Ctrl Pts',(-2.41119263359704,1.43375716545184,25.7632098769083));
#96102=CARTESIAN_POINT('Ctrl Pts',(-2.50966873944702,-1.2534242474276,25.9223101443956));
#96103=CARTESIAN_POINT('Ctrl Pts',(-0.302217792031812,-2.78893777843403,
26.0814104118829));
#96104=CARTESIAN_POINT('Ctrl Pts',(2.18291609085233,-1.76192703200078,26.2405106793702));
#96105=CARTESIAN_POINT('Ctrl Pts',(2.66234890658549,0.883972751503175,26.3996109468574));
#96106=CARTESIAN_POINT('Ctrl Pts',(0.695569490229732,2.71766307883422,26.5587112143448));
#96107=CARTESIAN_POINT('Ctrl Pts',(-1.91031120660023,2.05431755571885,26.717811481832));
#96108=CARTESIAN_POINT('Ctrl Pts',(-2.76096491979815,-0.496570475804816,
26.8769117493193));
#96109=CARTESIAN_POINT('Ctrl Pts',(-1.07479630198138,-2.59120096384751,
27.0360120168066));
#96110=CARTESIAN_POINT('Ctrl Pts',(1.59891375129768,-2.30499118039708,27.1951122842938));
#96111=CARTESIAN_POINT('Ctrl Pts',(2.80351418982834,0.0990843742891699,
27.3542125517811));
#96112=CARTESIAN_POINT('Ctrl Pts',(1.43219729196881,2.41211949179022,27.5133128192684));
#96113=CARTESIAN_POINT('Ctrl Pts',(-1.25504725373308,2.50885749230484,27.6724130867557));
#96114=CARTESIAN_POINT('Ctrl Pts',(-2.78913267129164,0.300413827462487,
27.8315133542429));
#96115=CARTESIAN_POINT('Ctrl Pts',(-1.76051474048145,-2.18405525899521,
27.9906136217303));
#96116=CARTESIAN_POINT('Ctrl Pts',(0.885694589519864,-2.66177659090546,
28.1497138892175));
#96117=CARTESIAN_POINT('Ctrl Pts',(2.71811240879197,-0.693811544274251,
28.3088141567048));
#96118=CARTESIAN_POINT('Ctrl Pts',(2.05308152547941,1.91163955167607,28.4679144241921));
#96119=CARTESIAN_POINT('Ctrl Pts',(-0.498356180275029,2.76064315755925,
28.6270146916793));
#96120=CARTESIAN_POINT('Ctrl Pts',(-2.59189560638986,1.0731200731391,28.7861149591667));
#96121=CARTESIAN_POINT('Ctrl Pts',(-2.30395651142684,-1.60040429868549,
28.9452152266539));
#96122=CARTESIAN_POINT('Ctrl Pts',(0.10089768302309,-2.80344951503636,29.1043154941412));
#96123=CARTESIAN_POINT('Ctrl Pts',(2.41304534085417,-1.43063681931478,29.2634157616285));
#96124=CARTESIAN_POINT('Ctrl Pts',(2.50804519556235,1.25666973497962,29.4225160291157));
#96125=CARTESIAN_POINT('Ctrl Pts',(0.298609737212693,2.78932639729359,29.581616296603));
#96126=CARTESIAN_POINT('Ctrl Pts',(-2.18519351342132,1.75910171243692,29.7407165640903));
#96127=CARTESIAN_POINT('Ctrl Pts',(-2.66120316165021,-0.887416056999214,
29.8998168315776));
#96128=CARTESIAN_POINT('Ctrl Pts',(-0.692053308057238,-2.71856060160596,
30.0589170990649));
#96129=CARTESIAN_POINT('Ctrl Pts',(1.91296709700241,-2.05184463631711,30.2180173665521));
#96130=CARTESIAN_POINT('Ctrl Pts',(2.76032024038351,0.500141676254002,30.3771176340394));
#96131=CARTESIAN_POINT('Ctrl Pts',(1.07144339534857,2.59258916459223,30.5362179015267));
#96132=CARTESIAN_POINT('Ctrl Pts',(-1.60189417653155,2.30292087857821,30.695318169014));
#96133=CARTESIAN_POINT('Ctrl Pts',(-2.80338366739918,-0.102710949545695,
30.8544184365013));
#96134=CARTESIAN_POINT('Ctrl Pts',(-1.42907574814251,-2.41397018040158,
31.0135187039885));
#96135=CARTESIAN_POINT('Ctrl Pts',(1.25829169048848,-2.50723184955934,31.1726189714758));
#96136=CARTESIAN_POINT('Ctrl Pts',(2.78951895635884,-0.296805522037135,
31.3317192389631));
#96137=CARTESIAN_POINT('Ctrl Pts',(1.75768794845828,2.18633085365451,31.4908195064504));
#96138=CARTESIAN_POINT('Ctrl Pts',(-0.889137153221077,2.66062861905961,
31.6499197739376));
#96139=CARTESIAN_POINT('Ctrl Pts',(-2.71900765708865,0.690294782314285,
31.809020041425));
#96140=CARTESIAN_POINT('Ctrl Pts',(-2.05060688874944,-1.91429384202386,
31.9681203089122));
#96141=CARTESIAN_POINT('Ctrl Pts',(0.501926962994743,-2.75999616840604,
32.1272205763995));
#96142=CARTESIAN_POINT('Ctrl Pts',(2.59328163816445,-1.06976626931127,32.2863208438868));
#96143=CARTESIAN_POINT('Ctrl Pts',(2.30188428228449,1.60338338421251,32.445421111374));
#96144=CARTESIAN_POINT('Ctrl Pts',(-0.104524173098342,2.80331664694433,
32.6045213788614));
#96145=CARTESIAN_POINT('Ctrl Pts',(-2.4148940100455,1.42751407910515,32.7636216463486));
#96146=CARTESIAN_POINT('Ctrl Pts',(-2.50641745463613,-1.25991311958106,
32.9227219138359));
#96147=CARTESIAN_POINT('Ctrl Pts',(-0.295001182690674,-2.78971034840684,
33.0818221813231));
#96148=CARTESIAN_POINT('Ctrl Pts',(2.18746727921893,-1.75627344913702,33.2409224488105));
#96149=CARTESIAN_POINT('Ctrl Pts',(2.66005296337403,0.890857877465394,33.4000227162977));
#96150=CARTESIAN_POINT('Ctrl Pts',(0.688535967781046,2.71945357505306,33.559122983785));
#96151=CARTESIAN_POINT('Ctrl Pts',(-1.9156197861854,2.04936828329418,33.7182232512723));
#96152=CARTESIAN_POINT('Ctrl Pts',(-2.75967094176237,-0.503712039750395,
33.8773235187596));
#96153=CARTESIAN_POINT('Ctrl Pts',(-1.06808869572879,-2.59397302681686,
34.0364237862468));
#96154=CARTESIAN_POINT('Ctrl Pts',(1.60487192110541,-2.30084672297929,34.1955240537341));
#96155=CARTESIAN_POINT('Ctrl Pts',(2.80324845369984,0.106337352922497,34.3546243212214));
#96156=CARTESIAN_POINT('Ctrl Pts',(1.425951812856,2.41581682939948,34.5137245887086));
#96157=CARTESIAN_POINT('Ctrl Pts',(-1.26153402157907,2.50560201113339,34.672824856196));
#96158=CARTESIAN_POINT('Ctrl Pts',(-2.7899005733575,0.293196719928112,34.8319251236832));
#96159=CARTESIAN_POINT('Ctrl Pts',(-1.75485821506492,-2.18860278963914,
34.9910253911705));
#96160=CARTESIAN_POINT('Ctrl Pts',(0.892578229012262,-2.65947619483432,
35.1501256586578));
#96161=CARTESIAN_POINT('Ctrl Pts',(2.71989835531262,-0.686776865193377,
35.3092259261451));
#96162=CARTESIAN_POINT('Ctrl Pts',(2.04812882046954,1.91694492893226,35.4683261936323));
#96163=CARTESIAN_POINT('Ctrl Pts',(-0.505496905774109,2.75934456058861,
35.6274264611197));
#96164=CARTESIAN_POINT('Ctrl Pts',(-2.59466333026019,1.066410675303,35.7865267286069));
#96165=CARTESIAN_POINT('Ctrl Pts',(-2.29980820109672,-1.60635978658748,
35.9456269960942));
#96166=CARTESIAN_POINT('Ctrl Pts',(0.108150488259582,-2.80317908769424,
36.1047272635815));
#96167=CARTESIAN_POINT('Ctrl Pts',(2.41673863807743,-1.42438895004866,36.2638275310687));
#96168=CARTESIAN_POINT('Ctrl Pts',(2.50478551939227,1.26315439580437,36.422927798556));
#96169=CARTESIAN_POINT('Ctrl Pts',(0.291392134504392,2.79008963113125,36.5820280660433));
#96170=CARTESIAN_POINT('Ctrl Pts',(-2.18973738444013,1.75344224683403,36.7411283335306));
#96171=CARTESIAN_POINT('Ctrl Pts',(-2.65889831368176,-0.894298207142014,
36.9002286010178));
#96172=CARTESIAN_POINT('Ctrl Pts',(-0.685017475287161,-2.72034199768123,
37.0593288685051));
#96173=CARTESIAN_POINT('Ctrl Pts',(1.91826926971012,-2.04688850079404,37.2184291359924));
#96174=CARTESIAN_POINT('Ctrl Pts',(2.75901702502127,0.507281560319236,37.3775294034797));
#96175=CARTESIAN_POINT('Ctrl Pts',(1.06473220873587,2.59535254820565,37.536629670967));
#96176=CARTESIAN_POINT('Ctrl Pts',(-1.60784698003624,2.29876871707125,37.6957299384542));
#96177=CARTESIAN_POINT('Ctrl Pts',(-2.80310854895656,-0.109963578351025,
37.8548302059416));
#96178=CARTESIAN_POINT('Ctrl Pts',(-1.42282549133698,-2.4176594356937,38.0139304734288));
#96179=CARTESIAN_POINT('Ctrl Pts',(1.26477424157903,-2.50396797975438,38.1730307409161));
#96180=CARTESIAN_POINT('Ctrl Pts',(2.79027752164898,-0.289587427174506,
38.3321310084034));
#96181=CARTESIAN_POINT('Ctrl Pts',(1.75202554503676,2.1908710631472,38.4912312758906));
#96182=CARTESIAN_POINT('Ctrl Pts',(-0.896017811135028,2.6583193201581,38.650331543378));
#96183=CARTESIAN_POINT('Ctrl Pts',(-2.72078450197331,0.683257798798514,
38.8094318108652));
#96184=CARTESIAN_POINT('Ctrl Pts',(-2.04564732478662,-1.91959280796486,
38.9685320783525));
#96185=CARTESIAN_POINT('Ctrl Pts',(0.509066002639091,-2.75868833519739,
39.1276323458398));
#96186=CARTESIAN_POINT('Ctrl Pts',(2.5960406803649,-1.06305329672964,39.286732613327));
#96187=CARTESIAN_POINT('Ctrl Pts',(2.29772827133774,1.60933350082956,39.4458328808143));
#96188=CARTESIAN_POINT('Ctrl Pts',(-0.111776622438346,2.80303683751629,
39.6049331483016));
#96189=CARTESIAN_POINT('Ctrl Pts',(-2.41857922186304,1.42126143737506,39.7640334157889));
#96190=CARTESIAN_POINT('Ctrl Pts',(-2.50314939256176,-1.26639355822537,
39.9231336832761));
#96191=CARTESIAN_POINT('Ctrl Pts',(-0.287782598693457,-2.79046424483211,
40.0822339507635));
#96192=CARTESIAN_POINT('Ctrl Pts',(2.19200382528608,-1.7506081102658,40.2413342182507));
#96193=CARTESIAN_POINT('Ctrl Pts',(2.65773921450559,0.897737040271954,40.400434485738));
#96194=CARTESIAN_POINT('Ctrl Pts',(0.681497836463564,2.72122586800371,40.5595347532253));
#96195=CARTESIAN_POINT('Ctrl Pts',(-1.92091554314286,2.04440529296648,40.7186350207125));
#96196=CARTESIAN_POINT('Ctrl Pts',(-2.7583584912545,-0.510850231987242,
40.8777352881999));
#96197=CARTESIAN_POINT('Ctrl Pts',(-1.0613739399866,-2.59672772645004,41.036835555687));
#96198=CARTESIAN_POINT('Ctrl Pts',(1.6108193483455,-2.29668686433149,41.1959358231744));
#96199=CARTESIAN_POINT('Ctrl Pts',(2.80296395340346,0.113589619763061,41.3550360906616));
#96200=CARTESIAN_POINT('Ctrl Pts',(1.41969678881716,2.41949799620072,41.514136358149));
#96201=CARTESIAN_POINT('Ctrl Pts',(-1.2680123450661,2.50232975815682,41.6732366256362));
#96202=CARTESIAN_POINT('Ctrl Pts',(-2.79064980060251,0.285977649816169,
41.8323368931235));
#96203=CARTESIAN_POINT('Ctrl Pts',(-1.74918994311403,-2.19313567038289,
41.9914371606108));
#96204=CARTESIAN_POINT('Ctrl Pts',(0.899455893833502,-2.65715799696691,
42.1505374280981));
#96205=CARTESIAN_POINT('Ctrl Pts',(2.72166609558782,-0.679737589018599,
42.3096376955853));
#96206=CARTESIAN_POINT('Ctrl Pts',(2.04316240585326,1.92223747469062,42.4687379630726));
#96207=CARTESIAN_POINT('Ctrl Pts',(-0.512634247617058,2.75802749333056,
42.6278382305599));
#96208=CARTESIAN_POINT('Ctrl Pts',(-2.59741368617366,1.05969413920951,42.7869384980472));
#96209=CARTESIAN_POINT('Ctrl Pts',(-2.29564449648816,-1.61230452196248,
42.9460387655344));
#96210=CARTESIAN_POINT('Ctrl Pts',(0.11540256956664,-2.80288989664852,43.1051390330218));
#96211=CARTESIAN_POINT('Ctrl Pts',(2.42041575832236,-1.41813154631793,43.2642393005089));
#96212=CARTESIAN_POINT('Ctrl Pts',(2.50150907688241,1.26963060142386,43.4233395679963));
#96213=CARTESIAN_POINT('Ctrl Pts',(0.284172581298068,2.79083418888245,43.5824398354835));
#96214=CARTESIAN_POINT('Ctrl Pts',(-2.19426659796431,1.74777104417508,43.7415401029709));
#96215=CARTESIAN_POINT('Ctrl Pts',(-2.65657566778475,-0.901174371100898,
43.900640370458));
#96216=CARTESIAN_POINT('Ctrl Pts',(-0.677977057200952,-2.72210518454085,
44.0597406379455));
#96217=CARTESIAN_POINT('Ctrl Pts',(1.92355860205693,-2.04191866396806,44.2188409054326));
#96218=CARTESIAN_POINT('Ctrl Pts',(2.75769534156078,0.514418048784537,44.37794117292));
#96219=CARTESIAN_POINT('Ctrl Pts',(1.05801389510723,2.59809855924461,44.5370414404072));
#96220=CARTESIAN_POINT('Ctrl Pts',(-1.61378902107108,2.29460116825178,44.6961417078945));
#96221=CARTESIAN_POINT('Ctrl Pts',(-2.8028146672597,-0.117215471105793,
44.8552419753818));
#96222=CARTESIAN_POINT('Ctrl Pts',(-1.41656571057567,-2.42133250781507,
45.014342242869));
#96223=CARTESIAN_POINT('Ctrl Pts',(1.27124832670454,-2.50068734913707,45.1734425103564));
#96224=CARTESIAN_POINT('Ctrl Pts',(2.79101740943663,-0.282367393789022,
45.3325427778436));
#96225=CARTESIAN_POINT('Ctrl Pts',(1.74635141434428,2.19539660735637,45.4916430453309));
#96226=CARTESIAN_POINT('Ctrl Pts',(-0.902892471930827,2.65599222758591,
45.6507433128183));
#96227=CARTESIAN_POINT('Ctrl Pts',(-2.72254313358101,0.676216241016185,
45.8098435803054));
#96228=CARTESIAN_POINT('Ctrl Pts',(-2.04067406992595,-1.92487892329463,
45.9689438477928));
#96229=CARTESIAN_POINT('Ctrl Pts',(0.516201638739318,-2.75736203874416,
46.12804411528));
#96230=CARTESIAN_POINT('Ctrl Pts',(2.59878233775354,-1.05633320330836,46.2871443827674));
#96231=CARTESIAN_POINT('Ctrl Pts',(2.29355689460039,1.61527283537019,46.4462446502545));
#96232=CARTESIAN_POINT('Ctrl Pts',(-0.119028351361985,2.80273828373448,
46.6053449177419));
#96233=CARTESIAN_POINT('Ctrl Pts',(-2.42224819137782,1.41499924701908,46.7644451852291));
#96234=CARTESIAN_POINT('Ctrl Pts',(-2.49986467621169,-1.27286545303251,
46.9235454527165));
#96235=CARTESIAN_POINT('Ctrl Pts',(-0.280561895474226,-2.79119959037926,
47.0826457202037));
#96236=CARTESIAN_POINT('Ctrl Pts',(2.19652533073393,-1.74493080967452,47.241745987691));
#96237=CARTESIAN_POINT('Ctrl Pts',(2.65540837738748,0.904609729110513,47.4008462551782));
#96238=CARTESIAN_POINT('Ctrl Pts',(0.674453804384293,2.72298083242374,47.5599465226655));
#96239=CARTESIAN_POINT('Ctrl Pts',(-1.92619588769776,2.03942692664895,47.7190467901528));
#96240=CARTESIAN_POINT('Ctrl Pts',(-2.7570324497735,-0.517981778342401,
47.8781470576401));
#96241=CARTESIAN_POINT('Ctrl Pts',(-1.05464278435862,-2.59947119907506,
48.0372473251273));
#96242=CARTESIAN_POINT('Ctrl Pts',(1.61673826111253,-2.29249989126509,48.1963475926147));
#96243=CARTESIAN_POINT('Ctrl Pts',(2.80269451719685,0.120818728651149,48.3554478601019));
#96244=CARTESIAN_POINT('Ctrl Pts',(1.41336773306382,2.42320569438391,48.5145481275892));
#96245=CARTESIAN_POINT('Ctrl Pts',(-1.27435908006578,2.49895924442061,48.6736483950764));
#96246=CARTESIAN_POINT('Ctrl Pts',(-2.79161521279367,0.27891219154285,48.8327486625638));
#96247=CARTESIAN_POINT('Ctrl Pts',(-1.74306162992693,-2.19795085039717,
48.991848930051));
#96248=CARTESIAN_POINT('Ctrl Pts',(0.905469678109174,-2.65425291543538,
49.1509491975383));
#96249=CARTESIAN_POINT('Ctrl Pts',(2.72507495425543,-0.67380191912698,49.3100494650256));
#96250=CARTESIAN_POINT('Ctrl Pts',(2.03481676979323,1.92982725944834,49.4691497325128));
#96251=CARTESIAN_POINT('Ctrl Pts',(0.337182413353676,2.47711500076564,49.5752165775044));
#96252=CARTESIAN_POINT('Ctrl Pts',(-0.43944522199609,2.33068358199152,49.6282500000002));
#96253=CARTESIAN_POINT('Ctrl Pts',(-1.12236674703393,2.30288577939295,-0.219489327336945));
#96254=CARTESIAN_POINT('Ctrl Pts',(-1.889731631375,1.92889205520008,-0.166455904841186));
#96255=CARTESIAN_POINT('Ctrl Pts',(-3.00772136534351,0.359822456008,-0.0603890598496661));
#96256=CARTESIAN_POINT('Ctrl Pts',(-1.92664562308743,-2.34132064310475,
0.0987112076376125));
#96257=CARTESIAN_POINT('Ctrl Pts',(0.927249804294889,-2.88380409372784,
0.257811475124891));
#96258=CARTESIAN_POINT('Ctrl Pts',(2.92784522127986,-0.780306587535148,
0.416911742612171));
#96259=CARTESIAN_POINT('Ctrl Pts',(2.23897820574364,2.04207354288632,0.576012010099449));
#96260=CARTESIAN_POINT('Ctrl Pts',(-0.507463326542365,2.98715522008745,
0.735112277586729));
#96261=CARTESIAN_POINT('Ctrl Pts',(-2.78744873331352,1.188114072284,0.894212545074006));
#96262=CARTESIAN_POINT('Ctrl Pts',(-2.50637764055038,-1.70286310223525,
1.05331281256129));
#96263=CARTESIAN_POINT('Ctrl Pts',(0.0776488068570673,-3.02907538336238,
1.21241308004856));
#96264=CARTESIAN_POINT('Ctrl Pts',(2.59030281306776,-1.57219671546807,1.37151334753584));
#96265=CARTESIAN_POINT('Ctrl Pts',(2.72295613408236,1.32928328733925,1.53061361502312));
#96266=CARTESIAN_POINT('Ctrl Pts',(0.353702731598795,3.00937394922191,1.6897138825104));
#96267=CARTESIAN_POINT('Ctrl Pts',(-2.34053491620105,1.9244107020416,1.84881414999768));
#96268=CARTESIAN_POINT('Ctrl Pts',(-2.88425066053474,-0.928740121585945,
2.00791441748496));
#96269=CARTESIAN_POINT('Ctrl Pts',(-0.777865918911568,-2.92854544993387,
2.16701468497224));
#96270=CARTESIAN_POINT('Ctrl Pts',(2.04323491749396,-2.2375541324242,2.32611495245952));
#96271=CARTESIAN_POINT('Ctrl Pts',(2.98697646298292,0.509341455803217,2.48521521994679));
#96272=CARTESIAN_POINT('Ctrl Pts',(1.18623220564852,2.78824487032034,2.64431548743408));
#96273=CARTESIAN_POINT('Ctrl Pts',(-1.7044426413725,2.50526089027857,2.80341575492135));
#96274=CARTESIAN_POINT('Ctrl Pts',(-3.02904614676457,-0.0796002539131367,
2.96251602240864));
#96275=CARTESIAN_POINT('Ctrl Pts',(-1.57050962970762,-2.59132324542585,
3.12161628989591));
#96276=CARTESIAN_POINT('Ctrl Pts',(1.33103829202283,-2.72209364370382,3.28071655738319));
#96277=CARTESIAN_POINT('Ctrl Pts',(3.00960521121801,-0.351757294752259,
3.43981682487047));
#96278=CARTESIAN_POINT('Ctrl Pts',(1.92289479510493,2.34177973278295,3.59891709235775));
#96279=CARTESIAN_POINT('Ctrl Pts',(-0.93060462174736,2.88364903544351,3.75801735984503));
#96280=CARTESIAN_POINT('Ctrl Pts',(-2.92904841423869,0.775971716819205,
3.91711762733231));
#96281=CARTESIAN_POINT('Ctrl Pts',(-2.23623185283338,-2.04468183767635,
4.07621789481958));
#96282=CARTESIAN_POINT('Ctrl Pts',(0.511273219910781,-2.98664634887032,
4.23531816230686));
#96283=CARTESIAN_POINT('Ctrl Pts',(2.78901161367073,-1.18442852753634,4.39441842979414));
#96284=CARTESIAN_POINT('Ctrl Pts',(2.50415788883102,1.70606271447192,4.55351869728142));
#96285=CARTESIAN_POINT('Ctrl Pts',(-0.0815594243589275,3.02899402086515,
4.7126189647687));
#96286=CARTESIAN_POINT('Ctrl Pts',(-2.59233852754708,1.56883322142171,4.87171923225597));
#96287=CARTESIAN_POINT('Ctrl Pts',(-2.72123214602623,-1.33279868152171,
5.03081949974326));
#96288=CARTESIAN_POINT('Ctrl Pts',(-0.349810593385746,-3.00983209944,5.18991976723053));
#96289=CARTESIAN_POINT('Ctrl Pts',(2.34302298393151,-1.92137971645832,5.34902003471782));
#96290=CARTESIAN_POINT('Ctrl Pts',(2.88304651100131,0.932469588486375,5.50812030220509));
#96291=CARTESIAN_POINT('Ctrl Pts',(0.774077029136096,2.92954970447966,5.66722056969238));
#96292=CARTESIAN_POINT('Ctrl Pts',(-2.04612781807473,2.23490887289647,5.82632083717965));
#96293=CARTESIAN_POINT('Ctrl Pts',(-2.98631502950102,-0.513204893416967,
5.98542110466694));
#96294=CARTESIAN_POINT('Ctrl Pts',(-1.18262433072315,-2.78977712558423,
6.14452137215421));
#96295=CARTESIAN_POINT('Ctrl Pts',(1.7076820616722,-2.50305387362997,6.30362163964149));
#96296=CARTESIAN_POINT('Ctrl Pts',(3.0289406341336,0.0835185784442948,6.46272190712876));
#96297=CARTESIAN_POINT('Ctrl Pts',(1.56715615346209,2.59335271583274,6.62182217461605));
#96298=CARTESIAN_POINT('Ctrl Pts',(-1.33455851168292,2.72036951478026,6.78092244210331));
#96299=CARTESIAN_POINT('Ctrl Pts',(-3.01005772939279,0.347863743114754,
6.94002270959062));
#96300=CARTESIAN_POINT('Ctrl Pts',(-1.91986383350621,-2.34426525351674,
7.09912297707787));
#96301=CARTESIAN_POINT('Ctrl Pts',(0.934334164867162,-2.88244278111692,
7.25822324456517));
#96302=CARTESIAN_POINT('Ctrl Pts',(2.93004976925262,-0.772182017243212,
7.41732351205244));
#96303=CARTESIAN_POINT('Ctrl Pts',(2.23358495789849,2.0475729422662,7.57642377953972));
#96304=CARTESIAN_POINT('Ctrl Pts',(-0.515136352183505,2.98598246088455,
7.735524047027));
#96305=CARTESIAN_POINT('Ctrl Pts',(-2.7905414703915,1.18081963909664,7.89462431451428));
#96306=CARTESIAN_POINT('Ctrl Pts',(-2.50194881124659,-1.7093006944224,8.05372458200156));
#96307=CARTESIAN_POINT('Ctrl Pts',(0.0854776975837867,-3.02888598023545,
8.21282484948884));
#96308=CARTESIAN_POINT('Ctrl Pts',(2.59436581917158,-1.56547842986266,8.37192511697612));
#96309=CARTESIAN_POINT('Ctrl Pts',(2.71950574544478,1.33631778351705,8.53102538446339));
#96310=CARTESIAN_POINT('Ctrl Pts',(0.34591674731299,3.01028210006628,8.69012565195066));
#96311=CARTESIAN_POINT('Ctrl Pts',(-2.34550654236051,1.91834714736283,8.84922591943796));
#96312=CARTESIAN_POINT('Ctrl Pts',(-2.88183784533965,-0.936198350361311,
9.00832618692522));
#96313=CARTESIAN_POINT('Ctrl Pts',(-0.770286682302,-2.93054860821643,9.16742645441252));
#96314=CARTESIAN_POINT('Ctrl Pts',(2.04901720983943,-2.23226010846248,9.32652672189978));
#96315=CARTESIAN_POINT('Ctrl Pts',(2.98564864305873,0.517067595438605,9.48562698938708));
#96316=CARTESIAN_POINT('Ctrl Pts',(1.17901445346493,2.79130464775379,9.64472725687434));
#96317=CARTESIAN_POINT('Ctrl Pts',(-1.71091861207316,2.50084270215316,9.80382752436164));
#96318=CARTESIAN_POINT('Ctrl Pts',(-3.02883005917894,-0.0874367809629802,
9.96292779184889));
#96319=CARTESIAN_POINT('Ctrl Pts',(-1.563800051333,-2.59537783713701,10.1220280593362));
#96320=CARTESIAN_POINT('Ctrl Pts',(1.33807649629206,-2.71864083838264,10.2811283268235));
#96321=CARTESIAN_POINT('Ctrl Pts',(3.01050521136452,-0.343969606794242,
10.4402285943107));
#96322=CARTESIAN_POINT('Ctrl Pts',(1.91682965866379,2.34674684994312,10.599328861798));
#96323=CARTESIAN_POINT('Ctrl Pts',(-0.938062144189482,2.88123170392277,
10.7584291292853));
#96324=CARTESIAN_POINT('Ctrl Pts',(-2.93104622116212,0.768391025105277,
10.9175293967726));
#96325=CARTESIAN_POINT('Ctrl Pts',(-2.23093432514284,-2.05046062019015,
11.0766296642599));
#96326=CARTESIAN_POINT('Ctrl Pts',(0.518998622374394,-2.98531357616324,
11.2357299317471));
#96327=CARTESIAN_POINT('Ctrl Pts',(2.79206665735174,-1.17720877458324,11.3948301992344));
#96328=CARTESIAN_POINT('Ctrl Pts',(2.49973554681248,1.71253581394761,11.5539304667217));
#96329=CARTESIAN_POINT('Ctrl Pts',(-0.0893958277622967,3.02877287098748,
11.713030734209));
#96330=CARTESIAN_POINT('Ctrl Pts',(-2.59638876930565,1.56212101857525,11.8721310016962));
#96331=CARTESIAN_POINT('Ctrl Pts',(-2.71777479395565,-1.33983464927223,
12.0312312691835));
#96332=CARTESIAN_POINT('Ctrl Pts',(-0.342022322373068,-3.01072706319415,
12.1903315366708));
#96333=CARTESIAN_POINT('Ctrl Pts',(2.34798617574567,-1.91531136804392,12.3494318041581));
#96334=CARTESIAN_POINT('Ctrl Pts',(2.88062435711988,0.939925545571957,12.5085320716454));
#96335=CARTESIAN_POINT('Ctrl Pts',(0.766495046446107,2.93154260788151,12.6676323391327));
#96336=CARTESIAN_POINT('Ctrl Pts',(-2.05190317271449,2.22960760849421,12.8267326066199));
#96337=CARTESIAN_POINT('Ctrl Pts',(-2.98497726033827,-0.520929432183016,
12.9858328741072));
#96338=CARTESIAN_POINT('Ctrl Pts',(-1.17540260320696,-2.79282749886659,
13.1449331415945));
#96339=CARTESIAN_POINT('Ctrl Pts',(1.71415229936921,-2.49862734568769,13.3040334090818));
#96340=CARTESIAN_POINT('Ctrl Pts',(3.02871441568501,0.0913548371621723,
13.463133676569));
#96341=CARTESIAN_POINT('Ctrl Pts',(1.56044133229185,2.59739861525457,13.6222339440563));
#96342=CARTESIAN_POINT('Ctrl Pts',(-1.34159224172202,2.71690761252612,13.7813342115436));
#96343=CARTESIAN_POINT('Ctrl Pts',(-3.01094765546235,0.34007489486417,13.9404344790309));
#96344=CARTESIAN_POINT('Ctrl Pts',(-1.91379227613845,-2.34922451924968,
14.0995347465181));
#96345=CARTESIAN_POINT('Ctrl Pts',(0.941788553729176,-2.88001580518507,
14.2586350140054));
#96346=CARTESIAN_POINT('Ctrl Pts',(2.9320377681669,-0.764598747117689,14.4177352814927));
#96347=CARTESIAN_POINT('Ctrl Pts',(2.22827995907167,2.05334486680895,14.57683554898));
#96348=CARTESIAN_POINT('Ctrl Pts',(-0.522860024056705,2.98463969572451,
14.7359358164673));
#96349=CARTESIAN_POINT('Ctrl Pts',(-2.79358717198003,1.17359594009171,14.8950360839545));
#96350=CARTESIAN_POINT('Ctrl Pts',(-2.49751809924244,-1.71576806766168,
15.0541363514418));
#96351=CARTESIAN_POINT('Ctrl Pts',(0.0933138083430479,-3.02865469329595,
15.2132366189291));
#96352=CARTESIAN_POINT('Ctrl Pts',(2.59840737456129,-1.55876099318549,15.3723368864164));
#96353=CARTESIAN_POINT('Ctrl Pts',(2.71603929445686,1.34334927290609,15.5314371539037));
#96354=CARTESIAN_POINT('Ctrl Pts',(0.338127325082262,3.01116698807685,15.6905374213909));
#96355=CARTESIAN_POINT('Ctrl Pts',(-2.35046187993708,1.91227238358288,15.8496376888782));
#96356=CARTESIAN_POINT('Ctrl Pts',(-2.87940604837291,-0.943651167881714,
16.0087379563655));
#96357=CARTESIAN_POINT('Ctrl Pts',(-0.762702127913354,-2.93253170181117,
16.1678382238528));
#96358=CARTESIAN_POINT('Ctrl Pts',(2.05478570187039,-2.22695137743062,16.32693849134));
#96359=CARTESIAN_POINT('Ctrl Pts',(2.98430088246319,0.52479039718779,16.4860387588273));
#96360=CARTESIAN_POINT('Ctrl Pts',(1.17178878599336,2.79434567637422,16.6451390263146));
#96361=CARTESIAN_POINT('Ctrl Pts',(-1.71738311814903,2.4964078079408,16.8042392938019));
#96362=CARTESIAN_POINT('Ctrl Pts',(-3.02859370384532,-0.0952727404853469,
16.9633395612892));
#96363=CARTESIAN_POINT('Ctrl Pts',(-1.55708000195918,-2.59941504680378,
17.1224398287764));
#96364=CARTESIAN_POINT('Ctrl Pts',(1.3451057420894,-2.71516984011115,17.2815400962637));
#96365=CARTESIAN_POINT('Ctrl Pts',(3.01138506094589,-0.336179613842111,
17.440640363751));
#96366=CARTESIAN_POINT('Ctrl Pts',(1.91075169101307,2.3516982572902,17.5997406312383));
#96367=CARTESIAN_POINT('Ctrl Pts',(-0.945513387250341,2.87879508693854,
17.7588408987256));
#96368=CARTESIAN_POINT('Ctrl Pts',(-2.93302440860768,0.760805189626565,
17.9179411662128));
#96369=CARTESIAN_POINT('Ctrl Pts',(-2.22562186412688,-2.05622567729603,
18.0770414337001));
#96370=CARTESIAN_POINT('Ctrl Pts',(0.526720550768654,-2.98396082069605,
18.2361417011874));
#96371=CARTESIAN_POINT('Ctrl Pts',(2.79510301173186,-1.16998114166793,18.3952419686747));
#96372=CARTESIAN_POINT('Ctrl Pts',(2.49529647224726,1.71899745015561,18.554342236162));
#96373=CARTESIAN_POINT('Ctrl Pts',(-0.0972316327695509,3.02853144735862,
18.7134425036492));
#96374=CARTESIAN_POINT('Ctrl Pts',(-2.60042163156048,1.55539835931616,18.8725427711365));
#96375=CARTESIAN_POINT('Ctrl Pts',(-2.7142992498527,-1.34686164853714,19.0316430386238));
#96376=CARTESIAN_POINT('Ctrl Pts',(-0.334231761958541,-3.01160187397823,
19.1907433061111));
#96377=CARTESIAN_POINT('Ctrl Pts',(2.35293365079182,-1.90923019906519,19.3498435735984));
#96378=CARTESIAN_POINT('Ctrl Pts',(2.87818292113752,0.947375211056012,19.5089438410856));
#96379=CARTESIAN_POINT('Ctrl Pts',(0.758907933050889,2.93351588835028,19.6680441085729));
#96380=CARTESIAN_POINT('Ctrl Pts',(-2.05766479248342,2.22429141971667,19.8271443760602));
#96381=CARTESIAN_POINT('Ctrl Pts',(-2.98361951056537,-0.528650483991836,
19.9862446435475));
#96382=CARTESIAN_POINT('Ctrl Pts',(-1.16817300787164,-2.79585917773611,
20.1453449110348));
#96383=CARTESIAN_POINT('Ctrl Pts',(1.72061106300608,-2.49418409262673,20.304445178522));
#96384=CARTESIAN_POINT('Ctrl Pts',(3.02846792386189,0.0991904843761558,
20.4635454460093));
#96385=CARTESIAN_POINT('Ctrl Pts',(1.55371606595995,2.60142712841028,20.6226457134966));
#96386=CARTESIAN_POINT('Ctrl Pts',(-1.34861699151466,2.71342752404575,20.7817459809838));
#96387=CARTESIAN_POINT('Ctrl Pts',(-3.01181742708317,0.332283770246491,
20.9408462484712));
#96388=CARTESIAN_POINT('Ctrl Pts',(-1.90770790837581,-2.35416805992508,
21.0999465159584));
#96389=CARTESIAN_POINT('Ctrl Pts',(0.949236638519778,-2.87756955122596,
21.2590467834457));
#96390=CARTESIAN_POINT('Ctrl Pts',(2.93400614083337,-0.757010358980113,
21.418147050933));
#96391=CARTESIAN_POINT('Ctrl Pts',(2.22296004475659,2.05910304683056,21.5772473184203));
#96392=CARTESIAN_POINT('Ctrl Pts',(-0.530580196049953,2.98327695221391,
21.7363475859076));
#96393=CARTESIAN_POINT('Ctrl Pts',(-2.79661417407061,1.16636438536093,21.8954478533948));
#96394=CARTESIAN_POINT('Ctrl Pts',(-2.49307066954462,-1.72222395602531,
22.0545481208821));
#96395=CARTESIAN_POINT('Ctrl Pts',(0.101149294485621,-3.02840313338171,
22.2136483883694));
#96396=CARTESIAN_POINT('Ctrl Pts',(2.60243153693252,-1.55203312259438,22.3727486558567));
#96397=CARTESIAN_POINT('Ctrl Pts',(2.71255466305499,1.35037177028763,22.5318489233439));
#96398=CARTESIAN_POINT('Ctrl Pts',(0.330335639520905,3.01203172017053,22.6909491908313));
#96399=CARTESIAN_POINT('Ctrl Pts',(-2.35540148417356,1.90618481958177,22.8500494583184));
#96400=CARTESIAN_POINT('Ctrl Pts',(-2.87695497746049,-0.951097668862907,
23.0091497258058));
#96401=CARTESIAN_POINT('Ctrl Pts',(-0.755112468208078,-2.93449516585184,
23.168249993293));
#96402=CARTESIAN_POINT('Ctrl Pts',(2.06054043973563,-2.22162773980366,23.3273502607804));
#96403=CARTESIAN_POINT('Ctrl Pts',(2.98293314578502,0.532509686135592,23.4864505282676));
#96404=CARTESIAN_POINT('Ctrl Pts',(1.16455527489253,2.79736800041952,23.6455507957549));
#96405=CARTESIAN_POINT('Ctrl Pts',(-1.72383612853853,2.49195620346673,23.8046510632421));
#96406=CARTESIAN_POINT('Ctrl Pts',(-3.0283370759452,-0.103108062278441,
23.9637513307295));
#96407=CARTESIAN_POINT('Ctrl Pts',(-1.55034952992354,-2.603434856707,24.1228515982167));
#96408=CARTESIAN_POINT('Ctrl Pts',(1.35212598412189,-2.71168066724558,24.281951865704));
#96409=CARTESIAN_POINT('Ctrl Pts',(3.01224475315065,-0.328387370596837,
24.4410521331913));
#96410=CARTESIAN_POINT('Ctrl Pts',(1.90466093332031,2.35663392302125,24.6001524006786));
#96411=CARTESIAN_POINT('Ctrl Pts',(-0.952958301306824,2.87633920009819,
24.7592526681658));
#96412=CARTESIAN_POINT('Ctrl Pts',(-2.93498296320111,0.75321426152879,24.9183529356531));
#96413=CARTESIAN_POINT('Ctrl Pts',(-2.22029450541524,-2.06197697059738,
25.0774532031404));
#96414=CARTESIAN_POINT('Ctrl Pts',(0.534438953441636,-2.9825880914225,25.2365534706277));
#96415=CARTESIAN_POINT('Ctrl Pts',(2.79812065646745,-1.16274567722322,25.395653738115));
#96416=CARTESIAN_POINT('Ctrl Pts',(2.4908406948593,1.72544757987134,25.5547540056022));
#96417=CARTESIAN_POINT('Ctrl Pts',(-0.105066786935228,3.02826975157997,
25.7138542730895));
#96418=CARTESIAN_POINT('Ctrl Pts',(-2.60443708731396,1.54866528865171,25.8729545405768));
#96419=CARTESIAN_POINT('Ctrl Pts',(-2.71080553698318,-1.3538796322836,26.0320548080641));
#96420=CARTESIAN_POINT('Ctrl Pts',(-0.326438964289283,-3.01245652593442,
26.1911550755514));
#96421=CARTESIAN_POINT('Ctrl Pts',(2.35786537595255,-1.90313625022889,26.3502553430386));
#96422=CARTESIAN_POINT('Ctrl Pts',(2.8757222193967,0.954818535073085,26.5093556105259));
#96423=CARTESIAN_POINT('Ctrl Pts',(0.751315739736407,2.93546953267709,26.6684558780132));
#96424=CARTESIAN_POINT('Ctrl Pts',(-2.06341263881479,2.21896034214911,26.8275561455005));
#96425=CARTESIAN_POINT('Ctrl Pts',(-2.98224178927072,-0.536367997160897,
26.9866564129878));
#96426=CARTESIAN_POINT('Ctrl Pts',(-1.16093559311012,-2.79887214189952,
27.145756680475));
#96427=CARTESIAN_POINT('Ctrl Pts',(1.72705830934953,-2.48972414418904,27.3048569479623));
#96428=CARTESIAN_POINT('Ctrl Pts',(3.02820116031421,0.107025467636496,27.4639572154496));
#96429=CARTESIAN_POINT('Ctrl Pts',(1.54698039948354,2.60543822833412,27.6230574829369));
#96430=CARTESIAN_POINT('Ctrl Pts',(-1.35563271403909,2.70992927263389,27.7821577504241));
#96431=CARTESIAN_POINT('Ctrl Pts',(-3.01266703843323,0.324490421413414,
27.9412580179114));
#96432=CARTESIAN_POINT('Ctrl Pts',(-1.90161077094541,-2.35909584245226,
28.1003582853987));
#96433=CARTESIAN_POINT('Ctrl Pts',(0.956678369383513,-2.87510403561414,
28.2594585528859));
#96434=CARTESIAN_POINT('Ctrl Pts',(2.93595487407624,-0.749416903625118,
28.4185588203733));
#96435=CARTESIAN_POINT('Ctrl Pts',(2.21762525056339,2.06484744378726,28.5776590878605));
#96436=CARTESIAN_POINT('Ctrl Pts',(-0.538296816486407,2.98189423947457,
28.7367593553478));
#96437=CARTESIAN_POINT('Ctrl Pts',(-2.79962245640135,1.15912502331042,28.8958596228351));
#96438=CARTESIAN_POINT('Ctrl Pts',(-2.48860655192302,-1.72866831629926,
29.0549598903224));
#96439=CARTESIAN_POINT('Ctrl Pts',(0.10898410356279,-3.02813130217658,29.2140601578096));
#96440=CARTESIAN_POINT('Ctrl Pts',(2.60643827934863,-1.54529486312395,29.3731604252969));
#96441=CARTESIAN_POINT('Ctrl Pts',(2.70905187456434,1.35738522865492,29.5322606927842));
#96442=CARTESIAN_POINT('Ctrl Pts',(0.322541742784441,3.01287629055901,29.6913609602715));
#96443=CARTESIAN_POINT('Ctrl Pts',(-2.3603253220056,1.90008449610808,29.8504612277587));
#96444=CARTESIAN_POINT('Ctrl Pts',(-2.87448464900915,-0.958537803459974,
30.0095614952461));
#96445=CARTESIAN_POINT('Ctrl Pts',(-0.747517753989358,-2.93643898719551,
30.1686617627333));
#96446=CARTESIAN_POINT('Ctrl Pts',(2.0662813849145,-2.21628923121666,30.3277620302206));
#96447=CARTESIAN_POINT('Ctrl Pts',(2.98154544217944,0.540225410611193,30.4868622977078));
#96448=CARTESIAN_POINT('Ctrl Pts',(1.15731396858162,2.80037159965905,30.6459625651952));
#96449=CARTESIAN_POINT('Ctrl Pts',(-1.73027760004697,2.48748791852882,30.8050628326824));
#96450=CARTESIAN_POINT('Ctrl Pts',(-3.02806017719635,-0.110942693894748,
30.9641631001697));
#96451=CARTESIAN_POINT('Ctrl Pts',(-1.54360868027803,-2.60743723993914,
31.123263367657));
#96452=CARTESIAN_POINT('Ctrl Pts',(1.35913717539795,-2.70817334314153,31.2823636351443));
#96453=CARTESIAN_POINT('Ctrl Pts',(3.01308428222424,-0.320592929217562,
31.4414639026316));
#96454=CARTESIAN_POINT('Ctrl Pts',(1.89855742635539,2.36155381409824,31.6005641701188));
#96455=CARTESIAN_POINT('Ctrl Pts',(-0.960396836524605,2.8738640598408,31.7596644376061));
#96456=CARTESIAN_POINT('Ctrl Pts',(-2.93692187183235,0.74561829162367,31.9187647050934));
#96457=CARTESIAN_POINT('Ctrl Pts',(-2.21495228466786,-2.0677144615966,32.0778649725806));
#96458=CARTESIAN_POINT('Ctrl Pts',(0.542153778728399,-2.98119539753127,
32.236965240068));
#96459=CARTESIAN_POINT('Ctrl Pts',(2.80111957135917,-1.15550242968141,32.3960655075552));
#96460=CARTESIAN_POINT('Ctrl Pts',(2.48636824447444,1.73188615991936,32.5551657750425));
#96461=CARTESIAN_POINT('Ctrl Pts',(-0.112901237812935,3.02798778540327,
32.7142660425298));
#96462=CARTESIAN_POINT('Ctrl Pts',(-2.60843510968768,1.54192185165126,32.8733663100171));
#96463=CARTESIAN_POINT('Ctrl Pts',(-2.70729367873307,-1.36088855353519,
33.0324665775044));
#96464=CARTESIAN_POINT('Ctrl Pts',(-0.318643981528126,-3.01329101334189,
33.1915668449916));
#96465=CARTESIAN_POINT('Ctrl Pts',(2.3627813182162,-1.89702956232622,33.3506671124789));
#96466=CARTESIAN_POINT('Ctrl Pts',(2.87324226836875,0.962255467799642,33.5097673799662));
#96467=CARTESIAN_POINT('Ctrl Pts',(0.743718517322665,2.93740352778477,33.6688676474535));
#96468=CARTESIAN_POINT('Ctrl Pts',(-2.06914667323407,2.21361441147628,33.8279679149407));
#96469=CARTESIAN_POINT('Ctrl Pts',(-2.98084410567647,-0.544081920031316,
33.987068182428));
#96470=CARTESIAN_POINT('Ctrl Pts',(-1.15369040736763,-2.80186637118884,
34.1461684499153));
#96471=CARTESIAN_POINT('Ctrl Pts',(1.73349399524354,-2.48524753022827,34.3052687174026));
#96472=CARTESIAN_POINT('Ctrl Pts',(3.0279141268276,0.11485973449802,34.4643689848899));
#96473=CARTESIAN_POINT('Ctrl Pts',(1.5402343779493,2.60943188817684,34.6234692523771));
#96474=CARTESIAN_POINT('Ctrl Pts',(-1.36263936233399,2.70641288170692,34.7825695198644));
#96475=CARTESIAN_POINT('Ctrl Pts',(-3.01349648382547,0.316694900531439,
34.9416697873517));
#96476=CARTESIAN_POINT('Ctrl Pts',(-1.89550090465978,-2.36400783384594,
35.100770054839));
#96477=CARTESIAN_POINT('Ctrl Pts',(0.964113696507479,-2.87261927485314,
35.2598703223262));
#96478=CARTESIAN_POINT('Ctrl Pts',(2.93788395485126,-0.741818431881178,
35.4189705898135));
#96479=CARTESIAN_POINT('Ctrl Pts',(2.21227561220165,2.07057801922768,35.5780708573008));
#96480=CARTESIAN_POINT('Ctrl Pts',(-0.546009833713229,2.98049156676203,
35.7371711247881));
#96481=CARTESIAN_POINT('Ctrl Pts',(-2.80261199883563,1.15187790239839,35.8962713922753));
#96482=CARTESIAN_POINT('Ctrl Pts',(-2.48412577625919,-1.73510110534684,
36.0553716597627));
#96483=CARTESIAN_POINT('Ctrl Pts',(0.116818183130627,-3.02783920150017,
36.2144719272499));
#96484=CARTESIAN_POINT('Ctrl Pts',(2.61042757498959,-1.53854625987814,36.3735721947372));
#96485=CARTESIAN_POINT('Ctrl Pts',(2.70553095243158,1.36438960106188,36.5326724622244));
#96486=CARTESIAN_POINT('Ctrl Pts',(0.314745687042946,3.01370069358903,36.6917727297118));
#96487=CARTESIAN_POINT('Ctrl Pts',(-2.36523336047438,1.89397145399557,36.850872997199));
#96488=CARTESIAN_POINT('Ctrl Pts',(-2.87199507955459,-0.96597152187078,
37.0099732646863));
#96489=CARTESIAN_POINT('Ctrl Pts',(-0.739918036094069,-2.93836315283081,
37.1690735321736));
#96490=CARTESIAN_POINT('Ctrl Pts',(2.07200849897867,-2.21093588740406,37.3281737996609));
#96491=CARTESIAN_POINT('Ctrl Pts',(2.98013778093542,0.54793751896766,37.4872740671482));
#96492=CARTESIAN_POINT('Ctrl Pts',(1.15006491553191,2.80335645398756,37.6463743346354));
#96493=CARTESIAN_POINT('Ctrl Pts',(-1.73670748955686,2.48300298303649,37.8054746021227));
#96494=CARTESIAN_POINT('Ctrl Pts',(-3.02776300945232,-0.11877658289139,
37.96457486961));
#96495=CARTESIAN_POINT('Ctrl Pts',(-1.53685749814404,-2.61142216970936,
38.1236751370973));
#96496=CARTESIAN_POINT('Ctrl Pts',(1.36613926898657,-2.70464789127603,38.2827754045845));
#96497=CARTESIAN_POINT('Ctrl Pts',(3.01390364254712,-0.312796341878149,
38.4418756720718));
#96498=CARTESIAN_POINT('Ctrl Pts',(1.89244121097349,2.36645789758878,38.6009759395591));
#96499=CARTESIAN_POINT('Ctrl Pts',(-0.967828943112242,2.87136968273423,
38.7600762070464));
#96500=CARTESIAN_POINT('Ctrl Pts',(-2.93884112152294,0.738017330756449,
38.9191764745336));
#96501=CARTESIAN_POINT('Ctrl Pts',(-2.20959523764404,-2.07343811188851,
39.0782767420209));
#96502=CARTESIAN_POINT('Ctrl Pts',(0.549864974988074,-2.97978274834466,
39.2373770095082));
#96503=CARTESIAN_POINT('Ctrl Pts',(2.80409973633321,-1.14825144752673,39.3964772769955));
#96504=CARTESIAN_POINT('Ctrl Pts',(2.48187915102991,1.73831314720165,39.5555775444828));
#96505=CARTESIAN_POINT('Ctrl Pts',(-0.120734932961047,3.02768555071591,
39.7146778119701));
#96506=CARTESIAN_POINT('Ctrl Pts',(-2.61241567192003,1.5351680934535,39.8737780794573));
#96507=CARTESIAN_POINT('Ctrl Pts',(-2.70376369860974,-1.36788836537608,
40.0328783469446));
#96508=CARTESIAN_POINT('Ctrl Pts',(-0.310846865852554,-3.01410533061485,
40.1919786144319));
#96509=CARTESIAN_POINT('Ctrl Pts',(2.36768144467684,-1.8909101762337,40.3510788819192));
#96510=CARTESIAN_POINT('Ctrl Pts',(2.87074308465372,0.969685959454866,40.5101791494065));
#96511=CARTESIAN_POINT('Ctrl Pts',(0.736116316663445,2.9393178607277,40.6692794168937));
#96512=CARTESIAN_POINT('Ctrl Pts',(-2.07486685735924,2.20825366348239,40.828379684381));
#96513=CARTESIAN_POINT('Ctrl Pts',(-2.97942646913829,-0.551792200968217,
40.9874799518683));
#96514=CARTESIAN_POINT('Ctrl Pts',(-1.14643749914141,-2.8048418455616,41.1465802193556));
#96515=CARTESIAN_POINT('Ctrl Pts',(1.7399180776094,-2.4807542807096,41.3056804868429));
#96516=CARTESIAN_POINT('Ctrl Pts',(3.02760682532339,0.122693232520313,41.4647807543301));
#96517=CARTESIAN_POINT('Ctrl Pts',(1.53347804651323,2.61340808120603,41.6238810218174));
#96518=CARTESIAN_POINT('Ctrl Pts',(-1.36963688949883,2.70287837480253,41.7829812893047));
#96519=CARTESIAN_POINT('Ctrl Pts',(-3.01430575770784,0.308897259781596,
41.942081556792));
#96520=CARTESIAN_POINT('Ctrl Pts',(-1.88937835041663,-2.36890400122672,
42.1011818242792));
#96521=CARTESIAN_POINT('Ctrl Pts',(0.971542570121709,-2.87011528557518,
42.2602820917666));
#96522=CARTESIAN_POINT('Ctrl Pts',(2.93979337024567,-0.73421499461035,42.4193823592538));
#96523=CARTESIAN_POINT('Ctrl Pts',(2.2069111654804,2.07629473479296,42.578482626741));
#96524=CARTESIAN_POINT('Ctrl Pts',(-0.553719196101618,2.97906894346535,
42.7375828942284));
#96525=CARTESIAN_POINT('Ctrl Pts',(-2.8055827813623,1.14462307113504,42.8966831617156));
#96526=CARTESIAN_POINT('Ctrl Pts',(-2.47962837254616,-1.74152228010872,
43.0557834292029));
#96527=CARTESIAN_POINT('Ctrl Pts',(0.124651480749879,-3.02752683330764,
43.2148836966902));
#96528=CARTESIAN_POINT('Ctrl Pts',(2.61439939715218,-1.53178735803035,43.3739839641774));
#96529=CARTESIAN_POINT('Ctrl Pts',(2.70199192022476,1.37138484062318,43.5330842316648));
#96530=CARTESIAN_POINT('Ctrl Pts',(0.306947524481237,3.01450492374214,43.692184499152));
#96531=CARTESIAN_POINT('Ctrl Pts',(-2.37012556672716,1.88784573416347,43.8512847666393));
#96532=CARTESIAN_POINT('Ctrl Pts',(-2.86948628576077,-0.973398774336397,
44.0103850341266));
#96533=CARTESIAN_POINT('Ctrl Pts',(-0.732313365393594,-2.94026764987723,
44.1694853016138));
#96534=CARTESIAN_POINT('Ctrl Pts',(2.07772174359431,-2.20556774420093,44.3285855691012));
#96535=CARTESIAN_POINT('Ctrl Pts',(2.97871017147186,0.555645959584653,44.4876858365884));
#96536=CARTESIAN_POINT('Ctrl Pts',(1.14280816427329,2.80632254342081,44.6467861040757));
#96537=CARTESIAN_POINT('Ctrl Pts',(-1.74312575404136,2.47850142701921,44.8058863715629));
#96538=CARTESIAN_POINT('Ctrl Pts',(-3.02744557467754,-0.126609676846878,
44.9649866390503));
#96539=CARTESIAN_POINT('Ctrl Pts',(-1.53009602875911,-2.61538961931251,
45.1240869065375));
#96540=CARTESIAN_POINT('Ctrl Pts',(1.37313221810741,-2.70110433530689,45.2831871740248));
#96541=CARTESIAN_POINT('Ctrl Pts',(3.01470282846356,-0.304997660653436,
45.4422874415121));
#96542=CARTESIAN_POINT('Ctrl Pts',(1.88631232844131,2.37134614045018,45.6013877089993));
#96543=CARTESIAN_POINT('Ctrl Pts',(-0.97525457194413,2.86885608588752,45.7604879764867));
#96544=CARTESIAN_POINT('Ctrl Pts',(-2.9407406982379,0.730411429019182,45.9195882439739));
#96545=CARTESIAN_POINT('Ctrl Pts',(-2.20422340246865,-2.07914788166006,
46.0786885114613));
#96546=CARTESIAN_POINT('Ctrl Pts',(0.557572494927398,-2.97835015618116,
46.2377887789484));
#96547=CARTESIAN_POINT('Ctrl Pts',(2.80706112319388,-1.14099277383441,46.3968890464358));
#96548=CARTESIAN_POINT('Ctrl Pts',(2.47737346030718,1.7447284882806,46.555989313923));
#96549=CARTESIAN_POINT('Ctrl Pts',(-0.128567849955195,3.02736306941306,
46.7150895814104));
#96550=CARTESIAN_POINT('Ctrl Pts',(-2.61637869011417,1.52840402135752,46.8741898488976));
#96551=CARTESIAN_POINT('Ctrl Pts',(-2.70021572945777,-1.37487894863602,
47.0332901163849));
#96552=CARTESIAN_POINT('Ctrl Pts',(-0.303047461110431,-3.01489961025401,
47.1923903838722));
#96553=CARTESIAN_POINT('Ctrl Pts',(2.37256532509137,-1.88477786975195,47.3514906513594));
#96554=CARTESIAN_POINT('Ctrl Pts',(2.86822544315535,0.977109458287476,47.5105909188468));
#96555=CARTESIAN_POINT('Ctrl Pts',(0.728507742327304,2.9412134763491,47.669691186334));
#96556=CARTESIAN_POINT('Ctrl Pts',(-2.08057039385854,2.20287630719366,47.8287914538213));
#96557=CARTESIAN_POINT('Ctrl Pts',(-2.97799415238172,-0.55949530339084,
47.9878917213085));
#96558=CARTESIAN_POINT('Ctrl Pts',(-1.1391668766645,-2.80780519314034,48.1469919887959));
#96559=CARTESIAN_POINT('Ctrl Pts',(1.74631136021662,-2.47623174369378,48.306092256283));
#96560=CARTESIAN_POINT('Ctrl Pts',(3.0273157952168,0.130501716601606,48.4651925237705));
#96561=CARTESIAN_POINT('Ctrl Pts',(1.52664175010871,2.6174129319684,48.6242927912576));
#96562=CARTESIAN_POINT('Ctrl Pts',(-1.37649228204864,2.69923773205355,48.783393058745));
#96563=CARTESIAN_POINT('Ctrl Pts',(-3.01534854262687,0.301265542054237,
48.9424933262322));
#96564=CARTESIAN_POINT('Ctrl Pts',(-1.88275888504304,-2.37410509268517,
49.1015935937195));
#96565=CARTESIAN_POINT('Ctrl Pts',(0.978038327691813,-2.86697737698299,
49.2606938612068));
#96566=CARTESIAN_POINT('Ctrl Pts',(2.94347543107135,-0.727803611882825,
49.419794128694));
#96567=CARTESIAN_POINT('Ctrl Pts',(2.19789667042551,2.08449280102471,49.5788943961813));
#96568=CARTESIAN_POINT('Ctrl Pts',(0.364205816777854,2.67564278674459,49.6849612411729));
#96569=CARTESIAN_POINT('Ctrl Pts',(-0.474664453624529,2.51747565713019,
49.7379946636686));
#96570=CARTESIAN_POINT('Ctrl Pts',(-1.20564430054339,2.47375567929515,-0.109744663668484));
#96571=CARTESIAN_POINT('Ctrl Pts',(-2.0299462514768,2.07201230690486,-0.0567112411727241));
#96572=CARTESIAN_POINT('Ctrl Pts',(-3.23088877261529,0.386520622104858,
0.049355603818795));
#96573=CARTESIAN_POINT('Ctrl Pts',(-2.06959919365079,-2.51504233938102,
0.208455871306074));
#96574=CARTESIAN_POINT('Ctrl Pts',(0.996050038619305,-3.09777706678723,
0.367556138793353));
#96575=CARTESIAN_POINT('Ctrl Pts',(3.1450859652048,-0.838203904761194,0.526656406280632));
#96576=CARTESIAN_POINT('Ctrl Pts',(2.40510628092737,2.19359165333219,0.685756673767911));
#96577=CARTESIAN_POINT('Ctrl Pts',(-0.545116174367747,3.20879665711233,
0.844856941255189));
#96578=CARTESIAN_POINT('Ctrl Pts',(-2.99427231540609,1.27626995670517,1.00395720874247));
#96579=CARTESIAN_POINT('Ctrl Pts',(-2.69234626321946,-1.82921242030833,
1.16305747622975));
#96580=CARTESIAN_POINT('Ctrl Pts',(0.0834102058696828,-3.25382721959455,
1.32215774371703));
#96581=CARTESIAN_POINT('Ctrl Pts',(2.78249852956668,-1.6888508273664,1.4812580112043));
#96582=CARTESIAN_POINT('Ctrl Pts',(2.92499448363151,1.42791366852541,1.64035827869159));
#96583=CARTESIAN_POINT('Ctrl Pts',(0.379946825371875,3.2326639751856,1.79945854617886));
#96584=CARTESIAN_POINT('Ctrl Pts',(-2.51419831298256,2.0671984455636,1.95855881366614));
#96585=CARTESIAN_POINT('Ctrl Pts',(-3.09825676803193,-0.997650934719184,
2.11765908115342));
#96586=CARTESIAN_POINT('Ctrl Pts',(-0.83558214300345,-3.14583814954029,
2.2767593486407));
#96587=CARTESIAN_POINT('Ctrl Pts',(2.19483919980503,-2.40357654398027,2.43585961612798));
#96588=CARTESIAN_POINT('Ctrl Pts',(3.20860463655859,0.54713365737409,2.59495988361525));
#96589=CARTESIAN_POINT('Ctrl Pts',(1.27424845901785,2.99512752431821,2.75406015110254));
#96590=CARTESIAN_POINT('Ctrl Pts',(-1.8309091583517,2.69114665212629,2.91316041858981));
#96591=CARTESIAN_POINT('Ctrl Pts',(-3.25379581369482,-0.085506446717136,
3.0722606860771));
#96592=CARTESIAN_POINT('Ctrl Pts',(-1.6870385629377,-2.78359467613364,3.23136095356437));
#96593=CARTESIAN_POINT('Ctrl Pts',(1.42979889133674,-2.92406799804922,3.39046122105165));
#96594=CARTESIAN_POINT('Ctrl Pts',(3.23291239639753,-0.377857040680476,
3.54956148853893));
#96595=CARTESIAN_POINT('Ctrl Pts',(2.06557006111335,2.51553549267108,3.70866175602621));
#96596=CARTESIAN_POINT('Ctrl Pts',(-0.999653777371921,3.09761050346267,
3.86776202351349));
#96597=CARTESIAN_POINT('Ctrl Pts',(-3.14637843287376,0.833547394590984,
4.02686229100077));
#96598=CARTESIAN_POINT('Ctrl Pts',(-2.40215615366969,-2.19639347881041,
4.18596255848805));
#96599=CARTESIAN_POINT('Ctrl Pts',(0.549208754834378,-3.20825002858447,
4.34506282597533));
#96600=CARTESIAN_POINT('Ctrl Pts',(2.99595115861851,-1.27231095129882,4.5041630934626));
#96601=CARTESIAN_POINT('Ctrl Pts',(2.68996180999494,1.83264943790287,4.66326336094988));
#96602=CARTESIAN_POINT('Ctrl Pts',(-0.0876109840156688,3.2537398201493,
4.82236362843716));
#96603=CARTESIAN_POINT('Ctrl Pts',(-2.7846852903256,1.68523776823255,4.98146389592444));
#96604=CARTESIAN_POINT('Ctrl Pts',(-2.92314257882448,-1.43168989850679,
5.14056416341172));
#96605=CARTESIAN_POINT('Ctrl Pts',(-0.375765897644029,-3.23315611930934,
5.29966443089899));
#96606=CARTESIAN_POINT('Ctrl Pts',(2.51687099077396,-2.06394256641075,5.45876469838628));
#96607=CARTESIAN_POINT('Ctrl Pts',(3.09696327281227,1.00165712122146,5.61786496587355));
#96608=CARTESIAN_POINT('Ctrl Pts',(0.831512124557827,3.14691691793094,5.77696523336084));
#96609=CARTESIAN_POINT('Ctrl Pts',(-2.19794674830152,2.40073501104863,5.93606550084811));
#96610=CARTESIAN_POINT('Ctrl Pts',(-3.20789412592581,-0.551283754970828,
6.0951657683354));
#96611=CARTESIAN_POINT('Ctrl Pts',(-1.27037288639211,-2.99677347011156,
6.25426603582267));
#96612=CARTESIAN_POINT('Ctrl Pts',(1.83438893769452,-2.68877587889142,6.41336630330995));
#96613=CARTESIAN_POINT('Ctrl Pts',(3.25368247222021,0.0897155037398571,
6.57246657079723));
#96614=CARTESIAN_POINT('Ctrl Pts',(1.68343626490711,2.7857747295214,6.73156683828451));
#96615=CARTESIAN_POINT('Ctrl Pts',(-1.43358030483734,2.92221594192265,6.89066710577178));
#96616=CARTESIAN_POINT('Ctrl Pts',(-3.23339849059068,0.373674594654671,
7.04976737325906));
#96617=CARTESIAN_POINT('Ctrl Pts',(-2.06231420772467,-2.51820543448332,
7.20886764074635));
#96618=CARTESIAN_POINT('Ctrl Pts',(1.0036600457489,-3.09631474727808,7.36796790823362));
#96619=CARTESIAN_POINT('Ctrl Pts',(3.14745408659262,-0.829476506259126,
7.52706817572091));
#96620=CARTESIAN_POINT('Ctrl Pts',(2.39931286398669,2.19949909805673,7.68616844320817));
#96621=CARTESIAN_POINT('Ctrl Pts',(-0.553358524434341,3.20753688132814,
7.84526871069548));
#96622=CARTESIAN_POINT('Ctrl Pts',(-2.99759452790126,1.26843428995784,8.00436897818272));
#96623=CARTESIAN_POINT('Ctrl Pts',(-2.68758882290656,-1.8361276700252,8.16346924567004));
#96624=CARTESIAN_POINT('Ctrl Pts',(0.0918199859252528,-3.25362376310308,
8.32256951315728));
#96625=CARTESIAN_POINT('Ctrl Pts',(2.78686300326932,-1.6816340572946,8.48166978064459));
#96626=CARTESIAN_POINT('Ctrl Pts',(2.92128808248718,1.43547011141395,8.64077004813185));
#96627=CARTESIAN_POINT('Ctrl Pts',(0.371583135336417,3.23363950915651,8.79987031561914));
#96628=CARTESIAN_POINT('Ctrl Pts',(-2.519538824682,2.06068498625201,8.95897058310642));
#96629=CARTESIAN_POINT('Ctrl Pts',(-3.09566492637596,-1.00566255038664,
9.11807085059368));
#96630=CARTESIAN_POINT('Ctrl Pts',(-0.827440540942498,-3.14798993849237,
9.27717111808098));
#96631=CARTESIAN_POINT('Ctrl Pts',(2.20105052763421,-2.39788971315312,9.43627138556825));
#96632=CARTESIAN_POINT('Ctrl Pts',(3.20717829483208,0.555433062395866,9.59537165305553));
#96633=CARTESIAN_POINT('Ctrl Pts',(1.26649516286409,2.99841433162368,9.75447192054281));
#96634=CARTESIAN_POINT('Ctrl Pts',(-1.83786563419738,2.6864006425477,9.91357218803009));
#96635=CARTESIAN_POINT('Ctrl Pts',(-3.25356369280678,-0.0939244296970033,
10.0726724555174));
#96636=CARTESIAN_POINT('Ctrl Pts',(-1.67983114615723,-2.78795011111111,
10.2317727230046));
#96637=CARTESIAN_POINT('Ctrl Pts',(1.43735931745029,-2.9203590009078,10.3908729904919));
#96638=CARTESIAN_POINT('Ctrl Pts',(3.23387917490375,-0.369491520563451,
10.5499732579792));
#96639=CARTESIAN_POINT('Ctrl Pts',(2.05905490267551,2.52087116081175,10.7090735254665));
#96640=CARTESIAN_POINT('Ctrl Pts',(-1.0076646342975,3.09501381037799,10.8681737929538));
#96641=CARTESIAN_POINT('Ctrl Pts',(-3.1485244734057,0.825404229459601,11.027274060441));
#96642=CARTESIAN_POINT('Ctrl Pts',(-2.39646555914347,-2.20260103638484,
11.1863743279283));
#96643=CARTESIAN_POINT('Ctrl Pts',(0.557507367987582,-3.20681836658766,
11.3454745954156));
#96644=CARTESIAN_POINT('Ctrl Pts',(2.9992328809358,-1.26455550592212,11.5045748629029));
#96645=CARTESIAN_POINT('Ctrl Pts',(2.68521133831194,1.83960282948396,11.6636751303901));
#96646=CARTESIAN_POINT('Ctrl Pts',(-0.0960288341747119,3.25350226135644,
11.8227753978775));
#96647=CARTESIAN_POINT('Ctrl Pts',(-2.78903605259199,1.67802753224925,11.9818756653647));
#96648=CARTESIAN_POINT('Ctrl Pts',(-2.9194286975732,-1.43924792215604,12.140975932852));
#96649=CARTESIAN_POINT('Ctrl Pts',(-0.367399751210757,-3.23411748773212,
12.3000762003393));
#96650=CARTESIAN_POINT('Ctrl Pts',(2.52220244231514,-2.05742395767715,12.4591764678265));
#96651=CARTESIAN_POINT('Ctrl Pts',(3.09436139955658,1.00966629664392,12.6182767353138));
#96652=CARTESIAN_POINT('Ctrl Pts',(0.823367572662327,3.14905769110897,12.7773770028011));
#96653=CARTESIAN_POINT('Ctrl Pts',(-2.20415062365994,2.39504040255355,12.9364772702884));
#96654=CARTESIAN_POINT('Ctrl Pts',(-3.20645709674549,-0.559581440341695,
13.0955775377757));
#96655=CARTESIAN_POINT('Ctrl Pts',(-1.26261531994337,-3.0000501754952,13.2546778052629));
#96656=CARTESIAN_POINT('Ctrl Pts',(1.8413392551582,-2.68402091069683,13.4137780727502));
#96657=CARTESIAN_POINT('Ctrl Pts',(3.25343946877775,0.0981331984780143,
13.5728783402375));
#96658=CARTESIAN_POINT('Ctrl Pts',(1.67622321632521,2.79012082725763,13.7319786077248));
#96659=CARTESIAN_POINT('Ctrl Pts',(-1.44113592474108,2.91849717287255,13.8910788752121));
#96660=CARTESIAN_POINT('Ctrl Pts',(-3.23435444754192,0.365307828153497,
14.0501791426993));
#96661=CARTESIAN_POINT('Ctrl Pts',(-2.05579215193925,-2.52353266863525,
14.2092794101866));
#96662=CARTESIAN_POINT('Ctrl Pts',(1.01166753658848,-3.09370769418467,14.3683796776739));
#96663=CARTESIAN_POINT('Ctrl Pts',(3.14958959137911,-0.821330571402732,
14.5274799451612));
#96664=CARTESIAN_POINT('Ctrl Pts',(2.39361424397959,2.20569928881124,14.6865802126485));
#96665=CARTESIAN_POINT('Ctrl Pts',(-0.561655278590501,3.2060944854567,14.8456804801357));
#96666=CARTESIAN_POINT('Ctrl Pts',(-3.00086621495993,1.26067460573952,15.004780747623));
#96667=CARTESIAN_POINT('Ctrl Pts',(-2.68282936020039,-1.84307491049364,
15.1638810151103));
#96668=CARTESIAN_POINT('Ctrl Pts',(0.100237521726537,-3.253375315097,15.3229812825976));
#96669=CARTESIAN_POINT('Ctrl Pts',(2.79120443465422,-1.67441819913995,15.4820815500848));
#96670=CARTESIAN_POINT('Ctrl Pts',(2.91756442719559,1.44302332441552,15.6411818175721));
#96671=CARTESIAN_POINT('Ctrl Pts',(0.363215752266829,3.23459005423402,15.8002820850594));
#96672=CARTESIAN_POINT('Ctrl Pts',(-2.52486183921557,2.05415948614449,15.9593823525467));
#96673=CARTESIAN_POINT('Ctrl Pts',(-3.09305269453573,-1.01366835329394,
16.118482620034));
#96674=CARTESIAN_POINT('Ctrl Pts',(-0.819293226533021,-3.15012017399361,
16.2775828875212));
#96675=CARTESIAN_POINT('Ctrl Pts',(2.20724703119086,-2.39218708401822,16.4366831550085));
#96676=CARTESIAN_POINT('Ctrl Pts',(3.20573053287298,0.563728881866405,16.5957834224958));
#96677=CARTESIAN_POINT('Ctrl Pts',(1.25873336412252,3.0016809989886,16.7548836899831));
#96678=CARTESIAN_POINT('Ctrl Pts',(-1.84480979476415,2.68163668732114,16.9139839574703));
#96679=CARTESIAN_POINT('Ctrl Pts',(-3.25330980034103,-0.10234180303989,
17.0730842249576));
#96680=CARTESIAN_POINT('Ctrl Pts',(-1.67261248144863,-2.7922868743284,17.2321844924449));
#96681=CARTESIAN_POINT('Ctrl Pts',(1.44491012038977,-2.91663046093255,17.3912847599322));
#96682=CARTESIAN_POINT('Ctrl Pts',(3.23482430770986,-0.361123524425976,
17.5503850274195));
#96683=CARTESIAN_POINT('Ctrl Pts',(2.0525259609759,2.52618995350001,17.7094852949067));
#96684=CARTESIAN_POINT('Ctrl Pts',(-1.01566874592325,3.0923964008838,17.868585562394));
#96685=CARTESIAN_POINT('Ctrl Pts',(-3.15064943873048,0.817255538905519,
18.0276858298813));
#96686=CARTESIAN_POINT('Ctrl Pts',(-2.3907589232665,-2.20879385015127,18.1867860973686));
#96687=CARTESIAN_POINT('Ctrl Pts',(0.565802249301867,-3.2053652391466,18.3458863648559));
#96688=CARTESIAN_POINT('Ctrl Pts',(3.00249452724035,-1.25679159590449,18.5049866323432));
#96689=CARTESIAN_POINT('Ctrl Pts',(2.68044289255802,1.84654390724392,18.6640868998304));
#96690=CARTESIAN_POINT('Ctrl Pts',(-0.104446041537755,3.25324292453723,
18.8231871673177));
#96691=CARTESIAN_POINT('Ctrl Pts',(-2.79336814582734,1.67080606400668,18.982287434805));
#96692=CARTESIAN_POINT('Ctrl Pts',(-2.91569527447413,-1.44679631187451,
19.1413877022923));
#96693=CARTESIAN_POINT('Ctrl Pts',(-0.359031145506217,-3.23505720787144,
19.3004879697795));
#96694=CARTESIAN_POINT('Ctrl Pts',(2.52751701093296,-2.05089157711685,19.4595882372668));
#96695=CARTESIAN_POINT('Ctrl Pts',(3.09173881350344,1.01766871363955,19.6186885047541));
#96696=CARTESIAN_POINT('Ctrl Pts',(0.81521750937268,3.15117738536831,19.7777887722414));
#96697=CARTESIAN_POINT('Ctrl Pts',(-2.21033974504533,2.38932976232191,19.9368890397287));
#96698=CARTESIAN_POINT('Ctrl Pts',(-3.2049986044304,-0.567875380029503,
20.0959893072159));
#96699=CARTESIAN_POINT('Ctrl Pts',(-1.25484930189775,-3.00330679937484,
20.2550895747032));
#96700=CARTESIAN_POINT('Ctrl Pts',(1.84827724720752,-2.67924797641044,20.4141898421905));
#96701=CARTESIAN_POINT('Ctrl Pts',(3.25317468771359,0.106550236339809,20.5732901096778));
#96702=CARTESIAN_POINT('Ctrl Pts',(1.66899894756981,2.7944482486987,20.732390377165));
#96703=CARTESIAN_POINT('Ctrl Pts',(-1.44868189808057,2.91475886821159,20.8914906446523));
#96704=CARTESIAN_POINT('Ctrl Pts',(-3.2352887546213,0.356938616382969,21.0505909121396));
#96705=CARTESIAN_POINT('Ctrl Pts',(-2.04925633525114,-2.52884301095924,
21.2096911796269));
#96706=CARTESIAN_POINT('Ctrl Pts',(1.01966825560611,-3.09107993266975,21.3687914471141));
#96707=CARTESIAN_POINT('Ctrl Pts',(3.15170401368621,-0.813179138787187,
21.5278917146015));
#96708=CARTESIAN_POINT('Ctrl Pts',(2.38789960178238,2.21188471522636,21.6869919820887));
#96709=CARTESIAN_POINT('Ctrl Pts',(-0.569948273182041,3.20463062887773,
21.846092249576));
#96710=CARTESIAN_POINT('Ctrl Pts',(-3.00411781505223,1.25290648291489,22.0051925170633));
#96711=CARTESIAN_POINT('Ctrl Pts',(-2.67805193937835,-1.85000981392972,
22.1642927845506));
#96712=CARTESIAN_POINT('Ctrl Pts',(0.108654386565719,-3.25310508989865,
22.3233930520378));
#96713=CARTESIAN_POINT('Ctrl Pts',(2.79552718249057,-1.66719113289409,22.4824933195252));
#96714=CARTESIAN_POINT('Ctrl Pts',(2.91382124253668,1.45056687821914,22.6415935870124));
#96715=CARTESIAN_POINT('Ctrl Pts',(0.354845937931631,3.23551894786259,22.8006938544997));
#96716=CARTESIAN_POINT('Ctrl Pts',(-2.53016795302409,2.04762023606288,22.959794121987));
#96717=CARTESIAN_POINT('Ctrl Pts',(-3.09041975865839,-1.02166737098641,
23.1188943894742));
#96718=CARTESIAN_POINT('Ctrl Pts',(-0.811140428001784,-3.15222932346388,
23.2779946569615));
#96719=CARTESIAN_POINT('Ctrl Pts',(2.21342876004792,-2.38646844224622,23.4370949244488));
#96720=CARTESIAN_POINT('Ctrl Pts',(3.20426131264257,0.572020927892142,23.596195191936));
#96721=CARTESIAN_POINT('Ctrl Pts',(1.25096313976878,3.00492757393324,23.7552954594234));
#96722=CARTESIAN_POINT('Ctrl Pts',(-1.8517416066857,2.67685478196211,23.9143957269106));
#96723=CARTESIAN_POINT('Ctrl Pts',(-3.25303413112153,-0.110758491335166,
24.0734959943979));
#96724=CARTESIAN_POINT('Ctrl Pts',(-1.66538262073583,-2.7966049467516,24.2325962618851));
#96725=CARTESIAN_POINT('Ctrl Pts',(1.45245125150157,-2.91288239784167,24.3916965293725));
#96726=CARTESIAN_POINT('Ctrl Pts',(3.235747787499,-0.352753111027735,24.5507967968597));
#96727=CARTESIAN_POINT('Ctrl Pts',(2.04598328023658,2.53149183657321,24.709897064347));
#96728=CARTESIAN_POINT('Ctrl Pts',(-1.0236660589441,3.08975829174553,24.8689973318343));
#96729=CARTESIAN_POINT('Ctrl Pts',(-3.15275331448154,0.809101377869387,
25.0280975993216));
#96730=CARTESIAN_POINT('Ctrl Pts',(-2.38503628431215,-2.21497187886412,
25.1871978668089));
#96731=CARTESIAN_POINT('Ctrl Pts',(0.574093343292813,-3.2038906558794,25.3462981342961));
#96732=CARTESIAN_POINT('Ctrl Pts',(3.00573607567908,-1.24901927327234,25.5053984017834));
#96733=CARTESIAN_POINT('Ctrl Pts',(2.67565650466255,1.853472624751,25.6644986692707));
#96734=CARTESIAN_POINT('Ctrl Pts',(-0.112862549767962,3.25296181141192,
25.823598936758));
#96735=CARTESIAN_POINT('Ctrl Pts',(-2.79768154103088,1.66357341185158,25.9826992042453));
#96736=CARTESIAN_POINT('Ctrl Pts',(-2.91194233451933,-1.4543350171396,26.1417994717325));
#96737=CARTESIAN_POINT('Ctrl Pts',(-0.350660136546753,-3.23597527343481,
26.3008997392198));
#96738=CARTESIAN_POINT('Ctrl Pts',(2.53281466105276,-2.04434546845699,26.4600000067071));
#96739=CARTESIAN_POINT('Ctrl Pts',(3.08909553220792,1.025664318643,26.6191002741944));
#96740=CARTESIAN_POINT('Ctrl Pts',(0.807061989243078,3.15327598651996,26.7782005416816));
#96741=CARTESIAN_POINT('Ctrl Pts',(-2.21651407102935,2.38360312857937,26.9373008091689));
#96742=CARTESIAN_POINT('Ctrl Pts',(-3.20351865874329,-0.576165518516979,
27.0964010766562));
#96743=CARTESIAN_POINT('Ctrl Pts',(-1.24707488423887,-3.00654331995151,
27.2555013441435));
#96744=CARTESIAN_POINT('Ctrl Pts',(1.85520286740139,-2.67445710798101,27.4146016116308));
#96745=CARTESIAN_POINT('Ctrl Pts',(3.25288813080007,0.114966560983826,27.5737018791181));
#96746=CARTESIAN_POINT('Ctrl Pts',(1.66176350699827,2.79875696487802,27.7328021466053));
#96747=CARTESIAN_POINT('Ctrl Pts',(-1.4562181743451,2.91100105296294,27.8919024140926));
#96748=CARTESIAN_POINT('Ctrl Pts',(-3.23620140557482,0.348567015364339,
28.0510026815798));
#96749=CARTESIAN_POINT('Ctrl Pts',(-2.04270680140936,-2.53413642590931,
28.2101029490672));
#96750=CARTESIAN_POINT('Ctrl Pts',(1.02766214924716,-3.08843148032283,28.3692032165544));
#96751=CARTESIAN_POINT('Ctrl Pts',(3.15379733936052,-0.805022262975986,
28.5283034840417));
#96752=CARTESIAN_POINT('Ctrl Pts',(2.38216897564738,2.21805533589845,28.687403751529));
#96753=CARTESIAN_POINT('Ctrl Pts',(-0.578237452697781,3.20314532138989,
28.8465040190163));
#96754=CARTESIAN_POINT('Ctrl Pts',(-3.00734930641285,1.24512997348174,29.0056042865036));
#96755=CARTESIAN_POINT('Ctrl Pts',(-2.6732565924192,-1.85693233391303,29.1647045539908));
#96756=CARTESIAN_POINT('Ctrl Pts',(0.117070524102486,-3.2528130893168,29.3238048214781));
#96757=CARTESIAN_POINT('Ctrl Pts',(2.79983121784309,-1.65995290693313,29.4829050889654));
#96758=CARTESIAN_POINT('Ctrl Pts',(2.91005855356632,1.45810072233022,29.6420053564527));
#96759=CARTESIAN_POINT('Ctrl Pts',(0.346473748356187,3.23642618382443,29.80110562394));
#96760=CARTESIAN_POINT('Ctrl Pts',(-2.53545713058987,2.04106727977924,29.9602058914272));
#96761=CARTESIAN_POINT('Ctrl Pts',(-3.08776613636808,-1.02965954992073,
30.1193061589145));
#96762=CARTESIAN_POINT('Ctrl Pts',(-0.802982199921472,-3.15431737278507,
30.2784064264018));
#96763=CARTESIAN_POINT('Ctrl Pts',(2.21959567282659,-2.38073382611621,30.437506693889));
#96764=CARTESIAN_POINT('Ctrl Pts',(3.20277064397537,0.580309144968386,30.5966069613764));
#96765=CARTESIAN_POINT('Ctrl Pts',(1.24318454181467,3.00815403472587,30.7557072288636));
#96766=CARTESIAN_POINT('Ctrl Pts',(-1.85866102356239,2.67205495847942,30.9148074963509));
#96767=CARTESIAN_POINT('Ctrl Pts',(-3.25273668699353,-0.119174438243803,
31.0739077638382));
#96768=CARTESIAN_POINT('Ctrl Pts',(-1.65814161241355,-2.80090429947669,
31.2330080313254));
#96769=CARTESIAN_POINT('Ctrl Pts',(1.45998266030742,-2.90911483672372,31.3921082988128));
#96770=CARTESIAN_POINT('Ctrl Pts',(3.23664960808963,-0.344380336397985,
31.5512085663));
#96771=CARTESIAN_POINT('Ctrl Pts',(2.0394269042525,2.53677677454196,31.7103088337873));
#96772=CARTESIAN_POINT('Ctrl Pts',(-1.03165651982814,3.08709950062199,31.8694091012746));
#96773=CARTESIAN_POINT('Ctrl Pts',(-3.15483608657604,0.800941800933051,
32.0285093687618));
#96774=CARTESIAN_POINT('Ctrl Pts',(-2.37929768058629,-2.22113508116935,
32.1876096362491));
#96775=CARTESIAN_POINT('Ctrl Pts',(0.582380594462059,-3.20239462665651,
32.3467099037364));
#96776=CARTESIAN_POINT('Ctrl Pts',(3.00895750455389,-1.24123859005156,32.5058101712237));
#96777=CARTESIAN_POINT('Ctrl Pts',(2.67085220666439,1.86038893562621,32.6649104387109));
#96778=CARTESIAN_POINT('Ctrl Pts',(-0.121278302527527,3.25265892386221,
32.8240107061983));
#96779=CARTESIAN_POINT('Ctrl Pts',(-2.80197620932986,1.65632962419737,32.9831109736855));
#96780=CARTESIAN_POINT('Ctrl Pts',(-2.90816990283,-1.46186398748932,33.1422112411728));
#96781=CARTESIAN_POINT('Ctrl Pts',(-0.342286780365579,-3.23687167827694,
33.3013115086601));
#96782=CARTESIAN_POINT('Ctrl Pts',(2.53809535721348,-2.03778567551542,33.4604117761474));
#96783=CARTESIAN_POINT('Ctrl Pts',(3.08643157336347,1.03365305813389,33.6195120436347));
#96784=CARTESIAN_POINT('Ctrl Pts',(0.798901066864283,3.15535348051648,33.7786123111219));
#96785=CARTESIAN_POINT('Ctrl Pts',(-2.22267356028275,2.37786053965839,33.9377125786092));
#96786=CARTESIAN_POINT('Ctrl Pts',(-3.20201726959057,-0.584451800312236,
34.0968128460964));
#96787=CARTESIAN_POINT('Ctrl Pts',(-1.23929211900646,-3.00975971556083,
34.2559131135838));
#96788=CARTESIAN_POINT('Ctrl Pts',(1.86211606938167,-2.66964833747724,34.415013381071));
#96789=CARTESIAN_POINT('Ctrl Pts',(3.25257979995536,0.12338211607354,34.5741136485583));
#96790=CARTESIAN_POINT('Ctrl Pts',(1.6545169430426,2.80304694695421,34.7332139160456));
#96791=CARTESIAN_POINT('Ctrl Pts',(-1.46374470308892,2.90722375228044,34.8923141835329));
#96792=CARTESIAN_POINT('Ctrl Pts',(-3.23709239429345,0.34019308113477,35.0514144510202));
#96793=CARTESIAN_POINT('Ctrl Pts',(-2.03614359425464,-2.53941287805274,
35.2105147185074));
#96794=CARTESIAN_POINT('Ctrl Pts',(1.0356491640027,-3.08576235487196,35.3696149859947));
#96795=CARTESIAN_POINT('Ctrl Pts',(3.1558695543899,-0.796859998568978,35.528715253482));
#96796=CARTESIAN_POINT('Ctrl Pts',(2.37642240393377,2.2242111095231,35.6878155209692));
#96797=CARTESIAN_POINT('Ctrl Pts',(-0.586522761652353,3.20163857293545,
35.8469157884566));
#96798=CARTESIAN_POINT('Ctrl Pts',(-3.01056066741105,1.23734512949377,36.0060160559438));
#96799=CARTESIAN_POINT('Ctrl Pts',(-2.66844335142165,-1.86384242410619,
36.1651163234311));
#96800=CARTESIAN_POINT('Ctrl Pts',(0.125485878001671,-3.25249931530609,
36.3242165909184));
#96801=CARTESIAN_POINT('Ctrl Pts',(2.80411651190175,-1.65270356970762,36.4833168584056));
#96802=CARTESIAN_POINT('Ctrl Pts',(2.90627638547088,1.46562480631938,36.642417125893));
#96803=CARTESIAN_POINT('Ctrl Pts',(0.338099239581502,3.2373117560468,36.8015173933802));
#96804=CARTESIAN_POINT('Ctrl Pts',(-2.54072933650863,2.03450066115712,36.9606176608675));
#96805=CARTESIAN_POINT('Ctrl Pts',(-3.08509184542742,-1.03764483659955,
37.1197179283548));
#96806=CARTESIAN_POINT('Ctrl Pts',(-0.794818596900981,-3.15638430798038,
37.2788181958421));
#96807=CARTESIAN_POINT('Ctrl Pts',(2.22574772824722,-2.37498327401409,37.4379184633293));
#96808=CARTESIAN_POINT('Ctrl Pts',(3.20125853684957,0.588593477616085,37.5970187308166));
#96809=CARTESIAN_POINT('Ctrl Pts',(1.23539762232795,3.01136035976947,37.7561189983039));
#96810=CARTESIAN_POINT('Ctrl Pts',(-1.86556799907749,2.66723724900174,37.9152192657912));
#96811=CARTESIAN_POINT('Ctrl Pts',(-3.25241746994808,-0.127589587431759,
38.0743195332785));
#96812=CARTESIAN_POINT('Ctrl Pts',(-1.65088950495109,-2.80518490372502,
38.2334198007657));
#96813=CARTESIAN_POINT('Ctrl Pts',(1.46750429639411,-2.90532780279767,38.392520068253));
#96814=CARTESIAN_POINT('Ctrl Pts',(3.23752976344525,-0.33600525658179,38.5516203357403));
#96815=CARTESIAN_POINT('Ctrl Pts',(2.03285687691022,2.54204473203035,38.7107206032276));
#96816=CARTESIAN_POINT('Ctrl Pts',(-1.03964007508946,3.08442004531035,38.8698208707148));
#96817=CARTESIAN_POINT('Ctrl Pts',(-3.15689774107258,0.792776862714387,
39.0289211382022));
#96818=CARTESIAN_POINT('Ctrl Pts',(-2.37354315050146,-2.22728341581217,
39.1880214056894));
#96819=CARTESIAN_POINT('Ctrl Pts',(0.590663947337058,-3.20087716149193,
39.3471216731767));
#96820=CARTESIAN_POINT('Ctrl Pts',(3.01215879230152,-1.23344959832382,39.5062219406639));
#96821=CARTESIAN_POINT('Ctrl Pts',(2.66603003072207,1.86729279357374,39.6653222081512));
#96822=CARTESIAN_POINT('Ctrl Pts',(-0.129693243483748,3.25233426391553,
39.8244224756385));
#96823=CARTESIAN_POINT('Ctrl Pts',(-2.80625212197701,1.64907474953194,39.9835227431257));
#96824=CARTESIAN_POINT('Ctrl Pts',(-2.90437800465771,-1.46938317252679,
40.1426230106131));
#96825=CARTESIAN_POINT('Ctrl Pts',(-0.333911133011649,-3.23774641639759,
40.3017232781004));
#96826=CARTESIAN_POINT('Ctrl Pts',(2.5433590640676,-2.03121224220161,40.4608235455876));
#96827=CARTESIAN_POINT('Ctrl Pts',(3.08374695480184,1.04163487863778,40.6199238130749));
#96828=CARTESIAN_POINT('Ctrl Pts',(0.790734796863326,3.15740985345169,40.7790240805622));
#96829=CARTESIAN_POINT('Ctrl Pts',(-2.22881817157562,2.3721020339983,40.9381243480495));
#96830=CARTESIAN_POINT('Ctrl Pts',(-3.20049444702208,-0.592734169949194,
41.0972246155367));
#96831=CARTESIAN_POINT('Ctrl Pts',(-1.23150105829622,-3.01295596467317,
41.2563248830241));
#96832=CARTESIAN_POINT('Ctrl Pts',(1.86901680687331,-2.66482169708772,41.4154251505113));
#96833=CARTESIAN_POINT('Ctrl Pts',(3.25224969724331,0.13179684527757,41.5745254179986));
#96834=CARTESIAN_POINT('Ctrl Pts',(1.64725930420931,2.80731816621134,41.7336256854858));
#96835=CARTESIAN_POINT('Ctrl Pts',(-1.47126143393157,2.90342699144824,41.8927259529732));
#96836=CARTESIAN_POINT('Ctrl Pts',(-3.23796171481316,0.331816869747021,
42.0518262204604));
#96837=CARTESIAN_POINT('Ctrl Pts',(-2.02956675771925,-2.54467233207055,
42.2109264879477));
#96838=CARTESIAN_POINT('Ctrl Pts',(1.04362924640992,-3.08307257418346,42.370026755435));
#96839=CARTESIAN_POINT('Ctrl Pts',(3.1579206449035,-0.788692400202103,42.5291270229223));
#96840=CARTESIAN_POINT('Ctrl Pts',(2.37065992510754,2.2303519948953,42.6882272904095));
#96841=CARTESIAN_POINT('Ctrl Pts',(-0.594804144586184,3.20011039360014,
42.8473275578968));
#96842=CARTESIAN_POINT('Ctrl Pts',(-3.01375187655094,1.22955200306058,43.0064278253841));
#96843=CARTESIAN_POINT('Ctrl Pts',(-2.66361224860416,-1.87074003825496,
43.1655280928714));
#96844=CARTESIAN_POINT('Ctrl Pts',(0.133900391933119,-3.25216376996676,
43.3246283603587));
#96845=CARTESIAN_POINT('Ctrl Pts',(2.80838303598201,-1.64544316974277,43.4837286278459));
#96846=CARTESIAN_POINT('Ctrl Pts',(2.90247476356711,1.47313907982251,43.6428288953332));
#96847=CARTESIAN_POINT('Ctrl Pts',(0.329722467664408,3.23817565860181,43.8019291628205));
#96848=CARTESIAN_POINT('Ctrl Pts',(-2.54598453549002,2.02792042415186,43.9610294303078));
#96849=CARTESIAN_POINT('Ctrl Pts',(-3.08239690373679,-1.0456231775719,44.120129697795));
#96850=CARTESIAN_POINT('Ctrl Pts',(-0.786649673586238,-3.15843011521361,
44.2792299652823));
#96851=CARTESIAN_POINT('Ctrl Pts',(2.23188488513169,-2.36921682443382,44.4383302327696));
#96852=CARTESIAN_POINT('Ctrl Pts',(3.19972500138294,0.596873870384775,44.5974305002568));
#96853=CARTESIAN_POINT('Ctrl Pts',(1.22760243343935,3.014546527597,44.7565307677442));
#96854=CARTESIAN_POINT('Ctrl Pts',(-1.87246248701163,2.66240168578663,44.9156310352314));
#96855=CARTESIAN_POINT('Ctrl Pts',(-3.25207648209538,-0.136003882587964,
45.0747313027187));
#96856=CARTESIAN_POINT('Ctrl Pts',(-1.64362634694256,-2.80944673080995,
45.233831570206));
#96857=CARTESIAN_POINT('Ctrl Pts',(1.47501610951029,-2.90152132147672,45.3929318376933));
#96858=CARTESIAN_POINT('Ctrl Pts',(3.23838824749048,-0.327627927517849,
45.5520321051805));
#96859=CARTESIAN_POINT('Ctrl Pts',(2.02627324253834,2.54729567354398,45.7111323726678));
#96860=CARTESIAN_POINT('Ctrl Pts',(-1.04761667195744,3.08171994418912,45.8702326401551));
#96861=CARTESIAN_POINT('Ctrl Pts',(-3.15893826289477,0.784606617022181,
46.0293329076424));
#96862=CARTESIAN_POINT('Ctrl Pts',(-2.36777273501135,-2.23341684002548,
46.1884331751296));
#96863=CARTESIAN_POINT('Ctrl Pts',(0.598943351115479,-3.19933827361817,
46.347533442617));
#96864=CARTESIAN_POINT('Ctrl Pts',(3.01533990863423,-1.22565234436046,46.5066337101042));
#96865=CARTESIAN_POINT('Ctrl Pts',(2.66119002601396,1.87418414119101,46.6657339775915));
#96866=CARTESIAN_POINT('Ctrl Pts',(-0.138107348548404,3.25198785509165,
46.8248342450789));
#96867=CARTESIAN_POINT('Ctrl Pts',(-2.81050918885052,1.64180879569596,46.983934512566));
#96868=CARTESIAN_POINT('Ctrl Pts',(-2.90056678270385,-1.47689244423952,
47.1430347800534));
#96869=CARTESIAN_POINT('Ctrl Pts',(-0.325533026746636,-3.23859963012878,
47.3021350475406));
#96870=CARTESIAN_POINT('Ctrl Pts',(2.54860531944881,-2.02462492982939,47.461235315028));
#96871=CARTESIAN_POINT('Ctrl Pts',(3.08104250892322,1.04960918746444,47.6203355825151));
#96872=CARTESIAN_POINT('Ctrl Pts',(0.782561680270313,3.15944612027446,47.7794358500025));
#96873=CARTESIAN_POINT('Ctrl Pts',(-2.23494490001932,2.36632568773837,47.9385361174897));
#96874=CARTESIAN_POINT('Ctrl Pts',(-3.19895585498994,-0.601008828439279,
48.0976363849771));
#96875=CARTESIAN_POINT('Ctrl Pts',(-1.22369096897038,-3.01613918720563,
48.2567366524642));
#96876=CARTESIAN_POINT('Ctrl Pts',(1.87588445932071,-2.65996359612247,48.4158369199516));
#96877=CARTESIAN_POINT('Ctrl Pts',(3.25193707323675,0.140184704552063,48.5749371874387));
#96878=CARTESIAN_POINT('Ctrl Pts',(1.63991576715359,2.81162016955288,48.7340374549263));
#96879=CARTESIAN_POINT('Ctrl Pts',(-1.4786254840315,2.8995162196865,48.8931377224133));
#96880=CARTESIAN_POINT('Ctrl Pts',(-3.23908187246008,0.323618892565623,
49.0522379899008));
#96881=CARTESIAN_POINT('Ctrl Pts',(-2.02245614015915,-2.55025933497318,
49.2113382573879));
#96882=CARTESIAN_POINT('Ctrl Pts',(1.05060697727445,-3.07970183853061,49.3704385248753));
#96883=CARTESIAN_POINT('Ctrl Pts',(3.16187590788727,-0.781805304638667,
49.5295387923625));
#96884=CARTESIAN_POINT('Ctrl Pts',(2.36097657105778,2.23915834260108,49.6886390598498));
#96885=CARTESIAN_POINT('Ctrl Pts',(0.391229220202036,2.87417057272355,49.7947059048413));
#96886=CARTESIAN_POINT('Ctrl Pts',(-0.509883685252968,2.70426773226887,
49.8477393273371));
#96887=CARTESIAN_POINT('Ctrl Pts',(-1.28892185405285,2.64462557919736,-2.24820162486594E-14));
#96888=CARTESIAN_POINT('Ctrl Pts',(-2.17016087157859,2.21513255860965,0.0530334224957372));
#96889=CARTESIAN_POINT('Ctrl Pts',(-3.45405617988707,0.413218788201715,
0.159100267487257));
#96890=CARTESIAN_POINT('Ctrl Pts',(-2.21255276421415,-2.68876403565728,
0.318200534974535));
#96891=CARTESIAN_POINT('Ctrl Pts',(1.06485027294372,-3.31175003984662,0.477300802461814));
#96892=CARTESIAN_POINT('Ctrl Pts',(3.36232670912974,-0.896101221987242,
0.636401069949093));
#96893=CARTESIAN_POINT('Ctrl Pts',(2.5712343561111,2.34510976377807,0.795501337436372));
#96894=CARTESIAN_POINT('Ctrl Pts',(-0.582769022193126,3.4304380941372,0.954601604923651));
#96895=CARTESIAN_POINT('Ctrl Pts',(-3.20109589749867,1.36442584112634,1.11370187241093));
#96896=CARTESIAN_POINT('Ctrl Pts',(-2.87831488588854,-1.95556173838141,
1.27280213989821));
#96897=CARTESIAN_POINT('Ctrl Pts',(0.0891716048822917,-3.47857905582672,
1.43190240738549));
#96898=CARTESIAN_POINT('Ctrl Pts',(2.97469424606561,-1.80550493926474,1.59100267487277));
#96899=CARTESIAN_POINT('Ctrl Pts',(3.12703283318065,1.52654404971158,1.75010294236005));
#96900=CARTESIAN_POINT('Ctrl Pts',(0.406190919144961,3.45595400114929,1.90920320984732));
#96901=CARTESIAN_POINT('Ctrl Pts',(-2.68786170976409,2.20998618908559,2.0683034773346));
#96902=CARTESIAN_POINT('Ctrl Pts',(-3.31226287552911,-1.06656174785242,
2.22740374482188));
#96903=CARTESIAN_POINT('Ctrl Pts',(-0.893298367095335,-3.3631308491467,
2.38650401230916));
#96904=CARTESIAN_POINT('Ctrl Pts',(2.34644348211611,-2.56959895553633,2.54560427979644));
#96905=CARTESIAN_POINT('Ctrl Pts',(3.43023281013426,0.584925858944962,2.70470454728372));
#96906=CARTESIAN_POINT('Ctrl Pts',(1.36226471238718,3.20201017831608,2.863804814771));
#96907=CARTESIAN_POINT('Ctrl Pts',(-1.9573756753309,2.87703241397402,3.02290508225827));
#96908=CARTESIAN_POINT('Ctrl Pts',(-3.47854548062508,-0.0914126395211362,
3.18200534974556));
#96909=CARTESIAN_POINT('Ctrl Pts',(-1.80356749616777,-2.97586610684143,
3.34110561723283));
#96910=CARTESIAN_POINT('Ctrl Pts',(1.52855949065065,-3.12604235239462,3.50020588472011));
#96911=CARTESIAN_POINT('Ctrl Pts',(3.45621958157706,-0.403956786608693,
3.65930615220739));
#96912=CARTESIAN_POINT('Ctrl Pts',(2.20824532712176,2.68929125255921,3.81840641969467));
#96913=CARTESIAN_POINT('Ctrl Pts',(-1.06870293299648,3.31157197148184,3.97750668718195));
#96914=CARTESIAN_POINT('Ctrl Pts',(-3.36370845150885,0.891123072362765,
4.13660695466923));
#96915=CARTESIAN_POINT('Ctrl Pts',(-2.56808045450599,-2.34810511994446,
4.2957072221565));
#96916=CARTESIAN_POINT('Ctrl Pts',(0.587144289757969,-3.42985370829862,
4.45480748964379));
#96917=CARTESIAN_POINT('Ctrl Pts',(3.20289070356629,-1.3601933750613,4.61390775713106));
#96918=CARTESIAN_POINT('Ctrl Pts',(2.87576573115885,1.95923616133382,4.77300802461835));
#96919=CARTESIAN_POINT('Ctrl Pts',(-0.0936625436724054,3.47848561943344,
4.93210829210562));
#96920=CARTESIAN_POINT('Ctrl Pts',(-2.97703205310412,1.80164231504339,5.0912085595929));
#96921=CARTESIAN_POINT('Ctrl Pts',(-3.12505301162273,-1.53058111549187,
5.25030882708019));
#96922=CARTESIAN_POINT('Ctrl Pts',(-0.401721201902316,-3.45648013917867,
5.40940909456745));
#96923=CARTESIAN_POINT('Ctrl Pts',(2.69071899761642,-2.20650541636319,5.56850936205474));
#96924=CARTESIAN_POINT('Ctrl Pts',(3.31088003462323,1.07084465395654,5.72760962954202));
#96925=CARTESIAN_POINT('Ctrl Pts',(0.888947219979559,3.36428413138222,5.8867098970293));
#96926=CARTESIAN_POINT('Ctrl Pts',(-2.34976567852831,2.56656114920079,6.04581016451657));
#96927=CARTESIAN_POINT('Ctrl Pts',(-3.42947322235061,-0.589362616524685,
6.20491043200386));
#96928=CARTESIAN_POINT('Ctrl Pts',(-1.35812144206107,-3.2037698146389,6.36401069949113));
#96929=CARTESIAN_POINT('Ctrl Pts',(1.96109581371684,-2.87449788415286,6.52311096697842));
#96930=CARTESIAN_POINT('Ctrl Pts',(3.47842431030683,0.0959124290354176,
6.68221123446568));
#96931=CARTESIAN_POINT('Ctrl Pts',(1.79971637635214,2.97819674321007,6.84131150195298));
#96932=CARTESIAN_POINT('Ctrl Pts',(-1.53260209799175,3.12406236906506,7.00041176944024));
#96933=CARTESIAN_POINT('Ctrl Pts',(-3.45673925178857,0.399485446194586,
7.15951203692754));
#96934=CARTESIAN_POINT('Ctrl Pts',(-2.20476458194314,-2.69214561544991,
7.3186123044148));
#96935=CARTESIAN_POINT('Ctrl Pts',(1.07298592663064,-3.31018671343923,7.47771257190209));
#96936=CARTESIAN_POINT('Ctrl Pts',(3.36485840393263,-0.886770995275038,
7.63681283938936));
#96937=CARTESIAN_POINT('Ctrl Pts',(2.56504077007488,2.35142525384727,7.79591310687664));
#96938=CARTESIAN_POINT('Ctrl Pts',(-0.591580696685175,3.42909130177173,
7.95501337436392));
#96939=CARTESIAN_POINT('Ctrl Pts',(-3.20464758541102,1.35604894081905,8.11411364185121));
#96940=CARTESIAN_POINT('Ctrl Pts',(-2.87322883456653,-1.96295464562801,
8.27321390933847));
#96941=CARTESIAN_POINT('Ctrl Pts',(0.098162274266716,-3.47836154597072,
8.43231417682577));
#96942=CARTESIAN_POINT('Ctrl Pts',(2.97936018736707,-1.79778968472654,8.59141444431303));
#96943=CARTESIAN_POINT('Ctrl Pts',(3.12307041952958,1.53462243931086,8.75051471180032));
#96944=CARTESIAN_POINT('Ctrl Pts',(0.397249523359848,3.45699691824673,8.90961497928758));
#96945=CARTESIAN_POINT('Ctrl Pts',(-2.6935711070035,2.20302282514118,9.06871524677488));
#96946=CARTESIAN_POINT('Ctrl Pts',(-3.30949200741227,-1.07512675041197,
9.22781551426215));
#96947=CARTESIAN_POINT('Ctrl Pts',(-0.884594399583002,-3.3654312687683,
9.38691578174943));
#96948=CARTESIAN_POINT('Ctrl Pts',(2.35308384542899,-2.56351931784376,9.54601604923671));
#96949=CARTESIAN_POINT('Ctrl Pts',(3.42870794660542,0.593798529353127,9.70511631672399));
#96950=CARTESIAN_POINT('Ctrl Pts',(1.35397587226326,3.20552401549357,9.86421658421125));
#96951=CARTESIAN_POINT('Ctrl Pts',(-1.9648126563216,2.87195858294223,10.0233168516986));
#96952=CARTESIAN_POINT('Ctrl Pts',(-3.47829732643462,-0.100412078431024,
10.1824171191858));
#96953=CARTESIAN_POINT('Ctrl Pts',(-1.79586224098147,-2.98052238508522,
10.3415173866731));
#96954=CARTESIAN_POINT('Ctrl Pts',(1.53664213860852,-3.12207716343297,10.5006176541604));
#96955=CARTESIAN_POINT('Ctrl Pts',(3.45725313844298,-0.395013434332659,
10.6597179216477));
#96956=CARTESIAN_POINT('Ctrl Pts',(2.20128014668724,2.69499547168037,10.8188181891349));
#96957=CARTESIAN_POINT('Ctrl Pts',(-1.07726712440552,3.30879591683321,10.9779184566222));
#96958=CARTESIAN_POINT('Ctrl Pts',(-3.36600272564927,0.882417433813924,
11.1370187241095));
#96959=CARTESIAN_POINT('Ctrl Pts',(-2.56199679314412,-2.35474145257953,
11.2961189915968));
#96960=CARTESIAN_POINT('Ctrl Pts',(0.596016113600773,-3.42832315701208,
11.455219259084));
#96961=CARTESIAN_POINT('Ctrl Pts',(3.20639910451986,-1.35190223726101,11.6143195265713));
#96962=CARTESIAN_POINT('Ctrl Pts',(2.87068712981141,1.96666984502031,11.7734197940586));
#96963=CARTESIAN_POINT('Ctrl Pts',(-0.102661840587129,3.47823165172538,
11.9325200615459));
#96964=CARTESIAN_POINT('Ctrl Pts',(-2.98168333587832,1.79393404592325,12.0916203290332));
#96965=CARTESIAN_POINT('Ctrl Pts',(-3.12108260119075,-1.53866119503986,
12.2507205965204));
#96966=CARTESIAN_POINT('Ctrl Pts',(-0.39277718004845,-3.45750791227009,
12.4098208640077));
#96967=CARTESIAN_POINT('Ctrl Pts',(2.69641870888462,-2.19953654731037,12.568921131495));
#96968=CARTESIAN_POINT('Ctrl Pts',(3.30809844199328,1.07940704771587,12.7280213989823));
#96969=CARTESIAN_POINT('Ctrl Pts',(0.880240098878547,3.36657277433645,12.8871216664696));
#96970=CARTESIAN_POINT('Ctrl Pts',(-2.3563980746054,2.56047319661288,13.0462219339568));
#96971=CARTESIAN_POINT('Ctrl Pts',(-3.42793693315271,-0.598233448500373,
13.2053222014441));
#96972=CARTESIAN_POINT('Ctrl Pts',(-1.34982803667978,-3.2072728521238,13.3644224689314));
#96973=CARTESIAN_POINT('Ctrl Pts',(1.96852621094718,-2.86941447570597,13.5235227364187));
#96974=CARTESIAN_POINT('Ctrl Pts',(3.47816452187051,0.104911559793856,13.6826230039059));
#96975=CARTESIAN_POINT('Ctrl Pts',(1.79200510035857,2.98284303926069,13.8417232713933));
#96976=CARTESIAN_POINT('Ctrl Pts',(-1.54067960776015,3.12008673321898,14.0008235388805));
#96977=CARTESIAN_POINT('Ctrl Pts',(-3.45776123962148,0.390540761442825,
14.1599238063678));
#96978=CARTESIAN_POINT('Ctrl Pts',(-2.19779202774005,-2.69784081802083,
14.3190240738551));
#96979=CARTESIAN_POINT('Ctrl Pts',(1.08154651944778,-3.30739958318427,14.4781243413423));
#96980=CARTESIAN_POINT('Ctrl Pts',(3.36714141459133,-0.87806239568778,14.6372246088297));
#96981=CARTESIAN_POINT('Ctrl Pts',(2.5589485288875,2.35805371081355,14.7963248763169));
#96982=CARTESIAN_POINT('Ctrl Pts',(-0.600450533124296,3.42754927518888,
14.9554251438042));
#96983=CARTESIAN_POINT('Ctrl Pts',(-3.20814525793984,1.34775327138733,15.1145254112915));
#96984=CARTESIAN_POINT('Ctrl Pts',(-2.86814062115834,-1.9703817533256,15.2736256787788));
#96985=CARTESIAN_POINT('Ctrl Pts',(0.107161235110024,-3.47809593689805,
15.432725946266));
#96986=CARTESIAN_POINT('Ctrl Pts',(2.98400149474715,-1.79007540509441,15.5918262137533));
#96987=CARTESIAN_POINT('Ctrl Pts',(3.11908955993432,1.54269737592496,15.7509264812406));
#96988=CARTESIAN_POINT('Ctrl Pts',(0.388304179451396,3.45801312039119,15.9100267487279));
#96989=CARTESIAN_POINT('Ctrl Pts',(-2.69926179849407,2.1960465887061,16.0691270162151));
#96990=CARTESIAN_POINT('Ctrl Pts',(-3.30669934069854,-1.08368553870617,
16.2282272837024));
#96991=CARTESIAN_POINT('Ctrl Pts',(-0.875884325152688,-3.36770864617604,
16.3873275511897));
#96992=CARTESIAN_POINT('Ctrl Pts',(2.35970836051133,-2.55742279060582,16.546427818677));
#96993=CARTESIAN_POINT('Ctrl Pts',(3.42716018328277,0.60266736654502,16.7055280861643));
#96994=CARTESIAN_POINT('Ctrl Pts',(1.34567794225167,3.20901632160298,16.8646283536515));
#96995=CARTESIAN_POINT('Ctrl Pts',(-1.97223647137926,2.86686556670147,17.0237286211388));
#96996=CARTESIAN_POINT('Ctrl Pts',(-3.47802589683674,-0.109410865594434,
17.1828288886261));
#96997=CARTESIAN_POINT('Ctrl Pts',(-1.78814496093809,-2.98515870185301,
17.3419291561134));
#96998=CARTESIAN_POINT('Ctrl Pts',(1.54471449869015,-3.11809108175395,17.5010294236007));
#96999=CARTESIAN_POINT('Ctrl Pts',(3.45826355447384,-0.386067435009841,
17.6601296910879));
#97000=CARTESIAN_POINT('Ctrl Pts',(2.19430023093872,2.70068164970982,17.8192299585752));
#97001=CARTESIAN_POINT('Ctrl Pts',(-1.08582410459616,3.30599771482907,17.9783302260625));
#97002=CARTESIAN_POINT('Ctrl Pts',(-3.36827446885328,0.873705888184473,
18.1374304935498));
#97003=CARTESIAN_POINT('Ctrl Pts',(-2.55589598240612,-2.3613620230065,18.2965307610371));
#97004=CARTESIAN_POINT('Ctrl Pts',(0.604883947835077,-3.42676965759715,
18.4556310285243));
#97005=CARTESIAN_POINT('Ctrl Pts',(3.20988604274885,-1.34360205014104,18.6147312960116));
#97006=CARTESIAN_POINT('Ctrl Pts',(2.86558931286877,1.97409036433223,18.7738315634989));
#97007=CARTESIAN_POINT('Ctrl Pts',(-0.111660450305955,3.47795440171584,
18.9329318309861));
#97008=CARTESIAN_POINT('Ctrl Pts',(-2.98631466009421,1.7862137686972,19.0920320984735));
#97009=CARTESIAN_POINT('Ctrl Pts',(-3.11709129909556,-1.54673097521187,
19.2511323659607));
#97010=CARTESIAN_POINT('Ctrl Pts',(-0.383830529053899,-3.45851254176464,
19.410232633448));
#97011=CARTESIAN_POINT('Ctrl Pts',(2.70210037107411,-2.1925529551685,19.5693329009353));
#97012=CARTESIAN_POINT('Ctrl Pts',(3.30529470586936,1.08796221622309,19.7284331684226));
#97013=CARTESIAN_POINT('Ctrl Pts',(0.871527085694471,3.36883888238634,19.8875334359098));
#97014=CARTESIAN_POINT('Ctrl Pts',(-2.36301469760723,2.55436810492716,20.0466337033971));
#97015=CARTESIAN_POINT('Ctrl Pts',(-3.42637769829543,-0.607100276067174,
20.2057339708844));
#97016=CARTESIAN_POINT('Ctrl Pts',(-1.34152559592387,-3.21075442101357,
20.3648342383717));
#97017=CARTESIAN_POINT('Ctrl Pts',(1.97594343140896,-2.86431186019415,20.5239345058589));
#97018=CARTESIAN_POINT('Ctrl Pts',(3.47788145156528,0.113909988303468,20.6830347733463));
#97019=CARTESIAN_POINT('Ctrl Pts',(1.78428182917969,2.9874693689871,20.8421350408335));
#97020=CARTESIAN_POINT('Ctrl Pts',(-1.54874680464648,3.11609021237743,21.0012353083208));
#97021=CARTESIAN_POINT('Ctrl Pts',(-3.45876008215943,0.381593462519445,
21.1603355758081));
#97022=CARTESIAN_POINT('Ctrl Pts',(-2.19080476212648,-2.7035179619934,21.3194358432953));
#97023=CARTESIAN_POINT('Ctrl Pts',(1.09009987269245,-3.30459031411354,21.4785361107827));
#97024=CARTESIAN_POINT('Ctrl Pts',(3.36940188653905,-0.869347918594261,
21.6376363782699));
#97025=CARTESIAN_POINT('Ctrl Pts',(2.55283915880816,2.36466638362217,21.7967366457572));
#97026=CARTESIAN_POINT('Ctrl Pts',(-0.609316350314126,3.42598430554155,
21.9558369132444));
#97027=CARTESIAN_POINT('Ctrl Pts',(-3.21162145603384,1.33944858046886,22.1149371807317));
#97028=CARTESIAN_POINT('Ctrl Pts',(-2.86303320921208,-1.97779567183414,
22.274037448219));
#97029=CARTESIAN_POINT('Ctrl Pts',(0.116159478645818,-3.47780704641558,
22.4331377157063));
#97030=CARTESIAN_POINT('Ctrl Pts',(2.98862282804862,-1.7823491431938,22.5922379831935));
#97031=CARTESIAN_POINT('Ctrl Pts',(3.11508782201838,1.55076198615064,22.7513382506809));
#97032=CARTESIAN_POINT('Ctrl Pts',(0.379356236342356,3.45900617555466,22.9104385181681));
#97033=CARTESIAN_POINT('Ctrl Pts',(-2.70493442187461,2.189055652544,23.0695387856555));
#97034=CARTESIAN_POINT('Ctrl Pts',(-3.30388453985629,-1.09223707310991,
23.2286390531427));
#97035=CARTESIAN_POINT('Ctrl Pts',(-0.867168387795486,-3.36996348107591,
23.38773932063));
#97036=CARTESIAN_POINT('Ctrl Pts',(2.3663170803602,-2.55130914468877,23.5468395881172));
#97037=CARTESIAN_POINT('Ctrl Pts',(3.42558947950012,0.611532169648694,23.7059398556046));
#97038=CARTESIAN_POINT('Ctrl Pts',(1.33737100464502,3.21248714744695,23.8650401230918));
#97039=CARTESIAN_POINT('Ctrl Pts',(-1.97964708483286,2.86175336045749,24.0241403905791));
#97040=CARTESIAN_POINT('Ctrl Pts',(-3.47773118629787,-0.118408920391893,
24.1832406580664));
#97041=CARTESIAN_POINT('Ctrl Pts',(-1.78041571154812,-2.98977503679619,
24.3423409255536));
#97042=CARTESIAN_POINT('Ctrl Pts',(1.55277651888125,-3.11408412843777,24.5014411930409));
#97043=CARTESIAN_POINT('Ctrl Pts',(3.45925082184736,-0.377118851458631,
24.6605414605282));
#97044=CARTESIAN_POINT('Ctrl Pts',(2.18730562715285,2.70634975012517,24.8196417280154));
#97045=CARTESIAN_POINT('Ctrl Pts',(-1.09437381658139,3.30317738339288,24.9787419955028));
#97046=CARTESIAN_POINT('Ctrl Pts',(-3.37052366576197,0.864988494209978,
25.13784226299));
#97047=CARTESIAN_POINT('Ctrl Pts',(-2.54977806320906,-2.36796678713085,
25.2969425304773));
#97048=CARTESIAN_POINT('Ctrl Pts',(0.613747733143994,-3.4251932203363,25.4560427979646));
#97049=CARTESIAN_POINT('Ctrl Pts',(3.21335149489072,-1.33529286932145,25.6151430654519));
#97050=CARTESIAN_POINT('Ctrl Pts',(2.86047231446579,1.98149766963065,25.7742433329392));
#97051=CARTESIAN_POINT('Ctrl Pts',(-0.120658312600698,3.47765387124387,
25.9333436004265));
#97052=CARTESIAN_POINT('Ctrl Pts',(-2.9909259947478,1.77848153505145,26.0924438679137));
#97053=CARTESIAN_POINT('Ctrl Pts',(-3.11307913205549,-1.5547904019956,26.251544135401));
#97054=CARTESIAN_POINT('Ctrl Pts',(-0.374881308804223,-3.45949402093519,
26.4106444028883));
#97055=CARTESIAN_POINT('Ctrl Pts',(2.70776394615297,-2.1855546866851,26.5697446703756));
#97056=CARTESIAN_POINT('Ctrl Pts',(3.30246884501914,1.0965101022129,26.7288449378628));
#97057=CARTESIAN_POINT('Ctrl Pts',(0.862808238749752,3.37108244036284,26.8879452053501));
#97058=CARTESIAN_POINT('Ctrl Pts',(-2.36961550324391,2.54824591500962,27.0470454728374));
#97059=CARTESIAN_POINT('Ctrl Pts',(-3.42479552821586,-0.61596303987306,
27.2061457403247));
#97060=CARTESIAN_POINT('Ctrl Pts',(-1.33321417536761,-3.21421449800351,
27.365246007812));
#97061=CARTESIAN_POINT('Ctrl Pts',(1.98334742545324,-2.85919007177297,27.5243462752992));
#97062=CARTESIAN_POINT('Ctrl Pts',(3.47757510128594,0.122907654331153,27.6834465427865));
#97063=CARTESIAN_POINT('Ctrl Pts',(1.77654661451301,2.99207570142192,27.8425468102738));
#97064=CARTESIAN_POINT('Ctrl Pts',(-1.55680363465111,3.112072833292,28.0016470777611));
#97065=CARTESIAN_POINT('Ctrl Pts',(-3.45973577271641,0.372643609315264,
28.1607473452483));
#97066=CARTESIAN_POINT('Ctrl Pts',(-2.18380283187331,-2.70917700936636,
28.3198476127356));
#97067=CARTESIAN_POINT('Ctrl Pts',(1.0986459291108,-3.30175892503151,28.4789478802229));
#97068=CARTESIAN_POINT('Ctrl Pts',(3.37163980464479,-0.860627622326853,
28.6380481477102));
#97069=CARTESIAN_POINT('Ctrl Pts',(2.54671270073136,2.37126322800964,28.7971484151974));
#97070=CARTESIAN_POINT('Ctrl Pts',(-0.618178088909158,3.4243964033052,28.9562486826848));
#97071=CARTESIAN_POINT('Ctrl Pts',(-3.21507615642433,1.33113492365306,29.115348950172));
#97072=CARTESIAN_POINT('Ctrl Pts',(-2.85790663291539,-1.9851963515268,29.2744492176593));
#97073=CARTESIAN_POINT('Ctrl Pts',(0.125156944642189,-3.47749487645702,
29.4335494851466));
#97074=CARTESIAN_POINT('Ctrl Pts',(2.99322415633754,-1.77461095074231,29.5926497526339));
#97075=CARTESIAN_POINT('Ctrl Pts',(3.11106523256831,1.55881621600552,29.7517500201211));
#97076=CARTESIAN_POINT('Ctrl Pts',(0.370405753927932,3.45997607708985,29.9108502876084));
#97077=CARTESIAN_POINT('Ctrl Pts',(-2.71058893917414,2.1820500634504,30.0699505550957));
#97078=CARTESIAN_POINT('Ctrl Pts',(-3.30104762372702,-1.10078129638149,
30.2290508225829));
#97079=CARTESIAN_POINT('Ctrl Pts',(-0.858446645853591,-3.37219575837462,
30.3881510900703));
#97080=CARTESIAN_POINT('Ctrl Pts',(2.37290996073868,-2.54517842101576,30.5472513575575));
#97081=CARTESIAN_POINT('Ctrl Pts',(3.4239958457713,0.620392879325578,30.7063516250448));
#97082=CARTESIAN_POINT('Ctrl Pts',(1.32905511504771,3.21593646979268,30.8654518925321));
#97083=CARTESIAN_POINT('Ctrl Pts',(-1.9870444470778,2.85662199843003,31.0245521600194));
#97084=CARTESIAN_POINT('Ctrl Pts',(-3.4774131967907,-0.12740618259286,31.1836524275066));
#97085=CARTESIAN_POINT('Ctrl Pts',(-1.77267454454907,-2.99437135901425,
31.3427526949939));
#97086=CARTESIAN_POINT('Ctrl Pts',(1.56082814521689,-3.11005633030592,31.5018529624812));
#97087=CARTESIAN_POINT('Ctrl Pts',(3.46021493395502,-0.368167743578406,
31.6609532299685));
#97088=CARTESIAN_POINT('Ctrl Pts',(2.18029638214961,2.71199973498569,31.8200534974558));
#97089=CARTESIAN_POINT('Ctrl Pts',(-1.10291620313167,3.30033494140318,31.979153764943));
#97090=CARTESIAN_POINT('Ctrl Pts',(-3.37275030131974,0.856265310242433,
32.1382540324303));
#97091=CARTESIAN_POINT('Ctrl Pts',(-2.54364307650471,-2.37455570074209,
32.2973542999176));
#97092=CARTESIAN_POINT('Ctrl Pts',(0.622607410195718,-3.42359385578174,
32.4564545674049));
#97093=CARTESIAN_POINT('Ctrl Pts',(3.21679543774861,-1.3269747504217,32.6155548348921));
#97094=CARTESIAN_POINT('Ctrl Pts',(2.85533616885434,1.98889171133305,32.7746551023795));
#97095=CARTESIAN_POINT('Ctrl Pts',(-0.12965536724212,3.47733006232115,32.9337553698667));
#97096=CARTESIAN_POINT('Ctrl Pts',(-2.99551730897204,1.77073739674347,33.092855637354));
#97097=CARTESIAN_POINT('Ctrl Pts',(-3.10904612692694,-1.56283942144345,
33.2519559048413));
#97098=CARTESIAN_POINT('Ctrl Pts',(-0.36592957920303,-3.460452343212,33.4110561723285));
#97099=CARTESIAN_POINT('Ctrl Pts',(2.71340939621074,-2.17854178870462,33.5701564398158));
#97100=CARTESIAN_POINT('Ctrl Pts',(3.29962087835819,1.10505064846814,33.7292567073031));
#97101=CARTESIAN_POINT('Ctrl Pts',(0.8540836164059,3.37330343324819,33.8883569747904));
#97102=CARTESIAN_POINT('Ctrl Pts',(-2.37620044733142,2.54210666784049,34.0474572422777));
#97103=CARTESIAN_POINT('Ctrl Pts',(-3.42319043350467,-0.624821680593156,
34.2065575097649));
#97104=CARTESIAN_POINT('Ctrl Pts',(-1.3248938306453,-3.21765305993281,34.3656577772522));
#97105=CARTESIAN_POINT('Ctrl Pts',(1.9907381435198,-2.85404914472622,34.5247580447395));
#97106=CARTESIAN_POINT('Ctrl Pts',(3.47724547308312,0.131904497649062,34.6838583122268));
#97107=CARTESIAN_POINT('Ctrl Pts',(1.76879950813591,2.99666200573157,34.8429585797141));
#97108=CARTESIAN_POINT('Ctrl Pts',(-1.56485004384385,3.10803462285397,35.0020588472013));
#97109=CARTESIAN_POINT('Ctrl Pts',(-3.46068830476142,0.363691261738097,
35.1611591146886));
#97110=CARTESIAN_POINT('Ctrl Pts',(-2.17678628384951,-2.71481792225954,
35.3202593821759));
#97111=CARTESIAN_POINT('Ctrl Pts',(1.10718463149792,-3.29890543489078,35.4793596496632));
#97112=CARTESIAN_POINT('Ctrl Pts',(3.37385515392854,-0.851901565256779,
35.6384599171505));
#97113=CARTESIAN_POINT('Ctrl Pts',(2.54056919566589,2.37784419981852,35.7975601846377));
#97114=CARTESIAN_POINT('Ctrl Pts',(-0.627035689591476,3.42278557910887,
35.956660452125));
#97115=CARTESIAN_POINT('Ctrl Pts',(-3.21850933598648,1.32281235658916,36.1157607196123));
#97116=CARTESIAN_POINT('Ctrl Pts',(-2.85276092658412,-1.99258374286554,
36.2748609870995));
#97117=CARTESIAN_POINT('Ctrl Pts',(0.134153572872717,-3.47715942911201,
36.4339612545869));
#97118=CARTESIAN_POINT('Ctrl Pts',(2.99780544881391,-1.76686087953711,36.5930615220741));
#97119=CARTESIAN_POINT('Ctrl Pts',(3.10702181851019,1.56686001157689,36.7521617895614));
#97120=CARTESIAN_POINT('Ctrl Pts',(0.361452792120057,3.46092281850458,36.9112620570486));
#97121=CARTESIAN_POINT('Ctrl Pts',(-2.71622531254288,2.17502986831866,37.070362324536));
#97122=CARTESIAN_POINT('Ctrl Pts',(-3.29818861130025,-1.10931815132831,
37.2294625920232));
#97123=CARTESIAN_POINT('Ctrl Pts',(-0.849719157707888,-3.37440546312996,
37.3885628595105));
#97124=CARTESIAN_POINT('Ctrl Pts',(2.37948695751577,-2.53903066062412,37.5476631269978));
#97125=CARTESIAN_POINT('Ctrl Pts',(3.42237929276372,0.629249436264508,37.7067633944851));
#97126=CARTESIAN_POINT('Ctrl Pts',(1.32073032912399,3.21936426555138,37.8658636619724));
#97127=CARTESIAN_POINT('Ctrl Pts',(-1.99442850859811,2.85147151496698,38.0249639294596));
#97128=CARTESIAN_POINT('Ctrl Pts',(-3.47707193044383,-0.136402591972126,
38.1840641969469));
#97129=CARTESIAN_POINT('Ctrl Pts',(-1.76492151175815,-2.99894763774068,
38.3431644644342));
#97130=CARTESIAN_POINT('Ctrl Pts',(1.56886932380165,-3.10600771431932,38.5022647319215));
#97131=CARTESIAN_POINT('Ctrl Pts',(3.46115588434339,-0.359214171285433,
38.6613649994088));
#97132=CARTESIAN_POINT('Ctrl Pts',(2.17327254284694,2.71763156647193,38.820465266896));
#97133=CARTESIAN_POINT('Ctrl Pts',(-1.11145120706667,3.29747040788648,38.9795655343833));
#97134=CARTESIAN_POINT('Ctrl Pts',(-3.37495436062222,0.847536394672323,
39.1386658018706));
#97135=CARTESIAN_POINT('Ctrl Pts',(-2.53749106335888,-2.38112871973583,
39.2977660693578));
#97136=CARTESIAN_POINT('Ctrl Pts',(0.631462919686039,-3.4219715746392,39.4568663368451));
#97137=CARTESIAN_POINT('Ctrl Pts',(3.22021784826983,-1.31864774912091,39.6159666043324));
#97138=CARTESIAN_POINT('Ctrl Pts',(2.85018091041424,1.99627243994583,39.7750668718197));
#97139=CARTESIAN_POINT('Ctrl Pts',(-0.138651554006447,3.47698297711515,
39.934167139307));
#97140=CARTESIAN_POINT('Ctrl Pts',(-3.00008857203401,1.76298140561038,40.0932674067942));
#97141=CARTESIAN_POINT('Ctrl Pts',(-3.10499231070567,-1.57087797967749,
40.2523676742816));
#97142=CARTESIAN_POINT('Ctrl Pts',(-0.356975400170752,-3.46138750218032,
40.4114679417688));
#97143=CARTESIAN_POINT('Ctrl Pts',(2.71903668345837,-2.17151430816952,40.5705682092561));
#97144=CARTESIAN_POINT('Ctrl Pts',(3.29675082494996,1.11358379782068,40.7296684767434));
#97145=CARTESIAN_POINT('Ctrl Pts',(0.845353277063212,3.37550184617569,40.8887687442307));
#97146=CARTESIAN_POINT('Ctrl Pts',(-2.382769485792,2.53595040451421,41.0478690117179));
#97147=CARTESIAN_POINT('Ctrl Pts',(-3.42156242490587,-0.633676138930166,
41.2069692792052));
#97148=CARTESIAN_POINT('Ctrl Pts',(-1.31656461745104,-3.22107008378474,
41.3660695466925));
#97149=CARTESIAN_POINT('Ctrl Pts',(1.99811553613721,-2.84888911346582,41.5251698141798));
#97150=CARTESIAN_POINT('Ctrl Pts',(3.47689256916324,0.140900458034825,41.684270081667));
#97151=CARTESIAN_POINT('Ctrl Pts',(1.76104056190537,3.00122825121666,41.8433703491544));
#97152=CARTESIAN_POINT('Ctrl Pts',(-1.5728859783643,3.10397560809395,42.0024706166416));
#97153=CARTESIAN_POINT('Ctrl Pts',(-3.4616176719185,0.354736479712447,42.1615708841289));
#97154=CARTESIAN_POINT('Ctrl Pts',(-2.16975516502185,-2.72044066291438,
42.3206711516162));
#97155=CARTESIAN_POINT('Ctrl Pts',(1.11571592269813,-3.29602986279173,42.4797714191035));
#97156=CARTESIAN_POINT('Ctrl Pts',(3.37604791956135,-0.843169805793855,
42.6388716865907));
#97157=CARTESIAN_POINT('Ctrl Pts',(2.53440868473468,2.38440925499764,42.797971954078));
#97158=CARTESIAN_POINT('Ctrl Pts',(-0.635889093070747,3.42115184373492,
42.9570722215653));
#97159=CARTESIAN_POINT('Ctrl Pts',(-3.22192097173958,1.31448093498611,43.1161724890526));
#97160=CARTESIAN_POINT('Ctrl Pts',(-2.84759612466217,-1.99995779640121,
43.2752727565398));
#97161=CARTESIAN_POINT('Ctrl Pts',(0.143149303116361,-3.47680070662587,
43.4343730240271));
#97162=CARTESIAN_POINT('Ctrl Pts',(3.00236667481184,-1.75909898145519,43.5934732915144));
#97163=CARTESIAN_POINT('Ctrl Pts',(3.10295760690946,1.57489331902183,43.7525735590017));
#97164=CARTESIAN_POINT('Ctrl Pts',(0.352497410847578,3.46184639346149,43.911673826489));
#97165=CARTESIAN_POINT('Ctrl Pts',(-2.72184350425287,2.16799511414025,44.0707740939763));
#97166=CARTESIAN_POINT('Ctrl Pts',(-3.29530752171281,-1.1178475808074,44.2298743614635));
#97167=CARTESIAN_POINT('Ctrl Pts',(-0.840985981778881,-3.37659258055,44.3889746289508));
#97168=CARTESIAN_POINT('Ctrl Pts',(2.38604802666906,-2.53286590466669,44.548074896438));
#97169=CARTESIAN_POINT('Ctrl Pts',(3.42073983129402,0.638101781184889,44.7071751639254));
#97170=CARTESIAN_POINT('Ctrl Pts',(1.31239670260541,3.2227705117732,44.8662754314126));
#97171=CARTESIAN_POINT('Ctrl Pts',(-2.0017992199819,2.84630194455405,45.0253756988999));
#97172=CARTESIAN_POINT('Ctrl Pts',(-3.47670738951322,-0.145398088329049,
45.1844759663872));
#97173=CARTESIAN_POINT('Ctrl Pts',(-1.757156665126,-3.00350384230738,45.3435762338744));
#97174=CARTESIAN_POINT('Ctrl Pts',(1.57690000091316,-3.10193830764655,45.5026765013618));
#97175=CARTESIAN_POINT('Ctrl Pts',(3.46207366651742,-0.350258194382263,
45.661776768849));
#97176=CARTESIAN_POINT('Ctrl Pts',(2.16623415663537,2.72324520663779,45.8208770363364));
#97177=CARTESIAN_POINT('Ctrl Pts',(-1.11997877197074,3.29458380249072,45.9799773038235));
#97178=CARTESIAN_POINT('Ctrl Pts',(-3.37713582755165,0.838801805025182,
46.1390775713109));
#97179=CARTESIAN_POINT('Ctrl Pts',(-2.53132206755406,-2.38768579839091,
46.2981778387981));
#97180=CARTESIAN_POINT('Ctrl Pts',(0.640314207303564,-3.42032639105517,
46.4572781062854));
#97181=CARTESIAN_POINT('Ctrl Pts',(3.22361869407457,-1.31031191488652,46.6163783737727));
#97182=CARTESIAN_POINT('Ctrl Pts',(2.84500659172074,2.00363979410143,46.77547864126));
#97183=CARTESIAN_POINT('Ctrl Pts',(-0.147646847141617,3.47661264077023,
46.9345789087473));
#97184=CARTESIAN_POINT('Ctrl Pts',(-3.00463968758686,1.75521357003441,47.0936791762345));
#97185=CARTESIAN_POINT('Ctrl Pts',(-3.10091783594993,-1.57890593984303,
47.2527794437217));
#97186=CARTESIAN_POINT('Ctrl Pts',(-0.348018592382841,-3.46229965000353,
47.4118797112091));
#97187=CARTESIAN_POINT('Ctrl Pts',(2.72464531380624,-2.16447198990683,47.5709799786964));
#97188=CARTESIAN_POINT('Ctrl Pts',(3.29385957469109,1.1221089166414,47.7300802461837));
#97189=CARTESIAN_POINT('Ctrl Pts',(0.836615618213322,3.37767876419982,47.8891805136709));
#97190=CARTESIAN_POINT('Ctrl Pts',(-2.3893194061801,2.52977506828308,48.0482807811582));
#97191=CARTESIAN_POINT('Ctrl Pts',(-3.41991755759816,-0.642522353487716,
48.2073810486454));
#97192=CARTESIAN_POINT('Ctrl Pts',(-1.30821506127625,-3.22447318127091,
48.3664813161328));
#97193=CARTESIAN_POINT('Ctrl Pts',(2.0054575584248,-2.84369544855116,48.52558158362));
#97194=CARTESIAN_POINT('Ctrl Pts',(3.47655835125671,0.14986769250252,48.6846818511074));
#97195=CARTESIAN_POINT('Ctrl Pts',(1.75318978419848,3.00582740713737,48.8437821185946));
#97196=CARTESIAN_POINT('Ctrl Pts',(-1.58075868601436,3.09979470731945,49.0028823860818));
#97197=CARTESIAN_POINT('Ctrl Pts',(-3.46281520229328,0.345972243077007,
49.1619826535692));
#97198=CARTESIAN_POINT('Ctrl Pts',(-2.16215339527527,-2.72641357726118,
49.3210829210564));
#97199=CARTESIAN_POINT('Ctrl Pts',(1.12317562685709,-3.29242630007822,49.4801831885437));
#97200=CARTESIAN_POINT('Ctrl Pts',(3.38027638470318,-0.83580699739451,49.639283456031));
#97201=CARTESIAN_POINT('Ctrl Pts',(2.52405647169005,2.39382388417745,49.7983837235182));
#97202=CARTESIAN_POINT('Ctrl Pts',(0.418252623626215,3.0726983587025,49.9044505685098));
#97203=CARTESIAN_POINT('Ctrl Pts',(-0.545102916881406,2.89105980740755,
49.9574839910056));
#97204=CARTESIAN_POINT('Ctrl Pts',(-2.943409633743,-0.00255526730400832,
48.1778238829104));
#97205=CARTESIAN_POINT('Ctrl Pts',(-2.94507379928574,-0.184399871474338,
48.1876762714888));
#97206=CARTESIAN_POINT('Ctrl Pts',(-2.92967483134683,-0.36596345305782,
48.1975286600671));
#97207=CARTESIAN_POINT('Ctrl Pts',(-2.89620078297484,-0.544131254489774,
48.2073810486455));
#97208=CARTESIAN_POINT('Ctrl Pts',(-2.71601672549087,-1.50317262941543,
48.2604144711412));
#97209=CARTESIAN_POINT('Ctrl Pts',(-2.01211589338358,-2.36382290534315,
48.313447893637));
#97210=CARTESIAN_POINT('Ctrl Pts',(-1.10788670737978,-2.73068508785373,
48.3664813161328));
#97211=CARTESIAN_POINT('Ctrl Pts',(-0.203657521375925,-3.09754727036433,
48.4195147386285));
#97212=CARTESIAN_POINT('Ctrl Pts',(0.900900018524468,-2.97062135945774,
48.4725481611243));
#97213=CARTESIAN_POINT('Ctrl Pts',(1.69836225394665,-2.4082312138288,48.52558158362));
#97214=CARTESIAN_POINT('Ctrl Pts',(2.49582448936878,-1.8458410681999,48.5786150061158));
#97215=CARTESIAN_POINT('Ctrl Pts',(2.98619142031275,-0.847986687848688,
48.6316484286116));
#97216=CARTESIAN_POINT('Ctrl Pts',(2.94414679127502,0.126933788099391,48.6846818511073));
#97217=CARTESIAN_POINT('Ctrl Pts',(2.9021021622373,1.10185426404747,48.7377152736031));
#97218=CARTESIAN_POINT('Ctrl Pts',(2.32764597321789,2.05384083559242,48.7907486960988));
#97219=CARTESIAN_POINT('Ctrl Pts',(1.48475980033937,2.54549533806191,48.8437821185946));
#97220=CARTESIAN_POINT('Ctrl Pts',(0.641873627460864,3.0371498405314,48.8968155410903));
#97221=CARTESIAN_POINT('Ctrl Pts',(-0.469442529276749,3.06847227392542,
48.9498489635861));
#97222=CARTESIAN_POINT('Ctrl Pts',(-1.33877669369204,2.62516307991536,49.0028823860819));
#97223=CARTESIAN_POINT('Ctrl Pts',(-1.63994290539553,2.47158605966431,49.0212549240546));
#97224=CARTESIAN_POINT('Ctrl Pts',(-1.91206741640369,2.26104566981987,49.0396274620273));
#97225=CARTESIAN_POINT('Ctrl Pts',(-2.1431563177438,2.01106840053142,49.0580000000001));
#97226=CARTESIAN_POINT('Ctrl Pts',(-1.3800144223764,-1.93381244560185,-1.49186218934005E-16));
#97227=CARTESIAN_POINT('Ctrl Pts',(-1.42855884494822,-1.90739843349394,
-1.70198841695918E-16));
#97228=CARTESIAN_POINT('Ctrl Pts',(-1.47602780810136,-1.87922026048844,
-6.28080395559761E-17));
#97229=CARTESIAN_POINT('Ctrl Pts',(-1.52231351314505,-1.84929882574418,
-5.72458747072346E-17));
#97230=CARTESIAN_POINT('Ctrl Pts',(-1.59072873207763,-1.80507174727851,
-2.99424423574721E-17));
#97231=CARTESIAN_POINT('Ctrl Pts',(-1.65656007365294,-1.7570385764509,1.23091517206865E-16));
#97232=CARTESIAN_POINT('Ctrl Pts',(-1.7197220395774,-1.70555950061155,9.0205620750794E-17));
#97233=CARTESIAN_POINT('Ctrl Pts',(-1.75666514687009,-1.67544965532371,
7.09708299489081E-17));
#97234=CARTESIAN_POINT('Ctrl Pts',(-1.79269476886278,-1.64415997886869,
-2.72191750387666E-16));
#97235=CARTESIAN_POINT('Ctrl Pts',(-1.82779071816502,-1.6117550919015,-2.98372437868011E-16));
#97236=CARTESIAN_POINT('Ctrl Pts',(-1.84338700953533,-1.59735468191086,
-3.10006875412424E-16));
#97237=CARTESIAN_POINT('Ctrl Pts',(-1.85879888268092,-1.58273396999838,
2.67280072439625E-17));
#97238=CARTESIAN_POINT('Ctrl Pts',(-1.87402439060531,-1.5678983186799,4.85722573273506E-17));
#97239=CARTESIAN_POINT('Ctrl Pts',(-1.88610726792344,-1.55612482936802,
6.59077311371403E-17));
#97240=CARTESIAN_POINT('Ctrl Pts',(-1.89807318870411,-1.54421540327689,
-6.57475537402881E-16));
#97241=CARTESIAN_POINT('Ctrl Pts',(-1.9099098864946,-1.53218449300995,-6.24500451351651E-16));
#97242=CARTESIAN_POINT('Ctrl Pts',(-1.96985570454349,-1.47125510454453,
-4.57501298077507E-16));
#97243=CARTESIAN_POINT('Ctrl Pts',(-2.02656004093552,-1.40714582547612,
-1.46167834437222E-16));
#97244=CARTESIAN_POINT('Ctrl Pts',(-2.07992731810956,-1.34024875153828,
-5.55111512312578E-17));
#97245=CARTESIAN_POINT('Ctrl Pts',(-2.12630479673919,-1.28211354619851,
2.3271739908326E-17));
#97246=CARTESIAN_POINT('Ctrl Pts',(-2.17016203790517,-1.22187184995567,
-9.84142147220768E-17));
#97247=CARTESIAN_POINT('Ctrl Pts',(-2.21142070906362,-1.15975295612777,
-6.93889390390723E-17));
#97248=CARTESIAN_POINT('Ctrl Pts',(-2.23103383926374,-1.13022350405562,
-5.55911967686331E-17));
#97249=CARTESIAN_POINT('Ctrl Pts',(-2.25005951597988,-1.10026950536354,
4.3764560536828E-17));
#97250=CARTESIAN_POINT('Ctrl Pts',(-2.26848790511312,-1.06991389685038,
6.93889390390723E-17));
#97251=CARTESIAN_POINT('Ctrl Pts',(-2.27568158581329,-1.05806432315601,
7.93916362771505E-17));
#97252=CARTESIAN_POINT('Ctrl Pts',(-2.28278479302695,-1.04615259821836,
-6.14134180165296E-16));
#97253=CARTESIAN_POINT('Ctrl Pts',(-2.28979518299867,-1.03418298191949,
-5.96744875736022E-16));
#97254=CARTESIAN_POINT('Ctrl Pts',(-2.33451667273546,-0.957825022572966,
-4.85813015639582E-16));
#97255=CARTESIAN_POINT('Ctrl Pts',(-2.37532290647229,-0.879355576208141,
3.37797804077662E-17));
#97256=CARTESIAN_POINT('Ctrl Pts',(-2.41211780815156,-0.79917323765487,
4.16333634234434E-17));
#97257=CARTESIAN_POINT('Ctrl Pts',(-2.44958736980381,-0.717520700462878,
4.96309473159603E-17));
#97258=CARTESIAN_POINT('Ctrl Pts',(-2.48289779686268,-0.634091186714558,
-9.2208182772125E-17));
#97259=CARTESIAN_POINT('Ctrl Pts',(-2.51191518147983,-0.549262804099503,
2.77555756156289E-17));
#97260=CARTESIAN_POINT('Ctrl Pts',(-2.54089888650409,-0.464532879199711,
1.47580095729576E-16));
#97261=CARTESIAN_POINT('Ctrl Pts',(-2.5656000783497,-0.378406464546764,
1.91681516741294E-16));
#97262=CARTESIAN_POINT('Ctrl Pts',(-2.58584421344203,-0.29123000762658,
2.77555756156289E-16));
#97263=CARTESIAN_POINT('Ctrl Pts',(-2.59738512851483,-0.241531856479369,
3.26511530236505E-16));
#97264=CARTESIAN_POINT('Ctrl Pts',(-2.60747670761929,-0.191491957172924,
-3.4674691487661E-16));
#97265=CARTESIAN_POINT('Ctrl Pts',(-2.6160795223077,-0.141171741385976,
-4.44089209850063E-16));
#97266=CARTESIAN_POINT('Ctrl Pts',(-2.61852700899685,-0.126855722409087,
-4.71782933342707E-16));
#97267=CARTESIAN_POINT('Ctrl Pts',(-2.62085423679858,-0.112515203783535,
-1.06649609279466E-16));
#97268=CARTESIAN_POINT('Ctrl Pts',(-2.62305934562411,-0.0981572642000985,
-1.11022302462516E-16));
#97269=CARTESIAN_POINT('Ctrl Pts',(-2.63712528078298,-0.00657092394452452,
-1.38914811925222E-16));
#97270=CARTESIAN_POINT('Ctrl Pts',(-2.64617739573217,0.0853990681092962,
3.71900126169414E-17));
#97271=CARTESIAN_POINT('Ctrl Pts',(-2.65008474750347,0.177354999775061,
0.));
#97272=CARTESIAN_POINT('Ctrl Pts',(-2.65202414172285,0.222996859722445,
-1.84590739994191E-17));
#97273=CARTESIAN_POINT('Ctrl Pts',(-2.65269545055373,0.268635769706036,
-6.63948877319936E-16));
#97274=CARTESIAN_POINT('Ctrl Pts',(-2.65207858378913,0.314225566990061,
-6.10622663543836E-16));
#97275=CARTESIAN_POINT('Ctrl Pts',(-2.65087965130116,0.402833175991634,
-5.06978677799186E-16));
#97276=CARTESIAN_POINT('Ctrl Pts',(-2.6448180687798,0.491254842453244,-1.68823756050878E-16));
#97277=CARTESIAN_POINT('Ctrl Pts',(-2.63413908118019,0.57922885720872,-1.11022302462516E-16));
#97278=CARTESIAN_POINT('Ctrl Pts',(-2.62324360658611,0.668986302263057,
-5.20490839622738E-17));
#97279=CARTESIAN_POINT('Ctrl Pts',(-2.60754152358555,0.758278489974549,
-4.16879648018951E-17));
#97280=CARTESIAN_POINT('Ctrl Pts',(-2.58723933329292,0.846831256180718,
0.));
#97281=CARTESIAN_POINT('Ctrl Pts',(-2.58290125787064,0.865752789922496,
8.90768596419273E-18));
#97282=CARTESIAN_POINT('Ctrl Pts',(-2.57835296575468,0.884640553812132,
2.73591279314061E-16));
#97283=CARTESIAN_POINT('Ctrl Pts',(-2.57359616799277,0.903491843796352,
3.05311331771918E-16));
#97284=CARTESIAN_POINT('Ctrl Pts',(-2.56983477539876,0.91839832207933,3.30393661601536E-16));
#97285=CARTESIAN_POINT('Ctrl Pts',(-2.56594255180041,0.933283371413798,
-3.67694354189373E-16));
#97286=CARTESIAN_POINT('Ctrl Pts',(-2.56192538081525,0.948127790528015,
-3.60822483003176E-16));
#97287=CARTESIAN_POINT('Ctrl Pts',(-2.53775413356268,1.0374463995828,-3.19474554786378E-16));
#97288=CARTESIAN_POINT('Ctrl Pts',(-2.50902828076505,1.12543873737851,1.53403928884733E-16));
#97289=CARTESIAN_POINT('Ctrl Pts',(-2.47603795129406,1.21182189566662,1.11022302462516E-16));
#97290=CARTESIAN_POINT('Ctrl Pts',(-2.44240452892675,1.29988895333818,6.78145150615047E-17));
#97291=CARTESIAN_POINT('Ctrl Pts',(-2.40433858917601,1.38628426565922,-5.02419088652809E-16));
#97292=CARTESIAN_POINT('Ctrl Pts',(-2.36209206550289,1.47071144652719,-5.55111512312578E-16));
#97293=CARTESIAN_POINT('Ctrl Pts',(-2.31947143010013,1.55588626757751,-6.08270550785587E-16));
#97294=CARTESIAN_POINT('Ctrl Pts',(-2.27259555516532,1.63905881902964,-3.99435617532735E-16));
#97295=CARTESIAN_POINT('Ctrl Pts',(-2.2216707389484,1.71991558864889,-4.44089209850063E-16));
#97296=CARTESIAN_POINT('Ctrl Pts',(-2.19223846647794,1.76664719518778,-4.69896994610052E-16));
#97297=CARTESIAN_POINT('Ctrl Pts',(-2.16145276924779,1.81260501793967,-5.62079449352428E-16));
#97298=CARTESIAN_POINT('Ctrl Pts',(-2.12934619443225,1.8577253685959,-6.10622663543836E-16));
#97299=CARTESIAN_POINT('Ctrl Pts',(-2.1208366219097,1.8696841308855,-6.23488626481735E-16));
#97300=CARTESIAN_POINT('Ctrl Pts',(-2.11223277684254,1.88158602620125,-3.37626995517435E-16));
#97301=CARTESIAN_POINT('Ctrl Pts',(-2.10353995800366,1.89342337724526,-3.33066907387547E-16));
#97302=CARTESIAN_POINT('Ctrl Pts',(-2.04535171670342,1.97266057885621,-3.02542458026509E-16));
#97303=CARTESIAN_POINT('Ctrl Pts',(-1.98333354102214,2.04880176073276,2.26492193510099E-16));
#97304=CARTESIAN_POINT('Ctrl Pts',(-1.91775995208173,2.12153850276279,1.66533453693773E-16));
#97305=CARTESIAN_POINT('Ctrl Pts',(-1.85197384149148,2.1945109819649,1.06380389752237E-16));
#97306=CARTESIAN_POINT('Ctrl Pts',(-1.78260884177838,2.26405782067553,-1.44367353459688E-16));
#97307=CARTESIAN_POINT('Ctrl Pts',(-1.70989166532765,2.32985284092625,0.));
#97308=CARTESIAN_POINT('Ctrl Pts',(-1.63853532905585,2.39441656327046,1.416656410899E-16));
#97309=CARTESIAN_POINT('Ctrl Pts',(-1.5639505801766,2.4553683545156,-2.41362646891836E-16));
#97310=CARTESIAN_POINT('Ctrl Pts',(-1.48631019665298,2.51237350747524,-2.22044604925031E-16));
#97311=CARTESIAN_POINT('Ctrl Pts',(-1.42254976981509,2.5591877131722,-2.06180095431707E-16));
#97312=CARTESIAN_POINT('Ctrl Pts',(-1.35672772912532,2.60333998688217,-1.8151660154858E-16));
#97313=CARTESIAN_POINT('Ctrl Pts',(-1.28892185405323,2.64462557919718,-1.66533453693773E-16));
#97314=CARTESIAN_POINT('Origin',(0.,0.,0.));
#97315=CARTESIAN_POINT('Origin',(-1.44337567297407,-2.5,-6.));
#97316=CARTESIAN_POINT('',(-1.44337567297407,-2.5,-6.));
#97317=CARTESIAN_POINT('',(1.44337567297406,-2.5,-6.));
#97318=CARTESIAN_POINT('',(-0.721687836487033,-2.5,-6.));
#97319=CARTESIAN_POINT('',(-1.44337567297407,-2.5,-3.));
#97320=CARTESIAN_POINT('',(-1.44337567297407,-2.5,-6.));
#97321=CARTESIAN_POINT('',(1.44337567297406,-2.5,-3.));
#97322=CARTESIAN_POINT('',(-1.44337567297407,-2.5,-3.));
#97323=CARTESIAN_POINT('',(1.44337567297406,-2.5,-6.));
#97324=CARTESIAN_POINT('Origin',(-2.88675134594813,3.53525079574969E-16,
-6.));
#97325=CARTESIAN_POINT('',(-2.88675134594813,3.53525079574969E-16,-6.));
#97326=CARTESIAN_POINT('',(-2.52590742770461,-0.625,-6.));
#97327=CARTESIAN_POINT('',(-2.88675134594813,5.55111512312578E-16,-3.));
#97328=CARTESIAN_POINT('',(-2.88675134594813,3.53525079574969E-16,-6.));
#97329=CARTESIAN_POINT('',(-2.88675134594813,3.53525079574969E-16,-3.));
#97330=CARTESIAN_POINT('Origin',(-1.44337567297406,2.5,-6.));
#97331=CARTESIAN_POINT('',(-1.44337567297406,2.5,-6.));
#97332=CARTESIAN_POINT('',(-1.80421959121758,1.875,-6.));
#97333=CARTESIAN_POINT('',(-1.44337567297406,2.5,-3.));
#97334=CARTESIAN_POINT('',(-1.44337567297406,2.5,-6.));
#97335=CARTESIAN_POINT('',(-1.44337567297406,2.5,-3.));
#97336=CARTESIAN_POINT('Origin',(1.44337567297406,2.5,-6.));
#97337=CARTESIAN_POINT('',(1.44337567297406,2.5,-6.));
#97338=CARTESIAN_POINT('',(0.721687836487033,2.5,-6.));
#97339=CARTESIAN_POINT('',(1.44337567297406,2.5,-3.));
#97340=CARTESIAN_POINT('',(1.44337567297406,2.5,-6.));
#97341=CARTESIAN_POINT('',(1.44337567297406,2.5,-3.));
#97342=CARTESIAN_POINT('Origin',(2.88675134594813,0.,-6.));
#97343=CARTESIAN_POINT('',(2.88675134594813,0.,-6.));
#97344=CARTESIAN_POINT('',(2.52590742770461,0.625,-6.));
#97345=CARTESIAN_POINT('',(2.88675134594813,0.,-3.));
#97346=CARTESIAN_POINT('',(2.88675134594813,0.,-6.));
#97347=CARTESIAN_POINT('',(2.88675134594813,0.,-3.));
#97348=CARTESIAN_POINT('Origin',(1.44337567297406,-2.5,-6.));
#97349=CARTESIAN_POINT('',(1.80421959121758,-1.875,-6.));
#97350=CARTESIAN_POINT('',(1.44337567297406,-2.5,-3.));
#97351=CARTESIAN_POINT('Origin',(0.,0.,-3.));
#97352=CARTESIAN_POINT('Origin',(0.,0.,0.));
#97353=CARTESIAN_POINT('',(-5.,-6.12323399573677E-16,0.));
#97354=CARTESIAN_POINT('Origin',(0.,0.,0.));
#97355=CARTESIAN_POINT('Origin',(0.,0.,-6.));
#97356=CARTESIAN_POINT('',(-5.,-6.12323399573677E-16,-6.));
#97357=CARTESIAN_POINT('',(-5.,-6.12323399573677E-16,-6.));
#97358=CARTESIAN_POINT('Origin',(0.,0.,-6.));
#97359=CARTESIAN_POINT('Origin',(0.,0.,-6.));
#97360=CARTESIAN_POINT('Origin',(0.,0.,50.));
#97361=CARTESIAN_POINT('',(0.,0.,0.));
#97362=CARTESIAN_POINT('Origin',(0.,0.,0.));
#97363=CARTESIAN_POINT('',(-3.5,-4.28626379701574E-16,32.));
#97364=CARTESIAN_POINT('Origin',(0.,0.,32.));
#97365=CARTESIAN_POINT('',(-3.5,-4.28626379701574E-16,0.));
#97366=CARTESIAN_POINT('',(-3.5,-4.28626379701574E-16,0.));
#97367=CARTESIAN_POINT('Origin',(0.,0.,0.));
#97368=CARTESIAN_POINT('Origin',(0.,0.,0.));
#97369=CARTESIAN_POINT('',(-6.,-7.34788079488412E-16,32.));
#97370=CARTESIAN_POINT('Origin',(0.,0.,32.));
#97371=CARTESIAN_POINT('',(-6.,-7.34788079488412E-16,0.));
#97372=CARTESIAN_POINT('',(-6.,-7.34788079488412E-16,0.));
#97373=CARTESIAN_POINT('Origin',(0.,0.,0.));
#97374=CARTESIAN_POINT('Origin',(0.,0.,32.));
#97375=CARTESIAN_POINT('Origin',(0.,0.,0.));
#97376=CARTESIAN_POINT('',(0.,0.,0.));
#97377=CARTESIAN_POINT('Origin',(0.,0.,0.));
#97378=CARTESIAN_POINT('',(-3.5,-4.28626379701574E-16,2.));
#97379=CARTESIAN_POINT('Origin',(0.,0.,2.));
#97380=CARTESIAN_POINT('',(-3.5,-4.28626379701574E-16,0.));
#97381=CARTESIAN_POINT('',(-3.5,-4.28626379701574E-16,0.));
#97382=CARTESIAN_POINT('Origin',(0.,0.,0.));
#97383=CARTESIAN_POINT('Origin',(0.,0.,0.));
#97384=CARTESIAN_POINT('',(-7.,-8.57252759403147E-16,2.));
#97385=CARTESIAN_POINT('Origin',(0.,0.,2.));
#97386=CARTESIAN_POINT('',(-7.,-8.57252759403147E-16,0.));
#97387=CARTESIAN_POINT('',(-7.,-8.57252759403147E-16,0.));
#97388=CARTESIAN_POINT('Origin',(0.,0.,0.));
#97389=CARTESIAN_POINT('Origin',(0.,0.,2.));
#97390=CARTESIAN_POINT('Origin',(0.,0.,0.));
#97391=CARTESIAN_POINT('',(0.,0.,50.));
#97392=CARTESIAN_POINT('',(0.,0.,450.));
#97393=CARTESIAN_POINT('',(0.,0.,456.));
#97394=CARTESIAN_POINT('',(0.,0.,-4.));
#97395=CARTESIAN_POINT('',(0.,0.,0.));
#97396=CARTESIAN_POINT('',(0.,0.,0.));
#97397=CARTESIAN_POINT('',(0.,0.,0.));
#97398=CARTESIAN_POINT('',(0.,0.,40.));
#97399=CARTESIAN_POINT('',(0.,0.,48.));
#97400=CARTESIAN_POINT('',(15.,0.,20.));
#97401=CARTESIAN_POINT('',(15.,0.,18.));
#97402=CARTESIAN_POINT('',(-7.5,12.9903810567666,20.));
#97403=CARTESIAN_POINT('',(-7.5,12.9903810567666,18.));
#97404=CARTESIAN_POINT('',(-7.50000000000001,-12.9903810567666,20.));
#97405=CARTESIAN_POINT('',(-7.50000000000001,-12.9903810567666,18.));
#97406=CARTESIAN_POINT('',(-250.,-200.,0.));
#97407=CARTESIAN_POINT('',(0.,0.,0.));
#97408=CARTESIAN_POINT('',(250.,-200.,0.));
#97409=CARTESIAN_POINT('',(-250.,200.,0.));
#97410=CARTESIAN_POINT('',(250.,200.,0.));
#97411=CARTESIAN_POINT('',(0.,0.,514.));
#97412=CARTESIAN_POINT('',(-160.,-225.,472.));
#97413=CARTESIAN_POINT('',(-160.,-225.,478.));
#97414=CARTESIAN_POINT('',(-160.,-225.,472.));
#97415=CARTESIAN_POINT('',(0.,-225.,472.));
#97416=CARTESIAN_POINT('',(0.,-225.,478.));
#97417=CARTESIAN_POINT('',(0.,-225.,472.));
#97418=CARTESIAN_POINT('',(160.,-225.,472.));
#97419=CARTESIAN_POINT('',(160.,-225.,478.));
#97420=CARTESIAN_POINT('',(160.,-225.,472.));
#97421=CARTESIAN_POINT('',(-160.,225.,472.));
#97422=CARTESIAN_POINT('',(-160.,225.,478.));
#97423=CARTESIAN_POINT('',(-160.,225.,472.));
#97424=CARTESIAN_POINT('',(0.,225.,472.));
#97425=CARTESIAN_POINT('',(0.,225.,478.));
#97426=CARTESIAN_POINT('',(0.,225.,472.));
#97427=CARTESIAN_POINT('',(160.,225.,472.));
#97428=CARTESIAN_POINT('',(160.,225.,478.));
#97429=CARTESIAN_POINT('',(160.,225.,472.));
#97430=UNCERTAINTY_MEASURE_WITH_UNIT(LENGTH_MEASURE(0.01),#97476,
'DISTANCE_ACCURACY_VALUE',
'Maximum model space distance between geometric entities at asserted c
onnectivities');
#97431=UNCERTAINTY_MEASURE_WITH_UNIT(LENGTH_MEASURE(0.01),#97476,
'DISTANCE_ACCURACY_VALUE',
'Maximum model space distance between geometric entities at asserted c
onnectivities');
#97432=UNCERTAINTY_MEASURE_WITH_UNIT(LENGTH_MEASURE(0.01),#97476,
'DISTANCE_ACCURACY_VALUE',
'Maximum model space distance between geometric entities at asserted c
onnectivities');
#97433=UNCERTAINTY_MEASURE_WITH_UNIT(LENGTH_MEASURE(0.01),#97476,
'DISTANCE_ACCURACY_VALUE',
'Maximum model space distance between geometric entities at asserted c
onnectivities');
#97434=UNCERTAINTY_MEASURE_WITH_UNIT(LENGTH_MEASURE(0.01),#97476,
'DISTANCE_ACCURACY_VALUE',
'Maximum model space distance between geometric entities at asserted c
onnectivities');
#97435=UNCERTAINTY_MEASURE_WITH_UNIT(LENGTH_MEASURE(0.01),#97476,
'DISTANCE_ACCURACY_VALUE',
'Maximum model space distance between geometric entities at asserted c
onnectivities');
#97436=UNCERTAINTY_MEASURE_WITH_UNIT(LENGTH_MEASURE(0.01),#97476,
'DISTANCE_ACCURACY_VALUE',
'Maximum model space distance between geometric entities at asserted c
onnectivities');
#97437=UNCERTAINTY_MEASURE_WITH_UNIT(LENGTH_MEASURE(0.01),#97476,
'DISTANCE_ACCURACY_VALUE',
'Maximum model space distance between geometric entities at asserted c
onnectivities');
#97438=UNCERTAINTY_MEASURE_WITH_UNIT(LENGTH_MEASURE(0.01),#97476,
'DISTANCE_ACCURACY_VALUE',
'Maximum model space distance between geometric entities at asserted c
onnectivities');
#97439=UNCERTAINTY_MEASURE_WITH_UNIT(LENGTH_MEASURE(0.01),#97476,
'DISTANCE_ACCURACY_VALUE',
'Maximum model space distance between geometric entities at asserted c
onnectivities');
#97440=UNCERTAINTY_MEASURE_WITH_UNIT(LENGTH_MEASURE(0.01),#97476,
'DISTANCE_ACCURACY_VALUE',
'Maximum model space distance between geometric entities at asserted c
onnectivities');
#97441=UNCERTAINTY_MEASURE_WITH_UNIT(LENGTH_MEASURE(0.01),#97476,
'DISTANCE_ACCURACY_VALUE',
'Maximum model space distance between geometric entities at asserted c
onnectivities');
#97442=UNCERTAINTY_MEASURE_WITH_UNIT(LENGTH_MEASURE(0.01),#97476,
'DISTANCE_ACCURACY_VALUE',
'Maximum model space distance between geometric entities at asserted c
onnectivities');
#97443=UNCERTAINTY_MEASURE_WITH_UNIT(LENGTH_MEASURE(0.01),#97476,
'DISTANCE_ACCURACY_VALUE',
'Maximum model space distance between geometric entities at asserted c
onnectivities');
#97444=UNCERTAINTY_MEASURE_WITH_UNIT(LENGTH_MEASURE(0.01),#97476,
'DISTANCE_ACCURACY_VALUE',
'Maximum model space distance between geometric entities at asserted c
onnectivities');
#97445=UNCERTAINTY_MEASURE_WITH_UNIT(LENGTH_MEASURE(0.01),#97476,
'DISTANCE_ACCURACY_VALUE',
'Maximum model space distance between geometric entities at asserted c
onnectivities');
#97446=UNCERTAINTY_MEASURE_WITH_UNIT(LENGTH_MEASURE(0.01),#97476,
'DISTANCE_ACCURACY_VALUE',
'Maximum model space distance between geometric entities at asserted c
onnectivities');
#97447=UNCERTAINTY_MEASURE_WITH_UNIT(LENGTH_MEASURE(0.01),#97476,
'DISTANCE_ACCURACY_VALUE',
'Maximum model space distance between geometric entities at asserted c
onnectivities');
#97448=UNCERTAINTY_MEASURE_WITH_UNIT(LENGTH_MEASURE(0.01),#97476,
'DISTANCE_ACCURACY_VALUE',
'Maximum model space distance between geometric entities at asserted c
onnectivities');
#97449=UNCERTAINTY_MEASURE_WITH_UNIT(LENGTH_MEASURE(0.01),#97476,
'DISTANCE_ACCURACY_VALUE',
'Maximum model space distance between geometric entities at asserted c
onnectivities');
#97450=UNCERTAINTY_MEASURE_WITH_UNIT(LENGTH_MEASURE(0.01),#97476,
'DISTANCE_ACCURACY_VALUE',
'Maximum model space distance between geometric entities at asserted c
onnectivities');
#97451=UNCERTAINTY_MEASURE_WITH_UNIT(LENGTH_MEASURE(0.01),#97476,
'DISTANCE_ACCURACY_VALUE',
'Maximum model space distance between geometric entities at asserted c
onnectivities');
#97452=UNCERTAINTY_MEASURE_WITH_UNIT(LENGTH_MEASURE(0.01),#97476,
'DISTANCE_ACCURACY_VALUE',
'Maximum model space distance between geometric entities at asserted c
onnectivities');
#97453=(
GEOMETRIC_REPRESENTATION_CONTEXT(3)
GLOBAL_UNCERTAINTY_ASSIGNED_CONTEXT((#97430))
GLOBAL_UNIT_ASSIGNED_CONTEXT((#97476,#97478,#97479))
REPRESENTATION_CONTEXT('','3D')
);
#97454=(
GEOMETRIC_REPRESENTATION_CONTEXT(3)
GLOBAL_UNCERTAINTY_ASSIGNED_CONTEXT((#97431))
GLOBAL_UNIT_ASSIGNED_CONTEXT((#97476,#97478,#97479))
REPRESENTATION_CONTEXT('','3D')
);
#97455=(
GEOMETRIC_REPRESENTATION_CONTEXT(3)
GLOBAL_UNCERTAINTY_ASSIGNED_CONTEXT((#97432))
GLOBAL_UNIT_ASSIGNED_CONTEXT((#97476,#97478,#97479))
REPRESENTATION_CONTEXT('','3D')
);
#97456=(
GEOMETRIC_REPRESENTATION_CONTEXT(3)
GLOBAL_UNCERTAINTY_ASSIGNED_CONTEXT((#97433))
GLOBAL_UNIT_ASSIGNED_CONTEXT((#97476,#97478,#97479))
REPRESENTATION_CONTEXT('','3D')
);
#97457=(
GEOMETRIC_REPRESENTATION_CONTEXT(3)
GLOBAL_UNCERTAINTY_ASSIGNED_CONTEXT((#97434))
GLOBAL_UNIT_ASSIGNED_CONTEXT((#97476,#97478,#97479))
REPRESENTATION_CONTEXT('','3D')
);
#97458=(
GEOMETRIC_REPRESENTATION_CONTEXT(3)
GLOBAL_UNCERTAINTY_ASSIGNED_CONTEXT((#97435))
GLOBAL_UNIT_ASSIGNED_CONTEXT((#97476,#97478,#97479))
REPRESENTATION_CONTEXT('','3D')
);
#97459=(
GEOMETRIC_REPRESENTATION_CONTEXT(3)
GLOBAL_UNCERTAINTY_ASSIGNED_CONTEXT((#97436))
GLOBAL_UNIT_ASSIGNED_CONTEXT((#97476,#97478,#97479))
REPRESENTATION_CONTEXT('','3D')
);
#97460=(
GEOMETRIC_REPRESENTATION_CONTEXT(3)
GLOBAL_UNCERTAINTY_ASSIGNED_CONTEXT((#97437))
GLOBAL_UNIT_ASSIGNED_CONTEXT((#97476,#97478,#97479))
REPRESENTATION_CONTEXT('','3D')
);
#97461=(
GEOMETRIC_REPRESENTATION_CONTEXT(3)
GLOBAL_UNCERTAINTY_ASSIGNED_CONTEXT((#97438))
GLOBAL_UNIT_ASSIGNED_CONTEXT((#97476,#97478,#97479))
REPRESENTATION_CONTEXT('','3D')
);
#97462=(
GEOMETRIC_REPRESENTATION_CONTEXT(3)
GLOBAL_UNCERTAINTY_ASSIGNED_CONTEXT((#97439))
GLOBAL_UNIT_ASSIGNED_CONTEXT((#97476,#97478,#97479))
REPRESENTATION_CONTEXT('','3D')
);
#97463=(
GEOMETRIC_REPRESENTATION_CONTEXT(3)
GLOBAL_UNCERTAINTY_ASSIGNED_CONTEXT((#97440))
GLOBAL_UNIT_ASSIGNED_CONTEXT((#97476,#97478,#97479))
REPRESENTATION_CONTEXT('','3D')
);
#97464=(
GEOMETRIC_REPRESENTATION_CONTEXT(3)
GLOBAL_UNCERTAINTY_ASSIGNED_CONTEXT((#97441))
GLOBAL_UNIT_ASSIGNED_CONTEXT((#97476,#97478,#97479))
REPRESENTATION_CONTEXT('','3D')
);
#97465=(
GEOMETRIC_REPRESENTATION_CONTEXT(3)
GLOBAL_UNCERTAINTY_ASSIGNED_CONTEXT((#97442))
GLOBAL_UNIT_ASSIGNED_CONTEXT((#97476,#97478,#97479))
REPRESENTATION_CONTEXT('','3D')
);
#97466=(
GEOMETRIC_REPRESENTATION_CONTEXT(3)
GLOBAL_UNCERTAINTY_ASSIGNED_CONTEXT((#97443))
GLOBAL_UNIT_ASSIGNED_CONTEXT((#97476,#97478,#97479))
REPRESENTATION_CONTEXT('','3D')
);
#97467=(
GEOMETRIC_REPRESENTATION_CONTEXT(3)
GLOBAL_UNCERTAINTY_ASSIGNED_CONTEXT((#97444))
GLOBAL_UNIT_ASSIGNED_CONTEXT((#97476,#97478,#97479))
REPRESENTATION_CONTEXT('','3D')
);
#97468=(
GEOMETRIC_REPRESENTATION_CONTEXT(3)
GLOBAL_UNCERTAINTY_ASSIGNED_CONTEXT((#97445))
GLOBAL_UNIT_ASSIGNED_CONTEXT((#97476,#97478,#97479))
REPRESENTATION_CONTEXT('','3D')
);
#97469=(
GEOMETRIC_REPRESENTATION_CONTEXT(3)
GLOBAL_UNCERTAINTY_ASSIGNED_CONTEXT((#97446))
GLOBAL_UNIT_ASSIGNED_CONTEXT((#97476,#97478,#97479))
REPRESENTATION_CONTEXT('','3D')
);
#97470=(
GEOMETRIC_REPRESENTATION_CONTEXT(3)
GLOBAL_UNCERTAINTY_ASSIGNED_CONTEXT((#97447))
GLOBAL_UNIT_ASSIGNED_CONTEXT((#97476,#97478,#97479))
REPRESENTATION_CONTEXT('','3D')
);
#97471=(
GEOMETRIC_REPRESENTATION_CONTEXT(3)
GLOBAL_UNCERTAINTY_ASSIGNED_CONTEXT((#97448))
GLOBAL_UNIT_ASSIGNED_CONTEXT((#97476,#97478,#97479))
REPRESENTATION_CONTEXT('','3D')
);
#97472=(
GEOMETRIC_REPRESENTATION_CONTEXT(3)
GLOBAL_UNCERTAINTY_ASSIGNED_CONTEXT((#97449))
GLOBAL_UNIT_ASSIGNED_CONTEXT((#97476,#97478,#97479))
REPRESENTATION_CONTEXT('','3D')
);
#97473=(
GEOMETRIC_REPRESENTATION_CONTEXT(3)
GLOBAL_UNCERTAINTY_ASSIGNED_CONTEXT((#97450))
GLOBAL_UNIT_ASSIGNED_CONTEXT((#97476,#97478,#97479))
REPRESENTATION_CONTEXT('','3D')
);
#97474=(
GEOMETRIC_REPRESENTATION_CONTEXT(3)
GLOBAL_UNCERTAINTY_ASSIGNED_CONTEXT((#97451))
GLOBAL_UNIT_ASSIGNED_CONTEXT((#97476,#97478,#97479))
REPRESENTATION_CONTEXT('','3D')
);
#97475=(
GEOMETRIC_REPRESENTATION_CONTEXT(3)
GLOBAL_UNCERTAINTY_ASSIGNED_CONTEXT((#97452))
GLOBAL_UNIT_ASSIGNED_CONTEXT((#97476,#97478,#97479))
REPRESENTATION_CONTEXT('','3D')
);
#97476=(
LENGTH_UNIT()
NAMED_UNIT(*)
SI_UNIT(.MILLI.,.METRE.)
);
#97477=(
LENGTH_UNIT()
NAMED_UNIT(*)
SI_UNIT($,.METRE.)
);
#97478=(
NAMED_UNIT(*)
PLANE_ANGLE_UNIT()
SI_UNIT($,.RADIAN.)
);
#97479=(
NAMED_UNIT(*)
SI_UNIT($,.STERADIAN.)
SOLID_ANGLE_UNIT()
);
#97480=SHAPE_DEFINITION_REPRESENTATION(#97502,#97603);
#97481=SHAPE_DEFINITION_REPRESENTATION(#97503,#97604);
#97482=SHAPE_DEFINITION_REPRESENTATION(#97504,#97605);
#97483=SHAPE_DEFINITION_REPRESENTATION(#97505,#97606);
#97484=SHAPE_DEFINITION_REPRESENTATION(#97506,#97607);
#97485=SHAPE_DEFINITION_REPRESENTATION(#97507,#97608);
#97486=SHAPE_DEFINITION_REPRESENTATION(#97508,#97609);
#97487=SHAPE_DEFINITION_REPRESENTATION(#97549,#97610);
#97488=SHAPE_DEFINITION_REPRESENTATION(#97550,#97611);
#97489=SHAPE_DEFINITION_REPRESENTATION(#97551,#97612);
#97490=SHAPE_DEFINITION_REPRESENTATION(#97552,#97613);
#97491=SHAPE_DEFINITION_REPRESENTATION(#97553,#97614);
#97492=SHAPE_DEFINITION_REPRESENTATION(#97554,#97615);
#97493=SHAPE_DEFINITION_REPRESENTATION(#97555,#97616);
#97494=SHAPE_DEFINITION_REPRESENTATION(#97556,#97617);
#97495=SHAPE_DEFINITION_REPRESENTATION(#97557,#97618);
#97496=SHAPE_DEFINITION_REPRESENTATION(#97558,#97619);
#97497=SHAPE_DEFINITION_REPRESENTATION(#97559,#97620);
#97498=SHAPE_DEFINITION_REPRESENTATION(#97560,#97621);
#97499=SHAPE_DEFINITION_REPRESENTATION(#97561,#97622);
#97500=SHAPE_DEFINITION_REPRESENTATION(#97562,#97623);
#97501=SHAPE_DEFINITION_REPRESENTATION(#97563,#97624);
#97502=PRODUCT_DEFINITION_SHAPE('',$,#97626);
#97503=PRODUCT_DEFINITION_SHAPE('',$,#97627);
#97504=PRODUCT_DEFINITION_SHAPE('',$,#97628);
#97505=PRODUCT_DEFINITION_SHAPE('',$,#97629);
#97506=PRODUCT_DEFINITION_SHAPE('',$,#97630);
#97507=PRODUCT_DEFINITION_SHAPE('',$,#97631);
#97508=PRODUCT_DEFINITION_SHAPE('',$,#97632);
#97509=PRODUCT_DEFINITION_SHAPE($,$,#251);
#97510=PRODUCT_DEFINITION_SHAPE($,$,#252);
#97511=PRODUCT_DEFINITION_SHAPE($,$,#253);
#97512=PRODUCT_DEFINITION_SHAPE($,$,#254);
#97513=PRODUCT_DEFINITION_SHAPE($,$,#255);
#97514=PRODUCT_DEFINITION_SHAPE($,$,#256);
#97515=PRODUCT_DEFINITION_SHAPE($,$,#257);
#97516=PRODUCT_DEFINITION_SHAPE($,$,#258);
#97517=PRODUCT_DEFINITION_SHAPE($,$,#259);
#97518=PRODUCT_DEFINITION_SHAPE($,$,#260);
#97519=PRODUCT_DEFINITION_SHAPE($,$,#261);
#97520=PRODUCT_DEFINITION_SHAPE($,$,#262);
#97521=PRODUCT_DEFINITION_SHAPE($,$,#263);
#97522=PRODUCT_DEFINITION_SHAPE($,$,#264);
#97523=PRODUCT_DEFINITION_SHAPE($,$,#265);
#97524=PRODUCT_DEFINITION_SHAPE($,$,#266);
#97525=PRODUCT_DEFINITION_SHAPE($,$,#267);
#97526=PRODUCT_DEFINITION_SHAPE($,$,#268);
#97527=PRODUCT_DEFINITION_SHAPE($,$,#269);
#97528=PRODUCT_DEFINITION_SHAPE($,$,#270);
#97529=PRODUCT_DEFINITION_SHAPE($,$,#271);
#97530=PRODUCT_DEFINITION_SHAPE($,$,#272);
#97531=PRODUCT_DEFINITION_SHAPE($,$,#273);
#97532=PRODUCT_DEFINITION_SHAPE($,$,#274);
#97533=PRODUCT_DEFINITION_SHAPE($,$,#275);
#97534=PRODUCT_DEFINITION_SHAPE($,$,#276);
#97535=PRODUCT_DEFINITION_SHAPE($,$,#277);
#97536=PRODUCT_DEFINITION_SHAPE($,$,#278);
#97537=PRODUCT_DEFINITION_SHAPE($,$,#279);
#97538=PRODUCT_DEFINITION_SHAPE($,$,#280);
#97539=PRODUCT_DEFINITION_SHAPE($,$,#281);
#97540=PRODUCT_DEFINITION_SHAPE($,$,#282);
#97541=PRODUCT_DEFINITION_SHAPE($,$,#283);
#97542=PRODUCT_DEFINITION_SHAPE($,$,#284);
#97543=PRODUCT_DEFINITION_SHAPE($,$,#285);
#97544=PRODUCT_DEFINITION_SHAPE($,$,#286);
#97545=PRODUCT_DEFINITION_SHAPE($,$,#287);
#97546=PRODUCT_DEFINITION_SHAPE($,$,#288);
#97547=PRODUCT_DEFINITION_SHAPE($,$,#289);
#97548=PRODUCT_DEFINITION_SHAPE($,$,#290);
#97549=PRODUCT_DEFINITION_SHAPE('',$,#97633);
#97550=PRODUCT_DEFINITION_SHAPE('',$,#97634);
#97551=PRODUCT_DEFINITION_SHAPE('',$,#97635);
#97552=PRODUCT_DEFINITION_SHAPE('',$,#97636);
#97553=PRODUCT_DEFINITION_SHAPE('',$,#97637);
#97554=PRODUCT_DEFINITION_SHAPE('',$,#97638);
#97555=PRODUCT_DEFINITION_SHAPE('',$,#97639);
#97556=PRODUCT_DEFINITION_SHAPE('',$,#97640);
#97557=PRODUCT_DEFINITION_SHAPE('',$,#97641);
#97558=PRODUCT_DEFINITION_SHAPE('',$,#97642);
#97559=PRODUCT_DEFINITION_SHAPE('',$,#97643);
#97560=PRODUCT_DEFINITION_SHAPE('',$,#97644);
#97561=PRODUCT_DEFINITION_SHAPE('',$,#97645);
#97562=PRODUCT_DEFINITION_SHAPE('',$,#97646);
#97563=PRODUCT_DEFINITION_SHAPE('',$,#97647);
#97564=PRODUCT_DEFINITION_SHAPE($,$,#291);
#97565=PRODUCT_DEFINITION_SHAPE($,$,#292);
#97566=PRODUCT_DEFINITION_SHAPE($,$,#293);
#97567=PRODUCT_DEFINITION_SHAPE($,$,#294);
#97568=PRODUCT_DEFINITION_SHAPE($,$,#295);
#97569=PRODUCT_DEFINITION_SHAPE($,$,#296);
#97570=PRODUCT_DEFINITION_SHAPE($,$,#297);
#97571=PRODUCT_DEFINITION_SHAPE($,$,#298);
#97572=PRODUCT_DEFINITION_SHAPE($,$,#299);
#97573=PRODUCT_DEFINITION_SHAPE($,$,#300);
#97574=PRODUCT_DEFINITION_SHAPE($,$,#301);
#97575=PRODUCT_DEFINITION_SHAPE($,$,#302);
#97576=PRODUCT_DEFINITION_SHAPE($,$,#303);
#97577=PRODUCT_DEFINITION_SHAPE($,$,#304);
#97578=PRODUCT_DEFINITION_SHAPE($,$,#305);
#97579=PRODUCT_DEFINITION_SHAPE($,$,#306);
#97580=PRODUCT_DEFINITION_SHAPE($,$,#307);
#97581=PRODUCT_DEFINITION_SHAPE($,$,#308);
#97582=PRODUCT_DEFINITION_SHAPE($,$,#309);
#97583=PRODUCT_DEFINITION_SHAPE($,$,#310);
#97584=PRODUCT_DEFINITION_SHAPE($,$,#311);
#97585=PRODUCT_DEFINITION_SHAPE($,$,#312);
#97586=PRODUCT_DEFINITION_SHAPE($,$,#313);
#97587=PRODUCT_DEFINITION_SHAPE($,$,#314);
#97588=PRODUCT_DEFINITION_SHAPE($,$,#315);
#97589=PRODUCT_DEFINITION_SHAPE($,$,#316);
#97590=PRODUCT_DEFINITION_SHAPE($,$,#317);
#97591=PRODUCT_DEFINITION_SHAPE($,$,#318);
#97592=PRODUCT_DEFINITION_SHAPE($,$,#319);
#97593=PRODUCT_DEFINITION_SHAPE($,$,#320);
#97594=PRODUCT_DEFINITION_SHAPE($,$,#321);
#97595=PRODUCT_DEFINITION_SHAPE($,$,#322);
#97596=PRODUCT_DEFINITION_SHAPE($,$,#323);
#97597=PRODUCT_DEFINITION_SHAPE($,$,#324);
#97598=PRODUCT_DEFINITION_SHAPE($,$,#325);
#97599=PRODUCT_DEFINITION_SHAPE($,$,#326);
#97600=PRODUCT_DEFINITION_SHAPE($,$,#327);
#97601=PRODUCT_DEFINITION_SHAPE($,$,#328);
#97602=PRODUCT_DEFINITION_SHAPE($,$,#329);
#97603=SHAPE_REPRESENTATION('',(#22040,#23478,#23479,#23480,#23481,#23482,
#23483,#23484,#23485,#23486,#23487,#23488,#23489,#23490,#23491,#23492,#23493,
#23494,#23495,#23496,#23497,#23498,#23499,#23500,#23501),#97453);
#97604=SHAPE_REPRESENTATION('',(#22041,#22256,#22257,#22258,#22259,#22260,
#22261,#22262,#22263,#22264,#22265,#22266,#22267,#22268,#22269,#22270,#22271,
#22272,#22273,#22274,#22275,#22276,#22277,#22278,#22279,#22280,#22281,#22282,
#22283,#22284,#22285,#22286,#22287,#22288,#22289,#22290,#22291,#22292,#22293,
#22294,#22295),#97454);
#97605=SHAPE_REPRESENTATION('',(#22042),#97455);
#97606=SHAPE_REPRESENTATION('',(#22071),#97456);
#97607=SHAPE_REPRESENTATION('',(#22082),#97457);
#97608=SHAPE_REPRESENTATION('',(#22177),#97458);
#97609=SHAPE_REPRESENTATION('',(#22247),#97459);
#97610=SHAPE_REPRESENTATION('',(#22296,#23463,#23464,#23465,#23466,#23467,
#23468,#23469,#23470,#23471,#23472,#23473,#23474,#23475,#23476,#23477),
#97460);
#97611=SHAPE_REPRESENTATION('',(#22297),#97461);
#97612=SHAPE_REPRESENTATION('',(#22609),#97462);
#97613=SHAPE_REPRESENTATION('',(#22635),#97463);
#97614=SHAPE_REPRESENTATION('',(#22695),#97464);
#97615=SHAPE_REPRESENTATION('',(#22701),#97465);
#97616=SHAPE_REPRESENTATION('',(#22788),#97466);
#97617=SHAPE_REPRESENTATION('',(#22809),#97467);
#97618=SHAPE_REPRESENTATION('',(#22950),#97468);
#97619=SHAPE_REPRESENTATION('',(#22981),#97469);
#97620=SHAPE_REPRESENTATION('',(#22990),#97470);
#97621=SHAPE_REPRESENTATION('',(#23042),#97471);
#97622=SHAPE_REPRESENTATION('',(#23325),#97472);
#97623=SHAPE_REPRESENTATION('',(#23445),#97473);
#97624=SHAPE_REPRESENTATION('',(#23454),#97474);
#97625=PRODUCT_DEFINITION_CONTEXT('part definition',#97693,'design');
#97626=PRODUCT_DEFINITION('MAS-653','MAS-653',#97648,#97625);
#97627=PRODUCT_DEFINITION('Connecting frame','Connecting frame',#97649,
#97625);
#97628=PRODUCT_DEFINITION('Longitudinal rail','Longitudinal rail',#97650,
#97625);
#97629=PRODUCT_DEFINITION('Transverse rail','Transverse rail',#97651,#97625);
#97630=PRODUCT_DEFINITION('Corner plate','Corner plate',#97652,#97625);
#97631=PRODUCT_DEFINITION('Socket head cap screw M8x25',
'Socket head cap screw M8x25',#97653,#97625);
#97632=PRODUCT_DEFINITION('Flat Washer M8','Flat washer M8',#97654,#97625);
#97633=PRODUCT_DEFINITION('Support leg','Support leg',#97655,#97625);
#97634=PRODUCT_DEFINITION('Leg post','Leg post',#97656,#97625);
#97635=PRODUCT_DEFINITION('Mounting plate','Mounting plate',#97657,#97625);
#97636=PRODUCT_DEFINITION('Socket head cap screw M10x20',
'Socket head cap screw M10x20',#97658,#97625);
#97637=PRODUCT_DEFINITION('Grip sole','Grip sole',#97659,#97625);
#97638=PRODUCT_DEFINITION('Swivel pad','Swivel pad',#97660,#97625);
#97639=PRODUCT_DEFINITION('Ball retainer','Ball retainer',#97661,#97625);
#97640=PRODUCT_DEFINITION('Adjusting spindle','Adjusting spindle',#97662,
#97625);
#97641=PRODUCT_DEFINITION('Lock nut M10','Lock nut M10',#97663,#97625);
#97642=PRODUCT_DEFINITION('Flat washer M10','Flat washer M10',#97664,#97625);
#97643=PRODUCT_DEFINITION('Socket head cap screw M6x16',
'Socket head cap screw M6x16',#97665,#97625);
#97644=PRODUCT_DEFINITION('Worktop','Worktop',#97666,#97625);
#97645=PRODUCT_DEFINITION('Socket head cap screw M6x50',
'Socket head cap screw M6x50',#97667,#97625);
#97646=PRODUCT_DEFINITION('Crush sleeve','Crush sleeve',#97668,#97625);
#97647=PRODUCT_DEFINITION('Flat washer M6','Flat washer M6',#97669,#97625);
#97648=PRODUCT_DEFINITION_FORMATION('',$,#97695);
#97649=PRODUCT_DEFINITION_FORMATION('',$,#97696);
#97650=PRODUCT_DEFINITION_FORMATION('',$,#97697);
#97651=PRODUCT_DEFINITION_FORMATION('',$,#97698);
#97652=PRODUCT_DEFINITION_FORMATION('',$,#97699);
#97653=PRODUCT_DEFINITION_FORMATION('',$,#97700);
#97654=PRODUCT_DEFINITION_FORMATION('',$,#97701);
#97655=PRODUCT_DEFINITION_FORMATION('',$,#97702);
#97656=PRODUCT_DEFINITION_FORMATION('',$,#97703);
#97657=PRODUCT_DEFINITION_FORMATION('',$,#97704);
#97658=PRODUCT_DEFINITION_FORMATION('',$,#97705);
#97659=PRODUCT_DEFINITION_FORMATION('',$,#97706);
#97660=PRODUCT_DEFINITION_FORMATION('',$,#97707);
#97661=PRODUCT_DEFINITION_FORMATION('',$,#97708);
#97662=PRODUCT_DEFINITION_FORMATION('',$,#97709);
#97663=PRODUCT_DEFINITION_FORMATION('',$,#97710);
#97664=PRODUCT_DEFINITION_FORMATION('',$,#97711);
#97665=PRODUCT_DEFINITION_FORMATION('',$,#97712);
#97666=PRODUCT_DEFINITION_FORMATION('',$,#97713);
#97667=PRODUCT_DEFINITION_FORMATION('',$,#97714);
#97668=PRODUCT_DEFINITION_FORMATION('',$,#97715);
#97669=PRODUCT_DEFINITION_FORMATION('',$,#97716);
#97670=PRODUCT_RELATED_PRODUCT_CATEGORY('MAS-653','MAS-653',(#97695));
#97671=PRODUCT_RELATED_PRODUCT_CATEGORY('Connecting frame',
'Connecting frame',(#97696));
#97672=PRODUCT_RELATED_PRODUCT_CATEGORY('Longitudinal rail',
'Longitudinal rail',(#97697));
#97673=PRODUCT_RELATED_PRODUCT_CATEGORY('Transverse rail',
'Transverse rail',(#97698));
#97674=PRODUCT_RELATED_PRODUCT_CATEGORY('Corner plate','Corner plate',(#97699));
#97675=PRODUCT_RELATED_PRODUCT_CATEGORY('Socket head cap screw M8x25',
'Socket head cap screw M8x25',(#97700));
#97676=PRODUCT_RELATED_PRODUCT_CATEGORY('Flat washer M8',
'Flat washer M8',(#97701));
#97677=PRODUCT_RELATED_PRODUCT_CATEGORY('Support leg','Support leg',(#97702));
#97678=PRODUCT_RELATED_PRODUCT_CATEGORY('Leg post','Leg post',(#97703));
#97679=PRODUCT_RELATED_PRODUCT_CATEGORY('Mounting plate',
'Mounting plate',(#97704));
#97680=PRODUCT_RELATED_PRODUCT_CATEGORY('Socket head cap screw M10x20',
'Socket head cap screw M10x20',(#97705));
#97681=PRODUCT_RELATED_PRODUCT_CATEGORY('Grip sole','Grip sole',(#97706));
#97682=PRODUCT_RELATED_PRODUCT_CATEGORY('Swivel pad','Swivel pad',(#97707));
#97683=PRODUCT_RELATED_PRODUCT_CATEGORY('Ball retainer','Ball retainer',
(#97708));
#97684=PRODUCT_RELATED_PRODUCT_CATEGORY('Adjusting spindle',
'Adjusting spindle',(#97709));
#97685=PRODUCT_RELATED_PRODUCT_CATEGORY('Lock nut M10','Lock nut M10',(#97710));
#97686=PRODUCT_RELATED_PRODUCT_CATEGORY('Flat washer M10',
'Flat washer M10',(#97711));
#97687=PRODUCT_RELATED_PRODUCT_CATEGORY('Socket head cap screw M6x16',
'Socket head cap screw M6x16',(#97712));
#97688=PRODUCT_RELATED_PRODUCT_CATEGORY('Worktop','Worktop',(#97713));
#97689=PRODUCT_RELATED_PRODUCT_CATEGORY('Socket head cap screw M6x50',
'Socket head cap screw M6x50',(#97714));
#97690=PRODUCT_RELATED_PRODUCT_CATEGORY('Crush sleeve','Crush sleeve',(#97715));
#97691=PRODUCT_RELATED_PRODUCT_CATEGORY('Flat washer M6',
'Flat washer M6',(#97716));
#97692=APPLICATION_PROTOCOL_DEFINITION('international standard',
'automotive_design',2009,#97693);
#97693=APPLICATION_CONTEXT(
'Core Data for Automotive Mechanical Design Process');
#97694=PRODUCT_CONTEXT('part definition',#97693,'mechanical');
#97695=PRODUCT('MAS-653','MAS-653',
'Independent compact industrial fixture table, bolted aluminum worktop
 on connected adjustable support base. Whole-mm nominal dimensions. No
 load rating assigned.',(#97694));
#97696=PRODUCT('Connecting frame','Connecting frame',$,(#97694));
#97697=PRODUCT('Longitudinal rail','Longitudinal rail',
'Steel rectangular hollow section, 50 x 40 mm, 4 mm wall. Square cut e
nds; weld to adjoining rails and corner plates.',(#97694));
#97698=PRODUCT('Transverse rail','Transverse rail',
'Steel rectangular hollow section, 50 x 40 mm, 4 mm wall. Square cut e
nds; weld to adjoining rails and corner plates.',(#97694));
#97699=PRODUCT('Corner plate','Corner plate',
'Weld rails to upper face. Four M8x1 attachment taps on 70 mm square p
attern match the leg plate clearance holes.',(#97694));
#97700=PRODUCT('Socket head cap screw M8x25',
'Socket head cap screw M8x25',$,(#97694));
#97701=PRODUCT('Flat Washer M8','Flat washer M8','NOT SPECIFIED',(#97694));
#97702=PRODUCT('Support leg','Support leg',$,(#97694));
#97703=PRODUCT('Leg post','Leg post',
'Independent aluminum extrusion section. Whole-mm nominal die dimensio
ns; parametric saw-cut length. Select structural loading, tolerances a
nd finish for the assembly application.',(#97694));
#97704=PRODUCT('Mounting plate','Mounting plate','Mounting plate',(#97694));
#97705=PRODUCT('Socket head cap screw M10x20',
'Socket head cap screw M10x20',$,(#97694));
#97706=PRODUCT('Grip sole','Grip sole',
'Bonded elastomer sole; nominal diameter 60 mm, thickness 4 mm.',(#97694));
#97707=PRODUCT('Swivel pad','Swivel pad',$,(#97694));
#97708=PRODUCT('Ball retainer','Ball retainer',$,(#97694));
#97709=PRODUCT('Adjusting spindle','Adjusting spindle',$,(#97694));
#97710=PRODUCT('Lock nut M10','Lock nut M10',$,(#97694));
#97711=PRODUCT('Flat washer M10','Flat washer M10',$,(#97694));
#97712=PRODUCT('Socket head cap screw M6x16',
'Socket head cap screw M6x16',$,(#97694));
#97713=PRODUCT('Worktop','Worktop',
'Aluminum fixture worktop. Six M6x1 through attachment holes; 650 x 55
0 x 20 mm stock.',(#97694));
#97714=PRODUCT('Socket head cap screw M6x50',
'Socket head cap screw M6x50',$,(#97694));
#97715=PRODUCT('Crush sleeve','Crush sleeve',
'Steel compression sleeve inside the hollow frame tube; protects tube 
walls when worktop fasteners are tightened.',(#97694));
#97716=PRODUCT('Flat washer M6','Flat washer M6',$,(#97694));
#97717=PRESENTATION_STYLE_ASSIGNMENT((#97724));
#97718=PRESENTATION_STYLE_ASSIGNMENT((#97725));
#97719=PRESENTATION_STYLE_ASSIGNMENT((#97726));
#97720=PRESENTATION_STYLE_ASSIGNMENT((#97727));
#97721=PRESENTATION_STYLE_ASSIGNMENT((#97728));
#97722=PRESENTATION_STYLE_ASSIGNMENT((#97729));
#97723=PRESENTATION_STYLE_ASSIGNMENT((#97730));
#97724=SURFACE_STYLE_USAGE(.BOTH.,#97731);
#97725=SURFACE_STYLE_USAGE(.BOTH.,#97732);
#97726=SURFACE_STYLE_USAGE(.BOTH.,#97733);
#97727=SURFACE_STYLE_USAGE(.BOTH.,#97734);
#97728=SURFACE_STYLE_USAGE(.BOTH.,#97735);
#97729=SURFACE_STYLE_USAGE(.BOTH.,#97736);
#97730=SURFACE_STYLE_USAGE(.BOTH.,#97737);
#97731=SURFACE_SIDE_STYLE('',(#97738));
#97732=SURFACE_SIDE_STYLE('',(#97739));
#97733=SURFACE_SIDE_STYLE('',(#97740));
#97734=SURFACE_SIDE_STYLE('',(#97741));
#97735=SURFACE_SIDE_STYLE('',(#97742));
#97736=SURFACE_SIDE_STYLE('',(#97743));
#97737=SURFACE_SIDE_STYLE('',(#97744));
#97738=SURFACE_STYLE_FILL_AREA(#97745);
#97739=SURFACE_STYLE_FILL_AREA(#97746);
#97740=SURFACE_STYLE_FILL_AREA(#97747);
#97741=SURFACE_STYLE_FILL_AREA(#97748);
#97742=SURFACE_STYLE_FILL_AREA(#97749);
#97743=SURFACE_STYLE_FILL_AREA(#97750);
#97744=SURFACE_STYLE_FILL_AREA(#97751);
#97745=FILL_AREA_STYLE('Steel - Satin',(#97752));
#97746=FILL_AREA_STYLE('Dark blue',(#97753));
#97747=FILL_AREA_STYLE('Sky blue',(#97754));
#97748=FILL_AREA_STYLE('Dark gray',(#97755));
#97749=FILL_AREA_STYLE('Light gray',(#97756));
#97750=FILL_AREA_STYLE('Gray',(#97757));
#97751=FILL_AREA_STYLE('Light blue',(#97758));
#97752=FILL_AREA_STYLE_COLOUR('Steel - Satin',#97759);
#97753=FILL_AREA_STYLE_COLOUR('Dark blue',#97760);
#97754=FILL_AREA_STYLE_COLOUR('Sky blue',#97761);
#97755=FILL_AREA_STYLE_COLOUR('Dark gray',#97762);
#97756=FILL_AREA_STYLE_COLOUR('Light gray',#97763);
#97757=FILL_AREA_STYLE_COLOUR('Gray',#97764);
#97758=FILL_AREA_STYLE_COLOUR('Light blue',#97765);
#97759=COLOUR_RGB('Steel - Satin',0.627450980392157,0.627450980392157,0.627450980392157);
#97760=COLOUR_RGB('Dark blue',0.0901960784313725,0.270588235294118,0.513725490196078);
#97761=COLOUR_RGB('Sky blue',0.317647058823529,0.686274509803922,0.890196078431372);
#97762=COLOUR_RGB('Dark gray',0.250980392156863,0.282352941176471,0.32156862745098);
#97763=COLOUR_RGB('Light gray',0.725490196078431,0.752941176470588,0.792156862745098);
#97764=COLOUR_RGB('Gray',0.407843137254902,0.447058823529412,0.498039215686275);
#97765=COLOUR_RGB('Light blue',0.662745098039216,0.831372549019608,0.949019607843137);
ENDSEC;
END-ISO-10303-21;
